#55329=CARTESIAN_POINT('Ctrl Pts',(66.2024832934866,-23.1474017566484,12.));
#55330=CARTESIAN_POINT('Ctrl Pts',(66.2222592165473,-23.1487761349328,0.));
#55331=CARTESIAN_POINT('Ctrl Pts',(66.2222592165473,-23.1487761349328,12.));
#55332=CARTESIAN_POINT('Ctrl Pts',(66.2420899237317,-23.1501329914488,0.));
#55333=CARTESIAN_POINT('Ctrl Pts',(66.2420899237317,-23.1501329914488,12.));
#55334=CARTESIAN_POINT('Ctrl Pts',(66.2619751878741,-23.1514722022483,0.));
#55335=CARTESIAN_POINT('Ctrl Pts',(66.2619751878741,-23.1514722022483,12.));
#55336=CARTESIAN_POINT('Ctrl Pts',(66.2819148131071,-23.1527936592625,0.));
#55337=CARTESIAN_POINT('Ctrl Pts',(66.2819148131071,-23.1527936592625,12.));
#55338=CARTESIAN_POINT('Ctrl Pts',(66.301908627539,-23.154097266617,0.));
#55339=CARTESIAN_POINT('Ctrl Pts',(66.301908627539,-23.154097266617,12.));
#55340=CARTESIAN_POINT('Ctrl Pts',(66.3219564725161,-23.1553829352531,0.));
#55341=CARTESIAN_POINT('Ctrl Pts',(66.3219564725161,-23.1553829352531,12.));
#55342=CARTESIAN_POINT('Ctrl Pts',(66.3420581937159,-23.1566505784626,0.));
#55343=CARTESIAN_POINT('Ctrl Pts',(66.3420581937159,-23.1566505784626,12.));
#55344=CARTESIAN_POINT('Ctrl Pts',(66.3622136300691,-23.1579001063438,0.));
#55345=CARTESIAN_POINT('Ctrl Pts',(66.3622136300691,-23.1579001063438,12.));
#55346=CARTESIAN_POINT('Ctrl Pts',(66.382422608185,-23.1591314230101,0.));
#55347=CARTESIAN_POINT('Ctrl Pts',(66.382422608185,-23.1591314230101,12.));
#55348=CARTESIAN_POINT('Ctrl Pts',(66.402684948127,-23.1603444294754,0.));
#55349=CARTESIAN_POINT('Ctrl Pts',(66.402684948127,-23.1603444294754,12.));
#55350=CARTESIAN_POINT('Ctrl Pts',(66.4230004670288,-23.1615390254636,0.));
#55351=CARTESIAN_POINT('Ctrl Pts',(66.4230004670288,-23.1615390254636,12.));
#55352=CARTESIAN_POINT('Ctrl Pts',(66.4433689832454,-23.1627151114875,0.));
#55353=CARTESIAN_POINT('Ctrl Pts',(66.4433689832454,-23.1627151114875,12.));
#55354=CARTESIAN_POINT('Ctrl Pts',(66.4637903210682,-23.163872591218,0.));
#55355=CARTESIAN_POINT('Ctrl Pts',(66.4637903210682,-23.163872591218,12.));
#55356=CARTESIAN_POINT('Ctrl Pts',(66.4842643105263,-23.1650113713792,0.));
#55357=CARTESIAN_POINT('Ctrl Pts',(66.4842643105263,-23.1650113713792,12.));
#55358=CARTESIAN_POINT('Ctrl Pts',(66.5047907851318,-23.1661313606123,0.));
#55359=CARTESIAN_POINT('Ctrl Pts',(66.5047907851318,-23.1661313606123,12.));
#55360=CARTESIAN_POINT('Ctrl Pts',(66.5253695803208,-23.1672324686928,0.));
#55361=CARTESIAN_POINT('Ctrl Pts',(66.5253695803208,-23.1672324686928,12.));
#55362=CARTESIAN_POINT('Ctrl Pts',(66.5460005315406,-23.1683146055736,0.));
#55363=CARTESIAN_POINT('Ctrl Pts',(66.5460005315406,-23.1683146055736,12.));
#55364=CARTESIAN_POINT('Ctrl Pts',(66.5666834726494,-23.169377680588,0.));
#55365=CARTESIAN_POINT('Ctrl Pts',(66.5666834726494,-23.169377680588,12.));
#55366=CARTESIAN_POINT('Ctrl Pts',(66.5874182367596,-23.1704216028626,0.));
#55367=CARTESIAN_POINT('Ctrl Pts',(66.5874182367596,-23.1704216028626,12.));
#55368=CARTESIAN_POINT('Ctrl Pts',(66.6082046569657,-23.1714462816794,0.));
#55369=CARTESIAN_POINT('Ctrl Pts',(66.6082046569657,-23.1714462816794,12.));
#55370=CARTESIAN_POINT('Ctrl Pts',(66.6290425670538,-23.1724516268299,0.));
#55371=CARTESIAN_POINT('Ctrl Pts',(66.6290425670538,-23.1724516268299,12.));
#55372=CARTESIAN_POINT('Ctrl Pts',(66.6499318023445,-23.1734375490421,0.));
#55373=CARTESIAN_POINT('Ctrl Pts',(66.6499318023445,-23.1734375490421,12.));
#55374=CARTESIAN_POINT('Ctrl Pts',(66.6708722000046,-23.174403960137,0.));
#55375=CARTESIAN_POINT('Ctrl Pts',(66.6708722000046,-23.174403960137,12.));
#55376=CARTESIAN_POINT('Ctrl Pts',(66.691863598595,-23.1753507727932,0.));
#55377=CARTESIAN_POINT('Ctrl Pts',(66.691863598595,-23.1753507727932,12.));
#55378=CARTESIAN_POINT('Ctrl Pts',(66.712905837789,-23.1762779004043,0.));
#55379=CARTESIAN_POINT('Ctrl Pts',(66.712905837789,-23.1762779004043,12.));
#55380=CARTESIAN_POINT('Ctrl Pts',(66.7339987580441,-23.1771852569137,0.));
#55381=CARTESIAN_POINT('Ctrl Pts',(66.7339987580441,-23.1771852569137,12.));
#55382=CARTESIAN_POINT('Ctrl Pts',(66.7551422002229,-23.1780727566309,0.));
#55383=CARTESIAN_POINT('Ctrl Pts',(66.7551422002229,-23.1780727566309,12.));
#55384=CARTESIAN_POINT('Ctrl Pts',(66.7763360056146,-23.1789403142376,0.));
#55385=CARTESIAN_POINT('Ctrl Pts',(66.7763360056146,-23.1789403142376,12.));
#55386=CARTESIAN_POINT('Ctrl Pts',(66.7975800161014,-23.1797878448645,0.));
#55387=CARTESIAN_POINT('Ctrl Pts',(66.7975800161014,-23.1797878448645,12.));
#55388=CARTESIAN_POINT('Ctrl Pts',(66.8188740742727,-23.1806152641475,0.));
#55389=CARTESIAN_POINT('Ctrl Pts',(66.8188740742727,-23.1806152641475,12.));
#55390=CARTESIAN_POINT('Ctrl Pts',(66.8402180235549,-23.1814224882948,0.));
#55391=CARTESIAN_POINT('Ctrl Pts',(66.8402180235549,-23.1814224882948,12.));
#55392=CARTESIAN_POINT('Ctrl Pts',(66.8616117083304,-23.1822094341508,0.));
#55393=CARTESIAN_POINT('Ctrl Pts',(66.8616117083304,-23.1822094341508,12.));
#55394=CARTESIAN_POINT('Ctrl Pts',(66.8830549738768,-23.1829760191583,0.));
#55395=CARTESIAN_POINT('Ctrl Pts',(66.8830549738768,-23.1829760191583,12.));
#55396=CARTESIAN_POINT('Ctrl Pts',(66.904547666305,-23.1837221613231,0.));
#55397=CARTESIAN_POINT('Ctrl Pts',(66.904547666305,-23.1837221613231,12.));
#55398=CARTESIAN_POINT('Ctrl Pts',(66.9260896324955,-23.1844477791816,0.));
#55399=CARTESIAN_POINT('Ctrl Pts',(66.9260896324955,-23.1844477791816,12.));
#55400=CARTESIAN_POINT('Ctrl Pts',(66.9476807200225,-23.1851527917666,0.));
#55401=CARTESIAN_POINT('Ctrl Pts',(66.9476807200225,-23.1851527917666,12.));
#55402=CARTESIAN_POINT('Ctrl Pts',(66.9693207771058,-23.1858371185852,0.));
#55403=CARTESIAN_POINT('Ctrl Pts',(66.9693207771058,-23.1858371185852,12.));
#55404=CARTESIAN_POINT('Ctrl Pts',(66.9910096526483,-23.1865006796291,0.));
#55405=CARTESIAN_POINT('Ctrl Pts',(66.9910096526483,-23.1865006796291,12.));
#55406=CARTESIAN_POINT('Ctrl Pts',(67.0127471962507,-23.1871433953796,0.));
#55407=CARTESIAN_POINT('Ctrl Pts',(67.0127471962507,-23.1871433953796,12.));
#55408=CARTESIAN_POINT('Ctrl Pts',(67.0345332582297,-23.1877651868155,0.));
#55409=CARTESIAN_POINT('Ctrl Pts',(67.0345332582297,-23.1877651868155,12.));
#55410=CARTESIAN_POINT('Ctrl Pts',(67.0563676896312,-23.1883659754268,0.));
#55411=CARTESIAN_POINT('Ctrl Pts',(67.0563676896312,-23.1883659754268,12.));
#55412=CARTESIAN_POINT('Ctrl Pts',(67.0782503422293,-23.1889456832116,0.));
#55413=CARTESIAN_POINT('Ctrl Pts',(67.0782503422293,-23.1889456832116,12.));
#55414=CARTESIAN_POINT('Ctrl Pts',(67.1001810685137,-23.1895042326626,0.));
#55415=CARTESIAN_POINT('Ctrl Pts',(67.1001810685137,-23.1895042326626,12.));
#55416=CARTESIAN_POINT('Ctrl Pts',(67.122159721674,-23.1900415467575,0.));
#55417=CARTESIAN_POINT('Ctrl Pts',(67.122159721674,-23.1900415467575,12.));
#55418=CARTESIAN_POINT('Ctrl Pts',(67.1441861555819,-23.1905575489506,0.));
#55419=CARTESIAN_POINT('Ctrl Pts',(67.1441861555819,-23.1905575489506,12.));
#55420=CARTESIAN_POINT('Ctrl Pts',(67.1662602247641,-23.1910521631658,0.));
#55421=CARTESIAN_POINT('Ctrl Pts',(67.1662602247641,-23.1910521631658,12.));
#55422=CARTESIAN_POINT('Ctrl Pts',(67.1883817844039,-23.1915253137924,0.));
#55423=CARTESIAN_POINT('Ctrl Pts',(67.1883817844039,-23.1915253137924,12.));
#55424=CARTESIAN_POINT('Ctrl Pts',(67.2105506903448,-23.1919769256804,0.));
#55425=CARTESIAN_POINT('Ctrl Pts',(67.2105506903448,-23.1919769256804,12.));
#55426=CARTESIAN_POINT('Ctrl Pts',(67.232766799088,-23.1924069241386,0.));
#55427=CARTESIAN_POINT('Ctrl Pts',(67.232766799088,-23.1924069241386,12.));
#55428=CARTESIAN_POINT('Ctrl Pts',(67.2550299677888,-23.1928152349344,0.));
#55429=CARTESIAN_POINT('Ctrl Pts',(67.2550299677888,-23.1928152349344,12.));
#55430=CARTESIAN_POINT('Ctrl Pts',(67.2773400542477,-23.1932017842954,0.));
#55431=CARTESIAN_POINT('Ctrl Pts',(67.2773400542477,-23.1932017842954,12.));
#55432=CARTESIAN_POINT('Ctrl Pts',(67.2996969169099,-23.193566498902,0.));
#55433=CARTESIAN_POINT('Ctrl Pts',(67.2996969169099,-23.193566498902,12.));
#55434=CARTESIAN_POINT('Ctrl Pts',(67.3221004148604,-23.1939093058802,0.));
#55435=CARTESIAN_POINT('Ctrl Pts',(67.3221004148604,-23.1939093058802,12.));
#55436=CARTESIAN_POINT('Ctrl Pts',(67.3445504078178,-23.1942301327979,0.));
#55437=CARTESIAN_POINT('Ctrl Pts',(67.3445504078178,-23.1942301327979,12.));
#55438=CARTESIAN_POINT('Ctrl Pts',(67.3670467561205,-23.1945289076608,0.));
#55439=CARTESIAN_POINT('Ctrl Pts',(67.3670467561205,-23.1945289076608,12.));
#55440=CARTESIAN_POINT('Ctrl Pts',(67.3895893207168,-23.1948055589123,0.));
#55441=CARTESIAN_POINT('Ctrl Pts',(67.3895893207168,-23.1948055589123,12.));
#55442=CARTESIAN_POINT('Ctrl Pts',(67.4121779631666,-23.195060015426,0.));
#55443=CARTESIAN_POINT('Ctrl Pts',(67.4121779631666,-23.195060015426,12.));
#55444=CARTESIAN_POINT('Ctrl Pts',(67.4348125456389,-23.1952922065009,0.));
#55445=CARTESIAN_POINT('Ctrl Pts',(67.4348125456389,-23.1952922065009,12.));
#55446=CARTESIAN_POINT('Ctrl Pts',(67.4574929309078,-23.1955020618591,0.));
#55447=CARTESIAN_POINT('Ctrl Pts',(67.4574929309078,-23.1955020618591,12.));
#55448=CARTESIAN_POINT('Ctrl Pts',(67.4802189823423,-23.1956895116446,0.));
#55449=CARTESIAN_POINT('Ctrl Pts',(67.4802189823423,-23.1956895116446,12.));
#55450=CARTESIAN_POINT('Ctrl Pts',(67.5029905638973,-23.1958544864225,0.));
#55451=CARTESIAN_POINT('Ctrl Pts',(67.5029905638973,-23.1958544864225,12.));
#55452=CARTESIAN_POINT('Ctrl Pts',(67.525807540117,-23.195996917171,0.));
#55453=CARTESIAN_POINT('Ctrl Pts',(67.525807540117,-23.195996917171,12.));
#55454=CARTESIAN_POINT('Ctrl Pts',(67.5486697761301,-23.1961167352777,0.));
#55455=CARTESIAN_POINT('Ctrl Pts',(67.5486697761301,-23.1961167352777,12.));
#55456=CARTESIAN_POINT('Ctrl Pts',(67.5715771376454,-23.1962138725358,0.));
#55457=CARTESIAN_POINT('Ctrl Pts',(67.5715771376454,-23.1962138725358,12.));
#55458=CARTESIAN_POINT('Ctrl Pts',(67.5945294909398,-23.1962882611444,0.));
#55459=CARTESIAN_POINT('Ctrl Pts',(67.5945294909398,-23.1962882611444,12.));
#55460=CARTESIAN_POINT('Ctrl Pts',(67.6175267028516,-23.1963398337056,0.));
#55461=CARTESIAN_POINT('Ctrl Pts',(67.6175267028516,-23.1963398337056,12.));
#55462=CARTESIAN_POINT('Ctrl Pts',(67.6405686407828,-23.1963685232176,0.));
#55463=CARTESIAN_POINT('Ctrl Pts',(67.6405686407828,-23.1963685232176,12.));
#55464=CARTESIAN_POINT('Ctrl Pts',(67.6636551726948,-23.196374263071,0.));
#55465=CARTESIAN_POINT('Ctrl Pts',(67.6636551726948,-23.196374263071,12.));
#55466=CARTESIAN_POINT('Ctrl Pts',(67.6867861671044,-23.1963569870457,0.));
#55467=CARTESIAN_POINT('Ctrl Pts',(67.6867861671044,-23.1963569870457,12.));
#55468=CARTESIAN_POINT('Ctrl Pts',(67.7099614930711,-23.1963166293116,0.));
#55469=CARTESIAN_POINT('Ctrl Pts',(67.7099614930711,-23.1963166293116,12.));
#55470=CARTESIAN_POINT('Ctrl Pts',(67.7331810201931,-23.1962531244261,0.));
#55471=CARTESIAN_POINT('Ctrl Pts',(67.7331810201931,-23.1962531244261,12.));
#55472=CARTESIAN_POINT('Ctrl Pts',(67.7564446186115,-23.1961664073274,0.));
#55473=CARTESIAN_POINT('Ctrl Pts',(67.7564446186115,-23.1961664073274,12.));
#55474=CARTESIAN_POINT('Ctrl Pts',(67.7797521590056,-23.1960564133308,0.));
#55475=CARTESIAN_POINT('Ctrl Pts',(67.7797521590056,-23.1960564133308,12.));
#55476=CARTESIAN_POINT('Ctrl Pts',(67.8031035125873,-23.1959230781265,0.));
#55477=CARTESIAN_POINT('Ctrl Pts',(67.8031035125873,-23.1959230781265,12.));
#55478=CARTESIAN_POINT('Ctrl Pts',(67.8264985510884,-23.1957663377798,0.));
#55479=CARTESIAN_POINT('Ctrl Pts',(67.8264985510884,-23.1957663377798,12.));
#55480=CARTESIAN_POINT('Ctrl Pts',(67.8499371467578,-23.1955861287276,0.));
#55481=CARTESIAN_POINT('Ctrl Pts',(67.8499371467578,-23.1955861287276,12.));
#55482=CARTESIAN_POINT('Ctrl Pts',(67.8734191723639,-23.1953823877727,0.));
#55483=CARTESIAN_POINT('Ctrl Pts',(67.8734191723639,-23.1953823877727,12.));
#55484=CARTESIAN_POINT('Ctrl Pts',(67.8969445011907,-23.19515505208,0.));
#55485=CARTESIAN_POINT('Ctrl Pts',(67.8969445011907,-23.19515505208,12.));
#55486=CARTESIAN_POINT('Ctrl Pts',(67.9205130070337,-23.1949040591748,0.));
#55487=CARTESIAN_POINT('Ctrl Pts',(67.9205130070337,-23.1949040591748,12.));
#55488=CARTESIAN_POINT('Ctrl Pts',(67.944124564187,-23.1946293469437,0.));
#55489=CARTESIAN_POINT('Ctrl Pts',(67.944124564187,-23.1946293469437,12.));
#55490=CARTESIAN_POINT('Ctrl Pts',(67.9677790474414,-23.1943308536307,0.));
#55491=CARTESIAN_POINT('Ctrl Pts',(67.9677790474414,-23.1943308536307,12.));
#55492=CARTESIAN_POINT('Ctrl Pts',(67.9914763320878,-23.194008517832,0.));
#55493=CARTESIAN_POINT('Ctrl Pts',(67.9914763320878,-23.194008517832,12.));
#55494=CARTESIAN_POINT('Ctrl Pts',(68.0152162939123,-23.193662278492,0.));
#55495=CARTESIAN_POINT('Ctrl Pts',(68.0152162939123,-23.193662278492,12.));
#55496=CARTESIAN_POINT('Ctrl Pts',(68.0389988091926,-23.1932920749021,0.));
#55497=CARTESIAN_POINT('Ctrl Pts',(68.0389988091926,-23.1932920749021,12.));
#55498=CARTESIAN_POINT('Ctrl Pts',(68.0628237546852,-23.1928978467018,0.));
#55499=CARTESIAN_POINT('Ctrl Pts',(68.0628237546852,-23.1928978467018,12.));
#55500=CARTESIAN_POINT('Ctrl Pts',(68.086691007624,-23.1924795338746,0.));
#55501=CARTESIAN_POINT('Ctrl Pts',(68.086691007624,-23.1924795338746,12.));
#55502=CARTESIAN_POINT('Ctrl Pts',(68.1106004457223,-23.1920370767424,0.));
#55503=CARTESIAN_POINT('Ctrl Pts',(68.1106004457223,-23.1920370767424,12.));
#55504=CARTESIAN_POINT('Ctrl Pts',(68.1345519471695,-23.1915704159624,0.));
#55505=CARTESIAN_POINT('Ctrl Pts',(68.1345519471695,-23.1915704159624,12.));
#55506=CARTESIAN_POINT('Ctrl Pts',(68.1585453906259,-23.1910794925252,0.));
#55507=CARTESIAN_POINT('Ctrl Pts',(68.1585453906259,-23.1910794925252,12.));
#55508=CARTESIAN_POINT('Ctrl Pts',(68.182580655213,-23.1905642477572,0.));
#55509=CARTESIAN_POINT('Ctrl Pts',(68.182580655213,-23.1905642477572,12.));
#55510=CARTESIAN_POINT('Ctrl Pts',(68.2066576205113,-23.1900246233165,0.));
#55511=CARTESIAN_POINT('Ctrl Pts',(68.2066576205113,-23.1900246233165,12.));
#55512=CARTESIAN_POINT('Ctrl Pts',(68.2307761665629,-23.189460561187,0.));
#55513=CARTESIAN_POINT('Ctrl Pts',(68.2307761665629,-23.189460561187,12.));
#55514=CARTESIAN_POINT('Ctrl Pts',(68.2549361738679,-23.1888720036757,0.));
#55515=CARTESIAN_POINT('Ctrl Pts',(68.2549361738679,-23.1888720036757,12.));
#55516=CARTESIAN_POINT('Ctrl Pts',(68.2791375233798,-23.1882588934108,0.));
#55517=CARTESIAN_POINT('Ctrl Pts',(68.2791375233798,-23.1882588934108,12.));
#55518=CARTESIAN_POINT('Ctrl Pts',(68.3033800964946,-23.1876211733439,0.));
#55519=CARTESIAN_POINT('Ctrl Pts',(68.3033800964946,-23.1876211733439,12.));
#55520=CARTESIAN_POINT('Ctrl Pts',(68.3276637750494,-23.1869587867464,0.));
#55521=CARTESIAN_POINT('Ctrl Pts',(68.3276637750494,-23.1869587867464,12.));
#55522=CARTESIAN_POINT('Ctrl Pts',(68.3519884413253,-23.1862716772034,0.));
#55523=CARTESIAN_POINT('Ctrl Pts',(68.3519884413253,-23.1862716772034,12.));
#55524=CARTESIAN_POINT('Ctrl Pts',(68.3763539780442,-23.1855597886117,0.));
#55525=CARTESIAN_POINT('Ctrl Pts',(68.3763539780442,-23.1855597886117,12.));
#55526=CARTESIAN_POINT('Ctrl Pts',(68.4007602683649,-23.1848230651776,0.));
#55527=CARTESIAN_POINT('Ctrl Pts',(68.4007602683649,-23.1848230651776,12.));
#55528=CARTESIAN_POINT('Ctrl Pts',(68.4252071958725,-23.1840614514191,0.));
#55529=CARTESIAN_POINT('Ctrl Pts',(68.4252071958725,-23.1840614514191,12.));
#55530=CARTESIAN_POINT('Ctrl Pts',(68.4496946445756,-23.1832748921629,0.));
#55531=CARTESIAN_POINT('Ctrl Pts',(68.4496946445756,-23.1832748921629,12.));
#55532=CARTESIAN_POINT('Ctrl Pts',(68.4742224989099,-23.1824633325385,0.));
#55533=CARTESIAN_POINT('Ctrl Pts',(68.4742224989099,-23.1824633325385,12.));
#55534=CARTESIAN_POINT('Ctrl Pts',(68.4987906437357,-23.1816267179752,0.));
#55535=CARTESIAN_POINT('Ctrl Pts',(68.4987906437357,-23.1816267179752,12.));
#55536=CARTESIAN_POINT('Ctrl Pts',(68.5233989643343,-23.1807649942011,0.));
#55537=CARTESIAN_POINT('Ctrl Pts',(68.5233989643343,-23.1807649942011,12.));
#55538=CARTESIAN_POINT('Ctrl Pts',(68.548047346398,-23.1798781072449,0.));
#55539=CARTESIAN_POINT('Ctrl Pts',(68.548047346398,-23.1798781072449,12.));
#55540=CARTESIAN_POINT('Ctrl Pts',(68.572735676027,-23.178966003434,0.));
#55541=CARTESIAN_POINT('Ctrl Pts',(68.572735676027,-23.178966003434,12.));
#55542=CARTESIAN_POINT('Ctrl Pts',(68.5974638397322,-23.1780286293873,0.));
#55543=CARTESIAN_POINT('Ctrl Pts',(68.5974638397322,-23.1780286293873,12.));
#55544=CARTESIAN_POINT('Ctrl Pts',(68.6222317244336,-23.1770659320137,0.));
#55545=CARTESIAN_POINT('Ctrl Pts',(68.6222317244336,-23.1770659320137,12.));
#55546=CARTESIAN_POINT('Ctrl Pts',(68.6470392174567,-23.1760778585094,0.));
#55547=CARTESIAN_POINT('Ctrl Pts',(68.6470392174567,-23.1760778585094,12.));
#55548=CARTESIAN_POINT('Ctrl Pts',(68.6718862065227,-23.1750643563606,0.));
#55549=CARTESIAN_POINT('Ctrl Pts',(68.6718862065227,-23.1750643563606,12.));
#55550=CARTESIAN_POINT('Ctrl Pts',(68.6967725797457,-23.1740253733423,0.));
#55551=CARTESIAN_POINT('Ctrl Pts',(68.6967725797457,-23.1740253733423,12.));
#55552=CARTESIAN_POINT('Ctrl Pts',(68.7216982256357,-23.1729608575116,0.));
#55553=CARTESIAN_POINT('Ctrl Pts',(68.7216982256357,-23.1729608575116,12.));
#55554=CARTESIAN_POINT('Ctrl Pts',(68.7466630330968,-23.1718707572047,0.));
#55555=CARTESIAN_POINT('Ctrl Pts',(68.7466630330968,-23.1718707572047,12.));
#55556=CARTESIAN_POINT('Ctrl Pts',(68.7716668914246,-23.1707550210359,0.));
#55557=CARTESIAN_POINT('Ctrl Pts',(68.7716668914246,-23.1707550210359,12.));
#55558=CARTESIAN_POINT('Ctrl Pts',(68.7967096902981,-23.1696135978993,0.));
#55559=CARTESIAN_POINT('Ctrl Pts',(68.7967096902981,-23.1696135978993,12.));
#55560=CARTESIAN_POINT('Ctrl Pts',(68.8217913197735,-23.1684464369681,0.));
#55561=CARTESIAN_POINT('Ctrl Pts',(68.8217913197735,-23.1684464369681,12.));
#55562=CARTESIAN_POINT('Ctrl Pts',(68.8469116702885,-23.1672534876885,0.));
#55563=CARTESIAN_POINT('Ctrl Pts',(68.8469116702885,-23.1672534876885,12.));
#55564=CARTESIAN_POINT('Ctrl Pts',(68.8720706326605,-23.1660346997763,0.));
#55565=CARTESIAN_POINT('Ctrl Pts',(68.8720706326605,-23.1660346997763,12.));
#55566=CARTESIAN_POINT('Ctrl Pts',(68.8972680980844,-23.1647900232152,0.));
#55567=CARTESIAN_POINT('Ctrl Pts',(68.8972680980844,-23.1647900232152,12.));
#55568=CARTESIAN_POINT('Ctrl Pts',(68.9225039581249,-23.1635194082582,0.));
#55569=CARTESIAN_POINT('Ctrl Pts',(68.9225039581249,-23.1635194082582,12.));
#55570=CARTESIAN_POINT('Ctrl Pts',(68.9477781047103,-23.1622228054291,0.));
#55571=CARTESIAN_POINT('Ctrl Pts',(68.9477781047103,-23.1622228054291,12.));
#55572=CARTESIAN_POINT('Ctrl Pts',(68.9730904301362,-23.1609001655154,0.));
#55573=CARTESIAN_POINT('Ctrl Pts',(68.9730904301362,-23.1609001655154,12.));
#55574=CARTESIAN_POINT('Ctrl Pts',(68.9984408270652,-23.1595514395655,0.));
#55575=CARTESIAN_POINT('Ctrl Pts',(68.9984408270652,-23.1595514395655,12.));
#55576=CARTESIAN_POINT('Ctrl Pts',(69.0238291885245,-23.1581765788869,0.));
#55577=CARTESIAN_POINT('Ctrl Pts',(69.0238291885245,-23.1581765788869,12.));
#55578=CARTESIAN_POINT('Ctrl Pts',(69.0492554078999,-23.1567755350472,0.));
#55579=CARTESIAN_POINT('Ctrl Pts',(69.0492554078999,-23.1567755350472,12.));
#55580=CARTESIAN_POINT('Ctrl Pts',(69.0747193789291,-23.1553482598768,0.));
#55581=CARTESIAN_POINT('Ctrl Pts',(69.0747193789291,-23.1553482598768,12.));
#55582=CARTESIAN_POINT('Ctrl Pts',(69.1002209957036,-23.153894705462,0.));
#55583=CARTESIAN_POINT('Ctrl Pts',(69.1002209957036,-23.153894705462,12.));
#55584=CARTESIAN_POINT('Ctrl Pts',(69.1257601526692,-23.1524148241413,0.));
#55585=CARTESIAN_POINT('Ctrl Pts',(69.1257601526692,-23.1524148241413,12.));
#55586=CARTESIAN_POINT('Ctrl Pts',(69.1513367446231,-23.1509085685033,0.));
#55587=CARTESIAN_POINT('Ctrl Pts',(69.1513367446231,-23.1509085685033,12.));
#55588=CARTESIAN_POINT('Ctrl Pts',(69.176950666708,-23.1493758913857,0.));
#55589=CARTESIAN_POINT('Ctrl Pts',(69.176950666708,-23.1493758913857,12.));
#55590=CARTESIAN_POINT('Ctrl Pts',(69.2026018144023,-23.1478167458788,0.));
#55591=CARTESIAN_POINT('Ctrl Pts',(69.2026018144023,-23.1478167458788,12.));
#55592=CARTESIAN_POINT('Ctrl Pts',(69.2282900835234,-23.1462310853205,0.));
#55593=CARTESIAN_POINT('Ctrl Pts',(69.2282900835234,-23.1462310853205,12.));
#55594=CARTESIAN_POINT('Ctrl Pts',(69.2540153702311,-23.1446188632931,0.));
#55595=CARTESIAN_POINT('Ctrl Pts',(69.2540153702311,-23.1446188632931,12.));
#55596=CARTESIAN_POINT('Ctrl Pts',(69.2797775710275,-23.1429800336221,0.));
#55597=CARTESIAN_POINT('Ctrl Pts',(69.2797775710275,-23.1429800336221,12.));
#55598=CARTESIAN_POINT('Ctrl Pts',(69.3055765827544,-23.1413145503763,0.));
#55599=CARTESIAN_POINT('Ctrl Pts',(69.3055765827544,-23.1413145503763,12.));
#55600=CARTESIAN_POINT('Ctrl Pts',(69.3314123025863,-23.1396223678725,0.));
#55601=CARTESIAN_POINT('Ctrl Pts',(69.3314123025863,-23.1396223678725,12.));
#55602=CARTESIAN_POINT('Ctrl Pts',(69.3572846280289,-23.1379034406718,0.));
#55603=CARTESIAN_POINT('Ctrl Pts',(69.3572846280289,-23.1379034406718,12.));
#55604=CARTESIAN_POINT('Ctrl Pts',(69.3831934569176,-23.1361577235708,0.));
#55605=CARTESIAN_POINT('Ctrl Pts',(69.3831934569176,-23.1361577235708,12.));
#55606=CARTESIAN_POINT('Ctrl Pts',(69.4091386874129,-23.1343851715989,0.));
#55607=CARTESIAN_POINT('Ctrl Pts',(69.4091386874129,-23.1343851715989,12.));
#55608=CARTESIAN_POINT('Ctrl Pts',(69.4351202179948,-23.1325857400145,0.));
#55609=CARTESIAN_POINT('Ctrl Pts',(69.4351202179948,-23.1325857400145,12.));
#55610=CARTESIAN_POINT('Ctrl Pts',(69.4611379474491,-23.1307593843063,0.));
#55611=CARTESIAN_POINT('Ctrl Pts',(69.4611379474491,-23.1307593843063,12.));
#55612=CARTESIAN_POINT('Ctrl Pts',(69.4871917748665,-23.1289060601927,0.));
#55613=CARTESIAN_POINT('Ctrl Pts',(69.4871917748665,-23.1289060601927,12.));
#55614=CARTESIAN_POINT('Ctrl Pts',(69.5132815996548,-23.1270257236207,0.));
#55615=CARTESIAN_POINT('Ctrl Pts',(69.5132815996548,-23.1270257236207,12.));
#55616=CARTESIAN_POINT('Ctrl Pts',(69.5394073215467,-23.1251183307678,0.));
#55617=CARTESIAN_POINT('Ctrl Pts',(69.5394073215467,-23.1251183307678,12.));
#55618=CARTESIAN_POINT('Ctrl Pts',(69.565568840605,-23.1231838380452,0.));
#55619=CARTESIAN_POINT('Ctrl Pts',(69.565568840605,-23.1231838380452,12.));
#55620=CARTESIAN_POINT('Ctrl Pts',(69.5917660572255,-23.1212222021049,0.));
#55621=CARTESIAN_POINT('Ctrl Pts',(69.5917660572255,-23.1212222021049,12.));
#55622=CARTESIAN_POINT('Ctrl Pts',(69.617998872135,-23.1192333798438,0.));
#55623=CARTESIAN_POINT('Ctrl Pts',(69.617998872135,-23.1192333798438,12.));
#55624=CARTESIAN_POINT('Ctrl Pts',(69.6442671863751,-23.1172173283856,0.));
#55625=CARTESIAN_POINT('Ctrl Pts',(69.6442671863751,-23.1172173283856,12.));
#55626=CARTESIAN_POINT('Ctrl Pts',(69.6705709012842,-23.1151740050679,0.));
#55627=CARTESIAN_POINT('Ctrl Pts',(69.6705709012842,-23.1151740050679,12.));
#55628=CARTESIAN_POINT('Ctrl Pts',(69.6969099184766,-23.1131033674301,0.));
#55629=CARTESIAN_POINT('Ctrl Pts',(69.6969099184766,-23.1131033674301,12.));
#55630=CARTESIAN_POINT('Ctrl Pts',(69.7232841398207,-23.111005373205,0.));
#55631=CARTESIAN_POINT('Ctrl Pts',(69.7232841398207,-23.111005373205,12.));
#55632=CARTESIAN_POINT('Ctrl Pts',(69.7496934674083,-23.1088799803094,0.));
#55633=CARTESIAN_POINT('Ctrl Pts',(69.7496934674083,-23.1088799803094,12.));
#55634=CARTESIAN_POINT('Ctrl Pts',(69.7761378035978,-23.1067271468615,0.));
#55635=CARTESIAN_POINT('Ctrl Pts',(69.7761378035978,-23.1067271468615,12.));
#55636=CARTESIAN_POINT('Ctrl Pts',(69.8026170510582,-23.1045468311994,0.));
#55637=CARTESIAN_POINT('Ctrl Pts',(69.8026170510582,-23.1045468311994,12.));
#55638=CARTESIAN_POINT('Ctrl Pts',(69.8291311128121,-23.1023389919052,0.));
#55639=CARTESIAN_POINT('Ctrl Pts',(69.8291311128121,-23.1023389919052,12.));
#55640=CARTESIAN_POINT('Ctrl Pts',(69.8556798922687,-23.100103587824,0.));
#55641=CARTESIAN_POINT('Ctrl Pts',(69.8556798922687,-23.100103587824,12.));
#55642=CARTESIAN_POINT('Ctrl Pts',(69.8822632932759,-23.0978405781018,0.));
#55643=CARTESIAN_POINT('Ctrl Pts',(69.8822632932759,-23.0978405781018,12.));
#55644=CARTESIAN_POINT('Ctrl Pts',(69.9088812200703,-23.0955499221556,0.));
#55645=CARTESIAN_POINT('Ctrl Pts',(69.9088812200703,-23.0955499221556,12.));
#55646=CARTESIAN_POINT('Ctrl Pts',(69.9355335771722,-23.0932315796066,0.));
#55647=CARTESIAN_POINT('Ctrl Pts',(69.9355335771722,-23.0932315796066,12.));
#55648=CARTESIAN_POINT('Ctrl Pts',(69.9622202692871,-23.0908855102251,0.));
#55649=CARTESIAN_POINT('Ctrl Pts',(69.9622202692871,-23.0908855102251,12.));
#55650=CARTESIAN_POINT('Ctrl Pts',(69.9889412012143,-23.0885116738799,0.));
#55651=CARTESIAN_POINT('Ctrl Pts',(69.9889412012143,-23.0885116738799,12.));
#55652=CARTESIAN_POINT('Ctrl Pts',(70.0156962777173,-23.0861100304731,0.));
#55653=CARTESIAN_POINT('Ctrl Pts',(70.0156962777173,-23.0861100304731,12.));
#55654=CARTESIAN_POINT('Ctrl Pts',(70.0424854035125,-23.0836805399378,0.));
#55655=CARTESIAN_POINT('Ctrl Pts',(70.0424854035125,-23.0836805399378,12.));
#55656=CARTESIAN_POINT('Ctrl Pts',(70.0693084835387,-23.081223162377,0.));
#55657=CARTESIAN_POINT('Ctrl Pts',(70.0693084835387,-23.081223162377,12.));
#55658=CARTESIAN_POINT('Ctrl Pts',(70.096165423165,-23.0787378581778,0.));
#55659=CARTESIAN_POINT('Ctrl Pts',(70.096165423165,-23.0787378581778,12.));
#55660=CARTESIAN_POINT('Ctrl Pts',(70.1230561284222,-23.076224588139,0.));
#55661=CARTESIAN_POINT('Ctrl Pts',(70.1230561284222,-23.076224588139,12.));
#55662=CARTESIAN_POINT('Ctrl Pts',(70.1499805062159,-23.0736833135934,0.));
#55663=CARTESIAN_POINT('Ctrl Pts',(70.1499805062159,-23.0736833135934,12.));
#55664=CARTESIAN_POINT('Ctrl Pts',(70.176938464556,-23.0711139965432,0.));
#55665=CARTESIAN_POINT('Ctrl Pts',(70.176938464556,-23.0711139965432,12.));
#55666=CARTESIAN_POINT('Ctrl Pts',(70.2039299120456,-23.0685165993682,0.));
#55667=CARTESIAN_POINT('Ctrl Pts',(70.2039299120456,-23.0685165993682,12.));
#55668=CARTESIAN_POINT('Ctrl Pts',(70.2309547573788,-23.0658910845425,0.));
#55669=CARTESIAN_POINT('Ctrl Pts',(70.2309547573788,-23.0658910845425,12.));
#55670=CARTESIAN_POINT('Ctrl Pts',(70.2580129087877,-23.0632374143276,0.));
#55671=CARTESIAN_POINT('Ctrl Pts',(70.2580129087877,-23.0632374143276,12.));
#55672=CARTESIAN_POINT('Ctrl Pts',(70.2851042736081,-23.0605555505326,0.));
#55673=CARTESIAN_POINT('Ctrl Pts',(70.2851042736081,-23.0605555505326,12.));
#55674=CARTESIAN_POINT('Ctrl Pts',(70.3122287575374,-23.0578454541116,0.));
#55675=CARTESIAN_POINT('Ctrl Pts',(70.3122287575374,-23.0578454541116,12.));
#55676=CARTESIAN_POINT('Ctrl Pts',(70.3393862652353,-23.0551070854942,0.));
#55677=CARTESIAN_POINT('Ctrl Pts',(70.3393862652353,-23.0551070854942,12.));
#55678=CARTESIAN_POINT('Ctrl Pts',(70.3665767016596,-23.0523404053188,0.));
#55679=CARTESIAN_POINT('Ctrl Pts',(70.3665767016596,-23.0523404053188,12.));
#55680=CARTESIAN_POINT('Ctrl Pts',(70.39379997323,-23.0495453750773,0.));
#55681=CARTESIAN_POINT('Ctrl Pts',(70.39379997323,-23.0495453750773,12.));
#55682=CARTESIAN_POINT('Ctrl Pts',(70.421055988934,-23.0467219577289,0.));
#55683=CARTESIAN_POINT('Ctrl Pts',(70.421055988934,-23.0467219577289,12.));
#55684=CARTESIAN_POINT('Ctrl Pts',(70.4483446617552,-23.0438701184996,0.));
#55685=CARTESIAN_POINT('Ctrl Pts',(70.4483446617552,-23.0438701184996,12.));
#55686=CARTESIAN_POINT('Ctrl Pts',(70.4756659090104,-23.0409898250727,0.));
#55687=CARTESIAN_POINT('Ctrl Pts',(70.4756659090104,-23.0409898250727,12.));
#55688=CARTESIAN_POINT('Ctrl Pts',(70.5030196491883,-23.0380810458237,0.));
#55689=CARTESIAN_POINT('Ctrl Pts',(70.5030196491883,-23.0380810458237,12.));
#55690=CARTESIAN_POINT('Ctrl Pts',(70.5304057994537,-23.035143748431,0.));
#55691=CARTESIAN_POINT('Ctrl Pts',(70.5304057994537,-23.035143748431,12.));
#55692=CARTESIAN_POINT('Ctrl Pts',(70.5578242727606,-23.0321778982705,0.));
#55693=CARTESIAN_POINT('Ctrl Pts',(70.5578242727606,-23.0321778982705,12.));
#55694=CARTESIAN_POINT('Ctrl Pts',(70.5852749754167,-23.0291834570688,0.));
#55695=CARTESIAN_POINT('Ctrl Pts',(70.5852749754167,-23.0291834570688,12.));
#55696=CARTESIAN_POINT('Ctrl Pts',(70.6127578036869,-23.0261603810187,0.));
#55697=CARTESIAN_POINT('Ctrl Pts',(70.6127578036869,-23.0261603810187,12.));
#55698=CARTESIAN_POINT('Ctrl Pts',(70.6402726486718,-23.0231086235263,0.));
#55699=CARTESIAN_POINT('Ctrl Pts',(70.6402726486718,-23.0231086235263,12.));
#55700=CARTESIAN_POINT('Ctrl Pts',(70.6678194023388,-23.0200281385906,0.));
#55701=CARTESIAN_POINT('Ctrl Pts',(70.6678194023388,-23.0200281385906,12.));
#55702=CARTESIAN_POINT('Ctrl Pts',(70.6953979633561,-23.0169188841084,0.));
#55703=CARTESIAN_POINT('Ctrl Pts',(70.6953979633561,-23.0169188841084,12.));
#55704=CARTESIAN_POINT('Ctrl Pts',(70.7230082425324,-23.0137808248899,0.));
#55705=CARTESIAN_POINT('Ctrl Pts',(70.7230082425324,-23.0137808248899,12.));
#55706=CARTESIAN_POINT('Ctrl Pts',(70.7506501695822,-23.0106139365941,0.));
#55707=CARTESIAN_POINT('Ctrl Pts',(70.7506501695822,-23.0106139365941,12.));
#55708=CARTESIAN_POINT('Ctrl Pts',(70.7783236950588,-23.0074182063611,0.));
#55709=CARTESIAN_POINT('Ctrl Pts',(70.7783236950588,-23.0074182063611,12.));
#55710=CARTESIAN_POINT('Ctrl Pts',(70.806028785987,-23.004193629142,0.));
#55711=CARTESIAN_POINT('Ctrl Pts',(70.806028785987,-23.004193629142,12.));
#55712=CARTESIAN_POINT('Ctrl Pts',(70.8282180956627,-23.0015908899222,0.));
#55713=CARTESIAN_POINT('Ctrl Pts',(70.8282180956627,-23.0015908899222,12.));
#55714=CARTESIAN_POINT('Ctrl Pts',(70.8448742696328,-22.9996258555187,0.));
#55715=CARTESIAN_POINT('Ctrl Pts',(70.8448742696328,-22.9996258555187,12.));
#55716=CARTESIAN_POINT('Ctrl Pts',(70.8559846927868,-22.9983100639354,0.));
#55717=CARTESIAN_POINT('Ctrl Pts',(70.8559846927868,-22.9983100639354,12.));
#55718=CARTESIAN_POINT('Ctrl Pts',(70.8615414811571,-22.9976507259817,0.));
#55719=CARTESIAN_POINT('Ctrl Pts',(70.8615414811571,-22.9976507259817,12.));
#55720=CARTESIAN_POINT('',(66.0656156664138,-23.1372951448024,0.));
#55721=CARTESIAN_POINT('Ctrl Pts',(66.0656156664138,-23.1372951448024,0.));
#55722=CARTESIAN_POINT('Ctrl Pts',(66.0694876382126,-23.1375957166104,0.));
#55723=CARTESIAN_POINT('Ctrl Pts',(66.0772371487248,-23.13819515974,0.));
#55724=CARTESIAN_POINT('Ctrl Pts',(66.088878115242,-23.1390892229779,0.));
#55725=CARTESIAN_POINT('Ctrl Pts',(66.1044328067355,-23.1402711039425,0.));
#55726=CARTESIAN_POINT('Ctrl Pts',(66.1239318368548,-23.1417314398398,0.));
#55727=CARTESIAN_POINT('Ctrl Pts',(66.1434865015027,-23.1431747350098,0.));
#55728=CARTESIAN_POINT('Ctrl Pts',(66.1630967296747,-23.1446009424903,0.));
#55729=CARTESIAN_POINT('Ctrl Pts',(66.1827623902899,-23.1460099850763,0.));
#55730=CARTESIAN_POINT('Ctrl Pts',(66.2024832934866,-23.1474017566484,0.));
#55731=CARTESIAN_POINT('Ctrl Pts',(66.2222592165473,-23.1487761349328,0.));
#55732=CARTESIAN_POINT('Ctrl Pts',(66.2420899237317,-23.1501329914488,0.));
#55733=CARTESIAN_POINT('Ctrl Pts',(66.2619751878741,-23.1514722022483,0.));
#55734=CARTESIAN_POINT('Ctrl Pts',(66.2819148131071,-23.1527936592625,0.));
#55735=CARTESIAN_POINT('Ctrl Pts',(66.301908627539,-23.154097266617,0.));
#55736=CARTESIAN_POINT('Ctrl Pts',(66.3219564725161,-23.1553829352531,0.));
#55737=CARTESIAN_POINT('Ctrl Pts',(66.3420581937159,-23.1566505784626,0.));
#55738=CARTESIAN_POINT('Ctrl Pts',(66.3622136300691,-23.1579001063438,0.));
#55739=CARTESIAN_POINT('Ctrl Pts',(66.382422608185,-23.1591314230101,0.));
#55740=CARTESIAN_POINT('Ctrl Pts',(66.402684948127,-23.1603444294754,0.));
#55741=CARTESIAN_POINT('Ctrl Pts',(66.4230004670288,-23.1615390254636,0.));
#55742=CARTESIAN_POINT('Ctrl Pts',(66.4433689832454,-23.1627151114875,0.));
#55743=CARTESIAN_POINT('Ctrl Pts',(66.4637903210682,-23.163872591218,0.));
#55744=CARTESIAN_POINT('Ctrl Pts',(66.4842643105263,-23.1650113713792,0.));
#55745=CARTESIAN_POINT('Ctrl Pts',(66.5047907851318,-23.1661313606123,0.));
#55746=CARTESIAN_POINT('Ctrl Pts',(66.5253695803208,-23.1672324686928,0.));
#55747=CARTESIAN_POINT('Ctrl Pts',(66.5460005315406,-23.1683146055736,0.));
#55748=CARTESIAN_POINT('Ctrl Pts',(66.5666834726494,-23.169377680588,0.));
#55749=CARTESIAN_POINT('Ctrl Pts',(66.5874182367596,-23.1704216028626,0.));
#55750=CARTESIAN_POINT('Ctrl Pts',(66.6082046569657,-23.1714462816794,0.));
#55751=CARTESIAN_POINT('Ctrl Pts',(66.6290425670538,-23.1724516268299,0.));
#55752=CARTESIAN_POINT('Ctrl Pts',(66.6499318023445,-23.1734375490421,0.));
#55753=CARTESIAN_POINT('Ctrl Pts',(66.6708722000046,-23.174403960137,0.));
#55754=CARTESIAN_POINT('Ctrl Pts',(66.691863598595,-23.1753507727932,0.));
#55755=CARTESIAN_POINT('Ctrl Pts',(66.712905837789,-23.1762779004043,0.));
#55756=CARTESIAN_POINT('Ctrl Pts',(66.7339987580441,-23.1771852569137,0.));
#55757=CARTESIAN_POINT('Ctrl Pts',(66.7551422002229,-23.1780727566309,0.));
#55758=CARTESIAN_POINT('Ctrl Pts',(66.7763360056146,-23.1789403142376,0.));
#55759=CARTESIAN_POINT('Ctrl Pts',(66.7975800161014,-23.1797878448645,0.));
#55760=CARTESIAN_POINT('Ctrl Pts',(66.8188740742727,-23.1806152641475,0.));
#55761=CARTESIAN_POINT('Ctrl Pts',(66.8402180235549,-23.1814224882948,0.));
#55762=CARTESIAN_POINT('Ctrl Pts',(66.8616117083304,-23.1822094341508,0.));
#55763=CARTESIAN_POINT('Ctrl Pts',(66.8830549738768,-23.1829760191583,0.));
#55764=CARTESIAN_POINT('Ctrl Pts',(66.904547666305,-23.1837221613231,0.));
#55765=CARTESIAN_POINT('Ctrl Pts',(66.9260896324955,-23.1844477791816,0.));
#55766=CARTESIAN_POINT('Ctrl Pts',(66.9476807200225,-23.1851527917666,0.));
#55767=CARTESIAN_POINT('Ctrl Pts',(66.9693207771058,-23.1858371185852,0.));
#55768=CARTESIAN_POINT('Ctrl Pts',(66.9910096526483,-23.1865006796291,0.));
#55769=CARTESIAN_POINT('Ctrl Pts',(67.0127471962507,-23.1871433953796,0.));
#55770=CARTESIAN_POINT('Ctrl Pts',(67.0345332582297,-23.1877651868155,0.));
#55771=CARTESIAN_POINT('Ctrl Pts',(67.0563676896312,-23.1883659754268,0.));
#55772=CARTESIAN_POINT('Ctrl Pts',(67.0782503422293,-23.1889456832116,0.));
#55773=CARTESIAN_POINT('Ctrl Pts',(67.1001810685137,-23.1895042326626,0.));
#55774=CARTESIAN_POINT('Ctrl Pts',(67.122159721674,-23.1900415467575,0.));
#55775=CARTESIAN_POINT('Ctrl Pts',(67.1441861555819,-23.1905575489506,0.));
#55776=CARTESIAN_POINT('Ctrl Pts',(67.1662602247641,-23.1910521631658,0.));
#55777=CARTESIAN_POINT('Ctrl Pts',(67.1883817844039,-23.1915253137924,0.));
#55778=CARTESIAN_POINT('Ctrl Pts',(67.2105506903448,-23.1919769256804,0.));
#55779=CARTESIAN_POINT('Ctrl Pts',(67.232766799088,-23.1924069241386,0.));
#55780=CARTESIAN_POINT('Ctrl Pts',(67.2550299677888,-23.1928152349344,0.));
#55781=CARTESIAN_POINT('Ctrl Pts',(67.2773400542477,-23.1932017842954,0.));
#55782=CARTESIAN_POINT('Ctrl Pts',(67.2996969169099,-23.193566498902,0.));
#55783=CARTESIAN_POINT('Ctrl Pts',(67.3221004148604,-23.1939093058802,0.));
#55784=CARTESIAN_POINT('Ctrl Pts',(67.3445504078178,-23.1942301327979,0.));
#55785=CARTESIAN_POINT('Ctrl Pts',(67.3670467561205,-23.1945289076608,0.));
#55786=CARTESIAN_POINT('Ctrl Pts',(67.3895893207168,-23.1948055589123,0.));
#55787=CARTESIAN_POINT('Ctrl Pts',(67.4121779631666,-23.195060015426,0.));
#55788=CARTESIAN_POINT('Ctrl Pts',(67.4348125456389,-23.1952922065009,0.));
#55789=CARTESIAN_POINT('Ctrl Pts',(67.4574929309078,-23.1955020618591,0.));
#55790=CARTESIAN_POINT('Ctrl Pts',(67.4802189823423,-23.1956895116446,0.));
#55791=CARTESIAN_POINT('Ctrl Pts',(67.5029905638973,-23.1958544864225,0.));
#55792=CARTESIAN_POINT('Ctrl Pts',(67.525807540117,-23.195996917171,0.));
#55793=CARTESIAN_POINT('Ctrl Pts',(67.5486697761301,-23.1961167352777,0.));
#55794=CARTESIAN_POINT('Ctrl Pts',(67.5715771376454,-23.1962138725358,0.));
#55795=CARTESIAN_POINT('Ctrl Pts',(67.5945294909398,-23.1962882611444,0.));
#55796=CARTESIAN_POINT('Ctrl Pts',(67.6175267028516,-23.1963398337056,0.));
#55797=CARTESIAN_POINT('Ctrl Pts',(67.6405686407828,-23.1963685232176,0.));
#55798=CARTESIAN_POINT('Ctrl Pts',(67.6636551726948,-23.196374263071,0.));
#55799=CARTESIAN_POINT('Ctrl Pts',(67.6867861671044,-23.1963569870457,0.));
#55800=CARTESIAN_POINT('Ctrl Pts',(67.7099614930711,-23.1963166293116,0.));
#55801=CARTESIAN_POINT('Ctrl Pts',(67.7331810201931,-23.1962531244261,0.));
#55802=CARTESIAN_POINT('Ctrl Pts',(67.7564446186115,-23.1961664073274,0.));
#55803=CARTESIAN_POINT('Ctrl Pts',(67.7797521590056,-23.1960564133308,0.));
#55804=CARTESIAN_POINT('Ctrl Pts',(67.8031035125873,-23.1959230781265,0.));
#55805=CARTESIAN_POINT('Ctrl Pts',(67.8264985510884,-23.1957663377798,0.));
#55806=CARTESIAN_POINT('Ctrl Pts',(67.8499371467578,-23.1955861287276,0.));
#55807=CARTESIAN_POINT('Ctrl Pts',(67.8734191723639,-23.1953823877727,0.));
#55808=CARTESIAN_POINT('Ctrl Pts',(67.8969445011907,-23.19515505208,0.));
#55809=CARTESIAN_POINT('Ctrl Pts',(67.9205130070337,-23.1949040591748,0.));
#55810=CARTESIAN_POINT('Ctrl Pts',(67.944124564187,-23.1946293469437,0.));
#55811=CARTESIAN_POINT('Ctrl Pts',(67.9677790474414,-23.1943308536307,0.));
#55812=CARTESIAN_POINT('Ctrl Pts',(67.9914763320878,-23.194008517832,0.));
#55813=CARTESIAN_POINT('Ctrl Pts',(68.0152162939123,-23.193662278492,0.));
#55814=CARTESIAN_POINT('Ctrl Pts',(68.0389988091926,-23.1932920749021,0.));
#55815=CARTESIAN_POINT('Ctrl Pts',(68.0628237546852,-23.1928978467018,0.));
#55816=CARTESIAN_POINT('Ctrl Pts',(68.086691007624,-23.1924795338746,0.));
#55817=CARTESIAN_POINT('Ctrl Pts',(68.1106004457223,-23.1920370767424,0.));
#55818=CARTESIAN_POINT('Ctrl Pts',(68.1345519471695,-23.1915704159624,0.));
#55819=CARTESIAN_POINT('Ctrl Pts',(68.1585453906259,-23.1910794925252,0.));
#55820=CARTESIAN_POINT('Ctrl Pts',(68.182580655213,-23.1905642477572,0.));
#55821=CARTESIAN_POINT('Ctrl Pts',(68.2066576205113,-23.1900246233165,0.));
#55822=CARTESIAN_POINT('Ctrl Pts',(68.2307761665629,-23.189460561187,0.));
#55823=CARTESIAN_POINT('Ctrl Pts',(68.2549361738679,-23.1888720036757,0.));
#55824=CARTESIAN_POINT('Ctrl Pts',(68.2791375233798,-23.1882588934108,0.));
#55825=CARTESIAN_POINT('Ctrl Pts',(68.3033800964946,-23.1876211733439,0.));
#55826=CARTESIAN_POINT('Ctrl Pts',(68.3276637750494,-23.1869587867464,0.));
#55827=CARTESIAN_POINT('Ctrl Pts',(68.3519884413253,-23.1862716772034,0.));
#55828=CARTESIAN_POINT('Ctrl Pts',(68.3763539780442,-23.1855597886117,0.));
#55829=CARTESIAN_POINT('Ctrl Pts',(68.4007602683649,-23.1848230651776,0.));
#55830=CARTESIAN_POINT('Ctrl Pts',(68.4252071958725,-23.1840614514191,0.));
#55831=CARTESIAN_POINT('Ctrl Pts',(68.4496946445756,-23.1832748921629,0.));
#55832=CARTESIAN_POINT('Ctrl Pts',(68.4742224989099,-23.1824633325385,0.));
#55833=CARTESIAN_POINT('Ctrl Pts',(68.4987906437357,-23.1816267179752,0.));
#55834=CARTESIAN_POINT('Ctrl Pts',(68.5233989643343,-23.1807649942011,0.));
#55835=CARTESIAN_POINT('Ctrl Pts',(68.548047346398,-23.1798781072449,0.));
#55836=CARTESIAN_POINT('Ctrl Pts',(68.572735676027,-23.178966003434,0.));
#55837=CARTESIAN_POINT('Ctrl Pts',(68.5974638397322,-23.1780286293873,0.));
#55838=CARTESIAN_POINT('Ctrl Pts',(68.6222317244336,-23.1770659320137,0.));
#55839=CARTESIAN_POINT('Ctrl Pts',(68.6470392174567,-23.1760778585094,0.));
#55840=CARTESIAN_POINT('Ctrl Pts',(68.6718862065227,-23.1750643563606,0.));
#55841=CARTESIAN_POINT('Ctrl Pts',(68.6967725797457,-23.1740253733423,0.));
#55842=CARTESIAN_POINT('Ctrl Pts',(68.7216982256357,-23.1729608575116,0.));
#55843=CARTESIAN_POINT('Ctrl Pts',(68.7466630330968,-23.1718707572047,0.));
#55844=CARTESIAN_POINT('Ctrl Pts',(68.7716668914246,-23.1707550210359,0.));
#55845=CARTESIAN_POINT('Ctrl Pts',(68.7967096902981,-23.1696135978993,0.));
#55846=CARTESIAN_POINT('Ctrl Pts',(68.8217913197735,-23.1684464369681,0.));
#55847=CARTESIAN_POINT('Ctrl Pts',(68.8469116702885,-23.1672534876885,0.));
#55848=CARTESIAN_POINT('Ctrl Pts',(68.8720706326605,-23.1660346997763,0.));
#55849=CARTESIAN_POINT('Ctrl Pts',(68.8972680980844,-23.1647900232152,0.));
#55850=CARTESIAN_POINT('Ctrl Pts',(68.9225039581249,-23.1635194082582,0.));
#55851=CARTESIAN_POINT('Ctrl Pts',(68.9477781047103,-23.1622228054291,0.));
#55852=CARTESIAN_POINT('Ctrl Pts',(68.9730904301362,-23.1609001655154,0.));
#55853=CARTESIAN_POINT('Ctrl Pts',(68.9984408270652,-23.1595514395655,0.));
#55854=CARTESIAN_POINT('Ctrl Pts',(69.0238291885245,-23.1581765788869,0.));
#55855=CARTESIAN_POINT('Ctrl Pts',(69.0492554078999,-23.1567755350472,0.));
#55856=CARTESIAN_POINT('Ctrl Pts',(69.0747193789291,-23.1553482598768,0.));
#55857=CARTESIAN_POINT('Ctrl Pts',(69.1002209957036,-23.153894705462,0.));
#55858=CARTESIAN_POINT('Ctrl Pts',(69.1257601526692,-23.1524148241413,0.));
#55859=CARTESIAN_POINT('Ctrl Pts',(69.1513367446231,-23.1509085685033,0.));
#55860=CARTESIAN_POINT('Ctrl Pts',(69.176950666708,-23.1493758913857,0.));
#55861=CARTESIAN_POINT('Ctrl Pts',(69.2026018144023,-23.1478167458788,0.));
#55862=CARTESIAN_POINT('Ctrl Pts',(69.2282900835234,-23.1462310853205,0.));
#55863=CARTESIAN_POINT('Ctrl Pts',(69.2540153702311,-23.1446188632931,0.));
#55864=CARTESIAN_POINT('Ctrl Pts',(69.2797775710275,-23.1429800336221,0.));
#55865=CARTESIAN_POINT('Ctrl Pts',(69.3055765827544,-23.1413145503763,0.));
#55866=CARTESIAN_POINT('Ctrl Pts',(69.3314123025863,-23.1396223678725,0.));
#55867=CARTESIAN_POINT('Ctrl Pts',(69.3572846280289,-23.1379034406718,0.));
#55868=CARTESIAN_POINT('Ctrl Pts',(69.3831934569176,-23.1361577235708,0.));
#55869=CARTESIAN_POINT('Ctrl Pts',(69.4091386874129,-23.1343851715989,0.));
#55870=CARTESIAN_POINT('Ctrl Pts',(69.4351202179948,-23.1325857400145,0.));
#55871=CARTESIAN_POINT('Ctrl Pts',(69.4611379474491,-23.1307593843063,0.));
#55872=CARTESIAN_POINT('Ctrl Pts',(69.4871917748665,-23.1289060601927,0.));
#55873=CARTESIAN_POINT('Ctrl Pts',(69.5132815996548,-23.1270257236207,0.));
#55874=CARTESIAN_POINT('Ctrl Pts',(69.5394073215467,-23.1251183307678,0.));
#55875=CARTESIAN_POINT('Ctrl Pts',(69.565568840605,-23.1231838380452,0.));
#55876=CARTESIAN_POINT('Ctrl Pts',(69.5917660572255,-23.1212222021049,0.));
#55877=CARTESIAN_POINT('Ctrl Pts',(69.617998872135,-23.1192333798438,0.));
#55878=CARTESIAN_POINT('Ctrl Pts',(69.6442671863751,-23.1172173283856,0.));
#55879=CARTESIAN_POINT('Ctrl Pts',(69.6705709012842,-23.1151740050679,0.));
#55880=CARTESIAN_POINT('Ctrl Pts',(69.6969099184766,-23.1131033674301,0.));
#55881=CARTESIAN_POINT('Ctrl Pts',(69.7232841398207,-23.111005373205,0.));
#55882=CARTESIAN_POINT('Ctrl Pts',(69.7496934674083,-23.1088799803094,0.));
#55883=CARTESIAN_POINT('Ctrl Pts',(69.7761378035978,-23.1067271468615,0.));
#55884=CARTESIAN_POINT('Ctrl Pts',(69.8026170510582,-23.1045468311994,0.));
#55885=CARTESIAN_POINT('Ctrl Pts',(69.8291311128121,-23.1023389919052,0.));
#55886=CARTESIAN_POINT('Ctrl Pts',(69.8556798922687,-23.100103587824,0.));
#55887=CARTESIAN_POINT('Ctrl Pts',(69.8822632932759,-23.0978405781018,0.));
#55888=CARTESIAN_POINT('Ctrl Pts',(69.9088812200703,-23.0955499221556,0.));
#55889=CARTESIAN_POINT('Ctrl Pts',(69.9355335771722,-23.0932315796066,0.));
#55890=CARTESIAN_POINT('Ctrl Pts',(69.9622202692871,-23.0908855102251,0.));
#55891=CARTESIAN_POINT('Ctrl Pts',(69.9889412012143,-23.0885116738799,0.));
#55892=CARTESIAN_POINT('Ctrl Pts',(70.0156962777173,-23.0861100304731,0.));
#55893=CARTESIAN_POINT('Ctrl Pts',(70.0424854035125,-23.0836805399378,0.));
#55894=CARTESIAN_POINT('Ctrl Pts',(70.0693084835387,-23.081223162377,0.));
#55895=CARTESIAN_POINT('Ctrl Pts',(70.096165423165,-23.0787378581778,0.));
#55896=CARTESIAN_POINT('Ctrl Pts',(70.1230561284222,-23.076224588139,0.));
#55897=CARTESIAN_POINT('Ctrl Pts',(70.1499805062159,-23.0736833135934,0.));
#55898=CARTESIAN_POINT('Ctrl Pts',(70.176938464556,-23.0711139965432,0.));
#55899=CARTESIAN_POINT('Ctrl Pts',(70.2039299120456,-23.0685165993682,0.));
#55900=CARTESIAN_POINT('Ctrl Pts',(70.2309547573788,-23.0658910845425,0.));
#55901=CARTESIAN_POINT('Ctrl Pts',(70.2580129087877,-23.0632374143276,0.));
#55902=CARTESIAN_POINT('Ctrl Pts',(70.2851042736081,-23.0605555505326,0.));
#55903=CARTESIAN_POINT('Ctrl Pts',(70.3122287575374,-23.0578454541116,0.));
#55904=CARTESIAN_POINT('Ctrl Pts',(70.3393862652353,-23.0551070854942,0.));
#55905=CARTESIAN_POINT('Ctrl Pts',(70.3665767016596,-23.0523404053188,0.));
#55906=CARTESIAN_POINT('Ctrl Pts',(70.39379997323,-23.0495453750773,0.));
#55907=CARTESIAN_POINT('Ctrl Pts',(70.421055988934,-23.0467219577289,0.));
#55908=CARTESIAN_POINT('Ctrl Pts',(70.4483446617552,-23.0438701184996,0.));
#55909=CARTESIAN_POINT('Ctrl Pts',(70.4756659090104,-23.0409898250727,0.));
#55910=CARTESIAN_POINT('Ctrl Pts',(70.4991133648756,-23.0384964376011,0.));
#55911=CARTESIAN_POINT('Ctrl Pts',(70.5171075702495,-23.0365694096159,0.));
#55912=CARTESIAN_POINT('Ctrl Pts',(70.5296341535253,-23.0352213647764,0.));
#55913=CARTESIAN_POINT('Ctrl Pts',(70.53668363813,-23.034460662331,0.));
#55914=CARTESIAN_POINT('Ctrl Pts',(70.5382514078489,-23.0342913834093,0.));
#55915=CARTESIAN_POINT('',(66.0656156664138,-23.1372951448024,12.));
#55916=CARTESIAN_POINT('',(66.0656156664138,-23.1372951448024,0.));
#55917=CARTESIAN_POINT('Ctrl Pts',(70.5382514078489,-23.0342913834094,12.));
#55918=CARTESIAN_POINT('Ctrl Pts',(70.53668363813,-23.034460662331,12.));
#55919=CARTESIAN_POINT('Ctrl Pts',(70.5296341535253,-23.0352213647764,12.));
#55920=CARTESIAN_POINT('Ctrl Pts',(70.5171075702495,-23.0365694096159,12.));
#55921=CARTESIAN_POINT('Ctrl Pts',(70.4991133648756,-23.0384964376011,12.));
#55922=CARTESIAN_POINT('Ctrl Pts',(70.4756659090104,-23.0409898250727,12.));
#55923=CARTESIAN_POINT('Ctrl Pts',(70.4483446617552,-23.0438701184996,12.));
#55924=CARTESIAN_POINT('Ctrl Pts',(70.421055988934,-23.0467219577289,12.));
#55925=CARTESIAN_POINT('Ctrl Pts',(70.39379997323,-23.0495453750773,12.));
#55926=CARTESIAN_POINT('Ctrl Pts',(70.3665767016596,-23.0523404053188,12.));
#55927=CARTESIAN_POINT('Ctrl Pts',(70.3393862652353,-23.0551070854942,12.));
#55928=CARTESIAN_POINT('Ctrl Pts',(70.3122287575374,-23.0578454541116,12.));
#55929=CARTESIAN_POINT('Ctrl Pts',(70.2851042736081,-23.0605555505326,12.));
#55930=CARTESIAN_POINT('Ctrl Pts',(70.2580129087877,-23.0632374143276,12.));
#55931=CARTESIAN_POINT('Ctrl Pts',(70.2309547573788,-23.0658910845425,12.));
#55932=CARTESIAN_POINT('Ctrl Pts',(70.2039299120456,-23.0685165993682,12.));
#55933=CARTESIAN_POINT('Ctrl Pts',(70.176938464556,-23.0711139965432,12.));
#55934=CARTESIAN_POINT('Ctrl Pts',(70.1499805062159,-23.0736833135934,12.));
#55935=CARTESIAN_POINT('Ctrl Pts',(70.1230561284222,-23.076224588139,12.));
#55936=CARTESIAN_POINT('Ctrl Pts',(70.096165423165,-23.0787378581778,12.));
#55937=CARTESIAN_POINT('Ctrl Pts',(70.0693084835387,-23.081223162377,12.));
#55938=CARTESIAN_POINT('Ctrl Pts',(70.0424854035125,-23.0836805399378,12.));
#55939=CARTESIAN_POINT('Ctrl Pts',(70.0156962777173,-23.0861100304731,12.));
#55940=CARTESIAN_POINT('Ctrl Pts',(69.9889412012143,-23.0885116738799,12.));
#55941=CARTESIAN_POINT('Ctrl Pts',(69.9622202692871,-23.0908855102251,12.));
#55942=CARTESIAN_POINT('Ctrl Pts',(69.9355335771722,-23.0932315796066,12.));
#55943=CARTESIAN_POINT('Ctrl Pts',(69.9088812200703,-23.0955499221556,12.));
#55944=CARTESIAN_POINT('Ctrl Pts',(69.8822632932759,-23.0978405781018,12.));
#55945=CARTESIAN_POINT('Ctrl Pts',(69.8556798922687,-23.100103587824,12.));
#55946=CARTESIAN_POINT('Ctrl Pts',(69.8291311128121,-23.1023389919052,12.));
#55947=CARTESIAN_POINT('Ctrl Pts',(69.8026170510582,-23.1045468311994,12.));
#55948=CARTESIAN_POINT('Ctrl Pts',(69.7761378035978,-23.1067271468615,12.));
#55949=CARTESIAN_POINT('Ctrl Pts',(69.7496934674083,-23.1088799803094,12.));
#55950=CARTESIAN_POINT('Ctrl Pts',(69.7232841398207,-23.111005373205,12.));
#55951=CARTESIAN_POINT('Ctrl Pts',(69.6969099184766,-23.1131033674301,12.));
#55952=CARTESIAN_POINT('Ctrl Pts',(69.6705709012842,-23.1151740050679,12.));
#55953=CARTESIAN_POINT('Ctrl Pts',(69.6442671863751,-23.1172173283856,12.));
#55954=CARTESIAN_POINT('Ctrl Pts',(69.617998872135,-23.1192333798438,12.));
#55955=CARTESIAN_POINT('Ctrl Pts',(69.5917660572255,-23.1212222021049,12.));
#55956=CARTESIAN_POINT('Ctrl Pts',(69.565568840605,-23.1231838380452,12.));
#55957=CARTESIAN_POINT('Ctrl Pts',(69.5394073215467,-23.1251183307678,12.));
#55958=CARTESIAN_POINT('Ctrl Pts',(69.5132815996548,-23.1270257236207,12.));
#55959=CARTESIAN_POINT('Ctrl Pts',(69.4871917748665,-23.1289060601927,12.));
#55960=CARTESIAN_POINT('Ctrl Pts',(69.4611379474491,-23.1307593843063,12.));
#55961=CARTESIAN_POINT('Ctrl Pts',(69.4351202179948,-23.1325857400145,12.));
#55962=CARTESIAN_POINT('Ctrl Pts',(69.4091386874129,-23.1343851715989,12.));
#55963=CARTESIAN_POINT('Ctrl Pts',(69.3831934569176,-23.1361577235708,12.));
#55964=CARTESIAN_POINT('Ctrl Pts',(69.3572846280289,-23.1379034406718,12.));
#55965=CARTESIAN_POINT('Ctrl Pts',(69.3314123025863,-23.1396223678725,12.));
#55966=CARTESIAN_POINT('Ctrl Pts',(69.3055765827544,-23.1413145503763,12.));
#55967=CARTESIAN_POINT('Ctrl Pts',(69.2797775710275,-23.1429800336221,12.));
#55968=CARTESIAN_POINT('Ctrl Pts',(69.2540153702311,-23.1446188632931,12.));
#55969=CARTESIAN_POINT('Ctrl Pts',(69.2282900835234,-23.1462310853205,12.));
#55970=CARTESIAN_POINT('Ctrl Pts',(69.2026018144023,-23.1478167458788,12.));
#55971=CARTESIAN_POINT('Ctrl Pts',(69.176950666708,-23.1493758913857,12.));
#55972=CARTESIAN_POINT('Ctrl Pts',(69.1513367446231,-23.1509085685033,12.));
#55973=CARTESIAN_POINT('Ctrl Pts',(69.1257601526692,-23.1524148241413,12.));
#55974=CARTESIAN_POINT('Ctrl Pts',(69.1002209957036,-23.153894705462,12.));
#55975=CARTESIAN_POINT('Ctrl Pts',(69.0747193789291,-23.1553482598768,12.));
#55976=CARTESIAN_POINT('Ctrl Pts',(69.0492554078999,-23.1567755350472,12.));
#55977=CARTESIAN_POINT('Ctrl Pts',(69.0238291885245,-23.1581765788869,12.));
#55978=CARTESIAN_POINT('Ctrl Pts',(68.9984408270652,-23.1595514395655,12.));
#55979=CARTESIAN_POINT('Ctrl Pts',(68.9730904301362,-23.1609001655154,12.));
#55980=CARTESIAN_POINT('Ctrl Pts',(68.9477781047103,-23.1622228054291,12.));
#55981=CARTESIAN_POINT('Ctrl Pts',(68.9225039581249,-23.1635194082582,12.));
#55982=CARTESIAN_POINT('Ctrl Pts',(68.8972680980844,-23.1647900232152,12.));
#55983=CARTESIAN_POINT('Ctrl Pts',(68.8720706326605,-23.1660346997763,12.));
#55984=CARTESIAN_POINT('Ctrl Pts',(68.8469116702885,-23.1672534876885,12.));
#55985=CARTESIAN_POINT('Ctrl Pts',(68.8217913197735,-23.1684464369681,12.));
#55986=CARTESIAN_POINT('Ctrl Pts',(68.7967096902981,-23.1696135978993,12.));
#55987=CARTESIAN_POINT('Ctrl Pts',(68.7716668914246,-23.1707550210359,12.));
#55988=CARTESIAN_POINT('Ctrl Pts',(68.7466630330968,-23.1718707572047,12.));
#55989=CARTESIAN_POINT('Ctrl Pts',(68.7216982256357,-23.1729608575116,12.));
#55990=CARTESIAN_POINT('Ctrl Pts',(68.6967725797457,-23.1740253733423,12.));
#55991=CARTESIAN_POINT('Ctrl Pts',(68.6718862065227,-23.1750643563606,12.));
#55992=CARTESIAN_POINT('Ctrl Pts',(68.6470392174567,-23.1760778585094,12.));
#55993=CARTESIAN_POINT('Ctrl Pts',(68.6222317244336,-23.1770659320137,12.));
#55994=CARTESIAN_POINT('Ctrl Pts',(68.5974638397322,-23.1780286293873,12.));
#55995=CARTESIAN_POINT('Ctrl Pts',(68.572735676027,-23.178966003434,12.));
#55996=CARTESIAN_POINT('Ctrl Pts',(68.548047346398,-23.1798781072449,12.));
#55997=CARTESIAN_POINT('Ctrl Pts',(68.5233989643343,-23.1807649942011,12.));
#55998=CARTESIAN_POINT('Ctrl Pts',(68.4987906437357,-23.1816267179752,12.));
#55999=CARTESIAN_POINT('Ctrl Pts',(68.4742224989099,-23.1824633325385,12.));
#56000=CARTESIAN_POINT('Ctrl Pts',(68.4496946445756,-23.1832748921629,12.));
#56001=CARTESIAN_POINT('Ctrl Pts',(68.4252071958725,-23.1840614514191,12.));
#56002=CARTESIAN_POINT('Ctrl Pts',(68.4007602683649,-23.1848230651776,12.));
#56003=CARTESIAN_POINT('Ctrl Pts',(68.3763539780442,-23.1855597886117,12.));
#56004=CARTESIAN_POINT('Ctrl Pts',(68.3519884413253,-23.1862716772034,12.));
#56005=CARTESIAN_POINT('Ctrl Pts',(68.3276637750494,-23.1869587867464,12.));
#56006=CARTESIAN_POINT('Ctrl Pts',(68.3033800964946,-23.1876211733439,12.));
#56007=CARTESIAN_POINT('Ctrl Pts',(68.2791375233798,-23.1882588934108,12.));
#56008=CARTESIAN_POINT('Ctrl Pts',(68.2549361738679,-23.1888720036757,12.));
#56009=CARTESIAN_POINT('Ctrl Pts',(68.2307761665629,-23.189460561187,12.));
#56010=CARTESIAN_POINT('Ctrl Pts',(68.2066576205113,-23.1900246233165,12.));
#56011=CARTESIAN_POINT('Ctrl Pts',(68.182580655213,-23.1905642477572,12.));
#56012=CARTESIAN_POINT('Ctrl Pts',(68.1585453906259,-23.1910794925252,12.));
#56013=CARTESIAN_POINT('Ctrl Pts',(68.1345519471695,-23.1915704159624,12.));
#56014=CARTESIAN_POINT('Ctrl Pts',(68.1106004457223,-23.1920370767424,12.));
#56015=CARTESIAN_POINT('Ctrl Pts',(68.086691007624,-23.1924795338746,12.));
#56016=CARTESIAN_POINT('Ctrl Pts',(68.0628237546852,-23.1928978467018,12.));
#56017=CARTESIAN_POINT('Ctrl Pts',(68.0389988091926,-23.1932920749021,12.));
#56018=CARTESIAN_POINT('Ctrl Pts',(68.0152162939123,-23.193662278492,12.));
#56019=CARTESIAN_POINT('Ctrl Pts',(67.9914763320878,-23.194008517832,12.));
#56020=CARTESIAN_POINT('Ctrl Pts',(67.9677790474414,-23.1943308536307,12.));
#56021=CARTESIAN_POINT('Ctrl Pts',(67.944124564187,-23.1946293469437,12.));
#56022=CARTESIAN_POINT('Ctrl Pts',(67.9205130070337,-23.1949040591748,12.));
#56023=CARTESIAN_POINT('Ctrl Pts',(67.8969445011907,-23.19515505208,12.));
#56024=CARTESIAN_POINT('Ctrl Pts',(67.8734191723639,-23.1953823877727,12.));
#56025=CARTESIAN_POINT('Ctrl Pts',(67.8499371467578,-23.1955861287276,12.));
#56026=CARTESIAN_POINT('Ctrl Pts',(67.8264985510884,-23.1957663377798,12.));
#56027=CARTESIAN_POINT('Ctrl Pts',(67.8031035125873,-23.1959230781265,12.));
#56028=CARTESIAN_POINT('Ctrl Pts',(67.7797521590056,-23.1960564133308,12.));
#56029=CARTESIAN_POINT('Ctrl Pts',(67.7564446186115,-23.1961664073274,12.));
#56030=CARTESIAN_POINT('Ctrl Pts',(67.7331810201931,-23.1962531244261,12.));
#56031=CARTESIAN_POINT('Ctrl Pts',(67.7099614930711,-23.1963166293116,12.));
#56032=CARTESIAN_POINT('Ctrl Pts',(67.6867861671044,-23.1963569870457,12.));
#56033=CARTESIAN_POINT('Ctrl Pts',(67.6636551726948,-23.196374263071,12.));
#56034=CARTESIAN_POINT('Ctrl Pts',(67.6405686407828,-23.1963685232176,12.));
#56035=CARTESIAN_POINT('Ctrl Pts',(67.6175267028516,-23.1963398337056,12.));
#56036=CARTESIAN_POINT('Ctrl Pts',(67.5945294909398,-23.1962882611444,12.));
#56037=CARTESIAN_POINT('Ctrl Pts',(67.5715771376454,-23.1962138725358,12.));
#56038=CARTESIAN_POINT('Ctrl Pts',(67.5486697761301,-23.1961167352777,12.));
#56039=CARTESIAN_POINT('Ctrl Pts',(67.525807540117,-23.195996917171,12.));
#56040=CARTESIAN_POINT('Ctrl Pts',(67.5029905638973,-23.1958544864225,12.));
#56041=CARTESIAN_POINT('Ctrl Pts',(67.4802189823423,-23.1956895116446,12.));
#56042=CARTESIAN_POINT('Ctrl Pts',(67.4574929309078,-23.1955020618591,12.));
#56043=CARTESIAN_POINT('Ctrl Pts',(67.4348125456389,-23.1952922065009,12.));
#56044=CARTESIAN_POINT('Ctrl Pts',(67.4121779631666,-23.195060015426,12.));
#56045=CARTESIAN_POINT('Ctrl Pts',(67.3895893207168,-23.1948055589123,12.));
#56046=CARTESIAN_POINT('Ctrl Pts',(67.3670467561205,-23.1945289076608,12.));
#56047=CARTESIAN_POINT('Ctrl Pts',(67.3445504078178,-23.1942301327979,12.));
#56048=CARTESIAN_POINT('Ctrl Pts',(67.3221004148604,-23.1939093058802,12.));
#56049=CARTESIAN_POINT('Ctrl Pts',(67.2996969169099,-23.193566498902,12.));
#56050=CARTESIAN_POINT('Ctrl Pts',(67.2773400542477,-23.1932017842954,12.));
#56051=CARTESIAN_POINT('Ctrl Pts',(67.2550299677888,-23.1928152349344,12.));
#56052=CARTESIAN_POINT('Ctrl Pts',(67.232766799088,-23.1924069241386,12.));
#56053=CARTESIAN_POINT('Ctrl Pts',(67.2105506903448,-23.1919769256804,12.));
#56054=CARTESIAN_POINT('Ctrl Pts',(67.1883817844039,-23.1915253137924,12.));
#56055=CARTESIAN_POINT('Ctrl Pts',(67.1662602247641,-23.1910521631658,12.));
#56056=CARTESIAN_POINT('Ctrl Pts',(67.1441861555819,-23.1905575489506,12.));
#56057=CARTESIAN_POINT('Ctrl Pts',(67.122159721674,-23.1900415467575,12.));
#56058=CARTESIAN_POINT('Ctrl Pts',(67.1001810685137,-23.1895042326626,12.));
#56059=CARTESIAN_POINT('Ctrl Pts',(67.0782503422293,-23.1889456832116,12.));
#56060=CARTESIAN_POINT('Ctrl Pts',(67.0563676896312,-23.1883659754268,12.));
#56061=CARTESIAN_POINT('Ctrl Pts',(67.0345332582297,-23.1877651868155,12.));
#56062=CARTESIAN_POINT('Ctrl Pts',(67.0127471962507,-23.1871433953796,12.));
#56063=CARTESIAN_POINT('Ctrl Pts',(66.9910096526483,-23.1865006796291,12.));
#56064=CARTESIAN_POINT('Ctrl Pts',(66.9693207771058,-23.1858371185852,12.));
#56065=CARTESIAN_POINT('Ctrl Pts',(66.9476807200225,-23.1851527917666,12.));
#56066=CARTESIAN_POINT('Ctrl Pts',(66.9260896324955,-23.1844477791816,12.));
#56067=CARTESIAN_POINT('Ctrl Pts',(66.904547666305,-23.1837221613231,12.));
#56068=CARTESIAN_POINT('Ctrl Pts',(66.8830549738768,-23.1829760191583,12.));
#56069=CARTESIAN_POINT('Ctrl Pts',(66.8616117083304,-23.1822094341508,12.));
#56070=CARTESIAN_POINT('Ctrl Pts',(66.8402180235549,-23.1814224882948,12.));
#56071=CARTESIAN_POINT('Ctrl Pts',(66.8188740742727,-23.1806152641475,12.));
#56072=CARTESIAN_POINT('Ctrl Pts',(66.7975800161014,-23.1797878448645,12.));
#56073=CARTESIAN_POINT('Ctrl Pts',(66.7763360056146,-23.1789403142376,12.));
#56074=CARTESIAN_POINT('Ctrl Pts',(66.7551422002229,-23.1780727566309,12.));
#56075=CARTESIAN_POINT('Ctrl Pts',(66.7339987580441,-23.1771852569137,12.));
#56076=CARTESIAN_POINT('Ctrl Pts',(66.712905837789,-23.1762779004043,12.));
#56077=CARTESIAN_POINT('Ctrl Pts',(66.691863598595,-23.1753507727932,12.));
#56078=CARTESIAN_POINT('Ctrl Pts',(66.6708722000046,-23.174403960137,12.));
#56079=CARTESIAN_POINT('Ctrl Pts',(66.6499318023445,-23.1734375490421,12.));
#56080=CARTESIAN_POINT('Ctrl Pts',(66.6290425670538,-23.1724516268299,12.));
#56081=CARTESIAN_POINT('Ctrl Pts',(66.6082046569657,-23.1714462816794,12.));
#56082=CARTESIAN_POINT('Ctrl Pts',(66.5874182367596,-23.1704216028626,12.));
#56083=CARTESIAN_POINT('Ctrl Pts',(66.5666834726494,-23.169377680588,12.));
#56084=CARTESIAN_POINT('Ctrl Pts',(66.5460005315406,-23.1683146055736,12.));
#56085=CARTESIAN_POINT('Ctrl Pts',(66.5253695803208,-23.1672324686928,12.));
#56086=CARTESIAN_POINT('Ctrl Pts',(66.5047907851318,-23.1661313606123,12.));
#56087=CARTESIAN_POINT('Ctrl Pts',(66.4842643105263,-23.1650113713792,12.));
#56088=CARTESIAN_POINT('Ctrl Pts',(66.4637903210682,-23.163872591218,12.));
#56089=CARTESIAN_POINT('Ctrl Pts',(66.4433689832454,-23.1627151114875,12.));
#56090=CARTESIAN_POINT('Ctrl Pts',(66.4230004670288,-23.1615390254636,12.));
#56091=CARTESIAN_POINT('Ctrl Pts',(66.402684948127,-23.1603444294754,12.));
#56092=CARTESIAN_POINT('Ctrl Pts',(66.382422608185,-23.1591314230101,12.));
#56093=CARTESIAN_POINT('Ctrl Pts',(66.3622136300691,-23.1579001063438,12.));
#56094=CARTESIAN_POINT('Ctrl Pts',(66.3420581937159,-23.1566505784626,12.));
#56095=CARTESIAN_POINT('Ctrl Pts',(66.3219564725161,-23.1553829352531,12.));
#56096=CARTESIAN_POINT('Ctrl Pts',(66.301908627539,-23.154097266617,12.));
#56097=CARTESIAN_POINT('Ctrl Pts',(66.2819148131071,-23.1527936592625,12.));
#56098=CARTESIAN_POINT('Ctrl Pts',(66.2619751878741,-23.1514722022483,12.));
#56099=CARTESIAN_POINT('Ctrl Pts',(66.2420899237317,-23.1501329914488,12.));
#56100=CARTESIAN_POINT('Ctrl Pts',(66.2222592165473,-23.1487761349328,12.));
#56101=CARTESIAN_POINT('Ctrl Pts',(66.2024832934866,-23.1474017566484,12.));
#56102=CARTESIAN_POINT('Ctrl Pts',(66.1827623902899,-23.1460099850763,12.));
#56103=CARTESIAN_POINT('Ctrl Pts',(66.1630967296747,-23.1446009424903,12.));
#56104=CARTESIAN_POINT('Ctrl Pts',(66.1434865015027,-23.1431747350098,12.));
#56105=CARTESIAN_POINT('Ctrl Pts',(66.1239318368548,-23.1417314398398,12.));
#56106=CARTESIAN_POINT('Ctrl Pts',(66.1044328067355,-23.1402711039425,12.));
#56107=CARTESIAN_POINT('Ctrl Pts',(66.088878115242,-23.1390892229779,12.));
#56108=CARTESIAN_POINT('Ctrl Pts',(66.0772371487248,-23.13819515974,12.));
#56109=CARTESIAN_POINT('Ctrl Pts',(66.0694876382126,-23.1375957166104,12.));
#56110=CARTESIAN_POINT('Ctrl Pts',(66.0656156664138,-23.1372951448024,12.));
#56111=CARTESIAN_POINT('Ctrl Pts',(70.9934796069117,-21.5904919935063,-5.55111512312578E-16));
#56112=CARTESIAN_POINT('Ctrl Pts',(70.9934796069117,-21.5904919935063,4.));
#56113=CARTESIAN_POINT('Ctrl Pts',(70.9934796069117,-21.5904919935063,8.));
#56114=CARTESIAN_POINT('Ctrl Pts',(70.9934796069117,-21.5904919935063,12.));
#56115=CARTESIAN_POINT('Ctrl Pts',(71.0762040404458,-21.6628164325802,-5.55111512312578E-16));
#56116=CARTESIAN_POINT('Ctrl Pts',(71.0762040404458,-21.6628164325802,4.));
#56117=CARTESIAN_POINT('Ctrl Pts',(71.0762040404458,-21.6628164325802,8.00000000000001));
#56118=CARTESIAN_POINT('Ctrl Pts',(71.0762040404458,-21.6628164325802,12.));
#56119=CARTESIAN_POINT('Ctrl Pts',(71.1771795679081,-21.8385342042357,-5.55111512312578E-16));
#56120=CARTESIAN_POINT('Ctrl Pts',(71.1771795679081,-21.8385342042357,4.));
#56121=CARTESIAN_POINT('Ctrl Pts',(71.1771795679082,-21.8385342042357,7.99999999999999));
#56122=CARTESIAN_POINT('Ctrl Pts',(71.1771795679082,-21.8385342042357,12.));
#56123=CARTESIAN_POINT('Ctrl Pts',(71.1663065220506,-22.0366423876808,-5.55111512312578E-16));
#56124=CARTESIAN_POINT('Ctrl Pts',(71.1663065220506,-22.0366423876808,4.));
#56125=CARTESIAN_POINT('Ctrl Pts',(71.1663065220506,-22.0366423876808,8.00000000000001));
#56126=CARTESIAN_POINT('Ctrl Pts',(71.1663065220506,-22.0366423876808,12.));
#56127=CARTESIAN_POINT('Ctrl Pts',(71.1418425484891,-22.1153394458689,-5.55111512312578E-16));
#56128=CARTESIAN_POINT('Ctrl Pts',(71.1418425484891,-22.1153394458689,4.));
#56129=CARTESIAN_POINT('Ctrl Pts',(71.1418425484892,-22.1153394458689,8.));
#56130=CARTESIAN_POINT('Ctrl Pts',(71.1418425484892,-22.1153394458689,12.));
#56131=CARTESIAN_POINT('',(70.9934796069117,-21.5904919935063,2.77555756156289E-16));
#56132=CARTESIAN_POINT('',(71.141842548489,-22.1153394458688,0.));
#56133=CARTESIAN_POINT('Ctrl Pts',(70.9934796069117,-21.5904919935063,-1.38777878078145E-16));
#56134=CARTESIAN_POINT('Ctrl Pts',(71.0762040404458,-21.6628164325802,-1.38777878078145E-16));
#56135=CARTESIAN_POINT('Ctrl Pts',(71.1339043418528,-21.7632265878119,-1.38777878078144E-16));
#56136=CARTESIAN_POINT('Ctrl Pts',(71.1550826601351,-21.8709478979137,-1.38777878078145E-16));
#56137=CARTESIAN_POINT('Ctrl Pts',(71.1709663988467,-21.95173888049,-1.38777878078145E-16));
#56138=CARTESIAN_POINT('Ctrl Pts',(71.1663065220506,-22.0366423876808,-1.38777878078145E-16));
#56139=CARTESIAN_POINT('Ctrl Pts',(71.1418425484891,-22.1153394458689,-1.38777878078145E-16));
#56140=CARTESIAN_POINT('',(71.141842548489,-22.1153394458688,12.));
#56141=CARTESIAN_POINT('Ctrl Pts',(71.1418425484891,-22.1153394458689,-5.55111512312578E-16));
#56142=CARTESIAN_POINT('Ctrl Pts',(71.1418425484891,-22.1153394458689,4.));
#56143=CARTESIAN_POINT('Ctrl Pts',(71.1418425484892,-22.1153394458689,8.));
#56144=CARTESIAN_POINT('Ctrl Pts',(71.1418425484892,-22.1153394458689,12.));
#56145=CARTESIAN_POINT('',(70.9934796069117,-21.5904919935063,12.));
#56146=CARTESIAN_POINT('Ctrl Pts',(71.1418425484892,-22.1153394458689,12.));
#56147=CARTESIAN_POINT('Ctrl Pts',(71.1663065220506,-22.0366423876808,12.));
#56148=CARTESIAN_POINT('Ctrl Pts',(71.1709663988467,-21.9517388804901,12.));
#56149=CARTESIAN_POINT('Ctrl Pts',(71.1550826601351,-21.8709478979137,12.));
#56150=CARTESIAN_POINT('Ctrl Pts',(71.1339043418529,-21.7632265878119,12.));
#56151=CARTESIAN_POINT('Ctrl Pts',(71.0762040404458,-21.6628164325802,12.));
#56152=CARTESIAN_POINT('Ctrl Pts',(70.9934796069117,-21.5904919935063,12.));
#56153=CARTESIAN_POINT('Ctrl Pts',(70.9934796069117,-21.5904919935063,12.));
#56154=CARTESIAN_POINT('Ctrl Pts',(70.9934796069117,-21.5904919935063,8.));
#56155=CARTESIAN_POINT('Ctrl Pts',(70.9934796069117,-21.5904919935063,4.));
#56156=CARTESIAN_POINT('Ctrl Pts',(70.9934796069117,-21.5904919935063,-5.55111512312578E-16));
#56157=CARTESIAN_POINT('Origin',(3.57524700084383E-10,-1.12623029467293E-10,
0.));
#56158=CARTESIAN_POINT('Origin',(3.57524700084383E-10,-1.12623029467293E-10,
12.));
#56159=CARTESIAN_POINT('Origin',(3.57524700084383E-10,-1.12623029467293E-10,
0.));
#56160=CARTESIAN_POINT('Ctrl Pts',(68.7132793373328,-28.7877620302391,0.));
#56161=CARTESIAN_POINT('Ctrl Pts',(68.7132793373328,-28.7877620302391,4.));
#56162=CARTESIAN_POINT('Ctrl Pts',(68.7132793373328,-28.7877620302391,8.));
#56163=CARTESIAN_POINT('Ctrl Pts',(68.7132793373328,-28.7877620302391,12.));
#56164=CARTESIAN_POINT('Ctrl Pts',(68.6708193334379,-28.8891094745186,0.));
#56165=CARTESIAN_POINT('Ctrl Pts',(68.6708193334379,-28.8891094745186,4.));
#56166=CARTESIAN_POINT('Ctrl Pts',(68.6708193334379,-28.8891094745186,8.));
#56167=CARTESIAN_POINT('Ctrl Pts',(68.6708193334379,-28.8891094745186,12.));
#56168=CARTESIAN_POINT('Ctrl Pts',(68.5360395709811,-29.0404604348957,0.));
#56169=CARTESIAN_POINT('Ctrl Pts',(68.5360395709811,-29.0404604348957,4.));
#56170=CARTESIAN_POINT('Ctrl Pts',(68.5360395709811,-29.0404604348957,7.99999999999999));
#56171=CARTESIAN_POINT('Ctrl Pts',(68.5360395709811,-29.0404604348957,12.));
#56172=CARTESIAN_POINT('Ctrl Pts',(68.3446561754307,-29.0927805237118,0.));
#56173=CARTESIAN_POINT('Ctrl Pts',(68.3446561754307,-29.0927805237118,4.));
#56174=CARTESIAN_POINT('Ctrl Pts',(68.3446561754307,-29.0927805237118,8.00000000000001));
#56175=CARTESIAN_POINT('Ctrl Pts',(68.3446561754307,-29.0927805237118,12.));
#56176=CARTESIAN_POINT('Ctrl Pts',(68.2622612909744,-29.0944526440248,0.));
#56177=CARTESIAN_POINT('Ctrl Pts',(68.2622612909744,-29.0944526440248,4.));
#56178=CARTESIAN_POINT('Ctrl Pts',(68.2622612909744,-29.0944526440248,8.));
#56179=CARTESIAN_POINT('Ctrl Pts',(68.2622612909744,-29.0944526440248,12.));
#56180=CARTESIAN_POINT('',(68.7132793373328,-28.7877620302391,0.));
#56181=CARTESIAN_POINT('',(68.2622612909744,-29.0944526440249,0.));
#56182=CARTESIAN_POINT('Ctrl Pts',(68.7132793373328,-28.7877620302391,0.));
#56183=CARTESIAN_POINT('Ctrl Pts',(68.6708193334379,-28.8891094745186,0.));
#56184=CARTESIAN_POINT('Ctrl Pts',(68.5938023263198,-28.9755957375912,0.));
#56185=CARTESIAN_POINT('Ctrl Pts',(68.4983025002323,-29.0297453895419,0.));
#56186=CARTESIAN_POINT('Ctrl Pts',(68.4266776306666,-29.0703576285049,0.));
#56187=CARTESIAN_POINT('Ctrl Pts',(68.3446561754307,-29.0927805237118,0.));
#56188=CARTESIAN_POINT('Ctrl Pts',(68.2622612909744,-29.0944526440248,0.));
#56189=CARTESIAN_POINT('',(68.2622612909744,-29.0944526440249,12.));
#56190=CARTESIAN_POINT('Ctrl Pts',(68.2622612909744,-29.0944526440248,0.));
#56191=CARTESIAN_POINT('Ctrl Pts',(68.2622612909744,-29.0944526440248,4.));
#56192=CARTESIAN_POINT('Ctrl Pts',(68.2622612909744,-29.0944526440248,8.));
#56193=CARTESIAN_POINT('Ctrl Pts',(68.2622612909744,-29.0944526440248,12.));
#56194=CARTESIAN_POINT('',(68.7132793373328,-28.7877620302391,12.));
#56195=CARTESIAN_POINT('Ctrl Pts',(68.2622612909744,-29.0944526440248,12.));
#56196=CARTESIAN_POINT('Ctrl Pts',(68.3446561754307,-29.0927805237118,12.));
#56197=CARTESIAN_POINT('Ctrl Pts',(68.4266776306666,-29.0703576285049,12.));
#56198=CARTESIAN_POINT('Ctrl Pts',(68.4983025002323,-29.0297453895419,12.));
#56199=CARTESIAN_POINT('Ctrl Pts',(68.5938023263198,-28.9755957375912,12.));
#56200=CARTESIAN_POINT('Ctrl Pts',(68.6708193334379,-28.8891094745186,12.));
#56201=CARTESIAN_POINT('Ctrl Pts',(68.7132793373328,-28.7877620302391,12.));
#56202=CARTESIAN_POINT('Ctrl Pts',(68.7132793373328,-28.7877620302391,12.));
#56203=CARTESIAN_POINT('Ctrl Pts',(68.7132793373328,-28.7877620302391,8.));
#56204=CARTESIAN_POINT('Ctrl Pts',(68.7132793373328,-28.7877620302391,4.));
#56205=CARTESIAN_POINT('Ctrl Pts',(68.7132793373328,-28.7877620302391,0.));
#56206=CARTESIAN_POINT('Ctrl Pts',(63.7976679095314,-28.8072485549237,0.));
#56207=CARTESIAN_POINT('Ctrl Pts',(63.7976679095314,-28.8072485549237,12.));
#56208=CARTESIAN_POINT('Ctrl Pts',(63.8014989507494,-28.8078854475432,0.));
#56209=CARTESIAN_POINT('Ctrl Pts',(63.8014989507494,-28.8078854475432,12.));
#56210=CARTESIAN_POINT('Ctrl Pts',(63.8091667271231,-28.8091580239553,0.));
#56211=CARTESIAN_POINT('Ctrl Pts',(63.8091667271231,-28.8091580239553,12.));
#56212=CARTESIAN_POINT('Ctrl Pts',(63.8206854735027,-28.8110632620958,0.));
#56213=CARTESIAN_POINT('Ctrl Pts',(63.8206854735027,-28.8110632620958,12.));
#56214=CARTESIAN_POINT('Ctrl Pts',(63.8360779669856,-28.8135963263369,0.));
#56215=CARTESIAN_POINT('Ctrl Pts',(63.8360779669856,-28.8135963263369,12.));
#56216=CARTESIAN_POINT('Ctrl Pts',(63.8553755207486,-28.8167505576681,0.));
#56217=CARTESIAN_POINT('Ctrl Pts',(63.8553755207486,-28.8167505576681,12.));
#56218=CARTESIAN_POINT('Ctrl Pts',(63.8747299825313,-28.8198926619858,0.));
#56219=CARTESIAN_POINT('Ctrl Pts',(63.8747299825313,-28.8198926619858,12.));
#56220=CARTESIAN_POINT('Ctrl Pts',(63.8941412856923,-28.823022586318,0.));
#56221=CARTESIAN_POINT('Ctrl Pts',(63.8941412856923,-28.823022586318,12.));
#56222=CARTESIAN_POINT('Ctrl Pts',(63.9136093063786,-28.8261402423291,0.));
#56223=CARTESIAN_POINT('Ctrl Pts',(63.9136093063786,-28.8261402423291,12.));
#56224=CARTESIAN_POINT('Ctrl Pts',(63.9331338646996,-28.829245507756,0.));
#56225=CARTESIAN_POINT('Ctrl Pts',(63.9331338646996,-28.829245507756,12.));
#56226=CARTESIAN_POINT('Ctrl Pts',(63.9527147494423,-28.8323382413789,0.));
#56227=CARTESIAN_POINT('Ctrl Pts',(63.9527147494423,-28.8323382413789,12.));
#56228=CARTESIAN_POINT('Ctrl Pts',(63.9723517369614,-28.8354182946601,0.));
#56229=CARTESIAN_POINT('Ctrl Pts',(63.9723517369614,-28.8354182946601,12.));
#56230=CARTESIAN_POINT('Ctrl Pts',(63.9920446117582,-28.8384855243243,0.));
#56231=CARTESIAN_POINT('Ctrl Pts',(63.9920446117582,-28.8384855243243,12.));
#56232=CARTESIAN_POINT('Ctrl Pts',(64.0117931881298,-28.8415398056428,0.));
#56233=CARTESIAN_POINT('Ctrl Pts',(64.0117931881298,-28.8415398056428,12.));
#56234=CARTESIAN_POINT('Ctrl Pts',(64.0315973031942,-28.844581028125,0.));
#56235=CARTESIAN_POINT('Ctrl Pts',(64.0315973031942,-28.844581028125,12.));
#56236=CARTESIAN_POINT('Ctrl Pts',(64.0514568066637,-28.8476090892232,0.));
#56237=CARTESIAN_POINT('Ctrl Pts',(64.0514568066637,-28.8476090892232,12.));
#56238=CARTESIAN_POINT('Ctrl Pts',(64.0713715523599,-28.8506238891093,0.));
#56239=CARTESIAN_POINT('Ctrl Pts',(64.0713715523599,-28.8506238891093,12.));
#56240=CARTESIAN_POINT('Ctrl Pts',(64.0913413876622,-28.8536253241854,0.));
#56241=CARTESIAN_POINT('Ctrl Pts',(64.0913413876622,-28.8536253241854,12.));
#56242=CARTESIAN_POINT('Ctrl Pts',(64.1113661481965,-28.8566132838179,0.));
#56243=CARTESIAN_POINT('Ctrl Pts',(64.1113661481965,-28.8566132838179,12.));
#56244=CARTESIAN_POINT('Ctrl Pts',(64.1314456633381,-28.8595876537148,0.));
#56245=CARTESIAN_POINT('Ctrl Pts',(64.1314456633381,-28.8595876537148,12.));
#56246=CARTESIAN_POINT('Ctrl Pts',(64.1515797596564,-28.8625483180438,0.));
#56247=CARTESIAN_POINT('Ctrl Pts',(64.1515797596564,-28.8625483180438,12.));
#56248=CARTESIAN_POINT('Ctrl Pts',(64.1717682648685,-28.8654951618649,0.));
#56249=CARTESIAN_POINT('Ctrl Pts',(64.1717682648685,-28.8654951618649,12.));
#56250=CARTESIAN_POINT('Ctrl Pts',(64.1920110123299,-28.8684280739014,0.));
#56251=CARTESIAN_POINT('Ctrl Pts',(64.1920110123299,-28.8684280739014,12.));
#56252=CARTESIAN_POINT('Ctrl Pts',(64.2123078408461,-28.8713469464185,0.));
#56253=CARTESIAN_POINT('Ctrl Pts',(64.2123078408461,-28.8713469464185,12.));
#56254=CARTESIAN_POINT('Ctrl Pts',(64.2326585925252,-28.8742516738947,0.));
#56255=CARTESIAN_POINT('Ctrl Pts',(64.2326585925252,-28.8742516738947,12.));
#56256=CARTESIAN_POINT('Ctrl Pts',(64.2530631112929,-28.877142152106,0.));
#56257=CARTESIAN_POINT('Ctrl Pts',(64.2530631112929,-28.877142152106,12.));
#56258=CARTESIAN_POINT('Ctrl Pts',(64.273521241071,-28.8800182770065,0.));
#56259=CARTESIAN_POINT('Ctrl Pts',(64.273521241071,-28.8800182770065,12.));
#56260=CARTESIAN_POINT('Ctrl Pts',(64.2940328242521,-28.882879943794,0.));
#56261=CARTESIAN_POINT('Ctrl Pts',(64.2940328242521,-28.882879943794,12.));
#56262=CARTESIAN_POINT('Ctrl Pts',(64.3145977025037,-28.8857270473959,0.));
#56263=CARTESIAN_POINT('Ctrl Pts',(64.3145977025037,-28.8857270473959,12.));
#56264=CARTESIAN_POINT('Ctrl Pts',(64.3352157174619,-28.8885594828926,0.));
#56265=CARTESIAN_POINT('Ctrl Pts',(64.3352157174619,-28.8885594828926,12.));
#56266=CARTESIAN_POINT('Ctrl Pts',(64.3558867114076,-28.8913771459323,0.));
#56267=CARTESIAN_POINT('Ctrl Pts',(64.3558867114076,-28.8913771459323,12.));
#56268=CARTESIAN_POINT('Ctrl Pts',(64.3766105280688,-28.89417993323,0.));
#56269=CARTESIAN_POINT('Ctrl Pts',(64.3766105280688,-28.89417993323,12.));
#56270=CARTESIAN_POINT('Ctrl Pts',(64.3973870129169,-28.8969677427504,0.));
#56271=CARTESIAN_POINT('Ctrl Pts',(64.3973870129169,-28.8969677427504,12.));
#56272=CARTESIAN_POINT('Ctrl Pts',(64.4182160127379,-28.899740473434,0.));
#56273=CARTESIAN_POINT('Ctrl Pts',(64.4182160127379,-28.899740473434,12.));
#56274=CARTESIAN_POINT('Ctrl Pts',(64.4390973753634,-28.9024980250307,0.));
#56275=CARTESIAN_POINT('Ctrl Pts',(64.4390973753634,-28.9024980250307,12.));
#56276=CARTESIAN_POINT('Ctrl Pts',(64.4600309493583,-28.9052402979062,0.));
#56277=CARTESIAN_POINT('Ctrl Pts',(64.4600309493583,-28.9052402979062,12.));
#56278=CARTESIAN_POINT('Ctrl Pts',(64.4810165836592,-28.9079671928264,0.));
#56279=CARTESIAN_POINT('Ctrl Pts',(64.4810165836592,-28.9079671928264,12.));
#56280=CARTESIAN_POINT('Ctrl Pts',(64.5020541275951,-28.910678610965,0.));
#56281=CARTESIAN_POINT('Ctrl Pts',(64.5020541275951,-28.910678610965,12.));
#56282=CARTESIAN_POINT('Ctrl Pts',(64.523143431047,-28.9133744539949,0.));
#56283=CARTESIAN_POINT('Ctrl Pts',(64.523143431047,-28.9133744539949,12.));
#56284=CARTESIAN_POINT('Ctrl Pts',(64.5442843445559,-28.9160546241538,0.));
#56285=CARTESIAN_POINT('Ctrl Pts',(64.5442843445559,-28.9160546241538,12.));
#56286=CARTESIAN_POINT('Ctrl Pts',(64.5654767194471,-28.9187190243224,0.));
#56287=CARTESIAN_POINT('Ctrl Pts',(64.5654767194471,-28.9187190243224,12.));
#56288=CARTESIAN_POINT('Ctrl Pts',(64.5867204079426,-28.9213675580985,0.));
#56289=CARTESIAN_POINT('Ctrl Pts',(64.5867204079426,-28.9213675580985,12.));
#56290=CARTESIAN_POINT('Ctrl Pts',(64.6080152631039,-28.9240001297542,0.));
#56291=CARTESIAN_POINT('Ctrl Pts',(64.6080152631039,-28.9240001297542,12.));
#56292=CARTESIAN_POINT('Ctrl Pts',(64.629361138774,-28.9266166441951,0.));
#56293=CARTESIAN_POINT('Ctrl Pts',(64.629361138774,-28.9266166441951,12.));
#56294=CARTESIAN_POINT('Ctrl Pts',(64.6507578895161,-28.9292170069222,0.));
#56295=CARTESIAN_POINT('Ctrl Pts',(64.6507578895161,-28.9292170069222,12.));
#56296=CARTESIAN_POINT('Ctrl Pts',(64.672205370541,-28.9318011239915,0.));
#56297=CARTESIAN_POINT('Ctrl Pts',(64.672205370541,-28.9318011239915,12.));
#56298=CARTESIAN_POINT('Ctrl Pts',(64.6937034376617,-28.9343689019882,0.));
#56299=CARTESIAN_POINT('Ctrl Pts',(64.6937034376617,-28.9343689019882,12.));
#56300=CARTESIAN_POINT('Ctrl Pts',(64.715251947329,-28.9369202480393,0.));
#56301=CARTESIAN_POINT('Ctrl Pts',(64.715251947329,-28.9369202480393,12.));
#56302=CARTESIAN_POINT('Ctrl Pts',(64.7368507566467,-28.9394550698204,0.));
#56303=CARTESIAN_POINT('Ctrl Pts',(64.7368507566467,-28.9394550698204,12.));
#56304=CARTESIAN_POINT('Ctrl Pts',(64.758499723388,-28.9419732755656,0.));
#56305=CARTESIAN_POINT('Ctrl Pts',(64.758499723388,-28.9419732755656,12.));
#56306=CARTESIAN_POINT('Ctrl Pts',(64.7801987060084,-28.944474774081,0.));
#56307=CARTESIAN_POINT('Ctrl Pts',(64.7801987060084,-28.944474774081,12.));
#56308=CARTESIAN_POINT('Ctrl Pts',(64.8019475636442,-28.9469594747432,0.));
#56309=CARTESIAN_POINT('Ctrl Pts',(64.8019475636442,-28.9469594747432,12.));
#56310=CARTESIAN_POINT('Ctrl Pts',(64.8237461561018,-28.9494272874832,0.));
#56311=CARTESIAN_POINT('Ctrl Pts',(64.8237461561018,-28.9494272874832,12.));
#56312=CARTESIAN_POINT('Ctrl Pts',(64.8455943438423,-28.9518781227765,0.));
#56313=CARTESIAN_POINT('Ctrl Pts',(64.8455943438423,-28.9518781227765,12.));
#56314=CARTESIAN_POINT('Ctrl Pts',(64.8674919879648,-28.9543118916328,0.));
#56315=CARTESIAN_POINT('Ctrl Pts',(64.8674919879648,-28.9543118916328,12.));
#56316=CARTESIAN_POINT('Ctrl Pts',(64.8894389501801,-28.9567285055867,0.));
#56317=CARTESIAN_POINT('Ctrl Pts',(64.8894389501801,-28.9567285055867,12.));
#56318=CARTESIAN_POINT('Ctrl Pts',(64.9114350928125,-28.9591278766934,0.));
#56319=CARTESIAN_POINT('Ctrl Pts',(64.9114350928125,-28.9591278766934,12.));
#56320=CARTESIAN_POINT('Ctrl Pts',(64.9334802788038,-28.961509917525,0.));
#56321=CARTESIAN_POINT('Ctrl Pts',(64.9334802788038,-28.961509917525,12.));
#56322=CARTESIAN_POINT('Ctrl Pts',(64.9555743717109,-28.9638745411677,0.));
#56323=CARTESIAN_POINT('Ctrl Pts',(64.9555743717109,-28.9638745411677,12.));
#56324=CARTESIAN_POINT('Ctrl Pts',(64.9777172357027,-28.9662216612217,0.));
#56325=CARTESIAN_POINT('Ctrl Pts',(64.9777172357027,-28.9662216612217,12.));
#56326=CARTESIAN_POINT('Ctrl Pts',(64.9999087355504,-28.9685511918019,0.));
#56327=CARTESIAN_POINT('Ctrl Pts',(64.9999087355504,-28.9685511918019,12.));
#56328=CARTESIAN_POINT('Ctrl Pts',(65.022148736628,-28.97086304753,0.));
#56329=CARTESIAN_POINT('Ctrl Pts',(65.022148736628,-28.97086304753,12.));
#56330=CARTESIAN_POINT('Ctrl Pts',(65.0444371049082,-28.9731571435283,0.));
#56331=CARTESIAN_POINT('Ctrl Pts',(65.0444371049082,-28.9731571435283,12.));
#56332=CARTESIAN_POINT('Ctrl Pts',(65.0667737069563,-28.9754333954135,0.));
#56333=CARTESIAN_POINT('Ctrl Pts',(65.0667737069563,-28.9754333954135,12.));
#56334=CARTESIAN_POINT('Ctrl Pts',(65.0891584099168,-28.9776917192933,0.));
#56335=CARTESIAN_POINT('Ctrl Pts',(65.0891584099168,-28.9776917192933,12.));
#56336=CARTESIAN_POINT('Ctrl Pts',(65.1115910815037,-28.9799320317641,0.));
#56337=CARTESIAN_POINT('Ctrl Pts',(65.1115910815037,-28.9799320317641,12.));
#56338=CARTESIAN_POINT('Ctrl Pts',(65.1340715900028,-28.9821542499043,0.));
#56339=CARTESIAN_POINT('Ctrl Pts',(65.1340715900028,-28.9821542499043,12.));
#56340=CARTESIAN_POINT('Ctrl Pts',(65.1565998042697,-28.9843582912693,0.));
#56341=CARTESIAN_POINT('Ctrl Pts',(65.1565998042697,-28.9843582912693,12.));
#56342=CARTESIAN_POINT('Ctrl Pts',(65.1791755937256,-28.9865440738884,0.));
#56343=CARTESIAN_POINT('Ctrl Pts',(65.1791755937256,-28.9865440738884,12.));
#56344=CARTESIAN_POINT('Ctrl Pts',(65.2017988283479,-28.9887115162634,0.));
#56345=CARTESIAN_POINT('Ctrl Pts',(65.2017988283479,-28.9887115162634,12.));
#56346=CARTESIAN_POINT('Ctrl Pts',(65.2244693786609,-28.9908605373663,0.));
#56347=CARTESIAN_POINT('Ctrl Pts',(65.2244693786609,-28.9908605373663,12.));
#56348=CARTESIAN_POINT('Ctrl Pts',(65.2471871157397,-28.9929910566325,0.));
#56349=CARTESIAN_POINT('Ctrl Pts',(65.2471871157397,-28.9929910566325,12.));
#56350=CARTESIAN_POINT('Ctrl Pts',(65.2699519112064,-28.9951029939557,0.));
#56351=CARTESIAN_POINT('Ctrl Pts',(65.2699519112064,-28.9951029939557,12.));
#56352=CARTESIAN_POINT('Ctrl Pts',(65.2927636372253,-28.9971962696845,0.));
#56353=CARTESIAN_POINT('Ctrl Pts',(65.2927636372253,-28.9971962696845,12.));
#56354=CARTESIAN_POINT('Ctrl Pts',(65.3156221664916,-28.9992708046212,0.));
#56355=CARTESIAN_POINT('Ctrl Pts',(65.3156221664916,-28.9992708046212,12.));
#56356=CARTESIAN_POINT('Ctrl Pts',(65.3385273722241,-29.0013265200185,0.));
#56357=CARTESIAN_POINT('Ctrl Pts',(65.3385273722241,-29.0013265200185,12.));
#56358=CARTESIAN_POINT('Ctrl Pts',(65.3614791281692,-29.003363337573,0.));
#56359=CARTESIAN_POINT('Ctrl Pts',(65.3614791281692,-29.003363337573,12.));
#56360=CARTESIAN_POINT('Ctrl Pts',(65.3844773085961,-29.0053811794207,0.));
#56361=CARTESIAN_POINT('Ctrl Pts',(65.3844773085961,-29.0053811794207,12.));
#56362=CARTESIAN_POINT('Ctrl Pts',(65.4075217882934,-29.0073799681342,0.));
#56363=CARTESIAN_POINT('Ctrl Pts',(65.4075217882934,-29.0073799681342,12.));
#56364=CARTESIAN_POINT('Ctrl Pts',(65.4306124425562,-29.0093596267216,0.));
#56365=CARTESIAN_POINT('Ctrl Pts',(65.4306124425562,-29.0093596267216,12.));
#56366=CARTESIAN_POINT('Ctrl Pts',(65.4537491471828,-29.0113200786239,0.));
#56367=CARTESIAN_POINT('Ctrl Pts',(65.4537491471828,-29.0113200786239,12.));
#56368=CARTESIAN_POINT('Ctrl Pts',(65.4769317784789,-29.013261247709,0.));
#56369=CARTESIAN_POINT('Ctrl Pts',(65.4769317784789,-29.013261247709,12.));
#56370=CARTESIAN_POINT('Ctrl Pts',(65.5001602132535,-29.0151830582675,0.));
#56371=CARTESIAN_POINT('Ctrl Pts',(65.5001602132535,-29.0151830582675,12.));
#56372=CARTESIAN_POINT('Ctrl Pts',(65.5234343288136,-29.0170854350095,0.));
#56373=CARTESIAN_POINT('Ctrl Pts',(65.5234343288136,-29.0170854350095,12.));
#56374=CARTESIAN_POINT('Ctrl Pts',(65.5467540029514,-29.0189683030642,0.));
#56375=CARTESIAN_POINT('Ctrl Pts',(65.5467540029514,-29.0189683030642,12.));
#56376=CARTESIAN_POINT('Ctrl Pts',(65.5701191139418,-29.0208315879764,0.));
#56377=CARTESIAN_POINT('Ctrl Pts',(65.5701191139418,-29.0208315879764,12.));
#56378=CARTESIAN_POINT('Ctrl Pts',(65.5935295405453,-29.0226752157003,0.));
#56379=CARTESIAN_POINT('Ctrl Pts',(65.5935295405453,-29.0226752157003,12.));
#56380=CARTESIAN_POINT('Ctrl Pts',(65.6169851620046,-29.0244991125959,0.));
#56381=CARTESIAN_POINT('Ctrl Pts',(65.6169851620046,-29.0244991125959,12.));
#56382=CARTESIAN_POINT('Ctrl Pts',(65.6404858580403,-29.0263032054267,0.));
#56383=CARTESIAN_POINT('Ctrl Pts',(65.6404858580403,-29.0263032054267,12.));
#56384=CARTESIAN_POINT('Ctrl Pts',(65.6640315088388,-29.0280874213596,0.));
#56385=CARTESIAN_POINT('Ctrl Pts',(65.6640315088388,-29.0280874213596,12.));
#56386=CARTESIAN_POINT('Ctrl Pts',(65.6876219950493,-29.0298516879612,0.));
#56387=CARTESIAN_POINT('Ctrl Pts',(65.6876219950493,-29.0298516879612,12.));
#56388=CARTESIAN_POINT('Ctrl Pts',(65.7112571977891,-29.0315959331919,0.));
#56389=CARTESIAN_POINT('Ctrl Pts',(65.7112571977891,-29.0315959331919,12.));
#56390=CARTESIAN_POINT('Ctrl Pts',(65.7349369986384,-29.0333200854028,0.));
#56391=CARTESIAN_POINT('Ctrl Pts',(65.7349369986384,-29.0333200854028,12.));
#56392=CARTESIAN_POINT('Ctrl Pts',(65.7586612796368,-29.035024073333,0.));
#56393=CARTESIAN_POINT('Ctrl Pts',(65.7586612796368,-29.035024073333,12.));
#56394=CARTESIAN_POINT('Ctrl Pts',(65.7824299232705,-29.0367078261103,0.));
#56395=CARTESIAN_POINT('Ctrl Pts',(65.7824299232705,-29.0367078261103,12.));
#56396=CARTESIAN_POINT('Ctrl Pts',(65.8062428124713,-29.0383712732469,0.));
#56397=CARTESIAN_POINT('Ctrl Pts',(65.8062428124713,-29.0383712732469,12.));
#56398=CARTESIAN_POINT('Ctrl Pts',(65.8300998306191,-29.0400143446338,0.));
#56399=CARTESIAN_POINT('Ctrl Pts',(65.8300998306191,-29.0400143446338,12.));
#56400=CARTESIAN_POINT('Ctrl Pts',(65.854000861539,-29.0416369705376,0.));
#56401=CARTESIAN_POINT('Ctrl Pts',(65.854000861539,-29.0416369705376,12.));
#56402=CARTESIAN_POINT('Ctrl Pts',(65.8779457894961,-29.0432390815978,0.));
#56403=CARTESIAN_POINT('Ctrl Pts',(65.8779457894961,-29.0432390815978,12.));
#56404=CARTESIAN_POINT('Ctrl Pts',(65.9019344991854,-29.0448206088289,0.));
#56405=CARTESIAN_POINT('Ctrl Pts',(65.9019344991854,-29.0448206088289,12.));
#56406=CARTESIAN_POINT('Ctrl Pts',(65.9259668757306,-29.0463814836158,0.));
#56407=CARTESIAN_POINT('Ctrl Pts',(65.9259668757306,-29.0463814836158,12.));
#56408=CARTESIAN_POINT('Ctrl Pts',(65.9500428046868,-29.0479216377081,0.));
#56409=CARTESIAN_POINT('Ctrl Pts',(65.9500428046868,-29.0479216377081,12.));
#56410=CARTESIAN_POINT('Ctrl Pts',(65.9741621720369,-29.0494410032173,0.));
#56411=CARTESIAN_POINT('Ctrl Pts',(65.9741621720369,-29.0494410032173,12.));
#56412=CARTESIAN_POINT('Ctrl Pts',(65.9983248641879,-29.0509395126143,0.));
#56413=CARTESIAN_POINT('Ctrl Pts',(65.9983248641879,-29.0509395126143,12.));
#56414=CARTESIAN_POINT('Ctrl Pts',(66.0225307679591,-29.0524170987307,0.));
#56415=CARTESIAN_POINT('Ctrl Pts',(66.0225307679591,-29.0524170987307,12.));
#56416=CARTESIAN_POINT('Ctrl Pts',(66.0467797705815,-29.0538736947552,0.));
#56417=CARTESIAN_POINT('Ctrl Pts',(66.0467797705815,-29.0538736947552,12.));
#56418=CARTESIAN_POINT('Ctrl Pts',(66.0710717597009,-29.0553092342279,0.));
#56419=CARTESIAN_POINT('Ctrl Pts',(66.0710717597009,-29.0553092342279,12.));
#56420=CARTESIAN_POINT('Ctrl Pts',(66.0954066233754,-29.0567236510374,0.));
#56421=CARTESIAN_POINT('Ctrl Pts',(66.0954066233754,-29.0567236510374,12.));
#56422=CARTESIAN_POINT('Ctrl Pts',(66.1197842500711,-29.058116879419,0.));
#56423=CARTESIAN_POINT('Ctrl Pts',(66.1197842500711,-29.058116879419,12.));
#56424=CARTESIAN_POINT('Ctrl Pts',(66.1442045286516,-29.0594888539556,0.));
#56425=CARTESIAN_POINT('Ctrl Pts',(66.1442045286516,-29.0594888539556,12.));
#56426=CARTESIAN_POINT('Ctrl Pts',(66.1686673483755,-29.0608395095746,0.));
#56427=CARTESIAN_POINT('Ctrl Pts',(66.1686673483755,-29.0608395095746,12.));
#56428=CARTESIAN_POINT('Ctrl Pts',(66.1931725989008,-29.062168781542,0.));
#56429=CARTESIAN_POINT('Ctrl Pts',(66.1931725989008,-29.062168781542,12.));
#56430=CARTESIAN_POINT('Ctrl Pts',(66.2177201702819,-29.0634766054599,0.));
#56431=CARTESIAN_POINT('Ctrl Pts',(66.2177201702819,-29.0634766054599,12.));
#56432=CARTESIAN_POINT('Ctrl Pts',(66.2423099529668,-29.0647629172645,0.));
#56433=CARTESIAN_POINT('Ctrl Pts',(66.2423099529668,-29.0647629172645,12.));
#56434=CARTESIAN_POINT('Ctrl Pts',(66.2669418377865,-29.0660276532272,0.));
#56435=CARTESIAN_POINT('Ctrl Pts',(66.2669418377865,-29.0660276532272,12.));
#56436=CARTESIAN_POINT('Ctrl Pts',(66.2916157159527,-29.0672707499527,0.));
#56437=CARTESIAN_POINT('Ctrl Pts',(66.2916157159527,-29.0672707499527,12.));
#56438=CARTESIAN_POINT('Ctrl Pts',(66.3163314790607,-29.0684921443718,0.));
#56439=CARTESIAN_POINT('Ctrl Pts',(66.3163314790607,-29.0684921443718,12.));
#56440=CARTESIAN_POINT('Ctrl Pts',(66.3410890190879,-29.0696917737398,0.));
#56441=CARTESIAN_POINT('Ctrl Pts',(66.3410890190879,-29.0696917737398,12.));
#56442=CARTESIAN_POINT('Ctrl Pts',(66.3658882283906,-29.0708695756336,0.));
#56443=CARTESIAN_POINT('Ctrl Pts',(66.3658882283906,-29.0708695756336,12.));
#56444=CARTESIAN_POINT('Ctrl Pts',(66.3907289996942,-29.0720254879535,0.));
#56445=CARTESIAN_POINT('Ctrl Pts',(66.3907289996942,-29.0720254879535,12.));
#56446=CARTESIAN_POINT('Ctrl Pts',(66.4156112260904,-29.0731594489219,0.));
#56447=CARTESIAN_POINT('Ctrl Pts',(66.4156112260904,-29.0731594489219,12.));
#56448=CARTESIAN_POINT('Ctrl Pts',(66.4405348010404,-29.0742713970763,0.));
#56449=CARTESIAN_POINT('Ctrl Pts',(66.4405348010404,-29.0742713970763,12.));
#56450=CARTESIAN_POINT('Ctrl Pts',(66.4654996183739,-29.075361271267,0.));
#56451=CARTESIAN_POINT('Ctrl Pts',(66.4654996183739,-29.075361271267,12.));
#56452=CARTESIAN_POINT('Ctrl Pts',(66.4905055722864,-29.0764290106553,0.));
#56453=CARTESIAN_POINT('Ctrl Pts',(66.4905055722864,-29.0764290106553,12.));
#56454=CARTESIAN_POINT('Ctrl Pts',(66.5155525573308,-29.0774745547146,0.));
#56455=CARTESIAN_POINT('Ctrl Pts',(66.5155525573308,-29.0774745547146,12.));
#56456=CARTESIAN_POINT('Ctrl Pts',(66.5406404684116,-29.0784978432294,0.));
#56457=CARTESIAN_POINT('Ctrl Pts',(66.5406404684116,-29.0784978432294,12.));
#56458=CARTESIAN_POINT('Ctrl Pts',(66.5657692007894,-29.0794988162892,0.));
#56459=CARTESIAN_POINT('Ctrl Pts',(66.5657692007894,-29.0794988162892,12.));
#56460=CARTESIAN_POINT('Ctrl Pts',(66.5909386500796,-29.0804774142852,0.));
#56461=CARTESIAN_POINT('Ctrl Pts',(66.5909386500796,-29.0804774142852,12.));
#56462=CARTESIAN_POINT('Ctrl Pts',(66.6161487122504,-29.0814335779086,0.));
#56463=CARTESIAN_POINT('Ctrl Pts',(66.6161487122504,-29.0814335779086,12.));
#56464=CARTESIAN_POINT('Ctrl Pts',(66.6413992836148,-29.0823672481508,0.));
#56465=CARTESIAN_POINT('Ctrl Pts',(66.6413992836148,-29.0823672481508,12.));
#56466=CARTESIAN_POINT('Ctrl Pts',(66.6666902608246,-29.0832783663049,0.));
#56467=CARTESIAN_POINT('Ctrl Pts',(66.6666902608246,-29.0832783663049,12.));
#56468=CARTESIAN_POINT('Ctrl Pts',(66.6920215408744,-29.0841668739585,0.));
#56469=CARTESIAN_POINT('Ctrl Pts',(66.6920215408744,-29.0841668739585,12.));
#56470=CARTESIAN_POINT('Ctrl Pts',(66.7173930211015,-29.0850327129914,0.));
#56471=CARTESIAN_POINT('Ctrl Pts',(66.7173930211015,-29.0850327129914,12.));
#56472=CARTESIAN_POINT('Ctrl Pts',(66.742804599184,-29.0858758255729,0.));
#56473=CARTESIAN_POINT('Ctrl Pts',(66.742804599184,-29.0858758255729,12.));
#56474=CARTESIAN_POINT('Ctrl Pts',(66.7682561731348,-29.086696154163,0.));
#56475=CARTESIAN_POINT('Ctrl Pts',(66.7682561731348,-29.086696154163,12.));
#56476=CARTESIAN_POINT('Ctrl Pts',(66.7937476412941,-29.0874936415138,0.));
#56477=CARTESIAN_POINT('Ctrl Pts',(66.7937476412941,-29.0874936415138,12.));
#56478=CARTESIAN_POINT('Ctrl Pts',(66.8192789023323,-29.0882682306636,0.));
#56479=CARTESIAN_POINT('Ctrl Pts',(66.8192789023323,-29.0882682306636,12.));
#56480=CARTESIAN_POINT('Ctrl Pts',(66.8448498552508,-29.0890198649327,0.));
#56481=CARTESIAN_POINT('Ctrl Pts',(66.8448498552508,-29.0890198649327,12.));
#56482=CARTESIAN_POINT('Ctrl Pts',(66.8704603993794,-29.0897484879208,0.));
#56483=CARTESIAN_POINT('Ctrl Pts',(66.8704603993794,-29.0897484879208,12.));
#56484=CARTESIAN_POINT('Ctrl Pts',(66.8961104343703,-29.0904540435064,0.));
#56485=CARTESIAN_POINT('Ctrl Pts',(66.8961104343703,-29.0904540435064,12.));
#56486=CARTESIAN_POINT('Ctrl Pts',(66.9217998601881,-29.0911364758484,0.));
#56487=CARTESIAN_POINT('Ctrl Pts',(66.9217998601881,-29.0911364758484,12.));
#56488=CARTESIAN_POINT('Ctrl Pts',(66.9475285771133,-29.0917957293825,0.));
#56489=CARTESIAN_POINT('Ctrl Pts',(66.9475285771133,-29.0917957293825,12.));
#56490=CARTESIAN_POINT('Ctrl Pts',(66.9732964857467,-29.092431748817,0.));
#56491=CARTESIAN_POINT('Ctrl Pts',(66.9732964857467,-29.092431748817,12.));
#56492=CARTESIAN_POINT('Ctrl Pts',(66.9991034870084,-29.0930444791329,0.));
#56493=CARTESIAN_POINT('Ctrl Pts',(66.9991034870084,-29.0930444791329,12.));
#56494=CARTESIAN_POINT('Ctrl Pts',(67.0249494821361,-29.0936338655828,0.));
#56495=CARTESIAN_POINT('Ctrl Pts',(67.0249494821361,-29.0936338655828,12.));
#56496=CARTESIAN_POINT('Ctrl Pts',(67.0508343726771,-29.0941998536958,0.));
#56497=CARTESIAN_POINT('Ctrl Pts',(67.0508343726771,-29.0941998536958,12.));
#56498=CARTESIAN_POINT('Ctrl Pts',(67.0767580604872,-29.0947423892725,0.));
#56499=CARTESIAN_POINT('Ctrl Pts',(67.0767580604872,-29.0947423892725,12.));
#56500=CARTESIAN_POINT('Ctrl Pts',(67.1027204477304,-29.0952614183778,0.));
#56501=CARTESIAN_POINT('Ctrl Pts',(67.1027204477304,-29.0952614183778,12.));
#56502=CARTESIAN_POINT('Ctrl Pts',(67.1287214368743,-29.0957568873358,0.));
#56503=CARTESIAN_POINT('Ctrl Pts',(67.1287214368743,-29.0957568873358,12.));
#56504=CARTESIAN_POINT('Ctrl Pts',(67.1547609306845,-29.0962287427275,0.));
#56505=CARTESIAN_POINT('Ctrl Pts',(67.1547609306845,-29.0962287427275,12.));
#56506=CARTESIAN_POINT('Ctrl Pts',(67.1808388322116,-29.0966769313893,0.));
#56507=CARTESIAN_POINT('Ctrl Pts',(67.1808388322116,-29.0966769313893,12.));
#56508=CARTESIAN_POINT('Ctrl Pts',(67.2069550447895,-29.0971014004135,0.));
#56509=CARTESIAN_POINT('Ctrl Pts',(67.2069550447895,-29.0971014004135,12.));
#56510=CARTESIAN_POINT('Ctrl Pts',(67.2331094720482,-29.0975020971474,0.));
#56511=CARTESIAN_POINT('Ctrl Pts',(67.2331094720482,-29.0975020971474,12.));
#56512=CARTESIAN_POINT('Ctrl Pts',(67.2593020179216,-29.0978789691965,0.));
#56513=CARTESIAN_POINT('Ctrl Pts',(67.2593020179216,-29.0978789691965,12.));
#56514=CARTESIAN_POINT('Ctrl Pts',(67.2855325866516,-29.0982319644277,0.));
#56515=CARTESIAN_POINT('Ctrl Pts',(67.2855325866516,-29.0982319644277,12.));
#56516=CARTESIAN_POINT('Ctrl Pts',(67.311801082791,-29.0985610309768,0.));
#56517=CARTESIAN_POINT('Ctrl Pts',(67.311801082791,-29.0985610309768,12.));
#56518=CARTESIAN_POINT('Ctrl Pts',(67.3381074112013,-29.0988661172526,0.));
#56519=CARTESIAN_POINT('Ctrl Pts',(67.3381074112013,-29.0988661172526,12.));
#56520=CARTESIAN_POINT('Ctrl Pts',(67.3644514770373,-29.0991471719172,0.));
#56521=CARTESIAN_POINT('Ctrl Pts',(67.3644514770373,-29.0991471719172,12.));
#56522=CARTESIAN_POINT('Ctrl Pts',(67.3908331857313,-29.0994041438715,0.));
#56523=CARTESIAN_POINT('Ctrl Pts',(67.3908331857313,-29.0994041438715,12.));
#56524=CARTESIAN_POINT('Ctrl Pts',(67.4172524429726,-29.0996369822418,0.));
#56525=CARTESIAN_POINT('Ctrl Pts',(67.4172524429726,-29.0996369822418,12.));
#56526=CARTESIAN_POINT('Ctrl Pts',(67.4437091546869,-29.0998456363687,0.));
#56527=CARTESIAN_POINT('Ctrl Pts',(67.4437091546869,-29.0998456363687,12.));
#56528=CARTESIAN_POINT('Ctrl Pts',(67.4702032270062,-29.1000300557961,0.));
#56529=CARTESIAN_POINT('Ctrl Pts',(67.4702032270062,-29.1000300557961,12.));
#56530=CARTESIAN_POINT('Ctrl Pts',(67.496734566311,-29.1001901902915,0.));
#56531=CARTESIAN_POINT('Ctrl Pts',(67.496734566311,-29.1001901902915,12.));
#56532=CARTESIAN_POINT('Ctrl Pts',(67.5233030792714,-29.1003259898686,0.));
#56533=CARTESIAN_POINT('Ctrl Pts',(67.5233030792714,-29.1003259898686,12.));
#56534=CARTESIAN_POINT('Ctrl Pts',(67.5499086728891,-29.1004374048149,0.));
#56535=CARTESIAN_POINT('Ctrl Pts',(67.5499086728891,-29.1004374048149,12.));
#56536=CARTESIAN_POINT('Ctrl Pts',(67.5765512545276,-29.1005243857137,0.));
#56537=CARTESIAN_POINT('Ctrl Pts',(67.5765512545276,-29.1005243857137,12.));
#56538=CARTESIAN_POINT('Ctrl Pts',(67.6032307319614,-29.1005868834863,0.));
#56539=CARTESIAN_POINT('Ctrl Pts',(67.6032307319614,-29.1005868834863,12.));
#56540=CARTESIAN_POINT('Ctrl Pts',(67.6299470133286,-29.1006248493577,0.));
#56541=CARTESIAN_POINT('Ctrl Pts',(67.6299470133286,-29.1006248493577,12.));
#56542=CARTESIAN_POINT('Ctrl Pts',(67.6567000070319,-29.1006382347812,0.));
#56543=CARTESIAN_POINT('Ctrl Pts',(67.6567000070319,-29.1006382347812,12.));
#56544=CARTESIAN_POINT('Ctrl Pts',(67.6834896216458,-29.1006269913747,0.));
#56545=CARTESIAN_POINT('Ctrl Pts',(67.6834896216458,-29.1006269913747,12.));
#56546=CARTESIAN_POINT('Ctrl Pts',(67.7103157658296,-29.1005910708625,0.));
#56547=CARTESIAN_POINT('Ctrl Pts',(67.7103157658296,-29.1005910708625,12.));
#56548=CARTESIAN_POINT('Ctrl Pts',(67.7371783482039,-29.1005304249989,0.));
#56549=CARTESIAN_POINT('Ctrl Pts',(67.7371783482039,-29.1005304249989,12.));
#56550=CARTESIAN_POINT('Ctrl Pts',(67.7640772773397,-29.1004450055647,0.));
#56551=CARTESIAN_POINT('Ctrl Pts',(67.7640772773397,-29.1004450055647,12.));
#56552=CARTESIAN_POINT('Ctrl Pts',(67.7910124620148,-29.10033476453,0.));
#56553=CARTESIAN_POINT('Ctrl Pts',(67.7910124620148,-29.10033476453,12.));
#56554=CARTESIAN_POINT('Ctrl Pts',(67.817983811411,-29.1001996541847,0.));
#56555=CARTESIAN_POINT('Ctrl Pts',(67.817983811411,-29.1001996541847,12.));
#56556=CARTESIAN_POINT('Ctrl Pts',(67.844991235333,-29.1000396272868,0.));
#56557=CARTESIAN_POINT('Ctrl Pts',(67.844991235333,-29.1000396272868,12.));
#56558=CARTESIAN_POINT('Ctrl Pts',(67.8720346444111,-29.0998546372027,0.));
#56559=CARTESIAN_POINT('Ctrl Pts',(67.8720346444111,-29.0998546372027,12.));
#56560=CARTESIAN_POINT('Ctrl Pts',(67.8991139503168,-29.0996446380617,0.));
#56561=CARTESIAN_POINT('Ctrl Pts',(67.8991139503168,-29.0996446380617,12.));
#56562=CARTESIAN_POINT('Ctrl Pts',(67.9262290652797,-29.0994095844208,0.));
#56563=CARTESIAN_POINT('Ctrl Pts',(67.9262290652797,-29.0994095844208,12.));
#56564=CARTESIAN_POINT('Ctrl Pts',(67.9533799016122,-29.0991494309395,0.));
#56565=CARTESIAN_POINT('Ctrl Pts',(67.9533799016122,-29.0991494309395,12.));
#56566=CARTESIAN_POINT('Ctrl Pts',(67.9805663711845,-29.0988641320243,0.));
#56567=CARTESIAN_POINT('Ctrl Pts',(67.9805663711845,-29.0988641320243,12.));
#56568=CARTESIAN_POINT('Ctrl Pts',(68.0077883850136,-29.0985536415537,0.));
#56569=CARTESIAN_POINT('Ctrl Pts',(68.0077883850136,-29.0985536415537,12.));
#56570=CARTESIAN_POINT('Ctrl Pts',(68.0350458525589,-29.0982179124113,0.));
#56571=CARTESIAN_POINT('Ctrl Pts',(68.0350458525589,-29.0982179124113,12.));
#56572=CARTESIAN_POINT('Ctrl Pts',(68.0623386822917,-29.0978568968678,0.));
#56573=CARTESIAN_POINT('Ctrl Pts',(68.0623386822917,-29.0978568968678,12.));
#56574=CARTESIAN_POINT('Ctrl Pts',(68.089666782962,-29.0974705474279,0.));
#56575=CARTESIAN_POINT('Ctrl Pts',(68.089666782962,-29.0974705474279,12.));
#56576=CARTESIAN_POINT('Ctrl Pts',(68.1170300647019,-29.0970588175741,0.));
#56577=CARTESIAN_POINT('Ctrl Pts',(68.1170300647019,-29.0970588175741,12.));
#56578=CARTESIAN_POINT('Ctrl Pts',(68.1444284400734,-29.0966216624741,0.));
#56579=CARTESIAN_POINT('Ctrl Pts',(68.1444284400734,-29.0966216624741,12.));
#56580=CARTESIAN_POINT('Ctrl Pts',(68.1718618254221,-29.0961590399024,0.));
#56581=CARTESIAN_POINT('Ctrl Pts',(68.1718618254221,-29.0961590399024,12.));
#56582=CARTESIAN_POINT('Ctrl Pts',(68.1993301411959,-29.0956709104588,0.));
#56583=CARTESIAN_POINT('Ctrl Pts',(68.1993301411959,-29.0956709104588,12.));
#56584=CARTESIAN_POINT('Ctrl Pts',(68.22683330895,-29.0951572355353,0.));
#56585=CARTESIAN_POINT('Ctrl Pts',(68.22683330895,-29.0951572355353,12.));
#56586=CARTESIAN_POINT('Ctrl Pts',(68.2543712489815,-29.0946179757133,0.));
#56587=CARTESIAN_POINT('Ctrl Pts',(68.2543712489815,-29.0946179757133,12.));
#56588=CARTESIAN_POINT('Ctrl Pts',(68.2819438775932,-29.0940530889142,0.));
#56589=CARTESIAN_POINT('Ctrl Pts',(68.2819438775932,-29.0940530889142,12.));
#56590=CARTESIAN_POINT('Ctrl Pts',(68.3095511047852,-29.0934625288442,0.));
#56591=CARTESIAN_POINT('Ctrl Pts',(68.3095511047852,-29.0934625288442,12.));
#56592=CARTESIAN_POINT('Ctrl Pts',(68.3371928310351,-29.0928462428219,0.));
#56593=CARTESIAN_POINT('Ctrl Pts',(68.3371928310351,-29.0928462428219,12.));
#56594=CARTESIAN_POINT('Ctrl Pts',(68.3648689519188,-29.0922041749393,0.));
#56595=CARTESIAN_POINT('Ctrl Pts',(68.3648689519188,-29.0922041749393,12.));
#56596=CARTESIAN_POINT('Ctrl Pts',(68.3925793638241,-29.091536269955,0.));
#56597=CARTESIAN_POINT('Ctrl Pts',(68.3925793638241,-29.091536269955,12.));
#56598=CARTESIAN_POINT('Ctrl Pts',(68.4203239694742,-29.0908424770941,0.));
#56599=CARTESIAN_POINT('Ctrl Pts',(68.4203239694742,-29.0908424770941,12.));
#56600=CARTESIAN_POINT('Ctrl Pts',(68.4481026830845,-29.0901227535274,0.));
#56601=CARTESIAN_POINT('Ctrl Pts',(68.4481026830845,-29.0901227535274,12.));
#56602=CARTESIAN_POINT('Ctrl Pts',(68.4759154367582,-29.0893770688808,0.));
#56603=CARTESIAN_POINT('Ctrl Pts',(68.4759154367582,-29.0893770688808,12.));
#56604=CARTESIAN_POINT('Ctrl Pts',(68.5037621823575,-29.0886054060334,0.));
#56605=CARTESIAN_POINT('Ctrl Pts',(68.5037621823575,-29.0886054060334,12.));
#56606=CARTESIAN_POINT('Ctrl Pts',(68.5316428874729,-29.0878077570819,0.));
#56607=CARTESIAN_POINT('Ctrl Pts',(68.5316428874729,-29.0878077570819,12.));
#56608=CARTESIAN_POINT('Ctrl Pts',(68.5539746037961,-29.0871488478365,0.));
#56609=CARTESIAN_POINT('Ctrl Pts',(68.5539746037961,-29.0871488478365,12.));
#56610=CARTESIAN_POINT('Ctrl Pts',(68.5707386600286,-29.0866429721959,0.));
#56611=CARTESIAN_POINT('Ctrl Pts',(68.5707386600286,-29.0866429721959,12.));
#56612=CARTESIAN_POINT('Ctrl Pts',(68.5819214834609,-29.086300524779,0.));
#56613=CARTESIAN_POINT('Ctrl Pts',(68.5819214834609,-29.086300524779,12.));
#56614=CARTESIAN_POINT('Ctrl Pts',(68.5875145916629,-29.086128001823,0.));
#56615=CARTESIAN_POINT('Ctrl Pts',(68.5875145916629,-29.086128001823,12.));
#56616=CARTESIAN_POINT('',(63.7976679095314,-28.8072485549237,0.));
#56617=CARTESIAN_POINT('Ctrl Pts',(63.7976679095314,-28.8072485549237,0.));
#56618=CARTESIAN_POINT('Ctrl Pts',(63.8014989507494,-28.8078854475432,0.));
#56619=CARTESIAN_POINT('Ctrl Pts',(63.8091667271231,-28.8091580239553,0.));
#56620=CARTESIAN_POINT('Ctrl Pts',(63.8206854735027,-28.8110632620958,0.));
#56621=CARTESIAN_POINT('Ctrl Pts',(63.8360779669856,-28.8135963263369,0.));
#56622=CARTESIAN_POINT('Ctrl Pts',(63.8553755207486,-28.8167505576681,0.));
#56623=CARTESIAN_POINT('Ctrl Pts',(63.8747299825313,-28.8198926619858,0.));
#56624=CARTESIAN_POINT('Ctrl Pts',(63.8941412856923,-28.823022586318,0.));
#56625=CARTESIAN_POINT('Ctrl Pts',(63.9136093063786,-28.8261402423291,0.));
#56626=CARTESIAN_POINT('Ctrl Pts',(63.9331338646996,-28.829245507756,0.));
#56627=CARTESIAN_POINT('Ctrl Pts',(63.9527147494423,-28.8323382413789,0.));
#56628=CARTESIAN_POINT('Ctrl Pts',(63.9723517369614,-28.8354182946601,0.));
#56629=CARTESIAN_POINT('Ctrl Pts',(63.9920446117582,-28.8384855243243,0.));
#56630=CARTESIAN_POINT('Ctrl Pts',(64.0117931881298,-28.8415398056428,0.));
#56631=CARTESIAN_POINT('Ctrl Pts',(64.0315973031942,-28.844581028125,0.));
#56632=CARTESIAN_POINT('Ctrl Pts',(64.0514568066637,-28.8476090892232,0.));
#56633=CARTESIAN_POINT('Ctrl Pts',(64.0713715523599,-28.8506238891093,0.));
#56634=CARTESIAN_POINT('Ctrl Pts',(64.0913413876622,-28.8536253241854,0.));
#56635=CARTESIAN_POINT('Ctrl Pts',(64.1113661481965,-28.8566132838179,0.));
#56636=CARTESIAN_POINT('Ctrl Pts',(64.1314456633381,-28.8595876537148,0.));
#56637=CARTESIAN_POINT('Ctrl Pts',(64.1515797596564,-28.8625483180438,0.));
#56638=CARTESIAN_POINT('Ctrl Pts',(64.1717682648685,-28.8654951618649,0.));
#56639=CARTESIAN_POINT('Ctrl Pts',(64.1920110123299,-28.8684280739014,0.));
#56640=CARTESIAN_POINT('Ctrl Pts',(64.2123078408461,-28.8713469464185,0.));
#56641=CARTESIAN_POINT('Ctrl Pts',(64.2326585925252,-28.8742516738947,0.));
#56642=CARTESIAN_POINT('Ctrl Pts',(64.2530631112929,-28.877142152106,0.));
#56643=CARTESIAN_POINT('Ctrl Pts',(64.273521241071,-28.8800182770065,0.));
#56644=CARTESIAN_POINT('Ctrl Pts',(64.2940328242521,-28.882879943794,0.));
#56645=CARTESIAN_POINT('Ctrl Pts',(64.3145977025037,-28.8857270473959,0.));
#56646=CARTESIAN_POINT('Ctrl Pts',(64.3352157174619,-28.8885594828926,0.));
#56647=CARTESIAN_POINT('Ctrl Pts',(64.3558867114076,-28.8913771459323,0.));
#56648=CARTESIAN_POINT('Ctrl Pts',(64.3766105280688,-28.89417993323,0.));
#56649=CARTESIAN_POINT('Ctrl Pts',(64.3973870129169,-28.8969677427504,0.));
#56650=CARTESIAN_POINT('Ctrl Pts',(64.4182160127379,-28.899740473434,0.));
#56651=CARTESIAN_POINT('Ctrl Pts',(64.4390973753634,-28.9024980250307,0.));
#56652=CARTESIAN_POINT('Ctrl Pts',(64.4600309493583,-28.9052402979062,0.));
#56653=CARTESIAN_POINT('Ctrl Pts',(64.4810165836592,-28.9079671928264,0.));
#56654=CARTESIAN_POINT('Ctrl Pts',(64.5020541275951,-28.910678610965,0.));
#56655=CARTESIAN_POINT('Ctrl Pts',(64.523143431047,-28.9133744539949,0.));
#56656=CARTESIAN_POINT('Ctrl Pts',(64.5442843445559,-28.9160546241538,0.));
#56657=CARTESIAN_POINT('Ctrl Pts',(64.5654767194471,-28.9187190243224,0.));
#56658=CARTESIAN_POINT('Ctrl Pts',(64.5867204079426,-28.9213675580985,0.));
#56659=CARTESIAN_POINT('Ctrl Pts',(64.6080152631039,-28.9240001297542,0.));
#56660=CARTESIAN_POINT('Ctrl Pts',(64.629361138774,-28.9266166441951,0.));
#56661=CARTESIAN_POINT('Ctrl Pts',(64.6507578895161,-28.9292170069222,0.));
#56662=CARTESIAN_POINT('Ctrl Pts',(64.672205370541,-28.9318011239915,0.));
#56663=CARTESIAN_POINT('Ctrl Pts',(64.6937034376617,-28.9343689019882,0.));
#56664=CARTESIAN_POINT('Ctrl Pts',(64.715251947329,-28.9369202480393,0.));
#56665=CARTESIAN_POINT('Ctrl Pts',(64.7368507566467,-28.9394550698204,0.));
#56666=CARTESIAN_POINT('Ctrl Pts',(64.758499723388,-28.9419732755656,0.));
#56667=CARTESIAN_POINT('Ctrl Pts',(64.7801987060084,-28.944474774081,0.));
#56668=CARTESIAN_POINT('Ctrl Pts',(64.8019475636442,-28.9469594747432,0.));
#56669=CARTESIAN_POINT('Ctrl Pts',(64.8237461561018,-28.9494272874832,0.));
#56670=CARTESIAN_POINT('Ctrl Pts',(64.8455943438423,-28.9518781227765,0.));
#56671=CARTESIAN_POINT('Ctrl Pts',(64.8674919879648,-28.9543118916328,0.));
#56672=CARTESIAN_POINT('Ctrl Pts',(64.8894389501801,-28.9567285055867,0.));
#56673=CARTESIAN_POINT('Ctrl Pts',(64.9114350928125,-28.9591278766934,0.));
#56674=CARTESIAN_POINT('Ctrl Pts',(64.9334802788038,-28.961509917525,0.));
#56675=CARTESIAN_POINT('Ctrl Pts',(64.9555743717109,-28.9638745411677,0.));
#56676=CARTESIAN_POINT('Ctrl Pts',(64.9777172357027,-28.9662216612217,0.));
#56677=CARTESIAN_POINT('Ctrl Pts',(64.9999087355504,-28.9685511918019,0.));
#56678=CARTESIAN_POINT('Ctrl Pts',(65.022148736628,-28.97086304753,0.));
#56679=CARTESIAN_POINT('Ctrl Pts',(65.0444371049082,-28.9731571435283,0.));
#56680=CARTESIAN_POINT('Ctrl Pts',(65.0667737069563,-28.9754333954135,0.));
#56681=CARTESIAN_POINT('Ctrl Pts',(65.0891584099168,-28.9776917192933,0.));
#56682=CARTESIAN_POINT('Ctrl Pts',(65.1115910815037,-28.9799320317641,0.));
#56683=CARTESIAN_POINT('Ctrl Pts',(65.1340715900028,-28.9821542499043,0.));
#56684=CARTESIAN_POINT('Ctrl Pts',(65.1565998042697,-28.9843582912693,0.));
#56685=CARTESIAN_POINT('Ctrl Pts',(65.1791755937256,-28.9865440738884,0.));
#56686=CARTESIAN_POINT('Ctrl Pts',(65.2017988283479,-28.9887115162634,0.));
#56687=CARTESIAN_POINT('Ctrl Pts',(65.2244693786609,-28.9908605373663,0.));
#56688=CARTESIAN_POINT('Ctrl Pts',(65.2471871157397,-28.9929910566325,0.));
#56689=CARTESIAN_POINT('Ctrl Pts',(65.2699519112064,-28.9951029939557,0.));
#56690=CARTESIAN_POINT('Ctrl Pts',(65.2927636372253,-28.9971962696845,0.));
#56691=CARTESIAN_POINT('Ctrl Pts',(65.3156221664916,-28.9992708046212,0.));
#56692=CARTESIAN_POINT('Ctrl Pts',(65.3385273722241,-29.0013265200185,0.));
#56693=CARTESIAN_POINT('Ctrl Pts',(65.3614791281692,-29.003363337573,0.));
#56694=CARTESIAN_POINT('Ctrl Pts',(65.3844773085961,-29.0053811794207,0.));
#56695=CARTESIAN_POINT('Ctrl Pts',(65.4075217882934,-29.0073799681342,0.));
#56696=CARTESIAN_POINT('Ctrl Pts',(65.4306124425562,-29.0093596267216,0.));
#56697=CARTESIAN_POINT('Ctrl Pts',(65.4537491471828,-29.0113200786239,0.));
#56698=CARTESIAN_POINT('Ctrl Pts',(65.4769317784789,-29.013261247709,0.));
#56699=CARTESIAN_POINT('Ctrl Pts',(65.5001602132535,-29.0151830582675,0.));
#56700=CARTESIAN_POINT('Ctrl Pts',(65.5234343288136,-29.0170854350095,0.));
#56701=CARTESIAN_POINT('Ctrl Pts',(65.5467540029514,-29.0189683030642,0.));
#56702=CARTESIAN_POINT('Ctrl Pts',(65.5701191139418,-29.0208315879764,0.));
#56703=CARTESIAN_POINT('Ctrl Pts',(65.5935295405453,-29.0226752157003,0.));
#56704=CARTESIAN_POINT('Ctrl Pts',(65.6169851620046,-29.0244991125959,0.));
#56705=CARTESIAN_POINT('Ctrl Pts',(65.6404858580403,-29.0263032054267,0.));
#56706=CARTESIAN_POINT('Ctrl Pts',(65.6640315088388,-29.0280874213596,0.));
#56707=CARTESIAN_POINT('Ctrl Pts',(65.6876219950493,-29.0298516879612,0.));
#56708=CARTESIAN_POINT('Ctrl Pts',(65.7112571977891,-29.0315959331919,0.));
#56709=CARTESIAN_POINT('Ctrl Pts',(65.7349369986384,-29.0333200854028,0.));
#56710=CARTESIAN_POINT('Ctrl Pts',(65.7586612796368,-29.035024073333,0.));
#56711=CARTESIAN_POINT('Ctrl Pts',(65.7824299232705,-29.0367078261103,0.));
#56712=CARTESIAN_POINT('Ctrl Pts',(65.8062428124713,-29.0383712732469,0.));
#56713=CARTESIAN_POINT('Ctrl Pts',(65.8300998306191,-29.0400143446338,0.));
#56714=CARTESIAN_POINT('Ctrl Pts',(65.854000861539,-29.0416369705376,0.));
#56715=CARTESIAN_POINT('Ctrl Pts',(65.8779457894961,-29.0432390815978,0.));
#56716=CARTESIAN_POINT('Ctrl Pts',(65.9019344991854,-29.0448206088289,0.));
#56717=CARTESIAN_POINT('Ctrl Pts',(65.9259668757306,-29.0463814836158,0.));
#56718=CARTESIAN_POINT('Ctrl Pts',(65.9500428046868,-29.0479216377081,0.));
#56719=CARTESIAN_POINT('Ctrl Pts',(65.9741621720369,-29.0494410032173,0.));
#56720=CARTESIAN_POINT('Ctrl Pts',(65.9983248641879,-29.0509395126143,0.));
#56721=CARTESIAN_POINT('Ctrl Pts',(66.0225307679591,-29.0524170987307,0.));
#56722=CARTESIAN_POINT('Ctrl Pts',(66.0467797705815,-29.0538736947552,0.));
#56723=CARTESIAN_POINT('Ctrl Pts',(66.0710717597009,-29.0553092342279,0.));
#56724=CARTESIAN_POINT('Ctrl Pts',(66.0954066233754,-29.0567236510374,0.));
#56725=CARTESIAN_POINT('Ctrl Pts',(66.1197842500711,-29.058116879419,0.));
#56726=CARTESIAN_POINT('Ctrl Pts',(66.1442045286516,-29.0594888539556,0.));
#56727=CARTESIAN_POINT('Ctrl Pts',(66.1686673483755,-29.0608395095746,0.));
#56728=CARTESIAN_POINT('Ctrl Pts',(66.1931725989008,-29.062168781542,0.));
#56729=CARTESIAN_POINT('Ctrl Pts',(66.2177201702819,-29.0634766054599,0.));
#56730=CARTESIAN_POINT('Ctrl Pts',(66.2423099529668,-29.0647629172645,0.));
#56731=CARTESIAN_POINT('Ctrl Pts',(66.2669418377865,-29.0660276532272,0.));
#56732=CARTESIAN_POINT('Ctrl Pts',(66.2916157159527,-29.0672707499527,0.));
#56733=CARTESIAN_POINT('Ctrl Pts',(66.3163314790607,-29.0684921443718,0.));
#56734=CARTESIAN_POINT('Ctrl Pts',(66.3410890190879,-29.0696917737398,0.));
#56735=CARTESIAN_POINT('Ctrl Pts',(66.3658882283906,-29.0708695756336,0.));
#56736=CARTESIAN_POINT('Ctrl Pts',(66.3907289996942,-29.0720254879535,0.));
#56737=CARTESIAN_POINT('Ctrl Pts',(66.4156112260904,-29.0731594489219,0.));
#56738=CARTESIAN_POINT('Ctrl Pts',(66.4405348010404,-29.0742713970763,0.));
#56739=CARTESIAN_POINT('Ctrl Pts',(66.4654996183739,-29.075361271267,0.));
#56740=CARTESIAN_POINT('Ctrl Pts',(66.4905055722864,-29.0764290106553,0.));
#56741=CARTESIAN_POINT('Ctrl Pts',(66.5155525573308,-29.0774745547146,0.));
#56742=CARTESIAN_POINT('Ctrl Pts',(66.5406404684116,-29.0784978432294,0.));
#56743=CARTESIAN_POINT('Ctrl Pts',(66.5657692007894,-29.0794988162892,0.));
#56744=CARTESIAN_POINT('Ctrl Pts',(66.5909386500796,-29.0804774142852,0.));
#56745=CARTESIAN_POINT('Ctrl Pts',(66.6161487122504,-29.0814335779086,0.));
#56746=CARTESIAN_POINT('Ctrl Pts',(66.6413992836148,-29.0823672481508,0.));
#56747=CARTESIAN_POINT('Ctrl Pts',(66.6666902608246,-29.0832783663049,0.));
#56748=CARTESIAN_POINT('Ctrl Pts',(66.6920215408744,-29.0841668739585,0.));
#56749=CARTESIAN_POINT('Ctrl Pts',(66.7173930211015,-29.0850327129914,0.));
#56750=CARTESIAN_POINT('Ctrl Pts',(66.742804599184,-29.0858758255729,0.));
#56751=CARTESIAN_POINT('Ctrl Pts',(66.7682561731348,-29.086696154163,0.));
#56752=CARTESIAN_POINT('Ctrl Pts',(66.7937476412941,-29.0874936415138,0.));
#56753=CARTESIAN_POINT('Ctrl Pts',(66.8192789023323,-29.0882682306636,0.));
#56754=CARTESIAN_POINT('Ctrl Pts',(66.8448498552508,-29.0890198649327,0.));
#56755=CARTESIAN_POINT('Ctrl Pts',(66.8704603993794,-29.0897484879208,0.));
#56756=CARTESIAN_POINT('Ctrl Pts',(66.8961104343703,-29.0904540435064,0.));
#56757=CARTESIAN_POINT('Ctrl Pts',(66.9217998601881,-29.0911364758484,0.));
#56758=CARTESIAN_POINT('Ctrl Pts',(66.9475285771133,-29.0917957293825,0.));
#56759=CARTESIAN_POINT('Ctrl Pts',(66.9732964857467,-29.092431748817,0.));
#56760=CARTESIAN_POINT('Ctrl Pts',(66.9991034870084,-29.0930444791329,0.));
#56761=CARTESIAN_POINT('Ctrl Pts',(67.0249494821361,-29.0936338655828,0.));
#56762=CARTESIAN_POINT('Ctrl Pts',(67.0508343726771,-29.0941998536958,0.));
#56763=CARTESIAN_POINT('Ctrl Pts',(67.0767580604872,-29.0947423892725,0.));
#56764=CARTESIAN_POINT('Ctrl Pts',(67.1027204477304,-29.0952614183778,0.));
#56765=CARTESIAN_POINT('Ctrl Pts',(67.1287214368743,-29.0957568873358,0.));
#56766=CARTESIAN_POINT('Ctrl Pts',(67.1547609306845,-29.0962287427275,0.));
#56767=CARTESIAN_POINT('Ctrl Pts',(67.1808388322116,-29.0966769313893,0.));
#56768=CARTESIAN_POINT('Ctrl Pts',(67.2069550447895,-29.0971014004135,0.));
#56769=CARTESIAN_POINT('Ctrl Pts',(67.2331094720482,-29.0975020971474,0.));
#56770=CARTESIAN_POINT('Ctrl Pts',(67.2593020179216,-29.0978789691965,0.));
#56771=CARTESIAN_POINT('Ctrl Pts',(67.2855325866516,-29.0982319644277,0.));
#56772=CARTESIAN_POINT('Ctrl Pts',(67.311801082791,-29.0985610309768,0.));
#56773=CARTESIAN_POINT('Ctrl Pts',(67.3381074112013,-29.0988661172526,0.));
#56774=CARTESIAN_POINT('Ctrl Pts',(67.3644514770373,-29.0991471719172,0.));
#56775=CARTESIAN_POINT('Ctrl Pts',(67.3908331857313,-29.0994041438715,0.));
#56776=CARTESIAN_POINT('Ctrl Pts',(67.4172524429726,-29.0996369822418,0.));
#56777=CARTESIAN_POINT('Ctrl Pts',(67.4437091546869,-29.0998456363687,0.));
#56778=CARTESIAN_POINT('Ctrl Pts',(67.4702032270062,-29.1000300557961,0.));
#56779=CARTESIAN_POINT('Ctrl Pts',(67.496734566311,-29.1001901902915,0.));
#56780=CARTESIAN_POINT('Ctrl Pts',(67.5233030792714,-29.1003259898686,0.));
#56781=CARTESIAN_POINT('Ctrl Pts',(67.5499086728891,-29.1004374048149,0.));
#56782=CARTESIAN_POINT('Ctrl Pts',(67.5765512545276,-29.1005243857137,0.));
#56783=CARTESIAN_POINT('Ctrl Pts',(67.6032307319614,-29.1005868834863,0.));
#56784=CARTESIAN_POINT('Ctrl Pts',(67.6299470133286,-29.1006248493577,0.));
#56785=CARTESIAN_POINT('Ctrl Pts',(67.6567000070319,-29.1006382347812,0.));
#56786=CARTESIAN_POINT('Ctrl Pts',(67.6834896216458,-29.1006269913747,0.));
#56787=CARTESIAN_POINT('Ctrl Pts',(67.7103157658296,-29.1005910708625,0.));
#56788=CARTESIAN_POINT('Ctrl Pts',(67.7371783482039,-29.1005304249989,0.));
#56789=CARTESIAN_POINT('Ctrl Pts',(67.7640772773397,-29.1004450055647,0.));
#56790=CARTESIAN_POINT('Ctrl Pts',(67.7910124620148,-29.10033476453,0.));
#56791=CARTESIAN_POINT('Ctrl Pts',(67.817983811411,-29.1001996541847,0.));
#56792=CARTESIAN_POINT('Ctrl Pts',(67.844991235333,-29.1000396272868,0.));
#56793=CARTESIAN_POINT('Ctrl Pts',(67.8720346444111,-29.0998546372027,0.));
#56794=CARTESIAN_POINT('Ctrl Pts',(67.8991139503168,-29.0996446380617,0.));
#56795=CARTESIAN_POINT('Ctrl Pts',(67.9262290652797,-29.0994095844208,0.));
#56796=CARTESIAN_POINT('Ctrl Pts',(67.9533799016122,-29.0991494309395,0.));
#56797=CARTESIAN_POINT('Ctrl Pts',(67.9805663711845,-29.0988641320243,0.));
#56798=CARTESIAN_POINT('Ctrl Pts',(68.0077883850136,-29.0985536415537,0.));
#56799=CARTESIAN_POINT('Ctrl Pts',(68.0350458525589,-29.0982179124113,0.));
#56800=CARTESIAN_POINT('Ctrl Pts',(68.0623386822917,-29.0978568968678,0.));
#56801=CARTESIAN_POINT('Ctrl Pts',(68.089666782962,-29.0974705474279,0.));
#56802=CARTESIAN_POINT('Ctrl Pts',(68.1170300647019,-29.0970588175741,0.));
#56803=CARTESIAN_POINT('Ctrl Pts',(68.1444284400734,-29.0966216624741,0.));
#56804=CARTESIAN_POINT('Ctrl Pts',(68.1718618254221,-29.0961590399024,0.));
#56805=CARTESIAN_POINT('Ctrl Pts',(68.1993301411959,-29.0956709104588,0.));
#56806=CARTESIAN_POINT('Ctrl Pts',(68.2229056854495,-29.0952305915108,0.));
#56807=CARTESIAN_POINT('Ctrl Pts',(68.2409993689947,-29.0948791947834,0.));
#56808=CARTESIAN_POINT('Ctrl Pts',(68.2535957746883,-29.0946280433311,0.));
#56809=CARTESIAN_POINT('Ctrl Pts',(68.2606847334624,-29.0944846386549,0.));
#56810=CARTESIAN_POINT('Ctrl Pts',(68.2622612909744,-29.0944526440249,0.));
#56811=CARTESIAN_POINT('',(63.7976679095314,-28.8072485549237,12.));
#56812=CARTESIAN_POINT('',(63.7976679095314,-28.8072485549237,0.));
#56813=CARTESIAN_POINT('Ctrl Pts',(68.2622612909744,-29.0944526440249,12.));
#56814=CARTESIAN_POINT('Ctrl Pts',(68.2606847334624,-29.0944846386549,12.));
#56815=CARTESIAN_POINT('Ctrl Pts',(68.2535957746883,-29.0946280433311,12.));
#56816=CARTESIAN_POINT('Ctrl Pts',(68.2409993689947,-29.0948791947834,12.));
#56817=CARTESIAN_POINT('Ctrl Pts',(68.2229056854495,-29.0952305915108,12.));
#56818=CARTESIAN_POINT('Ctrl Pts',(68.1993301411959,-29.0956709104588,12.));
#56819=CARTESIAN_POINT('Ctrl Pts',(68.1718618254221,-29.0961590399024,12.));
#56820=CARTESIAN_POINT('Ctrl Pts',(68.1444284400734,-29.0966216624741,12.));
#56821=CARTESIAN_POINT('Ctrl Pts',(68.1170300647019,-29.0970588175741,12.));
#56822=CARTESIAN_POINT('Ctrl Pts',(68.089666782962,-29.0974705474279,12.));
#56823=CARTESIAN_POINT('Ctrl Pts',(68.0623386822917,-29.0978568968678,12.));
#56824=CARTESIAN_POINT('Ctrl Pts',(68.0350458525589,-29.0982179124113,12.));
#56825=CARTESIAN_POINT('Ctrl Pts',(68.0077883850136,-29.0985536415537,12.));
#56826=CARTESIAN_POINT('Ctrl Pts',(67.9805663711845,-29.0988641320243,12.));
#56827=CARTESIAN_POINT('Ctrl Pts',(67.9533799016122,-29.0991494309395,12.));
#56828=CARTESIAN_POINT('Ctrl Pts',(67.9262290652797,-29.0994095844208,12.));
#56829=CARTESIAN_POINT('Ctrl Pts',(67.8991139503168,-29.0996446380617,12.));
#56830=CARTESIAN_POINT('Ctrl Pts',(67.8720346444111,-29.0998546372027,12.));
#56831=CARTESIAN_POINT('Ctrl Pts',(67.844991235333,-29.1000396272868,12.));
#56832=CARTESIAN_POINT('Ctrl Pts',(67.817983811411,-29.1001996541847,12.));
#56833=CARTESIAN_POINT('Ctrl Pts',(67.7910124620148,-29.10033476453,12.));
#56834=CARTESIAN_POINT('Ctrl Pts',(67.7640772773397,-29.1004450055647,12.));
#56835=CARTESIAN_POINT('Ctrl Pts',(67.7371783482039,-29.1005304249989,12.));
#56836=CARTESIAN_POINT('Ctrl Pts',(67.7103157658296,-29.1005910708625,12.));
#56837=CARTESIAN_POINT('Ctrl Pts',(67.6834896216458,-29.1006269913747,12.));
#56838=CARTESIAN_POINT('Ctrl Pts',(67.6567000070319,-29.1006382347812,12.));
#56839=CARTESIAN_POINT('Ctrl Pts',(67.6299470133286,-29.1006248493577,12.));
#56840=CARTESIAN_POINT('Ctrl Pts',(67.6032307319614,-29.1005868834863,12.));
#56841=CARTESIAN_POINT('Ctrl Pts',(67.5765512545276,-29.1005243857137,12.));
#56842=CARTESIAN_POINT('Ctrl Pts',(67.5499086728891,-29.1004374048149,12.));
#56843=CARTESIAN_POINT('Ctrl Pts',(67.5233030792714,-29.1003259898686,12.));
#56844=CARTESIAN_POINT('Ctrl Pts',(67.496734566311,-29.1001901902915,12.));
#56845=CARTESIAN_POINT('Ctrl Pts',(67.4702032270062,-29.1000300557961,12.));
#56846=CARTESIAN_POINT('Ctrl Pts',(67.4437091546869,-29.0998456363687,12.));
#56847=CARTESIAN_POINT('Ctrl Pts',(67.4172524429726,-29.0996369822418,12.));
#56848=CARTESIAN_POINT('Ctrl Pts',(67.3908331857313,-29.0994041438715,12.));
#56849=CARTESIAN_POINT('Ctrl Pts',(67.3644514770373,-29.0991471719172,12.));
#56850=CARTESIAN_POINT('Ctrl Pts',(67.3381074112013,-29.0988661172526,12.));
#56851=CARTESIAN_POINT('Ctrl Pts',(67.311801082791,-29.0985610309768,12.));
#56852=CARTESIAN_POINT('Ctrl Pts',(67.2855325866516,-29.0982319644277,12.));
#56853=CARTESIAN_POINT('Ctrl Pts',(67.2593020179216,-29.0978789691965,12.));
#56854=CARTESIAN_POINT('Ctrl Pts',(67.2331094720482,-29.0975020971474,12.));
#56855=CARTESIAN_POINT('Ctrl Pts',(67.2069550447895,-29.0971014004135,12.));
#56856=CARTESIAN_POINT('Ctrl Pts',(67.1808388322116,-29.0966769313893,12.));
#56857=CARTESIAN_POINT('Ctrl Pts',(67.1547609306845,-29.0962287427275,12.));
#56858=CARTESIAN_POINT('Ctrl Pts',(67.1287214368743,-29.0957568873358,12.));
#56859=CARTESIAN_POINT('Ctrl Pts',(67.1027204477304,-29.0952614183778,12.));
#56860=CARTESIAN_POINT('Ctrl Pts',(67.0767580604872,-29.0947423892725,12.));
#56861=CARTESIAN_POINT('Ctrl Pts',(67.0508343726771,-29.0941998536958,12.));
#56862=CARTESIAN_POINT('Ctrl Pts',(67.0249494821361,-29.0936338655828,12.));
#56863=CARTESIAN_POINT('Ctrl Pts',(66.9991034870084,-29.0930444791329,12.));
#56864=CARTESIAN_POINT('Ctrl Pts',(66.9732964857467,-29.092431748817,12.));
#56865=CARTESIAN_POINT('Ctrl Pts',(66.9475285771133,-29.0917957293825,12.));
#56866=CARTESIAN_POINT('Ctrl Pts',(66.9217998601881,-29.0911364758484,12.));
#56867=CARTESIAN_POINT('Ctrl Pts',(66.8961104343703,-29.0904540435064,12.));
#56868=CARTESIAN_POINT('Ctrl Pts',(66.8704603993794,-29.0897484879208,12.));
#56869=CARTESIAN_POINT('Ctrl Pts',(66.8448498552508,-29.0890198649327,12.));
#56870=CARTESIAN_POINT('Ctrl Pts',(66.8192789023323,-29.0882682306636,12.));
#56871=CARTESIAN_POINT('Ctrl Pts',(66.7937476412941,-29.0874936415138,12.));
#56872=CARTESIAN_POINT('Ctrl Pts',(66.7682561731348,-29.086696154163,12.));
#56873=CARTESIAN_POINT('Ctrl Pts',(66.742804599184,-29.0858758255729,12.));
#56874=CARTESIAN_POINT('Ctrl Pts',(66.7173930211015,-29.0850327129914,12.));
#56875=CARTESIAN_POINT('Ctrl Pts',(66.6920215408744,-29.0841668739585,12.));
#56876=CARTESIAN_POINT('Ctrl Pts',(66.6666902608246,-29.0832783663049,12.));
#56877=CARTESIAN_POINT('Ctrl Pts',(66.6413992836148,-29.0823672481508,12.));
#56878=CARTESIAN_POINT('Ctrl Pts',(66.6161487122504,-29.0814335779086,12.));
#56879=CARTESIAN_POINT('Ctrl Pts',(66.5909386500796,-29.0804774142852,12.));
#56880=CARTESIAN_POINT('Ctrl Pts',(66.5657692007894,-29.0794988162892,12.));
#56881=CARTESIAN_POINT('Ctrl Pts',(66.5406404684116,-29.0784978432294,12.));
#56882=CARTESIAN_POINT('Ctrl Pts',(66.5155525573308,-29.0774745547146,12.));
#56883=CARTESIAN_POINT('Ctrl Pts',(66.4905055722864,-29.0764290106553,12.));
#56884=CARTESIAN_POINT('Ctrl Pts',(66.4654996183739,-29.075361271267,12.));
#56885=CARTESIAN_POINT('Ctrl Pts',(66.4405348010404,-29.0742713970763,12.));
#56886=CARTESIAN_POINT('Ctrl Pts',(66.4156112260904,-29.0731594489219,12.));
#56887=CARTESIAN_POINT('Ctrl Pts',(66.3907289996942,-29.0720254879535,12.));
#56888=CARTESIAN_POINT('Ctrl Pts',(66.3658882283906,-29.0708695756336,12.));
#56889=CARTESIAN_POINT('Ctrl Pts',(66.3410890190879,-29.0696917737398,12.));
#56890=CARTESIAN_POINT('Ctrl Pts',(66.3163314790607,-29.0684921443718,12.));
#56891=CARTESIAN_POINT('Ctrl Pts',(66.2916157159527,-29.0672707499527,12.));
#56892=CARTESIAN_POINT('Ctrl Pts',(66.2669418377865,-29.0660276532272,12.));
#56893=CARTESIAN_POINT('Ctrl Pts',(66.2423099529668,-29.0647629172645,12.));
#56894=CARTESIAN_POINT('Ctrl Pts',(66.2177201702819,-29.0634766054599,12.));
#56895=CARTESIAN_POINT('Ctrl Pts',(66.1931725989008,-29.062168781542,12.));
#56896=CARTESIAN_POINT('Ctrl Pts',(66.1686673483755,-29.0608395095746,12.));
#56897=CARTESIAN_POINT('Ctrl Pts',(66.1442045286516,-29.0594888539556,12.));
#56898=CARTESIAN_POINT('Ctrl Pts',(66.1197842500711,-29.058116879419,12.));
#56899=CARTESIAN_POINT('Ctrl Pts',(66.0954066233754,-29.0567236510374,12.));
#56900=CARTESIAN_POINT('Ctrl Pts',(66.0710717597009,-29.0553092342279,12.));
#56901=CARTESIAN_POINT('Ctrl Pts',(66.0467797705815,-29.0538736947552,12.));
#56902=CARTESIAN_POINT('Ctrl Pts',(66.0225307679591,-29.0524170987307,12.));
#56903=CARTESIAN_POINT('Ctrl Pts',(65.9983248641879,-29.0509395126143,12.));
#56904=CARTESIAN_POINT('Ctrl Pts',(65.9741621720369,-29.0494410032173,12.));
#56905=CARTESIAN_POINT('Ctrl Pts',(65.9500428046868,-29.0479216377081,12.));
#56906=CARTESIAN_POINT('Ctrl Pts',(65.9259668757306,-29.0463814836158,12.));
#56907=CARTESIAN_POINT('Ctrl Pts',(65.9019344991854,-29.0448206088289,12.));
#56908=CARTESIAN_POINT('Ctrl Pts',(65.8779457894961,-29.0432390815978,12.));
#56909=CARTESIAN_POINT('Ctrl Pts',(65.854000861539,-29.0416369705376,12.));
#56910=CARTESIAN_POINT('Ctrl Pts',(65.8300998306191,-29.0400143446338,12.));
#56911=CARTESIAN_POINT('Ctrl Pts',(65.8062428124713,-29.0383712732469,12.));
#56912=CARTESIAN_POINT('Ctrl Pts',(65.7824299232705,-29.0367078261103,12.));
#56913=CARTESIAN_POINT('Ctrl Pts',(65.7586612796368,-29.035024073333,12.));
#56914=CARTESIAN_POINT('Ctrl Pts',(65.7349369986384,-29.0333200854028,12.));
#56915=CARTESIAN_POINT('Ctrl Pts',(65.7112571977891,-29.0315959331919,12.));
#56916=CARTESIAN_POINT('Ctrl Pts',(65.6876219950493,-29.0298516879612,12.));
#56917=CARTESIAN_POINT('Ctrl Pts',(65.6640315088388,-29.0280874213596,12.));
#56918=CARTESIAN_POINT('Ctrl Pts',(65.6404858580403,-29.0263032054267,12.));
#56919=CARTESIAN_POINT('Ctrl Pts',(65.6169851620046,-29.0244991125959,12.));
#56920=CARTESIAN_POINT('Ctrl Pts',(65.5935295405453,-29.0226752157003,12.));
#56921=CARTESIAN_POINT('Ctrl Pts',(65.5701191139418,-29.0208315879764,12.));
#56922=CARTESIAN_POINT('Ctrl Pts',(65.5467540029514,-29.0189683030642,12.));
#56923=CARTESIAN_POINT('Ctrl Pts',(65.5234343288136,-29.0170854350095,12.));
#56924=CARTESIAN_POINT('Ctrl Pts',(65.5001602132535,-29.0151830582675,12.));
#56925=CARTESIAN_POINT('Ctrl Pts',(65.4769317784789,-29.013261247709,12.));
#56926=CARTESIAN_POINT('Ctrl Pts',(65.4537491471828,-29.0113200786239,12.));
#56927=CARTESIAN_POINT('Ctrl Pts',(65.4306124425562,-29.0093596267216,12.));
#56928=CARTESIAN_POINT('Ctrl Pts',(65.4075217882934,-29.0073799681342,12.));
#56929=CARTESIAN_POINT('Ctrl Pts',(65.3844773085961,-29.0053811794207,12.));
#56930=CARTESIAN_POINT('Ctrl Pts',(65.3614791281692,-29.003363337573,12.));
#56931=CARTESIAN_POINT('Ctrl Pts',(65.3385273722241,-29.0013265200185,12.));
#56932=CARTESIAN_POINT('Ctrl Pts',(65.3156221664916,-28.9992708046212,12.));
#56933=CARTESIAN_POINT('Ctrl Pts',(65.2927636372253,-28.9971962696845,12.));
#56934=CARTESIAN_POINT('Ctrl Pts',(65.2699519112064,-28.9951029939557,12.));
#56935=CARTESIAN_POINT('Ctrl Pts',(65.2471871157397,-28.9929910566325,12.));
#56936=CARTESIAN_POINT('Ctrl Pts',(65.2244693786609,-28.9908605373663,12.));
#56937=CARTESIAN_POINT('Ctrl Pts',(65.2017988283479,-28.9887115162634,12.));
#56938=CARTESIAN_POINT('Ctrl Pts',(65.1791755937256,-28.9865440738884,12.));
#56939=CARTESIAN_POINT('Ctrl Pts',(65.1565998042697,-28.9843582912693,12.));
#56940=CARTESIAN_POINT('Ctrl Pts',(65.1340715900028,-28.9821542499043,12.));
#56941=CARTESIAN_POINT('Ctrl Pts',(65.1115910815037,-28.9799320317641,12.));
#56942=CARTESIAN_POINT('Ctrl Pts',(65.0891584099168,-28.9776917192933,12.));
#56943=CARTESIAN_POINT('Ctrl Pts',(65.0667737069563,-28.9754333954135,12.));
#56944=CARTESIAN_POINT('Ctrl Pts',(65.0444371049082,-28.9731571435283,12.));
#56945=CARTESIAN_POINT('Ctrl Pts',(65.022148736628,-28.97086304753,12.));
#56946=CARTESIAN_POINT('Ctrl Pts',(64.9999087355504,-28.9685511918019,12.));
#56947=CARTESIAN_POINT('Ctrl Pts',(64.9777172357027,-28.9662216612217,12.));
#56948=CARTESIAN_POINT('Ctrl Pts',(64.9555743717109,-28.9638745411677,12.));
#56949=CARTESIAN_POINT('Ctrl Pts',(64.9334802788038,-28.961509917525,12.));
#56950=CARTESIAN_POINT('Ctrl Pts',(64.9114350928125,-28.9591278766934,12.));
#56951=CARTESIAN_POINT('Ctrl Pts',(64.8894389501801,-28.9567285055867,12.));
#56952=CARTESIAN_POINT('Ctrl Pts',(64.8674919879648,-28.9543118916328,12.));
#56953=CARTESIAN_POINT('Ctrl Pts',(64.8455943438423,-28.9518781227765,12.));
#56954=CARTESIAN_POINT('Ctrl Pts',(64.8237461561018,-28.9494272874832,12.));
#56955=CARTESIAN_POINT('Ctrl Pts',(64.8019475636442,-28.9469594747432,12.));
#56956=CARTESIAN_POINT('Ctrl Pts',(64.7801987060084,-28.944474774081,12.));
#56957=CARTESIAN_POINT('Ctrl Pts',(64.758499723388,-28.9419732755656,12.));
#56958=CARTESIAN_POINT('Ctrl Pts',(64.7368507566467,-28.9394550698204,12.));
#56959=CARTESIAN_POINT('Ctrl Pts',(64.715251947329,-28.9369202480393,12.));
#56960=CARTESIAN_POINT('Ctrl Pts',(64.6937034376617,-28.9343689019882,12.));
#56961=CARTESIAN_POINT('Ctrl Pts',(64.672205370541,-28.9318011239915,12.));
#56962=CARTESIAN_POINT('Ctrl Pts',(64.6507578895161,-28.9292170069222,12.));
#56963=CARTESIAN_POINT('Ctrl Pts',(64.629361138774,-28.9266166441951,12.));
#56964=CARTESIAN_POINT('Ctrl Pts',(64.6080152631039,-28.9240001297542,12.));
#56965=CARTESIAN_POINT('Ctrl Pts',(64.5867204079426,-28.9213675580985,12.));
#56966=CARTESIAN_POINT('Ctrl Pts',(64.5654767194471,-28.9187190243224,12.));
#56967=CARTESIAN_POINT('Ctrl Pts',(64.5442843445559,-28.9160546241538,12.));
#56968=CARTESIAN_POINT('Ctrl Pts',(64.523143431047,-28.9133744539949,12.));
#56969=CARTESIAN_POINT('Ctrl Pts',(64.5020541275951,-28.910678610965,12.));
#56970=CARTESIAN_POINT('Ctrl Pts',(64.4810165836592,-28.9079671928264,12.));
#56971=CARTESIAN_POINT('Ctrl Pts',(64.4600309493583,-28.9052402979062,12.));
#56972=CARTESIAN_POINT('Ctrl Pts',(64.4390973753634,-28.9024980250307,12.));
#56973=CARTESIAN_POINT('Ctrl Pts',(64.4182160127379,-28.899740473434,12.));
#56974=CARTESIAN_POINT('Ctrl Pts',(64.3973870129169,-28.8969677427504,12.));
#56975=CARTESIAN_POINT('Ctrl Pts',(64.3766105280688,-28.89417993323,12.));
#56976=CARTESIAN_POINT('Ctrl Pts',(64.3558867114076,-28.8913771459323,12.));
#56977=CARTESIAN_POINT('Ctrl Pts',(64.3352157174619,-28.8885594828926,12.));
#56978=CARTESIAN_POINT('Ctrl Pts',(64.3145977025037,-28.8857270473959,12.));
#56979=CARTESIAN_POINT('Ctrl Pts',(64.2940328242521,-28.882879943794,12.));
#56980=CARTESIAN_POINT('Ctrl Pts',(64.273521241071,-28.8800182770065,12.));
#56981=CARTESIAN_POINT('Ctrl Pts',(64.2530631112929,-28.877142152106,12.));
#56982=CARTESIAN_POINT('Ctrl Pts',(64.2326585925252,-28.8742516738947,12.));
#56983=CARTESIAN_POINT('Ctrl Pts',(64.2123078408461,-28.8713469464185,12.));
#56984=CARTESIAN_POINT('Ctrl Pts',(64.1920110123299,-28.8684280739014,12.));
#56985=CARTESIAN_POINT('Ctrl Pts',(64.1717682648685,-28.8654951618649,12.));
#56986=CARTESIAN_POINT('Ctrl Pts',(64.1515797596564,-28.8625483180438,12.));
#56987=CARTESIAN_POINT('Ctrl Pts',(64.1314456633381,-28.8595876537148,12.));
#56988=CARTESIAN_POINT('Ctrl Pts',(64.1113661481965,-28.8566132838179,12.));
#56989=CARTESIAN_POINT('Ctrl Pts',(64.0913413876622,-28.8536253241854,12.));
#56990=CARTESIAN_POINT('Ctrl Pts',(64.0713715523599,-28.8506238891093,12.));
#56991=CARTESIAN_POINT('Ctrl Pts',(64.0514568066637,-28.8476090892232,12.));
#56992=CARTESIAN_POINT('Ctrl Pts',(64.0315973031942,-28.844581028125,12.));
#56993=CARTESIAN_POINT('Ctrl Pts',(64.0117931881298,-28.8415398056428,12.));
#56994=CARTESIAN_POINT('Ctrl Pts',(63.9920446117582,-28.8384855243243,12.));
#56995=CARTESIAN_POINT('Ctrl Pts',(63.9723517369614,-28.8354182946601,12.));
#56996=CARTESIAN_POINT('Ctrl Pts',(63.9527147494423,-28.8323382413789,12.));
#56997=CARTESIAN_POINT('Ctrl Pts',(63.9331338646996,-28.829245507756,12.));
#56998=CARTESIAN_POINT('Ctrl Pts',(63.9136093063786,-28.8261402423291,12.));
#56999=CARTESIAN_POINT('Ctrl Pts',(63.8941412856923,-28.823022586318,12.));
#57000=CARTESIAN_POINT('Ctrl Pts',(63.8747299825313,-28.8198926619858,12.));
#57001=CARTESIAN_POINT('Ctrl Pts',(63.8553755207486,-28.8167505576681,12.));
#57002=CARTESIAN_POINT('Ctrl Pts',(63.8360779669856,-28.8135963263369,12.));
#57003=CARTESIAN_POINT('Ctrl Pts',(63.8206854735027,-28.8110632620958,12.));
#57004=CARTESIAN_POINT('Ctrl Pts',(63.8091667271231,-28.8091580239553,12.));
#57005=CARTESIAN_POINT('Ctrl Pts',(63.8014989507494,-28.8078854475432,12.));
#57006=CARTESIAN_POINT('Ctrl Pts',(63.7976679095314,-28.8072485549237,12.));
#57007=CARTESIAN_POINT('Ctrl Pts',(68.8415926175082,-27.6958230985041,-5.55111512312578E-16));
#57008=CARTESIAN_POINT('Ctrl Pts',(68.8415926175082,-27.6958230985041,4.));
#57009=CARTESIAN_POINT('Ctrl Pts',(68.8415926175082,-27.6958230985041,8.));
#57010=CARTESIAN_POINT('Ctrl Pts',(68.8415926175082,-27.6958230985041,12.));
#57011=CARTESIAN_POINT('Ctrl Pts',(68.9176987693914,-27.7750822307,-5.55111512312578E-16));
#57012=CARTESIAN_POINT('Ctrl Pts',(68.9176987693914,-27.7750822307,4.));
#57013=CARTESIAN_POINT('Ctrl Pts',(68.9176987693914,-27.7750822307,8.));
#57014=CARTESIAN_POINT('Ctrl Pts',(68.9176987693914,-27.7750822307,12.));
#57015=CARTESIAN_POINT('Ctrl Pts',(69.0029745467582,-27.9589320265197,-5.55111512312578E-16));
#57016=CARTESIAN_POINT('Ctrl Pts',(69.0029745467582,-27.9589320265197,4.00000000000001));
#57017=CARTESIAN_POINT('Ctrl Pts',(69.0029745467582,-27.9589320265197,7.99999999999999));
#57018=CARTESIAN_POINT('Ctrl Pts',(69.0029745467582,-27.9589320265197,12.));
#57019=CARTESIAN_POINT('Ctrl Pts',(68.9748773050761,-28.1553386138883,-5.55111512312578E-16));
#57020=CARTESIAN_POINT('Ctrl Pts',(68.9748773050761,-28.1553386138883,4.));
#57021=CARTESIAN_POINT('Ctrl Pts',(68.9748773050761,-28.1553386138883,8.00000000000001));
#57022=CARTESIAN_POINT('Ctrl Pts',(68.9748773050761,-28.1553386138883,12.));
#57023=CARTESIAN_POINT('Ctrl Pts',(68.9436475237615,-28.2316040302245,-5.55111512312578E-16));
#57024=CARTESIAN_POINT('Ctrl Pts',(68.9436475237615,-28.2316040302245,4.));
#57025=CARTESIAN_POINT('Ctrl Pts',(68.9436475237615,-28.2316040302245,8.));
#57026=CARTESIAN_POINT('Ctrl Pts',(68.9436475237615,-28.2316040302245,12.));
#57027=CARTESIAN_POINT('',(68.8415926175082,-27.6958230985041,0.));
#57028=CARTESIAN_POINT('',(68.9436475237612,-28.2316040302243,0.));
#57029=CARTESIAN_POINT('Ctrl Pts',(68.8415926175082,-27.6958230985041,-5.55111512312578E-16));
#57030=CARTESIAN_POINT('Ctrl Pts',(68.9176987693914,-27.7750822307,-5.55111512312578E-16));
#57031=CARTESIAN_POINT('Ctrl Pts',(68.9664277850296,-27.8801392568827,-5.55111512312578E-16));
#57032=CARTESIAN_POINT('Ctrl Pts',(68.9781370393457,-27.9892964598977,-5.55111512312578E-16));
#57033=CARTESIAN_POINT('Ctrl Pts',(68.9869189800827,-28.0711643621589,-5.55111512312578E-16));
#57034=CARTESIAN_POINT('Ctrl Pts',(68.9748773050761,-28.1553386138883,-5.55111512312578E-16));
#57035=CARTESIAN_POINT('Ctrl Pts',(68.9436475237615,-28.2316040302245,-5.55111512312578E-16));
#57036=CARTESIAN_POINT('',(68.9436475237612,-28.2316040302243,12.));
#57037=CARTESIAN_POINT('Ctrl Pts',(68.9436475237615,-28.2316040302245,-5.55111512312578E-16));
#57038=CARTESIAN_POINT('Ctrl Pts',(68.9436475237615,-28.2316040302245,4.));
#57039=CARTESIAN_POINT('Ctrl Pts',(68.9436475237615,-28.2316040302245,8.));
#57040=CARTESIAN_POINT('Ctrl Pts',(68.9436475237615,-28.2316040302245,12.));
#57041=CARTESIAN_POINT('',(68.8415926175082,-27.6958230985041,12.));
#57042=CARTESIAN_POINT('Ctrl Pts',(68.9436475237615,-28.2316040302245,12.));
#57043=CARTESIAN_POINT('Ctrl Pts',(68.9748773050761,-28.1553386138883,12.));
#57044=CARTESIAN_POINT('Ctrl Pts',(68.9869189800827,-28.0711643621589,12.));
#57045=CARTESIAN_POINT('Ctrl Pts',(68.9781370393457,-27.9892964598977,12.));
#57046=CARTESIAN_POINT('Ctrl Pts',(68.9664277850296,-27.8801392568827,12.));
#57047=CARTESIAN_POINT('Ctrl Pts',(68.9176987693914,-27.7750822307,12.));
#57048=CARTESIAN_POINT('Ctrl Pts',(68.8415926175082,-27.6958230985041,12.));
#57049=CARTESIAN_POINT('Ctrl Pts',(68.8415926175082,-27.6958230985041,12.));
#57050=CARTESIAN_POINT('Ctrl Pts',(68.8415926175082,-27.6958230985041,8.));
#57051=CARTESIAN_POINT('Ctrl Pts',(68.8415926175082,-27.6958230985041,4.));
#57052=CARTESIAN_POINT('Ctrl Pts',(68.8415926175082,-27.6958230985041,-5.55111512312578E-16));
#57053=CARTESIAN_POINT('Origin',(3.4634846687719E-10,-1.43354795624835E-10,
0.));
#57054=CARTESIAN_POINT('Origin',(3.4634846687719E-10,-1.43354795624835E-10,
12.));
#57055=CARTESIAN_POINT('Origin',(3.4634846687719E-10,-1.43354795624835E-10,
0.));
#57056=CARTESIAN_POINT('Ctrl Pts',(65.9427857825597,-34.6669728017237,-5.55111512312578E-16));
#57057=CARTESIAN_POINT('Ctrl Pts',(65.9427857825597,-34.6669728017237,4.));
#57058=CARTESIAN_POINT('Ctrl Pts',(65.9427857825597,-34.6669728017237,8.));
#57059=CARTESIAN_POINT('Ctrl Pts',(65.9427857825597,-34.6669728017237,12.));
#57060=CARTESIAN_POINT('Ctrl Pts',(65.8916543400169,-34.7642339552035,-5.55111512312578E-16));
#57061=CARTESIAN_POINT('Ctrl Pts',(65.8916543400169,-34.7642339552035,4.));
#57062=CARTESIAN_POINT('Ctrl Pts',(65.8916543400169,-34.7642339552036,8.));
#57063=CARTESIAN_POINT('Ctrl Pts',(65.8916543400169,-34.7642339552036,12.));
#57064=CARTESIAN_POINT('Ctrl Pts',(65.7441961270804,-34.9032616822024,-5.55111512312578E-16));
#57065=CARTESIAN_POINT('Ctrl Pts',(65.7441961270804,-34.9032616822024,4.));
#57066=CARTESIAN_POINT('Ctrl Pts',(65.7441961270804,-34.9032616822024,8.));
#57067=CARTESIAN_POINT('Ctrl Pts',(65.7441961270804,-34.9032616822024,12.));
#57068=CARTESIAN_POINT('Ctrl Pts',(65.5489812297286,-34.9387029822717,-5.55111512312578E-16));
#57069=CARTESIAN_POINT('Ctrl Pts',(65.5489812297286,-34.9387029822717,4.));
#57070=CARTESIAN_POINT('Ctrl Pts',(65.5489812297286,-34.9387029822717,8.));
#57071=CARTESIAN_POINT('Ctrl Pts',(65.5489812297286,-34.9387029822717,12.));
#57072=CARTESIAN_POINT('Ctrl Pts',(65.4667541477954,-34.9331875523087,-5.55111512312578E-16));
#57073=CARTESIAN_POINT('Ctrl Pts',(65.4667541477954,-34.9331875523087,4.));
#57074=CARTESIAN_POINT('Ctrl Pts',(65.4667541477954,-34.9331875523087,8.));
#57075=CARTESIAN_POINT('Ctrl Pts',(65.4667541477954,-34.9331875523087,12.));
#57076=CARTESIAN_POINT('',(65.9427857825597,-34.6669728017237,0.));
#57077=CARTESIAN_POINT('',(65.4667541477955,-34.9331875523085,2.77555756156289E-16));
#57078=CARTESIAN_POINT('Ctrl Pts',(65.9427857825597,-34.6669728017237,-1.38777878078145E-16));
#57079=CARTESIAN_POINT('Ctrl Pts',(65.8916543400169,-34.7642339552035,-1.38777878078145E-16));
#57080=CARTESIAN_POINT('Ctrl Pts',(65.8073925040532,-34.8436783706315,-1.38777878078144E-16));
#57081=CARTESIAN_POINT('Ctrl Pts',(65.7075366486885,-34.8892986466538,-1.38777878078145E-16));
#57082=CARTESIAN_POINT('Ctrl Pts',(65.6326447571651,-34.9235138536706,-1.38777878078145E-16));
#57083=CARTESIAN_POINT('Ctrl Pts',(65.5489812297286,-34.9387029822717,-1.38777878078145E-16));
#57084=CARTESIAN_POINT('Ctrl Pts',(65.4667541477954,-34.9331875523087,-1.38777878078145E-16));
#57085=CARTESIAN_POINT('',(65.4667541477955,-34.9331875523085,12.));
#57086=CARTESIAN_POINT('Ctrl Pts',(65.4667541477954,-34.9331875523087,-5.55111512312578E-16));
#57087=CARTESIAN_POINT('Ctrl Pts',(65.4667541477954,-34.9331875523087,4.));
#57088=CARTESIAN_POINT('Ctrl Pts',(65.4667541477954,-34.9331875523087,8.));
#57089=CARTESIAN_POINT('Ctrl Pts',(65.4667541477954,-34.9331875523087,12.));
#57090=CARTESIAN_POINT('',(65.9427857825597,-34.6669728017237,12.));
#57091=CARTESIAN_POINT('Ctrl Pts',(65.4667541477954,-34.9331875523087,12.));
#57092=CARTESIAN_POINT('Ctrl Pts',(65.5489812297286,-34.9387029822717,12.));
#57093=CARTESIAN_POINT('Ctrl Pts',(65.6326447571651,-34.9235138536706,12.));
#57094=CARTESIAN_POINT('Ctrl Pts',(65.7075366486885,-34.8892986466538,12.));
#57095=CARTESIAN_POINT('Ctrl Pts',(65.8073925040532,-34.8436783706315,12.));
#57096=CARTESIAN_POINT('Ctrl Pts',(65.8916543400169,-34.7642339552036,12.));
#57097=CARTESIAN_POINT('Ctrl Pts',(65.9427857825597,-34.6669728017237,12.));
#57098=CARTESIAN_POINT('Ctrl Pts',(65.9427857825597,-34.6669728017237,12.));
#57099=CARTESIAN_POINT('Ctrl Pts',(65.9427857825597,-34.6669728017237,8.));
#57100=CARTESIAN_POINT('Ctrl Pts',(65.9427857825597,-34.6669728017237,4.));
#57101=CARTESIAN_POINT('Ctrl Pts',(65.9427857825597,-34.6669728017237,-5.55111512312578E-16));
#57102=CARTESIAN_POINT('Ctrl Pts',(61.0441813777723,-34.2579614092497,0.));
#57103=CARTESIAN_POINT('Ctrl Pts',(61.0441813777723,-34.2579614092497,12.));
#57104=CARTESIAN_POINT('Ctrl Pts',(61.0479423318725,-34.2589297755434,0.));
#57105=CARTESIAN_POINT('Ctrl Pts',(61.0479423318725,-34.2589297755434,12.));
#57106=CARTESIAN_POINT('Ctrl Pts',(61.0554700176998,-34.2608658001631,0.));
#57107=CARTESIAN_POINT('Ctrl Pts',(61.0554700176998,-34.2608658001631,12.));
#57108=CARTESIAN_POINT('Ctrl Pts',(61.0667788793266,-34.2637677131935,0.));
#57109=CARTESIAN_POINT('Ctrl Pts',(61.0667788793266,-34.2637677131935,12.));
#57110=CARTESIAN_POINT('Ctrl Pts',(61.0818920286293,-34.2676326825626,0.));
#57111=CARTESIAN_POINT('Ctrl Pts',(61.0818920286293,-34.2676326825626,12.));
#57112=CARTESIAN_POINT('Ctrl Pts',(61.1008412399997,-34.2724568037228,0.));
#57113=CARTESIAN_POINT('Ctrl Pts',(61.1008412399997,-34.2724568037228,12.));
#57114=CARTESIAN_POINT('Ctrl Pts',(61.1198481997764,-34.2772738038771,0.));
#57115=CARTESIAN_POINT('Ctrl Pts',(61.1198481997764,-34.2772738038771,12.));
#57116=CARTESIAN_POINT('Ctrl Pts',(61.1389128461885,-34.282083624447,0.));
#57117=CARTESIAN_POINT('Ctrl Pts',(61.1389128461885,-34.282083624447,12.));
#57118=CARTESIAN_POINT('Ctrl Pts',(61.1580350635532,-34.2868861666384,0.));
#57119=CARTESIAN_POINT('Ctrl Pts',(61.1580350635532,-34.2868861666384,12.));
#57120=CARTESIAN_POINT('Ctrl Pts',(61.1772146833205,-34.2916812929751,0.));
#57121=CARTESIAN_POINT('Ctrl Pts',(61.1772146833205,-34.2916812929751,12.));
#57122=CARTESIAN_POINT('Ctrl Pts',(61.1964515073891,-34.2964688443663,0.));
#57123=CARTESIAN_POINT('Ctrl Pts',(61.1964515073891,-34.2964688443663,12.));
#57124=CARTESIAN_POINT('Ctrl Pts',(61.2157453259107,-34.3012486533474,0.));
#57125=CARTESIAN_POINT('Ctrl Pts',(61.2157453259107,-34.3012486533474,12.));
#57126=CARTESIAN_POINT('Ctrl Pts',(61.2350959366939,-34.3060205584065,0.));
#57127=CARTESIAN_POINT('Ctrl Pts',(61.2350959366939,-34.3060205584065,12.));
#57128=CARTESIAN_POINT('Ctrl Pts',(61.2545031656133,-34.3107844191044,0.));
#57129=CARTESIAN_POINT('Ctrl Pts',(61.2545031656133,-34.3107844191044,12.));
#57130=CARTESIAN_POINT('Ctrl Pts',(61.2739668600365,-34.3155401111747,0.));
#57131=CARTESIAN_POINT('Ctrl Pts',(61.2739668600365,-34.3155401111747,12.));
#57132=CARTESIAN_POINT('Ctrl Pts',(61.2934868791854,-34.3202875193618,0.));
#57133=CARTESIAN_POINT('Ctrl Pts',(61.2934868791854,-34.3202875193618,12.));
#57134=CARTESIAN_POINT('Ctrl Pts',(61.3130630861386,-34.3250265314768,0.));
#57135=CARTESIAN_POINT('Ctrl Pts',(61.3130630861386,-34.3250265314768,12.));
#57136=CARTESIAN_POINT('Ctrl Pts',(61.3326953378851,-34.3297570310146,0.));
#57137=CARTESIAN_POINT('Ctrl Pts',(61.3326953378851,-34.3297570310146,12.));
#57138=CARTESIAN_POINT('Ctrl Pts',(61.3523834803188,-34.3344788934363,0.));
#57139=CARTESIAN_POINT('Ctrl Pts',(61.3523834803188,-34.3344788934363,12.));
#57140=CARTESIAN_POINT('Ctrl Pts',(61.3721273534256,-34.339191990014,0.));
#57141=CARTESIAN_POINT('Ctrl Pts',(61.3721273534256,-34.339191990014,12.));
#57142=CARTESIAN_POINT('Ctrl Pts',(61.3919267945302,-34.3438961902405,0.));
#57143=CARTESIAN_POINT('Ctrl Pts',(61.3919267945302,-34.3438961902405,12.));
#57144=CARTESIAN_POINT('Ctrl Pts',(61.4117816420228,-34.3485913645979,0.));
#57145=CARTESIAN_POINT('Ctrl Pts',(61.4117816420228,-34.3485913645979,12.));
#57146=CARTESIAN_POINT('Ctrl Pts',(61.4316917395918,-34.3532773877089,0.));
#57147=CARTESIAN_POINT('Ctrl Pts',(61.4316917395918,-34.3532773877089,12.));
#57148=CARTESIAN_POINT('Ctrl Pts',(61.4516569360454,-34.3579541381996,0.));
#57149=CARTESIAN_POINT('Ctrl Pts',(61.4516569360454,-34.3579541381996,12.));
#57150=CARTESIAN_POINT('Ctrl Pts',(61.4716770832896,-34.3626214971889,0.));
#57151=CARTESIAN_POINT('Ctrl Pts',(61.4716770832896,-34.3626214971889,12.));
#57152=CARTESIAN_POINT('Ctrl Pts',(61.4917520349278,-34.3672793472466,0.));
#57153=CARTESIAN_POINT('Ctrl Pts',(61.4917520349278,-34.3672793472466,12.));
#57154=CARTESIAN_POINT('Ctrl Pts',(61.5118816445437,-34.3719275711195,0.));
#57155=CARTESIAN_POINT('Ctrl Pts',(61.5118816445437,-34.3719275711195,12.));
#57156=CARTESIAN_POINT('Ctrl Pts',(61.5320657642638,-34.376566050668,0.));
#57157=CARTESIAN_POINT('Ctrl Pts',(61.5320657642638,-34.376566050668,12.));
#57158=CARTESIAN_POINT('Ctrl Pts',(61.5523042455158,-34.3811946674197,0.));
#57159=CARTESIAN_POINT('Ctrl Pts',(61.5523042455158,-34.3811946674197,12.));
#57160=CARTESIAN_POINT('Ctrl Pts',(61.5725969396829,-34.3858133030518,0.));
#57161=CARTESIAN_POINT('Ctrl Pts',(61.5725969396829,-34.3858133030518,12.));
#57162=CARTESIAN_POINT('Ctrl Pts',(61.5929436987409,-34.3904218398637,0.));
#57163=CARTESIAN_POINT('Ctrl Pts',(61.5929436987409,-34.3904218398637,12.));
#57164=CARTESIAN_POINT('Ctrl Pts',(61.6133443760142,-34.3950201613432,0.));
#57165=CARTESIAN_POINT('Ctrl Pts',(61.6133443760142,-34.3950201613432,12.));
#57166=CARTESIAN_POINT('Ctrl Pts',(61.6337988264556,-34.3996081523753,0.));
#57167=CARTESIAN_POINT('Ctrl Pts',(61.6337988264556,-34.3996081523753,12.));
#57168=CARTESIAN_POINT('Ctrl Pts',(61.6543069062416,-34.4041856989317,0.));
#57169=CARTESIAN_POINT('Ctrl Pts',(61.6543069062416,-34.4041856989317,12.));
#57170=CARTESIAN_POINT('Ctrl Pts',(61.6748684725205,-34.4087526878812,0.));
#57171=CARTESIAN_POINT('Ctrl Pts',(61.6748684725205,-34.4087526878812,12.));
#57172=CARTESIAN_POINT('Ctrl Pts',(61.695483383117,-34.4133090067704,0.));
#57173=CARTESIAN_POINT('Ctrl Pts',(61.695483383117,-34.4133090067704,12.));
#57174=CARTESIAN_POINT('Ctrl Pts',(61.7161514961914,-34.4178545435767,0.));
#57175=CARTESIAN_POINT('Ctrl Pts',(61.7161514961914,-34.4178545435767,12.));
#57176=CARTESIAN_POINT('Ctrl Pts',(61.7368726702596,-34.422389186718,0.));
#57177=CARTESIAN_POINT('Ctrl Pts',(61.7368726702596,-34.422389186718,12.));
#57178=CARTESIAN_POINT('Ctrl Pts',(61.7576467643432,-34.4269128251577,0.));
#57179=CARTESIAN_POINT('Ctrl Pts',(61.7576467643432,-34.4269128251577,12.));
#57180=CARTESIAN_POINT('Ctrl Pts',(61.7784736380727,-34.4314253484792,0.));
#57181=CARTESIAN_POINT('Ctrl Pts',(61.7784736380727,-34.4314253484792,12.));
#57182=CARTESIAN_POINT('Ctrl Pts',(61.7993531518036,-34.4359266469749,0.));
#57183=CARTESIAN_POINT('Ctrl Pts',(61.7993531518036,-34.4359266469749,12.));
#57184=CARTESIAN_POINT('Ctrl Pts',(61.8202851667222,-34.4404166117299,0.));
#57185=CARTESIAN_POINT('Ctrl Pts',(61.8202851667222,-34.4404166117299,12.));
#57186=CARTESIAN_POINT('Ctrl Pts',(61.8412695447926,-34.444895134574,0.));
#57187=CARTESIAN_POINT('Ctrl Pts',(61.8412695447926,-34.444895134574,12.));
#57188=CARTESIAN_POINT('Ctrl Pts',(61.8623061487018,-34.4493621080361,0.));
#57189=CARTESIAN_POINT('Ctrl Pts',(61.8623061487018,-34.4493621080361,12.));
#57190=CARTESIAN_POINT('Ctrl Pts',(61.8833948418025,-34.4538174253012,0.));
#57191=CARTESIAN_POINT('Ctrl Pts',(61.8833948418025,-34.4538174253012,12.));
#57192=CARTESIAN_POINT('Ctrl Pts',(61.9045354880444,-34.4582609801637,0.));
#57193=CARTESIAN_POINT('Ctrl Pts',(61.9045354880444,-34.4582609801637,12.));
#57194=CARTESIAN_POINT('Ctrl Pts',(61.9257279519308,-34.4626926669975,0.));
#57195=CARTESIAN_POINT('Ctrl Pts',(61.9257279519308,-34.4626926669975,12.));
#57196=CARTESIAN_POINT('Ctrl Pts',(61.9469720985531,-34.4671123807717,0.));
#57197=CARTESIAN_POINT('Ctrl Pts',(61.9469720985531,-34.4671123807717,12.));
#57198=CARTESIAN_POINT('Ctrl Pts',(61.9682677936053,-34.4715200170592,0.));
#57199=CARTESIAN_POINT('Ctrl Pts',(61.9682677936053,-34.4715200170592,12.));
#57200=CARTESIAN_POINT('Ctrl Pts',(61.9896149034001,-34.4759154720473,0.));
#57201=CARTESIAN_POINT('Ctrl Pts',(61.9896149034001,-34.4759154720473,12.));
#57202=CARTESIAN_POINT('Ctrl Pts',(62.0110132948794,-34.4802986425528,0.));
#57203=CARTESIAN_POINT('Ctrl Pts',(62.0110132948794,-34.4802986425528,12.));
#57204=CARTESIAN_POINT('Ctrl Pts',(62.0324628356141,-34.48466942602,0.));
#57205=CARTESIAN_POINT('Ctrl Pts',(62.0324628356141,-34.48466942602,12.));
#57206=CARTESIAN_POINT('Ctrl Pts',(62.0539633937939,-34.489027720504,0.));
#57207=CARTESIAN_POINT('Ctrl Pts',(62.0539633937939,-34.489027720504,12.));
#57208=CARTESIAN_POINT('Ctrl Pts',(62.0755148382135,-34.4933734246593,0.));
#57209=CARTESIAN_POINT('Ctrl Pts',(62.0755148382135,-34.4933734246593,12.));
#57210=CARTESIAN_POINT('Ctrl Pts',(62.0971170382567,-34.4977064377282,0.));
#57211=CARTESIAN_POINT('Ctrl Pts',(62.0971170382567,-34.4977064377282,12.));
#57212=CARTESIAN_POINT('Ctrl Pts',(62.1187698638707,-34.5020266595293,0.));
#57213=CARTESIAN_POINT('Ctrl Pts',(62.1187698638707,-34.5020266595293,12.));
#57214=CARTESIAN_POINT('Ctrl Pts',(62.1404731855687,-34.5063339904533,0.));
#57215=CARTESIAN_POINT('Ctrl Pts',(62.1404731855687,-34.5063339904533,12.));
#57216=CARTESIAN_POINT('Ctrl Pts',(62.1622268744337,-34.5106283314594,0.));
#57217=CARTESIAN_POINT('Ctrl Pts',(62.1622268744337,-34.5106283314594,12.));
#57218=CARTESIAN_POINT('Ctrl Pts',(62.184030802117,-34.514909584073,0.));
#57219=CARTESIAN_POINT('Ctrl Pts',(62.184030802117,-34.514909584073,12.));
#57220=CARTESIAN_POINT('Ctrl Pts',(62.2058848408346,-34.5191776503843,0.));
#57221=CARTESIAN_POINT('Ctrl Pts',(62.2058848408346,-34.5191776503843,12.));
#57222=CARTESIAN_POINT('Ctrl Pts',(62.2277888633576,-34.5234324330492,0.));
#57223=CARTESIAN_POINT('Ctrl Pts',(62.2277888633576,-34.5234324330492,12.));
#57224=CARTESIAN_POINT('Ctrl Pts',(62.2497427430136,-34.527673835281,0.));
#57225=CARTESIAN_POINT('Ctrl Pts',(62.2497427430136,-34.527673835281,12.));
#57226=CARTESIAN_POINT('Ctrl Pts',(62.2717463536828,-34.5319017608435,0.));
#57227=CARTESIAN_POINT('Ctrl Pts',(62.2717463536828,-34.5319017608435,12.));
#57228=CARTESIAN_POINT('Ctrl Pts',(62.2937995697927,-34.536116114045,0.));
#57229=CARTESIAN_POINT('Ctrl Pts',(62.2937995697927,-34.536116114045,12.));
#57230=CARTESIAN_POINT('Ctrl Pts',(62.3159022663052,-34.5403167997333,0.));
#57231=CARTESIAN_POINT('Ctrl Pts',(62.3159022663052,-34.5403167997333,12.));
#57232=CARTESIAN_POINT('Ctrl Pts',(62.3380543187067,-34.5445037232928,0.));
#57233=CARTESIAN_POINT('Ctrl Pts',(62.3380543187067,-34.5445037232928,12.));
#57234=CARTESIAN_POINT('Ctrl Pts',(62.3602556030114,-34.5486767906376,0.));
#57235=CARTESIAN_POINT('Ctrl Pts',(62.3602556030114,-34.5486767906376,12.));
#57236=CARTESIAN_POINT('Ctrl Pts',(62.3825059957593,-34.552835908207,0.));
#57237=CARTESIAN_POINT('Ctrl Pts',(62.3825059957593,-34.552835908207,12.));
#57238=CARTESIAN_POINT('Ctrl Pts',(62.4048053740129,-34.5569809829615,0.));
#57239=CARTESIAN_POINT('Ctrl Pts',(62.4048053740129,-34.5569809829615,12.));
#57240=CARTESIAN_POINT('Ctrl Pts',(62.4271536153473,-34.5611119223807,0.));
#57241=CARTESIAN_POINT('Ctrl Pts',(62.4271536153473,-34.5611119223807,12.));
#57242=CARTESIAN_POINT('Ctrl Pts',(62.4495505978415,-34.5652286344606,0.));
#57243=CARTESIAN_POINT('Ctrl Pts',(62.4495505978415,-34.5652286344606,12.));
#57244=CARTESIAN_POINT('Ctrl Pts',(62.4719962000829,-34.5693310277064,0.));
#57245=CARTESIAN_POINT('Ctrl Pts',(62.4719962000829,-34.5693310277064,12.));
#57246=CARTESIAN_POINT('Ctrl Pts',(62.494490301164,-34.5734190111279,0.));
#57247=CARTESIAN_POINT('Ctrl Pts',(62.494490301164,-34.5734190111279,12.));
#57248=CARTESIAN_POINT('Ctrl Pts',(62.5170327806774,-34.5774924942351,0.));
#57249=CARTESIAN_POINT('Ctrl Pts',(62.5170327806774,-34.5774924942351,12.));
#57250=CARTESIAN_POINT('Ctrl Pts',(62.5396235187053,-34.5815513870363,0.));
#57251=CARTESIAN_POINT('Ctrl Pts',(62.5396235187053,-34.5815513870363,12.));
#57252=CARTESIAN_POINT('Ctrl Pts',(62.5622623958125,-34.5855956000344,0.));
#57253=CARTESIAN_POINT('Ctrl Pts',(62.5622623958125,-34.5855956000344,12.));
#57254=CARTESIAN_POINT('Ctrl Pts',(62.5849492930501,-34.5896250442199,0.));
#57255=CARTESIAN_POINT('Ctrl Pts',(62.5849492930501,-34.5896250442199,12.));
#57256=CARTESIAN_POINT('Ctrl Pts',(62.6076840919521,-34.5936396310671,0.));
#57257=CARTESIAN_POINT('Ctrl Pts',(62.6076840919521,-34.5936396310671,12.));
#57258=CARTESIAN_POINT('Ctrl Pts',(62.6304666745319,-34.5976392725303,0.));
#57259=CARTESIAN_POINT('Ctrl Pts',(62.6304666745319,-34.5976392725303,12.));
#57260=CARTESIAN_POINT('Ctrl Pts',(62.6532969232695,-34.6016238810419,0.));
#57261=CARTESIAN_POINT('Ctrl Pts',(62.6532969232695,-34.6016238810419,12.));
#57262=CARTESIAN_POINT('Ctrl Pts',(62.6761747211081,-34.6055933695093,0.));
#57263=CARTESIAN_POINT('Ctrl Pts',(62.6761747211081,-34.6055933695093,12.));
#57264=CARTESIAN_POINT('Ctrl Pts',(62.6990999514597,-34.6095476513095,0.));
#57265=CARTESIAN_POINT('Ctrl Pts',(62.6990999514597,-34.6095476513095,12.));
#57266=CARTESIAN_POINT('Ctrl Pts',(62.7220724982005,-34.6134866402842,0.));
#57267=CARTESIAN_POINT('Ctrl Pts',(62.7220724982005,-34.6134866402842,12.));
#57268=CARTESIAN_POINT('Ctrl Pts',(62.7450922456662,-34.6174102507368,0.));
#57269=CARTESIAN_POINT('Ctrl Pts',(62.7450922456662,-34.6174102507368,12.));
#57270=CARTESIAN_POINT('Ctrl Pts',(62.7681590786398,-34.6213183974303,0.));
#57271=CARTESIAN_POINT('Ctrl Pts',(62.7681590786398,-34.6213183974303,12.));
#57272=CARTESIAN_POINT('Ctrl Pts',(62.7912728823482,-34.6252109955836,0.));
#57273=CARTESIAN_POINT('Ctrl Pts',(62.7912728823482,-34.6252109955836,12.));
#57274=CARTESIAN_POINT('Ctrl Pts',(62.8144335424671,-34.629087960866,0.));
#57275=CARTESIAN_POINT('Ctrl Pts',(62.8144335424671,-34.629087960866,12.));
#57276=CARTESIAN_POINT('Ctrl Pts',(62.8376409451167,-34.6329492093932,0.));
#57277=CARTESIAN_POINT('Ctrl Pts',(62.8376409451167,-34.6329492093932,12.));
#57278=CARTESIAN_POINT('Ctrl Pts',(62.8608949768583,-34.6367946577241,0.));
#57279=CARTESIAN_POINT('Ctrl Pts',(62.8608949768583,-34.6367946577241,12.));
#57280=CARTESIAN_POINT('Ctrl Pts',(62.8841955246819,-34.6406242228606,0.));
#57281=CARTESIAN_POINT('Ctrl Pts',(62.8841955246819,-34.6406242228606,12.));
#57282=CARTESIAN_POINT('Ctrl Pts',(62.9075424760042,-34.6444378222425,0.));
#57283=CARTESIAN_POINT('Ctrl Pts',(62.9075424760042,-34.6444378222425,12.));
#57284=CARTESIAN_POINT('Ctrl Pts',(62.9309357186733,-34.6482353737434,0.));
#57285=CARTESIAN_POINT('Ctrl Pts',(62.9309357186733,-34.6482353737434,12.));
#57286=CARTESIAN_POINT('Ctrl Pts',(62.9543751409647,-34.6520167956657,0.));
#57287=CARTESIAN_POINT('Ctrl Pts',(62.9543751409647,-34.6520167956657,12.));
#57288=CARTESIAN_POINT('Ctrl Pts',(62.9778606315777,-34.655782006739,0.));
#57289=CARTESIAN_POINT('Ctrl Pts',(62.9778606315777,-34.655782006739,12.));
#57290=CARTESIAN_POINT('Ctrl Pts',(63.0013920796225,-34.6595309261186,0.));
#57291=CARTESIAN_POINT('Ctrl Pts',(63.0013920796225,-34.6595309261186,12.));
#57292=CARTESIAN_POINT('Ctrl Pts',(63.0249693746198,-34.6632634733819,0.));
#57293=CARTESIAN_POINT('Ctrl Pts',(63.0249693746198,-34.6632634733819,12.));
#57294=CARTESIAN_POINT('Ctrl Pts',(63.0485924065039,-34.6669795685225,0.));
#57295=CARTESIAN_POINT('Ctrl Pts',(63.0485924065039,-34.6669795685225,12.));
#57296=CARTESIAN_POINT('Ctrl Pts',(63.0722610656194,-34.6706791319471,0.));
#57297=CARTESIAN_POINT('Ctrl Pts',(63.0722610656194,-34.6706791319471,12.));
#57298=CARTESIAN_POINT('Ctrl Pts',(63.0959752427169,-34.6743620844722,0.));
#57299=CARTESIAN_POINT('Ctrl Pts',(63.0959752427169,-34.6743620844722,12.));
#57300=CARTESIAN_POINT('Ctrl Pts',(63.119734828943,-34.6780283473252,0.));
#57301=CARTESIAN_POINT('Ctrl Pts',(63.119734828943,-34.6780283473252,12.));
#57302=CARTESIAN_POINT('Ctrl Pts',(63.1435397158385,-34.6816778421401,0.));
#57303=CARTESIAN_POINT('Ctrl Pts',(63.1435397158385,-34.6816778421401,12.));
#57304=CARTESIAN_POINT('Ctrl Pts',(63.1673897953425,-34.6853104909516,0.));
#57305=CARTESIAN_POINT('Ctrl Pts',(63.1673897953425,-34.6853104909516,12.));
#57306=CARTESIAN_POINT('Ctrl Pts',(63.1912849597885,-34.6889262161923,0.));
#57307=CARTESIAN_POINT('Ctrl Pts',(63.1912849597885,-34.6889262161923,12.));
#57308=CARTESIAN_POINT('Ctrl Pts',(63.2152251019014,-34.6925249406899,0.));
#57309=CARTESIAN_POINT('Ctrl Pts',(63.2152251019014,-34.6925249406899,12.));
#57310=CARTESIAN_POINT('Ctrl Pts',(63.2392101147853,-34.6961065876671,0.));
#57311=CARTESIAN_POINT('Ctrl Pts',(63.2392101147853,-34.6961065876671,12.));
#57312=CARTESIAN_POINT('Ctrl Pts',(63.2632398919234,-34.6996710807384,0.));
#57313=CARTESIAN_POINT('Ctrl Pts',(63.2632398919234,-34.6996710807384,12.));
#57314=CARTESIAN_POINT('Ctrl Pts',(63.2873143271812,-34.7032183439045,0.));
#57315=CARTESIAN_POINT('Ctrl Pts',(63.2873143271812,-34.7032183439045,12.));
#57316=CARTESIAN_POINT('Ctrl Pts',(63.311433314805,-34.7067483015492,0.));
#57317=CARTESIAN_POINT('Ctrl Pts',(63.311433314805,-34.7067483015492,12.));
#57318=CARTESIAN_POINT('Ctrl Pts',(63.3355967494169,-34.7102608784373,0.));
#57319=CARTESIAN_POINT('Ctrl Pts',(63.3355967494169,-34.7102608784373,12.));
#57320=CARTESIAN_POINT('Ctrl Pts',(63.3598045260049,-34.7137559997143,0.));
#57321=CARTESIAN_POINT('Ctrl Pts',(63.3598045260049,-34.7137559997143,12.));
#57322=CARTESIAN_POINT('Ctrl Pts',(63.3840565399206,-34.7172335909037,0.));
#57323=CARTESIAN_POINT('Ctrl Pts',(63.3840565399206,-34.7172335909037,12.));
#57324=CARTESIAN_POINT('Ctrl Pts',(63.4083526868837,-34.7206935779007,0.));
#57325=CARTESIAN_POINT('Ctrl Pts',(63.4083526868837,-34.7206935779007,12.));
#57326=CARTESIAN_POINT('Ctrl Pts',(63.4326928629796,-34.7241358869702,0.));
#57327=CARTESIAN_POINT('Ctrl Pts',(63.4326928629796,-34.7241358869702,12.));
#57328=CARTESIAN_POINT('Ctrl Pts',(63.4570769646568,-34.7275604447439,0.));
#57329=CARTESIAN_POINT('Ctrl Pts',(63.4570769646568,-34.7275604447439,12.));
#57330=CARTESIAN_POINT('Ctrl Pts',(63.481504888716,-34.7309671782212,0.));
#57331=CARTESIAN_POINT('Ctrl Pts',(63.481504888716,-34.7309671782212,12.));
#57332=CARTESIAN_POINT('Ctrl Pts',(63.5059765323082,-34.7343560147663,0.));
#57333=CARTESIAN_POINT('Ctrl Pts',(63.5059765323082,-34.7343560147663,12.));
#57334=CARTESIAN_POINT('Ctrl Pts',(63.5304917929378,-34.7377268821022,0.));
#57335=CARTESIAN_POINT('Ctrl Pts',(63.5304917929378,-34.7377268821022,12.));
#57336=CARTESIAN_POINT('Ctrl Pts',(63.5550505684621,-34.7410797083079,0.));
#57337=CARTESIAN_POINT('Ctrl Pts',(63.5550505684621,-34.7410797083079,12.));
#57338=CARTESIAN_POINT('Ctrl Pts',(63.5796527570874,-34.7444144218162,0.));
#57339=CARTESIAN_POINT('Ctrl Pts',(63.5796527570874,-34.7444144218162,12.));
#57340=CARTESIAN_POINT('Ctrl Pts',(63.6042982573598,-34.7477309514142,0.));
#57341=CARTESIAN_POINT('Ctrl Pts',(63.6042982573598,-34.7477309514142,12.));
#57342=CARTESIAN_POINT('Ctrl Pts',(63.628986968162,-34.7510292262415,0.));
#57343=CARTESIAN_POINT('Ctrl Pts',(63.628986968162,-34.7510292262415,12.));
#57344=CARTESIAN_POINT('Ctrl Pts',(63.6537187887174,-34.7543091757842,0.));
#57345=CARTESIAN_POINT('Ctrl Pts',(63.6537187887174,-34.7543091757842,12.));
#57346=CARTESIAN_POINT('Ctrl Pts',(63.6784936185893,-34.7575707298718,0.));
#57347=CARTESIAN_POINT('Ctrl Pts',(63.6784936185893,-34.7575707298718,12.));
#57348=CARTESIAN_POINT('Ctrl Pts',(63.7033113576782,-34.7608138186758,0.));
#57349=CARTESIAN_POINT('Ctrl Pts',(63.7033113576782,-34.7608138186758,12.));
#57350=CARTESIAN_POINT('Ctrl Pts',(63.7281719062135,-34.7640383727094,0.));
#57351=CARTESIAN_POINT('Ctrl Pts',(63.7281719062135,-34.7640383727094,12.));
#57352=CARTESIAN_POINT('Ctrl Pts',(63.7530751647478,-34.7672443228267,0.));
#57353=CARTESIAN_POINT('Ctrl Pts',(63.7530751647478,-34.7672443228267,12.));
#57354=CARTESIAN_POINT('Ctrl Pts',(63.7780210341618,-34.7704316002165,0.));
#57355=CARTESIAN_POINT('Ctrl Pts',(63.7780210341618,-34.7704316002165,12.));
#57356=CARTESIAN_POINT('Ctrl Pts',(63.8030094156635,-34.7736001363991,0.));
#57357=CARTESIAN_POINT('Ctrl Pts',(63.8030094156635,-34.7736001363991,12.));
#57358=CARTESIAN_POINT('Ctrl Pts',(63.8280402107858,-34.7767498632244,0.));
#57359=CARTESIAN_POINT('Ctrl Pts',(63.8280402107858,-34.7767498632244,12.));
#57360=CARTESIAN_POINT('Ctrl Pts',(63.8531133213794,-34.7798807128716,0.));
#57361=CARTESIAN_POINT('Ctrl Pts',(63.8531133213794,-34.7798807128716,12.));
#57362=CARTESIAN_POINT('Ctrl Pts',(63.8782286496059,-34.7829926178495,0.));
#57363=CARTESIAN_POINT('Ctrl Pts',(63.8782286496059,-34.7829926178495,12.));
#57364=CARTESIAN_POINT('Ctrl Pts',(63.9033860979428,-34.7860855109908,0.));
#57365=CARTESIAN_POINT('Ctrl Pts',(63.9033860979428,-34.7860855109908,12.));
#57366=CARTESIAN_POINT('Ctrl Pts',(63.9285855691838,-34.7891593254485,0.));
#57367=CARTESIAN_POINT('Ctrl Pts',(63.9285855691838,-34.7891593254485,12.));
#57368=CARTESIAN_POINT('Ctrl Pts',(63.9538269664365,-34.7922139946943,0.));
#57369=CARTESIAN_POINT('Ctrl Pts',(63.9538269664365,-34.7922139946943,12.));
#57370=CARTESIAN_POINT('Ctrl Pts',(63.9791101931169,-34.7952494525182,0.));
#57371=CARTESIAN_POINT('Ctrl Pts',(63.9791101931169,-34.7952494525182,12.));
#57372=CARTESIAN_POINT('Ctrl Pts',(64.0044351529413,-34.79826563303,0.));
#57373=CARTESIAN_POINT('Ctrl Pts',(64.0044351529413,-34.79826563303,12.));
#57374=CARTESIAN_POINT('Ctrl Pts',(64.0298017499304,-34.8012624706534,0.));
#57375=CARTESIAN_POINT('Ctrl Pts',(64.0298017499304,-34.8012624706534,12.));
#57376=CARTESIAN_POINT('Ctrl Pts',(64.05520988841,-34.8042399001215,0.));
#57377=CARTESIAN_POINT('Ctrl Pts',(64.05520988841,-34.8042399001215,12.));
#57378=CARTESIAN_POINT('Ctrl Pts',(64.0806594730084,-34.8071978564748,0.));
#57379=CARTESIAN_POINT('Ctrl Pts',(64.0806594730084,-34.8071978564748,12.));
#57380=CARTESIAN_POINT('Ctrl Pts',(64.1061504086512,-34.8101362750595,0.));
#57381=CARTESIAN_POINT('Ctrl Pts',(64.1061504086512,-34.8101362750595,12.));
#57382=CARTESIAN_POINT('Ctrl Pts',(64.1316826005502,-34.8130550915284,0.));
#57383=CARTESIAN_POINT('Ctrl Pts',(64.1316826005502,-34.8130550915284,12.));
#57384=CARTESIAN_POINT('Ctrl Pts',(64.1572559542084,-34.8159542418372,0.));
#57385=CARTESIAN_POINT('Ctrl Pts',(64.1572559542084,-34.8159542418372,12.));
#57386=CARTESIAN_POINT('Ctrl Pts',(64.1828703754237,-34.8188336622419,0.));
#57387=CARTESIAN_POINT('Ctrl Pts',(64.1828703754237,-34.8188336622419,12.));
#57388=CARTESIAN_POINT('Ctrl Pts',(64.2085257702885,-34.8216932892969,0.));
#57389=CARTESIAN_POINT('Ctrl Pts',(64.2085257702885,-34.8216932892969,12.));
#57390=CARTESIAN_POINT('Ctrl Pts',(64.2342220451878,-34.8245330598559,0.));
#57391=CARTESIAN_POINT('Ctrl Pts',(64.2342220451878,-34.8245330598559,12.));
#57392=CARTESIAN_POINT('Ctrl Pts',(64.259959106791,-34.8273529110742,0.));
#57393=CARTESIAN_POINT('Ctrl Pts',(64.259959106791,-34.8273529110742,12.));
#57394=CARTESIAN_POINT('Ctrl Pts',(64.2857368620513,-34.8301527804052,0.));
#57395=CARTESIAN_POINT('Ctrl Pts',(64.2857368620513,-34.8301527804052,12.));
#57396=CARTESIAN_POINT('Ctrl Pts',(64.3115552182056,-34.8329326055916,0.));
#57397=CARTESIAN_POINT('Ctrl Pts',(64.3115552182056,-34.8329326055916,12.));
#57398=CARTESIAN_POINT('Ctrl Pts',(64.3374140827708,-34.8356923246617,0.));
#57399=CARTESIAN_POINT('Ctrl Pts',(64.3374140827708,-34.8356923246617,12.));
#57400=CARTESIAN_POINT('Ctrl Pts',(64.3633133635384,-34.838431875925,0.));
#57401=CARTESIAN_POINT('Ctrl Pts',(64.3633133635384,-34.838431875925,12.));
#57402=CARTESIAN_POINT('Ctrl Pts',(64.3892529685614,-34.8411511979705,0.));
#57403=CARTESIAN_POINT('Ctrl Pts',(64.3892529685614,-34.8411511979705,12.));
#57404=CARTESIAN_POINT('Ctrl Pts',(64.4152328061526,-34.8438502296669,0.));
#57405=CARTESIAN_POINT('Ctrl Pts',(64.4152328061526,-34.8438502296669,12.));
#57406=CARTESIAN_POINT('Ctrl Pts',(64.4412527848979,-34.8465289101626,0.));
#57407=CARTESIAN_POINT('Ctrl Pts',(64.4412527848979,-34.8465289101626,12.));
#57408=CARTESIAN_POINT('Ctrl Pts',(64.4673128136631,-34.8491871788899,0.));
#57409=CARTESIAN_POINT('Ctrl Pts',(64.4673128136631,-34.8491871788899,12.));
#57410=CARTESIAN_POINT('Ctrl Pts',(64.4934128015983,-34.851824975568,0.));
#57411=CARTESIAN_POINT('Ctrl Pts',(64.4934128015983,-34.851824975568,12.));
#57412=CARTESIAN_POINT('Ctrl Pts',(64.5195526581398,-34.8544422402114,0.));
#57413=CARTESIAN_POINT('Ctrl Pts',(64.5195526581398,-34.8544422402114,12.));
#57414=CARTESIAN_POINT('Ctrl Pts',(64.5457322930074,-34.8570389131334,0.));
#57415=CARTESIAN_POINT('Ctrl Pts',(64.5457322930074,-34.8570389131334,12.));
#57416=CARTESIAN_POINT('Ctrl Pts',(64.5719516161913,-34.8596149349251,0.));
#57417=CARTESIAN_POINT('Ctrl Pts',(64.5719516161913,-34.8596149349251,12.));
#57418=CARTESIAN_POINT('Ctrl Pts',(64.5982105379374,-34.8621702464397,0.));
#57419=CARTESIAN_POINT('Ctrl Pts',(64.5982105379374,-34.8621702464397,12.));
#57420=CARTESIAN_POINT('Ctrl Pts',(64.6245089687276,-34.8647047887774,0.));
#57421=CARTESIAN_POINT('Ctrl Pts',(64.6245089687276,-34.8647047887774,12.));
#57422=CARTESIAN_POINT('Ctrl Pts',(64.6508468192609,-34.8672185032725,0.));
#57423=CARTESIAN_POINT('Ctrl Pts',(64.6508468192609,-34.8672185032725,12.));
#57424=CARTESIAN_POINT('Ctrl Pts',(64.6772240004241,-34.8697113314797,0.));
#57425=CARTESIAN_POINT('Ctrl Pts',(64.6772240004241,-34.8697113314797,12.));
#57426=CARTESIAN_POINT('Ctrl Pts',(64.7036404233319,-34.8721832151982,0.));
#57427=CARTESIAN_POINT('Ctrl Pts',(64.7036404233319,-34.8721832151982,12.));
#57428=CARTESIAN_POINT('Ctrl Pts',(64.7300959993662,-34.8746340964977,0.));
#57429=CARTESIAN_POINT('Ctrl Pts',(64.7300959993662,-34.8746340964977,12.));
#57430=CARTESIAN_POINT('Ctrl Pts',(64.7565906402153,-34.8770639177494,0.));
#57431=CARTESIAN_POINT('Ctrl Pts',(64.7565906402153,-34.8770639177494,12.));
#57432=CARTESIAN_POINT('Ctrl Pts',(64.7831242579023,-34.8794726216511,0.));
#57433=CARTESIAN_POINT('Ctrl Pts',(64.7831242579023,-34.8794726216511,12.));
#57434=CARTESIAN_POINT('Ctrl Pts',(64.8096967648299,-34.8818601512726,0.));
#57435=CARTESIAN_POINT('Ctrl Pts',(64.8096967648299,-34.8818601512726,12.));
#57436=CARTESIAN_POINT('Ctrl Pts',(64.8363080737369,-34.8842264500184,0.));
#57437=CARTESIAN_POINT('Ctrl Pts',(64.8363080737369,-34.8842264500184,12.));
#57438=CARTESIAN_POINT('Ctrl Pts',(64.8629580976057,-34.8865714615433,0.));
#57439=CARTESIAN_POINT('Ctrl Pts',(64.8629580976057,-34.8865714615433,12.));
#57440=CARTESIAN_POINT('Ctrl Pts',(64.8896467495754,-34.888895129681,0.));
#57441=CARTESIAN_POINT('Ctrl Pts',(64.8896467495754,-34.888895129681,12.));
#57442=CARTESIAN_POINT('Ctrl Pts',(64.9163739428606,-34.8911973983785,0.));
#57443=CARTESIAN_POINT('Ctrl Pts',(64.9163739428606,-34.8911973983785,12.));
#57444=CARTESIAN_POINT('Ctrl Pts',(64.943139590634,-34.8934782116097,0.));
#57445=CARTESIAN_POINT('Ctrl Pts',(64.943139590634,-34.8934782116097,12.));
#57446=CARTESIAN_POINT('Ctrl Pts',(64.9699436060178,-34.8957375133702,0.));
#57447=CARTESIAN_POINT('Ctrl Pts',(64.9699436060178,-34.8957375133702,12.));
#57448=CARTESIAN_POINT('Ctrl Pts',(64.9967859023225,-34.8979752478623,0.));
#57449=CARTESIAN_POINT('Ctrl Pts',(64.9967859023225,-34.8979752478623,12.));
#57450=CARTESIAN_POINT('Ctrl Pts',(65.0236663932338,-34.9001913596422,0.));
#57451=CARTESIAN_POINT('Ctrl Pts',(65.0236663932338,-34.9001913596422,12.));
#57452=CARTESIAN_POINT('Ctrl Pts',(65.0505849930172,-34.9023857937866,0.));
#57453=CARTESIAN_POINT('Ctrl Pts',(65.0505849930172,-34.9023857937866,12.));
#57454=CARTESIAN_POINT('Ctrl Pts',(65.0775416167073,-34.9045584960503,0.));
#57455=CARTESIAN_POINT('Ctrl Pts',(65.0775416167073,-34.9045584960503,12.));
#57456=CARTESIAN_POINT('Ctrl Pts',(65.1045361803097,-34.9067094130387,0.));
#57457=CARTESIAN_POINT('Ctrl Pts',(65.1045361803097,-34.9067094130387,12.));
#57458=CARTESIAN_POINT('Ctrl Pts',(65.1315686003485,-34.9088384918322,0.));
#57459=CARTESIAN_POINT('Ctrl Pts',(65.1315686003485,-34.9088384918322,12.));
#57460=CARTESIAN_POINT('Ctrl Pts',(65.1586387934216,-34.9109456796201,0.));
#57461=CARTESIAN_POINT('Ctrl Pts',(65.1586387934216,-34.9109456796201,12.));
#57462=CARTESIAN_POINT('Ctrl Pts',(65.1857466757082,-34.9130309233017,0.));
#57463=CARTESIAN_POINT('Ctrl Pts',(65.1857466757082,-34.9130309233017,12.));
#57464=CARTESIAN_POINT('Ctrl Pts',(65.2128921625837,-34.9150941691754,0.));
#57465=CARTESIAN_POINT('Ctrl Pts',(65.2128921625837,-34.9150941691754,12.));
#57466=CARTESIAN_POINT('Ctrl Pts',(65.2400751679586,-34.9171353624131,0.));
#57467=CARTESIAN_POINT('Ctrl Pts',(65.2400751679586,-34.9171353624131,12.));
#57468=CARTESIAN_POINT('Ctrl Pts',(65.2672956048121,-34.9191544474898,0.));
#57469=CARTESIAN_POINT('Ctrl Pts',(65.2672956048121,-34.9191544474898,12.));
#57470=CARTESIAN_POINT('Ctrl Pts',(65.2945533863812,-34.921151369138,0.));
#57471=CARTESIAN_POINT('Ctrl Pts',(65.2945533863812,-34.921151369138,12.));
#57472=CARTESIAN_POINT('Ctrl Pts',(65.3218484271941,-34.9231260731846,0.));
#57473=CARTESIAN_POINT('Ctrl Pts',(65.3218484271941,-34.9231260731846,12.));
#57474=CARTESIAN_POINT('Ctrl Pts',(65.3491806440529,-34.9250785073473,0.));
#57475=CARTESIAN_POINT('Ctrl Pts',(65.3491806440529,-34.9250785073473,12.));
#57476=CARTESIAN_POINT('Ctrl Pts',(65.3765499573019,-34.9270086222703,0.));
#57477=CARTESIAN_POINT('Ctrl Pts',(65.3765499573019,-34.9270086222703,12.));
#57478=CARTESIAN_POINT('Ctrl Pts',(65.4039562911254,-34.92891637177,0.));
#57479=CARTESIAN_POINT('Ctrl Pts',(65.4039562911254,-34.92891637177,12.));
#57480=CARTESIAN_POINT('Ctrl Pts',(65.4313995707423,-34.9308017105481,0.));
#57481=CARTESIAN_POINT('Ctrl Pts',(65.4313995707423,-34.9308017105481,12.));
#57482=CARTESIAN_POINT('Ctrl Pts',(65.4588797201884,-34.9326645923897,0.));
#57483=CARTESIAN_POINT('Ctrl Pts',(65.4588797201884,-34.9326645923897,12.));
#57484=CARTESIAN_POINT('Ctrl Pts',(65.4863966597523,-34.9345049680816,0.));
#57485=CARTESIAN_POINT('Ctrl Pts',(65.4863966597523,-34.9345049680816,12.));
#57486=CARTESIAN_POINT('Ctrl Pts',(65.5139503038116,-34.9363227836621,0.));
#57487=CARTESIAN_POINT('Ctrl Pts',(65.5139503038116,-34.9363227836621,12.));
#57488=CARTESIAN_POINT('Ctrl Pts',(65.5415405578138,-34.9381179779763,0.));
#57489=CARTESIAN_POINT('Ctrl Pts',(65.5415405578138,-34.9381179779763,12.));
#57490=CARTESIAN_POINT('Ctrl Pts',(65.5691673226051,-34.9398904862279,0.));
#57491=CARTESIAN_POINT('Ctrl Pts',(65.5691673226051,-34.9398904862279,12.));
#57492=CARTESIAN_POINT('Ctrl Pts',(65.5968304997821,-34.9416402443551,0.));
#57493=CARTESIAN_POINT('Ctrl Pts',(65.5968304997821,-34.9416402443551,12.));
#57494=CARTESIAN_POINT('Ctrl Pts',(65.6245299968635,-34.9433671932982,0.));
#57495=CARTESIAN_POINT('Ctrl Pts',(65.6245299968635,-34.9433671932982,12.));
#57496=CARTESIAN_POINT('Ctrl Pts',(65.6522657321239,-34.9450712829143,0.));
#57497=CARTESIAN_POINT('Ctrl Pts',(65.6522657321239,-34.9450712829143,12.));
#57498=CARTESIAN_POINT('Ctrl Pts',(65.6800376405722,-34.9467524770271,0.));
#57499=CARTESIAN_POINT('Ctrl Pts',(65.6800376405722,-34.9467524770271,12.));
#57500=CARTESIAN_POINT('Ctrl Pts',(65.707845675746,-34.9484107543857,0.));
#57501=CARTESIAN_POINT('Ctrl Pts',(65.707845675746,-34.9484107543857,12.));
#57502=CARTESIAN_POINT('Ctrl Pts',(65.7356898060478,-34.9500461042919,0.));
#57503=CARTESIAN_POINT('Ctrl Pts',(65.7356898060478,-34.9500461042919,12.));
#57504=CARTESIAN_POINT('Ctrl Pts',(65.757993971173,-34.9513360397181,0.));
#57505=CARTESIAN_POINT('Ctrl Pts',(65.757993971173,-34.9513360397181,12.));
#57506=CARTESIAN_POINT('Ctrl Pts',(65.7747383250775,-34.9522931728594,0.));
#57507=CARTESIAN_POINT('Ctrl Pts',(65.7747383250775,-34.9522931728594,12.));
#57508=CARTESIAN_POINT('Ctrl Pts',(65.7859084407494,-34.9529266758406,0.));
#57509=CARTESIAN_POINT('Ctrl Pts',(65.7859084407494,-34.9529266758406,12.));
#57510=CARTESIAN_POINT('Ctrl Pts',(65.7914953018524,-34.9532422808861,0.));
#57511=CARTESIAN_POINT('Ctrl Pts',(65.7914953018524,-34.9532422808861,12.));
#57512=CARTESIAN_POINT('',(61.0441813777723,-34.2579614092497,0.));
#57513=CARTESIAN_POINT('Ctrl Pts',(61.0441813777723,-34.2579614092497,0.));
#57514=CARTESIAN_POINT('Ctrl Pts',(61.0479423318725,-34.2589297755434,0.));
#57515=CARTESIAN_POINT('Ctrl Pts',(61.0554700176998,-34.2608658001631,0.));
#57516=CARTESIAN_POINT('Ctrl Pts',(61.0667788793266,-34.2637677131935,0.));
#57517=CARTESIAN_POINT('Ctrl Pts',(61.0818920286293,-34.2676326825626,0.));
#57518=CARTESIAN_POINT('Ctrl Pts',(61.1008412399997,-34.2724568037228,0.));
#57519=CARTESIAN_POINT('Ctrl Pts',(61.1198481997764,-34.2772738038771,0.));
#57520=CARTESIAN_POINT('Ctrl Pts',(61.1389128461885,-34.282083624447,0.));
#57521=CARTESIAN_POINT('Ctrl Pts',(61.1580350635532,-34.2868861666384,0.));
#57522=CARTESIAN_POINT('Ctrl Pts',(61.1772146833205,-34.2916812929751,0.));
#57523=CARTESIAN_POINT('Ctrl Pts',(61.1964515073891,-34.2964688443663,0.));
#57524=CARTESIAN_POINT('Ctrl Pts',(61.2157453259107,-34.3012486533474,0.));
#57525=CARTESIAN_POINT('Ctrl Pts',(61.2350959366939,-34.3060205584065,0.));
#57526=CARTESIAN_POINT('Ctrl Pts',(61.2545031656133,-34.3107844191044,0.));
#57527=CARTESIAN_POINT('Ctrl Pts',(61.2739668600365,-34.3155401111747,0.));
#57528=CARTESIAN_POINT('Ctrl Pts',(61.2934868791854,-34.3202875193618,0.));
#57529=CARTESIAN_POINT('Ctrl Pts',(61.3130630861386,-34.3250265314768,0.));
#57530=CARTESIAN_POINT('Ctrl Pts',(61.3326953378851,-34.3297570310146,0.));
#57531=CARTESIAN_POINT('Ctrl Pts',(61.3523834803188,-34.3344788934363,0.));
#57532=CARTESIAN_POINT('Ctrl Pts',(61.3721273534256,-34.339191990014,0.));
#57533=CARTESIAN_POINT('Ctrl Pts',(61.3919267945302,-34.3438961902405,0.));
#57534=CARTESIAN_POINT('Ctrl Pts',(61.4117816420228,-34.3485913645979,0.));
#57535=CARTESIAN_POINT('Ctrl Pts',(61.4316917395918,-34.3532773877089,0.));
#57536=CARTESIAN_POINT('Ctrl Pts',(61.4516569360454,-34.3579541381996,0.));
#57537=CARTESIAN_POINT('Ctrl Pts',(61.4716770832896,-34.3626214971889,0.));
#57538=CARTESIAN_POINT('Ctrl Pts',(61.4917520349278,-34.3672793472466,0.));
#57539=CARTESIAN_POINT('Ctrl Pts',(61.5118816445437,-34.3719275711195,0.));
#57540=CARTESIAN_POINT('Ctrl Pts',(61.5320657642638,-34.376566050668,0.));
#57541=CARTESIAN_POINT('Ctrl Pts',(61.5523042455158,-34.3811946674197,0.));
#57542=CARTESIAN_POINT('Ctrl Pts',(61.5725969396829,-34.3858133030518,0.));
#57543=CARTESIAN_POINT('Ctrl Pts',(61.5929436987409,-34.3904218398637,0.));
#57544=CARTESIAN_POINT('Ctrl Pts',(61.6133443760142,-34.3950201613432,0.));
#57545=CARTESIAN_POINT('Ctrl Pts',(61.6337988264556,-34.3996081523753,0.));
#57546=CARTESIAN_POINT('Ctrl Pts',(61.6543069062416,-34.4041856989317,0.));
#57547=CARTESIAN_POINT('Ctrl Pts',(61.6748684725205,-34.4087526878812,0.));
#57548=CARTESIAN_POINT('Ctrl Pts',(61.695483383117,-34.4133090067704,0.));
#57549=CARTESIAN_POINT('Ctrl Pts',(61.7161514961914,-34.4178545435767,0.));
#57550=CARTESIAN_POINT('Ctrl Pts',(61.7368726702596,-34.422389186718,0.));
#57551=CARTESIAN_POINT('Ctrl Pts',(61.7576467643432,-34.4269128251577,0.));
#57552=CARTESIAN_POINT('Ctrl Pts',(61.7784736380727,-34.4314253484792,0.));
#57553=CARTESIAN_POINT('Ctrl Pts',(61.7993531518036,-34.4359266469749,0.));
#57554=CARTESIAN_POINT('Ctrl Pts',(61.8202851667222,-34.4404166117299,0.));
#57555=CARTESIAN_POINT('Ctrl Pts',(61.8412695447926,-34.444895134574,0.));
#57556=CARTESIAN_POINT('Ctrl Pts',(61.8623061487018,-34.4493621080361,0.));
#57557=CARTESIAN_POINT('Ctrl Pts',(61.8833948418025,-34.4538174253012,0.));
#57558=CARTESIAN_POINT('Ctrl Pts',(61.9045354880444,-34.4582609801637,0.));
#57559=CARTESIAN_POINT('Ctrl Pts',(61.9257279519308,-34.4626926669975,0.));
#57560=CARTESIAN_POINT('Ctrl Pts',(61.9469720985531,-34.4671123807717,0.));
#57561=CARTESIAN_POINT('Ctrl Pts',(61.9682677936053,-34.4715200170592,0.));
#57562=CARTESIAN_POINT('Ctrl Pts',(61.9896149034001,-34.4759154720473,0.));
#57563=CARTESIAN_POINT('Ctrl Pts',(62.0110132948794,-34.4802986425528,0.));
#57564=CARTESIAN_POINT('Ctrl Pts',(62.0324628356141,-34.48466942602,0.));
#57565=CARTESIAN_POINT('Ctrl Pts',(62.0539633937939,-34.489027720504,0.));
#57566=CARTESIAN_POINT('Ctrl Pts',(62.0755148382135,-34.4933734246593,0.));
#57567=CARTESIAN_POINT('Ctrl Pts',(62.0971170382567,-34.4977064377282,0.));
#57568=CARTESIAN_POINT('Ctrl Pts',(62.1187698638707,-34.5020266595293,0.));
#57569=CARTESIAN_POINT('Ctrl Pts',(62.1404731855687,-34.5063339904533,0.));
#57570=CARTESIAN_POINT('Ctrl Pts',(62.1622268744337,-34.5106283314594,0.));
#57571=CARTESIAN_POINT('Ctrl Pts',(62.184030802117,-34.514909584073,0.));
#57572=CARTESIAN_POINT('Ctrl Pts',(62.2058848408346,-34.5191776503843,0.));
#57573=CARTESIAN_POINT('Ctrl Pts',(62.2277888633576,-34.5234324330492,0.));
#57574=CARTESIAN_POINT('Ctrl Pts',(62.2497427430136,-34.527673835281,0.));
#57575=CARTESIAN_POINT('Ctrl Pts',(62.2717463536828,-34.5319017608435,0.));
#57576=CARTESIAN_POINT('Ctrl Pts',(62.2937995697927,-34.536116114045,0.));
#57577=CARTESIAN_POINT('Ctrl Pts',(62.3159022663052,-34.5403167997333,0.));
#57578=CARTESIAN_POINT('Ctrl Pts',(62.3380543187067,-34.5445037232928,0.));
#57579=CARTESIAN_POINT('Ctrl Pts',(62.3602556030114,-34.5486767906376,0.));
#57580=CARTESIAN_POINT('Ctrl Pts',(62.3825059957593,-34.552835908207,0.));
#57581=CARTESIAN_POINT('Ctrl Pts',(62.4048053740129,-34.5569809829615,0.));
#57582=CARTESIAN_POINT('Ctrl Pts',(62.4271536153473,-34.5611119223807,0.));
#57583=CARTESIAN_POINT('Ctrl Pts',(62.4495505978415,-34.5652286344606,0.));
#57584=CARTESIAN_POINT('Ctrl Pts',(62.4719962000829,-34.5693310277064,0.));
#57585=CARTESIAN_POINT('Ctrl Pts',(62.494490301164,-34.5734190111279,0.));
#57586=CARTESIAN_POINT('Ctrl Pts',(62.5170327806774,-34.5774924942351,0.));
#57587=CARTESIAN_POINT('Ctrl Pts',(62.5396235187053,-34.5815513870363,0.));
#57588=CARTESIAN_POINT('Ctrl Pts',(62.5622623958125,-34.5855956000344,0.));
#57589=CARTESIAN_POINT('Ctrl Pts',(62.5849492930501,-34.5896250442199,0.));
#57590=CARTESIAN_POINT('Ctrl Pts',(62.6076840919521,-34.5936396310671,0.));
#57591=CARTESIAN_POINT('Ctrl Pts',(62.6304666745319,-34.5976392725303,0.));
#57592=CARTESIAN_POINT('Ctrl Pts',(62.6532969232695,-34.6016238810419,0.));
#57593=CARTESIAN_POINT('Ctrl Pts',(62.6761747211081,-34.6055933695093,0.));
#57594=CARTESIAN_POINT('Ctrl Pts',(62.6990999514597,-34.6095476513095,0.));
#57595=CARTESIAN_POINT('Ctrl Pts',(62.7220724982005,-34.6134866402842,0.));
#57596=CARTESIAN_POINT('Ctrl Pts',(62.7450922456662,-34.6174102507368,0.));
#57597=CARTESIAN_POINT('Ctrl Pts',(62.7681590786398,-34.6213183974303,0.));
#57598=CARTESIAN_POINT('Ctrl Pts',(62.7912728823482,-34.6252109955836,0.));
#57599=CARTESIAN_POINT('Ctrl Pts',(62.8144335424671,-34.629087960866,0.));
#57600=CARTESIAN_POINT('Ctrl Pts',(62.8376409451167,-34.6329492093932,0.));
#57601=CARTESIAN_POINT('Ctrl Pts',(62.8608949768583,-34.6367946577241,0.));
#57602=CARTESIAN_POINT('Ctrl Pts',(62.8841955246819,-34.6406242228606,0.));
#57603=CARTESIAN_POINT('Ctrl Pts',(62.9075424760042,-34.6444378222425,0.));
#57604=CARTESIAN_POINT('Ctrl Pts',(62.9309357186733,-34.6482353737434,0.));
#57605=CARTESIAN_POINT('Ctrl Pts',(62.9543751409647,-34.6520167956657,0.));
#57606=CARTESIAN_POINT('Ctrl Pts',(62.9778606315777,-34.655782006739,0.));
#57607=CARTESIAN_POINT('Ctrl Pts',(63.0013920796225,-34.6595309261186,0.));
#57608=CARTESIAN_POINT('Ctrl Pts',(63.0249693746198,-34.6632634733819,0.));
#57609=CARTESIAN_POINT('Ctrl Pts',(63.0485924065039,-34.6669795685225,0.));
#57610=CARTESIAN_POINT('Ctrl Pts',(63.0722610656194,-34.6706791319471,0.));
#57611=CARTESIAN_POINT('Ctrl Pts',(63.0959752427169,-34.6743620844722,0.));
#57612=CARTESIAN_POINT('Ctrl Pts',(63.119734828943,-34.6780283473252,0.));
#57613=CARTESIAN_POINT('Ctrl Pts',(63.1435397158385,-34.6816778421401,0.));
#57614=CARTESIAN_POINT('Ctrl Pts',(63.1673897953425,-34.6853104909516,0.));
#57615=CARTESIAN_POINT('Ctrl Pts',(63.1912849597885,-34.6889262161923,0.));
#57616=CARTESIAN_POINT('Ctrl Pts',(63.2152251019014,-34.6925249406899,0.));
#57617=CARTESIAN_POINT('Ctrl Pts',(63.2392101147853,-34.6961065876671,0.));
#57618=CARTESIAN_POINT('Ctrl Pts',(63.2632398919234,-34.6996710807384,0.));
#57619=CARTESIAN_POINT('Ctrl Pts',(63.2873143271812,-34.7032183439045,0.));
#57620=CARTESIAN_POINT('Ctrl Pts',(63.311433314805,-34.7067483015492,0.));
#57621=CARTESIAN_POINT('Ctrl Pts',(63.3355967494169,-34.7102608784373,0.));
#57622=CARTESIAN_POINT('Ctrl Pts',(63.3598045260049,-34.7137559997143,0.));
#57623=CARTESIAN_POINT('Ctrl Pts',(63.3840565399206,-34.7172335909037,0.));
#57624=CARTESIAN_POINT('Ctrl Pts',(63.4083526868837,-34.7206935779007,0.));
#57625=CARTESIAN_POINT('Ctrl Pts',(63.4326928629796,-34.7241358869702,0.));
#57626=CARTESIAN_POINT('Ctrl Pts',(63.4570769646568,-34.7275604447439,0.));
#57627=CARTESIAN_POINT('Ctrl Pts',(63.481504888716,-34.7309671782212,0.));
#57628=CARTESIAN_POINT('Ctrl Pts',(63.5059765323082,-34.7343560147663,0.));
#57629=CARTESIAN_POINT('Ctrl Pts',(63.5304917929378,-34.7377268821022,0.));
#57630=CARTESIAN_POINT('Ctrl Pts',(63.5550505684621,-34.7410797083079,0.));
#57631=CARTESIAN_POINT('Ctrl Pts',(63.5796527570874,-34.7444144218162,0.));
#57632=CARTESIAN_POINT('Ctrl Pts',(63.6042982573598,-34.7477309514142,0.));
#57633=CARTESIAN_POINT('Ctrl Pts',(63.628986968162,-34.7510292262415,0.));
#57634=CARTESIAN_POINT('Ctrl Pts',(63.6537187887174,-34.7543091757842,0.));
#57635=CARTESIAN_POINT('Ctrl Pts',(63.6784936185893,-34.7575707298718,0.));
#57636=CARTESIAN_POINT('Ctrl Pts',(63.7033113576782,-34.7608138186758,0.));
#57637=CARTESIAN_POINT('Ctrl Pts',(63.7281719062135,-34.7640383727094,0.));
#57638=CARTESIAN_POINT('Ctrl Pts',(63.7530751647478,-34.7672443228267,0.));
#57639=CARTESIAN_POINT('Ctrl Pts',(63.7780210341618,-34.7704316002165,0.));
#57640=CARTESIAN_POINT('Ctrl Pts',(63.8030094156635,-34.7736001363991,0.));
#57641=CARTESIAN_POINT('Ctrl Pts',(63.8280402107858,-34.7767498632244,0.));
#57642=CARTESIAN_POINT('Ctrl Pts',(63.8531133213794,-34.7798807128716,0.));
#57643=CARTESIAN_POINT('Ctrl Pts',(63.8782286496059,-34.7829926178495,0.));
#57644=CARTESIAN_POINT('Ctrl Pts',(63.9033860979428,-34.7860855109908,0.));
#57645=CARTESIAN_POINT('Ctrl Pts',(63.9285855691838,-34.7891593254485,0.));
#57646=CARTESIAN_POINT('Ctrl Pts',(63.9538269664365,-34.7922139946943,0.));
#57647=CARTESIAN_POINT('Ctrl Pts',(63.9791101931169,-34.7952494525182,0.));
#57648=CARTESIAN_POINT('Ctrl Pts',(64.0044351529413,-34.79826563303,0.));
#57649=CARTESIAN_POINT('Ctrl Pts',(64.0298017499304,-34.8012624706534,0.));
#57650=CARTESIAN_POINT('Ctrl Pts',(64.05520988841,-34.8042399001215,0.));
#57651=CARTESIAN_POINT('Ctrl Pts',(64.0806594730084,-34.8071978564748,0.));
#57652=CARTESIAN_POINT('Ctrl Pts',(64.1061504086512,-34.8101362750595,0.));
#57653=CARTESIAN_POINT('Ctrl Pts',(64.1316826005502,-34.8130550915284,0.));
#57654=CARTESIAN_POINT('Ctrl Pts',(64.1572559542084,-34.8159542418372,0.));
#57655=CARTESIAN_POINT('Ctrl Pts',(64.1828703754237,-34.8188336622419,0.));
#57656=CARTESIAN_POINT('Ctrl Pts',(64.2085257702885,-34.8216932892969,0.));
#57657=CARTESIAN_POINT('Ctrl Pts',(64.2342220451878,-34.8245330598559,0.));
#57658=CARTESIAN_POINT('Ctrl Pts',(64.259959106791,-34.8273529110742,0.));
#57659=CARTESIAN_POINT('Ctrl Pts',(64.2857368620513,-34.8301527804052,0.));
#57660=CARTESIAN_POINT('Ctrl Pts',(64.3115552182056,-34.8329326055916,0.));
#57661=CARTESIAN_POINT('Ctrl Pts',(64.3374140827708,-34.8356923246617,0.));
#57662=CARTESIAN_POINT('Ctrl Pts',(64.3633133635384,-34.838431875925,0.));
#57663=CARTESIAN_POINT('Ctrl Pts',(64.3892529685614,-34.8411511979705,0.));
#57664=CARTESIAN_POINT('Ctrl Pts',(64.4152328061526,-34.8438502296669,0.));
#57665=CARTESIAN_POINT('Ctrl Pts',(64.4412527848979,-34.8465289101626,0.));
#57666=CARTESIAN_POINT('Ctrl Pts',(64.4673128136631,-34.8491871788899,0.));
#57667=CARTESIAN_POINT('Ctrl Pts',(64.4934128015983,-34.851824975568,0.));
#57668=CARTESIAN_POINT('Ctrl Pts',(64.5195526581398,-34.8544422402114,0.));
#57669=CARTESIAN_POINT('Ctrl Pts',(64.5457322930074,-34.8570389131334,0.));
#57670=CARTESIAN_POINT('Ctrl Pts',(64.5719516161913,-34.8596149349251,0.));
#57671=CARTESIAN_POINT('Ctrl Pts',(64.5982105379374,-34.8621702464397,0.));
#57672=CARTESIAN_POINT('Ctrl Pts',(64.6245089687276,-34.8647047887774,0.));
#57673=CARTESIAN_POINT('Ctrl Pts',(64.6508468192609,-34.8672185032725,0.));
#57674=CARTESIAN_POINT('Ctrl Pts',(64.6772240004241,-34.8697113314797,0.));
#57675=CARTESIAN_POINT('Ctrl Pts',(64.7036404233319,-34.8721832151982,0.));
#57676=CARTESIAN_POINT('Ctrl Pts',(64.7300959993662,-34.8746340964977,0.));
#57677=CARTESIAN_POINT('Ctrl Pts',(64.7565906402153,-34.8770639177494,0.));
#57678=CARTESIAN_POINT('Ctrl Pts',(64.7831242579023,-34.8794726216511,0.));
#57679=CARTESIAN_POINT('Ctrl Pts',(64.8096967648299,-34.8818601512726,0.));
#57680=CARTESIAN_POINT('Ctrl Pts',(64.8363080737369,-34.8842264500184,0.));
#57681=CARTESIAN_POINT('Ctrl Pts',(64.8629580976057,-34.8865714615433,0.));
#57682=CARTESIAN_POINT('Ctrl Pts',(64.8896467495754,-34.888895129681,0.));
#57683=CARTESIAN_POINT('Ctrl Pts',(64.9163739428606,-34.8911973983785,0.));
#57684=CARTESIAN_POINT('Ctrl Pts',(64.943139590634,-34.8934782116097,0.));
#57685=CARTESIAN_POINT('Ctrl Pts',(64.9699436060178,-34.8957375133702,0.));
#57686=CARTESIAN_POINT('Ctrl Pts',(64.9967859023225,-34.8979752478623,0.));
#57687=CARTESIAN_POINT('Ctrl Pts',(65.0236663932338,-34.9001913596422,0.));
#57688=CARTESIAN_POINT('Ctrl Pts',(65.0505849930172,-34.9023857937866,0.));
#57689=CARTESIAN_POINT('Ctrl Pts',(65.0775416167073,-34.9045584960503,0.));
#57690=CARTESIAN_POINT('Ctrl Pts',(65.1045361803097,-34.9067094130387,0.));
#57691=CARTESIAN_POINT('Ctrl Pts',(65.1315686003485,-34.9088384918322,0.));
#57692=CARTESIAN_POINT('Ctrl Pts',(65.1586387934216,-34.9109456796201,0.));
#57693=CARTESIAN_POINT('Ctrl Pts',(65.1857466757082,-34.9130309233017,0.));
#57694=CARTESIAN_POINT('Ctrl Pts',(65.2128921625837,-34.9150941691754,0.));
#57695=CARTESIAN_POINT('Ctrl Pts',(65.2400751679586,-34.9171353624131,0.));
#57696=CARTESIAN_POINT('Ctrl Pts',(65.2672956048121,-34.9191544474898,0.));
#57697=CARTESIAN_POINT('Ctrl Pts',(65.2945533863812,-34.921151369138,0.));
#57698=CARTESIAN_POINT('Ctrl Pts',(65.3218484271941,-34.9231260731846,0.));
#57699=CARTESIAN_POINT('Ctrl Pts',(65.3491806440529,-34.9250785073473,0.));
#57700=CARTESIAN_POINT('Ctrl Pts',(65.3765499573019,-34.9270086222703,0.));
#57701=CARTESIAN_POINT('Ctrl Pts',(65.4039562911254,-34.92891637177,0.));
#57702=CARTESIAN_POINT('Ctrl Pts',(65.4274804996405,-34.9305324724386,0.));
#57703=CARTESIAN_POINT('Ctrl Pts',(65.4455359574999,-34.9317593813103,0.));
#57704=CARTESIAN_POINT('Ctrl Pts',(65.4581063193583,-34.9326070346592,0.));
#57705=CARTESIAN_POINT('Ctrl Pts',(65.4651808010451,-34.9330820191484,0.));
#57706=CARTESIAN_POINT('Ctrl Pts',(65.4667541477954,-34.9331875523085,0.));
#57707=CARTESIAN_POINT('',(61.0441813777723,-34.2579614092497,12.));
#57708=CARTESIAN_POINT('',(61.0441813777723,-34.2579614092497,0.));
#57709=CARTESIAN_POINT('Ctrl Pts',(65.4667541477954,-34.9331875523085,12.));
#57710=CARTESIAN_POINT('Ctrl Pts',(65.4651808010451,-34.9330820191484,12.));
#57711=CARTESIAN_POINT('Ctrl Pts',(65.4581063193583,-34.9326070346592,12.));
#57712=CARTESIAN_POINT('Ctrl Pts',(65.4455359574999,-34.9317593813103,12.));
#57713=CARTESIAN_POINT('Ctrl Pts',(65.4274804996405,-34.9305324724386,12.));
#57714=CARTESIAN_POINT('Ctrl Pts',(65.4039562911254,-34.92891637177,12.));
#57715=CARTESIAN_POINT('Ctrl Pts',(65.3765499573019,-34.9270086222703,12.));
#57716=CARTESIAN_POINT('Ctrl Pts',(65.3491806440529,-34.9250785073473,12.));
#57717=CARTESIAN_POINT('Ctrl Pts',(65.3218484271941,-34.9231260731846,12.));
#57718=CARTESIAN_POINT('Ctrl Pts',(65.2945533863812,-34.921151369138,12.));
#57719=CARTESIAN_POINT('Ctrl Pts',(65.2672956048121,-34.9191544474898,12.));
#57720=CARTESIAN_POINT('Ctrl Pts',(65.2400751679586,-34.9171353624131,12.));
#57721=CARTESIAN_POINT('Ctrl Pts',(65.2128921625837,-34.9150941691754,12.));
#57722=CARTESIAN_POINT('Ctrl Pts',(65.1857466757082,-34.9130309233017,12.));
#57723=CARTESIAN_POINT('Ctrl Pts',(65.1586387934216,-34.9109456796201,12.));
#57724=CARTESIAN_POINT('Ctrl Pts',(65.1315686003485,-34.9088384918322,12.));
#57725=CARTESIAN_POINT('Ctrl Pts',(65.1045361803097,-34.9067094130387,12.));
#57726=CARTESIAN_POINT('Ctrl Pts',(65.0775416167073,-34.9045584960503,12.));
#57727=CARTESIAN_POINT('Ctrl Pts',(65.0505849930172,-34.9023857937866,12.));
#57728=CARTESIAN_POINT('Ctrl Pts',(65.0236663932338,-34.9001913596422,12.));
#57729=CARTESIAN_POINT('Ctrl Pts',(64.9967859023225,-34.8979752478623,12.));
#57730=CARTESIAN_POINT('Ctrl Pts',(64.9699436060178,-34.8957375133702,12.));
#57731=CARTESIAN_POINT('Ctrl Pts',(64.943139590634,-34.8934782116097,12.));
#57732=CARTESIAN_POINT('Ctrl Pts',(64.9163739428606,-34.8911973983785,12.));
#57733=CARTESIAN_POINT('Ctrl Pts',(64.8896467495754,-34.888895129681,12.));
#57734=CARTESIAN_POINT('Ctrl Pts',(64.8629580976057,-34.8865714615433,12.));
#57735=CARTESIAN_POINT('Ctrl Pts',(64.8363080737369,-34.8842264500184,12.));
#57736=CARTESIAN_POINT('Ctrl Pts',(64.8096967648299,-34.8818601512726,12.));
#57737=CARTESIAN_POINT('Ctrl Pts',(64.7831242579023,-34.8794726216511,12.));
#57738=CARTESIAN_POINT('Ctrl Pts',(64.7565906402153,-34.8770639177494,12.));
#57739=CARTESIAN_POINT('Ctrl Pts',(64.7300959993662,-34.8746340964977,12.));
#57740=CARTESIAN_POINT('Ctrl Pts',(64.7036404233319,-34.8721832151982,12.));
#57741=CARTESIAN_POINT('Ctrl Pts',(64.6772240004241,-34.8697113314797,12.));
#57742=CARTESIAN_POINT('Ctrl Pts',(64.6508468192609,-34.8672185032725,12.));
#57743=CARTESIAN_POINT('Ctrl Pts',(64.6245089687276,-34.8647047887774,12.));
#57744=CARTESIAN_POINT('Ctrl Pts',(64.5982105379374,-34.8621702464397,12.));
#57745=CARTESIAN_POINT('Ctrl Pts',(64.5719516161913,-34.8596149349251,12.));
#57746=CARTESIAN_POINT('Ctrl Pts',(64.5457322930074,-34.8570389131334,12.));
#57747=CARTESIAN_POINT('Ctrl Pts',(64.5195526581398,-34.8544422402114,12.));
#57748=CARTESIAN_POINT('Ctrl Pts',(64.4934128015983,-34.851824975568,12.));
#57749=CARTESIAN_POINT('Ctrl Pts',(64.4673128136631,-34.8491871788899,12.));
#57750=CARTESIAN_POINT('Ctrl Pts',(64.4412527848979,-34.8465289101626,12.));
#57751=CARTESIAN_POINT('Ctrl Pts',(64.4152328061526,-34.8438502296669,12.));
#57752=CARTESIAN_POINT('Ctrl Pts',(64.3892529685614,-34.8411511979705,12.));
#57753=CARTESIAN_POINT('Ctrl Pts',(64.3633133635384,-34.838431875925,12.));
#57754=CARTESIAN_POINT('Ctrl Pts',(64.3374140827708,-34.8356923246617,12.));
#57755=CARTESIAN_POINT('Ctrl Pts',(64.3115552182056,-34.8329326055916,12.));
#57756=CARTESIAN_POINT('Ctrl Pts',(64.2857368620513,-34.8301527804052,12.));
#57757=CARTESIAN_POINT('Ctrl Pts',(64.259959106791,-34.8273529110742,12.));
#57758=CARTESIAN_POINT('Ctrl Pts',(64.2342220451878,-34.8245330598559,12.));
#57759=CARTESIAN_POINT('Ctrl Pts',(64.2085257702885,-34.8216932892969,12.));
#57760=CARTESIAN_POINT('Ctrl Pts',(64.1828703754237,-34.8188336622419,12.));
#57761=CARTESIAN_POINT('Ctrl Pts',(64.1572559542084,-34.8159542418372,12.));
#57762=CARTESIAN_POINT('Ctrl Pts',(64.1316826005502,-34.8130550915284,12.));
#57763=CARTESIAN_POINT('Ctrl Pts',(64.1061504086512,-34.8101362750595,12.));
#57764=CARTESIAN_POINT('Ctrl Pts',(64.0806594730084,-34.8071978564748,12.));
#57765=CARTESIAN_POINT('Ctrl Pts',(64.05520988841,-34.8042399001215,12.));
#57766=CARTESIAN_POINT('Ctrl Pts',(64.0298017499304,-34.8012624706534,12.));
#57767=CARTESIAN_POINT('Ctrl Pts',(64.0044351529413,-34.79826563303,12.));
#57768=CARTESIAN_POINT('Ctrl Pts',(63.9791101931169,-34.7952494525182,12.));
#57769=CARTESIAN_POINT('Ctrl Pts',(63.9538269664365,-34.7922139946943,12.));
#57770=CARTESIAN_POINT('Ctrl Pts',(63.9285855691838,-34.7891593254485,12.));
#57771=CARTESIAN_POINT('Ctrl Pts',(63.9033860979428,-34.7860855109908,12.));
#57772=CARTESIAN_POINT('Ctrl Pts',(63.8782286496059,-34.7829926178495,12.));
#57773=CARTESIAN_POINT('Ctrl Pts',(63.8531133213794,-34.7798807128716,12.));
#57774=CARTESIAN_POINT('Ctrl Pts',(63.8280402107858,-34.7767498632244,12.));
#57775=CARTESIAN_POINT('Ctrl Pts',(63.8030094156635,-34.7736001363991,12.));
#57776=CARTESIAN_POINT('Ctrl Pts',(63.7780210341618,-34.7704316002165,12.));
#57777=CARTESIAN_POINT('Ctrl Pts',(63.7530751647478,-34.7672443228267,12.));
#57778=CARTESIAN_POINT('Ctrl Pts',(63.7281719062135,-34.7640383727094,12.));
#57779=CARTESIAN_POINT('Ctrl Pts',(63.7033113576782,-34.7608138186758,12.));
#57780=CARTESIAN_POINT('Ctrl Pts',(63.6784936185893,-34.7575707298718,12.));
#57781=CARTESIAN_POINT('Ctrl Pts',(63.6537187887174,-34.7543091757842,12.));
#57782=CARTESIAN_POINT('Ctrl Pts',(63.628986968162,-34.7510292262415,12.));
#57783=CARTESIAN_POINT('Ctrl Pts',(63.6042982573598,-34.7477309514142,12.));
#57784=CARTESIAN_POINT('Ctrl Pts',(63.5796527570874,-34.7444144218162,12.));
#57785=CARTESIAN_POINT('Ctrl Pts',(63.5550505684621,-34.7410797083079,12.));
#57786=CARTESIAN_POINT('Ctrl Pts',(63.5304917929378,-34.7377268821022,12.));
#57787=CARTESIAN_POINT('Ctrl Pts',(63.5059765323082,-34.7343560147663,12.));
#57788=CARTESIAN_POINT('Ctrl Pts',(63.481504888716,-34.7309671782212,12.));
#57789=CARTESIAN_POINT('Ctrl Pts',(63.4570769646568,-34.7275604447439,12.));
#57790=CARTESIAN_POINT('Ctrl Pts',(63.4326928629796,-34.7241358869702,12.));
#57791=CARTESIAN_POINT('Ctrl Pts',(63.4083526868837,-34.7206935779007,12.));
#57792=CARTESIAN_POINT('Ctrl Pts',(63.3840565399206,-34.7172335909037,12.));
#57793=CARTESIAN_POINT('Ctrl Pts',(63.3598045260049,-34.7137559997143,12.));
#57794=CARTESIAN_POINT('Ctrl Pts',(63.3355967494169,-34.7102608784373,12.));
#57795=CARTESIAN_POINT('Ctrl Pts',(63.311433314805,-34.7067483015492,12.));
#57796=CARTESIAN_POINT('Ctrl Pts',(63.2873143271812,-34.7032183439045,12.));
#57797=CARTESIAN_POINT('Ctrl Pts',(63.2632398919234,-34.6996710807384,12.));
#57798=CARTESIAN_POINT('Ctrl Pts',(63.2392101147853,-34.6961065876671,12.));
#57799=CARTESIAN_POINT('Ctrl Pts',(63.2152251019014,-34.6925249406899,12.));
#57800=CARTESIAN_POINT('Ctrl Pts',(63.1912849597885,-34.6889262161923,12.));
#57801=CARTESIAN_POINT('Ctrl Pts',(63.1673897953425,-34.6853104909516,12.));
#57802=CARTESIAN_POINT('Ctrl Pts',(63.1435397158385,-34.6816778421401,12.));
#57803=CARTESIAN_POINT('Ctrl Pts',(63.119734828943,-34.6780283473252,12.));
#57804=CARTESIAN_POINT('Ctrl Pts',(63.0959752427169,-34.6743620844722,12.));
#57805=CARTESIAN_POINT('Ctrl Pts',(63.0722610656194,-34.6706791319471,12.));
#57806=CARTESIAN_POINT('Ctrl Pts',(63.0485924065039,-34.6669795685225,12.));
#57807=CARTESIAN_POINT('Ctrl Pts',(63.0249693746198,-34.6632634733819,12.));
#57808=CARTESIAN_POINT('Ctrl Pts',(63.0013920796225,-34.6595309261186,12.));
#57809=CARTESIAN_POINT('Ctrl Pts',(62.9778606315777,-34.655782006739,12.));
#57810=CARTESIAN_POINT('Ctrl Pts',(62.9543751409647,-34.6520167956657,12.));
#57811=CARTESIAN_POINT('Ctrl Pts',(62.9309357186733,-34.6482353737434,12.));
#57812=CARTESIAN_POINT('Ctrl Pts',(62.9075424760042,-34.6444378222425,12.));
#57813=CARTESIAN_POINT('Ctrl Pts',(62.8841955246819,-34.6406242228606,12.));
#57814=CARTESIAN_POINT('Ctrl Pts',(62.8608949768583,-34.6367946577241,12.));
#57815=CARTESIAN_POINT('Ctrl Pts',(62.8376409451167,-34.6329492093932,12.));
#57816=CARTESIAN_POINT('Ctrl Pts',(62.8144335424671,-34.629087960866,12.));
#57817=CARTESIAN_POINT('Ctrl Pts',(62.7912728823482,-34.6252109955836,12.));
#57818=CARTESIAN_POINT('Ctrl Pts',(62.7681590786398,-34.6213183974303,12.));
#57819=CARTESIAN_POINT('Ctrl Pts',(62.7450922456662,-34.6174102507368,12.));
#57820=CARTESIAN_POINT('Ctrl Pts',(62.7220724982005,-34.6134866402842,12.));
#57821=CARTESIAN_POINT('Ctrl Pts',(62.6990999514597,-34.6095476513095,12.));
#57822=CARTESIAN_POINT('Ctrl Pts',(62.6761747211081,-34.6055933695093,12.));
#57823=CARTESIAN_POINT('Ctrl Pts',(62.6532969232695,-34.6016238810419,12.));
#57824=CARTESIAN_POINT('Ctrl Pts',(62.6304666745319,-34.5976392725303,12.));
#57825=CARTESIAN_POINT('Ctrl Pts',(62.6076840919521,-34.5936396310671,12.));
#57826=CARTESIAN_POINT('Ctrl Pts',(62.5849492930501,-34.5896250442199,12.));
#57827=CARTESIAN_POINT('Ctrl Pts',(62.5622623958125,-34.5855956000344,12.));
#57828=CARTESIAN_POINT('Ctrl Pts',(62.5396235187053,-34.5815513870363,12.));
#57829=CARTESIAN_POINT('Ctrl Pts',(62.5170327806774,-34.5774924942351,12.));
#57830=CARTESIAN_POINT('Ctrl Pts',(62.494490301164,-34.5734190111279,12.));
#57831=CARTESIAN_POINT('Ctrl Pts',(62.4719962000829,-34.5693310277064,12.));
#57832=CARTESIAN_POINT('Ctrl Pts',(62.4495505978415,-34.5652286344606,12.));
#57833=CARTESIAN_POINT('Ctrl Pts',(62.4271536153473,-34.5611119223807,12.));
#57834=CARTESIAN_POINT('Ctrl Pts',(62.4048053740129,-34.5569809829615,12.));
#57835=CARTESIAN_POINT('Ctrl Pts',(62.3825059957593,-34.552835908207,12.));
#57836=CARTESIAN_POINT('Ctrl Pts',(62.3602556030114,-34.5486767906376,12.));
#57837=CARTESIAN_POINT('Ctrl Pts',(62.3380543187067,-34.5445037232928,12.));
#57838=CARTESIAN_POINT('Ctrl Pts',(62.3159022663052,-34.5403167997333,12.));
#57839=CARTESIAN_POINT('Ctrl Pts',(62.2937995697927,-34.536116114045,12.));
#57840=CARTESIAN_POINT('Ctrl Pts',(62.2717463536828,-34.5319017608435,12.));
#57841=CARTESIAN_POINT('Ctrl Pts',(62.2497427430136,-34.527673835281,12.));
#57842=CARTESIAN_POINT('Ctrl Pts',(62.2277888633576,-34.5234324330492,12.));
#57843=CARTESIAN_POINT('Ctrl Pts',(62.2058848408346,-34.5191776503843,12.));
#57844=CARTESIAN_POINT('Ctrl Pts',(62.184030802117,-34.514909584073,12.));
#57845=CARTESIAN_POINT('Ctrl Pts',(62.1622268744337,-34.5106283314594,12.));
#57846=CARTESIAN_POINT('Ctrl Pts',(62.1404731855687,-34.5063339904533,12.));
#57847=CARTESIAN_POINT('Ctrl Pts',(62.1187698638707,-34.5020266595293,12.));
#57848=CARTESIAN_POINT('Ctrl Pts',(62.0971170382567,-34.4977064377282,12.));
#57849=CARTESIAN_POINT('Ctrl Pts',(62.0755148382135,-34.4933734246593,12.));
#57850=CARTESIAN_POINT('Ctrl Pts',(62.0539633937939,-34.489027720504,12.));
#57851=CARTESIAN_POINT('Ctrl Pts',(62.0324628356141,-34.48466942602,12.));
#57852=CARTESIAN_POINT('Ctrl Pts',(62.0110132948794,-34.4802986425528,12.));
#57853=CARTESIAN_POINT('Ctrl Pts',(61.9896149034001,-34.4759154720473,12.));
#57854=CARTESIAN_POINT('Ctrl Pts',(61.9682677936053,-34.4715200170592,12.));
#57855=CARTESIAN_POINT('Ctrl Pts',(61.9469720985531,-34.4671123807717,12.));
#57856=CARTESIAN_POINT('Ctrl Pts',(61.9257279519308,-34.4626926669975,12.));
#57857=CARTESIAN_POINT('Ctrl Pts',(61.9045354880444,-34.4582609801637,12.));
#57858=CARTESIAN_POINT('Ctrl Pts',(61.8833948418025,-34.4538174253012,12.));
#57859=CARTESIAN_POINT('Ctrl Pts',(61.8623061487018,-34.4493621080361,12.));
#57860=CARTESIAN_POINT('Ctrl Pts',(61.8412695447926,-34.444895134574,12.));
#57861=CARTESIAN_POINT('Ctrl Pts',(61.8202851667222,-34.4404166117299,12.));
#57862=CARTESIAN_POINT('Ctrl Pts',(61.7993531518036,-34.4359266469749,12.));
#57863=CARTESIAN_POINT('Ctrl Pts',(61.7784736380727,-34.4314253484792,12.));
#57864=CARTESIAN_POINT('Ctrl Pts',(61.7576467643432,-34.4269128251577,12.));
#57865=CARTESIAN_POINT('Ctrl Pts',(61.7368726702596,-34.422389186718,12.));
#57866=CARTESIAN_POINT('Ctrl Pts',(61.7161514961914,-34.4178545435767,12.));
#57867=CARTESIAN_POINT('Ctrl Pts',(61.695483383117,-34.4133090067704,12.));
#57868=CARTESIAN_POINT('Ctrl Pts',(61.6748684725205,-34.4087526878812,12.));
#57869=CARTESIAN_POINT('Ctrl Pts',(61.6543069062416,-34.4041856989317,12.));
#57870=CARTESIAN_POINT('Ctrl Pts',(61.6337988264556,-34.3996081523753,12.));
#57871=CARTESIAN_POINT('Ctrl Pts',(61.6133443760142,-34.3950201613432,12.));
#57872=CARTESIAN_POINT('Ctrl Pts',(61.5929436987409,-34.3904218398637,12.));
#57873=CARTESIAN_POINT('Ctrl Pts',(61.5725969396829,-34.3858133030518,12.));
#57874=CARTESIAN_POINT('Ctrl Pts',(61.5523042455158,-34.3811946674197,12.));
#57875=CARTESIAN_POINT('Ctrl Pts',(61.5320657642638,-34.376566050668,12.));
#57876=CARTESIAN_POINT('Ctrl Pts',(61.5118816445437,-34.3719275711195,12.));
#57877=CARTESIAN_POINT('Ctrl Pts',(61.4917520349278,-34.3672793472466,12.));
#57878=CARTESIAN_POINT('Ctrl Pts',(61.4716770832896,-34.3626214971889,12.));
#57879=CARTESIAN_POINT('Ctrl Pts',(61.4516569360454,-34.3579541381996,12.));
#57880=CARTESIAN_POINT('Ctrl Pts',(61.4316917395918,-34.3532773877089,12.));
#57881=CARTESIAN_POINT('Ctrl Pts',(61.4117816420228,-34.3485913645979,12.));
#57882=CARTESIAN_POINT('Ctrl Pts',(61.3919267945302,-34.3438961902405,12.));
#57883=CARTESIAN_POINT('Ctrl Pts',(61.3721273534256,-34.339191990014,12.));
#57884=CARTESIAN_POINT('Ctrl Pts',(61.3523834803188,-34.3344788934363,12.));
#57885=CARTESIAN_POINT('Ctrl Pts',(61.3326953378851,-34.3297570310146,12.));
#57886=CARTESIAN_POINT('Ctrl Pts',(61.3130630861386,-34.3250265314768,12.));
#57887=CARTESIAN_POINT('Ctrl Pts',(61.2934868791854,-34.3202875193618,12.));
#57888=CARTESIAN_POINT('Ctrl Pts',(61.2739668600365,-34.3155401111747,12.));
#57889=CARTESIAN_POINT('Ctrl Pts',(61.2545031656133,-34.3107844191044,12.));
#57890=CARTESIAN_POINT('Ctrl Pts',(61.2350959366939,-34.3060205584065,12.));
#57891=CARTESIAN_POINT('Ctrl Pts',(61.2157453259107,-34.3012486533474,12.));
#57892=CARTESIAN_POINT('Ctrl Pts',(61.1964515073891,-34.2964688443663,12.));
#57893=CARTESIAN_POINT('Ctrl Pts',(61.1772146833205,-34.2916812929751,12.));
#57894=CARTESIAN_POINT('Ctrl Pts',(61.1580350635532,-34.2868861666384,12.));
#57895=CARTESIAN_POINT('Ctrl Pts',(61.1389128461885,-34.282083624447,12.));
#57896=CARTESIAN_POINT('Ctrl Pts',(61.1198481997764,-34.2772738038771,12.));
#57897=CARTESIAN_POINT('Ctrl Pts',(61.1008412399997,-34.2724568037228,12.));
#57898=CARTESIAN_POINT('Ctrl Pts',(61.0818920286293,-34.2676326825626,12.));
#57899=CARTESIAN_POINT('Ctrl Pts',(61.0667788793266,-34.2637677131935,12.));
#57900=CARTESIAN_POINT('Ctrl Pts',(61.0554700176998,-34.2608658001631,12.));
#57901=CARTESIAN_POINT('Ctrl Pts',(61.0479423318725,-34.2589297755434,12.));
#57902=CARTESIAN_POINT('Ctrl Pts',(61.0441813777723,-34.2579614092497,12.));
#57903=CARTESIAN_POINT('Ctrl Pts',(66.1657795405962,-33.590372266528,-5.55111512312578E-16));
#57904=CARTESIAN_POINT('Ctrl Pts',(66.1657795405962,-33.590372266528,4.));
#57905=CARTESIAN_POINT('Ctrl Pts',(66.1657795405962,-33.590372266528,8.));
#57906=CARTESIAN_POINT('Ctrl Pts',(66.1657795405962,-33.590372266528,12.));
#57907=CARTESIAN_POINT('Ctrl Pts',(66.2346881970582,-33.6759628819919,-5.55111512312578E-16));
#57908=CARTESIAN_POINT('Ctrl Pts',(66.2346881970582,-33.6759628819919,4.));
#57909=CARTESIAN_POINT('Ctrl Pts',(66.2346881970582,-33.675962881992,8.));
#57910=CARTESIAN_POINT('Ctrl Pts',(66.2346881970582,-33.675962881992,12.));
#57911=CARTESIAN_POINT('Ctrl Pts',(66.3036153738448,-33.8665453669335,-5.55111512312578E-16));
#57912=CARTESIAN_POINT('Ctrl Pts',(66.3036153738448,-33.8665453669335,4.));
#57913=CARTESIAN_POINT('Ctrl Pts',(66.3036153738447,-33.8665453669334,8.));
#57914=CARTESIAN_POINT('Ctrl Pts',(66.3036153738447,-33.8665453669334,12.));
#57915=CARTESIAN_POINT('Ctrl Pts',(66.2585076236406,-34.0597557125863,-5.55111512312578E-16));
#57916=CARTESIAN_POINT('Ctrl Pts',(66.2585076236406,-34.0597557125863,4.));
#57917=CARTESIAN_POINT('Ctrl Pts',(66.2585076236405,-34.0597557125862,8.));
#57918=CARTESIAN_POINT('Ctrl Pts',(66.2585076236405,-34.0597557125862,12.));
#57919=CARTESIAN_POINT('Ctrl Pts',(66.2207497120656,-34.1330090612018,-5.55111512312578E-16));
#57920=CARTESIAN_POINT('Ctrl Pts',(66.2207497120656,-34.1330090612018,4.));
#57921=CARTESIAN_POINT('Ctrl Pts',(66.2207497120656,-34.1330090612017,8.));
#57922=CARTESIAN_POINT('Ctrl Pts',(66.2207497120656,-34.1330090612017,12.));
#57923=CARTESIAN_POINT('',(66.1657795405962,-33.590372266528,-2.77555756156289E-16));
#57924=CARTESIAN_POINT('',(66.2207497120649,-34.1330090612014,2.77555756156289E-16));
#57925=CARTESIAN_POINT('Ctrl Pts',(66.1657795405962,-33.590372266528,-5.44214888274584E-16));
#57926=CARTESIAN_POINT('Ctrl Pts',(66.2346881970582,-33.6759628819919,-5.44214888274584E-16));
#57927=CARTESIAN_POINT('Ctrl Pts',(66.274075155222,-33.7848671591014,-5.44214888274584E-16));
#57928=CARTESIAN_POINT('Ctrl Pts',(66.2762262188581,-33.8946295131778,-5.44214888274584E-16));
#57929=CARTESIAN_POINT('Ctrl Pts',(66.2778395165852,-33.9769512787351,-5.44214888274584E-16));
#57930=CARTESIAN_POINT('Ctrl Pts',(66.2585076236406,-34.0597557125863,-5.44214888274584E-16));
#57931=CARTESIAN_POINT('Ctrl Pts',(66.2207497120656,-34.1330090612018,-5.44214888274584E-16));
#57932=CARTESIAN_POINT('',(66.2207497120649,-34.1330090612013,12.));
#57933=CARTESIAN_POINT('Ctrl Pts',(66.2207497120656,-34.1330090612018,-5.55111512312578E-16));
#57934=CARTESIAN_POINT('Ctrl Pts',(66.2207497120656,-34.1330090612018,4.));
#57935=CARTESIAN_POINT('Ctrl Pts',(66.2207497120656,-34.1330090612017,8.));
#57936=CARTESIAN_POINT('Ctrl Pts',(66.2207497120656,-34.1330090612017,12.));
#57937=CARTESIAN_POINT('',(66.1657795405962,-33.590372266528,12.));
#57938=CARTESIAN_POINT('Ctrl Pts',(66.2207497120656,-34.1330090612017,12.));
#57939=CARTESIAN_POINT('Ctrl Pts',(66.2585076236405,-34.0597557125862,12.));
#57940=CARTESIAN_POINT('Ctrl Pts',(66.2778395165851,-33.976951278735,12.));
#57941=CARTESIAN_POINT('Ctrl Pts',(66.2762262188581,-33.8946295131777,12.));
#57942=CARTESIAN_POINT('Ctrl Pts',(66.2740751552219,-33.7848671591014,12.));
#57943=CARTESIAN_POINT('Ctrl Pts',(66.2346881970582,-33.675962881992,12.));
#57944=CARTESIAN_POINT('Ctrl Pts',(66.1657795405962,-33.590372266528,12.));
#57945=CARTESIAN_POINT('Ctrl Pts',(66.1657795405962,-33.590372266528,12.));
#57946=CARTESIAN_POINT('Ctrl Pts',(66.1657795405962,-33.590372266528,8.));
#57947=CARTESIAN_POINT('Ctrl Pts',(66.1657795405962,-33.590372266528,4.));
#57948=CARTESIAN_POINT('Ctrl Pts',(66.1657795405962,-33.590372266528,-5.55111512312578E-16));
#57949=CARTESIAN_POINT('Origin',(3.3253631270614E-10,-1.72995545227681E-10,
0.));
#57950=CARTESIAN_POINT('Origin',(3.3253631270614E-10,-1.72995545227681E-10,
12.));
#57951=CARTESIAN_POINT('Origin',(3.3253631270614E-10,-1.72995545227681E-10,
0.));
#57952=CARTESIAN_POINT('Ctrl Pts',(62.6704278106385,-40.2823469776966,0.));
#57953=CARTESIAN_POINT('Ctrl Pts',(62.6704278106385,-40.2823469776966,4.));
#57954=CARTESIAN_POINT('Ctrl Pts',(62.6704278106385,-40.2823469776966,8.));
#57955=CARTESIAN_POINT('Ctrl Pts',(62.6704278106385,-40.2823469776966,12.));
#57956=CARTESIAN_POINT('Ctrl Pts',(62.6110140705996,-40.374781624271,0.));
#57957=CARTESIAN_POINT('Ctrl Pts',(62.6110140705996,-40.374781624271,4.));
#57958=CARTESIAN_POINT('Ctrl Pts',(62.6110140705996,-40.374781624271,8.));
#57959=CARTESIAN_POINT('Ctrl Pts',(62.6110140705996,-40.374781624271,12.));
#57960=CARTESIAN_POINT('Ctrl Pts',(62.451999785206,-40.5004281293559,0.));
#57961=CARTESIAN_POINT('Ctrl Pts',(62.451999785206,-40.5004281293559,4.));
#57962=CARTESIAN_POINT('Ctrl Pts',(62.451999785206,-40.5004281293559,7.99999999999999));
#57963=CARTESIAN_POINT('Ctrl Pts',(62.451999785206,-40.5004281293559,12.));
#57964=CARTESIAN_POINT('Ctrl Pts',(62.2544389573111,-40.5187208145707,0.));
#57965=CARTESIAN_POINT('Ctrl Pts',(62.2544389573111,-40.5187208145707,4.));
#57966=CARTESIAN_POINT('Ctrl Pts',(62.2544389573111,-40.5187208145707,8.00000000000001));
#57967=CARTESIAN_POINT('Ctrl Pts',(62.2544389573111,-40.5187208145707,12.));
#57968=CARTESIAN_POINT('Ctrl Pts',(62.1730054756448,-40.506059810084,0.));
#57969=CARTESIAN_POINT('Ctrl Pts',(62.1730054756448,-40.506059810084,4.));
#57970=CARTESIAN_POINT('Ctrl Pts',(62.1730054756447,-40.506059810084,8.));
#57971=CARTESIAN_POINT('Ctrl Pts',(62.1730054756447,-40.506059810084,12.));
#57972=CARTESIAN_POINT('',(62.6704278106385,-40.2823469776966,0.));
#57973=CARTESIAN_POINT('',(62.1730054756448,-40.5060598100837,0.));
#57974=CARTESIAN_POINT('Ctrl Pts',(62.6704278106385,-40.2823469776966,0.));
#57975=CARTESIAN_POINT('Ctrl Pts',(62.6110140705996,-40.374781624271,0.));
#57976=CARTESIAN_POINT('Ctrl Pts',(62.5201487646604,-40.4465796271766,0.));
#57977=CARTESIAN_POINT('Ctrl Pts',(62.4166968325983,-40.4833233215533,0.));
#57978=CARTESIAN_POINT('Ctrl Pts',(62.3391078835518,-40.5108810923358,0.));
#57979=CARTESIAN_POINT('Ctrl Pts',(62.2544389573111,-40.5187208145707,0.));
#57980=CARTESIAN_POINT('Ctrl Pts',(62.1730054756448,-40.506059810084,0.));
#57981=CARTESIAN_POINT('',(62.1730054756448,-40.5060598100837,12.));
#57982=CARTESIAN_POINT('Ctrl Pts',(62.1730054756448,-40.506059810084,0.));
#57983=CARTESIAN_POINT('Ctrl Pts',(62.1730054756448,-40.506059810084,4.));
#57984=CARTESIAN_POINT('Ctrl Pts',(62.1730054756447,-40.506059810084,8.));
#57985=CARTESIAN_POINT('Ctrl Pts',(62.1730054756447,-40.506059810084,12.));
#57986=CARTESIAN_POINT('',(62.6704278106385,-40.2823469776966,12.));
#57987=CARTESIAN_POINT('Ctrl Pts',(62.1730054756447,-40.506059810084,12.));
#57988=CARTESIAN_POINT('Ctrl Pts',(62.2544389573111,-40.5187208145707,12.));
#57989=CARTESIAN_POINT('Ctrl Pts',(62.3391078835518,-40.5108810923358,12.));
#57990=CARTESIAN_POINT('Ctrl Pts',(62.4166968325983,-40.4833233215533,12.));
#57991=CARTESIAN_POINT('Ctrl Pts',(62.5201487646604,-40.4465796271767,12.));
#57992=CARTESIAN_POINT('Ctrl Pts',(62.6110140705996,-40.374781624271,12.));
#57993=CARTESIAN_POINT('Ctrl Pts',(62.6704278106385,-40.2823469776966,12.));
#57994=CARTESIAN_POINT('Ctrl Pts',(62.6704278106385,-40.2823469776966,12.));
#57995=CARTESIAN_POINT('Ctrl Pts',(62.6704278106385,-40.2823469776966,8.));
#57996=CARTESIAN_POINT('Ctrl Pts',(62.6704278106385,-40.2823469776966,4.));
#57997=CARTESIAN_POINT('Ctrl Pts',(62.6704278106385,-40.2823469776966,0.));
#57998=CARTESIAN_POINT('Ctrl Pts',(57.8261117662438,-39.4479504917287,0.));
#57999=CARTESIAN_POINT('Ctrl Pts',(57.8261117662438,-39.4479504917287,12.));
#58000=CARTESIAN_POINT('Ctrl Pts',(57.8297740100947,-39.4492429618443,0.));
#58001=CARTESIAN_POINT('Ctrl Pts',(57.8297740100947,-39.4492429618443,12.));
#58002=CARTESIAN_POINT('Ctrl Pts',(57.837104315141,-39.4518277003553,0.));
#58003=CARTESIAN_POINT('Ctrl Pts',(57.837104315141,-39.4518277003553,12.));
#58004=CARTESIAN_POINT('Ctrl Pts',(57.8481172247495,-39.4557042029652,0.));
#58005=CARTESIAN_POINT('Ctrl Pts',(57.8481172247495,-39.4557042029652,12.));
#58006=CARTESIAN_POINT('Ctrl Pts',(57.8628360096803,-39.4608716627118,0.));
#58007=CARTESIAN_POINT('Ctrl Pts',(57.8628360096803,-39.4608716627118,12.));
#58008=CARTESIAN_POINT('Ctrl Pts',(57.8812926637177,-39.4673289592259,0.));
#58009=CARTESIAN_POINT('Ctrl Pts',(57.8812926637177,-39.4673289592259,12.));
#58010=CARTESIAN_POINT('Ctrl Pts',(57.8998074670478,-39.473784194937,0.));
#58011=CARTESIAN_POINT('Ctrl Pts',(57.8998074670478,-39.473784194937,12.));
#58012=CARTESIAN_POINT('Ctrl Pts',(57.9183803632403,-39.4802373061058,0.));
#58013=CARTESIAN_POINT('Ctrl Pts',(57.9183803632403,-39.4802373061058,12.));
#58014=CARTESIAN_POINT('Ctrl Pts',(57.937011245663,-39.4866881842317,0.));
#58015=CARTESIAN_POINT('Ctrl Pts',(57.937011245663,-39.4866881842317,12.));
#58016=CARTESIAN_POINT('Ctrl Pts',(57.9556999583892,-39.4931366776714,0.));
#58017=CARTESIAN_POINT('Ctrl Pts',(57.9556999583892,-39.4931366776714,12.));
#58018=CARTESIAN_POINT('Ctrl Pts',(57.974446317937,-39.499582610674,0.));
#58019=CARTESIAN_POINT('Ctrl Pts',(57.974446317937,-39.499582610674,12.));
#58020=CARTESIAN_POINT('Ctrl Pts',(57.9932501298522,-39.5060257981225,0.));
#58021=CARTESIAN_POINT('Ctrl Pts',(57.9932501298522,-39.5060257981225,12.));
#58022=CARTESIAN_POINT('Ctrl Pts',(58.0121112067895,-39.5124660614976,0.));
#58023=CARTESIAN_POINT('Ctrl Pts',(58.0121112067895,-39.5124660614976,12.));
#58024=CARTESIAN_POINT('Ctrl Pts',(58.0310293875262,-39.5189032457184,0.));
#58025=CARTESIAN_POINT('Ctrl Pts',(58.0310293875262,-39.5189032457184,12.));
#58026=CARTESIAN_POINT('Ctrl Pts',(58.0500045308412,-39.5253372136887,0.));
#58027=CARTESIAN_POINT('Ctrl Pts',(58.0500045308412,-39.5253372136887,12.));
#58028=CARTESIAN_POINT('Ctrl Pts',(58.0690365065374,-39.5317678383217,0.));
#58029=CARTESIAN_POINT('Ctrl Pts',(58.0690365065374,-39.5317678383217,12.));
#58030=CARTESIAN_POINT('Ctrl Pts',(58.088125187992,-39.5381949959221,0.));
#58031=CARTESIAN_POINT('Ctrl Pts',(58.088125187992,-39.5381949959221,12.));
#58032=CARTESIAN_POINT('Ctrl Pts',(58.1072704428928,-39.5446185579638,0.));
#58033=CARTESIAN_POINT('Ctrl Pts',(58.1072704428928,-39.5446185579638,12.));
#58034=CARTESIAN_POINT('Ctrl Pts',(58.126472128574,-39.5510383869505,0.));
#58035=CARTESIAN_POINT('Ctrl Pts',(58.126472128574,-39.5510383869505,12.));
#58036=CARTESIAN_POINT('Ctrl Pts',(58.1457300968499,-39.5574543406982,0.));
#58037=CARTESIAN_POINT('Ctrl Pts',(58.1457300968499,-39.5574543406982,12.));
#58038=CARTESIAN_POINT('Ctrl Pts',(58.1650441970387,-39.563866275018,0.));
#58039=CARTESIAN_POINT('Ctrl Pts',(58.1650441970387,-39.563866275018,12.));
#58040=CARTESIAN_POINT('Ctrl Pts',(58.1844142794338,-39.5702740467999,0.));
#58041=CARTESIAN_POINT('Ctrl Pts',(58.1844142794338,-39.5702740467999,12.));
#58042=CARTESIAN_POINT('Ctrl Pts',(58.2038401992457,-39.57667751752,0.));
#58043=CARTESIAN_POINT('Ctrl Pts',(58.2038401992457,-39.57667751752,12.));
#58044=CARTESIAN_POINT('Ctrl Pts',(58.2233218164365,-39.5830765530891,0.));
#58045=CARTESIAN_POINT('Ctrl Pts',(58.2233218164365,-39.5830765530891,12.));
#58046=CARTESIAN_POINT('Ctrl Pts',(58.2428589938369,-39.5894710221713,0.));
#58047=CARTESIAN_POINT('Ctrl Pts',(58.2428589938369,-39.5894710221713,12.));
#58048=CARTESIAN_POINT('Ctrl Pts',(58.2624515958419,-39.5958607950239,0.));
#58049=CARTESIAN_POINT('Ctrl Pts',(58.2624515958419,-39.5958607950239,12.));
#58050=CARTESIAN_POINT('Ctrl Pts',(58.2820994868118,-39.602245742079,0.));
#58051=CARTESIAN_POINT('Ctrl Pts',(58.2820994868118,-39.602245742079,12.));
#58052=CARTESIAN_POINT('Ctrl Pts',(58.3018025297323,-39.6086257327583,0.));
#58053=CARTESIAN_POINT('Ctrl Pts',(58.3018025297323,-39.6086257327583,12.));
#58054=CARTESIAN_POINT('Ctrl Pts',(58.3215605869221,-39.6150006360915,0.));
#58055=CARTESIAN_POINT('Ctrl Pts',(58.3215605869221,-39.6150006360915,12.));
#58056=CARTESIAN_POINT('Ctrl Pts',(58.3413735206423,-39.6213703212531,0.));
#58057=CARTESIAN_POINT('Ctrl Pts',(58.3413735206423,-39.6213703212531,12.));
#58058=CARTESIAN_POINT('Ctrl Pts',(58.3612411936904,-39.6277346580892,0.));
#58059=CARTESIAN_POINT('Ctrl Pts',(58.3612411936904,-39.6277346580892,12.));
#58060=CARTESIAN_POINT('Ctrl Pts',(58.3811634701037,-39.6340935177476,0.));
#58061=CARTESIAN_POINT('Ctrl Pts',(58.3811634701037,-39.6340935177476,12.));
#58062=CARTESIAN_POINT('Ctrl Pts',(58.4011402154196,-39.6404467729094,0.));
#58063=CARTESIAN_POINT('Ctrl Pts',(58.4011402154196,-39.6404467729094,12.));
#58064=CARTESIAN_POINT('Ctrl Pts',(58.4211712963004,-39.6467942974451,0.));
#58065=CARTESIAN_POINT('Ctrl Pts',(58.4211712963004,-39.6467942974451,12.));
#58066=CARTESIAN_POINT('Ctrl Pts',(58.4412565802979,-39.653135966204,0.));
#58067=CARTESIAN_POINT('Ctrl Pts',(58.4412565802979,-39.653135966204,12.));
#58068=CARTESIAN_POINT('Ctrl Pts',(58.4613959355788,-39.6594716547689,0.));
#58069=CARTESIAN_POINT('Ctrl Pts',(58.4613959355788,-39.6594716547689,12.));
#58070=CARTESIAN_POINT('Ctrl Pts',(58.4815892306066,-39.6658012391815,0.));
#58071=CARTESIAN_POINT('Ctrl Pts',(58.4815892306066,-39.6658012391815,12.));
#58072=CARTESIAN_POINT('Ctrl Pts',(58.5018363341604,-39.6721245959531,0.));
#58073=CARTESIAN_POINT('Ctrl Pts',(58.5018363341604,-39.6721245959531,12.));
#58074=CARTESIAN_POINT('Ctrl Pts',(58.5221371154761,-39.6784416021826,0.));
#58075=CARTESIAN_POINT('Ctrl Pts',(58.5221371154761,-39.6784416021826,12.));
#58076=CARTESIAN_POINT('Ctrl Pts',(58.5424914443415,-39.6847521356395,0.));
#58077=CARTESIAN_POINT('Ctrl Pts',(58.5424914443415,-39.6847521356395,12.));
#58078=CARTESIAN_POINT('Ctrl Pts',(58.5628991912052,-39.6910560748629,0.));
#58079=CARTESIAN_POINT('Ctrl Pts',(58.5628991912052,-39.6910560748629,12.));
#58080=CARTESIAN_POINT('Ctrl Pts',(58.5833602272743,-39.697353299254,0.));
#58081=CARTESIAN_POINT('Ctrl Pts',(58.5833602272743,-39.697353299254,12.));
#58082=CARTESIAN_POINT('Ctrl Pts',(58.6038744244659,-39.7036436890233,0.));
#58083=CARTESIAN_POINT('Ctrl Pts',(58.6038744244659,-39.7036436890233,12.));
#58084=CARTESIAN_POINT('Ctrl Pts',(58.6244416553562,-39.7099271251413,0.));
#58085=CARTESIAN_POINT('Ctrl Pts',(58.6244416553562,-39.7099271251413,12.));
#58086=CARTESIAN_POINT('Ctrl Pts',(58.6450617931274,-39.71620348929,0.));
#58087=CARTESIAN_POINT('Ctrl Pts',(58.6450617931274,-39.71620348929,12.));
#58088=CARTESIAN_POINT('Ctrl Pts',(58.6657347115034,-39.7224726638101,0.));
#58089=CARTESIAN_POINT('Ctrl Pts',(58.6657347115034,-39.7224726638101,12.));
#58090=CARTESIAN_POINT('Ctrl Pts',(58.6864602847088,-39.7287345316681,0.));
#58091=CARTESIAN_POINT('Ctrl Pts',(58.6864602847088,-39.7287345316681,12.));
#58092=CARTESIAN_POINT('Ctrl Pts',(58.7072383875027,-39.734988976475,0.));
#58093=CARTESIAN_POINT('Ctrl Pts',(58.7072383875027,-39.734988976475,12.));
#58094=CARTESIAN_POINT('Ctrl Pts',(58.7280688951916,-39.7412358824953,0.));
#58095=CARTESIAN_POINT('Ctrl Pts',(58.7280688951916,-39.7412358824953,12.));
#58096=CARTESIAN_POINT('Ctrl Pts',(58.7489516836445,-39.7474751346599,0.));
#58097=CARTESIAN_POINT('Ctrl Pts',(58.7489516836445,-39.7474751346599,12.));
#58098=CARTESIAN_POINT('Ctrl Pts',(58.7698866293029,-39.7537066185813,0.));
#58099=CARTESIAN_POINT('Ctrl Pts',(58.7698866293029,-39.7537066185813,12.));
#58100=CARTESIAN_POINT('Ctrl Pts',(58.7908736091798,-39.7599302205521,0.));
#58101=CARTESIAN_POINT('Ctrl Pts',(58.7908736091798,-39.7599302205521,12.));
#58102=CARTESIAN_POINT('Ctrl Pts',(58.8119125008517,-39.7661458275274,0.));
#58103=CARTESIAN_POINT('Ctrl Pts',(58.8119125008517,-39.7661458275274,12.));
#58104=CARTESIAN_POINT('Ctrl Pts',(58.8330031824453,-39.772353327112,0.));
#58105=CARTESIAN_POINT('Ctrl Pts',(58.8330031824453,-39.772353327112,12.));
#58106=CARTESIAN_POINT('Ctrl Pts',(58.8541455326231,-39.7785526075479,0.));
#58107=CARTESIAN_POINT('Ctrl Pts',(58.8541455326231,-39.7785526075479,12.));
#58108=CARTESIAN_POINT('Ctrl Pts',(58.8753394305585,-39.7847435576997,0.));
#58109=CARTESIAN_POINT('Ctrl Pts',(58.8753394305585,-39.7847435576997,12.));
#58110=CARTESIAN_POINT('Ctrl Pts',(58.8965847559391,-39.7909260670517,0.));
#58111=CARTESIAN_POINT('Ctrl Pts',(58.8965847559391,-39.7909260670517,12.));
#58112=CARTESIAN_POINT('Ctrl Pts',(58.9178813889703,-39.7971000257044,0.));
#58113=CARTESIAN_POINT('Ctrl Pts',(58.9178813889703,-39.7971000257044,12.));
#58114=CARTESIAN_POINT('Ctrl Pts',(58.9392292103747,-39.8032653243712,0.));
#58115=CARTESIAN_POINT('Ctrl Pts',(58.9392292103747,-39.8032653243712,12.));
#58116=CARTESIAN_POINT('Ctrl Pts',(58.9606281013875,-39.8094218543782,0.));
#58117=CARTESIAN_POINT('Ctrl Pts',(58.9606281013875,-39.8094218543782,12.));
#58118=CARTESIAN_POINT('Ctrl Pts',(58.9820779437484,-39.8155695076626,0.));
#58119=CARTESIAN_POINT('Ctrl Pts',(58.9820779437484,-39.8155695076626,12.));
#58120=CARTESIAN_POINT('Ctrl Pts',(59.0035786197024,-39.821708176766,0.));
#58121=CARTESIAN_POINT('Ctrl Pts',(59.0035786197024,-39.821708176766,12.));
#58122=CARTESIAN_POINT('Ctrl Pts',(59.0251300119973,-39.8278377548262,0.));
#58123=CARTESIAN_POINT('Ctrl Pts',(59.0251300119973,-39.8278377548262,12.));
#58124=CARTESIAN_POINT('Ctrl Pts',(59.0467320038784,-39.8339581355716,0.));
#58125=CARTESIAN_POINT('Ctrl Pts',(59.0467320038784,-39.8339581355716,12.));
#58126=CARTESIAN_POINT('Ctrl Pts',(59.0683844790764,-39.8400692133139,0.));
#58127=CARTESIAN_POINT('Ctrl Pts',(59.0683844790764,-39.8400692133139,12.));
#58128=CARTESIAN_POINT('Ctrl Pts',(59.090087321798,-39.8461708829456,0.));
#58129=CARTESIAN_POINT('Ctrl Pts',(59.090087321798,-39.8461708829456,12.));
#58130=CARTESIAN_POINT('Ctrl Pts',(59.1118404167292,-39.8522630399328,0.));
#58131=CARTESIAN_POINT('Ctrl Pts',(59.1118404167292,-39.8522630399328,12.));
#58132=CARTESIAN_POINT('Ctrl Pts',(59.1336436490342,-39.8583455803105,0.));
#58133=CARTESIAN_POINT('Ctrl Pts',(59.1336436490342,-39.8583455803105,12.));
#58134=CARTESIAN_POINT('Ctrl Pts',(59.1554969043522,-39.8644184006787,0.));
#58135=CARTESIAN_POINT('Ctrl Pts',(59.1554969043522,-39.8644184006787,12.));
#58136=CARTESIAN_POINT('Ctrl Pts',(59.1774000687879,-39.8704813981989,0.));
#58137=CARTESIAN_POINT('Ctrl Pts',(59.1774000687879,-39.8704813981989,12.));
#58138=CARTESIAN_POINT('Ctrl Pts',(59.1993530289028,-39.876534470591,0.));
#58139=CARTESIAN_POINT('Ctrl Pts',(59.1993530289028,-39.876534470591,12.));
#58140=CARTESIAN_POINT('Ctrl Pts',(59.2213556717209,-39.8825775161267,0.));
#58141=CARTESIAN_POINT('Ctrl Pts',(59.2213556717209,-39.8825775161267,12.));
#58142=CARTESIAN_POINT('Ctrl Pts',(59.2434078847247,-39.8886104336242,0.));
#58143=CARTESIAN_POINT('Ctrl Pts',(59.2434078847247,-39.8886104336242,12.));
#58144=CARTESIAN_POINT('Ctrl Pts',(59.2655095558521,-39.8946331224438,0.));
#58145=CARTESIAN_POINT('Ctrl Pts',(59.2655095558521,-39.8946331224438,12.));
#58146=CARTESIAN_POINT('Ctrl Pts',(59.2876605734846,-39.9006454824845,0.));
#58147=CARTESIAN_POINT('Ctrl Pts',(59.2876605734846,-39.9006454824845,12.));
#58148=CARTESIAN_POINT('Ctrl Pts',(59.3098608264419,-39.9066474141803,0.));
#58149=CARTESIAN_POINT('Ctrl Pts',(59.3098608264419,-39.9066474141803,12.));
#58150=CARTESIAN_POINT('Ctrl Pts',(59.3321102039852,-39.9126388184936,0.));
#58151=CARTESIAN_POINT('Ctrl Pts',(59.3321102039852,-39.9126388184936,12.));
#58152=CARTESIAN_POINT('Ctrl Pts',(59.3544085958151,-39.9186195969104,0.));
#58153=CARTESIAN_POINT('Ctrl Pts',(59.3544085958151,-39.9186195969104,12.));
#58154=CARTESIAN_POINT('Ctrl Pts',(59.3767558920675,-39.9245896514367,0.));
#58155=CARTESIAN_POINT('Ctrl Pts',(59.3767558920675,-39.9245896514367,12.));
#58156=CARTESIAN_POINT('Ctrl Pts',(59.3991519833016,-39.9305488845958,0.));
#58157=CARTESIAN_POINT('Ctrl Pts',(59.3991519833016,-39.9305488845958,12.));
#58158=CARTESIAN_POINT('Ctrl Pts',(59.4215967604967,-39.9364971994242,0.));
#58159=CARTESIAN_POINT('Ctrl Pts',(59.4215967604967,-39.9364971994242,12.));
#58160=CARTESIAN_POINT('Ctrl Pts',(59.4440901150582,-39.9424344994673,0.));
#58161=CARTESIAN_POINT('Ctrl Pts',(59.4440901150582,-39.9424344994673,12.));
#58162=CARTESIAN_POINT('Ctrl Pts',(59.4666319388133,-39.9483606887738,0.));
#58163=CARTESIAN_POINT('Ctrl Pts',(59.4666319388133,-39.9483606887738,12.));
#58164=CARTESIAN_POINT('Ctrl Pts',(59.4892221240068,-39.9542756718922,0.));
#58165=CARTESIAN_POINT('Ctrl Pts',(59.4892221240068,-39.9542756718922,12.));
#58166=CARTESIAN_POINT('Ctrl Pts',(59.511860563289,-39.9601793538683,0.));
#58167=CARTESIAN_POINT('Ctrl Pts',(59.511860563289,-39.9601793538683,12.));
#58168=CARTESIAN_POINT('Ctrl Pts',(59.5345471497128,-39.9660716402403,0.));
#58169=CARTESIAN_POINT('Ctrl Pts',(59.5345471497128,-39.9660716402403,12.));
#58170=CARTESIAN_POINT('Ctrl Pts',(59.5572817767388,-39.9719524370346,0.));
#58171=CARTESIAN_POINT('Ctrl Pts',(59.5572817767388,-39.9719524370346,12.));
#58172=CARTESIAN_POINT('Ctrl Pts',(59.5800643382314,-39.9778216507605,0.));
#58173=CARTESIAN_POINT('Ctrl Pts',(59.5800643382314,-39.9778216507605,12.));
#58174=CARTESIAN_POINT('Ctrl Pts',(59.6028947284562,-39.9836791884079,0.));
#58175=CARTESIAN_POINT('Ctrl Pts',(59.6028947284562,-39.9836791884079,12.));
#58176=CARTESIAN_POINT('Ctrl Pts',(59.6257728420669,-39.9895249574448,0.));
#58177=CARTESIAN_POINT('Ctrl Pts',(59.6257728420669,-39.9895249574448,12.));
#58178=CARTESIAN_POINT('Ctrl Pts',(59.6486985741041,-39.9953588658132,0.));
#58179=CARTESIAN_POINT('Ctrl Pts',(59.6486985741041,-39.9953588658132,12.));
#58180=CARTESIAN_POINT('Ctrl Pts',(59.6716718200005,-40.0011808219241,0.));
#58181=CARTESIAN_POINT('Ctrl Pts',(59.6716718200005,-40.0011808219241,12.));
#58182=CARTESIAN_POINT('Ctrl Pts',(59.6946924755773,-40.0069907346538,0.));
#58183=CARTESIAN_POINT('Ctrl Pts',(59.6946924755773,-40.0069907346538,12.));
#58184=CARTESIAN_POINT('Ctrl Pts',(59.7177604370403,-40.0127885133403,0.));
#58185=CARTESIAN_POINT('Ctrl Pts',(59.7177604370403,-40.0127885133403,12.));
#58186=CARTESIAN_POINT('Ctrl Pts',(59.7408756009679,-40.0185740677821,0.));
#58187=CARTESIAN_POINT('Ctrl Pts',(59.7408756009679,-40.0185740677821,12.));
#58188=CARTESIAN_POINT('Ctrl Pts',(59.7640378643106,-40.0243473082337,0.));
#58189=CARTESIAN_POINT('Ctrl Pts',(59.7640378643106,-40.0243473082337,12.));
#58190=CARTESIAN_POINT('Ctrl Pts',(59.7872471243942,-40.0301081454002,0.));
#58191=CARTESIAN_POINT('Ctrl Pts',(59.7872471243942,-40.0301081454002,12.));
#58192=CARTESIAN_POINT('Ctrl Pts',(59.8105032789179,-40.0358564904341,0.));
#58193=CARTESIAN_POINT('Ctrl Pts',(59.8105032789179,-40.0358564904341,12.));
#58194=CARTESIAN_POINT('Ctrl Pts',(59.8338062259492,-40.0415922549315,0.));
#58195=CARTESIAN_POINT('Ctrl Pts',(59.8338062259492,-40.0415922549315,12.));
#58196=CARTESIAN_POINT('Ctrl Pts',(59.8571558639145,-40.0473153509324,0.));
#58197=CARTESIAN_POINT('Ctrl Pts',(59.8571558639145,-40.0473153509324,12.));
#58198=CARTESIAN_POINT('Ctrl Pts',(59.8805520915972,-40.0530256909161,0.));
#58199=CARTESIAN_POINT('Ctrl Pts',(59.8805520915972,-40.0530256909161,12.));
#58200=CARTESIAN_POINT('Ctrl Pts',(59.9039948081428,-40.0587231877959,0.));
#58201=CARTESIAN_POINT('Ctrl Pts',(59.9039948081428,-40.0587231877959,12.));
#58202=CARTESIAN_POINT('Ctrl Pts',(59.927483913055,-40.0644077549158,0.));
#58203=CARTESIAN_POINT('Ctrl Pts',(59.927483913055,-40.0644077549158,12.));
#58204=CARTESIAN_POINT('Ctrl Pts',(59.9510193061929,-40.0700793060475,0.));
#58205=CARTESIAN_POINT('Ctrl Pts',(59.9510193061929,-40.0700793060475,12.));
#58206=CARTESIAN_POINT('Ctrl Pts',(59.974600887759,-40.0757377553894,0.));
#58207=CARTESIAN_POINT('Ctrl Pts',(59.974600887759,-40.0757377553894,12.));
#58208=CARTESIAN_POINT('Ctrl Pts',(59.9982285582991,-40.0813830175629,0.));
#58209=CARTESIAN_POINT('Ctrl Pts',(59.9982285582991,-40.0813830175629,12.));
#58210=CARTESIAN_POINT('Ctrl Pts',(60.0219022187066,-40.0870150076078,0.));
#58211=CARTESIAN_POINT('Ctrl Pts',(60.0219022187066,-40.0870150076078,12.));
#58212=CARTESIAN_POINT('Ctrl Pts',(60.0456217702203,-40.0926336409787,0.));
#58213=CARTESIAN_POINT('Ctrl Pts',(60.0456217702203,-40.0926336409787,12.));
#58214=CARTESIAN_POINT('Ctrl Pts',(60.0693871144207,-40.0982388335421,0.));
#58215=CARTESIAN_POINT('Ctrl Pts',(60.0693871144207,-40.0982388335421,12.));
#58216=CARTESIAN_POINT('Ctrl Pts',(60.0931981532194,-40.1038305015764,0.));
#58217=CARTESIAN_POINT('Ctrl Pts',(60.0931981532194,-40.1038305015764,12.));
#58218=CARTESIAN_POINT('Ctrl Pts',(60.1170547888572,-40.1094085617672,0.));
#58219=CARTESIAN_POINT('Ctrl Pts',(60.1170547888572,-40.1094085617672,12.));
#58220=CARTESIAN_POINT('Ctrl Pts',(60.1409569239092,-40.1149729312036,0.));
#58221=CARTESIAN_POINT('Ctrl Pts',(60.1409569239092,-40.1149729312036,12.));
#58222=CARTESIAN_POINT('Ctrl Pts',(60.1649044612829,-40.120523527374,0.));
#58223=CARTESIAN_POINT('Ctrl Pts',(60.1649044612829,-40.120523527374,12.));
#58224=CARTESIAN_POINT('Ctrl Pts',(60.1888973042151,-40.1260602681644,0.));
#58225=CARTESIAN_POINT('Ctrl Pts',(60.1888973042151,-40.1260602681644,12.));
#58226=CARTESIAN_POINT('Ctrl Pts',(60.2129353562617,-40.1315830718575,0.));
#58227=CARTESIAN_POINT('Ctrl Pts',(60.2129353562617,-40.1315830718575,12.));
#58228=CARTESIAN_POINT('Ctrl Pts',(60.2370185212957,-40.13709185713,0.));
#58229=CARTESIAN_POINT('Ctrl Pts',(60.2370185212957,-40.13709185713,12.));
#58230=CARTESIAN_POINT('Ctrl Pts',(60.2611467035109,-40.1425865430468,0.));
#58231=CARTESIAN_POINT('Ctrl Pts',(60.2611467035109,-40.1425865430468,12.));
#58232=CARTESIAN_POINT('Ctrl Pts',(60.2853198074215,-40.1480670490583,0.));
#58233=CARTESIAN_POINT('Ctrl Pts',(60.2853198074215,-40.1480670490583,12.));
#58234=CARTESIAN_POINT('Ctrl Pts',(60.3095377378589,-40.1535332949978,0.));
#58235=CARTESIAN_POINT('Ctrl Pts',(60.3095377378589,-40.1535332949978,12.));
#58236=CARTESIAN_POINT('Ctrl Pts',(60.3338003999616,-40.1589852010811,0.));
#58237=CARTESIAN_POINT('Ctrl Pts',(60.3338003999616,-40.1589852010811,12.));
#58238=CARTESIAN_POINT('Ctrl Pts',(60.3581076991731,-40.1644226879043,0.));
#58239=CARTESIAN_POINT('Ctrl Pts',(60.3581076991731,-40.1644226879043,12.));
#58240=CARTESIAN_POINT('Ctrl Pts',(60.382459541246,-40.1698456764387,0.));
#58241=CARTESIAN_POINT('Ctrl Pts',(60.382459541246,-40.1698456764387,12.));
#58242=CARTESIAN_POINT('Ctrl Pts',(60.4068558322414,-40.1752540880273,0.));
#58243=CARTESIAN_POINT('Ctrl Pts',(60.4068558322414,-40.1752540880273,12.));
#58244=CARTESIAN_POINT('Ctrl Pts',(60.4312964785269,-40.1806478443829,0.));
#58245=CARTESIAN_POINT('Ctrl Pts',(60.4312964785269,-40.1806478443829,12.));
#58246=CARTESIAN_POINT('Ctrl Pts',(60.4557813867677,-40.1860268675876,0.));
#58247=CARTESIAN_POINT('Ctrl Pts',(60.4557813867677,-40.1860268675876,12.));
#58248=CARTESIAN_POINT('Ctrl Pts',(60.4803104639211,-40.1913910800912,0.));
#58249=CARTESIAN_POINT('Ctrl Pts',(60.4803104639211,-40.1913910800912,12.));
#58250=CARTESIAN_POINT('Ctrl Pts',(60.5048836172423,-40.1967404047055,0.));
#58251=CARTESIAN_POINT('Ctrl Pts',(60.5048836172423,-40.1967404047055,12.));
#58252=CARTESIAN_POINT('Ctrl Pts',(60.5295007542838,-40.2020747646012,0.));
#58253=CARTESIAN_POINT('Ctrl Pts',(60.5295007542838,-40.2020747646012,12.));
#58254=CARTESIAN_POINT('Ctrl Pts',(60.5541617828927,-40.2073940833054,0.));
#58255=CARTESIAN_POINT('Ctrl Pts',(60.5541617828927,-40.2073940833054,12.));
#58256=CARTESIAN_POINT('Ctrl Pts',(60.5788666112043,-40.2126982847012,0.));
#58257=CARTESIAN_POINT('Ctrl Pts',(60.5788666112043,-40.2126982847012,12.));
#58258=CARTESIAN_POINT('Ctrl Pts',(60.6036151476347,-40.2179872930272,0.));
#58259=CARTESIAN_POINT('Ctrl Pts',(60.6036151476347,-40.2179872930272,12.));
#58260=CARTESIAN_POINT('Ctrl Pts',(60.6284073008865,-40.2232610328717,0.));
#58261=CARTESIAN_POINT('Ctrl Pts',(60.6284073008865,-40.2232610328717,12.));
#58262=CARTESIAN_POINT('Ctrl Pts',(60.6532429799493,-40.2285194291702,0.));
#58263=CARTESIAN_POINT('Ctrl Pts',(60.6532429799493,-40.2285194291702,12.));
#58264=CARTESIAN_POINT('Ctrl Pts',(60.6781220940979,-40.2337624072029,0.));
#58265=CARTESIAN_POINT('Ctrl Pts',(60.6781220940979,-40.2337624072029,12.));
#58266=CARTESIAN_POINT('Ctrl Pts',(60.7030445528863,-40.2389898925937,0.));
#58267=CARTESIAN_POINT('Ctrl Pts',(60.7030445528863,-40.2389898925937,12.));
#58268=CARTESIAN_POINT('Ctrl Pts',(60.72801026614,-40.2442018113116,0.));
#58269=CARTESIAN_POINT('Ctrl Pts',(60.72801026614,-40.2442018113116,12.));
#58270=CARTESIAN_POINT('Ctrl Pts',(60.7530191439603,-40.2493980896646,0.));
#58271=CARTESIAN_POINT('Ctrl Pts',(60.7530191439603,-40.2493980896646,12.));
#58272=CARTESIAN_POINT('Ctrl Pts',(60.7780710967253,-40.2545786542957,0.));
#58273=CARTESIAN_POINT('Ctrl Pts',(60.7780710967253,-40.2545786542957,12.));
#58274=CARTESIAN_POINT('Ctrl Pts',(60.8031660350878,-40.2597434321804,0.));
#58275=CARTESIAN_POINT('Ctrl Pts',(60.8031660350878,-40.2597434321804,12.));
#58276=CARTESIAN_POINT('Ctrl Pts',(60.8283038699703,-40.2648923506245,0.));
#58277=CARTESIAN_POINT('Ctrl Pts',(60.8283038699703,-40.2648923506245,12.));
#58278=CARTESIAN_POINT('Ctrl Pts',(60.8534845125535,-40.2700253372644,0.));
#58279=CARTESIAN_POINT('Ctrl Pts',(60.8534845125535,-40.2700253372644,12.));
#58280=CARTESIAN_POINT('Ctrl Pts',(60.8787078742817,-40.2751423200637,0.));
#58281=CARTESIAN_POINT('Ctrl Pts',(60.8787078742817,-40.2751423200637,12.));
#58282=CARTESIAN_POINT('Ctrl Pts',(60.903973866867,-40.2802432273105,0.));
#58283=CARTESIAN_POINT('Ctrl Pts',(60.903973866867,-40.2802432273105,12.));
#58284=CARTESIAN_POINT('Ctrl Pts',(60.9292824022888,-40.2853279876162,0.));
#58285=CARTESIAN_POINT('Ctrl Pts',(60.9292824022888,-40.2853279876162,12.));
#58286=CARTESIAN_POINT('Ctrl Pts',(60.9546333927919,-40.2903965299155,0.));
#58287=CARTESIAN_POINT('Ctrl Pts',(60.9546333927919,-40.2903965299155,12.));
#58288=CARTESIAN_POINT('Ctrl Pts',(60.9800267508781,-40.2954487834688,0.));
#58289=CARTESIAN_POINT('Ctrl Pts',(60.9800267508781,-40.2954487834688,12.));
#58290=CARTESIAN_POINT('Ctrl Pts',(61.0054623893059,-40.3004846778577,0.));
#58291=CARTESIAN_POINT('Ctrl Pts',(61.0054623893059,-40.3004846778577,12.));
#58292=CARTESIAN_POINT('Ctrl Pts',(61.0309402210915,-40.3055041429772,0.));
#58293=CARTESIAN_POINT('Ctrl Pts',(61.0309402210915,-40.3055041429772,12.));
#58294=CARTESIAN_POINT('Ctrl Pts',(61.0564601595047,-40.3105071090308,0.));
#58295=CARTESIAN_POINT('Ctrl Pts',(61.0564601595047,-40.3105071090308,12.));
#58296=CARTESIAN_POINT('Ctrl Pts',(61.0820221180646,-40.3154935065264,0.));
#58297=CARTESIAN_POINT('Ctrl Pts',(61.0820221180646,-40.3154935065264,12.));
#58298=CARTESIAN_POINT('Ctrl Pts',(61.1076260105265,-40.3204632662729,0.));
#58299=CARTESIAN_POINT('Ctrl Pts',(61.1076260105265,-40.3204632662729,12.));
#58300=CARTESIAN_POINT('Ctrl Pts',(61.1332717508799,-40.3254163193806,0.));
#58301=CARTESIAN_POINT('Ctrl Pts',(61.1332717508799,-40.3254163193806,12.));
#58302=CARTESIAN_POINT('Ctrl Pts',(61.1589592533623,-40.3303525972621,0.));
#58303=CARTESIAN_POINT('Ctrl Pts',(61.1589592533623,-40.3303525972621,12.));
#58304=CARTESIAN_POINT('Ctrl Pts',(61.184688432465,-40.3352720316373,0.));
#58305=CARTESIAN_POINT('Ctrl Pts',(61.184688432465,-40.3352720316373,12.));
#58306=CARTESIAN_POINT('Ctrl Pts',(61.2104592029375,-40.3401745545369,0.));
#58307=CARTESIAN_POINT('Ctrl Pts',(61.2104592029375,-40.3401745545369,12.));
#58308=CARTESIAN_POINT('Ctrl Pts',(61.236271479789,-40.3450600983104,0.));
#58309=CARTESIAN_POINT('Ctrl Pts',(61.236271479789,-40.3450600983104,12.));
#58310=CARTESIAN_POINT('Ctrl Pts',(61.2621251782849,-40.3499285956297,0.));
#58311=CARTESIAN_POINT('Ctrl Pts',(61.2621251782849,-40.3499285956297,12.));
#58312=CARTESIAN_POINT('Ctrl Pts',(61.2880202139358,-40.3547799794672,0.));
#58313=CARTESIAN_POINT('Ctrl Pts',(61.2880202139358,-40.3547799794672,12.));
#58314=CARTESIAN_POINT('Ctrl Pts',(61.3139565024838,-40.3596141830786,0.));
#58315=CARTESIAN_POINT('Ctrl Pts',(61.3139565024838,-40.3596141830786,12.));
#58316=CARTESIAN_POINT('Ctrl Pts',(61.3399339598851,-40.3644311399861,0.));
#58317=CARTESIAN_POINT('Ctrl Pts',(61.3399339598851,-40.3644311399861,12.));
#58318=CARTESIAN_POINT('Ctrl Pts',(61.3659525022917,-40.3692307839642,0.));
#58319=CARTESIAN_POINT('Ctrl Pts',(61.3659525022917,-40.3692307839642,12.));
#58320=CARTESIAN_POINT('Ctrl Pts',(61.3920120460232,-40.3740130490233,0.));
#58321=CARTESIAN_POINT('Ctrl Pts',(61.3920120460232,-40.3740130490233,12.));
#58322=CARTESIAN_POINT('Ctrl Pts',(61.418112507605,-40.3787778694373,0.));
#58323=CARTESIAN_POINT('Ctrl Pts',(61.418112507605,-40.3787778694373,12.));
#58324=CARTESIAN_POINT('Ctrl Pts',(61.4442538038053,-40.3835251797726,0.));
#58325=CARTESIAN_POINT('Ctrl Pts',(61.4442538038053,-40.3835251797726,12.));
#58326=CARTESIAN_POINT('Ctrl Pts',(61.4704358516711,-40.3882549149229,0.));
#58327=CARTESIAN_POINT('Ctrl Pts',(61.4704358516711,-40.3882549149229,12.));
#58328=CARTESIAN_POINT('Ctrl Pts',(61.4966585685544,-40.3929670101363,0.));
#58329=CARTESIAN_POINT('Ctrl Pts',(61.4966585685544,-40.3929670101363,12.));
#58330=CARTESIAN_POINT('Ctrl Pts',(61.5229218721532,-40.3976614010648,0.));
#58331=CARTESIAN_POINT('Ctrl Pts',(61.5229218721532,-40.3976614010648,12.));
#58332=CARTESIAN_POINT('Ctrl Pts',(61.5492256804709,-40.4023380237227,0.));
#58333=CARTESIAN_POINT('Ctrl Pts',(61.5492256804709,-40.4023380237227,12.));
#58334=CARTESIAN_POINT('Ctrl Pts',(61.5755699117318,-40.4069968143953,0.));
#58335=CARTESIAN_POINT('Ctrl Pts',(61.5755699117318,-40.4069968143953,12.));
#58336=CARTESIAN_POINT('Ctrl Pts',(61.6019544843008,-40.4116377095595,0.));
#58337=CARTESIAN_POINT('Ctrl Pts',(61.6019544843008,-40.4116377095595,12.));
#58338=CARTESIAN_POINT('Ctrl Pts',(61.628379316608,-40.4162606458119,0.));
#58339=CARTESIAN_POINT('Ctrl Pts',(61.628379316608,-40.4162606458119,12.));
#58340=CARTESIAN_POINT('Ctrl Pts',(61.6548443270397,-40.420865559772,0.));
#58341=CARTESIAN_POINT('Ctrl Pts',(61.6548443270397,-40.420865559772,12.));
#58342=CARTESIAN_POINT('Ctrl Pts',(61.6813494339295,-40.4254523880766,0.));
#58343=CARTESIAN_POINT('Ctrl Pts',(61.6813494339295,-40.4254523880766,12.));
#58344=CARTESIAN_POINT('Ctrl Pts',(61.7078945557812,-40.4300210675848,0.));
#58345=CARTESIAN_POINT('Ctrl Pts',(61.7078945557812,-40.4300210675848,12.));
#58346=CARTESIAN_POINT('Ctrl Pts',(61.7344796114409,-40.4345715355411,0.));
#58347=CARTESIAN_POINT('Ctrl Pts',(61.7344796114409,-40.4345715355411,12.));
#58348=CARTESIAN_POINT('Ctrl Pts',(61.7611045202875,-40.439103729759,0.));
#58349=CARTESIAN_POINT('Ctrl Pts',(61.7611045202875,-40.439103729759,12.));
#58350=CARTESIAN_POINT('Ctrl Pts',(61.7877692024064,-40.4436175887943,0.));
#58351=CARTESIAN_POINT('Ctrl Pts',(61.7877692024064,-40.4436175887943,12.));
#58352=CARTESIAN_POINT('Ctrl Pts',(61.8144735787767,-40.448113052135,0.));
#58353=CARTESIAN_POINT('Ctrl Pts',(61.8144735787767,-40.448113052135,12.));
#58354=CARTESIAN_POINT('Ctrl Pts',(61.8412175708523,-40.4525900597877,0.));
#58355=CARTESIAN_POINT('Ctrl Pts',(61.8412175708523,-40.4525900597877,12.));
#58356=CARTESIAN_POINT('Ctrl Pts',(61.8680011001513,-40.4570485518735,0.));
#58357=CARTESIAN_POINT('Ctrl Pts',(61.8680011001513,-40.4570485518735,12.));
#58358=CARTESIAN_POINT('Ctrl Pts',(61.8948240877998,-40.4614884681884,0.));
#58359=CARTESIAN_POINT('Ctrl Pts',(61.8948240877998,-40.4614884681884,12.));
#58360=CARTESIAN_POINT('Ctrl Pts',(61.9216864541758,-40.4659097478595,0.));
#58361=CARTESIAN_POINT('Ctrl Pts',(61.9216864541758,-40.4659097478595,12.));
#58362=CARTESIAN_POINT('Ctrl Pts',(61.9485881182957,-40.4703123287642,0.));
#58363=CARTESIAN_POINT('Ctrl Pts',(61.9485881182957,-40.4703123287642,12.));
#58364=CARTESIAN_POINT('Ctrl Pts',(61.9755289983093,-40.4746961480045,0.));
#58365=CARTESIAN_POINT('Ctrl Pts',(61.9755289983093,-40.4746961480045,12.));
#58366=CARTESIAN_POINT('Ctrl Pts',(62.0025090126008,-40.4790611429613,0.));
#58367=CARTESIAN_POINT('Ctrl Pts',(62.0025090126008,-40.4790611429613,12.));
#58368=CARTESIAN_POINT('Ctrl Pts',(62.0295280807449,-40.4834072522182,0.));
#58369=CARTESIAN_POINT('Ctrl Pts',(62.0295280807449,-40.4834072522182,12.));
#58370=CARTESIAN_POINT('Ctrl Pts',(62.0565861244171,-40.4877344164407,0.));
#58371=CARTESIAN_POINT('Ctrl Pts',(62.0565861244171,-40.4877344164407,12.));
#58372=CARTESIAN_POINT('Ctrl Pts',(62.0836830685665,-40.4920425795184,0.));
#58373=CARTESIAN_POINT('Ctrl Pts',(62.0836830685665,-40.4920425795184,12.));
#58374=CARTESIAN_POINT('Ctrl Pts',(62.110818841691,-40.4963316888357,0.));
#58375=CARTESIAN_POINT('Ctrl Pts',(62.110818841691,-40.4963316888357,12.));
#58376=CARTESIAN_POINT('Ctrl Pts',(62.137993373242,-40.500601692749,0.));
#58377=CARTESIAN_POINT('Ctrl Pts',(62.137993373242,-40.500601692749,12.));
#58378=CARTESIAN_POINT('Ctrl Pts',(62.1652065915724,-40.5048525385985,0.));
#58379=CARTESIAN_POINT('Ctrl Pts',(62.1652065915724,-40.5048525385985,12.));
#58380=CARTESIAN_POINT('Ctrl Pts',(62.1924584215634,-40.5090841704111,0.));
#58381=CARTESIAN_POINT('Ctrl Pts',(62.1924584215634,-40.5090841704111,12.));
#58382=CARTESIAN_POINT('Ctrl Pts',(62.2197487826212,-40.5132965269679,0.));
#58383=CARTESIAN_POINT('Ctrl Pts',(62.2197487826212,-40.5132965269679,12.));
#58384=CARTESIAN_POINT('Ctrl Pts',(62.2470775858834,-40.5174895391059,0.));
#58385=CARTESIAN_POINT('Ctrl Pts',(62.2470775858834,-40.5174895391059,12.));
#58386=CARTESIAN_POINT('Ctrl Pts',(62.2744447382207,-40.5216631336335,0.));
#58387=CARTESIAN_POINT('Ctrl Pts',(62.2744447382207,-40.5216631336335,12.));
#58388=CARTESIAN_POINT('Ctrl Pts',(62.3018501471876,-40.5258172381565,0.));
#58389=CARTESIAN_POINT('Ctrl Pts',(62.3018501471876,-40.5258172381565,12.));
#58390=CARTESIAN_POINT('Ctrl Pts',(62.3292937258021,-40.5299517857793,0.));
#58391=CARTESIAN_POINT('Ctrl Pts',(62.3292937258021,-40.5299517857793,12.));
#58392=CARTESIAN_POINT('Ctrl Pts',(62.35677539702,-40.5340667194272,0.));
#58393=CARTESIAN_POINT('Ctrl Pts',(62.35677539702,-40.5340667194272,12.));
#58394=CARTESIAN_POINT('Ctrl Pts',(62.3842950992504,-40.5381619973972,0.));
#58395=CARTESIAN_POINT('Ctrl Pts',(62.3842950992504,-40.5381619973972,12.));
#58396=CARTESIAN_POINT('Ctrl Pts',(62.4118527880601,-40.5422375944697,0.));
#58397=CARTESIAN_POINT('Ctrl Pts',(62.4118527880601,-40.5422375944697,12.));
#58398=CARTESIAN_POINT('Ctrl Pts',(62.439448432904,-40.5462934972335,0.));
#58399=CARTESIAN_POINT('Ctrl Pts',(62.439448432904,-40.5462934972335,12.));
#58400=CARTESIAN_POINT('Ctrl Pts',(62.4615552986669,-40.5495224601437,0.));
#58401=CARTESIAN_POINT('Ctrl Pts',(62.4615552986669,-40.5495224601437,12.));
#58402=CARTESIAN_POINT('Ctrl Pts',(62.4781525155997,-40.5519353177058,0.));
#58403=CARTESIAN_POINT('Ctrl Pts',(62.4781525155997,-40.5519353177058,12.));
#58404=CARTESIAN_POINT('Ctrl Pts',(62.4892249121863,-40.5535399497449,0.));
#58405=CARTESIAN_POINT('Ctrl Pts',(62.4892249121863,-40.5535399497449,12.));
#58406=CARTESIAN_POINT('Ctrl Pts',(62.4947630068039,-40.554341280847,0.));
#58407=CARTESIAN_POINT('Ctrl Pts',(62.4947630068039,-40.554341280847,12.));
#58408=CARTESIAN_POINT('',(57.8261117662438,-39.4479504917287,0.));
#58409=CARTESIAN_POINT('Ctrl Pts',(57.8261117662438,-39.4479504917287,0.));
#58410=CARTESIAN_POINT('Ctrl Pts',(57.8297740100947,-39.4492429618443,0.));
#58411=CARTESIAN_POINT('Ctrl Pts',(57.837104315141,-39.4518277003553,0.));
#58412=CARTESIAN_POINT('Ctrl Pts',(57.8481172247495,-39.4557042029652,0.));
#58413=CARTESIAN_POINT('Ctrl Pts',(57.8628360096803,-39.4608716627118,0.));
#58414=CARTESIAN_POINT('Ctrl Pts',(57.8812926637177,-39.4673289592259,0.));
#58415=CARTESIAN_POINT('Ctrl Pts',(57.8998074670478,-39.473784194937,0.));
#58416=CARTESIAN_POINT('Ctrl Pts',(57.9183803632403,-39.4802373061058,0.));
#58417=CARTESIAN_POINT('Ctrl Pts',(57.937011245663,-39.4866881842317,0.));
#58418=CARTESIAN_POINT('Ctrl Pts',(57.9556999583892,-39.4931366776714,0.));
#58419=CARTESIAN_POINT('Ctrl Pts',(57.974446317937,-39.499582610674,0.));
#58420=CARTESIAN_POINT('Ctrl Pts',(57.9932501298522,-39.5060257981225,0.));
#58421=CARTESIAN_POINT('Ctrl Pts',(58.0121112067895,-39.5124660614976,0.));
#58422=CARTESIAN_POINT('Ctrl Pts',(58.0310293875262,-39.5189032457184,0.));
#58423=CARTESIAN_POINT('Ctrl Pts',(58.0500045308412,-39.5253372136887,0.));
#58424=CARTESIAN_POINT('Ctrl Pts',(58.0690365065374,-39.5317678383217,0.));
#58425=CARTESIAN_POINT('Ctrl Pts',(58.088125187992,-39.5381949959221,0.));
#58426=CARTESIAN_POINT('Ctrl Pts',(58.1072704428928,-39.5446185579638,0.));
#58427=CARTESIAN_POINT('Ctrl Pts',(58.126472128574,-39.5510383869505,0.));
#58428=CARTESIAN_POINT('Ctrl Pts',(58.1457300968499,-39.5574543406982,0.));
#58429=CARTESIAN_POINT('Ctrl Pts',(58.1650441970387,-39.563866275018,0.));
#58430=CARTESIAN_POINT('Ctrl Pts',(58.1844142794338,-39.5702740467999,0.));
#58431=CARTESIAN_POINT('Ctrl Pts',(58.2038401992457,-39.57667751752,0.));
#58432=CARTESIAN_POINT('Ctrl Pts',(58.2233218164365,-39.5830765530891,0.));
#58433=CARTESIAN_POINT('Ctrl Pts',(58.2428589938369,-39.5894710221713,0.));
#58434=CARTESIAN_POINT('Ctrl Pts',(58.2624515958419,-39.5958607950239,0.));
#58435=CARTESIAN_POINT('Ctrl Pts',(58.2820994868118,-39.602245742079,0.));
#58436=CARTESIAN_POINT('Ctrl Pts',(58.3018025297323,-39.6086257327583,0.));
#58437=CARTESIAN_POINT('Ctrl Pts',(58.3215605869221,-39.6150006360915,0.));
#58438=CARTESIAN_POINT('Ctrl Pts',(58.3413735206423,-39.6213703212531,0.));
#58439=CARTESIAN_POINT('Ctrl Pts',(58.3612411936904,-39.6277346580892,0.));
#58440=CARTESIAN_POINT('Ctrl Pts',(58.3811634701037,-39.6340935177476,0.));
#58441=CARTESIAN_POINT('Ctrl Pts',(58.4011402154196,-39.6404467729094,0.));
#58442=CARTESIAN_POINT('Ctrl Pts',(58.4211712963004,-39.6467942974451,0.));
#58443=CARTESIAN_POINT('Ctrl Pts',(58.4412565802979,-39.653135966204,0.));
#58444=CARTESIAN_POINT('Ctrl Pts',(58.4613959355788,-39.6594716547689,0.));
#58445=CARTESIAN_POINT('Ctrl Pts',(58.4815892306066,-39.6658012391815,0.));
#58446=CARTESIAN_POINT('Ctrl Pts',(58.5018363341604,-39.6721245959531,0.));
#58447=CARTESIAN_POINT('Ctrl Pts',(58.5221371154761,-39.6784416021826,0.));
#58448=CARTESIAN_POINT('Ctrl Pts',(58.5424914443415,-39.6847521356395,0.));
#58449=CARTESIAN_POINT('Ctrl Pts',(58.5628991912052,-39.6910560748629,0.));
#58450=CARTESIAN_POINT('Ctrl Pts',(58.5833602272743,-39.697353299254,0.));
#58451=CARTESIAN_POINT('Ctrl Pts',(58.6038744244659,-39.7036436890233,0.));
#58452=CARTESIAN_POINT('Ctrl Pts',(58.6244416553562,-39.7099271251413,0.));
#58453=CARTESIAN_POINT('Ctrl Pts',(58.6450617931274,-39.71620348929,0.));
#58454=CARTESIAN_POINT('Ctrl Pts',(58.6657347115034,-39.7224726638101,0.));
#58455=CARTESIAN_POINT('Ctrl Pts',(58.6864602847088,-39.7287345316681,0.));
#58456=CARTESIAN_POINT('Ctrl Pts',(58.7072383875027,-39.734988976475,0.));
#58457=CARTESIAN_POINT('Ctrl Pts',(58.7280688951916,-39.7412358824953,0.));
#58458=CARTESIAN_POINT('Ctrl Pts',(58.7489516836445,-39.7474751346599,0.));
#58459=CARTESIAN_POINT('Ctrl Pts',(58.7698866293029,-39.7537066185813,0.));
#58460=CARTESIAN_POINT('Ctrl Pts',(58.7908736091798,-39.7599302205521,0.));
#58461=CARTESIAN_POINT('Ctrl Pts',(58.8119125008517,-39.7661458275274,0.));
#58462=CARTESIAN_POINT('Ctrl Pts',(58.8330031824453,-39.772353327112,0.));
#58463=CARTESIAN_POINT('Ctrl Pts',(58.8541455326231,-39.7785526075479,0.));
#58464=CARTESIAN_POINT('Ctrl Pts',(58.8753394305585,-39.7847435576997,0.));
#58465=CARTESIAN_POINT('Ctrl Pts',(58.8965847559391,-39.7909260670517,0.));
#58466=CARTESIAN_POINT('Ctrl Pts',(58.9178813889703,-39.7971000257044,0.));
#58467=CARTESIAN_POINT('Ctrl Pts',(58.9392292103747,-39.8032653243712,0.));
#58468=CARTESIAN_POINT('Ctrl Pts',(58.9606281013875,-39.8094218543782,0.));
#58469=CARTESIAN_POINT('Ctrl Pts',(58.9820779437484,-39.8155695076626,0.));
#58470=CARTESIAN_POINT('Ctrl Pts',(59.0035786197024,-39.821708176766,0.));
#58471=CARTESIAN_POINT('Ctrl Pts',(59.0251300119973,-39.8278377548262,0.));
#58472=CARTESIAN_POINT('Ctrl Pts',(59.0467320038784,-39.8339581355716,0.));
#58473=CARTESIAN_POINT('Ctrl Pts',(59.0683844790764,-39.8400692133139,0.));
#58474=CARTESIAN_POINT('Ctrl Pts',(59.090087321798,-39.8461708829456,0.));
#58475=CARTESIAN_POINT('Ctrl Pts',(59.1118404167292,-39.8522630399328,0.));
#58476=CARTESIAN_POINT('Ctrl Pts',(59.1336436490342,-39.8583455803105,0.));
#58477=CARTESIAN_POINT('Ctrl Pts',(59.1554969043522,-39.8644184006787,0.));
#58478=CARTESIAN_POINT('Ctrl Pts',(59.1774000687879,-39.8704813981989,0.));
#58479=CARTESIAN_POINT('Ctrl Pts',(59.1993530289028,-39.876534470591,0.));
#58480=CARTESIAN_POINT('Ctrl Pts',(59.2213556717209,-39.8825775161267,0.));
#58481=CARTESIAN_POINT('Ctrl Pts',(59.2434078847247,-39.8886104336242,0.));
#58482=CARTESIAN_POINT('Ctrl Pts',(59.2655095558521,-39.8946331224438,0.));
#58483=CARTESIAN_POINT('Ctrl Pts',(59.2876605734846,-39.9006454824845,0.));
#58484=CARTESIAN_POINT('Ctrl Pts',(59.3098608264419,-39.9066474141803,0.));
#58485=CARTESIAN_POINT('Ctrl Pts',(59.3321102039852,-39.9126388184936,0.));
#58486=CARTESIAN_POINT('Ctrl Pts',(59.3544085958151,-39.9186195969104,0.));
#58487=CARTESIAN_POINT('Ctrl Pts',(59.3767558920675,-39.9245896514367,0.));
#58488=CARTESIAN_POINT('Ctrl Pts',(59.3991519833016,-39.9305488845958,0.));
#58489=CARTESIAN_POINT('Ctrl Pts',(59.4215967604967,-39.9364971994242,0.));
#58490=CARTESIAN_POINT('Ctrl Pts',(59.4440901150582,-39.9424344994673,0.));
#58491=CARTESIAN_POINT('Ctrl Pts',(59.4666319388133,-39.9483606887738,0.));
#58492=CARTESIAN_POINT('Ctrl Pts',(59.4892221240068,-39.9542756718922,0.));
#58493=CARTESIAN_POINT('Ctrl Pts',(59.511860563289,-39.9601793538683,0.));
#58494=CARTESIAN_POINT('Ctrl Pts',(59.5345471497128,-39.9660716402403,0.));
#58495=CARTESIAN_POINT('Ctrl Pts',(59.5572817767388,-39.9719524370346,0.));
#58496=CARTESIAN_POINT('Ctrl Pts',(59.5800643382314,-39.9778216507605,0.));
#58497=CARTESIAN_POINT('Ctrl Pts',(59.6028947284562,-39.9836791884079,0.));
#58498=CARTESIAN_POINT('Ctrl Pts',(59.6257728420669,-39.9895249574448,0.));
#58499=CARTESIAN_POINT('Ctrl Pts',(59.6486985741041,-39.9953588658132,0.));
#58500=CARTESIAN_POINT('Ctrl Pts',(59.6716718200005,-40.0011808219241,0.));
#58501=CARTESIAN_POINT('Ctrl Pts',(59.6946924755773,-40.0069907346538,0.));
#58502=CARTESIAN_POINT('Ctrl Pts',(59.7177604370403,-40.0127885133403,0.));
#58503=CARTESIAN_POINT('Ctrl Pts',(59.7408756009679,-40.0185740677821,0.));
#58504=CARTESIAN_POINT('Ctrl Pts',(59.7640378643106,-40.0243473082337,0.));
#58505=CARTESIAN_POINT('Ctrl Pts',(59.7872471243942,-40.0301081454002,0.));
#58506=CARTESIAN_POINT('Ctrl Pts',(59.8105032789179,-40.0358564904341,0.));
#58507=CARTESIAN_POINT('Ctrl Pts',(59.8338062259492,-40.0415922549315,0.));
#58508=CARTESIAN_POINT('Ctrl Pts',(59.8571558639145,-40.0473153509324,0.));
#58509=CARTESIAN_POINT('Ctrl Pts',(59.8805520915972,-40.0530256909161,0.));
#58510=CARTESIAN_POINT('Ctrl Pts',(59.9039948081428,-40.0587231877959,0.));
#58511=CARTESIAN_POINT('Ctrl Pts',(59.927483913055,-40.0644077549158,0.));
#58512=CARTESIAN_POINT('Ctrl Pts',(59.9510193061929,-40.0700793060475,0.));
#58513=CARTESIAN_POINT('Ctrl Pts',(59.974600887759,-40.0757377553894,0.));
#58514=CARTESIAN_POINT('Ctrl Pts',(59.9982285582991,-40.0813830175629,0.));
#58515=CARTESIAN_POINT('Ctrl Pts',(60.0219022187066,-40.0870150076078,0.));
#58516=CARTESIAN_POINT('Ctrl Pts',(60.0456217702203,-40.0926336409787,0.));
#58517=CARTESIAN_POINT('Ctrl Pts',(60.0693871144207,-40.0982388335421,0.));
#58518=CARTESIAN_POINT('Ctrl Pts',(60.0931981532194,-40.1038305015764,0.));
#58519=CARTESIAN_POINT('Ctrl Pts',(60.1170547888572,-40.1094085617672,0.));
#58520=CARTESIAN_POINT('Ctrl Pts',(60.1409569239092,-40.1149729312036,0.));
#58521=CARTESIAN_POINT('Ctrl Pts',(60.1649044612829,-40.120523527374,0.));
#58522=CARTESIAN_POINT('Ctrl Pts',(60.1888973042151,-40.1260602681644,0.));
#58523=CARTESIAN_POINT('Ctrl Pts',(60.2129353562617,-40.1315830718575,0.));
#58524=CARTESIAN_POINT('Ctrl Pts',(60.2370185212957,-40.13709185713,0.));
#58525=CARTESIAN_POINT('Ctrl Pts',(60.2611467035109,-40.1425865430468,0.));
#58526=CARTESIAN_POINT('Ctrl Pts',(60.2853198074215,-40.1480670490583,0.));
#58527=CARTESIAN_POINT('Ctrl Pts',(60.3095377378589,-40.1535332949978,0.));
#58528=CARTESIAN_POINT('Ctrl Pts',(60.3338003999616,-40.1589852010811,0.));
#58529=CARTESIAN_POINT('Ctrl Pts',(60.3581076991731,-40.1644226879043,0.));
#58530=CARTESIAN_POINT('Ctrl Pts',(60.382459541246,-40.1698456764387,0.));
#58531=CARTESIAN_POINT('Ctrl Pts',(60.4068558322414,-40.1752540880273,0.));
#58532=CARTESIAN_POINT('Ctrl Pts',(60.4312964785269,-40.1806478443829,0.));
#58533=CARTESIAN_POINT('Ctrl Pts',(60.4557813867677,-40.1860268675876,0.));
#58534=CARTESIAN_POINT('Ctrl Pts',(60.4803104639211,-40.1913910800912,0.));
#58535=CARTESIAN_POINT('Ctrl Pts',(60.5048836172423,-40.1967404047055,0.));
#58536=CARTESIAN_POINT('Ctrl Pts',(60.5295007542838,-40.2020747646012,0.));
#58537=CARTESIAN_POINT('Ctrl Pts',(60.5541617828927,-40.2073940833054,0.));
#58538=CARTESIAN_POINT('Ctrl Pts',(60.5788666112043,-40.2126982847012,0.));
#58539=CARTESIAN_POINT('Ctrl Pts',(60.6036151476347,-40.2179872930272,0.));
#58540=CARTESIAN_POINT('Ctrl Pts',(60.6284073008865,-40.2232610328717,0.));
#58541=CARTESIAN_POINT('Ctrl Pts',(60.6532429799493,-40.2285194291702,0.));
#58542=CARTESIAN_POINT('Ctrl Pts',(60.6781220940979,-40.2337624072029,0.));
#58543=CARTESIAN_POINT('Ctrl Pts',(60.7030445528863,-40.2389898925937,0.));
#58544=CARTESIAN_POINT('Ctrl Pts',(60.72801026614,-40.2442018113116,0.));
#58545=CARTESIAN_POINT('Ctrl Pts',(60.7530191439603,-40.2493980896646,0.));
#58546=CARTESIAN_POINT('Ctrl Pts',(60.7780710967253,-40.2545786542957,0.));
#58547=CARTESIAN_POINT('Ctrl Pts',(60.8031660350878,-40.2597434321804,0.));
#58548=CARTESIAN_POINT('Ctrl Pts',(60.8283038699703,-40.2648923506245,0.));
#58549=CARTESIAN_POINT('Ctrl Pts',(60.8534845125535,-40.2700253372644,0.));
#58550=CARTESIAN_POINT('Ctrl Pts',(60.8787078742817,-40.2751423200637,0.));
#58551=CARTESIAN_POINT('Ctrl Pts',(60.903973866867,-40.2802432273105,0.));
#58552=CARTESIAN_POINT('Ctrl Pts',(60.9292824022888,-40.2853279876162,0.));
#58553=CARTESIAN_POINT('Ctrl Pts',(60.9546333927919,-40.2903965299155,0.));
#58554=CARTESIAN_POINT('Ctrl Pts',(60.9800267508781,-40.2954487834688,0.));
#58555=CARTESIAN_POINT('Ctrl Pts',(61.0054623893059,-40.3004846778577,0.));
#58556=CARTESIAN_POINT('Ctrl Pts',(61.0309402210915,-40.3055041429772,0.));
#58557=CARTESIAN_POINT('Ctrl Pts',(61.0564601595047,-40.3105071090308,0.));
#58558=CARTESIAN_POINT('Ctrl Pts',(61.0820221180646,-40.3154935065264,0.));
#58559=CARTESIAN_POINT('Ctrl Pts',(61.1076260105265,-40.3204632662729,0.));
#58560=CARTESIAN_POINT('Ctrl Pts',(61.1332717508799,-40.3254163193806,0.));
#58561=CARTESIAN_POINT('Ctrl Pts',(61.1589592533623,-40.3303525972621,0.));
#58562=CARTESIAN_POINT('Ctrl Pts',(61.184688432465,-40.3352720316373,0.));
#58563=CARTESIAN_POINT('Ctrl Pts',(61.2104592029375,-40.3401745545369,0.));
#58564=CARTESIAN_POINT('Ctrl Pts',(61.236271479789,-40.3450600983104,0.));
#58565=CARTESIAN_POINT('Ctrl Pts',(61.2621251782849,-40.3499285956297,0.));
#58566=CARTESIAN_POINT('Ctrl Pts',(61.2880202139358,-40.3547799794672,0.));
#58567=CARTESIAN_POINT('Ctrl Pts',(61.3139565024838,-40.3596141830786,0.));
#58568=CARTESIAN_POINT('Ctrl Pts',(61.3399339598851,-40.3644311399861,0.));
#58569=CARTESIAN_POINT('Ctrl Pts',(61.3659525022917,-40.3692307839642,0.));
#58570=CARTESIAN_POINT('Ctrl Pts',(61.3920120460232,-40.3740130490233,0.));
#58571=CARTESIAN_POINT('Ctrl Pts',(61.418112507605,-40.3787778694373,0.));
#58572=CARTESIAN_POINT('Ctrl Pts',(61.4442538038053,-40.3835251797726,0.));
#58573=CARTESIAN_POINT('Ctrl Pts',(61.4704358516711,-40.3882549149229,0.));
#58574=CARTESIAN_POINT('Ctrl Pts',(61.4966585685544,-40.3929670101363,0.));
#58575=CARTESIAN_POINT('Ctrl Pts',(61.5229218721532,-40.3976614010648,0.));
#58576=CARTESIAN_POINT('Ctrl Pts',(61.5492256804709,-40.4023380237227,0.));
#58577=CARTESIAN_POINT('Ctrl Pts',(61.5755699117318,-40.4069968143953,0.));
#58578=CARTESIAN_POINT('Ctrl Pts',(61.6019544843008,-40.4116377095595,0.));
#58579=CARTESIAN_POINT('Ctrl Pts',(61.628379316608,-40.4162606458119,0.));
#58580=CARTESIAN_POINT('Ctrl Pts',(61.6548443270397,-40.420865559772,0.));
#58581=CARTESIAN_POINT('Ctrl Pts',(61.6813494339295,-40.4254523880766,0.));
#58582=CARTESIAN_POINT('Ctrl Pts',(61.7078945557812,-40.4300210675848,0.));
#58583=CARTESIAN_POINT('Ctrl Pts',(61.7344796114409,-40.4345715355411,0.));
#58584=CARTESIAN_POINT('Ctrl Pts',(61.7611045202875,-40.439103729759,0.));
#58585=CARTESIAN_POINT('Ctrl Pts',(61.7877692024064,-40.4436175887943,0.));
#58586=CARTESIAN_POINT('Ctrl Pts',(61.8144735787767,-40.448113052135,0.));
#58587=CARTESIAN_POINT('Ctrl Pts',(61.8412175708523,-40.4525900597877,0.));
#58588=CARTESIAN_POINT('Ctrl Pts',(61.8680011001513,-40.4570485518735,0.));
#58589=CARTESIAN_POINT('Ctrl Pts',(61.8948240877998,-40.4614884681884,0.));
#58590=CARTESIAN_POINT('Ctrl Pts',(61.9216864541758,-40.4659097478595,0.));
#58591=CARTESIAN_POINT('Ctrl Pts',(61.9485881182957,-40.4703123287642,0.));
#58592=CARTESIAN_POINT('Ctrl Pts',(61.9755289983093,-40.4746961480045,0.));
#58593=CARTESIAN_POINT('Ctrl Pts',(62.0025090126008,-40.4790611429613,0.));
#58594=CARTESIAN_POINT('Ctrl Pts',(62.0295280807449,-40.4834072522182,0.));
#58595=CARTESIAN_POINT('Ctrl Pts',(62.0565861244171,-40.4877344164407,0.));
#58596=CARTESIAN_POINT('Ctrl Pts',(62.0836830685665,-40.4920425795184,0.));
#58597=CARTESIAN_POINT('Ctrl Pts',(62.110818841691,-40.4963316888357,0.));
#58598=CARTESIAN_POINT('Ctrl Pts',(62.1341126810363,-40.499991909619,0.));
#58599=CARTESIAN_POINT('Ctrl Pts',(62.1519925002735,-40.5027877865723,0.));
#58600=CARTESIAN_POINT('Ctrl Pts',(62.1644411502527,-40.5047277935687,0.));
#58601=CARTESIAN_POINT('Ctrl Pts',(62.1714473137748,-40.5058175523045,0.));
#58602=CARTESIAN_POINT('Ctrl Pts',(62.1730054756448,-40.5060598100837,0.));
#58603=CARTESIAN_POINT('',(57.8261117662438,-39.4479504917287,12.));
#58604=CARTESIAN_POINT('',(57.8261117662438,-39.4479504917287,0.));
#58605=CARTESIAN_POINT('Ctrl Pts',(62.1730054756448,-40.5060598100837,12.));
#58606=CARTESIAN_POINT('Ctrl Pts',(62.1714473137748,-40.5058175523045,12.));
#58607=CARTESIAN_POINT('Ctrl Pts',(62.1644411502527,-40.5047277935687,12.));
#58608=CARTESIAN_POINT('Ctrl Pts',(62.1519925002735,-40.5027877865723,12.));
#58609=CARTESIAN_POINT('Ctrl Pts',(62.1341126810363,-40.499991909619,12.));
#58610=CARTESIAN_POINT('Ctrl Pts',(62.110818841691,-40.4963316888357,12.));
#58611=CARTESIAN_POINT('Ctrl Pts',(62.0836830685665,-40.4920425795184,12.));
#58612=CARTESIAN_POINT('Ctrl Pts',(62.0565861244171,-40.4877344164407,12.));
#58613=CARTESIAN_POINT('Ctrl Pts',(62.0295280807449,-40.4834072522182,12.));
#58614=CARTESIAN_POINT('Ctrl Pts',(62.0025090126008,-40.4790611429613,12.));
#58615=CARTESIAN_POINT('Ctrl Pts',(61.9755289983093,-40.4746961480045,12.));
#58616=CARTESIAN_POINT('Ctrl Pts',(61.9485881182957,-40.4703123287642,12.));
#58617=CARTESIAN_POINT('Ctrl Pts',(61.9216864541758,-40.4659097478595,12.));
#58618=CARTESIAN_POINT('Ctrl Pts',(61.8948240877998,-40.4614884681884,12.));
#58619=CARTESIAN_POINT('Ctrl Pts',(61.8680011001513,-40.4570485518735,12.));
#58620=CARTESIAN_POINT('Ctrl Pts',(61.8412175708523,-40.4525900597877,12.));
#58621=CARTESIAN_POINT('Ctrl Pts',(61.8144735787767,-40.448113052135,12.));
#58622=CARTESIAN_POINT('Ctrl Pts',(61.7877692024064,-40.4436175887943,12.));
#58623=CARTESIAN_POINT('Ctrl Pts',(61.7611045202875,-40.439103729759,12.));
#58624=CARTESIAN_POINT('Ctrl Pts',(61.7344796114409,-40.4345715355411,12.));
#58625=CARTESIAN_POINT('Ctrl Pts',(61.7078945557812,-40.4300210675848,12.));
#58626=CARTESIAN_POINT('Ctrl Pts',(61.6813494339295,-40.4254523880766,12.));
#58627=CARTESIAN_POINT('Ctrl Pts',(61.6548443270397,-40.420865559772,12.));
#58628=CARTESIAN_POINT('Ctrl Pts',(61.628379316608,-40.4162606458119,12.));
#58629=CARTESIAN_POINT('Ctrl Pts',(61.6019544843008,-40.4116377095595,12.));
#58630=CARTESIAN_POINT('Ctrl Pts',(61.5755699117318,-40.4069968143953,12.));
#58631=CARTESIAN_POINT('Ctrl Pts',(61.5492256804709,-40.4023380237227,12.));
#58632=CARTESIAN_POINT('Ctrl Pts',(61.5229218721532,-40.3976614010648,12.));
#58633=CARTESIAN_POINT('Ctrl Pts',(61.4966585685544,-40.3929670101363,12.));
#58634=CARTESIAN_POINT('Ctrl Pts',(61.4704358516711,-40.3882549149229,12.));
#58635=CARTESIAN_POINT('Ctrl Pts',(61.4442538038053,-40.3835251797726,12.));
#58636=CARTESIAN_POINT('Ctrl Pts',(61.418112507605,-40.3787778694373,12.));
#58637=CARTESIAN_POINT('Ctrl Pts',(61.3920120460232,-40.3740130490233,12.));
#58638=CARTESIAN_POINT('Ctrl Pts',(61.3659525022917,-40.3692307839642,12.));
#58639=CARTESIAN_POINT('Ctrl Pts',(61.3399339598851,-40.3644311399861,12.));
#58640=CARTESIAN_POINT('Ctrl Pts',(61.3139565024838,-40.3596141830786,12.));
#58641=CARTESIAN_POINT('Ctrl Pts',(61.2880202139358,-40.3547799794672,12.));
#58642=CARTESIAN_POINT('Ctrl Pts',(61.2621251782849,-40.3499285956297,12.));
#58643=CARTESIAN_POINT('Ctrl Pts',(61.236271479789,-40.3450600983104,12.));
#58644=CARTESIAN_POINT('Ctrl Pts',(61.2104592029375,-40.3401745545369,12.));
#58645=CARTESIAN_POINT('Ctrl Pts',(61.184688432465,-40.3352720316373,12.));
#58646=CARTESIAN_POINT('Ctrl Pts',(61.1589592533623,-40.3303525972621,12.));
#58647=CARTESIAN_POINT('Ctrl Pts',(61.1332717508799,-40.3254163193806,12.));
#58648=CARTESIAN_POINT('Ctrl Pts',(61.1076260105265,-40.3204632662729,12.));
#58649=CARTESIAN_POINT('Ctrl Pts',(61.0820221180646,-40.3154935065264,12.));
#58650=CARTESIAN_POINT('Ctrl Pts',(61.0564601595047,-40.3105071090308,12.));
#58651=CARTESIAN_POINT('Ctrl Pts',(61.0309402210915,-40.3055041429772,12.));
#58652=CARTESIAN_POINT('Ctrl Pts',(61.0054623893059,-40.3004846778577,12.));
#58653=CARTESIAN_POINT('Ctrl Pts',(60.9800267508781,-40.2954487834688,12.));
#58654=CARTESIAN_POINT('Ctrl Pts',(60.9546333927919,-40.2903965299155,12.));
#58655=CARTESIAN_POINT('Ctrl Pts',(60.9292824022888,-40.2853279876162,12.));
#58656=CARTESIAN_POINT('Ctrl Pts',(60.903973866867,-40.2802432273105,12.));
#58657=CARTESIAN_POINT('Ctrl Pts',(60.8787078742817,-40.2751423200637,12.));
#58658=CARTESIAN_POINT('Ctrl Pts',(60.8534845125535,-40.2700253372644,12.));
#58659=CARTESIAN_POINT('Ctrl Pts',(60.8283038699703,-40.2648923506245,12.));
#58660=CARTESIAN_POINT('Ctrl Pts',(60.8031660350878,-40.2597434321804,12.));
#58661=CARTESIAN_POINT('Ctrl Pts',(60.7780710967253,-40.2545786542957,12.));
#58662=CARTESIAN_POINT('Ctrl Pts',(60.7530191439603,-40.2493980896646,12.));
#58663=CARTESIAN_POINT('Ctrl Pts',(60.72801026614,-40.2442018113116,12.));
#58664=CARTESIAN_POINT('Ctrl Pts',(60.7030445528863,-40.2389898925937,12.));
#58665=CARTESIAN_POINT('Ctrl Pts',(60.6781220940979,-40.2337624072029,12.));
#58666=CARTESIAN_POINT('Ctrl Pts',(60.6532429799493,-40.2285194291702,12.));
#58667=CARTESIAN_POINT('Ctrl Pts',(60.6284073008865,-40.2232610328717,12.));
#58668=CARTESIAN_POINT('Ctrl Pts',(60.6036151476347,-40.2179872930272,12.));
#58669=CARTESIAN_POINT('Ctrl Pts',(60.5788666112043,-40.2126982847012,12.));
#58670=CARTESIAN_POINT('Ctrl Pts',(60.5541617828927,-40.2073940833054,12.));
#58671=CARTESIAN_POINT('Ctrl Pts',(60.5295007542838,-40.2020747646012,12.));
#58672=CARTESIAN_POINT('Ctrl Pts',(60.5048836172423,-40.1967404047055,12.));
#58673=CARTESIAN_POINT('Ctrl Pts',(60.4803104639211,-40.1913910800912,12.));
#58674=CARTESIAN_POINT('Ctrl Pts',(60.4557813867677,-40.1860268675876,12.));
#58675=CARTESIAN_POINT('Ctrl Pts',(60.4312964785269,-40.1806478443829,12.));
#58676=CARTESIAN_POINT('Ctrl Pts',(60.4068558322414,-40.1752540880273,12.));
#58677=CARTESIAN_POINT('Ctrl Pts',(60.382459541246,-40.1698456764387,12.));
#58678=CARTESIAN_POINT('Ctrl Pts',(60.3581076991731,-40.1644226879043,12.));
#58679=CARTESIAN_POINT('Ctrl Pts',(60.3338003999616,-40.1589852010811,12.));
#58680=CARTESIAN_POINT('Ctrl Pts',(60.3095377378589,-40.1535332949978,12.));
#58681=CARTESIAN_POINT('Ctrl Pts',(60.2853198074215,-40.1480670490583,12.));
#58682=CARTESIAN_POINT('Ctrl Pts',(60.2611467035109,-40.1425865430468,12.));
#58683=CARTESIAN_POINT('Ctrl Pts',(60.2370185212957,-40.13709185713,12.));
#58684=CARTESIAN_POINT('Ctrl Pts',(60.2129353562617,-40.1315830718575,12.));
#58685=CARTESIAN_POINT('Ctrl Pts',(60.1888973042151,-40.1260602681644,12.));
#58686=CARTESIAN_POINT('Ctrl Pts',(60.1649044612829,-40.120523527374,12.));
#58687=CARTESIAN_POINT('Ctrl Pts',(60.1409569239092,-40.1149729312036,12.));
#58688=CARTESIAN_POINT('Ctrl Pts',(60.1170547888572,-40.1094085617672,12.));
#58689=CARTESIAN_POINT('Ctrl Pts',(60.0931981532194,-40.1038305015764,12.));
#58690=CARTESIAN_POINT('Ctrl Pts',(60.0693871144207,-40.0982388335421,12.));
#58691=CARTESIAN_POINT('Ctrl Pts',(60.0456217702203,-40.0926336409787,12.));
#58692=CARTESIAN_POINT('Ctrl Pts',(60.0219022187066,-40.0870150076078,12.));
#58693=CARTESIAN_POINT('Ctrl Pts',(59.9982285582991,-40.0813830175629,12.));
#58694=CARTESIAN_POINT('Ctrl Pts',(59.974600887759,-40.0757377553894,12.));
#58695=CARTESIAN_POINT('Ctrl Pts',(59.9510193061929,-40.0700793060475,12.));
#58696=CARTESIAN_POINT('Ctrl Pts',(59.927483913055,-40.0644077549158,12.));
#58697=CARTESIAN_POINT('Ctrl Pts',(59.9039948081428,-40.0587231877959,12.));
#58698=CARTESIAN_POINT('Ctrl Pts',(59.8805520915972,-40.0530256909161,12.));
#58699=CARTESIAN_POINT('Ctrl Pts',(59.8571558639145,-40.0473153509324,12.));
#58700=CARTESIAN_POINT('Ctrl Pts',(59.8338062259492,-40.0415922549315,12.));
#58701=CARTESIAN_POINT('Ctrl Pts',(59.8105032789179,-40.0358564904341,12.));
#58702=CARTESIAN_POINT('Ctrl Pts',(59.7872471243942,-40.0301081454002,12.));
#58703=CARTESIAN_POINT('Ctrl Pts',(59.7640378643106,-40.0243473082337,12.));
#58704=CARTESIAN_POINT('Ctrl Pts',(59.7408756009679,-40.0185740677821,12.));
#58705=CARTESIAN_POINT('Ctrl Pts',(59.7177604370403,-40.0127885133403,12.));
#58706=CARTESIAN_POINT('Ctrl Pts',(59.6946924755773,-40.0069907346538,12.));
#58707=CARTESIAN_POINT('Ctrl Pts',(59.6716718200005,-40.0011808219241,12.));
#58708=CARTESIAN_POINT('Ctrl Pts',(59.6486985741041,-39.9953588658132,12.));
#58709=CARTESIAN_POINT('Ctrl Pts',(59.6257728420669,-39.9895249574448,12.));
#58710=CARTESIAN_POINT('Ctrl Pts',(59.6028947284562,-39.9836791884079,12.));
#58711=CARTESIAN_POINT('Ctrl Pts',(59.5800643382314,-39.9778216507605,12.));
#58712=CARTESIAN_POINT('Ctrl Pts',(59.5572817767388,-39.9719524370346,12.));
#58713=CARTESIAN_POINT('Ctrl Pts',(59.5345471497128,-39.9660716402403,12.));
#58714=CARTESIAN_POINT('Ctrl Pts',(59.511860563289,-39.9601793538683,12.));
#58715=CARTESIAN_POINT('Ctrl Pts',(59.4892221240068,-39.9542756718922,12.));
#58716=CARTESIAN_POINT('Ctrl Pts',(59.4666319388133,-39.9483606887738,12.));
#58717=CARTESIAN_POINT('Ctrl Pts',(59.4440901150582,-39.9424344994673,12.));
#58718=CARTESIAN_POINT('Ctrl Pts',(59.4215967604967,-39.9364971994242,12.));
#58719=CARTESIAN_POINT('Ctrl Pts',(59.3991519833016,-39.9305488845958,12.));
#58720=CARTESIAN_POINT('Ctrl Pts',(59.3767558920675,-39.9245896514367,12.));
#58721=CARTESIAN_POINT('Ctrl Pts',(59.3544085958151,-39.9186195969104,12.));
#58722=CARTESIAN_POINT('Ctrl Pts',(59.3321102039852,-39.9126388184936,12.));
#58723=CARTESIAN_POINT('Ctrl Pts',(59.3098608264419,-39.9066474141803,12.));
#58724=CARTESIAN_POINT('Ctrl Pts',(59.2876605734846,-39.9006454824845,12.));
#58725=CARTESIAN_POINT('Ctrl Pts',(59.2655095558521,-39.8946331224438,12.));
#58726=CARTESIAN_POINT('Ctrl Pts',(59.2434078847247,-39.8886104336242,12.));
#58727=CARTESIAN_POINT('Ctrl Pts',(59.2213556717209,-39.8825775161267,12.));
#58728=CARTESIAN_POINT('Ctrl Pts',(59.1993530289028,-39.876534470591,12.));
#58729=CARTESIAN_POINT('Ctrl Pts',(59.1774000687879,-39.8704813981989,12.));
#58730=CARTESIAN_POINT('Ctrl Pts',(59.1554969043522,-39.8644184006787,12.));
#58731=CARTESIAN_POINT('Ctrl Pts',(59.1336436490342,-39.8583455803105,12.));
#58732=CARTESIAN_POINT('Ctrl Pts',(59.1118404167292,-39.8522630399328,12.));
#58733=CARTESIAN_POINT('Ctrl Pts',(59.090087321798,-39.8461708829456,12.));
#58734=CARTESIAN_POINT('Ctrl Pts',(59.0683844790764,-39.8400692133139,12.));
#58735=CARTESIAN_POINT('Ctrl Pts',(59.0467320038784,-39.8339581355716,12.));
#58736=CARTESIAN_POINT('Ctrl Pts',(59.0251300119973,-39.8278377548262,12.));
#58737=CARTESIAN_POINT('Ctrl Pts',(59.0035786197024,-39.821708176766,12.));
#58738=CARTESIAN_POINT('Ctrl Pts',(58.9820779437484,-39.8155695076626,12.));
#58739=CARTESIAN_POINT('Ctrl Pts',(58.9606281013875,-39.8094218543782,12.));
#58740=CARTESIAN_POINT('Ctrl Pts',(58.9392292103747,-39.8032653243712,12.));
#58741=CARTESIAN_POINT('Ctrl Pts',(58.9178813889703,-39.7971000257044,12.));
#58742=CARTESIAN_POINT('Ctrl Pts',(58.8965847559391,-39.7909260670517,12.));
#58743=CARTESIAN_POINT('Ctrl Pts',(58.8753394305585,-39.7847435576997,12.));
#58744=CARTESIAN_POINT('Ctrl Pts',(58.8541455326231,-39.7785526075479,12.));
#58745=CARTESIAN_POINT('Ctrl Pts',(58.8330031824453,-39.772353327112,12.));
#58746=CARTESIAN_POINT('Ctrl Pts',(58.8119125008517,-39.7661458275274,12.));
#58747=CARTESIAN_POINT('Ctrl Pts',(58.7908736091798,-39.7599302205521,12.));
#58748=CARTESIAN_POINT('Ctrl Pts',(58.7698866293029,-39.7537066185813,12.));
#58749=CARTESIAN_POINT('Ctrl Pts',(58.7489516836445,-39.7474751346599,12.));
#58750=CARTESIAN_POINT('Ctrl Pts',(58.7280688951916,-39.7412358824953,12.));
#58751=CARTESIAN_POINT('Ctrl Pts',(58.7072383875027,-39.734988976475,12.));
#58752=CARTESIAN_POINT('Ctrl Pts',(58.6864602847088,-39.7287345316681,12.));
#58753=CARTESIAN_POINT('Ctrl Pts',(58.6657347115034,-39.7224726638101,12.));
#58754=CARTESIAN_POINT('Ctrl Pts',(58.6450617931274,-39.71620348929,12.));
#58755=CARTESIAN_POINT('Ctrl Pts',(58.6244416553562,-39.7099271251413,12.));
#58756=CARTESIAN_POINT('Ctrl Pts',(58.6038744244659,-39.7036436890233,12.));
#58757=CARTESIAN_POINT('Ctrl Pts',(58.5833602272743,-39.697353299254,12.));
#58758=CARTESIAN_POINT('Ctrl Pts',(58.5628991912052,-39.6910560748629,12.));
#58759=CARTESIAN_POINT('Ctrl Pts',(58.5424914443415,-39.6847521356395,12.));
#58760=CARTESIAN_POINT('Ctrl Pts',(58.5221371154761,-39.6784416021826,12.));
#58761=CARTESIAN_POINT('Ctrl Pts',(58.5018363341604,-39.6721245959531,12.));
#58762=CARTESIAN_POINT('Ctrl Pts',(58.4815892306066,-39.6658012391815,12.));
#58763=CARTESIAN_POINT('Ctrl Pts',(58.4613959355788,-39.6594716547689,12.));
#58764=CARTESIAN_POINT('Ctrl Pts',(58.4412565802979,-39.653135966204,12.));
#58765=CARTESIAN_POINT('Ctrl Pts',(58.4211712963004,-39.6467942974451,12.));
#58766=CARTESIAN_POINT('Ctrl Pts',(58.4011402154196,-39.6404467729094,12.));
#58767=CARTESIAN_POINT('Ctrl Pts',(58.3811634701037,-39.6340935177476,12.));
#58768=CARTESIAN_POINT('Ctrl Pts',(58.3612411936904,-39.6277346580892,12.));
#58769=CARTESIAN_POINT('Ctrl Pts',(58.3413735206423,-39.6213703212531,12.));
#58770=CARTESIAN_POINT('Ctrl Pts',(58.3215605869221,-39.6150006360915,12.));
#58771=CARTESIAN_POINT('Ctrl Pts',(58.3018025297323,-39.6086257327583,12.));
#58772=CARTESIAN_POINT('Ctrl Pts',(58.2820994868118,-39.602245742079,12.));
#58773=CARTESIAN_POINT('Ctrl Pts',(58.2624515958419,-39.5958607950239,12.));
#58774=CARTESIAN_POINT('Ctrl Pts',(58.2428589938369,-39.5894710221713,12.));
#58775=CARTESIAN_POINT('Ctrl Pts',(58.2233218164365,-39.5830765530891,12.));
#58776=CARTESIAN_POINT('Ctrl Pts',(58.2038401992457,-39.57667751752,12.));
#58777=CARTESIAN_POINT('Ctrl Pts',(58.1844142794338,-39.5702740467999,12.));
#58778=CARTESIAN_POINT('Ctrl Pts',(58.1650441970387,-39.563866275018,12.));
#58779=CARTESIAN_POINT('Ctrl Pts',(58.1457300968499,-39.5574543406982,12.));
#58780=CARTESIAN_POINT('Ctrl Pts',(58.126472128574,-39.5510383869505,12.));
#58781=CARTESIAN_POINT('Ctrl Pts',(58.1072704428928,-39.5446185579638,12.));
#58782=CARTESIAN_POINT('Ctrl Pts',(58.088125187992,-39.5381949959221,12.));
#58783=CARTESIAN_POINT('Ctrl Pts',(58.0690365065374,-39.5317678383217,12.));
#58784=CARTESIAN_POINT('Ctrl Pts',(58.0500045308412,-39.5253372136887,12.));
#58785=CARTESIAN_POINT('Ctrl Pts',(58.0310293875262,-39.5189032457184,12.));
#58786=CARTESIAN_POINT('Ctrl Pts',(58.0121112067895,-39.5124660614976,12.));
#58787=CARTESIAN_POINT('Ctrl Pts',(57.9932501298522,-39.5060257981225,12.));
#58788=CARTESIAN_POINT('Ctrl Pts',(57.974446317937,-39.499582610674,12.));
#58789=CARTESIAN_POINT('Ctrl Pts',(57.9556999583892,-39.4931366776714,12.));
#58790=CARTESIAN_POINT('Ctrl Pts',(57.937011245663,-39.4866881842317,12.));
#58791=CARTESIAN_POINT('Ctrl Pts',(57.9183803632403,-39.4802373061058,12.));
#58792=CARTESIAN_POINT('Ctrl Pts',(57.8998074670478,-39.473784194937,12.));
#58793=CARTESIAN_POINT('Ctrl Pts',(57.8812926637177,-39.4673289592259,12.));
#58794=CARTESIAN_POINT('Ctrl Pts',(57.8628360096803,-39.4608716627118,12.));
#58795=CARTESIAN_POINT('Ctrl Pts',(57.8481172247495,-39.4557042029652,12.));
#58796=CARTESIAN_POINT('Ctrl Pts',(57.837104315141,-39.4518277003553,12.));
#58797=CARTESIAN_POINT('Ctrl Pts',(57.8297740100947,-39.4492429618443,12.));
#58798=CARTESIAN_POINT('Ctrl Pts',(57.8261117662438,-39.4479504917287,12.));
#58799=CARTESIAN_POINT('Ctrl Pts',(62.9864049293894,-39.2292784191813,-5.55111512312578E-16));
#58800=CARTESIAN_POINT('Ctrl Pts',(62.9864049293894,-39.2292784191813,4.));
#58801=CARTESIAN_POINT('Ctrl Pts',(62.9864049293894,-39.2292784191812,8.));
#58802=CARTESIAN_POINT('Ctrl Pts',(62.9864049293894,-39.2292784191812,12.));
#58803=CARTESIAN_POINT('Ctrl Pts',(63.0475916539463,-39.3205491216485,-5.55111512312578E-16));
#58804=CARTESIAN_POINT('Ctrl Pts',(63.0475916539463,-39.3205491216485,4.));
#58805=CARTESIAN_POINT('Ctrl Pts',(63.0475916539463,-39.3205491216485,8.));
#58806=CARTESIAN_POINT('Ctrl Pts',(63.0475916539463,-39.3205491216485,12.));
#58807=CARTESIAN_POINT('Ctrl Pts',(63.0996457958581,-39.5164137621548,-5.55111512312578E-16));
#58808=CARTESIAN_POINT('Ctrl Pts',(63.0996457958581,-39.5164137621548,4.));
#58809=CARTESIAN_POINT('Ctrl Pts',(63.0996457958582,-39.5164137621548,7.99999999999999));
#58810=CARTESIAN_POINT('Ctrl Pts',(63.0996457958582,-39.5164137621548,12.));
#58811=CARTESIAN_POINT('Ctrl Pts',(63.0378706912073,-39.7049575044674,-5.55111512312578E-16));
#58812=CARTESIAN_POINT('Ctrl Pts',(63.0378706912073,-39.7049575044674,4.));
#58813=CARTESIAN_POINT('Ctrl Pts',(63.0378706912074,-39.7049575044674,8.00000000000001));
#58814=CARTESIAN_POINT('Ctrl Pts',(63.0378706912074,-39.7049575044674,12.));
#58815=CARTESIAN_POINT('Ctrl Pts',(62.9938720098781,-39.7746412831476,-5.55111512312578E-16));
#58816=CARTESIAN_POINT('Ctrl Pts',(62.9938720098781,-39.7746412831476,4.));
#58817=CARTESIAN_POINT('Ctrl Pts',(62.9938720098781,-39.7746412831477,8.));
#58818=CARTESIAN_POINT('Ctrl Pts',(62.9938720098781,-39.7746412831477,12.));
#58819=CARTESIAN_POINT('',(62.9864049293894,-39.2292784191813,2.77555756156289E-16));
#58820=CARTESIAN_POINT('',(62.9938720098782,-39.7746412831477,0.));
#58821=CARTESIAN_POINT('Ctrl Pts',(62.9864049293894,-39.2292784191813,-1.38777878078145E-16));
#58822=CARTESIAN_POINT('Ctrl Pts',(63.0475916539463,-39.3205491216485,-1.38777878078145E-16));
#58823=CARTESIAN_POINT('Ctrl Pts',(63.0773368778959,-39.4324717733664,-1.38777878078144E-16));
#58824=CARTESIAN_POINT('Ctrl Pts',(63.0699133682741,-39.5420039277149,-1.38777878078145E-16));
#58825=CARTESIAN_POINT('Ctrl Pts',(63.0643457360577,-39.6241530434763,-1.38777878078145E-16));
#58826=CARTESIAN_POINT('Ctrl Pts',(63.0378706912073,-39.7049575044674,-1.38777878078145E-16));
#58827=CARTESIAN_POINT('Ctrl Pts',(62.9938720098781,-39.7746412831476,-1.38777878078145E-16));
#58828=CARTESIAN_POINT('',(62.9938720098782,-39.7746412831478,12.));
#58829=CARTESIAN_POINT('Ctrl Pts',(62.9938720098781,-39.7746412831476,-5.55111512312578E-16));
#58830=CARTESIAN_POINT('Ctrl Pts',(62.9938720098781,-39.7746412831476,4.));
#58831=CARTESIAN_POINT('Ctrl Pts',(62.9938720098781,-39.7746412831477,8.));
#58832=CARTESIAN_POINT('Ctrl Pts',(62.9938720098781,-39.7746412831477,12.));
#58833=CARTESIAN_POINT('',(62.9864049293894,-39.2292784191812,12.));
#58834=CARTESIAN_POINT('Ctrl Pts',(62.9938720098781,-39.7746412831477,12.));
#58835=CARTESIAN_POINT('Ctrl Pts',(63.0378706912074,-39.7049575044674,12.));
#58836=CARTESIAN_POINT('Ctrl Pts',(63.0643457360577,-39.6241530434763,12.));
#58837=CARTESIAN_POINT('Ctrl Pts',(63.0699133682741,-39.5420039277149,12.));
#58838=CARTESIAN_POINT('Ctrl Pts',(63.077336877896,-39.4324717733664,12.));
#58839=CARTESIAN_POINT('Ctrl Pts',(63.0475916539463,-39.3205491216485,12.));
#58840=CARTESIAN_POINT('Ctrl Pts',(62.9864049293894,-39.2292784191812,12.));
#58841=CARTESIAN_POINT('Ctrl Pts',(62.9864049293894,-39.2292784191812,12.));
#58842=CARTESIAN_POINT('Ctrl Pts',(62.9864049293894,-39.2292784191812,8.));
#58843=CARTESIAN_POINT('Ctrl Pts',(62.9864049293894,-39.2292784191813,4.));
#58844=CARTESIAN_POINT('Ctrl Pts',(62.9864049293894,-39.2292784191813,-5.55111512312578E-16));
#58845=CARTESIAN_POINT('Origin',(3.16193356404481E-10,-2.01319694273778E-10,
0.));
#58846=CARTESIAN_POINT('Origin',(3.16193356404481E-10,-2.01319694273778E-10,
12.));
#58847=CARTESIAN_POINT('Origin',(3.16193356404481E-10,-2.01319694273778E-10,
0.));
#58848=CARTESIAN_POINT('Ctrl Pts',(58.9211100416397,-45.591148170023,-2.77555756156289E-15));
#58849=CARTESIAN_POINT('Ctrl Pts',(58.9211100416397,-45.591148170023,4.));
#58850=CARTESIAN_POINT('Ctrl Pts',(58.9211100416396,-45.591148170023,8.));
#58851=CARTESIAN_POINT('Ctrl Pts',(58.9211100416396,-45.591148170023,12.));
#58852=CARTESIAN_POINT('Ctrl Pts',(58.8538661785413,-45.6780528262178,-2.77555756156289E-15));
#58853=CARTESIAN_POINT('Ctrl Pts',(58.8538661785413,-45.6780528262178,4.));
#58854=CARTESIAN_POINT('Ctrl Pts',(58.8538661785413,-45.6780528262179,8.));
#58855=CARTESIAN_POINT('Ctrl Pts',(58.8538661785413,-45.6780528262179,12.));
#58856=CARTESIAN_POINT('Ctrl Pts',(58.6845061116498,-45.7893619681936,-2.55630692362817E-15));
#58857=CARTESIAN_POINT('Ctrl Pts',(58.6845061116498,-45.7893619681936,4.));
#58858=CARTESIAN_POINT('Ctrl Pts',(58.6845061116497,-45.7893619681937,7.99999999999999));
#58859=CARTESIAN_POINT('Ctrl Pts',(58.6845061116497,-45.7893619681937,12.));
#58860=CARTESIAN_POINT('Ctrl Pts',(58.4861028141709,-45.7903667155979,-2.0357240208649E-15));
#58861=CARTESIAN_POINT('Ctrl Pts',(58.4861028141709,-45.7903667155979,4.));
#58862=CARTESIAN_POINT('Ctrl Pts',(58.4861028141708,-45.790366715598,8.00000000000001));
#58863=CARTESIAN_POINT('Ctrl Pts',(58.4861028141708,-45.790366715598,12.));
#58864=CARTESIAN_POINT('Ctrl Pts',(58.4060826907377,-45.7706564944765,-1.78476208015248E-15));
#58865=CARTESIAN_POINT('Ctrl Pts',(58.4060826907377,-45.7706564944765,4.));
#58866=CARTESIAN_POINT('Ctrl Pts',(58.4060826907376,-45.7706564944766,8.));
#58867=CARTESIAN_POINT('Ctrl Pts',(58.4060826907376,-45.7706564944766,12.));
#58868=CARTESIAN_POINT('',(58.9211100416397,-45.591148170023,2.77555756156289E-16));
#58869=CARTESIAN_POINT('',(58.4060826907377,-45.7706564944766,0.));
#58870=CARTESIAN_POINT('Ctrl Pts',(58.9211100416397,-45.591148170023,-9.71445146547012E-16));
#58871=CARTESIAN_POINT('Ctrl Pts',(58.8538661785413,-45.6780528262178,-9.71445146547012E-16));
#58872=CARTESIAN_POINT('Ctrl Pts',(58.7570889974605,-45.741658050204,-8.46159067727172E-16));
#58873=CARTESIAN_POINT('Ctrl Pts',(58.6508283125143,-45.7692455126974,-6.22478779983725E-16));
#58874=CARTESIAN_POINT('Ctrl Pts',(58.5711327988047,-45.7899361095675,-4.5471856417614E-16));
#58875=CARTESIAN_POINT('Ctrl Pts',(58.4861028141709,-45.7903667155979,-2.31611605849026E-16));
#58876=CARTESIAN_POINT('Ctrl Pts',(58.4060826907377,-45.7706564944765,1.93503348634022E-17));
#58877=CARTESIAN_POINT('',(58.4060826907376,-45.7706564944766,12.));
#58878=CARTESIAN_POINT('Ctrl Pts',(58.4060826907377,-45.7706564944765,-1.78476208015248E-15));
#58879=CARTESIAN_POINT('Ctrl Pts',(58.4060826907377,-45.7706564944765,4.));
#58880=CARTESIAN_POINT('Ctrl Pts',(58.4060826907376,-45.7706564944766,8.));
#58881=CARTESIAN_POINT('Ctrl Pts',(58.4060826907376,-45.7706564944766,12.));
#58882=CARTESIAN_POINT('',(58.9211100416396,-45.591148170023,12.));
#58883=CARTESIAN_POINT('Ctrl Pts',(58.4060826907376,-45.7706564944766,12.));
#58884=CARTESIAN_POINT('Ctrl Pts',(58.4861028141708,-45.790366715598,12.));
#58885=CARTESIAN_POINT('Ctrl Pts',(58.5711327988046,-45.7899361095676,12.));
#58886=CARTESIAN_POINT('Ctrl Pts',(58.6508283125142,-45.7692455126975,12.));
#58887=CARTESIAN_POINT('Ctrl Pts',(58.7570889974604,-45.7416580502041,12.));
#58888=CARTESIAN_POINT('Ctrl Pts',(58.8538661785413,-45.6780528262179,12.));
#58889=CARTESIAN_POINT('Ctrl Pts',(58.9211100416396,-45.591148170023,12.));
#58890=CARTESIAN_POINT('Ctrl Pts',(58.9211100416396,-45.591148170023,12.));
#58891=CARTESIAN_POINT('Ctrl Pts',(58.9211100416396,-45.591148170023,8.));
#58892=CARTESIAN_POINT('Ctrl Pts',(58.9211100416397,-45.591148170023,4.));
#58893=CARTESIAN_POINT('Ctrl Pts',(58.9211100416397,-45.591148170023,-2.77555756156289E-15));
#58894=CARTESIAN_POINT('Ctrl Pts',(54.1679505278134,-44.3377168516418,0.));
#58895=CARTESIAN_POINT('Ctrl Pts',(54.1679505278134,-44.3377168516418,12.));
#58896=CARTESIAN_POINT('Ctrl Pts',(54.1714861895278,-44.3393235891014,0.));
#58897=CARTESIAN_POINT('Ctrl Pts',(54.1714861895278,-44.3393235891014,12.));
#58898=CARTESIAN_POINT('Ctrl Pts',(54.1785633257456,-44.3425373700829,0.));
#58899=CARTESIAN_POINT('Ctrl Pts',(54.1785633257456,-44.3425373700829,12.));
#58900=CARTESIAN_POINT('Ctrl Pts',(54.1891964684439,-44.3473589597468,0.));
#58901=CARTESIAN_POINT('Ctrl Pts',(54.1891964684439,-44.3473589597468,12.));
#58902=CARTESIAN_POINT('Ctrl Pts',(54.203408870162,-44.3537895823819,0.));
#58903=CARTESIAN_POINT('Ctrl Pts',(54.203408870162,-44.3537895823819,12.));
#58904=CARTESIAN_POINT('Ctrl Pts',(54.2212325005847,-44.3618309103245,0.));
#58905=CARTESIAN_POINT('Ctrl Pts',(54.2212325005847,-44.3618309103245,12.));
#58906=CARTESIAN_POINT('Ctrl Pts',(54.2391142386354,-44.369875253351,0.));
#58907=CARTESIAN_POINT('Ctrl Pts',(54.2391142386354,-44.369875253351,12.));
#58908=CARTESIAN_POINT('Ctrl Pts',(54.2570540336536,-44.3779225430461,0.));
#58909=CARTESIAN_POINT('Ctrl Pts',(54.2570540336536,-44.3779225430461,12.));
#58910=CARTESIAN_POINT('Ctrl Pts',(54.2750517888695,-44.3859726620288,0.));
#58911=CARTESIAN_POINT('Ctrl Pts',(54.2750517888695,-44.3859726620288,12.));
#58912=CARTESIAN_POINT('Ctrl Pts',(54.2931073621661,-44.3940254456427,0.));
#58913=CARTESIAN_POINT('Ctrl Pts',(54.2931073621661,-44.3940254456427,12.));
#58914=CARTESIAN_POINT('Ctrl Pts',(54.3112205860776,-44.4020807028144,0.));
#58915=CARTESIAN_POINT('Ctrl Pts',(54.3112205860776,-44.4020807028144,12.));
#58916=CARTESIAN_POINT('Ctrl Pts',(54.3293912830237,-44.4101382321834,0.));
#58917=CARTESIAN_POINT('Ctrl Pts',(54.3293912830237,-44.4101382321834,12.));
#58918=CARTESIAN_POINT('Ctrl Pts',(54.347619281931,-44.4181978395814,0.));
#58919=CARTESIAN_POINT('Ctrl Pts',(54.347619281931,-44.4181978395814,12.));
#58920=CARTESIAN_POINT('Ctrl Pts',(54.3659044357064,-44.4262593564664,0.));
#58921=CARTESIAN_POINT('Ctrl Pts',(54.3659044357064,-44.4262593564664,12.));
#58922=CARTESIAN_POINT('Ctrl Pts',(54.3842466156151,-44.4343226339555,0.));
#58923=CARTESIAN_POINT('Ctrl Pts',(54.3842466156151,-44.4343226339555,12.));
#58924=CARTESIAN_POINT('Ctrl Pts',(54.4026457030316,-44.442387534098,0.));
#58925=CARTESIAN_POINT('Ctrl Pts',(54.4026457030316,-44.442387534098,12.));
#58926=CARTESIAN_POINT('Ctrl Pts',(54.4211015825959,-44.4504539226336,0.));
#58927=CARTESIAN_POINT('Ctrl Pts',(54.4211015825959,-44.4504539226336,12.));
#58928=CARTESIAN_POINT('Ctrl Pts',(54.4396141337008,-44.4585216599933,0.));
#58929=CARTESIAN_POINT('Ctrl Pts',(54.4396141337008,-44.4585216599933,12.));
#58930=CARTESIAN_POINT('Ctrl Pts',(54.4581832262072,-44.4665905967701,0.));
#58931=CARTESIAN_POINT('Ctrl Pts',(54.4581832262072,-44.4665905967701,12.));
#58932=CARTESIAN_POINT('Ctrl Pts',(54.4768087248854,-44.4746605784056,0.));
#58933=CARTESIAN_POINT('Ctrl Pts',(54.4768087248854,-44.4746605784056,12.));
#58934=CARTESIAN_POINT('Ctrl Pts',(54.4954904921938,-44.4827314481271,0.));
#58935=CARTESIAN_POINT('Ctrl Pts',(54.4954904921938,-44.4827314481271,12.));
#58936=CARTESIAN_POINT('Ctrl Pts',(54.5142283914684,-44.4908030503209,0.));
#58937=CARTESIAN_POINT('Ctrl Pts',(54.5142283914684,-44.4908030503209,12.));
#58938=CARTESIAN_POINT('Ctrl Pts',(54.5330222905438,-44.4988752343715,0.));
#58939=CARTESIAN_POINT('Ctrl Pts',(54.5330222905438,-44.4988752343715,12.));
#58940=CARTESIAN_POINT('Ctrl Pts',(54.5518720616016,-44.5069478544945,0.));
#58941=CARTESIAN_POINT('Ctrl Pts',(54.5518720616016,-44.5069478544945,12.));
#58942=CARTESIAN_POINT('Ctrl Pts',(54.5707775794412,-44.5150207678988,0.));
#58943=CARTESIAN_POINT('Ctrl Pts',(54.5707775794412,-44.5150207678988,12.));
#58944=CARTESIAN_POINT('Ctrl Pts',(54.5897387202815,-44.5230938335167,0.));
#58945=CARTESIAN_POINT('Ctrl Pts',(54.5897387202815,-44.5230938335167,12.));
#58946=CARTESIAN_POINT('Ctrl Pts',(54.6087553602914,-44.5311669104515,0.));
#58947=CARTESIAN_POINT('Ctrl Pts',(54.6087553602914,-44.5311669104515,12.));
#58948=CARTESIAN_POINT('Ctrl Pts',(54.6278273743587,-44.5392398566802,0.));
#58949=CARTESIAN_POINT('Ctrl Pts',(54.6278273743587,-44.5392398566802,12.));
#58950=CARTESIAN_POINT('Ctrl Pts',(54.6469546367408,-44.5473125297312,0.));
#58951=CARTESIAN_POINT('Ctrl Pts',(54.6469546367408,-44.5473125297312,12.));
#58952=CARTESIAN_POINT('Ctrl Pts',(54.6661370216252,-44.5553847872721,0.));
#58953=CARTESIAN_POINT('Ctrl Pts',(54.6661370216252,-44.5553847872721,12.));
#58954=CARTESIAN_POINT('Ctrl Pts',(54.6853744036751,-44.5634564876863,0.));
#58955=CARTESIAN_POINT('Ctrl Pts',(54.6853744036751,-44.5634564876863,12.));
#58956=CARTESIAN_POINT('Ctrl Pts',(54.7046666586754,-44.5715274907619,0.));
#58957=CARTESIAN_POINT('Ctrl Pts',(54.7046666586754,-44.5715274907619,12.));
#58958=CARTESIAN_POINT('Ctrl Pts',(54.7240136637717,-44.5795976579454,0.));
#58959=CARTESIAN_POINT('Ctrl Pts',(54.7240136637717,-44.5795976579454,12.));
#58960=CARTESIAN_POINT('Ctrl Pts',(54.7434152971267,-44.5876668519661,0.));
#58961=CARTESIAN_POINT('Ctrl Pts',(54.7434152971267,-44.5876668519661,12.));
#58962=CARTESIAN_POINT('Ctrl Pts',(54.7628714377037,-44.5957349366059,0.));
#58963=CARTESIAN_POINT('Ctrl Pts',(54.7628714377037,-44.5957349366059,12.));
#58964=CARTESIAN_POINT('Ctrl Pts',(54.7823819650148,-44.603801776431,0.));
#58965=CARTESIAN_POINT('Ctrl Pts',(54.7823819650148,-44.603801776431,12.));
#58966=CARTESIAN_POINT('Ctrl Pts',(54.8019467588278,-44.6118672364906,0.));
#58967=CARTESIAN_POINT('Ctrl Pts',(54.8019467588278,-44.6118672364906,12.));
#58968=CARTESIAN_POINT('Ctrl Pts',(54.8215656991837,-44.6199311823293,0.));
#58969=CARTESIAN_POINT('Ctrl Pts',(54.8215656991837,-44.6199311823293,12.));
#58970=CARTESIAN_POINT('Ctrl Pts',(54.8412386665276,-44.6279934801169,0.));
#58971=CARTESIAN_POINT('Ctrl Pts',(54.8412386665276,-44.6279934801169,12.));
#58972=CARTESIAN_POINT('Ctrl Pts',(54.860965541796,-44.6360539967392,0.));
#58973=CARTESIAN_POINT('Ctrl Pts',(54.860965541796,-44.6360539967392,12.));
#58974=CARTESIAN_POINT('Ctrl Pts',(54.8807462065164,-44.6441125999063,0.));
#58975=CARTESIAN_POINT('Ctrl Pts',(54.8807462065164,-44.6441125999063,12.));
#58976=CARTESIAN_POINT('Ctrl Pts',(54.9005805428969,-44.6521691582534,0.));
#58977=CARTESIAN_POINT('Ctrl Pts',(54.9005805428969,-44.6521691582534,12.));
#58978=CARTESIAN_POINT('Ctrl Pts',(54.9204684337822,-44.6602235412836,0.));
#58979=CARTESIAN_POINT('Ctrl Pts',(54.9204684337822,-44.6602235412836,12.));
#58980=CARTESIAN_POINT('Ctrl Pts',(54.9404097626077,-44.6682756193147,0.));
#58981=CARTESIAN_POINT('Ctrl Pts',(54.9404097626077,-44.6682756193147,12.));
#58982=CARTESIAN_POINT('Ctrl Pts',(54.9604044133501,-44.6763252634259,0.));
#58983=CARTESIAN_POINT('Ctrl Pts',(54.9604044133501,-44.6763252634259,12.));
#58984=CARTESIAN_POINT('Ctrl Pts',(54.9804522704686,-44.6843723454,0.));
#58985=CARTESIAN_POINT('Ctrl Pts',(54.9804522704686,-44.6843723454,12.));
#58986=CARTESIAN_POINT('Ctrl Pts',(55.0005532188667,-44.6924167376869,0.));
#58987=CARTESIAN_POINT('Ctrl Pts',(55.0005532188667,-44.6924167376869,12.));
#58988=CARTESIAN_POINT('Ctrl Pts',(55.0207071439237,-44.7004583134249,0.));
#58989=CARTESIAN_POINT('Ctrl Pts',(55.0207071439237,-44.7004583134249,12.));
#58990=CARTESIAN_POINT('Ctrl Pts',(55.0409139315078,-44.7084969464513,0.));
#58991=CARTESIAN_POINT('Ctrl Pts',(55.0409139315078,-44.7084969464513,12.));
#58992=CARTESIAN_POINT('Ctrl Pts',(55.0611734679894,-44.716532511316,0.));
#58993=CARTESIAN_POINT('Ctrl Pts',(55.0611734679894,-44.716532511316,12.));
#58994=CARTESIAN_POINT('Ctrl Pts',(55.0814856402495,-44.7245648832979,0.));
#58995=CARTESIAN_POINT('Ctrl Pts',(55.0814856402495,-44.7245648832979,12.));
#58996=CARTESIAN_POINT('Ctrl Pts',(55.1018503356795,-44.7325939384035,0.));
#58997=CARTESIAN_POINT('Ctrl Pts',(55.1018503356795,-44.7325939384035,12.));
#58998=CARTESIAN_POINT('Ctrl Pts',(55.1222674421743,-44.740619553348,0.));
#58999=CARTESIAN_POINT('Ctrl Pts',(55.1222674421743,-44.740619553348,12.));
#59000=CARTESIAN_POINT('Ctrl Pts',(55.14273684812,-44.748641605542,0.));
#59001=CARTESIAN_POINT('Ctrl Pts',(55.14273684812,-44.748641605542,12.));
#59002=CARTESIAN_POINT('Ctrl Pts',(55.1632584423815,-44.7566599730773,0.));
#59003=CARTESIAN_POINT('Ctrl Pts',(55.1632584423815,-44.7566599730773,12.));
#59004=CARTESIAN_POINT('Ctrl Pts',(55.1838321142779,-44.7646745347109,0.));
#59005=CARTESIAN_POINT('Ctrl Pts',(55.1838321142779,-44.7646745347109,12.));
#59006=CARTESIAN_POINT('Ctrl Pts',(55.2044577535866,-44.7726851698619,0.));
#59007=CARTESIAN_POINT('Ctrl Pts',(55.2044577535866,-44.7726851698619,12.));
#59008=CARTESIAN_POINT('Ctrl Pts',(55.2251352505475,-44.7806917586077,0.));
#59009=CARTESIAN_POINT('Ctrl Pts',(55.2251352505475,-44.7806917586077,12.));
#59010=CARTESIAN_POINT('Ctrl Pts',(55.2458644958617,-44.7886941816823,0.));
#59011=CARTESIAN_POINT('Ctrl Pts',(55.2458644958617,-44.7886941816823,12.));
#59012=CARTESIAN_POINT('Ctrl Pts',(55.2666453806882,-44.7966923204741,0.));
#59013=CARTESIAN_POINT('Ctrl Pts',(55.2666453806882,-44.7966923204741,12.));
#59014=CARTESIAN_POINT('Ctrl Pts',(55.2874777966349,-44.8046860570245,0.));
#59015=CARTESIAN_POINT('Ctrl Pts',(55.2874777966349,-44.8046860570245,12.));
#59016=CARTESIAN_POINT('Ctrl Pts',(55.3083616357605,-44.812675274021,0.));
#59017=CARTESIAN_POINT('Ctrl Pts',(55.3083616357605,-44.812675274021,12.));
#59018=CARTESIAN_POINT('Ctrl Pts',(55.3292967905725,-44.8206598547889,0.));
#59019=CARTESIAN_POINT('Ctrl Pts',(55.3292967905725,-44.8206598547889,12.));
#59020=CARTESIAN_POINT('Ctrl Pts',(55.3502831540229,-44.8286396832849,0.));
#59021=CARTESIAN_POINT('Ctrl Pts',(55.3502831540229,-44.8286396832849,12.));
#59022=CARTESIAN_POINT('Ctrl Pts',(55.3713206194962,-44.8366146440896,0.));
#59023=CARTESIAN_POINT('Ctrl Pts',(55.3713206194962,-44.8366146440896,12.));
#59024=CARTESIAN_POINT('Ctrl Pts',(55.3924090808002,-44.8445846224034,0.));
#59025=CARTESIAN_POINT('Ctrl Pts',(55.3924090808002,-44.8445846224034,12.));
#59026=CARTESIAN_POINT('Ctrl Pts',(55.4135484321706,-44.8525495040398,0.));
#59027=CARTESIAN_POINT('Ctrl Pts',(55.4135484321706,-44.8525495040398,12.));
#59028=CARTESIAN_POINT('Ctrl Pts',(55.4347385682697,-44.8605091754208,0.));
#59029=CARTESIAN_POINT('Ctrl Pts',(55.4347385682697,-44.8605091754208,12.));
#59030=CARTESIAN_POINT('Ctrl Pts',(55.4559793841838,-44.8684635235727,0.));
#59031=CARTESIAN_POINT('Ctrl Pts',(55.4559793841838,-44.8684635235727,12.));
#59032=CARTESIAN_POINT('Ctrl Pts',(55.4772707754139,-44.8764124361218,0.));
#59033=CARTESIAN_POINT('Ctrl Pts',(55.4772707754139,-44.8764124361218,12.));
#59034=CARTESIAN_POINT('Ctrl Pts',(55.4986126378676,-44.8843558012903,0.));
#59035=CARTESIAN_POINT('Ctrl Pts',(55.4986126378676,-44.8843558012903,12.));
#59036=CARTESIAN_POINT('Ctrl Pts',(55.5200048678648,-44.8922935078905,0.));
#59037=CARTESIAN_POINT('Ctrl Pts',(55.5200048678648,-44.8922935078905,12.));
#59038=CARTESIAN_POINT('Ctrl Pts',(55.541447362135,-44.9002254453192,0.));
#59039=CARTESIAN_POINT('Ctrl Pts',(55.541447362135,-44.9002254453192,12.));
#59040=CARTESIAN_POINT('Ctrl Pts',(55.5629400178136,-44.9081515035526,0.));
#59041=CARTESIAN_POINT('Ctrl Pts',(55.5629400178136,-44.9081515035526,12.));
#59042=CARTESIAN_POINT('Ctrl Pts',(55.5844827324315,-44.9160715731425,0.));
#59043=CARTESIAN_POINT('Ctrl Pts',(55.5844827324315,-44.9160715731425,12.));
#59044=CARTESIAN_POINT('Ctrl Pts',(55.6060754039089,-44.9239855452119,0.));
#59045=CARTESIAN_POINT('Ctrl Pts',(55.6060754039089,-44.9239855452119,12.));
#59046=CARTESIAN_POINT('Ctrl Pts',(55.6277179305604,-44.9318933114483,0.));
#59047=CARTESIAN_POINT('Ctrl Pts',(55.6277179305604,-44.9318933114483,12.));
#59048=CARTESIAN_POINT('Ctrl Pts',(55.6494102110922,-44.9397947640996,0.));
#59049=CARTESIAN_POINT('Ctrl Pts',(55.6494102110922,-44.9397947640996,12.));
#59050=CARTESIAN_POINT('Ctrl Pts',(55.671152144599,-44.9476897959694,0.));
#59051=CARTESIAN_POINT('Ctrl Pts',(55.671152144599,-44.9476897959694,12.));
#59052=CARTESIAN_POINT('Ctrl Pts',(55.6929436305522,-44.9555783004133,0.));
#59053=CARTESIAN_POINT('Ctrl Pts',(55.6929436305522,-44.9555783004133,12.));
#59054=CARTESIAN_POINT('Ctrl Pts',(55.7147845687969,-44.9634601713352,0.));
#59055=CARTESIAN_POINT('Ctrl Pts',(55.7147845687969,-44.9634601713352,12.));
#59056=CARTESIAN_POINT('Ctrl Pts',(55.7366748595582,-44.9713353031827,0.));
#59057=CARTESIAN_POINT('Ctrl Pts',(55.7366748595582,-44.9713353031827,12.));
#59058=CARTESIAN_POINT('Ctrl Pts',(55.7586144034376,-44.979203590942,0.));
#59059=CARTESIAN_POINT('Ctrl Pts',(55.7586144034376,-44.979203590942,12.));
#59060=CARTESIAN_POINT('Ctrl Pts',(55.7806031014093,-44.9870649301333,0.));
#59061=CARTESIAN_POINT('Ctrl Pts',(55.7806031014093,-44.9870649301333,12.));
#59062=CARTESIAN_POINT('Ctrl Pts',(55.8026408548078,-44.9949192168073,0.));
#59063=CARTESIAN_POINT('Ctrl Pts',(55.8026408548078,-44.9949192168073,12.));
#59064=CARTESIAN_POINT('Ctrl Pts',(55.8247275653257,-45.002766347541,0.));
#59065=CARTESIAN_POINT('Ctrl Pts',(55.8247275653257,-45.002766347541,12.));
#59066=CARTESIAN_POINT('Ctrl Pts',(55.8468631350195,-45.0106062194325,0.));
#59067=CARTESIAN_POINT('Ctrl Pts',(55.8468631350195,-45.0106062194325,12.));
#59068=CARTESIAN_POINT('Ctrl Pts',(55.8690474663058,-45.0184387300968,0.));
#59069=CARTESIAN_POINT('Ctrl Pts',(55.8690474663058,-45.0184387300968,12.));
#59070=CARTESIAN_POINT('Ctrl Pts',(55.8912804619588,-45.0262637776623,0.));
#59071=CARTESIAN_POINT('Ctrl Pts',(55.8912804619588,-45.0262637776623,12.));
#59072=CARTESIAN_POINT('Ctrl Pts',(55.9135620250977,-45.0340812607676,0.));
#59073=CARTESIAN_POINT('Ctrl Pts',(55.9135620250977,-45.0340812607676,12.));
#59074=CARTESIAN_POINT('Ctrl Pts',(55.9358920591861,-45.041891078557,0.));
#59075=CARTESIAN_POINT('Ctrl Pts',(55.9358920591861,-45.041891078557,12.));
#59076=CARTESIAN_POINT('Ctrl Pts',(55.958270468037,-45.0496931306767,0.));
#59077=CARTESIAN_POINT('Ctrl Pts',(55.958270468037,-45.0496931306767,12.));
#59078=CARTESIAN_POINT('Ctrl Pts',(55.9806971558099,-45.0574873172696,0.));
#59079=CARTESIAN_POINT('Ctrl Pts',(55.9806971558099,-45.0574873172696,12.));
#59080=CARTESIAN_POINT('Ctrl Pts',(56.0031720270074,-45.0652735389729,0.));
#59081=CARTESIAN_POINT('Ctrl Pts',(56.0031720270074,-45.0652735389729,12.));
#59082=CARTESIAN_POINT('Ctrl Pts',(56.025694986463,-45.0730516969142,0.));
#59083=CARTESIAN_POINT('Ctrl Pts',(56.025694986463,-45.0730516969142,12.));
#59084=CARTESIAN_POINT('Ctrl Pts',(56.0482659393412,-45.0808216927082,0.));
#59085=CARTESIAN_POINT('Ctrl Pts',(56.0482659393412,-45.0808216927082,12.));
#59086=CARTESIAN_POINT('Ctrl Pts',(56.070884791141,-45.0885834284513,0.));
#59087=CARTESIAN_POINT('Ctrl Pts',(56.070884791141,-45.0885834284513,12.));
#59088=CARTESIAN_POINT('Ctrl Pts',(56.0935514476945,-45.0963368067177,0.));
#59089=CARTESIAN_POINT('Ctrl Pts',(56.0935514476945,-45.0963368067177,12.));
#59090=CARTESIAN_POINT('Ctrl Pts',(56.1162658151621,-45.1040817305563,0.));
#59091=CARTESIAN_POINT('Ctrl Pts',(56.1162658151621,-45.1040817305563,12.));
#59092=CARTESIAN_POINT('Ctrl Pts',(56.1390278000226,-45.1118181034888,0.));
#59093=CARTESIAN_POINT('Ctrl Pts',(56.1390278000226,-45.1118181034888,12.));
#59094=CARTESIAN_POINT('Ctrl Pts',(56.1618373090729,-45.119545829506,0.));
#59095=CARTESIAN_POINT('Ctrl Pts',(56.1618373090729,-45.119545829506,12.));
#59096=CARTESIAN_POINT('Ctrl Pts',(56.1846942494321,-45.1272648130627,0.));
#59097=CARTESIAN_POINT('Ctrl Pts',(56.1846942494321,-45.1272648130627,12.));
#59098=CARTESIAN_POINT('Ctrl Pts',(56.2075985285391,-45.1349749590736,0.));
#59099=CARTESIAN_POINT('Ctrl Pts',(56.2075985285391,-45.1349749590736,12.));
#59100=CARTESIAN_POINT('Ctrl Pts',(56.2305500541491,-45.1426761729107,0.));
#59101=CARTESIAN_POINT('Ctrl Pts',(56.2305500541491,-45.1426761729107,12.));
#59102=CARTESIAN_POINT('Ctrl Pts',(56.2535487343227,-45.150368360401,0.));
#59103=CARTESIAN_POINT('Ctrl Pts',(56.2535487343227,-45.150368360401,12.));
#59104=CARTESIAN_POINT('Ctrl Pts',(56.2765944774252,-45.158051427823,0.));
#59105=CARTESIAN_POINT('Ctrl Pts',(56.2765944774252,-45.158051427823,12.));
#59106=CARTESIAN_POINT('Ctrl Pts',(56.2996871921321,-45.1657252819018,0.));
#59107=CARTESIAN_POINT('Ctrl Pts',(56.2996871921321,-45.1657252819018,12.));
#59108=CARTESIAN_POINT('Ctrl Pts',(56.3228267874265,-45.1733898298062,0.));
#59109=CARTESIAN_POINT('Ctrl Pts',(56.3228267874265,-45.1733898298062,12.));
#59110=CARTESIAN_POINT('Ctrl Pts',(56.3460131725962,-45.1810449791451,0.));
#59111=CARTESIAN_POINT('Ctrl Pts',(56.3460131725962,-45.1810449791451,12.));
#59112=CARTESIAN_POINT('Ctrl Pts',(56.3692462572228,-45.1886906379664,0.));
#59113=CARTESIAN_POINT('Ctrl Pts',(56.3692462572228,-45.1886906379664,12.));
#59114=CARTESIAN_POINT('Ctrl Pts',(56.3925259511804,-45.1963267147527,0.));
#59115=CARTESIAN_POINT('Ctrl Pts',(56.3925259511804,-45.1963267147527,12.));
#59116=CARTESIAN_POINT('Ctrl Pts',(56.4158521646412,-45.2039531184172,0.));
#59117=CARTESIAN_POINT('Ctrl Pts',(56.4158521646412,-45.2039531184172,12.));
#59118=CARTESIAN_POINT('Ctrl Pts',(56.4392248080733,-45.2115697583002,0.));
#59119=CARTESIAN_POINT('Ctrl Pts',(56.4392248080733,-45.2115697583002,12.));
#59120=CARTESIAN_POINT('Ctrl Pts',(56.4626437922385,-45.2191765441666,0.));
#59121=CARTESIAN_POINT('Ctrl Pts',(56.4626437922385,-45.2191765441666,12.));
#59122=CARTESIAN_POINT('Ctrl Pts',(56.4861090281819,-45.2267733862046,0.));
#59123=CARTESIAN_POINT('Ctrl Pts',(56.4861090281819,-45.2267733862046,12.));
#59124=CARTESIAN_POINT('Ctrl Pts',(56.5096204272299,-45.2343601950222,0.));
#59125=CARTESIAN_POINT('Ctrl Pts',(56.5096204272299,-45.2343601950222,12.));
#59126=CARTESIAN_POINT('Ctrl Pts',(56.533177900995,-45.2419368816424,0.));
#59127=CARTESIAN_POINT('Ctrl Pts',(56.533177900995,-45.2419368816424,12.));
#59128=CARTESIAN_POINT('Ctrl Pts',(56.5567813613752,-45.2495033574997,0.));
#59129=CARTESIAN_POINT('Ctrl Pts',(56.5567813613752,-45.2495033574997,12.));
#59130=CARTESIAN_POINT('Ctrl Pts',(56.5804307205507,-45.2570595344382,0.));
#59131=CARTESIAN_POINT('Ctrl Pts',(56.5804307205507,-45.2570595344382,12.));
#59132=CARTESIAN_POINT('Ctrl Pts',(56.604125890975,-45.2646053247094,0.));
#59133=CARTESIAN_POINT('Ctrl Pts',(56.604125890975,-45.2646053247094,12.));
#59134=CARTESIAN_POINT('Ctrl Pts',(56.6278667853716,-45.2721406409707,0.));
#59135=CARTESIAN_POINT('Ctrl Pts',(56.6278667853716,-45.2721406409707,12.));
#59136=CARTESIAN_POINT('Ctrl Pts',(56.6516533167398,-45.2796653962796,0.));
#59137=CARTESIAN_POINT('Ctrl Pts',(56.6516533167398,-45.2796653962796,12.));
#59138=CARTESIAN_POINT('Ctrl Pts',(56.6754853983535,-45.2871795040912,0.));
#59139=CARTESIAN_POINT('Ctrl Pts',(56.6754853983535,-45.2871795040912,12.));
#59140=CARTESIAN_POINT('Ctrl Pts',(56.6993629437596,-45.2946828782557,0.));
#59141=CARTESIAN_POINT('Ctrl Pts',(56.6993629437596,-45.2946828782557,12.));
#59142=CARTESIAN_POINT('Ctrl Pts',(56.7232858667697,-45.3021754330169,0.));
#59143=CARTESIAN_POINT('Ctrl Pts',(56.7232858667697,-45.3021754330169,12.));
#59144=CARTESIAN_POINT('Ctrl Pts',(56.747254081454,-45.3096570830107,0.));
#59145=CARTESIAN_POINT('Ctrl Pts',(56.747254081454,-45.3096570830107,12.));
#59146=CARTESIAN_POINT('Ctrl Pts',(56.771267502148,-45.3171277432592,0.));
#59147=CARTESIAN_POINT('Ctrl Pts',(56.771267502148,-45.3171277432592,12.));
#59148=CARTESIAN_POINT('Ctrl Pts',(56.7953260434521,-45.3245873291682,0.));
#59149=CARTESIAN_POINT('Ctrl Pts',(56.7953260434521,-45.3245873291682,12.));
#59150=CARTESIAN_POINT('Ctrl Pts',(56.8194296202292,-45.3320357565241,0.));
#59151=CARTESIAN_POINT('Ctrl Pts',(56.8194296202292,-45.3320357565241,12.));
#59152=CARTESIAN_POINT('Ctrl Pts',(56.8435781475982,-45.3394729414932,0.));
#59153=CARTESIAN_POINT('Ctrl Pts',(56.8435781475982,-45.3394729414932,12.));
#59154=CARTESIAN_POINT('Ctrl Pts',(56.8677715409266,-45.3468988006202,0.));
#59155=CARTESIAN_POINT('Ctrl Pts',(56.8677715409266,-45.3468988006202,12.));
#59156=CARTESIAN_POINT('Ctrl Pts',(56.8920097158371,-45.3543132508234,0.));
#59157=CARTESIAN_POINT('Ctrl Pts',(56.8920097158371,-45.3543132508234,12.));
#59158=CARTESIAN_POINT('Ctrl Pts',(56.916292588208,-45.3617162093918,0.));
#59159=CARTESIAN_POINT('Ctrl Pts',(56.916292588208,-45.3617162093918,12.));
#59160=CARTESIAN_POINT('Ctrl Pts',(56.9406200741714,-45.3691075939827,0.));
#59161=CARTESIAN_POINT('Ctrl Pts',(56.9406200741714,-45.3691075939827,12.));
#59162=CARTESIAN_POINT('Ctrl Pts',(56.9649920901079,-45.3764873226202,0.));
#59163=CARTESIAN_POINT('Ctrl Pts',(56.9649920901079,-45.3764873226202,12.));
#59164=CARTESIAN_POINT('Ctrl Pts',(56.9894085526383,-45.3838553136957,0.));
#59165=CARTESIAN_POINT('Ctrl Pts',(56.9894085526383,-45.3838553136957,12.));
#59166=CARTESIAN_POINT('Ctrl Pts',(57.0138693786287,-45.3912114859625,0.));
#59167=CARTESIAN_POINT('Ctrl Pts',(57.0138693786287,-45.3912114859625,12.));
#59168=CARTESIAN_POINT('Ctrl Pts',(57.0383744851917,-45.3985557585316,0.));
#59169=CARTESIAN_POINT('Ctrl Pts',(57.0383744851917,-45.3985557585316,12.));
#59170=CARTESIAN_POINT('Ctrl Pts',(57.0629237896848,-45.4058880508693,0.));
#59171=CARTESIAN_POINT('Ctrl Pts',(57.0629237896848,-45.4058880508693,12.));
#59172=CARTESIAN_POINT('Ctrl Pts',(57.0875172097048,-45.4132082827945,0.));
#59173=CARTESIAN_POINT('Ctrl Pts',(57.0875172097048,-45.4132082827945,12.));
#59174=CARTESIAN_POINT('Ctrl Pts',(57.1121546630776,-45.4205163744778,0.));
#59175=CARTESIAN_POINT('Ctrl Pts',(57.1121546630776,-45.4205163744778,12.));
#59176=CARTESIAN_POINT('Ctrl Pts',(57.1368360678629,-45.4278122464387,0.));
#59177=CARTESIAN_POINT('Ctrl Pts',(57.1368360678629,-45.4278122464387,12.));
#59178=CARTESIAN_POINT('Ctrl Pts',(57.1615613423586,-45.4350958195434,0.));
#59179=CARTESIAN_POINT('Ctrl Pts',(57.1615613423586,-45.4350958195434,12.));
#59180=CARTESIAN_POINT('Ctrl Pts',(57.1863304051011,-45.4423670150035,0.));
#59181=CARTESIAN_POINT('Ctrl Pts',(57.1863304051011,-45.4423670150035,12.));
#59182=CARTESIAN_POINT('Ctrl Pts',(57.2111431748629,-45.4496257543759,0.));
#59183=CARTESIAN_POINT('Ctrl Pts',(57.2111431748629,-45.4496257543759,12.));
#59184=CARTESIAN_POINT('Ctrl Pts',(57.2359995706441,-45.4568719595639,0.));
#59185=CARTESIAN_POINT('Ctrl Pts',(57.2359995706441,-45.4568719595639,12.));
#59186=CARTESIAN_POINT('Ctrl Pts',(57.2608995116727,-45.4641055528138,0.));
#59187=CARTESIAN_POINT('Ctrl Pts',(57.2608995116727,-45.4641055528138,12.));
#59188=CARTESIAN_POINT('Ctrl Pts',(57.2858429174056,-45.4713264567059,0.));
#59189=CARTESIAN_POINT('Ctrl Pts',(57.2858429174056,-45.4713264567059,12.));
#59190=CARTESIAN_POINT('Ctrl Pts',(57.3108297075262,-45.4785345941506,0.));
#59191=CARTESIAN_POINT('Ctrl Pts',(57.3108297075262,-45.4785345941506,12.));
#59192=CARTESIAN_POINT('Ctrl Pts',(57.335859801939,-45.4857298883826,0.));
#59193=CARTESIAN_POINT('Ctrl Pts',(57.335859801939,-45.4857298883826,12.));
#59194=CARTESIAN_POINT('Ctrl Pts',(57.360933120758,-45.4929122629576,0.));
#59195=CARTESIAN_POINT('Ctrl Pts',(57.360933120758,-45.4929122629576,12.));
#59196=CARTESIAN_POINT('Ctrl Pts',(57.3860495843043,-45.5000816417516,0.));
#59197=CARTESIAN_POINT('Ctrl Pts',(57.3860495843043,-45.5000816417516,12.));
#59198=CARTESIAN_POINT('Ctrl Pts',(57.4112091131193,-45.5072379489637,0.));
#59199=CARTESIAN_POINT('Ctrl Pts',(57.4112091131193,-45.5072379489637,12.));
#59200=CARTESIAN_POINT('Ctrl Pts',(57.4364116279708,-45.5143811091209,0.));
#59201=CARTESIAN_POINT('Ctrl Pts',(57.4364116279708,-45.5143811091209,12.));
#59202=CARTESIAN_POINT('Ctrl Pts',(57.4616570498566,-45.5215110470825,0.));
#59203=CARTESIAN_POINT('Ctrl Pts',(57.4616570498566,-45.5215110470825,12.));
#59204=CARTESIAN_POINT('Ctrl Pts',(57.4869453000055,-45.5286276880479,0.));
#59205=CARTESIAN_POINT('Ctrl Pts',(57.4869453000055,-45.5286276880479,12.));
#59206=CARTESIAN_POINT('Ctrl Pts',(57.5122762998732,-45.5357309575603,0.));
#59207=CARTESIAN_POINT('Ctrl Pts',(57.5122762998732,-45.5357309575603,12.));
#59208=CARTESIAN_POINT('Ctrl Pts',(57.5376499711338,-45.5428207814832,0.));
#59209=CARTESIAN_POINT('Ctrl Pts',(57.5376499711338,-45.5428207814832,12.));
#59210=CARTESIAN_POINT('Ctrl Pts',(57.5630662356671,-45.5498970859829,0.));
#59211=CARTESIAN_POINT('Ctrl Pts',(57.5630662356671,-45.5498970859829,12.));
#59212=CARTESIAN_POINT('Ctrl Pts',(57.5885250155432,-45.5569597975096,0.));
#59213=CARTESIAN_POINT('Ctrl Pts',(57.5885250155432,-45.5569597975096,12.));
#59214=CARTESIAN_POINT('Ctrl Pts',(57.6140262330048,-45.5640088427819,0.));
#59215=CARTESIAN_POINT('Ctrl Pts',(57.6140262330048,-45.5640088427819,12.));
#59216=CARTESIAN_POINT('Ctrl Pts',(57.6395698104416,-45.5710441487683,0.));
#59217=CARTESIAN_POINT('Ctrl Pts',(57.6395698104416,-45.5710441487683,12.));
#59218=CARTESIAN_POINT('Ctrl Pts',(57.6651556704249,-45.5780656427173,0.));
#59219=CARTESIAN_POINT('Ctrl Pts',(57.6651556704249,-45.5780656427173,12.));
#59220=CARTESIAN_POINT('Ctrl Pts',(57.6907837357425,-45.5850732521902,0.));
#59221=CARTESIAN_POINT('Ctrl Pts',(57.6907837357425,-45.5850732521902,12.));
#59222=CARTESIAN_POINT('Ctrl Pts',(57.7164539294316,-45.5920669050988,0.));
#59223=CARTESIAN_POINT('Ctrl Pts',(57.7164539294316,-45.5920669050988,12.));
#59224=CARTESIAN_POINT('Ctrl Pts',(57.7421661748021,-45.5990465297341,0.));
#59225=CARTESIAN_POINT('Ctrl Pts',(57.7421661748021,-45.5990465297341,12.));
#59226=CARTESIAN_POINT('Ctrl Pts',(57.7679203954735,-45.6060120548199,0.));
#59227=CARTESIAN_POINT('Ctrl Pts',(57.7679203954735,-45.6060120548199,12.));
#59228=CARTESIAN_POINT('Ctrl Pts',(57.7937165153379,-45.6129634094678,0.));
#59229=CARTESIAN_POINT('Ctrl Pts',(57.7937165153379,-45.6129634094678,12.));
#59230=CARTESIAN_POINT('Ctrl Pts',(57.819554458484,-45.619900523078,0.));
#59231=CARTESIAN_POINT('Ctrl Pts',(57.819554458484,-45.619900523078,12.));
#59232=CARTESIAN_POINT('Ctrl Pts',(57.8454341491236,-45.6268233252543,0.));
#59233=CARTESIAN_POINT('Ctrl Pts',(57.8454341491236,-45.6268233252543,12.));
#59234=CARTESIAN_POINT('Ctrl Pts',(57.8713555115232,-45.6337317457253,0.));
#59235=CARTESIAN_POINT('Ctrl Pts',(57.8713555115232,-45.6337317457253,12.));
#59236=CARTESIAN_POINT('Ctrl Pts',(57.8973184699037,-45.6406257142385,0.));
#59237=CARTESIAN_POINT('Ctrl Pts',(57.8973184699037,-45.6406257142385,12.));
#59238=CARTESIAN_POINT('Ctrl Pts',(57.923322948432,-45.6475051605542,0.));
#59239=CARTESIAN_POINT('Ctrl Pts',(57.923322948432,-45.6475051605542,12.));
#59240=CARTESIAN_POINT('Ctrl Pts',(57.9493688714249,-45.6543700146689,0.));
#59241=CARTESIAN_POINT('Ctrl Pts',(57.9493688714249,-45.6543700146689,12.));
#59242=CARTESIAN_POINT('Ctrl Pts',(57.975456163507,-45.6612202069928,0.));
#59243=CARTESIAN_POINT('Ctrl Pts',(57.975456163507,-45.6612202069928,12.));
#59244=CARTESIAN_POINT('Ctrl Pts',(58.0015847497838,-45.6680556685494,0.));
#59245=CARTESIAN_POINT('Ctrl Pts',(58.0015847497838,-45.6680556685494,12.));
#59246=CARTESIAN_POINT('Ctrl Pts',(58.0277545560001,-45.6748763311635,0.));
#59247=CARTESIAN_POINT('Ctrl Pts',(58.0277545560001,-45.6748763311635,12.));
#59248=CARTESIAN_POINT('Ctrl Pts',(58.0539655087095,-45.6816821276662,0.));
#59249=CARTESIAN_POINT('Ctrl Pts',(58.0539655087095,-45.6816821276662,12.));
#59250=CARTESIAN_POINT('Ctrl Pts',(58.0802175348939,-45.6884729914465,0.));
#59251=CARTESIAN_POINT('Ctrl Pts',(58.0802175348939,-45.6884729914465,12.));
#59252=CARTESIAN_POINT('Ctrl Pts',(58.1065105615884,-45.6952488560134,0.));
#59253=CARTESIAN_POINT('Ctrl Pts',(58.1065105615884,-45.6952488560134,12.));
#59254=CARTESIAN_POINT('Ctrl Pts',(58.1328445154667,-45.7020096545174,0.));
#59255=CARTESIAN_POINT('Ctrl Pts',(58.1328445154667,-45.7020096545174,12.));
#59256=CARTESIAN_POINT('Ctrl Pts',(58.159219322515,-45.708755319378,0.));
#59257=CARTESIAN_POINT('Ctrl Pts',(58.159219322515,-45.708755319378,12.));
#59258=CARTESIAN_POINT('Ctrl Pts',(58.1856349074723,-45.7154857816507,0.));
#59259=CARTESIAN_POINT('Ctrl Pts',(58.1856349074723,-45.7154857816507,12.));
#59260=CARTESIAN_POINT('Ctrl Pts',(58.2120911942819,-45.7222009715431,0.));
#59261=CARTESIAN_POINT('Ctrl Pts',(58.2120911942819,-45.7222009715431,12.));
#59262=CARTESIAN_POINT('Ctrl Pts',(58.2385881070959,-45.7289008195612,0.));
#59263=CARTESIAN_POINT('Ctrl Pts',(58.2385881070959,-45.7289008195612,12.));
#59264=CARTESIAN_POINT('Ctrl Pts',(58.2651255711481,-45.7355852575127,0.));
#59265=CARTESIAN_POINT('Ctrl Pts',(58.2651255711481,-45.7355852575127,12.));
#59266=CARTESIAN_POINT('Ctrl Pts',(58.2917035135833,-45.7422542194625,0.));
#59267=CARTESIAN_POINT('Ctrl Pts',(58.2917035135833,-45.7422542194625,12.));
#59268=CARTESIAN_POINT('Ctrl Pts',(58.3183218645265,-45.7489076429725,0.));
#59269=CARTESIAN_POINT('Ctrl Pts',(58.3183218645265,-45.7489076429725,12.));
#59270=CARTESIAN_POINT('Ctrl Pts',(58.3449805573335,-45.7555454693956,0.));
#59271=CARTESIAN_POINT('Ctrl Pts',(58.3449805573335,-45.7555454693956,12.));
#59272=CARTESIAN_POINT('Ctrl Pts',(58.3716795262251,-45.7621676411361,0.));
#59273=CARTESIAN_POINT('Ctrl Pts',(58.3716795262251,-45.7621676411361,12.));
#59274=CARTESIAN_POINT('Ctrl Pts',(58.3984187044166,-45.76877409949,0.));
#59275=CARTESIAN_POINT('Ctrl Pts',(58.3984187044166,-45.76877409949,12.));
#59276=CARTESIAN_POINT('Ctrl Pts',(58.4251980219532,-45.77536478215,0.));
#59277=CARTESIAN_POINT('Ctrl Pts',(58.4251980219532,-45.77536478215,12.));
#59278=CARTESIAN_POINT('Ctrl Pts',(58.4520174038836,-45.7819396211062,0.));
#59279=CARTESIAN_POINT('Ctrl Pts',(58.4520174038836,-45.7819396211062,12.));
#59280=CARTESIAN_POINT('Ctrl Pts',(58.4788767677114,-45.7884985397138,0.));
#59281=CARTESIAN_POINT('Ctrl Pts',(58.4788767677114,-45.7884985397138,12.));
#59282=CARTESIAN_POINT('Ctrl Pts',(58.5057760270406,-45.7950414569431,0.));
#59283=CARTESIAN_POINT('Ctrl Pts',(58.5057760270406,-45.7950414569431,12.));
#59284=CARTESIAN_POINT('Ctrl Pts',(58.5327150960874,-45.801568292618,0.));
#59285=CARTESIAN_POINT('Ctrl Pts',(58.5327150960874,-45.801568292618,12.));
#59286=CARTESIAN_POINT('Ctrl Pts',(58.5596938940308,-45.8080789725167,0.));
#59287=CARTESIAN_POINT('Ctrl Pts',(58.5596938940308,-45.8080789725167,12.));
#59288=CARTESIAN_POINT('Ctrl Pts',(58.5867123490943,-45.8145734330666,0.));
#59289=CARTESIAN_POINT('Ctrl Pts',(58.5867123490943,-45.8145734330666,12.));
#59290=CARTESIAN_POINT('Ctrl Pts',(58.6137704035561,-45.8210516273556,0.));
#59291=CARTESIAN_POINT('Ctrl Pts',(58.6137704035561,-45.8210516273556,12.));
#59292=CARTESIAN_POINT('Ctrl Pts',(58.64086801535,-45.8275135263874,0.));
#59293=CARTESIAN_POINT('Ctrl Pts',(58.64086801535,-45.8275135263874,12.));
#59294=CARTESIAN_POINT('Ctrl Pts',(58.668005155216,-45.8339591141396,0.));
#59295=CARTESIAN_POINT('Ctrl Pts',(58.668005155216,-45.8339591141396,12.));
#59296=CARTESIAN_POINT('Ctrl Pts',(58.6897464750196,-45.8391025301766,0.));
#59297=CARTESIAN_POINT('Ctrl Pts',(58.6897464750196,-45.8391025301766,12.));
#59298=CARTESIAN_POINT('Ctrl Pts',(58.7060702401382,-45.8429527488565,0.));
#59299=CARTESIAN_POINT('Ctrl Pts',(58.7060702401382,-45.8429527488565,12.));
#59300=CARTESIAN_POINT('Ctrl Pts',(58.7169606500157,-45.8455162977347,0.));
#59301=CARTESIAN_POINT('Ctrl Pts',(58.7169606500157,-45.8455162977347,12.));
#59302=CARTESIAN_POINT('Ctrl Pts',(58.722407829904,-45.8467972562798,0.));
#59303=CARTESIAN_POINT('Ctrl Pts',(58.722407829904,-45.8467972562798,12.));
#59304=CARTESIAN_POINT('',(54.1679505278134,-44.3377168516418,0.));
#59305=CARTESIAN_POINT('Ctrl Pts',(54.1679505278134,-44.3377168516418,0.));
#59306=CARTESIAN_POINT('Ctrl Pts',(54.1714861895278,-44.3393235891014,0.));
#59307=CARTESIAN_POINT('Ctrl Pts',(54.1785633257456,-44.3425373700829,0.));
#59308=CARTESIAN_POINT('Ctrl Pts',(54.1891964684439,-44.3473589597468,0.));
#59309=CARTESIAN_POINT('Ctrl Pts',(54.203408870162,-44.3537895823819,0.));
#59310=CARTESIAN_POINT('Ctrl Pts',(54.2212325005847,-44.3618309103245,0.));
#59311=CARTESIAN_POINT('Ctrl Pts',(54.2391142386354,-44.369875253351,0.));
#59312=CARTESIAN_POINT('Ctrl Pts',(54.2570540336536,-44.3779225430461,0.));
#59313=CARTESIAN_POINT('Ctrl Pts',(54.2750517888695,-44.3859726620288,0.));
#59314=CARTESIAN_POINT('Ctrl Pts',(54.2931073621661,-44.3940254456427,0.));
#59315=CARTESIAN_POINT('Ctrl Pts',(54.3112205860776,-44.4020807028144,0.));
#59316=CARTESIAN_POINT('Ctrl Pts',(54.3293912830237,-44.4101382321834,0.));
#59317=CARTESIAN_POINT('Ctrl Pts',(54.347619281931,-44.4181978395814,0.));
#59318=CARTESIAN_POINT('Ctrl Pts',(54.3659044357064,-44.4262593564664,0.));
#59319=CARTESIAN_POINT('Ctrl Pts',(54.3842466156151,-44.4343226339555,0.));
#59320=CARTESIAN_POINT('Ctrl Pts',(54.4026457030316,-44.442387534098,0.));
#59321=CARTESIAN_POINT('Ctrl Pts',(54.4211015825959,-44.4504539226336,0.));
#59322=CARTESIAN_POINT('Ctrl Pts',(54.4396141337008,-44.4585216599933,0.));
#59323=CARTESIAN_POINT('Ctrl Pts',(54.4581832262072,-44.4665905967701,0.));
#59324=CARTESIAN_POINT('Ctrl Pts',(54.4768087248854,-44.4746605784056,0.));
#59325=CARTESIAN_POINT('Ctrl Pts',(54.4954904921938,-44.4827314481271,0.));
#59326=CARTESIAN_POINT('Ctrl Pts',(54.5142283914684,-44.4908030503209,0.));
#59327=CARTESIAN_POINT('Ctrl Pts',(54.5330222905438,-44.4988752343715,0.));
#59328=CARTESIAN_POINT('Ctrl Pts',(54.5518720616016,-44.5069478544945,0.));
#59329=CARTESIAN_POINT('Ctrl Pts',(54.5707775794412,-44.5150207678988,0.));
#59330=CARTESIAN_POINT('Ctrl Pts',(54.5897387202815,-44.5230938335167,0.));
#59331=CARTESIAN_POINT('Ctrl Pts',(54.6087553602914,-44.5311669104515,0.));
#59332=CARTESIAN_POINT('Ctrl Pts',(54.6278273743587,-44.5392398566802,0.));
#59333=CARTESIAN_POINT('Ctrl Pts',(54.6469546367408,-44.5473125297312,0.));
#59334=CARTESIAN_POINT('Ctrl Pts',(54.6661370216252,-44.5553847872721,0.));
#59335=CARTESIAN_POINT('Ctrl Pts',(54.6853744036751,-44.5634564876863,0.));
#59336=CARTESIAN_POINT('Ctrl Pts',(54.7046666586754,-44.5715274907619,0.));
#59337=CARTESIAN_POINT('Ctrl Pts',(54.7240136637717,-44.5795976579454,0.));
#59338=CARTESIAN_POINT('Ctrl Pts',(54.7434152971267,-44.5876668519661,0.));
#59339=CARTESIAN_POINT('Ctrl Pts',(54.7628714377037,-44.5957349366059,0.));
#59340=CARTESIAN_POINT('Ctrl Pts',(54.7823819650148,-44.603801776431,0.));
#59341=CARTESIAN_POINT('Ctrl Pts',(54.8019467588278,-44.6118672364906,0.));
#59342=CARTESIAN_POINT('Ctrl Pts',(54.8215656991837,-44.6199311823293,0.));
#59343=CARTESIAN_POINT('Ctrl Pts',(54.8412386665276,-44.6279934801169,0.));
#59344=CARTESIAN_POINT('Ctrl Pts',(54.860965541796,-44.6360539967392,0.));
#59345=CARTESIAN_POINT('Ctrl Pts',(54.8807462065164,-44.6441125999063,0.));
#59346=CARTESIAN_POINT('Ctrl Pts',(54.9005805428969,-44.6521691582534,0.));
#59347=CARTESIAN_POINT('Ctrl Pts',(54.9204684337822,-44.6602235412836,0.));
#59348=CARTESIAN_POINT('Ctrl Pts',(54.9404097626077,-44.6682756193147,0.));
#59349=CARTESIAN_POINT('Ctrl Pts',(54.9604044133501,-44.6763252634259,0.));
#59350=CARTESIAN_POINT('Ctrl Pts',(54.9804522704686,-44.6843723454,0.));
#59351=CARTESIAN_POINT('Ctrl Pts',(55.0005532188667,-44.6924167376869,0.));
#59352=CARTESIAN_POINT('Ctrl Pts',(55.0207071439237,-44.7004583134249,0.));
#59353=CARTESIAN_POINT('Ctrl Pts',(55.0409139315078,-44.7084969464513,0.));
#59354=CARTESIAN_POINT('Ctrl Pts',(55.0611734679894,-44.716532511316,0.));
#59355=CARTESIAN_POINT('Ctrl Pts',(55.0814856402495,-44.7245648832979,0.));
#59356=CARTESIAN_POINT('Ctrl Pts',(55.1018503356795,-44.7325939384035,0.));
#59357=CARTESIAN_POINT('Ctrl Pts',(55.1222674421743,-44.740619553348,0.));
#59358=CARTESIAN_POINT('Ctrl Pts',(55.14273684812,-44.748641605542,0.));
#59359=CARTESIAN_POINT('Ctrl Pts',(55.1632584423815,-44.7566599730773,0.));
#59360=CARTESIAN_POINT('Ctrl Pts',(55.1838321142779,-44.7646745347109,0.));
#59361=CARTESIAN_POINT('Ctrl Pts',(55.2044577535866,-44.7726851698619,0.));
#59362=CARTESIAN_POINT('Ctrl Pts',(55.2251352505475,-44.7806917586077,0.));
#59363=CARTESIAN_POINT('Ctrl Pts',(55.2458644958617,-44.7886941816823,0.));
#59364=CARTESIAN_POINT('Ctrl Pts',(55.2666453806882,-44.7966923204741,0.));
#59365=CARTESIAN_POINT('Ctrl Pts',(55.2874777966349,-44.8046860570245,0.));
#59366=CARTESIAN_POINT('Ctrl Pts',(55.3083616357605,-44.812675274021,0.));
#59367=CARTESIAN_POINT('Ctrl Pts',(55.3292967905725,-44.8206598547889,0.));
#59368=CARTESIAN_POINT('Ctrl Pts',(55.3502831540229,-44.8286396832849,0.));
#59369=CARTESIAN_POINT('Ctrl Pts',(55.3713206194962,-44.8366146440896,0.));
#59370=CARTESIAN_POINT('Ctrl Pts',(55.3924090808002,-44.8445846224034,0.));
#59371=CARTESIAN_POINT('Ctrl Pts',(55.4135484321706,-44.8525495040398,0.));
#59372=CARTESIAN_POINT('Ctrl Pts',(55.4347385682697,-44.8605091754208,0.));
#59373=CARTESIAN_POINT('Ctrl Pts',(55.4559793841838,-44.8684635235727,0.));
#59374=CARTESIAN_POINT('Ctrl Pts',(55.4772707754139,-44.8764124361218,0.));
#59375=CARTESIAN_POINT('Ctrl Pts',(55.4986126378676,-44.8843558012903,0.));
#59376=CARTESIAN_POINT('Ctrl Pts',(55.5200048678648,-44.8922935078905,0.));
#59377=CARTESIAN_POINT('Ctrl Pts',(55.541447362135,-44.9002254453192,0.));
#59378=CARTESIAN_POINT('Ctrl Pts',(55.5629400178136,-44.9081515035526,0.));
#59379=CARTESIAN_POINT('Ctrl Pts',(55.5844827324315,-44.9160715731425,0.));
#59380=CARTESIAN_POINT('Ctrl Pts',(55.6060754039089,-44.9239855452119,0.));
#59381=CARTESIAN_POINT('Ctrl Pts',(55.6277179305604,-44.9318933114483,0.));
#59382=CARTESIAN_POINT('Ctrl Pts',(55.6494102110922,-44.9397947640996,0.));
#59383=CARTESIAN_POINT('Ctrl Pts',(55.671152144599,-44.9476897959694,0.));
#59384=CARTESIAN_POINT('Ctrl Pts',(55.6929436305522,-44.9555783004133,0.));
#59385=CARTESIAN_POINT('Ctrl Pts',(55.7147845687969,-44.9634601713352,0.));
#59386=CARTESIAN_POINT('Ctrl Pts',(55.7366748595582,-44.9713353031827,0.));
#59387=CARTESIAN_POINT('Ctrl Pts',(55.7586144034376,-44.979203590942,0.));
#59388=CARTESIAN_POINT('Ctrl Pts',(55.7806031014093,-44.9870649301333,0.));
#59389=CARTESIAN_POINT('Ctrl Pts',(55.8026408548078,-44.9949192168073,0.));
#59390=CARTESIAN_POINT('Ctrl Pts',(55.8247275653257,-45.002766347541,0.));
#59391=CARTESIAN_POINT('Ctrl Pts',(55.8468631350195,-45.0106062194325,0.));
#59392=CARTESIAN_POINT('Ctrl Pts',(55.8690474663058,-45.0184387300968,0.));
#59393=CARTESIAN_POINT('Ctrl Pts',(55.8912804619588,-45.0262637776623,0.));
#59394=CARTESIAN_POINT('Ctrl Pts',(55.9135620250977,-45.0340812607676,0.));
#59395=CARTESIAN_POINT('Ctrl Pts',(55.9358920591861,-45.041891078557,0.));
#59396=CARTESIAN_POINT('Ctrl Pts',(55.958270468037,-45.0496931306767,0.));
#59397=CARTESIAN_POINT('Ctrl Pts',(55.9806971558099,-45.0574873172696,0.));
#59398=CARTESIAN_POINT('Ctrl Pts',(56.0031720270074,-45.0652735389729,0.));
#59399=CARTESIAN_POINT('Ctrl Pts',(56.025694986463,-45.0730516969142,0.));
#59400=CARTESIAN_POINT('Ctrl Pts',(56.0482659393412,-45.0808216927082,0.));
#59401=CARTESIAN_POINT('Ctrl Pts',(56.070884791141,-45.0885834284513,0.));
#59402=CARTESIAN_POINT('Ctrl Pts',(56.0935514476945,-45.0963368067177,0.));
#59403=CARTESIAN_POINT('Ctrl Pts',(56.1162658151621,-45.1040817305563,0.));
#59404=CARTESIAN_POINT('Ctrl Pts',(56.1390278000226,-45.1118181034888,0.));
#59405=CARTESIAN_POINT('Ctrl Pts',(56.1618373090729,-45.119545829506,0.));
#59406=CARTESIAN_POINT('Ctrl Pts',(56.1846942494321,-45.1272648130627,0.));
#59407=CARTESIAN_POINT('Ctrl Pts',(56.2075985285391,-45.1349749590736,0.));
#59408=CARTESIAN_POINT('Ctrl Pts',(56.2305500541491,-45.1426761729107,0.));
#59409=CARTESIAN_POINT('Ctrl Pts',(56.2535487343227,-45.150368360401,0.));
#59410=CARTESIAN_POINT('Ctrl Pts',(56.2765944774252,-45.158051427823,0.));
#59411=CARTESIAN_POINT('Ctrl Pts',(56.2996871921321,-45.1657252819018,0.));
#59412=CARTESIAN_POINT('Ctrl Pts',(56.3228267874265,-45.1733898298062,0.));
#59413=CARTESIAN_POINT('Ctrl Pts',(56.3460131725962,-45.1810449791451,0.));
#59414=CARTESIAN_POINT('Ctrl Pts',(56.3692462572228,-45.1886906379664,0.));
#59415=CARTESIAN_POINT('Ctrl Pts',(56.3925259511804,-45.1963267147527,0.));
#59416=CARTESIAN_POINT('Ctrl Pts',(56.4158521646412,-45.2039531184172,0.));
#59417=CARTESIAN_POINT('Ctrl Pts',(56.4392248080733,-45.2115697583002,0.));
#59418=CARTESIAN_POINT('Ctrl Pts',(56.4626437922385,-45.2191765441666,0.));
#59419=CARTESIAN_POINT('Ctrl Pts',(56.4861090281819,-45.2267733862046,0.));
#59420=CARTESIAN_POINT('Ctrl Pts',(56.5096204272299,-45.2343601950222,0.));
#59421=CARTESIAN_POINT('Ctrl Pts',(56.533177900995,-45.2419368816424,0.));
#59422=CARTESIAN_POINT('Ctrl Pts',(56.5567813613752,-45.2495033574997,0.));
#59423=CARTESIAN_POINT('Ctrl Pts',(56.5804307205507,-45.2570595344382,0.));
#59424=CARTESIAN_POINT('Ctrl Pts',(56.604125890975,-45.2646053247094,0.));
#59425=CARTESIAN_POINT('Ctrl Pts',(56.6278667853716,-45.2721406409707,0.));
#59426=CARTESIAN_POINT('Ctrl Pts',(56.6516533167398,-45.2796653962796,0.));
#59427=CARTESIAN_POINT('Ctrl Pts',(56.6754853983535,-45.2871795040912,0.));
#59428=CARTESIAN_POINT('Ctrl Pts',(56.6993629437596,-45.2946828782557,0.));
#59429=CARTESIAN_POINT('Ctrl Pts',(56.7232858667697,-45.3021754330169,0.));
#59430=CARTESIAN_POINT('Ctrl Pts',(56.747254081454,-45.3096570830107,0.));
#59431=CARTESIAN_POINT('Ctrl Pts',(56.771267502148,-45.3171277432592,0.));
#59432=CARTESIAN_POINT('Ctrl Pts',(56.7953260434521,-45.3245873291682,0.));
#59433=CARTESIAN_POINT('Ctrl Pts',(56.8194296202292,-45.3320357565241,0.));
#59434=CARTESIAN_POINT('Ctrl Pts',(56.8435781475982,-45.3394729414932,0.));
#59435=CARTESIAN_POINT('Ctrl Pts',(56.8677715409266,-45.3468988006202,0.));
#59436=CARTESIAN_POINT('Ctrl Pts',(56.8920097158371,-45.3543132508234,0.));
#59437=CARTESIAN_POINT('Ctrl Pts',(56.916292588208,-45.3617162093918,0.));
#59438=CARTESIAN_POINT('Ctrl Pts',(56.9406200741714,-45.3691075939827,0.));
#59439=CARTESIAN_POINT('Ctrl Pts',(56.9649920901079,-45.3764873226202,0.));
#59440=CARTESIAN_POINT('Ctrl Pts',(56.9894085526383,-45.3838553136957,0.));
#59441=CARTESIAN_POINT('Ctrl Pts',(57.0138693786287,-45.3912114859625,0.));
#59442=CARTESIAN_POINT('Ctrl Pts',(57.0383744851917,-45.3985557585316,0.));
#59443=CARTESIAN_POINT('Ctrl Pts',(57.0629237896848,-45.4058880508693,0.));
#59444=CARTESIAN_POINT('Ctrl Pts',(57.0875172097048,-45.4132082827945,0.));
#59445=CARTESIAN_POINT('Ctrl Pts',(57.1121546630776,-45.4205163744778,0.));
#59446=CARTESIAN_POINT('Ctrl Pts',(57.1368360678629,-45.4278122464387,0.));
#59447=CARTESIAN_POINT('Ctrl Pts',(57.1615613423586,-45.4350958195434,0.));
#59448=CARTESIAN_POINT('Ctrl Pts',(57.1863304051011,-45.4423670150035,0.));
#59449=CARTESIAN_POINT('Ctrl Pts',(57.2111431748629,-45.4496257543759,0.));
#59450=CARTESIAN_POINT('Ctrl Pts',(57.2359995706441,-45.4568719595639,0.));
#59451=CARTESIAN_POINT('Ctrl Pts',(57.2608995116727,-45.4641055528138,0.));
#59452=CARTESIAN_POINT('Ctrl Pts',(57.2858429174056,-45.4713264567059,0.));
#59453=CARTESIAN_POINT('Ctrl Pts',(57.3108297075262,-45.4785345941506,0.));
#59454=CARTESIAN_POINT('Ctrl Pts',(57.335859801939,-45.4857298883826,0.));
#59455=CARTESIAN_POINT('Ctrl Pts',(57.360933120758,-45.4929122629576,0.));
#59456=CARTESIAN_POINT('Ctrl Pts',(57.3860495843043,-45.5000816417516,0.));
#59457=CARTESIAN_POINT('Ctrl Pts',(57.4112091131193,-45.5072379489637,0.));
#59458=CARTESIAN_POINT('Ctrl Pts',(57.4364116279708,-45.5143811091209,0.));
#59459=CARTESIAN_POINT('Ctrl Pts',(57.4616570498566,-45.5215110470825,0.));
#59460=CARTESIAN_POINT('Ctrl Pts',(57.4869453000055,-45.5286276880479,0.));
#59461=CARTESIAN_POINT('Ctrl Pts',(57.5122762998732,-45.5357309575603,0.));
#59462=CARTESIAN_POINT('Ctrl Pts',(57.5376499711338,-45.5428207814832,0.));
#59463=CARTESIAN_POINT('Ctrl Pts',(57.5630662356671,-45.5498970859829,0.));
#59464=CARTESIAN_POINT('Ctrl Pts',(57.5885250155432,-45.5569597975096,0.));
#59465=CARTESIAN_POINT('Ctrl Pts',(57.6140262330048,-45.5640088427819,0.));
#59466=CARTESIAN_POINT('Ctrl Pts',(57.6395698104416,-45.5710441487683,0.));
#59467=CARTESIAN_POINT('Ctrl Pts',(57.6651556704249,-45.5780656427173,0.));
#59468=CARTESIAN_POINT('Ctrl Pts',(57.6907837357425,-45.5850732521902,0.));
#59469=CARTESIAN_POINT('Ctrl Pts',(57.7164539294316,-45.5920669050988,0.));
#59470=CARTESIAN_POINT('Ctrl Pts',(57.7421661748021,-45.5990465297341,0.));
#59471=CARTESIAN_POINT('Ctrl Pts',(57.7679203954735,-45.6060120548199,0.));
#59472=CARTESIAN_POINT('Ctrl Pts',(57.7937165153379,-45.6129634094678,0.));
#59473=CARTESIAN_POINT('Ctrl Pts',(57.819554458484,-45.619900523078,0.));
#59474=CARTESIAN_POINT('Ctrl Pts',(57.8454341491236,-45.6268233252543,0.));
#59475=CARTESIAN_POINT('Ctrl Pts',(57.8713555115232,-45.6337317457253,0.));
#59476=CARTESIAN_POINT('Ctrl Pts',(57.8973184699037,-45.6406257142385,0.));
#59477=CARTESIAN_POINT('Ctrl Pts',(57.923322948432,-45.6475051605542,0.));
#59478=CARTESIAN_POINT('Ctrl Pts',(57.9493688714249,-45.6543700146689,0.));
#59479=CARTESIAN_POINT('Ctrl Pts',(57.975456163507,-45.6612202069928,0.));
#59480=CARTESIAN_POINT('Ctrl Pts',(58.0015847497838,-45.6680556685494,0.));
#59481=CARTESIAN_POINT('Ctrl Pts',(58.0277545560001,-45.6748763311635,0.));
#59482=CARTESIAN_POINT('Ctrl Pts',(58.0539655087095,-45.6816821276662,0.));
#59483=CARTESIAN_POINT('Ctrl Pts',(58.0802175348939,-45.6884729914465,0.));
#59484=CARTESIAN_POINT('Ctrl Pts',(58.1065105615884,-45.6952488560134,0.));
#59485=CARTESIAN_POINT('Ctrl Pts',(58.1328445154667,-45.7020096545174,0.));
#59486=CARTESIAN_POINT('Ctrl Pts',(58.159219322515,-45.708755319378,0.));
#59487=CARTESIAN_POINT('Ctrl Pts',(58.1856349074723,-45.7154857816507,0.));
#59488=CARTESIAN_POINT('Ctrl Pts',(58.2120911942819,-45.7222009715431,0.));
#59489=CARTESIAN_POINT('Ctrl Pts',(58.2385881070959,-45.7289008195612,0.));
#59490=CARTESIAN_POINT('Ctrl Pts',(58.2651255711481,-45.7355852575127,0.));
#59491=CARTESIAN_POINT('Ctrl Pts',(58.2917035135833,-45.7422542194625,0.));
#59492=CARTESIAN_POINT('Ctrl Pts',(58.3183218645265,-45.7489076429725,0.));
#59493=CARTESIAN_POINT('Ctrl Pts',(58.3449805573335,-45.7555454693956,0.));
#59494=CARTESIAN_POINT('Ctrl Pts',(58.3678667473265,-45.7612219538034,0.));
#59495=CARTESIAN_POINT('Ctrl Pts',(58.3854348517209,-45.7655655205267,0.));
#59496=CARTESIAN_POINT('Ctrl Pts',(58.397667048078,-45.7685831165459,0.));
#59497=CARTESIAN_POINT('Ctrl Pts',(58.4045515723007,-45.7702793558063,0.));
#59498=CARTESIAN_POINT('Ctrl Pts',(58.4060826907377,-45.7706564944766,0.));
#59499=CARTESIAN_POINT('',(54.1679505278134,-44.3377168516418,12.));
#59500=CARTESIAN_POINT('',(54.1679505278134,-44.3377168516418,0.));
#59501=CARTESIAN_POINT('Ctrl Pts',(58.4060826907375,-45.7706564944766,12.));
#59502=CARTESIAN_POINT('Ctrl Pts',(58.4045515723006,-45.7702793558062,12.));
#59503=CARTESIAN_POINT('Ctrl Pts',(58.3976670480779,-45.7685831165459,12.));
#59504=CARTESIAN_POINT('Ctrl Pts',(58.3854348517209,-45.7655655205267,12.));
#59505=CARTESIAN_POINT('Ctrl Pts',(58.3678667473265,-45.7612219538034,12.));
#59506=CARTESIAN_POINT('Ctrl Pts',(58.3449805573335,-45.7555454693956,12.));
#59507=CARTESIAN_POINT('Ctrl Pts',(58.3183218645265,-45.7489076429725,12.));
#59508=CARTESIAN_POINT('Ctrl Pts',(58.2917035135833,-45.7422542194625,12.));
#59509=CARTESIAN_POINT('Ctrl Pts',(58.2651255711481,-45.7355852575127,12.));
#59510=CARTESIAN_POINT('Ctrl Pts',(58.2385881070959,-45.7289008195612,12.));
#59511=CARTESIAN_POINT('Ctrl Pts',(58.2120911942819,-45.7222009715431,12.));
#59512=CARTESIAN_POINT('Ctrl Pts',(58.1856349074723,-45.7154857816507,12.));
#59513=CARTESIAN_POINT('Ctrl Pts',(58.159219322515,-45.708755319378,12.));
#59514=CARTESIAN_POINT('Ctrl Pts',(58.1328445154667,-45.7020096545174,12.));
#59515=CARTESIAN_POINT('Ctrl Pts',(58.1065105615884,-45.6952488560134,12.));
#59516=CARTESIAN_POINT('Ctrl Pts',(58.0802175348939,-45.6884729914465,12.));
#59517=CARTESIAN_POINT('Ctrl Pts',(58.0539655087095,-45.6816821276662,12.));
#59518=CARTESIAN_POINT('Ctrl Pts',(58.0277545560001,-45.6748763311635,12.));
#59519=CARTESIAN_POINT('Ctrl Pts',(58.0015847497838,-45.6680556685494,12.));
#59520=CARTESIAN_POINT('Ctrl Pts',(57.975456163507,-45.6612202069928,12.));
#59521=CARTESIAN_POINT('Ctrl Pts',(57.9493688714249,-45.6543700146689,12.));
#59522=CARTESIAN_POINT('Ctrl Pts',(57.923322948432,-45.6475051605542,12.));
#59523=CARTESIAN_POINT('Ctrl Pts',(57.8973184699037,-45.6406257142385,12.));
#59524=CARTESIAN_POINT('Ctrl Pts',(57.8713555115232,-45.6337317457253,12.));
#59525=CARTESIAN_POINT('Ctrl Pts',(57.8454341491236,-45.6268233252543,12.));
#59526=CARTESIAN_POINT('Ctrl Pts',(57.819554458484,-45.619900523078,12.));
#59527=CARTESIAN_POINT('Ctrl Pts',(57.7937165153379,-45.6129634094678,12.));
#59528=CARTESIAN_POINT('Ctrl Pts',(57.7679203954735,-45.6060120548199,12.));
#59529=CARTESIAN_POINT('Ctrl Pts',(57.7421661748021,-45.5990465297341,12.));
#59530=CARTESIAN_POINT('Ctrl Pts',(57.7164539294316,-45.5920669050988,12.));
#59531=CARTESIAN_POINT('Ctrl Pts',(57.6907837357425,-45.5850732521902,12.));
#59532=CARTESIAN_POINT('Ctrl Pts',(57.6651556704249,-45.5780656427173,12.));
#59533=CARTESIAN_POINT('Ctrl Pts',(57.6395698104416,-45.5710441487683,12.));
#59534=CARTESIAN_POINT('Ctrl Pts',(57.6140262330048,-45.5640088427819,12.));
#59535=CARTESIAN_POINT('Ctrl Pts',(57.5885250155432,-45.5569597975096,12.));
#59536=CARTESIAN_POINT('Ctrl Pts',(57.5630662356671,-45.5498970859829,12.));
#59537=CARTESIAN_POINT('Ctrl Pts',(57.5376499711338,-45.5428207814832,12.));
#59538=CARTESIAN_POINT('Ctrl Pts',(57.5122762998732,-45.5357309575603,12.));
#59539=CARTESIAN_POINT('Ctrl Pts',(57.4869453000055,-45.5286276880479,12.));
#59540=CARTESIAN_POINT('Ctrl Pts',(57.4616570498566,-45.5215110470825,12.));
#59541=CARTESIAN_POINT('Ctrl Pts',(57.4364116279708,-45.5143811091209,12.));
#59542=CARTESIAN_POINT('Ctrl Pts',(57.4112091131193,-45.5072379489637,12.));
#59543=CARTESIAN_POINT('Ctrl Pts',(57.3860495843043,-45.5000816417516,12.));
#59544=CARTESIAN_POINT('Ctrl Pts',(57.360933120758,-45.4929122629576,12.));
#59545=CARTESIAN_POINT('Ctrl Pts',(57.335859801939,-45.4857298883826,12.));
#59546=CARTESIAN_POINT('Ctrl Pts',(57.3108297075262,-45.4785345941506,12.));
#59547=CARTESIAN_POINT('Ctrl Pts',(57.2858429174056,-45.4713264567059,12.));
#59548=CARTESIAN_POINT('Ctrl Pts',(57.2608995116727,-45.4641055528138,12.));
#59549=CARTESIAN_POINT('Ctrl Pts',(57.2359995706441,-45.4568719595639,12.));
#59550=CARTESIAN_POINT('Ctrl Pts',(57.2111431748629,-45.4496257543759,12.));
#59551=CARTESIAN_POINT('Ctrl Pts',(57.1863304051011,-45.4423670150035,12.));
#59552=CARTESIAN_POINT('Ctrl Pts',(57.1615613423586,-45.4350958195434,12.));
#59553=CARTESIAN_POINT('Ctrl Pts',(57.1368360678629,-45.4278122464387,12.));
#59554=CARTESIAN_POINT('Ctrl Pts',(57.1121546630776,-45.4205163744778,12.));
#59555=CARTESIAN_POINT('Ctrl Pts',(57.0875172097048,-45.4132082827945,12.));
#59556=CARTESIAN_POINT('Ctrl Pts',(57.0629237896848,-45.4058880508693,12.));
#59557=CARTESIAN_POINT('Ctrl Pts',(57.0383744851917,-45.3985557585316,12.));
#59558=CARTESIAN_POINT('Ctrl Pts',(57.0138693786287,-45.3912114859625,12.));
#59559=CARTESIAN_POINT('Ctrl Pts',(56.9894085526383,-45.3838553136957,12.));
#59560=CARTESIAN_POINT('Ctrl Pts',(56.9649920901079,-45.3764873226202,12.));
#59561=CARTESIAN_POINT('Ctrl Pts',(56.9406200741714,-45.3691075939827,12.));
#59562=CARTESIAN_POINT('Ctrl Pts',(56.916292588208,-45.3617162093918,12.));
#59563=CARTESIAN_POINT('Ctrl Pts',(56.8920097158371,-45.3543132508234,12.));
#59564=CARTESIAN_POINT('Ctrl Pts',(56.8677715409266,-45.3468988006202,12.));
#59565=CARTESIAN_POINT('Ctrl Pts',(56.8435781475982,-45.3394729414932,12.));
#59566=CARTESIAN_POINT('Ctrl Pts',(56.8194296202292,-45.3320357565241,12.));
#59567=CARTESIAN_POINT('Ctrl Pts',(56.7953260434521,-45.3245873291682,12.));
#59568=CARTESIAN_POINT('Ctrl Pts',(56.771267502148,-45.3171277432592,12.));
#59569=CARTESIAN_POINT('Ctrl Pts',(56.747254081454,-45.3096570830107,12.));
#59570=CARTESIAN_POINT('Ctrl Pts',(56.7232858667697,-45.3021754330169,12.));
#59571=CARTESIAN_POINT('Ctrl Pts',(56.6993629437596,-45.2946828782557,12.));
#59572=CARTESIAN_POINT('Ctrl Pts',(56.6754853983535,-45.2871795040912,12.));
#59573=CARTESIAN_POINT('Ctrl Pts',(56.6516533167398,-45.2796653962796,12.));
#59574=CARTESIAN_POINT('Ctrl Pts',(56.6278667853716,-45.2721406409707,12.));
#59575=CARTESIAN_POINT('Ctrl Pts',(56.604125890975,-45.2646053247094,12.));
#59576=CARTESIAN_POINT('Ctrl Pts',(56.5804307205507,-45.2570595344382,12.));
#59577=CARTESIAN_POINT('Ctrl Pts',(56.5567813613752,-45.2495033574997,12.));
#59578=CARTESIAN_POINT('Ctrl Pts',(56.533177900995,-45.2419368816424,12.));
#59579=CARTESIAN_POINT('Ctrl Pts',(56.5096204272299,-45.2343601950222,12.));
#59580=CARTESIAN_POINT('Ctrl Pts',(56.4861090281819,-45.2267733862046,12.));
#59581=CARTESIAN_POINT('Ctrl Pts',(56.4626437922385,-45.2191765441666,12.));
#59582=CARTESIAN_POINT('Ctrl Pts',(56.4392248080733,-45.2115697583002,12.));
#59583=CARTESIAN_POINT('Ctrl Pts',(56.4158521646412,-45.2039531184172,12.));
#59584=CARTESIAN_POINT('Ctrl Pts',(56.3925259511804,-45.1963267147527,12.));
#59585=CARTESIAN_POINT('Ctrl Pts',(56.3692462572228,-45.1886906379664,12.));
#59586=CARTESIAN_POINT('Ctrl Pts',(56.3460131725962,-45.1810449791451,12.));
#59587=CARTESIAN_POINT('Ctrl Pts',(56.3228267874265,-45.1733898298062,12.));
#59588=CARTESIAN_POINT('Ctrl Pts',(56.2996871921321,-45.1657252819018,12.));
#59589=CARTESIAN_POINT('Ctrl Pts',(56.2765944774252,-45.158051427823,12.));
#59590=CARTESIAN_POINT('Ctrl Pts',(56.2535487343227,-45.150368360401,12.));
#59591=CARTESIAN_POINT('Ctrl Pts',(56.2305500541491,-45.1426761729107,12.));
#59592=CARTESIAN_POINT('Ctrl Pts',(56.2075985285391,-45.1349749590736,12.));
#59593=CARTESIAN_POINT('Ctrl Pts',(56.1846942494321,-45.1272648130627,12.));
#59594=CARTESIAN_POINT('Ctrl Pts',(56.1618373090729,-45.119545829506,12.));
#59595=CARTESIAN_POINT('Ctrl Pts',(56.1390278000226,-45.1118181034888,12.));
#59596=CARTESIAN_POINT('Ctrl Pts',(56.1162658151621,-45.1040817305563,12.));
#59597=CARTESIAN_POINT('Ctrl Pts',(56.0935514476945,-45.0963368067177,12.));
#59598=CARTESIAN_POINT('Ctrl Pts',(56.070884791141,-45.0885834284513,12.));
#59599=CARTESIAN_POINT('Ctrl Pts',(56.0482659393412,-45.0808216927082,12.));
#59600=CARTESIAN_POINT('Ctrl Pts',(56.025694986463,-45.0730516969142,12.));
#59601=CARTESIAN_POINT('Ctrl Pts',(56.0031720270074,-45.0652735389729,12.));
#59602=CARTESIAN_POINT('Ctrl Pts',(55.9806971558099,-45.0574873172696,12.));
#59603=CARTESIAN_POINT('Ctrl Pts',(55.958270468037,-45.0496931306767,12.));
#59604=CARTESIAN_POINT('Ctrl Pts',(55.9358920591861,-45.041891078557,12.));
#59605=CARTESIAN_POINT('Ctrl Pts',(55.9135620250977,-45.0340812607676,12.));
#59606=CARTESIAN_POINT('Ctrl Pts',(55.8912804619588,-45.0262637776623,12.));
#59607=CARTESIAN_POINT('Ctrl Pts',(55.8690474663058,-45.0184387300968,12.));
#59608=CARTESIAN_POINT('Ctrl Pts',(55.8468631350195,-45.0106062194325,12.));
#59609=CARTESIAN_POINT('Ctrl Pts',(55.8247275653257,-45.002766347541,12.));
#59610=CARTESIAN_POINT('Ctrl Pts',(55.8026408548078,-44.9949192168073,12.));
#59611=CARTESIAN_POINT('Ctrl Pts',(55.7806031014093,-44.9870649301333,12.));
#59612=CARTESIAN_POINT('Ctrl Pts',(55.7586144034376,-44.979203590942,12.));
#59613=CARTESIAN_POINT('Ctrl Pts',(55.7366748595582,-44.9713353031827,12.));
#59614=CARTESIAN_POINT('Ctrl Pts',(55.7147845687969,-44.9634601713352,12.));
#59615=CARTESIAN_POINT('Ctrl Pts',(55.6929436305522,-44.9555783004133,12.));
#59616=CARTESIAN_POINT('Ctrl Pts',(55.671152144599,-44.9476897959694,12.));
#59617=CARTESIAN_POINT('Ctrl Pts',(55.6494102110922,-44.9397947640996,12.));
#59618=CARTESIAN_POINT('Ctrl Pts',(55.6277179305604,-44.9318933114483,12.));
#59619=CARTESIAN_POINT('Ctrl Pts',(55.6060754039089,-44.9239855452119,12.));
#59620=CARTESIAN_POINT('Ctrl Pts',(55.5844827324315,-44.9160715731425,12.));
#59621=CARTESIAN_POINT('Ctrl Pts',(55.5629400178136,-44.9081515035526,12.));
#59622=CARTESIAN_POINT('Ctrl Pts',(55.541447362135,-44.9002254453192,12.));
#59623=CARTESIAN_POINT('Ctrl Pts',(55.5200048678648,-44.8922935078905,12.));
#59624=CARTESIAN_POINT('Ctrl Pts',(55.4986126378676,-44.8843558012903,12.));
#59625=CARTESIAN_POINT('Ctrl Pts',(55.4772707754139,-44.8764124361218,12.));
#59626=CARTESIAN_POINT('Ctrl Pts',(55.4559793841838,-44.8684635235727,12.));
#59627=CARTESIAN_POINT('Ctrl Pts',(55.4347385682697,-44.8605091754208,12.));
#59628=CARTESIAN_POINT('Ctrl Pts',(55.4135484321706,-44.8525495040398,12.));
#59629=CARTESIAN_POINT('Ctrl Pts',(55.3924090808002,-44.8445846224034,12.));
#59630=CARTESIAN_POINT('Ctrl Pts',(55.3713206194962,-44.8366146440896,12.));
#59631=CARTESIAN_POINT('Ctrl Pts',(55.3502831540229,-44.8286396832849,12.));
#59632=CARTESIAN_POINT('Ctrl Pts',(55.3292967905725,-44.8206598547889,12.));
#59633=CARTESIAN_POINT('Ctrl Pts',(55.3083616357605,-44.812675274021,12.));
#59634=CARTESIAN_POINT('Ctrl Pts',(55.2874777966349,-44.8046860570245,12.));
#59635=CARTESIAN_POINT('Ctrl Pts',(55.2666453806882,-44.7966923204741,12.));
#59636=CARTESIAN_POINT('Ctrl Pts',(55.2458644958617,-44.7886941816823,12.));
#59637=CARTESIAN_POINT('Ctrl Pts',(55.2251352505475,-44.7806917586077,12.));
#59638=CARTESIAN_POINT('Ctrl Pts',(55.2044577535866,-44.7726851698619,12.));
#59639=CARTESIAN_POINT('Ctrl Pts',(55.1838321142779,-44.7646745347109,12.));
#59640=CARTESIAN_POINT('Ctrl Pts',(55.1632584423815,-44.7566599730773,12.));
#59641=CARTESIAN_POINT('Ctrl Pts',(55.14273684812,-44.748641605542,12.));
#59642=CARTESIAN_POINT('Ctrl Pts',(55.1222674421743,-44.740619553348,12.));
#59643=CARTESIAN_POINT('Ctrl Pts',(55.1018503356795,-44.7325939384035,12.));
#59644=CARTESIAN_POINT('Ctrl Pts',(55.0814856402495,-44.7245648832979,12.));
#59645=CARTESIAN_POINT('Ctrl Pts',(55.0611734679894,-44.716532511316,12.));
#59646=CARTESIAN_POINT('Ctrl Pts',(55.0409139315078,-44.7084969464513,12.));
#59647=CARTESIAN_POINT('Ctrl Pts',(55.0207071439237,-44.7004583134249,12.));
#59648=CARTESIAN_POINT('Ctrl Pts',(55.0005532188667,-44.6924167376869,12.));
#59649=CARTESIAN_POINT('Ctrl Pts',(54.9804522704686,-44.6843723454,12.));
#59650=CARTESIAN_POINT('Ctrl Pts',(54.9604044133501,-44.6763252634259,12.));
#59651=CARTESIAN_POINT('Ctrl Pts',(54.9404097626077,-44.6682756193147,12.));
#59652=CARTESIAN_POINT('Ctrl Pts',(54.9204684337822,-44.6602235412836,12.));
#59653=CARTESIAN_POINT('Ctrl Pts',(54.9005805428969,-44.6521691582534,12.));
#59654=CARTESIAN_POINT('Ctrl Pts',(54.8807462065164,-44.6441125999063,12.));
#59655=CARTESIAN_POINT('Ctrl Pts',(54.860965541796,-44.6360539967392,12.));
#59656=CARTESIAN_POINT('Ctrl Pts',(54.8412386665276,-44.6279934801169,12.));
#59657=CARTESIAN_POINT('Ctrl Pts',(54.8215656991837,-44.6199311823293,12.));
#59658=CARTESIAN_POINT('Ctrl Pts',(54.8019467588278,-44.6118672364906,12.));
#59659=CARTESIAN_POINT('Ctrl Pts',(54.7823819650148,-44.603801776431,12.));
#59660=CARTESIAN_POINT('Ctrl Pts',(54.7628714377037,-44.5957349366059,12.));
#59661=CARTESIAN_POINT('Ctrl Pts',(54.7434152971267,-44.5876668519661,12.));
#59662=CARTESIAN_POINT('Ctrl Pts',(54.7240136637717,-44.5795976579454,12.));
#59663=CARTESIAN_POINT('Ctrl Pts',(54.7046666586754,-44.5715274907619,12.));
#59664=CARTESIAN_POINT('Ctrl Pts',(54.6853744036751,-44.5634564876863,12.));
#59665=CARTESIAN_POINT('Ctrl Pts',(54.6661370216252,-44.5553847872721,12.));
#59666=CARTESIAN_POINT('Ctrl Pts',(54.6469546367408,-44.5473125297312,12.));
#59667=CARTESIAN_POINT('Ctrl Pts',(54.6278273743587,-44.5392398566802,12.));
#59668=CARTESIAN_POINT('Ctrl Pts',(54.6087553602914,-44.5311669104515,12.));
#59669=CARTESIAN_POINT('Ctrl Pts',(54.5897387202815,-44.5230938335167,12.));
#59670=CARTESIAN_POINT('Ctrl Pts',(54.5707775794412,-44.5150207678988,12.));
#59671=CARTESIAN_POINT('Ctrl Pts',(54.5518720616016,-44.5069478544945,12.));
#59672=CARTESIAN_POINT('Ctrl Pts',(54.5330222905438,-44.4988752343715,12.));
#59673=CARTESIAN_POINT('Ctrl Pts',(54.5142283914684,-44.4908030503209,12.));
#59674=CARTESIAN_POINT('Ctrl Pts',(54.4954904921938,-44.4827314481271,12.));
#59675=CARTESIAN_POINT('Ctrl Pts',(54.4768087248854,-44.4746605784056,12.));
#59676=CARTESIAN_POINT('Ctrl Pts',(54.4581832262072,-44.4665905967701,12.));
#59677=CARTESIAN_POINT('Ctrl Pts',(54.4396141337008,-44.4585216599933,12.));
#59678=CARTESIAN_POINT('Ctrl Pts',(54.4211015825959,-44.4504539226336,12.));
#59679=CARTESIAN_POINT('Ctrl Pts',(54.4026457030316,-44.442387534098,12.));
#59680=CARTESIAN_POINT('Ctrl Pts',(54.3842466156151,-44.4343226339555,12.));
#59681=CARTESIAN_POINT('Ctrl Pts',(54.3659044357064,-44.4262593564664,12.));
#59682=CARTESIAN_POINT('Ctrl Pts',(54.347619281931,-44.4181978395814,12.));
#59683=CARTESIAN_POINT('Ctrl Pts',(54.3293912830237,-44.4101382321834,12.));
#59684=CARTESIAN_POINT('Ctrl Pts',(54.3112205860776,-44.4020807028144,12.));
#59685=CARTESIAN_POINT('Ctrl Pts',(54.2931073621661,-44.3940254456427,12.));
#59686=CARTESIAN_POINT('Ctrl Pts',(54.2750517888695,-44.3859726620288,12.));
#59687=CARTESIAN_POINT('Ctrl Pts',(54.2570540336536,-44.3779225430461,12.));
#59688=CARTESIAN_POINT('Ctrl Pts',(54.2391142386354,-44.369875253351,12.));
#59689=CARTESIAN_POINT('Ctrl Pts',(54.2212325005847,-44.3618309103245,12.));
#59690=CARTESIAN_POINT('Ctrl Pts',(54.203408870162,-44.3537895823819,12.));
#59691=CARTESIAN_POINT('Ctrl Pts',(54.1891964684439,-44.3473589597468,12.));
#59692=CARTESIAN_POINT('Ctrl Pts',(54.1785633257456,-44.3425373700829,12.));
#59693=CARTESIAN_POINT('Ctrl Pts',(54.1714861895278,-44.3393235891014,12.));
#59694=CARTESIAN_POINT('Ctrl Pts',(54.1679505278134,-44.3377168516418,12.));
#59695=CARTESIAN_POINT('Ctrl Pts',(59.3276657444391,-44.569626075779,0.));
#59696=CARTESIAN_POINT('Ctrl Pts',(59.3276657444391,-44.569626075779,4.));
#59697=CARTESIAN_POINT('Ctrl Pts',(59.3276657444392,-44.5696260757792,8.));
#59698=CARTESIAN_POINT('Ctrl Pts',(59.3276657444392,-44.5696260757792,12.));
#59699=CARTESIAN_POINT('Ctrl Pts',(59.3806648691717,-44.6658822400931,0.));
#59700=CARTESIAN_POINT('Ctrl Pts',(59.3806648691717,-44.6658822400931,4.));
#59701=CARTESIAN_POINT('Ctrl Pts',(59.3806648691718,-44.6658822400932,8.00000000000001));
#59702=CARTESIAN_POINT('Ctrl Pts',(59.3806648691718,-44.6658822400932,12.));
#59703=CARTESIAN_POINT('Ctrl Pts',(59.4154499491515,-44.8655383388338,0.));
#59704=CARTESIAN_POINT('Ctrl Pts',(59.4154499491515,-44.8655383388338,4.));
#59705=CARTESIAN_POINT('Ctrl Pts',(59.4154499491515,-44.8655383388339,7.99999999999999));
#59706=CARTESIAN_POINT('Ctrl Pts',(59.4154499491515,-44.8655383388339,12.));
#59707=CARTESIAN_POINT('Ctrl Pts',(59.3374774995078,-45.0479805952316,0.));
#59708=CARTESIAN_POINT('Ctrl Pts',(59.3374774995078,-45.0479805952316,4.));
#59709=CARTESIAN_POINT('Ctrl Pts',(59.3374774995078,-45.0479805952316,8.00000000000001));
#59710=CARTESIAN_POINT('Ctrl Pts',(59.3374774995078,-45.0479805952316,12.));
#59711=CARTESIAN_POINT('Ctrl Pts',(59.2875729049562,-45.1135644683446,0.));
#59712=CARTESIAN_POINT('Ctrl Pts',(59.2875729049562,-45.1135644683446,4.));
#59713=CARTESIAN_POINT('Ctrl Pts',(59.2875729049562,-45.1135644683447,8.));
#59714=CARTESIAN_POINT('Ctrl Pts',(59.2875729049562,-45.1135644683447,12.));
#59715=CARTESIAN_POINT('',(59.3276657444391,-44.569626075779,0.));
#59716=CARTESIAN_POINT('',(59.2875729049563,-45.1135644683447,0.));
#59717=CARTESIAN_POINT('Ctrl Pts',(59.3276657444391,-44.569626075779,1.38777878078145E-16));
#59718=CARTESIAN_POINT('Ctrl Pts',(59.3806648691717,-44.6658822400931,1.38777878078145E-16));
#59719=CARTESIAN_POINT('Ctrl Pts',(59.4005420577316,-44.7799714393735,1.38777878078145E-16));
#59720=CARTESIAN_POINT('Ctrl Pts',(59.3836004611083,-44.8884397921746,1.38777878078145E-16));
#59721=CARTESIAN_POINT('Ctrl Pts',(59.3708942636408,-44.9697910567754,1.38777878078145E-16));
#59722=CARTESIAN_POINT('Ctrl Pts',(59.3374774995078,-45.0479805952316,1.38777878078144E-16));
#59723=CARTESIAN_POINT('Ctrl Pts',(59.2875729049562,-45.1135644683446,1.38777878078145E-16));
#59724=CARTESIAN_POINT('',(59.2875729049563,-45.1135644683447,12.));
#59725=CARTESIAN_POINT('Ctrl Pts',(59.2875729049562,-45.1135644683446,0.));
#59726=CARTESIAN_POINT('Ctrl Pts',(59.2875729049562,-45.1135644683446,4.));
#59727=CARTESIAN_POINT('Ctrl Pts',(59.2875729049562,-45.1135644683447,8.));
#59728=CARTESIAN_POINT('Ctrl Pts',(59.2875729049562,-45.1135644683447,12.));
#59729=CARTESIAN_POINT('',(59.3276657444392,-44.5696260757792,12.));
#59730=CARTESIAN_POINT('Ctrl Pts',(59.2875729049562,-45.1135644683447,12.));
#59731=CARTESIAN_POINT('Ctrl Pts',(59.3374774995078,-45.0479805952316,12.));
#59732=CARTESIAN_POINT('Ctrl Pts',(59.3708942636408,-44.9697910567755,12.));
#59733=CARTESIAN_POINT('Ctrl Pts',(59.3836004611083,-44.8884397921747,12.));
#59734=CARTESIAN_POINT('Ctrl Pts',(59.4005420577316,-44.7799714393736,12.));
#59735=CARTESIAN_POINT('Ctrl Pts',(59.3806648691718,-44.6658822400932,12.));
#59736=CARTESIAN_POINT('Ctrl Pts',(59.3276657444392,-44.5696260757792,12.));
#59737=CARTESIAN_POINT('Ctrl Pts',(59.3276657444392,-44.5696260757792,12.));
#59738=CARTESIAN_POINT('Ctrl Pts',(59.3276657444392,-44.5696260757792,8.));
#59739=CARTESIAN_POINT('Ctrl Pts',(59.3276657444391,-44.569626075779,4.));
#59740=CARTESIAN_POINT('Ctrl Pts',(59.3276657444391,-44.569626075779,0.));
#59741=CARTESIAN_POINT('Origin',(2.97443977737815E-10,-2.28111678886296E-10,
0.));
#59742=CARTESIAN_POINT('Origin',(2.97443977737815E-10,-2.28111678886296E-10,
12.));
#59743=CARTESIAN_POINT('Origin',(2.97443977737815E-10,-2.28111678886296E-10,
0.));
#59744=CARTESIAN_POINT('Ctrl Pts',(54.7233670476848,-50.5529731960877,0.));
#59745=CARTESIAN_POINT('Ctrl Pts',(54.7233670476848,-50.5529731960877,4.));
#59746=CARTESIAN_POINT('Ctrl Pts',(54.7233670476849,-50.5529731960877,8.));
#59747=CARTESIAN_POINT('Ctrl Pts',(54.7233670476849,-50.5529731960877,12.));
#59748=CARTESIAN_POINT('Ctrl Pts',(54.6488048279281,-50.6336864649949,0.));
#59749=CARTESIAN_POINT('Ctrl Pts',(54.6488048279281,-50.6336864649949,4.));
#59750=CARTESIAN_POINT('Ctrl Pts',(54.6488048279282,-50.6336864649949,8.));
#59751=CARTESIAN_POINT('Ctrl Pts',(54.6488048279282,-50.6336864649949,12.));
#59752=CARTESIAN_POINT('Ctrl Pts',(54.4703879751549,-50.7298112257547,0.));
#59753=CARTESIAN_POINT('Ctrl Pts',(54.4703879751549,-50.7298112257547,4.));
#59754=CARTESIAN_POINT('Ctrl Pts',(54.470387975155,-50.7298112257547,8.));
#59755=CARTESIAN_POINT('Ctrl Pts',(54.470387975155,-50.7298112257547,12.));
#59756=CARTESIAN_POINT('Ctrl Pts',(54.2726521137402,-50.7135202769403,0.));
#59757=CARTESIAN_POINT('Ctrl Pts',(54.2726521137402,-50.7135202769403,4.));
#59758=CARTESIAN_POINT('Ctrl Pts',(54.2726521137402,-50.7135202769403,8.00000000000001));
#59759=CARTESIAN_POINT('Ctrl Pts',(54.2726521137402,-50.7135202769403,12.));
#59760=CARTESIAN_POINT('Ctrl Pts',(54.194654349997,-50.6869108458685,0.));
#59761=CARTESIAN_POINT('Ctrl Pts',(54.194654349997,-50.6869108458685,4.));
#59762=CARTESIAN_POINT('Ctrl Pts',(54.194654349997,-50.6869108458684,8.));
#59763=CARTESIAN_POINT('Ctrl Pts',(54.194654349997,-50.6869108458684,12.));
#59764=CARTESIAN_POINT('',(54.7233670476848,-50.5529731960877,0.));
#59765=CARTESIAN_POINT('',(54.1946543499969,-50.6869108458685,0.));
#59766=CARTESIAN_POINT('Ctrl Pts',(54.7233670476848,-50.5529731960877,0.));
#59767=CARTESIAN_POINT('Ctrl Pts',(54.6488048279281,-50.6336864649949,0.));
#59768=CARTESIAN_POINT('Ctrl Pts',(54.5468523406292,-50.6886148997148,0.));
#59769=CARTESIAN_POINT('Ctrl Pts',(54.4385916056105,-50.7068361639615,0.));
#59770=CARTESIAN_POINT('Ctrl Pts',(54.3573960543465,-50.7205021121465,0.));
#59771=CARTESIAN_POINT('Ctrl Pts',(54.2726521137402,-50.7135202769403,0.));
#59772=CARTESIAN_POINT('Ctrl Pts',(54.194654349997,-50.6869108458685,0.));
#59773=CARTESIAN_POINT('',(54.1946543499969,-50.6869108458685,12.));
#59774=CARTESIAN_POINT('Ctrl Pts',(54.194654349997,-50.6869108458685,0.));
#59775=CARTESIAN_POINT('Ctrl Pts',(54.194654349997,-50.6869108458685,4.));
#59776=CARTESIAN_POINT('Ctrl Pts',(54.194654349997,-50.6869108458684,8.));
#59777=CARTESIAN_POINT('Ctrl Pts',(54.194654349997,-50.6869108458684,12.));
#59778=CARTESIAN_POINT('',(54.7233670476849,-50.5529731960877,12.));
#59779=CARTESIAN_POINT('Ctrl Pts',(54.194654349997,-50.6869108458684,12.));
#59780=CARTESIAN_POINT('Ctrl Pts',(54.2726521137402,-50.7135202769403,12.));
#59781=CARTESIAN_POINT('Ctrl Pts',(54.3573960543465,-50.7205021121465,12.));
#59782=CARTESIAN_POINT('Ctrl Pts',(54.4385916056105,-50.7068361639615,12.));
#59783=CARTESIAN_POINT('Ctrl Pts',(54.5468523406292,-50.6886148997148,12.));
#59784=CARTESIAN_POINT('Ctrl Pts',(54.6488048279282,-50.6336864649949,12.));
#59785=CARTESIAN_POINT('Ctrl Pts',(54.7233670476849,-50.5529731960877,12.));
#59786=CARTESIAN_POINT('Ctrl Pts',(54.7233670476849,-50.5529731960877,12.));
#59787=CARTESIAN_POINT('Ctrl Pts',(54.7233670476849,-50.5529731960877,8.));
#59788=CARTESIAN_POINT('Ctrl Pts',(54.7233670476848,-50.5529731960877,4.));
#59789=CARTESIAN_POINT('Ctrl Pts',(54.7233670476848,-50.5529731960877,0.));
#59790=CARTESIAN_POINT('Ctrl Pts',(50.0975384783634,-48.8900464144686,0.));
#59791=CARTESIAN_POINT('Ctrl Pts',(50.0975384783634,-48.8900464144686,12.));
#59792=CARTESIAN_POINT('Ctrl Pts',(50.1009206494209,-48.8919551910299,0.));
#59793=CARTESIAN_POINT('Ctrl Pts',(50.1009206494209,-48.8919551910299,12.));
#59794=CARTESIAN_POINT('Ctrl Pts',(50.1076907555303,-48.8957735556681,0.));
#59795=CARTESIAN_POINT('Ctrl Pts',(50.1076907555303,-48.8957735556681,12.));
#59796=CARTESIAN_POINT('Ctrl Pts',(50.1178632066821,-48.9015035371772,0.));
#59797=CARTESIAN_POINT('Ctrl Pts',(50.1178632066821,-48.9015035371772,12.));
#59798=CARTESIAN_POINT('Ctrl Pts',(50.1314610602286,-48.9091483817797,0.));
#59799=CARTESIAN_POINT('Ctrl Pts',(50.1314610602286,-48.9091483817797,12.));
#59800=CARTESIAN_POINT('Ctrl Pts',(50.148516018447,-48.9187125417897,0.));
#59801=CARTESIAN_POINT('Ctrl Pts',(50.148516018447,-48.9187125417897,12.));
#59802=CARTESIAN_POINT('Ctrl Pts',(50.1656286003943,-48.9282847698237,0.));
#59803=CARTESIAN_POINT('Ctrl Pts',(50.1656286003943,-48.9282847698237,12.));
#59804=CARTESIAN_POINT('Ctrl Pts',(50.1827987615659,-48.9378649933116,0.));
#59805=CARTESIAN_POINT('Ctrl Pts',(50.1827987615659,-48.9378649933116,12.));
#59806=CARTESIAN_POINT('Ctrl Pts',(50.2000264157903,-48.9474530868847,0.));
#59807=CARTESIAN_POINT('Ctrl Pts',(50.2000264157903,-48.9474530868847,12.));
#59808=CARTESIAN_POINT('Ctrl Pts',(50.2173114358423,-48.9570488741273,0.));
#59809=CARTESIAN_POINT('Ctrl Pts',(50.2173114358423,-48.9570488741273,12.));
#59810=CARTESIAN_POINT('Ctrl Pts',(50.2346536715465,-48.9666521500969,0.));
#59811=CARTESIAN_POINT('Ctrl Pts',(50.2346536715465,-48.9666521500969,12.));
#59812=CARTESIAN_POINT('Ctrl Pts',(50.252052963548,-48.9762626987227,0.));
#59813=CARTESIAN_POINT('Ctrl Pts',(50.252052963548,-48.9762626987227,12.));
#59814=CARTESIAN_POINT('Ctrl Pts',(50.2695091583472,-48.9858803116649,0.));
#59815=CARTESIAN_POINT('Ctrl Pts',(50.2695091583472,-48.9858803116649,12.));
#59816=CARTESIAN_POINT('Ctrl Pts',(50.2870221241003,-48.9955048082028,0.));
#59817=CARTESIAN_POINT('Ctrl Pts',(50.2870221241003,-48.9955048082028,12.));
#59818=CARTESIAN_POINT('Ctrl Pts',(50.3045917455383,-49.0051360288002,0.));
#59819=CARTESIAN_POINT('Ctrl Pts',(50.3045917455383,-49.0051360288002,12.));
#59820=CARTESIAN_POINT('Ctrl Pts',(50.3222179165102,-49.0147738256925,0.));
#59821=CARTESIAN_POINT('Ctrl Pts',(50.3222179165102,-49.0147738256925,12.));
#59822=CARTESIAN_POINT('Ctrl Pts',(50.3399005337967,-49.0244180550759,0.));
#59823=CARTESIAN_POINT('Ctrl Pts',(50.3399005337967,-49.0244180550759,12.));
#59824=CARTESIAN_POINT('Ctrl Pts',(50.3576394894136,-49.034068567401,0.));
#59825=CARTESIAN_POINT('Ctrl Pts',(50.3576394894136,-49.034068567401,12.));
#59826=CARTESIAN_POINT('Ctrl Pts',(50.3754346667389,-49.0437252024868,0.));
#59827=CARTESIAN_POINT('Ctrl Pts',(50.3754346667389,-49.0437252024868,12.));
#59828=CARTESIAN_POINT('Ctrl Pts',(50.393285944528,-49.0533877945771,0.));
#59829=CARTESIAN_POINT('Ctrl Pts',(50.393285944528,-49.0533877945771,12.));
#59830=CARTESIAN_POINT('Ctrl Pts',(50.4111931994264,-49.0630561755082,0.));
#59831=CARTESIAN_POINT('Ctrl Pts',(50.4111931994264,-49.0630561755082,12.));
#59832=CARTESIAN_POINT('Ctrl Pts',(50.4291563088528,-49.0727301783477,0.));
#59833=CARTESIAN_POINT('Ctrl Pts',(50.4291563088528,-49.0727301783477,12.));
#59834=CARTESIAN_POINT('Ctrl Pts',(50.4471751542717,-49.0824096415339,0.));
#59835=CARTESIAN_POINT('Ctrl Pts',(50.4471751542717,-49.0824096415339,12.));
#59836=CARTESIAN_POINT('Ctrl Pts',(50.465249621057,-49.0920944086973,0.));
#59837=CARTESIAN_POINT('Ctrl Pts',(50.465249621057,-49.0920944086973,12.));
#59838=CARTESIAN_POINT('Ctrl Pts',(50.4833795969296,-49.1017843266782,0.));
#59839=CARTESIAN_POINT('Ctrl Pts',(50.4833795969296,-49.1017843266782,12.));
#59840=CARTESIAN_POINT('Ctrl Pts',(50.5015649708742,-49.1114792441573,0.));
#59841=CARTESIAN_POINT('Ctrl Pts',(50.5015649708742,-49.1114792441573,12.));
#59842=CARTESIAN_POINT('Ctrl Pts',(50.5198056318111,-49.1211790099817,0.));
#59843=CARTESIAN_POINT('Ctrl Pts',(50.5198056318111,-49.1211790099817,12.));
#59844=CARTESIAN_POINT('Ctrl Pts',(50.5381014674822,-49.1308834717645,0.));
#59845=CARTESIAN_POINT('Ctrl Pts',(50.5381014674822,-49.1308834717645,12.));
#59846=CARTESIAN_POINT('Ctrl Pts',(50.5564523650406,-49.1405924766169,0.));
#59847=CARTESIAN_POINT('Ctrl Pts',(50.5564523650406,-49.1405924766169,12.));
#59848=CARTESIAN_POINT('Ctrl Pts',(50.5748582115575,-49.1503058717831,0.));
#59849=CARTESIAN_POINT('Ctrl Pts',(50.5748582115575,-49.1503058717831,12.));
#59850=CARTESIAN_POINT('Ctrl Pts',(50.593318894516,-49.1600235052613,0.));
#59851=CARTESIAN_POINT('Ctrl Pts',(50.593318894516,-49.1600235052613,12.));
#59852=CARTESIAN_POINT('Ctrl Pts',(50.6118343023937,-49.1697452265473,0.));
#59853=CARTESIAN_POINT('Ctrl Pts',(50.6118343023937,-49.1697452265473,12.));
#59854=CARTESIAN_POINT('Ctrl Pts',(50.6304043248796,-49.1794708869074,0.));
#59855=CARTESIAN_POINT('Ctrl Pts',(50.6304043248796,-49.1794708869074,12.));
#59856=CARTESIAN_POINT('Ctrl Pts',(50.6490288525639,-49.1892003389743,0.));
#59857=CARTESIAN_POINT('Ctrl Pts',(50.6490288525639,-49.1892003389743,12.));
#59858=CARTESIAN_POINT('Ctrl Pts',(50.6677077767427,-49.1989334364992,0.));
#59859=CARTESIAN_POINT('Ctrl Pts',(50.6677077767427,-49.1989334364992,12.));
#59860=CARTESIAN_POINT('Ctrl Pts',(50.6864409891905,-49.2086700340625,0.));
#59861=CARTESIAN_POINT('Ctrl Pts',(50.6864409891905,-49.2086700340625,12.));
#59862=CARTESIAN_POINT('Ctrl Pts',(50.7052283818941,-49.218409986748,0.));
#59863=CARTESIAN_POINT('Ctrl Pts',(50.7052283818941,-49.218409986748,12.));
#59864=CARTESIAN_POINT('Ctrl Pts',(50.7240698470698,-49.2281531501569,0.));
#59865=CARTESIAN_POINT('Ctrl Pts',(50.7240698470698,-49.2281531501569,12.));
#59866=CARTESIAN_POINT('Ctrl Pts',(50.7429652772816,-49.2378993805482,0.));
#59867=CARTESIAN_POINT('Ctrl Pts',(50.7429652772816,-49.2378993805482,12.));
#59868=CARTESIAN_POINT('Ctrl Pts',(50.7619145655207,-49.2476485349373,0.));
#59869=CARTESIAN_POINT('Ctrl Pts',(50.7619145655207,-49.2476485349373,12.));
#59870=CARTESIAN_POINT('Ctrl Pts',(50.7809176052954,-49.2574004712122,0.));
#59871=CARTESIAN_POINT('Ctrl Pts',(50.7809176052954,-49.2574004712122,12.));
#59872=CARTESIAN_POINT('Ctrl Pts',(50.799974290711,-49.2671550482415,0.));
#59873=CARTESIAN_POINT('Ctrl Pts',(50.799974290711,-49.2671550482415,12.));
#59874=CARTESIAN_POINT('Ctrl Pts',(50.8190845164319,-49.2769121258144,0.));
#59875=CARTESIAN_POINT('Ctrl Pts',(50.8190845164319,-49.2769121258144,12.));
#59876=CARTESIAN_POINT('Ctrl Pts',(50.8382481776392,-49.2866715645828,0.));
#59877=CARTESIAN_POINT('Ctrl Pts',(50.8382481776392,-49.2866715645828,12.));
#59878=CARTESIAN_POINT('Ctrl Pts',(50.8574651699877,-49.2964332260043,0.));
#59879=CARTESIAN_POINT('Ctrl Pts',(50.8574651699877,-49.2964332260043,12.));
#59880=CARTESIAN_POINT('Ctrl Pts',(50.8767353895509,-49.3061969722798,0.));
#59881=CARTESIAN_POINT('Ctrl Pts',(50.8767353895509,-49.3061969722798,12.));
#59882=CARTESIAN_POINT('Ctrl Pts',(50.8960587327869,-49.3159626663129,0.));
#59883=CARTESIAN_POINT('Ctrl Pts',(50.8960587327869,-49.3159626663129,12.));
#59884=CARTESIAN_POINT('Ctrl Pts',(50.9154350965681,-49.325730171735,0.));
#59885=CARTESIAN_POINT('Ctrl Pts',(50.9154350965681,-49.325730171735,12.));
#59886=CARTESIAN_POINT('Ctrl Pts',(50.9348643781928,-49.3354993529163,0.));
#59887=CARTESIAN_POINT('Ctrl Pts',(50.9348643781928,-49.3354993529163,12.));
#59888=CARTESIAN_POINT('Ctrl Pts',(50.9543464753974,-49.3452700749804,0.));
#59889=CARTESIAN_POINT('Ctrl Pts',(50.9543464753974,-49.3452700749804,12.));
#59890=CARTESIAN_POINT('Ctrl Pts',(50.9738812863635,-49.3550422038221,0.));
#59891=CARTESIAN_POINT('Ctrl Pts',(50.9738812863635,-49.3550422038221,12.));
#59892=CARTESIAN_POINT('Ctrl Pts',(50.9934687097179,-49.3648156061049,0.));
#59893=CARTESIAN_POINT('Ctrl Pts',(50.9934687097179,-49.3648156061049,12.));
#59894=CARTESIAN_POINT('Ctrl Pts',(51.0131086445268,-49.3745901492429,0.));
#59895=CARTESIAN_POINT('Ctrl Pts',(51.0131086445268,-49.3745901492429,12.));
#59896=CARTESIAN_POINT('Ctrl Pts',(51.0328009902857,-49.3843657013851,0.));
#59897=CARTESIAN_POINT('Ctrl Pts',(51.0328009902857,-49.3843657013851,12.));
#59898=CARTESIAN_POINT('Ctrl Pts',(51.0525456469072,-49.3941421314014,0.));
#59899=CARTESIAN_POINT('Ctrl Pts',(51.0525456469072,-49.3941421314014,12.));
#59900=CARTESIAN_POINT('Ctrl Pts',(51.0723425146987,-49.4039193088636,0.));
#59901=CARTESIAN_POINT('Ctrl Pts',(51.0723425146987,-49.4039193088636,12.));
#59902=CARTESIAN_POINT('Ctrl Pts',(51.0921914943663,-49.4136971040428,0.));
#59903=CARTESIAN_POINT('Ctrl Pts',(51.0921914943663,-49.4136971040428,12.));
#59904=CARTESIAN_POINT('Ctrl Pts',(51.1120924870196,-49.4234753879071,0.));
#59905=CARTESIAN_POINT('Ctrl Pts',(51.1120924870196,-49.4234753879071,12.));
#59906=CARTESIAN_POINT('Ctrl Pts',(51.1320453941702,-49.4332540321178,0.));
#59907=CARTESIAN_POINT('Ctrl Pts',(51.1320453941702,-49.4332540321178,12.));
#59908=CARTESIAN_POINT('Ctrl Pts',(51.1520501177291,-49.4430329090288,0.));
#59909=CARTESIAN_POINT('Ctrl Pts',(51.1520501177291,-49.4430329090288,12.));
#59910=CARTESIAN_POINT('Ctrl Pts',(51.1721065599972,-49.4528118916833,0.));
#59911=CARTESIAN_POINT('Ctrl Pts',(51.1721065599972,-49.4528118916833,12.));
#59912=CARTESIAN_POINT('Ctrl Pts',(51.1922146236686,-49.4625908538076,0.));
#59913=CARTESIAN_POINT('Ctrl Pts',(51.1922146236686,-49.4625908538076,12.));
#59914=CARTESIAN_POINT('Ctrl Pts',(51.2123742118288,-49.4723696698022,0.));
#59915=CARTESIAN_POINT('Ctrl Pts',(51.2123742118288,-49.4723696698022,12.));
#59916=CARTESIAN_POINT('Ctrl Pts',(51.2325852279507,-49.4821482147357,0.));
#59917=CARTESIAN_POINT('Ctrl Pts',(51.2325852279507,-49.4821482147357,12.));
#59918=CARTESIAN_POINT('Ctrl Pts',(51.2528475758841,-49.4919263643357,0.));
#59919=CARTESIAN_POINT('Ctrl Pts',(51.2528475758841,-49.4919263643357,12.));
#59920=CARTESIAN_POINT('Ctrl Pts',(51.2731611598465,-49.5017039949841,0.));
#59921=CARTESIAN_POINT('Ctrl Pts',(51.2731611598465,-49.5017039949841,12.));
#59922=CARTESIAN_POINT('Ctrl Pts',(51.2935258844278,-49.5114809837111,0.));
#59923=CARTESIAN_POINT('Ctrl Pts',(51.2935258844278,-49.5114809837111,12.));
#59924=CARTESIAN_POINT('Ctrl Pts',(51.3139416545903,-49.5212572081901,0.));
#59925=CARTESIAN_POINT('Ctrl Pts',(51.3139416545903,-49.5212572081901,12.));
#59926=CARTESIAN_POINT('Ctrl Pts',(51.3344083756659,-49.5310325467334,0.));
#59927=CARTESIAN_POINT('Ctrl Pts',(51.3344083756659,-49.5310325467334,12.));
#59928=CARTESIAN_POINT('Ctrl Pts',(51.354925953347,-49.5408068782871,0.));
#59929=CARTESIAN_POINT('Ctrl Pts',(51.354925953347,-49.5408068782871,12.));
#59930=CARTESIAN_POINT('Ctrl Pts',(51.3754942936796,-49.5505800824268,0.));
#59931=CARTESIAN_POINT('Ctrl Pts',(51.3754942936796,-49.5505800824268,12.));
#59932=CARTESIAN_POINT('Ctrl Pts',(51.3961133030688,-49.5603520393514,0.));
#59933=CARTESIAN_POINT('Ctrl Pts',(51.3961133030688,-49.5603520393514,12.));
#59934=CARTESIAN_POINT('Ctrl Pts',(51.4167828882765,-49.5701226298779,0.));
#59935=CARTESIAN_POINT('Ctrl Pts',(51.4167828882765,-49.5701226298779,12.));
#59936=CARTESIAN_POINT('Ctrl Pts',(51.4375029564191,-49.579891735436,0.));
#59937=CARTESIAN_POINT('Ctrl Pts',(51.4375029564191,-49.579891735436,12.));
#59938=CARTESIAN_POINT('Ctrl Pts',(51.4582734149562,-49.5896592380634,0.));
#59939=CARTESIAN_POINT('Ctrl Pts',(51.4582734149562,-49.5896592380634,12.));
#59940=CARTESIAN_POINT('Ctrl Pts',(51.4790941716859,-49.5994250204003,0.));
#59941=CARTESIAN_POINT('Ctrl Pts',(51.4790941716859,-49.5994250204003,12.));
#59942=CARTESIAN_POINT('Ctrl Pts',(51.4999651347496,-49.609188965684,0.));
#59943=CARTESIAN_POINT('Ctrl Pts',(51.4999651347496,-49.609188965684,12.));
#59944=CARTESIAN_POINT('Ctrl Pts',(51.5208862126303,-49.6189509577441,0.));
#59945=CARTESIAN_POINT('Ctrl Pts',(51.5208862126303,-49.6189509577441,12.));
#59946=CARTESIAN_POINT('Ctrl Pts',(51.5418573141494,-49.6287108809975,0.));
#59947=CARTESIAN_POINT('Ctrl Pts',(51.5418573141494,-49.6287108809975,12.));
#59948=CARTESIAN_POINT('Ctrl Pts',(51.5628783484556,-49.6384686204443,0.));
#59949=CARTESIAN_POINT('Ctrl Pts',(51.5628783484556,-49.6384686204443,12.));
#59950=CARTESIAN_POINT('Ctrl Pts',(51.5839492250218,-49.6482240616627,0.));
#59951=CARTESIAN_POINT('Ctrl Pts',(51.5839492250218,-49.6482240616627,12.));
#59952=CARTESIAN_POINT('Ctrl Pts',(51.6050698536525,-49.6579770908063,0.));
#59953=CARTESIAN_POINT('Ctrl Pts',(51.6050698536525,-49.6579770908063,12.));
#59954=CARTESIAN_POINT('Ctrl Pts',(51.6262401444799,-49.6677275945975,0.));
#59955=CARTESIAN_POINT('Ctrl Pts',(51.6262401444799,-49.6677275945975,12.));
#59956=CARTESIAN_POINT('Ctrl Pts',(51.6474600079611,-49.6774754603235,0.));
#59957=CARTESIAN_POINT('Ctrl Pts',(51.6474600079611,-49.6774754603235,12.));
#59958=CARTESIAN_POINT('Ctrl Pts',(51.6687293548656,-49.6872205758314,0.));
#59959=CARTESIAN_POINT('Ctrl Pts',(51.6687293548656,-49.6872205758314,12.));
#59960=CARTESIAN_POINT('Ctrl Pts',(51.6900480962743,-49.6969628295236,0.));
#59961=CARTESIAN_POINT('Ctrl Pts',(51.6900480962743,-49.6969628295236,12.));
#59962=CARTESIAN_POINT('Ctrl Pts',(51.7114161435847,-49.7067021103534,0.));
#59963=CARTESIAN_POINT('Ctrl Pts',(51.7114161435847,-49.7067021103534,12.));
#59964=CARTESIAN_POINT('Ctrl Pts',(51.7328334085084,-49.7164383078206,0.));
#59965=CARTESIAN_POINT('Ctrl Pts',(51.7328334085084,-49.7164383078206,12.));
#59966=CARTESIAN_POINT('Ctrl Pts',(51.7542998030679,-49.7261713119672,0.));
#59967=CARTESIAN_POINT('Ctrl Pts',(51.7542998030679,-49.7261713119672,12.));
#59968=CARTESIAN_POINT('Ctrl Pts',(51.7758152395857,-49.7359010133741,0.));
#59969=CARTESIAN_POINT('Ctrl Pts',(51.7758152395857,-49.7359010133741,12.));
#59970=CARTESIAN_POINT('Ctrl Pts',(51.7973796306826,-49.7456273031555,0.));
#59971=CARTESIAN_POINT('Ctrl Pts',(51.7973796306826,-49.7456273031555,12.));
#59972=CARTESIAN_POINT('Ctrl Pts',(51.8189928892841,-49.7553500729563,0.));
#59973=CARTESIAN_POINT('Ctrl Pts',(51.8189928892841,-49.7553500729563,12.));
#59974=CARTESIAN_POINT('Ctrl Pts',(51.8406549286176,-49.7650692149464,0.));
#59975=CARTESIAN_POINT('Ctrl Pts',(51.8406549286176,-49.7650692149464,12.));
#59976=CARTESIAN_POINT('Ctrl Pts',(51.8623656622092,-49.7747846218177,0.));
#59977=CARTESIAN_POINT('Ctrl Pts',(51.8623656622092,-49.7747846218177,12.));
#59978=CARTESIAN_POINT('Ctrl Pts',(51.8841250038716,-49.78449618678,0.));
#59979=CARTESIAN_POINT('Ctrl Pts',(51.8841250038716,-49.78449618678,12.));
#59980=CARTESIAN_POINT('Ctrl Pts',(51.9059328677051,-49.7942038035568,0.));
#59981=CARTESIAN_POINT('Ctrl Pts',(51.9059328677051,-49.7942038035568,12.));
#59982=CARTESIAN_POINT('Ctrl Pts',(51.9277891681013,-49.8039073663808,0.));
#59983=CARTESIAN_POINT('Ctrl Pts',(51.9277891681013,-49.8039073663808,12.));
#59984=CARTESIAN_POINT('Ctrl Pts',(51.9496938197418,-49.8136067699896,0.));
#59985=CARTESIAN_POINT('Ctrl Pts',(51.9496938197418,-49.8136067699896,12.));
#59986=CARTESIAN_POINT('Ctrl Pts',(51.9716467375938,-49.8233019096224,0.));
#59987=CARTESIAN_POINT('Ctrl Pts',(51.9716467375938,-49.8233019096224,12.));
#59988=CARTESIAN_POINT('Ctrl Pts',(51.9936478369008,-49.8329926810172,0.));
#59989=CARTESIAN_POINT('Ctrl Pts',(51.9936478369008,-49.8329926810172,12.));
#59990=CARTESIAN_POINT('Ctrl Pts',(52.015697033182,-49.8426789804068,0.));
#59991=CARTESIAN_POINT('Ctrl Pts',(52.015697033182,-49.8426789804068,12.));
#59992=CARTESIAN_POINT('Ctrl Pts',(52.0377942422373,-49.8523607045146,0.));
#59993=CARTESIAN_POINT('Ctrl Pts',(52.0377942422373,-49.8523607045146,12.));
#59994=CARTESIAN_POINT('Ctrl Pts',(52.059939380145,-49.8620377505498,0.));
#59995=CARTESIAN_POINT('Ctrl Pts',(52.059939380145,-49.8620377505498,12.));
#59996=CARTESIAN_POINT('Ctrl Pts',(52.0821323632588,-49.871710016205,0.));
#59997=CARTESIAN_POINT('Ctrl Pts',(52.0821323632588,-49.871710016205,12.));
#59998=CARTESIAN_POINT('Ctrl Pts',(52.1043731081968,-49.8813773996523,0.));
#59999=CARTESIAN_POINT('Ctrl Pts',(52.1043731081968,-49.8813773996523,12.));
#60000=CARTESIAN_POINT('Ctrl Pts',(52.1266615318414,-49.8910397995404,0.));
#60001=CARTESIAN_POINT('Ctrl Pts',(52.1266615318414,-49.8910397995404,12.));
#60002=CARTESIAN_POINT('Ctrl Pts',(52.1489975513449,-49.90069711499,0.));
#60003=CARTESIAN_POINT('Ctrl Pts',(52.1489975513449,-49.90069711499,12.));
#60004=CARTESIAN_POINT('Ctrl Pts',(52.1713810841277,-49.9103492455904,0.));
#60005=CARTESIAN_POINT('Ctrl Pts',(52.1713810841277,-49.9103492455904,12.));
#60006=CARTESIAN_POINT('Ctrl Pts',(52.1938120478752,-49.919996091396,0.));
#60007=CARTESIAN_POINT('Ctrl Pts',(52.1938120478752,-49.919996091396,12.));
#60008=CARTESIAN_POINT('Ctrl Pts',(52.2162903605272,-49.9296375529241,0.));
#60009=CARTESIAN_POINT('Ctrl Pts',(52.2162903605272,-49.9296375529241,12.));
#60010=CARTESIAN_POINT('Ctrl Pts',(52.238815940277,-49.9392735311507,0.));
#60011=CARTESIAN_POINT('Ctrl Pts',(52.238815940277,-49.9392735311507,12.));
#60012=CARTESIAN_POINT('Ctrl Pts',(52.2613887055773,-49.9489039275064,0.));
#60013=CARTESIAN_POINT('Ctrl Pts',(52.2613887055773,-49.9489039275064,12.));
#60014=CARTESIAN_POINT('Ctrl Pts',(52.2840085751385,-49.9585286438734,0.));
#60015=CARTESIAN_POINT('Ctrl Pts',(52.2840085751385,-49.9585286438734,12.));
#60016=CARTESIAN_POINT('Ctrl Pts',(52.3066754679264,-49.9681475825824,0.));
#60017=CARTESIAN_POINT('Ctrl Pts',(52.3066754679264,-49.9681475825824,12.));
#60018=CARTESIAN_POINT('Ctrl Pts',(52.3293893031524,-49.9777606464103,0.));
#60019=CARTESIAN_POINT('Ctrl Pts',(52.3293893031524,-49.9777606464103,12.));
#60020=CARTESIAN_POINT('Ctrl Pts',(52.3521500002711,-49.9873677385769,0.));
#60021=CARTESIAN_POINT('Ctrl Pts',(52.3521500002711,-49.9873677385769,12.));
#60022=CARTESIAN_POINT('Ctrl Pts',(52.3749574789865,-49.9969687627402,0.));
#60023=CARTESIAN_POINT('Ctrl Pts',(52.3749574789865,-49.9969687627402,12.));
#60024=CARTESIAN_POINT('Ctrl Pts',(52.3978116592505,-50.0065636229934,0.));
#60025=CARTESIAN_POINT('Ctrl Pts',(52.3978116592505,-50.0065636229934,12.));
#60026=CARTESIAN_POINT('Ctrl Pts',(52.420712461261,-50.0161522238619,0.));
#60027=CARTESIAN_POINT('Ctrl Pts',(52.420712461261,-50.0161522238619,12.));
#60028=CARTESIAN_POINT('Ctrl Pts',(52.4436598054523,-50.0257344703008,0.));
#60029=CARTESIAN_POINT('Ctrl Pts',(52.4436598054523,-50.0257344703008,12.));
#60030=CARTESIAN_POINT('Ctrl Pts',(52.4666536124926,-50.0353102676933,0.));
#60031=CARTESIAN_POINT('Ctrl Pts',(52.4666536124926,-50.0353102676933,12.));
#60032=CARTESIAN_POINT('Ctrl Pts',(52.4896938032896,-50.0448795218453,0.));
#60033=CARTESIAN_POINT('Ctrl Pts',(52.4896938032896,-50.0448795218453,12.));
#60034=CARTESIAN_POINT('Ctrl Pts',(52.5127802989903,-50.0544421389824,0.));
#60035=CARTESIAN_POINT('Ctrl Pts',(52.5127802989903,-50.0544421389824,12.));
#60036=CARTESIAN_POINT('Ctrl Pts',(52.5359130209789,-50.0639980257477,0.));
#60037=CARTESIAN_POINT('Ctrl Pts',(52.5359130209789,-50.0639980257477,12.));
#60038=CARTESIAN_POINT('Ctrl Pts',(52.5590918908691,-50.0735470891996,0.));
#60039=CARTESIAN_POINT('Ctrl Pts',(52.5590918908691,-50.0735470891996,12.));
#60040=CARTESIAN_POINT('Ctrl Pts',(52.5823168304981,-50.0830892368095,0.));
#60041=CARTESIAN_POINT('Ctrl Pts',(52.5823168304981,-50.0830892368095,12.));
#60042=CARTESIAN_POINT('Ctrl Pts',(52.6055877619338,-50.0926243764569,0.));
#60043=CARTESIAN_POINT('Ctrl Pts',(52.6055877619338,-50.0926243764569,12.));
#60044=CARTESIAN_POINT('Ctrl Pts',(52.6289046074743,-50.1021524164261,0.));
#60045=CARTESIAN_POINT('Ctrl Pts',(52.6289046074743,-50.1021524164261,12.));
#60046=CARTESIAN_POINT('Ctrl Pts',(52.6522672896462,-50.1116732654041,0.));
#60047=CARTESIAN_POINT('Ctrl Pts',(52.6522672896462,-50.1116732654041,12.));
#60048=CARTESIAN_POINT('Ctrl Pts',(52.6756757311979,-50.1211868324781,0.));
#60049=CARTESIAN_POINT('Ctrl Pts',(52.6756757311979,-50.1211868324781,12.));
#60050=CARTESIAN_POINT('Ctrl Pts',(52.6991298550928,-50.1306930271343,0.));
#60051=CARTESIAN_POINT('Ctrl Pts',(52.6991298550928,-50.1306930271343,12.));
#60052=CARTESIAN_POINT('Ctrl Pts',(52.7226295845155,-50.1401917592532,0.));
#60053=CARTESIAN_POINT('Ctrl Pts',(52.7226295845155,-50.1401917592532,12.));
#60054=CARTESIAN_POINT('Ctrl Pts',(52.7461748428733,-50.1496829391068,0.));
#60055=CARTESIAN_POINT('Ctrl Pts',(52.7461748428733,-50.1496829391068,12.));
#60056=CARTESIAN_POINT('Ctrl Pts',(52.769765553794,-50.1591664773561,0.));
#60057=CARTESIAN_POINT('Ctrl Pts',(52.769765553794,-50.1591664773561,12.));
#60058=CARTESIAN_POINT('Ctrl Pts',(52.793401641121,-50.1686422850493,0.));
#60059=CARTESIAN_POINT('Ctrl Pts',(52.793401641121,-50.1686422850493,12.));
#60060=CARTESIAN_POINT('Ctrl Pts',(52.8170830289052,-50.1781102736215,0.));
#60061=CARTESIAN_POINT('Ctrl Pts',(52.8170830289052,-50.1781102736215,12.));
#60062=CARTESIAN_POINT('Ctrl Pts',(52.8408096414101,-50.1875703548893,0.));
#60063=CARTESIAN_POINT('Ctrl Pts',(52.8408096414101,-50.1875703548893,12.));
#60064=CARTESIAN_POINT('Ctrl Pts',(52.8645814031137,-50.1970224410476,0.));
#60065=CARTESIAN_POINT('Ctrl Pts',(52.8645814031137,-50.1970224410476,12.));
#60066=CARTESIAN_POINT('Ctrl Pts',(52.8883982387068,-50.2064664446663,0.));
#60067=CARTESIAN_POINT('Ctrl Pts',(52.8883982387068,-50.2064664446663,12.));
#60068=CARTESIAN_POINT('Ctrl Pts',(52.9122600730882,-50.2159022786876,0.));
#60069=CARTESIAN_POINT('Ctrl Pts',(52.9122600730882,-50.2159022786876,12.));
#60070=CARTESIAN_POINT('Ctrl Pts',(52.9361668313539,-50.2253298564237,0.));
#60071=CARTESIAN_POINT('Ctrl Pts',(52.9361668313539,-50.2253298564237,12.));
#60072=CARTESIAN_POINT('Ctrl Pts',(52.9601184388027,-50.2347490915553,0.));
#60073=CARTESIAN_POINT('Ctrl Pts',(52.9601184388027,-50.2347490915553,12.));
#60074=CARTESIAN_POINT('Ctrl Pts',(52.9841148209404,-50.2441598981286,0.));
#60075=CARTESIAN_POINT('Ctrl Pts',(52.9841148209404,-50.2441598981286,12.));
#60076=CARTESIAN_POINT('Ctrl Pts',(53.0081559034802,-50.2535621905553,0.));
#60077=CARTESIAN_POINT('Ctrl Pts',(53.0081559034802,-50.2535621905553,12.));
#60078=CARTESIAN_POINT('Ctrl Pts',(53.0322416123404,-50.2629558836111,0.));
#60079=CARTESIAN_POINT('Ctrl Pts',(53.0322416123404,-50.2629558836111,12.));
#60080=CARTESIAN_POINT('Ctrl Pts',(53.0563718736361,-50.272340892437,0.));
#60081=CARTESIAN_POINT('Ctrl Pts',(53.0563718736361,-50.272340892437,12.));
#60082=CARTESIAN_POINT('Ctrl Pts',(53.0805466136791,-50.2817171325354,0.));
#60083=CARTESIAN_POINT('Ctrl Pts',(53.0805466136791,-50.2817171325354,12.));
#60084=CARTESIAN_POINT('Ctrl Pts',(53.1047657589806,-50.2910845197615,0.));
#60085=CARTESIAN_POINT('Ctrl Pts',(53.1047657589806,-50.2910845197615,12.));
#60086=CARTESIAN_POINT('Ctrl Pts',(53.1290292362482,-50.3004429703188,0.));
#60087=CARTESIAN_POINT('Ctrl Pts',(53.1290292362482,-50.3004429703188,12.));
#60088=CARTESIAN_POINT('Ctrl Pts',(53.153336972382,-50.3097924007536,0.));
#60089=CARTESIAN_POINT('Ctrl Pts',(53.153336972382,-50.3097924007536,12.));
#60090=CARTESIAN_POINT('Ctrl Pts',(53.1776888944622,-50.3191327279497,0.));
#60091=CARTESIAN_POINT('Ctrl Pts',(53.1776888944622,-50.3191327279497,12.));
#60092=CARTESIAN_POINT('Ctrl Pts',(53.202084929748,-50.3284638691285,0.));
#60093=CARTESIAN_POINT('Ctrl Pts',(53.202084929748,-50.3284638691285,12.));
#60094=CARTESIAN_POINT('Ctrl Pts',(53.2265250056896,-50.3377857418522,0.));
#60095=CARTESIAN_POINT('Ctrl Pts',(53.2265250056896,-50.3377857418522,12.));
#60096=CARTESIAN_POINT('Ctrl Pts',(53.2510090499341,-50.3470982640294,0.));
#60097=CARTESIAN_POINT('Ctrl Pts',(53.2510090499341,-50.3470982640294,12.));
#60098=CARTESIAN_POINT('Ctrl Pts',(53.2755369903291,-50.3564013539198,0.));
#60099=CARTESIAN_POINT('Ctrl Pts',(53.2755369903291,-50.3564013539198,12.));
#60100=CARTESIAN_POINT('Ctrl Pts',(53.3001087549222,-50.3656949301424,0.));
#60101=CARTESIAN_POINT('Ctrl Pts',(53.3001087549222,-50.3656949301424,12.));
#60102=CARTESIAN_POINT('Ctrl Pts',(53.3247242719575,-50.3749789116777,0.));
#60103=CARTESIAN_POINT('Ctrl Pts',(53.3247242719575,-50.3749789116777,12.));
#60104=CARTESIAN_POINT('Ctrl Pts',(53.3493834698685,-50.3842532178451,0.));
#60105=CARTESIAN_POINT('Ctrl Pts',(53.3493834698685,-50.3842532178451,12.));
#60106=CARTESIAN_POINT('Ctrl Pts',(53.3740862772673,-50.393517768283,0.));
#60107=CARTESIAN_POINT('Ctrl Pts',(53.3740862772673,-50.393517768283,12.));
#60108=CARTESIAN_POINT('Ctrl Pts',(53.3988326229308,-50.4027724829296,0.));
#60109=CARTESIAN_POINT('Ctrl Pts',(53.3988326229308,-50.4027724829296,12.));
#60110=CARTESIAN_POINT('Ctrl Pts',(53.4236224357846,-50.4120172820054,0.));
#60111=CARTESIAN_POINT('Ctrl Pts',(53.4236224357846,-50.4120172820054,12.));
#60112=CARTESIAN_POINT('Ctrl Pts',(53.4484556448787,-50.4212520859924,0.));
#60113=CARTESIAN_POINT('Ctrl Pts',(53.4484556448787,-50.4212520859924,12.));
#60114=CARTESIAN_POINT('Ctrl Pts',(53.4733321794199,-50.4304768156677,0.));
#60115=CARTESIAN_POINT('Ctrl Pts',(53.4733321794199,-50.4304768156677,12.));
#60116=CARTESIAN_POINT('Ctrl Pts',(53.4982519688032,-50.4396913921389,0.));
#60117=CARTESIAN_POINT('Ctrl Pts',(53.4982519688032,-50.4396913921389,12.));
#60118=CARTESIAN_POINT('Ctrl Pts',(53.5232149426415,-50.4488957368841,0.));
#60119=CARTESIAN_POINT('Ctrl Pts',(53.5232149426415,-50.4488957368841,12.));
#60120=CARTESIAN_POINT('Ctrl Pts',(53.5482210307864,-50.4580897717835,0.));
#60121=CARTESIAN_POINT('Ctrl Pts',(53.5482210307864,-50.4580897717835,12.));
#60122=CARTESIAN_POINT('Ctrl Pts',(53.5732701633602,-50.467273419175,0.));
#60123=CARTESIAN_POINT('Ctrl Pts',(53.5732701633602,-50.467273419175,12.));
#60124=CARTESIAN_POINT('Ctrl Pts',(53.5983622707231,-50.4764466018064,0.));
#60125=CARTESIAN_POINT('Ctrl Pts',(53.5983622707231,-50.4764466018064,12.));
#60126=CARTESIAN_POINT('Ctrl Pts',(53.6234972834055,-50.485609242731,0.));
#60127=CARTESIAN_POINT('Ctrl Pts',(53.6234972834055,-50.485609242731,12.));
#60128=CARTESIAN_POINT('Ctrl Pts',(53.6486751320434,-50.4947612652147,0.));
#60129=CARTESIAN_POINT('Ctrl Pts',(53.6486751320434,-50.4947612652147,12.));
#60130=CARTESIAN_POINT('Ctrl Pts',(53.6738957473158,-50.5039025926531,0.));
#60131=CARTESIAN_POINT('Ctrl Pts',(53.6738957473158,-50.5039025926531,12.));
#60132=CARTESIAN_POINT('Ctrl Pts',(53.6991590598551,-50.5130331484563,0.));
#60133=CARTESIAN_POINT('Ctrl Pts',(53.6991590598551,-50.5130331484563,12.));
#60134=CARTESIAN_POINT('Ctrl Pts',(53.7244650002382,-50.5221528560427,0.));
#60135=CARTESIAN_POINT('Ctrl Pts',(53.7244650002382,-50.5221528560427,12.));
#60136=CARTESIAN_POINT('Ctrl Pts',(53.7498134991714,-50.5312616390789,0.));
#60137=CARTESIAN_POINT('Ctrl Pts',(53.7498134991714,-50.5312616390789,12.));
#60138=CARTESIAN_POINT('Ctrl Pts',(53.7752044876312,-50.5403594216706,0.));
#60139=CARTESIAN_POINT('Ctrl Pts',(53.7752044876312,-50.5403594216706,12.));
#60140=CARTESIAN_POINT('Ctrl Pts',(53.8006378970198,-50.5494461285762,0.));
#60141=CARTESIAN_POINT('Ctrl Pts',(53.8006378970198,-50.5494461285762,12.));
#60142=CARTESIAN_POINT('Ctrl Pts',(53.8261136593064,-50.5585216854082,0.));
#60143=CARTESIAN_POINT('Ctrl Pts',(53.8261136593064,-50.5585216854082,12.));
#60144=CARTESIAN_POINT('Ctrl Pts',(53.8516317071783,-50.567586018852,0.));
#60145=CARTESIAN_POINT('Ctrl Pts',(53.8516317071783,-50.567586018852,12.));
#60146=CARTESIAN_POINT('Ctrl Pts',(53.8771919737007,-50.5766390561861,0.));
#60147=CARTESIAN_POINT('Ctrl Pts',(53.8771919737007,-50.5766390561861,12.));
#60148=CARTESIAN_POINT('Ctrl Pts',(53.9027943919814,-50.5856807248133,0.));
#60149=CARTESIAN_POINT('Ctrl Pts',(53.9027943919814,-50.5856807248133,12.));
#60150=CARTESIAN_POINT('Ctrl Pts',(53.9284388947996,-50.5947109517476,0.));
#60151=CARTESIAN_POINT('Ctrl Pts',(53.9284388947996,-50.5947109517476,12.));
#60152=CARTESIAN_POINT('Ctrl Pts',(53.954125414313,-50.603729663215,0.));
#60153=CARTESIAN_POINT('Ctrl Pts',(53.954125414313,-50.603729663215,12.));
#60154=CARTESIAN_POINT('Ctrl Pts',(53.9798538815561,-50.6127367839738,0.));
#60155=CARTESIAN_POINT('Ctrl Pts',(53.9798538815561,-50.6127367839738,12.));
#60156=CARTESIAN_POINT('Ctrl Pts',(54.0056242268443,-50.6217322378686,0.));
#60157=CARTESIAN_POINT('Ctrl Pts',(54.0056242268443,-50.6217322378686,12.));
#60158=CARTESIAN_POINT('Ctrl Pts',(54.0314363806751,-50.630715949059,0.));
#60159=CARTESIAN_POINT('Ctrl Pts',(54.0314363806751,-50.630715949059,12.));
#60160=CARTESIAN_POINT('Ctrl Pts',(54.0572902745101,-50.6396878430961,0.));
#60161=CARTESIAN_POINT('Ctrl Pts',(54.0572902745101,-50.6396878430961,12.));
#60162=CARTESIAN_POINT('Ctrl Pts',(54.0831858415182,-50.648647847946,0.));
#60163=CARTESIAN_POINT('Ctrl Pts',(54.0831858415182,-50.648647847946,12.));
#60164=CARTESIAN_POINT('Ctrl Pts',(54.1091230175319,-50.657595895318,0.));
#60165=CARTESIAN_POINT('Ctrl Pts',(54.1091230175319,-50.657595895318,12.));
#60166=CARTESIAN_POINT('Ctrl Pts',(54.1351017412721,-50.6665319209798,0.));
#60167=CARTESIAN_POINT('Ctrl Pts',(54.1351017412721,-50.6665319209798,12.));
#60168=CARTESIAN_POINT('Ctrl Pts',(54.1611219522299,-50.6754558618218,0.));
#60169=CARTESIAN_POINT('Ctrl Pts',(54.1611219522299,-50.6754558618218,12.));
#60170=CARTESIAN_POINT('Ctrl Pts',(54.1871835889908,-50.6843676535428,0.));
#60171=CARTESIAN_POINT('Ctrl Pts',(54.1871835889908,-50.6843676535428,12.));
#60172=CARTESIAN_POINT('Ctrl Pts',(54.2132865872968,-50.6932672279758,0.));
#60173=CARTESIAN_POINT('Ctrl Pts',(54.2132865872968,-50.6932672279758,12.));
#60174=CARTESIAN_POINT('Ctrl Pts',(54.2394308784093,-50.7021545108369,0.));
#60175=CARTESIAN_POINT('Ctrl Pts',(54.2394308784093,-50.7021545108369,12.));
#60176=CARTESIAN_POINT('Ctrl Pts',(54.2656163868258,-50.7110294185832,0.));
#60177=CARTESIAN_POINT('Ctrl Pts',(54.2656163868258,-50.7110294185832,12.));
#60178=CARTESIAN_POINT('Ctrl Pts',(54.2918430335414,-50.7198918629632,0.));
#60179=CARTESIAN_POINT('Ctrl Pts',(54.2918430335414,-50.7198918629632,12.));
#60180=CARTESIAN_POINT('Ctrl Pts',(54.3181107400862,-50.7287417566296,0.));
#60181=CARTESIAN_POINT('Ctrl Pts',(54.3181107400862,-50.7287417566296,12.));
#60182=CARTESIAN_POINT('Ctrl Pts',(54.344419432416,-50.7375790185988,0.));
#60183=CARTESIAN_POINT('Ctrl Pts',(54.344419432416,-50.7375790185988,12.));
#60184=CARTESIAN_POINT('Ctrl Pts',(54.3707690445679,-50.7464035792846,0.));
#60185=CARTESIAN_POINT('Ctrl Pts',(54.3707690445679,-50.7464035792846,12.));
#60186=CARTESIAN_POINT('Ctrl Pts',(54.3971595231285,-50.7552153869224,0.));
#60187=CARTESIAN_POINT('Ctrl Pts',(54.3971595231285,-50.7552153869224,12.));
#60188=CARTESIAN_POINT('Ctrl Pts',(54.4235908287188,-50.7640144089601,0.));
#60189=CARTESIAN_POINT('Ctrl Pts',(54.4235908287188,-50.7640144089601,12.));
#60190=CARTESIAN_POINT('Ctrl Pts',(54.4500629335867,-50.772800626886,0.));
#60191=CARTESIAN_POINT('Ctrl Pts',(54.4500629335867,-50.772800626886,12.));
#60192=CARTESIAN_POINT('Ctrl Pts',(54.4712732428597,-50.7798193515479,0.));
#60193=CARTESIAN_POINT('Ctrl Pts',(54.4712732428597,-50.7798193515479,12.));
#60194=CARTESIAN_POINT('Ctrl Pts',(54.4871993224549,-50.7850776288567,0.));
#60195=CARTESIAN_POINT('Ctrl Pts',(54.4871993224549,-50.7850776288567,12.));
#60196=CARTESIAN_POINT('Ctrl Pts',(54.4978248630284,-50.7885805844191,0.));
#60197=CARTESIAN_POINT('Ctrl Pts',(54.4978248630284,-50.7885805844191,12.));
#60198=CARTESIAN_POINT('Ctrl Pts',(54.5031396718592,-50.7903314215393,0.));
#60199=CARTESIAN_POINT('Ctrl Pts',(54.5031396718592,-50.7903314215393,12.));
#60200=CARTESIAN_POINT('',(50.0975384783634,-48.8900464144686,0.));
#60201=CARTESIAN_POINT('Ctrl Pts',(50.0975384783634,-48.8900464144686,0.));
#60202=CARTESIAN_POINT('Ctrl Pts',(50.1009206494209,-48.8919551910299,0.));
#60203=CARTESIAN_POINT('Ctrl Pts',(50.1076907555303,-48.8957735556681,0.));
#60204=CARTESIAN_POINT('Ctrl Pts',(50.1178632066821,-48.9015035371772,0.));
#60205=CARTESIAN_POINT('Ctrl Pts',(50.1314610602286,-48.9091483817797,0.));
#60206=CARTESIAN_POINT('Ctrl Pts',(50.148516018447,-48.9187125417897,0.));
#60207=CARTESIAN_POINT('Ctrl Pts',(50.1656286003943,-48.9282847698237,0.));
#60208=CARTESIAN_POINT('Ctrl Pts',(50.1827987615659,-48.9378649933116,0.));
#60209=CARTESIAN_POINT('Ctrl Pts',(50.2000264157903,-48.9474530868847,0.));
#60210=CARTESIAN_POINT('Ctrl Pts',(50.2173114358423,-48.9570488741273,0.));
#60211=CARTESIAN_POINT('Ctrl Pts',(50.2346536715465,-48.9666521500969,0.));
#60212=CARTESIAN_POINT('Ctrl Pts',(50.252052963548,-48.9762626987227,0.));
#60213=CARTESIAN_POINT('Ctrl Pts',(50.2695091583472,-48.9858803116649,0.));
#60214=CARTESIAN_POINT('Ctrl Pts',(50.2870221241003,-48.9955048082028,0.));
#60215=CARTESIAN_POINT('Ctrl Pts',(50.3045917455383,-49.0051360288002,0.));
#60216=CARTESIAN_POINT('Ctrl Pts',(50.3222179165102,-49.0147738256925,0.));
#60217=CARTESIAN_POINT('Ctrl Pts',(50.3399005337967,-49.0244180550759,0.));
#60218=CARTESIAN_POINT('Ctrl Pts',(50.3576394894136,-49.034068567401,0.));
#60219=CARTESIAN_POINT('Ctrl Pts',(50.3754346667389,-49.0437252024868,0.));
#60220=CARTESIAN_POINT('Ctrl Pts',(50.393285944528,-49.0533877945771,0.));
#60221=CARTESIAN_POINT('Ctrl Pts',(50.4111931994264,-49.0630561755082,0.));
#60222=CARTESIAN_POINT('Ctrl Pts',(50.4291563088528,-49.0727301783477,0.));
#60223=CARTESIAN_POINT('Ctrl Pts',(50.4471751542717,-49.0824096415339,0.));
#60224=CARTESIAN_POINT('Ctrl Pts',(50.465249621057,-49.0920944086973,0.));
#60225=CARTESIAN_POINT('Ctrl Pts',(50.4833795969296,-49.1017843266782,0.));
#60226=CARTESIAN_POINT('Ctrl Pts',(50.5015649708742,-49.1114792441573,0.));
#60227=CARTESIAN_POINT('Ctrl Pts',(50.5198056318111,-49.1211790099817,0.));
#60228=CARTESIAN_POINT('Ctrl Pts',(50.5381014674822,-49.1308834717645,0.));
#60229=CARTESIAN_POINT('Ctrl Pts',(50.5564523650406,-49.1405924766169,0.));
#60230=CARTESIAN_POINT('Ctrl Pts',(50.5748582115575,-49.1503058717831,0.));
#60231=CARTESIAN_POINT('Ctrl Pts',(50.593318894516,-49.1600235052613,0.));
#60232=CARTESIAN_POINT('Ctrl Pts',(50.6118343023937,-49.1697452265473,0.));
#60233=CARTESIAN_POINT('Ctrl Pts',(50.6304043248796,-49.1794708869074,0.));
#60234=CARTESIAN_POINT('Ctrl Pts',(50.6490288525639,-49.1892003389743,0.));
#60235=CARTESIAN_POINT('Ctrl Pts',(50.6677077767427,-49.1989334364992,0.));
#60236=CARTESIAN_POINT('Ctrl Pts',(50.6864409891905,-49.2086700340625,0.));
#60237=CARTESIAN_POINT('Ctrl Pts',(50.7052283818941,-49.218409986748,0.));
#60238=CARTESIAN_POINT('Ctrl Pts',(50.7240698470698,-49.2281531501569,0.));
#60239=CARTESIAN_POINT('Ctrl Pts',(50.7429652772816,-49.2378993805482,0.));
#60240=CARTESIAN_POINT('Ctrl Pts',(50.7619145655207,-49.2476485349373,0.));
#60241=CARTESIAN_POINT('Ctrl Pts',(50.7809176052954,-49.2574004712122,0.));
#60242=CARTESIAN_POINT('Ctrl Pts',(50.799974290711,-49.2671550482415,0.));
#60243=CARTESIAN_POINT('Ctrl Pts',(50.8190845164319,-49.2769121258144,0.));
#60244=CARTESIAN_POINT('Ctrl Pts',(50.8382481776392,-49.2866715645828,0.));
#60245=CARTESIAN_POINT('Ctrl Pts',(50.8574651699877,-49.2964332260043,0.));
#60246=CARTESIAN_POINT('Ctrl Pts',(50.8767353895509,-49.3061969722798,0.));
#60247=CARTESIAN_POINT('Ctrl Pts',(50.8960587327869,-49.3159626663129,0.));
#60248=CARTESIAN_POINT('Ctrl Pts',(50.9154350965681,-49.325730171735,0.));
#60249=CARTESIAN_POINT('Ctrl Pts',(50.9348643781928,-49.3354993529163,0.));
#60250=CARTESIAN_POINT('Ctrl Pts',(50.9543464753974,-49.3452700749804,0.));
#60251=CARTESIAN_POINT('Ctrl Pts',(50.9738812863635,-49.3550422038221,0.));
#60252=CARTESIAN_POINT('Ctrl Pts',(50.9934687097179,-49.3648156061049,0.));
#60253=CARTESIAN_POINT('Ctrl Pts',(51.0131086445268,-49.3745901492429,0.));
#60254=CARTESIAN_POINT('Ctrl Pts',(51.0328009902857,-49.3843657013851,0.));
#60255=CARTESIAN_POINT('Ctrl Pts',(51.0525456469072,-49.3941421314014,0.));
#60256=CARTESIAN_POINT('Ctrl Pts',(51.0723425146987,-49.4039193088636,0.));
#60257=CARTESIAN_POINT('Ctrl Pts',(51.0921914943663,-49.4136971040428,0.));
#60258=CARTESIAN_POINT('Ctrl Pts',(51.1120924870196,-49.4234753879071,0.));
#60259=CARTESIAN_POINT('Ctrl Pts',(51.1320453941702,-49.4332540321178,0.));
#60260=CARTESIAN_POINT('Ctrl Pts',(51.1520501177291,-49.4430329090288,0.));
#60261=CARTESIAN_POINT('Ctrl Pts',(51.1721065599972,-49.4528118916833,0.));
#60262=CARTESIAN_POINT('Ctrl Pts',(51.1922146236686,-49.4625908538076,0.));
#60263=CARTESIAN_POINT('Ctrl Pts',(51.2123742118288,-49.4723696698022,0.));
#60264=CARTESIAN_POINT('Ctrl Pts',(51.2325852279507,-49.4821482147357,0.));
#60265=CARTESIAN_POINT('Ctrl Pts',(51.2528475758841,-49.4919263643357,0.));
#60266=CARTESIAN_POINT('Ctrl Pts',(51.2731611598465,-49.5017039949841,0.));
#60267=CARTESIAN_POINT('Ctrl Pts',(51.2935258844278,-49.5114809837111,0.));
#60268=CARTESIAN_POINT('Ctrl Pts',(51.3139416545903,-49.5212572081901,0.));
#60269=CARTESIAN_POINT('Ctrl Pts',(51.3344083756659,-49.5310325467334,0.));
#60270=CARTESIAN_POINT('Ctrl Pts',(51.354925953347,-49.5408068782871,0.));
#60271=CARTESIAN_POINT('Ctrl Pts',(51.3754942936796,-49.5505800824268,0.));
#60272=CARTESIAN_POINT('Ctrl Pts',(51.3961133030688,-49.5603520393514,0.));
#60273=CARTESIAN_POINT('Ctrl Pts',(51.4167828882765,-49.5701226298779,0.));
#60274=CARTESIAN_POINT('Ctrl Pts',(51.4375029564191,-49.579891735436,0.));
#60275=CARTESIAN_POINT('Ctrl Pts',(51.4582734149562,-49.5896592380634,0.));
#60276=CARTESIAN_POINT('Ctrl Pts',(51.4790941716859,-49.5994250204003,0.));
#60277=CARTESIAN_POINT('Ctrl Pts',(51.4999651347496,-49.609188965684,0.));
#60278=CARTESIAN_POINT('Ctrl Pts',(51.5208862126303,-49.6189509577441,0.));
#60279=CARTESIAN_POINT('Ctrl Pts',(51.5418573141494,-49.6287108809975,0.));
#60280=CARTESIAN_POINT('Ctrl Pts',(51.5628783484556,-49.6384686204443,0.));
#60281=CARTESIAN_POINT('Ctrl Pts',(51.5839492250218,-49.6482240616627,0.));
#60282=CARTESIAN_POINT('Ctrl Pts',(51.6050698536525,-49.6579770908063,0.));
#60283=CARTESIAN_POINT('Ctrl Pts',(51.6262401444799,-49.6677275945975,0.));
#60284=CARTESIAN_POINT('Ctrl Pts',(51.6474600079611,-49.6774754603235,0.));
#60285=CARTESIAN_POINT('Ctrl Pts',(51.6687293548656,-49.6872205758314,0.));
#60286=CARTESIAN_POINT('Ctrl Pts',(51.6900480962743,-49.6969628295236,0.));
#60287=CARTESIAN_POINT('Ctrl Pts',(51.7114161435847,-49.7067021103534,0.));
#60288=CARTESIAN_POINT('Ctrl Pts',(51.7328334085084,-49.7164383078206,0.));
#60289=CARTESIAN_POINT('Ctrl Pts',(51.7542998030679,-49.7261713119672,0.));
#60290=CARTESIAN_POINT('Ctrl Pts',(51.7758152395857,-49.7359010133741,0.));
#60291=CARTESIAN_POINT('Ctrl Pts',(51.7973796306826,-49.7456273031555,0.));
#60292=CARTESIAN_POINT('Ctrl Pts',(51.8189928892841,-49.7553500729563,0.));
#60293=CARTESIAN_POINT('Ctrl Pts',(51.8406549286176,-49.7650692149464,0.));
#60294=CARTESIAN_POINT('Ctrl Pts',(51.8623656622092,-49.7747846218177,0.));
#60295=CARTESIAN_POINT('Ctrl Pts',(51.8841250038716,-49.78449618678,0.));
#60296=CARTESIAN_POINT('Ctrl Pts',(51.9059328677051,-49.7942038035568,0.));
#60297=CARTESIAN_POINT('Ctrl Pts',(51.9277891681013,-49.8039073663808,0.));
#60298=CARTESIAN_POINT('Ctrl Pts',(51.9496938197418,-49.8136067699896,0.));
#60299=CARTESIAN_POINT('Ctrl Pts',(51.9716467375938,-49.8233019096224,0.));
#60300=CARTESIAN_POINT('Ctrl Pts',(51.9936478369008,-49.8329926810172,0.));
#60301=CARTESIAN_POINT('Ctrl Pts',(52.015697033182,-49.8426789804068,0.));
#60302=CARTESIAN_POINT('Ctrl Pts',(52.0377942422373,-49.8523607045146,0.));
#60303=CARTESIAN_POINT('Ctrl Pts',(52.059939380145,-49.8620377505498,0.));
#60304=CARTESIAN_POINT('Ctrl Pts',(52.0821323632588,-49.871710016205,0.));
#60305=CARTESIAN_POINT('Ctrl Pts',(52.1043731081968,-49.8813773996523,0.));
#60306=CARTESIAN_POINT('Ctrl Pts',(52.1266615318414,-49.8910397995404,0.));
#60307=CARTESIAN_POINT('Ctrl Pts',(52.1489975513449,-49.90069711499,0.));
#60308=CARTESIAN_POINT('Ctrl Pts',(52.1713810841277,-49.9103492455904,0.));
#60309=CARTESIAN_POINT('Ctrl Pts',(52.1938120478752,-49.919996091396,0.));
#60310=CARTESIAN_POINT('Ctrl Pts',(52.2162903605272,-49.9296375529241,0.));
#60311=CARTESIAN_POINT('Ctrl Pts',(52.238815940277,-49.9392735311507,0.));
#60312=CARTESIAN_POINT('Ctrl Pts',(52.2613887055773,-49.9489039275064,0.));
#60313=CARTESIAN_POINT('Ctrl Pts',(52.2840085751385,-49.9585286438734,0.));
#60314=CARTESIAN_POINT('Ctrl Pts',(52.3066754679264,-49.9681475825824,0.));
#60315=CARTESIAN_POINT('Ctrl Pts',(52.3293893031524,-49.9777606464103,0.));
#60316=CARTESIAN_POINT('Ctrl Pts',(52.3521500002711,-49.9873677385769,0.));
#60317=CARTESIAN_POINT('Ctrl Pts',(52.3749574789865,-49.9969687627402,0.));
#60318=CARTESIAN_POINT('Ctrl Pts',(52.3978116592505,-50.0065636229934,0.));
#60319=CARTESIAN_POINT('Ctrl Pts',(52.420712461261,-50.0161522238619,0.));
#60320=CARTESIAN_POINT('Ctrl Pts',(52.4436598054523,-50.0257344703008,0.));
#60321=CARTESIAN_POINT('Ctrl Pts',(52.4666536124926,-50.0353102676933,0.));
#60322=CARTESIAN_POINT('Ctrl Pts',(52.4896938032896,-50.0448795218453,0.));
#60323=CARTESIAN_POINT('Ctrl Pts',(52.5127802989903,-50.0544421389824,0.));
#60324=CARTESIAN_POINT('Ctrl Pts',(52.5359130209789,-50.0639980257477,0.));
#60325=CARTESIAN_POINT('Ctrl Pts',(52.5590918908691,-50.0735470891996,0.));
#60326=CARTESIAN_POINT('Ctrl Pts',(52.5823168304981,-50.0830892368095,0.));
#60327=CARTESIAN_POINT('Ctrl Pts',(52.6055877619338,-50.0926243764569,0.));
#60328=CARTESIAN_POINT('Ctrl Pts',(52.6289046074743,-50.1021524164261,0.));
#60329=CARTESIAN_POINT('Ctrl Pts',(52.6522672896462,-50.1116732654041,0.));
#60330=CARTESIAN_POINT('Ctrl Pts',(52.6756757311979,-50.1211868324781,0.));
#60331=CARTESIAN_POINT('Ctrl Pts',(52.6991298550928,-50.1306930271343,0.));
#60332=CARTESIAN_POINT('Ctrl Pts',(52.7226295845155,-50.1401917592532,0.));
#60333=CARTESIAN_POINT('Ctrl Pts',(52.7461748428733,-50.1496829391068,0.));
#60334=CARTESIAN_POINT('Ctrl Pts',(52.769765553794,-50.1591664773561,0.));
#60335=CARTESIAN_POINT('Ctrl Pts',(52.793401641121,-50.1686422850493,0.));
#60336=CARTESIAN_POINT('Ctrl Pts',(52.8170830289052,-50.1781102736215,0.));
#60337=CARTESIAN_POINT('Ctrl Pts',(52.8408096414101,-50.1875703548893,0.));
#60338=CARTESIAN_POINT('Ctrl Pts',(52.8645814031137,-50.1970224410476,0.));
#60339=CARTESIAN_POINT('Ctrl Pts',(52.8883982387068,-50.2064664446663,0.));
#60340=CARTESIAN_POINT('Ctrl Pts',(52.9122600730882,-50.2159022786876,0.));
#60341=CARTESIAN_POINT('Ctrl Pts',(52.9361668313539,-50.2253298564237,0.));
#60342=CARTESIAN_POINT('Ctrl Pts',(52.9601184388027,-50.2347490915553,0.));
#60343=CARTESIAN_POINT('Ctrl Pts',(52.9841148209404,-50.2441598981286,0.));
#60344=CARTESIAN_POINT('Ctrl Pts',(53.0081559034802,-50.2535621905553,0.));
#60345=CARTESIAN_POINT('Ctrl Pts',(53.0322416123404,-50.2629558836111,0.));
#60346=CARTESIAN_POINT('Ctrl Pts',(53.0563718736361,-50.272340892437,0.));
#60347=CARTESIAN_POINT('Ctrl Pts',(53.0805466136791,-50.2817171325354,0.));
#60348=CARTESIAN_POINT('Ctrl Pts',(53.1047657589806,-50.2910845197615,0.));
#60349=CARTESIAN_POINT('Ctrl Pts',(53.1290292362482,-50.3004429703188,0.));
#60350=CARTESIAN_POINT('Ctrl Pts',(53.153336972382,-50.3097924007536,0.));
#60351=CARTESIAN_POINT('Ctrl Pts',(53.1776888944622,-50.3191327279497,0.));
#60352=CARTESIAN_POINT('Ctrl Pts',(53.202084929748,-50.3284638691285,0.));
#60353=CARTESIAN_POINT('Ctrl Pts',(53.2265250056896,-50.3377857418522,0.));
#60354=CARTESIAN_POINT('Ctrl Pts',(53.2510090499341,-50.3470982640294,0.));
#60355=CARTESIAN_POINT('Ctrl Pts',(53.2755369903291,-50.3564013539198,0.));
#60356=CARTESIAN_POINT('Ctrl Pts',(53.3001087549222,-50.3656949301424,0.));
#60357=CARTESIAN_POINT('Ctrl Pts',(53.3247242719575,-50.3749789116777,0.));
#60358=CARTESIAN_POINT('Ctrl Pts',(53.3493834698685,-50.3842532178451,0.));
#60359=CARTESIAN_POINT('Ctrl Pts',(53.3740862772673,-50.393517768283,0.));
#60360=CARTESIAN_POINT('Ctrl Pts',(53.3988326229308,-50.4027724829296,0.));
#60361=CARTESIAN_POINT('Ctrl Pts',(53.4236224357846,-50.4120172820054,0.));
#60362=CARTESIAN_POINT('Ctrl Pts',(53.4484556448787,-50.4212520859924,0.));
#60363=CARTESIAN_POINT('Ctrl Pts',(53.4733321794199,-50.4304768156677,0.));
#60364=CARTESIAN_POINT('Ctrl Pts',(53.4982519688032,-50.4396913921389,0.));
#60365=CARTESIAN_POINT('Ctrl Pts',(53.5232149426415,-50.4488957368841,0.));
#60366=CARTESIAN_POINT('Ctrl Pts',(53.5482210307864,-50.4580897717835,0.));
#60367=CARTESIAN_POINT('Ctrl Pts',(53.5732701633602,-50.467273419175,0.));
#60368=CARTESIAN_POINT('Ctrl Pts',(53.5983622707231,-50.4764466018064,0.));
#60369=CARTESIAN_POINT('Ctrl Pts',(53.6234972834055,-50.485609242731,0.));
#60370=CARTESIAN_POINT('Ctrl Pts',(53.6486751320434,-50.4947612652147,0.));
#60371=CARTESIAN_POINT('Ctrl Pts',(53.6738957473158,-50.5039025926531,0.));
#60372=CARTESIAN_POINT('Ctrl Pts',(53.6991590598551,-50.5130331484563,0.));
#60373=CARTESIAN_POINT('Ctrl Pts',(53.7244650002382,-50.5221528560427,0.));
#60374=CARTESIAN_POINT('Ctrl Pts',(53.7498134991714,-50.5312616390789,0.));
#60375=CARTESIAN_POINT('Ctrl Pts',(53.7752044876312,-50.5403594216706,0.));
#60376=CARTESIAN_POINT('Ctrl Pts',(53.8006378970198,-50.5494461285762,0.));
#60377=CARTESIAN_POINT('Ctrl Pts',(53.8261136593064,-50.5585216854082,0.));
#60378=CARTESIAN_POINT('Ctrl Pts',(53.8516317071783,-50.567586018852,0.));
#60379=CARTESIAN_POINT('Ctrl Pts',(53.8771919737007,-50.5766390561861,0.));
#60380=CARTESIAN_POINT('Ctrl Pts',(53.9027943919814,-50.5856807248133,0.));
#60381=CARTESIAN_POINT('Ctrl Pts',(53.9284388947996,-50.5947109517476,0.));
#60382=CARTESIAN_POINT('Ctrl Pts',(53.954125414313,-50.603729663215,0.));
#60383=CARTESIAN_POINT('Ctrl Pts',(53.9798538815561,-50.6127367839738,0.));
#60384=CARTESIAN_POINT('Ctrl Pts',(54.0056242268443,-50.6217322378686,0.));
#60385=CARTESIAN_POINT('Ctrl Pts',(54.0314363806751,-50.630715949059,0.));
#60386=CARTESIAN_POINT('Ctrl Pts',(54.0572902745101,-50.6396878430961,0.));
#60387=CARTESIAN_POINT('Ctrl Pts',(54.0831858415182,-50.648647847946,0.));
#60388=CARTESIAN_POINT('Ctrl Pts',(54.1091230175319,-50.657595895318,0.));
#60389=CARTESIAN_POINT('Ctrl Pts',(54.1351017412721,-50.6665319209798,0.));
#60390=CARTESIAN_POINT('Ctrl Pts',(54.157406104188,-50.6741814675381,0.));
#60391=CARTESIAN_POINT('Ctrl Pts',(54.1745287898573,-50.6800396668658,0.));
#60392=CARTESIAN_POINT('Ctrl Pts',(54.1864514381918,-50.6841118861801,0.));
#60393=CARTESIAN_POINT('Ctrl Pts',(54.1931619277288,-50.68640169656,0.));
#60394=CARTESIAN_POINT('Ctrl Pts',(54.1946543499969,-50.6869108458685,0.));
#60395=CARTESIAN_POINT('',(50.0975384783634,-48.8900464144686,12.));
#60396=CARTESIAN_POINT('',(50.0975384783634,-48.8900464144686,0.));
#60397=CARTESIAN_POINT('Ctrl Pts',(54.1946543499969,-50.6869108458685,12.));
#60398=CARTESIAN_POINT('Ctrl Pts',(54.1931619277288,-50.68640169656,12.));
#60399=CARTESIAN_POINT('Ctrl Pts',(54.1864514381918,-50.6841118861801,12.));
#60400=CARTESIAN_POINT('Ctrl Pts',(54.1745287898573,-50.6800396668658,12.));
#60401=CARTESIAN_POINT('Ctrl Pts',(54.157406104188,-50.6741814675381,12.));
#60402=CARTESIAN_POINT('Ctrl Pts',(54.1351017412721,-50.6665319209798,12.));
#60403=CARTESIAN_POINT('Ctrl Pts',(54.1091230175319,-50.657595895318,12.));
#60404=CARTESIAN_POINT('Ctrl Pts',(54.0831858415182,-50.648647847946,12.));
#60405=CARTESIAN_POINT('Ctrl Pts',(54.0572902745101,-50.6396878430961,12.));
#60406=CARTESIAN_POINT('Ctrl Pts',(54.0314363806751,-50.630715949059,12.));
#60407=CARTESIAN_POINT('Ctrl Pts',(54.0056242268443,-50.6217322378686,12.));
#60408=CARTESIAN_POINT('Ctrl Pts',(53.9798538815561,-50.6127367839738,12.));
#60409=CARTESIAN_POINT('Ctrl Pts',(53.954125414313,-50.603729663215,12.));
#60410=CARTESIAN_POINT('Ctrl Pts',(53.9284388947996,-50.5947109517476,12.));
#60411=CARTESIAN_POINT('Ctrl Pts',(53.9027943919814,-50.5856807248133,12.));
#60412=CARTESIAN_POINT('Ctrl Pts',(53.8771919737007,-50.5766390561861,12.));
#60413=CARTESIAN_POINT('Ctrl Pts',(53.8516317071783,-50.567586018852,12.));
#60414=CARTESIAN_POINT('Ctrl Pts',(53.8261136593064,-50.5585216854082,12.));
#60415=CARTESIAN_POINT('Ctrl Pts',(53.8006378970198,-50.5494461285762,12.));
#60416=CARTESIAN_POINT('Ctrl Pts',(53.7752044876312,-50.5403594216706,12.));
#60417=CARTESIAN_POINT('Ctrl Pts',(53.7498134991714,-50.5312616390789,12.));
#60418=CARTESIAN_POINT('Ctrl Pts',(53.7244650002382,-50.5221528560427,12.));
#60419=CARTESIAN_POINT('Ctrl Pts',(53.6991590598551,-50.5130331484563,12.));
#60420=CARTESIAN_POINT('Ctrl Pts',(53.6738957473158,-50.5039025926531,12.));
#60421=CARTESIAN_POINT('Ctrl Pts',(53.6486751320434,-50.4947612652147,12.));
#60422=CARTESIAN_POINT('Ctrl Pts',(53.6234972834055,-50.485609242731,12.));
#60423=CARTESIAN_POINT('Ctrl Pts',(53.5983622707231,-50.4764466018064,12.));
#60424=CARTESIAN_POINT('Ctrl Pts',(53.5732701633602,-50.467273419175,12.));
#60425=CARTESIAN_POINT('Ctrl Pts',(53.5482210307864,-50.4580897717835,12.));
#60426=CARTESIAN_POINT('Ctrl Pts',(53.5232149426415,-50.4488957368841,12.));
#60427=CARTESIAN_POINT('Ctrl Pts',(53.4982519688032,-50.4396913921389,12.));
#60428=CARTESIAN_POINT('Ctrl Pts',(53.4733321794199,-50.4304768156677,12.));
#60429=CARTESIAN_POINT('Ctrl Pts',(53.4484556448787,-50.4212520859924,12.));
#60430=CARTESIAN_POINT('Ctrl Pts',(53.4236224357846,-50.4120172820054,12.));
#60431=CARTESIAN_POINT('Ctrl Pts',(53.3988326229308,-50.4027724829296,12.));
#60432=CARTESIAN_POINT('Ctrl Pts',(53.3740862772673,-50.393517768283,12.));
#60433=CARTESIAN_POINT('Ctrl Pts',(53.3493834698685,-50.3842532178451,12.));
#60434=CARTESIAN_POINT('Ctrl Pts',(53.3247242719575,-50.3749789116777,12.));
#60435=CARTESIAN_POINT('Ctrl Pts',(53.3001087549222,-50.3656949301424,12.));
#60436=CARTESIAN_POINT('Ctrl Pts',(53.2755369903291,-50.3564013539198,12.));
#60437=CARTESIAN_POINT('Ctrl Pts',(53.2510090499341,-50.3470982640294,12.));
#60438=CARTESIAN_POINT('Ctrl Pts',(53.2265250056896,-50.3377857418522,12.));
#60439=CARTESIAN_POINT('Ctrl Pts',(53.202084929748,-50.3284638691285,12.));
#60440=CARTESIAN_POINT('Ctrl Pts',(53.1776888944622,-50.3191327279497,12.));
#60441=CARTESIAN_POINT('Ctrl Pts',(53.153336972382,-50.3097924007536,12.));
#60442=CARTESIAN_POINT('Ctrl Pts',(53.1290292362482,-50.3004429703188,12.));
#60443=CARTESIAN_POINT('Ctrl Pts',(53.1047657589806,-50.2910845197615,12.));
#60444=CARTESIAN_POINT('Ctrl Pts',(53.0805466136791,-50.2817171325354,12.));
#60445=CARTESIAN_POINT('Ctrl Pts',(53.0563718736361,-50.272340892437,12.));
#60446=CARTESIAN_POINT('Ctrl Pts',(53.0322416123404,-50.2629558836111,12.));
#60447=CARTESIAN_POINT('Ctrl Pts',(53.0081559034802,-50.2535621905553,12.));
#60448=CARTESIAN_POINT('Ctrl Pts',(52.9841148209404,-50.2441598981286,12.));
#60449=CARTESIAN_POINT('Ctrl Pts',(52.9601184388027,-50.2347490915553,12.));
#60450=CARTESIAN_POINT('Ctrl Pts',(52.9361668313539,-50.2253298564237,12.));
#60451=CARTESIAN_POINT('Ctrl Pts',(52.9122600730882,-50.2159022786876,12.));
#60452=CARTESIAN_POINT('Ctrl Pts',(52.8883982387068,-50.2064664446663,12.));
#60453=CARTESIAN_POINT('Ctrl Pts',(52.8645814031137,-50.1970224410476,12.));
#60454=CARTESIAN_POINT('Ctrl Pts',(52.8408096414101,-50.1875703548893,12.));
#60455=CARTESIAN_POINT('Ctrl Pts',(52.8170830289052,-50.1781102736215,12.));
#60456=CARTESIAN_POINT('Ctrl Pts',(52.793401641121,-50.1686422850493,12.));
#60457=CARTESIAN_POINT('Ctrl Pts',(52.769765553794,-50.1591664773561,12.));
#60458=CARTESIAN_POINT('Ctrl Pts',(52.7461748428733,-50.1496829391068,12.));
#60459=CARTESIAN_POINT('Ctrl Pts',(52.7226295845155,-50.1401917592532,12.));
#60460=CARTESIAN_POINT('Ctrl Pts',(52.6991298550928,-50.1306930271343,12.));
#60461=CARTESIAN_POINT('Ctrl Pts',(52.6756757311979,-50.1211868324781,12.));
#60462=CARTESIAN_POINT('Ctrl Pts',(52.6522672896462,-50.1116732654041,12.));
#60463=CARTESIAN_POINT('Ctrl Pts',(52.6289046074743,-50.1021524164261,12.));
#60464=CARTESIAN_POINT('Ctrl Pts',(52.6055877619338,-50.0926243764569,12.));
#60465=CARTESIAN_POINT('Ctrl Pts',(52.5823168304981,-50.0830892368095,12.));
#60466=CARTESIAN_POINT('Ctrl Pts',(52.5590918908691,-50.0735470891996,12.));
#60467=CARTESIAN_POINT('Ctrl Pts',(52.5359130209789,-50.0639980257477,12.));
#60468=CARTESIAN_POINT('Ctrl Pts',(52.5127802989903,-50.0544421389824,12.));
#60469=CARTESIAN_POINT('Ctrl Pts',(52.4896938032896,-50.0448795218453,12.));
#60470=CARTESIAN_POINT('Ctrl Pts',(52.4666536124926,-50.0353102676933,12.));
#60471=CARTESIAN_POINT('Ctrl Pts',(52.4436598054523,-50.0257344703008,12.));
#60472=CARTESIAN_POINT('Ctrl Pts',(52.420712461261,-50.0161522238619,12.));
#60473=CARTESIAN_POINT('Ctrl Pts',(52.3978116592505,-50.0065636229934,12.));
#60474=CARTESIAN_POINT('Ctrl Pts',(52.3749574789865,-49.9969687627402,12.));
#60475=CARTESIAN_POINT('Ctrl Pts',(52.3521500002711,-49.9873677385769,12.));
#60476=CARTESIAN_POINT('Ctrl Pts',(52.3293893031524,-49.9777606464103,12.));
#60477=CARTESIAN_POINT('Ctrl Pts',(52.3066754679264,-49.9681475825824,12.));
#60478=CARTESIAN_POINT('Ctrl Pts',(52.2840085751385,-49.9585286438734,12.));
#60479=CARTESIAN_POINT('Ctrl Pts',(52.2613887055773,-49.9489039275064,12.));
#60480=CARTESIAN_POINT('Ctrl Pts',(52.238815940277,-49.9392735311507,12.));
#60481=CARTESIAN_POINT('Ctrl Pts',(52.2162903605272,-49.9296375529241,12.));
#60482=CARTESIAN_POINT('Ctrl Pts',(52.1938120478752,-49.919996091396,12.));
#60483=CARTESIAN_POINT('Ctrl Pts',(52.1713810841277,-49.9103492455904,12.));
#60484=CARTESIAN_POINT('Ctrl Pts',(52.1489975513449,-49.90069711499,12.));
#60485=CARTESIAN_POINT('Ctrl Pts',(52.1266615318414,-49.8910397995404,12.));
#60486=CARTESIAN_POINT('Ctrl Pts',(52.1043731081968,-49.8813773996523,12.));
#60487=CARTESIAN_POINT('Ctrl Pts',(52.0821323632588,-49.871710016205,12.));
#60488=CARTESIAN_POINT('Ctrl Pts',(52.059939380145,-49.8620377505498,12.));
#60489=CARTESIAN_POINT('Ctrl Pts',(52.0377942422373,-49.8523607045146,12.));
#60490=CARTESIAN_POINT('Ctrl Pts',(52.015697033182,-49.8426789804068,12.));
#60491=CARTESIAN_POINT('Ctrl Pts',(51.9936478369008,-49.8329926810172,12.));
#60492=CARTESIAN_POINT('Ctrl Pts',(51.9716467375938,-49.8233019096224,12.));
#60493=CARTESIAN_POINT('Ctrl Pts',(51.9496938197418,-49.8136067699896,12.));
#60494=CARTESIAN_POINT('Ctrl Pts',(51.9277891681013,-49.8039073663808,12.));
#60495=CARTESIAN_POINT('Ctrl Pts',(51.9059328677051,-49.7942038035568,12.));
#60496=CARTESIAN_POINT('Ctrl Pts',(51.8841250038716,-49.78449618678,12.));
#60497=CARTESIAN_POINT('Ctrl Pts',(51.8623656622092,-49.7747846218177,12.));
#60498=CARTESIAN_POINT('Ctrl Pts',(51.8406549286176,-49.7650692149464,12.));
#60499=CARTESIAN_POINT('Ctrl Pts',(51.8189928892841,-49.7553500729563,12.));
#60500=CARTESIAN_POINT('Ctrl Pts',(51.7973796306826,-49.7456273031555,12.));
#60501=CARTESIAN_POINT('Ctrl Pts',(51.7758152395857,-49.7359010133741,12.));
#60502=CARTESIAN_POINT('Ctrl Pts',(51.7542998030679,-49.7261713119672,12.));
#60503=CARTESIAN_POINT('Ctrl Pts',(51.7328334085084,-49.7164383078206,12.));
#60504=CARTESIAN_POINT('Ctrl Pts',(51.7114161435847,-49.7067021103534,12.));
#60505=CARTESIAN_POINT('Ctrl Pts',(51.6900480962743,-49.6969628295236,12.));
#60506=CARTESIAN_POINT('Ctrl Pts',(51.6687293548656,-49.6872205758314,12.));
#60507=CARTESIAN_POINT('Ctrl Pts',(51.6474600079611,-49.6774754603235,12.));
#60508=CARTESIAN_POINT('Ctrl Pts',(51.6262401444799,-49.6677275945975,12.));
#60509=CARTESIAN_POINT('Ctrl Pts',(51.6050698536525,-49.6579770908063,12.));
#60510=CARTESIAN_POINT('Ctrl Pts',(51.5839492250218,-49.6482240616627,12.));
#60511=CARTESIAN_POINT('Ctrl Pts',(51.5628783484556,-49.6384686204443,12.));
#60512=CARTESIAN_POINT('Ctrl Pts',(51.5418573141494,-49.6287108809975,12.));
#60513=CARTESIAN_POINT('Ctrl Pts',(51.5208862126303,-49.6189509577441,12.));
#60514=CARTESIAN_POINT('Ctrl Pts',(51.4999651347496,-49.609188965684,12.));
#60515=CARTESIAN_POINT('Ctrl Pts',(51.4790941716859,-49.5994250204003,12.));
#60516=CARTESIAN_POINT('Ctrl Pts',(51.4582734149562,-49.5896592380634,12.));
#60517=CARTESIAN_POINT('Ctrl Pts',(51.4375029564191,-49.579891735436,12.));
#60518=CARTESIAN_POINT('Ctrl Pts',(51.4167828882765,-49.5701226298779,12.));
#60519=CARTESIAN_POINT('Ctrl Pts',(51.3961133030688,-49.5603520393514,12.));
#60520=CARTESIAN_POINT('Ctrl Pts',(51.3754942936796,-49.5505800824268,12.));
#60521=CARTESIAN_POINT('Ctrl Pts',(51.354925953347,-49.5408068782871,12.));
#60522=CARTESIAN_POINT('Ctrl Pts',(51.3344083756659,-49.5310325467334,12.));
#60523=CARTESIAN_POINT('Ctrl Pts',(51.3139416545903,-49.5212572081901,12.));
#60524=CARTESIAN_POINT('Ctrl Pts',(51.2935258844278,-49.5114809837111,12.));
#60525=CARTESIAN_POINT('Ctrl Pts',(51.2731611598465,-49.5017039949841,12.));
#60526=CARTESIAN_POINT('Ctrl Pts',(51.2528475758841,-49.4919263643357,12.));
#60527=CARTESIAN_POINT('Ctrl Pts',(51.2325852279507,-49.4821482147357,12.));
#60528=CARTESIAN_POINT('Ctrl Pts',(51.2123742118288,-49.4723696698022,12.));
#60529=CARTESIAN_POINT('Ctrl Pts',(51.1922146236686,-49.4625908538076,12.));
#60530=CARTESIAN_POINT('Ctrl Pts',(51.1721065599972,-49.4528118916833,12.));
#60531=CARTESIAN_POINT('Ctrl Pts',(51.1520501177291,-49.4430329090288,12.));
#60532=CARTESIAN_POINT('Ctrl Pts',(51.1320453941702,-49.4332540321178,12.));
#60533=CARTESIAN_POINT('Ctrl Pts',(51.1120924870196,-49.4234753879071,12.));
#60534=CARTESIAN_POINT('Ctrl Pts',(51.0921914943663,-49.4136971040428,12.));
#60535=CARTESIAN_POINT('Ctrl Pts',(51.0723425146987,-49.4039193088636,12.));
#60536=CARTESIAN_POINT('Ctrl Pts',(51.0525456469072,-49.3941421314014,12.));
#60537=CARTESIAN_POINT('Ctrl Pts',(51.0328009902857,-49.3843657013851,12.));
#60538=CARTESIAN_POINT('Ctrl Pts',(51.0131086445268,-49.3745901492429,12.));
#60539=CARTESIAN_POINT('Ctrl Pts',(50.9934687097179,-49.3648156061049,12.));
#60540=CARTESIAN_POINT('Ctrl Pts',(50.9738812863635,-49.3550422038221,12.));
#60541=CARTESIAN_POINT('Ctrl Pts',(50.9543464753974,-49.3452700749804,12.));
#60542=CARTESIAN_POINT('Ctrl Pts',(50.9348643781928,-49.3354993529163,12.));
#60543=CARTESIAN_POINT('Ctrl Pts',(50.9154350965681,-49.325730171735,12.));
#60544=CARTESIAN_POINT('Ctrl Pts',(50.8960587327869,-49.3159626663129,12.));
#60545=CARTESIAN_POINT('Ctrl Pts',(50.8767353895509,-49.3061969722798,12.));
#60546=CARTESIAN_POINT('Ctrl Pts',(50.8574651699877,-49.2964332260043,12.));
#60547=CARTESIAN_POINT('Ctrl Pts',(50.8382481776392,-49.2866715645828,12.));
#60548=CARTESIAN_POINT('Ctrl Pts',(50.8190845164319,-49.2769121258144,12.));
#60549=CARTESIAN_POINT('Ctrl Pts',(50.799974290711,-49.2671550482415,12.));
#60550=CARTESIAN_POINT('Ctrl Pts',(50.7809176052954,-49.2574004712122,12.));
#60551=CARTESIAN_POINT('Ctrl Pts',(50.7619145655207,-49.2476485349373,12.));
#60552=CARTESIAN_POINT('Ctrl Pts',(50.7429652772816,-49.2378993805482,12.));
#60553=CARTESIAN_POINT('Ctrl Pts',(50.7240698470698,-49.2281531501569,12.));
#60554=CARTESIAN_POINT('Ctrl Pts',(50.7052283818941,-49.218409986748,12.));
#60555=CARTESIAN_POINT('Ctrl Pts',(50.6864409891905,-49.2086700340625,12.));
#60556=CARTESIAN_POINT('Ctrl Pts',(50.6677077767427,-49.1989334364992,12.));
#60557=CARTESIAN_POINT('Ctrl Pts',(50.6490288525639,-49.1892003389743,12.));
#60558=CARTESIAN_POINT('Ctrl Pts',(50.6304043248796,-49.1794708869074,12.));
#60559=CARTESIAN_POINT('Ctrl Pts',(50.6118343023937,-49.1697452265473,12.));
#60560=CARTESIAN_POINT('Ctrl Pts',(50.593318894516,-49.1600235052613,12.));
#60561=CARTESIAN_POINT('Ctrl Pts',(50.5748582115575,-49.1503058717831,12.));
#60562=CARTESIAN_POINT('Ctrl Pts',(50.5564523650406,-49.1405924766169,12.));
#60563=CARTESIAN_POINT('Ctrl Pts',(50.5381014674822,-49.1308834717645,12.));
#60564=CARTESIAN_POINT('Ctrl Pts',(50.5198056318111,-49.1211790099817,12.));
#60565=CARTESIAN_POINT('Ctrl Pts',(50.5015649708742,-49.1114792441573,12.));
#60566=CARTESIAN_POINT('Ctrl Pts',(50.4833795969296,-49.1017843266782,12.));
#60567=CARTESIAN_POINT('Ctrl Pts',(50.465249621057,-49.0920944086973,12.));
#60568=CARTESIAN_POINT('Ctrl Pts',(50.4471751542717,-49.0824096415339,12.));
#60569=CARTESIAN_POINT('Ctrl Pts',(50.4291563088528,-49.0727301783477,12.));
#60570=CARTESIAN_POINT('Ctrl Pts',(50.4111931994264,-49.0630561755082,12.));
#60571=CARTESIAN_POINT('Ctrl Pts',(50.393285944528,-49.0533877945771,12.));
#60572=CARTESIAN_POINT('Ctrl Pts',(50.3754346667389,-49.0437252024868,12.));
#60573=CARTESIAN_POINT('Ctrl Pts',(50.3576394894136,-49.034068567401,12.));
#60574=CARTESIAN_POINT('Ctrl Pts',(50.3399005337967,-49.0244180550759,12.));
#60575=CARTESIAN_POINT('Ctrl Pts',(50.3222179165102,-49.0147738256925,12.));
#60576=CARTESIAN_POINT('Ctrl Pts',(50.3045917455383,-49.0051360288002,12.));
#60577=CARTESIAN_POINT('Ctrl Pts',(50.2870221241003,-48.9955048082028,12.));
#60578=CARTESIAN_POINT('Ctrl Pts',(50.2695091583472,-48.9858803116649,12.));
#60579=CARTESIAN_POINT('Ctrl Pts',(50.252052963548,-48.9762626987227,12.));
#60580=CARTESIAN_POINT('Ctrl Pts',(50.2346536715465,-48.9666521500969,12.));
#60581=CARTESIAN_POINT('Ctrl Pts',(50.2173114358423,-48.9570488741273,12.));
#60582=CARTESIAN_POINT('Ctrl Pts',(50.2000264157903,-48.9474530868847,12.));
#60583=CARTESIAN_POINT('Ctrl Pts',(50.1827987615659,-48.9378649933116,12.));
#60584=CARTESIAN_POINT('Ctrl Pts',(50.1656286003943,-48.9282847698237,12.));
#60585=CARTESIAN_POINT('Ctrl Pts',(50.148516018447,-48.9187125417897,12.));
#60586=CARTESIAN_POINT('Ctrl Pts',(50.1314610602286,-48.9091483817797,12.));
#60587=CARTESIAN_POINT('Ctrl Pts',(50.1178632066821,-48.9015035371772,12.));
#60588=CARTESIAN_POINT('Ctrl Pts',(50.1076907555303,-48.8957735556681,12.));
#60589=CARTESIAN_POINT('Ctrl Pts',(50.1009206494209,-48.8919551910299,12.));
#60590=CARTESIAN_POINT('Ctrl Pts',(50.0975384783634,-48.8900464144686,12.));
#60591=CARTESIAN_POINT('Ctrl Pts',(55.2174072001497,-49.5707719660643,-5.55111512312578E-16));
#60592=CARTESIAN_POINT('Ctrl Pts',(55.2174072001497,-49.5707719660643,4.));
#60593=CARTESIAN_POINT('Ctrl Pts',(55.2174072001497,-49.5707719660643,8.));
#60594=CARTESIAN_POINT('Ctrl Pts',(55.2174072001497,-49.5707719660643,12.));
#60595=CARTESIAN_POINT('Ctrl Pts',(55.2618153697169,-49.6712810246937,-5.55111512312578E-16));
#60596=CARTESIAN_POINT('Ctrl Pts',(55.2618153697169,-49.6712810246937,4.));
#60597=CARTESIAN_POINT('Ctrl Pts',(55.2618153697169,-49.6712810246937,8.));
#60598=CARTESIAN_POINT('Ctrl Pts',(55.2618153697169,-49.6712810246937,12.));
#60599=CARTESIAN_POINT('Ctrl Pts',(55.2790667815471,-49.8732090625343,-6.28195156302604E-16));
#60600=CARTESIAN_POINT('Ctrl Pts',(55.2790667815471,-49.8732090625343,4.));
#60601=CARTESIAN_POINT('Ctrl Pts',(55.2790667815471,-49.8732090625343,7.99999999999999));
#60602=CARTESIAN_POINT('Ctrl Pts',(55.2790667815471,-49.8732090625343,12.));
#60603=CARTESIAN_POINT('Ctrl Pts',(55.1854902750883,-50.0481613529515,-8.01722692509434E-16));
#60604=CARTESIAN_POINT('Ctrl Pts',(55.1854902750883,-50.0481613529515,4.));
#60605=CARTESIAN_POINT('Ctrl Pts',(55.1854902750883,-50.0481613529515,8.00000000000001));
#60606=CARTESIAN_POINT('Ctrl Pts',(55.1854902750883,-50.0481613529515,12.));
#60607=CARTESIAN_POINT('Ctrl Pts',(55.1300595714122,-50.1091461876223,-8.85376672737052E-16));
#60608=CARTESIAN_POINT('Ctrl Pts',(55.1300595714122,-50.1091461876223,4.));
#60609=CARTESIAN_POINT('Ctrl Pts',(55.1300595714122,-50.1091461876224,8.));
#60610=CARTESIAN_POINT('Ctrl Pts',(55.1300595714122,-50.1091461876224,12.));
#60611=CARTESIAN_POINT('',(55.2174072001497,-49.5707719660643,0.));
#60612=CARTESIAN_POINT('',(55.1300595714124,-50.1091461876225,0.));
#60613=CARTESIAN_POINT('Ctrl Pts',(55.2174072001497,-49.5707719660643,-4.91496295208056E-16));
#60614=CARTESIAN_POINT('Ctrl Pts',(55.2618153697169,-49.6712810246937,-4.91496295208056E-16));
#60615=CARTESIAN_POINT('Ctrl Pts',(55.2716733193341,-49.7866684748883,-5.3325837748807E-16));
#60616=CARTESIAN_POINT('Ctrl Pts',(55.2453425609387,-49.893247517761,-6.07818465389898E-16));
#60617=CARTESIAN_POINT('Ctrl Pts',(55.2255944921421,-49.9731817999155,-6.6373853131627E-16));
#60618=CARTESIAN_POINT('Ctrl Pts',(55.1854902750883,-50.0481613529515,-7.38107475404911E-16));
#60619=CARTESIAN_POINT('Ctrl Pts',(55.1300595714122,-50.1091461876223,-8.21761455632529E-16));
#60620=CARTESIAN_POINT('',(55.1300595714124,-50.1091461876225,12.));
#60621=CARTESIAN_POINT('Ctrl Pts',(55.1300595714122,-50.1091461876223,-8.85376672737052E-16));
#60622=CARTESIAN_POINT('Ctrl Pts',(55.1300595714122,-50.1091461876223,4.));
#60623=CARTESIAN_POINT('Ctrl Pts',(55.1300595714122,-50.1091461876224,8.));
#60624=CARTESIAN_POINT('Ctrl Pts',(55.1300595714122,-50.1091461876224,12.));
#60625=CARTESIAN_POINT('',(55.2174072001497,-49.5707719660643,12.));
#60626=CARTESIAN_POINT('Ctrl Pts',(55.1300595714122,-50.1091461876224,12.));
#60627=CARTESIAN_POINT('Ctrl Pts',(55.1854902750883,-50.0481613529515,12.));
#60628=CARTESIAN_POINT('Ctrl Pts',(55.2255944921421,-49.9731817999156,12.));
#60629=CARTESIAN_POINT('Ctrl Pts',(55.2453425609387,-49.893247517761,12.));
#60630=CARTESIAN_POINT('Ctrl Pts',(55.2716733193342,-49.7866684748883,12.));
#60631=CARTESIAN_POINT('Ctrl Pts',(55.2618153697169,-49.6712810246937,12.));
#60632=CARTESIAN_POINT('Ctrl Pts',(55.2174072001497,-49.5707719660643,12.));
#60633=CARTESIAN_POINT('Ctrl Pts',(55.2174072001497,-49.5707719660643,12.));
#60634=CARTESIAN_POINT('Ctrl Pts',(55.2174072001497,-49.5707719660643,8.));
#60635=CARTESIAN_POINT('Ctrl Pts',(55.2174072001497,-49.5707719660643,4.));
#60636=CARTESIAN_POINT('Ctrl Pts',(55.2174072001497,-49.5707719660643,-5.55111512312578E-16));
#60637=CARTESIAN_POINT('Origin',(2.7643087079898E-10,-2.53167595884892E-10,
0.));
#60638=CARTESIAN_POINT('Origin',(2.7643087079898E-10,-2.53167595884892E-10,
12.));
#60639=CARTESIAN_POINT('Origin',(2.7643087079898E-10,-2.53167595884892E-10,
0.));
#60640=CARTESIAN_POINT('Ctrl Pts',(50.1091461876248,-55.1300595714103,-5.55111512312578E-16));
#60641=CARTESIAN_POINT('Ctrl Pts',(50.1091461876248,-55.1300595714103,4.));
#60642=CARTESIAN_POINT('Ctrl Pts',(50.1091461876248,-55.1300595714103,8.));
#60643=CARTESIAN_POINT('Ctrl Pts',(50.1091461876248,-55.1300595714103,12.));
#60644=CARTESIAN_POINT('Ctrl Pts',(50.0278330747241,-55.2039671763175,-5.55111512312578E-16));
#60645=CARTESIAN_POINT('Ctrl Pts',(50.0278330747241,-55.2039671763175,4.));
#60646=CARTESIAN_POINT('Ctrl Pts',(50.0278330747241,-55.2039671763174,8.00000000000001));
#60647=CARTESIAN_POINT('Ctrl Pts',(50.0278330747241,-55.2039671763174,12.));
#60648=CARTESIAN_POINT('Ctrl Pts',(49.8417173275618,-55.2841761056302,-6.28195156314307E-16));
#60649=CARTESIAN_POINT('Ctrl Pts',(49.8417173275618,-55.2841761056302,4.00000000000001));
#60650=CARTESIAN_POINT('Ctrl Pts',(49.8417173275618,-55.2841761056302,7.99999999999999));
#60651=CARTESIAN_POINT('Ctrl Pts',(49.8417173275618,-55.2841761056302,12.));
#60652=CARTESIAN_POINT('Ctrl Pts',(49.6461537600011,-55.2507133273144,-8.01722692544929E-16));
#60653=CARTESIAN_POINT('Ctrl Pts',(49.6461537600011,-55.2507133273144,4.));
#60654=CARTESIAN_POINT('Ctrl Pts',(49.6461537600011,-55.2507133273144,8.00000000000001));
#60655=CARTESIAN_POINT('Ctrl Pts',(49.6461537600011,-55.2507133273144,12.));
#60656=CARTESIAN_POINT('Ctrl Pts',(49.5707719660263,-55.2174072001298,-8.85376672782319E-16));
#60657=CARTESIAN_POINT('Ctrl Pts',(49.5707719660263,-55.2174072001298,4.));
#60658=CARTESIAN_POINT('Ctrl Pts',(49.5707719660263,-55.2174072001297,8.));
#60659=CARTESIAN_POINT('Ctrl Pts',(49.5707719660263,-55.2174072001297,12.));
#60660=CARTESIAN_POINT('',(50.1091461876248,-55.1300595714103,0.));
#60661=CARTESIAN_POINT('',(49.5707719660262,-55.21740720013,0.));
#60662=CARTESIAN_POINT('Ctrl Pts',(50.1091461876248,-55.1300595714103,-5.27668960562141E-16));
#60663=CARTESIAN_POINT('Ctrl Pts',(50.0278330747241,-55.2039671763175,-5.27668960562141E-16));
#60664=CARTESIAN_POINT('Ctrl Pts',(49.9214812192028,-55.2498008502104,-5.69431042848843E-16));
#60665=CARTESIAN_POINT('Ctrl Pts',(49.8120443611024,-55.2585172318166,-6.43991130761306E-16));
#60666=CARTESIAN_POINT('Ctrl Pts',(49.7299667175271,-55.2650545180212,-6.99911196695654E-16));
#60667=CARTESIAN_POINT('Ctrl Pts',(49.6461537600011,-55.2507133273144,-7.74280140794491E-16));
#60668=CARTESIAN_POINT('Ctrl Pts',(49.5707719660263,-55.2174072001298,-8.57934121031881E-16));
#60669=CARTESIAN_POINT('',(49.5707719660262,-55.21740720013,12.));
#60670=CARTESIAN_POINT('Ctrl Pts',(49.5707719660263,-55.2174072001298,-8.85376672782319E-16));
#60671=CARTESIAN_POINT('Ctrl Pts',(49.5707719660263,-55.2174072001298,4.));
#60672=CARTESIAN_POINT('Ctrl Pts',(49.5707719660263,-55.2174072001297,8.));
#60673=CARTESIAN_POINT('Ctrl Pts',(49.5707719660263,-55.2174072001297,12.));
#60674=CARTESIAN_POINT('',(50.1091461876248,-55.1300595714103,12.));
#60675=CARTESIAN_POINT('Ctrl Pts',(49.5707719660263,-55.2174072001297,12.));
#60676=CARTESIAN_POINT('Ctrl Pts',(49.6461537600011,-55.2507133273144,12.));
#60677=CARTESIAN_POINT('Ctrl Pts',(49.7299667175271,-55.2650545180211,12.));
#60678=CARTESIAN_POINT('Ctrl Pts',(49.8120443611024,-55.2585172318165,12.));
#60679=CARTESIAN_POINT('Ctrl Pts',(49.9214812192028,-55.2498008502104,12.));
#60680=CARTESIAN_POINT('Ctrl Pts',(50.0278330747241,-55.2039671763174,12.));
#60681=CARTESIAN_POINT('Ctrl Pts',(50.1091461876248,-55.1300595714103,12.));
#60682=CARTESIAN_POINT('Ctrl Pts',(50.1091461876248,-55.1300595714103,12.));
#60683=CARTESIAN_POINT('Ctrl Pts',(50.1091461876248,-55.1300595714103,8.));
#60684=CARTESIAN_POINT('Ctrl Pts',(50.1091461876248,-55.1300595714103,4.));
#60685=CARTESIAN_POINT('Ctrl Pts',(50.1091461876248,-55.1300595714103,-5.55111512312578E-16));
#60686=CARTESIAN_POINT('Ctrl Pts',(45.6458539113724,-53.0702932034641,0.));
#60687=CARTESIAN_POINT('Ctrl Pts',(45.6458539113724,-53.0702932034641,12.));
#60688=CARTESIAN_POINT('Ctrl Pts',(45.6490568514089,-53.0724894921849,0.));
#60689=CARTESIAN_POINT('Ctrl Pts',(45.6490568514089,-53.0724894921849,12.));
#60690=CARTESIAN_POINT('Ctrl Pts',(45.6554684028145,-53.0768833804193,0.));
#60691=CARTESIAN_POINT('Ctrl Pts',(45.6554684028145,-53.0768833804193,12.));
#60692=CARTESIAN_POINT('Ctrl Pts',(45.6651027439241,-53.0834781451546,0.));
#60693=CARTESIAN_POINT('Ctrl Pts',(45.6651027439241,-53.0834781451546,12.));
#60694=CARTESIAN_POINT('Ctrl Pts',(45.6779825614231,-53.0922790298409,0.));
#60695=CARTESIAN_POINT('Ctrl Pts',(45.6779825614231,-53.0922790298409,12.));
#60696=CARTESIAN_POINT('Ctrl Pts',(45.694139048907,-53.1032932328857,0.));
#60697=CARTESIAN_POINT('Ctrl Pts',(45.694139048907,-53.1032932328857,12.));
#60698=CARTESIAN_POINT('Ctrl Pts',(45.7103522376696,-53.114320495492,0.));
#60699=CARTESIAN_POINT('Ctrl Pts',(45.7103522376696,-53.114320495492,12.));
#60700=CARTESIAN_POINT('Ctrl Pts',(45.7266220897003,-53.1253607414872,0.));
#60701=CARTESIAN_POINT('Ctrl Pts',(45.7266220897003,-53.1253607414872,12.));
#60702=CARTESIAN_POINT('Ctrl Pts',(45.7429485300823,-53.1364138384693,0.));
#60703=CARTESIAN_POINT('Ctrl Pts',(45.7429485300823,-53.1364138384693,12.));
#60704=CARTESIAN_POINT('Ctrl Pts',(45.7593314474501,-53.1474795996053,0.));
#60705=CARTESIAN_POINT('Ctrl Pts',(45.7593314474501,-53.1474795996053,12.));
#60706=CARTESIAN_POINT('Ctrl Pts',(45.7757707100618,-53.1585578076444,0.));
#60707=CARTESIAN_POINT('Ctrl Pts',(45.7757707100618,-53.1585578076444,12.));
#60708=CARTESIAN_POINT('Ctrl Pts',(45.7922661780005,-53.1696482334487,0.));
#60709=CARTESIAN_POINT('Ctrl Pts',(45.7922661780005,-53.1696482334487,12.));
#60710=CARTESIAN_POINT('Ctrl Pts',(45.8088177165089,-53.1807506560933,0.));
#60711=CARTESIAN_POINT('Ctrl Pts',(45.8088177165089,-53.1807506560933,12.));
#60712=CARTESIAN_POINT('Ctrl Pts',(45.8254252099957,-53.1918648840541,0.));
#60713=CARTESIAN_POINT('Ctrl Pts',(45.8254252099957,-53.1918648840541,12.));
#60714=CARTESIAN_POINT('Ctrl Pts',(45.8420885575349,-53.2029907483557,0.));
#60715=CARTESIAN_POINT('Ctrl Pts',(45.8420885575349,-53.2029907483557,12.));
#60716=CARTESIAN_POINT('Ctrl Pts',(45.8588076662582,-53.2141280925439,0.));
#60717=CARTESIAN_POINT('Ctrl Pts',(45.8588076662582,-53.2141280925439,12.));
#60718=CARTESIAN_POINT('Ctrl Pts',(45.8755824458722,-53.2252767643662,0.));
#60719=CARTESIAN_POINT('Ctrl Pts',(45.8755824458722,-53.2252767643662,12.));
#60720=CARTESIAN_POINT('Ctrl Pts',(45.8924128018379,-53.2364366054306,0.));
#60721=CARTESIAN_POINT('Ctrl Pts',(45.8924128018379,-53.2364366054306,12.));
#60722=CARTESIAN_POINT('Ctrl Pts',(45.9092986319377,-53.2476074460017,0.));
#60723=CARTESIAN_POINT('Ctrl Pts',(45.9092986319377,-53.2476074460017,12.));
#60724=CARTESIAN_POINT('Ctrl Pts',(45.9262398298349,-53.2587891103866,0.));
#60725=CARTESIAN_POINT('Ctrl Pts',(45.9262398298349,-53.2587891103866,12.));
#60726=CARTESIAN_POINT('Ctrl Pts',(45.9432362873008,-53.2699814203105,0.));
#60727=CARTESIAN_POINT('Ctrl Pts',(45.9432362873008,-53.2699814203105,12.));
#60728=CARTESIAN_POINT('Ctrl Pts',(45.9602878967698,-53.2811841987926,0.));
#60729=CARTESIAN_POINT('Ctrl Pts',(45.9602878967698,-53.2811841987926,12.));
#60730=CARTESIAN_POINT('Ctrl Pts',(45.9773945542384,-53.292397274555,0.));
#60731=CARTESIAN_POINT('Ctrl Pts',(45.9773945542384,-53.292397274555,12.));
#60732=CARTESIAN_POINT('Ctrl Pts',(45.9945561591453,-53.3036204818329,0.));
#60733=CARTESIAN_POINT('Ctrl Pts',(45.9945561591453,-53.3036204818329,12.));
#60734=CARTESIAN_POINT('Ctrl Pts',(46.0117726129873,-53.3148536582635,0.));
#60735=CARTESIAN_POINT('Ctrl Pts',(46.0117726129873,-53.3148536582635,12.));
#60736=CARTESIAN_POINT('Ctrl Pts',(46.02904381836,-53.326096643428,0.));
#60737=CARTESIAN_POINT('Ctrl Pts',(46.02904381836,-53.326096643428,12.));
#60738=CARTESIAN_POINT('Ctrl Pts',(46.0463696777801,-53.3373492770671,0.));
#60739=CARTESIAN_POINT('Ctrl Pts',(46.0463696777801,-53.3373492770671,12.));
#60740=CARTESIAN_POINT('Ctrl Pts',(46.0637500926982,-53.3486113975901,0.));
#60741=CARTESIAN_POINT('Ctrl Pts',(46.0637500926982,-53.3486113975901,12.));
#60742=CARTESIAN_POINT('Ctrl Pts',(46.0811849640218,-53.3598828428546,0.));
#60743=CARTESIAN_POINT('Ctrl Pts',(46.0811849640218,-53.3598828428546,12.));
#60744=CARTESIAN_POINT('Ctrl Pts',(46.0986741925656,-53.3711634508437,0.));
#60745=CARTESIAN_POINT('Ctrl Pts',(46.0986741925656,-53.3711634508437,12.));
#60746=CARTESIAN_POINT('Ctrl Pts',(46.1162176794884,-53.3824530603276,0.));
#60747=CARTESIAN_POINT('Ctrl Pts',(46.1162176794884,-53.3824530603276,12.));
#60748=CARTESIAN_POINT('Ctrl Pts',(46.1338153268097,-53.3937515116549,0.));
#60749=CARTESIAN_POINT('Ctrl Pts',(46.1338153268097,-53.3937515116549,12.));
#60750=CARTESIAN_POINT('Ctrl Pts',(46.1514670376012,-53.4050586470436,0.));
#60751=CARTESIAN_POINT('Ctrl Pts',(46.1514670376012,-53.4050586470436,12.));
#60752=CARTESIAN_POINT('Ctrl Pts',(46.1691727157134,-53.4163743101517,0.));
#60753=CARTESIAN_POINT('Ctrl Pts',(46.1691727157134,-53.4163743101517,12.));
#60754=CARTESIAN_POINT('Ctrl Pts',(46.1869322656023,-53.4276983458125,0.));
#60755=CARTESIAN_POINT('Ctrl Pts',(46.1869322656023,-53.4276983458125,12.));
#60756=CARTESIAN_POINT('Ctrl Pts',(46.2047455921286,-53.4390305997274,0.));
#60757=CARTESIAN_POINT('Ctrl Pts',(46.2047455921286,-53.4390305997274,12.));
#60758=CARTESIAN_POINT('Ctrl Pts',(46.2226126003202,-53.4503709181178,0.));
#60759=CARTESIAN_POINT('Ctrl Pts',(46.2226126003202,-53.4503709181178,12.));
#60760=CARTESIAN_POINT('Ctrl Pts',(46.2405331953889,-53.4617191477402,0.));
#60761=CARTESIAN_POINT('Ctrl Pts',(46.2405331953889,-53.4617191477402,12.));
#60762=CARTESIAN_POINT('Ctrl Pts',(46.2585072828353,-53.4730751360371,0.));
#60763=CARTESIAN_POINT('Ctrl Pts',(46.2585072828353,-53.4730751360371,12.));
#60764=CARTESIAN_POINT('Ctrl Pts',(46.2765347685198,-53.4844387312414,0.));
#60765=CARTESIAN_POINT('Ctrl Pts',(46.2765347685198,-53.4844387312414,12.));
#60766=CARTESIAN_POINT('Ctrl Pts',(46.2946155587417,-53.4958097825006,0.));
#60767=CARTESIAN_POINT('Ctrl Pts',(46.2946155587417,-53.4958097825006,12.));
#60768=CARTESIAN_POINT('Ctrl Pts',(46.3127495603098,-53.5071881399911,0.));
#60769=CARTESIAN_POINT('Ctrl Pts',(46.3127495603098,-53.5071881399911,12.));
#60770=CARTESIAN_POINT('Ctrl Pts',(46.3309366805093,-53.5185736548548,0.));
#60771=CARTESIAN_POINT('Ctrl Pts',(46.3309366805093,-53.5185736548548,12.));
#60772=CARTESIAN_POINT('Ctrl Pts',(46.3491768270655,-53.5299661791385,0.));
#60773=CARTESIAN_POINT('Ctrl Pts',(46.3491768270655,-53.5299661791385,12.));
#60774=CARTESIAN_POINT('Ctrl Pts',(46.3674699081046,-53.5413655657327,0.));
#60775=CARTESIAN_POINT('Ctrl Pts',(46.3674699081046,-53.5413655657327,12.));
#60776=CARTESIAN_POINT('Ctrl Pts',(46.3858158321059,-53.5527716683048,0.));
#60777=CARTESIAN_POINT('Ctrl Pts',(46.3858158321059,-53.5527716683048,12.));
#60778=CARTESIAN_POINT('Ctrl Pts',(46.4042145078701,-53.5641843412559,0.));
#60779=CARTESIAN_POINT('Ctrl Pts',(46.4042145078701,-53.5641843412559,12.));
#60780=CARTESIAN_POINT('Ctrl Pts',(46.4226658445474,-53.5756034397481,0.));
#60781=CARTESIAN_POINT('Ctrl Pts',(46.4226658445474,-53.5756034397481,12.));
#60782=CARTESIAN_POINT('Ctrl Pts',(46.4411697516478,-53.5870288197166,0.));
#60783=CARTESIAN_POINT('Ctrl Pts',(46.4411697516478,-53.5870288197166,12.));
#60784=CARTESIAN_POINT('Ctrl Pts',(46.459726139052,-53.5984603378855,0.));
#60785=CARTESIAN_POINT('Ctrl Pts',(46.459726139052,-53.5984603378855,12.));
#60786=CARTESIAN_POINT('Ctrl Pts',(46.4783349170173,-53.6098978517859,0.));
#60787=CARTESIAN_POINT('Ctrl Pts',(46.4783349170173,-53.6098978517859,12.));
#60788=CARTESIAN_POINT('Ctrl Pts',(46.496995996177,-53.6213412197533,0.));
#60789=CARTESIAN_POINT('Ctrl Pts',(46.496995996177,-53.6213412197533,12.));
#60790=CARTESIAN_POINT('Ctrl Pts',(46.5157092875373,-53.6327903009094,0.));
#60791=CARTESIAN_POINT('Ctrl Pts',(46.5157092875373,-53.6327903009094,12.));
#60792=CARTESIAN_POINT('Ctrl Pts',(46.5344747024676,-53.6442449551455,0.));
#60793=CARTESIAN_POINT('Ctrl Pts',(46.5344747024676,-53.6442449551455,12.));
#60794=CARTESIAN_POINT('Ctrl Pts',(46.5532921526901,-53.6557050431071,0.));
#60795=CARTESIAN_POINT('Ctrl Pts',(46.5532921526901,-53.6557050431071,12.));
#60796=CARTESIAN_POINT('Ctrl Pts',(46.5721615502591,-53.6671704261737,0.));
#60797=CARTESIAN_POINT('Ctrl Pts',(46.5721615502591,-53.6671704261737,12.));
#60798=CARTESIAN_POINT('Ctrl Pts',(46.5910828075653,-53.678640966456,0.));
#60799=CARTESIAN_POINT('Ctrl Pts',(46.5910828075653,-53.678640966456,12.));
#60800=CARTESIAN_POINT('Ctrl Pts',(46.6100558373402,-53.6901165267941,0.));
#60801=CARTESIAN_POINT('Ctrl Pts',(46.6100558373402,-53.6901165267941,12.));
#60802=CARTESIAN_POINT('Ctrl Pts',(46.6290805526559,-53.701596970754,0.));
#60803=CARTESIAN_POINT('Ctrl Pts',(46.6290805526559,-53.701596970754,12.));
#60804=CARTESIAN_POINT('Ctrl Pts',(46.6481568669216,-53.7130821626263,0.));
#60805=CARTESIAN_POINT('Ctrl Pts',(46.6481568669216,-53.7130821626263,12.));
#60806=CARTESIAN_POINT('Ctrl Pts',(46.6672846938752,-53.7245719674222,0.));
#60807=CARTESIAN_POINT('Ctrl Pts',(46.6672846938752,-53.7245719674222,12.));
#60808=CARTESIAN_POINT('Ctrl Pts',(46.6864639475863,-53.7360662508677,0.));
#60809=CARTESIAN_POINT('Ctrl Pts',(46.6864639475863,-53.7360662508677,12.));
#60810=CARTESIAN_POINT('Ctrl Pts',(46.7056945424559,-53.7475648793948,0.));
#60811=CARTESIAN_POINT('Ctrl Pts',(46.7056945424559,-53.7475648793948,12.));
#60812=CARTESIAN_POINT('Ctrl Pts',(46.724976393213,-53.7590677201344,0.));
#60813=CARTESIAN_POINT('Ctrl Pts',(46.724976393213,-53.7590677201344,12.));
#60814=CARTESIAN_POINT('Ctrl Pts',(46.7443094149041,-53.770574640907,0.));
#60815=CARTESIAN_POINT('Ctrl Pts',(46.7443094149041,-53.770574640907,12.));
#60816=CARTESIAN_POINT('Ctrl Pts',(46.7636935228851,-53.782085510217,0.));
#60817=CARTESIAN_POINT('Ctrl Pts',(46.7636935228851,-53.782085510217,12.));
#60818=CARTESIAN_POINT('Ctrl Pts',(46.7831286328268,-53.7936001972468,0.));
#60819=CARTESIAN_POINT('Ctrl Pts',(46.7831286328268,-53.7936001972468,12.));
#60820=CARTESIAN_POINT('Ctrl Pts',(46.8026146607144,-53.8051185718525,0.));
#60821=CARTESIAN_POINT('Ctrl Pts',(46.8026146607144,-53.8051185718525,12.));
#60822=CARTESIAN_POINT('Ctrl Pts',(46.8221515228459,-53.8166405045582,0.));
#60823=CARTESIAN_POINT('Ctrl Pts',(46.8221515228459,-53.8166405045582,12.));
#60824=CARTESIAN_POINT('Ctrl Pts',(46.8417391358231,-53.8281658665517,0.));
#60825=CARTESIAN_POINT('Ctrl Pts',(46.8417391358231,-53.8281658665517,12.));
#60826=CARTESIAN_POINT('Ctrl Pts',(46.8613774165452,-53.8396945296777,0.));
#60827=CARTESIAN_POINT('Ctrl Pts',(46.8613774165452,-53.8396945296777,12.));
#60828=CARTESIAN_POINT('Ctrl Pts',(46.8810662822146,-53.851226366434,0.));
#60829=CARTESIAN_POINT('Ctrl Pts',(46.8810662822146,-53.851226366434,12.));
#60830=CARTESIAN_POINT('Ctrl Pts',(46.900805650336,-53.8627612499648,0.));
#60831=CARTESIAN_POINT('Ctrl Pts',(46.900805650336,-53.8627612499648,12.));
#60832=CARTESIAN_POINT('Ctrl Pts',(46.9205954387128,-53.8742990540557,0.));
#60833=CARTESIAN_POINT('Ctrl Pts',(46.9205954387128,-53.8742990540557,12.));
#60834=CARTESIAN_POINT('Ctrl Pts',(46.9404355654381,-53.8858396531277,0.));
#60835=CARTESIAN_POINT('Ctrl Pts',(46.9404355654381,-53.8858396531277,12.));
#60836=CARTESIAN_POINT('Ctrl Pts',(46.9603259488894,-53.8973829222317,0.));
#60837=CARTESIAN_POINT('Ctrl Pts',(46.9603259488894,-53.8973829222317,12.));
#60838=CARTESIAN_POINT('Ctrl Pts',(46.9802665077342,-53.9089287370436,0.));
#60839=CARTESIAN_POINT('Ctrl Pts',(46.9802665077342,-53.9089287370436,12.));
#60840=CARTESIAN_POINT('Ctrl Pts',(47.0002571609286,-53.9204769738584,0.));
#60841=CARTESIAN_POINT('Ctrl Pts',(47.0002571609286,-53.9204769738584,12.));
#60842=CARTESIAN_POINT('Ctrl Pts',(47.0202978277148,-53.9320275095864,0.));
#60843=CARTESIAN_POINT('Ctrl Pts',(47.0202978277148,-53.9320275095864,12.));
#60844=CARTESIAN_POINT('Ctrl Pts',(47.04038842761,-53.9435802217468,0.));
#60845=CARTESIAN_POINT('Ctrl Pts',(47.04038842761,-53.9435802217468,12.));
#60846=CARTESIAN_POINT('Ctrl Pts',(47.0605288804042,-53.9551349884637,0.));
#60847=CARTESIAN_POINT('Ctrl Pts',(47.0605288804042,-53.9551349884637,12.));
#60848=CARTESIAN_POINT('Ctrl Pts',(47.0807191061673,-53.9666916884624,0.));
#60849=CARTESIAN_POINT('Ctrl Pts',(47.0807191061673,-53.9666916884624,12.));
#60850=CARTESIAN_POINT('Ctrl Pts',(47.1009590252466,-53.9782502010642,0.));
#60851=CARTESIAN_POINT('Ctrl Pts',(47.1009590252466,-53.9782502010642,12.));
#60852=CARTESIAN_POINT('Ctrl Pts',(47.1212485582632,-53.9898104061809,0.));
#60853=CARTESIAN_POINT('Ctrl Pts',(47.1212485582632,-53.9898104061809,12.));
#60854=CARTESIAN_POINT('Ctrl Pts',(47.1415876261012,-54.0013721843094,0.));
#60855=CARTESIAN_POINT('Ctrl Pts',(47.1415876261012,-54.0013721843094,12.));
#60856=CARTESIAN_POINT('Ctrl Pts',(47.161976149906,-54.0129354165269,0.));
#60857=CARTESIAN_POINT('Ctrl Pts',(47.161976149906,-54.0129354165269,12.));
#60858=CARTESIAN_POINT('Ctrl Pts',(47.1824140510906,-54.0244999844872,0.));
#60859=CARTESIAN_POINT('Ctrl Pts',(47.1824140510906,-54.0244999844872,12.));
#60860=CARTESIAN_POINT('Ctrl Pts',(47.2029012513334,-54.0360657704156,0.));
#60861=CARTESIAN_POINT('Ctrl Pts',(47.2029012513334,-54.0360657704156,12.));
#60862=CARTESIAN_POINT('Ctrl Pts',(47.2234376725752,-54.047632657105,0.));
#60863=CARTESIAN_POINT('Ctrl Pts',(47.2234376725752,-54.047632657105,12.));
#60864=CARTESIAN_POINT('Ctrl Pts',(47.2440232370085,-54.0592005279108,0.));
#60865=CARTESIAN_POINT('Ctrl Pts',(47.2440232370085,-54.0592005279108,12.));
#60866=CARTESIAN_POINT('Ctrl Pts',(47.2646578670767,-54.0707692667461,0.));
#60867=CARTESIAN_POINT('Ctrl Pts',(47.2646578670767,-54.0707692667461,12.));
#60868=CARTESIAN_POINT('Ctrl Pts',(47.2853414854805,-54.082338758079,0.));
#60869=CARTESIAN_POINT('Ctrl Pts',(47.2853414854805,-54.082338758079,12.));
#60870=CARTESIAN_POINT('Ctrl Pts',(47.3060740151754,-54.0939088869271,0.));
#60871=CARTESIAN_POINT('Ctrl Pts',(47.3060740151754,-54.0939088869271,12.));
#60872=CARTESIAN_POINT('Ctrl Pts',(47.326855379369,-54.1054795388538,0.));
#60873=CARTESIAN_POINT('Ctrl Pts',(47.326855379369,-54.1054795388538,12.));
#60874=CARTESIAN_POINT('Ctrl Pts',(47.3476855015095,-54.1170505999637,0.));
#60875=CARTESIAN_POINT('Ctrl Pts',(47.3476855015095,-54.1170505999637,12.));
#60876=CARTESIAN_POINT('Ctrl Pts',(47.3685643052867,-54.1286219568981,0.));
#60877=CARTESIAN_POINT('Ctrl Pts',(47.3685643052867,-54.1286219568981,12.));
#60878=CARTESIAN_POINT('Ctrl Pts',(47.3894917146361,-54.1401934968306,0.));
#60879=CARTESIAN_POINT('Ctrl Pts',(47.3894917146361,-54.1401934968306,12.));
#60880=CARTESIAN_POINT('Ctrl Pts',(47.4104676537381,-54.1517651074638,0.));
#60881=CARTESIAN_POINT('Ctrl Pts',(47.4104676537381,-54.1517651074638,12.));
#60882=CARTESIAN_POINT('Ctrl Pts',(47.4314920470142,-54.163336677024,0.));
#60883=CARTESIAN_POINT('Ctrl Pts',(47.4314920470142,-54.163336677024,12.));
#60884=CARTESIAN_POINT('Ctrl Pts',(47.4525648191173,-54.1749080942593,0.));
#60885=CARTESIAN_POINT('Ctrl Pts',(47.4525648191173,-54.1749080942593,12.));
#60886=CARTESIAN_POINT('Ctrl Pts',(47.473685894932,-54.1864792484343,0.));
#60887=CARTESIAN_POINT('Ctrl Pts',(47.473685894932,-54.1864792484343,12.));
#60888=CARTESIAN_POINT('Ctrl Pts',(47.4948551995798,-54.1980500293267,0.));
#60889=CARTESIAN_POINT('Ctrl Pts',(47.4948551995798,-54.1980500293267,12.));
#60890=CARTESIAN_POINT('Ctrl Pts',(47.5160726584172,-54.2096203272228,0.));
#60891=CARTESIAN_POINT('Ctrl Pts',(47.5160726584172,-54.2096203272228,12.));
#60892=CARTESIAN_POINT('Ctrl Pts',(47.5373381970328,-54.2211900329141,0.));
#60893=CARTESIAN_POINT('Ctrl Pts',(47.5373381970328,-54.2211900329141,12.));
#60894=CARTESIAN_POINT('Ctrl Pts',(47.5586517412368,-54.232759037693,0.));
#60895=CARTESIAN_POINT('Ctrl Pts',(47.5586517412368,-54.232759037693,12.));
#60896=CARTESIAN_POINT('Ctrl Pts',(47.5800132170614,-54.2443272333498,0.));
#60897=CARTESIAN_POINT('Ctrl Pts',(47.5800132170614,-54.2443272333498,12.));
#60898=CARTESIAN_POINT('Ctrl Pts',(47.6014225507663,-54.2558945121684,0.));
#60899=CARTESIAN_POINT('Ctrl Pts',(47.6014225507663,-54.2558945121684,12.));
#60900=CARTESIAN_POINT('Ctrl Pts',(47.6228796688376,-54.2674607669228,0.));
#60901=CARTESIAN_POINT('Ctrl Pts',(47.6228796688376,-54.2674607669228,12.));
#60902=CARTESIAN_POINT('Ctrl Pts',(47.6443844979846,-54.2790258908736,0.));
#60903=CARTESIAN_POINT('Ctrl Pts',(47.6443844979846,-54.2790258908736,12.));
#60904=CARTESIAN_POINT('Ctrl Pts',(47.6659369651299,-54.2905897777647,0.));
#60905=CARTESIAN_POINT('Ctrl Pts',(47.6659369651299,-54.2905897777647,12.));
#60906=CARTESIAN_POINT('Ctrl Pts',(47.6875369974086,-54.3021523218188,0.));
#60907=CARTESIAN_POINT('Ctrl Pts',(47.6875369974086,-54.3021523218188,12.));
#60908=CARTESIAN_POINT('Ctrl Pts',(47.7091845221747,-54.3137134177345,0.));
#60909=CARTESIAN_POINT('Ctrl Pts',(47.7091845221747,-54.3137134177345,12.));
#60910=CARTESIAN_POINT('Ctrl Pts',(47.7308794669994,-54.3252729606824,0.));
#60911=CARTESIAN_POINT('Ctrl Pts',(47.7308794669994,-54.3252729606824,12.));
#60912=CARTESIAN_POINT('Ctrl Pts',(47.7526217596694,-54.3368308463023,0.));
#60913=CARTESIAN_POINT('Ctrl Pts',(47.7526217596694,-54.3368308463023,12.));
#60914=CARTESIAN_POINT('Ctrl Pts',(47.7744113281767,-54.3483869706998,0.));
#60915=CARTESIAN_POINT('Ctrl Pts',(47.7744113281767,-54.3483869706998,12.));
#60916=CARTESIAN_POINT('Ctrl Pts',(47.7962481007179,-54.3599412304431,0.));
#60917=CARTESIAN_POINT('Ctrl Pts',(47.7962481007179,-54.3599412304431,12.));
#60918=CARTESIAN_POINT('Ctrl Pts',(47.8181320056988,-54.3714935225585,0.));
#60919=CARTESIAN_POINT('Ctrl Pts',(47.8181320056988,-54.3714935225585,12.));
#60920=CARTESIAN_POINT('Ctrl Pts',(47.8400629717352,-54.3830437445275,0.));
#60921=CARTESIAN_POINT('Ctrl Pts',(47.8400629717352,-54.3830437445275,12.));
#60922=CARTESIAN_POINT('Ctrl Pts',(47.8620409276495,-54.3945917942835,0.));
#60923=CARTESIAN_POINT('Ctrl Pts',(47.8620409276495,-54.3945917942835,12.));
#60924=CARTESIAN_POINT('Ctrl Pts',(47.8840658024626,-54.4061375702088,0.));
#60925=CARTESIAN_POINT('Ctrl Pts',(47.8840658024626,-54.4061375702088,12.));
#60926=CARTESIAN_POINT('Ctrl Pts',(47.9061375253909,-54.4176809711324,0.));
#60927=CARTESIAN_POINT('Ctrl Pts',(47.9061375253909,-54.4176809711324,12.));
#60928=CARTESIAN_POINT('Ctrl Pts',(47.9282560258528,-54.4292218963253,0.));
#60929=CARTESIAN_POINT('Ctrl Pts',(47.9282560258528,-54.4292218963253,12.));
#60930=CARTESIAN_POINT('Ctrl Pts',(47.9504212334681,-54.4407602454974,0.));
#60931=CARTESIAN_POINT('Ctrl Pts',(47.9504212334681,-54.4407602454974,12.));
#60932=CARTESIAN_POINT('Ctrl Pts',(47.972633078057,-54.4522959187952,0.));
#60933=CARTESIAN_POINT('Ctrl Pts',(47.972633078057,-54.4522959187952,12.));
#60934=CARTESIAN_POINT('Ctrl Pts',(47.9948914896316,-54.4638288167991,0.));
#60935=CARTESIAN_POINT('Ctrl Pts',(47.9948914896316,-54.4638288167991,12.));
#60936=CARTESIAN_POINT('Ctrl Pts',(48.0171963983912,-54.4753588405202,0.));
#60937=CARTESIAN_POINT('Ctrl Pts',(48.0171963983912,-54.4753588405202,12.));
#60938=CARTESIAN_POINT('Ctrl Pts',(48.039547734729,-54.4868858913961,0.));
#60939=CARTESIAN_POINT('Ctrl Pts',(48.039547734729,-54.4868858913961,12.));
#60940=CARTESIAN_POINT('Ctrl Pts',(48.0619454292321,-54.4984098712883,0.));
#60941=CARTESIAN_POINT('Ctrl Pts',(48.0619454292321,-54.4984098712883,12.));
#60942=CARTESIAN_POINT('Ctrl Pts',(48.0843894126807,-54.5099306824788,0.));
#60943=CARTESIAN_POINT('Ctrl Pts',(48.0843894126807,-54.5099306824788,12.));
#60944=CARTESIAN_POINT('Ctrl Pts',(48.1068796160406,-54.5214482276679,0.));
#60945=CARTESIAN_POINT('Ctrl Pts',(48.1068796160406,-54.5214482276679,12.));
#60946=CARTESIAN_POINT('Ctrl Pts',(48.1294159704571,-54.5329624099719,0.));
#60947=CARTESIAN_POINT('Ctrl Pts',(48.1294159704571,-54.5329624099719,12.));
#60948=CARTESIAN_POINT('Ctrl Pts',(48.1519984072617,-54.5444731329196,0.));
#60949=CARTESIAN_POINT('Ctrl Pts',(48.1519984072617,-54.5444731329196,12.));
#60950=CARTESIAN_POINT('Ctrl Pts',(48.1746268579732,-54.5559803004487,0.));
#60951=CARTESIAN_POINT('Ctrl Pts',(48.1746268579732,-54.5559803004487,12.));
#60952=CARTESIAN_POINT('Ctrl Pts',(48.1973012542966,-54.5674838169041,0.));
#60953=CARTESIAN_POINT('Ctrl Pts',(48.1973012542966,-54.5674838169041,12.));
#60954=CARTESIAN_POINT('Ctrl Pts',(48.2200215281178,-54.5789835870348,0.));
#60955=CARTESIAN_POINT('Ctrl Pts',(48.2200215281178,-54.5789835870348,12.));
#60956=CARTESIAN_POINT('Ctrl Pts',(48.2427876114955,-54.5904795159936,0.));
#60957=CARTESIAN_POINT('Ctrl Pts',(48.2427876114955,-54.5904795159936,12.));
#60958=CARTESIAN_POINT('Ctrl Pts',(48.2655994366672,-54.6019715093319,0.));
#60959=CARTESIAN_POINT('Ctrl Pts',(48.2655994366672,-54.6019715093319,12.));
#60960=CARTESIAN_POINT('Ctrl Pts',(48.288456936051,-54.6134594729964,0.));
#60961=CARTESIAN_POINT('Ctrl Pts',(48.288456936051,-54.6134594729964,12.));
#60962=CARTESIAN_POINT('Ctrl Pts',(48.3113600422443,-54.6249433133262,0.));
#60963=CARTESIAN_POINT('Ctrl Pts',(48.3113600422443,-54.6249433133262,12.));
#60964=CARTESIAN_POINT('Ctrl Pts',(48.3343086880192,-54.636422937049,0.));
#60965=CARTESIAN_POINT('Ctrl Pts',(48.3343086880192,-54.636422937049,12.));
#60966=CARTESIAN_POINT('Ctrl Pts',(48.3573028063121,-54.647898251279,0.));
#60967=CARTESIAN_POINT('Ctrl Pts',(48.3573028063121,-54.647898251279,12.));
#60968=CARTESIAN_POINT('Ctrl Pts',(48.3803423302294,-54.6593691635143,0.));
#60969=CARTESIAN_POINT('Ctrl Pts',(48.3803423302294,-54.6593691635143,12.));
#60970=CARTESIAN_POINT('Ctrl Pts',(48.4034271930516,-54.6708355816359,0.));
#60971=CARTESIAN_POINT('Ctrl Pts',(48.4034271930516,-54.6708355816359,12.));
#60972=CARTESIAN_POINT('Ctrl Pts',(48.4265573282341,-54.6822974139065,0.));
#60973=CARTESIAN_POINT('Ctrl Pts',(48.4265573282341,-54.6822974139065,12.));
#60974=CARTESIAN_POINT('Ctrl Pts',(48.4497326694051,-54.6937545689694,0.));
#60975=CARTESIAN_POINT('Ctrl Pts',(48.4497326694051,-54.6937545689694,12.));
#60976=CARTESIAN_POINT('Ctrl Pts',(48.4729531503565,-54.7052069558493,0.));
#60977=CARTESIAN_POINT('Ctrl Pts',(48.4729531503565,-54.7052069558493,12.));
#60978=CARTESIAN_POINT('Ctrl Pts',(48.4962187050451,-54.7166544839475,0.));
#60979=CARTESIAN_POINT('Ctrl Pts',(48.4962187050451,-54.7166544839475,12.));
#60980=CARTESIAN_POINT('Ctrl Pts',(48.5195292675955,-54.7280970630346,0.));
#60981=CARTESIAN_POINT('Ctrl Pts',(48.5195292675955,-54.7280970630346,12.));
#60982=CARTESIAN_POINT('Ctrl Pts',(48.5428847722974,-54.7395346032451,0.));
#60983=CARTESIAN_POINT('Ctrl Pts',(48.5428847722974,-54.7395346032451,12.));
#60984=CARTESIAN_POINT('Ctrl Pts',(48.5662851536027,-54.7509670150716,0.));
#60985=CARTESIAN_POINT('Ctrl Pts',(48.5662851536027,-54.7509670150716,12.));
#60986=CARTESIAN_POINT('Ctrl Pts',(48.5897303461131,-54.7623942093591,0.));
#60987=CARTESIAN_POINT('Ctrl Pts',(48.5897303461131,-54.7623942093591,12.));
#60988=CARTESIAN_POINT('Ctrl Pts',(48.6132202845792,-54.773816097304,0.));
#60989=CARTESIAN_POINT('Ctrl Pts',(48.6132202845792,-54.773816097304,12.));
#60990=CARTESIAN_POINT('Ctrl Pts',(48.6367549039121,-54.7852325904591,0.));
#60991=CARTESIAN_POINT('Ctrl Pts',(48.6367549039121,-54.7852325904591,12.));
#60992=CARTESIAN_POINT('Ctrl Pts',(48.6603341391891,-54.7966436007395,0.));
#60993=CARTESIAN_POINT('Ctrl Pts',(48.6603341391891,-54.7966436007395,12.));
#60994=CARTESIAN_POINT('Ctrl Pts',(48.6839579256565,-54.8080490404274,0.));
#60995=CARTESIAN_POINT('Ctrl Pts',(48.6839579256565,-54.8080490404274,12.));
#60996=CARTESIAN_POINT('Ctrl Pts',(48.7076261987284,-54.8194488221803,0.));
#60997=CARTESIAN_POINT('Ctrl Pts',(48.7076261987284,-54.8194488221803,12.));
#60998=CARTESIAN_POINT('Ctrl Pts',(48.7313388939834,-54.8308428590334,0.));
#60999=CARTESIAN_POINT('Ctrl Pts',(48.7313388939834,-54.8308428590334,12.));
#61000=CARTESIAN_POINT('Ctrl Pts',(48.755095947159,-54.8422310643752,0.));
#61001=CARTESIAN_POINT('Ctrl Pts',(48.755095947159,-54.8422310643752,12.));
#61002=CARTESIAN_POINT('Ctrl Pts',(48.7788972941431,-54.8536133519285,0.));
#61003=CARTESIAN_POINT('Ctrl Pts',(48.7788972941431,-54.8536133519285,12.));
#61004=CARTESIAN_POINT('Ctrl Pts',(48.8027428709613,-54.8649896357284,0.));
#61005=CARTESIAN_POINT('Ctrl Pts',(48.8027428709613,-54.8649896357284,12.));
#61006=CARTESIAN_POINT('Ctrl Pts',(48.8266326137629,-54.8763598301045,0.));
#61007=CARTESIAN_POINT('Ctrl Pts',(48.8266326137629,-54.8763598301045,12.));
#61008=CARTESIAN_POINT('Ctrl Pts',(48.8505664587984,-54.8877238496577,0.));
#61009=CARTESIAN_POINT('Ctrl Pts',(48.8505664587984,-54.8877238496577,12.));
#61010=CARTESIAN_POINT('Ctrl Pts',(48.8745443424488,-54.8990816092964,0.));
#61011=CARTESIAN_POINT('Ctrl Pts',(48.8745443424488,-54.8990816092964,12.));
#61012=CARTESIAN_POINT('Ctrl Pts',(48.8985662012535,-54.910433024275,0.));
#61013=CARTESIAN_POINT('Ctrl Pts',(48.8985662012535,-54.910433024275,12.));
#61014=CARTESIAN_POINT('Ctrl Pts',(48.922631971937,-54.9217780102357,0.));
#61015=CARTESIAN_POINT('Ctrl Pts',(48.922631971937,-54.9217780102357,12.));
#61016=CARTESIAN_POINT('Ctrl Pts',(48.9467415914266,-54.933116483242,0.));
#61017=CARTESIAN_POINT('Ctrl Pts',(48.9467415914266,-54.933116483242,12.));
#61018=CARTESIAN_POINT('Ctrl Pts',(48.9708949968789,-54.9444483598372,0.));
#61019=CARTESIAN_POINT('Ctrl Pts',(48.9708949968789,-54.9444483598372,12.));
#61020=CARTESIAN_POINT('Ctrl Pts',(48.995092125652,-54.9557735569936,0.));
#61021=CARTESIAN_POINT('Ctrl Pts',(48.995092125652,-54.9557735569936,12.));
#61022=CARTESIAN_POINT('Ctrl Pts',(49.0193329152475,-54.9670919920024,0.));
#61023=CARTESIAN_POINT('Ctrl Pts',(49.0193329152475,-54.9670919920024,12.));
#61024=CARTESIAN_POINT('Ctrl Pts',(49.0436173032527,-54.9784035823764,0.));
#61025=CARTESIAN_POINT('Ctrl Pts',(49.0436173032527,-54.9784035823764,12.));
#61026=CARTESIAN_POINT('Ctrl Pts',(49.0679452272871,-54.9897082457607,0.));
#61027=CARTESIAN_POINT('Ctrl Pts',(49.0679452272871,-54.9897082457607,12.));
#61028=CARTESIAN_POINT('Ctrl Pts',(49.0923166249222,-55.0010058998111,0.));
#61029=CARTESIAN_POINT('Ctrl Pts',(49.0923166249222,-55.0010058998111,12.));
#61030=CARTESIAN_POINT('Ctrl Pts',(49.1167314336737,-55.0122964621868,0.));
#61031=CARTESIAN_POINT('Ctrl Pts',(49.1167314336737,-55.0122964621868,12.));
#61032=CARTESIAN_POINT('Ctrl Pts',(49.1411895911645,-55.0235798508056,0.));
#61033=CARTESIAN_POINT('Ctrl Pts',(49.1411895911645,-55.0235798508056,12.));
#61034=CARTESIAN_POINT('Ctrl Pts',(49.1656910352484,-55.0348559840462,0.));
#61035=CARTESIAN_POINT('Ctrl Pts',(49.1656910352484,-55.0348559840462,12.));
#61036=CARTESIAN_POINT('Ctrl Pts',(49.1902357041462,-55.0461247809745,0.));
#61037=CARTESIAN_POINT('Ctrl Pts',(49.1902357041462,-55.0461247809745,12.));
#61038=CARTESIAN_POINT('Ctrl Pts',(49.2148235365694,-55.0573861615569,0.));
#61039=CARTESIAN_POINT('Ctrl Pts',(49.2148235365694,-55.0573861615569,12.));
#61040=CARTESIAN_POINT('Ctrl Pts',(49.2394544718512,-55.0686400468911,0.));
#61041=CARTESIAN_POINT('Ctrl Pts',(49.2394544718512,-55.0686400468911,12.));
#61042=CARTESIAN_POINT('Ctrl Pts',(49.2641284496496,-55.0798863586986,0.));
#61043=CARTESIAN_POINT('Ctrl Pts',(49.2641284496496,-55.0798863586986,12.));
#61044=CARTESIAN_POINT('Ctrl Pts',(49.2888454096544,-55.0911250188282,0.));
#61045=CARTESIAN_POINT('Ctrl Pts',(49.2888454096544,-55.0911250188282,12.));
#61046=CARTESIAN_POINT('Ctrl Pts',(49.3136052912614,-55.1023559487133,0.));
#61047=CARTESIAN_POINT('Ctrl Pts',(49.3136052912614,-55.1023559487133,12.));
#61048=CARTESIAN_POINT('Ctrl Pts',(49.3384080333166,-55.1135790689475,0.));
#61049=CARTESIAN_POINT('Ctrl Pts',(49.3384080333166,-55.1135790689475,12.));
#61050=CARTESIAN_POINT('Ctrl Pts',(49.3632535736744,-55.1247942985649,0.));
#61051=CARTESIAN_POINT('Ctrl Pts',(49.3632535736744,-55.1247942985649,12.));
#61052=CARTESIAN_POINT('Ctrl Pts',(49.3881418495529,-55.1360015556262,0.));
#61053=CARTESIAN_POINT('Ctrl Pts',(49.3881418495529,-55.1360015556262,12.));
#61054=CARTESIAN_POINT('Ctrl Pts',(49.413072798324,-55.1472007585224,0.));
#61055=CARTESIAN_POINT('Ctrl Pts',(49.413072798324,-55.1472007585224,12.));
#61056=CARTESIAN_POINT('Ctrl Pts',(49.4380463581989,-55.158391827114,0.));
#61057=CARTESIAN_POINT('Ctrl Pts',(49.4380463581989,-55.158391827114,12.));
#61058=CARTESIAN_POINT('Ctrl Pts',(49.4630624688787,-55.1695746838168,0.));
#61059=CARTESIAN_POINT('Ctrl Pts',(49.4630624688787,-55.1695746838168,12.));
#61060=CARTESIAN_POINT('Ctrl Pts',(49.4881210723921,-55.1807492550073,0.));
#61061=CARTESIAN_POINT('Ctrl Pts',(49.4881210723921,-55.1807492550073,12.));
#61062=CARTESIAN_POINT('Ctrl Pts',(49.5132221132916,-55.1919154713569,0.));
#61063=CARTESIAN_POINT('Ctrl Pts',(49.5132221132916,-55.1919154713569,12.));
#61064=CARTESIAN_POINT('Ctrl Pts',(49.5383655367987,-55.2030732647222,0.));
#61065=CARTESIAN_POINT('Ctrl Pts',(49.5383655367987,-55.2030732647222,12.));
#61066=CARTESIAN_POINT('Ctrl Pts',(49.5635512873368,-55.2142225656943,0.));
#61067=CARTESIAN_POINT('Ctrl Pts',(49.5635512873368,-55.2142225656943,12.));
#61068=CARTESIAN_POINT('Ctrl Pts',(49.5887793068337,-55.225363300765,0.));
#61069=CARTESIAN_POINT('Ctrl Pts',(49.5887793068337,-55.225363300765,12.));
#61070=CARTESIAN_POINT('Ctrl Pts',(49.6140495332865,-55.2364953899423,0.));
#61071=CARTESIAN_POINT('Ctrl Pts',(49.6140495332865,-55.2364953899423,12.));
#61072=CARTESIAN_POINT('Ctrl Pts',(49.6393618987614,-55.2476187434204,0.));
#61073=CARTESIAN_POINT('Ctrl Pts',(49.6393618987614,-55.2476187434204,12.));
#61074=CARTESIAN_POINT('Ctrl Pts',(49.6647163322457,-55.2587332663982,0.));
#61075=CARTESIAN_POINT('Ctrl Pts',(49.6647163322457,-55.2587332663982,12.));
#61076=CARTESIAN_POINT('Ctrl Pts',(49.690112763181,-55.2698388650215,0.));
#61077=CARTESIAN_POINT('Ctrl Pts',(49.690112763181,-55.2698388650215,12.));
#61078=CARTESIAN_POINT('Ctrl Pts',(49.7155511248629,-55.2809354521616,0.));
#61079=CARTESIAN_POINT('Ctrl Pts',(49.7155511248629,-55.2809354521616,12.));
#61080=CARTESIAN_POINT('Ctrl Pts',(49.7410313576444,-55.292022952748,0.));
#61081=CARTESIAN_POINT('Ctrl Pts',(49.7410313576444,-55.292022952748,12.));
#61082=CARTESIAN_POINT('Ctrl Pts',(49.7665534128269,-55.3031013105578,0.));
#61083=CARTESIAN_POINT('Ctrl Pts',(49.7665534128269,-55.3031013105578,12.));
#61084=CARTESIAN_POINT('Ctrl Pts',(49.7921172540185,-55.3141704897307,0.));
#61085=CARTESIAN_POINT('Ctrl Pts',(49.7921172540185,-55.3141704897307,12.));
#61086=CARTESIAN_POINT('Ctrl Pts',(49.817722855186,-55.3252304694066,0.));
#61087=CARTESIAN_POINT('Ctrl Pts',(49.817722855186,-55.3252304694066,12.));
#61088=CARTESIAN_POINT('Ctrl Pts',(49.8382407306675,-55.3340710859607,0.));
#61089=CARTESIAN_POINT('Ctrl Pts',(49.8382407306675,-55.3340710859607,12.));
#61090=CARTESIAN_POINT('Ctrl Pts',(49.8536479176573,-55.340697403233,0.));
#61091=CARTESIAN_POINT('Ctrl Pts',(49.8536479176573,-55.340697403233,12.));
#61092=CARTESIAN_POINT('Ctrl Pts',(49.8639277221471,-55.3451131058727,0.));
#61093=CARTESIAN_POINT('Ctrl Pts',(49.8639277221471,-55.3451131058727,12.));
#61094=CARTESIAN_POINT('Ctrl Pts',(49.869069711016,-55.3473204966403,0.));
#61095=CARTESIAN_POINT('Ctrl Pts',(49.869069711016,-55.3473204966403,12.));
#61096=CARTESIAN_POINT('',(45.6458539113724,-53.0702932034641,0.));
#61097=CARTESIAN_POINT('Ctrl Pts',(45.6458539113724,-53.0702932034641,0.));
#61098=CARTESIAN_POINT('Ctrl Pts',(45.6490568514089,-53.0724894921849,0.));
#61099=CARTESIAN_POINT('Ctrl Pts',(45.6554684028145,-53.0768833804193,0.));
#61100=CARTESIAN_POINT('Ctrl Pts',(45.6651027439241,-53.0834781451546,0.));
#61101=CARTESIAN_POINT('Ctrl Pts',(45.6779825614231,-53.0922790298409,0.));
#61102=CARTESIAN_POINT('Ctrl Pts',(45.694139048907,-53.1032932328857,0.));
#61103=CARTESIAN_POINT('Ctrl Pts',(45.7103522376696,-53.114320495492,0.));
#61104=CARTESIAN_POINT('Ctrl Pts',(45.7266220897003,-53.1253607414872,0.));
#61105=CARTESIAN_POINT('Ctrl Pts',(45.7429485300823,-53.1364138384693,0.));
#61106=CARTESIAN_POINT('Ctrl Pts',(45.7593314474501,-53.1474795996053,0.));
#61107=CARTESIAN_POINT('Ctrl Pts',(45.7757707100618,-53.1585578076444,0.));
#61108=CARTESIAN_POINT('Ctrl Pts',(45.7922661780005,-53.1696482334487,0.));
#61109=CARTESIAN_POINT('Ctrl Pts',(45.8088177165089,-53.1807506560933,0.));
#61110=CARTESIAN_POINT('Ctrl Pts',(45.8254252099957,-53.1918648840541,0.));
#61111=CARTESIAN_POINT('Ctrl Pts',(45.8420885575349,-53.2029907483557,0.));
#61112=CARTESIAN_POINT('Ctrl Pts',(45.8588076662582,-53.2141280925439,0.));
#61113=CARTESIAN_POINT('Ctrl Pts',(45.8755824458722,-53.2252767643662,0.));
#61114=CARTESIAN_POINT('Ctrl Pts',(45.8924128018379,-53.2364366054306,0.));
#61115=CARTESIAN_POINT('Ctrl Pts',(45.9092986319377,-53.2476074460017,0.));
#61116=CARTESIAN_POINT('Ctrl Pts',(45.9262398298349,-53.2587891103866,0.));
#61117=CARTESIAN_POINT('Ctrl Pts',(45.9432362873008,-53.2699814203105,0.));
#61118=CARTESIAN_POINT('Ctrl Pts',(45.9602878967698,-53.2811841987926,0.));
#61119=CARTESIAN_POINT('Ctrl Pts',(45.9773945542384,-53.292397274555,0.));
#61120=CARTESIAN_POINT('Ctrl Pts',(45.9945561591453,-53.3036204818329,0.));
#61121=CARTESIAN_POINT('Ctrl Pts',(46.0117726129873,-53.3148536582635,0.));
#61122=CARTESIAN_POINT('Ctrl Pts',(46.02904381836,-53.326096643428,0.));
#61123=CARTESIAN_POINT('Ctrl Pts',(46.0463696777801,-53.3373492770671,0.));
#61124=CARTESIAN_POINT('Ctrl Pts',(46.0637500926982,-53.3486113975901,0.));
#61125=CARTESIAN_POINT('Ctrl Pts',(46.0811849640218,-53.3598828428546,0.));
#61126=CARTESIAN_POINT('Ctrl Pts',(46.0986741925656,-53.3711634508437,0.));
#61127=CARTESIAN_POINT('Ctrl Pts',(46.1162176794884,-53.3824530603276,0.));
#61128=CARTESIAN_POINT('Ctrl Pts',(46.1338153268097,-53.3937515116549,0.));
#61129=CARTESIAN_POINT('Ctrl Pts',(46.1514670376012,-53.4050586470436,0.));
#61130=CARTESIAN_POINT('Ctrl Pts',(46.1691727157134,-53.4163743101517,0.));
#61131=CARTESIAN_POINT('Ctrl Pts',(46.1869322656023,-53.4276983458125,0.));
#61132=CARTESIAN_POINT('Ctrl Pts',(46.2047455921286,-53.4390305997274,0.));
#61133=CARTESIAN_POINT('Ctrl Pts',(46.2226126003202,-53.4503709181178,0.));
#61134=CARTESIAN_POINT('Ctrl Pts',(46.2405331953889,-53.4617191477402,0.));
#61135=CARTESIAN_POINT('Ctrl Pts',(46.2585072828353,-53.4730751360371,0.));
#61136=CARTESIAN_POINT('Ctrl Pts',(46.2765347685198,-53.4844387312414,0.));
#61137=CARTESIAN_POINT('Ctrl Pts',(46.2946155587417,-53.4958097825006,0.));
#61138=CARTESIAN_POINT('Ctrl Pts',(46.3127495603098,-53.5071881399911,0.));
#61139=CARTESIAN_POINT('Ctrl Pts',(46.3309366805093,-53.5185736548548,0.));
#61140=CARTESIAN_POINT('Ctrl Pts',(46.3491768270655,-53.5299661791385,0.));
#61141=CARTESIAN_POINT('Ctrl Pts',(46.3674699081046,-53.5413655657327,0.));
#61142=CARTESIAN_POINT('Ctrl Pts',(46.3858158321059,-53.5527716683048,0.));
#61143=CARTESIAN_POINT('Ctrl Pts',(46.4042145078701,-53.5641843412559,0.));
#61144=CARTESIAN_POINT('Ctrl Pts',(46.4226658445474,-53.5756034397481,0.));
#61145=CARTESIAN_POINT('Ctrl Pts',(46.4411697516478,-53.5870288197166,0.));
#61146=CARTESIAN_POINT('Ctrl Pts',(46.459726139052,-53.5984603378855,0.));
#61147=CARTESIAN_POINT('Ctrl Pts',(46.4783349170173,-53.6098978517859,0.));
#61148=CARTESIAN_POINT('Ctrl Pts',(46.496995996177,-53.6213412197533,0.));
#61149=CARTESIAN_POINT('Ctrl Pts',(46.5157092875373,-53.6327903009094,0.));
#61150=CARTESIAN_POINT('Ctrl Pts',(46.5344747024676,-53.6442449551455,0.));
#61151=CARTESIAN_POINT('Ctrl Pts',(46.5532921526901,-53.6557050431071,0.));
#61152=CARTESIAN_POINT('Ctrl Pts',(46.5721615502591,-53.6671704261737,0.));
#61153=CARTESIAN_POINT('Ctrl Pts',(46.5910828075653,-53.678640966456,0.));
#61154=CARTESIAN_POINT('Ctrl Pts',(46.6100558373402,-53.6901165267941,0.));
#61155=CARTESIAN_POINT('Ctrl Pts',(46.6290805526559,-53.701596970754,0.));
#61156=CARTESIAN_POINT('Ctrl Pts',(46.6481568669216,-53.7130821626263,0.));
#61157=CARTESIAN_POINT('Ctrl Pts',(46.6672846938752,-53.7245719674222,0.));
#61158=CARTESIAN_POINT('Ctrl Pts',(46.6864639475863,-53.7360662508677,0.));
#61159=CARTESIAN_POINT('Ctrl Pts',(46.7056945424559,-53.7475648793948,0.));
#61160=CARTESIAN_POINT('Ctrl Pts',(46.724976393213,-53.7590677201344,0.));
#61161=CARTESIAN_POINT('Ctrl Pts',(46.7443094149041,-53.770574640907,0.));
#61162=CARTESIAN_POINT('Ctrl Pts',(46.7636935228851,-53.782085510217,0.));
#61163=CARTESIAN_POINT('Ctrl Pts',(46.7831286328268,-53.7936001972468,0.));
#61164=CARTESIAN_POINT('Ctrl Pts',(46.8026146607144,-53.8051185718525,0.));
#61165=CARTESIAN_POINT('Ctrl Pts',(46.8221515228459,-53.8166405045582,0.));
#61166=CARTESIAN_POINT('Ctrl Pts',(46.8417391358231,-53.8281658665517,0.));
#61167=CARTESIAN_POINT('Ctrl Pts',(46.8613774165452,-53.8396945296777,0.));
#61168=CARTESIAN_POINT('Ctrl Pts',(46.8810662822146,-53.851226366434,0.));
#61169=CARTESIAN_POINT('Ctrl Pts',(46.900805650336,-53.8627612499648,0.));
#61170=CARTESIAN_POINT('Ctrl Pts',(46.9205954387128,-53.8742990540557,0.));
#61171=CARTESIAN_POINT('Ctrl Pts',(46.9404355654381,-53.8858396531277,0.));
#61172=CARTESIAN_POINT('Ctrl Pts',(46.9603259488894,-53.8973829222317,0.));
#61173=CARTESIAN_POINT('Ctrl Pts',(46.9802665077342,-53.9089287370436,0.));
#61174=CARTESIAN_POINT('Ctrl Pts',(47.0002571609286,-53.9204769738584,0.));
#61175=CARTESIAN_POINT('Ctrl Pts',(47.0202978277148,-53.9320275095864,0.));
#61176=CARTESIAN_POINT('Ctrl Pts',(47.04038842761,-53.9435802217468,0.));
#61177=CARTESIAN_POINT('Ctrl Pts',(47.0605288804042,-53.9551349884637,0.));
#61178=CARTESIAN_POINT('Ctrl Pts',(47.0807191061673,-53.9666916884624,0.));
#61179=CARTESIAN_POINT('Ctrl Pts',(47.1009590252466,-53.9782502010642,0.));
#61180=CARTESIAN_POINT('Ctrl Pts',(47.1212485582632,-53.9898104061809,0.));
#61181=CARTESIAN_POINT('Ctrl Pts',(47.1415876261012,-54.0013721843094,0.));
#61182=CARTESIAN_POINT('Ctrl Pts',(47.161976149906,-54.0129354165269,0.));
#61183=CARTESIAN_POINT('Ctrl Pts',(47.1824140510906,-54.0244999844872,0.));
#61184=CARTESIAN_POINT('Ctrl Pts',(47.2029012513334,-54.0360657704156,0.));
#61185=CARTESIAN_POINT('Ctrl Pts',(47.2234376725752,-54.047632657105,0.));
#61186=CARTESIAN_POINT('Ctrl Pts',(47.2440232370085,-54.0592005279108,0.));
#61187=CARTESIAN_POINT('Ctrl Pts',(47.2646578670767,-54.0707692667461,0.));
#61188=CARTESIAN_POINT('Ctrl Pts',(47.2853414854805,-54.082338758079,0.));
#61189=CARTESIAN_POINT('Ctrl Pts',(47.3060740151754,-54.0939088869271,0.));
#61190=CARTESIAN_POINT('Ctrl Pts',(47.326855379369,-54.1054795388538,0.));
#61191=CARTESIAN_POINT('Ctrl Pts',(47.3476855015095,-54.1170505999637,0.));
#61192=CARTESIAN_POINT('Ctrl Pts',(47.3685643052867,-54.1286219568981,0.));
#61193=CARTESIAN_POINT('Ctrl Pts',(47.3894917146361,-54.1401934968306,0.));
#61194=CARTESIAN_POINT('Ctrl Pts',(47.4104676537381,-54.1517651074638,0.));
#61195=CARTESIAN_POINT('Ctrl Pts',(47.4314920470142,-54.163336677024,0.));
#61196=CARTESIAN_POINT('Ctrl Pts',(47.4525648191173,-54.1749080942593,0.));
#61197=CARTESIAN_POINT('Ctrl Pts',(47.473685894932,-54.1864792484343,0.));
#61198=CARTESIAN_POINT('Ctrl Pts',(47.4948551995798,-54.1980500293267,0.));
#61199=CARTESIAN_POINT('Ctrl Pts',(47.5160726584172,-54.2096203272228,0.));
#61200=CARTESIAN_POINT('Ctrl Pts',(47.5373381970328,-54.2211900329141,0.));
#61201=CARTESIAN_POINT('Ctrl Pts',(47.5586517412368,-54.232759037693,0.));
#61202=CARTESIAN_POINT('Ctrl Pts',(47.5800132170614,-54.2443272333498,0.));
#61203=CARTESIAN_POINT('Ctrl Pts',(47.6014225507663,-54.2558945121684,0.));
#61204=CARTESIAN_POINT('Ctrl Pts',(47.6228796688376,-54.2674607669228,0.));
#61205=CARTESIAN_POINT('Ctrl Pts',(47.6443844979846,-54.2790258908736,0.));
#61206=CARTESIAN_POINT('Ctrl Pts',(47.6659369651299,-54.2905897777647,0.));
#61207=CARTESIAN_POINT('Ctrl Pts',(47.6875369974086,-54.3021523218188,0.));
#61208=CARTESIAN_POINT('Ctrl Pts',(47.7091845221747,-54.3137134177345,0.));
#61209=CARTESIAN_POINT('Ctrl Pts',(47.7308794669994,-54.3252729606824,0.));
#61210=CARTESIAN_POINT('Ctrl Pts',(47.7526217596694,-54.3368308463023,0.));
#61211=CARTESIAN_POINT('Ctrl Pts',(47.7744113281767,-54.3483869706998,0.));
#61212=CARTESIAN_POINT('Ctrl Pts',(47.7962481007179,-54.3599412304431,0.));
#61213=CARTESIAN_POINT('Ctrl Pts',(47.8181320056988,-54.3714935225585,0.));
#61214=CARTESIAN_POINT('Ctrl Pts',(47.8400629717352,-54.3830437445275,0.));
#61215=CARTESIAN_POINT('Ctrl Pts',(47.8620409276495,-54.3945917942835,0.));
#61216=CARTESIAN_POINT('Ctrl Pts',(47.8840658024626,-54.4061375702088,0.));
#61217=CARTESIAN_POINT('Ctrl Pts',(47.9061375253909,-54.4176809711324,0.));
#61218=CARTESIAN_POINT('Ctrl Pts',(47.9282560258528,-54.4292218963253,0.));
#61219=CARTESIAN_POINT('Ctrl Pts',(47.9504212334681,-54.4407602454974,0.));
#61220=CARTESIAN_POINT('Ctrl Pts',(47.972633078057,-54.4522959187952,0.));
#61221=CARTESIAN_POINT('Ctrl Pts',(47.9948914896316,-54.4638288167991,0.));
#61222=CARTESIAN_POINT('Ctrl Pts',(48.0171963983912,-54.4753588405202,0.));
#61223=CARTESIAN_POINT('Ctrl Pts',(48.039547734729,-54.4868858913961,0.));
#61224=CARTESIAN_POINT('Ctrl Pts',(48.0619454292321,-54.4984098712883,0.));
#61225=CARTESIAN_POINT('Ctrl Pts',(48.0843894126807,-54.5099306824788,0.));
#61226=CARTESIAN_POINT('Ctrl Pts',(48.1068796160406,-54.5214482276679,0.));
#61227=CARTESIAN_POINT('Ctrl Pts',(48.1294159704571,-54.5329624099719,0.));
#61228=CARTESIAN_POINT('Ctrl Pts',(48.1519984072617,-54.5444731329196,0.));
#61229=CARTESIAN_POINT('Ctrl Pts',(48.1746268579732,-54.5559803004487,0.));
#61230=CARTESIAN_POINT('Ctrl Pts',(48.1973012542966,-54.5674838169041,0.));
#61231=CARTESIAN_POINT('Ctrl Pts',(48.2200215281178,-54.5789835870348,0.));
#61232=CARTESIAN_POINT('Ctrl Pts',(48.2427876114955,-54.5904795159936,0.));
#61233=CARTESIAN_POINT('Ctrl Pts',(48.2655994366672,-54.6019715093319,0.));
#61234=CARTESIAN_POINT('Ctrl Pts',(48.288456936051,-54.6134594729964,0.));
#61235=CARTESIAN_POINT('Ctrl Pts',(48.3113600422443,-54.6249433133262,0.));
#61236=CARTESIAN_POINT('Ctrl Pts',(48.3343086880192,-54.636422937049,0.));
#61237=CARTESIAN_POINT('Ctrl Pts',(48.3573028063121,-54.647898251279,0.));
#61238=CARTESIAN_POINT('Ctrl Pts',(48.3803423302294,-54.6593691635143,0.));
#61239=CARTESIAN_POINT('Ctrl Pts',(48.4034271930516,-54.6708355816359,0.));
#61240=CARTESIAN_POINT('Ctrl Pts',(48.4265573282341,-54.6822974139065,0.));
#61241=CARTESIAN_POINT('Ctrl Pts',(48.4497326694051,-54.6937545689694,0.));
#61242=CARTESIAN_POINT('Ctrl Pts',(48.4729531503565,-54.7052069558493,0.));
#61243=CARTESIAN_POINT('Ctrl Pts',(48.4962187050451,-54.7166544839475,0.));
#61244=CARTESIAN_POINT('Ctrl Pts',(48.5195292675955,-54.7280970630346,0.));
#61245=CARTESIAN_POINT('Ctrl Pts',(48.5428847722974,-54.7395346032451,0.));
#61246=CARTESIAN_POINT('Ctrl Pts',(48.5662851536027,-54.7509670150716,0.));
#61247=CARTESIAN_POINT('Ctrl Pts',(48.5897303461131,-54.7623942093591,0.));
#61248=CARTESIAN_POINT('Ctrl Pts',(48.6132202845792,-54.773816097304,0.));
#61249=CARTESIAN_POINT('Ctrl Pts',(48.6367549039121,-54.7852325904591,0.));
#61250=CARTESIAN_POINT('Ctrl Pts',(48.6603341391891,-54.7966436007395,0.));
#61251=CARTESIAN_POINT('Ctrl Pts',(48.6839579256565,-54.8080490404274,0.));
#61252=CARTESIAN_POINT('Ctrl Pts',(48.7076261987284,-54.8194488221803,0.));
#61253=CARTESIAN_POINT('Ctrl Pts',(48.7313388939834,-54.8308428590334,0.));
#61254=CARTESIAN_POINT('Ctrl Pts',(48.755095947159,-54.8422310643752,0.));
#61255=CARTESIAN_POINT('Ctrl Pts',(48.7788972941431,-54.8536133519285,0.));
#61256=CARTESIAN_POINT('Ctrl Pts',(48.8027428709613,-54.8649896357284,0.));
#61257=CARTESIAN_POINT('Ctrl Pts',(48.8266326137629,-54.8763598301045,0.));
#61258=CARTESIAN_POINT('Ctrl Pts',(48.8505664587984,-54.8877238496577,0.));
#61259=CARTESIAN_POINT('Ctrl Pts',(48.8745443424488,-54.8990816092964,0.));
#61260=CARTESIAN_POINT('Ctrl Pts',(48.8985662012535,-54.910433024275,0.));
#61261=CARTESIAN_POINT('Ctrl Pts',(48.922631971937,-54.9217780102357,0.));
#61262=CARTESIAN_POINT('Ctrl Pts',(48.9467415914266,-54.933116483242,0.));
#61263=CARTESIAN_POINT('Ctrl Pts',(48.9708949968789,-54.9444483598372,0.));
#61264=CARTESIAN_POINT('Ctrl Pts',(48.995092125652,-54.9557735569936,0.));
#61265=CARTESIAN_POINT('Ctrl Pts',(49.0193329152475,-54.9670919920024,0.));
#61266=CARTESIAN_POINT('Ctrl Pts',(49.0436173032527,-54.9784035823764,0.));
#61267=CARTESIAN_POINT('Ctrl Pts',(49.0679452272871,-54.9897082457607,0.));
#61268=CARTESIAN_POINT('Ctrl Pts',(49.0923166249222,-55.0010058998111,0.));
#61269=CARTESIAN_POINT('Ctrl Pts',(49.1167314336737,-55.0122964621868,0.));
#61270=CARTESIAN_POINT('Ctrl Pts',(49.1411895911645,-55.0235798508056,0.));
#61271=CARTESIAN_POINT('Ctrl Pts',(49.1656910352484,-55.0348559840462,0.));
#61272=CARTESIAN_POINT('Ctrl Pts',(49.1902357041462,-55.0461247809745,0.));
#61273=CARTESIAN_POINT('Ctrl Pts',(49.2148235365694,-55.0573861615569,0.));
#61274=CARTESIAN_POINT('Ctrl Pts',(49.2394544718512,-55.0686400468911,0.));
#61275=CARTESIAN_POINT('Ctrl Pts',(49.2641284496496,-55.0798863586986,0.));
#61276=CARTESIAN_POINT('Ctrl Pts',(49.2888454096544,-55.0911250188282,0.));
#61277=CARTESIAN_POINT('Ctrl Pts',(49.3136052912614,-55.1023559487133,0.));
#61278=CARTESIAN_POINT('Ctrl Pts',(49.3384080333166,-55.1135790689475,0.));
#61279=CARTESIAN_POINT('Ctrl Pts',(49.3632535736744,-55.1247942985649,0.));
#61280=CARTESIAN_POINT('Ctrl Pts',(49.3881418495529,-55.1360015556262,0.));
#61281=CARTESIAN_POINT('Ctrl Pts',(49.413072798324,-55.1472007585224,0.));
#61282=CARTESIAN_POINT('Ctrl Pts',(49.4380463581989,-55.158391827114,0.));
#61283=CARTESIAN_POINT('Ctrl Pts',(49.4630624688787,-55.1695746838168,0.));
#61284=CARTESIAN_POINT('Ctrl Pts',(49.4881210723921,-55.1807492550073,0.));
#61285=CARTESIAN_POINT('Ctrl Pts',(49.5132221132916,-55.1919154713569,0.));
#61286=CARTESIAN_POINT('Ctrl Pts',(49.5347748994608,-55.2014798623976,0.));
#61287=CARTESIAN_POINT('Ctrl Pts',(49.5513218524282,-55.2088081098956,0.));
#61288=CARTESIAN_POINT('Ctrl Pts',(49.5628442141874,-55.2139039604571,0.));
#61289=CARTESIAN_POINT('Ctrl Pts',(49.5693295981614,-55.216769915117,0.));
#61290=CARTESIAN_POINT('Ctrl Pts',(49.5707719660262,-55.21740720013,0.));
#61291=CARTESIAN_POINT('',(45.6458539113724,-53.0702932034641,12.));
#61292=CARTESIAN_POINT('',(45.6458539113724,-53.0702932034641,0.));
#61293=CARTESIAN_POINT('Ctrl Pts',(49.5707719660262,-55.21740720013,12.));
#61294=CARTESIAN_POINT('Ctrl Pts',(49.5693295981614,-55.216769915117,12.));
#61295=CARTESIAN_POINT('Ctrl Pts',(49.5628442141874,-55.2139039604571,12.));
#61296=CARTESIAN_POINT('Ctrl Pts',(49.5513218524282,-55.2088081098956,12.));
#61297=CARTESIAN_POINT('Ctrl Pts',(49.5347748994608,-55.2014798623976,12.));
#61298=CARTESIAN_POINT('Ctrl Pts',(49.5132221132916,-55.1919154713569,12.));
#61299=CARTESIAN_POINT('Ctrl Pts',(49.4881210723921,-55.1807492550073,12.));
#61300=CARTESIAN_POINT('Ctrl Pts',(49.4630624688787,-55.1695746838168,12.));
#61301=CARTESIAN_POINT('Ctrl Pts',(49.4380463581989,-55.158391827114,12.));
#61302=CARTESIAN_POINT('Ctrl Pts',(49.413072798324,-55.1472007585224,12.));
#61303=CARTESIAN_POINT('Ctrl Pts',(49.3881418495529,-55.1360015556262,12.));
#61304=CARTESIAN_POINT('Ctrl Pts',(49.3632535736744,-55.1247942985649,12.));
#61305=CARTESIAN_POINT('Ctrl Pts',(49.3384080333166,-55.1135790689475,12.));
#61306=CARTESIAN_POINT('Ctrl Pts',(49.3136052912614,-55.1023559487133,12.));
#61307=CARTESIAN_POINT('Ctrl Pts',(49.2888454096544,-55.0911250188282,12.));
#61308=CARTESIAN_POINT('Ctrl Pts',(49.2641284496496,-55.0798863586986,12.));
#61309=CARTESIAN_POINT('Ctrl Pts',(49.2394544718512,-55.0686400468911,12.));
#61310=CARTESIAN_POINT('Ctrl Pts',(49.2148235365694,-55.0573861615569,12.));
#61311=CARTESIAN_POINT('Ctrl Pts',(49.1902357041462,-55.0461247809745,12.));
#61312=CARTESIAN_POINT('Ctrl Pts',(49.1656910352484,-55.0348559840462,12.));
#61313=CARTESIAN_POINT('Ctrl Pts',(49.1411895911645,-55.0235798508056,12.));
#61314=CARTESIAN_POINT('Ctrl Pts',(49.1167314336737,-55.0122964621868,12.));
#61315=CARTESIAN_POINT('Ctrl Pts',(49.0923166249222,-55.0010058998111,12.));
#61316=CARTESIAN_POINT('Ctrl Pts',(49.0679452272871,-54.9897082457607,12.));
#61317=CARTESIAN_POINT('Ctrl Pts',(49.0436173032527,-54.9784035823764,12.));
#61318=CARTESIAN_POINT('Ctrl Pts',(49.0193329152475,-54.9670919920024,12.));
#61319=CARTESIAN_POINT('Ctrl Pts',(48.995092125652,-54.9557735569936,12.));
#61320=CARTESIAN_POINT('Ctrl Pts',(48.9708949968789,-54.9444483598372,12.));
#61321=CARTESIAN_POINT('Ctrl Pts',(48.9467415914266,-54.933116483242,12.));
#61322=CARTESIAN_POINT('Ctrl Pts',(48.922631971937,-54.9217780102357,12.));
#61323=CARTESIAN_POINT('Ctrl Pts',(48.8985662012535,-54.910433024275,12.));
#61324=CARTESIAN_POINT('Ctrl Pts',(48.8745443424488,-54.8990816092964,12.));
#61325=CARTESIAN_POINT('Ctrl Pts',(48.8505664587984,-54.8877238496577,12.));
#61326=CARTESIAN_POINT('Ctrl Pts',(48.8266326137629,-54.8763598301045,12.));
#61327=CARTESIAN_POINT('Ctrl Pts',(48.8027428709613,-54.8649896357284,12.));
#61328=CARTESIAN_POINT('Ctrl Pts',(48.7788972941431,-54.8536133519285,12.));
#61329=CARTESIAN_POINT('Ctrl Pts',(48.755095947159,-54.8422310643752,12.));
#61330=CARTESIAN_POINT('Ctrl Pts',(48.7313388939834,-54.8308428590334,12.));
#61331=CARTESIAN_POINT('Ctrl Pts',(48.7076261987284,-54.8194488221803,12.));
#61332=CARTESIAN_POINT('Ctrl Pts',(48.6839579256565,-54.8080490404274,12.));
#61333=CARTESIAN_POINT('Ctrl Pts',(48.6603341391891,-54.7966436007395,12.));
#61334=CARTESIAN_POINT('Ctrl Pts',(48.6367549039121,-54.7852325904591,12.));
#61335=CARTESIAN_POINT('Ctrl Pts',(48.6132202845792,-54.773816097304,12.));
#61336=CARTESIAN_POINT('Ctrl Pts',(48.5897303461131,-54.7623942093591,12.));
#61337=CARTESIAN_POINT('Ctrl Pts',(48.5662851536027,-54.7509670150716,12.));
#61338=CARTESIAN_POINT('Ctrl Pts',(48.5428847722974,-54.7395346032451,12.));
#61339=CARTESIAN_POINT('Ctrl Pts',(48.5195292675955,-54.7280970630346,12.));
#61340=CARTESIAN_POINT('Ctrl Pts',(48.4962187050451,-54.7166544839475,12.));
#61341=CARTESIAN_POINT('Ctrl Pts',(48.4729531503565,-54.7052069558493,12.));
#61342=CARTESIAN_POINT('Ctrl Pts',(48.4497326694051,-54.6937545689694,12.));
#61343=CARTESIAN_POINT('Ctrl Pts',(48.4265573282341,-54.6822974139065,12.));
#61344=CARTESIAN_POINT('Ctrl Pts',(48.4034271930516,-54.6708355816359,12.));
#61345=CARTESIAN_POINT('Ctrl Pts',(48.3803423302294,-54.6593691635143,12.));
#61346=CARTESIAN_POINT('Ctrl Pts',(48.3573028063121,-54.647898251279,12.));
#61347=CARTESIAN_POINT('Ctrl Pts',(48.3343086880192,-54.636422937049,12.));
#61348=CARTESIAN_POINT('Ctrl Pts',(48.3113600422443,-54.6249433133262,12.));
#61349=CARTESIAN_POINT('Ctrl Pts',(48.288456936051,-54.6134594729964,12.));
#61350=CARTESIAN_POINT('Ctrl Pts',(48.2655994366672,-54.6019715093319,12.));
#61351=CARTESIAN_POINT('Ctrl Pts',(48.2427876114955,-54.5904795159936,12.));
#61352=CARTESIAN_POINT('Ctrl Pts',(48.2200215281178,-54.5789835870348,12.));
#61353=CARTESIAN_POINT('Ctrl Pts',(48.1973012542966,-54.5674838169041,12.));
#61354=CARTESIAN_POINT('Ctrl Pts',(48.1746268579732,-54.5559803004487,12.));
#61355=CARTESIAN_POINT('Ctrl Pts',(48.1519984072617,-54.5444731329196,12.));
#61356=CARTESIAN_POINT('Ctrl Pts',(48.1294159704571,-54.5329624099719,12.));
#61357=CARTESIAN_POINT('Ctrl Pts',(48.1068796160406,-54.5214482276679,12.));
#61358=CARTESIAN_POINT('Ctrl Pts',(48.0843894126807,-54.5099306824788,12.));
#61359=CARTESIAN_POINT('Ctrl Pts',(48.0619454292321,-54.4984098712883,12.));
#61360=CARTESIAN_POINT('Ctrl Pts',(48.039547734729,-54.4868858913961,12.));
#61361=CARTESIAN_POINT('Ctrl Pts',(48.0171963983912,-54.4753588405202,12.));
#61362=CARTESIAN_POINT('Ctrl Pts',(47.9948914896316,-54.4638288167991,12.));
#61363=CARTESIAN_POINT('Ctrl Pts',(47.972633078057,-54.4522959187952,12.));
#61364=CARTESIAN_POINT('Ctrl Pts',(47.9504212334681,-54.4407602454974,12.));
#61365=CARTESIAN_POINT('Ctrl Pts',(47.9282560258528,-54.4292218963253,12.));
#61366=CARTESIAN_POINT('Ctrl Pts',(47.9061375253909,-54.4176809711324,12.));
#61367=CARTESIAN_POINT('Ctrl Pts',(47.8840658024626,-54.4061375702088,12.));
#61368=CARTESIAN_POINT('Ctrl Pts',(47.8620409276495,-54.3945917942835,12.));
#61369=CARTESIAN_POINT('Ctrl Pts',(47.8400629717352,-54.3830437445275,12.));
#61370=CARTESIAN_POINT('Ctrl Pts',(47.8181320056988,-54.3714935225585,12.));
#61371=CARTESIAN_POINT('Ctrl Pts',(47.7962481007179,-54.3599412304431,12.));
#61372=CARTESIAN_POINT('Ctrl Pts',(47.7744113281767,-54.3483869706998,12.));
#61373=CARTESIAN_POINT('Ctrl Pts',(47.7526217596694,-54.3368308463023,12.));
#61374=CARTESIAN_POINT('Ctrl Pts',(47.7308794669994,-54.3252729606824,12.));
#61375=CARTESIAN_POINT('Ctrl Pts',(47.7091845221747,-54.3137134177345,12.));
#61376=CARTESIAN_POINT('Ctrl Pts',(47.6875369974086,-54.3021523218188,12.));
#61377=CARTESIAN_POINT('Ctrl Pts',(47.6659369651299,-54.2905897777647,12.));
#61378=CARTESIAN_POINT('Ctrl Pts',(47.6443844979846,-54.2790258908736,12.));
#61379=CARTESIAN_POINT('Ctrl Pts',(47.6228796688376,-54.2674607669228,12.));
#61380=CARTESIAN_POINT('Ctrl Pts',(47.6014225507663,-54.2558945121684,12.));
#61381=CARTESIAN_POINT('Ctrl Pts',(47.5800132170614,-54.2443272333498,12.));
#61382=CARTESIAN_POINT('Ctrl Pts',(47.5586517412368,-54.232759037693,12.));
#61383=CARTESIAN_POINT('Ctrl Pts',(47.5373381970328,-54.2211900329141,12.));
#61384=CARTESIAN_POINT('Ctrl Pts',(47.5160726584172,-54.2096203272228,12.));
#61385=CARTESIAN_POINT('Ctrl Pts',(47.4948551995798,-54.1980500293267,12.));
#61386=CARTESIAN_POINT('Ctrl Pts',(47.473685894932,-54.1864792484343,12.));
#61387=CARTESIAN_POINT('Ctrl Pts',(47.4525648191173,-54.1749080942593,12.));
#61388=CARTESIAN_POINT('Ctrl Pts',(47.4314920470142,-54.163336677024,12.));
#61389=CARTESIAN_POINT('Ctrl Pts',(47.4104676537381,-54.1517651074638,12.));
#61390=CARTESIAN_POINT('Ctrl Pts',(47.3894917146361,-54.1401934968306,12.));
#61391=CARTESIAN_POINT('Ctrl Pts',(47.3685643052867,-54.1286219568981,12.));
#61392=CARTESIAN_POINT('Ctrl Pts',(47.3476855015095,-54.1170505999637,12.));
#61393=CARTESIAN_POINT('Ctrl Pts',(47.326855379369,-54.1054795388538,12.));
#61394=CARTESIAN_POINT('Ctrl Pts',(47.3060740151754,-54.0939088869271,12.));
#61395=CARTESIAN_POINT('Ctrl Pts',(47.2853414854805,-54.082338758079,12.));
#61396=CARTESIAN_POINT('Ctrl Pts',(47.2646578670767,-54.0707692667461,12.));
#61397=CARTESIAN_POINT('Ctrl Pts',(47.2440232370085,-54.0592005279108,12.));
#61398=CARTESIAN_POINT('Ctrl Pts',(47.2234376725752,-54.047632657105,12.));
#61399=CARTESIAN_POINT('Ctrl Pts',(47.2029012513334,-54.0360657704156,12.));
#61400=CARTESIAN_POINT('Ctrl Pts',(47.1824140510906,-54.0244999844872,12.));
#61401=CARTESIAN_POINT('Ctrl Pts',(47.161976149906,-54.0129354165269,12.));
#61402=CARTESIAN_POINT('Ctrl Pts',(47.1415876261012,-54.0013721843094,12.));
#61403=CARTESIAN_POINT('Ctrl Pts',(47.1212485582632,-53.9898104061809,12.));
#61404=CARTESIAN_POINT('Ctrl Pts',(47.1009590252466,-53.9782502010642,12.));
#61405=CARTESIAN_POINT('Ctrl Pts',(47.0807191061673,-53.9666916884624,12.));
#61406=CARTESIAN_POINT('Ctrl Pts',(47.0605288804042,-53.9551349884637,12.));
#61407=CARTESIAN_POINT('Ctrl Pts',(47.04038842761,-53.9435802217468,12.));
#61408=CARTESIAN_POINT('Ctrl Pts',(47.0202978277148,-53.9320275095864,12.));
#61409=CARTESIAN_POINT('Ctrl Pts',(47.0002571609286,-53.9204769738584,12.));
#61410=CARTESIAN_POINT('Ctrl Pts',(46.9802665077342,-53.9089287370436,12.));
#61411=CARTESIAN_POINT('Ctrl Pts',(46.9603259488894,-53.8973829222317,12.));
#61412=CARTESIAN_POINT('Ctrl Pts',(46.9404355654381,-53.8858396531277,12.));
#61413=CARTESIAN_POINT('Ctrl Pts',(46.9205954387128,-53.8742990540557,12.));
#61414=CARTESIAN_POINT('Ctrl Pts',(46.900805650336,-53.8627612499648,12.));
#61415=CARTESIAN_POINT('Ctrl Pts',(46.8810662822146,-53.851226366434,12.));
#61416=CARTESIAN_POINT('Ctrl Pts',(46.8613774165452,-53.8396945296777,12.));
#61417=CARTESIAN_POINT('Ctrl Pts',(46.8417391358231,-53.8281658665517,12.));
#61418=CARTESIAN_POINT('Ctrl Pts',(46.8221515228459,-53.8166405045582,12.));
#61419=CARTESIAN_POINT('Ctrl Pts',(46.8026146607144,-53.8051185718525,12.));
#61420=CARTESIAN_POINT('Ctrl Pts',(46.7831286328268,-53.7936001972468,12.));
#61421=CARTESIAN_POINT('Ctrl Pts',(46.7636935228851,-53.782085510217,12.));
#61422=CARTESIAN_POINT('Ctrl Pts',(46.7443094149041,-53.770574640907,12.));
#61423=CARTESIAN_POINT('Ctrl Pts',(46.724976393213,-53.7590677201344,12.));
#61424=CARTESIAN_POINT('Ctrl Pts',(46.7056945424559,-53.7475648793948,12.));
#61425=CARTESIAN_POINT('Ctrl Pts',(46.6864639475863,-53.7360662508677,12.));
#61426=CARTESIAN_POINT('Ctrl Pts',(46.6672846938752,-53.7245719674222,12.));
#61427=CARTESIAN_POINT('Ctrl Pts',(46.6481568669216,-53.7130821626263,12.));
#61428=CARTESIAN_POINT('Ctrl Pts',(46.6290805526559,-53.701596970754,12.));
#61429=CARTESIAN_POINT('Ctrl Pts',(46.6100558373402,-53.6901165267941,12.));
#61430=CARTESIAN_POINT('Ctrl Pts',(46.5910828075653,-53.678640966456,12.));
#61431=CARTESIAN_POINT('Ctrl Pts',(46.5721615502591,-53.6671704261737,12.));
#61432=CARTESIAN_POINT('Ctrl Pts',(46.5532921526901,-53.6557050431071,12.));
#61433=CARTESIAN_POINT('Ctrl Pts',(46.5344747024676,-53.6442449551455,12.));
#61434=CARTESIAN_POINT('Ctrl Pts',(46.5157092875373,-53.6327903009094,12.));
#61435=CARTESIAN_POINT('Ctrl Pts',(46.496995996177,-53.6213412197533,12.));
#61436=CARTESIAN_POINT('Ctrl Pts',(46.4783349170173,-53.6098978517859,12.));
#61437=CARTESIAN_POINT('Ctrl Pts',(46.459726139052,-53.5984603378855,12.));
#61438=CARTESIAN_POINT('Ctrl Pts',(46.4411697516478,-53.5870288197166,12.));
#61439=CARTESIAN_POINT('Ctrl Pts',(46.4226658445474,-53.5756034397481,12.));
#61440=CARTESIAN_POINT('Ctrl Pts',(46.4042145078701,-53.5641843412559,12.));
#61441=CARTESIAN_POINT('Ctrl Pts',(46.3858158321059,-53.5527716683048,12.));
#61442=CARTESIAN_POINT('Ctrl Pts',(46.3674699081046,-53.5413655657327,12.));
#61443=CARTESIAN_POINT('Ctrl Pts',(46.3491768270655,-53.5299661791385,12.));
#61444=CARTESIAN_POINT('Ctrl Pts',(46.3309366805093,-53.5185736548548,12.));
#61445=CARTESIAN_POINT('Ctrl Pts',(46.3127495603098,-53.5071881399911,12.));
#61446=CARTESIAN_POINT('Ctrl Pts',(46.2946155587417,-53.4958097825006,12.));
#61447=CARTESIAN_POINT('Ctrl Pts',(46.2765347685198,-53.4844387312414,12.));
#61448=CARTESIAN_POINT('Ctrl Pts',(46.2585072828353,-53.4730751360371,12.));
#61449=CARTESIAN_POINT('Ctrl Pts',(46.2405331953889,-53.4617191477402,12.));
#61450=CARTESIAN_POINT('Ctrl Pts',(46.2226126003202,-53.4503709181178,12.));
#61451=CARTESIAN_POINT('Ctrl Pts',(46.2047455921286,-53.4390305997274,12.));
#61452=CARTESIAN_POINT('Ctrl Pts',(46.1869322656023,-53.4276983458125,12.));
#61453=CARTESIAN_POINT('Ctrl Pts',(46.1691727157134,-53.4163743101517,12.));
#61454=CARTESIAN_POINT('Ctrl Pts',(46.1514670376012,-53.4050586470436,12.));
#61455=CARTESIAN_POINT('Ctrl Pts',(46.1338153268097,-53.3937515116549,12.));
#61456=CARTESIAN_POINT('Ctrl Pts',(46.1162176794884,-53.3824530603276,12.));
#61457=CARTESIAN_POINT('Ctrl Pts',(46.0986741925656,-53.3711634508437,12.));
#61458=CARTESIAN_POINT('Ctrl Pts',(46.0811849640218,-53.3598828428546,12.));
#61459=CARTESIAN_POINT('Ctrl Pts',(46.0637500926982,-53.3486113975901,12.));
#61460=CARTESIAN_POINT('Ctrl Pts',(46.0463696777801,-53.3373492770671,12.));
#61461=CARTESIAN_POINT('Ctrl Pts',(46.02904381836,-53.326096643428,12.));
#61462=CARTESIAN_POINT('Ctrl Pts',(46.0117726129873,-53.3148536582635,12.));
#61463=CARTESIAN_POINT('Ctrl Pts',(45.9945561591453,-53.3036204818329,12.));
#61464=CARTESIAN_POINT('Ctrl Pts',(45.9773945542384,-53.292397274555,12.));
#61465=CARTESIAN_POINT('Ctrl Pts',(45.9602878967698,-53.2811841987926,12.));
#61466=CARTESIAN_POINT('Ctrl Pts',(45.9432362873008,-53.2699814203105,12.));
#61467=CARTESIAN_POINT('Ctrl Pts',(45.9262398298349,-53.2587891103866,12.));
#61468=CARTESIAN_POINT('Ctrl Pts',(45.9092986319377,-53.2476074460017,12.));
#61469=CARTESIAN_POINT('Ctrl Pts',(45.8924128018379,-53.2364366054306,12.));
#61470=CARTESIAN_POINT('Ctrl Pts',(45.8755824458722,-53.2252767643662,12.));
#61471=CARTESIAN_POINT('Ctrl Pts',(45.8588076662582,-53.2141280925439,12.));
#61472=CARTESIAN_POINT('Ctrl Pts',(45.8420885575349,-53.2029907483557,12.));
#61473=CARTESIAN_POINT('Ctrl Pts',(45.8254252099957,-53.1918648840541,12.));
#61474=CARTESIAN_POINT('Ctrl Pts',(45.8088177165089,-53.1807506560933,12.));
#61475=CARTESIAN_POINT('Ctrl Pts',(45.7922661780005,-53.1696482334487,12.));
#61476=CARTESIAN_POINT('Ctrl Pts',(45.7757707100618,-53.1585578076444,12.));
#61477=CARTESIAN_POINT('Ctrl Pts',(45.7593314474501,-53.1474795996053,12.));
#61478=CARTESIAN_POINT('Ctrl Pts',(45.7429485300823,-53.1364138384693,12.));
#61479=CARTESIAN_POINT('Ctrl Pts',(45.7266220897003,-53.1253607414872,12.));
#61480=CARTESIAN_POINT('Ctrl Pts',(45.7103522376696,-53.114320495492,12.));
#61481=CARTESIAN_POINT('Ctrl Pts',(45.694139048907,-53.1032932328857,12.));
#61482=CARTESIAN_POINT('Ctrl Pts',(45.6779825614231,-53.0922790298409,12.));
#61483=CARTESIAN_POINT('Ctrl Pts',(45.6651027439241,-53.0834781451546,12.));
#61484=CARTESIAN_POINT('Ctrl Pts',(45.6554684028145,-53.0768833804193,12.));
#61485=CARTESIAN_POINT('Ctrl Pts',(45.6490568514089,-53.0724894921849,12.));
#61486=CARTESIAN_POINT('Ctrl Pts',(45.6458539113724,-53.0702932034641,12.));
#61487=CARTESIAN_POINT('Ctrl Pts',(50.6869108458849,-54.1946543500368,0.));
#61488=CARTESIAN_POINT('Ctrl Pts',(50.6869108458849,-54.1946543500368,4.));
#61489=CARTESIAN_POINT('Ctrl Pts',(50.6869108458849,-54.1946543500368,8.));
#61490=CARTESIAN_POINT('Ctrl Pts',(50.6869108458849,-54.1946543500368,12.));
#61491=CARTESIAN_POINT('Ctrl Pts',(50.722390087302,-54.2986513683562,0.));
#61492=CARTESIAN_POINT('Ctrl Pts',(50.722390087302,-54.2986513683562,4.));
#61493=CARTESIAN_POINT('Ctrl Pts',(50.722390087302,-54.2986513683562,8.));
#61494=CARTESIAN_POINT('Ctrl Pts',(50.722390087302,-54.2986513683562,12.));
#61495=CARTESIAN_POINT('Ctrl Pts',(50.7219766588193,-54.501314566926,0.));
#61496=CARTESIAN_POINT('Ctrl Pts',(50.7219766588193,-54.501314566926,4.));
#61497=CARTESIAN_POINT('Ctrl Pts',(50.7219766588193,-54.5013145669259,7.99999999999999));
#61498=CARTESIAN_POINT('Ctrl Pts',(50.7219766588193,-54.5013145669259,12.));
#61499=CARTESIAN_POINT('Ctrl Pts',(50.6135081477654,-54.6674453828693,0.));
#61500=CARTESIAN_POINT('Ctrl Pts',(50.6135081477654,-54.6674453828693,4.));
#61501=CARTESIAN_POINT('Ctrl Pts',(50.6135081477654,-54.6674453828692,8.00000000000001));
#61502=CARTESIAN_POINT('Ctrl Pts',(50.6135081477654,-54.6674453828692,12.));
#61503=CARTESIAN_POINT('Ctrl Pts',(50.5529731960897,-54.7233670476825,0.));
#61504=CARTESIAN_POINT('Ctrl Pts',(50.5529731960897,-54.7233670476825,4.));
#61505=CARTESIAN_POINT('Ctrl Pts',(50.5529731960896,-54.7233670476824,8.));
#61506=CARTESIAN_POINT('Ctrl Pts',(50.5529731960896,-54.7233670476824,12.));
#61507=CARTESIAN_POINT('',(50.6869108458849,-54.1946543500368,0.));
#61508=CARTESIAN_POINT('',(50.5529731960899,-54.7233670476828,0.));
#61509=CARTESIAN_POINT('Ctrl Pts',(50.6869108458849,-54.1946543500368,7.52391395153922E-35));
#61510=CARTESIAN_POINT('Ctrl Pts',(50.722390087302,-54.2986513683562,7.52391395153921E-35));
#61511=CARTESIAN_POINT('Ctrl Pts',(50.7221538424548,-54.4144589103961,7.52391395153922E-35));
#61512=CARTESIAN_POINT('Ctrl Pts',(50.6866343053394,-54.5183375111702,7.52391395153922E-35));
#61513=CARTESIAN_POINT('Ctrl Pts',(50.6599946525028,-54.5962464617507,7.52391395153922E-35));
#61514=CARTESIAN_POINT('Ctrl Pts',(50.6135081477654,-54.6674453828693,7.52391395153921E-35));
#61515=CARTESIAN_POINT('Ctrl Pts',(50.5529731960897,-54.7233670476825,7.52391395153922E-35));
#61516=CARTESIAN_POINT('',(50.55297319609,-54.7233670476827,12.));
#61517=CARTESIAN_POINT('Ctrl Pts',(50.5529731960897,-54.7233670476825,0.));
#61518=CARTESIAN_POINT('Ctrl Pts',(50.5529731960897,-54.7233670476825,4.));
#61519=CARTESIAN_POINT('Ctrl Pts',(50.5529731960896,-54.7233670476824,8.));
#61520=CARTESIAN_POINT('Ctrl Pts',(50.5529731960896,-54.7233670476824,12.));
#61521=CARTESIAN_POINT('',(50.6869108458849,-54.1946543500368,12.));
#61522=CARTESIAN_POINT('Ctrl Pts',(50.5529731960896,-54.7233670476824,12.));
#61523=CARTESIAN_POINT('Ctrl Pts',(50.6135081477654,-54.6674453828692,12.));
#61524=CARTESIAN_POINT('Ctrl Pts',(50.6599946525028,-54.5962464617507,12.));
#61525=CARTESIAN_POINT('Ctrl Pts',(50.6866343053393,-54.5183375111701,12.));
#61526=CARTESIAN_POINT('Ctrl Pts',(50.7221538424547,-54.414458910396,12.));
#61527=CARTESIAN_POINT('Ctrl Pts',(50.722390087302,-54.2986513683562,12.));
#61528=CARTESIAN_POINT('Ctrl Pts',(50.6869108458849,-54.1946543500368,12.));
#61529=CARTESIAN_POINT('Ctrl Pts',(50.6869108458849,-54.1946543500368,12.));
#61530=CARTESIAN_POINT('Ctrl Pts',(50.6869108458849,-54.1946543500368,8.));
#61531=CARTESIAN_POINT('Ctrl Pts',(50.6869108458849,-54.1946543500368,4.));
#61532=CARTESIAN_POINT('Ctrl Pts',(50.6869108458849,-54.1946543500368,0.));
#61533=CARTESIAN_POINT('Origin',(2.53313958019842E-10,-2.7629675461203E-10,
0.));
#61534=CARTESIAN_POINT('Origin',(2.53313958019842E-10,-2.7629675461203E-10,
12.));
#61535=CARTESIAN_POINT('Origin',(2.53313958019842E-10,-2.7629675461203E-10,
0.));
#61536=CARTESIAN_POINT('Ctrl Pts',(45.1135644683471,-59.2875729049545,0.));
#61537=CARTESIAN_POINT('Ctrl Pts',(45.1135644683471,-59.2875729049545,4.));
#61538=CARTESIAN_POINT('Ctrl Pts',(45.1135644683471,-59.2875729049545,8.));
#61539=CARTESIAN_POINT('Ctrl Pts',(45.1135644683471,-59.2875729049545,12.));
#61540=CARTESIAN_POINT('Ctrl Pts',(45.0261193041895,-59.3541123643618,0.));
#61541=CARTESIAN_POINT('Ctrl Pts',(45.0261193041895,-59.3541123643618,4.));
#61542=CARTESIAN_POINT('Ctrl Pts',(45.0261193041895,-59.3541123643618,8.));
#61543=CARTESIAN_POINT('Ctrl Pts',(45.0261193041895,-59.3541123643618,12.));
#61544=CARTESIAN_POINT('Ctrl Pts',(44.8337211159575,-59.4177951463802,0.));
#61545=CARTESIAN_POINT('Ctrl Pts',(44.8337211159575,-59.4177951463802,4.00000000000001));
#61546=CARTESIAN_POINT('Ctrl Pts',(44.8337211159575,-59.4177951463802,8.));
#61547=CARTESIAN_POINT('Ctrl Pts',(44.8337211159575,-59.4177951463802,12.));
#61548=CARTESIAN_POINT('Ctrl Pts',(44.6418181989799,-59.3674150879748,0.));
#61549=CARTESIAN_POINT('Ctrl Pts',(44.6418181989799,-59.3674150879748,4.));
#61550=CARTESIAN_POINT('Ctrl Pts',(44.6418181989798,-59.3674150879747,8.00000000000001));
#61551=CARTESIAN_POINT('Ctrl Pts',(44.6418181989798,-59.3674150879747,12.));
#61552=CARTESIAN_POINT('Ctrl Pts',(44.5696260757423,-59.3276657444157,0.));
#61553=CARTESIAN_POINT('Ctrl Pts',(44.5696260757423,-59.3276657444157,4.));
#61554=CARTESIAN_POINT('Ctrl Pts',(44.5696260757423,-59.3276657444157,8.));
#61555=CARTESIAN_POINT('Ctrl Pts',(44.5696260757423,-59.3276657444157,12.));
#61556=CARTESIAN_POINT('',(45.1135644683471,-59.2875729049545,0.));
#61557=CARTESIAN_POINT('',(44.5696260757422,-59.3276657444159,0.));
#61558=CARTESIAN_POINT('Ctrl Pts',(45.1135644683471,-59.2875729049545,0.));
#61559=CARTESIAN_POINT('Ctrl Pts',(45.0261193041895,-59.3541123643618,0.));
#61560=CARTESIAN_POINT('Ctrl Pts',(44.9161774823427,-59.3905025255151,0.));
#61561=CARTESIAN_POINT('Ctrl Pts',(44.8063973817217,-59.3896476775505,0.));
#61562=CARTESIAN_POINT('Ctrl Pts',(44.724062306256,-59.3890065415771,0.));
#61563=CARTESIAN_POINT('Ctrl Pts',(44.6418181989799,-59.3674150879748,0.));
#61564=CARTESIAN_POINT('Ctrl Pts',(44.5696260757423,-59.3276657444157,0.));
#61565=CARTESIAN_POINT('',(44.5696260757422,-59.3276657444159,12.));
#61566=CARTESIAN_POINT('Ctrl Pts',(44.5696260757423,-59.3276657444157,0.));
#61567=CARTESIAN_POINT('Ctrl Pts',(44.5696260757423,-59.3276657444157,4.));
#61568=CARTESIAN_POINT('Ctrl Pts',(44.5696260757423,-59.3276657444157,8.));
#61569=CARTESIAN_POINT('Ctrl Pts',(44.5696260757423,-59.3276657444157,12.));
#61570=CARTESIAN_POINT('',(45.1135644683471,-59.2875729049545,12.));
#61571=CARTESIAN_POINT('Ctrl Pts',(44.5696260757423,-59.3276657444157,12.));
#61572=CARTESIAN_POINT('Ctrl Pts',(44.6418181989798,-59.3674150879747,12.));
#61573=CARTESIAN_POINT('Ctrl Pts',(44.724062306256,-59.3890065415771,12.));
#61574=CARTESIAN_POINT('Ctrl Pts',(44.8063973817217,-59.3896476775505,12.));
#61575=CARTESIAN_POINT('Ctrl Pts',(44.9161774823427,-59.3905025255151,12.));
#61576=CARTESIAN_POINT('Ctrl Pts',(45.0261193041895,-59.3541123643618,12.));
#61577=CARTESIAN_POINT('Ctrl Pts',(45.1135644683471,-59.2875729049545,12.));
#61578=CARTESIAN_POINT('Ctrl Pts',(45.1135644683471,-59.2875729049545,12.));
#61579=CARTESIAN_POINT('Ctrl Pts',(45.1135644683471,-59.2875729049545,8.));
#61580=CARTESIAN_POINT('Ctrl Pts',(45.1135644683471,-59.2875729049545,4.));
#61581=CARTESIAN_POINT('Ctrl Pts',(45.1135644683471,-59.2875729049545,0.));
#61582=CARTESIAN_POINT('Ctrl Pts',(40.8467768343956,-56.8466430164621,0.));
#61583=CARTESIAN_POINT('Ctrl Pts',(40.8467768343956,-56.8466430164621,12.));
#61584=CARTESIAN_POINT('Ctrl Pts',(40.8497761671036,-56.8491101022591,0.));
#61585=CARTESIAN_POINT('Ctrl Pts',(40.8497761671036,-56.8491101022591,12.));
#61586=CARTESIAN_POINT('Ctrl Pts',(40.8557803680278,-56.8540460739472,0.));
#61587=CARTESIAN_POINT('Ctrl Pts',(40.8557803680278,-56.8540460739472,12.));
#61588=CARTESIAN_POINT('Ctrl Pts',(40.864803275942,-56.8614554317668,0.));
#61589=CARTESIAN_POINT('Ctrl Pts',(40.864803275942,-56.8614554317668,12.));
#61590=CARTESIAN_POINT('Ctrl Pts',(40.8768670342052,-56.8713453764905,0.));
#61591=CARTESIAN_POINT('Ctrl Pts',(40.8768670342052,-56.8713453764905,12.));
#61592=CARTESIAN_POINT('Ctrl Pts',(40.8920020903293,-56.8837257978343,0.));
#61593=CARTESIAN_POINT('Ctrl Pts',(40.8920020903293,-56.8837257978343,12.));
#61594=CARTESIAN_POINT('Ctrl Pts',(40.9071924937508,-56.8961241708861,0.));
#61595=CARTESIAN_POINT('Ctrl Pts',(40.9071924937508,-56.8961241708861,12.));
#61596=CARTESIAN_POINT('Ctrl Pts',(40.9224382132427,-56.9085404164502,0.));
#61597=CARTESIAN_POINT('Ctrl Pts',(40.9224382132427,-56.9085404164502,12.));
#61598=CARTESIAN_POINT('Ctrl Pts',(40.9377391857129,-56.9209743960992,0.));
#61599=CARTESIAN_POINT('Ctrl Pts',(40.9377391857129,-56.9209743960992,12.));
#61600=CARTESIAN_POINT('Ctrl Pts',(40.9530953165031,-56.9334259140049,0.));
#61601=CARTESIAN_POINT('Ctrl Pts',(40.9530953165031,-56.9334259140049,12.));
#61602=CARTESIAN_POINT('Ctrl Pts',(40.9685064933074,-56.9458947422608,0.));
#61603=CARTESIAN_POINT('Ctrl Pts',(40.9685064933074,-56.9458947422608,12.));
#61604=CARTESIAN_POINT('Ctrl Pts',(40.9839725967121,-56.9583806404069,0.));
#61605=CARTESIAN_POINT('Ctrl Pts',(40.9839725967121,-56.9583806404069,12.));
#61606=CARTESIAN_POINT('Ctrl Pts',(40.9994935117276,-56.9708833766137,0.));
#61607=CARTESIAN_POINT('Ctrl Pts',(40.9994935117276,-56.9708833766137,12.));
#61608=CARTESIAN_POINT('Ctrl Pts',(41.0150691398947,-56.9834027500117,0.));
#61609=CARTESIAN_POINT('Ctrl Pts',(41.0150691398947,-56.9834027500117,12.));
#61610=CARTESIAN_POINT('Ctrl Pts',(41.0306993953989,-56.995938583472,0.));
#61611=CARTESIAN_POINT('Ctrl Pts',(41.0306993953989,-56.995938583472,12.));
#61612=CARTESIAN_POINT('Ctrl Pts',(41.0463841993608,-57.008490713042,0.));
#61613=CARTESIAN_POINT('Ctrl Pts',(41.0463841993608,-57.008490713042,12.));
#61614=CARTESIAN_POINT('Ctrl Pts',(41.0621234751007,-57.0210589791788,0.));
#61615=CARTESIAN_POINT('Ctrl Pts',(41.0621234751007,-57.0210589791788,12.));
#61616=CARTESIAN_POINT('Ctrl Pts',(41.0779171422438,-57.0336432158536,0.));
#61617=CARTESIAN_POINT('Ctrl Pts',(41.0779171422438,-57.0336432158536,12.));
#61618=CARTESIAN_POINT('Ctrl Pts',(41.0937651137549,-57.046243245068,0.));
#61619=CARTESIAN_POINT('Ctrl Pts',(41.0937651137549,-57.046243245068,12.));
#61620=CARTESIAN_POINT('Ctrl Pts',(41.1096672990148,-57.0588588825298,0.));
#61621=CARTESIAN_POINT('Ctrl Pts',(41.1096672990148,-57.0588588825298,12.));
#61622=CARTESIAN_POINT('Ctrl Pts',(41.1256236057443,-57.0714899412099,0.));
#61623=CARTESIAN_POINT('Ctrl Pts',(41.1256236057443,-57.0714899412099,12.));
#61624=CARTESIAN_POINT('Ctrl Pts',(41.1416339422117,-57.084136235426,0.));
#61625=CARTESIAN_POINT('Ctrl Pts',(41.1416339422117,-57.084136235426,12.));
#61626=CARTESIAN_POINT('Ctrl Pts',(41.1576982197375,-57.0967975854874,0.));
#61627=CARTESIAN_POINT('Ctrl Pts',(41.1576982197375,-57.0967975854874,12.));
#61628=CARTESIAN_POINT('Ctrl Pts',(41.1738163525902,-57.1094738174957,0.));
#61629=CARTESIAN_POINT('Ctrl Pts',(41.1738163525902,-57.1094738174957,12.));
#61630=CARTESIAN_POINT('Ctrl Pts',(41.1899882567923,-57.1221647611207,0.));
#61631=CARTESIAN_POINT('Ctrl Pts',(41.1899882567923,-57.1221647611207,12.));
#61632=CARTESIAN_POINT('Ctrl Pts',(41.2062138492915,-57.1348702480647,0.));
#61633=CARTESIAN_POINT('Ctrl Pts',(41.2062138492915,-57.1348702480647,12.));
#61634=CARTESIAN_POINT('Ctrl Pts',(41.222493046943,-57.147590110182,0.));
#61635=CARTESIAN_POINT('Ctrl Pts',(41.222493046943,-57.147590110182,12.));
#61636=CARTESIAN_POINT('Ctrl Pts',(41.2388257656559,-57.1603241779077,0.));
#61637=CARTESIAN_POINT('Ctrl Pts',(41.2388257656559,-57.1603241779077,12.));
#61638=CARTESIAN_POINT('Ctrl Pts',(41.2552119208466,-57.17307228108,0.));
#61639=CARTESIAN_POINT('Ctrl Pts',(41.2552119208466,-57.17307228108,12.));
#61640=CARTESIAN_POINT('Ctrl Pts',(41.2716514278276,-57.1858342496538,0.));
#61641=CARTESIAN_POINT('Ctrl Pts',(41.2716514278276,-57.1858342496538,12.));
#61642=CARTESIAN_POINT('Ctrl Pts',(41.2881442021863,-57.1986099143983,0.));
#61643=CARTESIAN_POINT('Ctrl Pts',(41.2881442021863,-57.1986099143983,12.));
#61644=CARTESIAN_POINT('Ctrl Pts',(41.3046901602293,-57.2113991077302,0.));
#61645=CARTESIAN_POINT('Ctrl Pts',(41.3046901602293,-57.2113991077302,12.));
#61646=CARTESIAN_POINT('Ctrl Pts',(41.321289219149,-57.2242016640198,0.));
#61647=CARTESIAN_POINT('Ctrl Pts',(41.321289219149,-57.2242016640198,12.));
#61648=CARTESIAN_POINT('Ctrl Pts',(41.3379412967875,-57.2370174191401,0.));
#61649=CARTESIAN_POINT('Ctrl Pts',(41.3379412967875,-57.2370174191401,12.));
#61650=CARTESIAN_POINT('Ctrl Pts',(41.3546463114885,-57.2498462101879,0.));
#61651=CARTESIAN_POINT('Ctrl Pts',(41.3546463114885,-57.2498462101879,12.));
#61652=CARTESIAN_POINT('Ctrl Pts',(41.3714041819224,-57.2626878751596,0.));
#61653=CARTESIAN_POINT('Ctrl Pts',(41.3714041819224,-57.2626878751596,12.));
#61654=CARTESIAN_POINT('Ctrl Pts',(41.3882148268814,-57.2755422525844,0.));
#61655=CARTESIAN_POINT('Ctrl Pts',(41.3882148268814,-57.2755422525844,12.));
#61656=CARTESIAN_POINT('Ctrl Pts',(41.4050781652938,-57.2884091815406,0.));
#61657=CARTESIAN_POINT('Ctrl Pts',(41.4050781652938,-57.2884091815406,12.));
#61658=CARTESIAN_POINT('Ctrl Pts',(41.4219941163163,-57.3012885018151,0.));
#61659=CARTESIAN_POINT('Ctrl Pts',(41.4219941163163,-57.3012885018151,12.));
#61660=CARTESIAN_POINT('Ctrl Pts',(41.4389625993948,-57.3141800540137,0.));
#61661=CARTESIAN_POINT('Ctrl Pts',(41.4389625993948,-57.3141800540137,12.));
#61662=CARTESIAN_POINT('Ctrl Pts',(41.4559835343328,-57.3270836796911,0.));
#61663=CARTESIAN_POINT('Ctrl Pts',(41.4559835343328,-57.3270836796911,12.));
#61664=CARTESIAN_POINT('Ctrl Pts',(41.4730568413518,-57.3399992214717,0.));
#61665=CARTESIAN_POINT('Ctrl Pts',(41.4730568413518,-57.3399992214717,12.));
#61666=CARTESIAN_POINT('Ctrl Pts',(41.4901824410637,-57.3529265229835,0.));
#61667=CARTESIAN_POINT('Ctrl Pts',(41.4901824410637,-57.3529265229835,12.));
#61668=CARTESIAN_POINT('Ctrl Pts',(41.5073602544396,-57.3658654287937,0.));
#61669=CARTESIAN_POINT('Ctrl Pts',(41.5073602544396,-57.3658654287937,12.));
#61670=CARTESIAN_POINT('Ctrl Pts',(41.5245902027771,-57.3788157843454,0.));
#61671=CARTESIAN_POINT('Ctrl Pts',(41.5245902027771,-57.3788157843454,12.));
#61672=CARTESIAN_POINT('Ctrl Pts',(41.5418722076572,-57.3917774358863,0.));
#61673=CARTESIAN_POINT('Ctrl Pts',(41.5418722076572,-57.3917774358863,12.));
#61674=CARTESIAN_POINT('Ctrl Pts',(41.5592061909176,-57.4047502304231,0.));
#61675=CARTESIAN_POINT('Ctrl Pts',(41.5592061909176,-57.4047502304231,12.));
#61676=CARTESIAN_POINT('Ctrl Pts',(41.5765920746777,-57.4177340157508,0.));
#61677=CARTESIAN_POINT('Ctrl Pts',(41.5765920746777,-57.4177340157508,12.));
#61678=CARTESIAN_POINT('Ctrl Pts',(41.5940297813477,-57.4307286404662,0.));
#61679=CARTESIAN_POINT('Ctrl Pts',(41.5940297813477,-57.4307286404662,12.));
#61680=CARTESIAN_POINT('Ctrl Pts',(41.6115192336388,-57.4437339539841,0.));
#61681=CARTESIAN_POINT('Ctrl Pts',(41.6115192336388,-57.4437339539841,12.));
#61682=CARTESIAN_POINT('Ctrl Pts',(41.6290603545666,-57.4567498065562,0.));
#61683=CARTESIAN_POINT('Ctrl Pts',(41.6290603545666,-57.4567498065562,12.));
#61684=CARTESIAN_POINT('Ctrl Pts',(41.6466530674515,-57.4697760492683,0.));
#61685=CARTESIAN_POINT('Ctrl Pts',(41.6466530674515,-57.4697760492683,12.));
#61686=CARTESIAN_POINT('Ctrl Pts',(41.6642972959165,-57.4828125340218,0.));
#61687=CARTESIAN_POINT('Ctrl Pts',(41.6642972959165,-57.4828125340218,12.));
#61688=CARTESIAN_POINT('Ctrl Pts',(41.6819929638797,-57.4958591135165,0.));
#61689=CARTESIAN_POINT('Ctrl Pts',(41.6819929638797,-57.4958591135165,12.));
#61690=CARTESIAN_POINT('Ctrl Pts',(41.6997399955447,-57.5089156412343,0.));
#61691=CARTESIAN_POINT('Ctrl Pts',(41.6997399955447,-57.5089156412343,12.));
#61692=CARTESIAN_POINT('Ctrl Pts',(41.7175383153821,-57.5219819714171,0.));
#61693=CARTESIAN_POINT('Ctrl Pts',(41.7175383153821,-57.5219819714171,12.));
#61694=CARTESIAN_POINT('Ctrl Pts',(41.7353878481337,-57.5350579590649,0.));
#61695=CARTESIAN_POINT('Ctrl Pts',(41.7353878481337,-57.5350579590649,12.));
#61696=CARTESIAN_POINT('Ctrl Pts',(41.7532885188175,-57.5481434599335,0.));
#61697=CARTESIAN_POINT('Ctrl Pts',(41.7532885188175,-57.5481434599335,12.));
#61698=CARTESIAN_POINT('Ctrl Pts',(41.7712402527273,-57.561238330532,0.));
#61699=CARTESIAN_POINT('Ctrl Pts',(41.7712402527273,-57.561238330532,12.));
#61700=CARTESIAN_POINT('Ctrl Pts',(41.7892429754297,-57.5743424281204,0.));
#61701=CARTESIAN_POINT('Ctrl Pts',(41.7892429754297,-57.5743424281204,12.));
#61702=CARTESIAN_POINT('Ctrl Pts',(41.8072966127558,-57.5874556107056,0.));
#61703=CARTESIAN_POINT('Ctrl Pts',(41.8072966127558,-57.5874556107056,12.));
#61704=CARTESIAN_POINT('Ctrl Pts',(41.8254010908051,-57.6005777370349,0.));
#61705=CARTESIAN_POINT('Ctrl Pts',(41.8254010908051,-57.6005777370349,12.));
#61706=CARTESIAN_POINT('Ctrl Pts',(41.8435563359456,-57.6137086665882,0.));
#61707=CARTESIAN_POINT('Ctrl Pts',(41.8435563359456,-57.6137086665882,12.));
#61708=CARTESIAN_POINT('Ctrl Pts',(41.8617622748108,-57.6268482595702,0.));
#61709=CARTESIAN_POINT('Ctrl Pts',(41.8617622748108,-57.6268482595702,12.));
#61710=CARTESIAN_POINT('Ctrl Pts',(41.8800188342909,-57.6399963769003,0.));
#61711=CARTESIAN_POINT('Ctrl Pts',(41.8800188342909,-57.6399963769003,12.));
#61712=CARTESIAN_POINT('Ctrl Pts',(41.8983259415245,-57.6531528802059,0.));
#61713=CARTESIAN_POINT('Ctrl Pts',(41.8983259415245,-57.6531528802059,12.));
#61714=CARTESIAN_POINT('Ctrl Pts',(41.9166835239046,-57.6663176318176,0.));
#61715=CARTESIAN_POINT('Ctrl Pts',(41.9166835239046,-57.6663176318176,12.));
#61716=CARTESIAN_POINT('Ctrl Pts',(41.9350915090791,-57.6794904947641,0.));
#61717=CARTESIAN_POINT('Ctrl Pts',(41.9350915090791,-57.6794904947641,12.));
#61718=CARTESIAN_POINT('Ctrl Pts',(41.9535498249489,-57.6926713327674,0.));
#61719=CARTESIAN_POINT('Ctrl Pts',(41.9535498249489,-57.6926713327674,12.));
#61720=CARTESIAN_POINT('Ctrl Pts',(41.9720583996601,-57.7058600102365,0.));
#61721=CARTESIAN_POINT('Ctrl Pts',(41.9720583996601,-57.7058600102365,12.));
#61722=CARTESIAN_POINT('Ctrl Pts',(41.9906171615975,-57.7190563922614,0.));
#61723=CARTESIAN_POINT('Ctrl Pts',(41.9906171615975,-57.7190563922614,12.));
#61724=CARTESIAN_POINT('Ctrl Pts',(42.0092260393911,-57.7322603446086,0.));
#61725=CARTESIAN_POINT('Ctrl Pts',(42.0092260393911,-57.7322603446086,12.));
#61726=CARTESIAN_POINT('Ctrl Pts',(42.0278849619156,-57.7454717337151,0.));
#61727=CARTESIAN_POINT('Ctrl Pts',(42.0278849619156,-57.7454717337151,12.));
#61728=CARTESIAN_POINT('Ctrl Pts',(42.0465938582878,-57.7586904266828,0.));
#61729=CARTESIAN_POINT('Ctrl Pts',(42.0465938582878,-57.7586904266828,12.));
#61730=CARTESIAN_POINT('Ctrl Pts',(42.0653526578571,-57.7719162912721,0.));
#61731=CARTESIAN_POINT('Ctrl Pts',(42.0653526578571,-57.7719162912721,12.));
#61732=CARTESIAN_POINT('Ctrl Pts',(42.0841612902018,-57.7851491958954,0.));
#61733=CARTESIAN_POINT('Ctrl Pts',(42.0841612902018,-57.7851491958954,12.));
#61734=CARTESIAN_POINT('Ctrl Pts',(42.1030196851344,-57.798389009613,0.));
#61735=CARTESIAN_POINT('Ctrl Pts',(42.1030196851344,-57.798389009613,12.));
#61736=CARTESIAN_POINT('Ctrl Pts',(42.121927772701,-57.8116356021274,0.));
#61737=CARTESIAN_POINT('Ctrl Pts',(42.121927772701,-57.8116356021274,12.));
#61738=CARTESIAN_POINT('Ctrl Pts',(42.1408854831792,-57.8248888437787,0.));
#61739=CARTESIAN_POINT('Ctrl Pts',(42.1408854831792,-57.8248888437787,12.));
#61740=CARTESIAN_POINT('Ctrl Pts',(42.1598927470671,-57.8381486055376,0.));
#61741=CARTESIAN_POINT('Ctrl Pts',(42.1598927470671,-57.8381486055376,12.));
#61742=CARTESIAN_POINT('Ctrl Pts',(42.1789494950824,-57.8514147590012,0.));
#61743=CARTESIAN_POINT('Ctrl Pts',(42.1789494950824,-57.8514147590012,12.));
#61744=CARTESIAN_POINT('Ctrl Pts',(42.1980556581689,-57.86468717639,0.));
#61745=CARTESIAN_POINT('Ctrl Pts',(42.1980556581689,-57.86468717639,12.));
#61746=CARTESIAN_POINT('Ctrl Pts',(42.2172111674946,-57.8779657305422,0.));
#61747=CARTESIAN_POINT('Ctrl Pts',(42.2172111674946,-57.8779657305422,12.));
#61748=CARTESIAN_POINT('Ctrl Pts',(42.2364159544492,-57.8912502949084,0.));
#61749=CARTESIAN_POINT('Ctrl Pts',(42.2364159544492,-57.8912502949084,12.));
#61750=CARTESIAN_POINT('Ctrl Pts',(42.2556699506332,-57.9045407435447,0.));
#61751=CARTESIAN_POINT('Ctrl Pts',(42.2556699506332,-57.9045407435447,12.));
#61752=CARTESIAN_POINT('Ctrl Pts',(42.274973087857,-57.9178369511084,0.));
#61753=CARTESIAN_POINT('Ctrl Pts',(42.274973087857,-57.9178369511084,12.));
#61754=CARTESIAN_POINT('Ctrl Pts',(42.2943252981471,-57.9311387928541,0.));
#61755=CARTESIAN_POINT('Ctrl Pts',(42.2943252981471,-57.9311387928541,12.));
#61756=CARTESIAN_POINT('Ctrl Pts',(42.3137265137446,-57.9444461446292,0.));
#61757=CARTESIAN_POINT('Ctrl Pts',(42.3137265137446,-57.9444461446292,12.));
#61758=CARTESIAN_POINT('Ctrl Pts',(42.3331766671028,-57.9577588828693,0.));
#61759=CARTESIAN_POINT('Ctrl Pts',(42.3331766671028,-57.9577588828693,12.));
#61760=CARTESIAN_POINT('Ctrl Pts',(42.3526756908764,-57.9710768845923,0.));
#61761=CARTESIAN_POINT('Ctrl Pts',(42.3526756908764,-57.9710768845923,12.));
#61762=CARTESIAN_POINT('Ctrl Pts',(42.3722235179216,-57.9844000273936,0.));
#61763=CARTESIAN_POINT('Ctrl Pts',(42.3722235179216,-57.9844000273936,12.));
#61764=CARTESIAN_POINT('Ctrl Pts',(42.3918200813025,-57.9977281894437,0.));
#61765=CARTESIAN_POINT('Ctrl Pts',(42.3918200813025,-57.9977281894437,12.));
#61766=CARTESIAN_POINT('Ctrl Pts',(42.4114653142891,-58.011061249483,0.));
#61767=CARTESIAN_POINT('Ctrl Pts',(42.4114653142891,-58.011061249483,12.));
#61768=CARTESIAN_POINT('Ctrl Pts',(42.4311591503551,-58.0243990868175,0.));
#61769=CARTESIAN_POINT('Ctrl Pts',(42.4311591503551,-58.0243990868175,12.));
#61770=CARTESIAN_POINT('Ctrl Pts',(42.4509015231668,-58.0377415813132,0.));
#61771=CARTESIAN_POINT('Ctrl Pts',(42.4509015231668,-58.0377415813132,12.));
#61772=CARTESIAN_POINT('Ctrl Pts',(42.4706923665838,-58.0510886133917,0.));
#61773=CARTESIAN_POINT('Ctrl Pts',(42.4706923665838,-58.0510886133917,12.));
#61774=CARTESIAN_POINT('Ctrl Pts',(42.490531614665,-58.064440064027,0.));
#61775=CARTESIAN_POINT('Ctrl Pts',(42.490531614665,-58.064440064027,12.));
#61776=CARTESIAN_POINT('Ctrl Pts',(42.5104192016664,-58.0777958147404,0.));
#61777=CARTESIAN_POINT('Ctrl Pts',(42.5104192016664,-58.0777958147404,12.));
#61778=CARTESIAN_POINT('Ctrl Pts',(42.5303550620388,-58.0911557475967,0.));
#61779=CARTESIAN_POINT('Ctrl Pts',(42.5303550620388,-58.0911557475967,12.));
#61780=CARTESIAN_POINT('Ctrl Pts',(42.5503391304183,-58.1045197452003,0.));
#61781=CARTESIAN_POINT('Ctrl Pts',(42.5503391304183,-58.1045197452003,12.));
#61782=CARTESIAN_POINT('Ctrl Pts',(42.5703713416263,-58.1178876906905,0.));
#61783=CARTESIAN_POINT('Ctrl Pts',(42.5703713416263,-58.1178876906905,12.));
#61784=CARTESIAN_POINT('Ctrl Pts',(42.5904516306759,-58.1312594677383,0.));
#61785=CARTESIAN_POINT('Ctrl Pts',(42.5904516306759,-58.1312594677383,12.));
#61786=CARTESIAN_POINT('Ctrl Pts',(42.6105799327697,-58.1446349605419,0.));
#61787=CARTESIAN_POINT('Ctrl Pts',(42.6105799327697,-58.1446349605419,12.));
#61788=CARTESIAN_POINT('Ctrl Pts',(42.6307561832978,-58.158014053823,0.));
#61789=CARTESIAN_POINT('Ctrl Pts',(42.6307561832978,-58.158014053823,12.));
#61790=CARTESIAN_POINT('Ctrl Pts',(42.650980317827,-58.1713966328217,0.));
#61791=CARTESIAN_POINT('Ctrl Pts',(42.650980317827,-58.1713966328217,12.));
#61792=CARTESIAN_POINT('Ctrl Pts',(42.6712522721021,-58.1847825832932,0.));
#61793=CARTESIAN_POINT('Ctrl Pts',(42.6712522721021,-58.1847825832932,12.));
#61794=CARTESIAN_POINT('Ctrl Pts',(42.6915719820517,-58.1981717915043,0.));
#61795=CARTESIAN_POINT('Ctrl Pts',(42.6915719820517,-58.1981717915043,12.));
#61796=CARTESIAN_POINT('Ctrl Pts',(42.7119393837867,-58.2115641442302,0.));
#61797=CARTESIAN_POINT('Ctrl Pts',(42.7119393837867,-58.2115641442302,12.));
#61798=CARTESIAN_POINT('Ctrl Pts',(42.7323544135983,-58.2249595287497,0.));
#61799=CARTESIAN_POINT('Ctrl Pts',(42.7323544135983,-58.2249595287497,12.));
#61800=CARTESIAN_POINT('Ctrl Pts',(42.7528170079482,-58.238357832842,0.));
#61801=CARTESIAN_POINT('Ctrl Pts',(42.7528170079482,-58.238357832842,12.));
#61802=CARTESIAN_POINT('Ctrl Pts',(42.7733271034679,-58.2517589447818,0.));
#61803=CARTESIAN_POINT('Ctrl Pts',(42.7733271034679,-58.2517589447818,12.));
#61804=CARTESIAN_POINT('Ctrl Pts',(42.7938846369651,-58.2651627533368,0.));
#61805=CARTESIAN_POINT('Ctrl Pts',(42.7938846369651,-58.2651627533368,12.));
#61806=CARTESIAN_POINT('Ctrl Pts',(42.8144895454234,-58.278569147764,0.));
#61807=CARTESIAN_POINT('Ctrl Pts',(42.8144895454234,-58.278569147764,12.));
#61808=CARTESIAN_POINT('Ctrl Pts',(42.8351417659998,-58.2919780178063,0.));
#61809=CARTESIAN_POINT('Ctrl Pts',(42.8351417659998,-58.2919780178063,12.));
#61810=CARTESIAN_POINT('Ctrl Pts',(42.8558412360154,-58.305389253689,0.));
#61811=CARTESIAN_POINT('Ctrl Pts',(42.8558412360154,-58.305389253689,12.));
#61812=CARTESIAN_POINT('Ctrl Pts',(42.8765878929545,-58.3188027461157,0.));
#61813=CARTESIAN_POINT('Ctrl Pts',(42.8765878929545,-58.3188027461157,12.));
#61814=CARTESIAN_POINT('Ctrl Pts',(42.8973816744703,-58.3322183862647,0.));
#61815=CARTESIAN_POINT('Ctrl Pts',(42.8973816744703,-58.3322183862647,12.));
#61816=CARTESIAN_POINT('Ctrl Pts',(42.9182225183851,-58.3456360657861,0.));
#61817=CARTESIAN_POINT('Ctrl Pts',(42.9182225183851,-58.3456360657861,12.));
#61818=CARTESIAN_POINT('Ctrl Pts',(42.9391103626881,-58.3590556767981,0.));
#61819=CARTESIAN_POINT('Ctrl Pts',(42.9391103626881,-58.3590556767981,12.));
#61820=CARTESIAN_POINT('Ctrl Pts',(42.9600451455267,-58.3724771118835,0.));
#61821=CARTESIAN_POINT('Ctrl Pts',(42.9600451455267,-58.3724771118835,12.));
#61822=CARTESIAN_POINT('Ctrl Pts',(42.9810268052043,-58.3859002640871,0.));
#61823=CARTESIAN_POINT('Ctrl Pts',(42.9810268052043,-58.3859002640871,12.));
#61824=CARTESIAN_POINT('Ctrl Pts',(43.002055280187,-58.3993250269115,0.));
#61825=CARTESIAN_POINT('Ctrl Pts',(43.002055280187,-58.3993250269115,12.));
#61826=CARTESIAN_POINT('Ctrl Pts',(43.0231305091033,-58.4127512943144,0.));
#61827=CARTESIAN_POINT('Ctrl Pts',(43.0231305091033,-58.4127512943144,12.));
#61828=CARTESIAN_POINT('Ctrl Pts',(43.0442524307432,-58.4261789607055,0.));
#61829=CARTESIAN_POINT('Ctrl Pts',(43.0442524307432,-58.4261789607055,12.));
#61830=CARTESIAN_POINT('Ctrl Pts',(43.0654209840502,-58.4396079209438,0.));
#61831=CARTESIAN_POINT('Ctrl Pts',(43.0654209840502,-58.4396079209438,12.));
#61832=CARTESIAN_POINT('Ctrl Pts',(43.0866361081166,-58.4530380703335,0.));
#61833=CARTESIAN_POINT('Ctrl Pts',(43.0866361081166,-58.4530380703335,12.));
#61834=CARTESIAN_POINT('Ctrl Pts',(43.1078977421908,-58.4664693046206,0.));
#61835=CARTESIAN_POINT('Ctrl Pts',(43.1078977421908,-58.4664693046206,12.));
#61836=CARTESIAN_POINT('Ctrl Pts',(43.1292058256774,-58.4799015199904,0.));
#61837=CARTESIAN_POINT('Ctrl Pts',(43.1292058256774,-58.4799015199904,12.));
#61838=CARTESIAN_POINT('Ctrl Pts',(43.1505602981366,-58.4933346130638,0.));
#61839=CARTESIAN_POINT('Ctrl Pts',(43.1505602981366,-58.4933346130638,12.));
#61840=CARTESIAN_POINT('Ctrl Pts',(43.1719610992772,-58.5067684808946,0.));
#61841=CARTESIAN_POINT('Ctrl Pts',(43.1719610992772,-58.5067684808946,12.));
#61842=CARTESIAN_POINT('Ctrl Pts',(43.1934081689504,-58.5202030209667,0.));
#61843=CARTESIAN_POINT('Ctrl Pts',(43.1934081689504,-58.5202030209667,12.));
#61844=CARTESIAN_POINT('Ctrl Pts',(43.214901447157,-58.5336381311911,0.));
#61845=CARTESIAN_POINT('Ctrl Pts',(43.214901447157,-58.5336381311911,12.));
#61846=CARTESIAN_POINT('Ctrl Pts',(43.2364408740489,-58.5470737099027,0.));
#61847=CARTESIAN_POINT('Ctrl Pts',(43.2364408740489,-58.5470737099027,12.));
#61848=CARTESIAN_POINT('Ctrl Pts',(43.2580263899278,-58.5605096558578,0.));
#61849=CARTESIAN_POINT('Ctrl Pts',(43.2580263899278,-58.5605096558578,12.));
#61850=CARTESIAN_POINT('Ctrl Pts',(43.2796579352405,-58.5739458682317,0.));
#61851=CARTESIAN_POINT('Ctrl Pts',(43.2796579352405,-58.5739458682317,12.));
#61852=CARTESIAN_POINT('Ctrl Pts',(43.3013354505708,-58.5873822466163,0.));
#61853=CARTESIAN_POINT('Ctrl Pts',(43.3013354505708,-58.5873822466163,12.));
#61854=CARTESIAN_POINT('Ctrl Pts',(43.3230588766456,-58.6008186910166,0.));
#61855=CARTESIAN_POINT('Ctrl Pts',(43.3230588766456,-58.6008186910166,12.));
#61856=CARTESIAN_POINT('Ctrl Pts',(43.3448281543375,-58.6142551018473,0.));
#61857=CARTESIAN_POINT('Ctrl Pts',(43.3448281543375,-58.6142551018473,12.));
#61858=CARTESIAN_POINT('Ctrl Pts',(43.3666432246635,-58.627691379929,0.));
#61859=CARTESIAN_POINT('Ctrl Pts',(43.3666432246635,-58.627691379929,12.));
#61860=CARTESIAN_POINT('Ctrl Pts',(43.3885040287808,-58.6411274264854,0.));
#61861=CARTESIAN_POINT('Ctrl Pts',(43.3885040287808,-58.6411274264854,12.));
#61862=CARTESIAN_POINT('Ctrl Pts',(43.4104105079766,-58.6545631431388,0.));
#61863=CARTESIAN_POINT('Ctrl Pts',(43.4104105079766,-58.6545631431388,12.));
#61864=CARTESIAN_POINT('Ctrl Pts',(43.4323626036736,-58.6679984319095,0.));
#61865=CARTESIAN_POINT('Ctrl Pts',(43.4323626036736,-58.6679984319095,12.));
#61866=CARTESIAN_POINT('Ctrl Pts',(43.4543602574352,-58.6814331952138,0.));
#61867=CARTESIAN_POINT('Ctrl Pts',(43.4543602574352,-58.6814331952138,12.));
#61868=CARTESIAN_POINT('Ctrl Pts',(43.4764034109655,-58.6948673358639,0.));
#61869=CARTESIAN_POINT('Ctrl Pts',(43.4764034109655,-58.6948673358639,12.));
#61870=CARTESIAN_POINT('Ctrl Pts',(43.4984920061071,-58.708300757066,0.));
#61871=CARTESIAN_POINT('Ctrl Pts',(43.4984920061071,-58.708300757066,12.));
#61872=CARTESIAN_POINT('Ctrl Pts',(43.5206259848333,-58.7217333624206,0.));
#61873=CARTESIAN_POINT('Ctrl Pts',(43.5206259848333,-58.7217333624206,12.));
#61874=CARTESIAN_POINT('Ctrl Pts',(43.5428052892483,-58.7351650559176,0.));
#61875=CARTESIAN_POINT('Ctrl Pts',(43.5428052892483,-58.7351650559176,12.));
#61876=CARTESIAN_POINT('Ctrl Pts',(43.5650298615912,-58.7485957419296,0.));
#61877=CARTESIAN_POINT('Ctrl Pts',(43.5650298615912,-58.7485957419296,12.));
#61878=CARTESIAN_POINT('Ctrl Pts',(43.5872996442343,-58.7620253252059,0.));
#61879=CARTESIAN_POINT('Ctrl Pts',(43.5872996442343,-58.7620253252059,12.));
#61880=CARTESIAN_POINT('Ctrl Pts',(43.6096145796798,-58.7754537108672,0.));
#61881=CARTESIAN_POINT('Ctrl Pts',(43.6096145796798,-58.7754537108672,12.));
#61882=CARTESIAN_POINT('Ctrl Pts',(43.6319746105488,-58.7888808043976,0.));
#61883=CARTESIAN_POINT('Ctrl Pts',(43.6319746105488,-58.7888808043976,12.));
#61884=CARTESIAN_POINT('Ctrl Pts',(43.6543796795797,-58.8023065116446,0.));
#61885=CARTESIAN_POINT('Ctrl Pts',(43.6543796795797,-58.8023065116446,12.));
#61886=CARTESIAN_POINT('Ctrl Pts',(43.6768297296403,-58.8157307388247,0.));
#61887=CARTESIAN_POINT('Ctrl Pts',(43.6768297296403,-58.8157307388247,12.));
#61888=CARTESIAN_POINT('Ctrl Pts',(43.6993247037318,-58.8291533925299,0.));
#61889=CARTESIAN_POINT('Ctrl Pts',(43.6993247037318,-58.8291533925299,12.));
#61890=CARTESIAN_POINT('Ctrl Pts',(43.7218645449921,-58.8425743797325,0.));
#61891=CARTESIAN_POINT('Ctrl Pts',(43.7218645449921,-58.8425743797325,12.));
#61892=CARTESIAN_POINT('Ctrl Pts',(43.7444491966935,-58.8559936077933,0.));
#61893=CARTESIAN_POINT('Ctrl Pts',(43.7444491966935,-58.8559936077933,12.));
#61894=CARTESIAN_POINT('Ctrl Pts',(43.7670786022392,-58.8694109844636,0.));
#61895=CARTESIAN_POINT('Ctrl Pts',(43.7670786022392,-58.8694109844636,12.));
#61896=CARTESIAN_POINT('Ctrl Pts',(43.7897527051599,-58.882826417861,0.));
#61897=CARTESIAN_POINT('Ctrl Pts',(43.7897527051599,-58.882826417861,12.));
#61898=CARTESIAN_POINT('Ctrl Pts',(43.812471449107,-58.8962398164486,0.));
#61899=CARTESIAN_POINT('Ctrl Pts',(43.812471449107,-58.8962398164486,12.));
#61900=CARTESIAN_POINT('Ctrl Pts',(43.8352347778419,-58.9096510890128,0.));
#61901=CARTESIAN_POINT('Ctrl Pts',(43.8352347778419,-58.9096510890128,12.));
#61902=CARTESIAN_POINT('Ctrl Pts',(43.8580426352236,-58.9230601446445,0.));
#61903=CARTESIAN_POINT('Ctrl Pts',(43.8580426352236,-58.9230601446445,12.));
#61904=CARTESIAN_POINT('Ctrl Pts',(43.8808949651882,-58.9364668927132,0.));
#61905=CARTESIAN_POINT('Ctrl Pts',(43.8808949651882,-58.9364668927132,12.));
#61906=CARTESIAN_POINT('Ctrl Pts',(43.9037917117749,-58.9498712429066,0.));
#61907=CARTESIAN_POINT('Ctrl Pts',(43.9037917117749,-58.9498712429066,12.));
#61908=CARTESIAN_POINT('Ctrl Pts',(43.9267328191508,-58.9632731052704,0.));
#61909=CARTESIAN_POINT('Ctrl Pts',(43.9267328191508,-58.9632731052704,12.));
#61910=CARTESIAN_POINT('Ctrl Pts',(43.9497182316333,-58.9766723902531,0.));
#61911=CARTESIAN_POINT('Ctrl Pts',(43.9497182316333,-58.9766723902531,12.));
#61912=CARTESIAN_POINT('Ctrl Pts',(43.9727478937053,-58.9900690087404,0.));
#61913=CARTESIAN_POINT('Ctrl Pts',(43.9727478937053,-58.9900690087404,12.));
#61914=CARTESIAN_POINT('Ctrl Pts',(43.9958217500364,-59.0034628721161,0.));
#61915=CARTESIAN_POINT('Ctrl Pts',(43.9958217500364,-59.0034628721161,12.));
#61916=CARTESIAN_POINT('Ctrl Pts',(44.0189397454593,-59.0168538922087,0.));
#61917=CARTESIAN_POINT('Ctrl Pts',(44.0189397454593,-59.0168538922087,12.));
#61918=CARTESIAN_POINT('Ctrl Pts',(44.0421018249219,-59.0302419811772,0.));
#61919=CARTESIAN_POINT('Ctrl Pts',(44.0421018249219,-59.0302419811772,12.));
#61920=CARTESIAN_POINT('Ctrl Pts',(44.0653079334384,-59.0436270514085,0.));
#61921=CARTESIAN_POINT('Ctrl Pts',(44.0653079334384,-59.0436270514085,12.));
#61922=CARTESIAN_POINT('Ctrl Pts',(44.0885580160433,-59.0570090154243,0.));
#61923=CARTESIAN_POINT('Ctrl Pts',(44.0885580160433,-59.0570090154243,12.));
#61924=CARTESIAN_POINT('Ctrl Pts',(44.1118520177224,-59.0703877857529,0.));
#61925=CARTESIAN_POINT('Ctrl Pts',(44.1118520177224,-59.0703877857529,12.));
#61926=CARTESIAN_POINT('Ctrl Pts',(44.1351898834057,-59.0837632749209,0.));
#61927=CARTESIAN_POINT('Ctrl Pts',(44.1351898834057,-59.0837632749209,12.));
#61928=CARTESIAN_POINT('Ctrl Pts',(44.1585715581074,-59.0971353957218,0.));
#61929=CARTESIAN_POINT('Ctrl Pts',(44.1585715581074,-59.0971353957218,12.));
#61930=CARTESIAN_POINT('Ctrl Pts',(44.1819969870314,-59.1105040614285,0.));
#61931=CARTESIAN_POINT('Ctrl Pts',(44.1819969870314,-59.1105040614285,12.));
#61932=CARTESIAN_POINT('Ctrl Pts',(44.2054661156876,-59.1238691860307,0.));
#61933=CARTESIAN_POINT('Ctrl Pts',(44.2054661156876,-59.1238691860307,12.));
#61934=CARTESIAN_POINT('Ctrl Pts',(44.2289788899962,-59.1372306844575,0.));
#61935=CARTESIAN_POINT('Ctrl Pts',(44.2289788899962,-59.1372306844575,12.));
#61936=CARTESIAN_POINT('Ctrl Pts',(44.2525352563979,-59.1505884728194,0.));
#61937=CARTESIAN_POINT('Ctrl Pts',(44.2525352563979,-59.1505884728194,12.));
#61938=CARTESIAN_POINT('Ctrl Pts',(44.2761351616027,-59.1639424678766,0.));
#61939=CARTESIAN_POINT('Ctrl Pts',(44.2761351616027,-59.1639424678766,12.));
#61940=CARTESIAN_POINT('Ctrl Pts',(44.2997785523413,-59.1772925865191,0.));
#61941=CARTESIAN_POINT('Ctrl Pts',(44.2997785523413,-59.1772925865191,12.));
#61942=CARTESIAN_POINT('Ctrl Pts',(44.3234653750877,-59.1906387451971,0.));
#61943=CARTESIAN_POINT('Ctrl Pts',(44.3234653750877,-59.1906387451971,12.));
#61944=CARTESIAN_POINT('Ctrl Pts',(44.3471955758412,-59.2039808594765,0.));
#61945=CARTESIAN_POINT('Ctrl Pts',(44.3471955758412,-59.2039808594765,12.));
#61946=CARTESIAN_POINT('Ctrl Pts',(44.3709690997495,-59.217318843283,0.));
#61947=CARTESIAN_POINT('Ctrl Pts',(44.3709690997495,-59.217318843283,12.));
#61948=CARTESIAN_POINT('Ctrl Pts',(44.394785891411,-59.2306526095175,0.));
#61949=CARTESIAN_POINT('Ctrl Pts',(44.394785891411,-59.2306526095175,12.));
#61950=CARTESIAN_POINT('Ctrl Pts',(44.4186458955486,-59.2439820714231,0.));
#61951=CARTESIAN_POINT('Ctrl Pts',(44.4186458955486,-59.2439820714231,12.));
#61952=CARTESIAN_POINT('Ctrl Pts',(44.4425490575932,-59.2573071437801,0.));
#61953=CARTESIAN_POINT('Ctrl Pts',(44.4425490575932,-59.2573071437801,12.));
#61954=CARTESIAN_POINT('Ctrl Pts',(44.4664953242373,-59.2706277440438,0.));
#61955=CARTESIAN_POINT('Ctrl Pts',(44.4664953242373,-59.2706277440438,12.));
#61956=CARTESIAN_POINT('Ctrl Pts',(44.490484644147,-59.2839437938187,0.));
#61957=CARTESIAN_POINT('Ctrl Pts',(44.490484644147,-59.2839437938187,12.));
#61958=CARTESIAN_POINT('Ctrl Pts',(44.514516968128,-59.2972552192072,0.));
#61959=CARTESIAN_POINT('Ctrl Pts',(44.514516968128,-59.2972552192072,12.));
#61960=CARTESIAN_POINT('Ctrl Pts',(44.5385922475494,-59.3105619475512,0.));
#61961=CARTESIAN_POINT('Ctrl Pts',(44.5385922475494,-59.3105619475512,12.));
#61962=CARTESIAN_POINT('Ctrl Pts',(44.5627104330956,-59.3238639048618,0.));
#61963=CARTESIAN_POINT('Ctrl Pts',(44.5627104330956,-59.3238639048618,12.));
#61964=CARTESIAN_POINT('Ctrl Pts',(44.586871473322,-59.3371610128494,0.));
#61965=CARTESIAN_POINT('Ctrl Pts',(44.586871473322,-59.3371610128494,12.));
#61966=CARTESIAN_POINT('Ctrl Pts',(44.6110753134333,-59.3504531864223,0.));
#61967=CARTESIAN_POINT('Ctrl Pts',(44.6110753134333,-59.3504531864223,12.));
#61968=CARTESIAN_POINT('Ctrl Pts',(44.6353218935813,-59.3637403301959,0.));
#61969=CARTESIAN_POINT('Ctrl Pts',(44.6353218935813,-59.3637403301959,12.));
#61970=CARTESIAN_POINT('Ctrl Pts',(44.6596111512861,-59.3770223435405,0.));
#61971=CARTESIAN_POINT('Ctrl Pts',(44.6596111512861,-59.3770223435405,12.));
#61972=CARTESIAN_POINT('Ctrl Pts',(44.6839430244376,-59.3902991268094,0.));
#61973=CARTESIAN_POINT('Ctrl Pts',(44.6839430244376,-59.3902991268094,12.));
#61974=CARTESIAN_POINT('Ctrl Pts',(44.708317454179,-59.403570587392,0.));
#61975=CARTESIAN_POINT('Ctrl Pts',(44.708317454179,-59.403570587392,12.));
#61976=CARTESIAN_POINT('Ctrl Pts',(44.7327343876333,-59.4168366453047,0.));
#61977=CARTESIAN_POINT('Ctrl Pts',(44.7327343876333,-59.4168366453047,12.));
#61978=CARTESIAN_POINT('Ctrl Pts',(44.7571937811872,-59.4300972402943,0.));
#61979=CARTESIAN_POINT('Ctrl Pts',(44.7571937811872,-59.4300972402943,12.));
#61980=CARTESIAN_POINT('Ctrl Pts',(44.7816956017127,-59.4433523334651,0.));
#61981=CARTESIAN_POINT('Ctrl Pts',(44.7816956017127,-59.4433523334651,12.));
#61982=CARTESIAN_POINT('Ctrl Pts',(44.8062398250937,-59.4566019017674,0.));
#61983=CARTESIAN_POINT('Ctrl Pts',(44.8062398250937,-59.4566019017674,12.));
#61984=CARTESIAN_POINT('Ctrl Pts',(44.8259091133624,-59.4671971277837,0.));
#61985=CARTESIAN_POINT('Ctrl Pts',(44.8259091133624,-59.4671971277837,12.));
#61986=CARTESIAN_POINT('Ctrl Pts',(44.8406801497506,-59.475141054744,0.));
#61987=CARTESIAN_POINT('Ctrl Pts',(44.8406801497506,-59.475141054744,12.));
#61988=CARTESIAN_POINT('Ctrl Pts',(44.8505359826374,-59.4804358982977,0.));
#61989=CARTESIAN_POINT('Ctrl Pts',(44.8505359826374,-59.4804358982977,12.));
#61990=CARTESIAN_POINT('Ctrl Pts',(44.8554660179045,-59.483083043136,0.));
#61991=CARTESIAN_POINT('Ctrl Pts',(44.8554660179045,-59.483083043136,12.));
#61992=CARTESIAN_POINT('',(40.8467768343956,-56.8466430164621,0.));
#61993=CARTESIAN_POINT('Ctrl Pts',(40.8467768343956,-56.8466430164621,0.));
#61994=CARTESIAN_POINT('Ctrl Pts',(40.8497761671036,-56.8491101022591,0.));
#61995=CARTESIAN_POINT('Ctrl Pts',(40.8557803680278,-56.8540460739472,0.));
#61996=CARTESIAN_POINT('Ctrl Pts',(40.864803275942,-56.8614554317668,0.));
#61997=CARTESIAN_POINT('Ctrl Pts',(40.8768670342052,-56.8713453764905,0.));
#61998=CARTESIAN_POINT('Ctrl Pts',(40.8920020903293,-56.8837257978343,0.));
#61999=CARTESIAN_POINT('Ctrl Pts',(40.9071924937508,-56.8961241708861,0.));
#62000=CARTESIAN_POINT('Ctrl Pts',(40.9224382132427,-56.9085404164502,0.));
#62001=CARTESIAN_POINT('Ctrl Pts',(40.9377391857129,-56.9209743960992,0.));
#62002=CARTESIAN_POINT('Ctrl Pts',(40.9530953165031,-56.9334259140049,0.));
#62003=CARTESIAN_POINT('Ctrl Pts',(40.9685064933074,-56.9458947422608,0.));
#62004=CARTESIAN_POINT('Ctrl Pts',(40.9839725967121,-56.9583806404069,0.));
#62005=CARTESIAN_POINT('Ctrl Pts',(40.9994935117276,-56.9708833766137,0.));
#62006=CARTESIAN_POINT('Ctrl Pts',(41.0150691398947,-56.9834027500117,0.));
#62007=CARTESIAN_POINT('Ctrl Pts',(41.0306993953989,-56.995938583472,0.));
#62008=CARTESIAN_POINT('Ctrl Pts',(41.0463841993608,-57.008490713042,0.));
#62009=CARTESIAN_POINT('Ctrl Pts',(41.0621234751007,-57.0210589791788,0.));
#62010=CARTESIAN_POINT('Ctrl Pts',(41.0779171422438,-57.0336432158536,0.));
#62011=CARTESIAN_POINT('Ctrl Pts',(41.0937651137549,-57.046243245068,0.));
#62012=CARTESIAN_POINT('Ctrl Pts',(41.1096672990148,-57.0588588825298,0.));
#62013=CARTESIAN_POINT('Ctrl Pts',(41.1256236057443,-57.0714899412099,0.));
#62014=CARTESIAN_POINT('Ctrl Pts',(41.1416339422117,-57.084136235426,0.));
#62015=CARTESIAN_POINT('Ctrl Pts',(41.1576982197375,-57.0967975854874,0.));
#62016=CARTESIAN_POINT('Ctrl Pts',(41.1738163525902,-57.1094738174957,0.));
#62017=CARTESIAN_POINT('Ctrl Pts',(41.1899882567923,-57.1221647611207,0.));
#62018=CARTESIAN_POINT('Ctrl Pts',(41.2062138492915,-57.1348702480647,0.));
#62019=CARTESIAN_POINT('Ctrl Pts',(41.222493046943,-57.147590110182,0.));
#62020=CARTESIAN_POINT('Ctrl Pts',(41.2388257656559,-57.1603241779077,0.));
#62021=CARTESIAN_POINT('Ctrl Pts',(41.2552119208466,-57.17307228108,0.));
#62022=CARTESIAN_POINT('Ctrl Pts',(41.2716514278276,-57.1858342496538,0.));
#62023=CARTESIAN_POINT('Ctrl Pts',(41.2881442021863,-57.1986099143983,0.));
#62024=CARTESIAN_POINT('Ctrl Pts',(41.3046901602293,-57.2113991077302,0.));
#62025=CARTESIAN_POINT('Ctrl Pts',(41.321289219149,-57.2242016640198,0.));
#62026=CARTESIAN_POINT('Ctrl Pts',(41.3379412967875,-57.2370174191401,0.));
#62027=CARTESIAN_POINT('Ctrl Pts',(41.3546463114885,-57.2498462101879,0.));
#62028=CARTESIAN_POINT('Ctrl Pts',(41.3714041819224,-57.2626878751596,0.));
#62029=CARTESIAN_POINT('Ctrl Pts',(41.3882148268814,-57.2755422525844,0.));
#62030=CARTESIAN_POINT('Ctrl Pts',(41.4050781652938,-57.2884091815406,0.));
#62031=CARTESIAN_POINT('Ctrl Pts',(41.4219941163163,-57.3012885018151,0.));
#62032=CARTESIAN_POINT('Ctrl Pts',(41.4389625993948,-57.3141800540137,0.));
#62033=CARTESIAN_POINT('Ctrl Pts',(41.4559835343328,-57.3270836796911,0.));
#62034=CARTESIAN_POINT('Ctrl Pts',(41.4730568413518,-57.3399992214717,0.));
#62035=CARTESIAN_POINT('Ctrl Pts',(41.4901824410637,-57.3529265229835,0.));
#62036=CARTESIAN_POINT('Ctrl Pts',(41.5073602544396,-57.3658654287937,0.));
#62037=CARTESIAN_POINT('Ctrl Pts',(41.5245902027771,-57.3788157843454,0.));
#62038=CARTESIAN_POINT('Ctrl Pts',(41.5418722076572,-57.3917774358863,0.));
#62039=CARTESIAN_POINT('Ctrl Pts',(41.5592061909176,-57.4047502304231,0.));
#62040=CARTESIAN_POINT('Ctrl Pts',(41.5765920746777,-57.4177340157508,0.));
#62041=CARTESIAN_POINT('Ctrl Pts',(41.5940297813477,-57.4307286404662,0.));
#62042=CARTESIAN_POINT('Ctrl Pts',(41.6115192336388,-57.4437339539841,0.));
#62043=CARTESIAN_POINT('Ctrl Pts',(41.6290603545666,-57.4567498065562,0.));
#62044=CARTESIAN_POINT('Ctrl Pts',(41.6466530674515,-57.4697760492683,0.));
#62045=CARTESIAN_POINT('Ctrl Pts',(41.6642972959165,-57.4828125340218,0.));
#62046=CARTESIAN_POINT('Ctrl Pts',(41.6819929638797,-57.4958591135165,0.));
#62047=CARTESIAN_POINT('Ctrl Pts',(41.6997399955447,-57.5089156412343,0.));
#62048=CARTESIAN_POINT('Ctrl Pts',(41.7175383153821,-57.5219819714171,0.));
#62049=CARTESIAN_POINT('Ctrl Pts',(41.7353878481337,-57.5350579590649,0.));
#62050=CARTESIAN_POINT('Ctrl Pts',(41.7532885188175,-57.5481434599335,0.));
#62051=CARTESIAN_POINT('Ctrl Pts',(41.7712402527273,-57.561238330532,0.));
#62052=CARTESIAN_POINT('Ctrl Pts',(41.7892429754297,-57.5743424281204,0.));
#62053=CARTESIAN_POINT('Ctrl Pts',(41.8072966127558,-57.5874556107056,0.));
#62054=CARTESIAN_POINT('Ctrl Pts',(41.8254010908051,-57.6005777370349,0.));
#62055=CARTESIAN_POINT('Ctrl Pts',(41.8435563359456,-57.6137086665882,0.));
#62056=CARTESIAN_POINT('Ctrl Pts',(41.8617622748108,-57.6268482595702,0.));
#62057=CARTESIAN_POINT('Ctrl Pts',(41.8800188342909,-57.6399963769003,0.));
#62058=CARTESIAN_POINT('Ctrl Pts',(41.8983259415245,-57.6531528802059,0.));
#62059=CARTESIAN_POINT('Ctrl Pts',(41.9166835239046,-57.6663176318176,0.));
#62060=CARTESIAN_POINT('Ctrl Pts',(41.9350915090791,-57.6794904947641,0.));
#62061=CARTESIAN_POINT('Ctrl Pts',(41.9535498249489,-57.6926713327674,0.));
#62062=CARTESIAN_POINT('Ctrl Pts',(41.9720583996601,-57.7058600102365,0.));
#62063=CARTESIAN_POINT('Ctrl Pts',(41.9906171615975,-57.7190563922614,0.));
#62064=CARTESIAN_POINT('Ctrl Pts',(42.0092260393911,-57.7322603446086,0.));
#62065=CARTESIAN_POINT('Ctrl Pts',(42.0278849619156,-57.7454717337151,0.));
#62066=CARTESIAN_POINT('Ctrl Pts',(42.0465938582878,-57.7586904266828,0.));
#62067=CARTESIAN_POINT('Ctrl Pts',(42.0653526578571,-57.7719162912721,0.));
#62068=CARTESIAN_POINT('Ctrl Pts',(42.0841612902018,-57.7851491958954,0.));
#62069=CARTESIAN_POINT('Ctrl Pts',(42.1030196851344,-57.798389009613,0.));
#62070=CARTESIAN_POINT('Ctrl Pts',(42.121927772701,-57.8116356021274,0.));
#62071=CARTESIAN_POINT('Ctrl Pts',(42.1408854831792,-57.8248888437787,0.));
#62072=CARTESIAN_POINT('Ctrl Pts',(42.1598927470671,-57.8381486055376,0.));
#62073=CARTESIAN_POINT('Ctrl Pts',(42.1789494950824,-57.8514147590012,0.));
#62074=CARTESIAN_POINT('Ctrl Pts',(42.1980556581689,-57.86468717639,0.));
#62075=CARTESIAN_POINT('Ctrl Pts',(42.2172111674946,-57.8779657305422,0.));
#62076=CARTESIAN_POINT('Ctrl Pts',(42.2364159544492,-57.8912502949084,0.));
#62077=CARTESIAN_POINT('Ctrl Pts',(42.2556699506332,-57.9045407435447,0.));
#62078=CARTESIAN_POINT('Ctrl Pts',(42.274973087857,-57.9178369511084,0.));
#62079=CARTESIAN_POINT('Ctrl Pts',(42.2943252981471,-57.9311387928541,0.));
#62080=CARTESIAN_POINT('Ctrl Pts',(42.3137265137446,-57.9444461446292,0.));
#62081=CARTESIAN_POINT('Ctrl Pts',(42.3331766671028,-57.9577588828693,0.));
#62082=CARTESIAN_POINT('Ctrl Pts',(42.3526756908764,-57.9710768845923,0.));
#62083=CARTESIAN_POINT('Ctrl Pts',(42.3722235179216,-57.9844000273936,0.));
#62084=CARTESIAN_POINT('Ctrl Pts',(42.3918200813025,-57.9977281894437,0.));
#62085=CARTESIAN_POINT('Ctrl Pts',(42.4114653142891,-58.011061249483,0.));
#62086=CARTESIAN_POINT('Ctrl Pts',(42.4311591503551,-58.0243990868175,0.));
#62087=CARTESIAN_POINT('Ctrl Pts',(42.4509015231668,-58.0377415813132,0.));
#62088=CARTESIAN_POINT('Ctrl Pts',(42.4706923665838,-58.0510886133917,0.));
#62089=CARTESIAN_POINT('Ctrl Pts',(42.490531614665,-58.064440064027,0.));
#62090=CARTESIAN_POINT('Ctrl Pts',(42.5104192016664,-58.0777958147404,0.));
#62091=CARTESIAN_POINT('Ctrl Pts',(42.5303550620388,-58.0911557475967,0.));
#62092=CARTESIAN_POINT('Ctrl Pts',(42.5503391304183,-58.1045197452003,0.));
#62093=CARTESIAN_POINT('Ctrl Pts',(42.5703713416263,-58.1178876906905,0.));
#62094=CARTESIAN_POINT('Ctrl Pts',(42.5904516306759,-58.1312594677383,0.));
#62095=CARTESIAN_POINT('Ctrl Pts',(42.6105799327697,-58.1446349605419,0.));
#62096=CARTESIAN_POINT('Ctrl Pts',(42.6307561832978,-58.158014053823,0.));
#62097=CARTESIAN_POINT('Ctrl Pts',(42.650980317827,-58.1713966328217,0.));
#62098=CARTESIAN_POINT('Ctrl Pts',(42.6712522721021,-58.1847825832932,0.));
#62099=CARTESIAN_POINT('Ctrl Pts',(42.6915719820517,-58.1981717915043,0.));
#62100=CARTESIAN_POINT('Ctrl Pts',(42.7119393837867,-58.2115641442302,0.));
#62101=CARTESIAN_POINT('Ctrl Pts',(42.7323544135983,-58.2249595287497,0.));
#62102=CARTESIAN_POINT('Ctrl Pts',(42.7528170079482,-58.238357832842,0.));
#62103=CARTESIAN_POINT('Ctrl Pts',(42.7733271034679,-58.2517589447818,0.));
#62104=CARTESIAN_POINT('Ctrl Pts',(42.7938846369651,-58.2651627533368,0.));
#62105=CARTESIAN_POINT('Ctrl Pts',(42.8144895454234,-58.278569147764,0.));
#62106=CARTESIAN_POINT('Ctrl Pts',(42.8351417659998,-58.2919780178063,0.));
#62107=CARTESIAN_POINT('Ctrl Pts',(42.8558412360154,-58.305389253689,0.));
#62108=CARTESIAN_POINT('Ctrl Pts',(42.8765878929545,-58.3188027461157,0.));
#62109=CARTESIAN_POINT('Ctrl Pts',(42.8973816744703,-58.3322183862647,0.));
#62110=CARTESIAN_POINT('Ctrl Pts',(42.9182225183851,-58.3456360657861,0.));
#62111=CARTESIAN_POINT('Ctrl Pts',(42.9391103626881,-58.3590556767981,0.));
#62112=CARTESIAN_POINT('Ctrl Pts',(42.9600451455267,-58.3724771118835,0.));
#62113=CARTESIAN_POINT('Ctrl Pts',(42.9810268052043,-58.3859002640871,0.));
#62114=CARTESIAN_POINT('Ctrl Pts',(43.002055280187,-58.3993250269115,0.));
#62115=CARTESIAN_POINT('Ctrl Pts',(43.0231305091033,-58.4127512943144,0.));
#62116=CARTESIAN_POINT('Ctrl Pts',(43.0442524307432,-58.4261789607055,0.));
#62117=CARTESIAN_POINT('Ctrl Pts',(43.0654209840502,-58.4396079209438,0.));
#62118=CARTESIAN_POINT('Ctrl Pts',(43.0866361081166,-58.4530380703335,0.));
#62119=CARTESIAN_POINT('Ctrl Pts',(43.1078977421908,-58.4664693046206,0.));
#62120=CARTESIAN_POINT('Ctrl Pts',(43.1292058256774,-58.4799015199904,0.));
#62121=CARTESIAN_POINT('Ctrl Pts',(43.1505602981366,-58.4933346130638,0.));
#62122=CARTESIAN_POINT('Ctrl Pts',(43.1719610992772,-58.5067684808946,0.));
#62123=CARTESIAN_POINT('Ctrl Pts',(43.1934081689504,-58.5202030209667,0.));
#62124=CARTESIAN_POINT('Ctrl Pts',(43.214901447157,-58.5336381311911,0.));
#62125=CARTESIAN_POINT('Ctrl Pts',(43.2364408740489,-58.5470737099027,0.));
#62126=CARTESIAN_POINT('Ctrl Pts',(43.2580263899278,-58.5605096558578,0.));
#62127=CARTESIAN_POINT('Ctrl Pts',(43.2796579352405,-58.5739458682317,0.));
#62128=CARTESIAN_POINT('Ctrl Pts',(43.3013354505708,-58.5873822466163,0.));
#62129=CARTESIAN_POINT('Ctrl Pts',(43.3230588766456,-58.6008186910166,0.));
#62130=CARTESIAN_POINT('Ctrl Pts',(43.3448281543375,-58.6142551018473,0.));
#62131=CARTESIAN_POINT('Ctrl Pts',(43.3666432246635,-58.627691379929,0.));
#62132=CARTESIAN_POINT('Ctrl Pts',(43.3885040287808,-58.6411274264854,0.));
#62133=CARTESIAN_POINT('Ctrl Pts',(43.4104105079766,-58.6545631431388,0.));
#62134=CARTESIAN_POINT('Ctrl Pts',(43.4323626036736,-58.6679984319095,0.));
#62135=CARTESIAN_POINT('Ctrl Pts',(43.4543602574352,-58.6814331952138,0.));
#62136=CARTESIAN_POINT('Ctrl Pts',(43.4764034109655,-58.6948673358639,0.));
#62137=CARTESIAN_POINT('Ctrl Pts',(43.4984920061071,-58.708300757066,0.));
#62138=CARTESIAN_POINT('Ctrl Pts',(43.5206259848333,-58.7217333624206,0.));
#62139=CARTESIAN_POINT('Ctrl Pts',(43.5428052892483,-58.7351650559176,0.));
#62140=CARTESIAN_POINT('Ctrl Pts',(43.5650298615912,-58.7485957419296,0.));
#62141=CARTESIAN_POINT('Ctrl Pts',(43.5872996442343,-58.7620253252059,0.));
#62142=CARTESIAN_POINT('Ctrl Pts',(43.6096145796798,-58.7754537108672,0.));
#62143=CARTESIAN_POINT('Ctrl Pts',(43.6319746105488,-58.7888808043976,0.));
#62144=CARTESIAN_POINT('Ctrl Pts',(43.6543796795797,-58.8023065116446,0.));
#62145=CARTESIAN_POINT('Ctrl Pts',(43.6768297296403,-58.8157307388247,0.));
#62146=CARTESIAN_POINT('Ctrl Pts',(43.6993247037318,-58.8291533925299,0.));
#62147=CARTESIAN_POINT('Ctrl Pts',(43.7218645449921,-58.8425743797325,0.));
#62148=CARTESIAN_POINT('Ctrl Pts',(43.7444491966935,-58.8559936077933,0.));
#62149=CARTESIAN_POINT('Ctrl Pts',(43.7670786022392,-58.8694109844636,0.));
#62150=CARTESIAN_POINT('Ctrl Pts',(43.7897527051599,-58.882826417861,0.));
#62151=CARTESIAN_POINT('Ctrl Pts',(43.812471449107,-58.8962398164486,0.));
#62152=CARTESIAN_POINT('Ctrl Pts',(43.8352347778419,-58.9096510890128,0.));
#62153=CARTESIAN_POINT('Ctrl Pts',(43.8580426352236,-58.9230601446445,0.));
#62154=CARTESIAN_POINT('Ctrl Pts',(43.8808949651882,-58.9364668927132,0.));
#62155=CARTESIAN_POINT('Ctrl Pts',(43.9037917117749,-58.9498712429066,0.));
#62156=CARTESIAN_POINT('Ctrl Pts',(43.9267328191508,-58.9632731052704,0.));
#62157=CARTESIAN_POINT('Ctrl Pts',(43.9497182316333,-58.9766723902531,0.));
#62158=CARTESIAN_POINT('Ctrl Pts',(43.9727478937053,-58.9900690087404,0.));
#62159=CARTESIAN_POINT('Ctrl Pts',(43.9958217500364,-59.0034628721161,0.));
#62160=CARTESIAN_POINT('Ctrl Pts',(44.0189397454593,-59.0168538922087,0.));
#62161=CARTESIAN_POINT('Ctrl Pts',(44.0421018249219,-59.0302419811772,0.));
#62162=CARTESIAN_POINT('Ctrl Pts',(44.0653079334384,-59.0436270514085,0.));
#62163=CARTESIAN_POINT('Ctrl Pts',(44.0885580160433,-59.0570090154243,0.));
#62164=CARTESIAN_POINT('Ctrl Pts',(44.1118520177224,-59.0703877857529,0.));
#62165=CARTESIAN_POINT('Ctrl Pts',(44.1351898834057,-59.0837632749209,0.));
#62166=CARTESIAN_POINT('Ctrl Pts',(44.1585715581074,-59.0971353957218,0.));
#62167=CARTESIAN_POINT('Ctrl Pts',(44.1819969870314,-59.1105040614285,0.));
#62168=CARTESIAN_POINT('Ctrl Pts',(44.2054661156876,-59.1238691860307,0.));
#62169=CARTESIAN_POINT('Ctrl Pts',(44.2289788899962,-59.1372306844575,0.));
#62170=CARTESIAN_POINT('Ctrl Pts',(44.2525352563979,-59.1505884728194,0.));
#62171=CARTESIAN_POINT('Ctrl Pts',(44.2761351616027,-59.1639424678766,0.));
#62172=CARTESIAN_POINT('Ctrl Pts',(44.2997785523413,-59.1772925865191,0.));
#62173=CARTESIAN_POINT('Ctrl Pts',(44.3234653750877,-59.1906387451971,0.));
#62174=CARTESIAN_POINT('Ctrl Pts',(44.3471955758412,-59.2039808594765,0.));
#62175=CARTESIAN_POINT('Ctrl Pts',(44.3709690997495,-59.217318843283,0.));
#62176=CARTESIAN_POINT('Ctrl Pts',(44.394785891411,-59.2306526095175,0.));
#62177=CARTESIAN_POINT('Ctrl Pts',(44.4186458955486,-59.2439820714231,0.));
#62178=CARTESIAN_POINT('Ctrl Pts',(44.4425490575932,-59.2573071437801,0.));
#62179=CARTESIAN_POINT('Ctrl Pts',(44.4664953242373,-59.2706277440438,0.));
#62180=CARTESIAN_POINT('Ctrl Pts',(44.490484644147,-59.2839437938187,0.));
#62181=CARTESIAN_POINT('Ctrl Pts',(44.514516968128,-59.2972552192072,0.));
#62182=CARTESIAN_POINT('Ctrl Pts',(44.5351541478336,-59.3086616639392,0.));
#62183=CARTESIAN_POINT('Ctrl Pts',(44.5509994357954,-59.317404187219,0.));
#62184=CARTESIAN_POINT('Ctrl Pts',(44.5620338188487,-59.3234848865279,0.));
#62185=CARTESIAN_POINT('Ctrl Pts',(44.5682447395714,-59.3269051738223,0.));
#62186=CARTESIAN_POINT('Ctrl Pts',(44.5696260757422,-59.3276657444159,0.));
#62187=CARTESIAN_POINT('',(40.8467768343956,-56.8466430164621,12.));
#62188=CARTESIAN_POINT('',(40.8467768343956,-56.8466430164621,0.));
#62189=CARTESIAN_POINT('Ctrl Pts',(44.5696260757422,-59.3276657444159,12.));
#62190=CARTESIAN_POINT('Ctrl Pts',(44.5682447395714,-59.3269051738223,12.));
#62191=CARTESIAN_POINT('Ctrl Pts',(44.5620338188486,-59.3234848865279,12.));
#62192=CARTESIAN_POINT('Ctrl Pts',(44.5509994357954,-59.317404187219,12.));
#62193=CARTESIAN_POINT('Ctrl Pts',(44.5351541478336,-59.3086616639392,12.));
#62194=CARTESIAN_POINT('Ctrl Pts',(44.514516968128,-59.2972552192072,12.));
#62195=CARTESIAN_POINT('Ctrl Pts',(44.490484644147,-59.2839437938187,12.));
#62196=CARTESIAN_POINT('Ctrl Pts',(44.4664953242373,-59.2706277440438,12.));
#62197=CARTESIAN_POINT('Ctrl Pts',(44.4425490575932,-59.2573071437801,12.));
#62198=CARTESIAN_POINT('Ctrl Pts',(44.4186458955486,-59.2439820714231,12.));
#62199=CARTESIAN_POINT('Ctrl Pts',(44.394785891411,-59.2306526095175,12.));
#62200=CARTESIAN_POINT('Ctrl Pts',(44.3709690997495,-59.217318843283,12.));
#62201=CARTESIAN_POINT('Ctrl Pts',(44.3471955758412,-59.2039808594765,12.));
#62202=CARTESIAN_POINT('Ctrl Pts',(44.3234653750877,-59.1906387451971,12.));
#62203=CARTESIAN_POINT('Ctrl Pts',(44.2997785523413,-59.1772925865191,12.));
#62204=CARTESIAN_POINT('Ctrl Pts',(44.2761351616027,-59.1639424678766,12.));
#62205=CARTESIAN_POINT('Ctrl Pts',(44.2525352563979,-59.1505884728194,12.));
#62206=CARTESIAN_POINT('Ctrl Pts',(44.2289788899962,-59.1372306844575,12.));
#62207=CARTESIAN_POINT('Ctrl Pts',(44.2054661156876,-59.1238691860307,12.));
#62208=CARTESIAN_POINT('Ctrl Pts',(44.1819969870314,-59.1105040614285,12.));
#62209=CARTESIAN_POINT('Ctrl Pts',(44.1585715581074,-59.0971353957218,12.));
#62210=CARTESIAN_POINT('Ctrl Pts',(44.1351898834057,-59.0837632749209,12.));
#62211=CARTESIAN_POINT('Ctrl Pts',(44.1118520177224,-59.0703877857529,12.));
#62212=CARTESIAN_POINT('Ctrl Pts',(44.0885580160433,-59.0570090154243,12.));
#62213=CARTESIAN_POINT('Ctrl Pts',(44.0653079334384,-59.0436270514085,12.));
#62214=CARTESIAN_POINT('Ctrl Pts',(44.0421018249219,-59.0302419811772,12.));
#62215=CARTESIAN_POINT('Ctrl Pts',(44.0189397454593,-59.0168538922087,12.));
#62216=CARTESIAN_POINT('Ctrl Pts',(43.9958217500364,-59.0034628721161,12.));
#62217=CARTESIAN_POINT('Ctrl Pts',(43.9727478937053,-58.9900690087404,12.));
#62218=CARTESIAN_POINT('Ctrl Pts',(43.9497182316333,-58.9766723902531,12.));
#62219=CARTESIAN_POINT('Ctrl Pts',(43.9267328191508,-58.9632731052704,12.));
#62220=CARTESIAN_POINT('Ctrl Pts',(43.9037917117749,-58.9498712429066,12.));
#62221=CARTESIAN_POINT('Ctrl Pts',(43.8808949651882,-58.9364668927132,12.));
#62222=CARTESIAN_POINT('Ctrl Pts',(43.8580426352236,-58.9230601446445,12.));
#62223=CARTESIAN_POINT('Ctrl Pts',(43.8352347778419,-58.9096510890128,12.));
#62224=CARTESIAN_POINT('Ctrl Pts',(43.812471449107,-58.8962398164486,12.));
#62225=CARTESIAN_POINT('Ctrl Pts',(43.7897527051599,-58.882826417861,12.));
#62226=CARTESIAN_POINT('Ctrl Pts',(43.7670786022392,-58.8694109844636,12.));
#62227=CARTESIAN_POINT('Ctrl Pts',(43.7444491966935,-58.8559936077933,12.));
#62228=CARTESIAN_POINT('Ctrl Pts',(43.7218645449921,-58.8425743797325,12.));
#62229=CARTESIAN_POINT('Ctrl Pts',(43.6993247037318,-58.8291533925299,12.));
#62230=CARTESIAN_POINT('Ctrl Pts',(43.6768297296403,-58.8157307388247,12.));
#62231=CARTESIAN_POINT('Ctrl Pts',(43.6543796795797,-58.8023065116446,12.));
#62232=CARTESIAN_POINT('Ctrl Pts',(43.6319746105488,-58.7888808043976,12.));
#62233=CARTESIAN_POINT('Ctrl Pts',(43.6096145796798,-58.7754537108672,12.));
#62234=CARTESIAN_POINT('Ctrl Pts',(43.5872996442343,-58.7620253252059,12.));
#62235=CARTESIAN_POINT('Ctrl Pts',(43.5650298615912,-58.7485957419296,12.));
#62236=CARTESIAN_POINT('Ctrl Pts',(43.5428052892483,-58.7351650559176,12.));
#62237=CARTESIAN_POINT('Ctrl Pts',(43.5206259848333,-58.7217333624206,12.));
#62238=CARTESIAN_POINT('Ctrl Pts',(43.4984920061071,-58.708300757066,12.));
#62239=CARTESIAN_POINT('Ctrl Pts',(43.4764034109655,-58.6948673358639,12.));
#62240=CARTESIAN_POINT('Ctrl Pts',(43.4543602574352,-58.6814331952138,12.));
#62241=CARTESIAN_POINT('Ctrl Pts',(43.4323626036736,-58.6679984319095,12.));
#62242=CARTESIAN_POINT('Ctrl Pts',(43.4104105079766,-58.6545631431388,12.));
#62243=CARTESIAN_POINT('Ctrl Pts',(43.3885040287808,-58.6411274264854,12.));
#62244=CARTESIAN_POINT('Ctrl Pts',(43.3666432246635,-58.627691379929,12.));
#62245=CARTESIAN_POINT('Ctrl Pts',(43.3448281543375,-58.6142551018473,12.));
#62246=CARTESIAN_POINT('Ctrl Pts',(43.3230588766456,-58.6008186910166,12.));
#62247=CARTESIAN_POINT('Ctrl Pts',(43.3013354505708,-58.5873822466163,12.));
#62248=CARTESIAN_POINT('Ctrl Pts',(43.2796579352405,-58.5739458682317,12.));
#62249=CARTESIAN_POINT('Ctrl Pts',(43.2580263899278,-58.5605096558578,12.));
#62250=CARTESIAN_POINT('Ctrl Pts',(43.2364408740489,-58.5470737099027,12.));
#62251=CARTESIAN_POINT('Ctrl Pts',(43.214901447157,-58.5336381311911,12.));
#62252=CARTESIAN_POINT('Ctrl Pts',(43.1934081689504,-58.5202030209667,12.));
#62253=CARTESIAN_POINT('Ctrl Pts',(43.1719610992772,-58.5067684808946,12.));
#62254=CARTESIAN_POINT('Ctrl Pts',(43.1505602981366,-58.4933346130638,12.));
#62255=CARTESIAN_POINT('Ctrl Pts',(43.1292058256774,-58.4799015199904,12.));
#62256=CARTESIAN_POINT('Ctrl Pts',(43.1078977421908,-58.4664693046206,12.));
#62257=CARTESIAN_POINT('Ctrl Pts',(43.0866361081166,-58.4530380703335,12.));
#62258=CARTESIAN_POINT('Ctrl Pts',(43.0654209840502,-58.4396079209438,12.));
#62259=CARTESIAN_POINT('Ctrl Pts',(43.0442524307432,-58.4261789607055,12.));
#62260=CARTESIAN_POINT('Ctrl Pts',(43.0231305091033,-58.4127512943144,12.));
#62261=CARTESIAN_POINT('Ctrl Pts',(43.002055280187,-58.3993250269115,12.));
#62262=CARTESIAN_POINT('Ctrl Pts',(42.9810268052043,-58.3859002640871,12.));
#62263=CARTESIAN_POINT('Ctrl Pts',(42.9600451455267,-58.3724771118835,12.));
#62264=CARTESIAN_POINT('Ctrl Pts',(42.9391103626881,-58.3590556767981,12.));
#62265=CARTESIAN_POINT('Ctrl Pts',(42.9182225183851,-58.3456360657861,12.));
#62266=CARTESIAN_POINT('Ctrl Pts',(42.8973816744703,-58.3322183862647,12.));
#62267=CARTESIAN_POINT('Ctrl Pts',(42.8765878929545,-58.3188027461157,12.));
#62268=CARTESIAN_POINT('Ctrl Pts',(42.8558412360154,-58.305389253689,12.));
#62269=CARTESIAN_POINT('Ctrl Pts',(42.8351417659998,-58.2919780178063,12.));
#62270=CARTESIAN_POINT('Ctrl Pts',(42.8144895454234,-58.278569147764,12.));
#62271=CARTESIAN_POINT('Ctrl Pts',(42.7938846369651,-58.2651627533368,12.));
#62272=CARTESIAN_POINT('Ctrl Pts',(42.7733271034679,-58.2517589447818,12.));
#62273=CARTESIAN_POINT('Ctrl Pts',(42.7528170079482,-58.238357832842,12.));
#62274=CARTESIAN_POINT('Ctrl Pts',(42.7323544135983,-58.2249595287497,12.));
#62275=CARTESIAN_POINT('Ctrl Pts',(42.7119393837867,-58.2115641442302,12.));
#62276=CARTESIAN_POINT('Ctrl Pts',(42.6915719820517,-58.1981717915043,12.));
#62277=CARTESIAN_POINT('Ctrl Pts',(42.6712522721021,-58.1847825832932,12.));
#62278=CARTESIAN_POINT('Ctrl Pts',(42.650980317827,-58.1713966328217,12.));
#62279=CARTESIAN_POINT('Ctrl Pts',(42.6307561832978,-58.158014053823,12.));
#62280=CARTESIAN_POINT('Ctrl Pts',(42.6105799327697,-58.1446349605419,12.));
#62281=CARTESIAN_POINT('Ctrl Pts',(42.5904516306759,-58.1312594677383,12.));
#62282=CARTESIAN_POINT('Ctrl Pts',(42.5703713416263,-58.1178876906905,12.));
#62283=CARTESIAN_POINT('Ctrl Pts',(42.5503391304183,-58.1045197452003,12.));
#62284=CARTESIAN_POINT('Ctrl Pts',(42.5303550620388,-58.0911557475967,12.));
#62285=CARTESIAN_POINT('Ctrl Pts',(42.5104192016664,-58.0777958147404,12.));
#62286=CARTESIAN_POINT('Ctrl Pts',(42.490531614665,-58.064440064027,12.));
#62287=CARTESIAN_POINT('Ctrl Pts',(42.4706923665838,-58.0510886133917,12.));
#62288=CARTESIAN_POINT('Ctrl Pts',(42.4509015231668,-58.0377415813132,12.));
#62289=CARTESIAN_POINT('Ctrl Pts',(42.4311591503551,-58.0243990868175,12.));
#62290=CARTESIAN_POINT('Ctrl Pts',(42.4114653142891,-58.011061249483,12.));
#62291=CARTESIAN_POINT('Ctrl Pts',(42.3918200813025,-57.9977281894437,12.));
#62292=CARTESIAN_POINT('Ctrl Pts',(42.3722235179216,-57.9844000273936,12.));
#62293=CARTESIAN_POINT('Ctrl Pts',(42.3526756908764,-57.9710768845923,12.));
#62294=CARTESIAN_POINT('Ctrl Pts',(42.3331766671028,-57.9577588828693,12.));
#62295=CARTESIAN_POINT('Ctrl Pts',(42.3137265137446,-57.9444461446292,12.));
#62296=CARTESIAN_POINT('Ctrl Pts',(42.2943252981471,-57.9311387928541,12.));
#62297=CARTESIAN_POINT('Ctrl Pts',(42.274973087857,-57.9178369511084,12.));
#62298=CARTESIAN_POINT('Ctrl Pts',(42.2556699506332,-57.9045407435447,12.));
#62299=CARTESIAN_POINT('Ctrl Pts',(42.2364159544492,-57.8912502949084,12.));
#62300=CARTESIAN_POINT('Ctrl Pts',(42.2172111674946,-57.8779657305422,12.));
#62301=CARTESIAN_POINT('Ctrl Pts',(42.1980556581689,-57.86468717639,12.));
#62302=CARTESIAN_POINT('Ctrl Pts',(42.1789494950824,-57.8514147590012,12.));
#62303=CARTESIAN_POINT('Ctrl Pts',(42.1598927470671,-57.8381486055376,12.));
#62304=CARTESIAN_POINT('Ctrl Pts',(42.1408854831792,-57.8248888437787,12.));
#62305=CARTESIAN_POINT('Ctrl Pts',(42.121927772701,-57.8116356021274,12.));
#62306=CARTESIAN_POINT('Ctrl Pts',(42.1030196851344,-57.798389009613,12.));
#62307=CARTESIAN_POINT('Ctrl Pts',(42.0841612902018,-57.7851491958954,12.));
#62308=CARTESIAN_POINT('Ctrl Pts',(42.0653526578571,-57.7719162912721,12.));
#62309=CARTESIAN_POINT('Ctrl Pts',(42.0465938582878,-57.7586904266828,12.));
#62310=CARTESIAN_POINT('Ctrl Pts',(42.0278849619156,-57.7454717337151,12.));
#62311=CARTESIAN_POINT('Ctrl Pts',(42.0092260393911,-57.7322603446086,12.));
#62312=CARTESIAN_POINT('Ctrl Pts',(41.9906171615975,-57.7190563922614,12.));
#62313=CARTESIAN_POINT('Ctrl Pts',(41.9720583996601,-57.7058600102365,12.));
#62314=CARTESIAN_POINT('Ctrl Pts',(41.9535498249489,-57.6926713327674,12.));
#62315=CARTESIAN_POINT('Ctrl Pts',(41.9350915090791,-57.6794904947641,12.));
#62316=CARTESIAN_POINT('Ctrl Pts',(41.9166835239046,-57.6663176318176,12.));
#62317=CARTESIAN_POINT('Ctrl Pts',(41.8983259415245,-57.6531528802059,12.));
#62318=CARTESIAN_POINT('Ctrl Pts',(41.8800188342909,-57.6399963769003,12.));
#62319=CARTESIAN_POINT('Ctrl Pts',(41.8617622748108,-57.6268482595702,12.));
#62320=CARTESIAN_POINT('Ctrl Pts',(41.8435563359456,-57.6137086665882,12.));
#62321=CARTESIAN_POINT('Ctrl Pts',(41.8254010908051,-57.6005777370349,12.));
#62322=CARTESIAN_POINT('Ctrl Pts',(41.8072966127558,-57.5874556107056,12.));
#62323=CARTESIAN_POINT('Ctrl Pts',(41.7892429754297,-57.5743424281204,12.));
#62324=CARTESIAN_POINT('Ctrl Pts',(41.7712402527273,-57.561238330532,12.));
#62325=CARTESIAN_POINT('Ctrl Pts',(41.7532885188175,-57.5481434599335,12.));
#62326=CARTESIAN_POINT('Ctrl Pts',(41.7353878481337,-57.5350579590649,12.));
#62327=CARTESIAN_POINT('Ctrl Pts',(41.7175383153821,-57.5219819714171,12.));
#62328=CARTESIAN_POINT('Ctrl Pts',(41.6997399955447,-57.5089156412343,12.));
#62329=CARTESIAN_POINT('Ctrl Pts',(41.6819929638797,-57.4958591135165,12.));
#62330=CARTESIAN_POINT('Ctrl Pts',(41.6642972959165,-57.4828125340218,12.));
#62331=CARTESIAN_POINT('Ctrl Pts',(41.6466530674515,-57.4697760492683,12.));
#62332=CARTESIAN_POINT('Ctrl Pts',(41.6290603545666,-57.4567498065562,12.));
#62333=CARTESIAN_POINT('Ctrl Pts',(41.6115192336388,-57.4437339539841,12.));
#62334=CARTESIAN_POINT('Ctrl Pts',(41.5940297813477,-57.4307286404662,12.));
#62335=CARTESIAN_POINT('Ctrl Pts',(41.5765920746777,-57.4177340157508,12.));
#62336=CARTESIAN_POINT('Ctrl Pts',(41.5592061909176,-57.4047502304231,12.));
#62337=CARTESIAN_POINT('Ctrl Pts',(41.5418722076572,-57.3917774358863,12.));
#62338=CARTESIAN_POINT('Ctrl Pts',(41.5245902027771,-57.3788157843454,12.));
#62339=CARTESIAN_POINT('Ctrl Pts',(41.5073602544396,-57.3658654287937,12.));
#62340=CARTESIAN_POINT('Ctrl Pts',(41.4901824410637,-57.3529265229835,12.));
#62341=CARTESIAN_POINT('Ctrl Pts',(41.4730568413518,-57.3399992214717,12.));
#62342=CARTESIAN_POINT('Ctrl Pts',(41.4559835343328,-57.3270836796911,12.));
#62343=CARTESIAN_POINT('Ctrl Pts',(41.4389625993948,-57.3141800540137,12.));
#62344=CARTESIAN_POINT('Ctrl Pts',(41.4219941163163,-57.3012885018151,12.));
#62345=CARTESIAN_POINT('Ctrl Pts',(41.4050781652938,-57.2884091815406,12.));
#62346=CARTESIAN_POINT('Ctrl Pts',(41.3882148268814,-57.2755422525844,12.));
#62347=CARTESIAN_POINT('Ctrl Pts',(41.3714041819224,-57.2626878751596,12.));
#62348=CARTESIAN_POINT('Ctrl Pts',(41.3546463114885,-57.2498462101879,12.));
#62349=CARTESIAN_POINT('Ctrl Pts',(41.3379412967875,-57.2370174191401,12.));
#62350=CARTESIAN_POINT('Ctrl Pts',(41.321289219149,-57.2242016640198,12.));
#62351=CARTESIAN_POINT('Ctrl Pts',(41.3046901602293,-57.2113991077302,12.));
#62352=CARTESIAN_POINT('Ctrl Pts',(41.2881442021863,-57.1986099143983,12.));
#62353=CARTESIAN_POINT('Ctrl Pts',(41.2716514278276,-57.1858342496538,12.));
#62354=CARTESIAN_POINT('Ctrl Pts',(41.2552119208466,-57.17307228108,12.));
#62355=CARTESIAN_POINT('Ctrl Pts',(41.2388257656559,-57.1603241779077,12.));
#62356=CARTESIAN_POINT('Ctrl Pts',(41.222493046943,-57.147590110182,12.));
#62357=CARTESIAN_POINT('Ctrl Pts',(41.2062138492915,-57.1348702480647,12.));
#62358=CARTESIAN_POINT('Ctrl Pts',(41.1899882567923,-57.1221647611207,12.));
#62359=CARTESIAN_POINT('Ctrl Pts',(41.1738163525902,-57.1094738174957,12.));
#62360=CARTESIAN_POINT('Ctrl Pts',(41.1576982197375,-57.0967975854874,12.));
#62361=CARTESIAN_POINT('Ctrl Pts',(41.1416339422117,-57.084136235426,12.));
#62362=CARTESIAN_POINT('Ctrl Pts',(41.1256236057443,-57.0714899412099,12.));
#62363=CARTESIAN_POINT('Ctrl Pts',(41.1096672990148,-57.0588588825298,12.));
#62364=CARTESIAN_POINT('Ctrl Pts',(41.0937651137549,-57.046243245068,12.));
#62365=CARTESIAN_POINT('Ctrl Pts',(41.0779171422438,-57.0336432158536,12.));
#62366=CARTESIAN_POINT('Ctrl Pts',(41.0621234751007,-57.0210589791788,12.));
#62367=CARTESIAN_POINT('Ctrl Pts',(41.0463841993608,-57.008490713042,12.));
#62368=CARTESIAN_POINT('Ctrl Pts',(41.0306993953989,-56.995938583472,12.));
#62369=CARTESIAN_POINT('Ctrl Pts',(41.0150691398947,-56.9834027500117,12.));
#62370=CARTESIAN_POINT('Ctrl Pts',(40.9994935117276,-56.9708833766137,12.));
#62371=CARTESIAN_POINT('Ctrl Pts',(40.9839725967121,-56.9583806404069,12.));
#62372=CARTESIAN_POINT('Ctrl Pts',(40.9685064933074,-56.9458947422608,12.));
#62373=CARTESIAN_POINT('Ctrl Pts',(40.9530953165031,-56.9334259140049,12.));
#62374=CARTESIAN_POINT('Ctrl Pts',(40.9377391857129,-56.9209743960992,12.));
#62375=CARTESIAN_POINT('Ctrl Pts',(40.9224382132427,-56.9085404164502,12.));
#62376=CARTESIAN_POINT('Ctrl Pts',(40.9071924937508,-56.8961241708861,12.));
#62377=CARTESIAN_POINT('Ctrl Pts',(40.8920020903293,-56.8837257978343,12.));
#62378=CARTESIAN_POINT('Ctrl Pts',(40.8768670342052,-56.8713453764905,12.));
#62379=CARTESIAN_POINT('Ctrl Pts',(40.864803275942,-56.8614554317668,12.));
#62380=CARTESIAN_POINT('Ctrl Pts',(40.8557803680278,-56.8540460739472,12.));
#62381=CARTESIAN_POINT('Ctrl Pts',(40.8497761671036,-56.8491101022591,12.));
#62382=CARTESIAN_POINT('Ctrl Pts',(40.8467768343956,-56.8466430164621,12.));
#62383=CARTESIAN_POINT('Ctrl Pts',(45.7706564944895,-58.4060826907792,-5.55111512312578E-16));
#62384=CARTESIAN_POINT('Ctrl Pts',(45.7706564944895,-58.4060826907792,4.));
#62385=CARTESIAN_POINT('Ctrl Pts',(45.7706564944895,-58.4060826907792,8.));
#62386=CARTESIAN_POINT('Ctrl Pts',(45.7706564944895,-58.4060826907792,12.));
#62387=CARTESIAN_POINT('Ctrl Pts',(45.7969367893064,-58.5127761886842,-5.55111512312578E-16));
#62388=CARTESIAN_POINT('Ctrl Pts',(45.7969367893064,-58.5127761886842,4.));
#62389=CARTESIAN_POINT('Ctrl Pts',(45.7969367893065,-58.5127761886843,8.00000000000001));
#62390=CARTESIAN_POINT('Ctrl Pts',(45.7969367893065,-58.5127761886843,12.));
#62391=CARTESIAN_POINT('Ctrl Pts',(45.7788617791412,-58.7146322050558,-5.55111512312578E-16));
#62392=CARTESIAN_POINT('Ctrl Pts',(45.7788617791412,-58.7146322050558,4.));
#62393=CARTESIAN_POINT('Ctrl Pts',(45.7788617791413,-58.7146322050559,7.99999999999999));
#62394=CARTESIAN_POINT('Ctrl Pts',(45.7788617791413,-58.7146322050559,12.));
#62395=CARTESIAN_POINT('Ctrl Pts',(45.6563266621664,-58.870677144318,-5.55111512312578E-16));
#62396=CARTESIAN_POINT('Ctrl Pts',(45.6563266621664,-58.870677144318,4.));
#62397=CARTESIAN_POINT('Ctrl Pts',(45.6563266621664,-58.870677144318,8.00000000000001));
#62398=CARTESIAN_POINT('Ctrl Pts',(45.6563266621664,-58.870677144318,12.));
#62399=CARTESIAN_POINT('Ctrl Pts',(45.5911481700253,-58.9211100416379,-5.55111512312578E-16));
#62400=CARTESIAN_POINT('Ctrl Pts',(45.5911481700253,-58.9211100416379,4.));
#62401=CARTESIAN_POINT('Ctrl Pts',(45.5911481700253,-58.9211100416379,8.));
#62402=CARTESIAN_POINT('Ctrl Pts',(45.5911481700253,-58.9211100416379,12.));
#62403=CARTESIAN_POINT('',(45.7706564944895,-58.4060826907792,2.77555756156289E-16));
#62404=CARTESIAN_POINT('',(45.5911481700253,-58.9211100416379,0.));
#62405=CARTESIAN_POINT('Ctrl Pts',(45.7706564944895,-58.4060826907792,-1.38777878078145E-16));
#62406=CARTESIAN_POINT('Ctrl Pts',(45.7969367893064,-58.5127761886842,-1.38777878078145E-16));
#62407=CARTESIAN_POINT('Ctrl Pts',(45.7866082120692,-58.6281224837537,-1.38777878078144E-16));
#62408=CARTESIAN_POINT('Ctrl Pts',(45.7421702122002,-58.7285100597671,-1.38777878078145E-16));
#62409=CARTESIAN_POINT('Ctrl Pts',(45.7088417122985,-58.8038007417771,-1.38777878078145E-16));
#62410=CARTESIAN_POINT('Ctrl Pts',(45.6563266621664,-58.870677144318,-1.38777878078145E-16));
#62411=CARTESIAN_POINT('Ctrl Pts',(45.5911481700253,-58.9211100416379,-1.38777878078145E-16));
#62412=CARTESIAN_POINT('',(45.5911481700253,-58.9211100416379,12.));
#62413=CARTESIAN_POINT('Ctrl Pts',(45.5911481700253,-58.9211100416379,-5.55111512312578E-16));
#62414=CARTESIAN_POINT('Ctrl Pts',(45.5911481700253,-58.9211100416379,4.));
#62415=CARTESIAN_POINT('Ctrl Pts',(45.5911481700253,-58.9211100416379,8.));
#62416=CARTESIAN_POINT('Ctrl Pts',(45.5911481700253,-58.9211100416379,12.));
#62417=CARTESIAN_POINT('',(45.7706564944895,-58.4060826907792,12.));
#62418=CARTESIAN_POINT('Ctrl Pts',(45.5911481700253,-58.9211100416379,12.));
#62419=CARTESIAN_POINT('Ctrl Pts',(45.6563266621664,-58.870677144318,12.));
#62420=CARTESIAN_POINT('Ctrl Pts',(45.7088417122985,-58.8038007417771,12.));
#62421=CARTESIAN_POINT('Ctrl Pts',(45.7421702122002,-58.7285100597671,12.));
#62422=CARTESIAN_POINT('Ctrl Pts',(45.7866082120692,-58.6281224837538,12.));
#62423=CARTESIAN_POINT('Ctrl Pts',(45.7969367893065,-58.5127761886843,12.));
#62424=CARTESIAN_POINT('Ctrl Pts',(45.7706564944895,-58.4060826907792,12.));
#62425=CARTESIAN_POINT('Ctrl Pts',(45.7706564944895,-58.4060826907792,12.));
#62426=CARTESIAN_POINT('Ctrl Pts',(45.7706564944895,-58.4060826907792,8.));
#62427=CARTESIAN_POINT('Ctrl Pts',(45.7706564944895,-58.4060826907792,4.));
#62428=CARTESIAN_POINT('Ctrl Pts',(45.7706564944895,-58.4060826907792,-5.55111512312578E-16));
#62429=CARTESIAN_POINT('Origin',(2.28269173065022E-10,-2.97323128204029E-10,
0.));
#62430=CARTESIAN_POINT('Origin',(2.28269173065022E-10,-2.97323128204029E-10,
12.));
#62431=CARTESIAN_POINT('Origin',(2.28269173065022E-10,-2.97323128204029E-10,
0.));
#62432=CARTESIAN_POINT('Ctrl Pts',(39.7746412831502,-62.9938720098767,0.));
#62433=CARTESIAN_POINT('Ctrl Pts',(39.7746412831502,-62.9938720098767,4.));
#62434=CARTESIAN_POINT('Ctrl Pts',(39.7746412831501,-62.9938720098767,8.));
#62435=CARTESIAN_POINT('Ctrl Pts',(39.7746412831501,-62.9938720098767,12.));
#62436=CARTESIAN_POINT('Ctrl Pts',(39.681729578236,-63.0525369183203,0.));
#62437=CARTESIAN_POINT('Ctrl Pts',(39.681729578236,-63.0525369183203,4.));
#62438=CARTESIAN_POINT('Ctrl Pts',(39.6817295782359,-63.0525369183203,8.00000000000001));
#62439=CARTESIAN_POINT('Ctrl Pts',(39.6817295782359,-63.0525369183203,12.));
#62440=CARTESIAN_POINT('Ctrl Pts',(39.4845131830967,-63.0992090147608,-7.30833037966997E-17));
#62441=CARTESIAN_POINT('Ctrl Pts',(39.4845131830967,-63.0992090147608,4.00000000000001));
#62442=CARTESIAN_POINT('Ctrl Pts',(39.4845131830966,-63.0992090147609,7.99999999999999));
#62443=CARTESIAN_POINT('Ctrl Pts',(39.4845131830966,-63.0992090147609,12.));
#62444=CARTESIAN_POINT('Ctrl Pts',(39.2977314459981,-63.0322949727904,-2.46611180233029E-16));
#62445=CARTESIAN_POINT('Ctrl Pts',(39.2977314459981,-63.0322949727904,3.99999999999999));
#62446=CARTESIAN_POINT('Ctrl Pts',(39.2977314459979,-63.0322949727905,8.00000000000001));
#62447=CARTESIAN_POINT('Ctrl Pts',(39.2977314459979,-63.0322949727905,12.));
#62448=CARTESIAN_POINT('Ctrl Pts',(39.2292784191464,-62.9864049293629,-3.30265160470605E-16));
#62449=CARTESIAN_POINT('Ctrl Pts',(39.2292784191464,-62.9864049293629,4.));
#62450=CARTESIAN_POINT('Ctrl Pts',(39.2292784191463,-62.986404929363,8.));
#62451=CARTESIAN_POINT('Ctrl Pts',(39.2292784191463,-62.986404929363,12.));
#62452=CARTESIAN_POINT('',(39.7746412831502,-62.9938720098767,0.));
#62453=CARTESIAN_POINT('',(39.2292784191464,-62.9864049293629,0.));
#62454=CARTESIAN_POINT('Ctrl Pts',(39.7746412831502,-62.9938720098767,2.74425517504384E-17));
#62455=CARTESIAN_POINT('Ctrl Pts',(39.681729578236,-63.0525369183203,2.74425517504384E-17));
#62456=CARTESIAN_POINT('Ctrl Pts',(39.5690344952992,-63.0792066877149,-1.431933613339E-17));
#62457=CARTESIAN_POINT('Ctrl Pts',(39.4597466476411,-63.0687871057916,-8.88794518179137E-17));
#62458=CARTESIAN_POINT('Ctrl Pts',(39.3777807618975,-63.0609724193492,-1.44799538581306E-16));
#62459=CARTESIAN_POINT('Ctrl Pts',(39.2977314459981,-63.0322949727904,-2.1916862848259E-16));
#62460=CARTESIAN_POINT('Ctrl Pts',(39.2292784191464,-62.9864049293629,-3.02822608720167E-16));
#62461=CARTESIAN_POINT('',(39.2292784191464,-62.9864049293629,12.));
#62462=CARTESIAN_POINT('Ctrl Pts',(39.2292784191464,-62.9864049293629,-3.30265160470605E-16));
#62463=CARTESIAN_POINT('Ctrl Pts',(39.2292784191464,-62.9864049293629,4.));
#62464=CARTESIAN_POINT('Ctrl Pts',(39.2292784191463,-62.986404929363,8.));
#62465=CARTESIAN_POINT('Ctrl Pts',(39.2292784191463,-62.986404929363,12.));
#62466=CARTESIAN_POINT('',(39.7746412831501,-62.9938720098767,12.));
#62467=CARTESIAN_POINT('Ctrl Pts',(39.2292784191463,-62.986404929363,12.));
#62468=CARTESIAN_POINT('Ctrl Pts',(39.2977314459979,-63.0322949727905,12.));
#62469=CARTESIAN_POINT('Ctrl Pts',(39.3777807618974,-63.0609724193492,12.));
#62470=CARTESIAN_POINT('Ctrl Pts',(39.459746647641,-63.0687871057917,12.));
#62471=CARTESIAN_POINT('Ctrl Pts',(39.5690344952991,-63.079206687715,12.));
#62472=CARTESIAN_POINT('Ctrl Pts',(39.6817295782359,-63.0525369183203,12.));
#62473=CARTESIAN_POINT('Ctrl Pts',(39.7746412831501,-62.9938720098767,12.));
#62474=CARTESIAN_POINT('Ctrl Pts',(39.7746412831501,-62.9938720098767,12.));
#62475=CARTESIAN_POINT('Ctrl Pts',(39.7746412831501,-62.9938720098767,8.));
#62476=CARTESIAN_POINT('Ctrl Pts',(39.7746412831502,-62.9938720098767,4.));
#62477=CARTESIAN_POINT('Ctrl Pts',(39.7746412831502,-62.9938720098767,0.));
#62478=CARTESIAN_POINT('Ctrl Pts',(35.7368311217509,-60.1903555511633,0.));
#62479=CARTESIAN_POINT('Ctrl Pts',(35.7368311217509,-60.1903555511633,12.));
#62480=CARTESIAN_POINT('Ctrl Pts',(35.7396040203974,-60.1930746580239,0.));
#62481=CARTESIAN_POINT('Ctrl Pts',(35.7396040203974,-60.1930746580239,12.));
#62482=CARTESIAN_POINT('Ctrl Pts',(35.7451551752456,-60.1985151474406,0.));
#62483=CARTESIAN_POINT('Ctrl Pts',(35.7451551752456,-60.1985151474406,12.));
#62484=CARTESIAN_POINT('Ctrl Pts',(35.7534979801871,-60.2066827086579,0.));
#62485=CARTESIAN_POINT('Ctrl Pts',(35.7534979801871,-60.2066827086579,12.));
#62486=CARTESIAN_POINT('Ctrl Pts',(35.7646538667299,-60.2175864449678,0.));
#62487=CARTESIAN_POINT('Ctrl Pts',(35.7646538667299,-60.2175864449678,12.));
#62488=CARTESIAN_POINT('Ctrl Pts',(35.7786523045783,-60.2312388621286,0.));
#62489=CARTESIAN_POINT('Ctrl Pts',(35.7786523045783,-60.2312388621286,12.));
#62490=CARTESIAN_POINT('Ctrl Pts',(35.7927043145165,-60.2449139865206,0.));
#62491=CARTESIAN_POINT('Ctrl Pts',(35.7927043145165,-60.2449139865206,12.));
#62492=CARTESIAN_POINT('Ctrl Pts',(35.8068098723386,-60.2586117365278,0.));
#62493=CARTESIAN_POINT('Ctrl Pts',(35.8068098723386,-60.2586117365278,12.));
#62494=CARTESIAN_POINT('Ctrl Pts',(35.8209689272574,-60.2723319687507,0.));
#62495=CARTESIAN_POINT('Ctrl Pts',(35.8209689272574,-60.2723319687507,12.));
#62496=CARTESIAN_POINT('Ctrl Pts',(35.8351814020424,-60.2860744798563,0.));
#62497=CARTESIAN_POINT('Ctrl Pts',(35.8351814020424,-60.2860744798563,12.));
#62498=CARTESIAN_POINT('Ctrl Pts',(35.8494472046784,-60.2998390330173,0.));
#62499=CARTESIAN_POINT('Ctrl Pts',(35.8494472046784,-60.2998390330173,12.));
#62500=CARTESIAN_POINT('Ctrl Pts',(35.8637662371635,-60.313625378281,0.));
#62501=CARTESIAN_POINT('Ctrl Pts',(35.8637662371635,-60.313625378281,12.));
#62502=CARTESIAN_POINT('Ctrl Pts',(35.878138405151,-60.3274332746781,0.));
#62503=CARTESIAN_POINT('Ctrl Pts',(35.878138405151,-60.3274332746781,12.));
#62504=CARTESIAN_POINT('Ctrl Pts',(35.8925636280633,-60.3412625135223,0.));
#62505=CARTESIAN_POINT('Ctrl Pts',(35.8925636280633,-60.3412625135223,12.));
#62506=CARTESIAN_POINT('Ctrl Pts',(35.9070418358501,-60.3551129108794,0.));
#62507=CARTESIAN_POINT('Ctrl Pts',(35.9070418358501,-60.3551129108794,12.));
#62508=CARTESIAN_POINT('Ctrl Pts',(35.9215729642219,-60.368984296546,0.));
#62509=CARTESIAN_POINT('Ctrl Pts',(35.9215729642219,-60.368984296546,12.));
#62510=CARTESIAN_POINT('Ctrl Pts',(35.9361569506956,-60.3828765049031,0.));
#62511=CARTESIAN_POINT('Ctrl Pts',(35.9361569506956,-60.3828765049031,12.));
#62512=CARTESIAN_POINT('Ctrl Pts',(35.9507937296727,-60.3967893635487,0.));
#62513=CARTESIAN_POINT('Ctrl Pts',(35.9507937296727,-60.3967893635487,12.));
#62514=CARTESIAN_POINT('Ctrl Pts',(35.9654832299627,-60.4107226875759,0.));
#62515=CARTESIAN_POINT('Ctrl Pts',(35.9654832299627,-60.4107226875759,12.));
#62516=CARTESIAN_POINT('Ctrl Pts',(35.9802253773535,-60.424676285496,0.));
#62517=CARTESIAN_POINT('Ctrl Pts',(35.9802253773535,-60.424676285496,12.));
#62518=CARTESIAN_POINT('Ctrl Pts',(35.9950200962175,-60.438649962949,0.));
#62519=CARTESIAN_POINT('Ctrl Pts',(35.9950200962175,-60.438649962949,12.));
#62520=CARTESIAN_POINT('Ctrl Pts',(36.0098673113557,-60.452643526964,0.));
#62521=CARTESIAN_POINT('Ctrl Pts',(36.0098673113557,-60.452643526964,12.));
#62522=CARTESIAN_POINT('Ctrl Pts',(36.0247669500867,-60.4666567908053,0.));
#62523=CARTESIAN_POINT('Ctrl Pts',(36.0247669500867,-60.4666567908053,12.));
#62524=CARTESIAN_POINT('Ctrl Pts',(36.0397189421617,-60.4806895737643,0.));
#62525=CARTESIAN_POINT('Ctrl Pts',(36.0397189421617,-60.4806895737643,12.));
#62526=CARTESIAN_POINT('Ctrl Pts',(36.0547232187682,-60.4947416988396,0.));
#62527=CARTESIAN_POINT('Ctrl Pts',(36.0547232187682,-60.4947416988396,12.));
#62528=CARTESIAN_POINT('Ctrl Pts',(36.0697797118377,-60.5088129911357,0.));
#62529=CARTESIAN_POINT('Ctrl Pts',(36.0697797118377,-60.5088129911357,12.));
#62530=CARTESIAN_POINT('Ctrl Pts',(36.0848883531969,-60.5229032759001,0.));
#62531=CARTESIAN_POINT('Ctrl Pts',(36.0848883531969,-60.5229032759001,12.));
#62532=CARTESIAN_POINT('Ctrl Pts',(36.1000490738532,-60.5370123768841,0.));
#62533=CARTESIAN_POINT('Ctrl Pts',(36.1000490738532,-60.5370123768841,12.));
#62534=CARTESIAN_POINT('Ctrl Pts',(36.1152618043757,-60.5511401172014,0.));
#62535=CARTESIAN_POINT('Ctrl Pts',(36.1152618043757,-60.5511401172014,12.));
#62536=CARTESIAN_POINT('Ctrl Pts',(36.1305264752195,-60.5652863200732,0.));
#62537=CARTESIAN_POINT('Ctrl Pts',(36.1305264752195,-60.5652863200732,12.));
#62538=CARTESIAN_POINT('Ctrl Pts',(36.1458430170425,-60.5794508095555,0.));
#62539=CARTESIAN_POINT('Ctrl Pts',(36.1458430170425,-60.5794508095555,12.));
#62540=CARTESIAN_POINT('Ctrl Pts',(36.1612113610758,-60.5936334114082,0.));
#62541=CARTESIAN_POINT('Ctrl Pts',(36.1612113610758,-60.5936334114082,12.));
#62542=CARTESIAN_POINT('Ctrl Pts',(36.1766314392624,-60.6078339534151,0.));
#62543=CARTESIAN_POINT('Ctrl Pts',(36.1766314392624,-60.6078339534151,12.));
#62544=CARTESIAN_POINT('Ctrl Pts',(36.1921031840618,-60.6220522649129,0.));
#62545=CARTESIAN_POINT('Ctrl Pts',(36.1921031840618,-60.6220522649129,12.));
#62546=CARTESIAN_POINT('Ctrl Pts',(36.2076265283261,-60.6362881765014,0.));
#62547=CARTESIAN_POINT('Ctrl Pts',(36.2076265283261,-60.6362881765014,12.));
#62548=CARTESIAN_POINT('Ctrl Pts',(36.2232014051549,-60.6505415197054,0.));
#62549=CARTESIAN_POINT('Ctrl Pts',(36.2232014051549,-60.6505415197054,12.));
#62550=CARTESIAN_POINT('Ctrl Pts',(36.2388277477225,-60.6648121265907,0.));
#62551=CARTESIAN_POINT('Ctrl Pts',(36.2388277477225,-60.6648121265907,12.));
#62552=CARTESIAN_POINT('Ctrl Pts',(36.2545054892911,-60.6790998297823,0.));
#62553=CARTESIAN_POINT('Ctrl Pts',(36.2545054892911,-60.6790998297823,12.));
#62554=CARTESIAN_POINT('Ctrl Pts',(36.2702345632883,-60.6934044626304,0.));
#62555=CARTESIAN_POINT('Ctrl Pts',(36.2702345632883,-60.6934044626304,12.));
#62556=CARTESIAN_POINT('Ctrl Pts',(36.2860149033587,-60.7077258593268,0.));
#62557=CARTESIAN_POINT('Ctrl Pts',(36.2860149033587,-60.7077258593268,12.));
#62558=CARTESIAN_POINT('Ctrl Pts',(36.3018464434204,-60.7220638550396,0.));
#62559=CARTESIAN_POINT('Ctrl Pts',(36.3018464434204,-60.7220638550396,12.));
#62560=CARTESIAN_POINT('Ctrl Pts',(36.3177291177148,-60.7364182860388,0.));
#62561=CARTESIAN_POINT('Ctrl Pts',(36.3177291177148,-60.7364182860388,12.));
#62562=CARTESIAN_POINT('Ctrl Pts',(36.3336628607844,-60.7507889896283,0.));
#62563=CARTESIAN_POINT('Ctrl Pts',(36.3336628607844,-60.7507889896283,12.));
#62564=CARTESIAN_POINT('Ctrl Pts',(36.349647607448,-60.7651758040791,0.));
#62565=CARTESIAN_POINT('Ctrl Pts',(36.349647607448,-60.7651758040791,12.));
#62566=CARTESIAN_POINT('Ctrl Pts',(36.3656832927733,-60.779578568563,0.));
#62567=CARTESIAN_POINT('Ctrl Pts',(36.3656832927733,-60.779578568563,12.));
#62568=CARTESIAN_POINT('Ctrl Pts',(36.38176985204,-60.7939971230781,0.));
#62569=CARTESIAN_POINT('Ctrl Pts',(36.38176985204,-60.7939971230781,12.));
#62570=CARTESIAN_POINT('Ctrl Pts',(36.3979072207175,-60.8084313084009,0.));
#62571=CARTESIAN_POINT('Ctrl Pts',(36.3979072207175,-60.8084313084009,12.));
#62572=CARTESIAN_POINT('Ctrl Pts',(36.414095334487,-60.8228809661179,0.));
#62573=CARTESIAN_POINT('Ctrl Pts',(36.414095334487,-60.8228809661179,12.));
#62574=CARTESIAN_POINT('Ctrl Pts',(36.4303341292497,-60.8373459386397,0.));
#62575=CARTESIAN_POINT('Ctrl Pts',(36.4303341292497,-60.8373459386397,12.));
#62576=CARTESIAN_POINT('Ctrl Pts',(36.4466235411353,-60.851826069218,0.));
#62577=CARTESIAN_POINT('Ctrl Pts',(36.4466235411353,-60.851826069218,12.));
#62578=CARTESIAN_POINT('Ctrl Pts',(36.4629635065038,-60.8663212019645,0.));
#62579=CARTESIAN_POINT('Ctrl Pts',(36.4629635065038,-60.8663212019645,12.));
#62580=CARTESIAN_POINT('Ctrl Pts',(36.4793539619459,-60.8808311818488,0.));
#62581=CARTESIAN_POINT('Ctrl Pts',(36.4793539619459,-60.8808311818488,12.));
#62582=CARTESIAN_POINT('Ctrl Pts',(36.4957948442832,-60.8953558546791,0.));
#62583=CARTESIAN_POINT('Ctrl Pts',(36.4957948442832,-60.8953558546791,12.));
#62584=CARTESIAN_POINT('Ctrl Pts',(36.5122860905611,-60.9098950670847,0.));
#62585=CARTESIAN_POINT('Ctrl Pts',(36.5122860905611,-60.9098950670847,12.));
#62586=CARTESIAN_POINT('Ctrl Pts',(36.5288276380417,-60.9244486664989,0.));
#62587=CARTESIAN_POINT('Ctrl Pts',(36.5288276380417,-60.9244486664989,12.));
#62588=CARTESIAN_POINT('Ctrl Pts',(36.5454194241866,-60.9390165011357,0.));
#62589=CARTESIAN_POINT('Ctrl Pts',(36.5454194241866,-60.9390165011357,12.));
#62590=CARTESIAN_POINT('Ctrl Pts',(36.5620613866616,-60.9535984199874,0.));
#62591=CARTESIAN_POINT('Ctrl Pts',(36.5620613866616,-60.9535984199874,12.));
#62592=CARTESIAN_POINT('Ctrl Pts',(36.5787534633416,-60.9681942728237,0.));
#62593=CARTESIAN_POINT('Ctrl Pts',(36.5787534633416,-60.9681942728237,12.));
#62594=CARTESIAN_POINT('Ctrl Pts',(36.5954955923109,-60.9828039101887,0.));
#62595=CARTESIAN_POINT('Ctrl Pts',(36.5954955923109,-60.9828039101887,12.));
#62596=CARTESIAN_POINT('Ctrl Pts',(36.61228771186,-60.9974271833981,0.));
#62597=CARTESIAN_POINT('Ctrl Pts',(36.61228771186,-60.9974271833981,12.));
#62598=CARTESIAN_POINT('Ctrl Pts',(36.6291297604775,-61.012063944535,0.));
#62599=CARTESIAN_POINT('Ctrl Pts',(36.6291297604775,-61.012063944535,12.));
#62600=CARTESIAN_POINT('Ctrl Pts',(36.6460216768553,-61.0267140464434,0.));
#62601=CARTESIAN_POINT('Ctrl Pts',(36.6460216768553,-61.0267140464434,12.));
#62602=CARTESIAN_POINT('Ctrl Pts',(36.6629633998886,-61.0413773427204,0.));
#62603=CARTESIAN_POINT('Ctrl Pts',(36.6629633998886,-61.0413773427204,12.));
#62604=CARTESIAN_POINT('Ctrl Pts',(36.6799548686741,-61.0560536877084,0.));
#62605=CARTESIAN_POINT('Ctrl Pts',(36.6799548686741,-61.0560536877084,12.));
#62606=CARTESIAN_POINT('Ctrl Pts',(36.6969960225019,-61.0707429364841,0.));
#62607=CARTESIAN_POINT('Ctrl Pts',(36.6969960225019,-61.0707429364841,12.));
#62608=CARTESIAN_POINT('Ctrl Pts',(36.7140868008479,-61.085444944851,0.));
#62609=CARTESIAN_POINT('Ctrl Pts',(36.7140868008479,-61.085444944851,12.));
#62610=CARTESIAN_POINT('Ctrl Pts',(36.7312271433799,-61.1001595693357,0.));
#62611=CARTESIAN_POINT('Ctrl Pts',(36.7312271433799,-61.1001595693357,12.));
#62612=CARTESIAN_POINT('Ctrl Pts',(36.7484169899591,-61.114886667182,0.));
#62613=CARTESIAN_POINT('Ctrl Pts',(36.7484169899591,-61.114886667182,12.));
#62614=CARTESIAN_POINT('Ctrl Pts',(36.7656562806381,-61.1296260963468,0.));
#62615=CARTESIAN_POINT('Ctrl Pts',(36.7656562806381,-61.1296260963468,12.));
#62616=CARTESIAN_POINT('Ctrl Pts',(36.782944955654,-61.1443777154926,0.));
#62617=CARTESIAN_POINT('Ctrl Pts',(36.782944955654,-61.1443777154926,12.));
#62618=CARTESIAN_POINT('Ctrl Pts',(36.8002829554221,-61.1591413839809,0.));
#62619=CARTESIAN_POINT('Ctrl Pts',(36.8002829554221,-61.1591413839809,12.));
#62620=CARTESIAN_POINT('Ctrl Pts',(36.8176702205436,-61.1739169618688,0.));
#62621=CARTESIAN_POINT('Ctrl Pts',(36.8176702205436,-61.1739169618688,12.));
#62622=CARTESIAN_POINT('Ctrl Pts',(36.8351066918043,-61.1887043099026,0.));
#62623=CARTESIAN_POINT('Ctrl Pts',(36.8351066918043,-61.1887043099026,12.));
#62624=CARTESIAN_POINT('Ctrl Pts',(36.8525923101736,-61.2035032895121,0.));
#62625=CARTESIAN_POINT('Ctrl Pts',(36.8525923101736,-61.2035032895121,12.));
#62626=CARTESIAN_POINT('Ctrl Pts',(36.8701270167954,-61.2183137628031,0.));
#62627=CARTESIAN_POINT('Ctrl Pts',(36.8701270167954,-61.2183137628031,12.));
#62628=CARTESIAN_POINT('Ctrl Pts',(36.8877107529844,-61.2331355925513,0.));
#62629=CARTESIAN_POINT('Ctrl Pts',(36.8877107529844,-61.2331355925513,12.));
#62630=CARTESIAN_POINT('Ctrl Pts',(36.9053434602324,-61.2479686421979,0.));
#62631=CARTESIAN_POINT('Ctrl Pts',(36.9053434602324,-61.2479686421979,12.));
#62632=CARTESIAN_POINT('Ctrl Pts',(36.9230250802079,-61.2628127758443,0.));
#62633=CARTESIAN_POINT('Ctrl Pts',(36.9230250802079,-61.2628127758443,12.));
#62634=CARTESIAN_POINT('Ctrl Pts',(36.9407555547542,-61.2776678582473,0.));
#62635=CARTESIAN_POINT('Ctrl Pts',(36.9407555547542,-61.2776678582473,12.));
#62636=CARTESIAN_POINT('Ctrl Pts',(36.9585348258798,-61.2925337548113,0.));
#62637=CARTESIAN_POINT('Ctrl Pts',(36.9585348258798,-61.2925337548113,12.));
#62638=CARTESIAN_POINT('Ctrl Pts',(36.976362835757,-61.3074103315834,0.));
#62639=CARTESIAN_POINT('Ctrl Pts',(36.976362835757,-61.3074103315834,12.));
#62640=CARTESIAN_POINT('Ctrl Pts',(36.994239526729,-61.3222974552519,0.));
#62641=CARTESIAN_POINT('Ctrl Pts',(36.994239526729,-61.3222974552519,12.));
#62642=CARTESIAN_POINT('Ctrl Pts',(37.0121648413088,-61.3371949931396,0.));
#62643=CARTESIAN_POINT('Ctrl Pts',(37.0121648413088,-61.3371949931396,12.));
#62644=CARTESIAN_POINT('Ctrl Pts',(37.0301387221766,-61.352102813199,0.));
#62645=CARTESIAN_POINT('Ctrl Pts',(37.0301387221766,-61.352102813199,12.));
#62646=CARTESIAN_POINT('Ctrl Pts',(37.0481611121698,-61.367020784004,0.));
#62647=CARTESIAN_POINT('Ctrl Pts',(37.0481611121698,-61.367020784004,12.));
#62648=CARTESIAN_POINT('Ctrl Pts',(37.0662319542827,-61.3819487747458,0.));
#62649=CARTESIAN_POINT('Ctrl Pts',(37.0662319542827,-61.3819487747458,12.));
#62650=CARTESIAN_POINT('Ctrl Pts',(37.0843511916729,-61.3968866552294,0.));
#62651=CARTESIAN_POINT('Ctrl Pts',(37.0843511916729,-61.3968866552294,12.));
#62652=CARTESIAN_POINT('Ctrl Pts',(37.1025187676597,-61.411834295869,0.));
#62653=CARTESIAN_POINT('Ctrl Pts',(37.1025187676597,-61.411834295869,12.));
#62654=CARTESIAN_POINT('Ctrl Pts',(37.1207346257229,-61.4267915676833,0.));
#62655=CARTESIAN_POINT('Ctrl Pts',(37.1207346257229,-61.4267915676833,12.));
#62656=CARTESIAN_POINT('Ctrl Pts',(37.138998709492,-61.4417583422888,0.));
#62657=CARTESIAN_POINT('Ctrl Pts',(37.138998709492,-61.4417583422888,12.));
#62658=CARTESIAN_POINT('Ctrl Pts',(37.157310962747,-61.4567344918946,0.));
#62659=CARTESIAN_POINT('Ctrl Pts',(37.157310962747,-61.4567344918946,12.));
#62660=CARTESIAN_POINT('Ctrl Pts',(37.175671329425,-61.471719889301,0.));
#62661=CARTESIAN_POINT('Ctrl Pts',(37.175671329425,-61.471719889301,12.));
#62662=CARTESIAN_POINT('Ctrl Pts',(37.1940797536182,-61.4867144078939,0.));
#62663=CARTESIAN_POINT('Ctrl Pts',(37.1940797536182,-61.4867144078939,12.));
#62664=CARTESIAN_POINT('Ctrl Pts',(37.2125361795727,-61.5017179216404,0.));
#62665=CARTESIAN_POINT('Ctrl Pts',(37.2125361795727,-61.5017179216404,12.));
#62666=CARTESIAN_POINT('Ctrl Pts',(37.2310405516775,-61.5167303050823,0.));
#62667=CARTESIAN_POINT('Ctrl Pts',(37.2310405516775,-61.5167303050823,12.));
#62668=CARTESIAN_POINT('Ctrl Pts',(37.2495928144661,-61.5317514333319,0.));
#62669=CARTESIAN_POINT('Ctrl Pts',(37.2495928144661,-61.5317514333319,12.));
#62670=CARTESIAN_POINT('Ctrl Pts',(37.2681929126218,-61.5467811820685,0.));
#62671=CARTESIAN_POINT('Ctrl Pts',(37.2681929126218,-61.5467811820685,12.));
#62672=CARTESIAN_POINT('Ctrl Pts',(37.286840790977,-61.5618194275348,0.));
#62673=CARTESIAN_POINT('Ctrl Pts',(37.286840790977,-61.5618194275348,12.));
#62674=CARTESIAN_POINT('Ctrl Pts',(37.3055363945108,-61.5768660465313,0.));
#62675=CARTESIAN_POINT('Ctrl Pts',(37.3055363945108,-61.5768660465313,12.));
#62676=CARTESIAN_POINT('Ctrl Pts',(37.3242796683395,-61.591920916412,0.));
#62677=CARTESIAN_POINT('Ctrl Pts',(37.3242796683395,-61.591920916412,12.));
#62678=CARTESIAN_POINT('Ctrl Pts',(37.3430705577178,-61.6069839150804,0.));
#62679=CARTESIAN_POINT('Ctrl Pts',(37.3430705577178,-61.6069839150804,12.));
#62680=CARTESIAN_POINT('Ctrl Pts',(37.3619090080447,-61.6220549209862,0.));
#62681=CARTESIAN_POINT('Ctrl Pts',(37.3619090080447,-61.6220549209862,12.));
#62682=CARTESIAN_POINT('Ctrl Pts',(37.3807949648623,-61.6371338131208,0.));
#62683=CARTESIAN_POINT('Ctrl Pts',(37.3807949648623,-61.6371338131208,12.));
#62684=CARTESIAN_POINT('Ctrl Pts',(37.3997283738534,-61.6522204710133,0.));
#62685=CARTESIAN_POINT('Ctrl Pts',(37.3997283738534,-61.6522204710133,12.));
#62686=CARTESIAN_POINT('Ctrl Pts',(37.4187091808324,-61.6673147747249,0.));
#62687=CARTESIAN_POINT('Ctrl Pts',(37.4187091808324,-61.6673147747249,12.));
#62688=CARTESIAN_POINT('Ctrl Pts',(37.4377373317456,-61.6824166048453,0.));
#62689=CARTESIAN_POINT('Ctrl Pts',(37.4377373317456,-61.6824166048453,12.));
#62690=CARTESIAN_POINT('Ctrl Pts',(37.4568127726776,-61.69752584249,0.));
#62691=CARTESIAN_POINT('Ctrl Pts',(37.4568127726776,-61.69752584249,12.));
#62692=CARTESIAN_POINT('Ctrl Pts',(37.475935449851,-61.7126423692965,0.));
#62693=CARTESIAN_POINT('Ctrl Pts',(37.475935449851,-61.7126423692965,12.));
#62694=CARTESIAN_POINT('Ctrl Pts',(37.4951053096235,-61.7277660674203,0.));
#62695=CARTESIAN_POINT('Ctrl Pts',(37.4951053096235,-61.7277660674203,12.));
#62696=CARTESIAN_POINT('Ctrl Pts',(37.5143222984794,-61.7428968195295,0.));
#62697=CARTESIAN_POINT('Ctrl Pts',(37.5143222984794,-61.7428968195295,12.));
#62698=CARTESIAN_POINT('Ctrl Pts',(37.5335863630286,-61.7580345088013,0.));
#62699=CARTESIAN_POINT('Ctrl Pts',(37.5335863630286,-61.7580345088013,12.));
#62700=CARTESIAN_POINT('Ctrl Pts',(37.5528974500142,-61.7731790189191,0.));
#62701=CARTESIAN_POINT('Ctrl Pts',(37.5528974500142,-61.7731790189191,12.));
#62702=CARTESIAN_POINT('Ctrl Pts',(37.5722555063112,-61.7883302340689,0.));
#62703=CARTESIAN_POINT('Ctrl Pts',(37.5722555063112,-61.7883302340689,12.));
#62704=CARTESIAN_POINT('Ctrl Pts',(37.5916604789252,-61.8034880389362,0.));
#62705=CARTESIAN_POINT('Ctrl Pts',(37.5916604789252,-61.8034880389362,12.));
#62706=CARTESIAN_POINT('Ctrl Pts',(37.6111123149836,-61.8186523187011,0.));
#62707=CARTESIAN_POINT('Ctrl Pts',(37.6111123149836,-61.8186523187011,12.));
#62708=CARTESIAN_POINT('Ctrl Pts',(37.6306109617341,-61.8338229590345,0.));
#62709=CARTESIAN_POINT('Ctrl Pts',(37.6306109617341,-61.8338229590345,12.));
#62710=CARTESIAN_POINT('Ctrl Pts',(37.6501563665518,-61.848999846095,0.));
#62711=CARTESIAN_POINT('Ctrl Pts',(37.6501563665518,-61.848999846095,12.));
#62712=CARTESIAN_POINT('Ctrl Pts',(37.6697484769389,-61.8641828665257,0.));
#62713=CARTESIAN_POINT('Ctrl Pts',(37.6697484769389,-61.8641828665257,12.));
#62714=CARTESIAN_POINT('Ctrl Pts',(37.689387240523,-61.879371907451,0.));
#62715=CARTESIAN_POINT('Ctrl Pts',(37.689387240523,-61.879371907451,12.));
#62716=CARTESIAN_POINT('Ctrl Pts',(37.7090726050489,-61.8945668564714,0.));
#62717=CARTESIAN_POINT('Ctrl Pts',(37.7090726050489,-61.8945668564714,12.));
#62718=CARTESIAN_POINT('Ctrl Pts',(37.7288045183765,-61.9097676016616,0.));
#62719=CARTESIAN_POINT('Ctrl Pts',(37.7288045183765,-61.9097676016616,12.));
#62720=CARTESIAN_POINT('Ctrl Pts',(37.748582928488,-61.9249740315664,0.));
#62721=CARTESIAN_POINT('Ctrl Pts',(37.748582928488,-61.9249740315664,12.));
#62722=CARTESIAN_POINT('Ctrl Pts',(37.7684077834877,-61.940186035198,0.));
#62723=CARTESIAN_POINT('Ctrl Pts',(37.7684077834877,-61.940186035198,12.));
#62724=CARTESIAN_POINT('Ctrl Pts',(37.7882790316012,-61.9554035020334,0.));
#62725=CARTESIAN_POINT('Ctrl Pts',(37.7882790316012,-61.9554035020334,12.));
#62726=CARTESIAN_POINT('Ctrl Pts',(37.808196621168,-61.9706263220101,0.));
#62727=CARTESIAN_POINT('Ctrl Pts',(37.808196621168,-61.9706263220101,12.));
#62728=CARTESIAN_POINT('Ctrl Pts',(37.8281605006371,-61.9858543855221,0.));
#62729=CARTESIAN_POINT('Ctrl Pts',(37.8281605006371,-61.9858543855221,12.));
#62730=CARTESIAN_POINT('Ctrl Pts',(37.8481706185742,-62.0010875834176,0.));
#62731=CARTESIAN_POINT('Ctrl Pts',(37.8481706185742,-62.0010875834176,12.));
#62732=CARTESIAN_POINT('Ctrl Pts',(37.8682269236628,-62.0163258069954,0.));
#62733=CARTESIAN_POINT('Ctrl Pts',(37.8682269236628,-62.0163258069954,12.));
#62734=CARTESIAN_POINT('Ctrl Pts',(37.888329364703,-62.0315689480022,0.));
#62735=CARTESIAN_POINT('Ctrl Pts',(37.888329364703,-62.0315689480022,12.));
#62736=CARTESIAN_POINT('Ctrl Pts',(37.9084778906054,-62.0468168986289,0.));
#62737=CARTESIAN_POINT('Ctrl Pts',(37.9084778906054,-62.0468168986289,12.));
#62738=CARTESIAN_POINT('Ctrl Pts',(37.9286724503849,-62.0620695515072,0.));
#62739=CARTESIAN_POINT('Ctrl Pts',(37.9286724503849,-62.0620695515072,12.));
#62740=CARTESIAN_POINT('Ctrl Pts',(37.9489129931685,-62.0773267997072,0.));
#62741=CARTESIAN_POINT('Ctrl Pts',(37.9489129931685,-62.0773267997072,12.));
#62742=CARTESIAN_POINT('Ctrl Pts',(37.9691994681963,-62.0925885367346,0.));
#62743=CARTESIAN_POINT('Ctrl Pts',(37.9691994681963,-62.0925885367346,12.));
#62744=CARTESIAN_POINT('Ctrl Pts',(37.9895318248212,-62.107854656528,0.));
#62745=CARTESIAN_POINT('Ctrl Pts',(37.9895318248212,-62.107854656528,12.));
#62746=CARTESIAN_POINT('Ctrl Pts',(38.0099100125041,-62.1231250534558,0.));
#62747=CARTESIAN_POINT('Ctrl Pts',(38.0099100125041,-62.1231250534558,12.));
#62748=CARTESIAN_POINT('Ctrl Pts',(38.0303339808059,-62.1383996223136,0.));
#62749=CARTESIAN_POINT('Ctrl Pts',(38.0303339808059,-62.1383996223136,12.));
#62750=CARTESIAN_POINT('Ctrl Pts',(38.0508036793944,-62.153678258321,0.));
#62751=CARTESIAN_POINT('Ctrl Pts',(38.0508036793944,-62.153678258321,12.));
#62752=CARTESIAN_POINT('Ctrl Pts',(38.0713190580466,-62.1689608571182,0.));
#62753=CARTESIAN_POINT('Ctrl Pts',(38.0713190580466,-62.1689608571182,12.));
#62754=CARTESIAN_POINT('Ctrl Pts',(38.0918800666479,-62.1842473147626,0.));
#62755=CARTESIAN_POINT('Ctrl Pts',(38.0918800666479,-62.1842473147626,12.));
#62756=CARTESIAN_POINT('Ctrl Pts',(38.1124866551884,-62.1995375277253,0.));
#62757=CARTESIAN_POINT('Ctrl Pts',(38.1124866551884,-62.1995375277253,12.));
#62758=CARTESIAN_POINT('Ctrl Pts',(38.1331387737528,-62.2148313928859,0.));
#62759=CARTESIAN_POINT('Ctrl Pts',(38.1331387737528,-62.2148313928859,12.));
#62760=CARTESIAN_POINT('Ctrl Pts',(38.1538363725264,-62.2301288075318,0.));
#62761=CARTESIAN_POINT('Ctrl Pts',(38.1538363725264,-62.2301288075318,12.));
#62762=CARTESIAN_POINT('Ctrl Pts',(38.1745794017997,-62.245429669358,0.));
#62763=CARTESIAN_POINT('Ctrl Pts',(38.1745794017997,-62.245429669358,12.));
#62764=CARTESIAN_POINT('Ctrl Pts',(38.1953678119692,-62.2607338764655,0.));
#62765=CARTESIAN_POINT('Ctrl Pts',(38.1953678119692,-62.2607338764655,12.));
#62766=CARTESIAN_POINT('Ctrl Pts',(38.2162015535351,-62.2760413273601,0.));
#62767=CARTESIAN_POINT('Ctrl Pts',(38.2162015535351,-62.2760413273601,12.));
#62768=CARTESIAN_POINT('Ctrl Pts',(38.2370805770931,-62.2913519209517,0.));
#62769=CARTESIAN_POINT('Ctrl Pts',(38.2370805770931,-62.2913519209517,12.));
#62770=CARTESIAN_POINT('Ctrl Pts',(38.2580048333356,-62.3066655565497,0.));
#62771=CARTESIAN_POINT('Ctrl Pts',(38.2580048333356,-62.3066655565497,12.));
#62772=CARTESIAN_POINT('Ctrl Pts',(38.2789742730559,-62.3219821338564,0.));
#62773=CARTESIAN_POINT('Ctrl Pts',(38.2789742730559,-62.3219821338564,12.));
#62774=CARTESIAN_POINT('Ctrl Pts',(38.2999888471474,-62.337301552961,0.));
#62775=CARTESIAN_POINT('Ctrl Pts',(38.2999888471474,-62.337301552961,12.));
#62776=CARTESIAN_POINT('Ctrl Pts',(38.3210485066003,-62.3526237143338,0.));
#62777=CARTESIAN_POINT('Ctrl Pts',(38.3210485066003,-62.3526237143338,12.));
#62778=CARTESIAN_POINT('Ctrl Pts',(38.3421532024915,-62.3679485188178,0.));
#62779=CARTESIAN_POINT('Ctrl Pts',(38.3421532024915,-62.3679485188178,12.));
#62780=CARTESIAN_POINT('Ctrl Pts',(38.3633028859835,-62.3832758676281,0.));
#62781=CARTESIAN_POINT('Ctrl Pts',(38.3633028859835,-62.3832758676281,12.));
#62782=CARTESIAN_POINT('Ctrl Pts',(38.384497508335,-62.3986056623587,0.));
#62783=CARTESIAN_POINT('Ctrl Pts',(38.384497508335,-62.3986056623587,12.));
#62784=CARTESIAN_POINT('Ctrl Pts',(38.4057370209054,-62.4139378049891,0.));
#62785=CARTESIAN_POINT('Ctrl Pts',(38.4057370209054,-62.4139378049891,12.));
#62786=CARTESIAN_POINT('Ctrl Pts',(38.4270213751567,-62.42927219789,0.));
#62787=CARTESIAN_POINT('Ctrl Pts',(38.4270213751567,-62.42927219789,12.));
#62788=CARTESIAN_POINT('Ctrl Pts',(38.4483505226512,-62.4446087438304,0.));
#62789=CARTESIAN_POINT('Ctrl Pts',(38.4483505226512,-62.4446087438304,12.));
#62790=CARTESIAN_POINT('Ctrl Pts',(38.4697244150473,-62.4599473459799,0.));
#62791=CARTESIAN_POINT('Ctrl Pts',(38.4697244150473,-62.4599473459799,12.));
#62792=CARTESIAN_POINT('Ctrl Pts',(38.4911430040988,-62.4752879078842,0.));
#62793=CARTESIAN_POINT('Ctrl Pts',(38.4911430040988,-62.4752879078842,12.));
#62794=CARTESIAN_POINT('Ctrl Pts',(38.5126062416496,-62.4906303334435,0.));
#62795=CARTESIAN_POINT('Ctrl Pts',(38.5126062416496,-62.4906303334435,12.));
#62796=CARTESIAN_POINT('Ctrl Pts',(38.5341140796247,-62.5059745268899,0.));
#62797=CARTESIAN_POINT('Ctrl Pts',(38.5341140796247,-62.5059745268899,12.));
#62798=CARTESIAN_POINT('Ctrl Pts',(38.5556664700201,-62.5213203927672,0.));
#62799=CARTESIAN_POINT('Ctrl Pts',(38.5556664700201,-62.5213203927672,12.));
#62800=CARTESIAN_POINT('Ctrl Pts',(38.5772633648841,-62.5366678359035,0.));
#62801=CARTESIAN_POINT('Ctrl Pts',(38.5772633648841,-62.5366678359035,12.));
#62802=CARTESIAN_POINT('Ctrl Pts',(38.5989047163401,-62.5520167614529,0.));
#62803=CARTESIAN_POINT('Ctrl Pts',(38.5989047163401,-62.5520167614529,12.));
#62804=CARTESIAN_POINT('Ctrl Pts',(38.6205904766078,-62.567367074937,0.));
#62805=CARTESIAN_POINT('Ctrl Pts',(38.6205904766078,-62.567367074937,12.));
#62806=CARTESIAN_POINT('Ctrl Pts',(38.6423205980214,-62.5827186822923,0.));
#62807=CARTESIAN_POINT('Ctrl Pts',(38.6423205980214,-62.5827186822923,12.));
#62808=CARTESIAN_POINT('Ctrl Pts',(38.6640950330418,-62.5980714899048,0.));
#62809=CARTESIAN_POINT('Ctrl Pts',(38.6640950330418,-62.5980714899048,12.));
#62810=CARTESIAN_POINT('Ctrl Pts',(38.6859137342726,-62.6134254046731,0.));
#62811=CARTESIAN_POINT('Ctrl Pts',(38.6859137342726,-62.6134254046731,12.));
#62812=CARTESIAN_POINT('Ctrl Pts',(38.7077766544411,-62.6287803339534,0.));
#62813=CARTESIAN_POINT('Ctrl Pts',(38.7077766544411,-62.6287803339534,12.));
#62814=CARTESIAN_POINT('Ctrl Pts',(38.7296837463605,-62.6441361854406,0.));
#62815=CARTESIAN_POINT('Ctrl Pts',(38.7296837463605,-62.6441361854406,12.));
#62816=CARTESIAN_POINT('Ctrl Pts',(38.7516349628902,-62.6594928670626,0.));
#62817=CARTESIAN_POINT('Ctrl Pts',(38.7516349628902,-62.6594928670626,12.));
#62818=CARTESIAN_POINT('Ctrl Pts',(38.7736302568982,-62.6748502868836,0.));
#62819=CARTESIAN_POINT('Ctrl Pts',(38.7736302568982,-62.6748502868836,12.));
#62820=CARTESIAN_POINT('Ctrl Pts',(38.7956695812032,-62.6902083529698,0.));
#62821=CARTESIAN_POINT('Ctrl Pts',(38.7956695812032,-62.6902083529698,12.));
#62822=CARTESIAN_POINT('Ctrl Pts',(38.8177528885687,-62.7055669733811,0.));
#62823=CARTESIAN_POINT('Ctrl Pts',(38.8177528885687,-62.7055669733811,12.));
#62824=CARTESIAN_POINT('Ctrl Pts',(38.8398801318185,-62.7209260564505,0.));
#62825=CARTESIAN_POINT('Ctrl Pts',(38.8398801318185,-62.7209260564505,12.));
#62826=CARTESIAN_POINT('Ctrl Pts',(38.8620512639239,-62.7362855110052,0.));
#62827=CARTESIAN_POINT('Ctrl Pts',(38.8620512639239,-62.7362855110052,12.));
#62828=CARTESIAN_POINT('Ctrl Pts',(38.8842662380984,-62.7516452466129,0.));
#62829=CARTESIAN_POINT('Ctrl Pts',(38.8842662380984,-62.7516452466129,12.));
#62830=CARTESIAN_POINT('Ctrl Pts',(38.9065250078824,-62.7670051738131,0.));
#62831=CARTESIAN_POINT('Ctrl Pts',(38.9065250078824,-62.7670051738131,12.));
#62832=CARTESIAN_POINT('Ctrl Pts',(38.928827527232,-62.7823652043677,0.));
#62833=CARTESIAN_POINT('Ctrl Pts',(38.928827527232,-62.7823652043677,12.));
#62834=CARTESIAN_POINT('Ctrl Pts',(38.9511737503146,-62.797725250709,0.));
#62835=CARTESIAN_POINT('Ctrl Pts',(38.9511737503146,-62.797725250709,12.));
#62836=CARTESIAN_POINT('Ctrl Pts',(38.9735636313073,-62.8130852254004,0.));
#62837=CARTESIAN_POINT('Ctrl Pts',(38.9735636313073,-62.8130852254004,12.));
#62838=CARTESIAN_POINT('Ctrl Pts',(38.9959971241695,-62.8284450405451,0.));
#62839=CARTESIAN_POINT('Ctrl Pts',(38.9959971241695,-62.8284450405451,12.));
#62840=CARTESIAN_POINT('Ctrl Pts',(39.018474182465,-62.8438046073237,0.));
#62841=CARTESIAN_POINT('Ctrl Pts',(39.018474182465,-62.8438046073237,12.));
#62842=CARTESIAN_POINT('Ctrl Pts',(39.0409947590519,-62.859163835209,0.));
#62843=CARTESIAN_POINT('Ctrl Pts',(39.0409947590519,-62.859163835209,12.));
#62844=CARTESIAN_POINT('Ctrl Pts',(39.0635588063309,-62.8745226326046,0.));
#62845=CARTESIAN_POINT('Ctrl Pts',(39.0635588063309,-62.8745226326046,12.));
#62846=CARTESIAN_POINT('Ctrl Pts',(39.0861662767964,-62.8898809082658,0.));
#62847=CARTESIAN_POINT('Ctrl Pts',(39.0861662767964,-62.8898809082658,12.));
#62848=CARTESIAN_POINT('Ctrl Pts',(39.1088171235144,-62.9052385725416,0.));
#62849=CARTESIAN_POINT('Ctrl Pts',(39.1088171235144,-62.9052385725416,12.));
#62850=CARTESIAN_POINT('Ctrl Pts',(39.1315113005745,-62.9205955385551,0.));
#62851=CARTESIAN_POINT('Ctrl Pts',(39.1315113005745,-62.9205955385551,12.));
#62852=CARTESIAN_POINT('Ctrl Pts',(39.1542487636708,-62.9359517237352,0.));
#62853=CARTESIAN_POINT('Ctrl Pts',(39.1542487636708,-62.9359517237352,12.));
#62854=CARTESIAN_POINT('Ctrl Pts',(39.1770294702367,-62.9513070501777,0.));
#62855=CARTESIAN_POINT('Ctrl Pts',(39.1770294702367,-62.9513070501777,12.));
#62856=CARTESIAN_POINT('Ctrl Pts',(39.199853378159,-62.9666614412627,0.));
#62857=CARTESIAN_POINT('Ctrl Pts',(39.199853378159,-62.9666614412627,12.));
#62858=CARTESIAN_POINT('Ctrl Pts',(39.2227204447583,-62.9820148189849,0.));
#62859=CARTESIAN_POINT('Ctrl Pts',(39.2227204447583,-62.9820148189849,12.));
#62860=CARTESIAN_POINT('Ctrl Pts',(39.2456306256092,-62.9973671008685,0.));
#62861=CARTESIAN_POINT('Ctrl Pts',(39.2456306256092,-62.9973671008685,12.));
#62862=CARTESIAN_POINT('Ctrl Pts',(39.2685838735411,-63.0127181973702,0.));
#62863=CARTESIAN_POINT('Ctrl Pts',(39.2685838735411,-63.0127181973702,12.));
#62864=CARTESIAN_POINT('Ctrl Pts',(39.2915801372468,-63.0280680082522,0.));
#62865=CARTESIAN_POINT('Ctrl Pts',(39.2915801372468,-63.0280680082522,12.));
#62866=CARTESIAN_POINT('Ctrl Pts',(39.3146193632546,-63.0434164278221,0.));
#62867=CARTESIAN_POINT('Ctrl Pts',(39.3146193632546,-63.0434164278221,12.));
#62868=CARTESIAN_POINT('Ctrl Pts',(39.3377014983757,-63.0587633513993,0.));
#62869=CARTESIAN_POINT('Ctrl Pts',(39.3377014983757,-63.0587633513993,12.));
#62870=CARTESIAN_POINT('Ctrl Pts',(39.3608264920487,-63.0741086815957,0.));
#62871=CARTESIAN_POINT('Ctrl Pts',(39.3608264920487,-63.0741086815957,12.));
#62872=CARTESIAN_POINT('Ctrl Pts',(39.3839942985688,-63.0894523341238,0.));
#62873=CARTESIAN_POINT('Ctrl Pts',(39.3839942985688,-63.0894523341238,12.));
#62874=CARTESIAN_POINT('Ctrl Pts',(39.4072048797401,-63.1047942451583,0.));
#62875=CARTESIAN_POINT('Ctrl Pts',(39.4072048797401,-63.1047942451583,12.));
#62876=CARTESIAN_POINT('Ctrl Pts',(39.4304582059507,-63.1201343730643,0.));
#62877=CARTESIAN_POINT('Ctrl Pts',(39.4304582059507,-63.1201343730643,12.));
#62878=CARTESIAN_POINT('Ctrl Pts',(39.4537542551852,-63.1354726927781,0.));
#62879=CARTESIAN_POINT('Ctrl Pts',(39.4537542551852,-63.1354726927781,12.));
#62880=CARTESIAN_POINT('Ctrl Pts',(39.4724252610807,-63.1477418921889,0.));
#62881=CARTESIAN_POINT('Ctrl Pts',(39.4724252610807,-63.1477418921889,12.));
#62882=CARTESIAN_POINT('Ctrl Pts',(39.4864477303614,-63.1569429707564,0.));
#62883=CARTESIAN_POINT('Ctrl Pts',(39.4864477303614,-63.1569429707564,12.));
#62884=CARTESIAN_POINT('Ctrl Pts',(39.4958045828059,-63.1630766582674,0.));
#62885=CARTESIAN_POINT('Ctrl Pts',(39.4958045828059,-63.1630766582674,12.));
#62886=CARTESIAN_POINT('Ctrl Pts',(39.5004851439258,-63.1661434108059,0.));
#62887=CARTESIAN_POINT('Ctrl Pts',(39.5004851439258,-63.1661434108059,12.));
#62888=CARTESIAN_POINT('',(35.7368311217509,-60.1903555511633,0.));
#62889=CARTESIAN_POINT('Ctrl Pts',(35.7368311217509,-60.1903555511633,0.));
#62890=CARTESIAN_POINT('Ctrl Pts',(35.7396040203974,-60.1930746580239,0.));
#62891=CARTESIAN_POINT('Ctrl Pts',(35.7451551752456,-60.1985151474406,0.));
#62892=CARTESIAN_POINT('Ctrl Pts',(35.7534979801871,-60.2066827086579,0.));
#62893=CARTESIAN_POINT('Ctrl Pts',(35.7646538667299,-60.2175864449678,0.));
#62894=CARTESIAN_POINT('Ctrl Pts',(35.7786523045783,-60.2312388621286,0.));
#62895=CARTESIAN_POINT('Ctrl Pts',(35.7927043145165,-60.2449139865206,0.));
#62896=CARTESIAN_POINT('Ctrl Pts',(35.8068098723386,-60.2586117365278,0.));
#62897=CARTESIAN_POINT('Ctrl Pts',(35.8209689272574,-60.2723319687507,0.));
#62898=CARTESIAN_POINT('Ctrl Pts',(35.8351814020424,-60.2860744798563,0.));
#62899=CARTESIAN_POINT('Ctrl Pts',(35.8494472046784,-60.2998390330173,0.));
#62900=CARTESIAN_POINT('Ctrl Pts',(35.8637662371635,-60.313625378281,0.));
#62901=CARTESIAN_POINT('Ctrl Pts',(35.878138405151,-60.3274332746781,0.));
#62902=CARTESIAN_POINT('Ctrl Pts',(35.8925636280633,-60.3412625135223,0.));
#62903=CARTESIAN_POINT('Ctrl Pts',(35.9070418358501,-60.3551129108794,0.));
#62904=CARTESIAN_POINT('Ctrl Pts',(35.9215729642219,-60.368984296546,0.));
#62905=CARTESIAN_POINT('Ctrl Pts',(35.9361569506956,-60.3828765049031,0.));
#62906=CARTESIAN_POINT('Ctrl Pts',(35.9507937296727,-60.3967893635487,0.));
#62907=CARTESIAN_POINT('Ctrl Pts',(35.9654832299627,-60.4107226875759,0.));
#62908=CARTESIAN_POINT('Ctrl Pts',(35.9802253773535,-60.424676285496,0.));
#62909=CARTESIAN_POINT('Ctrl Pts',(35.9950200962175,-60.438649962949,0.));
#62910=CARTESIAN_POINT('Ctrl Pts',(36.0098673113557,-60.452643526964,0.));
#62911=CARTESIAN_POINT('Ctrl Pts',(36.0247669500867,-60.4666567908053,0.));
#62912=CARTESIAN_POINT('Ctrl Pts',(36.0397189421617,-60.4806895737643,0.));
#62913=CARTESIAN_POINT('Ctrl Pts',(36.0547232187682,-60.4947416988396,0.));
#62914=CARTESIAN_POINT('Ctrl Pts',(36.0697797118377,-60.5088129911357,0.));
#62915=CARTESIAN_POINT('Ctrl Pts',(36.0848883531969,-60.5229032759001,0.));
#62916=CARTESIAN_POINT('Ctrl Pts',(36.1000490738532,-60.5370123768841,0.));
#62917=CARTESIAN_POINT('Ctrl Pts',(36.1152618043757,-60.5511401172014,0.));
#62918=CARTESIAN_POINT('Ctrl Pts',(36.1305264752195,-60.5652863200732,0.));
#62919=CARTESIAN_POINT('Ctrl Pts',(36.1458430170425,-60.5794508095555,0.));
#62920=CARTESIAN_POINT('Ctrl Pts',(36.1612113610758,-60.5936334114082,0.));
#62921=CARTESIAN_POINT('Ctrl Pts',(36.1766314392624,-60.6078339534151,0.));
#62922=CARTESIAN_POINT('Ctrl Pts',(36.1921031840618,-60.6220522649129,0.));
#62923=CARTESIAN_POINT('Ctrl Pts',(36.2076265283261,-60.6362881765014,0.));
#62924=CARTESIAN_POINT('Ctrl Pts',(36.2232014051549,-60.6505415197054,0.));
#62925=CARTESIAN_POINT('Ctrl Pts',(36.2388277477225,-60.6648121265907,0.));
#62926=CARTESIAN_POINT('Ctrl Pts',(36.2545054892911,-60.6790998297823,0.));
#62927=CARTESIAN_POINT('Ctrl Pts',(36.2702345632883,-60.6934044626304,0.));
#62928=CARTESIAN_POINT('Ctrl Pts',(36.2860149033587,-60.7077258593268,0.));
#62929=CARTESIAN_POINT('Ctrl Pts',(36.3018464434204,-60.7220638550396,0.));
#62930=CARTESIAN_POINT('Ctrl Pts',(36.3177291177148,-60.7364182860388,0.));
#62931=CARTESIAN_POINT('Ctrl Pts',(36.3336628607844,-60.7507889896283,0.));
#62932=CARTESIAN_POINT('Ctrl Pts',(36.349647607448,-60.7651758040791,0.));
#62933=CARTESIAN_POINT('Ctrl Pts',(36.3656832927733,-60.779578568563,0.));
#62934=CARTESIAN_POINT('Ctrl Pts',(36.38176985204,-60.7939971230781,0.));
#62935=CARTESIAN_POINT('Ctrl Pts',(36.3979072207175,-60.8084313084009,0.));
#62936=CARTESIAN_POINT('Ctrl Pts',(36.414095334487,-60.8228809661179,0.));
#62937=CARTESIAN_POINT('Ctrl Pts',(36.4303341292497,-60.8373459386397,0.));
#62938=CARTESIAN_POINT('Ctrl Pts',(36.4466235411353,-60.851826069218,0.));
#62939=CARTESIAN_POINT('Ctrl Pts',(36.4629635065038,-60.8663212019645,0.));
#62940=CARTESIAN_POINT('Ctrl Pts',(36.4793539619459,-60.8808311818488,0.));
#62941=CARTESIAN_POINT('Ctrl Pts',(36.4957948442832,-60.8953558546791,0.));
#62942=CARTESIAN_POINT('Ctrl Pts',(36.5122860905611,-60.9098950670847,0.));
#62943=CARTESIAN_POINT('Ctrl Pts',(36.5288276380417,-60.9244486664989,0.));
#62944=CARTESIAN_POINT('Ctrl Pts',(36.5454194241866,-60.9390165011357,0.));
#62945=CARTESIAN_POINT('Ctrl Pts',(36.5620613866616,-60.9535984199874,0.));
#62946=CARTESIAN_POINT('Ctrl Pts',(36.5787534633416,-60.9681942728237,0.));
#62947=CARTESIAN_POINT('Ctrl Pts',(36.5954955923109,-60.9828039101887,0.));
#62948=CARTESIAN_POINT('Ctrl Pts',(36.61228771186,-60.9974271833981,0.));
#62949=CARTESIAN_POINT('Ctrl Pts',(36.6291297604775,-61.012063944535,0.));
#62950=CARTESIAN_POINT('Ctrl Pts',(36.6460216768553,-61.0267140464434,0.));
#62951=CARTESIAN_POINT('Ctrl Pts',(36.6629633998886,-61.0413773427204,0.));
#62952=CARTESIAN_POINT('Ctrl Pts',(36.6799548686741,-61.0560536877084,0.));
#62953=CARTESIAN_POINT('Ctrl Pts',(36.6969960225019,-61.0707429364841,0.));
#62954=CARTESIAN_POINT('Ctrl Pts',(36.7140868008479,-61.085444944851,0.));
#62955=CARTESIAN_POINT('Ctrl Pts',(36.7312271433799,-61.1001595693357,0.));
#62956=CARTESIAN_POINT('Ctrl Pts',(36.7484169899591,-61.114886667182,0.));
#62957=CARTESIAN_POINT('Ctrl Pts',(36.7656562806381,-61.1296260963468,0.));
#62958=CARTESIAN_POINT('Ctrl Pts',(36.782944955654,-61.1443777154926,0.));
#62959=CARTESIAN_POINT('Ctrl Pts',(36.8002829554221,-61.1591413839809,0.));
#62960=CARTESIAN_POINT('Ctrl Pts',(36.8176702205436,-61.1739169618688,0.));
#62961=CARTESIAN_POINT('Ctrl Pts',(36.8351066918043,-61.1887043099026,0.));
#62962=CARTESIAN_POINT('Ctrl Pts',(36.8525923101736,-61.2035032895121,0.));
#62963=CARTESIAN_POINT('Ctrl Pts',(36.8701270167954,-61.2183137628031,0.));
#62964=CARTESIAN_POINT('Ctrl Pts',(36.8877107529844,-61.2331355925513,0.));
#62965=CARTESIAN_POINT('Ctrl Pts',(36.9053434602324,-61.2479686421979,0.));
#62966=CARTESIAN_POINT('Ctrl Pts',(36.9230250802079,-61.2628127758443,0.));
#62967=CARTESIAN_POINT('Ctrl Pts',(36.9407555547542,-61.2776678582473,0.));
#62968=CARTESIAN_POINT('Ctrl Pts',(36.9585348258798,-61.2925337548113,0.));
#62969=CARTESIAN_POINT('Ctrl Pts',(36.976362835757,-61.3074103315834,0.));
#62970=CARTESIAN_POINT('Ctrl Pts',(36.994239526729,-61.3222974552519,0.));
#62971=CARTESIAN_POINT('Ctrl Pts',(37.0121648413088,-61.3371949931396,0.));
#62972=CARTESIAN_POINT('Ctrl Pts',(37.0301387221766,-61.352102813199,0.));
#62973=CARTESIAN_POINT('Ctrl Pts',(37.0481611121698,-61.367020784004,0.));
#62974=CARTESIAN_POINT('Ctrl Pts',(37.0662319542827,-61.3819487747458,0.));
#62975=CARTESIAN_POINT('Ctrl Pts',(37.0843511916729,-61.3968866552294,0.));
#62976=CARTESIAN_POINT('Ctrl Pts',(37.1025187676597,-61.411834295869,0.));
#62977=CARTESIAN_POINT('Ctrl Pts',(37.1207346257229,-61.4267915676833,0.));
#62978=CARTESIAN_POINT('Ctrl Pts',(37.138998709492,-61.4417583422888,0.));
#62979=CARTESIAN_POINT('Ctrl Pts',(37.157310962747,-61.4567344918946,0.));
#62980=CARTESIAN_POINT('Ctrl Pts',(37.175671329425,-61.471719889301,0.));
#62981=CARTESIAN_POINT('Ctrl Pts',(37.1940797536182,-61.4867144078939,0.));
#62982=CARTESIAN_POINT('Ctrl Pts',(37.2125361795727,-61.5017179216404,0.));
#62983=CARTESIAN_POINT('Ctrl Pts',(37.2310405516775,-61.5167303050823,0.));
#62984=CARTESIAN_POINT('Ctrl Pts',(37.2495928144661,-61.5317514333319,0.));
#62985=CARTESIAN_POINT('Ctrl Pts',(37.2681929126218,-61.5467811820685,0.));
#62986=CARTESIAN_POINT('Ctrl Pts',(37.286840790977,-61.5618194275348,0.));
#62987=CARTESIAN_POINT('Ctrl Pts',(37.3055363945108,-61.5768660465313,0.));
#62988=CARTESIAN_POINT('Ctrl Pts',(37.3242796683395,-61.591920916412,0.));
#62989=CARTESIAN_POINT('Ctrl Pts',(37.3430705577178,-61.6069839150804,0.));
#62990=CARTESIAN_POINT('Ctrl Pts',(37.3619090080447,-61.6220549209862,0.));
#62991=CARTESIAN_POINT('Ctrl Pts',(37.3807949648623,-61.6371338131208,0.));
#62992=CARTESIAN_POINT('Ctrl Pts',(37.3997283738534,-61.6522204710133,0.));
#62993=CARTESIAN_POINT('Ctrl Pts',(37.4187091808324,-61.6673147747249,0.));
#62994=CARTESIAN_POINT('Ctrl Pts',(37.4377373317456,-61.6824166048453,0.));
#62995=CARTESIAN_POINT('Ctrl Pts',(37.4568127726776,-61.69752584249,0.));
#62996=CARTESIAN_POINT('Ctrl Pts',(37.475935449851,-61.7126423692965,0.));
#62997=CARTESIAN_POINT('Ctrl Pts',(37.4951053096235,-61.7277660674203,0.));
#62998=CARTESIAN_POINT('Ctrl Pts',(37.5143222984794,-61.7428968195295,0.));
#62999=CARTESIAN_POINT('Ctrl Pts',(37.5335863630286,-61.7580345088013,0.));
#63000=CARTESIAN_POINT('Ctrl Pts',(37.5528974500142,-61.7731790189191,0.));
#63001=CARTESIAN_POINT('Ctrl Pts',(37.5722555063112,-61.7883302340689,0.));
#63002=CARTESIAN_POINT('Ctrl Pts',(37.5916604789252,-61.8034880389362,0.));
#63003=CARTESIAN_POINT('Ctrl Pts',(37.6111123149836,-61.8186523187011,0.));
#63004=CARTESIAN_POINT('Ctrl Pts',(37.6306109617341,-61.8338229590345,0.));
#63005=CARTESIAN_POINT('Ctrl Pts',(37.6501563665518,-61.848999846095,0.));
#63006=CARTESIAN_POINT('Ctrl Pts',(37.6697484769389,-61.8641828665257,0.));
#63007=CARTESIAN_POINT('Ctrl Pts',(37.689387240523,-61.879371907451,0.));
#63008=CARTESIAN_POINT('Ctrl Pts',(37.7090726050489,-61.8945668564714,0.));
#63009=CARTESIAN_POINT('Ctrl Pts',(37.7288045183765,-61.9097676016616,0.));
#63010=CARTESIAN_POINT('Ctrl Pts',(37.748582928488,-61.9249740315664,0.));
#63011=CARTESIAN_POINT('Ctrl Pts',(37.7684077834877,-61.940186035198,0.));
#63012=CARTESIAN_POINT('Ctrl Pts',(37.7882790316012,-61.9554035020334,0.));
#63013=CARTESIAN_POINT('Ctrl Pts',(37.808196621168,-61.9706263220101,0.));
#63014=CARTESIAN_POINT('Ctrl Pts',(37.8281605006371,-61.9858543855221,0.));
#63015=CARTESIAN_POINT('Ctrl Pts',(37.8481706185742,-62.0010875834176,0.));
#63016=CARTESIAN_POINT('Ctrl Pts',(37.8682269236628,-62.0163258069954,0.));
#63017=CARTESIAN_POINT('Ctrl Pts',(37.888329364703,-62.0315689480022,0.));
#63018=CARTESIAN_POINT('Ctrl Pts',(37.9084778906054,-62.0468168986289,0.));
#63019=CARTESIAN_POINT('Ctrl Pts',(37.9286724503849,-62.0620695515072,0.));
#63020=CARTESIAN_POINT('Ctrl Pts',(37.9489129931685,-62.0773267997072,0.));
#63021=CARTESIAN_POINT('Ctrl Pts',(37.9691994681963,-62.0925885367346,0.));
#63022=CARTESIAN_POINT('Ctrl Pts',(37.9895318248212,-62.107854656528,0.));
#63023=CARTESIAN_POINT('Ctrl Pts',(38.0099100125041,-62.1231250534558,0.));
#63024=CARTESIAN_POINT('Ctrl Pts',(38.0303339808059,-62.1383996223136,0.));
#63025=CARTESIAN_POINT('Ctrl Pts',(38.0508036793944,-62.153678258321,0.));
#63026=CARTESIAN_POINT('Ctrl Pts',(38.0713190580466,-62.1689608571182,0.));
#63027=CARTESIAN_POINT('Ctrl Pts',(38.0918800666479,-62.1842473147626,0.));
#63028=CARTESIAN_POINT('Ctrl Pts',(38.1124866551884,-62.1995375277253,0.));
#63029=CARTESIAN_POINT('Ctrl Pts',(38.1331387737528,-62.2148313928859,0.));
#63030=CARTESIAN_POINT('Ctrl Pts',(38.1538363725264,-62.2301288075318,0.));
#63031=CARTESIAN_POINT('Ctrl Pts',(38.1745794017997,-62.245429669358,0.));
#63032=CARTESIAN_POINT('Ctrl Pts',(38.1953678119692,-62.2607338764655,0.));
#63033=CARTESIAN_POINT('Ctrl Pts',(38.2162015535351,-62.2760413273601,0.));
#63034=CARTESIAN_POINT('Ctrl Pts',(38.2370805770931,-62.2913519209517,0.));
#63035=CARTESIAN_POINT('Ctrl Pts',(38.2580048333356,-62.3066655565497,0.));
#63036=CARTESIAN_POINT('Ctrl Pts',(38.2789742730559,-62.3219821338564,0.));
#63037=CARTESIAN_POINT('Ctrl Pts',(38.2999888471474,-62.337301552961,0.));
#63038=CARTESIAN_POINT('Ctrl Pts',(38.3210485066003,-62.3526237143338,0.));
#63039=CARTESIAN_POINT('Ctrl Pts',(38.3421532024915,-62.3679485188178,0.));
#63040=CARTESIAN_POINT('Ctrl Pts',(38.3633028859835,-62.3832758676281,0.));
#63041=CARTESIAN_POINT('Ctrl Pts',(38.384497508335,-62.3986056623587,0.));
#63042=CARTESIAN_POINT('Ctrl Pts',(38.4057370209054,-62.4139378049891,0.));
#63043=CARTESIAN_POINT('Ctrl Pts',(38.4270213751567,-62.42927219789,0.));
#63044=CARTESIAN_POINT('Ctrl Pts',(38.4483505226512,-62.4446087438304,0.));
#63045=CARTESIAN_POINT('Ctrl Pts',(38.4697244150473,-62.4599473459799,0.));
#63046=CARTESIAN_POINT('Ctrl Pts',(38.4911430040988,-62.4752879078842,0.));
#63047=CARTESIAN_POINT('Ctrl Pts',(38.5126062416496,-62.4906303334435,0.));
#63048=CARTESIAN_POINT('Ctrl Pts',(38.5341140796247,-62.5059745268899,0.));
#63049=CARTESIAN_POINT('Ctrl Pts',(38.5556664700201,-62.5213203927672,0.));
#63050=CARTESIAN_POINT('Ctrl Pts',(38.5772633648841,-62.5366678359035,0.));
#63051=CARTESIAN_POINT('Ctrl Pts',(38.5989047163401,-62.5520167614529,0.));
#63052=CARTESIAN_POINT('Ctrl Pts',(38.6205904766078,-62.567367074937,0.));
#63053=CARTESIAN_POINT('Ctrl Pts',(38.6423205980214,-62.5827186822923,0.));
#63054=CARTESIAN_POINT('Ctrl Pts',(38.6640950330418,-62.5980714899048,0.));
#63055=CARTESIAN_POINT('Ctrl Pts',(38.6859137342726,-62.6134254046731,0.));
#63056=CARTESIAN_POINT('Ctrl Pts',(38.7077766544411,-62.6287803339534,0.));
#63057=CARTESIAN_POINT('Ctrl Pts',(38.7296837463605,-62.6441361854406,0.));
#63058=CARTESIAN_POINT('Ctrl Pts',(38.7516349628902,-62.6594928670626,0.));
#63059=CARTESIAN_POINT('Ctrl Pts',(38.7736302568982,-62.6748502868836,0.));
#63060=CARTESIAN_POINT('Ctrl Pts',(38.7956695812032,-62.6902083529698,0.));
#63061=CARTESIAN_POINT('Ctrl Pts',(38.8177528885687,-62.7055669733811,0.));
#63062=CARTESIAN_POINT('Ctrl Pts',(38.8398801318185,-62.7209260564505,0.));
#63063=CARTESIAN_POINT('Ctrl Pts',(38.8620512639239,-62.7362855110052,0.));
#63064=CARTESIAN_POINT('Ctrl Pts',(38.8842662380984,-62.7516452466129,0.));
#63065=CARTESIAN_POINT('Ctrl Pts',(38.9065250078824,-62.7670051738131,0.));
#63066=CARTESIAN_POINT('Ctrl Pts',(38.928827527232,-62.7823652043677,0.));
#63067=CARTESIAN_POINT('Ctrl Pts',(38.9511737503146,-62.797725250709,0.));
#63068=CARTESIAN_POINT('Ctrl Pts',(38.9735636313073,-62.8130852254004,0.));
#63069=CARTESIAN_POINT('Ctrl Pts',(38.9959971241695,-62.8284450405451,0.));
#63070=CARTESIAN_POINT('Ctrl Pts',(39.018474182465,-62.8438046073237,0.));
#63071=CARTESIAN_POINT('Ctrl Pts',(39.0409947590519,-62.859163835209,0.));
#63072=CARTESIAN_POINT('Ctrl Pts',(39.0635588063309,-62.8745226326046,0.));
#63073=CARTESIAN_POINT('Ctrl Pts',(39.0861662767964,-62.8898809082658,0.));
#63074=CARTESIAN_POINT('Ctrl Pts',(39.1088171235144,-62.9052385725416,0.));
#63075=CARTESIAN_POINT('Ctrl Pts',(39.1315113005745,-62.9205955385551,0.));
#63076=CARTESIAN_POINT('Ctrl Pts',(39.1542487636708,-62.9359517237352,0.));
#63077=CARTESIAN_POINT('Ctrl Pts',(39.1770294702367,-62.9513070501777,0.));
#63078=CARTESIAN_POINT('Ctrl Pts',(39.1965939820803,-62.9644687386693,0.));
#63079=CARTESIAN_POINT('Ctrl Pts',(39.2116170128276,-62.9745590018499,0.));
#63080=CARTESIAN_POINT('Ctrl Pts',(39.2220794388572,-62.9815782721128,0.));
#63081=CARTESIAN_POINT('Ctrl Pts',(39.2279686274718,-62.9855268615901,0.));
#63082=CARTESIAN_POINT('Ctrl Pts',(39.2292784191464,-62.9864049293629,0.));
#63083=CARTESIAN_POINT('',(35.7368311217509,-60.1903555511633,12.));
#63084=CARTESIAN_POINT('',(35.7368311217509,-60.1903555511633,0.));
#63085=CARTESIAN_POINT('Ctrl Pts',(39.2292784191464,-62.9864049293629,12.));
#63086=CARTESIAN_POINT('Ctrl Pts',(39.2279686274718,-62.9855268615901,12.));
#63087=CARTESIAN_POINT('Ctrl Pts',(39.2220794388571,-62.9815782721128,12.));
#63088=CARTESIAN_POINT('Ctrl Pts',(39.2116170128275,-62.9745590018499,12.));
#63089=CARTESIAN_POINT('Ctrl Pts',(39.1965939820803,-62.9644687386693,12.));
#63090=CARTESIAN_POINT('Ctrl Pts',(39.1770294702367,-62.9513070501777,12.));
#63091=CARTESIAN_POINT('Ctrl Pts',(39.1542487636708,-62.9359517237352,12.));
#63092=CARTESIAN_POINT('Ctrl Pts',(39.1315113005745,-62.9205955385551,12.));
#63093=CARTESIAN_POINT('Ctrl Pts',(39.1088171235144,-62.9052385725416,12.));
#63094=CARTESIAN_POINT('Ctrl Pts',(39.0861662767964,-62.8898809082658,12.));
#63095=CARTESIAN_POINT('Ctrl Pts',(39.0635588063309,-62.8745226326046,12.));
#63096=CARTESIAN_POINT('Ctrl Pts',(39.0409947590519,-62.859163835209,12.));
#63097=CARTESIAN_POINT('Ctrl Pts',(39.018474182465,-62.8438046073237,12.));
#63098=CARTESIAN_POINT('Ctrl Pts',(38.9959971241695,-62.8284450405451,12.));
#63099=CARTESIAN_POINT('Ctrl Pts',(38.9735636313073,-62.8130852254004,12.));
#63100=CARTESIAN_POINT('Ctrl Pts',(38.9511737503146,-62.797725250709,12.));
#63101=CARTESIAN_POINT('Ctrl Pts',(38.928827527232,-62.7823652043677,12.));
#63102=CARTESIAN_POINT('Ctrl Pts',(38.9065250078824,-62.7670051738131,12.));
#63103=CARTESIAN_POINT('Ctrl Pts',(38.8842662380984,-62.7516452466129,12.));
#63104=CARTESIAN_POINT('Ctrl Pts',(38.8620512639239,-62.7362855110052,12.));
#63105=CARTESIAN_POINT('Ctrl Pts',(38.8398801318185,-62.7209260564505,12.));
#63106=CARTESIAN_POINT('Ctrl Pts',(38.8177528885687,-62.7055669733811,12.));
#63107=CARTESIAN_POINT('Ctrl Pts',(38.7956695812032,-62.6902083529698,12.));
#63108=CARTESIAN_POINT('Ctrl Pts',(38.7736302568982,-62.6748502868836,12.));
#63109=CARTESIAN_POINT('Ctrl Pts',(38.7516349628902,-62.6594928670626,12.));
#63110=CARTESIAN_POINT('Ctrl Pts',(38.7296837463605,-62.6441361854406,12.));
#63111=CARTESIAN_POINT('Ctrl Pts',(38.7077766544411,-62.6287803339534,12.));
#63112=CARTESIAN_POINT('Ctrl Pts',(38.6859137342726,-62.6134254046731,12.));
#63113=CARTESIAN_POINT('Ctrl Pts',(38.6640950330418,-62.5980714899048,12.));
#63114=CARTESIAN_POINT('Ctrl Pts',(38.6423205980214,-62.5827186822923,12.));
#63115=CARTESIAN_POINT('Ctrl Pts',(38.6205904766078,-62.567367074937,12.));
#63116=CARTESIAN_POINT('Ctrl Pts',(38.5989047163401,-62.5520167614529,12.));
#63117=CARTESIAN_POINT('Ctrl Pts',(38.5772633648841,-62.5366678359035,12.));
#63118=CARTESIAN_POINT('Ctrl Pts',(38.5556664700201,-62.5213203927672,12.));
#63119=CARTESIAN_POINT('Ctrl Pts',(38.5341140796247,-62.5059745268899,12.));
#63120=CARTESIAN_POINT('Ctrl Pts',(38.5126062416496,-62.4906303334435,12.));
#63121=CARTESIAN_POINT('Ctrl Pts',(38.4911430040988,-62.4752879078842,12.));
#63122=CARTESIAN_POINT('Ctrl Pts',(38.4697244150473,-62.4599473459799,12.));
#63123=CARTESIAN_POINT('Ctrl Pts',(38.4483505226512,-62.4446087438304,12.));
#63124=CARTESIAN_POINT('Ctrl Pts',(38.4270213751567,-62.42927219789,12.));
#63125=CARTESIAN_POINT('Ctrl Pts',(38.4057370209054,-62.4139378049891,12.));
#63126=CARTESIAN_POINT('Ctrl Pts',(38.384497508335,-62.3986056623587,12.));
#63127=CARTESIAN_POINT('Ctrl Pts',(38.3633028859835,-62.3832758676281,12.));
#63128=CARTESIAN_POINT('Ctrl Pts',(38.3421532024915,-62.3679485188178,12.));
#63129=CARTESIAN_POINT('Ctrl Pts',(38.3210485066003,-62.3526237143338,12.));
#63130=CARTESIAN_POINT('Ctrl Pts',(38.2999888471474,-62.337301552961,12.));
#63131=CARTESIAN_POINT('Ctrl Pts',(38.2789742730559,-62.3219821338564,12.));
#63132=CARTESIAN_POINT('Ctrl Pts',(38.2580048333356,-62.3066655565497,12.));
#63133=CARTESIAN_POINT('Ctrl Pts',(38.2370805770931,-62.2913519209517,12.));
#63134=CARTESIAN_POINT('Ctrl Pts',(38.2162015535351,-62.2760413273601,12.));
#63135=CARTESIAN_POINT('Ctrl Pts',(38.1953678119692,-62.2607338764655,12.));
#63136=CARTESIAN_POINT('Ctrl Pts',(38.1745794017997,-62.245429669358,12.));
#63137=CARTESIAN_POINT('Ctrl Pts',(38.1538363725264,-62.2301288075318,12.));
#63138=CARTESIAN_POINT('Ctrl Pts',(38.1331387737528,-62.2148313928859,12.));
#63139=CARTESIAN_POINT('Ctrl Pts',(38.1124866551884,-62.1995375277253,12.));
#63140=CARTESIAN_POINT('Ctrl Pts',(38.0918800666479,-62.1842473147626,12.));
#63141=CARTESIAN_POINT('Ctrl Pts',(38.0713190580466,-62.1689608571182,12.));
#63142=CARTESIAN_POINT('Ctrl Pts',(38.0508036793944,-62.153678258321,12.));
#63143=CARTESIAN_POINT('Ctrl Pts',(38.0303339808059,-62.1383996223136,12.));
#63144=CARTESIAN_POINT('Ctrl Pts',(38.0099100125041,-62.1231250534558,12.));
#63145=CARTESIAN_POINT('Ctrl Pts',(37.9895318248212,-62.107854656528,12.));
#63146=CARTESIAN_POINT('Ctrl Pts',(37.9691994681963,-62.0925885367346,12.));
#63147=CARTESIAN_POINT('Ctrl Pts',(37.9489129931685,-62.0773267997072,12.));
#63148=CARTESIAN_POINT('Ctrl Pts',(37.9286724503849,-62.0620695515072,12.));
#63149=CARTESIAN_POINT('Ctrl Pts',(37.9084778906054,-62.0468168986289,12.));
#63150=CARTESIAN_POINT('Ctrl Pts',(37.888329364703,-62.0315689480022,12.));
#63151=CARTESIAN_POINT('Ctrl Pts',(37.8682269236628,-62.0163258069954,12.));
#63152=CARTESIAN_POINT('Ctrl Pts',(37.8481706185742,-62.0010875834176,12.));
#63153=CARTESIAN_POINT('Ctrl Pts',(37.8281605006371,-61.9858543855221,12.));
#63154=CARTESIAN_POINT('Ctrl Pts',(37.808196621168,-61.9706263220101,12.));
#63155=CARTESIAN_POINT('Ctrl Pts',(37.7882790316012,-61.9554035020334,12.));
#63156=CARTESIAN_POINT('Ctrl Pts',(37.7684077834877,-61.940186035198,12.));
#63157=CARTESIAN_POINT('Ctrl Pts',(37.748582928488,-61.9249740315664,12.));
#63158=CARTESIAN_POINT('Ctrl Pts',(37.7288045183765,-61.9097676016616,12.));
#63159=CARTESIAN_POINT('Ctrl Pts',(37.7090726050489,-61.8945668564714,12.));
#63160=CARTESIAN_POINT('Ctrl Pts',(37.689387240523,-61.879371907451,12.));
#63161=CARTESIAN_POINT('Ctrl Pts',(37.6697484769389,-61.8641828665257,12.));
#63162=CARTESIAN_POINT('Ctrl Pts',(37.6501563665518,-61.848999846095,12.));
#63163=CARTESIAN_POINT('Ctrl Pts',(37.6306109617341,-61.8338229590345,12.));
#63164=CARTESIAN_POINT('Ctrl Pts',(37.6111123149836,-61.8186523187011,12.));
#63165=CARTESIAN_POINT('Ctrl Pts',(37.5916604789252,-61.8034880389362,12.));
#63166=CARTESIAN_POINT('Ctrl Pts',(37.5722555063112,-61.7883302340689,12.));
#63167=CARTESIAN_POINT('Ctrl Pts',(37.5528974500142,-61.7731790189191,12.));
#63168=CARTESIAN_POINT('Ctrl Pts',(37.5335863630286,-61.7580345088013,12.));
#63169=CARTESIAN_POINT('Ctrl Pts',(37.5143222984794,-61.7428968195295,12.));
#63170=CARTESIAN_POINT('Ctrl Pts',(37.4951053096235,-61.7277660674203,12.));
#63171=CARTESIAN_POINT('Ctrl Pts',(37.475935449851,-61.7126423692965,12.));
#63172=CARTESIAN_POINT('Ctrl Pts',(37.4568127726776,-61.69752584249,12.));
#63173=CARTESIAN_POINT('Ctrl Pts',(37.4377373317456,-61.6824166048453,12.));
#63174=CARTESIAN_POINT('Ctrl Pts',(37.4187091808324,-61.6673147747249,12.));
#63175=CARTESIAN_POINT('Ctrl Pts',(37.3997283738534,-61.6522204710133,12.));
#63176=CARTESIAN_POINT('Ctrl Pts',(37.3807949648623,-61.6371338131208,12.));
#63177=CARTESIAN_POINT('Ctrl Pts',(37.3619090080447,-61.6220549209862,12.));
#63178=CARTESIAN_POINT('Ctrl Pts',(37.3430705577178,-61.6069839150804,12.));
#63179=CARTESIAN_POINT('Ctrl Pts',(37.3242796683395,-61.591920916412,12.));
#63180=CARTESIAN_POINT('Ctrl Pts',(37.3055363945108,-61.5768660465313,12.));
#63181=CARTESIAN_POINT('Ctrl Pts',(37.286840790977,-61.5618194275348,12.));
#63182=CARTESIAN_POINT('Ctrl Pts',(37.2681929126218,-61.5467811820685,12.));
#63183=CARTESIAN_POINT('Ctrl Pts',(37.2495928144661,-61.5317514333319,12.));
#63184=CARTESIAN_POINT('Ctrl Pts',(37.2310405516775,-61.5167303050823,12.));
#63185=CARTESIAN_POINT('Ctrl Pts',(37.2125361795727,-61.5017179216404,12.));
#63186=CARTESIAN_POINT('Ctrl Pts',(37.1940797536182,-61.4867144078939,12.));
#63187=CARTESIAN_POINT('Ctrl Pts',(37.175671329425,-61.471719889301,12.));
#63188=CARTESIAN_POINT('Ctrl Pts',(37.157310962747,-61.4567344918946,12.));
#63189=CARTESIAN_POINT('Ctrl Pts',(37.138998709492,-61.4417583422888,12.));
#63190=CARTESIAN_POINT('Ctrl Pts',(37.1207346257229,-61.4267915676833,12.));
#63191=CARTESIAN_POINT('Ctrl Pts',(37.1025187676597,-61.411834295869,12.));
#63192=CARTESIAN_POINT('Ctrl Pts',(37.0843511916729,-61.3968866552294,12.));
#63193=CARTESIAN_POINT('Ctrl Pts',(37.0662319542827,-61.3819487747458,12.));
#63194=CARTESIAN_POINT('Ctrl Pts',(37.0481611121698,-61.367020784004,12.));
#63195=CARTESIAN_POINT('Ctrl Pts',(37.0301387221766,-61.352102813199,12.));
#63196=CARTESIAN_POINT('Ctrl Pts',(37.0121648413088,-61.3371949931396,12.));
#63197=CARTESIAN_POINT('Ctrl Pts',(36.994239526729,-61.3222974552519,12.));
#63198=CARTESIAN_POINT('Ctrl Pts',(36.976362835757,-61.3074103315834,12.));
#63199=CARTESIAN_POINT('Ctrl Pts',(36.9585348258798,-61.2925337548113,12.));
#63200=CARTESIAN_POINT('Ctrl Pts',(36.9407555547542,-61.2776678582473,12.));
#63201=CARTESIAN_POINT('Ctrl Pts',(36.9230250802079,-61.2628127758443,12.));
#63202=CARTESIAN_POINT('Ctrl Pts',(36.9053434602324,-61.2479686421979,12.));
#63203=CARTESIAN_POINT('Ctrl Pts',(36.8877107529844,-61.2331355925513,12.));
#63204=CARTESIAN_POINT('Ctrl Pts',(36.8701270167954,-61.2183137628031,12.));
#63205=CARTESIAN_POINT('Ctrl Pts',(36.8525923101736,-61.2035032895121,12.));
#63206=CARTESIAN_POINT('Ctrl Pts',(36.8351066918043,-61.1887043099026,12.));
#63207=CARTESIAN_POINT('Ctrl Pts',(36.8176702205436,-61.1739169618688,12.));
#63208=CARTESIAN_POINT('Ctrl Pts',(36.8002829554221,-61.1591413839809,12.));
#63209=CARTESIAN_POINT('Ctrl Pts',(36.782944955654,-61.1443777154926,12.));
#63210=CARTESIAN_POINT('Ctrl Pts',(36.7656562806381,-61.1296260963468,12.));
#63211=CARTESIAN_POINT('Ctrl Pts',(36.7484169899591,-61.114886667182,12.));
#63212=CARTESIAN_POINT('Ctrl Pts',(36.7312271433799,-61.1001595693357,12.));
#63213=CARTESIAN_POINT('Ctrl Pts',(36.7140868008479,-61.085444944851,12.));
#63214=CARTESIAN_POINT('Ctrl Pts',(36.6969960225019,-61.0707429364841,12.));
#63215=CARTESIAN_POINT('Ctrl Pts',(36.6799548686741,-61.0560536877084,12.));
#63216=CARTESIAN_POINT('Ctrl Pts',(36.6629633998886,-61.0413773427204,12.));
#63217=CARTESIAN_POINT('Ctrl Pts',(36.6460216768553,-61.0267140464434,12.));
#63218=CARTESIAN_POINT('Ctrl Pts',(36.6291297604775,-61.012063944535,12.));
#63219=CARTESIAN_POINT('Ctrl Pts',(36.61228771186,-60.9974271833981,12.));
#63220=CARTESIAN_POINT('Ctrl Pts',(36.5954955923109,-60.9828039101887,12.));
#63221=CARTESIAN_POINT('Ctrl Pts',(36.5787534633416,-60.9681942728237,12.));
#63222=CARTESIAN_POINT('Ctrl Pts',(36.5620613866616,-60.9535984199874,12.));
#63223=CARTESIAN_POINT('Ctrl Pts',(36.5454194241866,-60.9390165011357,12.));
#63224=CARTESIAN_POINT('Ctrl Pts',(36.5288276380417,-60.9244486664989,12.));
#63225=CARTESIAN_POINT('Ctrl Pts',(36.5122860905611,-60.9098950670847,12.));
#63226=CARTESIAN_POINT('Ctrl Pts',(36.4957948442832,-60.8953558546791,12.));
#63227=CARTESIAN_POINT('Ctrl Pts',(36.4793539619459,-60.8808311818488,12.));
#63228=CARTESIAN_POINT('Ctrl Pts',(36.4629635065038,-60.8663212019645,12.));
#63229=CARTESIAN_POINT('Ctrl Pts',(36.4466235411353,-60.851826069218,12.));
#63230=CARTESIAN_POINT('Ctrl Pts',(36.4303341292497,-60.8373459386397,12.));
#63231=CARTESIAN_POINT('Ctrl Pts',(36.414095334487,-60.8228809661179,12.));
#63232=CARTESIAN_POINT('Ctrl Pts',(36.3979072207175,-60.8084313084009,12.));
#63233=CARTESIAN_POINT('Ctrl Pts',(36.38176985204,-60.7939971230781,12.));
#63234=CARTESIAN_POINT('Ctrl Pts',(36.3656832927733,-60.779578568563,12.));
#63235=CARTESIAN_POINT('Ctrl Pts',(36.349647607448,-60.7651758040791,12.));
#63236=CARTESIAN_POINT('Ctrl Pts',(36.3336628607844,-60.7507889896283,12.));
#63237=CARTESIAN_POINT('Ctrl Pts',(36.3177291177148,-60.7364182860388,12.));
#63238=CARTESIAN_POINT('Ctrl Pts',(36.3018464434204,-60.7220638550396,12.));
#63239=CARTESIAN_POINT('Ctrl Pts',(36.2860149033587,-60.7077258593268,12.));
#63240=CARTESIAN_POINT('Ctrl Pts',(36.2702345632883,-60.6934044626304,12.));
#63241=CARTESIAN_POINT('Ctrl Pts',(36.2545054892911,-60.6790998297823,12.));
#63242=CARTESIAN_POINT('Ctrl Pts',(36.2388277477225,-60.6648121265907,12.));
#63243=CARTESIAN_POINT('Ctrl Pts',(36.2232014051549,-60.6505415197054,12.));
#63244=CARTESIAN_POINT('Ctrl Pts',(36.2076265283261,-60.6362881765014,12.));
#63245=CARTESIAN_POINT('Ctrl Pts',(36.1921031840618,-60.6220522649129,12.));
#63246=CARTESIAN_POINT('Ctrl Pts',(36.1766314392624,-60.6078339534151,12.));
#63247=CARTESIAN_POINT('Ctrl Pts',(36.1612113610758,-60.5936334114082,12.));
#63248=CARTESIAN_POINT('Ctrl Pts',(36.1458430170425,-60.5794508095555,12.));
#63249=CARTESIAN_POINT('Ctrl Pts',(36.1305264752195,-60.5652863200732,12.));
#63250=CARTESIAN_POINT('Ctrl Pts',(36.1152618043757,-60.5511401172014,12.));
#63251=CARTESIAN_POINT('Ctrl Pts',(36.1000490738532,-60.5370123768841,12.));
#63252=CARTESIAN_POINT('Ctrl Pts',(36.0848883531969,-60.5229032759001,12.));
#63253=CARTESIAN_POINT('Ctrl Pts',(36.0697797118377,-60.5088129911357,12.));
#63254=CARTESIAN_POINT('Ctrl Pts',(36.0547232187682,-60.4947416988396,12.));
#63255=CARTESIAN_POINT('Ctrl Pts',(36.0397189421617,-60.4806895737643,12.));
#63256=CARTESIAN_POINT('Ctrl Pts',(36.0247669500867,-60.4666567908053,12.));
#63257=CARTESIAN_POINT('Ctrl Pts',(36.0098673113557,-60.452643526964,12.));
#63258=CARTESIAN_POINT('Ctrl Pts',(35.9950200962175,-60.438649962949,12.));
#63259=CARTESIAN_POINT('Ctrl Pts',(35.9802253773535,-60.424676285496,12.));
#63260=CARTESIAN_POINT('Ctrl Pts',(35.9654832299627,-60.4107226875759,12.));
#63261=CARTESIAN_POINT('Ctrl Pts',(35.9507937296727,-60.3967893635487,12.));
#63262=CARTESIAN_POINT('Ctrl Pts',(35.9361569506956,-60.3828765049031,12.));
#63263=CARTESIAN_POINT('Ctrl Pts',(35.9215729642219,-60.368984296546,12.));
#63264=CARTESIAN_POINT('Ctrl Pts',(35.9070418358501,-60.3551129108794,12.));
#63265=CARTESIAN_POINT('Ctrl Pts',(35.8925636280633,-60.3412625135223,12.));
#63266=CARTESIAN_POINT('Ctrl Pts',(35.878138405151,-60.3274332746781,12.));
#63267=CARTESIAN_POINT('Ctrl Pts',(35.8637662371635,-60.313625378281,12.));
#63268=CARTESIAN_POINT('Ctrl Pts',(35.8494472046784,-60.2998390330173,12.));
#63269=CARTESIAN_POINT('Ctrl Pts',(35.8351814020424,-60.2860744798563,12.));
#63270=CARTESIAN_POINT('Ctrl Pts',(35.8209689272574,-60.2723319687507,12.));
#63271=CARTESIAN_POINT('Ctrl Pts',(35.8068098723386,-60.2586117365278,12.));
#63272=CARTESIAN_POINT('Ctrl Pts',(35.7927043145165,-60.2449139865206,12.));
#63273=CARTESIAN_POINT('Ctrl Pts',(35.7786523045783,-60.2312388621286,12.));
#63274=CARTESIAN_POINT('Ctrl Pts',(35.7646538667299,-60.2175864449678,12.));
#63275=CARTESIAN_POINT('Ctrl Pts',(35.7534979801871,-60.2066827086579,12.));
#63276=CARTESIAN_POINT('Ctrl Pts',(35.7451551752456,-60.1985151474406,12.));
#63277=CARTESIAN_POINT('Ctrl Pts',(35.7396040203974,-60.1930746580239,12.));
#63278=CARTESIAN_POINT('Ctrl Pts',(35.7368311217509,-60.1903555511633,12.));
#63279=CARTESIAN_POINT('Ctrl Pts',(40.506059810093,-62.1730054756874,-5.55111512312578E-16));
#63280=CARTESIAN_POINT('Ctrl Pts',(40.506059810093,-62.1730054756874,4.));
#63281=CARTESIAN_POINT('Ctrl Pts',(40.506059810093,-62.1730054756875,8.));
#63282=CARTESIAN_POINT('Ctrl Pts',(40.506059810093,-62.1730054756875,12.));
#63283=CARTESIAN_POINT('Ctrl Pts',(40.5229411493977,-62.2815834512357,-5.55111512312578E-16));
#63284=CARTESIAN_POINT('Ctrl Pts',(40.5229411493977,-62.2815834512357,4.));
#63285=CARTESIAN_POINT('Ctrl Pts',(40.5229411493977,-62.2815834512358,8.));
#63286=CARTESIAN_POINT('Ctrl Pts',(40.5229411493977,-62.2815834512358,12.));
#63287=CARTESIAN_POINT('Ctrl Pts',(40.4873422218647,-62.4810961163746,-5.55111512312578E-16));
#63288=CARTESIAN_POINT('Ctrl Pts',(40.4873422218647,-62.4810961163746,4.));
#63289=CARTESIAN_POINT('Ctrl Pts',(40.4873422218647,-62.4810961163747,7.99999999999999));
#63290=CARTESIAN_POINT('Ctrl Pts',(40.4873422218647,-62.4810961163747,12.));
#63291=CARTESIAN_POINT('Ctrl Pts',(40.3516729626244,-62.6258675056116,-5.55111512312578E-16));
#63292=CARTESIAN_POINT('Ctrl Pts',(40.3516729626244,-62.6258675056116,4.));
#63293=CARTESIAN_POINT('Ctrl Pts',(40.3516729626244,-62.6258675056116,8.00000000000001));
#63294=CARTESIAN_POINT('Ctrl Pts',(40.3516729626244,-62.6258675056116,12.));
#63295=CARTESIAN_POINT('Ctrl Pts',(40.282346977699,-62.6704278106373,-5.55111512312578E-16));
#63296=CARTESIAN_POINT('Ctrl Pts',(40.282346977699,-62.6704278106373,4.));
#63297=CARTESIAN_POINT('Ctrl Pts',(40.282346977699,-62.6704278106374,8.));
#63298=CARTESIAN_POINT('Ctrl Pts',(40.282346977699,-62.6704278106374,12.));
#63299=CARTESIAN_POINT('',(40.506059810093,-62.1730054756875,2.77555756156289E-16));
#63300=CARTESIAN_POINT('',(40.2823469776988,-62.6704278106371,0.));
#63301=CARTESIAN_POINT('Ctrl Pts',(40.506059810093,-62.1730054756874,-5.55111512312578E-16));
#63302=CARTESIAN_POINT('Ctrl Pts',(40.5229411493977,-62.2815834512357,-5.55111512312578E-16));
#63303=CARTESIAN_POINT('Ctrl Pts',(40.5025989050931,-62.395590688458,-5.55111512312578E-16));
#63304=CARTESIAN_POINT('Ctrl Pts',(40.4495806341086,-62.4917232233449,-5.55111512312578E-16));
#63305=CARTESIAN_POINT('Ctrl Pts',(40.4098169308703,-62.56382262451,-5.55111512312578E-16));
#63306=CARTESIAN_POINT('Ctrl Pts',(40.3516729626244,-62.6258675056116,-5.55111512312578E-16));
#63307=CARTESIAN_POINT('Ctrl Pts',(40.282346977699,-62.6704278106373,-5.55111512312578E-16));
#63308=CARTESIAN_POINT('',(40.2823469776988,-62.6704278106371,12.));
#63309=CARTESIAN_POINT('Ctrl Pts',(40.282346977699,-62.6704278106373,-5.55111512312578E-16));
#63310=CARTESIAN_POINT('Ctrl Pts',(40.282346977699,-62.6704278106373,4.));
#63311=CARTESIAN_POINT('Ctrl Pts',(40.282346977699,-62.6704278106374,8.));
#63312=CARTESIAN_POINT('Ctrl Pts',(40.282346977699,-62.6704278106374,12.));
#63313=CARTESIAN_POINT('',(40.506059810093,-62.1730054756875,12.));
#63314=CARTESIAN_POINT('Ctrl Pts',(40.282346977699,-62.6704278106374,12.));
#63315=CARTESIAN_POINT('Ctrl Pts',(40.3516729626244,-62.6258675056116,12.));
#63316=CARTESIAN_POINT('Ctrl Pts',(40.4098169308703,-62.5638226245101,12.));
#63317=CARTESIAN_POINT('Ctrl Pts',(40.4495806341086,-62.4917232233449,12.));
#63318=CARTESIAN_POINT('Ctrl Pts',(40.5025989050932,-62.395590688458,12.));
#63319=CARTESIAN_POINT('Ctrl Pts',(40.5229411493977,-62.2815834512358,12.));
#63320=CARTESIAN_POINT('Ctrl Pts',(40.506059810093,-62.1730054756875,12.));
#63321=CARTESIAN_POINT('Ctrl Pts',(40.506059810093,-62.1730054756875,12.));
#63322=CARTESIAN_POINT('Ctrl Pts',(40.506059810093,-62.1730054756875,8.));
#63323=CARTESIAN_POINT('Ctrl Pts',(40.506059810093,-62.1730054756874,4.));
#63324=CARTESIAN_POINT('Ctrl Pts',(40.506059810093,-62.1730054756874,-5.55111512312578E-16));
#63325=CARTESIAN_POINT('Origin',(2.01487121870483E-10,-3.16086693261782E-10,
0.));
#63326=CARTESIAN_POINT('Origin',(2.01487121870483E-10,-3.16086693261782E-10,
12.));
#63327=CARTESIAN_POINT('Origin',(2.01487121870483E-10,-3.16086693261782E-10,
0.));
#63328=CARTESIAN_POINT('Ctrl Pts',(34.1330090612035,-66.2207497120638,0.));
#63329=CARTESIAN_POINT('Ctrl Pts',(34.1330090612035,-66.2207497120638,4.));
#63330=CARTESIAN_POINT('Ctrl Pts',(34.1330090612035,-66.2207497120638,8.));
#63331=CARTESIAN_POINT('Ctrl Pts',(34.1330090612035,-66.2207497120638,12.));
#63332=CARTESIAN_POINT('Ctrl Pts',(34.0353379297088,-66.2710935941676,0.));
#63333=CARTESIAN_POINT('Ctrl Pts',(34.0353379297088,-66.2710935941676,4.));
#63334=CARTESIAN_POINT('Ctrl Pts',(34.0353379297088,-66.2710935941676,8.));
#63335=CARTESIAN_POINT('Ctrl Pts',(34.0353379297088,-66.2710935941676,12.));
#63336=CARTESIAN_POINT('Ctrl Pts',(33.8348041971631,-66.3003999311009,0.));
#63337=CARTESIAN_POINT('Ctrl Pts',(33.8348041971631,-66.3003999311009,4.00000000000001));
#63338=CARTESIAN_POINT('Ctrl Pts',(33.8348041971632,-66.3003999311009,8.));
#63339=CARTESIAN_POINT('Ctrl Pts',(33.8348041971632,-66.3003999311009,12.));
#63340=CARTESIAN_POINT('Ctrl Pts',(33.6545652280937,-66.2174610329229,0.));
#63341=CARTESIAN_POINT('Ctrl Pts',(33.6545652280937,-66.2174610329229,3.99999999999999));
#63342=CARTESIAN_POINT('Ctrl Pts',(33.6545652280938,-66.2174610329229,8.));
#63343=CARTESIAN_POINT('Ctrl Pts',(33.6545652280938,-66.2174610329229,12.));
#63344=CARTESIAN_POINT('Ctrl Pts',(33.5903722664954,-66.1657795405668,0.));
#63345=CARTESIAN_POINT('Ctrl Pts',(33.5903722664954,-66.1657795405668,4.));
#63346=CARTESIAN_POINT('Ctrl Pts',(33.5903722664955,-66.1657795405668,8.));
#63347=CARTESIAN_POINT('Ctrl Pts',(33.5903722664955,-66.1657795405668,12.));
#63348=CARTESIAN_POINT('',(34.1330090612035,-66.2207497120638,0.));
#63349=CARTESIAN_POINT('',(33.5903722664955,-66.1657795405667,0.));
#63350=CARTESIAN_POINT('Ctrl Pts',(34.1330090612035,-66.2207497120638,0.));
#63351=CARTESIAN_POINT('Ctrl Pts',(34.0353379297088,-66.2710935941676,0.));
#63352=CARTESIAN_POINT('Ctrl Pts',(33.920747225397,-66.2878400724152,0.));
#63353=CARTESIAN_POINT('Ctrl Pts',(33.8127833826284,-66.2679350453204,0.));
#63354=CARTESIAN_POINT('Ctrl Pts',(33.731810500552,-66.2530062749992,0.));
#63355=CARTESIAN_POINT('Ctrl Pts',(33.6545652280937,-66.2174610329229,0.));
#63356=CARTESIAN_POINT('Ctrl Pts',(33.5903722664954,-66.1657795405668,0.));
#63357=CARTESIAN_POINT('',(33.5903722664955,-66.1657795405668,12.));
#63358=CARTESIAN_POINT('Ctrl Pts',(33.5903722664954,-66.1657795405668,0.));
#63359=CARTESIAN_POINT('Ctrl Pts',(33.5903722664954,-66.1657795405668,4.));
#63360=CARTESIAN_POINT('Ctrl Pts',(33.5903722664955,-66.1657795405668,8.));
#63361=CARTESIAN_POINT('Ctrl Pts',(33.5903722664955,-66.1657795405668,12.));
#63362=CARTESIAN_POINT('',(34.1330090612035,-66.2207497120638,12.));
#63363=CARTESIAN_POINT('Ctrl Pts',(33.5903722664955,-66.1657795405668,12.));
#63364=CARTESIAN_POINT('Ctrl Pts',(33.6545652280938,-66.2174610329229,12.));
#63365=CARTESIAN_POINT('Ctrl Pts',(33.7318105005521,-66.2530062749992,12.));
#63366=CARTESIAN_POINT('Ctrl Pts',(33.8127833826285,-66.2679350453203,12.));
#63367=CARTESIAN_POINT('Ctrl Pts',(33.920747225397,-66.2878400724152,12.));
#63368=CARTESIAN_POINT('Ctrl Pts',(34.0353379297088,-66.2710935941676,12.));
#63369=CARTESIAN_POINT('Ctrl Pts',(34.1330090612035,-66.2207497120638,12.));
#63370=CARTESIAN_POINT('Ctrl Pts',(34.1330090612035,-66.2207497120638,12.));
#63371=CARTESIAN_POINT('Ctrl Pts',(34.1330090612035,-66.2207497120638,8.));
#63372=CARTESIAN_POINT('Ctrl Pts',(34.1330090612035,-66.2207497120638,4.));
#63373=CARTESIAN_POINT('Ctrl Pts',(34.1330090612035,-66.2207497120638,0.));
#63374=CARTESIAN_POINT('Ctrl Pts',(30.354906545781,-63.0759831361898,0.));
#63375=CARTESIAN_POINT('Ctrl Pts',(30.354906545781,-63.0759831361898,12.));
#63376=CARTESIAN_POINT('Ctrl Pts',(30.3574319069329,-63.078933570069,0.));
#63377=CARTESIAN_POINT('Ctrl Pts',(30.3574319069329,-63.078933570069,12.));
#63378=CARTESIAN_POINT('Ctrl Pts',(30.362487768065,-63.0848371718048,0.));
#63379=CARTESIAN_POINT('Ctrl Pts',(30.362487768065,-63.0848371718048,12.));
#63380=CARTESIAN_POINT('Ctrl Pts',(30.3700869762507,-63.0937007763471,0.));
#63381=CARTESIAN_POINT('Ctrl Pts',(30.3700869762507,-63.0937007763471,12.));
#63382=CARTESIAN_POINT('Ctrl Pts',(30.3802500880402,-63.105535320226,0.));
#63383=CARTESIAN_POINT('Ctrl Pts',(30.3802500880402,-63.105535320226,12.));
#63384=CARTESIAN_POINT('Ctrl Pts',(30.3930053710484,-63.1203558300657,0.));
#63385=CARTESIAN_POINT('Ctrl Pts',(30.3930053710484,-63.1203558300657,12.));
#63386=CARTESIAN_POINT('Ctrl Pts',(30.4058120432228,-63.1352036298441,0.));
#63387=CARTESIAN_POINT('Ctrl Pts',(30.4058120432228,-63.1352036298441,12.));
#63388=CARTESIAN_POINT('Ctrl Pts',(30.418670087563,-63.1500786361459,0.));
#63389=CARTESIAN_POINT('Ctrl Pts',(30.418670087563,-63.1500786361459,12.));
#63390=CARTESIAN_POINT('Ctrl Pts',(30.431579465973,-63.164980701691,0.));
#63391=CARTESIAN_POINT('Ctrl Pts',(30.431579465973,-63.164980701691,12.));
#63392=CARTESIAN_POINT('Ctrl Pts',(30.444540119238,-63.179909617189,0.));
#63393=CARTESIAN_POINT('Ctrl Pts',(30.444540119238,-63.179909617189,12.));
#63394=CARTESIAN_POINT('Ctrl Pts',(30.4575519763336,-63.1948651386942,0.));
#63395=CARTESIAN_POINT('Ctrl Pts',(30.4575519763336,-63.1948651386942,12.));
#63396=CARTESIAN_POINT('Ctrl Pts',(30.4706149614159,-63.2098470086636,0.));
#63397=CARTESIAN_POINT('Ctrl Pts',(30.4706149614159,-63.2098470086636,12.));
#63398=CARTESIAN_POINT('Ctrl Pts',(30.4837290014989,-63.2248549788222,0.));
#63399=CARTESIAN_POINT('Ctrl Pts',(30.4837290014989,-63.2248549788222,12.));
#63400=CARTESIAN_POINT('Ctrl Pts',(30.4968940344997,-63.2398888342546,0.));
#63401=CARTESIAN_POINT('Ctrl Pts',(30.4968940344997,-63.2398888342546,12.));
#63402=CARTESIAN_POINT('Ctrl Pts',(30.5101100066659,-63.2549483856215,0.));
#63403=CARTESIAN_POINT('Ctrl Pts',(30.5101100066659,-63.2549483856215,12.));
#63404=CARTESIAN_POINT('Ctrl Pts',(30.5233768687864,-63.2700334577639,0.));
#63405=CARTESIAN_POINT('Ctrl Pts',(30.5233768687864,-63.2700334577639,12.));
#63406=CARTESIAN_POINT('Ctrl Pts',(30.5366945730508,-63.2851438802474,0.));
#63407=CARTESIAN_POINT('Ctrl Pts',(30.5366945730508,-63.2851438802474,12.));
#63408=CARTESIAN_POINT('Ctrl Pts',(30.5500630691359,-63.3002794756086,0.));
#63409=CARTESIAN_POINT('Ctrl Pts',(30.5500630691359,-63.3002794756086,12.));
#63410=CARTESIAN_POINT('Ctrl Pts',(30.5634823022379,-63.3154400534397,0.));
#63411=CARTESIAN_POINT('Ctrl Pts',(30.5634823022379,-63.3154400534397,12.));
#63412=CARTESIAN_POINT('Ctrl Pts',(30.5769522151163,-63.3306254165126,0.));
#63413=CARTESIAN_POINT('Ctrl Pts',(30.5769522151163,-63.3306254165126,12.));
#63414=CARTESIAN_POINT('Ctrl Pts',(30.5904727493711,-63.3458353646154,0.));
#63415=CARTESIAN_POINT('Ctrl Pts',(30.5904727493711,-63.3458353646154,12.));
#63416=CARTESIAN_POINT('Ctrl Pts',(30.6040438469078,-63.3610696989577,0.));
#63417=CARTESIAN_POINT('Ctrl Pts',(30.6040438469078,-63.3610696989577,12.));
#63418=CARTESIAN_POINT('Ctrl Pts',(30.6176654515967,-63.3763282271796,0.));
#63419=CARTESIAN_POINT('Ctrl Pts',(30.6176654515967,-63.3763282271796,12.));
#63420=CARTESIAN_POINT('Ctrl Pts',(30.6313375092062,-63.3916107631376,0.));
#63421=CARTESIAN_POINT('Ctrl Pts',(30.6313375092062,-63.3916107631376,12.));
#63422=CARTESIAN_POINT('Ctrl Pts',(30.645059966612,-63.4069171245067,0.));
#63423=CARTESIAN_POINT('Ctrl Pts',(30.645059966612,-63.4069171245067,12.));
#63424=CARTESIAN_POINT('Ctrl Pts',(30.6588327712483,-63.422247131124,0.));
#63425=CARTESIAN_POINT('Ctrl Pts',(30.6588327712483,-63.422247131124,12.));
#63426=CARTESIAN_POINT('Ctrl Pts',(30.6726558704315,-63.4376006029604,0.));
#63427=CARTESIAN_POINT('Ctrl Pts',(30.6726558704315,-63.4376006029604,12.));
#63428=CARTESIAN_POINT('Ctrl Pts',(30.6865292107929,-63.4529773584249,0.));
#63429=CARTESIAN_POINT('Ctrl Pts',(30.6865292107929,-63.4529773584249,12.));
#63430=CARTESIAN_POINT('Ctrl Pts',(30.7004527385821,-63.468377215253,0.));
#63431=CARTESIAN_POINT('Ctrl Pts',(30.7004527385821,-63.468377215253,12.));
#63432=CARTESIAN_POINT('Ctrl Pts',(30.7144263999265,-63.4837999912772,0.));
#63433=CARTESIAN_POINT('Ctrl Pts',(30.7144263999265,-63.4837999912772,12.));
#63434=CARTESIAN_POINT('Ctrl Pts',(30.7284501410822,-63.4992455051795,0.));
#63435=CARTESIAN_POINT('Ctrl Pts',(30.7284501410822,-63.4992455051795,12.));
#63436=CARTESIAN_POINT('Ctrl Pts',(30.7425239087281,-63.5147135773894,0.));
#63437=CARTESIAN_POINT('Ctrl Pts',(30.7425239087281,-63.5147135773894,12.));
#63438=CARTESIAN_POINT('Ctrl Pts',(30.7566476500757,-63.5302040304142,0.));
#63439=CARTESIAN_POINT('Ctrl Pts',(30.7566476500757,-63.5302040304142,12.));
#63440=CARTESIAN_POINT('Ctrl Pts',(30.7708213127158,-63.5457166883537,0.));
#63441=CARTESIAN_POINT('Ctrl Pts',(30.7708213127158,-63.5457166883537,12.));
#63442=CARTESIAN_POINT('Ctrl Pts',(30.7850448445204,-63.5612513766,0.));
#63443=CARTESIAN_POINT('Ctrl Pts',(30.7850448445204,-63.5612513766,12.));
#63444=CARTESIAN_POINT('Ctrl Pts',(30.7993181935271,-63.5768079214882,0.));
#63445=CARTESIAN_POINT('Ctrl Pts',(30.7993181935271,-63.5768079214882,12.));
#63446=CARTESIAN_POINT('Ctrl Pts',(30.813641307801,-63.5923861498988,0.));
#63447=CARTESIAN_POINT('Ctrl Pts',(30.813641307801,-63.5923861498988,12.));
#63448=CARTESIAN_POINT('Ctrl Pts',(30.8280141354458,-63.6079858892771,0.));
#63449=CARTESIAN_POINT('Ctrl Pts',(30.8280141354458,-63.6079858892771,12.));
#63450=CARTESIAN_POINT('Ctrl Pts',(30.8424366246671,-63.6236069678055,0.));
#63451=CARTESIAN_POINT('Ctrl Pts',(30.8424366246671,-63.6236069678055,12.));
#63452=CARTESIAN_POINT('Ctrl Pts',(30.8569087238131,-63.6392492145233,0.));
#63453=CARTESIAN_POINT('Ctrl Pts',(30.8569087238131,-63.6392492145233,12.));
#63454=CARTESIAN_POINT('Ctrl Pts',(30.8714303814194,-63.6549124594666,0.));
#63455=CARTESIAN_POINT('Ctrl Pts',(30.8714303814194,-63.6549124594666,12.));
#63456=CARTESIAN_POINT('Ctrl Pts',(30.8860015462475,-63.6705965337971,0.));
#63457=CARTESIAN_POINT('Ctrl Pts',(30.8860015462475,-63.6705965337971,12.));
#63458=CARTESIAN_POINT('Ctrl Pts',(30.900622167269,-63.6863012697328,0.));
#63459=CARTESIAN_POINT('Ctrl Pts',(30.900622167269,-63.6863012697328,12.));
#63460=CARTESIAN_POINT('Ctrl Pts',(30.9152921936464,-63.7020265004792,0.));
#63461=CARTESIAN_POINT('Ctrl Pts',(30.9152921936464,-63.7020265004792,12.));
#63462=CARTESIAN_POINT('Ctrl Pts',(30.9300115747115,-63.717772060161,0.));
#63463=CARTESIAN_POINT('Ctrl Pts',(30.9300115747115,-63.717772060161,12.));
#63464=CARTESIAN_POINT('Ctrl Pts',(30.9447802599354,-63.7335377837441,0.));
#63465=CARTESIAN_POINT('Ctrl Pts',(30.9447802599354,-63.7335377837441,12.));
#63466=CARTESIAN_POINT('Ctrl Pts',(30.9595981989103,-63.7493235069871,0.));
#63467=CARTESIAN_POINT('Ctrl Pts',(30.9595981989103,-63.7493235069871,12.));
#63468=CARTESIAN_POINT('Ctrl Pts',(30.9744653413688,-63.7651290664733,0.));
#63469=CARTESIAN_POINT('Ctrl Pts',(30.9744653413688,-63.7651290664733,12.));
#63470=CARTESIAN_POINT('Ctrl Pts',(30.9893816371909,-63.7809542996264,0.));
#63471=CARTESIAN_POINT('Ctrl Pts',(30.9893816371909,-63.7809542996264,12.));
#63472=CARTESIAN_POINT('Ctrl Pts',(31.0043470364108,-63.796799044728,0.));
#63473=CARTESIAN_POINT('Ctrl Pts',(31.0043470364108,-63.796799044728,12.));
#63474=CARTESIAN_POINT('Ctrl Pts',(31.019361489217,-63.8126631409364,0.));
#63475=CARTESIAN_POINT('Ctrl Pts',(31.019361489217,-63.8126631409364,12.));
#63476=CARTESIAN_POINT('Ctrl Pts',(31.0344249459538,-63.8285464282846,0.));
#63477=CARTESIAN_POINT('Ctrl Pts',(31.0344249459538,-63.8285464282846,12.));
#63478=CARTESIAN_POINT('Ctrl Pts',(31.0495373571214,-63.8444487476611,0.));
#63479=CARTESIAN_POINT('Ctrl Pts',(31.0495373571214,-63.8444487476611,12.));
#63480=CARTESIAN_POINT('Ctrl Pts',(31.0646986733723,-63.8603699407922,0.));
#63481=CARTESIAN_POINT('Ctrl Pts',(31.0646986733723,-63.8603699407922,12.));
#63482=CARTESIAN_POINT('Ctrl Pts',(31.0799088455041,-63.8763098502237,0.));
#63483=CARTESIAN_POINT('Ctrl Pts',(31.0799088455041,-63.8763098502237,12.));
#63484=CARTESIAN_POINT('Ctrl Pts',(31.0951678244455,-63.8922683192965,0.));
#63485=CARTESIAN_POINT('Ctrl Pts',(31.0951678244455,-63.8922683192965,12.));
#63486=CARTESIAN_POINT('Ctrl Pts',(31.1104755612607,-63.9082451921448,0.));
#63487=CARTESIAN_POINT('Ctrl Pts',(31.1104755612607,-63.9082451921448,12.));
#63488=CARTESIAN_POINT('Ctrl Pts',(31.1258320071545,-63.9242403136955,0.));
#63489=CARTESIAN_POINT('Ctrl Pts',(31.1258320071545,-63.9242403136955,12.));
#63490=CARTESIAN_POINT('Ctrl Pts',(31.1412371134727,-63.9402535296651,0.));
#63491=CARTESIAN_POINT('Ctrl Pts',(31.1412371134727,-63.9402535296651,12.));
#63492=CARTESIAN_POINT('Ctrl Pts',(31.1566908316991,-63.9562846865567,0.));
#63493=CARTESIAN_POINT('Ctrl Pts',(31.1566908316991,-63.9562846865567,12.));
#63494=CARTESIAN_POINT('Ctrl Pts',(31.1721931134487,-63.9723336316551,0.));
#63495=CARTESIAN_POINT('Ctrl Pts',(31.1721931134487,-63.9723336316551,12.));
#63496=CARTESIAN_POINT('Ctrl Pts',(31.1877439104716,-63.9884002130211,0.));
#63497=CARTESIAN_POINT('Ctrl Pts',(31.1877439104716,-63.9884002130211,12.));
#63498=CARTESIAN_POINT('Ctrl Pts',(31.2033431746558,-64.0044842794832,0.));
#63499=CARTESIAN_POINT('Ctrl Pts',(31.2033431746558,-64.0044842794832,12.));
#63500=CARTESIAN_POINT('Ctrl Pts',(31.2189908580245,-64.02058568063,0.));
#63501=CARTESIAN_POINT('Ctrl Pts',(31.2189908580245,-64.02058568063,12.));
#63502=CARTESIAN_POINT('Ctrl Pts',(31.2346869127297,-64.0367042667984,0.));
#63503=CARTESIAN_POINT('Ctrl Pts',(31.2346869127297,-64.0367042667984,12.));
#63504=CARTESIAN_POINT('Ctrl Pts',(31.2504312910451,-64.0528398890657,0.));
#63505=CARTESIAN_POINT('Ctrl Pts',(31.2504312910451,-64.0528398890657,12.));
#63506=CARTESIAN_POINT('Ctrl Pts',(31.2662239453728,-64.0689923992461,0.));
#63507=CARTESIAN_POINT('Ctrl Pts',(31.2662239453728,-64.0689923992461,12.));
#63508=CARTESIAN_POINT('Ctrl Pts',(31.2820648282447,-64.0851616498853,0.));
#63509=CARTESIAN_POINT('Ctrl Pts',(31.2820648282447,-64.0851616498853,12.));
#63510=CARTESIAN_POINT('Ctrl Pts',(31.2979538923214,-64.1013474942557,0.));
#63511=CARTESIAN_POINT('Ctrl Pts',(31.2979538923214,-64.1013474942557,12.));
#63512=CARTESIAN_POINT('Ctrl Pts',(31.3138910903858,-64.1175497863491,0.));
#63513=CARTESIAN_POINT('Ctrl Pts',(31.3138910903858,-64.1175497863491,12.));
#63514=CARTESIAN_POINT('Ctrl Pts',(31.3298763753376,-64.1337683808691,0.));
#63515=CARTESIAN_POINT('Ctrl Pts',(31.3298763753376,-64.1337683808691,12.));
#63516=CARTESIAN_POINT('Ctrl Pts',(31.3459097002006,-64.1500031332282,0.));
#63517=CARTESIAN_POINT('Ctrl Pts',(31.3459097002006,-64.1500031332282,12.));
#63518=CARTESIAN_POINT('Ctrl Pts',(31.3619910181228,-64.166253899542,0.));
#63519=CARTESIAN_POINT('Ctrl Pts',(31.3619910181228,-64.166253899542,12.));
#63520=CARTESIAN_POINT('Ctrl Pts',(31.3781202823754,-64.1825205366225,0.));
#63521=CARTESIAN_POINT('Ctrl Pts',(31.3781202823754,-64.1825205366225,12.));
#63522=CARTESIAN_POINT('Ctrl Pts',(31.3942974463445,-64.1988029019707,0.));
#63523=CARTESIAN_POINT('Ctrl Pts',(31.3942974463445,-64.1988029019707,12.));
#63524=CARTESIAN_POINT('Ctrl Pts',(31.410522463528,-64.2151008537697,0.));
#63525=CARTESIAN_POINT('Ctrl Pts',(31.410522463528,-64.2151008537697,12.));
#63526=CARTESIAN_POINT('Ctrl Pts',(31.4267952875423,-64.231414250881,0.));
#63527=CARTESIAN_POINT('Ctrl Pts',(31.4267952875423,-64.231414250881,12.));
#63528=CARTESIAN_POINT('Ctrl Pts',(31.4431158721221,-64.2477429528393,0.));
#63529=CARTESIAN_POINT('Ctrl Pts',(31.4431158721221,-64.2477429528393,12.));
#63530=CARTESIAN_POINT('Ctrl Pts',(31.4594841711194,-64.2640868198473,0.));
#63531=CARTESIAN_POINT('Ctrl Pts',(31.4594841711194,-64.2640868198473,12.));
#63532=CARTESIAN_POINT('Ctrl Pts',(31.4759001384941,-64.2804457127671,0.));
#63533=CARTESIAN_POINT('Ctrl Pts',(31.4759001384941,-64.2804457127671,12.));
#63534=CARTESIAN_POINT('Ctrl Pts',(31.4923637283131,-64.2968194931158,0.));
#63535=CARTESIAN_POINT('Ctrl Pts',(31.4923637283131,-64.2968194931158,12.));
#63536=CARTESIAN_POINT('Ctrl Pts',(31.5088748947582,-64.3132080230637,0.));
#63537=CARTESIAN_POINT('Ctrl Pts',(31.5088748947582,-64.3132080230637,12.));
#63538=CARTESIAN_POINT('Ctrl Pts',(31.5254335921245,-64.3296111654283,0.));
#63539=CARTESIAN_POINT('Ctrl Pts',(31.5254335921245,-64.3296111654283,12.));
#63540=CARTESIAN_POINT('Ctrl Pts',(31.5420397748191,-64.3460287836687,0.));
#63541=CARTESIAN_POINT('Ctrl Pts',(31.5420397748191,-64.3460287836687,12.));
#63542=CARTESIAN_POINT('Ctrl Pts',(31.5586933973515,-64.3624607418769,0.));
#63543=CARTESIAN_POINT('Ctrl Pts',(31.5586933973515,-64.3624607418769,12.));
#63544=CARTESIAN_POINT('Ctrl Pts',(31.5753944143336,-64.3789069047734,0.));
#63545=CARTESIAN_POINT('Ctrl Pts',(31.5753944143336,-64.3789069047734,12.));
#63546=CARTESIAN_POINT('Ctrl Pts',(31.5921427804865,-64.3953671377046,0.));
#63547=CARTESIAN_POINT('Ctrl Pts',(31.5921427804865,-64.3953671377046,12.));
#63548=CARTESIAN_POINT('Ctrl Pts',(31.6089384506395,-64.4118413066378,0.));
#63549=CARTESIAN_POINT('Ctrl Pts',(31.6089384506395,-64.4118413066378,12.));
#63550=CARTESIAN_POINT('Ctrl Pts',(31.6257813797287,-64.4283292781565,0.));
#63551=CARTESIAN_POINT('Ctrl Pts',(31.6257813797287,-64.4283292781565,12.));
#63552=CARTESIAN_POINT('Ctrl Pts',(31.6426715227878,-64.4448309194525,0.));
#63553=CARTESIAN_POINT('Ctrl Pts',(31.6426715227878,-64.4448309194525,12.));
#63554=CARTESIAN_POINT('Ctrl Pts',(31.6596088349481,-64.4613460983214,0.));
#63555=CARTESIAN_POINT('Ctrl Pts',(31.6596088349481,-64.4613460983214,12.));
#63556=CARTESIAN_POINT('Ctrl Pts',(31.6765932714464,-64.4778746831614,0.));
#63557=CARTESIAN_POINT('Ctrl Pts',(31.6765932714464,-64.4778746831614,12.));
#63558=CARTESIAN_POINT('Ctrl Pts',(31.6936247876228,-64.4944165429675,0.));
#63559=CARTESIAN_POINT('Ctrl Pts',(31.6936247876228,-64.4944165429675,12.));
#63560=CARTESIAN_POINT('Ctrl Pts',(31.71070333892,-64.510971547327,0.));
#63561=CARTESIAN_POINT('Ctrl Pts',(31.71070333892,-64.510971547327,12.));
#63562=CARTESIAN_POINT('Ctrl Pts',(31.7278288808731,-64.5275395664124,0.));
#63563=CARTESIAN_POINT('Ctrl Pts',(31.7278288808731,-64.5275395664124,12.));
#63564=CARTESIAN_POINT('Ctrl Pts',(31.7450013691111,-64.544120470977,0.));
#63565=CARTESIAN_POINT('Ctrl Pts',(31.7450013691111,-64.544120470977,12.));
#63566=CARTESIAN_POINT('Ctrl Pts',(31.7622207593634,-64.5607141323521,0.));
#63567=CARTESIAN_POINT('Ctrl Pts',(31.7622207593634,-64.5607141323521,12.));
#63568=CARTESIAN_POINT('Ctrl Pts',(31.7794870074583,-64.5773204224429,0.));
#63569=CARTESIAN_POINT('Ctrl Pts',(31.7794870074583,-64.5773204224429,12.));
#63570=CARTESIAN_POINT('Ctrl Pts',(31.7968000693218,-64.5939392137235,0.));
#63571=CARTESIAN_POINT('Ctrl Pts',(31.7968000693218,-64.5939392137235,12.));
#63572=CARTESIAN_POINT('Ctrl Pts',(31.8141599009684,-64.6105703792312,0.));
#63573=CARTESIAN_POINT('Ctrl Pts',(31.8141599009684,-64.6105703792312,12.));
#63574=CARTESIAN_POINT('Ctrl Pts',(31.8315664585025,-64.6272137925627,0.));
#63575=CARTESIAN_POINT('Ctrl Pts',(31.8315664585025,-64.6272137925627,12.));
#63576=CARTESIAN_POINT('Ctrl Pts',(31.8490196981248,-64.6438693278714,0.));
#63577=CARTESIAN_POINT('Ctrl Pts',(31.8490196981248,-64.6438693278714,12.));
#63578=CARTESIAN_POINT('Ctrl Pts',(31.866519576131,-64.6605368598629,0.));
#63579=CARTESIAN_POINT('Ctrl Pts',(31.866519576131,-64.6605368598629,12.));
#63580=CARTESIAN_POINT('Ctrl Pts',(31.8840660489106,-64.6772162637907,0.));
#63581=CARTESIAN_POINT('Ctrl Pts',(31.8840660489106,-64.6772162637907,12.));
#63582=CARTESIAN_POINT('Ctrl Pts',(31.9016590729373,-64.6939074154498,0.));
#63583=CARTESIAN_POINT('Ctrl Pts',(31.9016590729373,-64.6939074154498,12.));
#63584=CARTESIAN_POINT('Ctrl Pts',(31.9192986047705,-64.7106101911732,0.));
#63585=CARTESIAN_POINT('Ctrl Pts',(31.9192986047705,-64.7106101911732,12.));
#63586=CARTESIAN_POINT('Ctrl Pts',(31.9369846010615,-64.7273244678297,0.));
#63587=CARTESIAN_POINT('Ctrl Pts',(31.9369846010615,-64.7273244678297,12.));
#63588=CARTESIAN_POINT('Ctrl Pts',(31.9547170185533,-64.7440501228203,0.));
#63589=CARTESIAN_POINT('Ctrl Pts',(31.9547170185533,-64.7440501228203,12.));
#63590=CARTESIAN_POINT('Ctrl Pts',(31.9724958140789,-64.7607870340735,0.));
#63591=CARTESIAN_POINT('Ctrl Pts',(31.9724958140789,-64.7607870340735,12.));
#63592=CARTESIAN_POINT('Ctrl Pts',(31.9903209445519,-64.7775350800401,0.));
#63593=CARTESIAN_POINT('Ctrl Pts',(31.9903209445519,-64.7775350800401,12.));
#63594=CARTESIAN_POINT('Ctrl Pts',(32.0081923669676,-64.7942941396881,0.));
#63595=CARTESIAN_POINT('Ctrl Pts',(32.0081923669676,-64.7942941396881,12.));
#63596=CARTESIAN_POINT('Ctrl Pts',(32.0261100384092,-64.8110640925021,0.));
#63597=CARTESIAN_POINT('Ctrl Pts',(32.0261100384092,-64.8110640925021,12.));
#63598=CARTESIAN_POINT('Ctrl Pts',(32.0440739160477,-64.8278448184787,0.));
#63599=CARTESIAN_POINT('Ctrl Pts',(32.0440739160477,-64.8278448184787,12.));
#63600=CARTESIAN_POINT('Ctrl Pts',(32.0620839571408,-64.8446361981234,0.));
#63601=CARTESIAN_POINT('Ctrl Pts',(32.0620839571408,-64.8446361981234,12.));
#63602=CARTESIAN_POINT('Ctrl Pts',(32.0801401190241,-64.861438112445,0.));
#63603=CARTESIAN_POINT('Ctrl Pts',(32.0801401190241,-64.861438112445,12.));
#63604=CARTESIAN_POINT('Ctrl Pts',(32.0982423591108,-64.878250442952,0.));
#63605=CARTESIAN_POINT('Ctrl Pts',(32.0982423591108,-64.878250442952,12.));
#63606=CARTESIAN_POINT('Ctrl Pts',(32.1163906348979,-64.8950730716493,0.));
#63607=CARTESIAN_POINT('Ctrl Pts',(32.1163906348979,-64.8950730716493,12.));
#63608=CARTESIAN_POINT('Ctrl Pts',(32.1345849039671,-64.9119058810362,0.));
#63609=CARTESIAN_POINT('Ctrl Pts',(32.1345849039671,-64.9119058810362,12.));
#63610=CARTESIAN_POINT('Ctrl Pts',(32.1528251239831,-64.9287487541019,0.));
#63611=CARTESIAN_POINT('Ctrl Pts',(32.1528251239831,-64.9287487541019,12.));
#63612=CARTESIAN_POINT('Ctrl Pts',(32.1711112526859,-64.9456015743203,0.));
#63613=CARTESIAN_POINT('Ctrl Pts',(32.1711112526859,-64.9456015743203,12.));
#63614=CARTESIAN_POINT('Ctrl Pts',(32.1894432478888,-64.9624642256478,0.));
#63615=CARTESIAN_POINT('Ctrl Pts',(32.1894432478888,-64.9624642256478,12.));
#63616=CARTESIAN_POINT('Ctrl Pts',(32.2078210674857,-64.9793365925194,0.));
#63617=CARTESIAN_POINT('Ctrl Pts',(32.2078210674857,-64.9793365925194,12.));
#63618=CARTESIAN_POINT('Ctrl Pts',(32.2262446694516,-64.996218559847,0.));
#63619=CARTESIAN_POINT('Ctrl Pts',(32.2262446694516,-64.996218559847,12.));
#63620=CARTESIAN_POINT('Ctrl Pts',(32.244714011842,-65.0131100130155,0.));
#63621=CARTESIAN_POINT('Ctrl Pts',(32.244714011842,-65.0131100130155,12.));
#63622=CARTESIAN_POINT('Ctrl Pts',(32.2632290527854,-65.0300108378786,0.));
#63623=CARTESIAN_POINT('Ctrl Pts',(32.2632290527854,-65.0300108378786,12.));
#63624=CARTESIAN_POINT('Ctrl Pts',(32.2817897504799,-65.0469209207548,0.));
#63625=CARTESIAN_POINT('Ctrl Pts',(32.2817897504799,-65.0469209207548,12.));
#63626=CARTESIAN_POINT('Ctrl Pts',(32.3003960632,-65.0638401484245,0.));
#63627=CARTESIAN_POINT('Ctrl Pts',(32.3003960632,-65.0638401484245,12.));
#63628=CARTESIAN_POINT('Ctrl Pts',(32.3190479492985,-65.0807684081278,0.));
#63629=CARTESIAN_POINT('Ctrl Pts',(32.3190479492985,-65.0807684081278,12.));
#63630=CARTESIAN_POINT('Ctrl Pts',(32.3377453672051,-65.097705587561,0.));
#63631=CARTESIAN_POINT('Ctrl Pts',(32.3377453672051,-65.097705587561,12.));
#63632=CARTESIAN_POINT('Ctrl Pts',(32.3564882754212,-65.1146515748723,0.));
#63633=CARTESIAN_POINT('Ctrl Pts',(32.3564882754212,-65.1146515748723,12.));
#63634=CARTESIAN_POINT('Ctrl Pts',(32.3752766325134,-65.1316062586586,0.));
#63635=CARTESIAN_POINT('Ctrl Pts',(32.3752766325134,-65.1316062586586,12.));
#63636=CARTESIAN_POINT('Ctrl Pts',(32.3941103971218,-65.1485695279628,0.));
#63637=CARTESIAN_POINT('Ctrl Pts',(32.3941103971218,-65.1485695279628,12.));
#63638=CARTESIAN_POINT('Ctrl Pts',(32.4129895279612,-65.165541272272,0.));
#63639=CARTESIAN_POINT('Ctrl Pts',(32.4129895279612,-65.165541272272,12.));
#63640=CARTESIAN_POINT('Ctrl Pts',(32.4319139838212,-65.182521381514,0.));
#63641=CARTESIAN_POINT('Ctrl Pts',(32.4319139838212,-65.182521381514,12.));
#63642=CARTESIAN_POINT('Ctrl Pts',(32.4508837235613,-65.1995097460546,0.));
#63643=CARTESIAN_POINT('Ctrl Pts',(32.4508837235613,-65.1995097460546,12.));
#63644=CARTESIAN_POINT('Ctrl Pts',(32.4698987061036,-65.2165062566936,0.));
#63645=CARTESIAN_POINT('Ctrl Pts',(32.4698987061036,-65.2165062566936,12.));
#63646=CARTESIAN_POINT('Ctrl Pts',(32.4889588904396,-65.2335108046625,0.));
#63647=CARTESIAN_POINT('Ctrl Pts',(32.4889588904396,-65.2335108046625,12.));
#63648=CARTESIAN_POINT('Ctrl Pts',(32.508064235633,-65.2505232816215,0.));
#63649=CARTESIAN_POINT('Ctrl Pts',(32.508064235633,-65.2505232816215,12.));
#63650=CARTESIAN_POINT('Ctrl Pts',(32.527214700819,-65.2675435796558,0.));
#63651=CARTESIAN_POINT('Ctrl Pts',(32.527214700819,-65.2675435796558,12.));
#63652=CARTESIAN_POINT('Ctrl Pts',(32.5464102452013,-65.2845715912717,0.));
#63653=CARTESIAN_POINT('Ctrl Pts',(32.5464102452013,-65.2845715912717,12.));
#63654=CARTESIAN_POINT('Ctrl Pts',(32.565650828042,-65.3016072093908,0.));
#63655=CARTESIAN_POINT('Ctrl Pts',(32.565650828042,-65.3016072093908,12.));
#63656=CARTESIAN_POINT('Ctrl Pts',(32.5849364086678,-65.3186503273498,0.));
#63657=CARTESIAN_POINT('Ctrl Pts',(32.5849364086678,-65.3186503273498,12.));
#63658=CARTESIAN_POINT('Ctrl Pts',(32.6042669464751,-65.3357008389005,0.));
#63659=CARTESIAN_POINT('Ctrl Pts',(32.6042669464751,-65.3357008389005,12.));
#63660=CARTESIAN_POINT('Ctrl Pts',(32.6236424009301,-65.3527586382082,0.));
#63661=CARTESIAN_POINT('Ctrl Pts',(32.6236424009301,-65.3527586382082,12.));
#63662=CARTESIAN_POINT('Ctrl Pts',(32.6430627315672,-65.3698236198512,0.));
#63663=CARTESIAN_POINT('Ctrl Pts',(32.6430627315672,-65.3698236198512,12.));
#63664=CARTESIAN_POINT('Ctrl Pts',(32.6625278979807,-65.3868956788178,0.));
#63665=CARTESIAN_POINT('Ctrl Pts',(32.6625278979807,-65.3868956788178,12.));
#63666=CARTESIAN_POINT('Ctrl Pts',(32.6820378598262,-65.4039747105033,0.));
#63667=CARTESIAN_POINT('Ctrl Pts',(32.6820378598262,-65.4039747105033,12.));
#63668=CARTESIAN_POINT('Ctrl Pts',(32.701592576826,-65.421060610703,0.));
#63669=CARTESIAN_POINT('Ctrl Pts',(32.701592576826,-65.421060610703,12.));
#63670=CARTESIAN_POINT('Ctrl Pts',(32.7211920087681,-65.4381532756063,0.));
#63671=CARTESIAN_POINT('Ctrl Pts',(32.7211920087681,-65.4381532756063,12.));
#63672=CARTESIAN_POINT('Ctrl Pts',(32.7408361155037,-65.4552526017907,0.));
#63673=CARTESIAN_POINT('Ctrl Pts',(32.7408361155037,-65.4552526017907,12.));
#63674=CARTESIAN_POINT('Ctrl Pts',(32.7605248569382,-65.4723584862129,0.));
#63675=CARTESIAN_POINT('Ctrl Pts',(32.7605248569382,-65.4723584862129,12.));
#63676=CARTESIAN_POINT('Ctrl Pts',(32.7802581930293,-65.4894708262071,0.));
#63677=CARTESIAN_POINT('Ctrl Pts',(32.7802581930293,-65.4894708262071,12.));
#63678=CARTESIAN_POINT('Ctrl Pts',(32.800036083798,-65.5065895194939,0.));
#63679=CARTESIAN_POINT('Ctrl Pts',(32.800036083798,-65.5065895194939,12.));
#63680=CARTESIAN_POINT('Ctrl Pts',(32.8198584893318,-65.5237144641864,0.));
#63681=CARTESIAN_POINT('Ctrl Pts',(32.8198584893318,-65.5237144641864,12.));
#63682=CARTESIAN_POINT('Ctrl Pts',(32.8397253697864,-65.5408455587963,0.));
#63683=CARTESIAN_POINT('Ctrl Pts',(32.8397253697864,-65.5408455587963,12.));
#63684=CARTESIAN_POINT('Ctrl Pts',(32.8596366853826,-65.5579827022413,0.));
#63685=CARTESIAN_POINT('Ctrl Pts',(32.8596366853826,-65.5579827022413,12.));
#63686=CARTESIAN_POINT('Ctrl Pts',(32.8795923964021,-65.575125793846,0.));
#63687=CARTESIAN_POINT('Ctrl Pts',(32.8795923964021,-65.575125793846,12.));
#63688=CARTESIAN_POINT('Ctrl Pts',(32.899592463189,-65.5922747333182,0.));
#63689=CARTESIAN_POINT('Ctrl Pts',(32.899592463189,-65.5922747333182,12.));
#63690=CARTESIAN_POINT('Ctrl Pts',(32.9196368461457,-65.6094294207267,0.));
#63691=CARTESIAN_POINT('Ctrl Pts',(32.9196368461457,-65.6094294207267,12.));
#63692=CARTESIAN_POINT('Ctrl Pts',(32.9397255057273,-65.6265897564782,0.));
#63693=CARTESIAN_POINT('Ctrl Pts',(32.9397255057273,-65.6265897564782,12.));
#63694=CARTESIAN_POINT('Ctrl Pts',(32.9598584024317,-65.6437556412956,0.));
#63695=CARTESIAN_POINT('Ctrl Pts',(32.9598584024317,-65.6437556412956,12.));
#63696=CARTESIAN_POINT('Ctrl Pts',(32.9800354967846,-65.6609269761902,0.));
#63697=CARTESIAN_POINT('Ctrl Pts',(32.9800354967846,-65.6609269761902,12.));
#63698=CARTESIAN_POINT('Ctrl Pts',(33.000256749358,-65.6781036625041,0.));
#63699=CARTESIAN_POINT('Ctrl Pts',(33.000256749358,-65.6781036625041,12.));
#63700=CARTESIAN_POINT('Ctrl Pts',(33.0205221207877,-65.6952856019542,0.));
#63701=CARTESIAN_POINT('Ctrl Pts',(33.0205221207877,-65.6952856019542,12.));
#63702=CARTESIAN_POINT('Ctrl Pts',(33.0408315717874,-65.7124726966805,0.));
#63703=CARTESIAN_POINT('Ctrl Pts',(33.0408315717874,-65.7124726966805,12.));
#63704=CARTESIAN_POINT('Ctrl Pts',(33.0611850631579,-65.729664849282,0.));
#63705=CARTESIAN_POINT('Ctrl Pts',(33.0611850631579,-65.729664849282,12.));
#63706=CARTESIAN_POINT('Ctrl Pts',(33.0815825557976,-65.7468619628808,0.));
#63707=CARTESIAN_POINT('Ctrl Pts',(33.0815825557976,-65.7468619628808,12.));
#63708=CARTESIAN_POINT('Ctrl Pts',(33.102024010688,-65.7640639410653,0.));
#63709=CARTESIAN_POINT('Ctrl Pts',(33.102024010688,-65.7640639410653,12.));
#63710=CARTESIAN_POINT('Ctrl Pts',(33.1225093888668,-65.7812706877691,0.));
#63711=CARTESIAN_POINT('Ctrl Pts',(33.1225093888668,-65.7812706877691,12.));
#63712=CARTESIAN_POINT('Ctrl Pts',(33.1430386513975,-65.7984821071622,0.));
#63713=CARTESIAN_POINT('Ctrl Pts',(33.1430386513975,-65.7984821071622,12.));
#63714=CARTESIAN_POINT('Ctrl Pts',(33.16361175934,-65.8156981035504,0.));
#63715=CARTESIAN_POINT('Ctrl Pts',(33.16361175934,-65.8156981035504,12.));
#63716=CARTESIAN_POINT('Ctrl Pts',(33.1842286737053,-65.8329185812379,0.));
#63717=CARTESIAN_POINT('Ctrl Pts',(33.1842286737053,-65.8329185812379,12.));
#63718=CARTESIAN_POINT('Ctrl Pts',(33.2048893554495,-65.8501434445174,0.));
#63719=CARTESIAN_POINT('Ctrl Pts',(33.2048893554495,-65.8501434445174,12.));
#63720=CARTESIAN_POINT('Ctrl Pts',(33.2255937655655,-65.8673725979591,0.));
#63721=CARTESIAN_POINT('Ctrl Pts',(33.2255937655655,-65.8673725979591,12.));
#63722=CARTESIAN_POINT('Ctrl Pts',(33.2463418651497,-65.8846059466382,0.));
#63723=CARTESIAN_POINT('Ctrl Pts',(33.2463418651497,-65.8846059466382,12.));
#63724=CARTESIAN_POINT('Ctrl Pts',(33.2671336154754,-65.901843396389,0.));
#63725=CARTESIAN_POINT('Ctrl Pts',(33.2671336154754,-65.901843396389,12.));
#63726=CARTESIAN_POINT('Ctrl Pts',(33.2879689780566,-65.9190848540422,0.));
#63727=CARTESIAN_POINT('Ctrl Pts',(33.2879689780566,-65.9190848540422,12.));
#63728=CARTESIAN_POINT('Ctrl Pts',(33.308847914715,-65.9363302276822,0.));
#63729=CARTESIAN_POINT('Ctrl Pts',(33.308847914715,-65.9363302276822,12.));
#63730=CARTESIAN_POINT('Ctrl Pts',(33.3297703874249,-65.9535794260802,0.));
#63731=CARTESIAN_POINT('Ctrl Pts',(33.3297703874249,-65.9535794260802,12.));
#63732=CARTESIAN_POINT('Ctrl Pts',(33.3507363581578,-65.9708323581386,0.));
#63733=CARTESIAN_POINT('Ctrl Pts',(33.3507363581578,-65.9708323581386,12.));
#63734=CARTESIAN_POINT('Ctrl Pts',(33.3717457887094,-65.9880889322822,0.));
#63735=CARTESIAN_POINT('Ctrl Pts',(33.3717457887094,-65.9880889322822,12.));
#63736=CARTESIAN_POINT('Ctrl Pts',(33.3927986405612,-66.0053490559826,0.));
#63737=CARTESIAN_POINT('Ctrl Pts',(33.3927986405612,-66.0053490559826,12.));
#63738=CARTESIAN_POINT('Ctrl Pts',(33.4138948746407,-66.0226126349482,0.));
#63739=CARTESIAN_POINT('Ctrl Pts',(33.4138948746407,-66.0226126349482,12.));
#63740=CARTESIAN_POINT('Ctrl Pts',(33.4350344515128,-66.0398795737827,0.));
#63741=CARTESIAN_POINT('Ctrl Pts',(33.4350344515128,-66.0398795737827,12.));
#63742=CARTESIAN_POINT('Ctrl Pts',(33.4562173318052,-66.0571497774484,0.));
#63743=CARTESIAN_POINT('Ctrl Pts',(33.4562173318052,-66.0571497774484,12.));
#63744=CARTESIAN_POINT('Ctrl Pts',(33.4774434765761,-66.0744231525445,0.));
#63745=CARTESIAN_POINT('Ctrl Pts',(33.4774434765761,-66.0744231525445,12.));
#63746=CARTESIAN_POINT('Ctrl Pts',(33.4987128476617,-66.0916996085237,0.));
#63747=CARTESIAN_POINT('Ctrl Pts',(33.4987128476617,-66.0916996085237,12.));
#63748=CARTESIAN_POINT('Ctrl Pts',(33.5200254081212,-66.1089790592673,0.));
#63749=CARTESIAN_POINT('Ctrl Pts',(33.5200254081212,-66.1089790592673,12.));
#63750=CARTESIAN_POINT('Ctrl Pts',(33.5413811223397,-66.1262614234579,0.));
#63751=CARTESIAN_POINT('Ctrl Pts',(33.5413811223397,-66.1262614234579,12.));
#63752=CARTESIAN_POINT('Ctrl Pts',(33.5627799550422,-66.1435466210967,0.));
#63753=CARTESIAN_POINT('Ctrl Pts',(33.5627799550422,-66.1435466210967,12.));
#63754=CARTESIAN_POINT('Ctrl Pts',(33.5842218705103,-66.1608345707552,0.));
#63755=CARTESIAN_POINT('Ctrl Pts',(33.5842218705103,-66.1608345707552,12.));
#63756=CARTESIAN_POINT('Ctrl Pts',(33.6057068316758,-66.1781251863998,0.));
#63757=CARTESIAN_POINT('Ctrl Pts',(33.6057068316758,-66.1781251863998,12.));
#63758=CARTESIAN_POINT('Ctrl Pts',(33.6272347993519,-66.1954183747167,0.));
#63759=CARTESIAN_POINT('Ctrl Pts',(33.6272347993519,-66.1954183747167,12.));
#63760=CARTESIAN_POINT('Ctrl Pts',(33.648805731163,-66.2127140313777,0.));
#63761=CARTESIAN_POINT('Ctrl Pts',(33.648805731163,-66.2127140313777,12.));
#63762=CARTESIAN_POINT('Ctrl Pts',(33.6704195830525,-66.2300120464323,0.));
#63763=CARTESIAN_POINT('Ctrl Pts',(33.6704195830525,-66.2300120464323,12.));
#63764=CARTESIAN_POINT('Ctrl Pts',(33.6920763111575,-66.2473123109627,0.));
#63765=CARTESIAN_POINT('Ctrl Pts',(33.6920763111575,-66.2473123109627,12.));
#63766=CARTESIAN_POINT('Ctrl Pts',(33.713775873597,-66.2646147235444,0.));
#63767=CARTESIAN_POINT('Ctrl Pts',(33.713775873597,-66.2646147235444,12.));
#63768=CARTESIAN_POINT('Ctrl Pts',(33.7355182321862,-66.2819191962273,0.));
#63769=CARTESIAN_POINT('Ctrl Pts',(33.7355182321862,-66.2819191962273,12.));
#63770=CARTESIAN_POINT('Ctrl Pts',(33.7573033544373,-66.2992256621001,0.));
#63771=CARTESIAN_POINT('Ctrl Pts',(33.7573033544373,-66.2992256621001,12.));
#63772=CARTESIAN_POINT('Ctrl Pts',(33.7791312144798,-66.3165340771053,0.));
#63773=CARTESIAN_POINT('Ctrl Pts',(33.7791312144798,-66.3165340771053,12.));
#63774=CARTESIAN_POINT('Ctrl Pts',(33.8010017925666,-66.333844414356,0.));
#63775=CARTESIAN_POINT('Ctrl Pts',(33.8010017925666,-66.333844414356,12.));
#63776=CARTESIAN_POINT('Ctrl Pts',(33.8185324184601,-66.3476942111456,0.));
#63777=CARTESIAN_POINT('Ctrl Pts',(33.8185324184601,-66.3476942111456,12.));
#63778=CARTESIAN_POINT('Ctrl Pts',(33.831699601175,-66.3580824155565,0.));
#63779=CARTESIAN_POINT('Ctrl Pts',(33.831699601175,-66.3580824155565,12.));
#63780=CARTESIAN_POINT('Ctrl Pts',(33.8404862618803,-66.3650082659593,0.));
#63781=CARTESIAN_POINT('Ctrl Pts',(33.8404862618803,-66.3650082659593,12.));
#63782=CARTESIAN_POINT('Ctrl Pts',(33.8448817269567,-66.3684712863594,0.));
#63783=CARTESIAN_POINT('Ctrl Pts',(33.8448817269567,-66.3684712863594,12.));
#63784=CARTESIAN_POINT('',(30.354906545781,-63.0759831361898,0.));
#63785=CARTESIAN_POINT('Ctrl Pts',(30.354906545781,-63.0759831361898,0.));
#63786=CARTESIAN_POINT('Ctrl Pts',(30.3574319069329,-63.078933570069,0.));
#63787=CARTESIAN_POINT('Ctrl Pts',(30.362487768065,-63.0848371718048,0.));
#63788=CARTESIAN_POINT('Ctrl Pts',(30.3700869762507,-63.0937007763471,0.));
#63789=CARTESIAN_POINT('Ctrl Pts',(30.3802500880402,-63.105535320226,0.));
#63790=CARTESIAN_POINT('Ctrl Pts',(30.3930053710484,-63.1203558300657,0.));
#63791=CARTESIAN_POINT('Ctrl Pts',(30.4058120432228,-63.1352036298441,0.));
#63792=CARTESIAN_POINT('Ctrl Pts',(30.418670087563,-63.1500786361459,0.));
#63793=CARTESIAN_POINT('Ctrl Pts',(30.431579465973,-63.164980701691,0.));
#63794=CARTESIAN_POINT('Ctrl Pts',(30.444540119238,-63.179909617189,0.));
#63795=CARTESIAN_POINT('Ctrl Pts',(30.4575519763336,-63.1948651386942,0.));
#63796=CARTESIAN_POINT('Ctrl Pts',(30.4706149614159,-63.2098470086636,0.));
#63797=CARTESIAN_POINT('Ctrl Pts',(30.4837290014989,-63.2248549788222,0.));
#63798=CARTESIAN_POINT('Ctrl Pts',(30.4968940344997,-63.2398888342546,0.));
#63799=CARTESIAN_POINT('Ctrl Pts',(30.5101100066659,-63.2549483856215,0.));
#63800=CARTESIAN_POINT('Ctrl Pts',(30.5233768687864,-63.2700334577639,0.));
#63801=CARTESIAN_POINT('Ctrl Pts',(30.5366945730508,-63.2851438802474,0.));
#63802=CARTESIAN_POINT('Ctrl Pts',(30.5500630691359,-63.3002794756086,0.));
#63803=CARTESIAN_POINT('Ctrl Pts',(30.5634823022379,-63.3154400534397,0.));
#63804=CARTESIAN_POINT('Ctrl Pts',(30.5769522151163,-63.3306254165126,0.));
#63805=CARTESIAN_POINT('Ctrl Pts',(30.5904727493711,-63.3458353646154,0.));
#63806=CARTESIAN_POINT('Ctrl Pts',(30.6040438469078,-63.3610696989577,0.));
#63807=CARTESIAN_POINT('Ctrl Pts',(30.6176654515967,-63.3763282271796,0.));
#63808=CARTESIAN_POINT('Ctrl Pts',(30.6313375092062,-63.3916107631376,0.));
#63809=CARTESIAN_POINT('Ctrl Pts',(30.645059966612,-63.4069171245067,0.));
#63810=CARTESIAN_POINT('Ctrl Pts',(30.6588327712483,-63.422247131124,0.));
#63811=CARTESIAN_POINT('Ctrl Pts',(30.6726558704315,-63.4376006029604,0.));
#63812=CARTESIAN_POINT('Ctrl Pts',(30.6865292107929,-63.4529773584249,0.));
#63813=CARTESIAN_POINT('Ctrl Pts',(30.7004527385821,-63.468377215253,0.));
#63814=CARTESIAN_POINT('Ctrl Pts',(30.7144263999265,-63.4837999912772,0.));
#63815=CARTESIAN_POINT('Ctrl Pts',(30.7284501410822,-63.4992455051795,0.));
#63816=CARTESIAN_POINT('Ctrl Pts',(30.7425239087281,-63.5147135773894,0.));
#63817=CARTESIAN_POINT('Ctrl Pts',(30.7566476500757,-63.5302040304142,0.));
#63818=CARTESIAN_POINT('Ctrl Pts',(30.7708213127158,-63.5457166883537,0.));
#63819=CARTESIAN_POINT('Ctrl Pts',(30.7850448445204,-63.5612513766,0.));
#63820=CARTESIAN_POINT('Ctrl Pts',(30.7993181935271,-63.5768079214882,0.));
#63821=CARTESIAN_POINT('Ctrl Pts',(30.813641307801,-63.5923861498988,0.));
#63822=CARTESIAN_POINT('Ctrl Pts',(30.8280141354458,-63.6079858892771,0.));
#63823=CARTESIAN_POINT('Ctrl Pts',(30.8424366246671,-63.6236069678055,0.));
#63824=CARTESIAN_POINT('Ctrl Pts',(30.8569087238131,-63.6392492145233,0.));
#63825=CARTESIAN_POINT('Ctrl Pts',(30.8714303814194,-63.6549124594666,0.));
#63826=CARTESIAN_POINT('Ctrl Pts',(30.8860015462475,-63.6705965337971,0.));
#63827=CARTESIAN_POINT('Ctrl Pts',(30.900622167269,-63.6863012697328,0.));
#63828=CARTESIAN_POINT('Ctrl Pts',(30.9152921936464,-63.7020265004792,0.));
#63829=CARTESIAN_POINT('Ctrl Pts',(30.9300115747115,-63.717772060161,0.));
#63830=CARTESIAN_POINT('Ctrl Pts',(30.9447802599354,-63.7335377837441,0.));
#63831=CARTESIAN_POINT('Ctrl Pts',(30.9595981989103,-63.7493235069871,0.));
#63832=CARTESIAN_POINT('Ctrl Pts',(30.9744653413688,-63.7651290664733,0.));
#63833=CARTESIAN_POINT('Ctrl Pts',(30.9893816371909,-63.7809542996264,0.));
#63834=CARTESIAN_POINT('Ctrl Pts',(31.0043470364108,-63.796799044728,0.));
#63835=CARTESIAN_POINT('Ctrl Pts',(31.019361489217,-63.8126631409364,0.));
#63836=CARTESIAN_POINT('Ctrl Pts',(31.0344249459538,-63.8285464282846,0.));
#63837=CARTESIAN_POINT('Ctrl Pts',(31.0495373571214,-63.8444487476611,0.));
#63838=CARTESIAN_POINT('Ctrl Pts',(31.0646986733723,-63.8603699407922,0.));
#63839=CARTESIAN_POINT('Ctrl Pts',(31.0799088455041,-63.8763098502237,0.));
#63840=CARTESIAN_POINT('Ctrl Pts',(31.0951678244455,-63.8922683192965,0.));
#63841=CARTESIAN_POINT('Ctrl Pts',(31.1104755612607,-63.9082451921448,0.));
#63842=CARTESIAN_POINT('Ctrl Pts',(31.1258320071545,-63.9242403136955,0.));
#63843=CARTESIAN_POINT('Ctrl Pts',(31.1412371134727,-63.9402535296651,0.));
#63844=CARTESIAN_POINT('Ctrl Pts',(31.1566908316991,-63.9562846865567,0.));
#63845=CARTESIAN_POINT('Ctrl Pts',(31.1721931134487,-63.9723336316551,0.));
#63846=CARTESIAN_POINT('Ctrl Pts',(31.1877439104716,-63.9884002130211,0.));
#63847=CARTESIAN_POINT('Ctrl Pts',(31.2033431746558,-64.0044842794832,0.));
#63848=CARTESIAN_POINT('Ctrl Pts',(31.2189908580245,-64.02058568063,0.));
#63849=CARTESIAN_POINT('Ctrl Pts',(31.2346869127297,-64.0367042667984,0.));
#63850=CARTESIAN_POINT('Ctrl Pts',(31.2504312910451,-64.0528398890657,0.));
#63851=CARTESIAN_POINT('Ctrl Pts',(31.2662239453728,-64.0689923992461,0.));
#63852=CARTESIAN_POINT('Ctrl Pts',(31.2820648282447,-64.0851616498853,0.));
#63853=CARTESIAN_POINT('Ctrl Pts',(31.2979538923214,-64.1013474942557,0.));
#63854=CARTESIAN_POINT('Ctrl Pts',(31.3138910903858,-64.1175497863491,0.));
#63855=CARTESIAN_POINT('Ctrl Pts',(31.3298763753376,-64.1337683808691,0.));
#63856=CARTESIAN_POINT('Ctrl Pts',(31.3459097002006,-64.1500031332282,0.));
#63857=CARTESIAN_POINT('Ctrl Pts',(31.3619910181228,-64.166253899542,0.));
#63858=CARTESIAN_POINT('Ctrl Pts',(31.3781202823754,-64.1825205366225,0.));
#63859=CARTESIAN_POINT('Ctrl Pts',(31.3942974463445,-64.1988029019707,0.));
#63860=CARTESIAN_POINT('Ctrl Pts',(31.410522463528,-64.2151008537697,0.));
#63861=CARTESIAN_POINT('Ctrl Pts',(31.4267952875423,-64.231414250881,0.));
#63862=CARTESIAN_POINT('Ctrl Pts',(31.4431158721221,-64.2477429528393,0.));
#63863=CARTESIAN_POINT('Ctrl Pts',(31.4594841711194,-64.2640868198473,0.));
#63864=CARTESIAN_POINT('Ctrl Pts',(31.4759001384941,-64.2804457127671,0.));
#63865=CARTESIAN_POINT('Ctrl Pts',(31.4923637283131,-64.2968194931158,0.));
#63866=CARTESIAN_POINT('Ctrl Pts',(31.5088748947582,-64.3132080230637,0.));
#63867=CARTESIAN_POINT('Ctrl Pts',(31.5254335921245,-64.3296111654283,0.));
#63868=CARTESIAN_POINT('Ctrl Pts',(31.5420397748191,-64.3460287836687,0.));
#63869=CARTESIAN_POINT('Ctrl Pts',(31.5586933973515,-64.3624607418769,0.));
#63870=CARTESIAN_POINT('Ctrl Pts',(31.5753944143336,-64.3789069047734,0.));
#63871=CARTESIAN_POINT('Ctrl Pts',(31.5921427804865,-64.3953671377046,0.));
#63872=CARTESIAN_POINT('Ctrl Pts',(31.6089384506395,-64.4118413066378,0.));
#63873=CARTESIAN_POINT('Ctrl Pts',(31.6257813797287,-64.4283292781565,0.));
#63874=CARTESIAN_POINT('Ctrl Pts',(31.6426715227878,-64.4448309194525,0.));
#63875=CARTESIAN_POINT('Ctrl Pts',(31.6596088349481,-64.4613460983214,0.));
#63876=CARTESIAN_POINT('Ctrl Pts',(31.6765932714464,-64.4778746831614,0.));
#63877=CARTESIAN_POINT('Ctrl Pts',(31.6936247876228,-64.4944165429675,0.));
#63878=CARTESIAN_POINT('Ctrl Pts',(31.71070333892,-64.510971547327,0.));
#63879=CARTESIAN_POINT('Ctrl Pts',(31.7278288808731,-64.5275395664124,0.));
#63880=CARTESIAN_POINT('Ctrl Pts',(31.7450013691111,-64.544120470977,0.));
#63881=CARTESIAN_POINT('Ctrl Pts',(31.7622207593634,-64.5607141323521,0.));
#63882=CARTESIAN_POINT('Ctrl Pts',(31.7794870074583,-64.5773204224429,0.));
#63883=CARTESIAN_POINT('Ctrl Pts',(31.7968000693218,-64.5939392137235,0.));
#63884=CARTESIAN_POINT('Ctrl Pts',(31.8141599009684,-64.6105703792312,0.));
#63885=CARTESIAN_POINT('Ctrl Pts',(31.8315664585025,-64.6272137925627,0.));
#63886=CARTESIAN_POINT('Ctrl Pts',(31.8490196981248,-64.6438693278714,0.));
#63887=CARTESIAN_POINT('Ctrl Pts',(31.866519576131,-64.6605368598629,0.));
#63888=CARTESIAN_POINT('Ctrl Pts',(31.8840660489106,-64.6772162637907,0.));
#63889=CARTESIAN_POINT('Ctrl Pts',(31.9016590729373,-64.6939074154498,0.));
#63890=CARTESIAN_POINT('Ctrl Pts',(31.9192986047705,-64.7106101911732,0.));
#63891=CARTESIAN_POINT('Ctrl Pts',(31.9369846010615,-64.7273244678297,0.));
#63892=CARTESIAN_POINT('Ctrl Pts',(31.9547170185533,-64.7440501228203,0.));
#63893=CARTESIAN_POINT('Ctrl Pts',(31.9724958140789,-64.7607870340735,0.));
#63894=CARTESIAN_POINT('Ctrl Pts',(31.9903209445519,-64.7775350800401,0.));
#63895=CARTESIAN_POINT('Ctrl Pts',(32.0081923669676,-64.7942941396881,0.));
#63896=CARTESIAN_POINT('Ctrl Pts',(32.0261100384092,-64.8110640925021,0.));
#63897=CARTESIAN_POINT('Ctrl Pts',(32.0440739160477,-64.8278448184787,0.));
#63898=CARTESIAN_POINT('Ctrl Pts',(32.0620839571408,-64.8446361981234,0.));
#63899=CARTESIAN_POINT('Ctrl Pts',(32.0801401190241,-64.861438112445,0.));
#63900=CARTESIAN_POINT('Ctrl Pts',(32.0982423591108,-64.878250442952,0.));
#63901=CARTESIAN_POINT('Ctrl Pts',(32.1163906348979,-64.8950730716493,0.));
#63902=CARTESIAN_POINT('Ctrl Pts',(32.1345849039671,-64.9119058810362,0.));
#63903=CARTESIAN_POINT('Ctrl Pts',(32.1528251239831,-64.9287487541019,0.));
#63904=CARTESIAN_POINT('Ctrl Pts',(32.1711112526859,-64.9456015743203,0.));
#63905=CARTESIAN_POINT('Ctrl Pts',(32.1894432478888,-64.9624642256478,0.));
#63906=CARTESIAN_POINT('Ctrl Pts',(32.2078210674857,-64.9793365925194,0.));
#63907=CARTESIAN_POINT('Ctrl Pts',(32.2262446694516,-64.996218559847,0.));
#63908=CARTESIAN_POINT('Ctrl Pts',(32.244714011842,-65.0131100130155,0.));
#63909=CARTESIAN_POINT('Ctrl Pts',(32.2632290527854,-65.0300108378786,0.));
#63910=CARTESIAN_POINT('Ctrl Pts',(32.2817897504799,-65.0469209207548,0.));
#63911=CARTESIAN_POINT('Ctrl Pts',(32.3003960632,-65.0638401484245,0.));
#63912=CARTESIAN_POINT('Ctrl Pts',(32.3190479492985,-65.0807684081278,0.));
#63913=CARTESIAN_POINT('Ctrl Pts',(32.3377453672051,-65.097705587561,0.));
#63914=CARTESIAN_POINT('Ctrl Pts',(32.3564882754212,-65.1146515748723,0.));
#63915=CARTESIAN_POINT('Ctrl Pts',(32.3752766325134,-65.1316062586586,0.));
#63916=CARTESIAN_POINT('Ctrl Pts',(32.3941103971218,-65.1485695279628,0.));
#63917=CARTESIAN_POINT('Ctrl Pts',(32.4129895279612,-65.165541272272,0.));
#63918=CARTESIAN_POINT('Ctrl Pts',(32.4319139838212,-65.182521381514,0.));
#63919=CARTESIAN_POINT('Ctrl Pts',(32.4508837235613,-65.1995097460546,0.));
#63920=CARTESIAN_POINT('Ctrl Pts',(32.4698987061036,-65.2165062566936,0.));
#63921=CARTESIAN_POINT('Ctrl Pts',(32.4889588904396,-65.2335108046625,0.));
#63922=CARTESIAN_POINT('Ctrl Pts',(32.508064235633,-65.2505232816215,0.));
#63923=CARTESIAN_POINT('Ctrl Pts',(32.527214700819,-65.2675435796558,0.));
#63924=CARTESIAN_POINT('Ctrl Pts',(32.5464102452013,-65.2845715912717,0.));
#63925=CARTESIAN_POINT('Ctrl Pts',(32.565650828042,-65.3016072093908,0.));
#63926=CARTESIAN_POINT('Ctrl Pts',(32.5849364086678,-65.3186503273498,0.));
#63927=CARTESIAN_POINT('Ctrl Pts',(32.6042669464751,-65.3357008389005,0.));
#63928=CARTESIAN_POINT('Ctrl Pts',(32.6236424009301,-65.3527586382082,0.));
#63929=CARTESIAN_POINT('Ctrl Pts',(32.6430627315672,-65.3698236198512,0.));
#63930=CARTESIAN_POINT('Ctrl Pts',(32.6625278979807,-65.3868956788178,0.));
#63931=CARTESIAN_POINT('Ctrl Pts',(32.6820378598262,-65.4039747105033,0.));
#63932=CARTESIAN_POINT('Ctrl Pts',(32.701592576826,-65.421060610703,0.));
#63933=CARTESIAN_POINT('Ctrl Pts',(32.7211920087681,-65.4381532756063,0.));
#63934=CARTESIAN_POINT('Ctrl Pts',(32.7408361155037,-65.4552526017907,0.));
#63935=CARTESIAN_POINT('Ctrl Pts',(32.7605248569382,-65.4723584862129,0.));
#63936=CARTESIAN_POINT('Ctrl Pts',(32.7802581930293,-65.4894708262071,0.));
#63937=CARTESIAN_POINT('Ctrl Pts',(32.800036083798,-65.5065895194939,0.));
#63938=CARTESIAN_POINT('Ctrl Pts',(32.8198584893318,-65.5237144641864,0.));
#63939=CARTESIAN_POINT('Ctrl Pts',(32.8397253697864,-65.5408455587963,0.));
#63940=CARTESIAN_POINT('Ctrl Pts',(32.8596366853826,-65.5579827022413,0.));
#63941=CARTESIAN_POINT('Ctrl Pts',(32.8795923964021,-65.575125793846,0.));
#63942=CARTESIAN_POINT('Ctrl Pts',(32.899592463189,-65.5922747333182,0.));
#63943=CARTESIAN_POINT('Ctrl Pts',(32.9196368461457,-65.6094294207267,0.));
#63944=CARTESIAN_POINT('Ctrl Pts',(32.9397255057273,-65.6265897564782,0.));
#63945=CARTESIAN_POINT('Ctrl Pts',(32.9598584024317,-65.6437556412956,0.));
#63946=CARTESIAN_POINT('Ctrl Pts',(32.9800354967846,-65.6609269761902,0.));
#63947=CARTESIAN_POINT('Ctrl Pts',(33.000256749358,-65.6781036625041,0.));
#63948=CARTESIAN_POINT('Ctrl Pts',(33.0205221207877,-65.6952856019542,0.));
#63949=CARTESIAN_POINT('Ctrl Pts',(33.0408315717874,-65.7124726966805,0.));
#63950=CARTESIAN_POINT('Ctrl Pts',(33.0611850631579,-65.729664849282,0.));
#63951=CARTESIAN_POINT('Ctrl Pts',(33.0815825557976,-65.7468619628808,0.));
#63952=CARTESIAN_POINT('Ctrl Pts',(33.102024010688,-65.7640639410653,0.));
#63953=CARTESIAN_POINT('Ctrl Pts',(33.1225093888668,-65.7812706877691,0.));
#63954=CARTESIAN_POINT('Ctrl Pts',(33.1430386513975,-65.7984821071622,0.));
#63955=CARTESIAN_POINT('Ctrl Pts',(33.16361175934,-65.8156981035504,0.));
#63956=CARTESIAN_POINT('Ctrl Pts',(33.1842286737053,-65.8329185812379,0.));
#63957=CARTESIAN_POINT('Ctrl Pts',(33.2048893554495,-65.8501434445174,0.));
#63958=CARTESIAN_POINT('Ctrl Pts',(33.2255937655655,-65.8673725979591,0.));
#63959=CARTESIAN_POINT('Ctrl Pts',(33.2463418651497,-65.8846059466382,0.));
#63960=CARTESIAN_POINT('Ctrl Pts',(33.2671336154754,-65.901843396389,0.));
#63961=CARTESIAN_POINT('Ctrl Pts',(33.2879689780566,-65.9190848540422,0.));
#63962=CARTESIAN_POINT('Ctrl Pts',(33.308847914715,-65.9363302276822,0.));
#63963=CARTESIAN_POINT('Ctrl Pts',(33.3297703874249,-65.9535794260802,0.));
#63964=CARTESIAN_POINT('Ctrl Pts',(33.3507363581578,-65.9708323581386,0.));
#63965=CARTESIAN_POINT('Ctrl Pts',(33.3717457887094,-65.9880889322822,0.));
#63966=CARTESIAN_POINT('Ctrl Pts',(33.3927986405612,-66.0053490559826,0.));
#63967=CARTESIAN_POINT('Ctrl Pts',(33.4138948746407,-66.0226126349482,0.));
#63968=CARTESIAN_POINT('Ctrl Pts',(33.4350344515128,-66.0398795737827,0.));
#63969=CARTESIAN_POINT('Ctrl Pts',(33.4562173318052,-66.0571497774484,0.));
#63970=CARTESIAN_POINT('Ctrl Pts',(33.4774434765761,-66.0744231525445,0.));
#63971=CARTESIAN_POINT('Ctrl Pts',(33.4987128476617,-66.0916996085237,0.));
#63972=CARTESIAN_POINT('Ctrl Pts',(33.5200254081212,-66.1089790592673,0.));
#63973=CARTESIAN_POINT('Ctrl Pts',(33.5413811223397,-66.1262614234579,0.));
#63974=CARTESIAN_POINT('Ctrl Pts',(33.5597240685728,-66.1410781873124,0.));
#63975=CARTESIAN_POINT('Ctrl Pts',(33.5738105077705,-66.1524393973985,0.));
#63976=CARTESIAN_POINT('Ctrl Pts',(33.5836213513971,-66.1603438177304,0.));
#63977=CARTESIAN_POINT('Ctrl Pts',(33.5891439876225,-66.1647906582406,0.));
#63978=CARTESIAN_POINT('Ctrl Pts',(33.5903722664954,-66.1657795405667,0.));
#63979=CARTESIAN_POINT('',(30.354906545781,-63.0759831361898,12.));
#63980=CARTESIAN_POINT('',(30.354906545781,-63.0759831361898,0.));
#63981=CARTESIAN_POINT('Ctrl Pts',(33.5903722664955,-66.1657795405668,12.));
#63982=CARTESIAN_POINT('Ctrl Pts',(33.5891439876225,-66.1647906582407,12.));
#63983=CARTESIAN_POINT('Ctrl Pts',(33.5836213513971,-66.1603438177305,12.));
#63984=CARTESIAN_POINT('Ctrl Pts',(33.5738105077705,-66.1524393973985,12.));
#63985=CARTESIAN_POINT('Ctrl Pts',(33.5597240685728,-66.1410781873124,12.));
#63986=CARTESIAN_POINT('Ctrl Pts',(33.5413811223397,-66.1262614234579,12.));
#63987=CARTESIAN_POINT('Ctrl Pts',(33.5200254081212,-66.1089790592673,12.));
#63988=CARTESIAN_POINT('Ctrl Pts',(33.4987128476617,-66.0916996085237,12.));
#63989=CARTESIAN_POINT('Ctrl Pts',(33.4774434765761,-66.0744231525445,12.));
#63990=CARTESIAN_POINT('Ctrl Pts',(33.4562173318052,-66.0571497774484,12.));
#63991=CARTESIAN_POINT('Ctrl Pts',(33.4350344515128,-66.0398795737827,12.));
#63992=CARTESIAN_POINT('Ctrl Pts',(33.4138948746407,-66.0226126349482,12.));
#63993=CARTESIAN_POINT('Ctrl Pts',(33.3927986405612,-66.0053490559826,12.));
#63994=CARTESIAN_POINT('Ctrl Pts',(33.3717457887094,-65.9880889322822,12.));
#63995=CARTESIAN_POINT('Ctrl Pts',(33.3507363581578,-65.9708323581386,12.));
#63996=CARTESIAN_POINT('Ctrl Pts',(33.3297703874249,-65.9535794260802,12.));
#63997=CARTESIAN_POINT('Ctrl Pts',(33.308847914715,-65.9363302276822,12.));
#63998=CARTESIAN_POINT('Ctrl Pts',(33.2879689780566,-65.9190848540422,12.));
#63999=CARTESIAN_POINT('Ctrl Pts',(33.2671336154754,-65.901843396389,12.));
#64000=CARTESIAN_POINT('Ctrl Pts',(33.2463418651497,-65.8846059466382,12.));
#64001=CARTESIAN_POINT('Ctrl Pts',(33.2255937655655,-65.8673725979591,12.));
#64002=CARTESIAN_POINT('Ctrl Pts',(33.2048893554495,-65.8501434445174,12.));
#64003=CARTESIAN_POINT('Ctrl Pts',(33.1842286737053,-65.8329185812379,12.));
#64004=CARTESIAN_POINT('Ctrl Pts',(33.16361175934,-65.8156981035504,12.));
#64005=CARTESIAN_POINT('Ctrl Pts',(33.1430386513975,-65.7984821071622,12.));
#64006=CARTESIAN_POINT('Ctrl Pts',(33.1225093888668,-65.7812706877691,12.));
#64007=CARTESIAN_POINT('Ctrl Pts',(33.102024010688,-65.7640639410653,12.));
#64008=CARTESIAN_POINT('Ctrl Pts',(33.0815825557976,-65.7468619628808,12.));
#64009=CARTESIAN_POINT('Ctrl Pts',(33.0611850631579,-65.729664849282,12.));
#64010=CARTESIAN_POINT('Ctrl Pts',(33.0408315717874,-65.7124726966805,12.));
#64011=CARTESIAN_POINT('Ctrl Pts',(33.0205221207877,-65.6952856019542,12.));
#64012=CARTESIAN_POINT('Ctrl Pts',(33.000256749358,-65.6781036625041,12.));
#64013=CARTESIAN_POINT('Ctrl Pts',(32.9800354967846,-65.6609269761902,12.));
#64014=CARTESIAN_POINT('Ctrl Pts',(32.9598584024317,-65.6437556412956,12.));
#64015=CARTESIAN_POINT('Ctrl Pts',(32.9397255057273,-65.6265897564782,12.));
#64016=CARTESIAN_POINT('Ctrl Pts',(32.9196368461457,-65.6094294207267,12.));
#64017=CARTESIAN_POINT('Ctrl Pts',(32.899592463189,-65.5922747333182,12.));
#64018=CARTESIAN_POINT('Ctrl Pts',(32.8795923964021,-65.575125793846,12.));
#64019=CARTESIAN_POINT('Ctrl Pts',(32.8596366853826,-65.5579827022413,12.));
#64020=CARTESIAN_POINT('Ctrl Pts',(32.8397253697864,-65.5408455587963,12.));
#64021=CARTESIAN_POINT('Ctrl Pts',(32.8198584893318,-65.5237144641864,12.));
#64022=CARTESIAN_POINT('Ctrl Pts',(32.800036083798,-65.5065895194939,12.));
#64023=CARTESIAN_POINT('Ctrl Pts',(32.7802581930293,-65.4894708262071,12.));
#64024=CARTESIAN_POINT('Ctrl Pts',(32.7605248569382,-65.4723584862129,12.));
#64025=CARTESIAN_POINT('Ctrl Pts',(32.7408361155037,-65.4552526017907,12.));
#64026=CARTESIAN_POINT('Ctrl Pts',(32.7211920087681,-65.4381532756063,12.));
#64027=CARTESIAN_POINT('Ctrl Pts',(32.701592576826,-65.421060610703,12.));
#64028=CARTESIAN_POINT('Ctrl Pts',(32.6820378598262,-65.4039747105033,12.));
#64029=CARTESIAN_POINT('Ctrl Pts',(32.6625278979807,-65.3868956788178,12.));
#64030=CARTESIAN_POINT('Ctrl Pts',(32.6430627315672,-65.3698236198512,12.));
#64031=CARTESIAN_POINT('Ctrl Pts',(32.6236424009301,-65.3527586382082,12.));
#64032=CARTESIAN_POINT('Ctrl Pts',(32.6042669464751,-65.3357008389005,12.));
#64033=CARTESIAN_POINT('Ctrl Pts',(32.5849364086678,-65.3186503273498,12.));
#64034=CARTESIAN_POINT('Ctrl Pts',(32.565650828042,-65.3016072093908,12.));
#64035=CARTESIAN_POINT('Ctrl Pts',(32.5464102452013,-65.2845715912717,12.));
#64036=CARTESIAN_POINT('Ctrl Pts',(32.527214700819,-65.2675435796558,12.));
#64037=CARTESIAN_POINT('Ctrl Pts',(32.508064235633,-65.2505232816215,12.));
#64038=CARTESIAN_POINT('Ctrl Pts',(32.4889588904396,-65.2335108046625,12.));
#64039=CARTESIAN_POINT('Ctrl Pts',(32.4698987061036,-65.2165062566936,12.));
#64040=CARTESIAN_POINT('Ctrl Pts',(32.4508837235613,-65.1995097460546,12.));
#64041=CARTESIAN_POINT('Ctrl Pts',(32.4319139838212,-65.182521381514,12.));
#64042=CARTESIAN_POINT('Ctrl Pts',(32.4129895279612,-65.165541272272,12.));
#64043=CARTESIAN_POINT('Ctrl Pts',(32.3941103971218,-65.1485695279628,12.));
#64044=CARTESIAN_POINT('Ctrl Pts',(32.3752766325134,-65.1316062586586,12.));
#64045=CARTESIAN_POINT('Ctrl Pts',(32.3564882754212,-65.1146515748723,12.));
#64046=CARTESIAN_POINT('Ctrl Pts',(32.3377453672051,-65.097705587561,12.));
#64047=CARTESIAN_POINT('Ctrl Pts',(32.3190479492985,-65.0807684081278,12.));
#64048=CARTESIAN_POINT('Ctrl Pts',(32.3003960632,-65.0638401484245,12.));
#64049=CARTESIAN_POINT('Ctrl Pts',(32.2817897504799,-65.0469209207548,12.));
#64050=CARTESIAN_POINT('Ctrl Pts',(32.2632290527854,-65.0300108378786,12.));
#64051=CARTESIAN_POINT('Ctrl Pts',(32.244714011842,-65.0131100130155,12.));
#64052=CARTESIAN_POINT('Ctrl Pts',(32.2262446694516,-64.996218559847,12.));
#64053=CARTESIAN_POINT('Ctrl Pts',(32.2078210674857,-64.9793365925194,12.));
#64054=CARTESIAN_POINT('Ctrl Pts',(32.1894432478888,-64.9624642256478,12.));
#64055=CARTESIAN_POINT('Ctrl Pts',(32.1711112526859,-64.9456015743203,12.));
#64056=CARTESIAN_POINT('Ctrl Pts',(32.1528251239831,-64.9287487541019,12.));
#64057=CARTESIAN_POINT('Ctrl Pts',(32.1345849039671,-64.9119058810362,12.));
#64058=CARTESIAN_POINT('Ctrl Pts',(32.1163906348979,-64.8950730716493,12.));
#64059=CARTESIAN_POINT('Ctrl Pts',(32.0982423591108,-64.878250442952,12.));
#64060=CARTESIAN_POINT('Ctrl Pts',(32.0801401190241,-64.861438112445,12.));
#64061=CARTESIAN_POINT('Ctrl Pts',(32.0620839571408,-64.8446361981234,12.));
#64062=CARTESIAN_POINT('Ctrl Pts',(32.0440739160477,-64.8278448184787,12.));
#64063=CARTESIAN_POINT('Ctrl Pts',(32.0261100384092,-64.8110640925021,12.));
#64064=CARTESIAN_POINT('Ctrl Pts',(32.0081923669676,-64.7942941396881,12.));
#64065=CARTESIAN_POINT('Ctrl Pts',(31.9903209445519,-64.7775350800401,12.));
#64066=CARTESIAN_POINT('Ctrl Pts',(31.9724958140789,-64.7607870340735,12.));
#64067=CARTESIAN_POINT('Ctrl Pts',(31.9547170185533,-64.7440501228203,12.));
#64068=CARTESIAN_POINT('Ctrl Pts',(31.9369846010615,-64.7273244678297,12.));
#64069=CARTESIAN_POINT('Ctrl Pts',(31.9192986047705,-64.7106101911732,12.));
#64070=CARTESIAN_POINT('Ctrl Pts',(31.9016590729373,-64.6939074154498,12.));
#64071=CARTESIAN_POINT('Ctrl Pts',(31.8840660489106,-64.6772162637907,12.));
#64072=CARTESIAN_POINT('Ctrl Pts',(31.866519576131,-64.6605368598629,12.));
#64073=CARTESIAN_POINT('Ctrl Pts',(31.8490196981248,-64.6438693278714,12.));
#64074=CARTESIAN_POINT('Ctrl Pts',(31.8315664585025,-64.6272137925627,12.));
#64075=CARTESIAN_POINT('Ctrl Pts',(31.8141599009684,-64.6105703792312,12.));
#64076=CARTESIAN_POINT('Ctrl Pts',(31.7968000693218,-64.5939392137235,12.));
#64077=CARTESIAN_POINT('Ctrl Pts',(31.7794870074583,-64.5773204224429,12.));
#64078=CARTESIAN_POINT('Ctrl Pts',(31.7622207593634,-64.5607141323521,12.));
#64079=CARTESIAN_POINT('Ctrl Pts',(31.7450013691111,-64.544120470977,12.));
#64080=CARTESIAN_POINT('Ctrl Pts',(31.7278288808731,-64.5275395664124,12.));
#64081=CARTESIAN_POINT('Ctrl Pts',(31.71070333892,-64.510971547327,12.));
#64082=CARTESIAN_POINT('Ctrl Pts',(31.6936247876228,-64.4944165429675,12.));
#64083=CARTESIAN_POINT('Ctrl Pts',(31.6765932714464,-64.4778746831614,12.));
#64084=CARTESIAN_POINT('Ctrl Pts',(31.6596088349481,-64.4613460983214,12.));
#64085=CARTESIAN_POINT('Ctrl Pts',(31.6426715227878,-64.4448309194525,12.));
#64086=CARTESIAN_POINT('Ctrl Pts',(31.6257813797287,-64.4283292781565,12.));
#64087=CARTESIAN_POINT('Ctrl Pts',(31.6089384506395,-64.4118413066378,12.));
#64088=CARTESIAN_POINT('Ctrl Pts',(31.5921427804865,-64.3953671377046,12.));
#64089=CARTESIAN_POINT('Ctrl Pts',(31.5753944143336,-64.3789069047734,12.));
#64090=CARTESIAN_POINT('Ctrl Pts',(31.5586933973515,-64.3624607418769,12.));
#64091=CARTESIAN_POINT('Ctrl Pts',(31.5420397748191,-64.3460287836687,12.));
#64092=CARTESIAN_POINT('Ctrl Pts',(31.5254335921245,-64.3296111654283,12.));
#64093=CARTESIAN_POINT('Ctrl Pts',(31.5088748947582,-64.3132080230637,12.));
#64094=CARTESIAN_POINT('Ctrl Pts',(31.4923637283131,-64.2968194931158,12.));
#64095=CARTESIAN_POINT('Ctrl Pts',(31.4759001384941,-64.2804457127671,12.));
#64096=CARTESIAN_POINT('Ctrl Pts',(31.4594841711194,-64.2640868198473,12.));
#64097=CARTESIAN_POINT('Ctrl Pts',(31.4431158721221,-64.2477429528393,12.));
#64098=CARTESIAN_POINT('Ctrl Pts',(31.4267952875423,-64.231414250881,12.));
#64099=CARTESIAN_POINT('Ctrl Pts',(31.410522463528,-64.2151008537697,12.));
#64100=CARTESIAN_POINT('Ctrl Pts',(31.3942974463445,-64.1988029019707,12.));
#64101=CARTESIAN_POINT('Ctrl Pts',(31.3781202823754,-64.1825205366225,12.));
#64102=CARTESIAN_POINT('Ctrl Pts',(31.3619910181228,-64.166253899542,12.));
#64103=CARTESIAN_POINT('Ctrl Pts',(31.3459097002006,-64.1500031332282,12.));
#64104=CARTESIAN_POINT('Ctrl Pts',(31.3298763753376,-64.1337683808691,12.));
#64105=CARTESIAN_POINT('Ctrl Pts',(31.3138910903858,-64.1175497863491,12.));
#64106=CARTESIAN_POINT('Ctrl Pts',(31.2979538923214,-64.1013474942557,12.));
#64107=CARTESIAN_POINT('Ctrl Pts',(31.2820648282447,-64.0851616498853,12.));
#64108=CARTESIAN_POINT('Ctrl Pts',(31.2662239453728,-64.0689923992461,12.));
#64109=CARTESIAN_POINT('Ctrl Pts',(31.2504312910451,-64.0528398890657,12.));
#64110=CARTESIAN_POINT('Ctrl Pts',(31.2346869127297,-64.0367042667984,12.));
#64111=CARTESIAN_POINT('Ctrl Pts',(31.2189908580245,-64.02058568063,12.));
#64112=CARTESIAN_POINT('Ctrl Pts',(31.2033431746558,-64.0044842794832,12.));
#64113=CARTESIAN_POINT('Ctrl Pts',(31.1877439104716,-63.9884002130211,12.));
#64114=CARTESIAN_POINT('Ctrl Pts',(31.1721931134487,-63.9723336316551,12.));
#64115=CARTESIAN_POINT('Ctrl Pts',(31.1566908316991,-63.9562846865567,12.));
#64116=CARTESIAN_POINT('Ctrl Pts',(31.1412371134727,-63.9402535296651,12.));
#64117=CARTESIAN_POINT('Ctrl Pts',(31.1258320071545,-63.9242403136955,12.));
#64118=CARTESIAN_POINT('Ctrl Pts',(31.1104755612607,-63.9082451921448,12.));
#64119=CARTESIAN_POINT('Ctrl Pts',(31.0951678244455,-63.8922683192965,12.));
#64120=CARTESIAN_POINT('Ctrl Pts',(31.0799088455041,-63.8763098502237,12.));
#64121=CARTESIAN_POINT('Ctrl Pts',(31.0646986733723,-63.8603699407922,12.));
#64122=CARTESIAN_POINT('Ctrl Pts',(31.0495373571214,-63.8444487476611,12.));
#64123=CARTESIAN_POINT('Ctrl Pts',(31.0344249459538,-63.8285464282846,12.));
#64124=CARTESIAN_POINT('Ctrl Pts',(31.019361489217,-63.8126631409364,12.));
#64125=CARTESIAN_POINT('Ctrl Pts',(31.0043470364108,-63.796799044728,12.));
#64126=CARTESIAN_POINT('Ctrl Pts',(30.9893816371909,-63.7809542996264,12.));
#64127=CARTESIAN_POINT('Ctrl Pts',(30.9744653413688,-63.7651290664733,12.));
#64128=CARTESIAN_POINT('Ctrl Pts',(30.9595981989103,-63.7493235069871,12.));
#64129=CARTESIAN_POINT('Ctrl Pts',(30.9447802599354,-63.7335377837441,12.));
#64130=CARTESIAN_POINT('Ctrl Pts',(30.9300115747115,-63.717772060161,12.));
#64131=CARTESIAN_POINT('Ctrl Pts',(30.9152921936464,-63.7020265004792,12.));
#64132=CARTESIAN_POINT('Ctrl Pts',(30.900622167269,-63.6863012697328,12.));
#64133=CARTESIAN_POINT('Ctrl Pts',(30.8860015462475,-63.6705965337971,12.));
#64134=CARTESIAN_POINT('Ctrl Pts',(30.8714303814194,-63.6549124594666,12.));
#64135=CARTESIAN_POINT('Ctrl Pts',(30.8569087238131,-63.6392492145233,12.));
#64136=CARTESIAN_POINT('Ctrl Pts',(30.8424366246671,-63.6236069678055,12.));
#64137=CARTESIAN_POINT('Ctrl Pts',(30.8280141354458,-63.6079858892771,12.));
#64138=CARTESIAN_POINT('Ctrl Pts',(30.813641307801,-63.5923861498988,12.));
#64139=CARTESIAN_POINT('Ctrl Pts',(30.7993181935271,-63.5768079214882,12.));
#64140=CARTESIAN_POINT('Ctrl Pts',(30.7850448445204,-63.5612513766,12.));
#64141=CARTESIAN_POINT('Ctrl Pts',(30.7708213127158,-63.5457166883537,12.));
#64142=CARTESIAN_POINT('Ctrl Pts',(30.7566476500757,-63.5302040304142,12.));
#64143=CARTESIAN_POINT('Ctrl Pts',(30.7425239087281,-63.5147135773894,12.));
#64144=CARTESIAN_POINT('Ctrl Pts',(30.7284501410822,-63.4992455051795,12.));
#64145=CARTESIAN_POINT('Ctrl Pts',(30.7144263999265,-63.4837999912772,12.));
#64146=CARTESIAN_POINT('Ctrl Pts',(30.7004527385821,-63.468377215253,12.));
#64147=CARTESIAN_POINT('Ctrl Pts',(30.6865292107929,-63.4529773584249,12.));
#64148=CARTESIAN_POINT('Ctrl Pts',(30.6726558704315,-63.4376006029604,12.));
#64149=CARTESIAN_POINT('Ctrl Pts',(30.6588327712483,-63.422247131124,12.));
#64150=CARTESIAN_POINT('Ctrl Pts',(30.645059966612,-63.4069171245067,12.));
#64151=CARTESIAN_POINT('Ctrl Pts',(30.6313375092062,-63.3916107631376,12.));
#64152=CARTESIAN_POINT('Ctrl Pts',(30.6176654515967,-63.3763282271796,12.));
#64153=CARTESIAN_POINT('Ctrl Pts',(30.6040438469078,-63.3610696989577,12.));
#64154=CARTESIAN_POINT('Ctrl Pts',(30.5904727493711,-63.3458353646154,12.));
#64155=CARTESIAN_POINT('Ctrl Pts',(30.5769522151163,-63.3306254165126,12.));
#64156=CARTESIAN_POINT('Ctrl Pts',(30.5634823022379,-63.3154400534397,12.));
#64157=CARTESIAN_POINT('Ctrl Pts',(30.5500630691359,-63.3002794756086,12.));
#64158=CARTESIAN_POINT('Ctrl Pts',(30.5366945730508,-63.2851438802474,12.));
#64159=CARTESIAN_POINT('Ctrl Pts',(30.5233768687864,-63.2700334577639,12.));
#64160=CARTESIAN_POINT('Ctrl Pts',(30.5101100066659,-63.2549483856215,12.));
#64161=CARTESIAN_POINT('Ctrl Pts',(30.4968940344997,-63.2398888342546,12.));
#64162=CARTESIAN_POINT('Ctrl Pts',(30.4837290014989,-63.2248549788222,12.));
#64163=CARTESIAN_POINT('Ctrl Pts',(30.4706149614159,-63.2098470086636,12.));
#64164=CARTESIAN_POINT('Ctrl Pts',(30.4575519763336,-63.1948651386942,12.));
#64165=CARTESIAN_POINT('Ctrl Pts',(30.444540119238,-63.179909617189,12.));
#64166=CARTESIAN_POINT('Ctrl Pts',(30.431579465973,-63.164980701691,12.));
#64167=CARTESIAN_POINT('Ctrl Pts',(30.418670087563,-63.1500786361459,12.));
#64168=CARTESIAN_POINT('Ctrl Pts',(30.4058120432228,-63.1352036298441,12.));
#64169=CARTESIAN_POINT('Ctrl Pts',(30.3930053710484,-63.1203558300657,12.));
#64170=CARTESIAN_POINT('Ctrl Pts',(30.3802500880402,-63.105535320226,12.));
#64171=CARTESIAN_POINT('Ctrl Pts',(30.3700869762507,-63.0937007763471,12.));
#64172=CARTESIAN_POINT('Ctrl Pts',(30.362487768065,-63.0848371718048,12.));
#64173=CARTESIAN_POINT('Ctrl Pts',(30.3574319069329,-63.078933570069,12.));
#64174=CARTESIAN_POINT('Ctrl Pts',(30.354906545781,-63.0759831361898,12.));
#64175=CARTESIAN_POINT('Ctrl Pts',(34.933187552314,-65.4667541478395,-5.55111512312578E-16));
#64176=CARTESIAN_POINT('Ctrl Pts',(34.933187552314,-65.4667541478395,4.));
#64177=CARTESIAN_POINT('Ctrl Pts',(34.933187552314,-65.4667541478394,8.));
#64178=CARTESIAN_POINT('Ctrl Pts',(34.933187552314,-65.4667541478394,12.));
#64179=CARTESIAN_POINT('Ctrl Pts',(34.940541458921,-65.5763902570758,-5.55111512312578E-16));
#64180=CARTESIAN_POINT('Ctrl Pts',(34.940541458921,-65.5763902570758,4.));
#64181=CARTESIAN_POINT('Ctrl Pts',(34.940541458921,-65.5763902570757,8.00000000000001));
#64182=CARTESIAN_POINT('Ctrl Pts',(34.940541458921,-65.5763902570757,12.));
#64183=CARTESIAN_POINT('Ctrl Pts',(34.8876896346298,-65.7720412680595,-5.55111512312578E-16));
#64184=CARTESIAN_POINT('Ctrl Pts',(34.8876896346298,-65.7720412680595,4.));
#64185=CARTESIAN_POINT('Ctrl Pts',(34.8876896346298,-65.7720412680595,7.99999999999999));
#64186=CARTESIAN_POINT('Ctrl Pts',(34.8876896346298,-65.7720412680595,12.));
#64187=CARTESIAN_POINT('Ctrl Pts',(34.7399186668304,-65.9044372006549,-5.55111512312578E-16));
#64188=CARTESIAN_POINT('Ctrl Pts',(34.7399186668304,-65.9044372006549,4.));
#64189=CARTESIAN_POINT('Ctrl Pts',(34.7399186668304,-65.9044372006548,8.00000000000001));
#64190=CARTESIAN_POINT('Ctrl Pts',(34.7399186668304,-65.9044372006548,12.));
#64191=CARTESIAN_POINT('Ctrl Pts',(34.6669728017261,-65.9427857825589,-5.55111512312578E-16));
#64192=CARTESIAN_POINT('Ctrl Pts',(34.6669728017261,-65.9427857825589,4.));
#64193=CARTESIAN_POINT('Ctrl Pts',(34.6669728017261,-65.9427857825589,8.));
#64194=CARTESIAN_POINT('Ctrl Pts',(34.6669728017261,-65.9427857825589,12.));
#64195=CARTESIAN_POINT('',(34.933187552314,-65.4667541478395,2.77555756156289E-16));
#64196=CARTESIAN_POINT('',(34.6669728017259,-65.9427857825585,0.));
#64197=CARTESIAN_POINT('Ctrl Pts',(34.933187552314,-65.4667541478395,-1.38777878078145E-16));
#64198=CARTESIAN_POINT('Ctrl Pts',(34.940541458921,-65.5763902570758,-1.38777878078145E-16));
#64199=CARTESIAN_POINT('Ctrl Pts',(34.9103404164689,-65.6881908347808,-1.38777878078144E-16));
#64200=CARTESIAN_POINT('Ctrl Pts',(34.8491453679733,-65.779336693012,-1.38777878078145E-16));
#64201=CARTESIAN_POINT('Ctrl Pts',(34.8032490816015,-65.8476960866854,-1.38777878078145E-16));
#64202=CARTESIAN_POINT('Ctrl Pts',(34.7399186668304,-65.9044372006549,-1.38777878078145E-16));
#64203=CARTESIAN_POINT('Ctrl Pts',(34.6669728017261,-65.9427857825589,-1.38777878078145E-16));
#64204=CARTESIAN_POINT('',(34.6669728017259,-65.9427857825585,12.));
#64205=CARTESIAN_POINT('Ctrl Pts',(34.6669728017261,-65.9427857825589,-5.55111512312578E-16));
#64206=CARTESIAN_POINT('Ctrl Pts',(34.6669728017261,-65.9427857825589,4.));
#64207=CARTESIAN_POINT('Ctrl Pts',(34.6669728017261,-65.9427857825589,8.));
#64208=CARTESIAN_POINT('Ctrl Pts',(34.6669728017261,-65.9427857825589,12.));
#64209=CARTESIAN_POINT('',(34.933187552314,-65.4667541478394,12.));
#64210=CARTESIAN_POINT('Ctrl Pts',(34.6669728017261,-65.9427857825589,12.));
#64211=CARTESIAN_POINT('Ctrl Pts',(34.7399186668304,-65.9044372006548,12.));
#64212=CARTESIAN_POINT('Ctrl Pts',(34.8032490816015,-65.8476960866854,12.));
#64213=CARTESIAN_POINT('Ctrl Pts',(34.8491453679733,-65.779336693012,12.));
#64214=CARTESIAN_POINT('Ctrl Pts',(34.9103404164689,-65.6881908347807,12.));
#64215=CARTESIAN_POINT('Ctrl Pts',(34.940541458921,-65.5763902570757,12.));
#64216=CARTESIAN_POINT('Ctrl Pts',(34.933187552314,-65.4667541478394,12.));
#64217=CARTESIAN_POINT('Ctrl Pts',(34.933187552314,-65.4667541478394,12.));
#64218=CARTESIAN_POINT('Ctrl Pts',(34.933187552314,-65.4667541478394,8.));
#64219=CARTESIAN_POINT('Ctrl Pts',(34.933187552314,-65.4667541478395,4.));
#64220=CARTESIAN_POINT('Ctrl Pts',(34.933187552314,-65.4667541478395,-5.55111512312578E-16));
#64221=CARTESIAN_POINT('Origin',(1.73171632017258E-10,-3.32444647725449E-10,
0.));
#64222=CARTESIAN_POINT('Origin',(1.73171632017258E-10,-3.32444647725449E-10,
12.));
#64223=CARTESIAN_POINT('Origin',(1.73171632017258E-10,-3.32444647725449E-10,
0.));
#64224=CARTESIAN_POINT('Ctrl Pts',(28.2316040302268,-68.9436475237602,0.));
#64225=CARTESIAN_POINT('Ctrl Pts',(28.2316040302268,-68.9436475237602,4.));
#64226=CARTESIAN_POINT('Ctrl Pts',(28.2316040302268,-68.9436475237602,8.));
#64227=CARTESIAN_POINT('Ctrl Pts',(28.2316040302268,-68.9436475237602,12.));
#64228=CARTESIAN_POINT('Ctrl Pts',(28.1299168084376,-68.9852872321829,0.));
#64229=CARTESIAN_POINT('Ctrl Pts',(28.1299168084376,-68.9852872321829,4.));
#64230=CARTESIAN_POINT('Ctrl Pts',(28.1299168084376,-68.9852872321829,8.));
#64231=CARTESIAN_POINT('Ctrl Pts',(28.1299168084376,-68.9852872321829,12.));
#64232=CARTESIAN_POINT('Ctrl Pts',(27.9275918177428,-68.9970049015576,0.));
#64233=CARTESIAN_POINT('Ctrl Pts',(27.9275918177428,-68.9970049015576,4.));
#64234=CARTESIAN_POINT('Ctrl Pts',(27.9275918177428,-68.9970049015576,7.99999999999999));
#64235=CARTESIAN_POINT('Ctrl Pts',(27.9275918177428,-68.9970049015576,12.));
#64236=CARTESIAN_POINT('Ctrl Pts',(27.7552674476217,-68.8986722313987,0.));
#64237=CARTESIAN_POINT('Ctrl Pts',(27.7552674476217,-68.8986722313987,4.));
#64238=CARTESIAN_POINT('Ctrl Pts',(27.7552674476217,-68.8986722313987,8.00000000000001));
#64239=CARTESIAN_POINT('Ctrl Pts',(27.7552674476217,-68.8986722313987,12.));
#64240=CARTESIAN_POINT('Ctrl Pts',(27.6958230984752,-68.8415926174768,0.));
#64241=CARTESIAN_POINT('Ctrl Pts',(27.6958230984752,-68.8415926174768,4.));
#64242=CARTESIAN_POINT('Ctrl Pts',(27.6958230984752,-68.8415926174768,8.));
#64243=CARTESIAN_POINT('Ctrl Pts',(27.6958230984752,-68.8415926174768,12.));
#64244=CARTESIAN_POINT('',(28.2316040302268,-68.9436475237602,0.));
#64245=CARTESIAN_POINT('',(27.6958230984751,-68.8415926174769,0.));
#64246=CARTESIAN_POINT('Ctrl Pts',(28.2316040302268,-68.9436475237602,0.));
#64247=CARTESIAN_POINT('Ctrl Pts',(28.1299168084376,-68.9852872321829,0.));
#64248=CARTESIAN_POINT('Ctrl Pts',(28.0143025280406,-68.9919830432541,0.));
#64249=CARTESIAN_POINT('Ctrl Pts',(27.9084843686472,-68.9627440495797,0.));
#64250=CARTESIAN_POINT('Ctrl Pts',(27.8291207491021,-68.9408148043239,0.));
#64251=CARTESIAN_POINT('Ctrl Pts',(27.7552674476217,-68.8986722313987,0.));
#64252=CARTESIAN_POINT('Ctrl Pts',(27.6958230984752,-68.8415926174768,0.));
#64253=CARTESIAN_POINT('',(27.6958230984751,-68.8415926174769,12.));
#64254=CARTESIAN_POINT('Ctrl Pts',(27.6958230984752,-68.8415926174768,0.));
#64255=CARTESIAN_POINT('Ctrl Pts',(27.6958230984752,-68.8415926174768,4.));
#64256=CARTESIAN_POINT('Ctrl Pts',(27.6958230984752,-68.8415926174768,8.));
#64257=CARTESIAN_POINT('Ctrl Pts',(27.6958230984752,-68.8415926174768,12.));
#64258=CARTESIAN_POINT('',(28.2316040302268,-68.9436475237602,12.));
#64259=CARTESIAN_POINT('Ctrl Pts',(27.6958230984752,-68.8415926174768,12.));
#64260=CARTESIAN_POINT('Ctrl Pts',(27.7552674476217,-68.8986722313987,12.));
#64261=CARTESIAN_POINT('Ctrl Pts',(27.8291207491021,-68.9408148043239,12.));
#64262=CARTESIAN_POINT('Ctrl Pts',(27.9084843686472,-68.9627440495797,12.));
#64263=CARTESIAN_POINT('Ctrl Pts',(28.0143025280406,-68.9919830432541,12.));
#64264=CARTESIAN_POINT('Ctrl Pts',(28.1299168084376,-68.9852872321829,12.));
#64265=CARTESIAN_POINT('Ctrl Pts',(28.2316040302268,-68.9436475237602,12.));
#64266=CARTESIAN_POINT('Ctrl Pts',(28.2316040302268,-68.9436475237602,12.));
#64267=CARTESIAN_POINT('Ctrl Pts',(28.2316040302268,-68.9436475237602,8.));
#64268=CARTESIAN_POINT('Ctrl Pts',(28.2316040302268,-68.9436475237602,4.));
#64269=CARTESIAN_POINT('Ctrl Pts',(28.2316040302268,-68.9436475237602,0.));
#64270=CARTESIAN_POINT('Ctrl Pts',(24.7419628022041,-65.4815644032299,0.));
#64271=CARTESIAN_POINT('Ctrl Pts',(24.7419628022041,-65.4815644032299,12.));
#64272=CARTESIAN_POINT('Ctrl Pts',(24.7442214063382,-65.4847237095443,0.));
#64273=CARTESIAN_POINT('Ctrl Pts',(24.7442214063382,-65.4847237095443,12.));
#64274=CARTESIAN_POINT('Ctrl Pts',(24.7487434955981,-65.4910454936254,0.));
#64275=CARTESIAN_POINT('Ctrl Pts',(24.7487434955981,-65.4910454936254,12.));
#64276=CARTESIAN_POINT('Ctrl Pts',(24.7555412724651,-65.5005376841101,0.));
#64277=CARTESIAN_POINT('Ctrl Pts',(24.7555412724651,-65.5005376841101,12.));
#64278=CARTESIAN_POINT('Ctrl Pts',(24.7646342620841,-65.5132129675333,0.));
#64279=CARTESIAN_POINT('Ctrl Pts',(24.7646342620841,-65.5132129675333,12.));
#64280=CARTESIAN_POINT('Ctrl Pts',(24.7760493148465,-65.5290887770232,0.));
#64281=CARTESIAN_POINT('Ctrl Pts',(24.7760493148465,-65.5290887770232,12.));
#64282=CARTESIAN_POINT('Ctrl Pts',(24.787513182749,-65.5449962514662,0.));
#64283=CARTESIAN_POINT('Ctrl Pts',(24.787513182749,-65.5449962514662,12.));
#64284=CARTESIAN_POINT('Ctrl Pts',(24.7990258561259,-65.5609353062829,0.));
#64285=CARTESIAN_POINT('Ctrl Pts',(24.7990258561259,-65.5609353062829,12.));
#64286=CARTESIAN_POINT('Ctrl Pts',(24.8105873098626,-65.5769057914333,0.));
#64287=CARTESIAN_POINT('Ctrl Pts',(24.8105873098626,-65.5769057914333,12.));
#64288=CARTESIAN_POINT('Ctrl Pts',(24.8221975032103,-65.5929074932624,0.));
#64289=CARTESIAN_POINT('Ctrl Pts',(24.8221975032103,-65.5929074932624,12.));
#64290=CARTESIAN_POINT('Ctrl Pts',(24.8338563866763,-65.6089401625628,0.));
#64291=CARTESIAN_POINT('Ctrl Pts',(24.8338563866763,-65.6089401625628,12.));
#64292=CARTESIAN_POINT('Ctrl Pts',(24.8455639071516,-65.6250035361612,0.));
#64293=CARTESIAN_POINT('Ctrl Pts',(24.8455639071516,-65.6250035361612,12.));
#64294=CARTESIAN_POINT('Ctrl Pts',(24.8573200135665,-65.6410973603661,0.));
#64295=CARTESIAN_POINT('Ctrl Pts',(24.8573200135665,-65.6410973603661,12.));
#64296=CARTESIAN_POINT('Ctrl Pts',(24.8691246628056,-65.6572214156692,0.));
#64297=CARTESIAN_POINT('Ctrl Pts',(24.8691246628056,-65.6572214156692,12.));
#64298=CARTESIAN_POINT('Ctrl Pts',(24.8809778178228,-65.6733755087669,0.));
#64299=CARTESIAN_POINT('Ctrl Pts',(24.8809778178228,-65.6733755087669,12.));
#64300=CARTESIAN_POINT('Ctrl Pts',(24.8928794448607,-65.6895594608776,0.));
#64301=CARTESIAN_POINT('Ctrl Pts',(24.8928794448607,-65.6895594608776,12.));
#64302=CARTESIAN_POINT('Ctrl Pts',(24.9048295111448,-65.7057730980483,0.));
#64303=CARTESIAN_POINT('Ctrl Pts',(24.9048295111448,-65.7057730980483,12.));
#64304=CARTESIAN_POINT('Ctrl Pts',(24.9168279820106,-65.7220162391054,0.));
#64305=CARTESIAN_POINT('Ctrl Pts',(24.9168279820106,-65.7220162391054,12.));
#64306=CARTESIAN_POINT('Ctrl Pts',(24.928874819458,-65.7382886895888,0.));
#64307=CARTESIAN_POINT('Ctrl Pts',(24.928874819458,-65.7382886895888,12.));
#64308=CARTESIAN_POINT('Ctrl Pts',(24.9409699836537,-65.7545902480323,0.));
#64309=CARTESIAN_POINT('Ctrl Pts',(24.9409699836537,-65.7545902480323,12.));
#64310=CARTESIAN_POINT('Ctrl Pts',(24.9531134338696,-65.7709207098959,0.));
#64311=CARTESIAN_POINT('Ctrl Pts',(24.9531134338696,-65.7709207098959,12.));
#64312=CARTESIAN_POINT('Ctrl Pts',(24.965305129558,-65.7872798720823,0.));
#64313=CARTESIAN_POINT('Ctrl Pts',(24.965305129558,-65.7872798720823,12.));
#64314=CARTESIAN_POINT('Ctrl Pts',(24.9775450315682,-65.8036675380718,0.));
#64315=CARTESIAN_POINT('Ctrl Pts',(24.9775450315682,-65.8036675380718,12.));
#64316=CARTESIAN_POINT('Ctrl Pts',(24.9898331020983,-65.8200835177024,0.));
#64317=CARTESIAN_POINT('Ctrl Pts',(24.9898331020983,-65.8200835177024,12.));
#64318=CARTESIAN_POINT('Ctrl Pts',(25.0021693041169,-65.8365276247128,0.));
#64319=CARTESIAN_POINT('Ctrl Pts',(25.0021693041169,-65.8365276247128,12.));
#64320=CARTESIAN_POINT('Ctrl Pts',(25.0145536009604,-65.8529996750445,0.));
#64321=CARTESIAN_POINT('Ctrl Pts',(25.0145536009604,-65.8529996750445,12.));
#64322=CARTESIAN_POINT('Ctrl Pts',(25.0269859558362,-65.8694994847617,0.));
#64323=CARTESIAN_POINT('Ctrl Pts',(25.0269859558362,-65.8694994847617,12.));
#64324=CARTESIAN_POINT('Ctrl Pts',(25.0394663314055,-65.8860268683128,0.));
#64325=CARTESIAN_POINT('Ctrl Pts',(25.0394663314055,-65.8860268683128,12.));
#64326=CARTESIAN_POINT('Ctrl Pts',(25.0519946900078,-65.9025816394424,0.));
#64327=CARTESIAN_POINT('Ctrl Pts',(25.0519946900078,-65.9025816394424,12.));
#64328=CARTESIAN_POINT('Ctrl Pts',(25.0645709938524,-65.919163611981,0.));
#64329=CARTESIAN_POINT('Ctrl Pts',(25.0645709938524,-65.919163611981,12.));
#64330=CARTESIAN_POINT('Ctrl Pts',(25.0771952052028,-65.9357726006163,0.));
#64331=CARTESIAN_POINT('Ctrl Pts',(25.0771952052028,-65.9357726006163,12.));
#64332=CARTESIAN_POINT('Ctrl Pts',(25.0898672865915,-65.952408421814,0.));
#64333=CARTESIAN_POINT('Ctrl Pts',(25.0898672865915,-65.952408421814,12.));
#64334=CARTESIAN_POINT('Ctrl Pts',(25.1025872009003,-65.9690708941558,0.));
#64335=CARTESIAN_POINT('Ctrl Pts',(25.1025872009003,-65.9690708941558,12.));
#64336=CARTESIAN_POINT('Ctrl Pts',(25.1153549112503,-65.9857598378433,0.));
#64337=CARTESIAN_POINT('Ctrl Pts',(25.1153549112503,-65.9857598378433,12.));
#64338=CARTESIAN_POINT('Ctrl Pts',(25.1281703809297,-66.0024750743897,0.));
#64339=CARTESIAN_POINT('Ctrl Pts',(25.1281703809297,-66.0024750743897,12.));
#64340=CARTESIAN_POINT('Ctrl Pts',(25.1410335733098,-66.0192164262621,0.));
#64341=CARTESIAN_POINT('Ctrl Pts',(25.1410335733098,-66.0192164262621,12.));
#64342=CARTESIAN_POINT('Ctrl Pts',(25.1539444517418,-66.0359837164734,0.));
#64343=CARTESIAN_POINT('Ctrl Pts',(25.1539444517418,-66.0359837164734,12.));
#64344=CARTESIAN_POINT('Ctrl Pts',(25.166902979566,-66.0527767686025,0.));
#64345=CARTESIAN_POINT('Ctrl Pts',(25.166902979566,-66.0527767686025,12.));
#64346=CARTESIAN_POINT('Ctrl Pts',(25.1799091201599,-66.0695954069713,0.));
#64347=CARTESIAN_POINT('Ctrl Pts',(25.1799091201599,-66.0695954069713,12.));
#64348=CARTESIAN_POINT('Ctrl Pts',(25.1929628369684,-66.086439456768,0.));
#64349=CARTESIAN_POINT('Ctrl Pts',(25.1929628369684,-66.086439456768,12.));
#64350=CARTESIAN_POINT('Ctrl Pts',(25.2060640935365,-66.10330874419,0.));
#64351=CARTESIAN_POINT('Ctrl Pts',(25.2060640935365,-66.10330874419,12.));
#64352=CARTESIAN_POINT('Ctrl Pts',(25.2192128535357,-66.1202030965759,0.));
#64353=CARTESIAN_POINT('Ctrl Pts',(25.2192128535357,-66.1202030965759,12.));
#64354=CARTESIAN_POINT('Ctrl Pts',(25.2324090807549,-66.1371223423345,0.));
#64355=CARTESIAN_POINT('Ctrl Pts',(25.2324090807549,-66.1371223423345,12.));
#64356=CARTESIAN_POINT('Ctrl Pts',(25.2456527390874,-66.1540663108754,0.));
#64357=CARTESIAN_POINT('Ctrl Pts',(25.2456527390874,-66.1540663108754,12.));
#64358=CARTESIAN_POINT('Ctrl Pts',(25.2589437925146,-66.1710348325384,0.));
#64359=CARTESIAN_POINT('Ctrl Pts',(25.2589437925146,-66.1710348325384,12.));
#64360=CARTESIAN_POINT('Ctrl Pts',(25.2722822050836,-66.1880277385136,0.));
#64361=CARTESIAN_POINT('Ctrl Pts',(25.2722822050836,-66.1880277385136,12.));
#64362=CARTESIAN_POINT('Ctrl Pts',(25.285667940893,-66.2050448607911,0.));
#64363=CARTESIAN_POINT('Ctrl Pts',(25.285667940893,-66.2050448607911,12.));
#64364=CARTESIAN_POINT('Ctrl Pts',(25.2991009641094,-66.2220860321952,0.));
#64365=CARTESIAN_POINT('Ctrl Pts',(25.2991009641094,-66.2220860321952,12.));
#64366=CARTESIAN_POINT('Ctrl Pts',(25.3125812389729,-66.2391510863998,0.));
#64367=CARTESIAN_POINT('Ctrl Pts',(25.3125812389729,-66.2391510863998,12.));
#64368=CARTESIAN_POINT('Ctrl Pts',(25.3261087298026,-66.2562398579471,0.));
#64369=CARTESIAN_POINT('Ctrl Pts',(25.3261087298026,-66.2562398579471,12.));
#64370=CARTESIAN_POINT('Ctrl Pts',(25.3396834009949,-66.2733521822662,0.));
#64371=CARTESIAN_POINT('Ctrl Pts',(25.3396834009949,-66.2733521822662,12.));
#64372=CARTESIAN_POINT('Ctrl Pts',(25.3533052170248,-66.290487895671,0.));
#64373=CARTESIAN_POINT('Ctrl Pts',(25.3533052170248,-66.290487895671,12.));
#64374=CARTESIAN_POINT('Ctrl Pts',(25.3669741424488,-66.3076468353413,0.));
#64375=CARTESIAN_POINT('Ctrl Pts',(25.3669741424488,-66.3076468353413,12.));
#64376=CARTESIAN_POINT('Ctrl Pts',(25.3806901419012,-66.3248288393046,0.));
#64377=CARTESIAN_POINT('Ctrl Pts',(25.3806901419012,-66.3248288393046,12.));
#64378=CARTESIAN_POINT('Ctrl Pts',(25.3944531800901,-66.3420337464178,0.));
#64379=CARTESIAN_POINT('Ctrl Pts',(25.3944531800901,-66.3420337464178,12.));
#64380=CARTESIAN_POINT('Ctrl Pts',(25.4082632217847,-66.359261396341,0.));
#64381=CARTESIAN_POINT('Ctrl Pts',(25.4082632217847,-66.359261396341,12.));
#64382=CARTESIAN_POINT('Ctrl Pts',(25.4221202318199,-66.3765116295365,0.));
#64383=CARTESIAN_POINT('Ctrl Pts',(25.4221202318199,-66.3765116295365,12.));
#64384=CARTESIAN_POINT('Ctrl Pts',(25.4360241751017,-66.3937842872685,0.));
#64385=CARTESIAN_POINT('Ctrl Pts',(25.4360241751017,-66.3937842872685,12.));
#64386=CARTESIAN_POINT('Ctrl Pts',(25.4499750166078,-66.4110792116,0.));
#64387=CARTESIAN_POINT('Ctrl Pts',(25.4499750166078,-66.4110792116,12.));
#64388=CARTESIAN_POINT('Ctrl Pts',(25.4639727213849,-66.4283962453899,0.));
#64389=CARTESIAN_POINT('Ctrl Pts',(25.4639727213849,-66.4283962453899,12.));
#64390=CARTESIAN_POINT('Ctrl Pts',(25.4780172545417,-66.4457352322871,0.));
#64391=CARTESIAN_POINT('Ctrl Pts',(25.4780172545417,-66.4457352322871,12.));
#64392=CARTESIAN_POINT('Ctrl Pts',(25.4921085812547,-66.4630960167252,0.));
#64393=CARTESIAN_POINT('Ctrl Pts',(25.4921085812547,-66.4630960167252,12.));
#64394=CARTESIAN_POINT('Ctrl Pts',(25.5062466667702,-66.4804784439148,0.));
#64395=CARTESIAN_POINT('Ctrl Pts',(25.5062466667702,-66.4804784439148,12.));
#64396=CARTESIAN_POINT('Ctrl Pts',(25.5204314764033,-66.4978823598354,0.));
#64397=CARTESIAN_POINT('Ctrl Pts',(25.5204314764033,-66.4978823598354,12.));
#64398=CARTESIAN_POINT('Ctrl Pts',(25.534662975532,-66.5153076112231,0.));
#64399=CARTESIAN_POINT('Ctrl Pts',(25.534662975532,-66.5153076112231,12.));
#64400=CARTESIAN_POINT('Ctrl Pts',(25.5489411295911,-66.5327540455624,0.));
#64401=CARTESIAN_POINT('Ctrl Pts',(25.5489411295911,-66.5327540455624,12.));
#64402=CARTESIAN_POINT('Ctrl Pts',(25.5632659040792,-66.5502215110829,0.));
#64403=CARTESIAN_POINT('Ctrl Pts',(25.5632659040792,-66.5502215110829,12.));
#64404=CARTESIAN_POINT('Ctrl Pts',(25.5776372645601,-66.5677098567542,0.));
#64405=CARTESIAN_POINT('Ctrl Pts',(25.5776372645601,-66.5677098567542,12.));
#64406=CARTESIAN_POINT('Ctrl Pts',(25.5920551766629,-66.5852189322813,0.));
#64407=CARTESIAN_POINT('Ctrl Pts',(25.5920551766629,-66.5852189322813,12.));
#64408=CARTESIAN_POINT('Ctrl Pts',(25.6065196060755,-66.6027485880963,0.));
#64409=CARTESIAN_POINT('Ctrl Pts',(25.6065196060755,-66.6027485880963,12.));
#64410=CARTESIAN_POINT('Ctrl Pts',(25.6210305185403,-66.6202986753507,0.));
#64411=CARTESIAN_POINT('Ctrl Pts',(25.6210305185403,-66.6202986753507,12.));
#64412=CARTESIAN_POINT('Ctrl Pts',(25.6355878798613,-66.6378690459129,0.));
#64413=CARTESIAN_POINT('Ctrl Pts',(25.6355878798613,-66.6378690459129,12.));
#64414=CARTESIAN_POINT('Ctrl Pts',(25.6501916559055,-66.6554595523624,0.));
#64415=CARTESIAN_POINT('Ctrl Pts',(25.6501916559055,-66.6554595523624,12.));
#64416=CARTESIAN_POINT('Ctrl Pts',(25.6648418126013,-66.6730700479837,0.));
#64417=CARTESIAN_POINT('Ctrl Pts',(25.6648418126013,-66.6730700479837,12.));
#64418=CARTESIAN_POINT('Ctrl Pts',(25.6795383159319,-66.6907003867572,0.));
#64419=CARTESIAN_POINT('Ctrl Pts',(25.6795383159319,-66.6907003867572,12.));
#64420=CARTESIAN_POINT('Ctrl Pts',(25.6942811319322,-66.7083504233529,0.));
#64421=CARTESIAN_POINT('Ctrl Pts',(25.6942811319322,-66.7083504233529,12.));
#64422=CARTESIAN_POINT('Ctrl Pts',(25.7090702266962,-66.7260200131266,0.));
#64423=CARTESIAN_POINT('Ctrl Pts',(25.7090702266962,-66.7260200131266,12.));
#64424=CARTESIAN_POINT('Ctrl Pts',(25.7239055663772,-66.7437090121153,0.));
#64425=CARTESIAN_POINT('Ctrl Pts',(25.7239055663772,-66.7437090121153,12.));
#64426=CARTESIAN_POINT('Ctrl Pts',(25.7387871171866,-66.7614172770316,0.));
#64427=CARTESIAN_POINT('Ctrl Pts',(25.7387871171866,-66.7614172770316,12.));
#64428=CARTESIAN_POINT('Ctrl Pts',(25.7537148453863,-66.7791446652545,0.));
#64429=CARTESIAN_POINT('Ctrl Pts',(25.7537148453863,-66.7791446652545,12.));
#64430=CARTESIAN_POINT('Ctrl Pts',(25.7686887172877,-66.7968910348245,0.));
#64431=CARTESIAN_POINT('Ctrl Pts',(25.7686887172877,-66.7968910348245,12.));
#64432=CARTESIAN_POINT('Ctrl Pts',(25.7837086992594,-66.8146562444433,0.));
#64433=CARTESIAN_POINT('Ctrl Pts',(25.7837086992594,-66.8146562444433,12.));
#64434=CARTESIAN_POINT('Ctrl Pts',(25.7987747577269,-66.8324401534668,0.));
#64435=CARTESIAN_POINT('Ctrl Pts',(25.7987747577269,-66.8324401534668,12.));
#64436=CARTESIAN_POINT('Ctrl Pts',(25.8138868591709,-66.8502426219001,0.));
#64437=CARTESIAN_POINT('Ctrl Pts',(25.8138868591709,-66.8502426219001,12.));
#64438=CARTESIAN_POINT('Ctrl Pts',(25.8290449701192,-66.8680635103876,0.));
#64439=CARTESIAN_POINT('Ctrl Pts',(25.8290449701192,-66.8680635103876,12.));
#64440=CARTESIAN_POINT('Ctrl Pts',(25.844249057147,-66.8859026802088,0.));
#64441=CARTESIAN_POINT('Ctrl Pts',(25.844249057147,-66.8859026802088,12.));
#64442=CARTESIAN_POINT('Ctrl Pts',(25.8594990868833,-66.9037599932761,0.));
#64443=CARTESIAN_POINT('Ctrl Pts',(25.8594990868833,-66.9037599932761,12.));
#64444=CARTESIAN_POINT('Ctrl Pts',(25.874795026011,-66.92163531213,0.));
#64445=CARTESIAN_POINT('Ctrl Pts',(25.874795026011,-66.92163531213,12.));
#64446=CARTESIAN_POINT('Ctrl Pts',(25.890136841266,-66.939528499934,0.));
#64447=CARTESIAN_POINT('Ctrl Pts',(25.890136841266,-66.939528499934,12.));
#64448=CARTESIAN_POINT('Ctrl Pts',(25.9055244994277,-66.9574394204663,0.));
#64449=CARTESIAN_POINT('Ctrl Pts',(25.9055244994277,-66.9574394204663,12.));
#64450=CARTESIAN_POINT('Ctrl Pts',(25.9209579673209,-66.975367938115,0.));
#64451=CARTESIAN_POINT('Ctrl Pts',(25.9209579673209,-66.975367938115,12.));
#64452=CARTESIAN_POINT('Ctrl Pts',(25.9364372118222,-66.9933139178778,0.));
#64453=CARTESIAN_POINT('Ctrl Pts',(25.9364372118222,-66.9933139178778,12.));
#64454=CARTESIAN_POINT('Ctrl Pts',(25.9519621998598,-67.0112772253556,0.));
#64455=CARTESIAN_POINT('Ctrl Pts',(25.9519621998598,-67.0112772253556,12.));
#64456=CARTESIAN_POINT('Ctrl Pts',(25.967532898412,-67.0292577267489,0.));
#64457=CARTESIAN_POINT('Ctrl Pts',(25.967532898412,-67.0292577267489,12.));
#64458=CARTESIAN_POINT('Ctrl Pts',(25.9831492744983,-67.0472552888485,0.));
#64459=CARTESIAN_POINT('Ctrl Pts',(25.9831492744983,-67.0472552888485,12.));
#64460=CARTESIAN_POINT('Ctrl Pts',(25.9988112951814,-67.0652697790325,0.));
#64461=CARTESIAN_POINT('Ctrl Pts',(25.9988112951814,-67.0652697790325,12.));
#64462=CARTESIAN_POINT('Ctrl Pts',(26.014518927573,-67.0833010652634,0.));
#64463=CARTESIAN_POINT('Ctrl Pts',(26.014518927573,-67.0833010652634,12.));
#64464=CARTESIAN_POINT('Ctrl Pts',(26.0302721388339,-67.101349016084,0.));
#64465=CARTESIAN_POINT('Ctrl Pts',(26.0302721388339,-67.101349016084,12.));
#64466=CARTESIAN_POINT('Ctrl Pts',(26.0460708961725,-67.1194135006124,0.));
#64467=CARTESIAN_POINT('Ctrl Pts',(26.0460708961725,-67.1194135006124,12.));
#64468=CARTESIAN_POINT('Ctrl Pts',(26.061915166836,-67.1374943885354,0.));
#64469=CARTESIAN_POINT('Ctrl Pts',(26.061915166836,-67.1374943885354,12.));
#64470=CARTESIAN_POINT('Ctrl Pts',(26.0778049181128,-67.1555915501049,0.));
#64471=CARTESIAN_POINT('Ctrl Pts',(26.0778049181128,-67.1555915501049,12.));
#64472=CARTESIAN_POINT('Ctrl Pts',(26.0937401173383,-67.173704856136,0.));
#64473=CARTESIAN_POINT('Ctrl Pts',(26.0937401173383,-67.173704856136,12.));
#64474=CARTESIAN_POINT('Ctrl Pts',(26.1097207318949,-67.1918341780018,0.));
#64475=CARTESIAN_POINT('Ctrl Pts',(26.1097207318949,-67.1918341780018,12.));
#64476=CARTESIAN_POINT('Ctrl Pts',(26.1257467292102,-67.2099793876297,0.));
#64477=CARTESIAN_POINT('Ctrl Pts',(26.1257467292102,-67.2099793876297,12.));
#64478=CARTESIAN_POINT('Ctrl Pts',(26.1418180767489,-67.2281403574938,0.));
#64479=CARTESIAN_POINT('Ctrl Pts',(26.1418180767489,-67.2281403574938,12.));
#64480=CARTESIAN_POINT('Ctrl Pts',(26.1579347420138,-67.2463169606115,0.));
#64481=CARTESIAN_POINT('Ctrl Pts',(26.1579347420138,-67.2463169606115,12.));
#64482=CARTESIAN_POINT('Ctrl Pts',(26.1740966925528,-67.2645090705421,0.));
#64483=CARTESIAN_POINT('Ctrl Pts',(26.1740966925528,-67.2645090705421,12.));
#64484=CARTESIAN_POINT('Ctrl Pts',(26.1903038959589,-67.282716561383,0.));
#64485=CARTESIAN_POINT('Ctrl Pts',(26.1903038959589,-67.282716561383,12.));
#64486=CARTESIAN_POINT('Ctrl Pts',(26.2065563198683,-67.3009393077652,0.));
#64487=CARTESIAN_POINT('Ctrl Pts',(26.2065563198683,-67.3009393077652,12.));
#64488=CARTESIAN_POINT('Ctrl Pts',(26.2228539319526,-67.3191771848464,0.));
#64489=CARTESIAN_POINT('Ctrl Pts',(26.2228539319526,-67.3191771848464,12.));
#64490=CARTESIAN_POINT('Ctrl Pts',(26.2391966999191,-67.3374300683074,0.));
#64491=CARTESIAN_POINT('Ctrl Pts',(26.2391966999191,-67.3374300683074,12.));
#64492=CARTESIAN_POINT('Ctrl Pts',(26.255584591518,-67.3556978343507,0.));
#64493=CARTESIAN_POINT('Ctrl Pts',(26.255584591518,-67.3556978343507,12.));
#64494=CARTESIAN_POINT('Ctrl Pts',(26.2720175745423,-67.3739803596969,0.));
#64495=CARTESIAN_POINT('Ctrl Pts',(26.2720175745423,-67.3739803596969,12.));
#64496=CARTESIAN_POINT('Ctrl Pts',(26.2884956168269,-67.392277521581,0.));
#64497=CARTESIAN_POINT('Ctrl Pts',(26.2884956168269,-67.392277521581,12.));
#64498=CARTESIAN_POINT('Ctrl Pts',(26.3050186862407,-67.4105891977461,0.));
#64499=CARTESIAN_POINT('Ctrl Pts',(26.3050186862407,-67.4105891977461,12.));
#64500=CARTESIAN_POINT('Ctrl Pts',(26.321586750686,-67.4289152664398,0.));
#64501=CARTESIAN_POINT('Ctrl Pts',(26.321586750686,-67.4289152664398,12.));
#64502=CARTESIAN_POINT('Ctrl Pts',(26.3381997781055,-67.4472556064119,0.));
#64503=CARTESIAN_POINT('Ctrl Pts',(26.3381997781055,-67.4472556064119,12.));
#64504=CARTESIAN_POINT('Ctrl Pts',(26.3548577364833,-67.4656100969116,0.));
#64505=CARTESIAN_POINT('Ctrl Pts',(26.3548577364833,-67.4656100969116,12.));
#64506=CARTESIAN_POINT('Ctrl Pts',(26.3715605938432,-67.4839786176836,0.));
#64507=CARTESIAN_POINT('Ctrl Pts',(26.3715605938432,-67.4839786176836,12.));
#64508=CARTESIAN_POINT('Ctrl Pts',(26.3883083182421,-67.5023610489622,0.));
#64509=CARTESIAN_POINT('Ctrl Pts',(26.3883083182421,-67.5023610489622,12.));
#64510=CARTESIAN_POINT('Ctrl Pts',(26.4051008777675,-67.5207572714683,0.));
#64511=CARTESIAN_POINT('Ctrl Pts',(26.4051008777675,-67.5207572714683,12.));
#64512=CARTESIAN_POINT('Ctrl Pts',(26.4219382405458,-67.5391671664072,0.));
#64513=CARTESIAN_POINT('Ctrl Pts',(26.4219382405458,-67.5391671664072,12.));
#64514=CARTESIAN_POINT('Ctrl Pts',(26.4388203747425,-67.5575906154657,0.));
#64515=CARTESIAN_POINT('Ctrl Pts',(26.4388203747425,-67.5575906154657,12.));
#64516=CARTESIAN_POINT('Ctrl Pts',(26.455747248562,-67.5760275008093,0.));
#64517=CARTESIAN_POINT('Ctrl Pts',(26.455747248562,-67.5760275008093,12.));
#64518=CARTESIAN_POINT('Ctrl Pts',(26.4727188302409,-67.5944777050768,0.));
#64519=CARTESIAN_POINT('Ctrl Pts',(26.4727188302409,-67.5944777050768,12.));
#64520=CARTESIAN_POINT('Ctrl Pts',(26.4897350880439,-67.6129411113758,0.));
#64521=CARTESIAN_POINT('Ctrl Pts',(26.4897350880439,-67.6129411113758,12.));
#64522=CARTESIAN_POINT('Ctrl Pts',(26.5067959902725,-67.6314176032811,0.));
#64523=CARTESIAN_POINT('Ctrl Pts',(26.5067959902725,-67.6314176032811,12.));
#64524=CARTESIAN_POINT('Ctrl Pts',(26.5239015052653,-67.649907064832,0.));
#64525=CARTESIAN_POINT('Ctrl Pts',(26.5239015052653,-67.649907064832,12.));
#64526=CARTESIAN_POINT('Ctrl Pts',(26.5410516013984,-67.6684093805291,0.));
#64527=CARTESIAN_POINT('Ctrl Pts',(26.5410516013984,-67.6684093805291,12.));
#64528=CARTESIAN_POINT('Ctrl Pts',(26.5582462470794,-67.6869244353294,0.));
#64529=CARTESIAN_POINT('Ctrl Pts',(26.5582462470794,-67.6869244353294,12.));
#64530=CARTESIAN_POINT('Ctrl Pts',(26.5754854107421,-67.7054521146425,0.));
#64531=CARTESIAN_POINT('Ctrl Pts',(26.5754854107421,-67.7054521146425,12.));
#64532=CARTESIAN_POINT('Ctrl Pts',(26.5927690608543,-67.7239923043288,0.));
#64533=CARTESIAN_POINT('Ctrl Pts',(26.5927690608543,-67.7239923043288,12.));
#64534=CARTESIAN_POINT('Ctrl Pts',(26.6100971659201,-67.7425448906977,0.));
#64535=CARTESIAN_POINT('Ctrl Pts',(26.6100971659201,-67.7425448906977,12.));
#64536=CARTESIAN_POINT('Ctrl Pts',(26.6274696944792,-67.7611097605042,0.));
#64537=CARTESIAN_POINT('Ctrl Pts',(26.6274696944792,-67.7611097605042,12.));
#64538=CARTESIAN_POINT('Ctrl Pts',(26.6448866151029,-67.7796868009455,0.));
#64539=CARTESIAN_POINT('Ctrl Pts',(26.6448866151029,-67.7796868009455,12.));
#64540=CARTESIAN_POINT('Ctrl Pts',(26.662347896387,-67.798275899657,0.));
#64541=CARTESIAN_POINT('Ctrl Pts',(26.662347896387,-67.798275899657,12.));
#64542=CARTESIAN_POINT('Ctrl Pts',(26.6798535069589,-67.8168769447098,0.));
#64543=CARTESIAN_POINT('Ctrl Pts',(26.6798535069589,-67.8168769447098,12.));
#64544=CARTESIAN_POINT('Ctrl Pts',(26.6974034154804,-67.8354898246086,0.));
#64545=CARTESIAN_POINT('Ctrl Pts',(26.6974034154804,-67.8354898246086,12.));
#64546=CARTESIAN_POINT('Ctrl Pts',(26.7149975906477,-67.8541144282875,0.));
#64547=CARTESIAN_POINT('Ctrl Pts',(26.7149975906477,-67.8541144282875,12.));
#64548=CARTESIAN_POINT('Ctrl Pts',(26.7326360011884,-67.8727506451064,0.));
#64549=CARTESIAN_POINT('Ctrl Pts',(26.7326360011884,-67.8727506451064,12.));
#64550=CARTESIAN_POINT('Ctrl Pts',(26.7503186158522,-67.8913983648437,0.));
#64551=CARTESIAN_POINT('Ctrl Pts',(26.7503186158522,-67.8913983648437,12.));
#64552=CARTESIAN_POINT('Ctrl Pts',(26.7680454034168,-67.9100574776972,0.));
#64553=CARTESIAN_POINT('Ctrl Pts',(26.7680454034168,-67.9100574776972,12.));
#64554=CARTESIAN_POINT('Ctrl Pts',(26.7858163326933,-67.928727874284,0.));
#64555=CARTESIAN_POINT('Ctrl Pts',(26.7858163326933,-67.928727874284,12.));
#64556=CARTESIAN_POINT('Ctrl Pts',(26.8036313725262,-67.9474094456396,0.));
#64557=CARTESIAN_POINT('Ctrl Pts',(26.8036313725262,-67.9474094456396,12.));
#64558=CARTESIAN_POINT('Ctrl Pts',(26.821490491792,-67.9661020832164,0.));
#64559=CARTESIAN_POINT('Ctrl Pts',(26.821490491792,-67.9661020832164,12.));
#64560=CARTESIAN_POINT('Ctrl Pts',(26.8393936593911,-67.9848056788809,0.));
#64561=CARTESIAN_POINT('Ctrl Pts',(26.8393936593911,-67.9848056788809,12.));
#64562=CARTESIAN_POINT('Ctrl Pts',(26.8573408442496,-68.0035201249102,0.));
#64563=CARTESIAN_POINT('Ctrl Pts',(26.8573408442496,-68.0035201249102,12.));
#64564=CARTESIAN_POINT('Ctrl Pts',(26.8753320153251,-68.0222453139856,0.));
#64565=CARTESIAN_POINT('Ctrl Pts',(26.8753320153251,-68.0222453139856,12.));
#64566=CARTESIAN_POINT('Ctrl Pts',(26.8933671416062,-68.0409811391869,0.));
#64567=CARTESIAN_POINT('Ctrl Pts',(26.8933671416062,-68.0409811391869,12.));
#64568=CARTESIAN_POINT('Ctrl Pts',(26.9114461921109,-68.0597274939859,0.));
#64569=CARTESIAN_POINT('Ctrl Pts',(26.9114461921109,-68.0597274939859,12.));
#64570=CARTESIAN_POINT('Ctrl Pts',(26.9295691358778,-68.0784842722369,0.));
#64571=CARTESIAN_POINT('Ctrl Pts',(26.9295691358778,-68.0784842722369,12.));
#64572=CARTESIAN_POINT('Ctrl Pts',(26.9477359419651,-68.0972513681751,0.));
#64573=CARTESIAN_POINT('Ctrl Pts',(26.9477359419651,-68.0972513681751,12.));
#64574=CARTESIAN_POINT('Ctrl Pts',(26.9659465794601,-68.1160286764255,0.));
#64575=CARTESIAN_POINT('Ctrl Pts',(26.9659465794601,-68.1160286764255,12.));
#64576=CARTESIAN_POINT('Ctrl Pts',(26.9842010174821,-68.1348160920107,0.));
#64577=CARTESIAN_POINT('Ctrl Pts',(26.9842010174821,-68.1348160920107,12.));
#64578=CARTESIAN_POINT('Ctrl Pts',(27.0024992251838,-68.1536135103557,0.));
#64579=CARTESIAN_POINT('Ctrl Pts',(27.0024992251838,-68.1536135103557,12.));
#64580=CARTESIAN_POINT('Ctrl Pts',(27.0208411717472,-68.1724208272958,0.));
#64581=CARTESIAN_POINT('Ctrl Pts',(27.0208411717472,-68.1724208272958,12.));
#64582=CARTESIAN_POINT('Ctrl Pts',(27.0392268263797,-68.1912379390773,0.));
#64583=CARTESIAN_POINT('Ctrl Pts',(27.0392268263797,-68.1912379390773,12.));
#64584=CARTESIAN_POINT('Ctrl Pts',(27.0576561583172,-68.2100647423332,0.));
#64585=CARTESIAN_POINT('Ctrl Pts',(27.0576561583172,-68.2100647423332,12.));
#64586=CARTESIAN_POINT('Ctrl Pts',(27.0761291368225,-68.2289011340615,0.));
#64587=CARTESIAN_POINT('Ctrl Pts',(27.0761291368225,-68.2289011340615,12.));
#64588=CARTESIAN_POINT('Ctrl Pts',(27.0946457311812,-68.2477470116013,0.));
#64589=CARTESIAN_POINT('Ctrl Pts',(27.0946457311812,-68.2477470116013,12.));
#64590=CARTESIAN_POINT('Ctrl Pts',(27.1132059106943,-68.2666022726104,0.));
#64591=CARTESIAN_POINT('Ctrl Pts',(27.1132059106943,-68.2666022726104,12.));
#64592=CARTESIAN_POINT('Ctrl Pts',(27.1318096446648,-68.2854668150364,0.));
#64593=CARTESIAN_POINT('Ctrl Pts',(27.1318096446648,-68.2854668150364,12.));
#64594=CARTESIAN_POINT('Ctrl Pts',(27.1504569024136,-68.3043405371603,0.));
#64595=CARTESIAN_POINT('Ctrl Pts',(27.1504569024136,-68.3043405371603,12.));
#64596=CARTESIAN_POINT('Ctrl Pts',(27.1691476532921,-68.3232233376425,0.));
#64597=CARTESIAN_POINT('Ctrl Pts',(27.1691476532921,-68.3232233376425,12.));
#64598=CARTESIAN_POINT('Ctrl Pts',(27.1878818666926,-68.3421151155711,0.));
#64599=CARTESIAN_POINT('Ctrl Pts',(27.1878818666926,-68.3421151155711,12.));
#64600=CARTESIAN_POINT('Ctrl Pts',(27.2066595120541,-68.3610157704994,0.));
#64601=CARTESIAN_POINT('Ctrl Pts',(27.2066595120541,-68.3610157704994,12.));
#64602=CARTESIAN_POINT('Ctrl Pts',(27.2254805588673,-68.3799252025102,0.));
#64603=CARTESIAN_POINT('Ctrl Pts',(27.2254805588673,-68.3799252025102,12.));
#64604=CARTESIAN_POINT('Ctrl Pts',(27.244344976665,-68.3988433121581,0.));
#64605=CARTESIAN_POINT('Ctrl Pts',(27.244344976665,-68.3988433121581,12.));
#64606=CARTESIAN_POINT('Ctrl Pts',(27.2632527350059,-68.4177700003465,0.));
#64607=CARTESIAN_POINT('Ctrl Pts',(27.2632527350059,-68.4177700003465,12.));
#64608=CARTESIAN_POINT('Ctrl Pts',(27.2822038034538,-68.4367051682164,0.));
#64609=CARTESIAN_POINT('Ctrl Pts',(27.2822038034538,-68.4367051682164,12.));
#64610=CARTESIAN_POINT('Ctrl Pts',(27.301198151557,-68.4556487170441,0.));
#64611=CARTESIAN_POINT('Ctrl Pts',(27.301198151557,-68.4556487170441,12.));
#64612=CARTESIAN_POINT('Ctrl Pts',(27.3202357488154,-68.4746005480997,0.));
#64613=CARTESIAN_POINT('Ctrl Pts',(27.3202357488154,-68.4746005480997,12.));
#64614=CARTESIAN_POINT('Ctrl Pts',(27.3393165646751,-68.4935605626372,0.));
#64615=CARTESIAN_POINT('Ctrl Pts',(27.3393165646751,-68.4935605626372,12.));
#64616=CARTESIAN_POINT('Ctrl Pts',(27.3584405685947,-68.5125286621902,0.));
#64617=CARTESIAN_POINT('Ctrl Pts',(27.3584405685947,-68.5125286621902,12.));
#64618=CARTESIAN_POINT('Ctrl Pts',(27.3776077300918,-68.5315047488046,0.));
#64619=CARTESIAN_POINT('Ctrl Pts',(27.3776077300918,-68.5315047488046,12.));
#64620=CARTESIAN_POINT('Ctrl Pts',(27.3968180187941,-68.5504887252976,0.));
#64621=CARTESIAN_POINT('Ctrl Pts',(27.3968180187941,-68.5504887252976,12.));
#64622=CARTESIAN_POINT('Ctrl Pts',(27.4160714044825,-68.5694804955002,0.));
#64623=CARTESIAN_POINT('Ctrl Pts',(27.4160714044825,-68.5694804955002,12.));
#64624=CARTESIAN_POINT('Ctrl Pts',(27.4353678571349,-68.5884799645193,0.));
#64625=CARTESIAN_POINT('Ctrl Pts',(27.4353678571349,-68.5884799645193,12.));
#64626=CARTESIAN_POINT('Ctrl Pts',(27.4547073468212,-68.6074870381588,0.));
#64627=CARTESIAN_POINT('Ctrl Pts',(27.4547073468212,-68.6074870381588,12.));
#64628=CARTESIAN_POINT('Ctrl Pts',(27.4740898435976,-68.6265016223536,0.));
#64629=CARTESIAN_POINT('Ctrl Pts',(27.4740898435976,-68.6265016223536,12.));
#64630=CARTESIAN_POINT('Ctrl Pts',(27.4935153173863,-68.6455236225471,0.));
#64631=CARTESIAN_POINT('Ctrl Pts',(27.4935153173863,-68.6455236225471,12.));
#64632=CARTESIAN_POINT('Ctrl Pts',(27.5129837378797,-68.664552943206,0.));
#64633=CARTESIAN_POINT('Ctrl Pts',(27.5129837378797,-68.664552943206,12.));
#64634=CARTESIAN_POINT('Ctrl Pts',(27.5324950743722,-68.683589486992,0.));
#64635=CARTESIAN_POINT('Ctrl Pts',(27.5324950743722,-68.683589486992,12.));
#64636=CARTESIAN_POINT('Ctrl Pts',(27.552049295893,-68.7026331554349,0.));
#64637=CARTESIAN_POINT('Ctrl Pts',(27.552049295893,-68.7026331554349,12.));
#64638=CARTESIAN_POINT('Ctrl Pts',(27.5716463715027,-68.721683850427,0.));
#64639=CARTESIAN_POINT('Ctrl Pts',(27.5716463715027,-68.721683850427,12.));
#64640=CARTESIAN_POINT('Ctrl Pts',(27.5912862705482,-68.7407414755291,0.));
#64641=CARTESIAN_POINT('Ctrl Pts',(27.5912862705482,-68.7407414755291,12.));
#64642=CARTESIAN_POINT('Ctrl Pts',(27.6109689629025,-68.7598059372121,0.));
#64643=CARTESIAN_POINT('Ctrl Pts',(27.6109689629025,-68.7598059372121,12.));
#64644=CARTESIAN_POINT('Ctrl Pts',(27.6306944192711,-68.7788771464655,0.));
#64645=CARTESIAN_POINT('Ctrl Pts',(27.6306944192711,-68.7788771464655,12.));
#64646=CARTESIAN_POINT('Ctrl Pts',(27.6504626112621,-68.7979550191773,0.));
#64647=CARTESIAN_POINT('Ctrl Pts',(27.6504626112621,-68.7979550191773,12.));
#64648=CARTESIAN_POINT('Ctrl Pts',(27.6702735107069,-68.8170394725786,0.));
#64649=CARTESIAN_POINT('Ctrl Pts',(27.6702735107069,-68.8170394725786,12.));
#64650=CARTESIAN_POINT('Ctrl Pts',(27.6901270891201,-68.8361304224378,0.));
#64651=CARTESIAN_POINT('Ctrl Pts',(27.6901270891201,-68.8361304224378,12.));
#64652=CARTESIAN_POINT('Ctrl Pts',(27.7100233170728,-68.8552277798181,0.));
#64653=CARTESIAN_POINT('Ctrl Pts',(27.7100233170728,-68.8552277798181,12.));
#64654=CARTESIAN_POINT('Ctrl Pts',(27.7299621636602,-68.8743314483451,0.));
#64655=CARTESIAN_POINT('Ctrl Pts',(27.7299621636602,-68.8743314483451,12.));
#64656=CARTESIAN_POINT('Ctrl Pts',(27.7499435957607,-68.8934413203945,0.));
#64657=CARTESIAN_POINT('Ctrl Pts',(27.7499435957607,-68.8934413203945,12.));
#64658=CARTESIAN_POINT('Ctrl Pts',(27.7699675790683,-68.9125572825946,0.));
#64659=CARTESIAN_POINT('Ctrl Pts',(27.7699675790683,-68.9125572825946,12.));
#64660=CARTESIAN_POINT('Ctrl Pts',(27.7900340793796,-68.9316792226187,0.));
#64661=CARTESIAN_POINT('Ctrl Pts',(27.7900340793796,-68.9316792226187,12.));
#64662=CARTESIAN_POINT('Ctrl Pts',(27.8101430638128,-68.9508070357786,0.));
#64663=CARTESIAN_POINT('Ctrl Pts',(27.8101430638128,-68.9508070357786,12.));
#64664=CARTESIAN_POINT('Ctrl Pts',(27.8302945019938,-68.9699406311305,0.));
#64665=CARTESIAN_POINT('Ctrl Pts',(27.8302945019938,-68.9699406311305,12.));
#64666=CARTESIAN_POINT('Ctrl Pts',(27.8504883673902,-68.9890799391863,0.));
#64667=CARTESIAN_POINT('Ctrl Pts',(27.8504883673902,-68.9890799391863,12.));
#64668=CARTESIAN_POINT('Ctrl Pts',(27.8707246380697,-69.0082249138015,0.));
#64669=CARTESIAN_POINT('Ctrl Pts',(27.8707246380697,-69.0082249138015,12.));
#64670=CARTESIAN_POINT('Ctrl Pts',(27.8910032967036,-69.0273755264702,0.));
#64671=CARTESIAN_POINT('Ctrl Pts',(27.8910032967036,-69.0273755264702,12.));
#64672=CARTESIAN_POINT('Ctrl Pts',(27.9072601239469,-69.0427005153223,0.));
#64673=CARTESIAN_POINT('Ctrl Pts',(27.9072601239469,-69.0427005153223,12.));
#64674=CARTESIAN_POINT('Ctrl Pts',(27.919471809885,-69.0541967850685,0.));
#64675=CARTESIAN_POINT('Ctrl Pts',(27.919471809885,-69.0541967850685,12.));
#64676=CARTESIAN_POINT('Ctrl Pts',(27.9276214070575,-69.0618620884596,0.));
#64677=CARTESIAN_POINT('Ctrl Pts',(27.9276214070575,-69.0618620884596,12.));
#64678=CARTESIAN_POINT('Ctrl Pts',(27.9316983239472,-69.065695021045,0.));
#64679=CARTESIAN_POINT('Ctrl Pts',(27.9316983239472,-69.065695021045,12.));
#64680=CARTESIAN_POINT('',(24.7419628022041,-65.4815644032299,0.));
#64681=CARTESIAN_POINT('Ctrl Pts',(24.7419628022041,-65.4815644032299,0.));
#64682=CARTESIAN_POINT('Ctrl Pts',(24.7442214063382,-65.4847237095443,0.));
#64683=CARTESIAN_POINT('Ctrl Pts',(24.7487434955981,-65.4910454936254,0.));
#64684=CARTESIAN_POINT('Ctrl Pts',(24.7555412724651,-65.5005376841101,0.));
#64685=CARTESIAN_POINT('Ctrl Pts',(24.7646342620841,-65.5132129675333,0.));
#64686=CARTESIAN_POINT('Ctrl Pts',(24.7760493148465,-65.5290887770232,0.));
#64687=CARTESIAN_POINT('Ctrl Pts',(24.787513182749,-65.5449962514662,0.));
#64688=CARTESIAN_POINT('Ctrl Pts',(24.7990258561259,-65.5609353062829,0.));
#64689=CARTESIAN_POINT('Ctrl Pts',(24.8105873098626,-65.5769057914333,0.));
#64690=CARTESIAN_POINT('Ctrl Pts',(24.8221975032103,-65.5929074932624,0.));
#64691=CARTESIAN_POINT('Ctrl Pts',(24.8338563866763,-65.6089401625628,0.));
#64692=CARTESIAN_POINT('Ctrl Pts',(24.8455639071516,-65.6250035361612,0.));
#64693=CARTESIAN_POINT('Ctrl Pts',(24.8573200135665,-65.6410973603661,0.));
#64694=CARTESIAN_POINT('Ctrl Pts',(24.8691246628056,-65.6572214156692,0.));
#64695=CARTESIAN_POINT('Ctrl Pts',(24.8809778178228,-65.6733755087669,0.));
#64696=CARTESIAN_POINT('Ctrl Pts',(24.8928794448607,-65.6895594608776,0.));
#64697=CARTESIAN_POINT('Ctrl Pts',(24.9048295111448,-65.7057730980483,0.));
#64698=CARTESIAN_POINT('Ctrl Pts',(24.9168279820106,-65.7220162391054,0.));
#64699=CARTESIAN_POINT('Ctrl Pts',(24.928874819458,-65.7382886895888,0.));
#64700=CARTESIAN_POINT('Ctrl Pts',(24.9409699836537,-65.7545902480323,0.));
#64701=CARTESIAN_POINT('Ctrl Pts',(24.9531134338696,-65.7709207098959,0.));
#64702=CARTESIAN_POINT('Ctrl Pts',(24.965305129558,-65.7872798720823,0.));
#64703=CARTESIAN_POINT('Ctrl Pts',(24.9775450315682,-65.8036675380718,0.));
#64704=CARTESIAN_POINT('Ctrl Pts',(24.9898331020983,-65.8200835177024,0.));
#64705=CARTESIAN_POINT('Ctrl Pts',(25.0021693041169,-65.8365276247128,0.));
#64706=CARTESIAN_POINT('Ctrl Pts',(25.0145536009604,-65.8529996750445,0.));
#64707=CARTESIAN_POINT('Ctrl Pts',(25.0269859558362,-65.8694994847617,0.));
#64708=CARTESIAN_POINT('Ctrl Pts',(25.0394663314055,-65.8860268683128,0.));
#64709=CARTESIAN_POINT('Ctrl Pts',(25.0519946900078,-65.9025816394424,0.));
#64710=CARTESIAN_POINT('Ctrl Pts',(25.0645709938524,-65.919163611981,0.));
#64711=CARTESIAN_POINT('Ctrl Pts',(25.0771952052028,-65.9357726006163,0.));
#64712=CARTESIAN_POINT('Ctrl Pts',(25.0898672865915,-65.952408421814,0.));
#64713=CARTESIAN_POINT('Ctrl Pts',(25.1025872009003,-65.9690708941558,0.));
#64714=CARTESIAN_POINT('Ctrl Pts',(25.1153549112503,-65.9857598378433,0.));
#64715=CARTESIAN_POINT('Ctrl Pts',(25.1281703809297,-66.0024750743897,0.));
#64716=CARTESIAN_POINT('Ctrl Pts',(25.1410335733098,-66.0192164262621,0.));
#64717=CARTESIAN_POINT('Ctrl Pts',(25.1539444517418,-66.0359837164734,0.));
#64718=CARTESIAN_POINT('Ctrl Pts',(25.166902979566,-66.0527767686025,0.));
#64719=CARTESIAN_POINT('Ctrl Pts',(25.1799091201599,-66.0695954069713,0.));
#64720=CARTESIAN_POINT('Ctrl Pts',(25.1929628369684,-66.086439456768,0.));
#64721=CARTESIAN_POINT('Ctrl Pts',(25.2060640935365,-66.10330874419,0.));
#64722=CARTESIAN_POINT('Ctrl Pts',(25.2192128535357,-66.1202030965759,0.));
#64723=CARTESIAN_POINT('Ctrl Pts',(25.2324090807549,-66.1371223423345,0.));
#64724=CARTESIAN_POINT('Ctrl Pts',(25.2456527390874,-66.1540663108754,0.));
#64725=CARTESIAN_POINT('Ctrl Pts',(25.2589437925146,-66.1710348325384,0.));
#64726=CARTESIAN_POINT('Ctrl Pts',(25.2722822050836,-66.1880277385136,0.));
#64727=CARTESIAN_POINT('Ctrl Pts',(25.285667940893,-66.2050448607911,0.));
#64728=CARTESIAN_POINT('Ctrl Pts',(25.2991009641094,-66.2220860321952,0.));
#64729=CARTESIAN_POINT('Ctrl Pts',(25.3125812389729,-66.2391510863998,0.));
#64730=CARTESIAN_POINT('Ctrl Pts',(25.3261087298026,-66.2562398579471,0.));
#64731=CARTESIAN_POINT('Ctrl Pts',(25.3396834009949,-66.2733521822662,0.));
#64732=CARTESIAN_POINT('Ctrl Pts',(25.3533052170248,-66.290487895671,0.));
#64733=CARTESIAN_POINT('Ctrl Pts',(25.3669741424488,-66.3076468353413,0.));
#64734=CARTESIAN_POINT('Ctrl Pts',(25.3806901419012,-66.3248288393046,0.));
#64735=CARTESIAN_POINT('Ctrl Pts',(25.3944531800901,-66.3420337464178,0.));
#64736=CARTESIAN_POINT('Ctrl Pts',(25.4082632217847,-66.359261396341,0.));
#64737=CARTESIAN_POINT('Ctrl Pts',(25.4221202318199,-66.3765116295365,0.));
#64738=CARTESIAN_POINT('Ctrl Pts',(25.4360241751017,-66.3937842872685,0.));
#64739=CARTESIAN_POINT('Ctrl Pts',(25.4499750166078,-66.4110792116,0.));
#64740=CARTESIAN_POINT('Ctrl Pts',(25.4639727213849,-66.4283962453899,0.));
#64741=CARTESIAN_POINT('Ctrl Pts',(25.4780172545417,-66.4457352322871,0.));
#64742=CARTESIAN_POINT('Ctrl Pts',(25.4921085812547,-66.4630960167252,0.));
#64743=CARTESIAN_POINT('Ctrl Pts',(25.5062466667702,-66.4804784439148,0.));
#64744=CARTESIAN_POINT('Ctrl Pts',(25.5204314764033,-66.4978823598354,0.));
#64745=CARTESIAN_POINT('Ctrl Pts',(25.534662975532,-66.5153076112231,0.));
#64746=CARTESIAN_POINT('Ctrl Pts',(25.5489411295911,-66.5327540455624,0.));
#64747=CARTESIAN_POINT('Ctrl Pts',(25.5632659040792,-66.5502215110829,0.));
#64748=CARTESIAN_POINT('Ctrl Pts',(25.5776372645601,-66.5677098567542,0.));
#64749=CARTESIAN_POINT('Ctrl Pts',(25.5920551766629,-66.5852189322813,0.));
#64750=CARTESIAN_POINT('Ctrl Pts',(25.6065196060755,-66.6027485880963,0.));
#64751=CARTESIAN_POINT('Ctrl Pts',(25.6210305185403,-66.6202986753507,0.));
#64752=CARTESIAN_POINT('Ctrl Pts',(25.6355878798613,-66.6378690459129,0.));
#64753=CARTESIAN_POINT('Ctrl Pts',(25.6501916559055,-66.6554595523624,0.));
#64754=CARTESIAN_POINT('Ctrl Pts',(25.6648418126013,-66.6730700479837,0.));
#64755=CARTESIAN_POINT('Ctrl Pts',(25.6795383159319,-66.6907003867572,0.));
#64756=CARTESIAN_POINT('Ctrl Pts',(25.6942811319322,-66.7083504233529,0.));
#64757=CARTESIAN_POINT('Ctrl Pts',(25.7090702266962,-66.7260200131266,0.));
#64758=CARTESIAN_POINT('Ctrl Pts',(25.7239055663772,-66.7437090121153,0.));
#64759=CARTESIAN_POINT('Ctrl Pts',(25.7387871171866,-66.7614172770316,0.));
#64760=CARTESIAN_POINT('Ctrl Pts',(25.7537148453863,-66.7791446652545,0.));
#64761=CARTESIAN_POINT('Ctrl Pts',(25.7686887172877,-66.7968910348245,0.));
#64762=CARTESIAN_POINT('Ctrl Pts',(25.7837086992594,-66.8146562444433,0.));
#64763=CARTESIAN_POINT('Ctrl Pts',(25.7987747577269,-66.8324401534668,0.));
#64764=CARTESIAN_POINT('Ctrl Pts',(25.8138868591709,-66.8502426219001,0.));
#64765=CARTESIAN_POINT('Ctrl Pts',(25.8290449701192,-66.8680635103876,0.));
#64766=CARTESIAN_POINT('Ctrl Pts',(25.844249057147,-66.8859026802088,0.));
#64767=CARTESIAN_POINT('Ctrl Pts',(25.8594990868833,-66.9037599932761,0.));
#64768=CARTESIAN_POINT('Ctrl Pts',(25.874795026011,-66.92163531213,0.));
#64769=CARTESIAN_POINT('Ctrl Pts',(25.890136841266,-66.939528499934,0.));
#64770=CARTESIAN_POINT('Ctrl Pts',(25.9055244994277,-66.9574394204663,0.));
#64771=CARTESIAN_POINT('Ctrl Pts',(25.9209579673209,-66.975367938115,0.));
#64772=CARTESIAN_POINT('Ctrl Pts',(25.9364372118222,-66.9933139178778,0.));
#64773=CARTESIAN_POINT('Ctrl Pts',(25.9519621998598,-67.0112772253556,0.));
#64774=CARTESIAN_POINT('Ctrl Pts',(25.967532898412,-67.0292577267489,0.));
#64775=CARTESIAN_POINT('Ctrl Pts',(25.9831492744983,-67.0472552888485,0.));
#64776=CARTESIAN_POINT('Ctrl Pts',(25.9988112951814,-67.0652697790325,0.));
#64777=CARTESIAN_POINT('Ctrl Pts',(26.014518927573,-67.0833010652634,0.));
#64778=CARTESIAN_POINT('Ctrl Pts',(26.0302721388339,-67.101349016084,0.));
#64779=CARTESIAN_POINT('Ctrl Pts',(26.0460708961725,-67.1194135006124,0.));
#64780=CARTESIAN_POINT('Ctrl Pts',(26.061915166836,-67.1374943885354,0.));
#64781=CARTESIAN_POINT('Ctrl Pts',(26.0778049181128,-67.1555915501049,0.));
#64782=CARTESIAN_POINT('Ctrl Pts',(26.0937401173383,-67.173704856136,0.));
#64783=CARTESIAN_POINT('Ctrl Pts',(26.1097207318949,-67.1918341780018,0.));
#64784=CARTESIAN_POINT('Ctrl Pts',(26.1257467292102,-67.2099793876297,0.));
#64785=CARTESIAN_POINT('Ctrl Pts',(26.1418180767489,-67.2281403574938,0.));
#64786=CARTESIAN_POINT('Ctrl Pts',(26.1579347420138,-67.2463169606115,0.));
#64787=CARTESIAN_POINT('Ctrl Pts',(26.1740966925528,-67.2645090705421,0.));
#64788=CARTESIAN_POINT('Ctrl Pts',(26.1903038959589,-67.282716561383,0.));
#64789=CARTESIAN_POINT('Ctrl Pts',(26.2065563198683,-67.3009393077652,0.));
#64790=CARTESIAN_POINT('Ctrl Pts',(26.2228539319526,-67.3191771848464,0.));
#64791=CARTESIAN_POINT('Ctrl Pts',(26.2391966999191,-67.3374300683074,0.));
#64792=CARTESIAN_POINT('Ctrl Pts',(26.255584591518,-67.3556978343507,0.));
#64793=CARTESIAN_POINT('Ctrl Pts',(26.2720175745423,-67.3739803596969,0.));
#64794=CARTESIAN_POINT('Ctrl Pts',(26.2884956168269,-67.392277521581,0.));
#64795=CARTESIAN_POINT('Ctrl Pts',(26.3050186862407,-67.4105891977461,0.));
#64796=CARTESIAN_POINT('Ctrl Pts',(26.321586750686,-67.4289152664398,0.));
#64797=CARTESIAN_POINT('Ctrl Pts',(26.3381997781055,-67.4472556064119,0.));
#64798=CARTESIAN_POINT('Ctrl Pts',(26.3548577364833,-67.4656100969116,0.));
#64799=CARTESIAN_POINT('Ctrl Pts',(26.3715605938432,-67.4839786176836,0.));
#64800=CARTESIAN_POINT('Ctrl Pts',(26.3883083182421,-67.5023610489622,0.));
#64801=CARTESIAN_POINT('Ctrl Pts',(26.4051008777675,-67.5207572714683,0.));
#64802=CARTESIAN_POINT('Ctrl Pts',(26.4219382405458,-67.5391671664072,0.));
#64803=CARTESIAN_POINT('Ctrl Pts',(26.4388203747425,-67.5575906154657,0.));
#64804=CARTESIAN_POINT('Ctrl Pts',(26.455747248562,-67.5760275008093,0.));
#64805=CARTESIAN_POINT('Ctrl Pts',(26.4727188302409,-67.5944777050768,0.));
#64806=CARTESIAN_POINT('Ctrl Pts',(26.4897350880439,-67.6129411113758,0.));
#64807=CARTESIAN_POINT('Ctrl Pts',(26.5067959902725,-67.6314176032811,0.));
#64808=CARTESIAN_POINT('Ctrl Pts',(26.5239015052653,-67.649907064832,0.));
#64809=CARTESIAN_POINT('Ctrl Pts',(26.5410516013984,-67.6684093805291,0.));
#64810=CARTESIAN_POINT('Ctrl Pts',(26.5582462470794,-67.6869244353294,0.));
#64811=CARTESIAN_POINT('Ctrl Pts',(26.5754854107421,-67.7054521146425,0.));
#64812=CARTESIAN_POINT('Ctrl Pts',(26.5927690608543,-67.7239923043288,0.));
#64813=CARTESIAN_POINT('Ctrl Pts',(26.6100971659201,-67.7425448906977,0.));
#64814=CARTESIAN_POINT('Ctrl Pts',(26.6274696944792,-67.7611097605042,0.));
#64815=CARTESIAN_POINT('Ctrl Pts',(26.6448866151029,-67.7796868009455,0.));
#64816=CARTESIAN_POINT('Ctrl Pts',(26.662347896387,-67.798275899657,0.));
#64817=CARTESIAN_POINT('Ctrl Pts',(26.6798535069589,-67.8168769447098,0.));
#64818=CARTESIAN_POINT('Ctrl Pts',(26.6974034154804,-67.8354898246086,0.));
#64819=CARTESIAN_POINT('Ctrl Pts',(26.7149975906477,-67.8541144282875,0.));
#64820=CARTESIAN_POINT('Ctrl Pts',(26.7326360011884,-67.8727506451064,0.));
#64821=CARTESIAN_POINT('Ctrl Pts',(26.7503186158522,-67.8913983648437,0.));
#64822=CARTESIAN_POINT('Ctrl Pts',(26.7680454034168,-67.9100574776972,0.));
#64823=CARTESIAN_POINT('Ctrl Pts',(26.7858163326933,-67.928727874284,0.));
#64824=CARTESIAN_POINT('Ctrl Pts',(26.8036313725262,-67.9474094456396,0.));
#64825=CARTESIAN_POINT('Ctrl Pts',(26.821490491792,-67.9661020832164,0.));
#64826=CARTESIAN_POINT('Ctrl Pts',(26.8393936593911,-67.9848056788809,0.));
#64827=CARTESIAN_POINT('Ctrl Pts',(26.8573408442496,-68.0035201249102,0.));
#64828=CARTESIAN_POINT('Ctrl Pts',(26.8753320153251,-68.0222453139856,0.));
#64829=CARTESIAN_POINT('Ctrl Pts',(26.8933671416062,-68.0409811391869,0.));
#64830=CARTESIAN_POINT('Ctrl Pts',(26.9114461921109,-68.0597274939859,0.));
#64831=CARTESIAN_POINT('Ctrl Pts',(26.9295691358778,-68.0784842722369,0.));
#64832=CARTESIAN_POINT('Ctrl Pts',(26.9477359419651,-68.0972513681751,0.));
#64833=CARTESIAN_POINT('Ctrl Pts',(26.9659465794601,-68.1160286764255,0.));
#64834=CARTESIAN_POINT('Ctrl Pts',(26.9842010174821,-68.1348160920107,0.));
#64835=CARTESIAN_POINT('Ctrl Pts',(27.0024992251838,-68.1536135103557,0.));
#64836=CARTESIAN_POINT('Ctrl Pts',(27.0208411717472,-68.1724208272958,0.));
#64837=CARTESIAN_POINT('Ctrl Pts',(27.0392268263797,-68.1912379390773,0.));
#64838=CARTESIAN_POINT('Ctrl Pts',(27.0576561583172,-68.2100647423332,0.));
#64839=CARTESIAN_POINT('Ctrl Pts',(27.0761291368225,-68.2289011340615,0.));
#64840=CARTESIAN_POINT('Ctrl Pts',(27.0946457311812,-68.2477470116013,0.));
#64841=CARTESIAN_POINT('Ctrl Pts',(27.1132059106943,-68.2666022726104,0.));
#64842=CARTESIAN_POINT('Ctrl Pts',(27.1318096446648,-68.2854668150364,0.));
#64843=CARTESIAN_POINT('Ctrl Pts',(27.1504569024136,-68.3043405371603,0.));
#64844=CARTESIAN_POINT('Ctrl Pts',(27.1691476532921,-68.3232233376425,0.));
#64845=CARTESIAN_POINT('Ctrl Pts',(27.1878818666926,-68.3421151155711,0.));
#64846=CARTESIAN_POINT('Ctrl Pts',(27.2066595120541,-68.3610157704994,0.));
#64847=CARTESIAN_POINT('Ctrl Pts',(27.2254805588673,-68.3799252025102,0.));
#64848=CARTESIAN_POINT('Ctrl Pts',(27.244344976665,-68.3988433121581,0.));
#64849=CARTESIAN_POINT('Ctrl Pts',(27.2632527350059,-68.4177700003465,0.));
#64850=CARTESIAN_POINT('Ctrl Pts',(27.2822038034538,-68.4367051682164,0.));
#64851=CARTESIAN_POINT('Ctrl Pts',(27.301198151557,-68.4556487170441,0.));
#64852=CARTESIAN_POINT('Ctrl Pts',(27.3202357488154,-68.4746005480997,0.));
#64853=CARTESIAN_POINT('Ctrl Pts',(27.3393165646751,-68.4935605626372,0.));
#64854=CARTESIAN_POINT('Ctrl Pts',(27.3584405685947,-68.5125286621902,0.));
#64855=CARTESIAN_POINT('Ctrl Pts',(27.3776077300918,-68.5315047488046,0.));
#64856=CARTESIAN_POINT('Ctrl Pts',(27.3968180187941,-68.5504887252976,0.));
#64857=CARTESIAN_POINT('Ctrl Pts',(27.4160714044825,-68.5694804955002,0.));
#64858=CARTESIAN_POINT('Ctrl Pts',(27.4353678571349,-68.5884799645193,0.));
#64859=CARTESIAN_POINT('Ctrl Pts',(27.4547073468212,-68.6074870381588,0.));
#64860=CARTESIAN_POINT('Ctrl Pts',(27.4740898435976,-68.6265016223536,0.));
#64861=CARTESIAN_POINT('Ctrl Pts',(27.4935153173863,-68.6455236225471,0.));
#64862=CARTESIAN_POINT('Ctrl Pts',(27.5129837378797,-68.664552943206,0.));
#64863=CARTESIAN_POINT('Ctrl Pts',(27.5324950743722,-68.683589486992,0.));
#64864=CARTESIAN_POINT('Ctrl Pts',(27.552049295893,-68.7026331554349,0.));
#64865=CARTESIAN_POINT('Ctrl Pts',(27.5716463715027,-68.721683850427,0.));
#64866=CARTESIAN_POINT('Ctrl Pts',(27.5912862705482,-68.7407414755291,0.));
#64867=CARTESIAN_POINT('Ctrl Pts',(27.6109689629025,-68.7598059372121,0.));
#64868=CARTESIAN_POINT('Ctrl Pts',(27.6306944192711,-68.7788771464655,0.));
#64869=CARTESIAN_POINT('Ctrl Pts',(27.6504626112621,-68.7979550191773,0.));
#64870=CARTESIAN_POINT('Ctrl Pts',(27.667444390988,-68.8143140938752,0.));
#64871=CARTESIAN_POINT('Ctrl Pts',(27.6804870323283,-68.8268597851978,0.));
#64872=CARTESIAN_POINT('Ctrl Pts',(27.689571627108,-68.8355891981874,0.));
#64873=CARTESIAN_POINT('Ctrl Pts',(27.6946856803477,-68.8405004465891,0.));
#64874=CARTESIAN_POINT('Ctrl Pts',(27.6958230984751,-68.8415926174769,0.));
#64875=CARTESIAN_POINT('',(24.7419628022041,-65.4815644032299,12.));
#64876=CARTESIAN_POINT('',(24.7419628022041,-65.4815644032299,0.));
#64877=CARTESIAN_POINT('Ctrl Pts',(27.6958230984751,-68.8415926174769,12.));
#64878=CARTESIAN_POINT('Ctrl Pts',(27.6946856803477,-68.8405004465891,12.));
#64879=CARTESIAN_POINT('Ctrl Pts',(27.689571627108,-68.8355891981874,12.));
#64880=CARTESIAN_POINT('Ctrl Pts',(27.6804870323283,-68.8268597851978,12.));
#64881=CARTESIAN_POINT('Ctrl Pts',(27.667444390988,-68.8143140938752,12.));
#64882=CARTESIAN_POINT('Ctrl Pts',(27.6504626112621,-68.7979550191773,12.));
#64883=CARTESIAN_POINT('Ctrl Pts',(27.6306944192711,-68.7788771464655,12.));
#64884=CARTESIAN_POINT('Ctrl Pts',(27.6109689629025,-68.7598059372121,12.));
#64885=CARTESIAN_POINT('Ctrl Pts',(27.5912862705482,-68.7407414755291,12.));
#64886=CARTESIAN_POINT('Ctrl Pts',(27.5716463715027,-68.721683850427,12.));
#64887=CARTESIAN_POINT('Ctrl Pts',(27.552049295893,-68.7026331554349,12.));
#64888=CARTESIAN_POINT('Ctrl Pts',(27.5324950743722,-68.683589486992,12.));
#64889=CARTESIAN_POINT('Ctrl Pts',(27.5129837378797,-68.664552943206,12.));
#64890=CARTESIAN_POINT('Ctrl Pts',(27.4935153173863,-68.6455236225471,12.));
#64891=CARTESIAN_POINT('Ctrl Pts',(27.4740898435976,-68.6265016223536,12.));
#64892=CARTESIAN_POINT('Ctrl Pts',(27.4547073468212,-68.6074870381588,12.));
#64893=CARTESIAN_POINT('Ctrl Pts',(27.4353678571349,-68.5884799645193,12.));
#64894=CARTESIAN_POINT('Ctrl Pts',(27.4160714044825,-68.5694804955002,12.));
#64895=CARTESIAN_POINT('Ctrl Pts',(27.3968180187941,-68.5504887252976,12.));
#64896=CARTESIAN_POINT('Ctrl Pts',(27.3776077300918,-68.5315047488046,12.));
#64897=CARTESIAN_POINT('Ctrl Pts',(27.3584405685947,-68.5125286621902,12.));
#64898=CARTESIAN_POINT('Ctrl Pts',(27.3393165646751,-68.4935605626372,12.));
#64899=CARTESIAN_POINT('Ctrl Pts',(27.3202357488154,-68.4746005480997,12.));
#64900=CARTESIAN_POINT('Ctrl Pts',(27.301198151557,-68.4556487170441,12.));
#64901=CARTESIAN_POINT('Ctrl Pts',(27.2822038034538,-68.4367051682164,12.));
#64902=CARTESIAN_POINT('Ctrl Pts',(27.2632527350059,-68.4177700003465,12.));
#64903=CARTESIAN_POINT('Ctrl Pts',(27.244344976665,-68.3988433121581,12.));
#64904=CARTESIAN_POINT('Ctrl Pts',(27.2254805588673,-68.3799252025102,12.));
#64905=CARTESIAN_POINT('Ctrl Pts',(27.2066595120541,-68.3610157704994,12.));
#64906=CARTESIAN_POINT('Ctrl Pts',(27.1878818666926,-68.3421151155711,12.));
#64907=CARTESIAN_POINT('Ctrl Pts',(27.1691476532921,-68.3232233376425,12.));
#64908=CARTESIAN_POINT('Ctrl Pts',(27.1504569024136,-68.3043405371603,12.));
#64909=CARTESIAN_POINT('Ctrl Pts',(27.1318096446648,-68.2854668150364,12.));
#64910=CARTESIAN_POINT('Ctrl Pts',(27.1132059106943,-68.2666022726104,12.));
#64911=CARTESIAN_POINT('Ctrl Pts',(27.0946457311812,-68.2477470116013,12.));
#64912=CARTESIAN_POINT('Ctrl Pts',(27.0761291368225,-68.2289011340615,12.));
#64913=CARTESIAN_POINT('Ctrl Pts',(27.0576561583172,-68.2100647423332,12.));
#64914=CARTESIAN_POINT('Ctrl Pts',(27.0392268263797,-68.1912379390773,12.));
#64915=CARTESIAN_POINT('Ctrl Pts',(27.0208411717472,-68.1724208272958,12.));
#64916=CARTESIAN_POINT('Ctrl Pts',(27.0024992251838,-68.1536135103557,12.));
#64917=CARTESIAN_POINT('Ctrl Pts',(26.9842010174821,-68.1348160920107,12.));
#64918=CARTESIAN_POINT('Ctrl Pts',(26.9659465794601,-68.1160286764255,12.));
#64919=CARTESIAN_POINT('Ctrl Pts',(26.9477359419651,-68.0972513681751,12.));
#64920=CARTESIAN_POINT('Ctrl Pts',(26.9295691358778,-68.0784842722369,12.));
#64921=CARTESIAN_POINT('Ctrl Pts',(26.9114461921109,-68.0597274939859,12.));
#64922=CARTESIAN_POINT('Ctrl Pts',(26.8933671416062,-68.0409811391869,12.));
#64923=CARTESIAN_POINT('Ctrl Pts',(26.8753320153251,-68.0222453139856,12.));
#64924=CARTESIAN_POINT('Ctrl Pts',(26.8573408442496,-68.0035201249102,12.));
#64925=CARTESIAN_POINT('Ctrl Pts',(26.8393936593911,-67.9848056788809,12.));
#64926=CARTESIAN_POINT('Ctrl Pts',(26.821490491792,-67.9661020832164,12.));
#64927=CARTESIAN_POINT('Ctrl Pts',(26.8036313725262,-67.9474094456396,12.));
#64928=CARTESIAN_POINT('Ctrl Pts',(26.7858163326933,-67.928727874284,12.));
#64929=CARTESIAN_POINT('Ctrl Pts',(26.7680454034168,-67.9100574776972,12.));
#64930=CARTESIAN_POINT('Ctrl Pts',(26.7503186158522,-67.8913983648437,12.));
#64931=CARTESIAN_POINT('Ctrl Pts',(26.7326360011884,-67.8727506451064,12.));
#64932=CARTESIAN_POINT('Ctrl Pts',(26.7149975906477,-67.8541144282875,12.));
#64933=CARTESIAN_POINT('Ctrl Pts',(26.6974034154804,-67.8354898246086,12.));
#64934=CARTESIAN_POINT('Ctrl Pts',(26.6798535069589,-67.8168769447098,12.));
#64935=CARTESIAN_POINT('Ctrl Pts',(26.662347896387,-67.798275899657,12.));
#64936=CARTESIAN_POINT('Ctrl Pts',(26.6448866151029,-67.7796868009455,12.));
#64937=CARTESIAN_POINT('Ctrl Pts',(26.6274696944792,-67.7611097605042,12.));
#64938=CARTESIAN_POINT('Ctrl Pts',(26.6100971659201,-67.7425448906977,12.));
#64939=CARTESIAN_POINT('Ctrl Pts',(26.5927690608543,-67.7239923043288,12.));
#64940=CARTESIAN_POINT('Ctrl Pts',(26.5754854107421,-67.7054521146425,12.));
#64941=CARTESIAN_POINT('Ctrl Pts',(26.5582462470794,-67.6869244353294,12.));
#64942=CARTESIAN_POINT('Ctrl Pts',(26.5410516013984,-67.6684093805291,12.));
#64943=CARTESIAN_POINT('Ctrl Pts',(26.5239015052653,-67.649907064832,12.));
#64944=CARTESIAN_POINT('Ctrl Pts',(26.5067959902725,-67.6314176032811,12.));
#64945=CARTESIAN_POINT('Ctrl Pts',(26.4897350880439,-67.6129411113758,12.));
#64946=CARTESIAN_POINT('Ctrl Pts',(26.4727188302409,-67.5944777050768,12.));
#64947=CARTESIAN_POINT('Ctrl Pts',(26.455747248562,-67.5760275008093,12.));
#64948=CARTESIAN_POINT('Ctrl Pts',(26.4388203747425,-67.5575906154657,12.));
#64949=CARTESIAN_POINT('Ctrl Pts',(26.4219382405458,-67.5391671664072,12.));
#64950=CARTESIAN_POINT('Ctrl Pts',(26.4051008777675,-67.5207572714683,12.));
#64951=CARTESIAN_POINT('Ctrl Pts',(26.3883083182421,-67.5023610489622,12.));
#64952=CARTESIAN_POINT('Ctrl Pts',(26.3715605938432,-67.4839786176836,12.));
#64953=CARTESIAN_POINT('Ctrl Pts',(26.3548577364833,-67.4656100969116,12.));
#64954=CARTESIAN_POINT('Ctrl Pts',(26.3381997781055,-67.4472556064119,12.));
#64955=CARTESIAN_POINT('Ctrl Pts',(26.321586750686,-67.4289152664398,12.));
#64956=CARTESIAN_POINT('Ctrl Pts',(26.3050186862407,-67.4105891977461,12.));
#64957=CARTESIAN_POINT('Ctrl Pts',(26.2884956168269,-67.392277521581,12.));
#64958=CARTESIAN_POINT('Ctrl Pts',(26.2720175745423,-67.3739803596969,12.));
#64959=CARTESIAN_POINT('Ctrl Pts',(26.255584591518,-67.3556978343507,12.));
#64960=CARTESIAN_POINT('Ctrl Pts',(26.2391966999191,-67.3374300683074,12.));
#64961=CARTESIAN_POINT('Ctrl Pts',(26.2228539319526,-67.3191771848464,12.));
#64962=CARTESIAN_POINT('Ctrl Pts',(26.2065563198683,-67.3009393077652,12.));
#64963=CARTESIAN_POINT('Ctrl Pts',(26.1903038959589,-67.282716561383,12.));
#64964=CARTESIAN_POINT('Ctrl Pts',(26.1740966925528,-67.2645090705421,12.));
#64965=CARTESIAN_POINT('Ctrl Pts',(26.1579347420138,-67.2463169606115,12.));
#64966=CARTESIAN_POINT('Ctrl Pts',(26.1418180767489,-67.2281403574938,12.));
#64967=CARTESIAN_POINT('Ctrl Pts',(26.1257467292102,-67.2099793876297,12.));
#64968=CARTESIAN_POINT('Ctrl Pts',(26.1097207318949,-67.1918341780018,12.));
#64969=CARTESIAN_POINT('Ctrl Pts',(26.0937401173383,-67.173704856136,12.));
#64970=CARTESIAN_POINT('Ctrl Pts',(26.0778049181128,-67.1555915501049,12.));
#64971=CARTESIAN_POINT('Ctrl Pts',(26.061915166836,-67.1374943885354,12.));
#64972=CARTESIAN_POINT('Ctrl Pts',(26.0460708961725,-67.1194135006124,12.));
#64973=CARTESIAN_POINT('Ctrl Pts',(26.0302721388339,-67.101349016084,12.));
#64974=CARTESIAN_POINT('Ctrl Pts',(26.014518927573,-67.0833010652634,12.));
#64975=CARTESIAN_POINT('Ctrl Pts',(25.9988112951814,-67.0652697790325,12.));
#64976=CARTESIAN_POINT('Ctrl Pts',(25.9831492744983,-67.0472552888485,12.));
#64977=CARTESIAN_POINT('Ctrl Pts',(25.967532898412,-67.0292577267489,12.));
#64978=CARTESIAN_POINT('Ctrl Pts',(25.9519621998598,-67.0112772253556,12.));
#64979=CARTESIAN_POINT('Ctrl Pts',(25.9364372118222,-66.9933139178778,12.));
#64980=CARTESIAN_POINT('Ctrl Pts',(25.9209579673209,-66.975367938115,12.));
#64981=CARTESIAN_POINT('Ctrl Pts',(25.9055244994277,-66.9574394204663,12.));
#64982=CARTESIAN_POINT('Ctrl Pts',(25.890136841266,-66.939528499934,12.));
#64983=CARTESIAN_POINT('Ctrl Pts',(25.874795026011,-66.92163531213,12.));
#64984=CARTESIAN_POINT('Ctrl Pts',(25.8594990868833,-66.9037599932761,12.));
#64985=CARTESIAN_POINT('Ctrl Pts',(25.844249057147,-66.8859026802088,12.));
#64986=CARTESIAN_POINT('Ctrl Pts',(25.8290449701192,-66.8680635103876,12.));
#64987=CARTESIAN_POINT('Ctrl Pts',(25.8138868591709,-66.8502426219001,12.));
#64988=CARTESIAN_POINT('Ctrl Pts',(25.7987747577269,-66.8324401534668,12.));
#64989=CARTESIAN_POINT('Ctrl Pts',(25.7837086992594,-66.8146562444433,12.));
#64990=CARTESIAN_POINT('Ctrl Pts',(25.7686887172877,-66.7968910348245,12.));
#64991=CARTESIAN_POINT('Ctrl Pts',(25.7537148453863,-66.7791446652545,12.));
#64992=CARTESIAN_POINT('Ctrl Pts',(25.7387871171866,-66.7614172770316,12.));
#64993=CARTESIAN_POINT('Ctrl Pts',(25.7239055663772,-66.7437090121153,12.));
#64994=CARTESIAN_POINT('Ctrl Pts',(25.7090702266962,-66.7260200131266,12.));
#64995=CARTESIAN_POINT('Ctrl Pts',(25.6942811319322,-66.7083504233529,12.));
#64996=CARTESIAN_POINT('Ctrl Pts',(25.6795383159319,-66.6907003867572,12.));
#64997=CARTESIAN_POINT('Ctrl Pts',(25.6648418126013,-66.6730700479837,12.));
#64998=CARTESIAN_POINT('Ctrl Pts',(25.6501916559055,-66.6554595523624,12.));
#64999=CARTESIAN_POINT('Ctrl Pts',(25.6355878798613,-66.6378690459129,12.));
#65000=CARTESIAN_POINT('Ctrl Pts',(25.6210305185403,-66.6202986753507,12.));
#65001=CARTESIAN_POINT('Ctrl Pts',(25.6065196060755,-66.6027485880963,12.));
#65002=CARTESIAN_POINT('Ctrl Pts',(25.5920551766629,-66.5852189322813,12.));
#65003=CARTESIAN_POINT('Ctrl Pts',(25.5776372645601,-66.5677098567542,12.));
#65004=CARTESIAN_POINT('Ctrl Pts',(25.5632659040792,-66.5502215110829,12.));
#65005=CARTESIAN_POINT('Ctrl Pts',(25.5489411295911,-66.5327540455624,12.));
#65006=CARTESIAN_POINT('Ctrl Pts',(25.534662975532,-66.5153076112231,12.));
#65007=CARTESIAN_POINT('Ctrl Pts',(25.5204314764033,-66.4978823598354,12.));
#65008=CARTESIAN_POINT('Ctrl Pts',(25.5062466667702,-66.4804784439148,12.));
#65009=CARTESIAN_POINT('Ctrl Pts',(25.4921085812547,-66.4630960167252,12.));
#65010=CARTESIAN_POINT('Ctrl Pts',(25.4780172545417,-66.4457352322871,12.));
#65011=CARTESIAN_POINT('Ctrl Pts',(25.4639727213849,-66.4283962453899,12.));
#65012=CARTESIAN_POINT('Ctrl Pts',(25.4499750166078,-66.4110792116,12.));
#65013=CARTESIAN_POINT('Ctrl Pts',(25.4360241751017,-66.3937842872685,12.));
#65014=CARTESIAN_POINT('Ctrl Pts',(25.4221202318199,-66.3765116295365,12.));
#65015=CARTESIAN_POINT('Ctrl Pts',(25.4082632217847,-66.359261396341,12.));
#65016=CARTESIAN_POINT('Ctrl Pts',(25.3944531800901,-66.3420337464178,12.));
#65017=CARTESIAN_POINT('Ctrl Pts',(25.3806901419012,-66.3248288393046,12.));
#65018=CARTESIAN_POINT('Ctrl Pts',(25.3669741424488,-66.3076468353413,12.));
#65019=CARTESIAN_POINT('Ctrl Pts',(25.3533052170248,-66.290487895671,12.));
#65020=CARTESIAN_POINT('Ctrl Pts',(25.3396834009949,-66.2733521822662,12.));
#65021=CARTESIAN_POINT('Ctrl Pts',(25.3261087298026,-66.2562398579471,12.));
#65022=CARTESIAN_POINT('Ctrl Pts',(25.3125812389729,-66.2391510863998,12.));
#65023=CARTESIAN_POINT('Ctrl Pts',(25.2991009641094,-66.2220860321952,12.));
#65024=CARTESIAN_POINT('Ctrl Pts',(25.285667940893,-66.2050448607911,12.));
#65025=CARTESIAN_POINT('Ctrl Pts',(25.2722822050836,-66.1880277385136,12.));
#65026=CARTESIAN_POINT('Ctrl Pts',(25.2589437925146,-66.1710348325384,12.));
#65027=CARTESIAN_POINT('Ctrl Pts',(25.2456527390874,-66.1540663108754,12.));
#65028=CARTESIAN_POINT('Ctrl Pts',(25.2324090807549,-66.1371223423345,12.));
#65029=CARTESIAN_POINT('Ctrl Pts',(25.2192128535357,-66.1202030965759,12.));
#65030=CARTESIAN_POINT('Ctrl Pts',(25.2060640935365,-66.10330874419,12.));
#65031=CARTESIAN_POINT('Ctrl Pts',(25.1929628369684,-66.086439456768,12.));
#65032=CARTESIAN_POINT('Ctrl Pts',(25.1799091201599,-66.0695954069713,12.));
#65033=CARTESIAN_POINT('Ctrl Pts',(25.166902979566,-66.0527767686025,12.));
#65034=CARTESIAN_POINT('Ctrl Pts',(25.1539444517418,-66.0359837164734,12.));
#65035=CARTESIAN_POINT('Ctrl Pts',(25.1410335733098,-66.0192164262621,12.));
#65036=CARTESIAN_POINT('Ctrl Pts',(25.1281703809297,-66.0024750743897,12.));
#65037=CARTESIAN_POINT('Ctrl Pts',(25.1153549112503,-65.9857598378433,12.));
#65038=CARTESIAN_POINT('Ctrl Pts',(25.1025872009003,-65.9690708941558,12.));
#65039=CARTESIAN_POINT('Ctrl Pts',(25.0898672865915,-65.952408421814,12.));
#65040=CARTESIAN_POINT('Ctrl Pts',(25.0771952052028,-65.9357726006163,12.));
#65041=CARTESIAN_POINT('Ctrl Pts',(25.0645709938524,-65.919163611981,12.));
#65042=CARTESIAN_POINT('Ctrl Pts',(25.0519946900078,-65.9025816394424,12.));
#65043=CARTESIAN_POINT('Ctrl Pts',(25.0394663314055,-65.8860268683128,12.));
#65044=CARTESIAN_POINT('Ctrl Pts',(25.0269859558362,-65.8694994847617,12.));
#65045=CARTESIAN_POINT('Ctrl Pts',(25.0145536009604,-65.8529996750445,12.));
#65046=CARTESIAN_POINT('Ctrl Pts',(25.0021693041169,-65.8365276247128,12.));
#65047=CARTESIAN_POINT('Ctrl Pts',(24.9898331020983,-65.8200835177024,12.));
#65048=CARTESIAN_POINT('Ctrl Pts',(24.9775450315682,-65.8036675380718,12.));
#65049=CARTESIAN_POINT('Ctrl Pts',(24.965305129558,-65.7872798720823,12.));
#65050=CARTESIAN_POINT('Ctrl Pts',(24.9531134338696,-65.7709207098959,12.));
#65051=CARTESIAN_POINT('Ctrl Pts',(24.9409699836537,-65.7545902480323,12.));
#65052=CARTESIAN_POINT('Ctrl Pts',(24.928874819458,-65.7382886895888,12.));
#65053=CARTESIAN_POINT('Ctrl Pts',(24.9168279820106,-65.7220162391054,12.));
#65054=CARTESIAN_POINT('Ctrl Pts',(24.9048295111448,-65.7057730980483,12.));
#65055=CARTESIAN_POINT('Ctrl Pts',(24.8928794448607,-65.6895594608776,12.));
#65056=CARTESIAN_POINT('Ctrl Pts',(24.8809778178228,-65.6733755087669,12.));
#65057=CARTESIAN_POINT('Ctrl Pts',(24.8691246628056,-65.6572214156692,12.));
#65058=CARTESIAN_POINT('Ctrl Pts',(24.8573200135665,-65.6410973603661,12.));
#65059=CARTESIAN_POINT('Ctrl Pts',(24.8455639071516,-65.6250035361612,12.));
#65060=CARTESIAN_POINT('Ctrl Pts',(24.8338563866763,-65.6089401625628,12.));
#65061=CARTESIAN_POINT('Ctrl Pts',(24.8221975032103,-65.5929074932624,12.));
#65062=CARTESIAN_POINT('Ctrl Pts',(24.8105873098626,-65.5769057914333,12.));
#65063=CARTESIAN_POINT('Ctrl Pts',(24.7990258561259,-65.5609353062829,12.));
#65064=CARTESIAN_POINT('Ctrl Pts',(24.787513182749,-65.5449962514662,12.));
#65065=CARTESIAN_POINT('Ctrl Pts',(24.7760493148465,-65.5290887770232,12.));
#65066=CARTESIAN_POINT('Ctrl Pts',(24.7646342620841,-65.5132129675333,12.));
#65067=CARTESIAN_POINT('Ctrl Pts',(24.7555412724651,-65.5005376841101,12.));
#65068=CARTESIAN_POINT('Ctrl Pts',(24.7487434955981,-65.4910454936254,12.));
#65069=CARTESIAN_POINT('Ctrl Pts',(24.7442214063382,-65.4847237095443,12.));
#65070=CARTESIAN_POINT('Ctrl Pts',(24.7419628022041,-65.4815644032299,12.));
#65071=CARTESIAN_POINT('Ctrl Pts',(29.0944526440265,-68.2622612910179,-1.11022302462516E-15));
#65072=CARTESIAN_POINT('Ctrl Pts',(29.0944526440265,-68.2622612910179,4.));
#65073=CARTESIAN_POINT('Ctrl Pts',(29.0944526440265,-68.2622612910179,8.));
#65074=CARTESIAN_POINT('Ctrl Pts',(29.0944526440265,-68.2622612910179,12.));
#65075=CARTESIAN_POINT('Ctrl Pts',(29.0922231502662,-68.3721211369509,-1.11022302462516E-15));
#65076=CARTESIAN_POINT('Ctrl Pts',(29.0922231502662,-68.3721211369509,4.));
#65077=CARTESIAN_POINT('Ctrl Pts',(29.0922231502662,-68.3721211369509,8.));
#65078=CARTESIAN_POINT('Ctrl Pts',(29.0922231502662,-68.3721211369509,12.));
#65079=CARTESIAN_POINT('Ctrl Pts',(29.0225207419379,-68.5624216146674,-1.11022302462516E-15));
#65080=CARTESIAN_POINT('Ctrl Pts',(29.0225207419379,-68.5624216146674,4.00000000000001));
#65081=CARTESIAN_POINT('Ctrl Pts',(29.0225207419379,-68.5624216146674,7.99999999999999));
#65082=CARTESIAN_POINT('Ctrl Pts',(29.0225207419379,-68.5624216146674,12.));
#65083=CARTESIAN_POINT('Ctrl Pts',(28.8637726134454,-68.6814343344129,-1.11022302462516E-15));
#65084=CARTESIAN_POINT('Ctrl Pts',(28.8637726134454,-68.6814343344129,4.));
#65085=CARTESIAN_POINT('Ctrl Pts',(28.8637726134454,-68.6814343344129,8.00000000000001));
#65086=CARTESIAN_POINT('Ctrl Pts',(28.8637726134454,-68.6814343344129,12.));
#65087=CARTESIAN_POINT('Ctrl Pts',(28.7877620302417,-68.7132793373315,-1.11022302462516E-15));
#65088=CARTESIAN_POINT('Ctrl Pts',(28.7877620302417,-68.7132793373315,4.));
#65089=CARTESIAN_POINT('Ctrl Pts',(28.7877620302417,-68.7132793373315,8.));
#65090=CARTESIAN_POINT('Ctrl Pts',(28.7877620302417,-68.7132793373315,12.));
#65091=CARTESIAN_POINT('',(29.0944526440265,-68.2622612910179,0.));
#65092=CARTESIAN_POINT('',(28.7877620302418,-68.7132793373317,0.));
#65093=CARTESIAN_POINT('Ctrl Pts',(29.0944526440265,-68.2622612910179,0.));
#65094=CARTESIAN_POINT('Ctrl Pts',(29.0922231502662,-68.3721211369509,-7.70371977754894E-31));
#65095=CARTESIAN_POINT('Ctrl Pts',(29.05239320265,-68.4808642670746,6.16297582203915E-31));
#65096=CARTESIAN_POINT('Ctrl Pts',(28.9834871015109,-68.5663297619425,3.08148791101958E-31));
#65097=CARTESIAN_POINT('Ctrl Pts',(28.9318075256565,-68.6304288830934,-6.16297582203912E-32));
#65098=CARTESIAN_POINT('Ctrl Pts',(28.8637726134454,-68.6814343344129,-1.4482993181792E-30));
#65099=CARTESIAN_POINT('Ctrl Pts',(28.7877620302417,-68.7132793373315,-6.16297582203914E-32));
#65100=CARTESIAN_POINT('',(28.7877620302418,-68.7132793373317,12.));
#65101=CARTESIAN_POINT('Ctrl Pts',(28.7877620302417,-68.7132793373315,-1.11022302462516E-15));
#65102=CARTESIAN_POINT('Ctrl Pts',(28.7877620302417,-68.7132793373315,4.));
#65103=CARTESIAN_POINT('Ctrl Pts',(28.7877620302417,-68.7132793373315,8.));
#65104=CARTESIAN_POINT('Ctrl Pts',(28.7877620302417,-68.7132793373315,12.));
#65105=CARTESIAN_POINT('',(29.0944526440265,-68.2622612910179,12.));
#65106=CARTESIAN_POINT('Ctrl Pts',(28.7877620302417,-68.7132793373315,12.));
#65107=CARTESIAN_POINT('Ctrl Pts',(28.8637726134454,-68.6814343344129,12.));
#65108=CARTESIAN_POINT('Ctrl Pts',(28.9318075256565,-68.6304288830934,12.));
#65109=CARTESIAN_POINT('Ctrl Pts',(28.9834871015109,-68.5663297619425,12.));
#65110=CARTESIAN_POINT('Ctrl Pts',(29.05239320265,-68.4808642670746,12.));
#65111=CARTESIAN_POINT('Ctrl Pts',(29.0922231502662,-68.3721211369509,12.));
#65112=CARTESIAN_POINT('Ctrl Pts',(29.0944526440265,-68.2622612910179,12.));
#65113=CARTESIAN_POINT('Ctrl Pts',(29.0944526440265,-68.2622612910179,12.));
#65114=CARTESIAN_POINT('Ctrl Pts',(29.0944526440265,-68.2622612910179,8.));
#65115=CARTESIAN_POINT('Ctrl Pts',(29.0944526440265,-68.2622612910179,4.));
#65116=CARTESIAN_POINT('Ctrl Pts',(29.0944526440265,-68.2622612910179,-1.11022302462516E-15));
#65117=CARTESIAN_POINT('Origin',(1.43538201480493E-10,-3.46272497684358E-10,
0.));
#65118=CARTESIAN_POINT('Origin',(1.43538201480493E-10,-3.46272497684358E-10,
12.));
#65119=CARTESIAN_POINT('Origin',(1.43538201480493E-10,-3.46272497684358E-10,
0.));
#65120=CARTESIAN_POINT('Ctrl Pts',(22.1153394458716,-71.1418425484881,0.));
#65121=CARTESIAN_POINT('Ctrl Pts',(22.1153394458716,-71.1418425484881,4.));
#65122=CARTESIAN_POINT('Ctrl Pts',(22.1153394458716,-71.1418425484881,8.));
#65123=CARTESIAN_POINT('Ctrl Pts',(22.1153394458716,-71.1418425484881,12.));
#65124=CARTESIAN_POINT('Ctrl Pts',(22.0104100349462,-71.1744611799059,0.));
#65125=CARTESIAN_POINT('Ctrl Pts',(22.0104100349462,-71.1744611799059,4.));
#65126=CARTESIAN_POINT('Ctrl Pts',(22.0104100349461,-71.1744611799059,8.));
#65127=CARTESIAN_POINT('Ctrl Pts',(22.0104100349461,-71.1744611799059,12.));
#65128=CARTESIAN_POINT('Ctrl Pts',(21.807833456103,-71.168501135194,-7.30818592425997E-17));
#65129=CARTESIAN_POINT('Ctrl Pts',(21.807833456103,-71.168501135194,4.00000000000001));
#65130=CARTESIAN_POINT('Ctrl Pts',(21.807833456103,-71.168501135194,7.99999999999999));
#65131=CARTESIAN_POINT('Ctrl Pts',(21.807833456103,-71.168501135194,12.));
#65132=CARTESIAN_POINT('Ctrl Pts',(21.6447353227843,-71.0555229320376,-2.46611180232746E-16));
#65133=CARTESIAN_POINT('Ctrl Pts',(21.6447353227843,-71.0555229320376,3.99999999999999));
#65134=CARTESIAN_POINT('Ctrl Pts',(21.6447353227843,-71.0555229320376,8.00000000000001));
#65135=CARTESIAN_POINT('Ctrl Pts',(21.6447353227843,-71.0555229320376,12.));
#65136=CARTESIAN_POINT('Ctrl Pts',(21.5904919934803,-70.9934796068775,-3.30265160470244E-16));
#65137=CARTESIAN_POINT('Ctrl Pts',(21.5904919934803,-70.9934796068775,4.));
#65138=CARTESIAN_POINT('Ctrl Pts',(21.5904919934803,-70.9934796068775,8.));
#65139=CARTESIAN_POINT('Ctrl Pts',(21.5904919934803,-70.9934796068775,12.));
#65140=CARTESIAN_POINT('',(22.1153394458716,-71.1418425484881,0.));
#65141=CARTESIAN_POINT('',(21.59049199348,-70.9934796068777,0.));
#65142=CARTESIAN_POINT('Ctrl Pts',(22.1153394458716,-71.1418425484881,2.74425517504379E-17));
#65143=CARTESIAN_POINT('Ctrl Pts',(22.0104100349462,-71.1744611799059,2.74425517504379E-17));
#65144=CARTESIAN_POINT('Ctrl Pts',(21.8946519898929,-71.1710554400705,-1.43185106739048E-17));
#65145=CARTESIAN_POINT('Ctrl Pts',(21.7917848658273,-71.1327049954369,-8.88787442811197E-17));
#65146=CARTESIAN_POINT('Ctrl Pts',(21.7146345227781,-71.1039421619618,-1.44798919486531E-16));
#65147=CARTESIAN_POINT('Ctrl Pts',(21.6447353227843,-71.0555229320376,-2.19168628482308E-16));
#65148=CARTESIAN_POINT('Ctrl Pts',(21.5904919934803,-70.9934796068775,-3.02822608719806E-16));
#65149=CARTESIAN_POINT('',(21.59049199348,-70.9934796068777,12.));
#65150=CARTESIAN_POINT('Ctrl Pts',(21.5904919934803,-70.9934796068775,-3.30265160470244E-16));
#65151=CARTESIAN_POINT('Ctrl Pts',(21.5904919934803,-70.9934796068775,4.));
#65152=CARTESIAN_POINT('Ctrl Pts',(21.5904919934803,-70.9934796068775,8.));
#65153=CARTESIAN_POINT('Ctrl Pts',(21.5904919934803,-70.9934796068775,12.));
#65154=CARTESIAN_POINT('',(22.1153394458716,-71.1418425484881,12.));
#65155=CARTESIAN_POINT('Ctrl Pts',(21.5904919934803,-70.9934796068775,12.));
#65156=CARTESIAN_POINT('Ctrl Pts',(21.6447353227843,-71.0555229320376,12.));
#65157=CARTESIAN_POINT('Ctrl Pts',(21.714634522778,-71.1039421619618,12.));
#65158=CARTESIAN_POINT('Ctrl Pts',(21.7917848658272,-71.132704995437,12.));
#65159=CARTESIAN_POINT('Ctrl Pts',(21.8946519898929,-71.1710554400705,12.));
#65160=CARTESIAN_POINT('Ctrl Pts',(22.0104100349461,-71.1744611799059,12.));
#65161=CARTESIAN_POINT('Ctrl Pts',(22.1153394458716,-71.1418425484881,12.));
#65162=CARTESIAN_POINT('Ctrl Pts',(22.1153394458716,-71.1418425484881,12.));
#65163=CARTESIAN_POINT('Ctrl Pts',(22.1153394458716,-71.1418425484881,8.));
#65164=CARTESIAN_POINT('Ctrl Pts',(22.1153394458716,-71.1418425484881,4.));
#65165=CARTESIAN_POINT('Ctrl Pts',(22.1153394458716,-71.1418425484881,0.));
#65166=CARTESIAN_POINT('Ctrl Pts',(18.9407177820968,-67.3887914263118,0.));
#65167=CARTESIAN_POINT('Ctrl Pts',(18.9407177820968,-67.3887914263118,12.));
#65168=CARTESIAN_POINT('Ctrl Pts',(18.9426924398719,-67.3921355608328,0.));
#65169=CARTESIAN_POINT('Ctrl Pts',(18.9426924398719,-67.3921355608328,12.));
#65170=CARTESIAN_POINT('Ctrl Pts',(18.9466463414299,-67.3988274146651,0.));
#65171=CARTESIAN_POINT('Ctrl Pts',(18.9466463414299,-67.3988274146651,12.));
#65172=CARTESIAN_POINT('Ctrl Pts',(18.9525909517915,-67.4088759497911,0.));
#65173=CARTESIAN_POINT('Ctrl Pts',(18.9525909517915,-67.4088759497911,12.));
#65174=CARTESIAN_POINT('Ctrl Pts',(18.9605446160985,-67.4222955061981,0.));
#65175=CARTESIAN_POINT('Ctrl Pts',(18.9605446160985,-67.4222955061981,12.));
#65176=CARTESIAN_POINT('Ctrl Pts',(18.970532563171,-67.4391057908418,0.));
#65177=CARTESIAN_POINT('Ctrl Pts',(18.970532563171,-67.4391057908418,12.));
#65178=CARTESIAN_POINT('Ctrl Pts',(18.9805663798448,-67.4559518744638,0.));
#65179=CARTESIAN_POINT('Ctrl Pts',(18.9805663798448,-67.4559518744638,12.));
#65180=CARTESIAN_POINT('Ctrl Pts',(18.9906460638625,-67.472833671964,0.));
#65181=CARTESIAN_POINT('Ctrl Pts',(18.9906460638625,-67.472833671964,12.));
#65182=CARTESIAN_POINT('Ctrl Pts',(19.0007716032819,-67.4897510316844,0.));
#65183=CARTESIAN_POINT('Ctrl Pts',(19.0007716032819,-67.4897510316844,12.));
#65184=CARTESIAN_POINT('Ctrl Pts',(19.0109429761306,-67.5067037372317,0.));
#65185=CARTESIAN_POINT('Ctrl Pts',(19.0109429761306,-67.5067037372317,12.));
#65186=CARTESIAN_POINT('Ctrl Pts',(19.021160154824,-67.5236915360331,0.));
#65187=CARTESIAN_POINT('Ctrl Pts',(19.021160154824,-67.5236915360331,12.));
#65188=CARTESIAN_POINT('Ctrl Pts',(19.0314231093923,-67.540714161288,0.));
#65189=CARTESIAN_POINT('Ctrl Pts',(19.0314231093923,-67.540714161288,12.));
#65190=CARTESIAN_POINT('Ctrl Pts',(19.0417318110708,-67.5577713558194,0.));
#65191=CARTESIAN_POINT('Ctrl Pts',(19.0417318110708,-67.5577713558194,12.));
#65192=CARTESIAN_POINT('Ctrl Pts',(19.0520862360395,-67.5748628971964,0.));
#65193=CARTESIAN_POINT('Ctrl Pts',(19.0520862360395,-67.5748628971964,12.));
#65194=CARTESIAN_POINT('Ctrl Pts',(19.062486364241,-67.5919885896222,0.));
#65195=CARTESIAN_POINT('Ctrl Pts',(19.062486364241,-67.5919885896222,12.));
#65196=CARTESIAN_POINT('Ctrl Pts',(19.072932177628,-67.6091482520534,0.));
#65197=CARTESIAN_POINT('Ctrl Pts',(19.072932177628,-67.6091482520534,12.));
#65198=CARTESIAN_POINT('Ctrl Pts',(19.0834236587118,-67.6263417083426,0.));
#65199=CARTESIAN_POINT('Ctrl Pts',(19.0834236587118,-67.6263417083426,12.));
#65200=CARTESIAN_POINT('Ctrl Pts',(19.0939607887501,-67.6435687749841,0.));
#65201=CARTESIAN_POINT('Ctrl Pts',(19.0939607887501,-67.6435687749841,12.));
#65202=CARTESIAN_POINT('Ctrl Pts',(19.1045435468358,-67.6608292549462,0.));
#65203=CARTESIAN_POINT('Ctrl Pts',(19.1045435468358,-67.6608292549462,12.));
#65204=CARTESIAN_POINT('Ctrl Pts',(19.115171910846,-67.6781229440573,0.));
#65205=CARTESIAN_POINT('Ctrl Pts',(19.115171910846,-67.6781229440573,12.));
#65206=CARTESIAN_POINT('Ctrl Pts',(19.1258458580345,-67.6954496350063,0.));
#65207=CARTESIAN_POINT('Ctrl Pts',(19.1258458580345,-67.6954496350063,12.));
#65208=CARTESIAN_POINT('Ctrl Pts',(19.136565365709,-67.7128091219348,0.));
#65209=CARTESIAN_POINT('Ctrl Pts',(19.136565365709,-67.7128091219348,12.));
#65210=CARTESIAN_POINT('Ctrl Pts',(19.1473304119955,-67.7302012056584,0.));
#65211=CARTESIAN_POINT('Ctrl Pts',(19.1473304119955,-67.7302012056584,12.));
#65212=CARTESIAN_POINT('Ctrl Pts',(19.1581409758097,-67.7476256934444,0.));
#65213=CARTESIAN_POINT('Ctrl Pts',(19.1581409758097,-67.7476256934444,12.));
#65214=CARTESIAN_POINT('Ctrl Pts',(19.1689970364949,-67.7650823965127,0.));
#65215=CARTESIAN_POINT('Ctrl Pts',(19.1689970364949,-67.7650823965127,12.));
#65216=CARTESIAN_POINT('Ctrl Pts',(19.1798985735687,-67.7825711283096,0.));
#65217=CARTESIAN_POINT('Ctrl Pts',(19.1798985735687,-67.7825711283096,12.));
#65218=CARTESIAN_POINT('Ctrl Pts',(19.1908455664097,-67.8000917023926,0.));
#65219=CARTESIAN_POINT('Ctrl Pts',(19.1908455664097,-67.8000917023926,12.));
#65220=CARTESIAN_POINT('Ctrl Pts',(19.201837993993,-67.8176439306621,0.));
#65221=CARTESIAN_POINT('Ctrl Pts',(19.201837993993,-67.8176439306621,12.));
#65222=CARTESIAN_POINT('Ctrl Pts',(19.2128758350345,-67.835227624289,0.));
#65223=CARTESIAN_POINT('Ctrl Pts',(19.2128758350345,-67.835227624289,12.));
#65224=CARTESIAN_POINT('Ctrl Pts',(19.2239590681133,-67.8528425945184,0.));
#65225=CARTESIAN_POINT('Ctrl Pts',(19.2239590681133,-67.8528425945184,12.));
#65226=CARTESIAN_POINT('Ctrl Pts',(19.2350876717874,-67.8704886534544,0.));
#65227=CARTESIAN_POINT('Ctrl Pts',(19.2350876717874,-67.8704886534544,12.));
#65228=CARTESIAN_POINT('Ctrl Pts',(19.2462616247279,-67.8881656149955,0.));
#65229=CARTESIAN_POINT('Ctrl Pts',(19.2462616247279,-67.8881656149955,12.));
#65230=CARTESIAN_POINT('Ctrl Pts',(19.2574809057696,-67.9058732951788,0.));
#65231=CARTESIAN_POINT('Ctrl Pts',(19.2574809057696,-67.9058732951788,12.));
#65232=CARTESIAN_POINT('Ctrl Pts',(19.2687454938442,-67.9236115116758,0.));
#65233=CARTESIAN_POINT('Ctrl Pts',(19.2687454938442,-67.9236115116758,12.));
#65234=CARTESIAN_POINT('Ctrl Pts',(19.280055367936,-67.9413800834793,0.));
#65235=CARTESIAN_POINT('Ctrl Pts',(19.280055367936,-67.9413800834793,12.));
#65236=CARTESIAN_POINT('Ctrl Pts',(19.2914105070286,-67.9591788305394,0.));
#65237=CARTESIAN_POINT('Ctrl Pts',(19.2914105070286,-67.9591788305394,12.));
#65238=CARTESIAN_POINT('Ctrl Pts',(19.302810890038,-67.9770075733485,0.));
#65239=CARTESIAN_POINT('Ctrl Pts',(19.302810890038,-67.9770075733485,12.));
#65240=CARTESIAN_POINT('Ctrl Pts',(19.3142564958202,-67.9948661329617,0.));
#65241=CARTESIAN_POINT('Ctrl Pts',(19.3142564958202,-67.9948661329617,12.));
#65242=CARTESIAN_POINT('Ctrl Pts',(19.3257473032034,-68.0127543311776,0.));
#65243=CARTESIAN_POINT('Ctrl Pts',(19.3257473032034,-68.0127543311776,12.));
#65244=CARTESIAN_POINT('Ctrl Pts',(19.3372832910076,-68.0306719906636,0.));
#65245=CARTESIAN_POINT('Ctrl Pts',(19.3372832910076,-68.0306719906636,12.));
#65246=CARTESIAN_POINT('Ctrl Pts',(19.3488644380641,-68.0486189351011,0.));
#65247=CARTESIAN_POINT('Ctrl Pts',(19.3488644380641,-68.0486189351011,12.));
#65248=CARTESIAN_POINT('Ctrl Pts',(19.3604907232313,-68.0665949893195,0.));
#65249=CARTESIAN_POINT('Ctrl Pts',(19.3604907232313,-68.0665949893195,12.));
#65250=CARTESIAN_POINT('Ctrl Pts',(19.3721621253912,-68.0845999792247,0.));
#65251=CARTESIAN_POINT('Ctrl Pts',(19.3721621253912,-68.0845999792247,12.));
#65252=CARTESIAN_POINT('Ctrl Pts',(19.3838786234421,-68.1026337317285,0.));
#65253=CARTESIAN_POINT('Ctrl Pts',(19.3838786234421,-68.1026337317285,12.));
#65254=CARTESIAN_POINT('Ctrl Pts',(19.3956401962894,-68.1206960746769,0.));
#65255=CARTESIAN_POINT('Ctrl Pts',(19.3956401962894,-68.1206960746769,12.));
#65256=CARTESIAN_POINT('Ctrl Pts',(19.4074468228299,-68.1387868367691,0.));
#65257=CARTESIAN_POINT('Ctrl Pts',(19.4074468228299,-68.1387868367691,12.));
#65258=CARTESIAN_POINT('Ctrl Pts',(19.4192984819418,-68.1569058475054,0.));
#65259=CARTESIAN_POINT('Ctrl Pts',(19.4192984819418,-68.1569058475054,12.));
#65260=CARTESIAN_POINT('Ctrl Pts',(19.4311951524983,-68.1750529372232,0.));
#65261=CARTESIAN_POINT('Ctrl Pts',(19.4311951524983,-68.1750529372232,12.));
#65262=CARTESIAN_POINT('Ctrl Pts',(19.4431368133719,-68.1932279371127,0.));
#65263=CARTESIAN_POINT('Ctrl Pts',(19.4431368133719,-68.1932279371127,12.));
#65264=CARTESIAN_POINT('Ctrl Pts',(19.455123443438,-68.2114306792358,0.));
#65265=CARTESIAN_POINT('Ctrl Pts',(19.455123443438,-68.2114306792358,12.));
#65266=CARTESIAN_POINT('Ctrl Pts',(19.467155021572,-68.2296609965448,0.));
#65267=CARTESIAN_POINT('Ctrl Pts',(19.467155021572,-68.2296609965448,12.));
#65268=CARTESIAN_POINT('Ctrl Pts',(19.4792315266501,-68.2479187228803,0.));
#65269=CARTESIAN_POINT('Ctrl Pts',(19.4792315266501,-68.2479187228803,12.));
#65270=CARTESIAN_POINT('Ctrl Pts',(19.4913529375543,-68.2662036929526,0.));
#65271=CARTESIAN_POINT('Ctrl Pts',(19.4913529375543,-68.2662036929526,12.));
#65272=CARTESIAN_POINT('Ctrl Pts',(19.5035192331705,-68.2845157423233,0.));
#65273=CARTESIAN_POINT('Ctrl Pts',(19.5035192331705,-68.2845157423233,12.));
#65274=CARTESIAN_POINT('Ctrl Pts',(19.5157303923856,-68.3028547073865,0.));
#65275=CARTESIAN_POINT('Ctrl Pts',(19.5157303923856,-68.3028547073865,12.));
#65276=CARTESIAN_POINT('Ctrl Pts',(19.5279863940773,-68.3212204253417,0.));
#65277=CARTESIAN_POINT('Ctrl Pts',(19.5279863940773,-68.3212204253417,12.));
#65278=CARTESIAN_POINT('Ctrl Pts',(19.540287217119,-68.3396127341938,0.));
#65279=CARTESIAN_POINT('Ctrl Pts',(19.540287217119,-68.3396127341938,12.));
#65280=CARTESIAN_POINT('Ctrl Pts',(19.5526328403852,-68.3580314727523,0.));
#65281=CARTESIAN_POINT('Ctrl Pts',(19.5526328403852,-68.3580314727523,12.));
#65282=CARTESIAN_POINT('Ctrl Pts',(19.5650232427515,-68.3764764806287,0.));
#65283=CARTESIAN_POINT('Ctrl Pts',(19.5650232427515,-68.3764764806287,12.));
#65284=CARTESIAN_POINT('Ctrl Pts',(19.5774584030937,-68.3949475982335,0.));
#65285=CARTESIAN_POINT('Ctrl Pts',(19.5774584030937,-68.3949475982335,12.));
#65286=CARTESIAN_POINT('Ctrl Pts',(19.5899383002802,-68.4134446667696,0.));
#65287=CARTESIAN_POINT('Ctrl Pts',(19.5899383002802,-68.4134446667696,12.));
#65288=CARTESIAN_POINT('Ctrl Pts',(19.6024629131784,-68.4319675282275,0.));
#65289=CARTESIAN_POINT('Ctrl Pts',(19.6024629131784,-68.4319675282275,12.));
#65290=CARTESIAN_POINT('Ctrl Pts',(19.6150322206577,-68.4505160253778,0.));
#65291=CARTESIAN_POINT('Ctrl Pts',(19.6150322206577,-68.4505160253778,12.));
#65292=CARTESIAN_POINT('Ctrl Pts',(19.6276462015888,-68.4690900017632,0.));
#65293=CARTESIAN_POINT('Ctrl Pts',(19.6276462015888,-68.4690900017632,12.));
#65294=CARTESIAN_POINT('Ctrl Pts',(19.6403048348395,-68.4876893016856,0.));
#65295=CARTESIAN_POINT('Ctrl Pts',(19.6403048348395,-68.4876893016856,12.));
#65296=CARTESIAN_POINT('Ctrl Pts',(19.6530080992686,-68.5063137701971,0.));
#65297=CARTESIAN_POINT('Ctrl Pts',(19.6530080992686,-68.5063137701971,12.));
#65298=CARTESIAN_POINT('Ctrl Pts',(19.6657559737336,-68.5249632530979,0.));
#65299=CARTESIAN_POINT('Ctrl Pts',(19.6657559737336,-68.5249632530979,12.));
#65300=CARTESIAN_POINT('Ctrl Pts',(19.6785484370926,-68.5436375969311,0.));
#65301=CARTESIAN_POINT('Ctrl Pts',(19.6785484370926,-68.5436375969311,12.));
#65302=CARTESIAN_POINT('Ctrl Pts',(19.6913854682046,-68.5623366489779,0.));
#65303=CARTESIAN_POINT('Ctrl Pts',(19.6913854682046,-68.5623366489779,12.));
#65304=CARTESIAN_POINT('Ctrl Pts',(19.7042670459237,-68.581060257249,0.));
#65305=CARTESIAN_POINT('Ctrl Pts',(19.7042670459237,-68.581060257249,12.));
#65306=CARTESIAN_POINT('Ctrl Pts',(19.7171931490956,-68.5998082704766,0.));
#65307=CARTESIAN_POINT('Ctrl Pts',(19.7171931490956,-68.5998082704766,12.));
#65308=CARTESIAN_POINT('Ctrl Pts',(19.7301637565652,-68.6185805381126,0.));
#65309=CARTESIAN_POINT('Ctrl Pts',(19.7301637565652,-68.6185805381126,12.));
#65310=CARTESIAN_POINT('Ctrl Pts',(19.7431788471775,-68.6373769103224,0.));
#65311=CARTESIAN_POINT('Ctrl Pts',(19.7431788471775,-68.6373769103224,12.));
#65312=CARTESIAN_POINT('Ctrl Pts',(19.7562383997781,-68.6561972379793,0.));
#65313=CARTESIAN_POINT('Ctrl Pts',(19.7562383997781,-68.6561972379793,12.));
#65314=CARTESIAN_POINT('Ctrl Pts',(19.7693423932058,-68.6750413726547,0.));
#65315=CARTESIAN_POINT('Ctrl Pts',(19.7693423932058,-68.6750413726547,12.));
#65316=CARTESIAN_POINT('Ctrl Pts',(19.7824908062913,-68.6939091666111,0.));
#65317=CARTESIAN_POINT('Ctrl Pts',(19.7824908062913,-68.6939091666111,12.));
#65318=CARTESIAN_POINT('Ctrl Pts',(19.795683617864,-68.7128004727998,0.));
#65319=CARTESIAN_POINT('Ctrl Pts',(19.795683617864,-68.7128004727998,12.));
#65320=CARTESIAN_POINT('Ctrl Pts',(19.8089208067532,-68.7317151448557,0.));
#65321=CARTESIAN_POINT('Ctrl Pts',(19.8089208067532,-68.7317151448557,12.));
#65322=CARTESIAN_POINT('Ctrl Pts',(19.8222023517874,-68.7506530370918,0.));
#65323=CARTESIAN_POINT('Ctrl Pts',(19.8222023517874,-68.7506530370918,12.));
#65324=CARTESIAN_POINT('Ctrl Pts',(19.835528231787,-68.7696140044892,0.));
#65325=CARTESIAN_POINT('Ctrl Pts',(19.835528231787,-68.7696140044892,12.));
#65326=CARTESIAN_POINT('Ctrl Pts',(19.8488984255641,-68.7885979026927,0.));
#65327=CARTESIAN_POINT('Ctrl Pts',(19.8488984255641,-68.7885979026927,12.));
#65328=CARTESIAN_POINT('Ctrl Pts',(19.8623129119304,-68.8076045880102,0.));
#65329=CARTESIAN_POINT('Ctrl Pts',(19.8623129119304,-68.8076045880102,12.));
#65330=CARTESIAN_POINT('Ctrl Pts',(19.8757716696968,-68.8266339174068,0.));
#65331=CARTESIAN_POINT('Ctrl Pts',(19.8757716696968,-68.8266339174068,12.));
#65332=CARTESIAN_POINT('Ctrl Pts',(19.8892746776733,-68.8456857484988,0.));
#65333=CARTESIAN_POINT('Ctrl Pts',(19.8892746776733,-68.8456857484988,12.));
#65334=CARTESIAN_POINT('Ctrl Pts',(19.9028219146606,-68.8647599395437,0.));
#65335=CARTESIAN_POINT('Ctrl Pts',(19.9028219146606,-68.8647599395437,12.));
#65336=CARTESIAN_POINT('Ctrl Pts',(19.9164133594512,-68.8838563494356,0.));
#65337=CARTESIAN_POINT('Ctrl Pts',(19.9164133594512,-68.8838563494356,12.));
#65338=CARTESIAN_POINT('Ctrl Pts',(19.9300489908364,-68.902974837704,0.));
#65339=CARTESIAN_POINT('Ctrl Pts',(19.9300489908364,-68.902974837704,12.));
#65340=CARTESIAN_POINT('Ctrl Pts',(19.9437287876063,-68.9221152645086,0.));
#65341=CARTESIAN_POINT('Ctrl Pts',(19.9437287876063,-68.9221152645086,12.));
#65342=CARTESIAN_POINT('Ctrl Pts',(19.9574527285492,-68.9412774906346,0.));
#65343=CARTESIAN_POINT('Ctrl Pts',(19.9574527285492,-68.9412774906346,12.));
#65344=CARTESIAN_POINT('Ctrl Pts',(19.9712207924436,-68.960461377483,0.));
#65345=CARTESIAN_POINT('Ctrl Pts',(19.9712207924436,-68.960461377483,12.));
#65346=CARTESIAN_POINT('Ctrl Pts',(19.9850329580599,-68.9796667870667,0.));
#65347=CARTESIAN_POINT('Ctrl Pts',(19.9850329580599,-68.9796667870667,12.));
#65348=CARTESIAN_POINT('Ctrl Pts',(19.9988892041671,-68.9988935820101,0.));
#65349=CARTESIAN_POINT('Ctrl Pts',(19.9988892041671,-68.9988935820101,12.));
#65350=CARTESIAN_POINT('Ctrl Pts',(20.0127895095326,-69.0181416255433,0.));
#65351=CARTESIAN_POINT('Ctrl Pts',(20.0127895095326,-69.0181416255433,12.));
#65352=CARTESIAN_POINT('Ctrl Pts',(20.026733852922,-69.0374107814977,0.));
#65353=CARTESIAN_POINT('Ctrl Pts',(20.026733852922,-69.0374107814977,12.));
#65354=CARTESIAN_POINT('Ctrl Pts',(20.0407222130902,-69.0567009142968,0.));
#65355=CARTESIAN_POINT('Ctrl Pts',(20.0407222130902,-69.0567009142968,12.));
#65356=CARTESIAN_POINT('Ctrl Pts',(20.0547545687839,-69.0760118889525,0.));
#65357=CARTESIAN_POINT('Ctrl Pts',(20.0547545687839,-69.0760118889525,12.));
#65358=CARTESIAN_POINT('Ctrl Pts',(20.0688308987478,-69.0953435710634,0.));
#65359=CARTESIAN_POINT('Ctrl Pts',(20.0688308987478,-69.0953435710634,12.));
#65360=CARTESIAN_POINT('Ctrl Pts',(20.082951181725,-69.1146958268104,0.));
#65361=CARTESIAN_POINT('Ctrl Pts',(20.082951181725,-69.1146958268104,12.));
#65362=CARTESIAN_POINT('Ctrl Pts',(20.0971153964557,-69.1340685229516,0.));
#65363=CARTESIAN_POINT('Ctrl Pts',(20.0971153964557,-69.1340685229516,12.));
#65364=CARTESIAN_POINT('Ctrl Pts',(20.1113235216693,-69.1534615268153,0.));
#65365=CARTESIAN_POINT('Ctrl Pts',(20.1113235216693,-69.1534615268153,12.));
#65366=CARTESIAN_POINT('Ctrl Pts',(20.125575536087,-69.172874706296,0.));
#65367=CARTESIAN_POINT('Ctrl Pts',(20.125575536087,-69.172874706296,12.));
#65368=CARTESIAN_POINT('Ctrl Pts',(20.1398714184278,-69.1923079298534,0.));
#65369=CARTESIAN_POINT('Ctrl Pts',(20.1398714184278,-69.1923079298534,12.));
#65370=CARTESIAN_POINT('Ctrl Pts',(20.1542111474086,-69.2117610665073,0.));
#65371=CARTESIAN_POINT('Ctrl Pts',(20.1542111474086,-69.2117610665073,12.));
#65372=CARTESIAN_POINT('Ctrl Pts',(20.1685947017433,-69.2312339858337,0.));
#65373=CARTESIAN_POINT('Ctrl Pts',(20.1685947017433,-69.2312339858337,12.));
#65374=CARTESIAN_POINT('Ctrl Pts',(20.183022060135,-69.2507265579562,0.));
#65375=CARTESIAN_POINT('Ctrl Pts',(20.183022060135,-69.2507265579562,12.));
#65376=CARTESIAN_POINT('Ctrl Pts',(20.1974932012775,-69.2702386535432,0.));
#65377=CARTESIAN_POINT('Ctrl Pts',(20.1974932012775,-69.2702386535432,12.));
#65378=CARTESIAN_POINT('Ctrl Pts',(20.2120081038621,-69.2897701438066,0.));
#65379=CARTESIAN_POINT('Ctrl Pts',(20.2120081038621,-69.2897701438066,12.));
#65380=CARTESIAN_POINT('Ctrl Pts',(20.2265667465783,-69.3093209004986,0.));
#65381=CARTESIAN_POINT('Ctrl Pts',(20.2265667465783,-69.3093209004986,12.));
#65382=CARTESIAN_POINT('Ctrl Pts',(20.2411691081122,-69.3288907959065,0.));
#65383=CARTESIAN_POINT('Ctrl Pts',(20.2411691081122,-69.3288907959065,12.));
#65384=CARTESIAN_POINT('Ctrl Pts',(20.255815167139,-69.3484797028454,0.));
#65385=CARTESIAN_POINT('Ctrl Pts',(20.255815167139,-69.3484797028454,12.));
#65386=CARTESIAN_POINT('Ctrl Pts',(20.270504902324,-69.3680874946548,0.));
#65387=CARTESIAN_POINT('Ctrl Pts',(20.270504902324,-69.3680874946548,12.));
#65388=CARTESIAN_POINT('Ctrl Pts',(20.2852382923299,-69.3877140451975,0.));
#65389=CARTESIAN_POINT('Ctrl Pts',(20.2852382923299,-69.3877140451975,12.));
#65390=CARTESIAN_POINT('Ctrl Pts',(20.3000153158167,-69.4073592288562,0.));
#65391=CARTESIAN_POINT('Ctrl Pts',(20.3000153158167,-69.4073592288562,12.));
#65392=CARTESIAN_POINT('Ctrl Pts',(20.3148359514414,-69.4270229205296,0.));
#65393=CARTESIAN_POINT('Ctrl Pts',(20.3148359514414,-69.4270229205296,12.));
#65394=CARTESIAN_POINT('Ctrl Pts',(20.3297001778505,-69.4467049956257,0.));
#65395=CARTESIAN_POINT('Ctrl Pts',(20.3297001778505,-69.4467049956257,12.));
#65396=CARTESIAN_POINT('Ctrl Pts',(20.3446079736798,-69.4664053300579,0.));
#65397=CARTESIAN_POINT('Ctrl Pts',(20.3446079736798,-69.4664053300579,12.));
#65398=CARTESIAN_POINT('Ctrl Pts',(20.3595593175619,-69.4861238002433,0.));
#65399=CARTESIAN_POINT('Ctrl Pts',(20.3595593175619,-69.4861238002433,12.));
#65400=CARTESIAN_POINT('Ctrl Pts',(20.3745541881266,-69.5058602831004,0.));
#65401=CARTESIAN_POINT('Ctrl Pts',(20.3745541881266,-69.5058602831004,12.));
#65402=CARTESIAN_POINT('Ctrl Pts',(20.3895925640006,-69.5256146560444,0.));
#65403=CARTESIAN_POINT('Ctrl Pts',(20.3895925640006,-69.5256146560444,12.));
#65404=CARTESIAN_POINT('Ctrl Pts',(20.4046744238002,-69.5453867969815,0.));
#65405=CARTESIAN_POINT('Ctrl Pts',(20.4046744238002,-69.5453867969815,12.));
#65406=CARTESIAN_POINT('Ctrl Pts',(20.4197997461305,-69.565176584305,0.));
#65407=CARTESIAN_POINT('Ctrl Pts',(20.4197997461305,-69.565176584305,12.));
#65408=CARTESIAN_POINT('Ctrl Pts',(20.4349685095928,-69.5849838968944,0.));
#65409=CARTESIAN_POINT('Ctrl Pts',(20.4349685095928,-69.5849838968944,12.));
#65410=CARTESIAN_POINT('Ctrl Pts',(20.4501806927854,-69.6048086141122,0.));
#65411=CARTESIAN_POINT('Ctrl Pts',(20.4501806927854,-69.6048086141122,12.));
#65412=CARTESIAN_POINT('Ctrl Pts',(20.4654362743036,-69.6246506158009,0.));
#65413=CARTESIAN_POINT('Ctrl Pts',(20.4654362743036,-69.6246506158009,12.));
#65414=CARTESIAN_POINT('Ctrl Pts',(20.4807352327335,-69.6445097822778,0.));
#65415=CARTESIAN_POINT('Ctrl Pts',(20.4807352327335,-69.6445097822778,12.));
#65416=CARTESIAN_POINT('Ctrl Pts',(20.4960775466486,-69.6643859943291,0.));
#65417=CARTESIAN_POINT('Ctrl Pts',(20.4960775466486,-69.6643859943291,12.));
#65418=CARTESIAN_POINT('Ctrl Pts',(20.511463194618,-69.6842791332102,0.));
#65419=CARTESIAN_POINT('Ctrl Pts',(20.511463194618,-69.6842791332102,12.));
#65420=CARTESIAN_POINT('Ctrl Pts',(20.5268921552075,-69.7041890806421,0.));
#65421=CARTESIAN_POINT('Ctrl Pts',(20.5268921552075,-69.7041890806421,12.));
#65422=CARTESIAN_POINT('Ctrl Pts',(20.5423644069799,-69.7241157188086,0.));
#65423=CARTESIAN_POINT('Ctrl Pts',(20.5423644069799,-69.7241157188086,12.));
#65424=CARTESIAN_POINT('Ctrl Pts',(20.5578799284897,-69.7440589303511,0.));
#65425=CARTESIAN_POINT('Ctrl Pts',(20.5578799284897,-69.7440589303511,12.));
#65426=CARTESIAN_POINT('Ctrl Pts',(20.5734386982781,-69.7640185983641,0.));
#65427=CARTESIAN_POINT('Ctrl Pts',(20.5734386982781,-69.7640185983641,12.));
#65428=CARTESIAN_POINT('Ctrl Pts',(20.5890406948808,-69.7839946063942,0.));
#65429=CARTESIAN_POINT('Ctrl Pts',(20.5890406948808,-69.7839946063942,12.));
#65430=CARTESIAN_POINT('Ctrl Pts',(20.6046858968305,-69.8039868384382,0.));
#65431=CARTESIAN_POINT('Ctrl Pts',(20.6046858968305,-69.8039868384382,12.));
#65432=CARTESIAN_POINT('Ctrl Pts',(20.6203742826565,-69.8239951789402,0.));
#65433=CARTESIAN_POINT('Ctrl Pts',(20.6203742826565,-69.8239951789402,12.));
#65434=CARTESIAN_POINT('Ctrl Pts',(20.6361058308812,-69.8440195127874,0.));
#65435=CARTESIAN_POINT('Ctrl Pts',(20.6361058308812,-69.8440195127874,12.));
#65436=CARTESIAN_POINT('Ctrl Pts',(20.6518805200131,-69.8640597253058,0.));
#65437=CARTESIAN_POINT('Ctrl Pts',(20.6518805200131,-69.8640597253058,12.));
#65438=CARTESIAN_POINT('Ctrl Pts',(20.6676983285542,-69.884115702258,0.));
#65439=CARTESIAN_POINT('Ctrl Pts',(20.6676983285542,-69.884115702258,12.));
#65440=CARTESIAN_POINT('Ctrl Pts',(20.683559235003,-69.9041873298416,0.));
#65441=CARTESIAN_POINT('Ctrl Pts',(20.683559235003,-69.9041873298416,12.));
#65442=CARTESIAN_POINT('Ctrl Pts',(20.6994632178551,-69.9242744946854,0.));
#65443=CARTESIAN_POINT('Ctrl Pts',(20.6994632178551,-69.9242744946854,12.));
#65444=CARTESIAN_POINT('Ctrl Pts',(20.7154102555996,-69.9443770838444,0.));
#65445=CARTESIAN_POINT('Ctrl Pts',(20.7154102555996,-69.9443770838444,12.));
#65446=CARTESIAN_POINT('Ctrl Pts',(20.7314003267118,-69.9644949847929,0.));
#65447=CARTESIAN_POINT('Ctrl Pts',(20.7314003267118,-69.9644949847929,12.));
#65448=CARTESIAN_POINT('Ctrl Pts',(20.7474334096581,-69.9846280854254,0.));
#65449=CARTESIAN_POINT('Ctrl Pts',(20.7474334096581,-69.9846280854254,12.));
#65450=CARTESIAN_POINT('Ctrl Pts',(20.7635094829016,-70.0047762740569,0.));
#65451=CARTESIAN_POINT('Ctrl Pts',(20.7635094829016,-70.0047762740569,12.));
#65452=CARTESIAN_POINT('Ctrl Pts',(20.7796285249022,-70.0249394394221,0.));
#65453=CARTESIAN_POINT('Ctrl Pts',(20.7796285249022,-70.0249394394221,12.));
#65454=CARTESIAN_POINT('Ctrl Pts',(20.7957905141155,-70.0451174706739,0.));
#65455=CARTESIAN_POINT('Ctrl Pts',(20.7957905141155,-70.0451174706739,12.));
#65456=CARTESIAN_POINT('Ctrl Pts',(20.8119954289845,-70.0653102573798,0.));
#65457=CARTESIAN_POINT('Ctrl Pts',(20.8119954289845,-70.0653102573798,12.));
#65458=CARTESIAN_POINT('Ctrl Pts',(20.8282432479425,-70.0855176895185,0.));
#65459=CARTESIAN_POINT('Ctrl Pts',(20.8282432479425,-70.0855176895185,12.));
#65460=CARTESIAN_POINT('Ctrl Pts',(20.8445339494184,-70.1057396574741,0.));
#65461=CARTESIAN_POINT('Ctrl Pts',(20.8445339494184,-70.1057396574741,12.));
#65462=CARTESIAN_POINT('Ctrl Pts',(20.8608675118377,-70.1259760520306,0.));
#65463=CARTESIAN_POINT('Ctrl Pts',(20.8608675118377,-70.1259760520306,12.));
#65464=CARTESIAN_POINT('Ctrl Pts',(20.8772439136206,-70.1462267643649,0.));
#65465=CARTESIAN_POINT('Ctrl Pts',(20.8772439136206,-70.1462267643649,12.));
#65466=CARTESIAN_POINT('Ctrl Pts',(20.893663133175,-70.1664916860366,0.));
#65467=CARTESIAN_POINT('Ctrl Pts',(20.893663133175,-70.1664916860366,12.));
#65468=CARTESIAN_POINT('Ctrl Pts',(20.9101251488948,-70.1867707089866,0.));
#65469=CARTESIAN_POINT('Ctrl Pts',(20.9101251488948,-70.1867707089866,12.));
#65470=CARTESIAN_POINT('Ctrl Pts',(20.9266299391687,-70.2070637255469,0.));
#65471=CARTESIAN_POINT('Ctrl Pts',(20.9266299391687,-70.2070637255469,12.));
#65472=CARTESIAN_POINT('Ctrl Pts',(20.9431774823833,-70.2273706284479,0.));
#65473=CARTESIAN_POINT('Ctrl Pts',(20.9431774823833,-70.2273706284479,12.));
#65474=CARTESIAN_POINT('Ctrl Pts',(20.9597677569227,-70.2476913108242,0.));
#65475=CARTESIAN_POINT('Ctrl Pts',(20.9597677569227,-70.2476913108242,12.));
#65476=CARTESIAN_POINT('Ctrl Pts',(20.9764007411648,-70.2680256662215,0.));
#65477=CARTESIAN_POINT('Ctrl Pts',(20.9764007411648,-70.2680256662215,12.));
#65478=CARTESIAN_POINT('Ctrl Pts',(20.993076413477,-70.2883735885971,0.));
#65479=CARTESIAN_POINT('Ctrl Pts',(20.993076413477,-70.2883735885971,12.));
#65480=CARTESIAN_POINT('Ctrl Pts',(21.0097947522212,-70.3087349722959,0.));
#65481=CARTESIAN_POINT('Ctrl Pts',(21.0097947522212,-70.3087349722959,12.));
#65482=CARTESIAN_POINT('Ctrl Pts',(21.0265557357544,-70.3291097120293,0.));
#65483=CARTESIAN_POINT('Ctrl Pts',(21.0265557357544,-70.3291097120293,12.));
#65484=CARTESIAN_POINT('Ctrl Pts',(21.0433593424265,-70.3494977028497,0.));
#65485=CARTESIAN_POINT('Ctrl Pts',(21.0433593424265,-70.3494977028497,12.));
#65486=CARTESIAN_POINT('Ctrl Pts',(21.0602055505751,-70.3698988401291,0.));
#65487=CARTESIAN_POINT('Ctrl Pts',(21.0602055505751,-70.3698988401291,12.));
#65488=CARTESIAN_POINT('Ctrl Pts',(21.0770943385145,-70.3903130195279,0.));
#65489=CARTESIAN_POINT('Ctrl Pts',(21.0770943385145,-70.3903130195279,12.));
#65490=CARTESIAN_POINT('Ctrl Pts',(21.0940256845477,-70.4107401370403,0.));
#65491=CARTESIAN_POINT('Ctrl Pts',(21.0940256845477,-70.4107401370403,12.));
#65492=CARTESIAN_POINT('Ctrl Pts',(21.110999566975,-70.4311800890411,0.));
#65493=CARTESIAN_POINT('Ctrl Pts',(21.110999566975,-70.4311800890411,12.));
#65494=CARTESIAN_POINT('Ctrl Pts',(21.1280159641003,-70.4516327723349,0.));
#65495=CARTESIAN_POINT('Ctrl Pts',(21.1280159641003,-70.4516327723349,12.));
#65496=CARTESIAN_POINT('Ctrl Pts',(21.1450748542334,-70.4720980841934,0.));
#65497=CARTESIAN_POINT('Ctrl Pts',(21.1450748542334,-70.4720980841934,12.));
#65498=CARTESIAN_POINT('Ctrl Pts',(21.1621762156894,-70.4925759224208,0.));
#65499=CARTESIAN_POINT('Ctrl Pts',(21.1621762156894,-70.4925759224208,12.));
#65500=CARTESIAN_POINT('Ctrl Pts',(21.1793200267843,-70.5130661852946,0.));
#65501=CARTESIAN_POINT('Ctrl Pts',(21.1793200267843,-70.5130661852946,12.));
#65502=CARTESIAN_POINT('Ctrl Pts',(21.1965062658295,-70.5335687714422,0.));
#65503=CARTESIAN_POINT('Ctrl Pts',(21.1965062658295,-70.5335687714422,12.));
#65504=CARTESIAN_POINT('Ctrl Pts',(21.2137349111207,-70.5540835797281,0.));
#65505=CARTESIAN_POINT('Ctrl Pts',(21.2137349111207,-70.5540835797281,12.));
#65506=CARTESIAN_POINT('Ctrl Pts',(21.2310059409265,-70.5746105091503,0.));
#65507=CARTESIAN_POINT('Ctrl Pts',(21.2310059409265,-70.5746105091503,12.));
#65508=CARTESIAN_POINT('Ctrl Pts',(21.2483193334676,-70.5951494586961,0.));
#65509=CARTESIAN_POINT('Ctrl Pts',(21.2483193334676,-70.5951494586961,12.));
#65510=CARTESIAN_POINT('Ctrl Pts',(21.2656750669129,-70.6157003273326,0.));
#65511=CARTESIAN_POINT('Ctrl Pts',(21.2656750669129,-70.6157003273326,12.));
#65512=CARTESIAN_POINT('Ctrl Pts',(21.2830731194187,-70.6362630143062,0.));
#65513=CARTESIAN_POINT('Ctrl Pts',(21.2830731194187,-70.6362630143062,12.));
#65514=CARTESIAN_POINT('Ctrl Pts',(21.3005134691563,-70.6568374193786,0.));
#65515=CARTESIAN_POINT('Ctrl Pts',(21.3005134691563,-70.6568374193786,12.));
#65516=CARTESIAN_POINT('Ctrl Pts',(21.3179960943388,-70.6774234430899,0.));
#65517=CARTESIAN_POINT('Ctrl Pts',(21.3179960943388,-70.6774234430899,12.));
#65518=CARTESIAN_POINT('Ctrl Pts',(21.3355209732438,-70.6980209870032,0.));
#65519=CARTESIAN_POINT('Ctrl Pts',(21.3355209732438,-70.6980209870032,12.));
#65520=CARTESIAN_POINT('Ctrl Pts',(21.353088084234,-70.7186299539698,0.));
#65521=CARTESIAN_POINT('Ctrl Pts',(21.353088084234,-70.7186299539698,12.));
#65522=CARTESIAN_POINT('Ctrl Pts',(21.3706974057028,-70.7392502475438,0.));
#65523=CARTESIAN_POINT('Ctrl Pts',(21.3706974057028,-70.7392502475438,12.));
#65524=CARTESIAN_POINT('Ctrl Pts',(21.3883489160187,-70.7598817714078,0.));
#65525=CARTESIAN_POINT('Ctrl Pts',(21.3883489160187,-70.7598817714078,12.));
#65526=CARTESIAN_POINT('Ctrl Pts',(21.4060425934594,-70.780524428744,0.));
#65527=CARTESIAN_POINT('Ctrl Pts',(21.4060425934594,-70.780524428744,12.));
#65528=CARTESIAN_POINT('Ctrl Pts',(21.4237784161592,-70.8011781217409,0.));
#65529=CARTESIAN_POINT('Ctrl Pts',(21.4237784161592,-70.8011781217409,12.));
#65530=CARTESIAN_POINT('Ctrl Pts',(21.4415563620127,-70.8218427507545,0.));
#65531=CARTESIAN_POINT('Ctrl Pts',(21.4415563620127,-70.8218427507545,12.));
#65532=CARTESIAN_POINT('Ctrl Pts',(21.4593764087492,-70.84251821499,0.));
#65533=CARTESIAN_POINT('Ctrl Pts',(21.4593764087492,-70.84251821499,12.));
#65534=CARTESIAN_POINT('Ctrl Pts',(21.4772385340978,-70.8632044140166,0.));
#65535=CARTESIAN_POINT('Ctrl Pts',(21.4772385340978,-70.8632044140166,12.));
#65536=CARTESIAN_POINT('Ctrl Pts',(21.4951427159272,-70.8839012490903,0.));
#65537=CARTESIAN_POINT('Ctrl Pts',(21.4951427159272,-70.8839012490903,12.));
#65538=CARTESIAN_POINT('Ctrl Pts',(21.5130889323766,-70.9046086244123,0.));
#65539=CARTESIAN_POINT('Ctrl Pts',(21.5130889323766,-70.9046086244123,12.));
#65540=CARTESIAN_POINT('Ctrl Pts',(21.5310771620209,-70.9253264487576,0.));
#65541=CARTESIAN_POINT('Ctrl Pts',(21.5310771620209,-70.9253264487576,12.));
#65542=CARTESIAN_POINT('Ctrl Pts',(21.549107383907,-70.9460546358597,0.));
#65543=CARTESIAN_POINT('Ctrl Pts',(21.549107383907,-70.9460546358597,12.));
#65544=CARTESIAN_POINT('Ctrl Pts',(21.5671795771872,-70.9667931008097,0.));
#65545=CARTESIAN_POINT('Ctrl Pts',(21.5671795771872,-70.9667931008097,12.));
#65546=CARTESIAN_POINT('Ctrl Pts',(21.5852937208258,-70.9875417572138,0.));
#65547=CARTESIAN_POINT('Ctrl Pts',(21.5852937208258,-70.9875417572138,12.));
#65548=CARTESIAN_POINT('Ctrl Pts',(21.6034497932573,-71.0083005139086,0.));
#65549=CARTESIAN_POINT('Ctrl Pts',(21.6034497932573,-71.0083005139086,12.));
#65550=CARTESIAN_POINT('Ctrl Pts',(21.6216477720941,-71.0290692721932,0.));
#65551=CARTESIAN_POINT('Ctrl Pts',(21.6216477720941,-71.0290692721932,12.));
#65552=CARTESIAN_POINT('Ctrl Pts',(21.6398876337206,-71.0498479219659,0.));
#65553=CARTESIAN_POINT('Ctrl Pts',(21.6398876337206,-71.0498479219659,12.));
#65554=CARTESIAN_POINT('Ctrl Pts',(21.6581693538424,-71.0706363472965,0.));
#65555=CARTESIAN_POINT('Ctrl Pts',(21.6581693538424,-71.0706363472965,12.));
#65556=CARTESIAN_POINT('Ctrl Pts',(21.6764929081762,-71.0914344333048,0.));
#65557=CARTESIAN_POINT('Ctrl Pts',(21.6764929081762,-71.0914344333048,12.));
#65558=CARTESIAN_POINT('Ctrl Pts',(21.6948582730895,-71.1122420728349,0.));
#65559=CARTESIAN_POINT('Ctrl Pts',(21.6948582730895,-71.1122420728349,12.));
#65560=CARTESIAN_POINT('Ctrl Pts',(21.7132654262501,-71.133059172642,0.));
#65561=CARTESIAN_POINT('Ctrl Pts',(21.7132654262501,-71.133059172642,12.));
#65562=CARTESIAN_POINT('Ctrl Pts',(21.7317143472826,-71.1538856611899,0.));
#65563=CARTESIAN_POINT('Ctrl Pts',(21.7317143472826,-71.1538856611899,12.));
#65564=CARTESIAN_POINT('Ctrl Pts',(21.7502050183602,-71.1747214905981,0.));
#65565=CARTESIAN_POINT('Ctrl Pts',(21.7502050183602,-71.1747214905981,12.));
#65566=CARTESIAN_POINT('Ctrl Pts',(21.7687374247045,-71.1955666309591,0.));
#65567=CARTESIAN_POINT('Ctrl Pts',(21.7687374247045,-71.1955666309591,12.));
#65568=CARTESIAN_POINT('Ctrl Pts',(21.7835967290261,-71.212250179455,0.));
#65569=CARTESIAN_POINT('Ctrl Pts',(21.7835967290261,-71.212250179455,12.));
#65570=CARTESIAN_POINT('Ctrl Pts',(21.7947599798838,-71.2247670209821,0.));
#65571=CARTESIAN_POINT('Ctrl Pts',(21.7947599798838,-71.2247670209821,12.));
#65572=CARTESIAN_POINT('Ctrl Pts',(21.8022104901682,-71.2331134397743,0.));
#65573=CARTESIAN_POINT('Ctrl Pts',(21.8022104901682,-71.2331134397743,12.));
#65574=CARTESIAN_POINT('Ctrl Pts',(21.8059378310718,-71.2372871136137,0.));
#65575=CARTESIAN_POINT('Ctrl Pts',(21.8059378310718,-71.2372871136137,12.));
#65576=CARTESIAN_POINT('',(18.9407177820968,-67.3887914263118,0.));
#65577=CARTESIAN_POINT('Ctrl Pts',(18.9407177820968,-67.3887914263118,0.));
#65578=CARTESIAN_POINT('Ctrl Pts',(18.9426924398719,-67.3921355608328,0.));
#65579=CARTESIAN_POINT('Ctrl Pts',(18.9466463414299,-67.3988274146651,0.));
#65580=CARTESIAN_POINT('Ctrl Pts',(18.9525909517915,-67.4088759497911,0.));
#65581=CARTESIAN_POINT('Ctrl Pts',(18.9605446160985,-67.4222955061981,0.));
#65582=CARTESIAN_POINT('Ctrl Pts',(18.970532563171,-67.4391057908418,0.));
#65583=CARTESIAN_POINT('Ctrl Pts',(18.9805663798448,-67.4559518744638,0.));
#65584=CARTESIAN_POINT('Ctrl Pts',(18.9906460638625,-67.472833671964,0.));
#65585=CARTESIAN_POINT('Ctrl Pts',(19.0007716032819,-67.4897510316844,0.));
#65586=CARTESIAN_POINT('Ctrl Pts',(19.0109429761306,-67.5067037372317,0.));
#65587=CARTESIAN_POINT('Ctrl Pts',(19.021160154824,-67.5236915360331,0.));
#65588=CARTESIAN_POINT('Ctrl Pts',(19.0314231093923,-67.540714161288,0.));
#65589=CARTESIAN_POINT('Ctrl Pts',(19.0417318110708,-67.5577713558194,0.));
#65590=CARTESIAN_POINT('Ctrl Pts',(19.0520862360395,-67.5748628971964,0.));
#65591=CARTESIAN_POINT('Ctrl Pts',(19.062486364241,-67.5919885896222,0.));
#65592=CARTESIAN_POINT('Ctrl Pts',(19.072932177628,-67.6091482520534,0.));
#65593=CARTESIAN_POINT('Ctrl Pts',(19.0834236587118,-67.6263417083426,0.));
#65594=CARTESIAN_POINT('Ctrl Pts',(19.0939607887501,-67.6435687749841,0.));
#65595=CARTESIAN_POINT('Ctrl Pts',(19.1045435468358,-67.6608292549462,0.));
#65596=CARTESIAN_POINT('Ctrl Pts',(19.115171910846,-67.6781229440573,0.));
#65597=CARTESIAN_POINT('Ctrl Pts',(19.1258458580345,-67.6954496350063,0.));
#65598=CARTESIAN_POINT('Ctrl Pts',(19.136565365709,-67.7128091219348,0.));
#65599=CARTESIAN_POINT('Ctrl Pts',(19.1473304119955,-67.7302012056584,0.));
#65600=CARTESIAN_POINT('Ctrl Pts',(19.1581409758097,-67.7476256934444,0.));
#65601=CARTESIAN_POINT('Ctrl Pts',(19.1689970364949,-67.7650823965127,0.));
#65602=CARTESIAN_POINT('Ctrl Pts',(19.1798985735687,-67.7825711283096,0.));
#65603=CARTESIAN_POINT('Ctrl Pts',(19.1908455664097,-67.8000917023926,0.));
#65604=CARTESIAN_POINT('Ctrl Pts',(19.201837993993,-67.8176439306621,0.));
#65605=CARTESIAN_POINT('Ctrl Pts',(19.2128758350345,-67.835227624289,0.));
#65606=CARTESIAN_POINT('Ctrl Pts',(19.2239590681133,-67.8528425945184,0.));
#65607=CARTESIAN_POINT('Ctrl Pts',(19.2350876717874,-67.8704886534544,0.));
#65608=CARTESIAN_POINT('Ctrl Pts',(19.2462616247279,-67.8881656149955,0.));
#65609=CARTESIAN_POINT('Ctrl Pts',(19.2574809057696,-67.9058732951788,0.));
#65610=CARTESIAN_POINT('Ctrl Pts',(19.2687454938442,-67.9236115116758,0.));
#65611=CARTESIAN_POINT('Ctrl Pts',(19.280055367936,-67.9413800834793,0.));
#65612=CARTESIAN_POINT('Ctrl Pts',(19.2914105070286,-67.9591788305394,0.));
#65613=CARTESIAN_POINT('Ctrl Pts',(19.302810890038,-67.9770075733485,0.));
#65614=CARTESIAN_POINT('Ctrl Pts',(19.3142564958202,-67.9948661329617,0.));
#65615=CARTESIAN_POINT('Ctrl Pts',(19.3257473032034,-68.0127543311776,0.));
#65616=CARTESIAN_POINT('Ctrl Pts',(19.3372832910076,-68.0306719906636,0.));
#65617=CARTESIAN_POINT('Ctrl Pts',(19.3488644380641,-68.0486189351011,0.));
#65618=CARTESIAN_POINT('Ctrl Pts',(19.3604907232313,-68.0665949893195,0.));
#65619=CARTESIAN_POINT('Ctrl Pts',(19.3721621253912,-68.0845999792247,0.));
#65620=CARTESIAN_POINT('Ctrl Pts',(19.3838786234421,-68.1026337317285,0.));
#65621=CARTESIAN_POINT('Ctrl Pts',(19.3956401962894,-68.1206960746769,0.));
#65622=CARTESIAN_POINT('Ctrl Pts',(19.4074468228299,-68.1387868367691,0.));
#65623=CARTESIAN_POINT('Ctrl Pts',(19.4192984819418,-68.1569058475054,0.));
#65624=CARTESIAN_POINT('Ctrl Pts',(19.4311951524983,-68.1750529372232,0.));
#65625=CARTESIAN_POINT('Ctrl Pts',(19.4431368133719,-68.1932279371127,0.));
#65626=CARTESIAN_POINT('Ctrl Pts',(19.455123443438,-68.2114306792358,0.));
#65627=CARTESIAN_POINT('Ctrl Pts',(19.467155021572,-68.2296609965448,0.));
#65628=CARTESIAN_POINT('Ctrl Pts',(19.4792315266501,-68.2479187228803,0.));
#65629=CARTESIAN_POINT('Ctrl Pts',(19.4913529375543,-68.2662036929526,0.));
#65630=CARTESIAN_POINT('Ctrl Pts',(19.5035192331705,-68.2845157423233,0.));
#65631=CARTESIAN_POINT('Ctrl Pts',(19.5157303923856,-68.3028547073865,0.));
#65632=CARTESIAN_POINT('Ctrl Pts',(19.5279863940773,-68.3212204253417,0.));
#65633=CARTESIAN_POINT('Ctrl Pts',(19.540287217119,-68.3396127341938,0.));
#65634=CARTESIAN_POINT('Ctrl Pts',(19.5526328403852,-68.3580314727523,0.));
#65635=CARTESIAN_POINT('Ctrl Pts',(19.5650232427515,-68.3764764806287,0.));
#65636=CARTESIAN_POINT('Ctrl Pts',(19.5774584030937,-68.3949475982335,0.));
#65637=CARTESIAN_POINT('Ctrl Pts',(19.5899383002802,-68.4134446667696,0.));
#65638=CARTESIAN_POINT('Ctrl Pts',(19.6024629131784,-68.4319675282275,0.));
#65639=CARTESIAN_POINT('Ctrl Pts',(19.6150322206577,-68.4505160253778,0.));
#65640=CARTESIAN_POINT('Ctrl Pts',(19.6276462015888,-68.4690900017632,0.));
#65641=CARTESIAN_POINT('Ctrl Pts',(19.6403048348395,-68.4876893016856,0.));
#65642=CARTESIAN_POINT('Ctrl Pts',(19.6530080992686,-68.5063137701971,0.));
#65643=CARTESIAN_POINT('Ctrl Pts',(19.6657559737336,-68.5249632530979,0.));
#65644=CARTESIAN_POINT('Ctrl Pts',(19.6785484370926,-68.5436375969311,0.));
#65645=CARTESIAN_POINT('Ctrl Pts',(19.6913854682046,-68.5623366489779,0.));
#65646=CARTESIAN_POINT('Ctrl Pts',(19.7042670459237,-68.581060257249,0.));
#65647=CARTESIAN_POINT('Ctrl Pts',(19.7171931490956,-68.5998082704766,0.));
#65648=CARTESIAN_POINT('Ctrl Pts',(19.7301637565652,-68.6185805381126,0.));
#65649=CARTESIAN_POINT('Ctrl Pts',(19.7431788471775,-68.6373769103224,0.));
#65650=CARTESIAN_POINT('Ctrl Pts',(19.7562383997781,-68.6561972379793,0.));
#65651=CARTESIAN_POINT('Ctrl Pts',(19.7693423932058,-68.6750413726547,0.));
#65652=CARTESIAN_POINT('Ctrl Pts',(19.7824908062913,-68.6939091666111,0.));
#65653=CARTESIAN_POINT('Ctrl Pts',(19.795683617864,-68.7128004727998,0.));
#65654=CARTESIAN_POINT('Ctrl Pts',(19.8089208067532,-68.7317151448557,0.));
#65655=CARTESIAN_POINT('Ctrl Pts',(19.8222023517874,-68.7506530370918,0.));
#65656=CARTESIAN_POINT('Ctrl Pts',(19.835528231787,-68.7696140044892,0.));
#65657=CARTESIAN_POINT('Ctrl Pts',(19.8488984255641,-68.7885979026927,0.));
#65658=CARTESIAN_POINT('Ctrl Pts',(19.8623129119304,-68.8076045880102,0.));
#65659=CARTESIAN_POINT('Ctrl Pts',(19.8757716696968,-68.8266339174068,0.));
#65660=CARTESIAN_POINT('Ctrl Pts',(19.8892746776733,-68.8456857484988,0.));
#65661=CARTESIAN_POINT('Ctrl Pts',(19.9028219146606,-68.8647599395437,0.));
#65662=CARTESIAN_POINT('Ctrl Pts',(19.9164133594512,-68.8838563494356,0.));
#65663=CARTESIAN_POINT('Ctrl Pts',(19.9300489908364,-68.902974837704,0.));
#65664=CARTESIAN_POINT('Ctrl Pts',(19.9437287876063,-68.9221152645086,0.));
#65665=CARTESIAN_POINT('Ctrl Pts',(19.9574527285492,-68.9412774906346,0.));
#65666=CARTESIAN_POINT('Ctrl Pts',(19.9712207924436,-68.960461377483,0.));
#65667=CARTESIAN_POINT('Ctrl Pts',(19.9850329580599,-68.9796667870667,0.));
#65668=CARTESIAN_POINT('Ctrl Pts',(19.9988892041671,-68.9988935820101,0.));
#65669=CARTESIAN_POINT('Ctrl Pts',(20.0127895095326,-69.0181416255433,0.));
#65670=CARTESIAN_POINT('Ctrl Pts',(20.026733852922,-69.0374107814977,0.));
#65671=CARTESIAN_POINT('Ctrl Pts',(20.0407222130902,-69.0567009142968,0.));
#65672=CARTESIAN_POINT('Ctrl Pts',(20.0547545687839,-69.0760118889525,0.));
#65673=CARTESIAN_POINT('Ctrl Pts',(20.0688308987478,-69.0953435710634,0.));
#65674=CARTESIAN_POINT('Ctrl Pts',(20.082951181725,-69.1146958268104,0.));
#65675=CARTESIAN_POINT('Ctrl Pts',(20.0971153964557,-69.1340685229516,0.));
#65676=CARTESIAN_POINT('Ctrl Pts',(20.1113235216693,-69.1534615268153,0.));
#65677=CARTESIAN_POINT('Ctrl Pts',(20.125575536087,-69.172874706296,0.));
#65678=CARTESIAN_POINT('Ctrl Pts',(20.1398714184278,-69.1923079298534,0.));
#65679=CARTESIAN_POINT('Ctrl Pts',(20.1542111474086,-69.2117610665073,0.));
#65680=CARTESIAN_POINT('Ctrl Pts',(20.1685947017433,-69.2312339858337,0.));
#65681=CARTESIAN_POINT('Ctrl Pts',(20.183022060135,-69.2507265579562,0.));
#65682=CARTESIAN_POINT('Ctrl Pts',(20.1974932012775,-69.2702386535432,0.));
#65683=CARTESIAN_POINT('Ctrl Pts',(20.2120081038621,-69.2897701438066,0.));
#65684=CARTESIAN_POINT('Ctrl Pts',(20.2265667465783,-69.3093209004986,0.));
#65685=CARTESIAN_POINT('Ctrl Pts',(20.2411691081122,-69.3288907959065,0.));
#65686=CARTESIAN_POINT('Ctrl Pts',(20.255815167139,-69.3484797028454,0.));
#65687=CARTESIAN_POINT('Ctrl Pts',(20.270504902324,-69.3680874946548,0.));
#65688=CARTESIAN_POINT('Ctrl Pts',(20.2852382923299,-69.3877140451975,0.));
#65689=CARTESIAN_POINT('Ctrl Pts',(20.3000153158167,-69.4073592288562,0.));
#65690=CARTESIAN_POINT('Ctrl Pts',(20.3148359514414,-69.4270229205296,0.));
#65691=CARTESIAN_POINT('Ctrl Pts',(20.3297001778505,-69.4467049956257,0.));
#65692=CARTESIAN_POINT('Ctrl Pts',(20.3446079736798,-69.4664053300579,0.));
#65693=CARTESIAN_POINT('Ctrl Pts',(20.3595593175619,-69.4861238002433,0.));
#65694=CARTESIAN_POINT('Ctrl Pts',(20.3745541881266,-69.5058602831004,0.));
#65695=CARTESIAN_POINT('Ctrl Pts',(20.3895925640006,-69.5256146560444,0.));
#65696=CARTESIAN_POINT('Ctrl Pts',(20.4046744238002,-69.5453867969815,0.));
#65697=CARTESIAN_POINT('Ctrl Pts',(20.4197997461305,-69.565176584305,0.));
#65698=CARTESIAN_POINT('Ctrl Pts',(20.4349685095928,-69.5849838968944,0.));
#65699=CARTESIAN_POINT('Ctrl Pts',(20.4501806927854,-69.6048086141122,0.));
#65700=CARTESIAN_POINT('Ctrl Pts',(20.4654362743036,-69.6246506158009,0.));
#65701=CARTESIAN_POINT('Ctrl Pts',(20.4807352327335,-69.6445097822778,0.));
#65702=CARTESIAN_POINT('Ctrl Pts',(20.4960775466486,-69.6643859943291,0.));
#65703=CARTESIAN_POINT('Ctrl Pts',(20.511463194618,-69.6842791332102,0.));
#65704=CARTESIAN_POINT('Ctrl Pts',(20.5268921552075,-69.7041890806421,0.));
#65705=CARTESIAN_POINT('Ctrl Pts',(20.5423644069799,-69.7241157188086,0.));
#65706=CARTESIAN_POINT('Ctrl Pts',(20.5578799284897,-69.7440589303511,0.));
#65707=CARTESIAN_POINT('Ctrl Pts',(20.5734386982781,-69.7640185983641,0.));
#65708=CARTESIAN_POINT('Ctrl Pts',(20.5890406948808,-69.7839946063942,0.));
#65709=CARTESIAN_POINT('Ctrl Pts',(20.6046858968305,-69.8039868384382,0.));
#65710=CARTESIAN_POINT('Ctrl Pts',(20.6203742826565,-69.8239951789402,0.));
#65711=CARTESIAN_POINT('Ctrl Pts',(20.6361058308812,-69.8440195127874,0.));
#65712=CARTESIAN_POINT('Ctrl Pts',(20.6518805200131,-69.8640597253058,0.));
#65713=CARTESIAN_POINT('Ctrl Pts',(20.6676983285542,-69.884115702258,0.));
#65714=CARTESIAN_POINT('Ctrl Pts',(20.683559235003,-69.9041873298416,0.));
#65715=CARTESIAN_POINT('Ctrl Pts',(20.6994632178551,-69.9242744946854,0.));
#65716=CARTESIAN_POINT('Ctrl Pts',(20.7154102555996,-69.9443770838444,0.));
#65717=CARTESIAN_POINT('Ctrl Pts',(20.7314003267118,-69.9644949847929,0.));
#65718=CARTESIAN_POINT('Ctrl Pts',(20.7474334096581,-69.9846280854254,0.));
#65719=CARTESIAN_POINT('Ctrl Pts',(20.7635094829016,-70.0047762740569,0.));
#65720=CARTESIAN_POINT('Ctrl Pts',(20.7796285249022,-70.0249394394221,0.));
#65721=CARTESIAN_POINT('Ctrl Pts',(20.7957905141155,-70.0451174706739,0.));
#65722=CARTESIAN_POINT('Ctrl Pts',(20.8119954289845,-70.0653102573798,0.));
#65723=CARTESIAN_POINT('Ctrl Pts',(20.8282432479425,-70.0855176895185,0.));
#65724=CARTESIAN_POINT('Ctrl Pts',(20.8445339494184,-70.1057396574741,0.));
#65725=CARTESIAN_POINT('Ctrl Pts',(20.8608675118377,-70.1259760520306,0.));
#65726=CARTESIAN_POINT('Ctrl Pts',(20.8772439136206,-70.1462267643649,0.));
#65727=CARTESIAN_POINT('Ctrl Pts',(20.893663133175,-70.1664916860366,0.));
#65728=CARTESIAN_POINT('Ctrl Pts',(20.9101251488948,-70.1867707089866,0.));
#65729=CARTESIAN_POINT('Ctrl Pts',(20.9266299391687,-70.2070637255469,0.));
#65730=CARTESIAN_POINT('Ctrl Pts',(20.9431774823833,-70.2273706284479,0.));
#65731=CARTESIAN_POINT('Ctrl Pts',(20.9597677569227,-70.2476913108242,0.));
#65732=CARTESIAN_POINT('Ctrl Pts',(20.9764007411648,-70.2680256662215,0.));
#65733=CARTESIAN_POINT('Ctrl Pts',(20.993076413477,-70.2883735885971,0.));
#65734=CARTESIAN_POINT('Ctrl Pts',(21.0097947522212,-70.3087349722959,0.));
#65735=CARTESIAN_POINT('Ctrl Pts',(21.0265557357544,-70.3291097120293,0.));
#65736=CARTESIAN_POINT('Ctrl Pts',(21.0433593424265,-70.3494977028497,0.));
#65737=CARTESIAN_POINT('Ctrl Pts',(21.0602055505751,-70.3698988401291,0.));
#65738=CARTESIAN_POINT('Ctrl Pts',(21.0770943385145,-70.3903130195279,0.));
#65739=CARTESIAN_POINT('Ctrl Pts',(21.0940256845477,-70.4107401370403,0.));
#65740=CARTESIAN_POINT('Ctrl Pts',(21.110999566975,-70.4311800890411,0.));
#65741=CARTESIAN_POINT('Ctrl Pts',(21.1280159641003,-70.4516327723349,0.));
#65742=CARTESIAN_POINT('Ctrl Pts',(21.1450748542334,-70.4720980841934,0.));
#65743=CARTESIAN_POINT('Ctrl Pts',(21.1621762156894,-70.4925759224208,0.));
#65744=CARTESIAN_POINT('Ctrl Pts',(21.1793200267843,-70.5130661852946,0.));
#65745=CARTESIAN_POINT('Ctrl Pts',(21.1965062658295,-70.5335687714422,0.));
#65746=CARTESIAN_POINT('Ctrl Pts',(21.2137349111207,-70.5540835797281,0.));
#65747=CARTESIAN_POINT('Ctrl Pts',(21.2310059409265,-70.5746105091503,0.));
#65748=CARTESIAN_POINT('Ctrl Pts',(21.2483193334676,-70.5951494586961,0.));
#65749=CARTESIAN_POINT('Ctrl Pts',(21.2656750669129,-70.6157003273326,0.));
#65750=CARTESIAN_POINT('Ctrl Pts',(21.2830731194187,-70.6362630143062,0.));
#65751=CARTESIAN_POINT('Ctrl Pts',(21.3005134691563,-70.6568374193786,0.));
#65752=CARTESIAN_POINT('Ctrl Pts',(21.3179960943388,-70.6774234430899,0.));
#65753=CARTESIAN_POINT('Ctrl Pts',(21.3355209732438,-70.6980209870032,0.));
#65754=CARTESIAN_POINT('Ctrl Pts',(21.353088084234,-70.7186299539698,0.));
#65755=CARTESIAN_POINT('Ctrl Pts',(21.3706974057028,-70.7392502475438,0.));
#65756=CARTESIAN_POINT('Ctrl Pts',(21.3883489160187,-70.7598817714078,0.));
#65757=CARTESIAN_POINT('Ctrl Pts',(21.4060425934594,-70.780524428744,0.));
#65758=CARTESIAN_POINT('Ctrl Pts',(21.4237784161592,-70.8011781217409,0.));
#65759=CARTESIAN_POINT('Ctrl Pts',(21.4415563620127,-70.8218427507545,0.));
#65760=CARTESIAN_POINT('Ctrl Pts',(21.4593764087492,-70.84251821499,0.));
#65761=CARTESIAN_POINT('Ctrl Pts',(21.4772385340978,-70.8632044140166,0.));
#65762=CARTESIAN_POINT('Ctrl Pts',(21.4951427159272,-70.8839012490903,0.));
#65763=CARTESIAN_POINT('Ctrl Pts',(21.5130889323766,-70.9046086244123,0.));
#65764=CARTESIAN_POINT('Ctrl Pts',(21.5310771620209,-70.9253264487576,0.));
#65765=CARTESIAN_POINT('Ctrl Pts',(21.549107383907,-70.9460546358597,0.));
#65766=CARTESIAN_POINT('Ctrl Pts',(21.5645987555282,-70.9638315189647,0.));
#65767=CARTESIAN_POINT('Ctrl Pts',(21.576498336635,-70.9774662112376,0.));
#65768=CARTESIAN_POINT('Ctrl Pts',(21.584787543316,-70.9869541807808,0.));
#65769=CARTESIAN_POINT('Ctrl Pts',(21.5894540925368,-70.9922924595081,0.));
#65770=CARTESIAN_POINT('Ctrl Pts',(21.59049199348,-70.9934796068777,0.));
#65771=CARTESIAN_POINT('',(18.9407177820968,-67.3887914263118,12.));
#65772=CARTESIAN_POINT('',(18.9407177820968,-67.3887914263118,0.));
#65773=CARTESIAN_POINT('Ctrl Pts',(21.59049199348,-70.9934796068777,12.));
#65774=CARTESIAN_POINT('Ctrl Pts',(21.5894540925368,-70.9922924595081,12.));
#65775=CARTESIAN_POINT('Ctrl Pts',(21.584787543316,-70.9869541807808,12.));
#65776=CARTESIAN_POINT('Ctrl Pts',(21.576498336635,-70.9774662112376,12.));
#65777=CARTESIAN_POINT('Ctrl Pts',(21.5645987555282,-70.9638315189647,12.));
#65778=CARTESIAN_POINT('Ctrl Pts',(21.549107383907,-70.9460546358597,12.));
#65779=CARTESIAN_POINT('Ctrl Pts',(21.5310771620209,-70.9253264487576,12.));
#65780=CARTESIAN_POINT('Ctrl Pts',(21.5130889323766,-70.9046086244123,12.));
#65781=CARTESIAN_POINT('Ctrl Pts',(21.4951427159272,-70.8839012490903,12.));
#65782=CARTESIAN_POINT('Ctrl Pts',(21.4772385340978,-70.8632044140166,12.));
#65783=CARTESIAN_POINT('Ctrl Pts',(21.4593764087492,-70.84251821499,12.));
#65784=CARTESIAN_POINT('Ctrl Pts',(21.4415563620127,-70.8218427507545,12.));
#65785=CARTESIAN_POINT('Ctrl Pts',(21.4237784161592,-70.8011781217409,12.));
#65786=CARTESIAN_POINT('Ctrl Pts',(21.4060425934594,-70.780524428744,12.));
#65787=CARTESIAN_POINT('Ctrl Pts',(21.3883489160187,-70.7598817714078,12.));
#65788=CARTESIAN_POINT('Ctrl Pts',(21.3706974057028,-70.7392502475438,12.));
#65789=CARTESIAN_POINT('Ctrl Pts',(21.353088084234,-70.7186299539698,12.));
#65790=CARTESIAN_POINT('Ctrl Pts',(21.3355209732438,-70.6980209870032,12.));
#65791=CARTESIAN_POINT('Ctrl Pts',(21.3179960943388,-70.6774234430899,12.));
#65792=CARTESIAN_POINT('Ctrl Pts',(21.3005134691563,-70.6568374193786,12.));
#65793=CARTESIAN_POINT('Ctrl Pts',(21.2830731194187,-70.6362630143062,12.));
#65794=CARTESIAN_POINT('Ctrl Pts',(21.2656750669129,-70.6157003273326,12.));
#65795=CARTESIAN_POINT('Ctrl Pts',(21.2483193334676,-70.5951494586961,12.));
#65796=CARTESIAN_POINT('Ctrl Pts',(21.2310059409265,-70.5746105091503,12.));
#65797=CARTESIAN_POINT('Ctrl Pts',(21.2137349111207,-70.5540835797281,12.));
#65798=CARTESIAN_POINT('Ctrl Pts',(21.1965062658295,-70.5335687714422,12.));
#65799=CARTESIAN_POINT('Ctrl Pts',(21.1793200267843,-70.5130661852946,12.));
#65800=CARTESIAN_POINT('Ctrl Pts',(21.1621762156894,-70.4925759224208,12.));
#65801=CARTESIAN_POINT('Ctrl Pts',(21.1450748542334,-70.4720980841934,12.));
#65802=CARTESIAN_POINT('Ctrl Pts',(21.1280159641003,-70.4516327723349,12.));
#65803=CARTESIAN_POINT('Ctrl Pts',(21.110999566975,-70.4311800890411,12.));
#65804=CARTESIAN_POINT('Ctrl Pts',(21.0940256845477,-70.4107401370403,12.));
#65805=CARTESIAN_POINT('Ctrl Pts',(21.0770943385145,-70.3903130195279,12.));
#65806=CARTESIAN_POINT('Ctrl Pts',(21.0602055505751,-70.3698988401291,12.));
#65807=CARTESIAN_POINT('Ctrl Pts',(21.0433593424265,-70.3494977028497,12.));
#65808=CARTESIAN_POINT('Ctrl Pts',(21.0265557357544,-70.3291097120293,12.));
#65809=CARTESIAN_POINT('Ctrl Pts',(21.0097947522212,-70.3087349722959,12.));
#65810=CARTESIAN_POINT('Ctrl Pts',(20.993076413477,-70.2883735885971,12.));
#65811=CARTESIAN_POINT('Ctrl Pts',(20.9764007411648,-70.2680256662215,12.));
#65812=CARTESIAN_POINT('Ctrl Pts',(20.9597677569227,-70.2476913108242,12.));
#65813=CARTESIAN_POINT('Ctrl Pts',(20.9431774823833,-70.2273706284479,12.));
#65814=CARTESIAN_POINT('Ctrl Pts',(20.9266299391687,-70.2070637255469,12.));
#65815=CARTESIAN_POINT('Ctrl Pts',(20.9101251488948,-70.1867707089866,12.));
#65816=CARTESIAN_POINT('Ctrl Pts',(20.893663133175,-70.1664916860366,12.));
#65817=CARTESIAN_POINT('Ctrl Pts',(20.8772439136206,-70.1462267643649,12.));
#65818=CARTESIAN_POINT('Ctrl Pts',(20.8608675118377,-70.1259760520306,12.));
#65819=CARTESIAN_POINT('Ctrl Pts',(20.8445339494184,-70.1057396574741,12.));
#65820=CARTESIAN_POINT('Ctrl Pts',(20.8282432479425,-70.0855176895185,12.));
#65821=CARTESIAN_POINT('Ctrl Pts',(20.8119954289845,-70.0653102573798,12.));
#65822=CARTESIAN_POINT('Ctrl Pts',(20.7957905141155,-70.0451174706739,12.));
#65823=CARTESIAN_POINT('Ctrl Pts',(20.7796285249022,-70.0249394394221,12.));
#65824=CARTESIAN_POINT('Ctrl Pts',(20.7635094829016,-70.0047762740569,12.));
#65825=CARTESIAN_POINT('Ctrl Pts',(20.7474334096581,-69.9846280854254,12.));
#65826=CARTESIAN_POINT('Ctrl Pts',(20.7314003267118,-69.9644949847929,12.));
#65827=CARTESIAN_POINT('Ctrl Pts',(20.7154102555996,-69.9443770838444,12.));
#65828=CARTESIAN_POINT('Ctrl Pts',(20.6994632178551,-69.9242744946854,12.));
#65829=CARTESIAN_POINT('Ctrl Pts',(20.683559235003,-69.9041873298416,12.));
#65830=CARTESIAN_POINT('Ctrl Pts',(20.6676983285542,-69.884115702258,12.));
#65831=CARTESIAN_POINT('Ctrl Pts',(20.6518805200131,-69.8640597253058,12.));
#65832=CARTESIAN_POINT('Ctrl Pts',(20.6361058308812,-69.8440195127874,12.));
#65833=CARTESIAN_POINT('Ctrl Pts',(20.6203742826565,-69.8239951789402,12.));
#65834=CARTESIAN_POINT('Ctrl Pts',(20.6046858968305,-69.8039868384382,12.));
#65835=CARTESIAN_POINT('Ctrl Pts',(20.5890406948808,-69.7839946063942,12.));
#65836=CARTESIAN_POINT('Ctrl Pts',(20.5734386982781,-69.7640185983641,12.));
#65837=CARTESIAN_POINT('Ctrl Pts',(20.5578799284897,-69.7440589303511,12.));
#65838=CARTESIAN_POINT('Ctrl Pts',(20.5423644069799,-69.7241157188086,12.));
#65839=CARTESIAN_POINT('Ctrl Pts',(20.5268921552075,-69.7041890806421,12.));
#65840=CARTESIAN_POINT('Ctrl Pts',(20.511463194618,-69.6842791332102,12.));
#65841=CARTESIAN_POINT('Ctrl Pts',(20.4960775466486,-69.6643859943291,12.));
#65842=CARTESIAN_POINT('Ctrl Pts',(20.4807352327335,-69.6445097822778,12.));
#65843=CARTESIAN_POINT('Ctrl Pts',(20.4654362743036,-69.6246506158009,12.));
#65844=CARTESIAN_POINT('Ctrl Pts',(20.4501806927854,-69.6048086141122,12.));
#65845=CARTESIAN_POINT('Ctrl Pts',(20.4349685095928,-69.5849838968944,12.));
#65846=CARTESIAN_POINT('Ctrl Pts',(20.4197997461305,-69.565176584305,12.));
#65847=CARTESIAN_POINT('Ctrl Pts',(20.4046744238002,-69.5453867969815,12.));
#65848=CARTESIAN_POINT('Ctrl Pts',(20.3895925640006,-69.5256146560444,12.));
#65849=CARTESIAN_POINT('Ctrl Pts',(20.3745541881266,-69.5058602831004,12.));
#65850=CARTESIAN_POINT('Ctrl Pts',(20.3595593175619,-69.4861238002433,12.));
#65851=CARTESIAN_POINT('Ctrl Pts',(20.3446079736798,-69.4664053300579,12.));
#65852=CARTESIAN_POINT('Ctrl Pts',(20.3297001778505,-69.4467049956257,12.));
#65853=CARTESIAN_POINT('Ctrl Pts',(20.3148359514414,-69.4270229205296,12.));
#65854=CARTESIAN_POINT('Ctrl Pts',(20.3000153158167,-69.4073592288562,12.));
#65855=CARTESIAN_POINT('Ctrl Pts',(20.2852382923299,-69.3877140451975,12.));
#65856=CARTESIAN_POINT('Ctrl Pts',(20.270504902324,-69.3680874946548,12.));
#65857=CARTESIAN_POINT('Ctrl Pts',(20.255815167139,-69.3484797028454,12.));
#65858=CARTESIAN_POINT('Ctrl Pts',(20.2411691081122,-69.3288907959065,12.));
#65859=CARTESIAN_POINT('Ctrl Pts',(20.2265667465783,-69.3093209004986,12.));
#65860=CARTESIAN_POINT('Ctrl Pts',(20.2120081038621,-69.2897701438066,12.));
#65861=CARTESIAN_POINT('Ctrl Pts',(20.1974932012775,-69.2702386535432,12.));
#65862=CARTESIAN_POINT('Ctrl Pts',(20.183022060135,-69.2507265579562,12.));
#65863=CARTESIAN_POINT('Ctrl Pts',(20.1685947017433,-69.2312339858337,12.));
#65864=CARTESIAN_POINT('Ctrl Pts',(20.1542111474086,-69.2117610665073,12.));
#65865=CARTESIAN_POINT('Ctrl Pts',(20.1398714184278,-69.1923079298534,12.));
#65866=CARTESIAN_POINT('Ctrl Pts',(20.125575536087,-69.172874706296,12.));
#65867=CARTESIAN_POINT('Ctrl Pts',(20.1113235216693,-69.1534615268153,12.));
#65868=CARTESIAN_POINT('Ctrl Pts',(20.0971153964557,-69.1340685229516,12.));
#65869=CARTESIAN_POINT('Ctrl Pts',(20.082951181725,-69.1146958268104,12.));
#65870=CARTESIAN_POINT('Ctrl Pts',(20.0688308987478,-69.0953435710634,12.));
#65871=CARTESIAN_POINT('Ctrl Pts',(20.0547545687839,-69.0760118889525,12.));
#65872=CARTESIAN_POINT('Ctrl Pts',(20.0407222130902,-69.0567009142968,12.));
#65873=CARTESIAN_POINT('Ctrl Pts',(20.026733852922,-69.0374107814977,12.));
#65874=CARTESIAN_POINT('Ctrl Pts',(20.0127895095326,-69.0181416255433,12.));
#65875=CARTESIAN_POINT('Ctrl Pts',(19.9988892041671,-68.9988935820101,12.));
#65876=CARTESIAN_POINT('Ctrl Pts',(19.9850329580599,-68.9796667870667,12.));
#65877=CARTESIAN_POINT('Ctrl Pts',(19.9712207924436,-68.960461377483,12.));
#65878=CARTESIAN_POINT('Ctrl Pts',(19.9574527285492,-68.9412774906346,12.));
#65879=CARTESIAN_POINT('Ctrl Pts',(19.9437287876063,-68.9221152645086,12.));
#65880=CARTESIAN_POINT('Ctrl Pts',(19.9300489908364,-68.902974837704,12.));
#65881=CARTESIAN_POINT('Ctrl Pts',(19.9164133594512,-68.8838563494356,12.));
#65882=CARTESIAN_POINT('Ctrl Pts',(19.9028219146606,-68.8647599395437,12.));
#65883=CARTESIAN_POINT('Ctrl Pts',(19.8892746776733,-68.8456857484988,12.));
#65884=CARTESIAN_POINT('Ctrl Pts',(19.8757716696968,-68.8266339174068,12.));
#65885=CARTESIAN_POINT('Ctrl Pts',(19.8623129119304,-68.8076045880102,12.));
#65886=CARTESIAN_POINT('Ctrl Pts',(19.8488984255641,-68.7885979026927,12.));
#65887=CARTESIAN_POINT('Ctrl Pts',(19.835528231787,-68.7696140044892,12.));
#65888=CARTESIAN_POINT('Ctrl Pts',(19.8222023517874,-68.7506530370918,12.));
#65889=CARTESIAN_POINT('Ctrl Pts',(19.8089208067532,-68.7317151448557,12.));
#65890=CARTESIAN_POINT('Ctrl Pts',(19.795683617864,-68.7128004727998,12.));
#65891=CARTESIAN_POINT('Ctrl Pts',(19.7824908062913,-68.6939091666111,12.));
#65892=CARTESIAN_POINT('Ctrl Pts',(19.7693423932058,-68.6750413726547,12.));
#65893=CARTESIAN_POINT('Ctrl Pts',(19.7562383997781,-68.6561972379793,12.));
#65894=CARTESIAN_POINT('Ctrl Pts',(19.7431788471775,-68.6373769103224,12.));
#65895=CARTESIAN_POINT('Ctrl Pts',(19.7301637565652,-68.6185805381126,12.));
#65896=CARTESIAN_POINT('Ctrl Pts',(19.7171931490956,-68.5998082704766,12.));
#65897=CARTESIAN_POINT('Ctrl Pts',(19.7042670459237,-68.581060257249,12.));
#65898=CARTESIAN_POINT('Ctrl Pts',(19.6913854682046,-68.5623366489779,12.));
#65899=CARTESIAN_POINT('Ctrl Pts',(19.6785484370926,-68.5436375969311,12.));
#65900=CARTESIAN_POINT('Ctrl Pts',(19.6657559737336,-68.5249632530979,12.));
#65901=CARTESIAN_POINT('Ctrl Pts',(19.6530080992686,-68.5063137701971,12.));
#65902=CARTESIAN_POINT('Ctrl Pts',(19.6403048348395,-68.4876893016856,12.));
#65903=CARTESIAN_POINT('Ctrl Pts',(19.6276462015888,-68.4690900017632,12.));
#65904=CARTESIAN_POINT('Ctrl Pts',(19.6150322206577,-68.4505160253778,12.));
#65905=CARTESIAN_POINT('Ctrl Pts',(19.6024629131784,-68.4319675282275,12.));
#65906=CARTESIAN_POINT('Ctrl Pts',(19.5899383002802,-68.4134446667696,12.));
#65907=CARTESIAN_POINT('Ctrl Pts',(19.5774584030937,-68.3949475982335,12.));
#65908=CARTESIAN_POINT('Ctrl Pts',(19.5650232427515,-68.3764764806287,12.));
#65909=CARTESIAN_POINT('Ctrl Pts',(19.5526328403852,-68.3580314727523,12.));
#65910=CARTESIAN_POINT('Ctrl Pts',(19.540287217119,-68.3396127341938,12.));
#65911=CARTESIAN_POINT('Ctrl Pts',(19.5279863940773,-68.3212204253417,12.));
#65912=CARTESIAN_POINT('Ctrl Pts',(19.5157303923856,-68.3028547073865,12.));
#65913=CARTESIAN_POINT('Ctrl Pts',(19.5035192331705,-68.2845157423233,12.));
#65914=CARTESIAN_POINT('Ctrl Pts',(19.4913529375543,-68.2662036929526,12.));
#65915=CARTESIAN_POINT('Ctrl Pts',(19.4792315266501,-68.2479187228803,12.));
#65916=CARTESIAN_POINT('Ctrl Pts',(19.467155021572,-68.2296609965448,12.));
#65917=CARTESIAN_POINT('Ctrl Pts',(19.455123443438,-68.2114306792358,12.));
#65918=CARTESIAN_POINT('Ctrl Pts',(19.4431368133719,-68.1932279371127,12.));
#65919=CARTESIAN_POINT('Ctrl Pts',(19.4311951524983,-68.1750529372232,12.));
#65920=CARTESIAN_POINT('Ctrl Pts',(19.4192984819418,-68.1569058475054,12.));
#65921=CARTESIAN_POINT('Ctrl Pts',(19.4074468228299,-68.1387868367691,12.));
#65922=CARTESIAN_POINT('Ctrl Pts',(19.3956401962894,-68.1206960746769,12.));
#65923=CARTESIAN_POINT('Ctrl Pts',(19.3838786234421,-68.1026337317285,12.));
#65924=CARTESIAN_POINT('Ctrl Pts',(19.3721621253912,-68.0845999792247,12.));
#65925=CARTESIAN_POINT('Ctrl Pts',(19.3604907232313,-68.0665949893195,12.));
#65926=CARTESIAN_POINT('Ctrl Pts',(19.3488644380641,-68.0486189351011,12.));
#65927=CARTESIAN_POINT('Ctrl Pts',(19.3372832910076,-68.0306719906636,12.));
#65928=CARTESIAN_POINT('Ctrl Pts',(19.3257473032034,-68.0127543311776,12.));
#65929=CARTESIAN_POINT('Ctrl Pts',(19.3142564958202,-67.9948661329617,12.));
#65930=CARTESIAN_POINT('Ctrl Pts',(19.302810890038,-67.9770075733485,12.));
#65931=CARTESIAN_POINT('Ctrl Pts',(19.2914105070286,-67.9591788305394,12.));
#65932=CARTESIAN_POINT('Ctrl Pts',(19.280055367936,-67.9413800834793,12.));
#65933=CARTESIAN_POINT('Ctrl Pts',(19.2687454938442,-67.9236115116758,12.));
#65934=CARTESIAN_POINT('Ctrl Pts',(19.2574809057696,-67.9058732951788,12.));
#65935=CARTESIAN_POINT('Ctrl Pts',(19.2462616247279,-67.8881656149955,12.));
#65936=CARTESIAN_POINT('Ctrl Pts',(19.2350876717874,-67.8704886534544,12.));
#65937=CARTESIAN_POINT('Ctrl Pts',(19.2239590681133,-67.8528425945184,12.));
#65938=CARTESIAN_POINT('Ctrl Pts',(19.2128758350345,-67.835227624289,12.));
#65939=CARTESIAN_POINT('Ctrl Pts',(19.201837993993,-67.8176439306621,12.));
#65940=CARTESIAN_POINT('Ctrl Pts',(19.1908455664097,-67.8000917023926,12.));
#65941=CARTESIAN_POINT('Ctrl Pts',(19.1798985735687,-67.7825711283096,12.));
#65942=CARTESIAN_POINT('Ctrl Pts',(19.1689970364949,-67.7650823965127,12.));
#65943=CARTESIAN_POINT('Ctrl Pts',(19.1581409758097,-67.7476256934444,12.));
#65944=CARTESIAN_POINT('Ctrl Pts',(19.1473304119955,-67.7302012056584,12.));
#65945=CARTESIAN_POINT('Ctrl Pts',(19.136565365709,-67.7128091219348,12.));
#65946=CARTESIAN_POINT('Ctrl Pts',(19.1258458580345,-67.6954496350063,12.));
#65947=CARTESIAN_POINT('Ctrl Pts',(19.115171910846,-67.6781229440573,12.));
#65948=CARTESIAN_POINT('Ctrl Pts',(19.1045435468358,-67.6608292549462,12.));
#65949=CARTESIAN_POINT('Ctrl Pts',(19.0939607887501,-67.6435687749841,12.));
#65950=CARTESIAN_POINT('Ctrl Pts',(19.0834236587118,-67.6263417083426,12.));
#65951=CARTESIAN_POINT('Ctrl Pts',(19.072932177628,-67.6091482520534,12.));
#65952=CARTESIAN_POINT('Ctrl Pts',(19.062486364241,-67.5919885896222,12.));
#65953=CARTESIAN_POINT('Ctrl Pts',(19.0520862360395,-67.5748628971964,12.));
#65954=CARTESIAN_POINT('Ctrl Pts',(19.0417318110708,-67.5577713558194,12.));
#65955=CARTESIAN_POINT('Ctrl Pts',(19.0314231093923,-67.540714161288,12.));
#65956=CARTESIAN_POINT('Ctrl Pts',(19.021160154824,-67.5236915360331,12.));
#65957=CARTESIAN_POINT('Ctrl Pts',(19.0109429761306,-67.5067037372317,12.));
#65958=CARTESIAN_POINT('Ctrl Pts',(19.0007716032819,-67.4897510316844,12.));
#65959=CARTESIAN_POINT('Ctrl Pts',(18.9906460638625,-67.472833671964,12.));
#65960=CARTESIAN_POINT('Ctrl Pts',(18.9805663798448,-67.4559518744638,12.));
#65961=CARTESIAN_POINT('Ctrl Pts',(18.970532563171,-67.4391057908418,12.));
#65962=CARTESIAN_POINT('Ctrl Pts',(18.9605446160985,-67.4222955061981,12.));
#65963=CARTESIAN_POINT('Ctrl Pts',(18.9525909517915,-67.4088759497911,12.));
#65964=CARTESIAN_POINT('Ctrl Pts',(18.9466463414299,-67.3988274146651,12.));
#65965=CARTESIAN_POINT('Ctrl Pts',(18.9426924398719,-67.3921355608328,12.));
#65966=CARTESIAN_POINT('Ctrl Pts',(18.9407177820968,-67.3887914263118,12.));
#65967=CARTESIAN_POINT('Ctrl Pts',(23.0342913834072,-70.538251407892,-5.55111512312578E-16));
#65968=CARTESIAN_POINT('Ctrl Pts',(23.0342913834072,-70.538251407892,4.));
#65969=CARTESIAN_POINT('Ctrl Pts',(23.0342913834072,-70.538251407892,8.));
#65970=CARTESIAN_POINT('Ctrl Pts',(23.0342913834072,-70.538251407892,12.));
#65971=CARTESIAN_POINT('Ctrl Pts',(23.0224954570734,-70.6474988907591,-5.55111512312578E-16));
#65972=CARTESIAN_POINT('Ctrl Pts',(23.0224954570734,-70.6474988907591,4.));
#65973=CARTESIAN_POINT('Ctrl Pts',(23.0224954570734,-70.6474988907591,8.00000000000001));
#65974=CARTESIAN_POINT('Ctrl Pts',(23.0224954570734,-70.6474988907591,12.));
#65975=CARTESIAN_POINT('Ctrl Pts',(22.9364730048789,-70.83100071469,-5.55111512312578E-16));
#65976=CARTESIAN_POINT('Ctrl Pts',(22.9364730048789,-70.83100071469,4.));
#65977=CARTESIAN_POINT('Ctrl Pts',(22.9364730048789,-70.83100071469,7.99999999999999));
#65978=CARTESIAN_POINT('Ctrl Pts',(22.9364730048789,-70.83100071469,12.));
#65979=CARTESIAN_POINT('Ctrl Pts',(22.7679558220498,-70.9357242819029,-5.55111512312578E-16));
#65980=CARTESIAN_POINT('Ctrl Pts',(22.7679558220498,-70.9357242819029,4.));
#65981=CARTESIAN_POINT('Ctrl Pts',(22.7679558220498,-70.9357242819029,8.00000000000001));
#65982=CARTESIAN_POINT('Ctrl Pts',(22.7679558220498,-70.9357242819029,12.));
#65983=CARTESIAN_POINT('Ctrl Pts',(22.6894590071812,-70.9608233461354,-5.55111512312578E-16));
#65984=CARTESIAN_POINT('Ctrl Pts',(22.6894590071812,-70.9608233461354,4.));
#65985=CARTESIAN_POINT('Ctrl Pts',(22.6894590071812,-70.9608233461354,8.));
#65986=CARTESIAN_POINT('Ctrl Pts',(22.6894590071812,-70.9608233461354,12.));
#65987=CARTESIAN_POINT('',(23.0342913834072,-70.538251407892,2.77555756156289E-16));
#65988=CARTESIAN_POINT('',(22.6894590071812,-70.9608233461355,0.));
#65989=CARTESIAN_POINT('Ctrl Pts',(23.0342913834072,-70.538251407892,-1.38777878078145E-16));
#65990=CARTESIAN_POINT('Ctrl Pts',(23.0224954570734,-70.6474988907591,-1.38777878078145E-16));
#65991=CARTESIAN_POINT('Ctrl Pts',(22.9733397701051,-70.7523570758625,-1.38777878078144E-16));
#65992=CARTESIAN_POINT('Ctrl Pts',(22.8972470282357,-70.8314917485681,-1.38777878078145E-16));
#65993=CARTESIAN_POINT('Ctrl Pts',(22.8401774718337,-70.8908427530974,-1.38777878078145E-16));
#65994=CARTESIAN_POINT('Ctrl Pts',(22.7679558220498,-70.9357242819029,-1.38777878078145E-16));
#65995=CARTESIAN_POINT('Ctrl Pts',(22.6894590071812,-70.9608233461354,-1.38777878078145E-16));
#65996=CARTESIAN_POINT('',(22.6894590071812,-70.9608233461355,12.));
#65997=CARTESIAN_POINT('Ctrl Pts',(22.6894590071812,-70.9608233461354,-5.55111512312578E-16));
#65998=CARTESIAN_POINT('Ctrl Pts',(22.6894590071812,-70.9608233461354,4.));
#65999=CARTESIAN_POINT('Ctrl Pts',(22.6894590071812,-70.9608233461354,8.));
#66000=CARTESIAN_POINT('Ctrl Pts',(22.6894590071812,-70.9608233461354,12.));
#66001=CARTESIAN_POINT('',(23.0342913834072,-70.538251407892,12.));
#66002=CARTESIAN_POINT('Ctrl Pts',(22.6894590071812,-70.9608233461354,12.));
#66003=CARTESIAN_POINT('Ctrl Pts',(22.7679558220498,-70.9357242819029,12.));
#66004=CARTESIAN_POINT('Ctrl Pts',(22.8401774718337,-70.8908427530974,12.));
#66005=CARTESIAN_POINT('Ctrl Pts',(22.8972470282357,-70.8314917485681,12.));
#66006=CARTESIAN_POINT('Ctrl Pts',(22.9733397701051,-70.7523570758625,12.));
#66007=CARTESIAN_POINT('Ctrl Pts',(23.0224954570734,-70.6474988907591,12.));
#66008=CARTESIAN_POINT('Ctrl Pts',(23.0342913834072,-70.538251407892,12.));
#66009=CARTESIAN_POINT('Ctrl Pts',(23.0342913834072,-70.538251407892,12.));
#66010=CARTESIAN_POINT('Ctrl Pts',(23.0342913834072,-70.538251407892,8.));
#66011=CARTESIAN_POINT('Ctrl Pts',(23.0342913834072,-70.538251407892,4.));
#66012=CARTESIAN_POINT('Ctrl Pts',(23.0342913834072,-70.538251407892,-5.55111512312578E-16));
#66013=CARTESIAN_POINT('Origin',(1.12812358559725E-10,-3.57465004850839E-10,
0.));
#66014=CARTESIAN_POINT('Origin',(1.12812358559725E-10,-3.57465004850839E-10,
12.));
#66015=CARTESIAN_POINT('Origin',(1.12812358559725E-10,-3.57465004850839E-10,
0.));
#66016=CARTESIAN_POINT('Ctrl Pts',(15.8307637747259,-72.7986051948032,-5.55111512312578E-16));
#66017=CARTESIAN_POINT('Ctrl Pts',(15.8307637747259,-72.7986051948032,4.));
#66018=CARTESIAN_POINT('Ctrl Pts',(15.830763774726,-72.7986051948032,8.));
#66019=CARTESIAN_POINT('Ctrl Pts',(15.830763774726,-72.7986051948032,12.));
#66020=CARTESIAN_POINT('Ctrl Pts',(15.7233907508395,-72.8219545017353,-5.55111512312578E-16));
#66021=CARTESIAN_POINT('Ctrl Pts',(15.7233907508395,-72.8219545017353,4.));
#66022=CARTESIAN_POINT('Ctrl Pts',(15.7233907508395,-72.8219545017353,8.));
#66023=CARTESIAN_POINT('Ctrl Pts',(15.7233907508395,-72.8219545017353,12.));
#66024=CARTESIAN_POINT('Ctrl Pts',(15.522104120072,-72.7983622347336,-5.55111512312578E-16));
#66025=CARTESIAN_POINT('Ctrl Pts',(15.522104120072,-72.7983622347336,4.00000000000001));
#66026=CARTESIAN_POINT('Ctrl Pts',(15.522104120072,-72.7983622347336,7.99999999999999));
#66027=CARTESIAN_POINT('Ctrl Pts',(15.522104120072,-72.7983622347336,12.));
#66028=CARTESIAN_POINT('Ctrl Pts',(15.3694736926916,-72.6715981986661,-5.55111512312578E-16));
#66029=CARTESIAN_POINT('Ctrl Pts',(15.3694736926916,-72.6715981986661,4.));
#66030=CARTESIAN_POINT('Ctrl Pts',(15.3694736926916,-72.6715981986661,8.00000000000001));
#66031=CARTESIAN_POINT('Ctrl Pts',(15.3694736926916,-72.6715981986661,12.));
#66032=CARTESIAN_POINT('Ctrl Pts',(15.3208442077189,-72.6050633494351,-5.55111512312578E-16));
#66033=CARTESIAN_POINT('Ctrl Pts',(15.3208442077189,-72.6050633494351,4.));
#66034=CARTESIAN_POINT('Ctrl Pts',(15.3208442077189,-72.605063349435,8.));
#66035=CARTESIAN_POINT('Ctrl Pts',(15.3208442077189,-72.605063349435,12.));
#66036=CARTESIAN_POINT('',(15.8307637747259,-72.7986051948032,0.));
#66037=CARTESIAN_POINT('',(15.3208442077189,-72.6050633494351,2.77555756156289E-16));
#66038=CARTESIAN_POINT('Ctrl Pts',(15.8307637747259,-72.7986051948032,-2.77555756156289E-16));
#66039=CARTESIAN_POINT('Ctrl Pts',(15.7233907508395,-72.8219545017353,-2.77555756156289E-16));
#66040=CARTESIAN_POINT('Ctrl Pts',(15.6083698189723,-72.8084732063058,-2.77555756156289E-16));
#66041=CARTESIAN_POINT('Ctrl Pts',(15.5092366269867,-72.7613031699568,-2.77555756156289E-16));
#66042=CARTESIAN_POINT('Ctrl Pts',(15.4348867329975,-72.7259256426951,-2.77555756156289E-16));
#66043=CARTESIAN_POINT('Ctrl Pts',(15.3694736926916,-72.6715981986661,-2.7755575615629E-16));
#66044=CARTESIAN_POINT('Ctrl Pts',(15.3208442077189,-72.6050633494351,-2.77555756156289E-16));
#66045=CARTESIAN_POINT('',(15.3208442077188,-72.6050633494351,12.));
#66046=CARTESIAN_POINT('Ctrl Pts',(15.3208442077189,-72.6050633494351,-5.55111512312578E-16));
#66047=CARTESIAN_POINT('Ctrl Pts',(15.3208442077189,-72.6050633494351,4.));
#66048=CARTESIAN_POINT('Ctrl Pts',(15.3208442077189,-72.605063349435,8.));
#66049=CARTESIAN_POINT('Ctrl Pts',(15.3208442077189,-72.605063349435,12.));
#66050=CARTESIAN_POINT('',(15.830763774726,-72.7986051948032,12.));
#66051=CARTESIAN_POINT('Ctrl Pts',(15.3208442077189,-72.605063349435,12.));
#66052=CARTESIAN_POINT('Ctrl Pts',(15.3694736926916,-72.6715981986661,12.));
#66053=CARTESIAN_POINT('Ctrl Pts',(15.4348867329975,-72.725925642695,12.));
#66054=CARTESIAN_POINT('Ctrl Pts',(15.5092366269867,-72.7613031699568,12.));
#66055=CARTESIAN_POINT('Ctrl Pts',(15.6083698189723,-72.8084732063058,12.));
#66056=CARTESIAN_POINT('Ctrl Pts',(15.7233907508395,-72.8219545017353,12.));
#66057=CARTESIAN_POINT('Ctrl Pts',(15.830763774726,-72.7986051948032,12.));
#66058=CARTESIAN_POINT('Ctrl Pts',(15.830763774726,-72.7986051948032,12.));
#66059=CARTESIAN_POINT('Ctrl Pts',(15.830763774726,-72.7986051948032,8.));
#66060=CARTESIAN_POINT('Ctrl Pts',(15.8307637747259,-72.7986051948032,4.));
#66061=CARTESIAN_POINT('Ctrl Pts',(15.8307637747259,-72.7986051948032,-5.55111512312578E-16));
#66062=CARTESIAN_POINT('Ctrl Pts',(12.9953224629497,-68.7831490561748,0.));
#66063=CARTESIAN_POINT('Ctrl Pts',(12.9953224629497,-68.7831490561748,12.));
#66064=CARTESIAN_POINT('Ctrl Pts',(12.9969981460277,-68.7866525680193,0.));
#66065=CARTESIAN_POINT('Ctrl Pts',(12.9969981460277,-68.7866525680193,12.));
#66066=CARTESIAN_POINT('Ctrl Pts',(13.0003537683054,-68.7936635625545,0.));
#66067=CARTESIAN_POINT('Ctrl Pts',(13.0003537683054,-68.7936635625545,12.));
#66068=CARTESIAN_POINT('Ctrl Pts',(13.0053999700875,-68.804191966902,0.));
#66069=CARTESIAN_POINT('Ctrl Pts',(13.0053999700875,-68.804191966902,12.));
#66070=CARTESIAN_POINT('Ctrl Pts',(13.0121537768945,-68.8182536653656,0.));
#66071=CARTESIAN_POINT('Ctrl Pts',(13.0121537768945,-68.8182536653656,12.));
#66072=CARTESIAN_POINT('Ctrl Pts',(13.0206386039691,-68.8358704887468,0.));
#66073=CARTESIAN_POINT('Ctrl Pts',(13.0206386039691,-68.8358704887468,12.));
#66074=CARTESIAN_POINT('Ctrl Pts',(13.0291660060107,-68.8535269726793,0.));
#66075=CARTESIAN_POINT('Ctrl Pts',(13.0291660060107,-68.8535269726793,12.));
#66076=CARTESIAN_POINT('Ctrl Pts',(13.0377359881875,-68.8712230321906,0.));
#66077=CARTESIAN_POINT('Ctrl Pts',(13.0377359881875,-68.8712230321906,12.));
#66078=CARTESIAN_POINT('Ctrl Pts',(13.0463485518206,-68.8889585151585,0.));
#66079=CARTESIAN_POINT('Ctrl Pts',(13.0463485518206,-68.8889585151585,12.));
#66080=CARTESIAN_POINT('Ctrl Pts',(13.0550036938813,-68.9067332040985,0.));
#66081=CARTESIAN_POINT('Ctrl Pts',(13.0550036938813,-68.9067332040985,12.));
#66082=CARTESIAN_POINT('Ctrl Pts',(13.0637014089029,-68.9245468449945,0.));
#66083=CARTESIAN_POINT('Ctrl Pts',(13.0637014089029,-68.9245468449945,12.));
#66084=CARTESIAN_POINT('Ctrl Pts',(13.072441690283,-68.9423991694492,0.));
#66085=CARTESIAN_POINT('Ctrl Pts',(13.072441690283,-68.9423991694492,12.));
#66086=CARTESIAN_POINT('Ctrl Pts',(13.0812245317807,-68.9602899187573,0.));
#66087=CARTESIAN_POINT('Ctrl Pts',(13.0812245317807,-68.9602899187573,12.));
#66088=CARTESIAN_POINT('Ctrl Pts',(13.090049929053,-68.9782188692581,0.));
#66089=CARTESIAN_POINT('Ctrl Pts',(13.090049929053,-68.9782188692581,12.));
#66090=CARTESIAN_POINT('Ctrl Pts',(13.0989178791833,-68.9961858241519,0.));
#66091=CARTESIAN_POINT('Ctrl Pts',(13.0989178791833,-68.9961858241519,12.));
#66092=CARTESIAN_POINT('Ctrl Pts',(13.1078283799722,-69.0141906015113,0.));
#66093=CARTESIAN_POINT('Ctrl Pts',(13.1078283799722,-69.0141906015113,12.));
#66094=CARTESIAN_POINT('Ctrl Pts',(13.1167814293497,-69.0322330243348,0.));
#66095=CARTESIAN_POINT('Ctrl Pts',(13.1167814293497,-69.0322330243348,12.));
#66096=CARTESIAN_POINT('Ctrl Pts',(13.1257770246385,-69.0503129081817,0.));
#66097=CARTESIAN_POINT('Ctrl Pts',(13.1257770246385,-69.0503129081817,12.));
#66098=CARTESIAN_POINT('Ctrl Pts',(13.1348151621834,-69.0684300549477,0.));
#66099=CARTESIAN_POINT('Ctrl Pts',(13.1348151621834,-69.0684300549477,12.));
#66100=CARTESIAN_POINT('Ctrl Pts',(13.1438958377404,-69.0865842593102,0.));
#66101=CARTESIAN_POINT('Ctrl Pts',(13.1438958377404,-69.0865842593102,12.));
#66102=CARTESIAN_POINT('Ctrl Pts',(13.1530190467183,-69.1047753127643,0.));
#66103=CARTESIAN_POINT('Ctrl Pts',(13.1530190467183,-69.1047753127643,12.));
#66104=CARTESIAN_POINT('Ctrl Pts',(13.1621847844528,-69.1230030082573,0.));
#66105=CARTESIAN_POINT('Ctrl Pts',(13.1621847844528,-69.1230030082573,12.));
#66106=CARTESIAN_POINT('Ctrl Pts',(13.1713930465132,-69.1412671454564,0.));
#66107=CARTESIAN_POINT('Ctrl Pts',(13.1713930465132,-69.1412671454564,12.));
#66108=CARTESIAN_POINT('Ctrl Pts',(13.1806438286934,-69.1595675305245,0.));
#66109=CARTESIAN_POINT('Ctrl Pts',(13.1806438286934,-69.1595675305245,12.));
#66110=CARTESIAN_POINT('Ctrl Pts',(13.1899371268683,-69.1779039735996,0.));
#66111=CARTESIAN_POINT('Ctrl Pts',(13.1899371268683,-69.1779039735996,12.));
#66112=CARTESIAN_POINT('Ctrl Pts',(13.1992729368928,-69.1962762870527,0.));
#66113=CARTESIAN_POINT('Ctrl Pts',(13.1992729368928,-69.1962762870527,12.));
#66114=CARTESIAN_POINT('Ctrl Pts',(13.2086512544735,-69.2146842833537,0.));
#66115=CARTESIAN_POINT('Ctrl Pts',(13.2086512544735,-69.2146842833537,12.));
#66116=CARTESIAN_POINT('Ctrl Pts',(13.2180720750594,-69.2331277732861,0.));
#66117=CARTESIAN_POINT('Ctrl Pts',(13.2180720750594,-69.2331277732861,12.));
#66118=CARTESIAN_POINT('Ctrl Pts',(13.2275353939051,-69.2516065668844,0.));
#66119=CARTESIAN_POINT('Ctrl Pts',(13.2275353939051,-69.2516065668844,12.));
#66120=CARTESIAN_POINT('Ctrl Pts',(13.237041206122,-69.2701204742449,0.));
#66121=CARTESIAN_POINT('Ctrl Pts',(13.237041206122,-69.2701204742449,12.));
#66122=CARTESIAN_POINT('Ctrl Pts',(13.2465895067262,-69.2886693063182,0.));
#66123=CARTESIAN_POINT('Ctrl Pts',(13.2465895067262,-69.2886693063182,12.));
#66124=CARTESIAN_POINT('Ctrl Pts',(13.2561802906896,-69.3072528758518,0.));
#66125=CARTESIAN_POINT('Ctrl Pts',(13.2561802906896,-69.3072528758518,12.));
#66126=CARTESIAN_POINT('Ctrl Pts',(13.265813552961,-69.3258709977382,0.));
#66127=CARTESIAN_POINT('Ctrl Pts',(13.265813552961,-69.3258709977382,12.));
#66128=CARTESIAN_POINT('Ctrl Pts',(13.2754892884433,-69.3445234885065,0.));
#66129=CARTESIAN_POINT('Ctrl Pts',(13.2754892884433,-69.3445234885065,12.));
#66130=CARTESIAN_POINT('Ctrl Pts',(13.2852074919765,-69.3632101660066,0.));
#66131=CARTESIAN_POINT('Ctrl Pts',(13.2852074919765,-69.3632101660066,12.));
#66132=CARTESIAN_POINT('Ctrl Pts',(13.2949681583167,-69.3819308490422,0.));
#66133=CARTESIAN_POINT('Ctrl Pts',(13.2949681583167,-69.3819308490422,12.));
#66134=CARTESIAN_POINT('Ctrl Pts',(13.3047712821051,-69.4006853569511,0.));
#66135=CARTESIAN_POINT('Ctrl Pts',(13.3047712821051,-69.4006853569511,12.));
#66136=CARTESIAN_POINT('Ctrl Pts',(13.3146168578743,-69.4194735096265,0.));
#66137=CARTESIAN_POINT('Ctrl Pts',(13.3146168578743,-69.4194735096265,12.));
#66138=CARTESIAN_POINT('Ctrl Pts',(13.3245048800643,-69.4382951276998,0.));
#66139=CARTESIAN_POINT('Ctrl Pts',(13.3245048800643,-69.4382951276998,12.));
#66140=CARTESIAN_POINT('Ctrl Pts',(13.3344353430313,-69.4571500326673,0.));
#66141=CARTESIAN_POINT('Ctrl Pts',(13.3344353430313,-69.4571500326673,12.));
#66142=CARTESIAN_POINT('Ctrl Pts',(13.3444082410543,-69.4760380470365,0.));
#66143=CARTESIAN_POINT('Ctrl Pts',(13.3444082410543,-69.4760380470365,12.));
#66144=CARTESIAN_POINT('Ctrl Pts',(13.3544235683393,-69.4949589944606,0.));
#66145=CARTESIAN_POINT('Ctrl Pts',(13.3544235683393,-69.4949589944606,12.));
#66146=CARTESIAN_POINT('Ctrl Pts',(13.3644813190219,-69.5139126996675,0.));
#66147=CARTESIAN_POINT('Ctrl Pts',(13.3644813190219,-69.5139126996675,12.));
#66148=CARTESIAN_POINT('Ctrl Pts',(13.3745814871664,-69.5328989883885,0.));
#66149=CARTESIAN_POINT('Ctrl Pts',(13.3745814871664,-69.5328989883885,12.));
#66150=CARTESIAN_POINT('Ctrl Pts',(13.3847240667627,-69.5519176872862,0.));
#66151=CARTESIAN_POINT('Ctrl Pts',(13.3847240667627,-69.5519176872862,12.));
#66152=CARTESIAN_POINT('Ctrl Pts',(13.3949090517177,-69.5709686238724,0.));
#66153=CARTESIAN_POINT('Ctrl Pts',(13.3949090517177,-69.5709686238724,12.));
#66154=CARTESIAN_POINT('Ctrl Pts',(13.4051364358499,-69.5900516264553,0.));
#66155=CARTESIAN_POINT('Ctrl Pts',(13.4051364358499,-69.5900516264553,12.));
#66156=CARTESIAN_POINT('Ctrl Pts',(13.4154062129002,-69.6091665241765,0.));
#66157=CARTESIAN_POINT('Ctrl Pts',(13.4154062129002,-69.6091665241765,12.));
#66158=CARTESIAN_POINT('Ctrl Pts',(13.4257183765341,-69.6283131470273,0.));
#66159=CARTESIAN_POINT('Ctrl Pts',(13.4257183765341,-69.6283131470273,12.));
#66160=CARTESIAN_POINT('Ctrl Pts',(13.4360729203442,-69.6474913258675,0.));
#66161=CARTESIAN_POINT('Ctrl Pts',(13.4360729203442,-69.6474913258675,12.));
#66162=CARTESIAN_POINT('Ctrl Pts',(13.4464698378453,-69.666700892444,0.));
#66163=CARTESIAN_POINT('Ctrl Pts',(13.4464698378453,-69.666700892444,12.));
#66164=CARTESIAN_POINT('Ctrl Pts',(13.456909122476,-69.6859416793886,0.));
#66165=CARTESIAN_POINT('Ctrl Pts',(13.456909122476,-69.6859416793886,12.));
#66166=CARTESIAN_POINT('Ctrl Pts',(13.4673907676044,-69.7052135201998,0.));
#66167=CARTESIAN_POINT('Ctrl Pts',(13.4673907676044,-69.7052135201998,12.));
#66168=CARTESIAN_POINT('Ctrl Pts',(13.4779147665285,-69.724516249225,0.));
#66169=CARTESIAN_POINT('Ctrl Pts',(13.4779147665285,-69.724516249225,12.));
#66170=CARTESIAN_POINT('Ctrl Pts',(13.4884811124748,-69.7438497016406,0.));
#66171=CARTESIAN_POINT('Ctrl Pts',(13.4884811124748,-69.7438497016406,12.));
#66172=CARTESIAN_POINT('Ctrl Pts',(13.4990897985904,-69.7632137134249,0.));
#66173=CARTESIAN_POINT('Ctrl Pts',(13.4990897985904,-69.7632137134249,12.));
#66174=CARTESIAN_POINT('Ctrl Pts',(13.5097408179479,-69.7826081213576,0.));
#66175=CARTESIAN_POINT('Ctrl Pts',(13.5097408179479,-69.7826081213576,12.));
#66176=CARTESIAN_POINT('Ctrl Pts',(13.5204341635507,-69.8020327630205,0.));
#66177=CARTESIAN_POINT('Ctrl Pts',(13.5204341635507,-69.8020327630205,12.));
#66178=CARTESIAN_POINT('Ctrl Pts',(13.5311698283339,-69.8214874767944,0.));
#66179=CARTESIAN_POINT('Ctrl Pts',(13.5311698283339,-69.8214874767944,12.));
#66180=CARTESIAN_POINT('Ctrl Pts',(13.5419478051625,-69.840972101856,0.));
#66181=CARTESIAN_POINT('Ctrl Pts',(13.5419478051625,-69.840972101856,12.));
#66182=CARTESIAN_POINT('Ctrl Pts',(13.5527680868255,-69.8604864781706,0.));
#66183=CARTESIAN_POINT('Ctrl Pts',(13.5527680868255,-69.8604864781706,12.));
#66184=CARTESIAN_POINT('Ctrl Pts',(13.5636306660421,-69.8800304464882,0.));
#66185=CARTESIAN_POINT('Ctrl Pts',(13.5636306660421,-69.8800304464882,12.));
#66186=CARTESIAN_POINT('Ctrl Pts',(13.5745355354656,-69.8996038483361,0.));
#66187=CARTESIAN_POINT('Ctrl Pts',(13.5745355354656,-69.8996038483361,12.));
#66188=CARTESIAN_POINT('Ctrl Pts',(13.5854826876834,-69.9192065260108,0.));
#66189=CARTESIAN_POINT('Ctrl Pts',(13.5854826876834,-69.9192065260108,12.));
#66190=CARTESIAN_POINT('Ctrl Pts',(13.5964721152135,-69.9388383225648,0.));
#66191=CARTESIAN_POINT('Ctrl Pts',(13.5964721152135,-69.9388383225648,12.));
#66192=CARTESIAN_POINT('Ctrl Pts',(13.6075038104998,-69.9584990817974,0.));
#66193=CARTESIAN_POINT('Ctrl Pts',(13.6075038104998,-69.9584990817974,12.));
#66194=CARTESIAN_POINT('Ctrl Pts',(13.6185777659198,-69.9781886482527,0.));
#66195=CARTESIAN_POINT('Ctrl Pts',(13.6185777659198,-69.9781886482527,12.));
#66196=CARTESIAN_POINT('Ctrl Pts',(13.6296939737865,-69.9979068672153,0.));
#66197=CARTESIAN_POINT('Ctrl Pts',(13.6296939737865,-69.9979068672153,12.));
#66198=CARTESIAN_POINT('Ctrl Pts',(13.6408524263496,-70.0176535847049,0.));
#66199=CARTESIAN_POINT('Ctrl Pts',(13.6408524263496,-70.0176535847049,12.));
#66200=CARTESIAN_POINT('Ctrl Pts',(13.6520531157907,-70.0374286474677,0.));
#66201=CARTESIAN_POINT('Ctrl Pts',(13.6520531157907,-70.0374286474677,12.));
#66202=CARTESIAN_POINT('Ctrl Pts',(13.6632960342196,-70.0572319029676,0.));
#66203=CARTESIAN_POINT('Ctrl Pts',(13.6632960342196,-70.0572319029676,12.));
#66204=CARTESIAN_POINT('Ctrl Pts',(13.6745811736829,-70.0770631993856,0.));
#66205=CARTESIAN_POINT('Ctrl Pts',(13.6745811736829,-70.0770631993856,12.));
#66206=CARTESIAN_POINT('Ctrl Pts',(13.6859085261653,-70.0969223856136,0.));
#66207=CARTESIAN_POINT('Ctrl Pts',(13.6859085261653,-70.0969223856136,12.));
#66208=CARTESIAN_POINT('Ctrl Pts',(13.6972780835897,-70.1168093112486,0.));
#66209=CARTESIAN_POINT('Ctrl Pts',(13.6972780835897,-70.1168093112486,12.));
#66210=CARTESIAN_POINT('Ctrl Pts',(13.7086898378121,-70.1367238265825,0.));
#66211=CARTESIAN_POINT('Ctrl Pts',(13.7086898378121,-70.1367238265825,12.));
#66212=CARTESIAN_POINT('Ctrl Pts',(13.7201437806199,-70.156665782595,0.));
#66213=CARTESIAN_POINT('Ctrl Pts',(13.7201437806199,-70.156665782595,12.));
#66214=CARTESIAN_POINT('Ctrl Pts',(13.7316399037392,-70.1766350309518,0.));
#66215=CARTESIAN_POINT('Ctrl Pts',(13.7316399037392,-70.1766350309518,12.));
#66216=CARTESIAN_POINT('Ctrl Pts',(13.7431781988364,-70.1966314239995,0.));
#66217=CARTESIAN_POINT('Ctrl Pts',(13.7431781988364,-70.1966314239995,12.));
#66218=CARTESIAN_POINT('Ctrl Pts',(13.754758657518,-70.2166548147604,0.));
#66219=CARTESIAN_POINT('Ctrl Pts',(13.754758657518,-70.2166548147604,12.));
#66220=CARTESIAN_POINT('Ctrl Pts',(13.7663812713243,-70.2367050569215,0.));
#66221=CARTESIAN_POINT('Ctrl Pts',(13.7663812713243,-70.2367050569215,12.));
#66222=CARTESIAN_POINT('Ctrl Pts',(13.7780460317294,-70.2567820048303,0.));
#66223=CARTESIAN_POINT('Ctrl Pts',(13.7780460317294,-70.2567820048303,12.));
#66224=CARTESIAN_POINT('Ctrl Pts',(13.7897529301491,-70.2768855134947,0.));
#66225=CARTESIAN_POINT('Ctrl Pts',(13.7897529301491,-70.2768855134947,12.));
#66226=CARTESIAN_POINT('Ctrl Pts',(13.8015019579414,-70.2970154385774,0.));
#66227=CARTESIAN_POINT('Ctrl Pts',(13.8015019579414,-70.2970154385774,12.));
#66228=CARTESIAN_POINT('Ctrl Pts',(13.8132931064063,-70.3171716363897,0.));
#66229=CARTESIAN_POINT('Ctrl Pts',(13.8132931064063,-70.3171716363897,12.));
#66230=CARTESIAN_POINT('Ctrl Pts',(13.825126366779,-70.3373539638809,0.));
#66231=CARTESIAN_POINT('Ctrl Pts',(13.825126366779,-70.3373539638809,12.));
#66232=CARTESIAN_POINT('Ctrl Pts',(13.8370017302309,-70.3575622786335,0.));
#66233=CARTESIAN_POINT('Ctrl Pts',(13.8370017302309,-70.3575622786335,12.));
#66234=CARTESIAN_POINT('Ctrl Pts',(13.8489191878767,-70.3777964388632,0.));
#66235=CARTESIAN_POINT('Ctrl Pts',(13.8489191878767,-70.3777964388632,12.));
#66236=CARTESIAN_POINT('Ctrl Pts',(13.8608787307751,-70.3980563034133,0.));
#66237=CARTESIAN_POINT('Ctrl Pts',(13.8608787307751,-70.3980563034133,12.));
#66238=CARTESIAN_POINT('Ctrl Pts',(13.8728803499287,-70.4183417317499,0.));
#66239=CARTESIAN_POINT('Ctrl Pts',(13.8728803499287,-70.4183417317499,12.));
#66240=CARTESIAN_POINT('Ctrl Pts',(13.8849240362763,-70.4386525839521,0.));
#66241=CARTESIAN_POINT('Ctrl Pts',(13.8849240362763,-70.4386525839521,12.));
#66242=CARTESIAN_POINT('Ctrl Pts',(13.8970097806953,-70.4589887207073,0.));
#66243=CARTESIAN_POINT('Ctrl Pts',(13.8970097806953,-70.4589887207073,12.));
#66244=CARTESIAN_POINT('Ctrl Pts',(13.9091375740088,-70.4793500033124,0.));
#66245=CARTESIAN_POINT('Ctrl Pts',(13.9091375740088,-70.4793500033124,12.));
#66246=CARTESIAN_POINT('Ctrl Pts',(13.9213074069852,-70.4997362936673,0.));
#66247=CARTESIAN_POINT('Ctrl Pts',(13.9213074069852,-70.4997362936673,12.));
#66248=CARTESIAN_POINT('Ctrl Pts',(13.9335192703388,-70.520147454271,0.));
#66249=CARTESIAN_POINT('Ctrl Pts',(13.9335192703388,-70.520147454271,12.));
#66250=CARTESIAN_POINT('Ctrl Pts',(13.9457731547215,-70.5405833482112,0.));
#66251=CARTESIAN_POINT('Ctrl Pts',(13.9457731547215,-70.5405833482112,12.));
#66252=CARTESIAN_POINT('Ctrl Pts',(13.958069050726,-70.5610438391612,0.));
#66253=CARTESIAN_POINT('Ctrl Pts',(13.958069050726,-70.5610438391612,12.));
#66254=CARTESIAN_POINT('Ctrl Pts',(13.9704069488917,-70.5815287913784,0.));
#66255=CARTESIAN_POINT('Ctrl Pts',(13.9704069488917,-70.5815287913784,12.));
#66256=CARTESIAN_POINT('Ctrl Pts',(13.9827868397057,-70.6020380697004,0.));
#66257=CARTESIAN_POINT('Ctrl Pts',(13.9827868397057,-70.6020380697004,12.));
#66258=CARTESIAN_POINT('Ctrl Pts',(13.9952087136018,-70.6225715395394,0.));
#66259=CARTESIAN_POINT('Ctrl Pts',(13.9952087136018,-70.6225715395394,12.));
#66260=CARTESIAN_POINT('Ctrl Pts',(14.0076725609536,-70.6431290668745,0.));
#66261=CARTESIAN_POINT('Ctrl Pts',(14.0076725609536,-70.6431290668745,12.));
#66262=CARTESIAN_POINT('Ctrl Pts',(14.0201783720769,-70.6637105182484,0.));
#66263=CARTESIAN_POINT('Ctrl Pts',(14.0201783720769,-70.6637105182484,12.));
#66264=CARTESIAN_POINT('Ctrl Pts',(14.0327261372362,-70.6843157607668,0.));
#66265=CARTESIAN_POINT('Ctrl Pts',(14.0327261372362,-70.6843157607668,12.));
#66266=CARTESIAN_POINT('Ctrl Pts',(14.0453158466451,-70.7049446620928,0.));
#66267=CARTESIAN_POINT('Ctrl Pts',(14.0453158466451,-70.7049446620928,12.));
#66268=CARTESIAN_POINT('Ctrl Pts',(14.0579474904657,-70.7255970904436,0.));
#66269=CARTESIAN_POINT('Ctrl Pts',(14.0579474904657,-70.7255970904436,12.));
#66270=CARTESIAN_POINT('Ctrl Pts',(14.0706210588016,-70.7462729145807,0.));
#66271=CARTESIAN_POINT('Ctrl Pts',(14.0706210588016,-70.7462729145807,12.));
#66272=CARTESIAN_POINT('Ctrl Pts',(14.0833365416996,-70.7669720038077,0.));
#66273=CARTESIAN_POINT('Ctrl Pts',(14.0833365416996,-70.7669720038077,12.));
#66274=CARTESIAN_POINT('Ctrl Pts',(14.0960939291569,-70.7876942279697,0.));
#66275=CARTESIAN_POINT('Ctrl Pts',(14.0960939291569,-70.7876942279697,12.));
#66276=CARTESIAN_POINT('Ctrl Pts',(14.1088932111214,-70.8084394574493,0.));
#66277=CARTESIAN_POINT('Ctrl Pts',(14.1088932111214,-70.8084394574493,12.));
#66278=CARTESIAN_POINT('Ctrl Pts',(14.1217343774913,-70.8292075631621,0.));
#66279=CARTESIAN_POINT('Ctrl Pts',(14.1217343774913,-70.8292075631621,12.));
#66280=CARTESIAN_POINT('Ctrl Pts',(14.1346174181078,-70.8499984165489,0.));
#66281=CARTESIAN_POINT('Ctrl Pts',(14.1346174181078,-70.8499984165489,12.));
#66282=CARTESIAN_POINT('Ctrl Pts',(14.1475423227568,-70.8708118895715,0.));
#66283=CARTESIAN_POINT('Ctrl Pts',(14.1475423227568,-70.8708118895715,12.));
#66284=CARTESIAN_POINT('Ctrl Pts',(14.1605090811754,-70.8916478547132,0.));
#66285=CARTESIAN_POINT('Ctrl Pts',(14.1605090811754,-70.8916478547132,12.));
#66286=CARTESIAN_POINT('Ctrl Pts',(14.1735176830533,-70.9125061849745,0.));
#66287=CARTESIAN_POINT('Ctrl Pts',(14.1735176830533,-70.9125061849745,12.));
#66288=CARTESIAN_POINT('Ctrl Pts',(14.186568118032,-70.9333867538704,0.));
#66289=CARTESIAN_POINT('Ctrl Pts',(14.186568118032,-70.9333867538704,12.));
#66290=CARTESIAN_POINT('Ctrl Pts',(14.1996603756982,-70.9542894354216,0.));
#66291=CARTESIAN_POINT('Ctrl Pts',(14.1996603756982,-70.9542894354216,12.));
#66292=CARTESIAN_POINT('Ctrl Pts',(14.2127944455838,-70.9752141041518,0.));
#66293=CARTESIAN_POINT('Ctrl Pts',(14.2127944455838,-70.9752141041518,12.));
#66294=CARTESIAN_POINT('Ctrl Pts',(14.2259703171737,-70.9961606350861,0.));
#66295=CARTESIAN_POINT('Ctrl Pts',(14.2259703171737,-70.9961606350861,12.));
#66296=CARTESIAN_POINT('Ctrl Pts',(14.2391879799061,-71.0171289037488,0.));
#66297=CARTESIAN_POINT('Ctrl Pts',(14.2391879799061,-71.0171289037488,12.));
#66298=CARTESIAN_POINT('Ctrl Pts',(14.2524474231732,-71.0381187861588,0.));
#66299=CARTESIAN_POINT('Ctrl Pts',(14.2524474231732,-71.0381187861588,12.));
#66300=CARTESIAN_POINT('Ctrl Pts',(14.2657486363139,-71.0591301588231,0.));
#66301=CARTESIAN_POINT('Ctrl Pts',(14.2657486363139,-71.0591301588231,12.));
#66302=CARTESIAN_POINT('Ctrl Pts',(14.2790916086133,-71.0801628987332,0.));
#66303=CARTESIAN_POINT('Ctrl Pts',(14.2790916086133,-71.0801628987332,12.));
#66304=CARTESIAN_POINT('Ctrl Pts',(14.2924763293105,-71.1012168833643,0.));
#66305=CARTESIAN_POINT('Ctrl Pts',(14.2924763293105,-71.1012168833643,12.));
#66306=CARTESIAN_POINT('Ctrl Pts',(14.3059027875994,-71.1222919906727,0.));
#66307=CARTESIAN_POINT('Ctrl Pts',(14.3059027875994,-71.1222919906727,12.));
#66308=CARTESIAN_POINT('Ctrl Pts',(14.3193709726294,-71.1433880990929,0.));
#66309=CARTESIAN_POINT('Ctrl Pts',(14.3193709726294,-71.1433880990929,12.));
#66310=CARTESIAN_POINT('Ctrl Pts',(14.3328808734989,-71.1645050875308,0.));
#66311=CARTESIAN_POINT('Ctrl Pts',(14.3328808734989,-71.1645050875308,12.));
#66312=CARTESIAN_POINT('Ctrl Pts',(14.3464324792533,-71.1856428353593,0.));
#66313=CARTESIAN_POINT('Ctrl Pts',(14.3464324792533,-71.1856428353593,12.));
#66314=CARTESIAN_POINT('Ctrl Pts',(14.3600257788924,-71.2068012224174,0.));
#66315=CARTESIAN_POINT('Ctrl Pts',(14.3600257788924,-71.2068012224174,12.));
#66316=CARTESIAN_POINT('Ctrl Pts',(14.3736607613722,-71.2279801290084,0.));
#66317=CARTESIAN_POINT('Ctrl Pts',(14.3736607613722,-71.2279801290084,12.));
#66318=CARTESIAN_POINT('Ctrl Pts',(14.3873374156056,-71.2491794358958,0.));
#66319=CARTESIAN_POINT('Ctrl Pts',(14.3873374156056,-71.2491794358958,12.));
#66320=CARTESIAN_POINT('Ctrl Pts',(14.401055730457,-71.2703990242988,0.));
#66321=CARTESIAN_POINT('Ctrl Pts',(14.401055730457,-71.2703990242988,12.));
#66322=CARTESIAN_POINT('Ctrl Pts',(14.4148156947383,-71.2916387758861,0.));
#66323=CARTESIAN_POINT('Ctrl Pts',(14.4148156947383,-71.2916387758861,12.));
#66324=CARTESIAN_POINT('Ctrl Pts',(14.4286172972166,-71.312898572777,0.));
#66325=CARTESIAN_POINT('Ctrl Pts',(14.4286172972166,-71.312898572777,12.));
#66326=CARTESIAN_POINT('Ctrl Pts',(14.4424605266165,-71.3341782975386,0.));
#66327=CARTESIAN_POINT('Ctrl Pts',(14.4424605266165,-71.3341782975386,12.));
#66328=CARTESIAN_POINT('Ctrl Pts',(14.4563453716204,-71.3554778331835,0.));
#66329=CARTESIAN_POINT('Ctrl Pts',(14.4563453716204,-71.3554778331835,12.));
#66330=CARTESIAN_POINT('Ctrl Pts',(14.4702718208651,-71.376797063165,0.));
#66331=CARTESIAN_POINT('Ctrl Pts',(14.4702718208651,-71.376797063165,12.));
#66332=CARTESIAN_POINT('Ctrl Pts',(14.4842398629355,-71.3981358713723,0.));
#66333=CARTESIAN_POINT('Ctrl Pts',(14.4842398629355,-71.3981358713723,12.));
#66334=CARTESIAN_POINT('Ctrl Pts',(14.4982494863718,-71.4194941421292,0.));
#66335=CARTESIAN_POINT('Ctrl Pts',(14.4982494863718,-71.4194941421292,12.));
#66336=CARTESIAN_POINT('Ctrl Pts',(14.5123006796728,-71.4408717601923,0.));
#66337=CARTESIAN_POINT('Ctrl Pts',(14.5123006796728,-71.4408717601923,12.));
#66338=CARTESIAN_POINT('Ctrl Pts',(14.5263934312969,-71.4622686107475,0.));
#66339=CARTESIAN_POINT('Ctrl Pts',(14.5263934312969,-71.4622686107475,12.));
#66340=CARTESIAN_POINT('Ctrl Pts',(14.540527729659,-71.4836845794048,0.));
#66341=CARTESIAN_POINT('Ctrl Pts',(14.540527729659,-71.4836845794048,12.));
#66342=CARTESIAN_POINT('Ctrl Pts',(14.5547035631233,-71.5051195521909,0.));
#66343=CARTESIAN_POINT('Ctrl Pts',(14.5547035631233,-71.5051195521909,12.));
#66344=CARTESIAN_POINT('Ctrl Pts',(14.5689209200091,-71.5265734155498,0.));
#66345=CARTESIAN_POINT('Ctrl Pts',(14.5689209200091,-71.5265734155498,12.));
#66346=CARTESIAN_POINT('Ctrl Pts',(14.5831797885952,-71.5480460563447,0.));
#66347=CARTESIAN_POINT('Ctrl Pts',(14.5831797885952,-71.5480460563447,12.));
#66348=CARTESIAN_POINT('Ctrl Pts',(14.597480157121,-71.5695373618562,0.));
#66349=CARTESIAN_POINT('Ctrl Pts',(14.597480157121,-71.5695373618562,12.));
#66350=CARTESIAN_POINT('Ctrl Pts',(14.6118220137849,-71.5910472197813,0.));
#66351=CARTESIAN_POINT('Ctrl Pts',(14.6118220137849,-71.5910472197813,12.));
#66352=CARTESIAN_POINT('Ctrl Pts',(14.626205346737,-71.612575518229,0.));
#66353=CARTESIAN_POINT('Ctrl Pts',(14.626205346737,-71.612575518229,12.));
#66354=CARTESIAN_POINT('Ctrl Pts',(14.6406301440814,-71.6341221457169,0.));
#66355=CARTESIAN_POINT('Ctrl Pts',(14.6406301440814,-71.6341221457169,12.));
#66356=CARTESIAN_POINT('Ctrl Pts',(14.6550963938829,-71.6556869911662,0.));
#66357=CARTESIAN_POINT('Ctrl Pts',(14.6550963938829,-71.6556869911662,12.));
#66358=CARTESIAN_POINT('Ctrl Pts',(14.6696040841678,-71.6772699438963,0.));
#66359=CARTESIAN_POINT('Ctrl Pts',(14.6696040841678,-71.6772699438963,12.));
#66360=CARTESIAN_POINT('Ctrl Pts',(14.6841532029232,-71.6988708936172,0.));
#66361=CARTESIAN_POINT('Ctrl Pts',(14.6841532029232,-71.6988708936172,12.));
#66362=CARTESIAN_POINT('Ctrl Pts',(14.69874373809,-71.7204897304194,0.));
#66363=CARTESIAN_POINT('Ctrl Pts',(14.69874373809,-71.7204897304194,12.));
#66364=CARTESIAN_POINT('Ctrl Pts',(14.7133756775625,-71.7421263447719,0.));
#66365=CARTESIAN_POINT('Ctrl Pts',(14.7133756775625,-71.7421263447719,12.));
#66366=CARTESIAN_POINT('Ctrl Pts',(14.7280490091957,-71.7637806275328,0.));
#66367=CARTESIAN_POINT('Ctrl Pts',(14.7280490091957,-71.7637806275328,12.));
#66368=CARTESIAN_POINT('Ctrl Pts',(14.7427637208072,-71.7854524699569,0.));
#66369=CARTESIAN_POINT('Ctrl Pts',(14.7427637208072,-71.7854524699569,12.));
#66370=CARTESIAN_POINT('Ctrl Pts',(14.7575198001776,-71.8071417637017,0.));
#66371=CARTESIAN_POINT('Ctrl Pts',(14.7575198001776,-71.8071417637017,12.));
#66372=CARTESIAN_POINT('Ctrl Pts',(14.7723172350451,-71.8288484008333,0.));
#66373=CARTESIAN_POINT('Ctrl Pts',(14.7723172350451,-71.8288484008333,12.));
#66374=CARTESIAN_POINT('Ctrl Pts',(14.7871560131016,-71.8505722738272,0.));
#66375=CARTESIAN_POINT('Ctrl Pts',(14.7871560131016,-71.8505722738272,12.));
#66376=CARTESIAN_POINT('Ctrl Pts',(14.8020361219998,-71.8723132755446,0.));
#66377=CARTESIAN_POINT('Ctrl Pts',(14.8020361219998,-71.8723132755446,12.));
#66378=CARTESIAN_POINT('Ctrl Pts',(14.8169575493557,-71.8940712992109,0.));
#66379=CARTESIAN_POINT('Ctrl Pts',(14.8169575493557,-71.8940712992109,12.));
#66380=CARTESIAN_POINT('Ctrl Pts',(14.8319202827482,-71.9158462383914,0.));
#66381=CARTESIAN_POINT('Ctrl Pts',(14.8319202827482,-71.9158462383914,12.));
#66382=CARTESIAN_POINT('Ctrl Pts',(14.8469243097162,-71.9376379869678,0.));
#66383=CARTESIAN_POINT('Ctrl Pts',(14.8469243097162,-71.9376379869678,12.));
#66384=CARTESIAN_POINT('Ctrl Pts',(14.8619696177506,-71.9594464391078,0.));
#66385=CARTESIAN_POINT('Ctrl Pts',(14.8619696177506,-71.9594464391078,12.));
#66386=CARTESIAN_POINT('Ctrl Pts',(14.8770561943014,-71.9812714893102,0.));
#66387=CARTESIAN_POINT('Ctrl Pts',(14.8770561943014,-71.9812714893102,12.));
#66388=CARTESIAN_POINT('Ctrl Pts',(14.8921840267832,-72.0031130324529,0.));
#66389=CARTESIAN_POINT('Ctrl Pts',(14.8921840267832,-72.0031130324529,12.));
#66390=CARTESIAN_POINT('Ctrl Pts',(14.9073531025764,-72.0249709638422,0.));
#66391=CARTESIAN_POINT('Ctrl Pts',(14.9073531025764,-72.0249709638422,12.));
#66392=CARTESIAN_POINT('Ctrl Pts',(14.9225634090268,-72.0468451792505,0.));
#66393=CARTESIAN_POINT('Ctrl Pts',(14.9225634090268,-72.0468451792505,12.));
#66394=CARTESIAN_POINT('Ctrl Pts',(14.9378149334388,-72.0687355749806,0.));
#66395=CARTESIAN_POINT('Ctrl Pts',(14.9378149334388,-72.0687355749806,12.));
#66396=CARTESIAN_POINT('Ctrl Pts',(14.9531076630767,-72.0906420478076,0.));
#66397=CARTESIAN_POINT('Ctrl Pts',(14.9531076630767,-72.0906420478076,12.));
#66398=CARTESIAN_POINT('Ctrl Pts',(14.9684415851698,-72.112564494854,0.));
#66399=CARTESIAN_POINT('Ctrl Pts',(14.9684415851698,-72.112564494854,12.));
#66400=CARTESIAN_POINT('Ctrl Pts',(14.9838166869107,-72.1345028134777,0.));
#66401=CARTESIAN_POINT('Ctrl Pts',(14.9838166869107,-72.1345028134777,12.));
#66402=CARTESIAN_POINT('Ctrl Pts',(14.9992329554537,-72.1564569011669,0.));
#66403=CARTESIAN_POINT('Ctrl Pts',(14.9992329554537,-72.1564569011669,12.));
#66404=CARTESIAN_POINT('Ctrl Pts',(15.0146903779062,-72.1784266553953,0.));
#66405=CARTESIAN_POINT('Ctrl Pts',(15.0146903779062,-72.1784266553953,12.));
#66406=CARTESIAN_POINT('Ctrl Pts',(15.0301889413257,-72.2004119736115,0.));
#66407=CARTESIAN_POINT('Ctrl Pts',(15.0301889413257,-72.2004119736115,12.));
#66408=CARTESIAN_POINT('Ctrl Pts',(15.0457286327331,-72.2224127535415,0.));
#66409=CARTESIAN_POINT('Ctrl Pts',(15.0457286327331,-72.2224127535415,12.));
#66410=CARTESIAN_POINT('Ctrl Pts',(15.0613094391189,-72.2444288934262,0.));
#66411=CARTESIAN_POINT('Ctrl Pts',(15.0613094391189,-72.2444288934262,12.));
#66412=CARTESIAN_POINT('Ctrl Pts',(15.0769313474476,-72.2664602922852,0.));
#66413=CARTESIAN_POINT('Ctrl Pts',(15.0769313474476,-72.2664602922852,12.));
#66414=CARTESIAN_POINT('Ctrl Pts',(15.0925943446589,-72.2885068501628,0.));
#66415=CARTESIAN_POINT('Ctrl Pts',(15.0925943446589,-72.2885068501628,12.));
#66416=CARTESIAN_POINT('Ctrl Pts',(15.1082984176649,-72.3105684683944,0.));
#66417=CARTESIAN_POINT('Ctrl Pts',(15.1082984176649,-72.3105684683944,12.));
#66418=CARTESIAN_POINT('Ctrl Pts',(15.124043553347,-72.3326450490177,0.));
#66419=CARTESIAN_POINT('Ctrl Pts',(15.124043553347,-72.3326450490177,12.));
#66420=CARTESIAN_POINT('Ctrl Pts',(15.1398297385506,-72.3547364941969,0.));
#66421=CARTESIAN_POINT('Ctrl Pts',(15.1398297385506,-72.3547364941969,12.));
#66422=CARTESIAN_POINT('Ctrl Pts',(15.1556569600744,-72.376842705589,0.));
#66423=CARTESIAN_POINT('Ctrl Pts',(15.1556569600744,-72.376842705589,12.));
#66424=CARTESIAN_POINT('Ctrl Pts',(15.1715252046606,-72.3989635838492,0.));
#66425=CARTESIAN_POINT('Ctrl Pts',(15.1715252046606,-72.3989635838492,12.));
#66426=CARTESIAN_POINT('Ctrl Pts',(15.1874344589725,-72.421099027786,0.));
#66427=CARTESIAN_POINT('Ctrl Pts',(15.1874344589725,-72.421099027786,12.));
#66428=CARTESIAN_POINT('Ctrl Pts',(15.2033847096091,-72.4432489350471,0.));
#66429=CARTESIAN_POINT('Ctrl Pts',(15.2033847096091,-72.4432489350471,12.));
#66430=CARTESIAN_POINT('Ctrl Pts',(15.2193759431372,-72.4654132036428,0.));
#66431=CARTESIAN_POINT('Ctrl Pts',(15.2193759431372,-72.4654132036428,12.));
#66432=CARTESIAN_POINT('Ctrl Pts',(15.235408146116,-72.4875917332761,0.));
#66433=CARTESIAN_POINT('Ctrl Pts',(15.235408146116,-72.4875917332761,12.));
#66434=CARTESIAN_POINT('Ctrl Pts',(15.2514813051172,-72.5097844266075,0.));
#66435=CARTESIAN_POINT('Ctrl Pts',(15.2514813051172,-72.5097844266075,12.));
#66436=CARTESIAN_POINT('Ctrl Pts',(15.2675954067479,-72.5319911908917,0.));
#66437=CARTESIAN_POINT('Ctrl Pts',(15.2675954067479,-72.5319911908917,12.));
#66438=CARTESIAN_POINT('Ctrl Pts',(15.2837504376535,-72.5542119383642,0.));
#66439=CARTESIAN_POINT('Ctrl Pts',(15.2837504376535,-72.5542119383642,12.));
#66440=CARTESIAN_POINT('Ctrl Pts',(15.299946384466,-72.5764465826224,0.));
#66441=CARTESIAN_POINT('Ctrl Pts',(15.299946384466,-72.5764465826224,12.));
#66442=CARTESIAN_POINT('Ctrl Pts',(15.3161832337594,-72.5986950357677,0.));
#66443=CARTESIAN_POINT('Ctrl Pts',(15.3161832337594,-72.5986950357677,12.));
#66444=CARTESIAN_POINT('Ctrl Pts',(15.3324609719955,-72.6209572051042,0.));
#66445=CARTESIAN_POINT('Ctrl Pts',(15.3324609719955,-72.6209572051042,12.));
#66446=CARTESIAN_POINT('Ctrl Pts',(15.3487795854745,-72.6432329903553,0.));
#66447=CARTESIAN_POINT('Ctrl Pts',(15.3487795854745,-72.6432329903553,12.));
#66448=CARTESIAN_POINT('Ctrl Pts',(15.3651390602665,-72.6655222797801,0.));
#66449=CARTESIAN_POINT('Ctrl Pts',(15.3651390602665,-72.6655222797801,12.));
#66450=CARTESIAN_POINT('Ctrl Pts',(15.3815393822736,-72.687824955772,0.));
#66451=CARTESIAN_POINT('Ctrl Pts',(15.3815393822736,-72.687824955772,12.));
#66452=CARTESIAN_POINT('Ctrl Pts',(15.3979805373174,-72.7101409017716,0.));
#66453=CARTESIAN_POINT('Ctrl Pts',(15.3979805373174,-72.7101409017716,12.));
#66454=CARTESIAN_POINT('Ctrl Pts',(15.4144625111944,-72.7324700089712,0.));
#66455=CARTESIAN_POINT('Ctrl Pts',(15.4144625111944,-72.7324700089712,12.));
#66456=CARTESIAN_POINT('Ctrl Pts',(15.4309852897844,-72.7548121825342,0.));
#66457=CARTESIAN_POINT('Ctrl Pts',(15.4309852897844,-72.7548121825342,12.));
#66458=CARTESIAN_POINT('Ctrl Pts',(15.4475488590243,-72.777167349421,0.));
#66459=CARTESIAN_POINT('Ctrl Pts',(15.4475488590243,-72.777167349421,12.));
#66460=CARTESIAN_POINT('Ctrl Pts',(15.4641532053281,-72.7995354603795,0.));
#66461=CARTESIAN_POINT('Ctrl Pts',(15.4641532053281,-72.7995354603795,12.));
#66462=CARTESIAN_POINT('Ctrl Pts',(15.4807983165804,-72.8219164843279,0.));
#66463=CARTESIAN_POINT('Ctrl Pts',(15.4807983165804,-72.8219164843279,12.));
#66464=CARTESIAN_POINT('Ctrl Pts',(15.494147009702,-72.8398316205897,0.));
#66465=CARTESIAN_POINT('Ctrl Pts',(15.494147009702,-72.8398316205897,12.));
#66466=CARTESIAN_POINT('Ctrl Pts',(15.5041768663998,-72.8532737731759,0.));
#66467=CARTESIAN_POINT('Ctrl Pts',(15.5041768663998,-72.8532737731759,12.));
#66468=CARTESIAN_POINT('Ctrl Pts',(15.5108715869141,-72.8622377860824,0.));
#66469=CARTESIAN_POINT('Ctrl Pts',(15.5108715869141,-72.8622377860824,12.));
#66470=CARTESIAN_POINT('Ctrl Pts',(15.5142209845168,-72.8667204369977,0.));
#66471=CARTESIAN_POINT('Ctrl Pts',(15.5142209845168,-72.8667204369977,12.));
#66472=CARTESIAN_POINT('',(12.9953224629497,-68.7831490561748,0.));
#66473=CARTESIAN_POINT('Ctrl Pts',(12.9953224629497,-68.7831490561748,0.));
#66474=CARTESIAN_POINT('Ctrl Pts',(12.9969981460277,-68.7866525680193,0.));
#66475=CARTESIAN_POINT('Ctrl Pts',(13.0003537683054,-68.7936635625545,0.));
#66476=CARTESIAN_POINT('Ctrl Pts',(13.0053999700875,-68.804191966902,0.));
#66477=CARTESIAN_POINT('Ctrl Pts',(13.0121537768945,-68.8182536653656,0.));
#66478=CARTESIAN_POINT('Ctrl Pts',(13.0206386039691,-68.8358704887468,0.));
#66479=CARTESIAN_POINT('Ctrl Pts',(13.0291660060107,-68.8535269726793,0.));
#66480=CARTESIAN_POINT('Ctrl Pts',(13.0377359881875,-68.8712230321906,0.));
#66481=CARTESIAN_POINT('Ctrl Pts',(13.0463485518206,-68.8889585151585,0.));
#66482=CARTESIAN_POINT('Ctrl Pts',(13.0550036938813,-68.9067332040985,0.));
#66483=CARTESIAN_POINT('Ctrl Pts',(13.0637014089029,-68.9245468449945,0.));
#66484=CARTESIAN_POINT('Ctrl Pts',(13.072441690283,-68.9423991694492,0.));
#66485=CARTESIAN_POINT('Ctrl Pts',(13.0812245317807,-68.9602899187573,0.));
#66486=CARTESIAN_POINT('Ctrl Pts',(13.090049929053,-68.9782188692581,0.));
#66487=CARTESIAN_POINT('Ctrl Pts',(13.0989178791833,-68.9961858241519,0.));
#66488=CARTESIAN_POINT('Ctrl Pts',(13.1078283799722,-69.0141906015113,0.));
#66489=CARTESIAN_POINT('Ctrl Pts',(13.1167814293497,-69.0322330243348,0.));
#66490=CARTESIAN_POINT('Ctrl Pts',(13.1257770246385,-69.0503129081817,0.));
#66491=CARTESIAN_POINT('Ctrl Pts',(13.1348151621834,-69.0684300549477,0.));
#66492=CARTESIAN_POINT('Ctrl Pts',(13.1438958377404,-69.0865842593102,0.));
#66493=CARTESIAN_POINT('Ctrl Pts',(13.1530190467183,-69.1047753127643,0.));
#66494=CARTESIAN_POINT('Ctrl Pts',(13.1621847844528,-69.1230030082573,0.));
#66495=CARTESIAN_POINT('Ctrl Pts',(13.1713930465132,-69.1412671454564,0.));
#66496=CARTESIAN_POINT('Ctrl Pts',(13.1806438286934,-69.1595675305245,0.));
#66497=CARTESIAN_POINT('Ctrl Pts',(13.1899371268683,-69.1779039735996,0.));
#66498=CARTESIAN_POINT('Ctrl Pts',(13.1992729368928,-69.1962762870527,0.));
#66499=CARTESIAN_POINT('Ctrl Pts',(13.2086512544735,-69.2146842833537,0.));
#66500=CARTESIAN_POINT('Ctrl Pts',(13.2180720750594,-69.2331277732861,0.));
#66501=CARTESIAN_POINT('Ctrl Pts',(13.2275353939051,-69.2516065668844,0.));
#66502=CARTESIAN_POINT('Ctrl Pts',(13.237041206122,-69.2701204742449,0.));
#66503=CARTESIAN_POINT('Ctrl Pts',(13.2465895067262,-69.2886693063182,0.));
#66504=CARTESIAN_POINT('Ctrl Pts',(13.2561802906896,-69.3072528758518,0.));
#66505=CARTESIAN_POINT('Ctrl Pts',(13.265813552961,-69.3258709977382,0.));
#66506=CARTESIAN_POINT('Ctrl Pts',(13.2754892884433,-69.3445234885065,0.));
#66507=CARTESIAN_POINT('Ctrl Pts',(13.2852074919765,-69.3632101660066,0.));
#66508=CARTESIAN_POINT('Ctrl Pts',(13.2949681583167,-69.3819308490422,0.));
#66509=CARTESIAN_POINT('Ctrl Pts',(13.3047712821051,-69.4006853569511,0.));
#66510=CARTESIAN_POINT('Ctrl Pts',(13.3146168578743,-69.4194735096265,0.));
#66511=CARTESIAN_POINT('Ctrl Pts',(13.3245048800643,-69.4382951276998,0.));
#66512=CARTESIAN_POINT('Ctrl Pts',(13.3344353430313,-69.4571500326673,0.));
#66513=CARTESIAN_POINT('Ctrl Pts',(13.3444082410543,-69.4760380470365,0.));
#66514=CARTESIAN_POINT('Ctrl Pts',(13.3544235683393,-69.4949589944606,0.));
#66515=CARTESIAN_POINT('Ctrl Pts',(13.3644813190219,-69.5139126996675,0.));
#66516=CARTESIAN_POINT('Ctrl Pts',(13.3745814871664,-69.5328989883885,0.));
#66517=CARTESIAN_POINT('Ctrl Pts',(13.3847240667627,-69.5519176872862,0.));
#66518=CARTESIAN_POINT('Ctrl Pts',(13.3949090517177,-69.5709686238724,0.));
#66519=CARTESIAN_POINT('Ctrl Pts',(13.4051364358499,-69.5900516264553,0.));
#66520=CARTESIAN_POINT('Ctrl Pts',(13.4154062129002,-69.6091665241765,0.));
#66521=CARTESIAN_POINT('Ctrl Pts',(13.4257183765341,-69.6283131470273,0.));
#66522=CARTESIAN_POINT('Ctrl Pts',(13.4360729203442,-69.6474913258675,0.));
#66523=CARTESIAN_POINT('Ctrl Pts',(13.4464698378453,-69.666700892444,0.));
#66524=CARTESIAN_POINT('Ctrl Pts',(13.456909122476,-69.6859416793886,0.));
#66525=CARTESIAN_POINT('Ctrl Pts',(13.4673907676044,-69.7052135201998,0.));
#66526=CARTESIAN_POINT('Ctrl Pts',(13.4779147665285,-69.724516249225,0.));
#66527=CARTESIAN_POINT('Ctrl Pts',(13.4884811124748,-69.7438497016406,0.));
#66528=CARTESIAN_POINT('Ctrl Pts',(13.4990897985904,-69.7632137134249,0.));
#66529=CARTESIAN_POINT('Ctrl Pts',(13.5097408179479,-69.7826081213576,0.));
#66530=CARTESIAN_POINT('Ctrl Pts',(13.5204341635507,-69.8020327630205,0.));
#66531=CARTESIAN_POINT('Ctrl Pts',(13.5311698283339,-69.8214874767944,0.));
#66532=CARTESIAN_POINT('Ctrl Pts',(13.5419478051625,-69.840972101856,0.));
#66533=CARTESIAN_POINT('Ctrl Pts',(13.5527680868255,-69.8604864781706,0.));
#66534=CARTESIAN_POINT('Ctrl Pts',(13.5636306660421,-69.8800304464882,0.));
#66535=CARTESIAN_POINT('Ctrl Pts',(13.5745355354656,-69.8996038483361,0.));
#66536=CARTESIAN_POINT('Ctrl Pts',(13.5854826876834,-69.9192065260108,0.));
#66537=CARTESIAN_POINT('Ctrl Pts',(13.5964721152135,-69.9388383225648,0.));
#66538=CARTESIAN_POINT('Ctrl Pts',(13.6075038104998,-69.9584990817974,0.));
#66539=CARTESIAN_POINT('Ctrl Pts',(13.6185777659198,-69.9781886482527,0.));
#66540=CARTESIAN_POINT('Ctrl Pts',(13.6296939737865,-69.9979068672153,0.));
#66541=CARTESIAN_POINT('Ctrl Pts',(13.6408524263496,-70.0176535847049,0.));
#66542=CARTESIAN_POINT('Ctrl Pts',(13.6520531157907,-70.0374286474677,0.));
#66543=CARTESIAN_POINT('Ctrl Pts',(13.6632960342196,-70.0572319029676,0.));
#66544=CARTESIAN_POINT('Ctrl Pts',(13.6745811736829,-70.0770631993856,0.));
#66545=CARTESIAN_POINT('Ctrl Pts',(13.6859085261653,-70.0969223856136,0.));
#66546=CARTESIAN_POINT('Ctrl Pts',(13.6972780835897,-70.1168093112486,0.));
#66547=CARTESIAN_POINT('Ctrl Pts',(13.7086898378121,-70.1367238265825,0.));
#66548=CARTESIAN_POINT('Ctrl Pts',(13.7201437806199,-70.156665782595,0.));
#66549=CARTESIAN_POINT('Ctrl Pts',(13.7316399037392,-70.1766350309518,0.));
#66550=CARTESIAN_POINT('Ctrl Pts',(13.7431781988364,-70.1966314239995,0.));
#66551=CARTESIAN_POINT('Ctrl Pts',(13.754758657518,-70.2166548147604,0.));
#66552=CARTESIAN_POINT('Ctrl Pts',(13.7663812713243,-70.2367050569215,0.));
#66553=CARTESIAN_POINT('Ctrl Pts',(13.7780460317294,-70.2567820048303,0.));
#66554=CARTESIAN_POINT('Ctrl Pts',(13.7897529301491,-70.2768855134947,0.));
#66555=CARTESIAN_POINT('Ctrl Pts',(13.8015019579414,-70.2970154385774,0.));
#66556=CARTESIAN_POINT('Ctrl Pts',(13.8132931064063,-70.3171716363897,0.));
#66557=CARTESIAN_POINT('Ctrl Pts',(13.825126366779,-70.3373539638809,0.));
#66558=CARTESIAN_POINT('Ctrl Pts',(13.8370017302309,-70.3575622786335,0.));
#66559=CARTESIAN_POINT('Ctrl Pts',(13.8489191878767,-70.3777964388632,0.));
#66560=CARTESIAN_POINT('Ctrl Pts',(13.8608787307751,-70.3980563034133,0.));
#66561=CARTESIAN_POINT('Ctrl Pts',(13.8728803499287,-70.4183417317499,0.));
#66562=CARTESIAN_POINT('Ctrl Pts',(13.8849240362763,-70.4386525839521,0.));
#66563=CARTESIAN_POINT('Ctrl Pts',(13.8970097806953,-70.4589887207073,0.));
#66564=CARTESIAN_POINT('Ctrl Pts',(13.9091375740088,-70.4793500033124,0.));
#66565=CARTESIAN_POINT('Ctrl Pts',(13.9213074069852,-70.4997362936673,0.));
#66566=CARTESIAN_POINT('Ctrl Pts',(13.9335192703388,-70.520147454271,0.));
#66567=CARTESIAN_POINT('Ctrl Pts',(13.9457731547215,-70.5405833482112,0.));
#66568=CARTESIAN_POINT('Ctrl Pts',(13.958069050726,-70.5610438391612,0.));
#66569=CARTESIAN_POINT('Ctrl Pts',(13.9704069488917,-70.5815287913784,0.));
#66570=CARTESIAN_POINT('Ctrl Pts',(13.9827868397057,-70.6020380697004,0.));
#66571=CARTESIAN_POINT('Ctrl Pts',(13.9952087136018,-70.6225715395394,0.));
#66572=CARTESIAN_POINT('Ctrl Pts',(14.0076725609536,-70.6431290668745,0.));
#66573=CARTESIAN_POINT('Ctrl Pts',(14.0201783720769,-70.6637105182484,0.));
#66574=CARTESIAN_POINT('Ctrl Pts',(14.0327261372362,-70.6843157607668,0.));
#66575=CARTESIAN_POINT('Ctrl Pts',(14.0453158466451,-70.7049446620928,0.));
#66576=CARTESIAN_POINT('Ctrl Pts',(14.0579474904657,-70.7255970904436,0.));
#66577=CARTESIAN_POINT('Ctrl Pts',(14.0706210588016,-70.7462729145807,0.));
#66578=CARTESIAN_POINT('Ctrl Pts',(14.0833365416996,-70.7669720038077,0.));
#66579=CARTESIAN_POINT('Ctrl Pts',(14.0960939291569,-70.7876942279697,0.));
#66580=CARTESIAN_POINT('Ctrl Pts',(14.1088932111214,-70.8084394574493,0.));
#66581=CARTESIAN_POINT('Ctrl Pts',(14.1217343774913,-70.8292075631621,0.));
#66582=CARTESIAN_POINT('Ctrl Pts',(14.1346174181078,-70.8499984165489,0.));
#66583=CARTESIAN_POINT('Ctrl Pts',(14.1475423227568,-70.8708118895715,0.));
#66584=CARTESIAN_POINT('Ctrl Pts',(14.1605090811754,-70.8916478547132,0.));
#66585=CARTESIAN_POINT('Ctrl Pts',(14.1735176830533,-70.9125061849745,0.));
#66586=CARTESIAN_POINT('Ctrl Pts',(14.186568118032,-70.9333867538704,0.));
#66587=CARTESIAN_POINT('Ctrl Pts',(14.1996603756982,-70.9542894354216,0.));
#66588=CARTESIAN_POINT('Ctrl Pts',(14.2127944455838,-70.9752141041518,0.));
#66589=CARTESIAN_POINT('Ctrl Pts',(14.2259703171737,-70.9961606350861,0.));
#66590=CARTESIAN_POINT('Ctrl Pts',(14.2391879799061,-71.0171289037488,0.));
#66591=CARTESIAN_POINT('Ctrl Pts',(14.2524474231732,-71.0381187861588,0.));
#66592=CARTESIAN_POINT('Ctrl Pts',(14.2657486363139,-71.0591301588231,0.));
#66593=CARTESIAN_POINT('Ctrl Pts',(14.2790916086133,-71.0801628987332,0.));
#66594=CARTESIAN_POINT('Ctrl Pts',(14.2924763293105,-71.1012168833643,0.));
#66595=CARTESIAN_POINT('Ctrl Pts',(14.3059027875994,-71.1222919906727,0.));
#66596=CARTESIAN_POINT('Ctrl Pts',(14.3193709726294,-71.1433880990929,0.));
#66597=CARTESIAN_POINT('Ctrl Pts',(14.3328808734989,-71.1645050875308,0.));
#66598=CARTESIAN_POINT('Ctrl Pts',(14.3464324792533,-71.1856428353593,0.));
#66599=CARTESIAN_POINT('Ctrl Pts',(14.3600257788924,-71.2068012224174,0.));
#66600=CARTESIAN_POINT('Ctrl Pts',(14.3736607613722,-71.2279801290084,0.));
#66601=CARTESIAN_POINT('Ctrl Pts',(14.3873374156056,-71.2491794358958,0.));
#66602=CARTESIAN_POINT('Ctrl Pts',(14.401055730457,-71.2703990242988,0.));
#66603=CARTESIAN_POINT('Ctrl Pts',(14.4148156947383,-71.2916387758861,0.));
#66604=CARTESIAN_POINT('Ctrl Pts',(14.4286172972166,-71.312898572777,0.));
#66605=CARTESIAN_POINT('Ctrl Pts',(14.4424605266165,-71.3341782975386,0.));
#66606=CARTESIAN_POINT('Ctrl Pts',(14.4563453716204,-71.3554778331835,0.));
#66607=CARTESIAN_POINT('Ctrl Pts',(14.4702718208651,-71.376797063165,0.));
#66608=CARTESIAN_POINT('Ctrl Pts',(14.4842398629355,-71.3981358713723,0.));
#66609=CARTESIAN_POINT('Ctrl Pts',(14.4982494863718,-71.4194941421292,0.));
#66610=CARTESIAN_POINT('Ctrl Pts',(14.5123006796728,-71.4408717601923,0.));
#66611=CARTESIAN_POINT('Ctrl Pts',(14.5263934312969,-71.4622686107475,0.));
#66612=CARTESIAN_POINT('Ctrl Pts',(14.540527729659,-71.4836845794048,0.));
#66613=CARTESIAN_POINT('Ctrl Pts',(14.5547035631233,-71.5051195521909,0.));
#66614=CARTESIAN_POINT('Ctrl Pts',(14.5689209200091,-71.5265734155498,0.));
#66615=CARTESIAN_POINT('Ctrl Pts',(14.5831797885952,-71.5480460563447,0.));
#66616=CARTESIAN_POINT('Ctrl Pts',(14.597480157121,-71.5695373618562,0.));
#66617=CARTESIAN_POINT('Ctrl Pts',(14.6118220137849,-71.5910472197813,0.));
#66618=CARTESIAN_POINT('Ctrl Pts',(14.626205346737,-71.612575518229,0.));
#66619=CARTESIAN_POINT('Ctrl Pts',(14.6406301440814,-71.6341221457169,0.));
#66620=CARTESIAN_POINT('Ctrl Pts',(14.6550963938829,-71.6556869911662,0.));
#66621=CARTESIAN_POINT('Ctrl Pts',(14.6696040841678,-71.6772699438963,0.));
#66622=CARTESIAN_POINT('Ctrl Pts',(14.6841532029232,-71.6988708936172,0.));
#66623=CARTESIAN_POINT('Ctrl Pts',(14.69874373809,-71.7204897304194,0.));
#66624=CARTESIAN_POINT('Ctrl Pts',(14.7133756775625,-71.7421263447719,0.));
#66625=CARTESIAN_POINT('Ctrl Pts',(14.7280490091957,-71.7637806275328,0.));
#66626=CARTESIAN_POINT('Ctrl Pts',(14.7427637208072,-71.7854524699569,0.));
#66627=CARTESIAN_POINT('Ctrl Pts',(14.7575198001776,-71.8071417637017,0.));
#66628=CARTESIAN_POINT('Ctrl Pts',(14.7723172350451,-71.8288484008333,0.));
#66629=CARTESIAN_POINT('Ctrl Pts',(14.7871560131016,-71.8505722738272,0.));
#66630=CARTESIAN_POINT('Ctrl Pts',(14.8020361219998,-71.8723132755446,0.));
#66631=CARTESIAN_POINT('Ctrl Pts',(14.8169575493557,-71.8940712992109,0.));
#66632=CARTESIAN_POINT('Ctrl Pts',(14.8319202827482,-71.9158462383914,0.));
#66633=CARTESIAN_POINT('Ctrl Pts',(14.8469243097162,-71.9376379869678,0.));
#66634=CARTESIAN_POINT('Ctrl Pts',(14.8619696177506,-71.9594464391078,0.));
#66635=CARTESIAN_POINT('Ctrl Pts',(14.8770561943014,-71.9812714893102,0.));
#66636=CARTESIAN_POINT('Ctrl Pts',(14.8921840267832,-72.0031130324529,0.));
#66637=CARTESIAN_POINT('Ctrl Pts',(14.9073531025764,-72.0249709638422,0.));
#66638=CARTESIAN_POINT('Ctrl Pts',(14.9225634090268,-72.0468451792505,0.));
#66639=CARTESIAN_POINT('Ctrl Pts',(14.9378149334388,-72.0687355749806,0.));
#66640=CARTESIAN_POINT('Ctrl Pts',(14.9531076630767,-72.0906420478076,0.));
#66641=CARTESIAN_POINT('Ctrl Pts',(14.9684415851698,-72.112564494854,0.));
#66642=CARTESIAN_POINT('Ctrl Pts',(14.9838166869107,-72.1345028134777,0.));
#66643=CARTESIAN_POINT('Ctrl Pts',(14.9992329554537,-72.1564569011669,0.));
#66644=CARTESIAN_POINT('Ctrl Pts',(15.0146903779062,-72.1784266553953,0.));
#66645=CARTESIAN_POINT('Ctrl Pts',(15.0301889413257,-72.2004119736115,0.));
#66646=CARTESIAN_POINT('Ctrl Pts',(15.0457286327331,-72.2224127535415,0.));
#66647=CARTESIAN_POINT('Ctrl Pts',(15.0613094391189,-72.2444288934262,0.));
#66648=CARTESIAN_POINT('Ctrl Pts',(15.0769313474476,-72.2664602922852,0.));
#66649=CARTESIAN_POINT('Ctrl Pts',(15.0925943446589,-72.2885068501628,0.));
#66650=CARTESIAN_POINT('Ctrl Pts',(15.1082984176649,-72.3105684683944,0.));
#66651=CARTESIAN_POINT('Ctrl Pts',(15.124043553347,-72.3326450490177,0.));
#66652=CARTESIAN_POINT('Ctrl Pts',(15.1398297385506,-72.3547364941969,0.));
#66653=CARTESIAN_POINT('Ctrl Pts',(15.1556569600744,-72.376842705589,0.));
#66654=CARTESIAN_POINT('Ctrl Pts',(15.1715252046606,-72.3989635838492,0.));
#66655=CARTESIAN_POINT('Ctrl Pts',(15.1874344589725,-72.421099027786,0.));
#66656=CARTESIAN_POINT('Ctrl Pts',(15.2033847096091,-72.4432489350471,0.));
#66657=CARTESIAN_POINT('Ctrl Pts',(15.2193759431372,-72.4654132036428,0.));
#66658=CARTESIAN_POINT('Ctrl Pts',(15.235408146116,-72.4875917332761,0.));
#66659=CARTESIAN_POINT('Ctrl Pts',(15.2514813051172,-72.5097844266075,0.));
#66660=CARTESIAN_POINT('Ctrl Pts',(15.2675954067479,-72.5319911908917,0.));
#66661=CARTESIAN_POINT('Ctrl Pts',(15.2837504376535,-72.5542119383642,0.));
#66662=CARTESIAN_POINT('Ctrl Pts',(15.297633502478,-72.5732713370618,0.));
#66663=CARTESIAN_POINT('Ctrl Pts',(15.3082994603539,-72.5878912620439,0.));
#66664=CARTESIAN_POINT('Ctrl Pts',(15.3157301930682,-72.5980655789635,0.));
#66665=CARTESIAN_POINT('Ctrl Pts',(15.3199137230129,-72.6037902604921,0.));
#66666=CARTESIAN_POINT('Ctrl Pts',(15.3208442077189,-72.6050633494351,0.));
#66667=CARTESIAN_POINT('',(12.9953224629497,-68.7831490561748,12.));
#66668=CARTESIAN_POINT('',(12.9953224629497,-68.7831490561748,0.));
#66669=CARTESIAN_POINT('Ctrl Pts',(15.3208442077188,-72.6050633494351,12.));
#66670=CARTESIAN_POINT('Ctrl Pts',(15.3199137230129,-72.603790260492,12.));
#66671=CARTESIAN_POINT('Ctrl Pts',(15.3157301930681,-72.5980655789635,12.));
#66672=CARTESIAN_POINT('Ctrl Pts',(15.3082994603539,-72.5878912620439,12.));
#66673=CARTESIAN_POINT('Ctrl Pts',(15.297633502478,-72.5732713370618,12.));
#66674=CARTESIAN_POINT('Ctrl Pts',(15.2837504376535,-72.5542119383642,12.));
#66675=CARTESIAN_POINT('Ctrl Pts',(15.2675954067479,-72.5319911908917,12.));
#66676=CARTESIAN_POINT('Ctrl Pts',(15.2514813051172,-72.5097844266075,12.));
#66677=CARTESIAN_POINT('Ctrl Pts',(15.235408146116,-72.4875917332761,12.));
#66678=CARTESIAN_POINT('Ctrl Pts',(15.2193759431372,-72.4654132036428,12.));
#66679=CARTESIAN_POINT('Ctrl Pts',(15.2033847096091,-72.4432489350471,12.));
#66680=CARTESIAN_POINT('Ctrl Pts',(15.1874344589725,-72.421099027786,12.));
#66681=CARTESIAN_POINT('Ctrl Pts',(15.1715252046606,-72.3989635838492,12.));
#66682=CARTESIAN_POINT('Ctrl Pts',(15.1556569600744,-72.376842705589,12.));
#66683=CARTESIAN_POINT('Ctrl Pts',(15.1398297385506,-72.3547364941969,12.));
#66684=CARTESIAN_POINT('Ctrl Pts',(15.124043553347,-72.3326450490177,12.));
#66685=CARTESIAN_POINT('Ctrl Pts',(15.1082984176649,-72.3105684683944,12.));
#66686=CARTESIAN_POINT('Ctrl Pts',(15.0925943446589,-72.2885068501628,12.));
#66687=CARTESIAN_POINT('Ctrl Pts',(15.0769313474476,-72.2664602922852,12.));
#66688=CARTESIAN_POINT('Ctrl Pts',(15.0613094391189,-72.2444288934262,12.));
#66689=CARTESIAN_POINT('Ctrl Pts',(15.0457286327331,-72.2224127535415,12.));
#66690=CARTESIAN_POINT('Ctrl Pts',(15.0301889413257,-72.2004119736115,12.));
#66691=CARTESIAN_POINT('Ctrl Pts',(15.0146903779062,-72.1784266553953,12.));
#66692=CARTESIAN_POINT('Ctrl Pts',(14.9992329554537,-72.1564569011669,12.));
#66693=CARTESIAN_POINT('Ctrl Pts',(14.9838166869107,-72.1345028134777,12.));
#66694=CARTESIAN_POINT('Ctrl Pts',(14.9684415851698,-72.112564494854,12.));
#66695=CARTESIAN_POINT('Ctrl Pts',(14.9531076630767,-72.0906420478076,12.));
#66696=CARTESIAN_POINT('Ctrl Pts',(14.9378149334388,-72.0687355749806,12.));
#66697=CARTESIAN_POINT('Ctrl Pts',(14.9225634090268,-72.0468451792505,12.));
#66698=CARTESIAN_POINT('Ctrl Pts',(14.9073531025764,-72.0249709638422,12.));
#66699=CARTESIAN_POINT('Ctrl Pts',(14.8921840267832,-72.0031130324529,12.));
#66700=CARTESIAN_POINT('Ctrl Pts',(14.8770561943014,-71.9812714893102,12.));
#66701=CARTESIAN_POINT('Ctrl Pts',(14.8619696177506,-71.9594464391078,12.));
#66702=CARTESIAN_POINT('Ctrl Pts',(14.8469243097162,-71.9376379869678,12.));
#66703=CARTESIAN_POINT('Ctrl Pts',(14.8319202827482,-71.9158462383914,12.));
#66704=CARTESIAN_POINT('Ctrl Pts',(14.8169575493557,-71.8940712992109,12.));
#66705=CARTESIAN_POINT('Ctrl Pts',(14.8020361219998,-71.8723132755446,12.));
#66706=CARTESIAN_POINT('Ctrl Pts',(14.7871560131016,-71.8505722738272,12.));
#66707=CARTESIAN_POINT('Ctrl Pts',(14.7723172350451,-71.8288484008333,12.));
#66708=CARTESIAN_POINT('Ctrl Pts',(14.7575198001776,-71.8071417637017,12.));
#66709=CARTESIAN_POINT('Ctrl Pts',(14.7427637208072,-71.7854524699569,12.));
#66710=CARTESIAN_POINT('Ctrl Pts',(14.7280490091957,-71.7637806275328,12.));
#66711=CARTESIAN_POINT('Ctrl Pts',(14.7133756775625,-71.7421263447719,12.));
#66712=CARTESIAN_POINT('Ctrl Pts',(14.69874373809,-71.7204897304194,12.));
#66713=CARTESIAN_POINT('Ctrl Pts',(14.6841532029232,-71.6988708936172,12.));
#66714=CARTESIAN_POINT('Ctrl Pts',(14.6696040841678,-71.6772699438963,12.));
#66715=CARTESIAN_POINT('Ctrl Pts',(14.6550963938829,-71.6556869911662,12.));
#66716=CARTESIAN_POINT('Ctrl Pts',(14.6406301440814,-71.6341221457169,12.));
#66717=CARTESIAN_POINT('Ctrl Pts',(14.626205346737,-71.612575518229,12.));
#66718=CARTESIAN_POINT('Ctrl Pts',(14.6118220137849,-71.5910472197813,12.));
#66719=CARTESIAN_POINT('Ctrl Pts',(14.597480157121,-71.5695373618562,12.));
#66720=CARTESIAN_POINT('Ctrl Pts',(14.5831797885952,-71.5480460563447,12.));
#66721=CARTESIAN_POINT('Ctrl Pts',(14.5689209200091,-71.5265734155498,12.));
#66722=CARTESIAN_POINT('Ctrl Pts',(14.5547035631233,-71.5051195521909,12.));
#66723=CARTESIAN_POINT('Ctrl Pts',(14.540527729659,-71.4836845794048,12.));
#66724=CARTESIAN_POINT('Ctrl Pts',(14.5263934312969,-71.4622686107475,12.));
#66725=CARTESIAN_POINT('Ctrl Pts',(14.5123006796728,-71.4408717601923,12.));
#66726=CARTESIAN_POINT('Ctrl Pts',(14.4982494863718,-71.4194941421292,12.));
#66727=CARTESIAN_POINT('Ctrl Pts',(14.4842398629355,-71.3981358713723,12.));
#66728=CARTESIAN_POINT('Ctrl Pts',(14.4702718208651,-71.376797063165,12.));
#66729=CARTESIAN_POINT('Ctrl Pts',(14.4563453716204,-71.3554778331835,12.));
#66730=CARTESIAN_POINT('Ctrl Pts',(14.4424605266165,-71.3341782975386,12.));
#66731=CARTESIAN_POINT('Ctrl Pts',(14.4286172972166,-71.312898572777,12.));
#66732=CARTESIAN_POINT('Ctrl Pts',(14.4148156947383,-71.2916387758861,12.));
#66733=CARTESIAN_POINT('Ctrl Pts',(14.401055730457,-71.2703990242988,12.));
#66734=CARTESIAN_POINT('Ctrl Pts',(14.3873374156056,-71.2491794358958,12.));
#66735=CARTESIAN_POINT('Ctrl Pts',(14.3736607613722,-71.2279801290084,12.));
#66736=CARTESIAN_POINT('Ctrl Pts',(14.3600257788924,-71.2068012224174,12.));
#66737=CARTESIAN_POINT('Ctrl Pts',(14.3464324792533,-71.1856428353593,12.));
#66738=CARTESIAN_POINT('Ctrl Pts',(14.3328808734989,-71.1645050875308,12.));
#66739=CARTESIAN_POINT('Ctrl Pts',(14.3193709726294,-71.1433880990929,12.));
#66740=CARTESIAN_POINT('Ctrl Pts',(14.3059027875994,-71.1222919906727,12.));
#66741=CARTESIAN_POINT('Ctrl Pts',(14.2924763293105,-71.1012168833643,12.));
#66742=CARTESIAN_POINT('Ctrl Pts',(14.2790916086133,-71.0801628987332,12.));
#66743=CARTESIAN_POINT('Ctrl Pts',(14.2657486363139,-71.0591301588231,12.));
#66744=CARTESIAN_POINT('Ctrl Pts',(14.2524474231732,-71.0381187861588,12.));
#66745=CARTESIAN_POINT('Ctrl Pts',(14.2391879799061,-71.0171289037488,12.));
#66746=CARTESIAN_POINT('Ctrl Pts',(14.2259703171737,-70.9961606350861,12.));
#66747=CARTESIAN_POINT('Ctrl Pts',(14.2127944455838,-70.9752141041518,12.));
#66748=CARTESIAN_POINT('Ctrl Pts',(14.1996603756982,-70.9542894354216,12.));
#66749=CARTESIAN_POINT('Ctrl Pts',(14.186568118032,-70.9333867538704,12.));
#66750=CARTESIAN_POINT('Ctrl Pts',(14.1735176830533,-70.9125061849745,12.));
#66751=CARTESIAN_POINT('Ctrl Pts',(14.1605090811754,-70.8916478547132,12.));
#66752=CARTESIAN_POINT('Ctrl Pts',(14.1475423227568,-70.8708118895715,12.));
#66753=CARTESIAN_POINT('Ctrl Pts',(14.1346174181078,-70.8499984165489,12.));
#66754=CARTESIAN_POINT('Ctrl Pts',(14.1217343774913,-70.8292075631621,12.));
#66755=CARTESIAN_POINT('Ctrl Pts',(14.1088932111214,-70.8084394574493,12.));
#66756=CARTESIAN_POINT('Ctrl Pts',(14.0960939291569,-70.7876942279697,12.));
#66757=CARTESIAN_POINT('Ctrl Pts',(14.0833365416996,-70.7669720038077,12.));
#66758=CARTESIAN_POINT('Ctrl Pts',(14.0706210588016,-70.7462729145807,12.));
#66759=CARTESIAN_POINT('Ctrl Pts',(14.0579474904657,-70.7255970904436,12.));
#66760=CARTESIAN_POINT('Ctrl Pts',(14.0453158466451,-70.7049446620928,12.));
#66761=CARTESIAN_POINT('Ctrl Pts',(14.0327261372362,-70.6843157607668,12.));
#66762=CARTESIAN_POINT('Ctrl Pts',(14.0201783720769,-70.6637105182484,12.));
#66763=CARTESIAN_POINT('Ctrl Pts',(14.0076725609536,-70.6431290668745,12.));
#66764=CARTESIAN_POINT('Ctrl Pts',(13.9952087136018,-70.6225715395394,12.));
#66765=CARTESIAN_POINT('Ctrl Pts',(13.9827868397057,-70.6020380697004,12.));
#66766=CARTESIAN_POINT('Ctrl Pts',(13.9704069488917,-70.5815287913784,12.));
#66767=CARTESIAN_POINT('Ctrl Pts',(13.958069050726,-70.5610438391612,12.));
#66768=CARTESIAN_POINT('Ctrl Pts',(13.9457731547215,-70.5405833482112,12.));
#66769=CARTESIAN_POINT('Ctrl Pts',(13.9335192703388,-70.520147454271,12.));
#66770=CARTESIAN_POINT('Ctrl Pts',(13.9213074069852,-70.4997362936673,12.));
#66771=CARTESIAN_POINT('Ctrl Pts',(13.9091375740088,-70.4793500033124,12.));
#66772=CARTESIAN_POINT('Ctrl Pts',(13.8970097806953,-70.4589887207073,12.));
#66773=CARTESIAN_POINT('Ctrl Pts',(13.8849240362763,-70.4386525839521,12.));
#66774=CARTESIAN_POINT('Ctrl Pts',(13.8728803499287,-70.4183417317499,12.));
#66775=CARTESIAN_POINT('Ctrl Pts',(13.8608787307751,-70.3980563034133,12.));
#66776=CARTESIAN_POINT('Ctrl Pts',(13.8489191878767,-70.3777964388632,12.));
#66777=CARTESIAN_POINT('Ctrl Pts',(13.8370017302309,-70.3575622786335,12.));
#66778=CARTESIAN_POINT('Ctrl Pts',(13.825126366779,-70.3373539638809,12.));
#66779=CARTESIAN_POINT('Ctrl Pts',(13.8132931064063,-70.3171716363897,12.));
#66780=CARTESIAN_POINT('Ctrl Pts',(13.8015019579414,-70.2970154385774,12.));
#66781=CARTESIAN_POINT('Ctrl Pts',(13.7897529301491,-70.2768855134947,12.));
#66782=CARTESIAN_POINT('Ctrl Pts',(13.7780460317294,-70.2567820048303,12.));
#66783=CARTESIAN_POINT('Ctrl Pts',(13.7663812713243,-70.2367050569215,12.));
#66784=CARTESIAN_POINT('Ctrl Pts',(13.754758657518,-70.2166548147604,12.));
#66785=CARTESIAN_POINT('Ctrl Pts',(13.7431781988364,-70.1966314239995,12.));
#66786=CARTESIAN_POINT('Ctrl Pts',(13.7316399037392,-70.1766350309518,12.));
#66787=CARTESIAN_POINT('Ctrl Pts',(13.7201437806199,-70.156665782595,12.));
#66788=CARTESIAN_POINT('Ctrl Pts',(13.7086898378121,-70.1367238265825,12.));
#66789=CARTESIAN_POINT('Ctrl Pts',(13.6972780835897,-70.1168093112486,12.));
#66790=CARTESIAN_POINT('Ctrl Pts',(13.6859085261653,-70.0969223856136,12.));
#66791=CARTESIAN_POINT('Ctrl Pts',(13.6745811736829,-70.0770631993856,12.));
#66792=CARTESIAN_POINT('Ctrl Pts',(13.6632960342196,-70.0572319029676,12.));
#66793=CARTESIAN_POINT('Ctrl Pts',(13.6520531157907,-70.0374286474677,12.));
#66794=CARTESIAN_POINT('Ctrl Pts',(13.6408524263496,-70.0176535847049,12.));
#66795=CARTESIAN_POINT('Ctrl Pts',(13.6296939737865,-69.9979068672153,12.));
#66796=CARTESIAN_POINT('Ctrl Pts',(13.6185777659198,-69.9781886482527,12.));
#66797=CARTESIAN_POINT('Ctrl Pts',(13.6075038104998,-69.9584990817974,12.));
#66798=CARTESIAN_POINT('Ctrl Pts',(13.5964721152135,-69.9388383225648,12.));
#66799=CARTESIAN_POINT('Ctrl Pts',(13.5854826876834,-69.9192065260108,12.));
#66800=CARTESIAN_POINT('Ctrl Pts',(13.5745355354656,-69.8996038483361,12.));
#66801=CARTESIAN_POINT('Ctrl Pts',(13.5636306660421,-69.8800304464882,12.));
#66802=CARTESIAN_POINT('Ctrl Pts',(13.5527680868255,-69.8604864781706,12.));
#66803=CARTESIAN_POINT('Ctrl Pts',(13.5419478051625,-69.840972101856,12.));
#66804=CARTESIAN_POINT('Ctrl Pts',(13.5311698283339,-69.8214874767944,12.));
#66805=CARTESIAN_POINT('Ctrl Pts',(13.5204341635507,-69.8020327630205,12.));
#66806=CARTESIAN_POINT('Ctrl Pts',(13.5097408179479,-69.7826081213576,12.));
#66807=CARTESIAN_POINT('Ctrl Pts',(13.4990897985904,-69.7632137134249,12.));
#66808=CARTESIAN_POINT('Ctrl Pts',(13.4884811124748,-69.7438497016406,12.));
#66809=CARTESIAN_POINT('Ctrl Pts',(13.4779147665285,-69.724516249225,12.));
#66810=CARTESIAN_POINT('Ctrl Pts',(13.4673907676044,-69.7052135201998,12.));
#66811=CARTESIAN_POINT('Ctrl Pts',(13.456909122476,-69.6859416793886,12.));
#66812=CARTESIAN_POINT('Ctrl Pts',(13.4464698378453,-69.666700892444,12.));
#66813=CARTESIAN_POINT('Ctrl Pts',(13.4360729203442,-69.6474913258675,12.));
#66814=CARTESIAN_POINT('Ctrl Pts',(13.4257183765341,-69.6283131470273,12.));
#66815=CARTESIAN_POINT('Ctrl Pts',(13.4154062129002,-69.6091665241765,12.));
#66816=CARTESIAN_POINT('Ctrl Pts',(13.4051364358499,-69.5900516264553,12.));
#66817=CARTESIAN_POINT('Ctrl Pts',(13.3949090517177,-69.5709686238724,12.));
#66818=CARTESIAN_POINT('Ctrl Pts',(13.3847240667627,-69.5519176872862,12.));
#66819=CARTESIAN_POINT('Ctrl Pts',(13.3745814871664,-69.5328989883885,12.));
#66820=CARTESIAN_POINT('Ctrl Pts',(13.3644813190219,-69.5139126996675,12.));
#66821=CARTESIAN_POINT('Ctrl Pts',(13.3544235683393,-69.4949589944606,12.));
#66822=CARTESIAN_POINT('Ctrl Pts',(13.3444082410543,-69.4760380470365,12.));
#66823=CARTESIAN_POINT('Ctrl Pts',(13.3344353430313,-69.4571500326673,12.));
#66824=CARTESIAN_POINT('Ctrl Pts',(13.3245048800643,-69.4382951276998,12.));
#66825=CARTESIAN_POINT('Ctrl Pts',(13.3146168578743,-69.4194735096265,12.));
#66826=CARTESIAN_POINT('Ctrl Pts',(13.3047712821051,-69.4006853569511,12.));
#66827=CARTESIAN_POINT('Ctrl Pts',(13.2949681583167,-69.3819308490422,12.));
#66828=CARTESIAN_POINT('Ctrl Pts',(13.2852074919765,-69.3632101660066,12.));
#66829=CARTESIAN_POINT('Ctrl Pts',(13.2754892884433,-69.3445234885065,12.));
#66830=CARTESIAN_POINT('Ctrl Pts',(13.265813552961,-69.3258709977382,12.));
#66831=CARTESIAN_POINT('Ctrl Pts',(13.2561802906896,-69.3072528758518,12.));
#66832=CARTESIAN_POINT('Ctrl Pts',(13.2465895067262,-69.2886693063182,12.));
#66833=CARTESIAN_POINT('Ctrl Pts',(13.237041206122,-69.2701204742449,12.));
#66834=CARTESIAN_POINT('Ctrl Pts',(13.2275353939051,-69.2516065668844,12.));
#66835=CARTESIAN_POINT('Ctrl Pts',(13.2180720750594,-69.2331277732861,12.));
#66836=CARTESIAN_POINT('Ctrl Pts',(13.2086512544735,-69.2146842833537,12.));
#66837=CARTESIAN_POINT('Ctrl Pts',(13.1992729368928,-69.1962762870527,12.));
#66838=CARTESIAN_POINT('Ctrl Pts',(13.1899371268683,-69.1779039735996,12.));
#66839=CARTESIAN_POINT('Ctrl Pts',(13.1806438286934,-69.1595675305245,12.));
#66840=CARTESIAN_POINT('Ctrl Pts',(13.1713930465132,-69.1412671454564,12.));
#66841=CARTESIAN_POINT('Ctrl Pts',(13.1621847844528,-69.1230030082573,12.));
#66842=CARTESIAN_POINT('Ctrl Pts',(13.1530190467183,-69.1047753127643,12.));
#66843=CARTESIAN_POINT('Ctrl Pts',(13.1438958377404,-69.0865842593102,12.));
#66844=CARTESIAN_POINT('Ctrl Pts',(13.1348151621834,-69.0684300549477,12.));
#66845=CARTESIAN_POINT('Ctrl Pts',(13.1257770246385,-69.0503129081817,12.));
#66846=CARTESIAN_POINT('Ctrl Pts',(13.1167814293497,-69.0322330243348,12.));
#66847=CARTESIAN_POINT('Ctrl Pts',(13.1078283799722,-69.0141906015113,12.));
#66848=CARTESIAN_POINT('Ctrl Pts',(13.0989178791833,-68.9961858241519,12.));
#66849=CARTESIAN_POINT('Ctrl Pts',(13.090049929053,-68.9782188692581,12.));
#66850=CARTESIAN_POINT('Ctrl Pts',(13.0812245317807,-68.9602899187573,12.));
#66851=CARTESIAN_POINT('Ctrl Pts',(13.072441690283,-68.9423991694492,12.));
#66852=CARTESIAN_POINT('Ctrl Pts',(13.0637014089029,-68.9245468449945,12.));
#66853=CARTESIAN_POINT('Ctrl Pts',(13.0550036938813,-68.9067332040985,12.));
#66854=CARTESIAN_POINT('Ctrl Pts',(13.0463485518206,-68.8889585151585,12.));
#66855=CARTESIAN_POINT('Ctrl Pts',(13.0377359881875,-68.8712230321906,12.));
#66856=CARTESIAN_POINT('Ctrl Pts',(13.0291660060107,-68.8535269726793,12.));
#66857=CARTESIAN_POINT('Ctrl Pts',(13.0206386039691,-68.8358704887468,12.));
#66858=CARTESIAN_POINT('Ctrl Pts',(13.0121537768945,-68.8182536653656,12.));
#66859=CARTESIAN_POINT('Ctrl Pts',(13.0053999700875,-68.804191966902,12.));
#66860=CARTESIAN_POINT('Ctrl Pts',(13.0003537683054,-68.7936635625545,12.));
#66861=CARTESIAN_POINT('Ctrl Pts',(12.9969981460277,-68.7866525680193,12.));
#66862=CARTESIAN_POINT('Ctrl Pts',(12.9953224629497,-68.7831490561748,12.));
#66863=CARTESIAN_POINT('Ctrl Pts',(16.7988252568748,-72.2774028393915,0.));
#66864=CARTESIAN_POINT('Ctrl Pts',(16.7988252568748,-72.2774028393915,4.));
#66865=CARTESIAN_POINT('Ctrl Pts',(16.7988252568748,-72.2774028393915,8.));
#66866=CARTESIAN_POINT('Ctrl Pts',(16.7988252568748,-72.2774028393915,12.));
#66867=CARTESIAN_POINT('Ctrl Pts',(16.7775526720893,-72.3852065198826,0.));
#66868=CARTESIAN_POINT('Ctrl Pts',(16.7775526720893,-72.3852065198826,4.));
#66869=CARTESIAN_POINT('Ctrl Pts',(16.7775526720893,-72.3852065198826,8.));
#66870=CARTESIAN_POINT('Ctrl Pts',(16.7775526720893,-72.3852065198826,12.));
#66871=CARTESIAN_POINT('Ctrl Pts',(16.6758649025558,-72.5605133546291,0.));
#66872=CARTESIAN_POINT('Ctrl Pts',(16.6758649025558,-72.5605133546291,4.));
#66873=CARTESIAN_POINT('Ctrl Pts',(16.6758649025558,-72.5605133546291,7.99999999999999));
#66874=CARTESIAN_POINT('Ctrl Pts',(16.6758649025558,-72.5605133546291,12.));
#66875=CARTESIAN_POINT('Ctrl Pts',(16.4988611391808,-72.6501505354464,0.));
#66876=CARTESIAN_POINT('Ctrl Pts',(16.4988611391808,-72.6501505354464,4.));
#66877=CARTESIAN_POINT('Ctrl Pts',(16.4988611391808,-72.6501505354464,8.00000000000001));
#66878=CARTESIAN_POINT('Ctrl Pts',(16.4988611391808,-72.6501505354464,12.));
#66879=CARTESIAN_POINT('Ctrl Pts',(16.4184755008061,-72.6683126419587,0.));
#66880=CARTESIAN_POINT('Ctrl Pts',(16.4184755008061,-72.6683126419587,4.));
#66881=CARTESIAN_POINT('Ctrl Pts',(16.4184755008061,-72.6683126419587,8.));
#66882=CARTESIAN_POINT('Ctrl Pts',(16.4184755008061,-72.6683126419587,12.));
#66883=CARTESIAN_POINT('',(16.7988252568748,-72.2774028393915,0.));
#66884=CARTESIAN_POINT('',(16.4184755008061,-72.6683126419586,0.));
#66885=CARTESIAN_POINT('Ctrl Pts',(16.7988252568748,-72.2774028393915,2.77555756156289E-16));
#66886=CARTESIAN_POINT('Ctrl Pts',(16.7775526720893,-72.3852065198826,2.77555756156289E-16));
#66887=CARTESIAN_POINT('Ctrl Pts',(16.719445375213,-72.4853818540234,2.77555756156289E-16));
#66888=CARTESIAN_POINT('Ctrl Pts',(16.6367451007558,-72.557583423616,2.77555756156289E-16));
#66889=CARTESIAN_POINT('Ctrl Pts',(16.5747198949129,-72.6117346008104,2.77555756156289E-16));
#66890=CARTESIAN_POINT('Ctrl Pts',(16.4988611391808,-72.6501505354464,2.77555756156289E-16));
#66891=CARTESIAN_POINT('Ctrl Pts',(16.4184755008061,-72.6683126419587,2.77555756156289E-16));
#66892=CARTESIAN_POINT('',(16.4184755008061,-72.6683126419586,12.));
#66893=CARTESIAN_POINT('Ctrl Pts',(16.4184755008061,-72.6683126419587,0.));
#66894=CARTESIAN_POINT('Ctrl Pts',(16.4184755008061,-72.6683126419587,4.));
#66895=CARTESIAN_POINT('Ctrl Pts',(16.4184755008061,-72.6683126419587,8.));
#66896=CARTESIAN_POINT('Ctrl Pts',(16.4184755008061,-72.6683126419587,12.));
#66897=CARTESIAN_POINT('',(16.7988252568748,-72.2774028393915,12.));
#66898=CARTESIAN_POINT('Ctrl Pts',(16.4184755008061,-72.6683126419587,12.));
#66899=CARTESIAN_POINT('Ctrl Pts',(16.4988611391808,-72.6501505354464,12.));
#66900=CARTESIAN_POINT('Ctrl Pts',(16.5747198949129,-72.6117346008104,12.));
#66901=CARTESIAN_POINT('Ctrl Pts',(16.6367451007558,-72.557583423616,12.));
#66902=CARTESIAN_POINT('Ctrl Pts',(16.7194453752131,-72.4853818540234,12.));
#66903=CARTESIAN_POINT('Ctrl Pts',(16.7775526720893,-72.3852065198826,12.));
#66904=CARTESIAN_POINT('Ctrl Pts',(16.7988252568748,-72.2774028393915,12.));
#66905=CARTESIAN_POINT('Ctrl Pts',(16.7988252568748,-72.2774028393915,12.));
#66906=CARTESIAN_POINT('Ctrl Pts',(16.7988252568748,-72.2774028393915,8.));
#66907=CARTESIAN_POINT('Ctrl Pts',(16.7988252568748,-72.2774028393915,4.));
#66908=CARTESIAN_POINT('Ctrl Pts',(16.7988252568748,-72.2774028393915,0.));
#66909=CARTESIAN_POINT('Origin',(8.12279454723525E-11,-3.65936987487134E-10,
0.));
#66910=CARTESIAN_POINT('Origin',(8.12279454723525E-11,-3.65936987487134E-10,
12.));
#66911=CARTESIAN_POINT('Origin',(8.12279454723525E-11,-3.65936987487134E-10,
0.));
#66912=CARTESIAN_POINT('Ctrl Pts',(9.42570643237823,-73.9013264985861,-5.55111512312578E-16));
#66913=CARTESIAN_POINT('Ctrl Pts',(9.42570643237823,-73.9013264985861,4.));
#66914=CARTESIAN_POINT('Ctrl Pts',(9.42570643237823,-73.9013264985861,8.));
#66915=CARTESIAN_POINT('Ctrl Pts',(9.42570643237823,-73.9013264985861,12.));
#66916=CARTESIAN_POINT('Ctrl Pts',(9.31670696907615,-73.9152287787081,-5.55111512312578E-16));
#66917=CARTESIAN_POINT('Ctrl Pts',(9.31670696907615,-73.9152287787081,4.));
#66918=CARTESIAN_POINT('Ctrl Pts',(9.31670696907615,-73.9152287787081,8.00000000000001));
#66919=CARTESIAN_POINT('Ctrl Pts',(9.31670696907615,-73.9152287787081,12.));
#66920=CARTESIAN_POINT('Ctrl Pts',(9.11824194722557,-73.8741839722668,-5.55111512312578E-16));
#66921=CARTESIAN_POINT('Ctrl Pts',(9.11824194722557,-73.8741839722668,4.));
#66922=CARTESIAN_POINT('Ctrl Pts',(9.11824194722557,-73.8741839722668,7.99999999999999));
#66923=CARTESIAN_POINT('Ctrl Pts',(9.11824194722557,-73.8741839722668,12.));
#66924=CARTESIAN_POINT('Ctrl Pts',(8.97724108745579,-73.734598722692,-5.55111512312578E-16));
#66925=CARTESIAN_POINT('Ctrl Pts',(8.97724108745579,-73.734598722692,4.));
#66926=CARTESIAN_POINT('Ctrl Pts',(8.97724108745578,-73.734598722692,8.00000000000001));
#66927=CARTESIAN_POINT('Ctrl Pts',(8.97724108745578,-73.734598722692,12.));
#66928=CARTESIAN_POINT('Ctrl Pts',(8.93459554655837,-73.6640787197675,-5.55111512312578E-16));
#66929=CARTESIAN_POINT('Ctrl Pts',(8.93459554655837,-73.6640787197675,4.));
#66930=CARTESIAN_POINT('Ctrl Pts',(8.93459554655836,-73.6640787197675,8.));
#66931=CARTESIAN_POINT('Ctrl Pts',(8.93459554655836,-73.6640787197675,12.));
#66932=CARTESIAN_POINT('',(9.42570643237823,-73.9013264985861,0.));
#66933=CARTESIAN_POINT('',(8.93459554655838,-73.6640787197675,0.));
#66934=CARTESIAN_POINT('Ctrl Pts',(9.42570643237823,-73.9013264985861,4.16333634234434E-16));
#66935=CARTESIAN_POINT('Ctrl Pts',(9.31670696907615,-73.9152287787081,4.16333634234434E-16));
#66936=CARTESIAN_POINT('Ctrl Pts',(9.20329838516153,-73.8917746035988,4.16333634234434E-16));
#66937=CARTESIAN_POINT('Ctrl Pts',(9.1086536092733,-73.8361439572622,4.16333634234434E-16));
#66938=CARTESIAN_POINT('Ctrl Pts',(9.03767002735712,-73.7944209725098,4.16333634234434E-16));
#66939=CARTESIAN_POINT('Ctrl Pts',(8.97724108745579,-73.734598722692,4.16333634234433E-16));
#66940=CARTESIAN_POINT('Ctrl Pts',(8.93459554655837,-73.6640787197675,4.16333634234434E-16));
#66941=CARTESIAN_POINT('',(8.93459554655838,-73.6640787197675,12.));
#66942=CARTESIAN_POINT('Ctrl Pts',(8.93459554655837,-73.6640787197675,-5.55111512312578E-16));
#66943=CARTESIAN_POINT('Ctrl Pts',(8.93459554655837,-73.6640787197675,4.));
#66944=CARTESIAN_POINT('Ctrl Pts',(8.93459554655836,-73.6640787197675,8.));
#66945=CARTESIAN_POINT('Ctrl Pts',(8.93459554655836,-73.6640787197675,12.));
#66946=CARTESIAN_POINT('',(9.42570643237823,-73.9013264985861,12.));
#66947=CARTESIAN_POINT('Ctrl Pts',(8.93459554655836,-73.6640787197675,12.));
#66948=CARTESIAN_POINT('Ctrl Pts',(8.97724108745578,-73.734598722692,12.));
#66949=CARTESIAN_POINT('Ctrl Pts',(9.03767002735712,-73.7944209725098,12.));
#66950=CARTESIAN_POINT('Ctrl Pts',(9.10865360927329,-73.8361439572622,12.));
#66951=CARTESIAN_POINT('Ctrl Pts',(9.20329838516153,-73.8917746035988,12.));
#66952=CARTESIAN_POINT('Ctrl Pts',(9.31670696907615,-73.9152287787081,12.));
#66953=CARTESIAN_POINT('Ctrl Pts',(9.42570643237823,-73.9013264985861,12.));
#66954=CARTESIAN_POINT('Ctrl Pts',(9.42570643237823,-73.9013264985861,12.));
#66955=CARTESIAN_POINT('Ctrl Pts',(9.42570643237823,-73.9013264985861,8.));
#66956=CARTESIAN_POINT('Ctrl Pts',(9.42570643237823,-73.9013264985861,4.));
#66957=CARTESIAN_POINT('Ctrl Pts',(9.42570643237823,-73.9013264985861,-5.55111512312578E-16));
#66958=CARTESIAN_POINT('Ctrl Pts',(6.95102489306925,-69.6540253893192,0.));
#66959=CARTESIAN_POINT('Ctrl Pts',(6.95102489306925,-69.6540253893192,12.));
#66960=CARTESIAN_POINT('Ctrl Pts',(6.95238884849024,-69.6576616146467,0.));
#66961=CARTESIAN_POINT('Ctrl Pts',(6.95238884849024,-69.6576616146467,12.));
#66962=CARTESIAN_POINT('Ctrl Pts',(6.95512065317599,-69.664938391983,0.));
#66963=CARTESIAN_POINT('Ctrl Pts',(6.95512065317599,-69.664938391983,12.));
#66964=CARTESIAN_POINT('Ctrl Pts',(6.9592300417359,-69.6758665380378,0.));
#66965=CARTESIAN_POINT('Ctrl Pts',(6.9592300417359,-69.6758665380378,12.));
#66966=CARTESIAN_POINT('Ctrl Pts',(6.96473259049512,-69.6904633605421,0.));
#66967=CARTESIAN_POINT('Ctrl Pts',(6.96473259049512,-69.6904633605421,12.));
#66968=CARTESIAN_POINT('Ctrl Pts',(6.97164972291439,-69.7087526479973,0.));
#66969=CARTESIAN_POINT('Ctrl Pts',(6.97164972291439,-69.7087526479973,12.));
#66970=CARTESIAN_POINT('Ctrl Pts',(6.97860581164526,-69.7270851557366,0.));
#66971=CARTESIAN_POINT('Ctrl Pts',(6.97860581164526,-69.7270851557366,12.));
#66972=CARTESIAN_POINT('Ctrl Pts',(6.98560086924213,-69.7454607995607,0.));
#66973=CARTESIAN_POINT('Ctrl Pts',(6.98560086924213,-69.7454607995607,12.));
#66974=CARTESIAN_POINT('Ctrl Pts',(6.9926349102794,-69.7638794280419,0.));
#66975=CARTESIAN_POINT('Ctrl Pts',(6.9926349102794,-69.7638794280419,12.));
#66976=CARTESIAN_POINT('Ctrl Pts',(6.99970795069475,-69.782340824259,0.));
#66977=CARTESIAN_POINT('Ctrl Pts',(6.99970795069475,-69.782340824259,12.));
#66978=CARTESIAN_POINT('Ctrl Pts',(7.0068200071815,-69.8008447346863,0.));
#66979=CARTESIAN_POINT('Ctrl Pts',(7.0068200071815,-69.8008447346863,12.));
#66980=CARTESIAN_POINT('Ctrl Pts',(7.01397109655454,-69.8193908913722,0.));
#66981=CARTESIAN_POINT('Ctrl Pts',(7.01397109655454,-69.8193908913722,12.));
#66982=CARTESIAN_POINT('Ctrl Pts',(7.02116123514451,-69.8379790360518,0.));
#66983=CARTESIAN_POINT('Ctrl Pts',(7.02116123514451,-69.8379790360518,12.));
#66984=CARTESIAN_POINT('Ctrl Pts',(7.02839043811812,-69.8566089455375,0.));
#66985=CARTESIAN_POINT('Ctrl Pts',(7.02839043811812,-69.8566089455375,12.));
#66986=CARTESIAN_POINT('Ctrl Pts',(7.0356587197222,-69.8752804235238,0.));
#66987=CARTESIAN_POINT('Ctrl Pts',(7.0356587197222,-69.8752804235238,12.));
#66988=CARTESIAN_POINT('Ctrl Pts',(7.04296609362165,-69.8939932885841,0.));
#66989=CARTESIAN_POINT('Ctrl Pts',(7.04296609362165,-69.8939932885841,12.));
#66990=CARTESIAN_POINT('Ctrl Pts',(7.05031257318115,-69.9127473642099,0.));
#66991=CARTESIAN_POINT('Ctrl Pts',(7.05031257318115,-69.9127473642099,12.));
#66992=CARTESIAN_POINT('Ctrl Pts',(7.05769817180856,-69.9315424664291,0.));
#66993=CARTESIAN_POINT('Ctrl Pts',(7.05769817180856,-69.9315424664291,12.));
#66994=CARTESIAN_POINT('Ctrl Pts',(7.06512290312849,-69.9503783975727,0.));
#66995=CARTESIAN_POINT('Ctrl Pts',(7.06512290312849,-69.9503783975727,12.));
#66996=CARTESIAN_POINT('Ctrl Pts',(7.0725867808083,-69.9692549527296,0.));
#66997=CARTESIAN_POINT('Ctrl Pts',(7.0725867808083,-69.9692549527296,12.));
#66998=CARTESIAN_POINT('Ctrl Pts',(7.08008981844651,-69.988171923788,0.));
#66999=CARTESIAN_POINT('Ctrl Pts',(7.08008981844651,-69.988171923788,12.));
#67000=CARTESIAN_POINT('Ctrl Pts',(7.08763202944245,-70.0071291040766,0.));
#67001=CARTESIAN_POINT('Ctrl Pts',(7.08763202944245,-70.0071291040766,12.));
#67002=CARTESIAN_POINT('Ctrl Pts',(7.09521342684248,-70.0261262936388,0.));
#67003=CARTESIAN_POINT('Ctrl Pts',(7.09521342684248,-70.0261262936388,12.));
#67004=CARTESIAN_POINT('Ctrl Pts',(7.10283402335033,-70.0451632990086,0.));
#67005=CARTESIAN_POINT('Ctrl Pts',(7.10283402335033,-70.0451632990086,12.));
#67006=CARTESIAN_POINT('Ctrl Pts',(7.11049383140445,-70.0642399306869,0.));
#67007=CARTESIAN_POINT('Ctrl Pts',(7.11049383140445,-70.0642399306869,12.));
#67008=CARTESIAN_POINT('Ctrl Pts',(7.11819286322825,-70.0833560013975,0.));
#67009=CARTESIAN_POINT('Ctrl Pts',(7.11819286322825,-70.0833560013975,12.));
#67010=CARTESIAN_POINT('Ctrl Pts',(7.12593113088903,-70.1025113239495,0.));
#67011=CARTESIAN_POINT('Ctrl Pts',(7.12593113088903,-70.1025113239495,12.));
#67012=CARTESIAN_POINT('Ctrl Pts',(7.13370864634442,-70.1217057094499,0.));
#67013=CARTESIAN_POINT('Ctrl Pts',(7.13370864634442,-70.1217057094499,12.));
#67014=CARTESIAN_POINT('Ctrl Pts',(7.14152542142373,-70.1409389682424,0.));
#67015=CARTESIAN_POINT('Ctrl Pts',(7.14152542142373,-70.1409389682424,12.));
#67016=CARTESIAN_POINT('Ctrl Pts',(7.14938146780813,-70.1602109107202,0.));
#67017=CARTESIAN_POINT('Ctrl Pts',(7.14938146780813,-70.1602109107202,12.));
#67018=CARTESIAN_POINT('Ctrl Pts',(7.15727679700932,-70.1795213481185,0.));
#67019=CARTESIAN_POINT('Ctrl Pts',(7.15727679700932,-70.1795213481185,12.));
#67020=CARTESIAN_POINT('Ctrl Pts',(7.16521142033863,-70.1988700934593,0.));
#67021=CARTESIAN_POINT('Ctrl Pts',(7.16521142033863,-70.1988700934593,12.));
#67022=CARTESIAN_POINT('Ctrl Pts',(7.17318534889715,-70.2182569618994,0.));
#67023=CARTESIAN_POINT('Ctrl Pts',(7.17318534889715,-70.2182569618994,12.));
#67024=CARTESIAN_POINT('Ctrl Pts',(7.18119859359777,-70.2376817702215,0.));
#67025=CARTESIAN_POINT('Ctrl Pts',(7.18119859359777,-70.2376817702215,12.));
#67026=CARTESIAN_POINT('Ctrl Pts',(7.18925116517554,-70.2571443365192,0.));
#67027=CARTESIAN_POINT('Ctrl Pts',(7.18925116517554,-70.2571443365192,12.));
#67028=CARTESIAN_POINT('Ctrl Pts',(7.19734307419872,-70.2766444798285,0.));
#67029=CARTESIAN_POINT('Ctrl Pts',(7.19734307419872,-70.2766444798285,12.));
#67030=CARTESIAN_POINT('Ctrl Pts',(7.20547433107482,-70.2961820197077,0.));
#67031=CARTESIAN_POINT('Ctrl Pts',(7.20547433107482,-70.2961820197077,12.));
#67032=CARTESIAN_POINT('Ctrl Pts',(7.21364494605449,-70.3157567762588,0.));
#67033=CARTESIAN_POINT('Ctrl Pts',(7.21364494605449,-70.3157567762588,12.));
#67034=CARTESIAN_POINT('Ctrl Pts',(7.2218549292319,-70.3353685703112,0.));
#67035=CARTESIAN_POINT('Ctrl Pts',(7.2218549292319,-70.3353685703112,12.));
#67036=CARTESIAN_POINT('Ctrl Pts',(7.23010429054228,-70.3550172235486,0.));
#67037=CARTESIAN_POINT('Ctrl Pts',(7.23010429054228,-70.3550172235486,12.));
#67038=CARTESIAN_POINT('Ctrl Pts',(7.23839303975606,-70.3747025586552,0.));
#67039=CARTESIAN_POINT('Ctrl Pts',(7.23839303975606,-70.3747025586552,12.));
#67040=CARTESIAN_POINT('Ctrl Pts',(7.24672118647084,-70.3944243994504,0.));
#67041=CARTESIAN_POINT('Ctrl Pts',(7.24672118647084,-70.3944243994504,12.));
#67042=CARTESIAN_POINT('Ctrl Pts',(7.25508874012042,-70.4141825708178,0.));
#67043=CARTESIAN_POINT('Ctrl Pts',(7.25508874012042,-70.4141825708178,12.));
#67044=CARTESIAN_POINT('Ctrl Pts',(7.26349570998032,-70.4339768986346,0.));
#67045=CARTESIAN_POINT('Ctrl Pts',(7.26349570998032,-70.4339768986346,12.));
#67046=CARTESIAN_POINT('Ctrl Pts',(7.27194210517062,-70.4538072096992,0.));
#67047=CARTESIAN_POINT('Ctrl Pts',(7.27194210517062,-70.4538072096992,12.));
#67048=CARTESIAN_POINT('Ctrl Pts',(7.2804279346547,-70.4736733316487,0.));
#67049=CARTESIAN_POINT('Ctrl Pts',(7.2804279346547,-70.4736733316487,12.));
#67050=CARTESIAN_POINT('Ctrl Pts',(7.28895320723861,-70.4935750929058,0.));
#67051=CARTESIAN_POINT('Ctrl Pts',(7.28895320723861,-70.4935750929058,12.));
#67052=CARTESIAN_POINT('Ctrl Pts',(7.29751793157822,-70.5135123227169,0.));
#67053=CARTESIAN_POINT('Ctrl Pts',(7.29751793157822,-70.5135123227169,12.));
#67054=CARTESIAN_POINT('Ctrl Pts',(7.30612211618052,-70.5334848511681,0.));
#67055=CARTESIAN_POINT('Ctrl Pts',(7.30612211618052,-70.5334848511681,12.));
#67056=CARTESIAN_POINT('Ctrl Pts',(7.31476576940391,-70.5534925092043,0.));
#67057=CARTESIAN_POINT('Ctrl Pts',(7.31476576940391,-70.5534925092043,12.));
#67058=CARTESIAN_POINT('Ctrl Pts',(7.32344889945219,-70.5735351286476,0.));
#67059=CARTESIAN_POINT('Ctrl Pts',(7.32344889945219,-70.5735351286476,12.));
#67060=CARTESIAN_POINT('Ctrl Pts',(7.3321715143759,-70.5936125421946,0.));
#67061=CARTESIAN_POINT('Ctrl Pts',(7.3321715143759,-70.5936125421946,12.));
#67062=CARTESIAN_POINT('Ctrl Pts',(7.34093362208007,-70.6137245833996,0.));
#67063=CARTESIAN_POINT('Ctrl Pts',(7.34093362208007,-70.6137245833996,12.));
#67064=CARTESIAN_POINT('Ctrl Pts',(7.34973523032577,-70.6338710866562,0.));
#67065=CARTESIAN_POINT('Ctrl Pts',(7.34973523032577,-70.6338710866562,12.));
#67066=CARTESIAN_POINT('Ctrl Pts',(7.35857634673054,-70.6540518871775,0.));
#67067=CARTESIAN_POINT('Ctrl Pts',(7.35857634673054,-70.6540518871775,12.));
#67068=CARTESIAN_POINT('Ctrl Pts',(7.367456978763,-70.6742668209687,0.));
#67069=CARTESIAN_POINT('Ctrl Pts',(7.367456978763,-70.6742668209687,12.));
#67070=CARTESIAN_POINT('Ctrl Pts',(7.37637713374767,-70.694515724827,0.));
#67071=CARTESIAN_POINT('Ctrl Pts',(7.37637713374767,-70.694515724827,12.));
#67072=CARTESIAN_POINT('Ctrl Pts',(7.38533681887032,-70.7147984363424,0.));
#67073=CARTESIAN_POINT('Ctrl Pts',(7.38533681887032,-70.7147984363424,12.));
#67074=CARTESIAN_POINT('Ctrl Pts',(7.3943360411789,-70.735114793895,0.));
#67075=CARTESIAN_POINT('Ctrl Pts',(7.3943360411789,-70.735114793895,12.));
#67076=CARTESIAN_POINT('Ctrl Pts',(7.40337480758229,-70.7554646366514,0.));
#67077=CARTESIAN_POINT('Ctrl Pts',(7.40337480758229,-70.7554646366514,12.));
#67078=CARTESIAN_POINT('Ctrl Pts',(7.41245312484486,-70.7758478045576,0.));
#67079=CARTESIAN_POINT('Ctrl Pts',(7.41245312484486,-70.7758478045576,12.));
#67080=CARTESIAN_POINT('Ctrl Pts',(7.42157099959315,-70.7962641383351,0.));
#67081=CARTESIAN_POINT('Ctrl Pts',(7.42157099959315,-70.7962641383351,12.));
#67082=CARTESIAN_POINT('Ctrl Pts',(7.43072843832007,-70.8167134794738,0.));
#67083=CARTESIAN_POINT('Ctrl Pts',(7.43072843832007,-70.8167134794738,12.));
#67084=CARTESIAN_POINT('Ctrl Pts',(7.43992544738606,-70.8371956702242,0.));
#67085=CARTESIAN_POINT('Ctrl Pts',(7.43992544738606,-70.8371956702242,12.));
#67086=CARTESIAN_POINT('Ctrl Pts',(7.44916203301644,-70.8577105535841,0.));
#67087=CARTESIAN_POINT('Ctrl Pts',(7.44916203301644,-70.8577105535841,12.));
#67088=CARTESIAN_POINT('Ctrl Pts',(7.45843820129775,-70.8782579732885,0.));
#67089=CARTESIAN_POINT('Ctrl Pts',(7.45843820129775,-70.8782579732885,12.));
#67090=CARTESIAN_POINT('Ctrl Pts',(7.46775395818518,-70.8988377738088,0.));
#67091=CARTESIAN_POINT('Ctrl Pts',(7.46775395818518,-70.8988377738088,12.));
#67092=CARTESIAN_POINT('Ctrl Pts',(7.47710930950553,-70.9194498003483,0.));
#67093=CARTESIAN_POINT('Ctrl Pts',(7.47710930950553,-70.9194498003483,12.));
#67094=CARTESIAN_POINT('Ctrl Pts',(7.48650426095822,-70.9400938988373,0.));
#67095=CARTESIAN_POINT('Ctrl Pts',(7.48650426095822,-70.9400938988373,12.));
#67096=CARTESIAN_POINT('Ctrl Pts',(7.49593881811141,-70.9607699159234,0.));
#67097=CARTESIAN_POINT('Ctrl Pts',(7.49593881811141,-70.9607699159234,12.));
#67098=CARTESIAN_POINT('Ctrl Pts',(7.50541298639948,-70.9814776989637,0.));
#67099=CARTESIAN_POINT('Ctrl Pts',(7.50541298639948,-70.9814776989637,12.));
#67100=CARTESIAN_POINT('Ctrl Pts',(7.51492677113111,-71.0022170960235,0.));
#67101=CARTESIAN_POINT('Ctrl Pts',(7.51492677113111,-71.0022170960235,12.));
#67102=CARTESIAN_POINT('Ctrl Pts',(7.52448017749135,-71.0229879558713,0.));
#67103=CARTESIAN_POINT('Ctrl Pts',(7.52448017749135,-71.0229879558713,12.));
#67104=CARTESIAN_POINT('Ctrl Pts',(7.53407321054253,-71.0437901279722,0.));
#67105=CARTESIAN_POINT('Ctrl Pts',(7.53407321054253,-71.0437901279722,12.));
#67106=CARTESIAN_POINT('Ctrl Pts',(7.54370587521947,-71.0646234624783,0.));
#67107=CARTESIAN_POINT('Ctrl Pts',(7.54370587521947,-71.0646234624783,12.));
#67108=CARTESIAN_POINT('Ctrl Pts',(7.55337817632872,-71.0854878102203,0.));
#67109=CARTESIAN_POINT('Ctrl Pts',(7.55337817632872,-71.0854878102203,12.));
#67110=CARTESIAN_POINT('Ctrl Pts',(7.56309011855616,-71.1063830227074,0.));
#67111=CARTESIAN_POINT('Ctrl Pts',(7.56309011855616,-71.1063830227074,12.));
#67112=CARTESIAN_POINT('Ctrl Pts',(7.57284170646865,-71.1273089521218,0.));
#67113=CARTESIAN_POINT('Ctrl Pts',(7.57284170646865,-71.1273089521218,12.));
#67114=CARTESIAN_POINT('Ctrl Pts',(7.58263294451465,-71.1482654513133,0.));
#67115=CARTESIAN_POINT('Ctrl Pts',(7.58263294451465,-71.1482654513133,12.));
#67116=CARTESIAN_POINT('Ctrl Pts',(7.59246383701859,-71.1692523737887,0.));
#67117=CARTESIAN_POINT('Ctrl Pts',(7.59246383701859,-71.1692523737887,12.));
#67118=CARTESIAN_POINT('Ctrl Pts',(7.60233438818156,-71.1902695737063,0.));
#67119=CARTESIAN_POINT('Ctrl Pts',(7.60233438818156,-71.1902695737063,12.));
#67120=CARTESIAN_POINT('Ctrl Pts',(7.61224460208886,-71.2113169058778,0.));
#67121=CARTESIAN_POINT('Ctrl Pts',(7.61224460208886,-71.2113169058778,12.));
#67122=CARTESIAN_POINT('Ctrl Pts',(7.62219448271124,-71.232394225762,0.));
#67123=CARTESIAN_POINT('Ctrl Pts',(7.62219448271124,-71.232394225762,12.));
#67124=CARTESIAN_POINT('Ctrl Pts',(7.63218403390514,-71.2535013894587,0.));
#67125=CARTESIAN_POINT('Ctrl Pts',(7.63218403390514,-71.2535013894587,12.));
#67126=CARTESIAN_POINT('Ctrl Pts',(7.64221325940671,-71.2746382536974,0.));
#67127=CARTESIAN_POINT('Ctrl Pts',(7.64221325940671,-71.2746382536974,12.));
#67128=CARTESIAN_POINT('Ctrl Pts',(7.65228216283342,-71.2958046758334,0.));
#67129=CARTESIAN_POINT('Ctrl Pts',(7.65228216283342,-71.2958046758334,12.));
#67130=CARTESIAN_POINT('Ctrl Pts',(7.66239074769118,-71.3170005138474,0.));
#67131=CARTESIAN_POINT('Ctrl Pts',(7.66239074769118,-71.3170005138474,12.));
#67132=CARTESIAN_POINT('Ctrl Pts',(7.67253901737539,-71.3382256263405,0.));
#67133=CARTESIAN_POINT('Ctrl Pts',(7.67253901737539,-71.3382256263405,12.));
#67134=CARTESIAN_POINT('Ctrl Pts',(7.68272697517102,-71.3594798725294,0.));
#67135=CARTESIAN_POINT('Ctrl Pts',(7.68272697517102,-71.3594798725294,12.));
#67136=CARTESIAN_POINT('Ctrl Pts',(7.69295462424646,-71.380763112236,0.));
#67137=CARTESIAN_POINT('Ctrl Pts',(7.69295462424646,-71.380763112236,12.));
#67138=CARTESIAN_POINT('Ctrl Pts',(7.70322196765572,-71.4020752058827,0.));
#67139=CARTESIAN_POINT('Ctrl Pts',(7.70322196765572,-71.4020752058827,12.));
#67140=CARTESIAN_POINT('Ctrl Pts',(7.71352900834537,-71.4234160144943,0.));
#67141=CARTESIAN_POINT('Ctrl Pts',(7.71352900834537,-71.4234160144943,12.));
#67142=CARTESIAN_POINT('Ctrl Pts',(7.72387574915544,-71.4447853996919,0.));
#67143=CARTESIAN_POINT('Ctrl Pts',(7.72387574915544,-71.4447853996919,12.));
#67144=CARTESIAN_POINT('Ctrl Pts',(7.73426219281931,-71.4661832236881,0.));
#67145=CARTESIAN_POINT('Ctrl Pts',(7.73426219281931,-71.4661832236881,12.));
#67146=CARTESIAN_POINT('Ctrl Pts',(7.74468834195734,-71.487609349277,0.));
#67147=CARTESIAN_POINT('Ctrl Pts',(7.74468834195734,-71.487609349277,12.));
#67148=CARTESIAN_POINT('Ctrl Pts',(7.75515419907954,-71.5090636398307,0.));
#67149=CARTESIAN_POINT('Ctrl Pts',(7.75515419907954,-71.5090636398307,12.));
#67150=CARTESIAN_POINT('Ctrl Pts',(7.76565976659218,-71.5305459592987,0.));
#67151=CARTESIAN_POINT('Ctrl Pts',(7.76565976659218,-71.5305459592987,12.));
#67152=CARTESIAN_POINT('Ctrl Pts',(7.77620504679867,-71.5520561722039,0.));
#67153=CARTESIAN_POINT('Ctrl Pts',(7.77620504679867,-71.5520561722039,12.));
#67154=CARTESIAN_POINT('Ctrl Pts',(7.78679004189934,-71.5735941436366,0.));
#67155=CARTESIAN_POINT('Ctrl Pts',(7.78679004189934,-71.5735941436366,12.));
#67156=CARTESIAN_POINT('Ctrl Pts',(7.79741475398511,-71.5951597392471,0.));
#67157=CARTESIAN_POINT('Ctrl Pts',(7.79741475398511,-71.5951597392471,12.));
#67158=CARTESIAN_POINT('Ctrl Pts',(7.80807918504016,-71.616752825242,0.));
#67159=CARTESIAN_POINT('Ctrl Pts',(7.80807918504016,-71.616752825242,12.));
#67160=CARTESIAN_POINT('Ctrl Pts',(7.81878333694855,-71.638373268384,0.));
#67161=CARTESIAN_POINT('Ctrl Pts',(7.81878333694855,-71.638373268384,12.));
#67162=CARTESIAN_POINT('Ctrl Pts',(7.82952721149503,-71.6600209359869,0.));
#67163=CARTESIAN_POINT('Ctrl Pts',(7.82952721149503,-71.6600209359869,12.));
#67164=CARTESIAN_POINT('Ctrl Pts',(7.84031081036488,-71.681695695912,0.));
#67165=CARTESIAN_POINT('Ctrl Pts',(7.84031081036488,-71.681695695912,12.));
#67166=CARTESIAN_POINT('Ctrl Pts',(7.85113413513738,-71.7033974165576,0.));
#67167=CARTESIAN_POINT('Ctrl Pts',(7.85113413513738,-71.7033974165576,12.));
#67168=CARTESIAN_POINT('Ctrl Pts',(7.86199718728829,-71.7251259668573,0.));
#67169=CARTESIAN_POINT('Ctrl Pts',(7.86199718728829,-71.7251259668573,12.));
#67170=CARTESIAN_POINT('Ctrl Pts',(7.87289996819653,-71.7468812162795,0.));
#67171=CARTESIAN_POINT('Ctrl Pts',(7.87289996819653,-71.7468812162795,12.));
#67172=CARTESIAN_POINT('Ctrl Pts',(7.88384247914521,-71.768663034824,0.));
#67173=CARTESIAN_POINT('Ctrl Pts',(7.88384247914521,-71.768663034824,12.));
#67174=CARTESIAN_POINT('Ctrl Pts',(7.89482472132134,-71.7904712930172,0.));
#67175=CARTESIAN_POINT('Ctrl Pts',(7.89482472132134,-71.7904712930172,12.));
#67176=CARTESIAN_POINT('Ctrl Pts',(7.90584669580955,-71.8123058619038,0.));
#67177=CARTESIAN_POINT('Ctrl Pts',(7.90584669580955,-71.8123058619038,12.));
#67178=CARTESIAN_POINT('Ctrl Pts',(7.9169084035937,-71.8341666130424,0.));
#67179=CARTESIAN_POINT('Ctrl Pts',(7.9169084035937,-71.8341666130424,12.));
#67180=CARTESIAN_POINT('Ctrl Pts',(7.92800984556399,-71.8560534185071,0.));
#67181=CARTESIAN_POINT('Ctrl Pts',(7.92800984556399,-71.8560534185071,12.));
#67182=CARTESIAN_POINT('Ctrl Pts',(7.93915102251795,-71.8779661508833,0.));
#67183=CARTESIAN_POINT('Ctrl Pts',(7.93915102251795,-71.8779661508833,12.));
#67184=CARTESIAN_POINT('Ctrl Pts',(7.95033193516045,-71.8999046832642,0.));
#67185=CARTESIAN_POINT('Ctrl Pts',(7.95033193516045,-71.8999046832642,12.));
#67186=CARTESIAN_POINT('Ctrl Pts',(7.96155258409751,-71.9218688892426,0.));
#67187=CARTESIAN_POINT('Ctrl Pts',(7.96155258409751,-71.9218688892426,12.));
#67188=CARTESIAN_POINT('Ctrl Pts',(7.97281296983701,-71.9438586429072,0.));
#67189=CARTESIAN_POINT('Ctrl Pts',(7.97281296983701,-71.9438586429072,12.));
#67190=CARTESIAN_POINT('Ctrl Pts',(7.98411309279597,-71.9658738188421,0.));
#67191=CARTESIAN_POINT('Ctrl Pts',(7.98411309279597,-71.9658738188421,12.));
#67192=CARTESIAN_POINT('Ctrl Pts',(7.99545295330181,-71.9879142921248,0.));
#67193=CARTESIAN_POINT('Ctrl Pts',(7.99545295330181,-71.9879142921248,12.));
#67194=CARTESIAN_POINT('Ctrl Pts',(8.00683255159249,-72.0099799383216,0.));
#67195=CARTESIAN_POINT('Ctrl Pts',(8.00683255159249,-72.0099799383216,12.));
#67196=CARTESIAN_POINT('Ctrl Pts',(8.01825188781069,-72.0320706334802,0.));
#67197=CARTESIAN_POINT('Ctrl Pts',(8.01825188781069,-72.0320706334802,12.));
#67198=CARTESIAN_POINT('Ctrl Pts',(8.02971096200327,-72.0541862541262,0.));
#67199=CARTESIAN_POINT('Ctrl Pts',(8.02971096200327,-72.0541862541262,12.));
#67200=CARTESIAN_POINT('Ctrl Pts',(8.04120977412891,-72.0763266772632,0.));
#67201=CARTESIAN_POINT('Ctrl Pts',(8.04120977412891,-72.0763266772632,12.));
#67202=CARTESIAN_POINT('Ctrl Pts',(8.05274832405956,-72.0984917803702,0.));
#67203=CARTESIAN_POINT('Ctrl Pts',(8.05274832405956,-72.0984917803702,12.));
#67204=CARTESIAN_POINT('Ctrl Pts',(8.06432661158088,-72.1206814413985,0.));
#67205=CARTESIAN_POINT('Ctrl Pts',(8.06432661158088,-72.1206814413985,12.));
#67206=CARTESIAN_POINT('Ctrl Pts',(8.07594463638699,-72.1428955387648,0.));
#67207=CARTESIAN_POINT('Ctrl Pts',(8.07594463638699,-72.1428955387648,12.));
#67208=CARTESIAN_POINT('Ctrl Pts',(8.08760239807814,-72.165133951346,0.));
#67209=CARTESIAN_POINT('Ctrl Pts',(8.08760239807814,-72.165133951346,12.));
#67210=CARTESIAN_POINT('Ctrl Pts',(8.09929989616873,-72.18739655848,0.));
#67211=CARTESIAN_POINT('Ctrl Pts',(8.09929989616873,-72.18739655848,12.));
#67212=CARTESIAN_POINT('Ctrl Pts',(8.11103713008921,-72.2096832399626,0.));
#67213=CARTESIAN_POINT('Ctrl Pts',(8.11103713008921,-72.2096832399626,12.));
#67214=CARTESIAN_POINT('Ctrl Pts',(8.12281409918661,-72.2319938760451,0.));
#67215=CARTESIAN_POINT('Ctrl Pts',(8.12281409918661,-72.2319938760451,12.));
#67216=CARTESIAN_POINT('Ctrl Pts',(8.13463080272028,-72.2543283474279,0.));
#67217=CARTESIAN_POINT('Ctrl Pts',(8.13463080272028,-72.2543283474279,12.));
#67218=CARTESIAN_POINT('Ctrl Pts',(8.14648723985792,-72.2766865352552,0.));
#67219=CARTESIAN_POINT('Ctrl Pts',(8.14648723985792,-72.2766865352552,12.));
#67220=CARTESIAN_POINT('Ctrl Pts',(8.15838340968327,-72.2990683211155,0.));
#67221=CARTESIAN_POINT('Ctrl Pts',(8.15838340968327,-72.2990683211155,12.));
#67222=CARTESIAN_POINT('Ctrl Pts',(8.17031931119881,-72.3214735870402,0.));
#67223=CARTESIAN_POINT('Ctrl Pts',(8.17031931119881,-72.3214735870402,12.));
#67224=CARTESIAN_POINT('Ctrl Pts',(8.18229494332621,-72.3439022155007,0.));
#67225=CARTESIAN_POINT('Ctrl Pts',(8.18229494332621,-72.3439022155007,12.));
#67226=CARTESIAN_POINT('Ctrl Pts',(8.19431030490318,-72.3663540894034,0.));
#67227=CARTESIAN_POINT('Ctrl Pts',(8.19431030490318,-72.3663540894034,12.));
#67228=CARTESIAN_POINT('Ctrl Pts',(8.20636539467781,-72.3888290920845,0.));
#67229=CARTESIAN_POINT('Ctrl Pts',(8.20636539467781,-72.3888290920845,12.));
#67230=CARTESIAN_POINT('Ctrl Pts',(8.21846021131563,-72.4113271073091,0.));
#67231=CARTESIAN_POINT('Ctrl Pts',(8.21846021131563,-72.4113271073091,12.));
#67232=CARTESIAN_POINT('Ctrl Pts',(8.23059475340354,-72.4338480192701,0.));
#67233=CARTESIAN_POINT('Ctrl Pts',(8.23059475340354,-72.4338480192701,12.));
#67234=CARTESIAN_POINT('Ctrl Pts',(8.24276901945036,-72.4563917125842,0.));
#67235=CARTESIAN_POINT('Ctrl Pts',(8.24276901945036,-72.4563917125842,12.));
#67236=CARTESIAN_POINT('Ctrl Pts',(8.25498300788492,-72.4789580722871,0.));
#67237=CARTESIAN_POINT('Ctrl Pts',(8.25498300788492,-72.4789580722871,12.));
#67238=CARTESIAN_POINT('Ctrl Pts',(8.26723671704923,-72.501546983825,0.));
#67239=CARTESIAN_POINT('Ctrl Pts',(8.26723671704923,-72.501546983825,12.));
#67240=CARTESIAN_POINT('Ctrl Pts',(8.27953014520384,-72.524158333056,0.));
#67241=CARTESIAN_POINT('Ctrl Pts',(8.27953014520384,-72.524158333056,12.));
#67242=CARTESIAN_POINT('Ctrl Pts',(8.29186329053288,-72.5467920062522,0.));
#67243=CARTESIAN_POINT('Ctrl Pts',(8.29186329053288,-72.5467920062522,12.));
#67244=CARTESIAN_POINT('Ctrl Pts',(8.30423615114454,-72.5694478900983,0.));
#67245=CARTESIAN_POINT('Ctrl Pts',(8.30423615114454,-72.5694478900983,12.));
#67246=CARTESIAN_POINT('Ctrl Pts',(8.31664872507007,-72.5921258716899,0.));
#67247=CARTESIAN_POINT('Ctrl Pts',(8.31664872507007,-72.5921258716899,12.));
#67248=CARTESIAN_POINT('Ctrl Pts',(8.32910101025652,-72.614825838529,0.));
#67249=CARTESIAN_POINT('Ctrl Pts',(8.32910101025652,-72.614825838529,12.));
#67250=CARTESIAN_POINT('Ctrl Pts',(8.34159300456964,-72.6375476785208,0.));
#67251=CARTESIAN_POINT('Ctrl Pts',(8.34159300456964,-72.6375476785208,12.));
#67252=CARTESIAN_POINT('Ctrl Pts',(8.35412470580082,-72.6602912799689,0.));
#67253=CARTESIAN_POINT('Ctrl Pts',(8.35412470580082,-72.6602912799689,12.));
#67254=CARTESIAN_POINT('Ctrl Pts',(8.36669611166833,-72.68305653157,0.));
#67255=CARTESIAN_POINT('Ctrl Pts',(8.36669611166833,-72.68305653157,12.));
#67256=CARTESIAN_POINT('Ctrl Pts',(8.37930721981734,-72.7058433224072,0.));
#67257=CARTESIAN_POINT('Ctrl Pts',(8.37930721981734,-72.7058433224072,12.));
#67258=CARTESIAN_POINT('Ctrl Pts',(8.39195802781406,-72.728651541938,0.));
#67259=CARTESIAN_POINT('Ctrl Pts',(8.39195802781406,-72.728651541938,12.));
#67260=CARTESIAN_POINT('Ctrl Pts',(8.40464853314492,-72.7514810799932,0.));
#67261=CARTESIAN_POINT('Ctrl Pts',(8.40464853314492,-72.7514810799932,12.));
#67262=CARTESIAN_POINT('Ctrl Pts',(8.41737873322352,-72.7743318267876,0.));
#67263=CARTESIAN_POINT('Ctrl Pts',(8.41737873322352,-72.7743318267876,12.));
#67264=CARTESIAN_POINT('Ctrl Pts',(8.4301486253917,-72.7972036729283,0.));
#67265=CARTESIAN_POINT('Ctrl Pts',(8.4301486253917,-72.7972036729283,12.));
#67266=CARTESIAN_POINT('Ctrl Pts',(8.44295820691906,-72.8200965094197,0.));
#67267=CARTESIAN_POINT('Ctrl Pts',(8.44295820691906,-72.8200965094197,12.));
#67268=CARTESIAN_POINT('Ctrl Pts',(8.4558074749977,-72.8430102276703,0.));
#67269=CARTESIAN_POINT('Ctrl Pts',(8.4558074749977,-72.8430102276703,12.));
#67270=CARTESIAN_POINT('Ctrl Pts',(8.46869642673762,-72.8659447194918,0.));
#67271=CARTESIAN_POINT('Ctrl Pts',(8.46869642673762,-72.8659447194918,12.));
#67272=CARTESIAN_POINT('Ctrl Pts',(8.48162505917627,-72.888899877077,0.));
#67273=CARTESIAN_POINT('Ctrl Pts',(8.48162505917627,-72.888899877077,12.));
#67274=CARTESIAN_POINT('Ctrl Pts',(8.49459336928275,-72.9118755929785,0.));
#67275=CARTESIAN_POINT('Ctrl Pts',(8.49459336928275,-72.9118755929785,12.));
#67276=CARTESIAN_POINT('Ctrl Pts',(8.50760135395978,-72.9348717600837,0.));
#67277=CARTESIAN_POINT('Ctrl Pts',(8.50760135395978,-72.9348717600837,12.));
#67278=CARTESIAN_POINT('Ctrl Pts',(8.52064901004243,-72.9578882715923,0.));
#67279=CARTESIAN_POINT('Ctrl Pts',(8.52064901004243,-72.9578882715923,12.));
#67280=CARTESIAN_POINT('Ctrl Pts',(8.53373633429302,-72.9809250209843,0.));
#67281=CARTESIAN_POINT('Ctrl Pts',(8.53373633429302,-72.9809250209843,12.));
#67282=CARTESIAN_POINT('Ctrl Pts',(8.54686332340438,-73.0039819020663,0.));
#67283=CARTESIAN_POINT('Ctrl Pts',(8.54686332340438,-73.0039819020663,12.));
#67284=CARTESIAN_POINT('Ctrl Pts',(8.56002997400095,-73.0270588090193,0.));
#67285=CARTESIAN_POINT('Ctrl Pts',(8.56002997400095,-73.0270588090193,12.));
#67286=CARTESIAN_POINT('Ctrl Pts',(8.57323628263594,-73.0501556364482,0.));
#67287=CARTESIAN_POINT('Ctrl Pts',(8.57323628263594,-73.0501556364482,12.));
#67288=CARTESIAN_POINT('Ctrl Pts',(8.58648224578722,-73.073272279419,0.));
#67289=CARTESIAN_POINT('Ctrl Pts',(8.58648224578722,-73.073272279419,12.));
#67290=CARTESIAN_POINT('Ctrl Pts',(8.59976785984538,-73.0964086335226,0.));
#67291=CARTESIAN_POINT('Ctrl Pts',(8.59976785984538,-73.0964086335226,12.));
#67292=CARTESIAN_POINT('Ctrl Pts',(8.61309312111988,-73.1195645948169,0.));
#67293=CARTESIAN_POINT('Ctrl Pts',(8.61309312111988,-73.1195645948169,12.));
#67294=CARTESIAN_POINT('Ctrl Pts',(8.62645802585474,-73.142740059703,0.));
#67295=CARTESIAN_POINT('Ctrl Pts',(8.62645802585474,-73.142740059703,12.));
#67296=CARTESIAN_POINT('Ctrl Pts',(8.63986257023734,-73.165934924813,0.));
#67297=CARTESIAN_POINT('Ctrl Pts',(8.63986257023734,-73.165934924813,12.));
#67298=CARTESIAN_POINT('Ctrl Pts',(8.65330675040535,-73.1891490869057,0.));
#67299=CARTESIAN_POINT('Ctrl Pts',(8.65330675040535,-73.1891490869057,12.));
#67300=CARTESIAN_POINT('Ctrl Pts',(8.66679056245095,-73.2123824427212,0.));
#67301=CARTESIAN_POINT('Ctrl Pts',(8.66679056245095,-73.2123824427212,12.));
#67302=CARTESIAN_POINT('Ctrl Pts',(8.68031400241883,-73.2356348889704,0.));
#67303=CARTESIAN_POINT('Ctrl Pts',(8.68031400241883,-73.2356348889704,12.));
#67304=CARTESIAN_POINT('Ctrl Pts',(8.69387706629303,-73.2589063226373,0.));
#67305=CARTESIAN_POINT('Ctrl Pts',(8.69387706629303,-73.2589063226373,12.));
#67306=CARTESIAN_POINT('Ctrl Pts',(8.70747974998244,-73.282196641216,0.));
#67307=CARTESIAN_POINT('Ctrl Pts',(8.70747974998244,-73.282196641216,12.));
#67308=CARTESIAN_POINT('Ctrl Pts',(8.72112204930231,-73.3055057429744,0.));
#67309=CARTESIAN_POINT('Ctrl Pts',(8.72112204930231,-73.3055057429744,12.));
#67310=CARTESIAN_POINT('Ctrl Pts',(8.73480395995359,-73.3288335271989,0.));
#67311=CARTESIAN_POINT('Ctrl Pts',(8.73480395995359,-73.3288335271989,12.));
#67312=CARTESIAN_POINT('Ctrl Pts',(8.74852547749735,-73.3521798944595,0.));
#67313=CARTESIAN_POINT('Ctrl Pts',(8.74852547749735,-73.3521798944595,12.));
#67314=CARTESIAN_POINT('Ctrl Pts',(8.76228659740304,-73.3755447460235,0.));
#67315=CARTESIAN_POINT('Ctrl Pts',(8.76228659740304,-73.3755447460235,12.));
#67316=CARTESIAN_POINT('Ctrl Pts',(8.77608731509303,-73.3989279832808,0.));
#67317=CARTESIAN_POINT('Ctrl Pts',(8.77608731509303,-73.3989279832808,12.));
#67318=CARTESIAN_POINT('Ctrl Pts',(8.78992762598737,-73.422329507112,0.));
#67319=CARTESIAN_POINT('Ctrl Pts',(8.78992762598737,-73.422329507112,12.));
#67320=CARTESIAN_POINT('Ctrl Pts',(8.80380752553713,-73.4457492173949,0.));
#67321=CARTESIAN_POINT('Ctrl Pts',(8.80380752553713,-73.4457492173949,12.));
#67322=CARTESIAN_POINT('Ctrl Pts',(8.81772700927592,-73.4691870121608,0.));
#67323=CARTESIAN_POINT('Ctrl Pts',(8.81772700927592,-73.4691870121608,12.));
#67324=CARTESIAN_POINT('Ctrl Pts',(8.83168607277414,-73.4926427882787,0.));
#67325=CARTESIAN_POINT('Ctrl Pts',(8.83168607277414,-73.4926427882787,12.));
#67326=CARTESIAN_POINT('Ctrl Pts',(8.84568471153893,-73.5161164429765,0.));
#67327=CARTESIAN_POINT('Ctrl Pts',(8.84568471153893,-73.5161164429765,12.));
#67328=CARTESIAN_POINT('Ctrl Pts',(8.85972292092182,-73.5396078751672,0.));
#67329=CARTESIAN_POINT('Ctrl Pts',(8.85972292092182,-73.5396078751672,12.));
#67330=CARTESIAN_POINT('Ctrl Pts',(8.87380069602954,-73.5631169867113,0.));
#67331=CARTESIAN_POINT('Ctrl Pts',(8.87380069602954,-73.5631169867113,12.));
#67332=CARTESIAN_POINT('Ctrl Pts',(8.8879180316034,-73.5866436840493,0.));
#67333=CARTESIAN_POINT('Ctrl Pts',(8.8879180316034,-73.5866436840493,12.));
#67334=CARTESIAN_POINT('Ctrl Pts',(8.9020749219887,-73.6101878785868,0.));
#67335=CARTESIAN_POINT('Ctrl Pts',(8.9020749219887,-73.6101878785868,12.));
#67336=CARTESIAN_POINT('Ctrl Pts',(8.91627136139886,-73.6337494830846,0.));
#67337=CARTESIAN_POINT('Ctrl Pts',(8.91627136139886,-73.6337494830846,12.));
#67338=CARTESIAN_POINT('Ctrl Pts',(8.9305073441197,-73.6573284088088,0.));
#67339=CARTESIAN_POINT('Ctrl Pts',(8.9305073441197,-73.6573284088088,12.));
#67340=CARTESIAN_POINT('Ctrl Pts',(8.94478286474382,-73.6809245622361,0.));
#67341=CARTESIAN_POINT('Ctrl Pts',(8.94478286474382,-73.6809245622361,12.));
#67342=CARTESIAN_POINT('Ctrl Pts',(8.95909791836289,-73.7045378422775,0.));
#67343=CARTESIAN_POINT('Ctrl Pts',(8.95909791836289,-73.7045378422775,12.));
#67344=CARTESIAN_POINT('Ctrl Pts',(8.97345250083917,-73.7281681364031,0.));
#67345=CARTESIAN_POINT('Ctrl Pts',(8.97345250083917,-73.7281681364031,12.));
#67346=CARTESIAN_POINT('Ctrl Pts',(8.98784660837827,-73.7518153262253,0.));
#67347=CARTESIAN_POINT('Ctrl Pts',(8.98784660837827,-73.7518153262253,12.));
#67348=CARTESIAN_POINT('Ctrl Pts',(9.00228023701466,-73.7754792943925,0.));
#67349=CARTESIAN_POINT('Ctrl Pts',(9.00228023701466,-73.7754792943925,12.));
#67350=CARTESIAN_POINT('Ctrl Pts',(9.01675338208221,-73.7991599312731,0.));
#67351=CARTESIAN_POINT('Ctrl Pts',(9.01675338208221,-73.7991599312731,12.));
#67352=CARTESIAN_POINT('Ctrl Pts',(9.0312660377798,-73.8228571411607,0.));
#67353=CARTESIAN_POINT('Ctrl Pts',(9.0312660377798,-73.8228571411607,12.));
#67354=CARTESIAN_POINT('Ctrl Pts',(9.04581819646384,-73.8465708500679,0.));
#67355=CARTESIAN_POINT('Ctrl Pts',(9.04581819646384,-73.8465708500679,12.));
#67356=CARTESIAN_POINT('Ctrl Pts',(9.06040984889249,-73.870301007746,0.));
#67357=CARTESIAN_POINT('Ctrl Pts',(9.06040984889249,-73.870301007746,12.));
#67358=CARTESIAN_POINT('Ctrl Pts',(9.07504098570546,-73.8940475821756,0.));
#67359=CARTESIAN_POINT('Ctrl Pts',(9.07504098570546,-73.8940475821756,12.));
#67360=CARTESIAN_POINT('Ctrl Pts',(9.08677747601237,-73.9130579611989,0.));
#67361=CARTESIAN_POINT('Ctrl Pts',(9.08677747601237,-73.9130579611989,12.));
#67362=CARTESIAN_POINT('Ctrl Pts',(9.09559760528458,-73.9273231219464,0.));
#67363=CARTESIAN_POINT('Ctrl Pts',(9.09559760528458,-73.9273231219464,12.));
#67364=CARTESIAN_POINT('Ctrl Pts',(9.10148558516323,-73.9368365074164,0.));
#67365=CARTESIAN_POINT('Ctrl Pts',(9.10148558516323,-73.9368365074164,12.));
#67366=CARTESIAN_POINT('Ctrl Pts',(9.10443154852686,-73.9415940197274,0.));
#67367=CARTESIAN_POINT('Ctrl Pts',(9.10443154852686,-73.9415940197274,12.));
#67368=CARTESIAN_POINT('',(6.95102489306925,-69.6540253893192,0.));
#67369=CARTESIAN_POINT('Ctrl Pts',(6.95102489306925,-69.6540253893192,0.));
#67370=CARTESIAN_POINT('Ctrl Pts',(6.95238884849024,-69.6576616146467,0.));
#67371=CARTESIAN_POINT('Ctrl Pts',(6.95512065317599,-69.664938391983,0.));
#67372=CARTESIAN_POINT('Ctrl Pts',(6.9592300417359,-69.6758665380378,0.));
#67373=CARTESIAN_POINT('Ctrl Pts',(6.96473259049512,-69.6904633605421,0.));
#67374=CARTESIAN_POINT('Ctrl Pts',(6.97164972291439,-69.7087526479973,0.));
#67375=CARTESIAN_POINT('Ctrl Pts',(6.97860581164526,-69.7270851557366,0.));
#67376=CARTESIAN_POINT('Ctrl Pts',(6.98560086924213,-69.7454607995607,0.));
#67377=CARTESIAN_POINT('Ctrl Pts',(6.9926349102794,-69.7638794280419,0.));
#67378=CARTESIAN_POINT('Ctrl Pts',(6.99970795069475,-69.782340824259,0.));
#67379=CARTESIAN_POINT('Ctrl Pts',(7.0068200071815,-69.8008447346863,0.));
#67380=CARTESIAN_POINT('Ctrl Pts',(7.01397109655454,-69.8193908913722,0.));
#67381=CARTESIAN_POINT('Ctrl Pts',(7.02116123514451,-69.8379790360518,0.));
#67382=CARTESIAN_POINT('Ctrl Pts',(7.02839043811812,-69.8566089455375,0.));
#67383=CARTESIAN_POINT('Ctrl Pts',(7.0356587197222,-69.8752804235238,0.));
#67384=CARTESIAN_POINT('Ctrl Pts',(7.04296609362165,-69.8939932885841,0.));
#67385=CARTESIAN_POINT('Ctrl Pts',(7.05031257318115,-69.9127473642099,0.));
#67386=CARTESIAN_POINT('Ctrl Pts',(7.05769817180856,-69.9315424664291,0.));
#67387=CARTESIAN_POINT('Ctrl Pts',(7.06512290312849,-69.9503783975727,0.));
#67388=CARTESIAN_POINT('Ctrl Pts',(7.0725867808083,-69.9692549527296,0.));
#67389=CARTESIAN_POINT('Ctrl Pts',(7.08008981844651,-69.988171923788,0.));
#67390=CARTESIAN_POINT('Ctrl Pts',(7.08763202944245,-70.0071291040766,0.));
#67391=CARTESIAN_POINT('Ctrl Pts',(7.09521342684248,-70.0261262936388,0.));
#67392=CARTESIAN_POINT('Ctrl Pts',(7.10283402335033,-70.0451632990086,0.));
#67393=CARTESIAN_POINT('Ctrl Pts',(7.11049383140445,-70.0642399306869,0.));
#67394=CARTESIAN_POINT('Ctrl Pts',(7.11819286322825,-70.0833560013975,0.));
#67395=CARTESIAN_POINT('Ctrl Pts',(7.12593113088903,-70.1025113239495,0.));
#67396=CARTESIAN_POINT('Ctrl Pts',(7.13370864634442,-70.1217057094499,0.));
#67397=CARTESIAN_POINT('Ctrl Pts',(7.14152542142373,-70.1409389682424,0.));
#67398=CARTESIAN_POINT('Ctrl Pts',(7.14938146780813,-70.1602109107202,0.));
#67399=CARTESIAN_POINT('Ctrl Pts',(7.15727679700932,-70.1795213481185,0.));
#67400=CARTESIAN_POINT('Ctrl Pts',(7.16521142033863,-70.1988700934593,0.));
#67401=CARTESIAN_POINT('Ctrl Pts',(7.17318534889715,-70.2182569618994,0.));
#67402=CARTESIAN_POINT('Ctrl Pts',(7.18119859359777,-70.2376817702215,0.));
#67403=CARTESIAN_POINT('Ctrl Pts',(7.18925116517554,-70.2571443365192,0.));
#67404=CARTESIAN_POINT('Ctrl Pts',(7.19734307419872,-70.2766444798285,0.));
#67405=CARTESIAN_POINT('Ctrl Pts',(7.20547433107482,-70.2961820197077,0.));
#67406=CARTESIAN_POINT('Ctrl Pts',(7.21364494605449,-70.3157567762588,0.));
#67407=CARTESIAN_POINT('Ctrl Pts',(7.2218549292319,-70.3353685703112,0.));
#67408=CARTESIAN_POINT('Ctrl Pts',(7.23010429054228,-70.3550172235486,0.));
#67409=CARTESIAN_POINT('Ctrl Pts',(7.23839303975606,-70.3747025586552,0.));
#67410=CARTESIAN_POINT('Ctrl Pts',(7.24672118647084,-70.3944243994504,0.));
#67411=CARTESIAN_POINT('Ctrl Pts',(7.25508874012042,-70.4141825708178,0.));
#67412=CARTESIAN_POINT('Ctrl Pts',(7.26349570998032,-70.4339768986346,0.));
#67413=CARTESIAN_POINT('Ctrl Pts',(7.27194210517062,-70.4538072096992,0.));
#67414=CARTESIAN_POINT('Ctrl Pts',(7.2804279346547,-70.4736733316487,0.));
#67415=CARTESIAN_POINT('Ctrl Pts',(7.28895320723861,-70.4935750929058,0.));
#67416=CARTESIAN_POINT('Ctrl Pts',(7.29751793157822,-70.5135123227169,0.));
#67417=CARTESIAN_POINT('Ctrl Pts',(7.30612211618052,-70.5334848511681,0.));
#67418=CARTESIAN_POINT('Ctrl Pts',(7.31476576940391,-70.5534925092043,0.));
#67419=CARTESIAN_POINT('Ctrl Pts',(7.32344889945219,-70.5735351286476,0.));
#67420=CARTESIAN_POINT('Ctrl Pts',(7.3321715143759,-70.5936125421946,0.));
#67421=CARTESIAN_POINT('Ctrl Pts',(7.34093362208007,-70.6137245833996,0.));
#67422=CARTESIAN_POINT('Ctrl Pts',(7.34973523032577,-70.6338710866562,0.));
#67423=CARTESIAN_POINT('Ctrl Pts',(7.35857634673054,-70.6540518871775,0.));
#67424=CARTESIAN_POINT('Ctrl Pts',(7.367456978763,-70.6742668209687,0.));
#67425=CARTESIAN_POINT('Ctrl Pts',(7.37637713374767,-70.694515724827,0.));
#67426=CARTESIAN_POINT('Ctrl Pts',(7.38533681887032,-70.7147984363424,0.));
#67427=CARTESIAN_POINT('Ctrl Pts',(7.3943360411789,-70.735114793895,0.));
#67428=CARTESIAN_POINT('Ctrl Pts',(7.40337480758229,-70.7554646366514,0.));
#67429=CARTESIAN_POINT('Ctrl Pts',(7.41245312484486,-70.7758478045576,0.));
#67430=CARTESIAN_POINT('Ctrl Pts',(7.42157099959315,-70.7962641383351,0.));
#67431=CARTESIAN_POINT('Ctrl Pts',(7.43072843832007,-70.8167134794738,0.));
#67432=CARTESIAN_POINT('Ctrl Pts',(7.43992544738606,-70.8371956702242,0.));
#67433=CARTESIAN_POINT('Ctrl Pts',(7.44916203301644,-70.8577105535841,0.));
#67434=CARTESIAN_POINT('Ctrl Pts',(7.45843820129775,-70.8782579732885,0.));
#67435=CARTESIAN_POINT('Ctrl Pts',(7.46775395818518,-70.8988377738088,0.));
#67436=CARTESIAN_POINT('Ctrl Pts',(7.47710930950553,-70.9194498003483,0.));
#67437=CARTESIAN_POINT('Ctrl Pts',(7.48650426095822,-70.9400938988373,0.));
#67438=CARTESIAN_POINT('Ctrl Pts',(7.49593881811141,-70.9607699159234,0.));
#67439=CARTESIAN_POINT('Ctrl Pts',(7.50541298639948,-70.9814776989637,0.));
#67440=CARTESIAN_POINT('Ctrl Pts',(7.51492677113111,-71.0022170960235,0.));
#67441=CARTESIAN_POINT('Ctrl Pts',(7.52448017749135,-71.0229879558713,0.));
#67442=CARTESIAN_POINT('Ctrl Pts',(7.53407321054253,-71.0437901279722,0.));
#67443=CARTESIAN_POINT('Ctrl Pts',(7.54370587521947,-71.0646234624783,0.));
#67444=CARTESIAN_POINT('Ctrl Pts',(7.55337817632872,-71.0854878102203,0.));
#67445=CARTESIAN_POINT('Ctrl Pts',(7.56309011855616,-71.1063830227074,0.));
#67446=CARTESIAN_POINT('Ctrl Pts',(7.57284170646865,-71.1273089521218,0.));
#67447=CARTESIAN_POINT('Ctrl Pts',(7.58263294451465,-71.1482654513133,0.));
#67448=CARTESIAN_POINT('Ctrl Pts',(7.59246383701859,-71.1692523737887,0.));
#67449=CARTESIAN_POINT('Ctrl Pts',(7.60233438818156,-71.1902695737063,0.));
#67450=CARTESIAN_POINT('Ctrl Pts',(7.61224460208886,-71.2113169058778,0.));
#67451=CARTESIAN_POINT('Ctrl Pts',(7.62219448271124,-71.232394225762,0.));
#67452=CARTESIAN_POINT('Ctrl Pts',(7.63218403390514,-71.2535013894587,0.));
#67453=CARTESIAN_POINT('Ctrl Pts',(7.64221325940671,-71.2746382536974,0.));
#67454=CARTESIAN_POINT('Ctrl Pts',(7.65228216283342,-71.2958046758334,0.));
#67455=CARTESIAN_POINT('Ctrl Pts',(7.66239074769118,-71.3170005138474,0.));
#67456=CARTESIAN_POINT('Ctrl Pts',(7.67253901737539,-71.3382256263405,0.));
#67457=CARTESIAN_POINT('Ctrl Pts',(7.68272697517102,-71.3594798725294,0.));
#67458=CARTESIAN_POINT('Ctrl Pts',(7.69295462424646,-71.380763112236,0.));
#67459=CARTESIAN_POINT('Ctrl Pts',(7.70322196765572,-71.4020752058827,0.));
#67460=CARTESIAN_POINT('Ctrl Pts',(7.71352900834537,-71.4234160144943,0.));
#67461=CARTESIAN_POINT('Ctrl Pts',(7.72387574915544,-71.4447853996919,0.));
#67462=CARTESIAN_POINT('Ctrl Pts',(7.73426219281931,-71.4661832236881,0.));
#67463=CARTESIAN_POINT('Ctrl Pts',(7.74468834195734,-71.487609349277,0.));
#67464=CARTESIAN_POINT('Ctrl Pts',(7.75515419907954,-71.5090636398307,0.));
#67465=CARTESIAN_POINT('Ctrl Pts',(7.76565976659218,-71.5305459592987,0.));
#67466=CARTESIAN_POINT('Ctrl Pts',(7.77620504679867,-71.5520561722039,0.));
#67467=CARTESIAN_POINT('Ctrl Pts',(7.78679004189934,-71.5735941436366,0.));
#67468=CARTESIAN_POINT('Ctrl Pts',(7.79741475398511,-71.5951597392471,0.));
#67469=CARTESIAN_POINT('Ctrl Pts',(7.80807918504016,-71.616752825242,0.));
#67470=CARTESIAN_POINT('Ctrl Pts',(7.81878333694855,-71.638373268384,0.));
#67471=CARTESIAN_POINT('Ctrl Pts',(7.82952721149503,-71.6600209359869,0.));
#67472=CARTESIAN_POINT('Ctrl Pts',(7.84031081036488,-71.681695695912,0.));
#67473=CARTESIAN_POINT('Ctrl Pts',(7.85113413513738,-71.7033974165576,0.));
#67474=CARTESIAN_POINT('Ctrl Pts',(7.86199718728829,-71.7251259668573,0.));
#67475=CARTESIAN_POINT('Ctrl Pts',(7.87289996819653,-71.7468812162795,0.));
#67476=CARTESIAN_POINT('Ctrl Pts',(7.88384247914521,-71.768663034824,0.));
#67477=CARTESIAN_POINT('Ctrl Pts',(7.89482472132134,-71.7904712930172,0.));
#67478=CARTESIAN_POINT('Ctrl Pts',(7.90584669580955,-71.8123058619038,0.));
#67479=CARTESIAN_POINT('Ctrl Pts',(7.9169084035937,-71.8341666130424,0.));
#67480=CARTESIAN_POINT('Ctrl Pts',(7.92800984556399,-71.8560534185071,0.));
#67481=CARTESIAN_POINT('Ctrl Pts',(7.93915102251795,-71.8779661508833,0.));
#67482=CARTESIAN_POINT('Ctrl Pts',(7.95033193516045,-71.8999046832642,0.));
#67483=CARTESIAN_POINT('Ctrl Pts',(7.96155258409751,-71.9218688892426,0.));
#67484=CARTESIAN_POINT('Ctrl Pts',(7.97281296983701,-71.9438586429072,0.));
#67485=CARTESIAN_POINT('Ctrl Pts',(7.98411309279597,-71.9658738188421,0.));
#67486=CARTESIAN_POINT('Ctrl Pts',(7.99545295330181,-71.9879142921248,0.));
#67487=CARTESIAN_POINT('Ctrl Pts',(8.00683255159249,-72.0099799383216,0.));
#67488=CARTESIAN_POINT('Ctrl Pts',(8.01825188781069,-72.0320706334802,0.));
#67489=CARTESIAN_POINT('Ctrl Pts',(8.02971096200327,-72.0541862541262,0.));
#67490=CARTESIAN_POINT('Ctrl Pts',(8.04120977412891,-72.0763266772632,0.));
#67491=CARTESIAN_POINT('Ctrl Pts',(8.05274832405956,-72.0984917803702,0.));
#67492=CARTESIAN_POINT('Ctrl Pts',(8.06432661158088,-72.1206814413985,0.));
#67493=CARTESIAN_POINT('Ctrl Pts',(8.07594463638699,-72.1428955387648,0.));
#67494=CARTESIAN_POINT('Ctrl Pts',(8.08760239807814,-72.165133951346,0.));
#67495=CARTESIAN_POINT('Ctrl Pts',(8.09929989616873,-72.18739655848,0.));
#67496=CARTESIAN_POINT('Ctrl Pts',(8.11103713008921,-72.2096832399626,0.));
#67497=CARTESIAN_POINT('Ctrl Pts',(8.12281409918661,-72.2319938760451,0.));
#67498=CARTESIAN_POINT('Ctrl Pts',(8.13463080272028,-72.2543283474279,0.));
#67499=CARTESIAN_POINT('Ctrl Pts',(8.14648723985792,-72.2766865352552,0.));
#67500=CARTESIAN_POINT('Ctrl Pts',(8.15838340968327,-72.2990683211155,0.));
#67501=CARTESIAN_POINT('Ctrl Pts',(8.17031931119881,-72.3214735870402,0.));
#67502=CARTESIAN_POINT('Ctrl Pts',(8.18229494332621,-72.3439022155007,0.));
#67503=CARTESIAN_POINT('Ctrl Pts',(8.19431030490318,-72.3663540894034,0.));
#67504=CARTESIAN_POINT('Ctrl Pts',(8.20636539467781,-72.3888290920845,0.));
#67505=CARTESIAN_POINT('Ctrl Pts',(8.21846021131563,-72.4113271073091,0.));
#67506=CARTESIAN_POINT('Ctrl Pts',(8.23059475340354,-72.4338480192701,0.));
#67507=CARTESIAN_POINT('Ctrl Pts',(8.24276901945036,-72.4563917125842,0.));
#67508=CARTESIAN_POINT('Ctrl Pts',(8.25498300788492,-72.4789580722871,0.));
#67509=CARTESIAN_POINT('Ctrl Pts',(8.26723671704923,-72.501546983825,0.));
#67510=CARTESIAN_POINT('Ctrl Pts',(8.27953014520384,-72.524158333056,0.));
#67511=CARTESIAN_POINT('Ctrl Pts',(8.29186329053288,-72.5467920062522,0.));
#67512=CARTESIAN_POINT('Ctrl Pts',(8.30423615114454,-72.5694478900983,0.));
#67513=CARTESIAN_POINT('Ctrl Pts',(8.31664872507007,-72.5921258716899,0.));
#67514=CARTESIAN_POINT('Ctrl Pts',(8.32910101025652,-72.614825838529,0.));
#67515=CARTESIAN_POINT('Ctrl Pts',(8.34159300456964,-72.6375476785208,0.));
#67516=CARTESIAN_POINT('Ctrl Pts',(8.35412470580082,-72.6602912799689,0.));
#67517=CARTESIAN_POINT('Ctrl Pts',(8.36669611166833,-72.68305653157,0.));
#67518=CARTESIAN_POINT('Ctrl Pts',(8.37930721981734,-72.7058433224072,0.));
#67519=CARTESIAN_POINT('Ctrl Pts',(8.39195802781406,-72.728651541938,0.));
#67520=CARTESIAN_POINT('Ctrl Pts',(8.40464853314492,-72.7514810799932,0.));
#67521=CARTESIAN_POINT('Ctrl Pts',(8.41737873322352,-72.7743318267876,0.));
#67522=CARTESIAN_POINT('Ctrl Pts',(8.4301486253917,-72.7972036729283,0.));
#67523=CARTESIAN_POINT('Ctrl Pts',(8.44295820691906,-72.8200965094197,0.));
#67524=CARTESIAN_POINT('Ctrl Pts',(8.4558074749977,-72.8430102276703,0.));
#67525=CARTESIAN_POINT('Ctrl Pts',(8.46869642673762,-72.8659447194918,0.));
#67526=CARTESIAN_POINT('Ctrl Pts',(8.48162505917627,-72.888899877077,0.));
#67527=CARTESIAN_POINT('Ctrl Pts',(8.49459336928275,-72.9118755929785,0.));
#67528=CARTESIAN_POINT('Ctrl Pts',(8.50760135395978,-72.9348717600837,0.));
#67529=CARTESIAN_POINT('Ctrl Pts',(8.52064901004243,-72.9578882715923,0.));
#67530=CARTESIAN_POINT('Ctrl Pts',(8.53373633429302,-72.9809250209843,0.));
#67531=CARTESIAN_POINT('Ctrl Pts',(8.54686332340438,-73.0039819020663,0.));
#67532=CARTESIAN_POINT('Ctrl Pts',(8.56002997400095,-73.0270588090193,0.));
#67533=CARTESIAN_POINT('Ctrl Pts',(8.57323628263594,-73.0501556364482,0.));
#67534=CARTESIAN_POINT('Ctrl Pts',(8.58648224578722,-73.073272279419,0.));
#67535=CARTESIAN_POINT('Ctrl Pts',(8.59976785984538,-73.0964086335226,0.));
#67536=CARTESIAN_POINT('Ctrl Pts',(8.61309312111988,-73.1195645948169,0.));
#67537=CARTESIAN_POINT('Ctrl Pts',(8.62645802585474,-73.142740059703,0.));
#67538=CARTESIAN_POINT('Ctrl Pts',(8.63986257023734,-73.165934924813,0.));
#67539=CARTESIAN_POINT('Ctrl Pts',(8.65330675040535,-73.1891490869057,0.));
#67540=CARTESIAN_POINT('Ctrl Pts',(8.66679056245095,-73.2123824427212,0.));
#67541=CARTESIAN_POINT('Ctrl Pts',(8.68031400241883,-73.2356348889704,0.));
#67542=CARTESIAN_POINT('Ctrl Pts',(8.69387706629303,-73.2589063226373,0.));
#67543=CARTESIAN_POINT('Ctrl Pts',(8.70747974998244,-73.282196641216,0.));
#67544=CARTESIAN_POINT('Ctrl Pts',(8.72112204930231,-73.3055057429744,0.));
#67545=CARTESIAN_POINT('Ctrl Pts',(8.73480395995359,-73.3288335271989,0.));
#67546=CARTESIAN_POINT('Ctrl Pts',(8.74852547749735,-73.3521798944595,0.));
#67547=CARTESIAN_POINT('Ctrl Pts',(8.76228659740304,-73.3755447460235,0.));
#67548=CARTESIAN_POINT('Ctrl Pts',(8.77608731509303,-73.3989279832808,0.));
#67549=CARTESIAN_POINT('Ctrl Pts',(8.78992762598737,-73.422329507112,0.));
#67550=CARTESIAN_POINT('Ctrl Pts',(8.80380752553713,-73.4457492173949,0.));
#67551=CARTESIAN_POINT('Ctrl Pts',(8.81772700927592,-73.4691870121608,0.));
#67552=CARTESIAN_POINT('Ctrl Pts',(8.83168607277414,-73.4926427882787,0.));
#67553=CARTESIAN_POINT('Ctrl Pts',(8.84568471153893,-73.5161164429765,0.));
#67554=CARTESIAN_POINT('Ctrl Pts',(8.85972292092182,-73.5396078751672,0.));
#67555=CARTESIAN_POINT('Ctrl Pts',(8.87380069602954,-73.5631169867113,0.));
#67556=CARTESIAN_POINT('Ctrl Pts',(8.8879180316034,-73.5866436840493,0.));
#67557=CARTESIAN_POINT('Ctrl Pts',(8.9020749219887,-73.6101878785868,0.));
#67558=CARTESIAN_POINT('Ctrl Pts',(8.91424402151027,-73.6303847393445,0.));
#67559=CARTESIAN_POINT('Ctrl Pts',(8.92359518177562,-73.645878630579,0.));
#67560=CARTESIAN_POINT('Ctrl Pts',(8.9301108881604,-73.6566618621799,0.));
#67561=CARTESIAN_POINT('Ctrl Pts',(8.93377955964004,-73.6627293782266,0.));
#67562=CARTESIAN_POINT('Ctrl Pts',(8.93459554655838,-73.6640787197675,0.));
#67563=CARTESIAN_POINT('',(6.95102489306925,-69.6540253893192,12.));
#67564=CARTESIAN_POINT('',(6.95102489306925,-69.6540253893192,0.));
#67565=CARTESIAN_POINT('Ctrl Pts',(8.93459554655838,-73.6640787197675,12.));
#67566=CARTESIAN_POINT('Ctrl Pts',(8.93377955964004,-73.6627293782266,12.));
#67567=CARTESIAN_POINT('Ctrl Pts',(8.9301108881604,-73.6566618621799,12.));
#67568=CARTESIAN_POINT('Ctrl Pts',(8.92359518177562,-73.645878630579,12.));
#67569=CARTESIAN_POINT('Ctrl Pts',(8.91424402151027,-73.6303847393445,12.));
#67570=CARTESIAN_POINT('Ctrl Pts',(8.9020749219887,-73.6101878785868,12.));
#67571=CARTESIAN_POINT('Ctrl Pts',(8.8879180316034,-73.5866436840493,12.));
#67572=CARTESIAN_POINT('Ctrl Pts',(8.87380069602954,-73.5631169867113,12.));
#67573=CARTESIAN_POINT('Ctrl Pts',(8.85972292092182,-73.5396078751672,12.));
#67574=CARTESIAN_POINT('Ctrl Pts',(8.84568471153893,-73.5161164429765,12.));
#67575=CARTESIAN_POINT('Ctrl Pts',(8.83168607277414,-73.4926427882787,12.));
#67576=CARTESIAN_POINT('Ctrl Pts',(8.81772700927592,-73.4691870121608,12.));
#67577=CARTESIAN_POINT('Ctrl Pts',(8.80380752553713,-73.4457492173949,12.));
#67578=CARTESIAN_POINT('Ctrl Pts',(8.78992762598737,-73.422329507112,12.));
#67579=CARTESIAN_POINT('Ctrl Pts',(8.77608731509303,-73.3989279832808,12.));
#67580=CARTESIAN_POINT('Ctrl Pts',(8.76228659740304,-73.3755447460235,12.));
#67581=CARTESIAN_POINT('Ctrl Pts',(8.74852547749735,-73.3521798944595,12.));
#67582=CARTESIAN_POINT('Ctrl Pts',(8.73480395995359,-73.3288335271989,12.));
#67583=CARTESIAN_POINT('Ctrl Pts',(8.72112204930231,-73.3055057429744,12.));
#67584=CARTESIAN_POINT('Ctrl Pts',(8.70747974998244,-73.282196641216,12.));
#67585=CARTESIAN_POINT('Ctrl Pts',(8.69387706629303,-73.2589063226373,12.));
#67586=CARTESIAN_POINT('Ctrl Pts',(8.68031400241883,-73.2356348889704,12.));
#67587=CARTESIAN_POINT('Ctrl Pts',(8.66679056245095,-73.2123824427212,12.));
#67588=CARTESIAN_POINT('Ctrl Pts',(8.65330675040535,-73.1891490869057,12.));
#67589=CARTESIAN_POINT('Ctrl Pts',(8.63986257023734,-73.165934924813,12.));
#67590=CARTESIAN_POINT('Ctrl Pts',(8.62645802585474,-73.142740059703,12.));
#67591=CARTESIAN_POINT('Ctrl Pts',(8.61309312111988,-73.1195645948169,12.));
#67592=CARTESIAN_POINT('Ctrl Pts',(8.59976785984538,-73.0964086335226,12.));
#67593=CARTESIAN_POINT('Ctrl Pts',(8.58648224578722,-73.073272279419,12.));
#67594=CARTESIAN_POINT('Ctrl Pts',(8.57323628263594,-73.0501556364482,12.));
#67595=CARTESIAN_POINT('Ctrl Pts',(8.56002997400095,-73.0270588090193,12.));
#67596=CARTESIAN_POINT('Ctrl Pts',(8.54686332340438,-73.0039819020663,12.));
#67597=CARTESIAN_POINT('Ctrl Pts',(8.53373633429302,-72.9809250209843,12.));
#67598=CARTESIAN_POINT('Ctrl Pts',(8.52064901004243,-72.9578882715923,12.));
#67599=CARTESIAN_POINT('Ctrl Pts',(8.50760135395978,-72.9348717600837,12.));
#67600=CARTESIAN_POINT('Ctrl Pts',(8.49459336928275,-72.9118755929785,12.));
#67601=CARTESIAN_POINT('Ctrl Pts',(8.48162505917627,-72.888899877077,12.));
#67602=CARTESIAN_POINT('Ctrl Pts',(8.46869642673762,-72.8659447194918,12.));
#67603=CARTESIAN_POINT('Ctrl Pts',(8.4558074749977,-72.8430102276703,12.));
#67604=CARTESIAN_POINT('Ctrl Pts',(8.44295820691906,-72.8200965094197,12.));
#67605=CARTESIAN_POINT('Ctrl Pts',(8.4301486253917,-72.7972036729283,12.));
#67606=CARTESIAN_POINT('Ctrl Pts',(8.41737873322352,-72.7743318267876,12.));
#67607=CARTESIAN_POINT('Ctrl Pts',(8.40464853314492,-72.7514810799932,12.));
#67608=CARTESIAN_POINT('Ctrl Pts',(8.39195802781406,-72.728651541938,12.));
#67609=CARTESIAN_POINT('Ctrl Pts',(8.37930721981734,-72.7058433224072,12.));
#67610=CARTESIAN_POINT('Ctrl Pts',(8.36669611166833,-72.68305653157,12.));
#67611=CARTESIAN_POINT('Ctrl Pts',(8.35412470580082,-72.6602912799689,12.));
#67612=CARTESIAN_POINT('Ctrl Pts',(8.34159300456964,-72.6375476785208,12.));
#67613=CARTESIAN_POINT('Ctrl Pts',(8.32910101025652,-72.614825838529,12.));
#67614=CARTESIAN_POINT('Ctrl Pts',(8.31664872507007,-72.5921258716899,12.));
#67615=CARTESIAN_POINT('Ctrl Pts',(8.30423615114454,-72.5694478900983,12.));
#67616=CARTESIAN_POINT('Ctrl Pts',(8.29186329053288,-72.5467920062522,12.));
#67617=CARTESIAN_POINT('Ctrl Pts',(8.27953014520384,-72.524158333056,12.));
#67618=CARTESIAN_POINT('Ctrl Pts',(8.26723671704923,-72.501546983825,12.));
#67619=CARTESIAN_POINT('Ctrl Pts',(8.25498300788492,-72.4789580722871,12.));
#67620=CARTESIAN_POINT('Ctrl Pts',(8.24276901945036,-72.4563917125842,12.));
#67621=CARTESIAN_POINT('Ctrl Pts',(8.23059475340354,-72.4338480192701,12.));
#67622=CARTESIAN_POINT('Ctrl Pts',(8.21846021131563,-72.4113271073091,12.));
#67623=CARTESIAN_POINT('Ctrl Pts',(8.20636539467781,-72.3888290920845,12.));
#67624=CARTESIAN_POINT('Ctrl Pts',(8.19431030490318,-72.3663540894034,12.));
#67625=CARTESIAN_POINT('Ctrl Pts',(8.18229494332621,-72.3439022155007,12.));
#67626=CARTESIAN_POINT('Ctrl Pts',(8.17031931119881,-72.3214735870402,12.));
#67627=CARTESIAN_POINT('Ctrl Pts',(8.15838340968327,-72.2990683211155,12.));
#67628=CARTESIAN_POINT('Ctrl Pts',(8.14648723985792,-72.2766865352552,12.));
#67629=CARTESIAN_POINT('Ctrl Pts',(8.13463080272028,-72.2543283474279,12.));
#67630=CARTESIAN_POINT('Ctrl Pts',(8.12281409918661,-72.2319938760451,12.));
#67631=CARTESIAN_POINT('Ctrl Pts',(8.11103713008921,-72.2096832399626,12.));
#67632=CARTESIAN_POINT('Ctrl Pts',(8.09929989616873,-72.18739655848,12.));
#67633=CARTESIAN_POINT('Ctrl Pts',(8.08760239807814,-72.165133951346,12.));
#67634=CARTESIAN_POINT('Ctrl Pts',(8.07594463638699,-72.1428955387648,12.));
#67635=CARTESIAN_POINT('Ctrl Pts',(8.06432661158088,-72.1206814413985,12.));
#67636=CARTESIAN_POINT('Ctrl Pts',(8.05274832405956,-72.0984917803702,12.));
#67637=CARTESIAN_POINT('Ctrl Pts',(8.04120977412891,-72.0763266772632,12.));
#67638=CARTESIAN_POINT('Ctrl Pts',(8.02971096200327,-72.0541862541262,12.));
#67639=CARTESIAN_POINT('Ctrl Pts',(8.01825188781069,-72.0320706334802,12.));
#67640=CARTESIAN_POINT('Ctrl Pts',(8.00683255159249,-72.0099799383216,12.));
#67641=CARTESIAN_POINT('Ctrl Pts',(7.99545295330181,-71.9879142921248,12.));
#67642=CARTESIAN_POINT('Ctrl Pts',(7.98411309279597,-71.9658738188421,12.));
#67643=CARTESIAN_POINT('Ctrl Pts',(7.97281296983701,-71.9438586429072,12.));
#67644=CARTESIAN_POINT('Ctrl Pts',(7.96155258409751,-71.9218688892426,12.));
#67645=CARTESIAN_POINT('Ctrl Pts',(7.95033193516045,-71.8999046832642,12.));
#67646=CARTESIAN_POINT('Ctrl Pts',(7.93915102251795,-71.8779661508833,12.));
#67647=CARTESIAN_POINT('Ctrl Pts',(7.92800984556399,-71.8560534185071,12.));
#67648=CARTESIAN_POINT('Ctrl Pts',(7.9169084035937,-71.8341666130424,12.));
#67649=CARTESIAN_POINT('Ctrl Pts',(7.90584669580955,-71.8123058619038,12.));
#67650=CARTESIAN_POINT('Ctrl Pts',(7.89482472132134,-71.7904712930172,12.));
#67651=CARTESIAN_POINT('Ctrl Pts',(7.88384247914521,-71.768663034824,12.));
#67652=CARTESIAN_POINT('Ctrl Pts',(7.87289996819653,-71.7468812162795,12.));
#67653=CARTESIAN_POINT('Ctrl Pts',(7.86199718728829,-71.7251259668573,12.));
#67654=CARTESIAN_POINT('Ctrl Pts',(7.85113413513738,-71.7033974165576,12.));
#67655=CARTESIAN_POINT('Ctrl Pts',(7.84031081036488,-71.681695695912,12.));
#67656=CARTESIAN_POINT('Ctrl Pts',(7.82952721149503,-71.6600209359869,12.));
#67657=CARTESIAN_POINT('Ctrl Pts',(7.81878333694855,-71.638373268384,12.));
#67658=CARTESIAN_POINT('Ctrl Pts',(7.80807918504016,-71.616752825242,12.));
#67659=CARTESIAN_POINT('Ctrl Pts',(7.79741475398511,-71.5951597392471,12.));
#67660=CARTESIAN_POINT('Ctrl Pts',(7.78679004189934,-71.5735941436366,12.));
#67661=CARTESIAN_POINT('Ctrl Pts',(7.77620504679867,-71.5520561722039,12.));
#67662=CARTESIAN_POINT('Ctrl Pts',(7.76565976659218,-71.5305459592987,12.));
#67663=CARTESIAN_POINT('Ctrl Pts',(7.75515419907954,-71.5090636398307,12.));
#67664=CARTESIAN_POINT('Ctrl Pts',(7.74468834195734,-71.487609349277,12.));
#67665=CARTESIAN_POINT('Ctrl Pts',(7.73426219281931,-71.4661832236881,12.));
#67666=CARTESIAN_POINT('Ctrl Pts',(7.72387574915544,-71.4447853996919,12.));
#67667=CARTESIAN_POINT('Ctrl Pts',(7.71352900834537,-71.4234160144943,12.));
#67668=CARTESIAN_POINT('Ctrl Pts',(7.70322196765572,-71.4020752058827,12.));
#67669=CARTESIAN_POINT('Ctrl Pts',(7.69295462424646,-71.380763112236,12.));
#67670=CARTESIAN_POINT('Ctrl Pts',(7.68272697517102,-71.3594798725294,12.));
#67671=CARTESIAN_POINT('Ctrl Pts',(7.67253901737539,-71.3382256263405,12.));
#67672=CARTESIAN_POINT('Ctrl Pts',(7.66239074769118,-71.3170005138474,12.));
#67673=CARTESIAN_POINT('Ctrl Pts',(7.65228216283342,-71.2958046758334,12.));
#67674=CARTESIAN_POINT('Ctrl Pts',(7.64221325940671,-71.2746382536974,12.));
#67675=CARTESIAN_POINT('Ctrl Pts',(7.63218403390514,-71.2535013894587,12.));
#67676=CARTESIAN_POINT('Ctrl Pts',(7.62219448271124,-71.232394225762,12.));
#67677=CARTESIAN_POINT('Ctrl Pts',(7.61224460208886,-71.2113169058778,12.));
#67678=CARTESIAN_POINT('Ctrl Pts',(7.60233438818156,-71.1902695737063,12.));
#67679=CARTESIAN_POINT('Ctrl Pts',(7.59246383701859,-71.1692523737887,12.));
#67680=CARTESIAN_POINT('Ctrl Pts',(7.58263294451465,-71.1482654513133,12.));
#67681=CARTESIAN_POINT('Ctrl Pts',(7.57284170646865,-71.1273089521218,12.));
#67682=CARTESIAN_POINT('Ctrl Pts',(7.56309011855616,-71.1063830227074,12.));
#67683=CARTESIAN_POINT('Ctrl Pts',(7.55337817632872,-71.0854878102203,12.));
#67684=CARTESIAN_POINT('Ctrl Pts',(7.54370587521947,-71.0646234624783,12.));
#67685=CARTESIAN_POINT('Ctrl Pts',(7.53407321054253,-71.0437901279722,12.));
#67686=CARTESIAN_POINT('Ctrl Pts',(7.52448017749135,-71.0229879558713,12.));
#67687=CARTESIAN_POINT('Ctrl Pts',(7.51492677113111,-71.0022170960235,12.));
#67688=CARTESIAN_POINT('Ctrl Pts',(7.50541298639948,-70.9814776989637,12.));
#67689=CARTESIAN_POINT('Ctrl Pts',(7.49593881811141,-70.9607699159234,12.));
#67690=CARTESIAN_POINT('Ctrl Pts',(7.48650426095822,-70.9400938988373,12.));
#67691=CARTESIAN_POINT('Ctrl Pts',(7.47710930950553,-70.9194498003483,12.));
#67692=CARTESIAN_POINT('Ctrl Pts',(7.46775395818518,-70.8988377738088,12.));
#67693=CARTESIAN_POINT('Ctrl Pts',(7.45843820129775,-70.8782579732885,12.));
#67694=CARTESIAN_POINT('Ctrl Pts',(7.44916203301644,-70.8577105535841,12.));
#67695=CARTESIAN_POINT('Ctrl Pts',(7.43992544738606,-70.8371956702242,12.));
#67696=CARTESIAN_POINT('Ctrl Pts',(7.43072843832007,-70.8167134794738,12.));
#67697=CARTESIAN_POINT('Ctrl Pts',(7.42157099959315,-70.7962641383351,12.));
#67698=CARTESIAN_POINT('Ctrl Pts',(7.41245312484486,-70.7758478045576,12.));
#67699=CARTESIAN_POINT('Ctrl Pts',(7.40337480758229,-70.7554646366514,12.));
#67700=CARTESIAN_POINT('Ctrl Pts',(7.3943360411789,-70.735114793895,12.));
#67701=CARTESIAN_POINT('Ctrl Pts',(7.38533681887032,-70.7147984363424,12.));
#67702=CARTESIAN_POINT('Ctrl Pts',(7.37637713374767,-70.694515724827,12.));
#67703=CARTESIAN_POINT('Ctrl Pts',(7.367456978763,-70.6742668209687,12.));
#67704=CARTESIAN_POINT('Ctrl Pts',(7.35857634673054,-70.6540518871775,12.));
#67705=CARTESIAN_POINT('Ctrl Pts',(7.34973523032577,-70.6338710866562,12.));
#67706=CARTESIAN_POINT('Ctrl Pts',(7.34093362208007,-70.6137245833996,12.));
#67707=CARTESIAN_POINT('Ctrl Pts',(7.3321715143759,-70.5936125421946,12.));
#67708=CARTESIAN_POINT('Ctrl Pts',(7.32344889945219,-70.5735351286476,12.));
#67709=CARTESIAN_POINT('Ctrl Pts',(7.31476576940391,-70.5534925092043,12.));
#67710=CARTESIAN_POINT('Ctrl Pts',(7.30612211618052,-70.5334848511681,12.));
#67711=CARTESIAN_POINT('Ctrl Pts',(7.29751793157822,-70.5135123227169,12.));
#67712=CARTESIAN_POINT('Ctrl Pts',(7.28895320723861,-70.4935750929058,12.));
#67713=CARTESIAN_POINT('Ctrl Pts',(7.2804279346547,-70.4736733316487,12.));
#67714=CARTESIAN_POINT('Ctrl Pts',(7.27194210517062,-70.4538072096992,12.));
#67715=CARTESIAN_POINT('Ctrl Pts',(7.26349570998032,-70.4339768986346,12.));
#67716=CARTESIAN_POINT('Ctrl Pts',(7.25508874012042,-70.4141825708178,12.));
#67717=CARTESIAN_POINT('Ctrl Pts',(7.24672118647084,-70.3944243994504,12.));
#67718=CARTESIAN_POINT('Ctrl Pts',(7.23839303975606,-70.3747025586552,12.));
#67719=CARTESIAN_POINT('Ctrl Pts',(7.23010429054228,-70.3550172235486,12.));
#67720=CARTESIAN_POINT('Ctrl Pts',(7.2218549292319,-70.3353685703112,12.));
#67721=CARTESIAN_POINT('Ctrl Pts',(7.21364494605449,-70.3157567762588,12.));
#67722=CARTESIAN_POINT('Ctrl Pts',(7.20547433107482,-70.2961820197077,12.));
#67723=CARTESIAN_POINT('Ctrl Pts',(7.19734307419872,-70.2766444798285,12.));
#67724=CARTESIAN_POINT('Ctrl Pts',(7.18925116517554,-70.2571443365192,12.));
#67725=CARTESIAN_POINT('Ctrl Pts',(7.18119859359777,-70.2376817702215,12.));
#67726=CARTESIAN_POINT('Ctrl Pts',(7.17318534889715,-70.2182569618994,12.));
#67727=CARTESIAN_POINT('Ctrl Pts',(7.16521142033863,-70.1988700934593,12.));
#67728=CARTESIAN_POINT('Ctrl Pts',(7.15727679700932,-70.1795213481185,12.));
#67729=CARTESIAN_POINT('Ctrl Pts',(7.14938146780813,-70.1602109107202,12.));
#67730=CARTESIAN_POINT('Ctrl Pts',(7.14152542142373,-70.1409389682424,12.));
#67731=CARTESIAN_POINT('Ctrl Pts',(7.13370864634442,-70.1217057094499,12.));
#67732=CARTESIAN_POINT('Ctrl Pts',(7.12593113088903,-70.1025113239495,12.));
#67733=CARTESIAN_POINT('Ctrl Pts',(7.11819286322825,-70.0833560013975,12.));
#67734=CARTESIAN_POINT('Ctrl Pts',(7.11049383140445,-70.0642399306869,12.));
#67735=CARTESIAN_POINT('Ctrl Pts',(7.10283402335033,-70.0451632990086,12.));
#67736=CARTESIAN_POINT('Ctrl Pts',(7.09521342684248,-70.0261262936388,12.));
#67737=CARTESIAN_POINT('Ctrl Pts',(7.08763202944245,-70.0071291040766,12.));
#67738=CARTESIAN_POINT('Ctrl Pts',(7.08008981844651,-69.988171923788,12.));
#67739=CARTESIAN_POINT('Ctrl Pts',(7.0725867808083,-69.9692549527296,12.));
#67740=CARTESIAN_POINT('Ctrl Pts',(7.06512290312849,-69.9503783975727,12.));
#67741=CARTESIAN_POINT('Ctrl Pts',(7.05769817180856,-69.9315424664291,12.));
#67742=CARTESIAN_POINT('Ctrl Pts',(7.05031257318115,-69.9127473642099,12.));
#67743=CARTESIAN_POINT('Ctrl Pts',(7.04296609362165,-69.8939932885841,12.));
#67744=CARTESIAN_POINT('Ctrl Pts',(7.0356587197222,-69.8752804235238,12.));
#67745=CARTESIAN_POINT('Ctrl Pts',(7.02839043811812,-69.8566089455375,12.));
#67746=CARTESIAN_POINT('Ctrl Pts',(7.02116123514451,-69.8379790360518,12.));
#67747=CARTESIAN_POINT('Ctrl Pts',(7.01397109655454,-69.8193908913722,12.));
#67748=CARTESIAN_POINT('Ctrl Pts',(7.0068200071815,-69.8008447346863,12.));
#67749=CARTESIAN_POINT('Ctrl Pts',(6.99970795069475,-69.782340824259,12.));
#67750=CARTESIAN_POINT('Ctrl Pts',(6.9926349102794,-69.7638794280419,12.));
#67751=CARTESIAN_POINT('Ctrl Pts',(6.98560086924213,-69.7454607995607,12.));
#67752=CARTESIAN_POINT('Ctrl Pts',(6.97860581164526,-69.7270851557366,12.));
#67753=CARTESIAN_POINT('Ctrl Pts',(6.97164972291439,-69.7087526479973,12.));
#67754=CARTESIAN_POINT('Ctrl Pts',(6.96473259049512,-69.6904633605421,12.));
#67755=CARTESIAN_POINT('Ctrl Pts',(6.9592300417359,-69.6758665380378,12.));
#67756=CARTESIAN_POINT('Ctrl Pts',(6.95512065317599,-69.664938391983,12.));
#67757=CARTESIAN_POINT('Ctrl Pts',(6.95238884849024,-69.6576616146467,12.));
#67758=CARTESIAN_POINT('Ctrl Pts',(6.95102489306925,-69.6540253893192,12.));
#67759=CARTESIAN_POINT('Ctrl Pts',(10.4355099267296,-73.4664795929938,-5.55111512312578E-16));
#67760=CARTESIAN_POINT('Ctrl Pts',(10.4355099267296,-73.4664795929938,4.));
#67761=CARTESIAN_POINT('Ctrl Pts',(10.4355099267296,-73.4664795929938,8.));
#67762=CARTESIAN_POINT('Ctrl Pts',(10.4355099267296,-73.4664795929938,12.));
#67763=CARTESIAN_POINT('Ctrl Pts',(10.4049225807075,-73.5720190200067,-5.55111512312578E-16));
#67764=CARTESIAN_POINT('Ctrl Pts',(10.4049225807075,-73.5720190200067,3.99999999999999));
#67765=CARTESIAN_POINT('Ctrl Pts',(10.4049225807075,-73.5720190200067,8.00000000000001));
#67766=CARTESIAN_POINT('Ctrl Pts',(10.4049225807075,-73.5720190200067,12.));
#67767=CARTESIAN_POINT('Ctrl Pts',(10.2883434191783,-73.7377969500798,-5.55111512312578E-16));
#67768=CARTESIAN_POINT('Ctrl Pts',(10.2883434191783,-73.7377969500798,4.00000000000001));
#67769=CARTESIAN_POINT('Ctrl Pts',(10.2883434191783,-73.7377969500798,7.99999999999999));
#67770=CARTESIAN_POINT('Ctrl Pts',(10.2883434191783,-73.7377969500798,12.));
#67771=CARTESIAN_POINT('Ctrl Pts',(10.1042001607579,-73.8116652760545,-5.55111512312578E-16));
#67772=CARTESIAN_POINT('Ctrl Pts',(10.1042001607579,-73.8116652760545,3.99999999999999));
#67773=CARTESIAN_POINT('Ctrl Pts',(10.1042001607579,-73.8116652760546,8.00000000000001));
#67774=CARTESIAN_POINT('Ctrl Pts',(10.1042001607579,-73.8116652760546,12.));
#67775=CARTESIAN_POINT('Ctrl Pts',(10.0225374821233,-73.8227522002495,-5.55111512312578E-16));
#67776=CARTESIAN_POINT('Ctrl Pts',(10.0225374821233,-73.8227522002495,4.));
#67777=CARTESIAN_POINT('Ctrl Pts',(10.0225374821233,-73.8227522002495,8.));
#67778=CARTESIAN_POINT('Ctrl Pts',(10.0225374821233,-73.8227522002495,12.));
#67779=CARTESIAN_POINT('',(10.4355099267296,-73.4664795929938,0.));
#67780=CARTESIAN_POINT('',(10.0225374821233,-73.8227522002494,0.));
#67781=CARTESIAN_POINT('Ctrl Pts',(10.4355099267296,-73.4664795929938,0.));
#67782=CARTESIAN_POINT('Ctrl Pts',(10.4049225807075,-73.5720190200067,-6.93334779979405E-31));
#67783=CARTESIAN_POINT('Ctrl Pts',(10.3383059169766,-73.6667492657628,3.85185988877447E-31));
#67784=CARTESIAN_POINT('Ctrl Pts',(10.2496275073219,-73.7314682122214,1.54074395550979E-31));
#67785=CARTESIAN_POINT('Ctrl Pts',(10.1831187000809,-73.7800074220654,-3.08148791101957E-32));
#67786=CARTESIAN_POINT('Ctrl Pts',(10.1042001607579,-73.8116652760545,-9.55261252416069E-31));
#67787=CARTESIAN_POINT('Ctrl Pts',(10.0225374821233,-73.8227522002495,4.62223186652938E-32));
#67788=CARTESIAN_POINT('',(10.0225374821233,-73.8227522002494,12.));
#67789=CARTESIAN_POINT('Ctrl Pts',(10.0225374821233,-73.8227522002495,-5.55111512312578E-16));
#67790=CARTESIAN_POINT('Ctrl Pts',(10.0225374821233,-73.8227522002495,4.));
#67791=CARTESIAN_POINT('Ctrl Pts',(10.0225374821233,-73.8227522002495,8.));
#67792=CARTESIAN_POINT('Ctrl Pts',(10.0225374821233,-73.8227522002495,12.));
#67793=CARTESIAN_POINT('',(10.4355099267296,-73.4664795929938,12.));
#67794=CARTESIAN_POINT('Ctrl Pts',(10.0225374821233,-73.8227522002495,12.));
#67795=CARTESIAN_POINT('Ctrl Pts',(10.1042001607579,-73.8116652760546,12.));
#67796=CARTESIAN_POINT('Ctrl Pts',(10.1831187000809,-73.7800074220654,12.));
#67797=CARTESIAN_POINT('Ctrl Pts',(10.2496275073219,-73.7314682122214,12.));
#67798=CARTESIAN_POINT('Ctrl Pts',(10.3383059169765,-73.6667492657628,12.));
#67799=CARTESIAN_POINT('Ctrl Pts',(10.4049225807075,-73.5720190200067,12.));
#67800=CARTESIAN_POINT('Ctrl Pts',(10.4355099267296,-73.4664795929938,12.));
#67801=CARTESIAN_POINT('Ctrl Pts',(10.4355099267296,-73.4664795929938,12.));
#67802=CARTESIAN_POINT('Ctrl Pts',(10.4355099267296,-73.4664795929938,8.));
#67803=CARTESIAN_POINT('Ctrl Pts',(10.4355099267296,-73.4664795929938,4.));
#67804=CARTESIAN_POINT('Ctrl Pts',(10.4355099267296,-73.4664795929938,-5.55111512312578E-16));
#67805=CARTESIAN_POINT('Origin',(4.90253386731613E-11,-3.71623968689858E-10,
0.));
#67806=CARTESIAN_POINT('Origin',(4.90253386731613E-11,-3.71623968689858E-10,
12.));
#67807=CARTESIAN_POINT('Origin',(4.90253386731613E-11,-3.71623968689858E-10,
0.));
#67808=CARTESIAN_POINT('Ctrl Pts',(2.94891377268305,-74.4416140848738,0.));
#67809=CARTESIAN_POINT('Ctrl Pts',(2.94891377268305,-74.4416140848738,4.));
#67810=CARTESIAN_POINT('Ctrl Pts',(2.94891377268299,-74.4416140848738,8.));
#67811=CARTESIAN_POINT('Ctrl Pts',(2.94891377268299,-74.4416140848738,12.));
#67812=CARTESIAN_POINT('Ctrl Pts',(2.83911742169683,-74.4459635334396,0.));
#67813=CARTESIAN_POINT('Ctrl Pts',(2.83911742169683,-74.4459635334396,4.));
#67814=CARTESIAN_POINT('Ctrl Pts',(2.83911742169676,-74.4459635334396,8.));
#67815=CARTESIAN_POINT('Ctrl Pts',(2.83911742169676,-74.4459635334396,12.));
#67816=CARTESIAN_POINT('Ctrl Pts',(2.64498412359382,-74.3877786926473,0.));
#67817=CARTESIAN_POINT('Ctrl Pts',(2.64498412359382,-74.3877786926473,4.));
#67818=CARTESIAN_POINT('Ctrl Pts',(2.64498412359375,-74.3877786926473,7.99999999999999));
#67819=CARTESIAN_POINT('Ctrl Pts',(2.64498412359375,-74.3877786926473,12.));
#67820=CARTESIAN_POINT('Ctrl Pts',(2.51668625693838,-74.2364344282704,0.));
#67821=CARTESIAN_POINT('Ctrl Pts',(2.51668625693838,-74.2364344282704,4.));
#67822=CARTESIAN_POINT('Ctrl Pts',(2.51668625693828,-74.2364344282705,8.00000000000001));
#67823=CARTESIAN_POINT('Ctrl Pts',(2.51668625693828,-74.2364344282705,12.));
#67824=CARTESIAN_POINT('Ctrl Pts',(2.48034921843256,-74.1624659714558,0.));
#67825=CARTESIAN_POINT('Ctrl Pts',(2.48034921843256,-74.1624659714558,4.));
#67826=CARTESIAN_POINT('Ctrl Pts',(2.48034921843243,-74.1624659714559,8.));
#67827=CARTESIAN_POINT('Ctrl Pts',(2.48034921843243,-74.1624659714559,12.));
#67828=CARTESIAN_POINT('',(2.94891377268305,-74.4416140848738,0.));
#67829=CARTESIAN_POINT('',(2.48034921843246,-74.1624659714559,0.));
#67830=CARTESIAN_POINT('Ctrl Pts',(2.94891377268305,-74.4416140848738,0.));
#67831=CARTESIAN_POINT('Ctrl Pts',(2.83911742169683,-74.4459635334396,0.));
#67832=CARTESIAN_POINT('Ctrl Pts',(2.72818410849511,-74.4127150529868,0.));
#67833=CARTESIAN_POINT('Ctrl Pts',(2.63874807903137,-74.3490471689147,0.));
#67834=CARTESIAN_POINT('Ctrl Pts',(2.57167105693357,-74.3012962558605,0.));
#67835=CARTESIAN_POINT('Ctrl Pts',(2.51668625693838,-74.2364344282704,0.));
#67836=CARTESIAN_POINT('Ctrl Pts',(2.48034921843256,-74.1624659714558,0.));
#67837=CARTESIAN_POINT('',(2.48034921843246,-74.1624659714559,12.));
#67838=CARTESIAN_POINT('Ctrl Pts',(2.48034921843256,-74.1624659714558,0.));
#67839=CARTESIAN_POINT('Ctrl Pts',(2.48034921843256,-74.1624659714558,4.));
#67840=CARTESIAN_POINT('Ctrl Pts',(2.48034921843243,-74.1624659714559,8.));
#67841=CARTESIAN_POINT('Ctrl Pts',(2.48034921843243,-74.1624659714559,12.));
#67842=CARTESIAN_POINT('',(2.94891377268299,-74.4416140848738,12.));
#67843=CARTESIAN_POINT('Ctrl Pts',(2.48034921843243,-74.1624659714559,12.));
#67844=CARTESIAN_POINT('Ctrl Pts',(2.51668625693828,-74.2364344282705,12.));
#67845=CARTESIAN_POINT('Ctrl Pts',(2.57167105693348,-74.3012962558605,12.));
#67846=CARTESIAN_POINT('Ctrl Pts',(2.63874807903129,-74.3490471689147,12.));
#67847=CARTESIAN_POINT('Ctrl Pts',(2.72818410849504,-74.4127150529869,12.));
#67848=CARTESIAN_POINT('Ctrl Pts',(2.83911742169676,-74.4459635334396,12.));
#67849=CARTESIAN_POINT('Ctrl Pts',(2.94891377268299,-74.4416140848738,12.));
#67850=CARTESIAN_POINT('Ctrl Pts',(2.94891377268299,-74.4416140848738,12.));
#67851=CARTESIAN_POINT('Ctrl Pts',(2.94891377268299,-74.4416140848738,8.));
#67852=CARTESIAN_POINT('Ctrl Pts',(2.94891377268305,-74.4416140848738,4.));
#67853=CARTESIAN_POINT('Ctrl Pts',(2.94891377268305,-74.4416140848738,0.));
#67854=CARTESIAN_POINT('Ctrl Pts',(0.853825826608976,-69.9947925310006,
0.));
#67855=CARTESIAN_POINT('Ctrl Pts',(0.853825826608976,-69.9947925310006,
12.));
#67856=CARTESIAN_POINT('Ctrl Pts',(0.854867673848587,-69.9985337959407,
0.));
#67857=CARTESIAN_POINT('Ctrl Pts',(0.854867673848587,-69.9985337959407,
12.));
#67858=CARTESIAN_POINT('Ctrl Pts',(0.856954870259198,-70.0060209754087,
0.));
#67859=CARTESIAN_POINT('Ctrl Pts',(0.856954870259198,-70.0060209754087,
12.));
#67860=CARTESIAN_POINT('Ctrl Pts',(0.860096170668728,-70.0172656933806,
0.));
#67861=CARTESIAN_POINT('Ctrl Pts',(0.860096170668728,-70.0172656933806,
12.));
#67862=CARTESIAN_POINT('Ctrl Pts',(0.864305583661538,-70.0322865492925,
0.));
#67863=CARTESIAN_POINT('Ctrl Pts',(0.864305583661538,-70.0322865492925,
12.));
#67864=CARTESIAN_POINT('Ctrl Pts',(0.869602377871117,-70.051109108301,0.));
#67865=CARTESIAN_POINT('Ctrl Pts',(0.869602377871117,-70.051109108301,12.));
#67866=CARTESIAN_POINT('Ctrl Pts',(0.874934213255831,-70.0699781183935,
0.));
#67867=CARTESIAN_POINT('Ctrl Pts',(0.874934213255831,-70.0699781183935,
12.));
#67868=CARTESIAN_POINT('Ctrl Pts',(0.880301109660721,-70.0888934967855,
0.));
#67869=CARTESIAN_POINT('Ctrl Pts',(0.880301109660721,-70.0888934967855,
12.));
#67870=CARTESIAN_POINT('Ctrl Pts',(0.885703094802528,-70.1078550938958,
0.));
#67871=CARTESIAN_POINT('Ctrl Pts',(0.885703094802528,-70.1078550938958,
12.));
#67872=CARTESIAN_POINT('Ctrl Pts',(0.891140203464235,-70.1268626950175,
0.));
#67873=CARTESIAN_POINT('Ctrl Pts',(0.891140203464235,-70.1268626950175,
12.));
#67874=CARTESIAN_POINT('Ctrl Pts',(0.896612474371837,-70.1459160490446,
0.));
#67875=CARTESIAN_POINT('Ctrl Pts',(0.896612474371837,-70.1459160490446,
12.));
#67876=CARTESIAN_POINT('Ctrl Pts',(0.902119947629764,-70.1650148905109,
0.));
#67877=CARTESIAN_POINT('Ctrl Pts',(0.902119947629764,-70.1650148905109,
12.));
#67878=CARTESIAN_POINT('Ctrl Pts',(0.907662662015778,-70.1841589635574,
0.));
#67879=CARTESIAN_POINT('Ctrl Pts',(0.907662662015778,-70.1841589635574,
12.));
#67880=CARTESIAN_POINT('Ctrl Pts',(0.913240652090973,-70.2033480471676,
0.));
#67881=CARTESIAN_POINT('Ctrl Pts',(0.913240652090973,-70.2033480471676,
12.));
#67882=CARTESIAN_POINT('Ctrl Pts',(0.918853949157111,-70.2225819470248,
0.));
#67883=CARTESIAN_POINT('Ctrl Pts',(0.918853949157111,-70.2225819470248,
12.));
#67884=CARTESIAN_POINT('Ctrl Pts',(0.924502582639448,-70.2418604835837,
0.));
#67885=CARTESIAN_POINT('Ctrl Pts',(0.924502582639448,-70.2418604835837,
12.));
#67886=CARTESIAN_POINT('Ctrl Pts',(0.93018658123554,-70.2611834821724,0.));
#67887=CARTESIAN_POINT('Ctrl Pts',(0.93018658123554,-70.2611834821724,12.));
#67888=CARTESIAN_POINT('Ctrl Pts',(0.935905974336473,-70.2805507606872,
0.));
#67889=CARTESIAN_POINT('Ctrl Pts',(0.935905974336473,-70.2805507606872,
12.));
#67890=CARTESIAN_POINT('Ctrl Pts',(0.941660792742972,-70.299962123399,0.));
#67891=CARTESIAN_POINT('Ctrl Pts',(0.941660792742972,-70.299962123399,12.));
#67892=CARTESIAN_POINT('Ctrl Pts',(0.947451067929597,-70.3194173673674,
0.));
#67893=CARTESIAN_POINT('Ctrl Pts',(0.947451067929597,-70.3194173673674,
12.));
#67894=CARTESIAN_POINT('Ctrl Pts',(0.953276831581235,-70.338916286458,0.));
#67895=CARTESIAN_POINT('Ctrl Pts',(0.953276831581235,-70.338916286458,12.));
#67896=CARTESIAN_POINT('Ctrl Pts',(0.959138115058824,-70.3584586759536,
0.));
#67897=CARTESIAN_POINT('Ctrl Pts',(0.959138115058824,-70.3584586759536,
12.));
#67898=CARTESIAN_POINT('Ctrl Pts',(0.965034948786442,-70.3780443377956,
0.));
#67899=CARTESIAN_POINT('Ctrl Pts',(0.965034948786442,-70.3780443377956,
12.));
#67900=CARTESIAN_POINT('Ctrl Pts',(0.970967362281167,-70.3976730803614,
0.));
#67901=CARTESIAN_POINT('Ctrl Pts',(0.970967362281167,-70.3976730803614,
12.));
#67902=CARTESIAN_POINT('Ctrl Pts',(0.976935384450034,-70.417344715957,0.));
#67903=CARTESIAN_POINT('Ctrl Pts',(0.976935384450034,-70.417344715957,12.));
#67904=CARTESIAN_POINT('Ctrl Pts',(0.982939043792148,-70.4370590590842,
0.));
#67905=CARTESIAN_POINT('Ctrl Pts',(0.982939043792148,-70.4370590590842,
12.));
#67906=CARTESIAN_POINT('Ctrl Pts',(0.988978368643642,-70.4568159243163,
0.));
#67907=CARTESIAN_POINT('Ctrl Pts',(0.988978368643642,-70.4568159243163,
12.));
#67908=CARTESIAN_POINT('Ctrl Pts',(0.995053387379748,-70.4766151245212,
0.));
#67909=CARTESIAN_POINT('Ctrl Pts',(0.995053387379748,-70.4766151245212,
12.));
#67910=CARTESIAN_POINT('Ctrl Pts',(1.00116412831442,-70.4964564717953,0.));
#67911=CARTESIAN_POINT('Ctrl Pts',(1.00116412831442,-70.4964564717953,12.));
#67912=CARTESIAN_POINT('Ctrl Pts',(1.00731061960967,-70.5163397782713,0.));
#67913=CARTESIAN_POINT('Ctrl Pts',(1.00731061960967,-70.5163397782713,12.));
#67914=CARTESIAN_POINT('Ctrl Pts',(1.01349288918536,-70.5362648569061,0.));
#67915=CARTESIAN_POINT('Ctrl Pts',(1.01349288918536,-70.5362648569061,12.));
#67916=CARTESIAN_POINT('Ctrl Pts',(1.01971096460596,-70.556231522419,0.));
#67917=CARTESIAN_POINT('Ctrl Pts',(1.01971096460596,-70.556231522419,12.));
#67918=CARTESIAN_POINT('Ctrl Pts',(1.02596487304048,-70.5762395916377,0.));
#67919=CARTESIAN_POINT('Ctrl Pts',(1.02596487304048,-70.5762395916377,12.));
#67920=CARTESIAN_POINT('Ctrl Pts',(1.0322546413287,-70.5962888829934,0.));
#67921=CARTESIAN_POINT('Ctrl Pts',(1.0322546413287,-70.5962888829934,12.));
#67922=CARTESIAN_POINT('Ctrl Pts',(1.03858029601903,-70.6163792162073,0.));
#67923=CARTESIAN_POINT('Ctrl Pts',(1.03858029601903,-70.6163792162073,12.));
#67924=CARTESIAN_POINT('Ctrl Pts',(1.04494186341155,-70.6365104119252,0.));
#67925=CARTESIAN_POINT('Ctrl Pts',(1.04494186341155,-70.6365104119252,12.));
#67926=CARTESIAN_POINT('Ctrl Pts',(1.05133936960071,-70.6566822912991,0.));
#67927=CARTESIAN_POINT('Ctrl Pts',(1.05133936960071,-70.6566822912991,12.));
#67928=CARTESIAN_POINT('Ctrl Pts',(1.05777284047729,-70.676894676009,0.));
#67929=CARTESIAN_POINT('Ctrl Pts',(1.05777284047729,-70.676894676009,12.));
#67930=CARTESIAN_POINT('Ctrl Pts',(1.0642423017128,-70.6971473884459,0.));
#67931=CARTESIAN_POINT('Ctrl Pts',(1.0642423017128,-70.6971473884459,12.));
#67932=CARTESIAN_POINT('Ctrl Pts',(1.07074777874595,-70.7174402518378,0.));
#67933=CARTESIAN_POINT('Ctrl Pts',(1.07074777874595,-70.7174402518378,12.));
#67934=CARTESIAN_POINT('Ctrl Pts',(1.07728929676408,-70.7377730903953,0.));
#67935=CARTESIAN_POINT('Ctrl Pts',(1.07728929676408,-70.7377730903953,12.));
#67936=CARTESIAN_POINT('Ctrl Pts',(1.08386688068342,-70.7581457294447,0.));
#67937=CARTESIAN_POINT('Ctrl Pts',(1.08386688068342,-70.7581457294447,12.));
#67938=CARTESIAN_POINT('Ctrl Pts',(1.09048055516426,-70.7785579953583,0.));
#67939=CARTESIAN_POINT('Ctrl Pts',(1.09048055516426,-70.7785579953583,12.));
#67940=CARTESIAN_POINT('Ctrl Pts',(1.09713034462265,-70.799009715484,0.));
#67941=CARTESIAN_POINT('Ctrl Pts',(1.09713034462265,-70.799009715484,12.));
#67942=CARTESIAN_POINT('Ctrl Pts',(1.10381627323946,-70.8195007180745,0.));
#67943=CARTESIAN_POINT('Ctrl Pts',(1.10381627323946,-70.8195007180745,12.));
#67944=CARTESIAN_POINT('Ctrl Pts',(1.11053836496639,-70.8400308322037,0.));
#67945=CARTESIAN_POINT('Ctrl Pts',(1.11053836496639,-70.8400308322037,12.));
#67946=CARTESIAN_POINT('Ctrl Pts',(1.11729664352992,-70.8605998877149,0.));
#67947=CARTESIAN_POINT('Ctrl Pts',(1.11729664352992,-70.8605998877149,12.));
#67948=CARTESIAN_POINT('Ctrl Pts',(1.12409113243513,-70.8812077152586,0.));
#67949=CARTESIAN_POINT('Ctrl Pts',(1.12409113243513,-70.8812077152586,12.));
#67950=CARTESIAN_POINT('Ctrl Pts',(1.13092185496564,-70.9018541463089,0.));
#67951=CARTESIAN_POINT('Ctrl Pts',(1.13092185496564,-70.9018541463089,12.));
#67952=CARTESIAN_POINT('Ctrl Pts',(1.13778883418213,-70.9225390131826,0.));
#67953=CARTESIAN_POINT('Ctrl Pts',(1.13778883418213,-70.9225390131826,12.));
#67954=CARTESIAN_POINT('Ctrl Pts',(1.14469209291488,-70.9432621490566,0.));
#67955=CARTESIAN_POINT('Ctrl Pts',(1.14469209291488,-70.9432621490566,12.));
#67956=CARTESIAN_POINT('Ctrl Pts',(1.15163165376523,-70.9640233879659,0.));
#67957=CARTESIAN_POINT('Ctrl Pts',(1.15163165376523,-70.9640233879659,12.));
#67958=CARTESIAN_POINT('Ctrl Pts',(1.15860753911484,-70.9848225647871,0.));
#67959=CARTESIAN_POINT('Ctrl Pts',(1.15860753911484,-70.9848225647871,12.));
#67960=CARTESIAN_POINT('Ctrl Pts',(1.1656197711288,-71.0056595152204,0.));
#67961=CARTESIAN_POINT('Ctrl Pts',(1.1656197711288,-71.0056595152204,12.));
#67962=CARTESIAN_POINT('Ctrl Pts',(1.17266837175776,-71.0265340757699,0.));
#67963=CARTESIAN_POINT('Ctrl Pts',(1.17266837175776,-71.0265340757699,12.));
#67964=CARTESIAN_POINT('Ctrl Pts',(1.17975336273503,-71.0474460837159,0.));
#67965=CARTESIAN_POINT('Ctrl Pts',(1.17975336273503,-71.0474460837159,12.));
#67966=CARTESIAN_POINT('Ctrl Pts',(1.18687476558132,-71.0683953771149,0.));
#67967=CARTESIAN_POINT('Ctrl Pts',(1.18687476558132,-71.0683953771149,12.));
#67968=CARTESIAN_POINT('Ctrl Pts',(1.19403260161001,-71.089381794801,0.));
#67969=CARTESIAN_POINT('Ctrl Pts',(1.19403260161001,-71.089381794801,12.));
#67970=CARTESIAN_POINT('Ctrl Pts',(1.20122689192835,-71.1104051763839,0.));
#67971=CARTESIAN_POINT('Ctrl Pts',(1.20122689192835,-71.1104051763839,12.));
#67972=CARTESIAN_POINT('Ctrl Pts',(1.20845765743647,-71.1314653622442,0.));
#67973=CARTESIAN_POINT('Ctrl Pts',(1.20845765743647,-71.1314653622442,12.));
#67974=CARTESIAN_POINT('Ctrl Pts',(1.21572491882262,-71.1525621935267,0.));
#67975=CARTESIAN_POINT('Ctrl Pts',(1.21572491882262,-71.1525621935267,12.));
#67976=CARTESIAN_POINT('Ctrl Pts',(1.22302869657017,-71.1736955121362,0.));
#67977=CARTESIAN_POINT('Ctrl Pts',(1.22302869657017,-71.1736955121362,12.));
#67978=CARTESIAN_POINT('Ctrl Pts',(1.23036901096238,-71.194865160732,0.));
#67979=CARTESIAN_POINT('Ctrl Pts',(1.23036901096238,-71.194865160732,12.));
#67980=CARTESIAN_POINT('Ctrl Pts',(1.23774588208426,-71.2160709827191,0.));
#67981=CARTESIAN_POINT('Ctrl Pts',(1.23774588208426,-71.2160709827191,12.));
#67982=CARTESIAN_POINT('Ctrl Pts',(1.24515932982112,-71.2373128222352,0.));
#67983=CARTESIAN_POINT('Ctrl Pts',(1.24515932982112,-71.2373128222352,12.));
#67984=CARTESIAN_POINT('Ctrl Pts',(1.25260937385568,-71.2585905241406,0.));
#67985=CARTESIAN_POINT('Ctrl Pts',(1.25260937385568,-71.2585905241406,12.));
#67986=CARTESIAN_POINT('Ctrl Pts',(1.2600960336757,-71.2799039340175,0.));
#67987=CARTESIAN_POINT('Ctrl Pts',(1.2600960336757,-71.2799039340175,12.));
#67988=CARTESIAN_POINT('Ctrl Pts',(1.26761932857724,-71.3012528981661,0.));
#67989=CARTESIAN_POINT('Ctrl Pts',(1.26761932857724,-71.3012528981661,12.));
#67990=CARTESIAN_POINT('Ctrl Pts',(1.27517927766607,-71.3226372635996,0.));
#67991=CARTESIAN_POINT('Ctrl Pts',(1.27517927766607,-71.3226372635996,12.));
#67992=CARTESIAN_POINT('Ctrl Pts',(1.28277589985471,-71.3440568780347,0.));
#67993=CARTESIAN_POINT('Ctrl Pts',(1.28277589985471,-71.3440568780347,12.));
#67994=CARTESIAN_POINT('Ctrl Pts',(1.29040921386058,-71.3655115898827,0.));
#67995=CARTESIAN_POINT('Ctrl Pts',(1.29040921386058,-71.3655115898827,12.));
#67996=CARTESIAN_POINT('Ctrl Pts',(1.29807923821413,-71.3870012482499,0.));
#67997=CARTESIAN_POINT('Ctrl Pts',(1.29807923821413,-71.3870012482499,12.));
#67998=CARTESIAN_POINT('Ctrl Pts',(1.30578599126139,-71.4085257029322,0.));
#67999=CARTESIAN_POINT('Ctrl Pts',(1.30578599126139,-71.4085257029322,12.));
#68000=CARTESIAN_POINT('Ctrl Pts',(1.31352949116536,-71.4300848044087,0.));
#68001=CARTESIAN_POINT('Ctrl Pts',(1.31352949116536,-71.4300848044087,12.));
#68002=CARTESIAN_POINT('Ctrl Pts',(1.32130975590225,-71.4516784038317,0.));
#68003=CARTESIAN_POINT('Ctrl Pts',(1.32130975590225,-71.4516784038317,12.));
#68004=CARTESIAN_POINT('Ctrl Pts',(1.32912680326123,-71.4733063530187,0.));
#68005=CARTESIAN_POINT('Ctrl Pts',(1.32912680326123,-71.4733063530187,12.));
#68006=CARTESIAN_POINT('Ctrl Pts',(1.33698065085219,-71.4949685044522,0.));
#68007=CARTESIAN_POINT('Ctrl Pts',(1.33698065085219,-71.4949685044522,12.));
#68008=CARTESIAN_POINT('Ctrl Pts',(1.3448713161078,-71.516664711275,0.));
#68009=CARTESIAN_POINT('Ctrl Pts',(1.3448713161078,-71.516664711275,12.));
#68010=CARTESIAN_POINT('Ctrl Pts',(1.35279881628454,-71.5383948272845,0.));
#68011=CARTESIAN_POINT('Ctrl Pts',(1.35279881628454,-71.5383948272845,12.));
#68012=CARTESIAN_POINT('Ctrl Pts',(1.36076316845815,-71.5601587069217,0.));
#68013=CARTESIAN_POINT('Ctrl Pts',(1.36076316845815,-71.5601587069217,12.));
#68014=CARTESIAN_POINT('Ctrl Pts',(1.36876438952465,-71.5819562052663,0.));
#68015=CARTESIAN_POINT('Ctrl Pts',(1.36876438952465,-71.5819562052663,12.));
#68016=CARTESIAN_POINT('Ctrl Pts',(1.37680249620779,-71.6037871780385,0.));
#68017=CARTESIAN_POINT('Ctrl Pts',(1.37680249620779,-71.6037871780385,12.));
#68018=CARTESIAN_POINT('Ctrl Pts',(1.38487750506081,-71.625651481593,0.));
#68019=CARTESIAN_POINT('Ctrl Pts',(1.38487750506081,-71.625651481593,12.));
#68020=CARTESIAN_POINT('Ctrl Pts',(1.39298943246721,-71.6475489729134,0.));
#68021=CARTESIAN_POINT('Ctrl Pts',(1.39298943246721,-71.6475489729134,12.));
#68022=CARTESIAN_POINT('Ctrl Pts',(1.40113829463576,-71.6694795096001,0.));
#68023=CARTESIAN_POINT('Ctrl Pts',(1.40113829463576,-71.6694795096001,12.));
#68024=CARTESIAN_POINT('Ctrl Pts',(1.40932410760247,-71.6914429498663,0.));
#68025=CARTESIAN_POINT('Ctrl Pts',(1.40932410760247,-71.6914429498663,12.));
#68026=CARTESIAN_POINT('Ctrl Pts',(1.41754688723772,-71.7134391525389,0.));
#68027=CARTESIAN_POINT('Ctrl Pts',(1.41754688723772,-71.7134391525389,12.));
#68028=CARTESIAN_POINT('Ctrl Pts',(1.42580664924769,-71.7354679770528,0.));
#68029=CARTESIAN_POINT('Ctrl Pts',(1.42580664924769,-71.7354679770528,12.));
#68030=CARTESIAN_POINT('Ctrl Pts',(1.43410340917495,-71.7575292834469,0.));
#68031=CARTESIAN_POINT('Ctrl Pts',(1.43410340917495,-71.7575292834469,12.));
#68032=CARTESIAN_POINT('Ctrl Pts',(1.44243718239314,-71.7796229323526,0.));
#68033=CARTESIAN_POINT('Ctrl Pts',(1.44243718239314,-71.7796229323526,12.));
#68034=CARTESIAN_POINT('Ctrl Pts',(1.45080798410964,-71.8017487849895,0.));
#68035=CARTESIAN_POINT('Ctrl Pts',(1.45080798410964,-71.8017487849895,12.));
#68036=CARTESIAN_POINT('Ctrl Pts',(1.45921582937231,-71.8239067031683,0.));
#68037=CARTESIAN_POINT('Ctrl Pts',(1.45921582937231,-71.8239067031683,12.));
#68038=CARTESIAN_POINT('Ctrl Pts',(1.46766073307087,-71.8460965492839,0.));
#68039=CARTESIAN_POINT('Ctrl Pts',(1.46766073307087,-71.8460965492839,12.));
#68040=CARTESIAN_POINT('Ctrl Pts',(1.47614270993728,-71.8683181863116,0.));
#68041=CARTESIAN_POINT('Ctrl Pts',(1.47614270993728,-71.8683181863116,12.));
#68042=CARTESIAN_POINT('Ctrl Pts',(1.48466177454019,-71.8905714777961,0.));
#68043=CARTESIAN_POINT('Ctrl Pts',(1.48466177454019,-71.8905714777961,12.));
#68044=CARTESIAN_POINT('Ctrl Pts',(1.49321794128798,-71.912856287848,0.));
#68045=CARTESIAN_POINT('Ctrl Pts',(1.49321794128798,-71.912856287848,12.));
#68046=CARTESIAN_POINT('Ctrl Pts',(1.50181122443533,-71.9351724811443,0.));
#68047=CARTESIAN_POINT('Ctrl Pts',(1.50181122443533,-71.9351724811443,12.));
#68048=CARTESIAN_POINT('Ctrl Pts',(1.51044163808453,-71.9575199229241,0.));
#68049=CARTESIAN_POINT('Ctrl Pts',(1.51044163808453,-71.9575199229241,12.));
#68050=CARTESIAN_POINT('Ctrl Pts',(1.51910919618565,-71.979898478983,0.));
#68051=CARTESIAN_POINT('Ctrl Pts',(1.51910919618565,-71.979898478983,12.));
#68052=CARTESIAN_POINT('Ctrl Pts',(1.52781391253101,-72.0023080156647,0.));
#68053=CARTESIAN_POINT('Ctrl Pts',(1.52781391253101,-72.0023080156647,12.));
#68054=CARTESIAN_POINT('Ctrl Pts',(1.53655580075812,-72.0247483998579,0.));
#68055=CARTESIAN_POINT('Ctrl Pts',(1.53655580075812,-72.0247483998579,12.));
#68056=CARTESIAN_POINT('Ctrl Pts',(1.54533487435625,-72.0472194989963,0.));
#68057=CARTESIAN_POINT('Ctrl Pts',(1.54533487435625,-72.0472194989963,12.));
#68058=CARTESIAN_POINT('Ctrl Pts',(1.55415114666773,-72.0697211810545,0.));
#68059=CARTESIAN_POINT('Ctrl Pts',(1.55415114666773,-72.0697211810545,12.));
#68060=CARTESIAN_POINT('Ctrl Pts',(1.56300463088808,-72.0922533145433,0.));
#68061=CARTESIAN_POINT('Ctrl Pts',(1.56300463088808,-72.0922533145433,12.));
#68062=CARTESIAN_POINT('Ctrl Pts',(1.5718953400604,-72.1148157684995,0.));
#68063=CARTESIAN_POINT('Ctrl Pts',(1.5718953400604,-72.1148157684995,12.));
#68064=CARTESIAN_POINT('Ctrl Pts',(1.58082328707802,-72.1374084124839,0.));
#68065=CARTESIAN_POINT('Ctrl Pts',(1.58082328707802,-72.1374084124839,12.));
#68066=CARTESIAN_POINT('Ctrl Pts',(1.58978848469122,-72.1600311165821,0.));
#68067=CARTESIAN_POINT('Ctrl Pts',(1.58978848469122,-72.1600311165821,12.));
#68068=CARTESIAN_POINT('Ctrl Pts',(1.59879094550846,-72.1826837514001,0.));
#68069=CARTESIAN_POINT('Ctrl Pts',(1.59879094550846,-72.1826837514001,12.));
#68070=CARTESIAN_POINT('Ctrl Pts',(1.60783068199662,-72.2053661880608,0.));
#68071=CARTESIAN_POINT('Ctrl Pts',(1.60783068199662,-72.2053661880608,12.));
#68072=CARTESIAN_POINT('Ctrl Pts',(1.61690770647539,-72.2280782981937,0.));
#68073=CARTESIAN_POINT('Ctrl Pts',(1.61690770647539,-72.2280782981937,12.));
#68074=CARTESIAN_POINT('Ctrl Pts',(1.62602203111929,-72.2508199539323,0.));
#68075=CARTESIAN_POINT('Ctrl Pts',(1.62602203111929,-72.2508199539323,12.));
#68076=CARTESIAN_POINT('Ctrl Pts',(1.63517366796462,-72.2735910279149,0.));
#68077=CARTESIAN_POINT('Ctrl Pts',(1.63517366796462,-72.2735910279149,12.));
#68078=CARTESIAN_POINT('Ctrl Pts',(1.64436262891078,-72.2963913932813,0.));
#68079=CARTESIAN_POINT('Ctrl Pts',(1.64436262891078,-72.2963913932813,12.));
#68080=CARTESIAN_POINT('Ctrl Pts',(1.65358892572062,-72.319220923669,0.));
#68081=CARTESIAN_POINT('Ctrl Pts',(1.65358892572062,-72.319220923669,12.));
#68082=CARTESIAN_POINT('Ctrl Pts',(1.66285257001496,-72.3420794932047,0.));
#68083=CARTESIAN_POINT('Ctrl Pts',(1.66285257001496,-72.3420794932047,12.));
#68084=CARTESIAN_POINT('Ctrl Pts',(1.67215357327364,-72.3649669765004,0.));
#68085=CARTESIAN_POINT('Ctrl Pts',(1.67215357327364,-72.3649669765004,12.));
#68086=CARTESIAN_POINT('Ctrl Pts',(1.68149194684281,-72.387883248654,0.));
#68087=CARTESIAN_POINT('Ctrl Pts',(1.68149194684281,-72.387883248654,12.));
#68088=CARTESIAN_POINT('Ctrl Pts',(1.69086770193636,-72.4108281852467,0.));
#68089=CARTESIAN_POINT('Ctrl Pts',(1.69086770193636,-72.4108281852467,12.));
#68090=CARTESIAN_POINT('Ctrl Pts',(1.70028084963647,-72.4338016623391,0.));
#68091=CARTESIAN_POINT('Ctrl Pts',(1.70028084963647,-72.4338016623391,12.));
#68092=CARTESIAN_POINT('Ctrl Pts',(1.70973140088841,-72.456803556463,0.));
#68093=CARTESIAN_POINT('Ctrl Pts',(1.70973140088841,-72.456803556463,12.));
#68094=CARTESIAN_POINT('Ctrl Pts',(1.71921936650037,-72.479833744618,0.));
#68095=CARTESIAN_POINT('Ctrl Pts',(1.71921936650037,-72.479833744618,12.));
#68096=CARTESIAN_POINT('Ctrl Pts',(1.72874475715102,-72.5028921042721,0.));
#68097=CARTESIAN_POINT('Ctrl Pts',(1.72874475715102,-72.5028921042721,12.));
#68098=CARTESIAN_POINT('Ctrl Pts',(1.73830758339124,-72.5259785133595,0.));
#68099=CARTESIAN_POINT('Ctrl Pts',(1.73830758339124,-72.5259785133595,12.));
#68100=CARTESIAN_POINT('Ctrl Pts',(1.74790785564473,-72.5490928502769,0.));
#68101=CARTESIAN_POINT('Ctrl Pts',(1.74790785564473,-72.5490928502769,12.));
#68102=CARTESIAN_POINT('Ctrl Pts',(1.75754558420343,-72.5722349938774,0.));
#68103=CARTESIAN_POINT('Ctrl Pts',(1.75754558420343,-72.5722349938774,12.));
#68104=CARTESIAN_POINT('Ctrl Pts',(1.76722077922574,-72.5954048234638,0.));
#68105=CARTESIAN_POINT('Ctrl Pts',(1.76722077922574,-72.5954048234638,12.));
#68106=CARTESIAN_POINT('Ctrl Pts',(1.77693345074426,-72.6186022187907,0.));
#68107=CARTESIAN_POINT('Ctrl Pts',(1.77693345074426,-72.6186022187907,12.));
#68108=CARTESIAN_POINT('Ctrl Pts',(1.7866836086681,-72.6418270600619,0.));
#68109=CARTESIAN_POINT('Ctrl Pts',(1.7866836086681,-72.6418270600619,12.));
#68110=CARTESIAN_POINT('Ctrl Pts',(1.79647126278358,-72.6650792279274,0.));
#68111=CARTESIAN_POINT('Ctrl Pts',(1.79647126278358,-72.6650792279274,12.));
#68112=CARTESIAN_POINT('Ctrl Pts',(1.8062964227505,-72.6883586034769,0.));
#68113=CARTESIAN_POINT('Ctrl Pts',(1.8062964227505,-72.6883586034769,12.));
#68114=CARTESIAN_POINT('Ctrl Pts',(1.8161590980987,-72.7116650682344,0.));
#68115=CARTESIAN_POINT('Ctrl Pts',(1.8161590980987,-72.7116650682344,12.));
#68116=CARTESIAN_POINT('Ctrl Pts',(1.82605929823564,-72.7349985041592,0.));
#68117=CARTESIAN_POINT('Ctrl Pts',(1.82605929823564,-72.7349985041592,12.));
#68118=CARTESIAN_POINT('Ctrl Pts',(1.83599703244924,-72.7583587936447,0.));
#68119=CARTESIAN_POINT('Ctrl Pts',(1.83599703244924,-72.7583587936447,12.));
#68120=CARTESIAN_POINT('Ctrl Pts',(1.84597230990856,-72.7817458195155,0.));
#68121=CARTESIAN_POINT('Ctrl Pts',(1.84597230990856,-72.7817458195155,12.));
#68122=CARTESIAN_POINT('Ctrl Pts',(1.85598513966113,-72.8051594650222,0.));
#68123=CARTESIAN_POINT('Ctrl Pts',(1.85598513966113,-72.8051594650222,12.));
#68124=CARTESIAN_POINT('Ctrl Pts',(1.8660355306277,-72.8285996138359,0.));
#68125=CARTESIAN_POINT('Ctrl Pts',(1.8660355306277,-72.8285996138359,12.));
#68126=CARTESIAN_POINT('Ctrl Pts',(1.87612349160944,-72.8520661500477,0.));
#68127=CARTESIAN_POINT('Ctrl Pts',(1.87612349160944,-72.8520661500477,12.));
#68128=CARTESIAN_POINT('Ctrl Pts',(1.88624903129187,-72.875558958168,0.));
#68129=CARTESIAN_POINT('Ctrl Pts',(1.88624903129187,-72.875558958168,12.));
#68130=CARTESIAN_POINT('Ctrl Pts',(1.89641215824581,-72.8990779231226,0.));
#68131=CARTESIAN_POINT('Ctrl Pts',(1.89641215824581,-72.8990779231226,12.));
#68132=CARTESIAN_POINT('Ctrl Pts',(1.90661288092586,-72.9226229302478,0.));
#68133=CARTESIAN_POINT('Ctrl Pts',(1.90661288092586,-72.9226229302478,12.));
#68134=CARTESIAN_POINT('Ctrl Pts',(1.91685120766436,-72.9461938652811,0.));
#68135=CARTESIAN_POINT('Ctrl Pts',(1.91685120766436,-72.9461938652811,12.));
#68136=CARTESIAN_POINT('Ctrl Pts',(1.9271271466766,-72.9697906143636,0.));
#68137=CARTESIAN_POINT('Ctrl Pts',(1.9271271466766,-72.9697906143636,12.));
#68138=CARTESIAN_POINT('Ctrl Pts',(1.93744070606565,-72.9934130640415,0.));
#68139=CARTESIAN_POINT('Ctrl Pts',(1.93744070606565,-72.9934130640415,12.));
#68140=CARTESIAN_POINT('Ctrl Pts',(1.94779189382301,-73.0170611012661,0.));
#68141=CARTESIAN_POINT('Ctrl Pts',(1.94779189382301,-73.0170611012661,12.));
#68142=CARTESIAN_POINT('Ctrl Pts',(1.95818071782766,-73.040734613391,0.));
#68143=CARTESIAN_POINT('Ctrl Pts',(1.95818071782766,-73.040734613391,12.));
#68144=CARTESIAN_POINT('Ctrl Pts',(1.96860718583931,-73.0644334881673,0.));
#68145=CARTESIAN_POINT('Ctrl Pts',(1.96860718583931,-73.0644334881673,12.));
#68146=CARTESIAN_POINT('Ctrl Pts',(1.97907130550157,-73.0881576137407,0.));
#68147=CARTESIAN_POINT('Ctrl Pts',(1.97907130550157,-73.0881576137407,12.));
#68148=CARTESIAN_POINT('Ctrl Pts',(1.98957308434917,-73.1119068786475,0.));
#68149=CARTESIAN_POINT('Ctrl Pts',(1.98957308434917,-73.1119068786475,12.));
#68150=CARTESIAN_POINT('Ctrl Pts',(2.00011252980981,-73.1356811718091,0.));
#68151=CARTESIAN_POINT('Ctrl Pts',(2.00011252980981,-73.1356811718091,12.));
#68152=CARTESIAN_POINT('Ctrl Pts',(2.01068964920466,-73.1594803825252,0.));
#68153=CARTESIAN_POINT('Ctrl Pts',(2.01068964920466,-73.1594803825252,12.));
#68154=CARTESIAN_POINT('Ctrl Pts',(2.02130444974361,-73.183304400462,0.));
#68155=CARTESIAN_POINT('Ctrl Pts',(2.02130444974361,-73.183304400462,12.));
#68156=CARTESIAN_POINT('Ctrl Pts',(2.03195693852454,-73.2071531156504,0.));
#68157=CARTESIAN_POINT('Ctrl Pts',(2.03195693852454,-73.2071531156504,12.));
#68158=CARTESIAN_POINT('Ctrl Pts',(2.04264712253928,-73.2310264184976,0.));
#68159=CARTESIAN_POINT('Ctrl Pts',(2.04264712253928,-73.2310264184976,12.));
#68160=CARTESIAN_POINT('Ctrl Pts',(2.05337500867402,-73.2549241997953,0.));
#68161=CARTESIAN_POINT('Ctrl Pts',(2.05337500867402,-73.2549241997953,12.));
#68162=CARTESIAN_POINT('Ctrl Pts',(2.06414060370834,-73.2788463507246,0.));
#68163=CARTESIAN_POINT('Ctrl Pts',(2.06414060370834,-73.2788463507246,12.));
#68164=CARTESIAN_POINT('Ctrl Pts',(2.0749439143094,-73.3027927628626,0.));
#68165=CARTESIAN_POINT('Ctrl Pts',(2.0749439143094,-73.3027927628626,12.));
#68166=CARTESIAN_POINT('Ctrl Pts',(2.08578494702743,-73.3267633281807,0.));
#68167=CARTESIAN_POINT('Ctrl Pts',(2.08578494702743,-73.3267633281807,12.));
#68168=CARTESIAN_POINT('Ctrl Pts',(2.09666370830715,-73.3507579390239,0.));
#68169=CARTESIAN_POINT('Ctrl Pts',(2.09666370830715,-73.3507579390239,12.));
#68170=CARTESIAN_POINT('Ctrl Pts',(2.10758020449389,-73.3747764880893,0.));
#68171=CARTESIAN_POINT('Ctrl Pts',(2.10758020449389,-73.3747764880893,12.));
#68172=CARTESIAN_POINT('Ctrl Pts',(2.11853444183761,-73.3988188684021,0.));
#68173=CARTESIAN_POINT('Ctrl Pts',(2.11853444183761,-73.3988188684021,12.));
#68174=CARTESIAN_POINT('Ctrl Pts',(2.12952642649367,-73.4228849732925,0.));
#68175=CARTESIAN_POINT('Ctrl Pts',(2.12952642649367,-73.4228849732925,12.));
#68176=CARTESIAN_POINT('Ctrl Pts',(2.14055616452057,-73.4469746963637,0.));
#68177=CARTESIAN_POINT('Ctrl Pts',(2.14055616452057,-73.4469746963637,12.));
#68178=CARTESIAN_POINT('Ctrl Pts',(2.15162366187906,-73.4710879315382,0.));
#68179=CARTESIAN_POINT('Ctrl Pts',(2.15162366187906,-73.4710879315382,12.));
#68180=CARTESIAN_POINT('Ctrl Pts',(2.16272892442919,-73.4952245731054,0.));
#68181=CARTESIAN_POINT('Ctrl Pts',(2.16272892442919,-73.4952245731054,12.));
#68182=CARTESIAN_POINT('Ctrl Pts',(2.17387195792305,-73.5193845157708,0.));
#68183=CARTESIAN_POINT('Ctrl Pts',(2.17387195792305,-73.5193845157708,12.));
#68184=CARTESIAN_POINT('Ctrl Pts',(2.18505276799752,-73.5435676546929,0.));
#68185=CARTESIAN_POINT('Ctrl Pts',(2.18505276799752,-73.5435676546929,12.));
#68186=CARTESIAN_POINT('Ctrl Pts',(2.19627136015677,-73.5677738855452,0.));
#68187=CARTESIAN_POINT('Ctrl Pts',(2.19627136015677,-73.5677738855452,12.));
#68188=CARTESIAN_POINT('Ctrl Pts',(2.20752773978348,-73.5920031044595,0.));
#68189=CARTESIAN_POINT('Ctrl Pts',(2.20752773978348,-73.5920031044595,12.));
#68190=CARTESIAN_POINT('Ctrl Pts',(2.21882191216517,-73.6162552079038,0.));
#68191=CARTESIAN_POINT('Ctrl Pts',(2.21882191216517,-73.6162552079038,12.));
#68192=CARTESIAN_POINT('Ctrl Pts',(2.23015388251287,-73.6405300925712,0.));
#68193=CARTESIAN_POINT('Ctrl Pts',(2.23015388251287,-73.6405300925712,12.));
#68194=CARTESIAN_POINT('Ctrl Pts',(2.24152365597697,-73.6648276552767,0.));
#68195=CARTESIAN_POINT('Ctrl Pts',(2.24152365597697,-73.6648276552767,12.));
#68196=CARTESIAN_POINT('Ctrl Pts',(2.25293123766424,-73.6891477928129,0.));
#68197=CARTESIAN_POINT('Ctrl Pts',(2.25293123766424,-73.6891477928129,12.));
#68198=CARTESIAN_POINT('Ctrl Pts',(2.26437663263666,-73.7134904019389,0.));
#68199=CARTESIAN_POINT('Ctrl Pts',(2.26437663263666,-73.7134904019389,12.));
#68200=CARTESIAN_POINT('Ctrl Pts',(2.27585984587198,-73.7378553796807,0.));
#68201=CARTESIAN_POINT('Ctrl Pts',(2.27585984587198,-73.7378553796807,12.));
#68202=CARTESIAN_POINT('Ctrl Pts',(2.28738088222863,-73.762242623566,0.));
#68203=CARTESIAN_POINT('Ctrl Pts',(2.28738088222863,-73.762242623566,12.));
#68204=CARTESIAN_POINT('Ctrl Pts',(2.29893974640434,-73.786652031885,0.));
#68205=CARTESIAN_POINT('Ctrl Pts',(2.29893974640434,-73.786652031885,12.));
#68206=CARTESIAN_POINT('Ctrl Pts',(2.31053644289416,-73.8110835039327,0.));
#68207=CARTESIAN_POINT('Ctrl Pts',(2.31053644289416,-73.8110835039327,12.));
#68208=CARTESIAN_POINT('Ctrl Pts',(2.32217097594197,-73.8355369402706,0.));
#68209=CARTESIAN_POINT('Ctrl Pts',(2.32217097594197,-73.8355369402706,12.));
#68210=CARTESIAN_POINT('Ctrl Pts',(2.33384334963957,-73.8600122421468,0.));
#68211=CARTESIAN_POINT('Ctrl Pts',(2.33384334963957,-73.8600122421468,12.));
#68212=CARTESIAN_POINT('Ctrl Pts',(2.3455535680212,-73.8845093109274,0.));
#68213=CARTESIAN_POINT('Ctrl Pts',(2.3455535680212,-73.8845093109274,12.));
#68214=CARTESIAN_POINT('Ctrl Pts',(2.35730163516315,-73.9090280474712,0.));
#68215=CARTESIAN_POINT('Ctrl Pts',(2.35730163516315,-73.9090280474712,12.));
#68216=CARTESIAN_POINT('Ctrl Pts',(2.36908755526003,-73.9335683516404,0.));
#68217=CARTESIAN_POINT('Ctrl Pts',(2.36908755526003,-73.9335683516404,12.));
#68218=CARTESIAN_POINT('Ctrl Pts',(2.3809113327496,-73.958130121465,0.));
#68219=CARTESIAN_POINT('Ctrl Pts',(2.3809113327496,-73.958130121465,12.));
#68220=CARTESIAN_POINT('Ctrl Pts',(2.39277297220756,-73.9827132538206,0.));
#68221=CARTESIAN_POINT('Ctrl Pts',(2.39277297220756,-73.9827132538206,12.));
#68222=CARTESIAN_POINT('Ctrl Pts',(2.40467247811536,-74.0073176459344,0.));
#68223=CARTESIAN_POINT('Ctrl Pts',(2.40467247811536,-74.0073176459344,12.));
#68224=CARTESIAN_POINT('Ctrl Pts',(2.41660985465251,-74.0319431966989,0.));
#68225=CARTESIAN_POINT('Ctrl Pts',(2.41660985465251,-74.0319431966989,12.));
#68226=CARTESIAN_POINT('Ctrl Pts',(2.42858510549778,-74.0565898079218,0.));
#68227=CARTESIAN_POINT('Ctrl Pts',(2.42858510549778,-74.0565898079218,12.));
#68228=CARTESIAN_POINT('Ctrl Pts',(2.44059823356675,-74.0812573859411,0.));
#68229=CARTESIAN_POINT('Ctrl Pts',(2.44059823356675,-74.0812573859411,12.));
#68230=CARTESIAN_POINT('Ctrl Pts',(2.45264924094774,-74.1059458420067,0.));
#68231=CARTESIAN_POINT('Ctrl Pts',(2.45264924094774,-74.1059458420067,12.));
#68232=CARTESIAN_POINT('Ctrl Pts',(2.46473812947959,-74.1306550887071,0.));
#68233=CARTESIAN_POINT('Ctrl Pts',(2.46473812947959,-74.1306550887071,12.));
#68234=CARTESIAN_POINT('Ctrl Pts',(2.47686490120353,-74.155385037148,0.));
#68235=CARTESIAN_POINT('Ctrl Pts',(2.47686490120353,-74.155385037148,12.));
#68236=CARTESIAN_POINT('Ctrl Pts',(2.48902955888384,-74.1801355936907,0.));
#68237=CARTESIAN_POINT('Ctrl Pts',(2.48902955888384,-74.1801355936907,12.));
#68238=CARTESIAN_POINT('Ctrl Pts',(2.50123210644134,-74.2049066572031,0.));
#68239=CARTESIAN_POINT('Ctrl Pts',(2.50123210644134,-74.2049066572031,12.));
#68240=CARTESIAN_POINT('Ctrl Pts',(2.51347254956166,-74.229698115223,0.));
#68241=CARTESIAN_POINT('Ctrl Pts',(2.51347254956166,-74.229698115223,12.));
#68242=CARTESIAN_POINT('Ctrl Pts',(2.52575089478303,-74.2545098494824,0.));
#68243=CARTESIAN_POINT('Ctrl Pts',(2.52575089478303,-74.2545098494824,12.));
#68244=CARTESIAN_POINT('Ctrl Pts',(2.53806714838285,-74.2793417427308,0.));
#68245=CARTESIAN_POINT('Ctrl Pts',(2.53806714838285,-74.2793417427308,12.));
#68246=CARTESIAN_POINT('Ctrl Pts',(2.5504213152678,-74.3041936853468,0.));
#68247=CARTESIAN_POINT('Ctrl Pts',(2.5504213152678,-74.3041936853468,12.));
#68248=CARTESIAN_POINT('Ctrl Pts',(2.56281339800017,-74.3290655814831,0.));
#68249=CARTESIAN_POINT('Ctrl Pts',(2.56281339800017,-74.3290655814831,12.));
#68250=CARTESIAN_POINT('Ctrl Pts',(2.57524339541389,-74.3539573567672,0.));
#68251=CARTESIAN_POINT('Ctrl Pts',(2.57524339541389,-74.3539573567672,12.));
#68252=CARTESIAN_POINT('Ctrl Pts',(2.58771130268175,-74.3788689603363,0.));
#68253=CARTESIAN_POINT('Ctrl Pts',(2.58771130268175,-74.3788689603363,12.));
#68254=CARTESIAN_POINT('Ctrl Pts',(2.60021711326976,-74.4038003594771,0.));
#68255=CARTESIAN_POINT('Ctrl Pts',(2.60021711326976,-74.4038003594771,12.));
#68256=CARTESIAN_POINT('Ctrl Pts',(2.61025207898402,-74.4237613007988,0.));
#68257=CARTESIAN_POINT('Ctrl Pts',(2.61025207898402,-74.4237613007988,12.));
#68258=CARTESIAN_POINT('Ctrl Pts',(2.61779535432111,-74.4387409032207,0.));
#68259=CARTESIAN_POINT('Ctrl Pts',(2.61779535432111,-74.4387409032207,12.));
#68260=CARTESIAN_POINT('Ctrl Pts',(2.62283178248202,-74.4487312586464,0.));
#68261=CARTESIAN_POINT('Ctrl Pts',(2.62283178248202,-74.4487312586464,12.));
#68262=CARTESIAN_POINT('Ctrl Pts',(2.62535189104655,-74.4537274248118,0.));
#68263=CARTESIAN_POINT('Ctrl Pts',(2.62535189104655,-74.4537274248118,12.));
#68264=CARTESIAN_POINT('',(0.853825826608976,-69.9947925310006,0.));
#68265=CARTESIAN_POINT('Ctrl Pts',(0.853825826608976,-69.9947925310006,
0.));
#68266=CARTESIAN_POINT('Ctrl Pts',(0.854867673848587,-69.9985337959407,
0.));
#68267=CARTESIAN_POINT('Ctrl Pts',(0.856954870259198,-70.0060209754087,
0.));
#68268=CARTESIAN_POINT('Ctrl Pts',(0.860096170668728,-70.0172656933806,
0.));
#68269=CARTESIAN_POINT('Ctrl Pts',(0.864305583661538,-70.0322865492925,
0.));
#68270=CARTESIAN_POINT('Ctrl Pts',(0.869602377871117,-70.051109108301,0.));
#68271=CARTESIAN_POINT('Ctrl Pts',(0.874934213255831,-70.0699781183935,
0.));
#68272=CARTESIAN_POINT('Ctrl Pts',(0.880301109660721,-70.0888934967855,
0.));
#68273=CARTESIAN_POINT('Ctrl Pts',(0.885703094802528,-70.1078550938958,
0.));
#68274=CARTESIAN_POINT('Ctrl Pts',(0.891140203464235,-70.1268626950175,
0.));
#68275=CARTESIAN_POINT('Ctrl Pts',(0.896612474371837,-70.1459160490446,
0.));
#68276=CARTESIAN_POINT('Ctrl Pts',(0.902119947629764,-70.1650148905109,
0.));
#68277=CARTESIAN_POINT('Ctrl Pts',(0.907662662015778,-70.1841589635574,
0.));
#68278=CARTESIAN_POINT('Ctrl Pts',(0.913240652090973,-70.2033480471676,
0.));
#68279=CARTESIAN_POINT('Ctrl Pts',(0.918853949157111,-70.2225819470248,
0.));
#68280=CARTESIAN_POINT('Ctrl Pts',(0.924502582639448,-70.2418604835837,
0.));
#68281=CARTESIAN_POINT('Ctrl Pts',(0.93018658123554,-70.2611834821724,0.));
#68282=CARTESIAN_POINT('Ctrl Pts',(0.935905974336473,-70.2805507606872,
0.));
#68283=CARTESIAN_POINT('Ctrl Pts',(0.941660792742972,-70.299962123399,0.));
#68284=CARTESIAN_POINT('Ctrl Pts',(0.947451067929597,-70.3194173673674,
0.));
#68285=CARTESIAN_POINT('Ctrl Pts',(0.953276831581235,-70.338916286458,0.));
#68286=CARTESIAN_POINT('Ctrl Pts',(0.959138115058824,-70.3584586759536,
0.));
#68287=CARTESIAN_POINT('Ctrl Pts',(0.965034948786442,-70.3780443377956,
0.));
#68288=CARTESIAN_POINT('Ctrl Pts',(0.970967362281167,-70.3976730803614,
0.));
#68289=CARTESIAN_POINT('Ctrl Pts',(0.976935384450034,-70.417344715957,0.));
#68290=CARTESIAN_POINT('Ctrl Pts',(0.982939043792148,-70.4370590590842,
0.));
#68291=CARTESIAN_POINT('Ctrl Pts',(0.988978368643642,-70.4568159243163,
0.));
#68292=CARTESIAN_POINT('Ctrl Pts',(0.995053387379748,-70.4766151245212,
0.));
#68293=CARTESIAN_POINT('Ctrl Pts',(1.00116412831442,-70.4964564717953,0.));
#68294=CARTESIAN_POINT('Ctrl Pts',(1.00731061960967,-70.5163397782713,0.));
#68295=CARTESIAN_POINT('Ctrl Pts',(1.01349288918536,-70.5362648569061,0.));
#68296=CARTESIAN_POINT('Ctrl Pts',(1.01971096460596,-70.556231522419,0.));
#68297=CARTESIAN_POINT('Ctrl Pts',(1.02596487304048,-70.5762395916377,0.));
#68298=CARTESIAN_POINT('Ctrl Pts',(1.0322546413287,-70.5962888829934,0.));
#68299=CARTESIAN_POINT('Ctrl Pts',(1.03858029601903,-70.6163792162073,0.));
#68300=CARTESIAN_POINT('Ctrl Pts',(1.04494186341155,-70.6365104119252,0.));
#68301=CARTESIAN_POINT('Ctrl Pts',(1.05133936960071,-70.6566822912991,0.));
#68302=CARTESIAN_POINT('Ctrl Pts',(1.05777284047729,-70.676894676009,0.));
#68303=CARTESIAN_POINT('Ctrl Pts',(1.0642423017128,-70.6971473884459,0.));
#68304=CARTESIAN_POINT('Ctrl Pts',(1.07074777874595,-70.7174402518378,0.));
#68305=CARTESIAN_POINT('Ctrl Pts',(1.07728929676408,-70.7377730903953,0.));
#68306=CARTESIAN_POINT('Ctrl Pts',(1.08386688068342,-70.7581457294447,0.));
#68307=CARTESIAN_POINT('Ctrl Pts',(1.09048055516426,-70.7785579953583,0.));
#68308=CARTESIAN_POINT('Ctrl Pts',(1.09713034462265,-70.799009715484,0.));
#68309=CARTESIAN_POINT('Ctrl Pts',(1.10381627323946,-70.8195007180745,0.));
#68310=CARTESIAN_POINT('Ctrl Pts',(1.11053836496639,-70.8400308322037,0.));
#68311=CARTESIAN_POINT('Ctrl Pts',(1.11729664352992,-70.8605998877149,0.));
#68312=CARTESIAN_POINT('Ctrl Pts',(1.12409113243513,-70.8812077152586,0.));
#68313=CARTESIAN_POINT('Ctrl Pts',(1.13092185496564,-70.9018541463089,0.));
#68314=CARTESIAN_POINT('Ctrl Pts',(1.13778883418213,-70.9225390131826,0.));
#68315=CARTESIAN_POINT('Ctrl Pts',(1.14469209291488,-70.9432621490566,0.));
#68316=CARTESIAN_POINT('Ctrl Pts',(1.15163165376523,-70.9640233879659,0.));
#68317=CARTESIAN_POINT('Ctrl Pts',(1.15860753911484,-70.9848225647871,0.));
#68318=CARTESIAN_POINT('Ctrl Pts',(1.1656197711288,-71.0056595152204,0.));
#68319=CARTESIAN_POINT('Ctrl Pts',(1.17266837175776,-71.0265340757699,0.));
#68320=CARTESIAN_POINT('Ctrl Pts',(1.17975336273503,-71.0474460837159,0.));
#68321=CARTESIAN_POINT('Ctrl Pts',(1.18687476558132,-71.0683953771149,0.));
#68322=CARTESIAN_POINT('Ctrl Pts',(1.19403260161001,-71.089381794801,0.));
#68323=CARTESIAN_POINT('Ctrl Pts',(1.20122689192835,-71.1104051763839,0.));
#68324=CARTESIAN_POINT('Ctrl Pts',(1.20845765743647,-71.1314653622442,0.));
#68325=CARTESIAN_POINT('Ctrl Pts',(1.21572491882262,-71.1525621935267,0.));
#68326=CARTESIAN_POINT('Ctrl Pts',(1.22302869657017,-71.1736955121362,0.));
#68327=CARTESIAN_POINT('Ctrl Pts',(1.23036901096238,-71.194865160732,0.));
#68328=CARTESIAN_POINT('Ctrl Pts',(1.23774588208426,-71.2160709827191,0.));
#68329=CARTESIAN_POINT('Ctrl Pts',(1.24515932982112,-71.2373128222352,0.));
#68330=CARTESIAN_POINT('Ctrl Pts',(1.25260937385568,-71.2585905241406,0.));
#68331=CARTESIAN_POINT('Ctrl Pts',(1.2600960336757,-71.2799039340175,0.));
#68332=CARTESIAN_POINT('Ctrl Pts',(1.26761932857724,-71.3012528981661,0.));
#68333=CARTESIAN_POINT('Ctrl Pts',(1.27517927766607,-71.3226372635996,0.));
#68334=CARTESIAN_POINT('Ctrl Pts',(1.28277589985471,-71.3440568780347,0.));
#68335=CARTESIAN_POINT('Ctrl Pts',(1.29040921386058,-71.3655115898827,0.));
#68336=CARTESIAN_POINT('Ctrl Pts',(1.29807923821413,-71.3870012482499,0.));
#68337=CARTESIAN_POINT('Ctrl Pts',(1.30578599126139,-71.4085257029322,0.));
#68338=CARTESIAN_POINT('Ctrl Pts',(1.31352949116536,-71.4300848044087,0.));
#68339=CARTESIAN_POINT('Ctrl Pts',(1.32130975590225,-71.4516784038317,0.));
#68340=CARTESIAN_POINT('Ctrl Pts',(1.32912680326123,-71.4733063530187,0.));
#68341=CARTESIAN_POINT('Ctrl Pts',(1.33698065085219,-71.4949685044522,0.));
#68342=CARTESIAN_POINT('Ctrl Pts',(1.3448713161078,-71.516664711275,0.));
#68343=CARTESIAN_POINT('Ctrl Pts',(1.35279881628454,-71.5383948272845,0.));
#68344=CARTESIAN_POINT('Ctrl Pts',(1.36076316845815,-71.5601587069217,0.));
#68345=CARTESIAN_POINT('Ctrl Pts',(1.36876438952465,-71.5819562052663,0.));
#68346=CARTESIAN_POINT('Ctrl Pts',(1.37680249620779,-71.6037871780385,0.));
#68347=CARTESIAN_POINT('Ctrl Pts',(1.38487750506081,-71.625651481593,0.));
#68348=CARTESIAN_POINT('Ctrl Pts',(1.39298943246721,-71.6475489729134,0.));
#68349=CARTESIAN_POINT('Ctrl Pts',(1.40113829463576,-71.6694795096001,0.));
#68350=CARTESIAN_POINT('Ctrl Pts',(1.40932410760247,-71.6914429498663,0.));
#68351=CARTESIAN_POINT('Ctrl Pts',(1.41754688723772,-71.7134391525389,0.));
#68352=CARTESIAN_POINT('Ctrl Pts',(1.42580664924769,-71.7354679770528,0.));
#68353=CARTESIAN_POINT('Ctrl Pts',(1.43410340917495,-71.7575292834469,0.));
#68354=CARTESIAN_POINT('Ctrl Pts',(1.44243718239314,-71.7796229323526,0.));
#68355=CARTESIAN_POINT('Ctrl Pts',(1.45080798410964,-71.8017487849895,0.));
#68356=CARTESIAN_POINT('Ctrl Pts',(1.45921582937231,-71.8239067031683,0.));
#68357=CARTESIAN_POINT('Ctrl Pts',(1.46766073307087,-71.8460965492839,0.));
#68358=CARTESIAN_POINT('Ctrl Pts',(1.47614270993728,-71.8683181863116,0.));
#68359=CARTESIAN_POINT('Ctrl Pts',(1.48466177454019,-71.8905714777961,0.));
#68360=CARTESIAN_POINT('Ctrl Pts',(1.49321794128798,-71.912856287848,0.));
#68361=CARTESIAN_POINT('Ctrl Pts',(1.50181122443533,-71.9351724811443,0.));
#68362=CARTESIAN_POINT('Ctrl Pts',(1.51044163808453,-71.9575199229241,0.));
#68363=CARTESIAN_POINT('Ctrl Pts',(1.51910919618565,-71.979898478983,0.));
#68364=CARTESIAN_POINT('Ctrl Pts',(1.52781391253101,-72.0023080156647,0.));
#68365=CARTESIAN_POINT('Ctrl Pts',(1.53655580075812,-72.0247483998579,0.));
#68366=CARTESIAN_POINT('Ctrl Pts',(1.54533487435625,-72.0472194989963,0.));
#68367=CARTESIAN_POINT('Ctrl Pts',(1.55415114666773,-72.0697211810545,0.));
#68368=CARTESIAN_POINT('Ctrl Pts',(1.56300463088808,-72.0922533145433,0.));
#68369=CARTESIAN_POINT('Ctrl Pts',(1.5718953400604,-72.1148157684995,0.));
#68370=CARTESIAN_POINT('Ctrl Pts',(1.58082328707802,-72.1374084124839,0.));
#68371=CARTESIAN_POINT('Ctrl Pts',(1.58978848469122,-72.1600311165821,0.));
#68372=CARTESIAN_POINT('Ctrl Pts',(1.59879094550846,-72.1826837514001,0.));
#68373=CARTESIAN_POINT('Ctrl Pts',(1.60783068199662,-72.2053661880608,0.));
#68374=CARTESIAN_POINT('Ctrl Pts',(1.61690770647539,-72.2280782981937,0.));
#68375=CARTESIAN_POINT('Ctrl Pts',(1.62602203111929,-72.2508199539323,0.));
#68376=CARTESIAN_POINT('Ctrl Pts',(1.63517366796462,-72.2735910279149,0.));
#68377=CARTESIAN_POINT('Ctrl Pts',(1.64436262891078,-72.2963913932813,0.));
#68378=CARTESIAN_POINT('Ctrl Pts',(1.65358892572062,-72.319220923669,0.));
#68379=CARTESIAN_POINT('Ctrl Pts',(1.66285257001496,-72.3420794932047,0.));
#68380=CARTESIAN_POINT('Ctrl Pts',(1.67215357327364,-72.3649669765004,0.));
#68381=CARTESIAN_POINT('Ctrl Pts',(1.68149194684281,-72.387883248654,0.));
#68382=CARTESIAN_POINT('Ctrl Pts',(1.69086770193636,-72.4108281852467,0.));
#68383=CARTESIAN_POINT('Ctrl Pts',(1.70028084963647,-72.4338016623391,0.));
#68384=CARTESIAN_POINT('Ctrl Pts',(1.70973140088841,-72.456803556463,0.));
#68385=CARTESIAN_POINT('Ctrl Pts',(1.71921936650037,-72.479833744618,0.));
#68386=CARTESIAN_POINT('Ctrl Pts',(1.72874475715102,-72.5028921042721,0.));
#68387=CARTESIAN_POINT('Ctrl Pts',(1.73830758339124,-72.5259785133595,0.));
#68388=CARTESIAN_POINT('Ctrl Pts',(1.74790785564473,-72.5490928502769,0.));
#68389=CARTESIAN_POINT('Ctrl Pts',(1.75754558420343,-72.5722349938774,0.));
#68390=CARTESIAN_POINT('Ctrl Pts',(1.76722077922574,-72.5954048234638,0.));
#68391=CARTESIAN_POINT('Ctrl Pts',(1.77693345074426,-72.6186022187907,0.));
#68392=CARTESIAN_POINT('Ctrl Pts',(1.7866836086681,-72.6418270600619,0.));
#68393=CARTESIAN_POINT('Ctrl Pts',(1.79647126278358,-72.6650792279274,0.));
#68394=CARTESIAN_POINT('Ctrl Pts',(1.8062964227505,-72.6883586034769,0.));
#68395=CARTESIAN_POINT('Ctrl Pts',(1.8161590980987,-72.7116650682344,0.));
#68396=CARTESIAN_POINT('Ctrl Pts',(1.82605929823564,-72.7349985041592,0.));
#68397=CARTESIAN_POINT('Ctrl Pts',(1.83599703244924,-72.7583587936447,0.));
#68398=CARTESIAN_POINT('Ctrl Pts',(1.84597230990856,-72.7817458195155,0.));
#68399=CARTESIAN_POINT('Ctrl Pts',(1.85598513966113,-72.8051594650222,0.));
#68400=CARTESIAN_POINT('Ctrl Pts',(1.8660355306277,-72.8285996138359,0.));
#68401=CARTESIAN_POINT('Ctrl Pts',(1.87612349160944,-72.8520661500477,0.));
#68402=CARTESIAN_POINT('Ctrl Pts',(1.88624903129187,-72.875558958168,0.));
#68403=CARTESIAN_POINT('Ctrl Pts',(1.89641215824581,-72.8990779231226,0.));
#68404=CARTESIAN_POINT('Ctrl Pts',(1.90661288092586,-72.9226229302478,0.));
#68405=CARTESIAN_POINT('Ctrl Pts',(1.91685120766436,-72.9461938652811,0.));
#68406=CARTESIAN_POINT('Ctrl Pts',(1.9271271466766,-72.9697906143636,0.));
#68407=CARTESIAN_POINT('Ctrl Pts',(1.93744070606565,-72.9934130640415,0.));
#68408=CARTESIAN_POINT('Ctrl Pts',(1.94779189382301,-73.0170611012661,0.));
#68409=CARTESIAN_POINT('Ctrl Pts',(1.95818071782766,-73.040734613391,0.));
#68410=CARTESIAN_POINT('Ctrl Pts',(1.96860718583931,-73.0644334881673,0.));
#68411=CARTESIAN_POINT('Ctrl Pts',(1.97907130550157,-73.0881576137407,0.));
#68412=CARTESIAN_POINT('Ctrl Pts',(1.98957308434917,-73.1119068786475,0.));
#68413=CARTESIAN_POINT('Ctrl Pts',(2.00011252980981,-73.1356811718091,0.));
#68414=CARTESIAN_POINT('Ctrl Pts',(2.01068964920466,-73.1594803825252,0.));
#68415=CARTESIAN_POINT('Ctrl Pts',(2.02130444974361,-73.183304400462,0.));
#68416=CARTESIAN_POINT('Ctrl Pts',(2.03195693852454,-73.2071531156504,0.));
#68417=CARTESIAN_POINT('Ctrl Pts',(2.04264712253928,-73.2310264184976,0.));
#68418=CARTESIAN_POINT('Ctrl Pts',(2.05337500867402,-73.2549241997953,0.));
#68419=CARTESIAN_POINT('Ctrl Pts',(2.06414060370834,-73.2788463507246,0.));
#68420=CARTESIAN_POINT('Ctrl Pts',(2.0749439143094,-73.3027927628626,0.));
#68421=CARTESIAN_POINT('Ctrl Pts',(2.08578494702743,-73.3267633281807,0.));
#68422=CARTESIAN_POINT('Ctrl Pts',(2.09666370830715,-73.3507579390239,0.));
#68423=CARTESIAN_POINT('Ctrl Pts',(2.10758020449389,-73.3747764880893,0.));
#68424=CARTESIAN_POINT('Ctrl Pts',(2.11853444183761,-73.3988188684021,0.));
#68425=CARTESIAN_POINT('Ctrl Pts',(2.12952642649367,-73.4228849732925,0.));
#68426=CARTESIAN_POINT('Ctrl Pts',(2.14055616452057,-73.4469746963637,0.));
#68427=CARTESIAN_POINT('Ctrl Pts',(2.15162366187906,-73.4710879315382,0.));
#68428=CARTESIAN_POINT('Ctrl Pts',(2.16272892442919,-73.4952245731054,0.));
#68429=CARTESIAN_POINT('Ctrl Pts',(2.17387195792305,-73.5193845157708,0.));
#68430=CARTESIAN_POINT('Ctrl Pts',(2.18505276799752,-73.5435676546929,0.));
#68431=CARTESIAN_POINT('Ctrl Pts',(2.19627136015677,-73.5677738855452,0.));
#68432=CARTESIAN_POINT('Ctrl Pts',(2.20752773978348,-73.5920031044595,0.));
#68433=CARTESIAN_POINT('Ctrl Pts',(2.21882191216517,-73.6162552079038,0.));
#68434=CARTESIAN_POINT('Ctrl Pts',(2.23015388251287,-73.6405300925712,0.));
#68435=CARTESIAN_POINT('Ctrl Pts',(2.24152365597697,-73.6648276552767,0.));
#68436=CARTESIAN_POINT('Ctrl Pts',(2.25293123766424,-73.6891477928129,0.));
#68437=CARTESIAN_POINT('Ctrl Pts',(2.26437663263666,-73.7134904019389,0.));
#68438=CARTESIAN_POINT('Ctrl Pts',(2.27585984587198,-73.7378553796807,0.));
#68439=CARTESIAN_POINT('Ctrl Pts',(2.28738088222863,-73.762242623566,0.));
#68440=CARTESIAN_POINT('Ctrl Pts',(2.29893974640434,-73.786652031885,0.));
#68441=CARTESIAN_POINT('Ctrl Pts',(2.31053644289416,-73.8110835039327,0.));
#68442=CARTESIAN_POINT('Ctrl Pts',(2.32217097594197,-73.8355369402706,0.));
#68443=CARTESIAN_POINT('Ctrl Pts',(2.33384334963957,-73.8600122421468,0.));
#68444=CARTESIAN_POINT('Ctrl Pts',(2.3455535680212,-73.8845093109274,0.));
#68445=CARTESIAN_POINT('Ctrl Pts',(2.35730163516315,-73.9090280474712,0.));
#68446=CARTESIAN_POINT('Ctrl Pts',(2.36908755526003,-73.9335683516404,0.));
#68447=CARTESIAN_POINT('Ctrl Pts',(2.3809113327496,-73.958130121465,0.));
#68448=CARTESIAN_POINT('Ctrl Pts',(2.39277297220756,-73.9827132538206,0.));
#68449=CARTESIAN_POINT('Ctrl Pts',(2.40467247811536,-74.0073176459344,0.));
#68450=CARTESIAN_POINT('Ctrl Pts',(2.41660985465251,-74.0319431966989,0.));
#68451=CARTESIAN_POINT('Ctrl Pts',(2.42858510549778,-74.0565898079218,0.));
#68452=CARTESIAN_POINT('Ctrl Pts',(2.44059823356675,-74.0812573859411,0.));
#68453=CARTESIAN_POINT('Ctrl Pts',(2.45264924094774,-74.1059458420067,0.));
#68454=CARTESIAN_POINT('Ctrl Pts',(2.46301176097121,-74.127126454519,0.));
#68455=CARTESIAN_POINT('Ctrl Pts',(2.47097695564999,-74.1433763941382,0.));
#68456=CARTESIAN_POINT('Ctrl Pts',(2.47652804724548,-74.1546864735169,0.));
#68457=CARTESIAN_POINT('Ctrl Pts',(2.47965393945489,-74.1610506466209,0.));
#68458=CARTESIAN_POINT('Ctrl Pts',(2.48034921843246,-74.1624659714559,0.));
#68459=CARTESIAN_POINT('',(0.853825826608976,-69.9947925310006,12.));
#68460=CARTESIAN_POINT('',(0.853825826608976,-69.9947925310006,0.));
#68461=CARTESIAN_POINT('Ctrl Pts',(2.48034921843246,-74.1624659714559,12.));
#68462=CARTESIAN_POINT('Ctrl Pts',(2.47965393945489,-74.1610506466209,12.));
#68463=CARTESIAN_POINT('Ctrl Pts',(2.47652804724548,-74.1546864735169,12.));
#68464=CARTESIAN_POINT('Ctrl Pts',(2.47097695565,-74.1433763941382,12.));
#68465=CARTESIAN_POINT('Ctrl Pts',(2.46301176097121,-74.127126454519,12.));
#68466=CARTESIAN_POINT('Ctrl Pts',(2.45264924094774,-74.1059458420067,12.));
#68467=CARTESIAN_POINT('Ctrl Pts',(2.44059823356675,-74.0812573859411,12.));
#68468=CARTESIAN_POINT('Ctrl Pts',(2.42858510549778,-74.0565898079218,12.));
#68469=CARTESIAN_POINT('Ctrl Pts',(2.41660985465251,-74.0319431966989,12.));
#68470=CARTESIAN_POINT('Ctrl Pts',(2.40467247811536,-74.0073176459344,12.));
#68471=CARTESIAN_POINT('Ctrl Pts',(2.39277297220756,-73.9827132538206,12.));
#68472=CARTESIAN_POINT('Ctrl Pts',(2.3809113327496,-73.958130121465,12.));
#68473=CARTESIAN_POINT('Ctrl Pts',(2.36908755526003,-73.9335683516404,12.));
#68474=CARTESIAN_POINT('Ctrl Pts',(2.35730163516315,-73.9090280474712,12.));
#68475=CARTESIAN_POINT('Ctrl Pts',(2.3455535680212,-73.8845093109274,12.));
#68476=CARTESIAN_POINT('Ctrl Pts',(2.33384334963957,-73.8600122421468,12.));
#68477=CARTESIAN_POINT('Ctrl Pts',(2.32217097594197,-73.8355369402706,12.));
#68478=CARTESIAN_POINT('Ctrl Pts',(2.31053644289416,-73.8110835039327,12.));
#68479=CARTESIAN_POINT('Ctrl Pts',(2.29893974640434,-73.786652031885,12.));
#68480=CARTESIAN_POINT('Ctrl Pts',(2.28738088222863,-73.762242623566,12.));
#68481=CARTESIAN_POINT('Ctrl Pts',(2.27585984587198,-73.7378553796807,12.));
#68482=CARTESIAN_POINT('Ctrl Pts',(2.26437663263666,-73.7134904019389,12.));
#68483=CARTESIAN_POINT('Ctrl Pts',(2.25293123766424,-73.6891477928129,12.));
#68484=CARTESIAN_POINT('Ctrl Pts',(2.24152365597697,-73.6648276552767,12.));
#68485=CARTESIAN_POINT('Ctrl Pts',(2.23015388251287,-73.6405300925712,12.));
#68486=CARTESIAN_POINT('Ctrl Pts',(2.21882191216517,-73.6162552079038,12.));
#68487=CARTESIAN_POINT('Ctrl Pts',(2.20752773978348,-73.5920031044595,12.));
#68488=CARTESIAN_POINT('Ctrl Pts',(2.19627136015677,-73.5677738855452,12.));
#68489=CARTESIAN_POINT('Ctrl Pts',(2.18505276799752,-73.5435676546929,12.));
#68490=CARTESIAN_POINT('Ctrl Pts',(2.17387195792305,-73.5193845157708,12.));
#68491=CARTESIAN_POINT('Ctrl Pts',(2.16272892442919,-73.4952245731054,12.));
#68492=CARTESIAN_POINT('Ctrl Pts',(2.15162366187906,-73.4710879315382,12.));
#68493=CARTESIAN_POINT('Ctrl Pts',(2.14055616452057,-73.4469746963637,12.));
#68494=CARTESIAN_POINT('Ctrl Pts',(2.12952642649367,-73.4228849732925,12.));
#68495=CARTESIAN_POINT('Ctrl Pts',(2.11853444183761,-73.3988188684021,12.));
#68496=CARTESIAN_POINT('Ctrl Pts',(2.10758020449389,-73.3747764880893,12.));
#68497=CARTESIAN_POINT('Ctrl Pts',(2.09666370830715,-73.3507579390239,12.));
#68498=CARTESIAN_POINT('Ctrl Pts',(2.08578494702743,-73.3267633281807,12.));
#68499=CARTESIAN_POINT('Ctrl Pts',(2.0749439143094,-73.3027927628626,12.));
#68500=CARTESIAN_POINT('Ctrl Pts',(2.06414060370834,-73.2788463507246,12.));
#68501=CARTESIAN_POINT('Ctrl Pts',(2.05337500867402,-73.2549241997953,12.));
#68502=CARTESIAN_POINT('Ctrl Pts',(2.04264712253928,-73.2310264184976,12.));
#68503=CARTESIAN_POINT('Ctrl Pts',(2.03195693852454,-73.2071531156504,12.));
#68504=CARTESIAN_POINT('Ctrl Pts',(2.02130444974361,-73.183304400462,12.));
#68505=CARTESIAN_POINT('Ctrl Pts',(2.01068964920466,-73.1594803825252,12.));
#68506=CARTESIAN_POINT('Ctrl Pts',(2.00011252980981,-73.1356811718091,12.));
#68507=CARTESIAN_POINT('Ctrl Pts',(1.98957308434917,-73.1119068786475,12.));
#68508=CARTESIAN_POINT('Ctrl Pts',(1.97907130550157,-73.0881576137407,12.));
#68509=CARTESIAN_POINT('Ctrl Pts',(1.96860718583931,-73.0644334881673,12.));
#68510=CARTESIAN_POINT('Ctrl Pts',(1.95818071782766,-73.040734613391,12.));
#68511=CARTESIAN_POINT('Ctrl Pts',(1.94779189382301,-73.0170611012661,12.));
#68512=CARTESIAN_POINT('Ctrl Pts',(1.93744070606565,-72.9934130640415,12.));
#68513=CARTESIAN_POINT('Ctrl Pts',(1.9271271466766,-72.9697906143636,12.));
#68514=CARTESIAN_POINT('Ctrl Pts',(1.91685120766436,-72.9461938652811,12.));
#68515=CARTESIAN_POINT('Ctrl Pts',(1.90661288092586,-72.9226229302478,12.));
#68516=CARTESIAN_POINT('Ctrl Pts',(1.89641215824581,-72.8990779231226,12.));
#68517=CARTESIAN_POINT('Ctrl Pts',(1.88624903129187,-72.875558958168,12.));
#68518=CARTESIAN_POINT('Ctrl Pts',(1.87612349160944,-72.8520661500477,12.));
#68519=CARTESIAN_POINT('Ctrl Pts',(1.8660355306277,-72.8285996138359,12.));
#68520=CARTESIAN_POINT('Ctrl Pts',(1.85598513966113,-72.8051594650222,12.));
#68521=CARTESIAN_POINT('Ctrl Pts',(1.84597230990856,-72.7817458195155,12.));
#68522=CARTESIAN_POINT('Ctrl Pts',(1.83599703244924,-72.7583587936447,12.));
#68523=CARTESIAN_POINT('Ctrl Pts',(1.82605929823564,-72.7349985041592,12.));
#68524=CARTESIAN_POINT('Ctrl Pts',(1.8161590980987,-72.7116650682344,12.));
#68525=CARTESIAN_POINT('Ctrl Pts',(1.8062964227505,-72.6883586034769,12.));
#68526=CARTESIAN_POINT('Ctrl Pts',(1.79647126278358,-72.6650792279274,12.));
#68527=CARTESIAN_POINT('Ctrl Pts',(1.7866836086681,-72.6418270600619,12.));
#68528=CARTESIAN_POINT('Ctrl Pts',(1.77693345074426,-72.6186022187907,12.));
#68529=CARTESIAN_POINT('Ctrl Pts',(1.76722077922574,-72.5954048234638,12.));
#68530=CARTESIAN_POINT('Ctrl Pts',(1.75754558420343,-72.5722349938774,12.));
#68531=CARTESIAN_POINT('Ctrl Pts',(1.74790785564473,-72.5490928502769,12.));
#68532=CARTESIAN_POINT('Ctrl Pts',(1.73830758339124,-72.5259785133595,12.));
#68533=CARTESIAN_POINT('Ctrl Pts',(1.72874475715102,-72.5028921042721,12.));
#68534=CARTESIAN_POINT('Ctrl Pts',(1.71921936650037,-72.479833744618,12.));
#68535=CARTESIAN_POINT('Ctrl Pts',(1.70973140088841,-72.456803556463,12.));
#68536=CARTESIAN_POINT('Ctrl Pts',(1.70028084963647,-72.4338016623391,12.));
#68537=CARTESIAN_POINT('Ctrl Pts',(1.69086770193636,-72.4108281852467,12.));
#68538=CARTESIAN_POINT('Ctrl Pts',(1.68149194684281,-72.387883248654,12.));
#68539=CARTESIAN_POINT('Ctrl Pts',(1.67215357327364,-72.3649669765004,12.));
#68540=CARTESIAN_POINT('Ctrl Pts',(1.66285257001496,-72.3420794932047,12.));
#68541=CARTESIAN_POINT('Ctrl Pts',(1.65358892572062,-72.319220923669,12.));
#68542=CARTESIAN_POINT('Ctrl Pts',(1.64436262891078,-72.2963913932813,12.));
#68543=CARTESIAN_POINT('Ctrl Pts',(1.63517366796462,-72.2735910279149,12.));
#68544=CARTESIAN_POINT('Ctrl Pts',(1.62602203111929,-72.2508199539323,12.));
#68545=CARTESIAN_POINT('Ctrl Pts',(1.61690770647539,-72.2280782981937,12.));
#68546=CARTESIAN_POINT('Ctrl Pts',(1.60783068199662,-72.2053661880608,12.));
#68547=CARTESIAN_POINT('Ctrl Pts',(1.59879094550846,-72.1826837514001,12.));
#68548=CARTESIAN_POINT('Ctrl Pts',(1.58978848469122,-72.1600311165821,12.));
#68549=CARTESIAN_POINT('Ctrl Pts',(1.58082328707802,-72.1374084124839,12.));
#68550=CARTESIAN_POINT('Ctrl Pts',(1.5718953400604,-72.1148157684995,12.));
#68551=CARTESIAN_POINT('Ctrl Pts',(1.56300463088808,-72.0922533145433,12.));
#68552=CARTESIAN_POINT('Ctrl Pts',(1.55415114666773,-72.0697211810545,12.));
#68553=CARTESIAN_POINT('Ctrl Pts',(1.54533487435625,-72.0472194989963,12.));
#68554=CARTESIAN_POINT('Ctrl Pts',(1.53655580075812,-72.0247483998579,12.));
#68555=CARTESIAN_POINT('Ctrl Pts',(1.52781391253101,-72.0023080156647,12.));
#68556=CARTESIAN_POINT('Ctrl Pts',(1.51910919618565,-71.979898478983,12.));
#68557=CARTESIAN_POINT('Ctrl Pts',(1.51044163808453,-71.9575199229241,12.));
#68558=CARTESIAN_POINT('Ctrl Pts',(1.50181122443533,-71.9351724811443,12.));
#68559=CARTESIAN_POINT('Ctrl Pts',(1.49321794128798,-71.912856287848,12.));
#68560=CARTESIAN_POINT('Ctrl Pts',(1.48466177454019,-71.8905714777961,12.));
#68561=CARTESIAN_POINT('Ctrl Pts',(1.47614270993728,-71.8683181863116,12.));
#68562=CARTESIAN_POINT('Ctrl Pts',(1.46766073307087,-71.8460965492839,12.));
#68563=CARTESIAN_POINT('Ctrl Pts',(1.45921582937231,-71.8239067031683,12.));
#68564=CARTESIAN_POINT('Ctrl Pts',(1.45080798410964,-71.8017487849895,12.));
#68565=CARTESIAN_POINT('Ctrl Pts',(1.44243718239314,-71.7796229323526,12.));
#68566=CARTESIAN_POINT('Ctrl Pts',(1.43410340917495,-71.7575292834469,12.));
#68567=CARTESIAN_POINT('Ctrl Pts',(1.42580664924769,-71.7354679770528,12.));
#68568=CARTESIAN_POINT('Ctrl Pts',(1.41754688723772,-71.7134391525389,12.));
#68569=CARTESIAN_POINT('Ctrl Pts',(1.40932410760247,-71.6914429498663,12.));
#68570=CARTESIAN_POINT('Ctrl Pts',(1.40113829463576,-71.6694795096001,12.));
#68571=CARTESIAN_POINT('Ctrl Pts',(1.39298943246721,-71.6475489729134,12.));
#68572=CARTESIAN_POINT('Ctrl Pts',(1.38487750506081,-71.625651481593,12.));
#68573=CARTESIAN_POINT('Ctrl Pts',(1.37680249620779,-71.6037871780385,12.));
#68574=CARTESIAN_POINT('Ctrl Pts',(1.36876438952465,-71.5819562052663,12.));
#68575=CARTESIAN_POINT('Ctrl Pts',(1.36076316845815,-71.5601587069217,12.));
#68576=CARTESIAN_POINT('Ctrl Pts',(1.35279881628454,-71.5383948272845,12.));
#68577=CARTESIAN_POINT('Ctrl Pts',(1.3448713161078,-71.516664711275,12.));
#68578=CARTESIAN_POINT('Ctrl Pts',(1.33698065085219,-71.4949685044522,12.));
#68579=CARTESIAN_POINT('Ctrl Pts',(1.32912680326123,-71.4733063530187,12.));
#68580=CARTESIAN_POINT('Ctrl Pts',(1.32130975590225,-71.4516784038317,12.));
#68581=CARTESIAN_POINT('Ctrl Pts',(1.31352949116536,-71.4300848044087,12.));
#68582=CARTESIAN_POINT('Ctrl Pts',(1.30578599126139,-71.4085257029322,12.));
#68583=CARTESIAN_POINT('Ctrl Pts',(1.29807923821413,-71.3870012482499,12.));
#68584=CARTESIAN_POINT('Ctrl Pts',(1.29040921386058,-71.3655115898827,12.));
#68585=CARTESIAN_POINT('Ctrl Pts',(1.28277589985471,-71.3440568780347,12.));
#68586=CARTESIAN_POINT('Ctrl Pts',(1.27517927766607,-71.3226372635996,12.));
#68587=CARTESIAN_POINT('Ctrl Pts',(1.26761932857724,-71.3012528981661,12.));
#68588=CARTESIAN_POINT('Ctrl Pts',(1.2600960336757,-71.2799039340175,12.));
#68589=CARTESIAN_POINT('Ctrl Pts',(1.25260937385568,-71.2585905241406,12.));
#68590=CARTESIAN_POINT('Ctrl Pts',(1.24515932982112,-71.2373128222352,12.));
#68591=CARTESIAN_POINT('Ctrl Pts',(1.23774588208426,-71.2160709827191,12.));
#68592=CARTESIAN_POINT('Ctrl Pts',(1.23036901096238,-71.194865160732,12.));
#68593=CARTESIAN_POINT('Ctrl Pts',(1.22302869657017,-71.1736955121362,12.));
#68594=CARTESIAN_POINT('Ctrl Pts',(1.21572491882262,-71.1525621935267,12.));
#68595=CARTESIAN_POINT('Ctrl Pts',(1.20845765743647,-71.1314653622442,12.));
#68596=CARTESIAN_POINT('Ctrl Pts',(1.20122689192835,-71.1104051763839,12.));
#68597=CARTESIAN_POINT('Ctrl Pts',(1.19403260161001,-71.089381794801,12.));
#68598=CARTESIAN_POINT('Ctrl Pts',(1.18687476558132,-71.0683953771149,12.));
#68599=CARTESIAN_POINT('Ctrl Pts',(1.17975336273503,-71.0474460837159,12.));
#68600=CARTESIAN_POINT('Ctrl Pts',(1.17266837175776,-71.0265340757699,12.));
#68601=CARTESIAN_POINT('Ctrl Pts',(1.1656197711288,-71.0056595152204,12.));
#68602=CARTESIAN_POINT('Ctrl Pts',(1.15860753911484,-70.9848225647871,12.));
#68603=CARTESIAN_POINT('Ctrl Pts',(1.15163165376523,-70.9640233879659,12.));
#68604=CARTESIAN_POINT('Ctrl Pts',(1.14469209291488,-70.9432621490566,12.));
#68605=CARTESIAN_POINT('Ctrl Pts',(1.13778883418213,-70.9225390131826,12.));
#68606=CARTESIAN_POINT('Ctrl Pts',(1.13092185496564,-70.9018541463089,12.));
#68607=CARTESIAN_POINT('Ctrl Pts',(1.12409113243513,-70.8812077152586,12.));
#68608=CARTESIAN_POINT('Ctrl Pts',(1.11729664352992,-70.8605998877149,12.));
#68609=CARTESIAN_POINT('Ctrl Pts',(1.11053836496639,-70.8400308322037,12.));
#68610=CARTESIAN_POINT('Ctrl Pts',(1.10381627323946,-70.8195007180745,12.));
#68611=CARTESIAN_POINT('Ctrl Pts',(1.09713034462265,-70.799009715484,12.));
#68612=CARTESIAN_POINT('Ctrl Pts',(1.09048055516426,-70.7785579953583,12.));
#68613=CARTESIAN_POINT('Ctrl Pts',(1.08386688068342,-70.7581457294447,12.));
#68614=CARTESIAN_POINT('Ctrl Pts',(1.07728929676408,-70.7377730903953,12.));
#68615=CARTESIAN_POINT('Ctrl Pts',(1.07074777874595,-70.7174402518378,12.));
#68616=CARTESIAN_POINT('Ctrl Pts',(1.0642423017128,-70.6971473884459,12.));
#68617=CARTESIAN_POINT('Ctrl Pts',(1.05777284047729,-70.676894676009,12.));
#68618=CARTESIAN_POINT('Ctrl Pts',(1.05133936960071,-70.6566822912991,12.));
#68619=CARTESIAN_POINT('Ctrl Pts',(1.04494186341155,-70.6365104119252,12.));
#68620=CARTESIAN_POINT('Ctrl Pts',(1.03858029601903,-70.6163792162073,12.));
#68621=CARTESIAN_POINT('Ctrl Pts',(1.0322546413287,-70.5962888829934,12.));
#68622=CARTESIAN_POINT('Ctrl Pts',(1.02596487304048,-70.5762395916377,12.));
#68623=CARTESIAN_POINT('Ctrl Pts',(1.01971096460596,-70.556231522419,12.));
#68624=CARTESIAN_POINT('Ctrl Pts',(1.01349288918536,-70.5362648569061,12.));
#68625=CARTESIAN_POINT('Ctrl Pts',(1.00731061960967,-70.5163397782713,12.));
#68626=CARTESIAN_POINT('Ctrl Pts',(1.00116412831442,-70.4964564717953,12.));
#68627=CARTESIAN_POINT('Ctrl Pts',(0.995053387379748,-70.4766151245212,
12.));
#68628=CARTESIAN_POINT('Ctrl Pts',(0.988978368643642,-70.4568159243163,
12.));
#68629=CARTESIAN_POINT('Ctrl Pts',(0.982939043792148,-70.4370590590842,
12.));
#68630=CARTESIAN_POINT('Ctrl Pts',(0.976935384450034,-70.417344715957,12.));
#68631=CARTESIAN_POINT('Ctrl Pts',(0.970967362281167,-70.3976730803614,
12.));
#68632=CARTESIAN_POINT('Ctrl Pts',(0.965034948786442,-70.3780443377956,
12.));
#68633=CARTESIAN_POINT('Ctrl Pts',(0.959138115058824,-70.3584586759536,
12.));
#68634=CARTESIAN_POINT('Ctrl Pts',(0.953276831581235,-70.338916286458,12.));
#68635=CARTESIAN_POINT('Ctrl Pts',(0.947451067929597,-70.3194173673674,
12.));
#68636=CARTESIAN_POINT('Ctrl Pts',(0.941660792742972,-70.299962123399,12.));
#68637=CARTESIAN_POINT('Ctrl Pts',(0.935905974336473,-70.2805507606872,
12.));
#68638=CARTESIAN_POINT('Ctrl Pts',(0.93018658123554,-70.2611834821724,12.));
#68639=CARTESIAN_POINT('Ctrl Pts',(0.924502582639448,-70.2418604835837,
12.));
#68640=CARTESIAN_POINT('Ctrl Pts',(0.918853949157111,-70.2225819470248,
12.));
#68641=CARTESIAN_POINT('Ctrl Pts',(0.913240652090973,-70.2033480471676,
12.));
#68642=CARTESIAN_POINT('Ctrl Pts',(0.907662662015778,-70.1841589635574,
12.));
#68643=CARTESIAN_POINT('Ctrl Pts',(0.902119947629764,-70.1650148905109,
12.));
#68644=CARTESIAN_POINT('Ctrl Pts',(0.896612474371837,-70.1459160490446,
12.));
#68645=CARTESIAN_POINT('Ctrl Pts',(0.891140203464235,-70.1268626950175,
12.));
#68646=CARTESIAN_POINT('Ctrl Pts',(0.885703094802528,-70.1078550938958,
12.));
#68647=CARTESIAN_POINT('Ctrl Pts',(0.880301109660721,-70.0888934967855,
12.));
#68648=CARTESIAN_POINT('Ctrl Pts',(0.874934213255831,-70.0699781183935,
12.));
#68649=CARTESIAN_POINT('Ctrl Pts',(0.869602377871117,-70.051109108301,12.));
#68650=CARTESIAN_POINT('Ctrl Pts',(0.864305583661538,-70.0322865492925,
12.));
#68651=CARTESIAN_POINT('Ctrl Pts',(0.860096170668728,-70.0172656933806,
12.));
#68652=CARTESIAN_POINT('Ctrl Pts',(0.856954870259198,-70.0060209754087,
12.));
#68653=CARTESIAN_POINT('Ctrl Pts',(0.854867673848587,-69.9985337959407,
12.));
#68654=CARTESIAN_POINT('Ctrl Pts',(0.853825826608976,-69.9947925310006,
12.));
#68655=CARTESIAN_POINT('Ctrl Pts',(3.99277406490873,-74.0964320766207,-5.55111512312578E-16));
#68656=CARTESIAN_POINT('Ctrl Pts',(3.99277406490873,-74.0964320766207,4.));
#68657=CARTESIAN_POINT('Ctrl Pts',(3.99277406490871,-74.0964320766207,8.));
#68658=CARTESIAN_POINT('Ctrl Pts',(3.99277406490871,-74.0964320766207,12.));
#68659=CARTESIAN_POINT('Ctrl Pts',(3.95310474582233,-74.1989040313892,-5.55111512312578E-16));
#68660=CARTESIAN_POINT('Ctrl Pts',(3.95310474582233,-74.1989040313892,4.));
#68661=CARTESIAN_POINT('Ctrl Pts',(3.95310474582231,-74.1989040313893,8.));
#68662=CARTESIAN_POINT('Ctrl Pts',(3.95310474582231,-74.1989040313893,12.));
#68663=CARTESIAN_POINT('Ctrl Pts',(3.82252142018535,-74.3538917248566,-5.55111512312578E-16));
#68664=CARTESIAN_POINT('Ctrl Pts',(3.82252142018535,-74.3538917248566,4.00000000000001));
#68665=CARTESIAN_POINT('Ctrl Pts',(3.82252142018533,-74.3538917248566,8.));
#68666=CARTESIAN_POINT('Ctrl Pts',(3.82252142018533,-74.3538917248566,12.));
#68667=CARTESIAN_POINT('Ctrl Pts',(3.63264011802873,-74.4114286752098,-5.55111512312578E-16));
#68668=CARTESIAN_POINT('Ctrl Pts',(3.63264011802873,-74.4114286752098,4.));
#68669=CARTESIAN_POINT('Ctrl Pts',(3.63264011802872,-74.4114286752098,8.00000000000001));
#68670=CARTESIAN_POINT('Ctrl Pts',(3.63264011802872,-74.4114286752098,12.));
#68671=CARTESIAN_POINT('Ctrl Pts',(3.55032190142808,-74.4153560388998,-5.55111512312578E-16));
#68672=CARTESIAN_POINT('Ctrl Pts',(3.55032190142808,-74.4153560388998,4.));
#68673=CARTESIAN_POINT('Ctrl Pts',(3.55032190142807,-74.4153560388998,8.));
#68674=CARTESIAN_POINT('Ctrl Pts',(3.55032190142807,-74.4153560388998,12.));
#68675=CARTESIAN_POINT('',(3.99277406490873,-74.0964320766207,-2.77555756156289E-16));
#68676=CARTESIAN_POINT('',(3.55032190142809,-74.4153560388999,0.));
#68677=CARTESIAN_POINT('Ctrl Pts',(3.99277406490873,-74.0964320766207,-1.38777878078145E-16));
#68678=CARTESIAN_POINT('Ctrl Pts',(3.95310474582233,-74.1989040313892,-1.38777878078145E-16));
#68679=CARTESIAN_POINT('Ctrl Pts',(3.8784857026012,-74.2874684276563,-1.38777878078144E-16));
#68680=CARTESIAN_POINT('Ctrl Pts',(3.78450405480223,-74.3442121731105,-1.38777878078144E-16));
#68681=CARTESIAN_POINT('Ctrl Pts',(3.714017818953,-74.3867699822013,-1.38777878078144E-16));
#68682=CARTESIAN_POINT('Ctrl Pts',(3.63264011802873,-74.4114286752098,-1.38777878078145E-16));
#68683=CARTESIAN_POINT('Ctrl Pts',(3.55032190142808,-74.4153560388998,-1.38777878078144E-16));
#68684=CARTESIAN_POINT('',(3.55032190142808,-74.4153560388999,12.));
#68685=CARTESIAN_POINT('Ctrl Pts',(3.55032190142808,-74.4153560388998,-5.55111512312578E-16));
#68686=CARTESIAN_POINT('Ctrl Pts',(3.55032190142808,-74.4153560388998,4.));
#68687=CARTESIAN_POINT('Ctrl Pts',(3.55032190142807,-74.4153560388998,8.));
#68688=CARTESIAN_POINT('Ctrl Pts',(3.55032190142807,-74.4153560388998,12.));
#68689=CARTESIAN_POINT('',(3.99277406490871,-74.0964320766207,12.));
#68690=CARTESIAN_POINT('Ctrl Pts',(3.55032190142807,-74.4153560388998,12.));
#68691=CARTESIAN_POINT('Ctrl Pts',(3.63264011802872,-74.4114286752098,12.));
#68692=CARTESIAN_POINT('Ctrl Pts',(3.71401781895298,-74.3867699822013,12.));
#68693=CARTESIAN_POINT('Ctrl Pts',(3.78450405480221,-74.3442121731106,12.));
#68694=CARTESIAN_POINT('Ctrl Pts',(3.87848570260118,-74.2874684276563,12.));
#68695=CARTESIAN_POINT('Ctrl Pts',(3.95310474582231,-74.1989040313893,12.));
#68696=CARTESIAN_POINT('Ctrl Pts',(3.99277406490871,-74.0964320766207,12.));
#68697=CARTESIAN_POINT('Ctrl Pts',(3.99277406490871,-74.0964320766207,12.));
#68698=CARTESIAN_POINT('Ctrl Pts',(3.99277406490871,-74.0964320766207,8.));
#68699=CARTESIAN_POINT('Ctrl Pts',(3.99277406490873,-74.0964320766207,4.));
#68700=CARTESIAN_POINT('Ctrl Pts',(3.99277406490873,-74.0964320766207,-5.55111512312578E-16));
#68701=CARTESIAN_POINT('Origin',(1.64496194443586E-11,-3.74482667098164E-10,
0.));
#68702=CARTESIAN_POINT('Origin',(1.64496194443586E-11,-3.74482667098164E-10,
12.));
#68703=CARTESIAN_POINT('Origin',(1.64496194443586E-11,-3.74482667098164E-10,
0.));
#68704=CARTESIAN_POINT('Ctrl Pts',(-3.55032190142517,-74.4153560389001,
0.));
#68705=CARTESIAN_POINT('Ctrl Pts',(-3.55032190142517,-74.4153560389001,
4.));
#68706=CARTESIAN_POINT('Ctrl Pts',(-3.55032190142517,-74.4153560389001,
8.));
#68707=CARTESIAN_POINT('Ctrl Pts',(-3.55032190142517,-74.4153560389001,
12.));
#68708=CARTESIAN_POINT('Ctrl Pts',(-3.66007952356784,-74.4101195539797,
0.));
#68709=CARTESIAN_POINT('Ctrl Pts',(-3.66007952356784,-74.4101195539797,
4.));
#68710=CARTESIAN_POINT('Ctrl Pts',(-3.66007952356784,-74.4101195539797,
8.));
#68711=CARTESIAN_POINT('Ctrl Pts',(-3.66007952356784,-74.4101195539797,
12.));
#68712=CARTESIAN_POINT('Ctrl Pts',(-3.84840282419245,-74.3352361483147,
0.));
#68713=CARTESIAN_POINT('Ctrl Pts',(-3.84840282419245,-74.3352361483147,
4.));
#68714=CARTESIAN_POINT('Ctrl Pts',(-3.84840282419245,-74.3352361483147,
7.99999999999999));
#68715=CARTESIAN_POINT('Ctrl Pts',(-3.84840282419245,-74.3352361483147,
12.));
#68716=CARTESIAN_POINT('Ctrl Pts',(-3.96302207561163,-74.1732860426646,
0.));
#68717=CARTESIAN_POINT('Ctrl Pts',(-3.96302207561163,-74.1732860426646,
4.));
#68718=CARTESIAN_POINT('Ctrl Pts',(-3.96302207561163,-74.1732860426646,
8.00000000000001));
#68719=CARTESIAN_POINT('Ctrl Pts',(-3.96302207561163,-74.1732860426646,
12.));
#68720=CARTESIAN_POINT('Ctrl Pts',(-3.99277406492189,-74.0964320765795,
0.));
#68721=CARTESIAN_POINT('Ctrl Pts',(-3.99277406492189,-74.0964320765795,
4.));
#68722=CARTESIAN_POINT('Ctrl Pts',(-3.99277406492189,-74.0964320765795,
8.));
#68723=CARTESIAN_POINT('Ctrl Pts',(-3.99277406492189,-74.0964320765795,
12.));
#68724=CARTESIAN_POINT('',(-3.55032190142517,-74.4153560389001,0.));
#68725=CARTESIAN_POINT('',(-3.99277406492187,-74.0964320765795,0.));
#68726=CARTESIAN_POINT('Ctrl Pts',(-3.55032190142517,-74.4153560389001,
0.));
#68727=CARTESIAN_POINT('Ctrl Pts',(-3.66007952356784,-74.4101195539797,
0.));
#68728=CARTESIAN_POINT('Ctrl Pts',(-3.76769283821047,-74.3673290364569,
0.));
#68729=CARTESIAN_POINT('Ctrl Pts',(-3.85123952454113,-74.2961085760817,
0.));
#68730=CARTESIAN_POINT('Ctrl Pts',(-3.91389953928912,-74.2426932308003,
0.));
#68731=CARTESIAN_POINT('Ctrl Pts',(-3.96302207561163,-74.1732860426646,
0.));
#68732=CARTESIAN_POINT('Ctrl Pts',(-3.99277406492189,-74.0964320765795,
0.));
#68733=CARTESIAN_POINT('',(-3.99277406492187,-74.0964320765795,12.));
#68734=CARTESIAN_POINT('Ctrl Pts',(-3.99277406492189,-74.0964320765795,
0.));
#68735=CARTESIAN_POINT('Ctrl Pts',(-3.99277406492189,-74.0964320765795,
4.));
#68736=CARTESIAN_POINT('Ctrl Pts',(-3.99277406492189,-74.0964320765795,
8.));
#68737=CARTESIAN_POINT('Ctrl Pts',(-3.99277406492189,-74.0964320765795,
12.));
#68738=CARTESIAN_POINT('',(-3.55032190142517,-74.4153560389001,12.));
#68739=CARTESIAN_POINT('Ctrl Pts',(-3.99277406492189,-74.0964320765795,
12.));
#68740=CARTESIAN_POINT('Ctrl Pts',(-3.96302207561163,-74.1732860426646,
12.));
#68741=CARTESIAN_POINT('Ctrl Pts',(-3.91389953928912,-74.2426932308003,
12.));
#68742=CARTESIAN_POINT('Ctrl Pts',(-3.85123952454113,-74.2961085760817,
12.));
#68743=CARTESIAN_POINT('Ctrl Pts',(-3.76769283821047,-74.3673290364569,
12.));
#68744=CARTESIAN_POINT('Ctrl Pts',(-3.66007952356784,-74.4101195539797,
12.));
#68745=CARTESIAN_POINT('Ctrl Pts',(-3.55032190142517,-74.4153560389001,
12.));
#68746=CARTESIAN_POINT('Ctrl Pts',(-3.55032190142517,-74.4153560389001,
12.));
#68747=CARTESIAN_POINT('Ctrl Pts',(-3.55032190142517,-74.4153560389001,
8.));
#68748=CARTESIAN_POINT('Ctrl Pts',(-3.55032190142517,-74.4153560389001,
4.));
#68749=CARTESIAN_POINT('Ctrl Pts',(-3.55032190142517,-74.4153560389001,
0.));
#68750=CARTESIAN_POINT('Ctrl Pts',(-5.24987136994592,-69.8028570375097,
0.));
#68751=CARTESIAN_POINT('Ctrl Pts',(-5.24987136994592,-69.8028570375097,
12.));
#68752=CARTESIAN_POINT('Ctrl Pts',(-5.24915955997427,-69.8066748687772,
0.));
#68753=CARTESIAN_POINT('Ctrl Pts',(-5.24915955997427,-69.8066748687772,
12.));
#68754=CARTESIAN_POINT('Ctrl Pts',(-5.24773285666376,-69.8143154684204,
0.));
#68755=CARTESIAN_POINT('Ctrl Pts',(-5.24773285666376,-69.8143154684204,
12.));
#68756=CARTESIAN_POINT('Ctrl Pts',(-5.2455835515975,-69.8257911792159,0.));
#68757=CARTESIAN_POINT('Ctrl Pts',(-5.2455835515975,-69.8257911792159,12.));
#68758=CARTESIAN_POINT('Ctrl Pts',(-5.24269931054569,-69.841121750752,0.));
#68759=CARTESIAN_POINT('Ctrl Pts',(-5.24269931054569,-69.841121750752,12.));
#68760=CARTESIAN_POINT('Ctrl Pts',(-5.23906316634803,-69.8603343302743,
0.));
#68761=CARTESIAN_POINT('Ctrl Pts',(-5.23906316634803,-69.8603343302743,
12.));
#68762=CARTESIAN_POINT('Ctrl Pts',(-5.2353961627962,-69.8795962381599,0.));
#68763=CARTESIAN_POINT('Ctrl Pts',(-5.2353961627962,-69.8795962381599,12.));
#68764=CARTESIAN_POINT('Ctrl Pts',(-5.23169827290555,-69.8989073936688,
0.));
#68765=CARTESIAN_POINT('Ctrl Pts',(-5.23169827290555,-69.8989073936688,
12.));
#68766=CARTESIAN_POINT('Ctrl Pts',(-5.22796945602794,-69.9182676502048,
0.));
#68767=CARTESIAN_POINT('Ctrl Pts',(-5.22796945602794,-69.9182676502048,
12.));
#68768=CARTESIAN_POINT('Ctrl Pts',(-5.22420965879981,-69.9376767969095,
0.));
#68769=CARTESIAN_POINT('Ctrl Pts',(-5.22420965879981,-69.9376767969095,
12.));
#68770=CARTESIAN_POINT('Ctrl Pts',(-5.22041882075721,-69.9571345870076,
0.));
#68771=CARTESIAN_POINT('Ctrl Pts',(-5.22041882075721,-69.9571345870076,
12.));
#68772=CARTESIAN_POINT('Ctrl Pts',(-5.21659687881139,-69.9766407595385,
0.));
#68773=CARTESIAN_POINT('Ctrl Pts',(-5.21659687881139,-69.9766407595385,
12.));
#68774=CARTESIAN_POINT('Ctrl Pts',(-5.21274377203259,-69.9961950629965,
0.));
#68775=CARTESIAN_POINT('Ctrl Pts',(-5.21274377203259,-69.9961950629965,
12.));
#68776=CARTESIAN_POINT('Ctrl Pts',(-5.20885944672836,-70.0157972802182,
0.));
#68777=CARTESIAN_POINT('Ctrl Pts',(-5.20885944672836,-70.0157972802182,
12.));
#68778=CARTESIAN_POINT('Ctrl Pts',(-5.20494385478025,-70.0354472203546,
0.));
#68779=CARTESIAN_POINT('Ctrl Pts',(-5.20494385478025,-70.0354472203546,
12.));
#68780=CARTESIAN_POINT('Ctrl Pts',(-5.20099695122656,-70.0551447071082,
0.));
#68781=CARTESIAN_POINT('Ctrl Pts',(-5.20099695122656,-70.0551447071082,
12.));
#68782=CARTESIAN_POINT('Ctrl Pts',(-5.19701869225528,-70.0748895689729,
0.));
#68783=CARTESIAN_POINT('Ctrl Pts',(-5.19701869225528,-70.0748895689729,
12.));
#68784=CARTESIAN_POINT('Ctrl Pts',(-5.1930090327158,-70.0946816270997,0.));
#68785=CARTESIAN_POINT('Ctrl Pts',(-5.1930090327158,-70.0946816270997,12.));
#68786=CARTESIAN_POINT('Ctrl Pts',(-5.18896792486565,-70.1145206891885,
0.));
#68787=CARTESIAN_POINT('Ctrl Pts',(-5.18896792486565,-70.1145206891885,
12.));
#68788=CARTESIAN_POINT('Ctrl Pts',(-5.18489531966265,-70.1344065558145,
0.));
#68789=CARTESIAN_POINT('Ctrl Pts',(-5.18489531966265,-70.1344065558145,
12.));
#68790=CARTESIAN_POINT('Ctrl Pts',(-5.18079116757666,-70.1543390243892,
0.));
#68791=CARTESIAN_POINT('Ctrl Pts',(-5.18079116757666,-70.1543390243892,
12.));
#68792=CARTESIAN_POINT('Ctrl Pts',(-5.17665541952383,-70.1743178937077,
0.));
#68793=CARTESIAN_POINT('Ctrl Pts',(-5.17665541952383,-70.1743178937077,
12.));
#68794=CARTESIAN_POINT('Ctrl Pts',(-5.17248802793389,-70.1943429691167,
0.));
#68795=CARTESIAN_POINT('Ctrl Pts',(-5.17248802793389,-70.1943429691167,
12.));
#68796=CARTESIAN_POINT('Ctrl Pts',(-5.16828894670108,-70.2144140622953,
0.));
#68797=CARTESIAN_POINT('Ctrl Pts',(-5.16828894670108,-70.2144140622953,
12.));
#68798=CARTESIAN_POINT('Ctrl Pts',(-5.16405813066976,-70.2345309887833,
0.));
#68799=CARTESIAN_POINT('Ctrl Pts',(-5.16405813066976,-70.2345309887833,
12.));
#68800=CARTESIAN_POINT('Ctrl Pts',(-5.15979553528203,-70.2546935662722,
0.));
#68801=CARTESIAN_POINT('Ctrl Pts',(-5.15979553528203,-70.2546935662722,
12.));
#68802=CARTESIAN_POINT('Ctrl Pts',(-5.15550111614859,-70.2749016125105,
0.));
#68803=CARTESIAN_POINT('Ctrl Pts',(-5.15550111614859,-70.2749016125105,
12.));
#68804=CARTESIAN_POINT('Ctrl Pts',(-5.15117482869254,-70.2951549435512,
0.));
#68805=CARTESIAN_POINT('Ctrl Pts',(-5.15117482869254,-70.2951549435512,
12.));
#68806=CARTESIAN_POINT('Ctrl Pts',(-5.1468166283308,-70.3154533746736,0.));
#68807=CARTESIAN_POINT('Ctrl Pts',(-5.1468166283308,-70.3154533746736,12.));
#68808=CARTESIAN_POINT('Ctrl Pts',(-5.14242647063479,-70.3357967211796,
0.));
#68809=CARTESIAN_POINT('Ctrl Pts',(-5.14242647063479,-70.3357967211796,
12.));
#68810=CARTESIAN_POINT('Ctrl Pts',(-5.13800431148904,-70.3561847991714,
0.));
#68811=CARTESIAN_POINT('Ctrl Pts',(-5.13800431148904,-70.3561847991714,
12.));
#68812=CARTESIAN_POINT('Ctrl Pts',(-5.13355010728567,-70.3766174264757,
0.));
#68813=CARTESIAN_POINT('Ctrl Pts',(-5.13355010728567,-70.3766174264757,
12.));
#68814=CARTESIAN_POINT('Ctrl Pts',(-5.12906381499456,-70.3970944229851,
0.));
#68815=CARTESIAN_POINT('Ctrl Pts',(-5.12906381499456,-70.3970944229851,
12.));
#68816=CARTESIAN_POINT('Ctrl Pts',(-5.12454539205328,-70.417615610161,0.));
#68817=CARTESIAN_POINT('Ctrl Pts',(-5.12454539205328,-70.417615610161,12.));
#68818=CARTESIAN_POINT('Ctrl Pts',(-5.11999479630212,-70.4381808107245,
0.));
#68819=CARTESIAN_POINT('Ctrl Pts',(-5.11999479630212,-70.4381808107245,
12.));
#68820=CARTESIAN_POINT('Ctrl Pts',(-5.11541198590932,-70.458789848296,0.));
#68821=CARTESIAN_POINT('Ctrl Pts',(-5.11541198590932,-70.458789848296,12.));
#68822=CARTESIAN_POINT('Ctrl Pts',(-5.11079691929213,-70.4794425469825,
0.));
#68823=CARTESIAN_POINT('Ctrl Pts',(-5.11079691929213,-70.4794425469825,
12.));
#68824=CARTESIAN_POINT('Ctrl Pts',(-5.10614955511664,-70.500138731399,0.));
#68825=CARTESIAN_POINT('Ctrl Pts',(-5.10614955511664,-70.500138731399,12.));
#68826=CARTESIAN_POINT('Ctrl Pts',(-5.10146985232941,-70.5208782268497,
0.));
#68827=CARTESIAN_POINT('Ctrl Pts',(-5.10146985232941,-70.5208782268497,
12.));
#68828=CARTESIAN_POINT('Ctrl Pts',(-5.09675777018183,-70.5416608594526,
0.));
#68829=CARTESIAN_POINT('Ctrl Pts',(-5.09675777018183,-70.5416608594526,
12.));
#68830=CARTESIAN_POINT('Ctrl Pts',(-5.09201326826134,-70.5624864562824,
0.));
#68831=CARTESIAN_POINT('Ctrl Pts',(-5.09201326826134,-70.5624864562824,
12.));
#68832=CARTESIAN_POINT('Ctrl Pts',(-5.08723630652273,-70.5833548455014,
0.));
#68833=CARTESIAN_POINT('Ctrl Pts',(-5.08723630652273,-70.5833548455014,
12.));
#68834=CARTESIAN_POINT('Ctrl Pts',(-5.08242684526687,-70.6042658562923,
0.));
#68835=CARTESIAN_POINT('Ctrl Pts',(-5.08242684526687,-70.6042658562923,
12.));
#68836=CARTESIAN_POINT('Ctrl Pts',(-5.07758484512302,-70.6252193187878,
0.));
#68837=CARTESIAN_POINT('Ctrl Pts',(-5.07758484512302,-70.6252193187878,
12.));
#68838=CARTESIAN_POINT('Ctrl Pts',(-5.07271026703355,-70.6462150640015,
0.));
#68839=CARTESIAN_POINT('Ctrl Pts',(-5.07271026703355,-70.6462150640015,
12.));
#68840=CARTESIAN_POINT('Ctrl Pts',(-5.06780307224072,-70.6672529237455,
0.));
#68841=CARTESIAN_POINT('Ctrl Pts',(-5.06780307224072,-70.6672529237455,
12.));
#68842=CARTESIAN_POINT('Ctrl Pts',(-5.0628632222782,-70.6883327305784,0.));
#68843=CARTESIAN_POINT('Ctrl Pts',(-5.0628632222782,-70.6883327305784,12.));
#68844=CARTESIAN_POINT('Ctrl Pts',(-5.05789067897057,-70.7094543178438,
0.));
#68845=CARTESIAN_POINT('Ctrl Pts',(-5.05789067897057,-70.7094543178438,
12.));
#68846=CARTESIAN_POINT('Ctrl Pts',(-5.05288540443482,-70.7306175196863,
0.));
#68847=CARTESIAN_POINT('Ctrl Pts',(-5.05288540443482,-70.7306175196863,
12.));
#68848=CARTESIAN_POINT('Ctrl Pts',(-5.04784736108346,-70.7518221710706,
0.));
#68849=CARTESIAN_POINT('Ctrl Pts',(-5.04784736108346,-70.7518221710706,
12.));
#68850=CARTESIAN_POINT('Ctrl Pts',(-5.0427765116335,-70.7730681077983,0.));
#68851=CARTESIAN_POINT('Ctrl Pts',(-5.0427765116335,-70.7730681077983,12.));
#68852=CARTESIAN_POINT('Ctrl Pts',(-5.03767281910479,-70.7943551665059,
0.));
#68853=CARTESIAN_POINT('Ctrl Pts',(-5.03767281910479,-70.7943551665059,
12.));
#68854=CARTESIAN_POINT('Ctrl Pts',(-5.03253624680941,-70.8156831846488,
0.));
#68855=CARTESIAN_POINT('Ctrl Pts',(-5.03253624680941,-70.8156831846488,
12.));
#68856=CARTESIAN_POINT('Ctrl Pts',(-5.02736675834693,-70.8370520004843,
0.));
#68857=CARTESIAN_POINT('Ctrl Pts',(-5.02736675834693,-70.8370520004843,
12.));
#68858=CARTESIAN_POINT('Ctrl Pts',(-5.02216431760061,-70.8584614530519,
0.));
#68859=CARTESIAN_POINT('Ctrl Pts',(-5.02216431760061,-70.8584614530519,
12.));
#68860=CARTESIAN_POINT('Ctrl Pts',(-5.0169288887379,-70.8799113821452,0.));
#68861=CARTESIAN_POINT('Ctrl Pts',(-5.0169288887379,-70.8799113821452,12.));
#68862=CARTESIAN_POINT('Ctrl Pts',(-5.01166043620568,-70.9014016283124,
0.));
#68863=CARTESIAN_POINT('Ctrl Pts',(-5.01166043620568,-70.9014016283124,
12.));
#68864=CARTESIAN_POINT('Ctrl Pts',(-5.00635892472513,-70.9229320328589,
0.));
#68865=CARTESIAN_POINT('Ctrl Pts',(-5.00635892472513,-70.9229320328589,
12.));
#68866=CARTESIAN_POINT('Ctrl Pts',(-5.00102431929039,-70.9445024378439,
0.));
#68867=CARTESIAN_POINT('Ctrl Pts',(-5.00102431929039,-70.9445024378439,
12.));
#68868=CARTESIAN_POINT('Ctrl Pts',(-4.99565658516913,-70.9661126860773,
0.));
#68869=CARTESIAN_POINT('Ctrl Pts',(-4.99565658516913,-70.9661126860773,
12.));
#68870=CARTESIAN_POINT('Ctrl Pts',(-4.99025568790664,-70.9877626211113,
0.));
#68871=CARTESIAN_POINT('Ctrl Pts',(-4.99025568790664,-70.9877626211113,
12.));
#68872=CARTESIAN_POINT('Ctrl Pts',(-4.98482159331863,-71.0094520872377,
0.));
#68873=CARTESIAN_POINT('Ctrl Pts',(-4.98482159331863,-71.0094520872377,
12.));
#68874=CARTESIAN_POINT('Ctrl Pts',(-4.97935426748585,-71.0311809294821,
0.));
#68875=CARTESIAN_POINT('Ctrl Pts',(-4.97935426748585,-71.0311809294821,
12.));
#68876=CARTESIAN_POINT('Ctrl Pts',(-4.97385367675159,-71.0529489935961,
0.));
#68877=CARTESIAN_POINT('Ctrl Pts',(-4.97385367675159,-71.0529489935961,
12.));
#68878=CARTESIAN_POINT('Ctrl Pts',(-4.96831978772191,-71.0747561260436,
0.));
#68879=CARTESIAN_POINT('Ctrl Pts',(-4.96831978772191,-71.0747561260436,
12.));
#68880=CARTESIAN_POINT('Ctrl Pts',(-4.96275256726766,-71.0966021739907,
0.));
#68881=CARTESIAN_POINT('Ctrl Pts',(-4.96275256726766,-71.0966021739907,
12.));
#68882=CARTESIAN_POINT('Ctrl Pts',(-4.95715198251685,-71.1184869853056,
0.));
#68883=CARTESIAN_POINT('Ctrl Pts',(-4.95715198251685,-71.1184869853056,
12.));
#68884=CARTESIAN_POINT('Ctrl Pts',(-4.95151800085101,-71.1404104085552,
0.));
#68885=CARTESIAN_POINT('Ctrl Pts',(-4.95151800085101,-71.1404104085552,
12.));
#68886=CARTESIAN_POINT('Ctrl Pts',(-4.94585058990341,-71.1623722930001,
0.));
#68887=CARTESIAN_POINT('Ctrl Pts',(-4.94585058990341,-71.1623722930001,
12.));
#68888=CARTESIAN_POINT('Ctrl Pts',(-4.94014971756115,-71.1843724885847,
0.));
#68889=CARTESIAN_POINT('Ctrl Pts',(-4.94014971756115,-71.1843724885847,
12.));
#68890=CARTESIAN_POINT('Ctrl Pts',(-4.93441535196617,-71.2064108459286,
0.));
#68891=CARTESIAN_POINT('Ctrl Pts',(-4.93441535196617,-71.2064108459286,
12.));
#68892=CARTESIAN_POINT('Ctrl Pts',(-4.92864746150732,-71.2284872163273,
0.));
#68893=CARTESIAN_POINT('Ctrl Pts',(-4.92864746150732,-71.2284872163273,
12.));
#68894=CARTESIAN_POINT('Ctrl Pts',(-4.92284601481721,-71.250601451747,0.));
#68895=CARTESIAN_POINT('Ctrl Pts',(-4.92284601481721,-71.250601451747,12.));
#68896=CARTESIAN_POINT('Ctrl Pts',(-4.91701098077036,-71.2727534048192,
0.));
#68897=CARTESIAN_POINT('Ctrl Pts',(-4.91701098077036,-71.2727534048192,
12.));
#68898=CARTESIAN_POINT('Ctrl Pts',(-4.91114232848603,-71.294942928829,0.));
#68899=CARTESIAN_POINT('Ctrl Pts',(-4.91114232848603,-71.294942928829,12.));
#68900=CARTESIAN_POINT('Ctrl Pts',(-4.90524002732779,-71.3171698777084,
0.));
#68901=CARTESIAN_POINT('Ctrl Pts',(-4.90524002732779,-71.3171698777084,
12.));
#68902=CARTESIAN_POINT('Ctrl Pts',(-4.89930404689575,-71.3394341060359,
0.));
#68903=CARTESIAN_POINT('Ctrl Pts',(-4.89930404689575,-71.3394341060359,
12.));
#68904=CARTESIAN_POINT('Ctrl Pts',(-4.89333435702414,-71.3617354690325,
0.));
#68905=CARTESIAN_POINT('Ctrl Pts',(-4.89333435702414,-71.3617354690325,
12.));
#68906=CARTESIAN_POINT('Ctrl Pts',(-4.88733092777975,-71.3840738225562,
0.));
#68907=CARTESIAN_POINT('Ctrl Pts',(-4.88733092777975,-71.3840738225562,
12.));
#68908=CARTESIAN_POINT('Ctrl Pts',(-4.88129372946551,-71.4064490230899,
0.));
#68909=CARTESIAN_POINT('Ctrl Pts',(-4.88129372946551,-71.4064490230899,
12.));
#68910=CARTESIAN_POINT('Ctrl Pts',(-4.87522273261908,-71.4288609277374,
0.));
#68911=CARTESIAN_POINT('Ctrl Pts',(-4.87522273261908,-71.4288609277374,
12.));
#68912=CARTESIAN_POINT('Ctrl Pts',(-4.8691179080055,-71.4513093942255,0.));
#68913=CARTESIAN_POINT('Ctrl Pts',(-4.8691179080055,-71.4513093942255,12.));
#68914=CARTESIAN_POINT('Ctrl Pts',(-4.86297922661503,-71.4737942808982,
0.));
#68915=CARTESIAN_POINT('Ctrl Pts',(-4.86297922661503,-71.4737942808982,
12.));
#68916=CARTESIAN_POINT('Ctrl Pts',(-4.8568066596618,-71.4963154467113,0.));
#68917=CARTESIAN_POINT('Ctrl Pts',(-4.8568066596618,-71.4963154467113,12.));
#68918=CARTESIAN_POINT('Ctrl Pts',(-4.8506001785878,-71.5188727512197,0.));
#68919=CARTESIAN_POINT('Ctrl Pts',(-4.8506001785878,-71.5188727512197,12.));
#68920=CARTESIAN_POINT('Ctrl Pts',(-4.84435975506048,-71.5414660545739,
0.));
#68921=CARTESIAN_POINT('Ctrl Pts',(-4.84435975506048,-71.5414660545739,
12.));
#68922=CARTESIAN_POINT('Ctrl Pts',(-4.83808536096583,-71.564095217521,0.));
#68923=CARTESIAN_POINT('Ctrl Pts',(-4.83808536096583,-71.564095217521,12.));
#68924=CARTESIAN_POINT('Ctrl Pts',(-4.83177696840637,-71.5867601014,0.));
#68925=CARTESIAN_POINT('Ctrl Pts',(-4.83177696840637,-71.5867601014,12.));
#68926=CARTESIAN_POINT('Ctrl Pts',(-4.82543454970027,-71.6094605681366,
0.));
#68927=CARTESIAN_POINT('Ctrl Pts',(-4.82543454970027,-71.6094605681366,
12.));
#68928=CARTESIAN_POINT('Ctrl Pts',(-4.81905807738557,-71.6321964802326,
0.));
#68929=CARTESIAN_POINT('Ctrl Pts',(-4.81905807738557,-71.6321964802326,
12.));
#68930=CARTESIAN_POINT('Ctrl Pts',(-4.81264752421732,-71.6549677007613,
0.));
#68931=CARTESIAN_POINT('Ctrl Pts',(-4.81264752421732,-71.6549677007613,
12.));
#68932=CARTESIAN_POINT('Ctrl Pts',(-4.80620286316088,-71.6777740933705,
0.));
#68933=CARTESIAN_POINT('Ctrl Pts',(-4.80620286316088,-71.6777740933705,
12.));
#68934=CARTESIAN_POINT('Ctrl Pts',(-4.79972406739014,-71.7006155222766,
0.));
#68935=CARTESIAN_POINT('Ctrl Pts',(-4.79972406739014,-71.7006155222766,
12.));
#68936=CARTESIAN_POINT('Ctrl Pts',(-4.79321111028672,-71.7234918522604,
0.));
#68937=CARTESIAN_POINT('Ctrl Pts',(-4.79321111028672,-71.7234918522604,
12.));
#68938=CARTESIAN_POINT('Ctrl Pts',(-4.7866639654445,-71.7464029486552,0.));
#68939=CARTESIAN_POINT('Ctrl Pts',(-4.7866639654445,-71.7464029486552,12.));
#68940=CARTESIAN_POINT('Ctrl Pts',(-4.78008260666642,-71.7693486773449,
0.));
#68941=CARTESIAN_POINT('Ctrl Pts',(-4.78008260666642,-71.7693486773449,
12.));
#68942=CARTESIAN_POINT('Ctrl Pts',(-4.77346700795787,-71.7923289047636,
0.));
#68943=CARTESIAN_POINT('Ctrl Pts',(-4.77346700795787,-71.7923289047636,
12.));
#68944=CARTESIAN_POINT('Ctrl Pts',(-4.76681714352503,-71.8153434978924,
0.));
#68945=CARTESIAN_POINT('Ctrl Pts',(-4.76681714352503,-71.8153434978924,
12.));
#68946=CARTESIAN_POINT('Ctrl Pts',(-4.76013298777422,-71.8383923242533,
0.));
#68947=CARTESIAN_POINT('Ctrl Pts',(-4.76013298777422,-71.8383923242533,
12.));
#68948=CARTESIAN_POINT('Ctrl Pts',(-4.75341451531671,-71.8614752519008,
0.));
#68949=CARTESIAN_POINT('Ctrl Pts',(-4.75341451531671,-71.8614752519008,
12.));
#68950=CARTESIAN_POINT('Ctrl Pts',(-4.74666170096545,-71.8845921494186,
0.));
#68951=CARTESIAN_POINT('Ctrl Pts',(-4.74666170096545,-71.8845921494186,
12.));
#68952=CARTESIAN_POINT('Ctrl Pts',(-4.7398745197286,-71.9077428859207,0.));
#68953=CARTESIAN_POINT('Ctrl Pts',(-4.7398745197286,-71.9077428859207,12.));
#68954=CARTESIAN_POINT('Ctrl Pts',(-4.73305294680784,-71.9309273310469,
0.));
#68955=CARTESIAN_POINT('Ctrl Pts',(-4.73305294680784,-71.9309273310469,
12.));
#68956=CARTESIAN_POINT('Ctrl Pts',(-4.72619695759778,-71.9541453549582,
0.));
#68957=CARTESIAN_POINT('Ctrl Pts',(-4.72619695759778,-71.9541453549582,
12.));
#68958=CARTESIAN_POINT('Ctrl Pts',(-4.7193065276908,-71.9773968283267,0.));
#68959=CARTESIAN_POINT('Ctrl Pts',(-4.7193065276908,-71.9773968283267,12.));
#68960=CARTESIAN_POINT('Ctrl Pts',(-4.7123816328741,-72.0006816223335,0.));
#68961=CARTESIAN_POINT('Ctrl Pts',(-4.7123816328741,-72.0006816223335,12.));
#68962=CARTESIAN_POINT('Ctrl Pts',(-4.70542224912312,-72.0239996086694,
0.));
#68963=CARTESIAN_POINT('Ctrl Pts',(-4.70542224912312,-72.0239996086694,
12.));
#68964=CARTESIAN_POINT('Ctrl Pts',(-4.69842835259997,-72.047350659532,0.));
#68965=CARTESIAN_POINT('Ctrl Pts',(-4.69842835259997,-72.047350659532,12.));
#68966=CARTESIAN_POINT('Ctrl Pts',(-4.6913999196528,-72.070734647621,0.));
#68967=CARTESIAN_POINT('Ctrl Pts',(-4.6913999196528,-72.070734647621,12.));
#68968=CARTESIAN_POINT('Ctrl Pts',(-4.6843369268206,-72.0941514461283,0.));
#68969=CARTESIAN_POINT('Ctrl Pts',(-4.6843369268206,-72.0941514461283,12.));
#68970=CARTESIAN_POINT('Ctrl Pts',(-4.67723935083087,-72.1176009287349,
0.));
#68971=CARTESIAN_POINT('Ctrl Pts',(-4.67723935083087,-72.1176009287349,
12.));
#68972=CARTESIAN_POINT('Ctrl Pts',(-4.67010716859281,-72.1410829696129,
0.));
#68973=CARTESIAN_POINT('Ctrl Pts',(-4.67010716859281,-72.1410829696129,
12.));
#68974=CARTESIAN_POINT('Ctrl Pts',(-4.6629403571957,-72.1645974434218,0.));
#68975=CARTESIAN_POINT('Ctrl Pts',(-4.6629403571957,-72.1645974434218,12.));
#68976=CARTESIAN_POINT('Ctrl Pts',(-4.65573889390824,-72.1881442253052,
0.));
#68977=CARTESIAN_POINT('Ctrl Pts',(-4.65573889390824,-72.1881442253052,
12.));
#68978=CARTESIAN_POINT('Ctrl Pts',(-4.64850275618325,-72.2117231908816,
0.));
#68979=CARTESIAN_POINT('Ctrl Pts',(-4.64850275618325,-72.2117231908816,
12.));
#68980=CARTESIAN_POINT('Ctrl Pts',(-4.64123192165627,-72.2353342162408,
0.));
#68981=CARTESIAN_POINT('Ctrl Pts',(-4.64123192165627,-72.2353342162408,
12.));
#68982=CARTESIAN_POINT('Ctrl Pts',(-4.63392636813842,-72.2589771779447,
0.));
#68983=CARTESIAN_POINT('Ctrl Pts',(-4.63392636813842,-72.2589771779447,
12.));
#68984=CARTESIAN_POINT('Ctrl Pts',(-4.62658607361465,-72.2826519530254,
0.));
#68985=CARTESIAN_POINT('Ctrl Pts',(-4.62658607361465,-72.2826519530254,
12.));
#68986=CARTESIAN_POINT('Ctrl Pts',(-4.61921101624294,-72.306358418981,0.));
#68987=CARTESIAN_POINT('Ctrl Pts',(-4.61921101624294,-72.306358418981,12.));
#68988=CARTESIAN_POINT('Ctrl Pts',(-4.61180117435868,-72.330096453767,0.));
#68989=CARTESIAN_POINT('Ctrl Pts',(-4.61180117435868,-72.330096453767,12.));
#68990=CARTESIAN_POINT('Ctrl Pts',(-4.60435652647463,-72.3538659357932,
0.));
#68991=CARTESIAN_POINT('Ctrl Pts',(-4.60435652647463,-72.3538659357932,
12.));
#68992=CARTESIAN_POINT('Ctrl Pts',(-4.5968770512734,-72.3776667439244,0.));
#68993=CARTESIAN_POINT('Ctrl Pts',(-4.5968770512734,-72.3776667439244,12.));
#68994=CARTESIAN_POINT('Ctrl Pts',(-4.58936272760551,-72.4014987574789,
0.));
#68995=CARTESIAN_POINT('Ctrl Pts',(-4.58936272760551,-72.4014987574789,
12.));
#68996=CARTESIAN_POINT('Ctrl Pts',(-4.58181353448851,-72.4253618562249,
0.));
#68997=CARTESIAN_POINT('Ctrl Pts',(-4.58181353448851,-72.4253618562249,
12.));
#68998=CARTESIAN_POINT('Ctrl Pts',(-4.57422945111094,-72.449255920373,0.));
#68999=CARTESIAN_POINT('Ctrl Pts',(-4.57422945111094,-72.449255920373,12.));
#69000=CARTESIAN_POINT('Ctrl Pts',(-4.56661045683366,-72.473180830571,0.));
#69001=CARTESIAN_POINT('Ctrl Pts',(-4.56661045683366,-72.473180830571,12.));
#69002=CARTESIAN_POINT('Ctrl Pts',(-4.55895653118213,-72.4971364679055,
0.));
#69003=CARTESIAN_POINT('Ctrl Pts',(-4.55895653118213,-72.4971364679055,
12.));
#69004=CARTESIAN_POINT('Ctrl Pts',(-4.55126765384403,-72.5211227138997,
0.));
#69005=CARTESIAN_POINT('Ctrl Pts',(-4.55126765384403,-72.5211227138997,
12.));
#69006=CARTESIAN_POINT('Ctrl Pts',(-4.54354380466825,-72.5451394505106,
0.));
#69007=CARTESIAN_POINT('Ctrl Pts',(-4.54354380466825,-72.5451394505106,
12.));
#69008=CARTESIAN_POINT('Ctrl Pts',(-4.53578496366802,-72.5691865601225,
0.));
#69009=CARTESIAN_POINT('Ctrl Pts',(-4.53578496366802,-72.5691865601225,
12.));
#69010=CARTESIAN_POINT('Ctrl Pts',(-4.5279911110239,-72.5932639255406,0.));
#69011=CARTESIAN_POINT('Ctrl Pts',(-4.5279911110239,-72.5932639255406,12.));
#69012=CARTESIAN_POINT('Ctrl Pts',(-4.52016222707632,-72.6173714299935,
0.));
#69013=CARTESIAN_POINT('Ctrl Pts',(-4.52016222707632,-72.6173714299935,
12.));
#69014=CARTESIAN_POINT('Ctrl Pts',(-4.5122982923226,-72.6415089571314,0.));
#69015=CARTESIAN_POINT('Ctrl Pts',(-4.5122982923226,-72.6415089571314,12.));
#69016=CARTESIAN_POINT('Ctrl Pts',(-4.50439928741605,-72.6656763910241,
0.));
#69017=CARTESIAN_POINT('Ctrl Pts',(-4.50439928741605,-72.6656763910241,
12.));
#69018=CARTESIAN_POINT('Ctrl Pts',(-4.49646519316822,-72.689873616155,0.));
#69019=CARTESIAN_POINT('Ctrl Pts',(-4.49646519316822,-72.689873616155,12.));
#69020=CARTESIAN_POINT('Ctrl Pts',(-4.48849599055354,-72.7141005174153,
0.));
#69021=CARTESIAN_POINT('Ctrl Pts',(-4.48849599055354,-72.7141005174153,
12.));
#69022=CARTESIAN_POINT('Ctrl Pts',(-4.48049166070223,-72.7383569801042,
0.));
#69023=CARTESIAN_POINT('Ctrl Pts',(-4.48049166070223,-72.7383569801042,
12.));
#69024=CARTESIAN_POINT('Ctrl Pts',(-4.47245218489623,-72.7626428899287,
0.));
#69025=CARTESIAN_POINT('Ctrl Pts',(-4.47245218489623,-72.7626428899287,
12.));
#69026=CARTESIAN_POINT('Ctrl Pts',(-4.46437754456795,-72.7869581329994,
0.));
#69027=CARTESIAN_POINT('Ctrl Pts',(-4.46437754456795,-72.7869581329994,
12.));
#69028=CARTESIAN_POINT('Ctrl Pts',(-4.45626772130138,-72.8113025958258,
0.));
#69029=CARTESIAN_POINT('Ctrl Pts',(-4.45626772130138,-72.8113025958258,
12.));
#69030=CARTESIAN_POINT('Ctrl Pts',(-4.44812269683724,-72.8356761653064,
0.));
#69031=CARTESIAN_POINT('Ctrl Pts',(-4.44812269683724,-72.8356761653064,
12.));
#69032=CARTESIAN_POINT('Ctrl Pts',(-4.43994245306805,-72.8600787287316,
0.));
#69033=CARTESIAN_POINT('Ctrl Pts',(-4.43994245306805,-72.8600787287316,
12.));
#69034=CARTESIAN_POINT('Ctrl Pts',(-4.43172697203341,-72.8845101737856,
0.));
#69035=CARTESIAN_POINT('Ctrl Pts',(-4.43172697203341,-72.8845101737856,
12.));
#69036=CARTESIAN_POINT('Ctrl Pts',(-4.42347623591941,-72.9089703885463,
0.));
#69037=CARTESIAN_POINT('Ctrl Pts',(-4.42347623591941,-72.9089703885463,
12.));
#69038=CARTESIAN_POINT('Ctrl Pts',(-4.41519022705926,-72.9334592614828,
0.));
#69039=CARTESIAN_POINT('Ctrl Pts',(-4.41519022705926,-72.9334592614828,
12.));
#69040=CARTESIAN_POINT('Ctrl Pts',(-4.40686892793965,-72.9579766814495,
0.));
#69041=CARTESIAN_POINT('Ctrl Pts',(-4.40686892793965,-72.9579766814495,
12.));
#69042=CARTESIAN_POINT('Ctrl Pts',(-4.3985123211973,-72.9825225376839,0.));
#69043=CARTESIAN_POINT('Ctrl Pts',(-4.3985123211973,-72.9825225376839,12.));
#69044=CARTESIAN_POINT('Ctrl Pts',(-4.39012038961145,-73.0070967198033,
0.));
#69045=CARTESIAN_POINT('Ctrl Pts',(-4.39012038961145,-73.0070967198033,
12.));
#69046=CARTESIAN_POINT('Ctrl Pts',(-4.38169311610153,-73.031699117799,0.));
#69047=CARTESIAN_POINT('Ctrl Pts',(-4.38169311610153,-73.031699117799,12.));
#69048=CARTESIAN_POINT('Ctrl Pts',(-4.37323048372607,-73.0563296220301,
0.));
#69049=CARTESIAN_POINT('Ctrl Pts',(-4.37323048372607,-73.0563296220301,
12.));
#69050=CARTESIAN_POINT('Ctrl Pts',(-4.36473247568638,-73.0809881232111,
0.));
#69051=CARTESIAN_POINT('Ctrl Pts',(-4.36473247568638,-73.0809881232111,
12.));
#69052=CARTESIAN_POINT('Ctrl Pts',(-4.35619907532716,-73.1056745124099,
0.));
#69053=CARTESIAN_POINT('Ctrl Pts',(-4.35619907532716,-73.1056745124099,
12.));
#69054=CARTESIAN_POINT('Ctrl Pts',(-4.34763026613154,-73.1303886810602,
0.));
#69055=CARTESIAN_POINT('Ctrl Pts',(-4.34763026613154,-73.1303886810602,
12.));
#69056=CARTESIAN_POINT('Ctrl Pts',(-4.33902603172139,-73.1551305209692,
0.));
#69057=CARTESIAN_POINT('Ctrl Pts',(-4.33902603172139,-73.1551305209692,
12.));
#69058=CARTESIAN_POINT('Ctrl Pts',(-4.33038635585878,-73.1798999243234,
0.));
#69059=CARTESIAN_POINT('Ctrl Pts',(-4.33038635585878,-73.1798999243234,
12.));
#69060=CARTESIAN_POINT('Ctrl Pts',(-4.32171122245218,-73.204696783693,0.));
#69061=CARTESIAN_POINT('Ctrl Pts',(-4.32171122245218,-73.204696783693,12.));
#69062=CARTESIAN_POINT('Ctrl Pts',(-4.31300061556103,-73.2295209920319,
0.));
#69063=CARTESIAN_POINT('Ctrl Pts',(-4.31300061556103,-73.2295209920319,
12.));
#69064=CARTESIAN_POINT('Ctrl Pts',(-4.30425451938234,-73.2543724426562,
0.));
#69065=CARTESIAN_POINT('Ctrl Pts',(-4.30425451938234,-73.2543724426562,
12.));
#69066=CARTESIAN_POINT('Ctrl Pts',(-4.29547291824289,-73.2792510292243,
0.));
#69067=CARTESIAN_POINT('Ctrl Pts',(-4.29547291824289,-73.2792510292243,
12.));
#69068=CARTESIAN_POINT('Ctrl Pts',(-4.28665579659302,-73.3041566457134,
0.));
#69069=CARTESIAN_POINT('Ctrl Pts',(-4.28665579659302,-73.3041566457134,
12.));
#69070=CARTESIAN_POINT('Ctrl Pts',(-4.27780313900392,-73.3290891863959,
0.));
#69071=CARTESIAN_POINT('Ctrl Pts',(-4.27780313900392,-73.3290891863959,
12.));
#69072=CARTESIAN_POINT('Ctrl Pts',(-4.26891493016703,-73.354048545808,0.));
#69073=CARTESIAN_POINT('Ctrl Pts',(-4.26891493016703,-73.354048545808,12.));
#69074=CARTESIAN_POINT('Ctrl Pts',(-4.25999115489904,-73.3790346187953,
0.));
#69075=CARTESIAN_POINT('Ctrl Pts',(-4.25999115489904,-73.3790346187953,
12.));
#69076=CARTESIAN_POINT('Ctrl Pts',(-4.25103179814892,-73.4040473005603,
0.));
#69077=CARTESIAN_POINT('Ctrl Pts',(-4.25103179814892,-73.4040473005603,
12.));
#69078=CARTESIAN_POINT('Ctrl Pts',(-4.24203684500941,-73.4290864867103,
0.));
#69079=CARTESIAN_POINT('Ctrl Pts',(-4.24203684500941,-73.4290864867103,
12.));
#69080=CARTESIAN_POINT('Ctrl Pts',(-4.23300628072757,-73.4541520732943,
0.));
#69081=CARTESIAN_POINT('Ctrl Pts',(-4.23300628072757,-73.4541520732943,
12.));
#69082=CARTESIAN_POINT('Ctrl Pts',(-4.22394009072753,-73.4792439568624,
0.));
#69083=CARTESIAN_POINT('Ctrl Pts',(-4.22394009072753,-73.4792439568624,
12.));
#69084=CARTESIAN_POINT('Ctrl Pts',(-4.21483826059436,-73.5043620344107,
0.));
#69085=CARTESIAN_POINT('Ctrl Pts',(-4.21483826059436,-73.5043620344107,
12.));
#69086=CARTESIAN_POINT('Ctrl Pts',(-4.20570077603727,-73.5295062032621,
0.));
#69087=CARTESIAN_POINT('Ctrl Pts',(-4.20570077603727,-73.5295062032621,
12.));
#69088=CARTESIAN_POINT('Ctrl Pts',(-4.19652762286126,-73.554676360957,0.));
#69089=CARTESIAN_POINT('Ctrl Pts',(-4.19652762286126,-73.554676360957,12.));
#69090=CARTESIAN_POINT('Ctrl Pts',(-4.18731878694238,-73.5798724051519,
0.));
#69091=CARTESIAN_POINT('Ctrl Pts',(-4.18731878694238,-73.5798724051519,
12.));
#69092=CARTESIAN_POINT('Ctrl Pts',(-4.17807425419816,-73.6050942334773,
0.));
#69093=CARTESIAN_POINT('Ctrl Pts',(-4.17807425419816,-73.6050942334773,
12.));
#69094=CARTESIAN_POINT('Ctrl Pts',(-4.16879401058786,-73.6303417435262,
0.));
#69095=CARTESIAN_POINT('Ctrl Pts',(-4.16879401058786,-73.6303417435262,
12.));
#69096=CARTESIAN_POINT('Ctrl Pts',(-4.1594780421779,-73.6556148331504,0.));
#69097=CARTESIAN_POINT('Ctrl Pts',(-4.1594780421779,-73.6556148331504,12.));
#69098=CARTESIAN_POINT('Ctrl Pts',(-4.15012633519728,-73.6809134006909,
0.));
#69099=CARTESIAN_POINT('Ctrl Pts',(-4.15012633519728,-73.6809134006909,
12.));
#69100=CARTESIAN_POINT('Ctrl Pts',(-4.14073887610155,-73.7062373452344,
0.));
#69101=CARTESIAN_POINT('Ctrl Pts',(-4.14073887610155,-73.7062373452344,
12.));
#69102=CARTESIAN_POINT('Ctrl Pts',(-4.13131565163575,-73.7315865668508,
0.));
#69103=CARTESIAN_POINT('Ctrl Pts',(-4.13131565163575,-73.7315865668508,
12.));
#69104=CARTESIAN_POINT('Ctrl Pts',(-4.12185664890551,-73.7569609668501,
0.));
#69105=CARTESIAN_POINT('Ctrl Pts',(-4.12185664890551,-73.7569609668501,
12.));
#69106=CARTESIAN_POINT('Ctrl Pts',(-4.1123618552278,-73.7823604472126,0.));
#69107=CARTESIAN_POINT('Ctrl Pts',(-4.1123618552278,-73.7823604472126,12.));
#69108=CARTESIAN_POINT('Ctrl Pts',(-4.10283125798724,-73.8077849100314,
0.));
#69109=CARTESIAN_POINT('Ctrl Pts',(-4.10283125798724,-73.8077849100314,
12.));
#69110=CARTESIAN_POINT('Ctrl Pts',(-4.09326484448231,-73.8332342568978,
0.));
#69111=CARTESIAN_POINT('Ctrl Pts',(-4.09326484448231,-73.8332342568978,
12.));
#69112=CARTESIAN_POINT('Ctrl Pts',(-4.08366260180679,-73.8587083884208,
0.));
#69113=CARTESIAN_POINT('Ctrl Pts',(-4.08366260180679,-73.8587083884208,
12.));
#69114=CARTESIAN_POINT('Ctrl Pts',(-4.07402451665253,-73.884207203405,0.));
#69115=CARTESIAN_POINT('Ctrl Pts',(-4.07402451665253,-73.884207203405,12.));
#69116=CARTESIAN_POINT('Ctrl Pts',(-4.06435057547335,-73.9097305995173,
0.));
#69117=CARTESIAN_POINT('Ctrl Pts',(-4.06435057547335,-73.9097305995173,
12.));
#69118=CARTESIAN_POINT('Ctrl Pts',(-4.05464076484761,-73.9352784747665,
0.));
#69119=CARTESIAN_POINT('Ctrl Pts',(-4.05464076484761,-73.9352784747665,
12.));
#69120=CARTESIAN_POINT('Ctrl Pts',(-4.04489507179964,-73.9608507287943,
0.));
#69121=CARTESIAN_POINT('Ctrl Pts',(-4.04489507179964,-73.9608507287943,
12.));
#69122=CARTESIAN_POINT('Ctrl Pts',(-4.0351134841066,-73.9864472641025,0.));
#69123=CARTESIAN_POINT('Ctrl Pts',(-4.0351134841066,-73.9864472641025,12.));
#69124=CARTESIAN_POINT('Ctrl Pts',(-4.02529599070085,-74.0120679876396,
0.));
#69125=CARTESIAN_POINT('Ctrl Pts',(-4.02529599070085,-74.0120679876396,
12.));
#69126=CARTESIAN_POINT('Ctrl Pts',(-4.01544258176693,-74.0377128111754,
0.));
#69127=CARTESIAN_POINT('Ctrl Pts',(-4.01544258176693,-74.0377128111754,
12.));
#69128=CARTESIAN_POINT('Ctrl Pts',(-4.00555324785459,-74.0633816477912,
0.));
#69129=CARTESIAN_POINT('Ctrl Pts',(-4.00555324785459,-74.0633816477912,
12.));
#69130=CARTESIAN_POINT('Ctrl Pts',(-3.99562797918271,-74.0890744091088,
0.));
#69131=CARTESIAN_POINT('Ctrl Pts',(-3.99562797918271,-74.0890744091088,
12.));
#69132=CARTESIAN_POINT('Ctrl Pts',(-3.98566676483639,-74.1147910020869,
0.));
#69133=CARTESIAN_POINT('Ctrl Pts',(-3.98566676483639,-74.1147910020869,
12.));
#69134=CARTESIAN_POINT('Ctrl Pts',(-3.97566959209546,-74.1405313263198,
0.));
#69135=CARTESIAN_POINT('Ctrl Pts',(-3.97566959209546,-74.1405313263198,
12.));
#69136=CARTESIAN_POINT('Ctrl Pts',(-3.96563644549422,-74.1662952702689,
0.));
#69137=CARTESIAN_POINT('Ctrl Pts',(-3.96563644549422,-74.1662952702689,
12.));
#69138=CARTESIAN_POINT('Ctrl Pts',(-3.9555673082116,-74.1920827166861,0.));
#69139=CARTESIAN_POINT('Ctrl Pts',(-3.9555673082116,-74.1920827166861,12.));
#69140=CARTESIAN_POINT('Ctrl Pts',(-3.94546216377498,-74.217893549314,0.));
#69141=CARTESIAN_POINT('Ctrl Pts',(-3.94546216377498,-74.217893549314,12.));
#69142=CARTESIAN_POINT('Ctrl Pts',(-3.93532099774229,-74.2437276593763,
0.));
#69143=CARTESIAN_POINT('Ctrl Pts',(-3.93532099774229,-74.2437276593763,
12.));
#69144=CARTESIAN_POINT('Ctrl Pts',(-3.92514379920729,-74.2695849516134,
0.));
#69145=CARTESIAN_POINT('Ctrl Pts',(-3.92514379920729,-74.2695849516134,
12.));
#69146=CARTESIAN_POINT('Ctrl Pts',(-3.91493056284964,-74.2954653518345,
0.));
#69147=CARTESIAN_POINT('Ctrl Pts',(-3.91493056284964,-74.2954653518345,
12.));
#69148=CARTESIAN_POINT('Ctrl Pts',(-3.9046812890452,-74.3213688089495,0.));
#69149=CARTESIAN_POINT('Ctrl Pts',(-3.9046812890452,-74.3213688089495,12.));
#69150=CARTESIAN_POINT('Ctrl Pts',(-3.89439598145193,-74.3472952898,0.));
#69151=CARTESIAN_POINT('Ctrl Pts',(-3.89439598145193,-74.3472952898,12.));
#69152=CARTESIAN_POINT('Ctrl Pts',(-3.88613891247869,-74.3680548786039,
0.));
#69153=CARTESIAN_POINT('Ctrl Pts',(-3.88613891247869,-74.3680548786039,
12.));
#69154=CARTESIAN_POINT('Ctrl Pts',(-3.87992989995678,-74.3836349188809,
0.));
#69155=CARTESIAN_POINT('Ctrl Pts',(-3.87992989995678,-74.3836349188809,
12.));
#69156=CARTESIAN_POINT('Ctrl Pts',(-3.87578335377301,-74.3940262116251,
0.));
#69157=CARTESIAN_POINT('Ctrl Pts',(-3.87578335377301,-74.3940262116251,
12.));
#69158=CARTESIAN_POINT('Ctrl Pts',(-3.87370827955545,-74.3992230078037,
0.));
#69159=CARTESIAN_POINT('Ctrl Pts',(-3.87370827955545,-74.3992230078037,
12.));
#69160=CARTESIAN_POINT('',(-5.24987136994592,-69.8028570375097,0.));
#69161=CARTESIAN_POINT('Ctrl Pts',(-5.24987136994592,-69.8028570375097,
0.));
#69162=CARTESIAN_POINT('Ctrl Pts',(-5.24915955997427,-69.8066748687772,
0.));
#69163=CARTESIAN_POINT('Ctrl Pts',(-5.24773285666376,-69.8143154684204,
0.));
#69164=CARTESIAN_POINT('Ctrl Pts',(-5.2455835515975,-69.8257911792159,0.));
#69165=CARTESIAN_POINT('Ctrl Pts',(-5.24269931054569,-69.841121750752,0.));
#69166=CARTESIAN_POINT('Ctrl Pts',(-5.23906316634803,-69.8603343302743,
0.));
#69167=CARTESIAN_POINT('Ctrl Pts',(-5.2353961627962,-69.8795962381599,0.));
#69168=CARTESIAN_POINT('Ctrl Pts',(-5.23169827290555,-69.8989073936688,
0.));
#69169=CARTESIAN_POINT('Ctrl Pts',(-5.22796945602794,-69.9182676502048,
0.));
#69170=CARTESIAN_POINT('Ctrl Pts',(-5.22420965879981,-69.9376767969095,
0.));
#69171=CARTESIAN_POINT('Ctrl Pts',(-5.22041882075721,-69.9571345870076,
0.));
#69172=CARTESIAN_POINT('Ctrl Pts',(-5.21659687881139,-69.9766407595385,
0.));
#69173=CARTESIAN_POINT('Ctrl Pts',(-5.21274377203259,-69.9961950629965,
0.));
#69174=CARTESIAN_POINT('Ctrl Pts',(-5.20885944672836,-70.0157972802182,
0.));
#69175=CARTESIAN_POINT('Ctrl Pts',(-5.20494385478025,-70.0354472203546,
0.));
#69176=CARTESIAN_POINT('Ctrl Pts',(-5.20099695122656,-70.0551447071082,
0.));
#69177=CARTESIAN_POINT('Ctrl Pts',(-5.19701869225528,-70.0748895689729,
0.));
#69178=CARTESIAN_POINT('Ctrl Pts',(-5.1930090327158,-70.0946816270997,0.));
#69179=CARTESIAN_POINT('Ctrl Pts',(-5.18896792486565,-70.1145206891885,
0.));
#69180=CARTESIAN_POINT('Ctrl Pts',(-5.18489531966265,-70.1344065558145,
0.));
#69181=CARTESIAN_POINT('Ctrl Pts',(-5.18079116757666,-70.1543390243892,
0.));
#69182=CARTESIAN_POINT('Ctrl Pts',(-5.17665541952383,-70.1743178937077,
0.));
#69183=CARTESIAN_POINT('Ctrl Pts',(-5.17248802793389,-70.1943429691167,
0.));
#69184=CARTESIAN_POINT('Ctrl Pts',(-5.16828894670108,-70.2144140622953,
0.));
#69185=CARTESIAN_POINT('Ctrl Pts',(-5.16405813066976,-70.2345309887833,
0.));
#69186=CARTESIAN_POINT('Ctrl Pts',(-5.15979553528203,-70.2546935662722,
0.));
#69187=CARTESIAN_POINT('Ctrl Pts',(-5.15550111614859,-70.2749016125105,
0.));
#69188=CARTESIAN_POINT('Ctrl Pts',(-5.15117482869254,-70.2951549435512,
0.));
#69189=CARTESIAN_POINT('Ctrl Pts',(-5.1468166283308,-70.3154533746736,0.));
#69190=CARTESIAN_POINT('Ctrl Pts',(-5.14242647063479,-70.3357967211796,
0.));
#69191=CARTESIAN_POINT('Ctrl Pts',(-5.13800431148904,-70.3561847991714,
0.));
#69192=CARTESIAN_POINT('Ctrl Pts',(-5.13355010728567,-70.3766174264757,
0.));
#69193=CARTESIAN_POINT('Ctrl Pts',(-5.12906381499456,-70.3970944229851,
0.));
#69194=CARTESIAN_POINT('Ctrl Pts',(-5.12454539205328,-70.417615610161,0.));
#69195=CARTESIAN_POINT('Ctrl Pts',(-5.11999479630212,-70.4381808107245,
0.));
#69196=CARTESIAN_POINT('Ctrl Pts',(-5.11541198590932,-70.458789848296,0.));
#69197=CARTESIAN_POINT('Ctrl Pts',(-5.11079691929213,-70.4794425469825,
0.));
#69198=CARTESIAN_POINT('Ctrl Pts',(-5.10614955511664,-70.500138731399,0.));
#69199=CARTESIAN_POINT('Ctrl Pts',(-5.10146985232941,-70.5208782268497,
0.));
#69200=CARTESIAN_POINT('Ctrl Pts',(-5.09675777018183,-70.5416608594526,
0.));
#69201=CARTESIAN_POINT('Ctrl Pts',(-5.09201326826134,-70.5624864562824,
0.));
#69202=CARTESIAN_POINT('Ctrl Pts',(-5.08723630652273,-70.5833548455014,
0.));
#69203=CARTESIAN_POINT('Ctrl Pts',(-5.08242684526687,-70.6042658562923,
0.));
#69204=CARTESIAN_POINT('Ctrl Pts',(-5.07758484512302,-70.6252193187878,
0.));
#69205=CARTESIAN_POINT('Ctrl Pts',(-5.07271026703355,-70.6462150640015,
0.));
#69206=CARTESIAN_POINT('Ctrl Pts',(-5.06780307224072,-70.6672529237455,
0.));
#69207=CARTESIAN_POINT('Ctrl Pts',(-5.0628632222782,-70.6883327305784,0.));
#69208=CARTESIAN_POINT('Ctrl Pts',(-5.05789067897057,-70.7094543178438,
0.));
#69209=CARTESIAN_POINT('Ctrl Pts',(-5.05288540443482,-70.7306175196863,
0.));
#69210=CARTESIAN_POINT('Ctrl Pts',(-5.04784736108346,-70.7518221710706,
0.));
#69211=CARTESIAN_POINT('Ctrl Pts',(-5.0427765116335,-70.7730681077983,0.));
#69212=CARTESIAN_POINT('Ctrl Pts',(-5.03767281910479,-70.7943551665059,
0.));
#69213=CARTESIAN_POINT('Ctrl Pts',(-5.03253624680941,-70.8156831846488,
0.));
#69214=CARTESIAN_POINT('Ctrl Pts',(-5.02736675834693,-70.8370520004843,
0.));
#69215=CARTESIAN_POINT('Ctrl Pts',(-5.02216431760061,-70.8584614530519,
0.));
#69216=CARTESIAN_POINT('Ctrl Pts',(-5.0169288887379,-70.8799113821452,0.));
#69217=CARTESIAN_POINT('Ctrl Pts',(-5.01166043620568,-70.9014016283124,
0.));
#69218=CARTESIAN_POINT('Ctrl Pts',(-5.00635892472513,-70.9229320328589,
0.));
#69219=CARTESIAN_POINT('Ctrl Pts',(-5.00102431929039,-70.9445024378439,
0.));
#69220=CARTESIAN_POINT('Ctrl Pts',(-4.99565658516913,-70.9661126860773,
0.));
#69221=CARTESIAN_POINT('Ctrl Pts',(-4.99025568790664,-70.9877626211113,
0.));
#69222=CARTESIAN_POINT('Ctrl Pts',(-4.98482159331863,-71.0094520872377,
0.));
#69223=CARTESIAN_POINT('Ctrl Pts',(-4.97935426748585,-71.0311809294821,
0.));
#69224=CARTESIAN_POINT('Ctrl Pts',(-4.97385367675159,-71.0529489935961,
0.));
#69225=CARTESIAN_POINT('Ctrl Pts',(-4.96831978772191,-71.0747561260436,
0.));
#69226=CARTESIAN_POINT('Ctrl Pts',(-4.96275256726766,-71.0966021739907,
0.));
#69227=CARTESIAN_POINT('Ctrl Pts',(-4.95715198251685,-71.1184869853056,
0.));
#69228=CARTESIAN_POINT('Ctrl Pts',(-4.95151800085101,-71.1404104085552,
0.));
#69229=CARTESIAN_POINT('Ctrl Pts',(-4.94585058990341,-71.1623722930001,
0.));
#69230=CARTESIAN_POINT('Ctrl Pts',(-4.94014971756115,-71.1843724885847,
0.));
#69231=CARTESIAN_POINT('Ctrl Pts',(-4.93441535196617,-71.2064108459286,
0.));
#69232=CARTESIAN_POINT('Ctrl Pts',(-4.92864746150732,-71.2284872163273,
0.));
#69233=CARTESIAN_POINT('Ctrl Pts',(-4.92284601481721,-71.250601451747,0.));
#69234=CARTESIAN_POINT('Ctrl Pts',(-4.91701098077036,-71.2727534048192,
0.));
#69235=CARTESIAN_POINT('Ctrl Pts',(-4.91114232848603,-71.294942928829,0.));
#69236=CARTESIAN_POINT('Ctrl Pts',(-4.90524002732779,-71.3171698777084,
0.));
#69237=CARTESIAN_POINT('Ctrl Pts',(-4.89930404689575,-71.3394341060359,
0.));
#69238=CARTESIAN_POINT('Ctrl Pts',(-4.89333435702414,-71.3617354690325,
0.));
#69239=CARTESIAN_POINT('Ctrl Pts',(-4.88733092777975,-71.3840738225562,
0.));
#69240=CARTESIAN_POINT('Ctrl Pts',(-4.88129372946551,-71.4064490230899,
0.));
#69241=CARTESIAN_POINT('Ctrl Pts',(-4.87522273261908,-71.4288609277374,
0.));
#69242=CARTESIAN_POINT('Ctrl Pts',(-4.8691179080055,-71.4513093942255,0.));
#69243=CARTESIAN_POINT('Ctrl Pts',(-4.86297922661503,-71.4737942808982,
0.));
#69244=CARTESIAN_POINT('Ctrl Pts',(-4.8568066596618,-71.4963154467113,0.));
#69245=CARTESIAN_POINT('Ctrl Pts',(-4.8506001785878,-71.5188727512197,0.));
#69246=CARTESIAN_POINT('Ctrl Pts',(-4.84435975506048,-71.5414660545739,
0.));
#69247=CARTESIAN_POINT('Ctrl Pts',(-4.83808536096583,-71.564095217521,0.));
#69248=CARTESIAN_POINT('Ctrl Pts',(-4.83177696840637,-71.5867601014,0.));
#69249=CARTESIAN_POINT('Ctrl Pts',(-4.82543454970027,-71.6094605681366,
0.));
#69250=CARTESIAN_POINT('Ctrl Pts',(-4.81905807738557,-71.6321964802326,
0.));
#69251=CARTESIAN_POINT('Ctrl Pts',(-4.81264752421732,-71.6549677007613,
0.));
#69252=CARTESIAN_POINT('Ctrl Pts',(-4.80620286316088,-71.6777740933705,
0.));
#69253=CARTESIAN_POINT('Ctrl Pts',(-4.79972406739014,-71.7006155222766,
0.));
#69254=CARTESIAN_POINT('Ctrl Pts',(-4.79321111028672,-71.7234918522604,
0.));
#69255=CARTESIAN_POINT('Ctrl Pts',(-4.7866639654445,-71.7464029486552,0.));
#69256=CARTESIAN_POINT('Ctrl Pts',(-4.78008260666642,-71.7693486773449,
0.));
#69257=CARTESIAN_POINT('Ctrl Pts',(-4.77346700795787,-71.7923289047636,
0.));
#69258=CARTESIAN_POINT('Ctrl Pts',(-4.76681714352503,-71.8153434978924,
0.));
#69259=CARTESIAN_POINT('Ctrl Pts',(-4.76013298777422,-71.8383923242533,
0.));
#69260=CARTESIAN_POINT('Ctrl Pts',(-4.75341451531671,-71.8614752519008,
0.));
#69261=CARTESIAN_POINT('Ctrl Pts',(-4.74666170096545,-71.8845921494186,
0.));
#69262=CARTESIAN_POINT('Ctrl Pts',(-4.7398745197286,-71.9077428859207,0.));
#69263=CARTESIAN_POINT('Ctrl Pts',(-4.73305294680784,-71.9309273310469,
0.));
#69264=CARTESIAN_POINT('Ctrl Pts',(-4.72619695759778,-71.9541453549582,
0.));
#69265=CARTESIAN_POINT('Ctrl Pts',(-4.7193065276908,-71.9773968283267,0.));
#69266=CARTESIAN_POINT('Ctrl Pts',(-4.7123816328741,-72.0006816223335,0.));
#69267=CARTESIAN_POINT('Ctrl Pts',(-4.70542224912312,-72.0239996086694,
0.));
#69268=CARTESIAN_POINT('Ctrl Pts',(-4.69842835259997,-72.047350659532,0.));
#69269=CARTESIAN_POINT('Ctrl Pts',(-4.6913999196528,-72.070734647621,0.));
#69270=CARTESIAN_POINT('Ctrl Pts',(-4.6843369268206,-72.0941514461283,0.));
#69271=CARTESIAN_POINT('Ctrl Pts',(-4.67723935083087,-72.1176009287349,
0.));
#69272=CARTESIAN_POINT('Ctrl Pts',(-4.67010716859281,-72.1410829696129,
0.));
#69273=CARTESIAN_POINT('Ctrl Pts',(-4.6629403571957,-72.1645974434218,0.));
#69274=CARTESIAN_POINT('Ctrl Pts',(-4.65573889390824,-72.1881442253052,
0.));
#69275=CARTESIAN_POINT('Ctrl Pts',(-4.64850275618325,-72.2117231908816,
0.));
#69276=CARTESIAN_POINT('Ctrl Pts',(-4.64123192165627,-72.2353342162408,
0.));
#69277=CARTESIAN_POINT('Ctrl Pts',(-4.63392636813842,-72.2589771779447,
0.));
#69278=CARTESIAN_POINT('Ctrl Pts',(-4.62658607361465,-72.2826519530254,
0.));
#69279=CARTESIAN_POINT('Ctrl Pts',(-4.61921101624294,-72.306358418981,0.));
#69280=CARTESIAN_POINT('Ctrl Pts',(-4.61180117435868,-72.330096453767,0.));
#69281=CARTESIAN_POINT('Ctrl Pts',(-4.60435652647463,-72.3538659357932,
0.));
#69282=CARTESIAN_POINT('Ctrl Pts',(-4.5968770512734,-72.3776667439244,0.));
#69283=CARTESIAN_POINT('Ctrl Pts',(-4.58936272760551,-72.4014987574789,
0.));
#69284=CARTESIAN_POINT('Ctrl Pts',(-4.58181353448851,-72.4253618562249,
0.));
#69285=CARTESIAN_POINT('Ctrl Pts',(-4.57422945111094,-72.449255920373,0.));
#69286=CARTESIAN_POINT('Ctrl Pts',(-4.56661045683366,-72.473180830571,0.));
#69287=CARTESIAN_POINT('Ctrl Pts',(-4.55895653118213,-72.4971364679055,
0.));
#69288=CARTESIAN_POINT('Ctrl Pts',(-4.55126765384403,-72.5211227138997,
0.));
#69289=CARTESIAN_POINT('Ctrl Pts',(-4.54354380466825,-72.5451394505106,
0.));
#69290=CARTESIAN_POINT('Ctrl Pts',(-4.53578496366802,-72.5691865601225,
0.));
#69291=CARTESIAN_POINT('Ctrl Pts',(-4.5279911110239,-72.5932639255406,0.));
#69292=CARTESIAN_POINT('Ctrl Pts',(-4.52016222707632,-72.6173714299935,
0.));
#69293=CARTESIAN_POINT('Ctrl Pts',(-4.5122982923226,-72.6415089571314,0.));
#69294=CARTESIAN_POINT('Ctrl Pts',(-4.50439928741605,-72.6656763910241,
0.));
#69295=CARTESIAN_POINT('Ctrl Pts',(-4.49646519316822,-72.689873616155,0.));
#69296=CARTESIAN_POINT('Ctrl Pts',(-4.48849599055354,-72.7141005174153,
0.));
#69297=CARTESIAN_POINT('Ctrl Pts',(-4.48049166070223,-72.7383569801042,
0.));
#69298=CARTESIAN_POINT('Ctrl Pts',(-4.47245218489623,-72.7626428899287,
0.));
#69299=CARTESIAN_POINT('Ctrl Pts',(-4.46437754456795,-72.7869581329994,
0.));
#69300=CARTESIAN_POINT('Ctrl Pts',(-4.45626772130138,-72.8113025958258,
0.));
#69301=CARTESIAN_POINT('Ctrl Pts',(-4.44812269683724,-72.8356761653064,
0.));
#69302=CARTESIAN_POINT('Ctrl Pts',(-4.43994245306805,-72.8600787287316,
0.));
#69303=CARTESIAN_POINT('Ctrl Pts',(-4.43172697203341,-72.8845101737856,
0.));
#69304=CARTESIAN_POINT('Ctrl Pts',(-4.42347623591941,-72.9089703885463,
0.));
#69305=CARTESIAN_POINT('Ctrl Pts',(-4.41519022705926,-72.9334592614828,
0.));
#69306=CARTESIAN_POINT('Ctrl Pts',(-4.40686892793965,-72.9579766814495,
0.));
#69307=CARTESIAN_POINT('Ctrl Pts',(-4.3985123211973,-72.9825225376839,0.));
#69308=CARTESIAN_POINT('Ctrl Pts',(-4.39012038961145,-73.0070967198033,
0.));
#69309=CARTESIAN_POINT('Ctrl Pts',(-4.38169311610153,-73.031699117799,0.));
#69310=CARTESIAN_POINT('Ctrl Pts',(-4.37323048372607,-73.0563296220301,
0.));
#69311=CARTESIAN_POINT('Ctrl Pts',(-4.36473247568638,-73.0809881232111,
0.));
#69312=CARTESIAN_POINT('Ctrl Pts',(-4.35619907532716,-73.1056745124099,
0.));
#69313=CARTESIAN_POINT('Ctrl Pts',(-4.34763026613154,-73.1303886810602,
0.));
#69314=CARTESIAN_POINT('Ctrl Pts',(-4.33902603172139,-73.1551305209692,
0.));
#69315=CARTESIAN_POINT('Ctrl Pts',(-4.33038635585878,-73.1798999243234,
0.));
#69316=CARTESIAN_POINT('Ctrl Pts',(-4.32171122245218,-73.204696783693,0.));
#69317=CARTESIAN_POINT('Ctrl Pts',(-4.31300061556103,-73.2295209920319,
0.));
#69318=CARTESIAN_POINT('Ctrl Pts',(-4.30425451938234,-73.2543724426562,
0.));
#69319=CARTESIAN_POINT('Ctrl Pts',(-4.29547291824289,-73.2792510292243,
0.));
#69320=CARTESIAN_POINT('Ctrl Pts',(-4.28665579659302,-73.3041566457134,
0.));
#69321=CARTESIAN_POINT('Ctrl Pts',(-4.27780313900392,-73.3290891863959,
0.));
#69322=CARTESIAN_POINT('Ctrl Pts',(-4.26891493016703,-73.354048545808,0.));
#69323=CARTESIAN_POINT('Ctrl Pts',(-4.25999115489904,-73.3790346187953,
0.));
#69324=CARTESIAN_POINT('Ctrl Pts',(-4.25103179814892,-73.4040473005603,
0.));
#69325=CARTESIAN_POINT('Ctrl Pts',(-4.24203684500941,-73.4290864867103,
0.));
#69326=CARTESIAN_POINT('Ctrl Pts',(-4.23300628072757,-73.4541520732943,
0.));
#69327=CARTESIAN_POINT('Ctrl Pts',(-4.22394009072753,-73.4792439568624,
0.));
#69328=CARTESIAN_POINT('Ctrl Pts',(-4.21483826059436,-73.5043620344107,
0.));
#69329=CARTESIAN_POINT('Ctrl Pts',(-4.20570077603727,-73.5295062032621,
0.));
#69330=CARTESIAN_POINT('Ctrl Pts',(-4.19652762286126,-73.554676360957,0.));
#69331=CARTESIAN_POINT('Ctrl Pts',(-4.18731878694238,-73.5798724051519,
0.));
#69332=CARTESIAN_POINT('Ctrl Pts',(-4.17807425419816,-73.6050942334773,
0.));
#69333=CARTESIAN_POINT('Ctrl Pts',(-4.16879401058786,-73.6303417435262,
0.));
#69334=CARTESIAN_POINT('Ctrl Pts',(-4.1594780421779,-73.6556148331504,0.));
#69335=CARTESIAN_POINT('Ctrl Pts',(-4.15012633519728,-73.6809134006909,
0.));
#69336=CARTESIAN_POINT('Ctrl Pts',(-4.14073887610155,-73.7062373452344,
0.));
#69337=CARTESIAN_POINT('Ctrl Pts',(-4.13131565163575,-73.7315865668508,
0.));
#69338=CARTESIAN_POINT('Ctrl Pts',(-4.12185664890551,-73.7569609668501,
0.));
#69339=CARTESIAN_POINT('Ctrl Pts',(-4.1123618552278,-73.7823604472126,0.));
#69340=CARTESIAN_POINT('Ctrl Pts',(-4.10283125798724,-73.8077849100314,
0.));
#69341=CARTESIAN_POINT('Ctrl Pts',(-4.09326484448231,-73.8332342568978,
0.));
#69342=CARTESIAN_POINT('Ctrl Pts',(-4.08366260180679,-73.8587083884208,
0.));
#69343=CARTESIAN_POINT('Ctrl Pts',(-4.07402451665253,-73.884207203405,0.));
#69344=CARTESIAN_POINT('Ctrl Pts',(-4.06435057547335,-73.9097305995173,
0.));
#69345=CARTESIAN_POINT('Ctrl Pts',(-4.05464076484761,-73.9352784747665,
0.));
#69346=CARTESIAN_POINT('Ctrl Pts',(-4.04489507179964,-73.9608507287943,
0.));
#69347=CARTESIAN_POINT('Ctrl Pts',(-4.0351134841066,-73.9864472641025,0.));
#69348=CARTESIAN_POINT('Ctrl Pts',(-4.02529599070085,-74.0120679876396,
0.));
#69349=CARTESIAN_POINT('Ctrl Pts',(-4.01544258176693,-74.0377128111754,
0.));
#69350=CARTESIAN_POINT('Ctrl Pts',(-4.00696550627608,-74.0597159781918,
0.));
#69351=CARTESIAN_POINT('Ctrl Pts',(-4.00044689712494,-74.076598294343,0.));
#69352=CARTESIAN_POINT('Ctrl Pts',(-3.99590266747771,-74.0883491449661,
0.));
#69353=CARTESIAN_POINT('Ctrl Pts',(-3.99334334446578,-74.0949615399272,
0.));
#69354=CARTESIAN_POINT('Ctrl Pts',(-3.99277406492187,-74.0964320765795,
0.));
#69355=CARTESIAN_POINT('',(-5.24987136994592,-69.8028570375097,12.));
#69356=CARTESIAN_POINT('',(-5.24987136994592,-69.8028570375097,0.));
#69357=CARTESIAN_POINT('Ctrl Pts',(-3.99277406492187,-74.0964320765795,
12.));
#69358=CARTESIAN_POINT('Ctrl Pts',(-3.99334334446578,-74.0949615399272,
12.));
#69359=CARTESIAN_POINT('Ctrl Pts',(-3.99590266747771,-74.0883491449661,
12.));
#69360=CARTESIAN_POINT('Ctrl Pts',(-4.00044689712494,-74.076598294343,12.));
#69361=CARTESIAN_POINT('Ctrl Pts',(-4.00696550627608,-74.0597159781918,
12.));
#69362=CARTESIAN_POINT('Ctrl Pts',(-4.01544258176693,-74.0377128111754,
12.));
#69363=CARTESIAN_POINT('Ctrl Pts',(-4.02529599070085,-74.0120679876396,
12.));
#69364=CARTESIAN_POINT('Ctrl Pts',(-4.0351134841066,-73.9864472641025,12.));
#69365=CARTESIAN_POINT('Ctrl Pts',(-4.04489507179964,-73.9608507287943,
12.));
#69366=CARTESIAN_POINT('Ctrl Pts',(-4.05464076484761,-73.9352784747665,
12.));
#69367=CARTESIAN_POINT('Ctrl Pts',(-4.06435057547335,-73.9097305995173,
12.));
#69368=CARTESIAN_POINT('Ctrl Pts',(-4.07402451665253,-73.884207203405,12.));
#69369=CARTESIAN_POINT('Ctrl Pts',(-4.08366260180679,-73.8587083884208,
12.));
#69370=CARTESIAN_POINT('Ctrl Pts',(-4.09326484448231,-73.8332342568978,
12.));
#69371=CARTESIAN_POINT('Ctrl Pts',(-4.10283125798724,-73.8077849100314,
12.));
#69372=CARTESIAN_POINT('Ctrl Pts',(-4.1123618552278,-73.7823604472126,12.));
#69373=CARTESIAN_POINT('Ctrl Pts',(-4.12185664890551,-73.7569609668501,
12.));
#69374=CARTESIAN_POINT('Ctrl Pts',(-4.13131565163575,-73.7315865668508,
12.));
#69375=CARTESIAN_POINT('Ctrl Pts',(-4.14073887610155,-73.7062373452344,
12.));
#69376=CARTESIAN_POINT('Ctrl Pts',(-4.15012633519728,-73.6809134006909,
12.));
#69377=CARTESIAN_POINT('Ctrl Pts',(-4.1594780421779,-73.6556148331504,12.));
#69378=CARTESIAN_POINT('Ctrl Pts',(-4.16879401058786,-73.6303417435262,
12.));
#69379=CARTESIAN_POINT('Ctrl Pts',(-4.17807425419816,-73.6050942334773,
12.));
#69380=CARTESIAN_POINT('Ctrl Pts',(-4.18731878694238,-73.5798724051519,
12.));
#69381=CARTESIAN_POINT('Ctrl Pts',(-4.19652762286126,-73.554676360957,12.));
#69382=CARTESIAN_POINT('Ctrl Pts',(-4.20570077603727,-73.5295062032621,
12.));
#69383=CARTESIAN_POINT('Ctrl Pts',(-4.21483826059436,-73.5043620344107,
12.));
#69384=CARTESIAN_POINT('Ctrl Pts',(-4.22394009072753,-73.4792439568624,
12.));
#69385=CARTESIAN_POINT('Ctrl Pts',(-4.23300628072757,-73.4541520732943,
12.));
#69386=CARTESIAN_POINT('Ctrl Pts',(-4.24203684500941,-73.4290864867103,
12.));
#69387=CARTESIAN_POINT('Ctrl Pts',(-4.25103179814892,-73.4040473005603,
12.));
#69388=CARTESIAN_POINT('Ctrl Pts',(-4.25999115489904,-73.3790346187953,
12.));
#69389=CARTESIAN_POINT('Ctrl Pts',(-4.26891493016703,-73.354048545808,12.));
#69390=CARTESIAN_POINT('Ctrl Pts',(-4.27780313900392,-73.3290891863959,
12.));
#69391=CARTESIAN_POINT('Ctrl Pts',(-4.28665579659302,-73.3041566457134,
12.));
#69392=CARTESIAN_POINT('Ctrl Pts',(-4.29547291824289,-73.2792510292243,
12.));
#69393=CARTESIAN_POINT('Ctrl Pts',(-4.30425451938234,-73.2543724426562,
12.));
#69394=CARTESIAN_POINT('Ctrl Pts',(-4.31300061556103,-73.2295209920319,
12.));
#69395=CARTESIAN_POINT('Ctrl Pts',(-4.32171122245218,-73.204696783693,12.));
#69396=CARTESIAN_POINT('Ctrl Pts',(-4.33038635585878,-73.1798999243234,
12.));
#69397=CARTESIAN_POINT('Ctrl Pts',(-4.33902603172139,-73.1551305209692,
12.));
#69398=CARTESIAN_POINT('Ctrl Pts',(-4.34763026613154,-73.1303886810602,
12.));
#69399=CARTESIAN_POINT('Ctrl Pts',(-4.35619907532716,-73.1056745124099,
12.));
#69400=CARTESIAN_POINT('Ctrl Pts',(-4.36473247568638,-73.0809881232111,
12.));
#69401=CARTESIAN_POINT('Ctrl Pts',(-4.37323048372607,-73.0563296220301,
12.));
#69402=CARTESIAN_POINT('Ctrl Pts',(-4.38169311610153,-73.031699117799,12.));
#69403=CARTESIAN_POINT('Ctrl Pts',(-4.39012038961145,-73.0070967198033,
12.));
#69404=CARTESIAN_POINT('Ctrl Pts',(-4.3985123211973,-72.9825225376839,12.));
#69405=CARTESIAN_POINT('Ctrl Pts',(-4.40686892793965,-72.9579766814495,
12.));
#69406=CARTESIAN_POINT('Ctrl Pts',(-4.41519022705926,-72.9334592614828,
12.));
#69407=CARTESIAN_POINT('Ctrl Pts',(-4.42347623591941,-72.9089703885463,
12.));
#69408=CARTESIAN_POINT('Ctrl Pts',(-4.43172697203341,-72.8845101737856,
12.));
#69409=CARTESIAN_POINT('Ctrl Pts',(-4.43994245306805,-72.8600787287316,
12.));
#69410=CARTESIAN_POINT('Ctrl Pts',(-4.44812269683724,-72.8356761653064,
12.));
#69411=CARTESIAN_POINT('Ctrl Pts',(-4.45626772130138,-72.8113025958258,
12.));
#69412=CARTESIAN_POINT('Ctrl Pts',(-4.46437754456795,-72.7869581329994,
12.));
#69413=CARTESIAN_POINT('Ctrl Pts',(-4.47245218489623,-72.7626428899287,
12.));
#69414=CARTESIAN_POINT('Ctrl Pts',(-4.48049166070223,-72.7383569801042,
12.));
#69415=CARTESIAN_POINT('Ctrl Pts',(-4.48849599055354,-72.7141005174153,
12.));
#69416=CARTESIAN_POINT('Ctrl Pts',(-4.49646519316822,-72.689873616155,12.));
#69417=CARTESIAN_POINT('Ctrl Pts',(-4.50439928741605,-72.6656763910241,
12.));
#69418=CARTESIAN_POINT('Ctrl Pts',(-4.5122982923226,-72.6415089571314,12.));
#69419=CARTESIAN_POINT('Ctrl Pts',(-4.52016222707632,-72.6173714299935,
12.));
#69420=CARTESIAN_POINT('Ctrl Pts',(-4.5279911110239,-72.5932639255406,12.));
#69421=CARTESIAN_POINT('Ctrl Pts',(-4.53578496366802,-72.5691865601225,
12.));
#69422=CARTESIAN_POINT('Ctrl Pts',(-4.54354380466825,-72.5451394505106,
12.));
#69423=CARTESIAN_POINT('Ctrl Pts',(-4.55126765384403,-72.5211227138997,
12.));
#69424=CARTESIAN_POINT('Ctrl Pts',(-4.55895653118213,-72.4971364679055,
12.));
#69425=CARTESIAN_POINT('Ctrl Pts',(-4.56661045683366,-72.473180830571,12.));
#69426=CARTESIAN_POINT('Ctrl Pts',(-4.57422945111094,-72.449255920373,12.));
#69427=CARTESIAN_POINT('Ctrl Pts',(-4.58181353448851,-72.4253618562249,
12.));
#69428=CARTESIAN_POINT('Ctrl Pts',(-4.58936272760551,-72.4014987574789,
12.));
#69429=CARTESIAN_POINT('Ctrl Pts',(-4.5968770512734,-72.3776667439244,12.));
#69430=CARTESIAN_POINT('Ctrl Pts',(-4.60435652647463,-72.3538659357932,
12.));
#69431=CARTESIAN_POINT('Ctrl Pts',(-4.61180117435868,-72.330096453767,12.));
#69432=CARTESIAN_POINT('Ctrl Pts',(-4.61921101624294,-72.306358418981,12.));
#69433=CARTESIAN_POINT('Ctrl Pts',(-4.62658607361465,-72.2826519530254,
12.));
#69434=CARTESIAN_POINT('Ctrl Pts',(-4.63392636813842,-72.2589771779447,
12.));
#69435=CARTESIAN_POINT('Ctrl Pts',(-4.64123192165627,-72.2353342162408,
12.));
#69436=CARTESIAN_POINT('Ctrl Pts',(-4.64850275618325,-72.2117231908816,
12.));
#69437=CARTESIAN_POINT('Ctrl Pts',(-4.65573889390824,-72.1881442253052,
12.));
#69438=CARTESIAN_POINT('Ctrl Pts',(-4.6629403571957,-72.1645974434218,12.));
#69439=CARTESIAN_POINT('Ctrl Pts',(-4.67010716859281,-72.1410829696129,
12.));
#69440=CARTESIAN_POINT('Ctrl Pts',(-4.67723935083087,-72.1176009287349,
12.));
#69441=CARTESIAN_POINT('Ctrl Pts',(-4.6843369268206,-72.0941514461283,12.));
#69442=CARTESIAN_POINT('Ctrl Pts',(-4.6913999196528,-72.070734647621,12.));
#69443=CARTESIAN_POINT('Ctrl Pts',(-4.69842835259997,-72.047350659532,12.));
#69444=CARTESIAN_POINT('Ctrl Pts',(-4.70542224912312,-72.0239996086694,
12.));
#69445=CARTESIAN_POINT('Ctrl Pts',(-4.7123816328741,-72.0006816223335,12.));
#69446=CARTESIAN_POINT('Ctrl Pts',(-4.7193065276908,-71.9773968283267,12.));
#69447=CARTESIAN_POINT('Ctrl Pts',(-4.72619695759778,-71.9541453549582,
12.));
#69448=CARTESIAN_POINT('Ctrl Pts',(-4.73305294680784,-71.9309273310469,
12.));
#69449=CARTESIAN_POINT('Ctrl Pts',(-4.7398745197286,-71.9077428859207,12.));
#69450=CARTESIAN_POINT('Ctrl Pts',(-4.74666170096545,-71.8845921494186,
12.));
#69451=CARTESIAN_POINT('Ctrl Pts',(-4.75341451531671,-71.8614752519008,
12.));
#69452=CARTESIAN_POINT('Ctrl Pts',(-4.76013298777422,-71.8383923242533,
12.));
#69453=CARTESIAN_POINT('Ctrl Pts',(-4.76681714352503,-71.8153434978924,
12.));
#69454=CARTESIAN_POINT('Ctrl Pts',(-4.77346700795787,-71.7923289047636,
12.));
#69455=CARTESIAN_POINT('Ctrl Pts',(-4.78008260666642,-71.7693486773449,
12.));
#69456=CARTESIAN_POINT('Ctrl Pts',(-4.7866639654445,-71.7464029486552,12.));
#69457=CARTESIAN_POINT('Ctrl Pts',(-4.79321111028672,-71.7234918522604,
12.));
#69458=CARTESIAN_POINT('Ctrl Pts',(-4.79972406739014,-71.7006155222766,
12.));
#69459=CARTESIAN_POINT('Ctrl Pts',(-4.80620286316088,-71.6777740933705,
12.));
#69460=CARTESIAN_POINT('Ctrl Pts',(-4.81264752421732,-71.6549677007613,
12.));
#69461=CARTESIAN_POINT('Ctrl Pts',(-4.81905807738557,-71.6321964802326,
12.));
#69462=CARTESIAN_POINT('Ctrl Pts',(-4.82543454970027,-71.6094605681366,
12.));
#69463=CARTESIAN_POINT('Ctrl Pts',(-4.83177696840637,-71.5867601014,12.));
#69464=CARTESIAN_POINT('Ctrl Pts',(-4.83808536096583,-71.564095217521,12.));
#69465=CARTESIAN_POINT('Ctrl Pts',(-4.84435975506048,-71.5414660545739,
12.));
#69466=CARTESIAN_POINT('Ctrl Pts',(-4.8506001785878,-71.5188727512197,12.));
#69467=CARTESIAN_POINT('Ctrl Pts',(-4.8568066596618,-71.4963154467113,12.));
#69468=CARTESIAN_POINT('Ctrl Pts',(-4.86297922661503,-71.4737942808982,
12.));
#69469=CARTESIAN_POINT('Ctrl Pts',(-4.8691179080055,-71.4513093942255,12.));
#69470=CARTESIAN_POINT('Ctrl Pts',(-4.87522273261908,-71.4288609277374,
12.));
#69471=CARTESIAN_POINT('Ctrl Pts',(-4.88129372946551,-71.4064490230899,
12.));
#69472=CARTESIAN_POINT('Ctrl Pts',(-4.88733092777975,-71.3840738225562,
12.));
#69473=CARTESIAN_POINT('Ctrl Pts',(-4.89333435702414,-71.3617354690325,
12.));
#69474=CARTESIAN_POINT('Ctrl Pts',(-4.89930404689575,-71.3394341060359,
12.));
#69475=CARTESIAN_POINT('Ctrl Pts',(-4.90524002732779,-71.3171698777084,
12.));
#69476=CARTESIAN_POINT('Ctrl Pts',(-4.91114232848603,-71.294942928829,12.));
#69477=CARTESIAN_POINT('Ctrl Pts',(-4.91701098077036,-71.2727534048192,
12.));
#69478=CARTESIAN_POINT('Ctrl Pts',(-4.92284601481721,-71.250601451747,12.));
#69479=CARTESIAN_POINT('Ctrl Pts',(-4.92864746150732,-71.2284872163273,
12.));
#69480=CARTESIAN_POINT('Ctrl Pts',(-4.93441535196617,-71.2064108459286,
12.));
#69481=CARTESIAN_POINT('Ctrl Pts',(-4.94014971756115,-71.1843724885847,
12.));
#69482=CARTESIAN_POINT('Ctrl Pts',(-4.94585058990341,-71.1623722930001,
12.));
#69483=CARTESIAN_POINT('Ctrl Pts',(-4.95151800085101,-71.1404104085552,
12.));
#69484=CARTESIAN_POINT('Ctrl Pts',(-4.95715198251685,-71.1184869853056,
12.));
#69485=CARTESIAN_POINT('Ctrl Pts',(-4.96275256726766,-71.0966021739907,
12.));
#69486=CARTESIAN_POINT('Ctrl Pts',(-4.96831978772191,-71.0747561260436,
12.));
#69487=CARTESIAN_POINT('Ctrl Pts',(-4.97385367675159,-71.0529489935961,
12.));
#69488=CARTESIAN_POINT('Ctrl Pts',(-4.97935426748585,-71.0311809294821,
12.));
#69489=CARTESIAN_POINT('Ctrl Pts',(-4.98482159331863,-71.0094520872377,
12.));
#69490=CARTESIAN_POINT('Ctrl Pts',(-4.99025568790664,-70.9877626211113,
12.));
#69491=CARTESIAN_POINT('Ctrl Pts',(-4.99565658516913,-70.9661126860773,
12.));
#69492=CARTESIAN_POINT('Ctrl Pts',(-5.00102431929039,-70.9445024378439,
12.));
#69493=CARTESIAN_POINT('Ctrl Pts',(-5.00635892472513,-70.9229320328589,
12.));
#69494=CARTESIAN_POINT('Ctrl Pts',(-5.01166043620568,-70.9014016283124,
12.));
#69495=CARTESIAN_POINT('Ctrl Pts',(-5.0169288887379,-70.8799113821452,12.));
#69496=CARTESIAN_POINT('Ctrl Pts',(-5.02216431760061,-70.8584614530519,
12.));
#69497=CARTESIAN_POINT('Ctrl Pts',(-5.02736675834693,-70.8370520004843,
12.));
#69498=CARTESIAN_POINT('Ctrl Pts',(-5.03253624680941,-70.8156831846488,
12.));
#69499=CARTESIAN_POINT('Ctrl Pts',(-5.03767281910479,-70.7943551665059,
12.));
#69500=CARTESIAN_POINT('Ctrl Pts',(-5.0427765116335,-70.7730681077983,12.));
#69501=CARTESIAN_POINT('Ctrl Pts',(-5.04784736108346,-70.7518221710706,
12.));
#69502=CARTESIAN_POINT('Ctrl Pts',(-5.05288540443482,-70.7306175196863,
12.));
#69503=CARTESIAN_POINT('Ctrl Pts',(-5.05789067897057,-70.7094543178438,
12.));
#69504=CARTESIAN_POINT('Ctrl Pts',(-5.0628632222782,-70.6883327305784,12.));
#69505=CARTESIAN_POINT('Ctrl Pts',(-5.06780307224072,-70.6672529237455,
12.));
#69506=CARTESIAN_POINT('Ctrl Pts',(-5.07271026703355,-70.6462150640015,
12.));
#69507=CARTESIAN_POINT('Ctrl Pts',(-5.07758484512302,-70.6252193187878,
12.));
#69508=CARTESIAN_POINT('Ctrl Pts',(-5.08242684526687,-70.6042658562923,
12.));
#69509=CARTESIAN_POINT('Ctrl Pts',(-5.08723630652273,-70.5833548455014,
12.));
#69510=CARTESIAN_POINT('Ctrl Pts',(-5.09201326826134,-70.5624864562824,
12.));
#69511=CARTESIAN_POINT('Ctrl Pts',(-5.09675777018183,-70.5416608594526,
12.));
#69512=CARTESIAN_POINT('Ctrl Pts',(-5.10146985232941,-70.5208782268497,
12.));
#69513=CARTESIAN_POINT('Ctrl Pts',(-5.10614955511664,-70.500138731399,12.));
#69514=CARTESIAN_POINT('Ctrl Pts',(-5.11079691929213,-70.4794425469825,
12.));
#69515=CARTESIAN_POINT('Ctrl Pts',(-5.11541198590932,-70.458789848296,12.));
#69516=CARTESIAN_POINT('Ctrl Pts',(-5.11999479630212,-70.4381808107245,
12.));
#69517=CARTESIAN_POINT('Ctrl Pts',(-5.12454539205328,-70.417615610161,12.));
#69518=CARTESIAN_POINT('Ctrl Pts',(-5.12906381499456,-70.3970944229851,
12.));
#69519=CARTESIAN_POINT('Ctrl Pts',(-5.13355010728567,-70.3766174264757,
12.));
#69520=CARTESIAN_POINT('Ctrl Pts',(-5.13800431148904,-70.3561847991714,
12.));
#69521=CARTESIAN_POINT('Ctrl Pts',(-5.14242647063479,-70.3357967211796,
12.));
#69522=CARTESIAN_POINT('Ctrl Pts',(-5.1468166283308,-70.3154533746736,12.));
#69523=CARTESIAN_POINT('Ctrl Pts',(-5.15117482869254,-70.2951549435512,
12.));
#69524=CARTESIAN_POINT('Ctrl Pts',(-5.15550111614859,-70.2749016125105,
12.));
#69525=CARTESIAN_POINT('Ctrl Pts',(-5.15979553528203,-70.2546935662722,
12.));
#69526=CARTESIAN_POINT('Ctrl Pts',(-5.16405813066976,-70.2345309887833,
12.));
#69527=CARTESIAN_POINT('Ctrl Pts',(-5.16828894670108,-70.2144140622953,
12.));
#69528=CARTESIAN_POINT('Ctrl Pts',(-5.17248802793389,-70.1943429691167,
12.));
#69529=CARTESIAN_POINT('Ctrl Pts',(-5.17665541952383,-70.1743178937077,
12.));
#69530=CARTESIAN_POINT('Ctrl Pts',(-5.18079116757666,-70.1543390243892,
12.));
#69531=CARTESIAN_POINT('Ctrl Pts',(-5.18489531966265,-70.1344065558145,
12.));
#69532=CARTESIAN_POINT('Ctrl Pts',(-5.18896792486565,-70.1145206891885,
12.));
#69533=CARTESIAN_POINT('Ctrl Pts',(-5.1930090327158,-70.0946816270997,12.));
#69534=CARTESIAN_POINT('Ctrl Pts',(-5.19701869225528,-70.0748895689729,
12.));
#69535=CARTESIAN_POINT('Ctrl Pts',(-5.20099695122656,-70.0551447071082,
12.));
#69536=CARTESIAN_POINT('Ctrl Pts',(-5.20494385478025,-70.0354472203546,
12.));
#69537=CARTESIAN_POINT('Ctrl Pts',(-5.20885944672836,-70.0157972802182,
12.));
#69538=CARTESIAN_POINT('Ctrl Pts',(-5.21274377203259,-69.9961950629965,
12.));
#69539=CARTESIAN_POINT('Ctrl Pts',(-5.21659687881139,-69.9766407595385,
12.));
#69540=CARTESIAN_POINT('Ctrl Pts',(-5.22041882075721,-69.9571345870076,
12.));
#69541=CARTESIAN_POINT('Ctrl Pts',(-5.22420965879981,-69.9376767969095,
12.));
#69542=CARTESIAN_POINT('Ctrl Pts',(-5.22796945602794,-69.9182676502048,
12.));
#69543=CARTESIAN_POINT('Ctrl Pts',(-5.23169827290555,-69.8989073936688,
12.));
#69544=CARTESIAN_POINT('Ctrl Pts',(-5.2353961627962,-69.8795962381599,12.));
#69545=CARTESIAN_POINT('Ctrl Pts',(-5.23906316634803,-69.8603343302743,
12.));
#69546=CARTESIAN_POINT('Ctrl Pts',(-5.24269931054569,-69.841121750752,12.));
#69547=CARTESIAN_POINT('Ctrl Pts',(-5.2455835515975,-69.8257911792159,12.));
#69548=CARTESIAN_POINT('Ctrl Pts',(-5.24773285666376,-69.8143154684204,
12.));
#69549=CARTESIAN_POINT('Ctrl Pts',(-5.24915955997427,-69.8066748687772,
12.));
#69550=CARTESIAN_POINT('Ctrl Pts',(-5.24987136994592,-69.8028570375097,
12.));
#69551=CARTESIAN_POINT('Ctrl Pts',(-2.480349218449,-74.1624659714954,0.));
#69552=CARTESIAN_POINT('Ctrl Pts',(-2.480349218449,-74.1624659714954,4.));
#69553=CARTESIAN_POINT('Ctrl Pts',(-2.480349218449,-74.1624659714954,8.));
#69554=CARTESIAN_POINT('Ctrl Pts',(-2.480349218449,-74.1624659714954,12.));
#69555=CARTESIAN_POINT('Ctrl Pts',(-2.52879860312845,-74.2610905805697,
0.));
#69556=CARTESIAN_POINT('Ctrl Pts',(-2.52879860312845,-74.2610905805697,
4.));
#69557=CARTESIAN_POINT('Ctrl Pts',(-2.52879860312844,-74.2610905805697,
8.));
#69558=CARTESIAN_POINT('Ctrl Pts',(-2.52879860312844,-74.2610905805697,
12.));
#69559=CARTESIAN_POINT('Ctrl Pts',(-2.67239300265255,-74.4041075779818,
-7.30788408099537E-17));
#69560=CARTESIAN_POINT('Ctrl Pts',(-2.67239300265255,-74.4041075779818,
4.));
#69561=CARTESIAN_POINT('Ctrl Pts',(-2.67239300265254,-74.4041075779819,
7.99999999999999));
#69562=CARTESIAN_POINT('Ctrl Pts',(-2.67239300265254,-74.4041075779819,
12.));
#69563=CARTESIAN_POINT('Ctrl Pts',(-2.86656650944673,-74.4448761712979,
-2.46611180197105E-16));
#69564=CARTESIAN_POINT('Ctrl Pts',(-2.86656650944673,-74.4448761712979,
4.));
#69565=CARTESIAN_POINT('Ctrl Pts',(-2.86656650944675,-74.444876171298,8.00000000000001));
#69566=CARTESIAN_POINT('Ctrl Pts',(-2.86656650944675,-74.444876171298,12.));
#69567=CARTESIAN_POINT('Ctrl Pts',(-2.94891377268011,-74.4416140848738,
-3.30265160424791E-16));
#69568=CARTESIAN_POINT('Ctrl Pts',(-2.94891377268011,-74.4416140848738,
4.));
#69569=CARTESIAN_POINT('Ctrl Pts',(-2.94891377268014,-74.4416140848739,
8.));
#69570=CARTESIAN_POINT('Ctrl Pts',(-2.94891377268014,-74.4416140848739,
12.));
#69571=CARTESIAN_POINT('',(-2.480349218449,-74.1624659714954,0.));
#69572=CARTESIAN_POINT('',(-2.94891377268011,-74.4416140848739,0.));
#69573=CARTESIAN_POINT('Ctrl Pts',(-2.480349218449,-74.1624659714954,2.74425517504386E-17));
#69574=CARTESIAN_POINT('Ctrl Pts',(-2.52879860312845,-74.2610905805697,
2.74425517504386E-17));
#69575=CARTESIAN_POINT('Ctrl Pts',(-2.61085254571365,-74.3428145790909,
-1.43167858552492E-17));
#69576=CARTESIAN_POINT('Ctrl Pts',(-2.70942211516255,-74.3911513436216,
-8.88772658534914E-17));
#69577=CARTESIAN_POINT('Ctrl Pts',(-2.78334929224922,-74.4274039170196,
-1.44797625852173E-16));
#69578=CARTESIAN_POINT('Ctrl Pts',(-2.86656650944673,-74.4448761712979,
-2.19168628446667E-16));
#69579=CARTESIAN_POINT('Ctrl Pts',(-2.94891377268011,-74.4416140848738,
-3.02822608674353E-16));
#69580=CARTESIAN_POINT('',(-2.94891377268014,-74.4416140848739,12.));
#69581=CARTESIAN_POINT('Ctrl Pts',(-2.94891377268011,-74.4416140848738,
-3.30265160424791E-16));
#69582=CARTESIAN_POINT('Ctrl Pts',(-2.94891377268011,-74.4416140848738,
4.));
#69583=CARTESIAN_POINT('Ctrl Pts',(-2.94891377268014,-74.4416140848739,
8.));
#69584=CARTESIAN_POINT('Ctrl Pts',(-2.94891377268014,-74.4416140848739,
12.));
#69585=CARTESIAN_POINT('',(-2.480349218449,-74.1624659714954,12.));
#69586=CARTESIAN_POINT('Ctrl Pts',(-2.94891377268014,-74.4416140848739,
12.));
#69587=CARTESIAN_POINT('Ctrl Pts',(-2.86656650944675,-74.444876171298,12.));
#69588=CARTESIAN_POINT('Ctrl Pts',(-2.78334929224923,-74.4274039170196,
12.));
#69589=CARTESIAN_POINT('Ctrl Pts',(-2.70942211516255,-74.3911513436216,
12.));
#69590=CARTESIAN_POINT('Ctrl Pts',(-2.61085254571364,-74.342814579091,12.));
#69591=CARTESIAN_POINT('Ctrl Pts',(-2.52879860312844,-74.2610905805697,
12.));
#69592=CARTESIAN_POINT('Ctrl Pts',(-2.480349218449,-74.1624659714954,12.));
#69593=CARTESIAN_POINT('Ctrl Pts',(-2.480349218449,-74.1624659714954,12.));
#69594=CARTESIAN_POINT('Ctrl Pts',(-2.480349218449,-74.1624659714954,8.));
#69595=CARTESIAN_POINT('Ctrl Pts',(-2.480349218449,-74.1624659714954,4.));
#69596=CARTESIAN_POINT('Ctrl Pts',(-2.480349218449,-74.1624659714954,0.));
#69597=CARTESIAN_POINT('Origin',(-1.62512913209675E-11,-3.74491326291036E-10,
0.));
#69598=CARTESIAN_POINT('Origin',(-1.62512913209675E-11,-3.74491326291036E-10,
12.));
#69599=CARTESIAN_POINT('Origin',(-1.62512913209675E-11,-3.74491326291036E-10,
0.));
#69600=CARTESIAN_POINT('Ctrl Pts',(-10.0225374821204,-73.8227522002498,
-5.55111512312578E-16));
#69601=CARTESIAN_POINT('Ctrl Pts',(-10.0225374821204,-73.8227522002498,
4.));
#69602=CARTESIAN_POINT('Ctrl Pts',(-10.0225374821204,-73.8227522002498,
8.));
#69603=CARTESIAN_POINT('Ctrl Pts',(-10.0225374821204,-73.8227522002498,
12.));
#69604=CARTESIAN_POINT('Ctrl Pts',(-10.1314210536414,-73.8079696346555,
-5.55111512312578E-16));
#69605=CARTESIAN_POINT('Ctrl Pts',(-10.1314210536414,-73.8079696346555,
4.));
#69606=CARTESIAN_POINT('Ctrl Pts',(-10.1314210536414,-73.8079696346555,
8.00000000000001));
#69607=CARTESIAN_POINT('Ctrl Pts',(-10.1314210536414,-73.8079696346555,
12.));
#69608=CARTESIAN_POINT('Ctrl Pts',(-10.3125002643516,-73.7169567649192,
-6.28191717183155E-16));
#69609=CARTESIAN_POINT('Ctrl Pts',(-10.3125002643516,-73.7169567649192,
4.00000000000001));
#69610=CARTESIAN_POINT('Ctrl Pts',(-10.3125002643516,-73.7169567649192,
8.));
#69611=CARTESIAN_POINT('Ctrl Pts',(-10.3125002643516,-73.7169567649192,
12.));
#69612=CARTESIAN_POINT('Ctrl Pts',(-10.4125694172275,-73.5456341632196,
-8.01722692545273E-16));
#69613=CARTESIAN_POINT('Ctrl Pts',(-10.4125694172275,-73.5456341632196,
4.));
#69614=CARTESIAN_POINT('Ctrl Pts',(-10.4125694172275,-73.5456341632196,
8.00000000000001));
#69615=CARTESIAN_POINT('Ctrl Pts',(-10.4125694172275,-73.5456341632196,
12.));
#69616=CARTESIAN_POINT('Ctrl Pts',(-10.4355099267388,-73.4664795929518,
-8.85376672782757E-16));
#69617=CARTESIAN_POINT('Ctrl Pts',(-10.4355099267388,-73.4664795929518,
4.));
#69618=CARTESIAN_POINT('Ctrl Pts',(-10.4355099267388,-73.4664795929518,
8.));
#69619=CARTESIAN_POINT('Ctrl Pts',(-10.4355099267388,-73.4664795929518,
12.));
#69620=CARTESIAN_POINT('',(-10.0225374821204,-73.8227522002498,0.));
#69621=CARTESIAN_POINT('',(-10.4355099267391,-73.4664795929519,0.));
#69622=CARTESIAN_POINT('Ctrl Pts',(-10.0225374821204,-73.8227522002498,
-5.27668960562141E-16));
#69623=CARTESIAN_POINT('Ctrl Pts',(-10.1314210536414,-73.8079696346555,
-5.27668960562141E-16));
#69624=CARTESIAN_POINT('Ctrl Pts',(-10.234894888333,-73.7559622805204,-5.69429077631042E-16));
#69625=CARTESIAN_POINT('Ctrl Pts',(-10.3119164592419,-73.6777313404382,
-6.43989446289017E-16));
#69626=CARTESIAN_POINT('Ctrl Pts',(-10.3696826374235,-73.6190581353765,
-6.99909722782499E-16));
#69627=CARTESIAN_POINT('Ctrl Pts',(-10.4125694172275,-73.5456341632196,
-7.74280140794835E-16));
#69628=CARTESIAN_POINT('Ctrl Pts',(-10.4355099267388,-73.4664795929518,
-8.5793412103232E-16));
#69629=CARTESIAN_POINT('',(-10.4355099267391,-73.4664795929519,12.));
#69630=CARTESIAN_POINT('Ctrl Pts',(-10.4355099267388,-73.4664795929518,
-8.85376672782757E-16));
#69631=CARTESIAN_POINT('Ctrl Pts',(-10.4355099267388,-73.4664795929518,
4.));
#69632=CARTESIAN_POINT('Ctrl Pts',(-10.4355099267388,-73.4664795929518,
8.));
#69633=CARTESIAN_POINT('Ctrl Pts',(-10.4355099267388,-73.4664795929518,
12.));
#69634=CARTESIAN_POINT('',(-10.0225374821204,-73.8227522002498,12.));
#69635=CARTESIAN_POINT('Ctrl Pts',(-10.4355099267388,-73.4664795929518,
12.));
#69636=CARTESIAN_POINT('Ctrl Pts',(-10.4125694172275,-73.5456341632196,
12.));
#69637=CARTESIAN_POINT('Ctrl Pts',(-10.3696826374235,-73.6190581353765,
12.));
#69638=CARTESIAN_POINT('Ctrl Pts',(-10.3119164592419,-73.6777313404382,
12.));
#69639=CARTESIAN_POINT('Ctrl Pts',(-10.234894888333,-73.7559622805204,12.));
#69640=CARTESIAN_POINT('Ctrl Pts',(-10.1314210536414,-73.8079696346555,
12.));
#69641=CARTESIAN_POINT('Ctrl Pts',(-10.0225374821204,-73.8227522002498,
12.));
#69642=CARTESIAN_POINT('Ctrl Pts',(-10.0225374821204,-73.8227522002498,
12.));
#69643=CARTESIAN_POINT('Ctrl Pts',(-10.0225374821204,-73.8227522002498,
8.));
#69644=CARTESIAN_POINT('Ctrl Pts',(-10.0225374821204,-73.8227522002498,
4.));
#69645=CARTESIAN_POINT('Ctrl Pts',(-10.0225374821204,-73.8227522002498,
-5.55111512312578E-16));
#69646=CARTESIAN_POINT('Ctrl Pts',(-11.3136138754165,-69.079679653846,0.));
#69647=CARTESIAN_POINT('Ctrl Pts',(-11.3136138754165,-69.079679653846,12.));
#69648=CARTESIAN_POINT('Ctrl Pts',(-11.3132375200165,-69.0835449954396,
0.));
#69649=CARTESIAN_POINT('Ctrl Pts',(-11.3132375200165,-69.0835449954396,
12.));
#69650=CARTESIAN_POINT('Ctrl Pts',(-11.3124821678798,-69.0912808656811,
0.));
#69651=CARTESIAN_POINT('Ctrl Pts',(-11.3124821678798,-69.0912808656811,
12.));
#69652=CARTESIAN_POINT('Ctrl Pts',(-11.3113412156661,-69.1029002322118,
0.));
#69653=CARTESIAN_POINT('Ctrl Pts',(-11.3113412156661,-69.1029002322118,
12.));
#69654=CARTESIAN_POINT('Ctrl Pts',(-11.3098040973713,-69.118423844466,0.));
#69655=CARTESIAN_POINT('Ctrl Pts',(-11.3098040973713,-69.118423844466,12.));
#69656=CARTESIAN_POINT('Ctrl Pts',(-11.3078562764384,-69.1378802251711,
0.));
#69657=CARTESIAN_POINT('Ctrl Pts',(-11.3078562764384,-69.1378802251711,
12.));
#69658=CARTESIAN_POINT('Ctrl Pts',(-11.3058820128307,-69.1573884361,0.));
#69659=CARTESIAN_POINT('Ctrl Pts',(-11.3058820128307,-69.1573884361,12.));
#69660=CARTESIAN_POINT('Ctrl Pts',(-11.3038812726292,-69.1769483991721,
0.));
#69661=CARTESIAN_POINT('Ctrl Pts',(-11.3038812726292,-69.1769483991721,
12.));
#69662=CARTESIAN_POINT('Ctrl Pts',(-11.3018540025638,-69.1965599718914,
0.));
#69663=CARTESIAN_POINT('Ctrl Pts',(-11.3018540025638,-69.1965599718914,
12.));
#69664=CARTESIAN_POINT('Ctrl Pts',(-11.2998001310964,-69.2162229488531,
0.));
#69665=CARTESIAN_POINT('Ctrl Pts',(-11.2998001310964,-69.2162229488531,
12.));
#69666=CARTESIAN_POINT('Ctrl Pts',(-11.2977195764852,-69.2359370894907,
0.));
#69667=CARTESIAN_POINT('Ctrl Pts',(-11.2977195764852,-69.2359370894907,
12.));
#69668=CARTESIAN_POINT('Ctrl Pts',(-11.2956122531375,-69.255702139335,0.));
#69669=CARTESIAN_POINT('Ctrl Pts',(-11.2956122531375,-69.255702139335,12.));
#69670=CARTESIAN_POINT('Ctrl Pts',(-11.2934780784351,-69.275517853148,0.));
#69671=CARTESIAN_POINT('Ctrl Pts',(-11.2934780784351,-69.275517853148,12.));
#69672=CARTESIAN_POINT('Ctrl Pts',(-11.2913169799628,-69.295384019272,0.));
#69673=CARTESIAN_POINT('Ctrl Pts',(-11.2913169799628,-69.295384019272,12.));
#69674=CARTESIAN_POINT('Ctrl Pts',(-11.2891288931517,-69.3153004517783,
0.));
#69675=CARTESIAN_POINT('Ctrl Pts',(-11.2891288931517,-69.3153004517783,
12.));
#69676=CARTESIAN_POINT('Ctrl Pts',(-11.2869137578459,-69.3352669789587,
0.));
#69677=CARTESIAN_POINT('Ctrl Pts',(-11.2869137578459,-69.3352669789587,
12.));
#69678=CARTESIAN_POINT('Ctrl Pts',(-11.2846715154524,-69.3552834337784,
0.));
#69679=CARTESIAN_POINT('Ctrl Pts',(-11.2846715154524,-69.3552834337784,
12.));
#69680=CARTESIAN_POINT('Ctrl Pts',(-11.2824021054045,-69.3753496420039,
0.));
#69681=CARTESIAN_POINT('Ctrl Pts',(-11.2824021054045,-69.3753496420039,
12.));
#69682=CARTESIAN_POINT('Ctrl Pts',(-11.2801054633815,-69.3954654162281,
0.));
#69683=CARTESIAN_POINT('Ctrl Pts',(-11.2801054633815,-69.3954654162281,
12.));
#69684=CARTESIAN_POINT('Ctrl Pts',(-11.2777815231469,-69.4156305620593,
0.));
#69685=CARTESIAN_POINT('Ctrl Pts',(-11.2777815231469,-69.4156305620593,
12.));
#69686=CARTESIAN_POINT('Ctrl Pts',(-11.2754302177021,-69.4358448819967,
0.));
#69687=CARTESIAN_POINT('Ctrl Pts',(-11.2754302177021,-69.4358448819967,
12.));
#69688=CARTESIAN_POINT('Ctrl Pts',(-11.2730514806139,-69.456108179879,0.));
#69689=CARTESIAN_POINT('Ctrl Pts',(-11.2730514806139,-69.456108179879,12.));
#69690=CARTESIAN_POINT('Ctrl Pts',(-11.270645247528,-69.4764202659397,0.));
#69691=CARTESIAN_POINT('Ctrl Pts',(-11.270645247528,-69.4764202659397,12.));
#69692=CARTESIAN_POINT('Ctrl Pts',(-11.2682114561007,-69.4967809565929,
0.));
#69693=CARTESIAN_POINT('Ctrl Pts',(-11.2682114561007,-69.4967809565929,
12.));
#69694=CARTESIAN_POINT('Ctrl Pts',(-11.2657500452716,-69.5171900720158,
0.));
#69695=CARTESIAN_POINT('Ctrl Pts',(-11.2657500452716,-69.5171900720158,
12.));
#69696=CARTESIAN_POINT('Ctrl Pts',(-11.263260954763,-69.5376474344771,0.));
#69697=CARTESIAN_POINT('Ctrl Pts',(-11.263260954763,-69.5376474344771,12.));
#69698=CARTESIAN_POINT('Ctrl Pts',(-11.2607441244702,-69.5581528662877,
0.));
#69699=CARTESIAN_POINT('Ctrl Pts',(-11.2607441244702,-69.5581528662877,
12.));
#69700=CARTESIAN_POINT('Ctrl Pts',(-11.2581994939541,-69.5787061880857,
0.));
#69701=CARTESIAN_POINT('Ctrl Pts',(-11.2581994939541,-69.5787061880857,
12.));
#69702=CARTESIAN_POINT('Ctrl Pts',(-11.2556270027016,-69.599307219739,0.));
#69703=CARTESIAN_POINT('Ctrl Pts',(-11.2556270027016,-69.599307219739,12.));
#69704=CARTESIAN_POINT('Ctrl Pts',(-11.2530265903557,-69.6199557811245,
0.));
#69705=CARTESIAN_POINT('Ctrl Pts',(-11.2530265903557,-69.6199557811245,
12.));
#69706=CARTESIAN_POINT('Ctrl Pts',(-11.2503981969412,-69.6406516928891,
0.));
#69707=CARTESIAN_POINT('Ctrl Pts',(-11.2503981969412,-69.6406516928891,
12.));
#69708=CARTESIAN_POINT('Ctrl Pts',(-11.2477417631386,-69.6613947773534,
0.));
#69709=CARTESIAN_POINT('Ctrl Pts',(-11.2477417631386,-69.6613947773534,
12.));
#69710=CARTESIAN_POINT('Ctrl Pts',(-11.2450572303841,-69.6821848588457,
0.));
#69711=CARTESIAN_POINT('Ctrl Pts',(-11.2450572303841,-69.6821848588457,
12.));
#69712=CARTESIAN_POINT('Ctrl Pts',(-11.2423445407166,-69.7030217632164,
0.));
#69713=CARTESIAN_POINT('Ctrl Pts',(-11.2423445407166,-69.7030217632164,
12.));
#69714=CARTESIAN_POINT('Ctrl Pts',(-11.239603636686,-69.7239053175356,0.));
#69715=CARTESIAN_POINT('Ctrl Pts',(-11.239603636686,-69.7239053175356,12.));
#69716=CARTESIAN_POINT('Ctrl Pts',(-11.2368344612472,-69.7448353497408,
0.));
#69717=CARTESIAN_POINT('Ctrl Pts',(-11.2368344612472,-69.7448353497408,
12.));
#69718=CARTESIAN_POINT('Ctrl Pts',(-11.2340369576456,-69.7658116882324,
0.));
#69719=CARTESIAN_POINT('Ctrl Pts',(-11.2340369576456,-69.7658116882324,
12.));
#69720=CARTESIAN_POINT('Ctrl Pts',(-11.2312110694187,-69.7868341618954,
0.));
#69721=CARTESIAN_POINT('Ctrl Pts',(-11.2312110694187,-69.7868341618954,
12.));
#69722=CARTESIAN_POINT('Ctrl Pts',(-11.2283567404437,-69.8079026002768,
0.));
#69723=CARTESIAN_POINT('Ctrl Pts',(-11.2283567404437,-69.8079026002768,
12.));
#69724=CARTESIAN_POINT('Ctrl Pts',(-11.225473914972,-69.8290168337076,0.));
#69725=CARTESIAN_POINT('Ctrl Pts',(-11.225473914972,-69.8290168337076,12.));
#69726=CARTESIAN_POINT('Ctrl Pts',(-11.2225625376736,-69.8501766934428,
0.));
#69727=CARTESIAN_POINT('Ctrl Pts',(-11.2225625376736,-69.8501766934428,
12.));
#69728=CARTESIAN_POINT('Ctrl Pts',(-11.219622553679,-69.871382011789,0.));
#69729=CARTESIAN_POINT('Ctrl Pts',(-11.219622553679,-69.871382011789,12.));
#69730=CARTESIAN_POINT('Ctrl Pts',(-11.2166539085523,-69.8926326220385,
0.));
#69731=CARTESIAN_POINT('Ctrl Pts',(-11.2166539085523,-69.8926326220385,
12.));
#69732=CARTESIAN_POINT('Ctrl Pts',(-11.2136565482677,-69.9139283584022,
0.));
#69733=CARTESIAN_POINT('Ctrl Pts',(-11.2136565482677,-69.9139283584022,
12.));
#69734=CARTESIAN_POINT('Ctrl Pts',(-11.2106304191882,-69.9352690559405,
0.));
#69735=CARTESIAN_POINT('Ctrl Pts',(-11.2106304191882,-69.9352690559405,
12.));
#69736=CARTESIAN_POINT('Ctrl Pts',(-11.2075754680449,-69.9566545504837,
0.));
#69737=CARTESIAN_POINT('Ctrl Pts',(-11.2075754680449,-69.9566545504837,
12.));
#69738=CARTESIAN_POINT('Ctrl Pts',(-11.2044916419244,-69.97808467858,0.));
#69739=CARTESIAN_POINT('Ctrl Pts',(-11.2044916419244,-69.97808467858,12.));
#69740=CARTESIAN_POINT('Ctrl Pts',(-11.2013788882714,-69.9995592775343,
0.));
#69741=CARTESIAN_POINT('Ctrl Pts',(-11.2013788882714,-69.9995592775343,
12.));
#69742=CARTESIAN_POINT('Ctrl Pts',(-11.1982371548919,-70.0210781854243,
0.));
#69743=CARTESIAN_POINT('Ctrl Pts',(-11.1982371548919,-70.0210781854243,
12.));
#69744=CARTESIAN_POINT('Ctrl Pts',(-11.1950663899576,-70.0426412411185,
0.));
#69745=CARTESIAN_POINT('Ctrl Pts',(-11.1950663899576,-70.0426412411185,
12.));
#69746=CARTESIAN_POINT('Ctrl Pts',(-11.1918665420166,-70.0642482842928,
0.));
#69747=CARTESIAN_POINT('Ctrl Pts',(-11.1918665420166,-70.0642482842928,
12.));
#69748=CARTESIAN_POINT('Ctrl Pts',(-11.1886375599914,-70.0858991554283,
0.));
#69749=CARTESIAN_POINT('Ctrl Pts',(-11.1886375599914,-70.0858991554283,
12.));
#69750=CARTESIAN_POINT('Ctrl Pts',(-11.185379393167,-70.1075936957968,0.));
#69751=CARTESIAN_POINT('Ctrl Pts',(-11.185379393167,-70.1075936957968,12.));
#69752=CARTESIAN_POINT('Ctrl Pts',(-11.1820919911846,-70.1293317474432,
0.));
#69753=CARTESIAN_POINT('Ctrl Pts',(-11.1820919911846,-70.1293317474432,
12.));
#69754=CARTESIAN_POINT('Ctrl Pts',(-11.1787753040363,-70.1511131531674,
0.));
#69755=CARTESIAN_POINT('Ctrl Pts',(-11.1787753040363,-70.1511131531674,
12.));
#69756=CARTESIAN_POINT('Ctrl Pts',(-11.1754292820631,-70.1729377564956,
0.));
#69757=CARTESIAN_POINT('Ctrl Pts',(-11.1754292820631,-70.1729377564956,
12.));
#69758=CARTESIAN_POINT('Ctrl Pts',(-11.1720538759498,-70.1948054016817,
0.));
#69759=CARTESIAN_POINT('Ctrl Pts',(-11.1720538759498,-70.1948054016817,
12.));
#69760=CARTESIAN_POINT('Ctrl Pts',(-11.168649036721,-70.2167159337095,0.));
#69761=CARTESIAN_POINT('Ctrl Pts',(-11.168649036721,-70.2167159337095,12.));
#69762=CARTESIAN_POINT('Ctrl Pts',(-11.1652147157383,-70.2386691982902,
0.));
#69763=CARTESIAN_POINT('Ctrl Pts',(-11.1652147157383,-70.2386691982902,
12.));
#69764=CARTESIAN_POINT('Ctrl Pts',(-11.1617508647017,-70.2606650418589,
0.));
#69765=CARTESIAN_POINT('Ctrl Pts',(-11.1617508647017,-70.2606650418589,
12.));
#69766=CARTESIAN_POINT('Ctrl Pts',(-11.1582574356522,-70.2827033115662,
0.));
#69767=CARTESIAN_POINT('Ctrl Pts',(-11.1582574356522,-70.2827033115662,
12.));
#69768=CARTESIAN_POINT('Ctrl Pts',(-11.1547343809647,-70.3047838552758,
0.));
#69769=CARTESIAN_POINT('Ctrl Pts',(-11.1547343809647,-70.3047838552758,
12.));
#69770=CARTESIAN_POINT('Ctrl Pts',(-11.1511816533422,-70.3269065215591,
0.));
#69771=CARTESIAN_POINT('Ctrl Pts',(-11.1511816533422,-70.3269065215591,
12.));
#69772=CARTESIAN_POINT('Ctrl Pts',(-11.1475992058124,-70.3490711596882,
0.));
#69773=CARTESIAN_POINT('Ctrl Pts',(-11.1475992058124,-70.3490711596882,
12.));
#69774=CARTESIAN_POINT('Ctrl Pts',(-11.1439869917269,-70.3712776196216,
0.));
#69775=CARTESIAN_POINT('Ctrl Pts',(-11.1439869917269,-70.3712776196216,
12.));
#69776=CARTESIAN_POINT('Ctrl Pts',(-11.1403449647622,-70.3935257519945,
0.));
#69777=CARTESIAN_POINT('Ctrl Pts',(-11.1403449647622,-70.3935257519945,
12.));
#69778=CARTESIAN_POINT('Ctrl Pts',(-11.1366730789122,-70.415815408119,0.));
#69779=CARTESIAN_POINT('Ctrl Pts',(-11.1366730789122,-70.415815408119,12.));
#69780=CARTESIAN_POINT('Ctrl Pts',(-11.1329712884845,-70.438146439981,0.));
#69781=CARTESIAN_POINT('Ctrl Pts',(-11.1329712884845,-70.438146439981,12.));
#69782=CARTESIAN_POINT('Ctrl Pts',(-11.1292395480975,-70.4605187002356,
0.));
#69783=CARTESIAN_POINT('Ctrl Pts',(-11.1292395480975,-70.4605187002356,
12.));
#69784=CARTESIAN_POINT('Ctrl Pts',(-11.1254778126824,-70.4829320421973,
0.));
#69785=CARTESIAN_POINT('Ctrl Pts',(-11.1254778126824,-70.4829320421973,
12.));
#69786=CARTESIAN_POINT('Ctrl Pts',(-11.121686037483,-70.5053863198306,0.));
#69787=CARTESIAN_POINT('Ctrl Pts',(-11.121686037483,-70.5053863198306,12.));
#69788=CARTESIAN_POINT('Ctrl Pts',(-11.117864178048,-70.5278813877519,0.));
#69789=CARTESIAN_POINT('Ctrl Pts',(-11.117864178048,-70.5278813877519,12.));
#69790=CARTESIAN_POINT('Ctrl Pts',(-11.1140121902274,-70.5504171012247,
0.));
#69791=CARTESIAN_POINT('Ctrl Pts',(-11.1140121902274,-70.5504171012247,
12.));
#69792=CARTESIAN_POINT('Ctrl Pts',(-11.11013003017,-70.5729933161538,0.));
#69793=CARTESIAN_POINT('Ctrl Pts',(-11.11013003017,-70.5729933161538,12.));
#69794=CARTESIAN_POINT('Ctrl Pts',(-11.1062176543257,-70.5956098890744,
0.));
#69795=CARTESIAN_POINT('Ctrl Pts',(-11.1062176543257,-70.5956098890744,
12.));
#69796=CARTESIAN_POINT('Ctrl Pts',(-11.1022750194439,-70.6182666771441,
0.));
#69797=CARTESIAN_POINT('Ctrl Pts',(-11.1022750194439,-70.6182666771441,
12.));
#69798=CARTESIAN_POINT('Ctrl Pts',(-11.0983020825662,-70.6409635381446,
0.));
#69799=CARTESIAN_POINT('Ctrl Pts',(-11.0983020825662,-70.6409635381446,
12.));
#69800=CARTESIAN_POINT('Ctrl Pts',(-11.0942988010231,-70.6637003304768,
0.));
#69801=CARTESIAN_POINT('Ctrl Pts',(-11.0942988010231,-70.6637003304768,
12.));
#69802=CARTESIAN_POINT('Ctrl Pts',(-11.0902651324325,-70.686476913156,0.));
#69803=CARTESIAN_POINT('Ctrl Pts',(-11.0902651324325,-70.686476913156,12.));
#69804=CARTESIAN_POINT('Ctrl Pts',(-11.0862010347022,-70.7092931457996,
0.));
#69805=CARTESIAN_POINT('Ctrl Pts',(-11.0862010347022,-70.7092931457996,
12.));
#69806=CARTESIAN_POINT('Ctrl Pts',(-11.0821064660276,-70.7321488886229,
0.));
#69807=CARTESIAN_POINT('Ctrl Pts',(-11.0821064660276,-70.7321488886229,
12.));
#69808=CARTESIAN_POINT('Ctrl Pts',(-11.0779813848851,-70.7550440024422,
0.));
#69809=CARTESIAN_POINT('Ctrl Pts',(-11.0779813848851,-70.7550440024422,
12.));
#69810=CARTESIAN_POINT('Ctrl Pts',(-11.0738257500292,-70.7779783486689,
0.));
#69811=CARTESIAN_POINT('Ctrl Pts',(-11.0738257500292,-70.7779783486689,
12.));
#69812=CARTESIAN_POINT('Ctrl Pts',(-11.0696395204907,-70.8009517893042,
0.));
#69813=CARTESIAN_POINT('Ctrl Pts',(-11.0696395204907,-70.8009517893042,
12.));
#69814=CARTESIAN_POINT('Ctrl Pts',(-11.0654226555798,-70.8239641869266,
0.));
#69815=CARTESIAN_POINT('Ctrl Pts',(-11.0654226555798,-70.8239641869266,
12.));
#69816=CARTESIAN_POINT('Ctrl Pts',(-11.061175114883,-70.847015404688,0.));
#69817=CARTESIAN_POINT('Ctrl Pts',(-11.061175114883,-70.847015404688,12.));
#69818=CARTESIAN_POINT('Ctrl Pts',(-11.0568968582566,-70.8701053063158,
0.));
#69819=CARTESIAN_POINT('Ctrl Pts',(-11.0568968582566,-70.8701053063158,
12.));
#69820=CARTESIAN_POINT('Ctrl Pts',(-11.0525878458242,-70.8932337561078,
0.));
#69821=CARTESIAN_POINT('Ctrl Pts',(-11.0525878458242,-70.8932337561078,
12.));
#69822=CARTESIAN_POINT('Ctrl Pts',(-11.0482480379752,-70.9164006189283,
0.));
#69823=CARTESIAN_POINT('Ctrl Pts',(-11.0482480379752,-70.9164006189283,
12.));
#69824=CARTESIAN_POINT('Ctrl Pts',(-11.0438773953686,-70.9396057601953,
0.));
#69825=CARTESIAN_POINT('Ctrl Pts',(-11.0438773953686,-70.9396057601953,
12.));
#69826=CARTESIAN_POINT('Ctrl Pts',(-11.039475878929,-70.9628490458779,0.));
#69827=CARTESIAN_POINT('Ctrl Pts',(-11.039475878929,-70.9628490458779,12.));
#69828=CARTESIAN_POINT('Ctrl Pts',(-11.0350434498408,-70.9861303424989,
0.));
#69829=CARTESIAN_POINT('Ctrl Pts',(-11.0350434498408,-70.9861303424989,
12.));
#69830=CARTESIAN_POINT('Ctrl Pts',(-11.0305800695457,-71.0094495171295,
0.));
#69831=CARTESIAN_POINT('Ctrl Pts',(-11.0305800695457,-71.0094495171295,
12.));
#69832=CARTESIAN_POINT('Ctrl Pts',(-11.0260856997414,-71.0328064373849,
0.));
#69833=CARTESIAN_POINT('Ctrl Pts',(-11.0260856997414,-71.0328064373849,
12.));
#69834=CARTESIAN_POINT('Ctrl Pts',(-11.0215603023854,-71.0562009714125,
0.));
#69835=CARTESIAN_POINT('Ctrl Pts',(-11.0215603023854,-71.0562009714125,
12.));
#69836=CARTESIAN_POINT('Ctrl Pts',(-11.0170038396913,-71.0796329878896,
0.));
#69837=CARTESIAN_POINT('Ctrl Pts',(-11.0170038396913,-71.0796329878896,
12.));
#69838=CARTESIAN_POINT('Ctrl Pts',(-11.0124162741223,-71.1031023560243,
0.));
#69839=CARTESIAN_POINT('Ctrl Pts',(-11.0124162741223,-71.1031023560243,
12.));
#69840=CARTESIAN_POINT('Ctrl Pts',(-11.0077975683895,-71.1266089455517,
0.));
#69841=CARTESIAN_POINT('Ctrl Pts',(-11.0077975683895,-71.1266089455517,
12.));
#69842=CARTESIAN_POINT('Ctrl Pts',(-11.0031476854503,-71.1501526267288,
0.));
#69843=CARTESIAN_POINT('Ctrl Pts',(-11.0031476854503,-71.1501526267288,
12.));
#69844=CARTESIAN_POINT('Ctrl Pts',(-10.9984665885127,-71.1737332703248,
0.));
#69845=CARTESIAN_POINT('Ctrl Pts',(-10.9984665885127,-71.1737332703248,
12.));
#69846=CARTESIAN_POINT('Ctrl Pts',(-10.993754241032,-71.1973507476188,0.));
#69847=CARTESIAN_POINT('Ctrl Pts',(-10.993754241032,-71.1973507476188,12.));
#69848=CARTESIAN_POINT('Ctrl Pts',(-10.9890106067038,-71.221004930401,0.));
#69849=CARTESIAN_POINT('Ctrl Pts',(-10.9890106067038,-71.221004930401,12.));
#69850=CARTESIAN_POINT('Ctrl Pts',(-10.9842356494627,-71.2446956909685,
0.));
#69851=CARTESIAN_POINT('Ctrl Pts',(-10.9842356494627,-71.2446956909685,
12.));
#69852=CARTESIAN_POINT('Ctrl Pts',(-10.9794293334806,-71.2684229021209,
0.));
#69853=CARTESIAN_POINT('Ctrl Pts',(-10.9794293334806,-71.2684229021209,
12.));
#69854=CARTESIAN_POINT('Ctrl Pts',(-10.9745916231711,-71.2921864371499,
0.));
#69855=CARTESIAN_POINT('Ctrl Pts',(-10.9745916231711,-71.2921864371499,
12.));
#69856=CARTESIAN_POINT('Ctrl Pts',(-10.9697224831862,-71.3159861698368,
0.));
#69857=CARTESIAN_POINT('Ctrl Pts',(-10.9697224831862,-71.3159861698368,
12.));
#69858=CARTESIAN_POINT('Ctrl Pts',(-10.96482187841,-71.3398219744547,0.));
#69859=CARTESIAN_POINT('Ctrl Pts',(-10.96482187841,-71.3398219744547,12.));
#69860=CARTESIAN_POINT('Ctrl Pts',(-10.9598897739565,-71.3636937257651,
0.));
#69861=CARTESIAN_POINT('Ctrl Pts',(-10.9598897739565,-71.3636937257651,
12.));
#69862=CARTESIAN_POINT('Ctrl Pts',(-10.9549261351689,-71.3876012990135,
0.));
#69863=CARTESIAN_POINT('Ctrl Pts',(-10.9549261351689,-71.3876012990135,
12.));
#69864=CARTESIAN_POINT('Ctrl Pts',(-10.9499309276235,-71.411544569919,0.));
#69865=CARTESIAN_POINT('Ctrl Pts',(-10.9499309276235,-71.411544569919,12.));
#69866=CARTESIAN_POINT('Ctrl Pts',(-10.9449041171269,-71.4355234146718,
0.));
#69867=CARTESIAN_POINT('Ctrl Pts',(-10.9449041171269,-71.4355234146718,
12.));
#69868=CARTESIAN_POINT('Ctrl Pts',(-10.9398456697094,-71.4595377099352,
0.));
#69869=CARTESIAN_POINT('Ctrl Pts',(-10.9398456697094,-71.4595377099352,
12.));
#69870=CARTESIAN_POINT('Ctrl Pts',(-10.9347555516236,-71.4835873328425,
0.));
#69871=CARTESIAN_POINT('Ctrl Pts',(-10.9347555516236,-71.4835873328425,
12.));
#69872=CARTESIAN_POINT('Ctrl Pts',(-10.9296337293425,-71.5076721609936,
0.));
#69873=CARTESIAN_POINT('Ctrl Pts',(-10.9296337293425,-71.5076721609936,
12.));
#69874=CARTESIAN_POINT('Ctrl Pts',(-10.9244801695642,-71.5317920724453,
0.));
#69875=CARTESIAN_POINT('Ctrl Pts',(-10.9244801695642,-71.5317920724453,
12.));
#69876=CARTESIAN_POINT('Ctrl Pts',(-10.9192948392099,-71.5559469457082,
0.));
#69877=CARTESIAN_POINT('Ctrl Pts',(-10.9192948392099,-71.5559469457082,
12.));
#69878=CARTESIAN_POINT('Ctrl Pts',(-10.9140777054169,-71.5801366597479,
0.));
#69879=CARTESIAN_POINT('Ctrl Pts',(-10.9140777054169,-71.5801366597479,
12.));
#69880=CARTESIAN_POINT('Ctrl Pts',(-10.9088287355364,-71.604361093983,0.));
#69881=CARTESIAN_POINT('Ctrl Pts',(-10.9088287355364,-71.604361093983,12.));
#69882=CARTESIAN_POINT('Ctrl Pts',(-10.9035478971329,-71.6286201282815,
0.));
#69883=CARTESIAN_POINT('Ctrl Pts',(-10.9035478971329,-71.6286201282815,
12.));
#69884=CARTESIAN_POINT('Ctrl Pts',(-10.8982351579872,-71.6529136429515,
0.));
#69885=CARTESIAN_POINT('Ctrl Pts',(-10.8982351579872,-71.6529136429515,
12.));
#69886=CARTESIAN_POINT('Ctrl Pts',(-10.8928904860967,-71.6772415187382,
0.));
#69887=CARTESIAN_POINT('Ctrl Pts',(-10.8928904860967,-71.6772415187382,
12.));
#69888=CARTESIAN_POINT('Ctrl Pts',(-10.8875138496674,-71.7016036368254,
0.));
#69889=CARTESIAN_POINT('Ctrl Pts',(-10.8875138496674,-71.7016036368254,
12.));
#69890=CARTESIAN_POINT('Ctrl Pts',(-10.8821052171122,-71.7259998788337,
0.));
#69891=CARTESIAN_POINT('Ctrl Pts',(-10.8821052171122,-71.7259998788337,
12.));
#69892=CARTESIAN_POINT('Ctrl Pts',(-10.8766645570496,-71.7504301268177,
0.));
#69893=CARTESIAN_POINT('Ctrl Pts',(-10.8766645570496,-71.7504301268177,
12.));
#69894=CARTESIAN_POINT('Ctrl Pts',(-10.8711918383071,-71.7748942632578,
0.));
#69895=CARTESIAN_POINT('Ctrl Pts',(-10.8711918383071,-71.7748942632578,
12.));
#69896=CARTESIAN_POINT('Ctrl Pts',(-10.8656870299218,-71.7993921710546,
0.));
#69897=CARTESIAN_POINT('Ctrl Pts',(-10.8656870299218,-71.7993921710546,
12.));
#69898=CARTESIAN_POINT('Ctrl Pts',(-10.860150101133,-71.8239237335318,0.));
#69899=CARTESIAN_POINT('Ctrl Pts',(-10.860150101133,-71.8239237335318,12.));
#69900=CARTESIAN_POINT('Ctrl Pts',(-10.8545810213799,-71.8484888344335,
0.));
#69901=CARTESIAN_POINT('Ctrl Pts',(-10.8545810213799,-71.8484888344335,
12.));
#69902=CARTESIAN_POINT('Ctrl Pts',(-10.8489797602998,-71.8730873579226,
0.));
#69903=CARTESIAN_POINT('Ctrl Pts',(-10.8489797602998,-71.8730873579226,
12.));
#69904=CARTESIAN_POINT('Ctrl Pts',(-10.8433462877312,-71.8977191885726,
0.));
#69905=CARTESIAN_POINT('Ctrl Pts',(-10.8433462877312,-71.8977191885726,
12.));
#69906=CARTESIAN_POINT('Ctrl Pts',(-10.8376805737158,-71.9223842113622,
0.));
#69907=CARTESIAN_POINT('Ctrl Pts',(-10.8376805737158,-71.9223842113622,
12.));
#69908=CARTESIAN_POINT('Ctrl Pts',(-10.8319825884917,-71.9470823116777,
0.));
#69909=CARTESIAN_POINT('Ctrl Pts',(-10.8319825884917,-71.9470823116777,
12.));
#69910=CARTESIAN_POINT('Ctrl Pts',(-10.8262523024897,-71.971813375312,0.));
#69911=CARTESIAN_POINT('Ctrl Pts',(-10.8262523024897,-71.971813375312,12.));
#69912=CARTESIAN_POINT('Ctrl Pts',(-10.8204896863328,-71.9965772884619,
0.));
#69913=CARTESIAN_POINT('Ctrl Pts',(-10.8204896863328,-71.9965772884619,
12.));
#69914=CARTESIAN_POINT('Ctrl Pts',(-10.8146947108376,-72.0213739377231,
0.));
#69915=CARTESIAN_POINT('Ctrl Pts',(-10.8146947108376,-72.0213739377231,
12.));
#69916=CARTESIAN_POINT('Ctrl Pts',(-10.8088673470187,-72.0462032100828,
0.));
#69917=CARTESIAN_POINT('Ctrl Pts',(-10.8088673470187,-72.0462032100828,
12.));
#69918=CARTESIAN_POINT('Ctrl Pts',(-10.8030075660811,-72.0710649929214,
0.));
#69919=CARTESIAN_POINT('Ctrl Pts',(-10.8030075660811,-72.0710649929214,
12.));
#69920=CARTESIAN_POINT('Ctrl Pts',(-10.7971153394168,-72.095959174012,0.));
#69921=CARTESIAN_POINT('Ctrl Pts',(-10.7971153394168,-72.095959174012,12.));
#69922=CARTESIAN_POINT('Ctrl Pts',(-10.7911906386027,-72.1208856415171,
0.));
#69923=CARTESIAN_POINT('Ctrl Pts',(-10.7911906386027,-72.1208856415171,
12.));
#69924=CARTESIAN_POINT('Ctrl Pts',(-10.7852334354015,-72.145844283983,0.));
#69925=CARTESIAN_POINT('Ctrl Pts',(-10.7852334354015,-72.145844283983,12.));
#69926=CARTESIAN_POINT('Ctrl Pts',(-10.779243701766,-72.17083499033,0.));
#69927=CARTESIAN_POINT('Ctrl Pts',(-10.779243701766,-72.17083499033,12.));
#69928=CARTESIAN_POINT('Ctrl Pts',(-10.7732214098343,-72.1958576498556,
0.));
#69929=CARTESIAN_POINT('Ctrl Pts',(-10.7732214098343,-72.1958576498556,
12.));
#69930=CARTESIAN_POINT('Ctrl Pts',(-10.7671665319254,-72.2209121522367,
0.));
#69931=CARTESIAN_POINT('Ctrl Pts',(-10.7671665319254,-72.2209121522367,
12.));
#69932=CARTESIAN_POINT('Ctrl Pts',(-10.7610790405385,-72.2459983875298,
0.));
#69933=CARTESIAN_POINT('Ctrl Pts',(-10.7610790405385,-72.2459983875298,
12.));
#69934=CARTESIAN_POINT('Ctrl Pts',(-10.7549589083535,-72.2711162461679,
0.));
#69935=CARTESIAN_POINT('Ctrl Pts',(-10.7549589083535,-72.2711162461679,
12.));
#69936=CARTESIAN_POINT('Ctrl Pts',(-10.7488061082368,-72.296265618955,0.));
#69937=CARTESIAN_POINT('Ctrl Pts',(-10.7488061082368,-72.296265618955,12.));
#69938=CARTESIAN_POINT('Ctrl Pts',(-10.7426206132375,-72.3214463970634,
0.));
#69939=CARTESIAN_POINT('Ctrl Pts',(-10.7426206132375,-72.3214463970634,
12.));
#69940=CARTESIAN_POINT('Ctrl Pts',(-10.73640239658,-72.3466584720311,0.));
#69941=CARTESIAN_POINT('Ctrl Pts',(-10.73640239658,-72.3466584720311,12.));
#69942=CARTESIAN_POINT('Ctrl Pts',(-10.7301514316607,-72.3719017357568,
0.));
#69943=CARTESIAN_POINT('Ctrl Pts',(-10.7301514316607,-72.3719017357568,
12.));
#69944=CARTESIAN_POINT('Ctrl Pts',(-10.7238676920469,-72.3971760804935,
0.));
#69945=CARTESIAN_POINT('Ctrl Pts',(-10.7238676920469,-72.3971760804935,
12.));
#69946=CARTESIAN_POINT('Ctrl Pts',(-10.7175511514789,-72.4224813988355,
0.));
#69947=CARTESIAN_POINT('Ctrl Pts',(-10.7175511514789,-72.4224813988355,
12.));
#69948=CARTESIAN_POINT('Ctrl Pts',(-10.7112017838707,-72.4478175837168,
0.));
#69949=CARTESIAN_POINT('Ctrl Pts',(-10.7112017838707,-72.4478175837168,
12.));
#69950=CARTESIAN_POINT('Ctrl Pts',(-10.7048195633062,-72.4731845284238,
0.));
#69951=CARTESIAN_POINT('Ctrl Pts',(-10.7048195633062,-72.4731845284238,
12.));
#69952=CARTESIAN_POINT('Ctrl Pts',(-10.6984044640399,-72.4985821266031,
0.));
#69953=CARTESIAN_POINT('Ctrl Pts',(-10.6984044640399,-72.4985821266031,
12.));
#69954=CARTESIAN_POINT('Ctrl Pts',(-10.691956460499,-72.5240102722662,0.));
#69955=CARTESIAN_POINT('Ctrl Pts',(-10.691956460499,-72.5240102722662,12.));
#69956=CARTESIAN_POINT('Ctrl Pts',(-10.6854755272903,-72.5494688597951,
0.));
#69957=CARTESIAN_POINT('Ctrl Pts',(-10.6854755272903,-72.5494688597951,
12.));
#69958=CARTESIAN_POINT('Ctrl Pts',(-10.6789616392041,-72.57495778394,0.));
#69959=CARTESIAN_POINT('Ctrl Pts',(-10.6789616392041,-72.57495778394,12.));
#69960=CARTESIAN_POINT('Ctrl Pts',(-10.6724147711994,-72.6004769398004,
0.));
#69961=CARTESIAN_POINT('Ctrl Pts',(-10.6724147711994,-72.6004769398004,
12.));
#69962=CARTESIAN_POINT('Ctrl Pts',(-10.6658348983944,-72.6260262228055,
0.));
#69963=CARTESIAN_POINT('Ctrl Pts',(-10.6658348983944,-72.6260262228055,
12.));
#69964=CARTESIAN_POINT('Ctrl Pts',(-10.659221996058,-72.6516055286908,0.));
#69965=CARTESIAN_POINT('Ctrl Pts',(-10.659221996058,-72.6516055286908,12.));
#69966=CARTESIAN_POINT('Ctrl Pts',(-10.6525760396055,-72.6772147534762,
0.));
#69967=CARTESIAN_POINT('Ctrl Pts',(-10.6525760396055,-72.6772147534762,
12.));
#69968=CARTESIAN_POINT('Ctrl Pts',(-10.6458970045948,-72.7028537934332,
0.));
#69969=CARTESIAN_POINT('Ctrl Pts',(-10.6458970045948,-72.7028537934332,
12.));
#69970=CARTESIAN_POINT('Ctrl Pts',(-10.6391848667354,-72.7285225451309,
0.));
#69971=CARTESIAN_POINT('Ctrl Pts',(-10.6391848667354,-72.7285225451309,
12.));
#69972=CARTESIAN_POINT('Ctrl Pts',(-10.6324396018999,-72.7542209054823,
0.));
#69973=CARTESIAN_POINT('Ctrl Pts',(-10.6324396018999,-72.7542209054823,
12.));
#69974=CARTESIAN_POINT('Ctrl Pts',(-10.6256611861395,-72.7799487717914,
0.));
#69975=CARTESIAN_POINT('Ctrl Pts',(-10.6256611861395,-72.7799487717914,
12.));
#69976=CARTESIAN_POINT('Ctrl Pts',(-10.6188495956973,-72.8057060417882,
0.));
#69977=CARTESIAN_POINT('Ctrl Pts',(-10.6188495956973,-72.8057060417882,
12.));
#69978=CARTESIAN_POINT('Ctrl Pts',(-10.6120048070366,-72.8314926136872,
0.));
#69979=CARTESIAN_POINT('Ctrl Pts',(-10.6120048070366,-72.8314926136872,
12.));
#69980=CARTESIAN_POINT('Ctrl Pts',(-10.6051267968202,-72.8573083861328,
0.));
#69981=CARTESIAN_POINT('Ctrl Pts',(-10.6051267968202,-72.8573083861328,
12.));
#69982=CARTESIAN_POINT('Ctrl Pts',(-10.5982155418625,-72.8831532580839,
0.));
#69983=CARTESIAN_POINT('Ctrl Pts',(-10.5982155418625,-72.8831532580839,
12.));
#69984=CARTESIAN_POINT('Ctrl Pts',(-10.5912710190928,-72.9090271287081,
0.));
#69985=CARTESIAN_POINT('Ctrl Pts',(-10.5912710190928,-72.9090271287081,
12.));
#69986=CARTESIAN_POINT('Ctrl Pts',(-10.5842932055209,-72.9349298972823,
0.));
#69987=CARTESIAN_POINT('Ctrl Pts',(-10.5842932055209,-72.9349298972823,
12.));
#69988=CARTESIAN_POINT('Ctrl Pts',(-10.5772820781959,-72.9608614630539,
0.));
#69989=CARTESIAN_POINT('Ctrl Pts',(-10.5772820781959,-72.9608614630539,
12.));
#69990=CARTESIAN_POINT('Ctrl Pts',(-10.5702376142052,-72.9868217252293,
0.));
#69991=CARTESIAN_POINT('Ctrl Pts',(-10.5702376142052,-72.9868217252293,
12.));
#69992=CARTESIAN_POINT('Ctrl Pts',(-10.5631597907653,-73.0128105832635,
0.));
#69993=CARTESIAN_POINT('Ctrl Pts',(-10.5631597907653,-73.0128105832635,
12.));
#69994=CARTESIAN_POINT('Ctrl Pts',(-10.5560485852975,-73.0388279370845,
0.));
#69995=CARTESIAN_POINT('Ctrl Pts',(-10.5560485852975,-73.0388279370845,
12.));
#69996=CARTESIAN_POINT('Ctrl Pts',(-10.5489039755138,-73.0648736873435,
0.));
#69997=CARTESIAN_POINT('Ctrl Pts',(-10.5489039755138,-73.0648736873435,
12.));
#69998=CARTESIAN_POINT('Ctrl Pts',(-10.5417259395001,-73.090947735646,0.));
#69999=CARTESIAN_POINT('Ctrl Pts',(-10.5417259395001,-73.090947735646,12.));
#70000=CARTESIAN_POINT('Ctrl Pts',(-10.5345144558097,-73.1170499848012,
0.));
#70001=CARTESIAN_POINT('Ctrl Pts',(-10.5345144558097,-73.1170499848012,
12.));
#70002=CARTESIAN_POINT('Ctrl Pts',(-10.5272695032649,-73.1431803382677,
0.));
#70003=CARTESIAN_POINT('Ctrl Pts',(-10.5272695032649,-73.1431803382677,
12.));
#70004=CARTESIAN_POINT('Ctrl Pts',(-10.5199910607652,-73.169338699611,0.));
#70005=CARTESIAN_POINT('Ctrl Pts',(-10.5199910607652,-73.169338699611,12.));
#70006=CARTESIAN_POINT('Ctrl Pts',(-10.5126791070804,-73.1955249719037,
0.));
#70007=CARTESIAN_POINT('Ctrl Pts',(-10.5126791070804,-73.1955249719037,
12.));
#70008=CARTESIAN_POINT('Ctrl Pts',(-10.505333620691,-73.2217390572578,0.));
#70009=CARTESIAN_POINT('Ctrl Pts',(-10.505333620691,-73.2217390572578,12.));
#70010=CARTESIAN_POINT('Ctrl Pts',(-10.4979545795197,-73.247980856023,0.));
#70011=CARTESIAN_POINT('Ctrl Pts',(-10.4979545795197,-73.247980856023,12.));
#70012=CARTESIAN_POINT('Ctrl Pts',(-10.4905419611529,-73.2742502674361,
0.));
#70013=CARTESIAN_POINT('Ctrl Pts',(-10.4905419611529,-73.2742502674361,
12.));
#70014=CARTESIAN_POINT('Ctrl Pts',(-10.4830957433311,-73.3005471910639,
0.));
#70015=CARTESIAN_POINT('Ctrl Pts',(-10.4830957433311,-73.3005471910639,
12.));
#70016=CARTESIAN_POINT('Ctrl Pts',(-10.475615904381,-73.3268715280609,0.));
#70017=CARTESIAN_POINT('Ctrl Pts',(-10.475615904381,-73.3268715280609,12.));
#70018=CARTESIAN_POINT('Ctrl Pts',(-10.4681024236288,-73.353223182365,0.));
#70019=CARTESIAN_POINT('Ctrl Pts',(-10.4681024236288,-73.353223182365,12.));
#70020=CARTESIAN_POINT('Ctrl Pts',(-10.460555281939,-73.3796020622437,0.));
#70021=CARTESIAN_POINT('Ctrl Pts',(-10.460555281939,-73.3796020622437,12.));
#70022=CARTESIAN_POINT('Ctrl Pts',(-10.4529744618438,-73.4060080806577,
0.));
#70023=CARTESIAN_POINT('Ctrl Pts',(-10.4529744618438,-73.4060080806577,
12.));
#70024=CARTESIAN_POINT('Ctrl Pts',(-10.4453599463534,-73.432441151843,0.));
#70025=CARTESIAN_POINT('Ctrl Pts',(-10.4453599463534,-73.432441151843,12.));
#70026=CARTESIAN_POINT('Ctrl Pts',(-10.4377117180212,-73.45890118861,0.));
#70027=CARTESIAN_POINT('Ctrl Pts',(-10.4377117180212,-73.45890118861,12.));
#70028=CARTESIAN_POINT('Ctrl Pts',(-10.4300297578648,-73.4853880992228,
0.));
#70029=CARTESIAN_POINT('Ctrl Pts',(-10.4300297578648,-73.4853880992228,
12.));
#70030=CARTESIAN_POINT('Ctrl Pts',(-10.4223140444615,-73.5119017847664,
0.));
#70031=CARTESIAN_POINT('Ctrl Pts',(-10.4223140444615,-73.5119017847664,
12.));
#70032=CARTESIAN_POINT('Ctrl Pts',(-10.4145645526831,-73.5384421354746,
0.));
#70033=CARTESIAN_POINT('Ctrl Pts',(-10.4145645526831,-73.5384421354746,
12.));
#70034=CARTESIAN_POINT('Ctrl Pts',(-10.4067812555539,-73.5650090360114,
0.));
#70035=CARTESIAN_POINT('Ctrl Pts',(-10.4067812555539,-73.5650090360114,
12.));
#70036=CARTESIAN_POINT('Ctrl Pts',(-10.3989641265313,-73.5916023719976,
0.));
#70037=CARTESIAN_POINT('Ctrl Pts',(-10.3989641265313,-73.5916023719976,
12.));
#70038=CARTESIAN_POINT('Ctrl Pts',(-10.3911131417478,-73.6182220363295,
0.));
#70039=CARTESIAN_POINT('Ctrl Pts',(-10.3911131417478,-73.6182220363295,
12.));
#70040=CARTESIAN_POINT('Ctrl Pts',(-10.3832282820361,-73.6448679350605,
0.));
#70041=CARTESIAN_POINT('Ctrl Pts',(-10.3832282820361,-73.6448679350605,
12.));
#70042=CARTESIAN_POINT('Ctrl Pts',(-10.3753095356302,-73.6715399947459,
0.));
#70043=CARTESIAN_POINT('Ctrl Pts',(-10.3753095356302,-73.6715399947459,
12.));
#70044=CARTESIAN_POINT('Ctrl Pts',(-10.3673568984515,-73.6982381644571,
0.));
#70045=CARTESIAN_POINT('Ctrl Pts',(-10.3673568984515,-73.6982381644571,
12.));
#70046=CARTESIAN_POINT('Ctrl Pts',(-10.3593703712542,-73.7249624108433,
0.));
#70047=CARTESIAN_POINT('Ctrl Pts',(-10.3593703712542,-73.7249624108433,
12.));
#70048=CARTESIAN_POINT('Ctrl Pts',(-10.3529540403026,-73.7463626541235,
0.));
#70049=CARTESIAN_POINT('Ctrl Pts',(-10.3529540403026,-73.7463626541235,
12.));
#70050=CARTESIAN_POINT('Ctrl Pts',(-10.3481265449303,-73.7624245587416,
0.));
#70051=CARTESIAN_POINT('Ctrl Pts',(-10.3481265449303,-73.7624245587416,
12.));
#70052=CARTESIAN_POINT('Ctrl Pts',(-10.3449014384438,-73.7731377047922,
0.));
#70053=CARTESIAN_POINT('Ctrl Pts',(-10.3449014384438,-73.7731377047922,
12.));
#70054=CARTESIAN_POINT('Ctrl Pts',(-10.343287191141,-73.778495580227,0.));
#70055=CARTESIAN_POINT('Ctrl Pts',(-10.343287191141,-73.778495580227,12.));
#70056=CARTESIAN_POINT('',(-11.3136138754165,-69.079679653846,0.));
#70057=CARTESIAN_POINT('Ctrl Pts',(-11.3136138754165,-69.079679653846,0.));
#70058=CARTESIAN_POINT('Ctrl Pts',(-11.3132375200165,-69.0835449954396,
0.));
#70059=CARTESIAN_POINT('Ctrl Pts',(-11.3124821678798,-69.0912808656811,
0.));
#70060=CARTESIAN_POINT('Ctrl Pts',(-11.3113412156661,-69.1029002322118,
0.));
#70061=CARTESIAN_POINT('Ctrl Pts',(-11.3098040973713,-69.118423844466,0.));
#70062=CARTESIAN_POINT('Ctrl Pts',(-11.3078562764384,-69.1378802251711,
0.));
#70063=CARTESIAN_POINT('Ctrl Pts',(-11.3058820128307,-69.1573884361,0.));
#70064=CARTESIAN_POINT('Ctrl Pts',(-11.3038812726292,-69.1769483991721,
0.));
#70065=CARTESIAN_POINT('Ctrl Pts',(-11.3018540025638,-69.1965599718914,
0.));
#70066=CARTESIAN_POINT('Ctrl Pts',(-11.2998001310964,-69.2162229488531,
0.));
#70067=CARTESIAN_POINT('Ctrl Pts',(-11.2977195764852,-69.2359370894907,
0.));
#70068=CARTESIAN_POINT('Ctrl Pts',(-11.2956122531375,-69.255702139335,0.));
#70069=CARTESIAN_POINT('Ctrl Pts',(-11.2934780784351,-69.275517853148,0.));
#70070=CARTESIAN_POINT('Ctrl Pts',(-11.2913169799628,-69.295384019272,0.));
#70071=CARTESIAN_POINT('Ctrl Pts',(-11.2891288931517,-69.3153004517783,
0.));
#70072=CARTESIAN_POINT('Ctrl Pts',(-11.2869137578459,-69.3352669789587,
0.));
#70073=CARTESIAN_POINT('Ctrl Pts',(-11.2846715154524,-69.3552834337784,
0.));
#70074=CARTESIAN_POINT('Ctrl Pts',(-11.2824021054045,-69.3753496420039,
0.));
#70075=CARTESIAN_POINT('Ctrl Pts',(-11.2801054633815,-69.3954654162281,
0.));
#70076=CARTESIAN_POINT('Ctrl Pts',(-11.2777815231469,-69.4156305620593,
0.));
#70077=CARTESIAN_POINT('Ctrl Pts',(-11.2754302177021,-69.4358448819967,
0.));
#70078=CARTESIAN_POINT('Ctrl Pts',(-11.2730514806139,-69.456108179879,0.));
#70079=CARTESIAN_POINT('Ctrl Pts',(-11.270645247528,-69.4764202659397,0.));
#70080=CARTESIAN_POINT('Ctrl Pts',(-11.2682114561007,-69.4967809565929,
0.));
#70081=CARTESIAN_POINT('Ctrl Pts',(-11.2657500452716,-69.5171900720158,
0.));
#70082=CARTESIAN_POINT('Ctrl Pts',(-11.263260954763,-69.5376474344771,0.));
#70083=CARTESIAN_POINT('Ctrl Pts',(-11.2607441244702,-69.5581528662877,
0.));
#70084=CARTESIAN_POINT('Ctrl Pts',(-11.2581994939541,-69.5787061880857,
0.));
#70085=CARTESIAN_POINT('Ctrl Pts',(-11.2556270027016,-69.599307219739,0.));
#70086=CARTESIAN_POINT('Ctrl Pts',(-11.2530265903557,-69.6199557811245,
0.));
#70087=CARTESIAN_POINT('Ctrl Pts',(-11.2503981969412,-69.6406516928891,
0.));
#70088=CARTESIAN_POINT('Ctrl Pts',(-11.2477417631386,-69.6613947773534,
0.));
#70089=CARTESIAN_POINT('Ctrl Pts',(-11.2450572303841,-69.6821848588457,
0.));
#70090=CARTESIAN_POINT('Ctrl Pts',(-11.2423445407166,-69.7030217632164,
0.));
#70091=CARTESIAN_POINT('Ctrl Pts',(-11.239603636686,-69.7239053175356,0.));
#70092=CARTESIAN_POINT('Ctrl Pts',(-11.2368344612472,-69.7448353497408,
0.));
#70093=CARTESIAN_POINT('Ctrl Pts',(-11.2340369576456,-69.7658116882324,
0.));
#70094=CARTESIAN_POINT('Ctrl Pts',(-11.2312110694187,-69.7868341618954,
0.));
#70095=CARTESIAN_POINT('Ctrl Pts',(-11.2283567404437,-69.8079026002768,
0.));
#70096=CARTESIAN_POINT('Ctrl Pts',(-11.225473914972,-69.8290168337076,0.));
#70097=CARTESIAN_POINT('Ctrl Pts',(-11.2225625376736,-69.8501766934428,
0.));
#70098=CARTESIAN_POINT('Ctrl Pts',(-11.219622553679,-69.871382011789,0.));
#70099=CARTESIAN_POINT('Ctrl Pts',(-11.2166539085523,-69.8926326220385,
0.));
#70100=CARTESIAN_POINT('Ctrl Pts',(-11.2136565482677,-69.9139283584022,
0.));
#70101=CARTESIAN_POINT('Ctrl Pts',(-11.2106304191882,-69.9352690559405,
0.));
#70102=CARTESIAN_POINT('Ctrl Pts',(-11.2075754680449,-69.9566545504837,
0.));
#70103=CARTESIAN_POINT('Ctrl Pts',(-11.2044916419244,-69.97808467858,0.));
#70104=CARTESIAN_POINT('Ctrl Pts',(-11.2013788882714,-69.9995592775343,
0.));
#70105=CARTESIAN_POINT('Ctrl Pts',(-11.1982371548919,-70.0210781854243,
0.));
#70106=CARTESIAN_POINT('Ctrl Pts',(-11.1950663899576,-70.0426412411185,
0.));
#70107=CARTESIAN_POINT('Ctrl Pts',(-11.1918665420166,-70.0642482842928,
0.));
#70108=CARTESIAN_POINT('Ctrl Pts',(-11.1886375599914,-70.0858991554283,
0.));
#70109=CARTESIAN_POINT('Ctrl Pts',(-11.185379393167,-70.1075936957968,0.));
#70110=CARTESIAN_POINT('Ctrl Pts',(-11.1820919911846,-70.1293317474432,
0.));
#70111=CARTESIAN_POINT('Ctrl Pts',(-11.1787753040363,-70.1511131531674,
0.));
#70112=CARTESIAN_POINT('Ctrl Pts',(-11.1754292820631,-70.1729377564956,
0.));
#70113=CARTESIAN_POINT('Ctrl Pts',(-11.1720538759498,-70.1948054016817,
0.));
#70114=CARTESIAN_POINT('Ctrl Pts',(-11.168649036721,-70.2167159337095,0.));
#70115=CARTESIAN_POINT('Ctrl Pts',(-11.1652147157383,-70.2386691982902,
0.));
#70116=CARTESIAN_POINT('Ctrl Pts',(-11.1617508647017,-70.2606650418589,
0.));
#70117=CARTESIAN_POINT('Ctrl Pts',(-11.1582574356522,-70.2827033115662,
0.));
#70118=CARTESIAN_POINT('Ctrl Pts',(-11.1547343809647,-70.3047838552758,
0.));
#70119=CARTESIAN_POINT('Ctrl Pts',(-11.1511816533422,-70.3269065215591,
0.));
#70120=CARTESIAN_POINT('Ctrl Pts',(-11.1475992058124,-70.3490711596882,
0.));
#70121=CARTESIAN_POINT('Ctrl Pts',(-11.1439869917269,-70.3712776196216,
0.));
#70122=CARTESIAN_POINT('Ctrl Pts',(-11.1403449647622,-70.3935257519945,
0.));
#70123=CARTESIAN_POINT('Ctrl Pts',(-11.1366730789122,-70.415815408119,0.));
#70124=CARTESIAN_POINT('Ctrl Pts',(-11.1329712884845,-70.438146439981,0.));
#70125=CARTESIAN_POINT('Ctrl Pts',(-11.1292395480975,-70.4605187002356,
0.));
#70126=CARTESIAN_POINT('Ctrl Pts',(-11.1254778126824,-70.4829320421973,
0.));
#70127=CARTESIAN_POINT('Ctrl Pts',(-11.121686037483,-70.5053863198306,0.));
#70128=CARTESIAN_POINT('Ctrl Pts',(-11.117864178048,-70.5278813877519,0.));
#70129=CARTESIAN_POINT('Ctrl Pts',(-11.1140121902274,-70.5504171012247,
0.));
#70130=CARTESIAN_POINT('Ctrl Pts',(-11.11013003017,-70.5729933161538,0.));
#70131=CARTESIAN_POINT('Ctrl Pts',(-11.1062176543257,-70.5956098890744,
0.));
#70132=CARTESIAN_POINT('Ctrl Pts',(-11.1022750194439,-70.6182666771441,
0.));
#70133=CARTESIAN_POINT('Ctrl Pts',(-11.0983020825662,-70.6409635381446,
0.));
#70134=CARTESIAN_POINT('Ctrl Pts',(-11.0942988010231,-70.6637003304768,
0.));
#70135=CARTESIAN_POINT('Ctrl Pts',(-11.0902651324325,-70.686476913156,0.));
#70136=CARTESIAN_POINT('Ctrl Pts',(-11.0862010347022,-70.7092931457996,
0.));
#70137=CARTESIAN_POINT('Ctrl Pts',(-11.0821064660276,-70.7321488886229,
0.));
#70138=CARTESIAN_POINT('Ctrl Pts',(-11.0779813848851,-70.7550440024422,
0.));
#70139=CARTESIAN_POINT('Ctrl Pts',(-11.0738257500292,-70.7779783486689,
0.));
#70140=CARTESIAN_POINT('Ctrl Pts',(-11.0696395204907,-70.8009517893042,
0.));
#70141=CARTESIAN_POINT('Ctrl Pts',(-11.0654226555798,-70.8239641869266,
0.));
#70142=CARTESIAN_POINT('Ctrl Pts',(-11.061175114883,-70.847015404688,0.));
#70143=CARTESIAN_POINT('Ctrl Pts',(-11.0568968582566,-70.8701053063158,
0.));
#70144=CARTESIAN_POINT('Ctrl Pts',(-11.0525878458242,-70.8932337561078,
0.));
#70145=CARTESIAN_POINT('Ctrl Pts',(-11.0482480379752,-70.9164006189283,
0.));
#70146=CARTESIAN_POINT('Ctrl Pts',(-11.0438773953686,-70.9396057601953,
0.));
#70147=CARTESIAN_POINT('Ctrl Pts',(-11.039475878929,-70.9628490458779,0.));
#70148=CARTESIAN_POINT('Ctrl Pts',(-11.0350434498408,-70.9861303424989,
0.));
#70149=CARTESIAN_POINT('Ctrl Pts',(-11.0305800695457,-71.0094495171295,
0.));
#70150=CARTESIAN_POINT('Ctrl Pts',(-11.0260856997414,-71.0328064373849,
0.));
#70151=CARTESIAN_POINT('Ctrl Pts',(-11.0215603023854,-71.0562009714125,
0.));
#70152=CARTESIAN_POINT('Ctrl Pts',(-11.0170038396913,-71.0796329878896,
0.));
#70153=CARTESIAN_POINT('Ctrl Pts',(-11.0124162741223,-71.1031023560243,
0.));
#70154=CARTESIAN_POINT('Ctrl Pts',(-11.0077975683895,-71.1266089455517,
0.));
#70155=CARTESIAN_POINT('Ctrl Pts',(-11.0031476854503,-71.1501526267288,
0.));
#70156=CARTESIAN_POINT('Ctrl Pts',(-10.9984665885127,-71.1737332703248,
0.));
#70157=CARTESIAN_POINT('Ctrl Pts',(-10.993754241032,-71.1973507476188,0.));
#70158=CARTESIAN_POINT('Ctrl Pts',(-10.9890106067038,-71.221004930401,0.));
#70159=CARTESIAN_POINT('Ctrl Pts',(-10.9842356494627,-71.2446956909685,
0.));
#70160=CARTESIAN_POINT('Ctrl Pts',(-10.9794293334806,-71.2684229021209,
0.));
#70161=CARTESIAN_POINT('Ctrl Pts',(-10.9745916231711,-71.2921864371499,
0.));
#70162=CARTESIAN_POINT('Ctrl Pts',(-10.9697224831862,-71.3159861698368,
0.));
#70163=CARTESIAN_POINT('Ctrl Pts',(-10.96482187841,-71.3398219744547,0.));
#70164=CARTESIAN_POINT('Ctrl Pts',(-10.9598897739565,-71.3636937257651,
0.));
#70165=CARTESIAN_POINT('Ctrl Pts',(-10.9549261351689,-71.3876012990135,
0.));
#70166=CARTESIAN_POINT('Ctrl Pts',(-10.9499309276235,-71.411544569919,0.));
#70167=CARTESIAN_POINT('Ctrl Pts',(-10.9449041171269,-71.4355234146718,
0.));
#70168=CARTESIAN_POINT('Ctrl Pts',(-10.9398456697094,-71.4595377099352,
0.));
#70169=CARTESIAN_POINT('Ctrl Pts',(-10.9347555516236,-71.4835873328425,
0.));
#70170=CARTESIAN_POINT('Ctrl Pts',(-10.9296337293425,-71.5076721609936,
0.));
#70171=CARTESIAN_POINT('Ctrl Pts',(-10.9244801695642,-71.5317920724453,
0.));
#70172=CARTESIAN_POINT('Ctrl Pts',(-10.9192948392099,-71.5559469457082,
0.));
#70173=CARTESIAN_POINT('Ctrl Pts',(-10.9140777054169,-71.5801366597479,
0.));
#70174=CARTESIAN_POINT('Ctrl Pts',(-10.9088287355364,-71.604361093983,0.));
#70175=CARTESIAN_POINT('Ctrl Pts',(-10.9035478971329,-71.6286201282815,
0.));
#70176=CARTESIAN_POINT('Ctrl Pts',(-10.8982351579872,-71.6529136429515,
0.));
#70177=CARTESIAN_POINT('Ctrl Pts',(-10.8928904860967,-71.6772415187382,
0.));
#70178=CARTESIAN_POINT('Ctrl Pts',(-10.8875138496674,-71.7016036368254,
0.));
#70179=CARTESIAN_POINT('Ctrl Pts',(-10.8821052171122,-71.7259998788337,
0.));
#70180=CARTESIAN_POINT('Ctrl Pts',(-10.8766645570496,-71.7504301268177,
0.));
#70181=CARTESIAN_POINT('Ctrl Pts',(-10.8711918383071,-71.7748942632578,
0.));
#70182=CARTESIAN_POINT('Ctrl Pts',(-10.8656870299218,-71.7993921710546,
0.));
#70183=CARTESIAN_POINT('Ctrl Pts',(-10.860150101133,-71.8239237335318,0.));
#70184=CARTESIAN_POINT('Ctrl Pts',(-10.8545810213799,-71.8484888344335,
0.));
#70185=CARTESIAN_POINT('Ctrl Pts',(-10.8489797602998,-71.8730873579226,
0.));
#70186=CARTESIAN_POINT('Ctrl Pts',(-10.8433462877312,-71.8977191885726,
0.));
#70187=CARTESIAN_POINT('Ctrl Pts',(-10.8376805737158,-71.9223842113622,
0.));
#70188=CARTESIAN_POINT('Ctrl Pts',(-10.8319825884917,-71.9470823116777,
0.));
#70189=CARTESIAN_POINT('Ctrl Pts',(-10.8262523024897,-71.971813375312,0.));
#70190=CARTESIAN_POINT('Ctrl Pts',(-10.8204896863328,-71.9965772884619,
0.));
#70191=CARTESIAN_POINT('Ctrl Pts',(-10.8146947108376,-72.0213739377231,
0.));
#70192=CARTESIAN_POINT('Ctrl Pts',(-10.8088673470187,-72.0462032100828,
0.));
#70193=CARTESIAN_POINT('Ctrl Pts',(-10.8030075660811,-72.0710649929214,
0.));
#70194=CARTESIAN_POINT('Ctrl Pts',(-10.7971153394168,-72.095959174012,0.));
#70195=CARTESIAN_POINT('Ctrl Pts',(-10.7911906386027,-72.1208856415171,
0.));
#70196=CARTESIAN_POINT('Ctrl Pts',(-10.7852334354015,-72.145844283983,0.));
#70197=CARTESIAN_POINT('Ctrl Pts',(-10.779243701766,-72.17083499033,0.));
#70198=CARTESIAN_POINT('Ctrl Pts',(-10.7732214098343,-72.1958576498556,
0.));
#70199=CARTESIAN_POINT('Ctrl Pts',(-10.7671665319254,-72.2209121522367,
0.));
#70200=CARTESIAN_POINT('Ctrl Pts',(-10.7610790405385,-72.2459983875298,
0.));
#70201=CARTESIAN_POINT('Ctrl Pts',(-10.7549589083535,-72.2711162461679,
0.));
#70202=CARTESIAN_POINT('Ctrl Pts',(-10.7488061082368,-72.296265618955,0.));
#70203=CARTESIAN_POINT('Ctrl Pts',(-10.7426206132375,-72.3214463970634,
0.));
#70204=CARTESIAN_POINT('Ctrl Pts',(-10.73640239658,-72.3466584720311,0.));
#70205=CARTESIAN_POINT('Ctrl Pts',(-10.7301514316607,-72.3719017357568,
0.));
#70206=CARTESIAN_POINT('Ctrl Pts',(-10.7238676920469,-72.3971760804935,
0.));
#70207=CARTESIAN_POINT('Ctrl Pts',(-10.7175511514789,-72.4224813988355,
0.));
#70208=CARTESIAN_POINT('Ctrl Pts',(-10.7112017838707,-72.4478175837168,
0.));
#70209=CARTESIAN_POINT('Ctrl Pts',(-10.7048195633062,-72.4731845284238,
0.));
#70210=CARTESIAN_POINT('Ctrl Pts',(-10.6984044640399,-72.4985821266031,
0.));
#70211=CARTESIAN_POINT('Ctrl Pts',(-10.691956460499,-72.5240102722662,0.));
#70212=CARTESIAN_POINT('Ctrl Pts',(-10.6854755272903,-72.5494688597951,
0.));
#70213=CARTESIAN_POINT('Ctrl Pts',(-10.6789616392041,-72.57495778394,0.));
#70214=CARTESIAN_POINT('Ctrl Pts',(-10.6724147711994,-72.6004769398004,
0.));
#70215=CARTESIAN_POINT('Ctrl Pts',(-10.6658348983944,-72.6260262228055,
0.));
#70216=CARTESIAN_POINT('Ctrl Pts',(-10.659221996058,-72.6516055286908,0.));
#70217=CARTESIAN_POINT('Ctrl Pts',(-10.6525760396055,-72.6772147534762,
0.));
#70218=CARTESIAN_POINT('Ctrl Pts',(-10.6458970045948,-72.7028537934332,
0.));
#70219=CARTESIAN_POINT('Ctrl Pts',(-10.6391848667354,-72.7285225451309,
0.));
#70220=CARTESIAN_POINT('Ctrl Pts',(-10.6324396018999,-72.7542209054823,
0.));
#70221=CARTESIAN_POINT('Ctrl Pts',(-10.6256611861395,-72.7799487717914,
0.));
#70222=CARTESIAN_POINT('Ctrl Pts',(-10.6188495956973,-72.8057060417882,
0.));
#70223=CARTESIAN_POINT('Ctrl Pts',(-10.6120048070366,-72.8314926136872,
0.));
#70224=CARTESIAN_POINT('Ctrl Pts',(-10.6051267968202,-72.8573083861328,
0.));
#70225=CARTESIAN_POINT('Ctrl Pts',(-10.5982155418625,-72.8831532580839,
0.));
#70226=CARTESIAN_POINT('Ctrl Pts',(-10.5912710190928,-72.9090271287081,
0.));
#70227=CARTESIAN_POINT('Ctrl Pts',(-10.5842932055209,-72.9349298972823,
0.));
#70228=CARTESIAN_POINT('Ctrl Pts',(-10.5772820781959,-72.9608614630539,
0.));
#70229=CARTESIAN_POINT('Ctrl Pts',(-10.5702376142052,-72.9868217252293,
0.));
#70230=CARTESIAN_POINT('Ctrl Pts',(-10.5631597907653,-73.0128105832635,
0.));
#70231=CARTESIAN_POINT('Ctrl Pts',(-10.5560485852975,-73.0388279370845,
0.));
#70232=CARTESIAN_POINT('Ctrl Pts',(-10.5489039755138,-73.0648736873435,
0.));
#70233=CARTESIAN_POINT('Ctrl Pts',(-10.5417259395001,-73.090947735646,0.));
#70234=CARTESIAN_POINT('Ctrl Pts',(-10.5345144558097,-73.1170499848012,
0.));
#70235=CARTESIAN_POINT('Ctrl Pts',(-10.5272695032649,-73.1431803382677,
0.));
#70236=CARTESIAN_POINT('Ctrl Pts',(-10.5199910607652,-73.169338699611,0.));
#70237=CARTESIAN_POINT('Ctrl Pts',(-10.5126791070804,-73.1955249719037,
0.));
#70238=CARTESIAN_POINT('Ctrl Pts',(-10.505333620691,-73.2217390572578,0.));
#70239=CARTESIAN_POINT('Ctrl Pts',(-10.4979545795197,-73.247980856023,0.));
#70240=CARTESIAN_POINT('Ctrl Pts',(-10.4905419611529,-73.2742502674361,
0.));
#70241=CARTESIAN_POINT('Ctrl Pts',(-10.4830957433311,-73.3005471910639,
0.));
#70242=CARTESIAN_POINT('Ctrl Pts',(-10.475615904381,-73.3268715280609,0.));
#70243=CARTESIAN_POINT('Ctrl Pts',(-10.4681024236288,-73.353223182365,0.));
#70244=CARTESIAN_POINT('Ctrl Pts',(-10.460555281939,-73.3796020622437,0.));
#70245=CARTESIAN_POINT('Ctrl Pts',(-10.4529744618438,-73.4060080806577,
0.));
#70246=CARTESIAN_POINT('Ctrl Pts',(-10.4464473465486,-73.4286663447915,
0.));
#70247=CARTESIAN_POINT('Ctrl Pts',(-10.4414249334768,-73.4460525528551,
0.));
#70248=CARTESIAN_POINT('Ctrl Pts',(-10.4379221501093,-73.458154743654,0.));
#70249=CARTESIAN_POINT('Ctrl Pts',(-10.4359488742883,-73.464965036154,0.));
#70250=CARTESIAN_POINT('Ctrl Pts',(-10.4355099267391,-73.4664795929519,
0.));
#70251=CARTESIAN_POINT('',(-11.3136138754165,-69.079679653846,12.));
#70252=CARTESIAN_POINT('',(-11.3136138754165,-69.079679653846,0.));
#70253=CARTESIAN_POINT('Ctrl Pts',(-10.4355099267391,-73.4664795929519,
12.));
#70254=CARTESIAN_POINT('Ctrl Pts',(-10.4359488742883,-73.464965036154,12.));
#70255=CARTESIAN_POINT('Ctrl Pts',(-10.4379221501093,-73.458154743654,12.));
#70256=CARTESIAN_POINT('Ctrl Pts',(-10.4414249334768,-73.4460525528551,
12.));
#70257=CARTESIAN_POINT('Ctrl Pts',(-10.4464473465486,-73.4286663447915,
12.));
#70258=CARTESIAN_POINT('Ctrl Pts',(-10.4529744618438,-73.4060080806577,
12.));
#70259=CARTESIAN_POINT('Ctrl Pts',(-10.460555281939,-73.3796020622437,12.));
#70260=CARTESIAN_POINT('Ctrl Pts',(-10.4681024236288,-73.353223182365,12.));
#70261=CARTESIAN_POINT('Ctrl Pts',(-10.475615904381,-73.3268715280609,12.));
#70262=CARTESIAN_POINT('Ctrl Pts',(-10.4830957433311,-73.3005471910639,
12.));
#70263=CARTESIAN_POINT('Ctrl Pts',(-10.4905419611529,-73.2742502674361,
12.));
#70264=CARTESIAN_POINT('Ctrl Pts',(-10.4979545795197,-73.247980856023,12.));
#70265=CARTESIAN_POINT('Ctrl Pts',(-10.505333620691,-73.2217390572578,12.));
#70266=CARTESIAN_POINT('Ctrl Pts',(-10.5126791070804,-73.1955249719037,
12.));
#70267=CARTESIAN_POINT('Ctrl Pts',(-10.5199910607652,-73.169338699611,12.));
#70268=CARTESIAN_POINT('Ctrl Pts',(-10.5272695032649,-73.1431803382677,
12.));
#70269=CARTESIAN_POINT('Ctrl Pts',(-10.5345144558097,-73.1170499848012,
12.));
#70270=CARTESIAN_POINT('Ctrl Pts',(-10.5417259395001,-73.090947735646,12.));
#70271=CARTESIAN_POINT('Ctrl Pts',(-10.5489039755138,-73.0648736873435,
12.));
#70272=CARTESIAN_POINT('Ctrl Pts',(-10.5560485852975,-73.0388279370845,
12.));
#70273=CARTESIAN_POINT('Ctrl Pts',(-10.5631597907653,-73.0128105832635,
12.));
#70274=CARTESIAN_POINT('Ctrl Pts',(-10.5702376142052,-72.9868217252293,
12.));
#70275=CARTESIAN_POINT('Ctrl Pts',(-10.5772820781959,-72.9608614630539,
12.));
#70276=CARTESIAN_POINT('Ctrl Pts',(-10.5842932055209,-72.9349298972823,
12.));
#70277=CARTESIAN_POINT('Ctrl Pts',(-10.5912710190928,-72.9090271287081,
12.));
#70278=CARTESIAN_POINT('Ctrl Pts',(-10.5982155418625,-72.8831532580839,
12.));
#70279=CARTESIAN_POINT('Ctrl Pts',(-10.6051267968202,-72.8573083861328,
12.));
#70280=CARTESIAN_POINT('Ctrl Pts',(-10.6120048070366,-72.8314926136872,
12.));
#70281=CARTESIAN_POINT('Ctrl Pts',(-10.6188495956973,-72.8057060417882,
12.));
#70282=CARTESIAN_POINT('Ctrl Pts',(-10.6256611861395,-72.7799487717914,
12.));
#70283=CARTESIAN_POINT('Ctrl Pts',(-10.6324396018999,-72.7542209054823,
12.));
#70284=CARTESIAN_POINT('Ctrl Pts',(-10.6391848667354,-72.7285225451309,
12.));
#70285=CARTESIAN_POINT('Ctrl Pts',(-10.6458970045948,-72.7028537934332,
12.));
#70286=CARTESIAN_POINT('Ctrl Pts',(-10.6525760396055,-72.6772147534762,
12.));
#70287=CARTESIAN_POINT('Ctrl Pts',(-10.659221996058,-72.6516055286908,12.));
#70288=CARTESIAN_POINT('Ctrl Pts',(-10.6658348983944,-72.6260262228055,
12.));
#70289=CARTESIAN_POINT('Ctrl Pts',(-10.6724147711994,-72.6004769398004,
12.));
#70290=CARTESIAN_POINT('Ctrl Pts',(-10.6789616392041,-72.57495778394,12.));
#70291=CARTESIAN_POINT('Ctrl Pts',(-10.6854755272903,-72.5494688597951,
12.));
#70292=CARTESIAN_POINT('Ctrl Pts',(-10.691956460499,-72.5240102722662,12.));
#70293=CARTESIAN_POINT('Ctrl Pts',(-10.6984044640399,-72.4985821266031,
12.));
#70294=CARTESIAN_POINT('Ctrl Pts',(-10.7048195633062,-72.4731845284238,
12.));
#70295=CARTESIAN_POINT('Ctrl Pts',(-10.7112017838707,-72.4478175837168,
12.));
#70296=CARTESIAN_POINT('Ctrl Pts',(-10.7175511514789,-72.4224813988355,
12.));
#70297=CARTESIAN_POINT('Ctrl Pts',(-10.7238676920469,-72.3971760804935,
12.));
#70298=CARTESIAN_POINT('Ctrl Pts',(-10.7301514316607,-72.3719017357568,
12.));
#70299=CARTESIAN_POINT('Ctrl Pts',(-10.73640239658,-72.3466584720311,12.));
#70300=CARTESIAN_POINT('Ctrl Pts',(-10.7426206132375,-72.3214463970634,
12.));
#70301=CARTESIAN_POINT('Ctrl Pts',(-10.7488061082368,-72.296265618955,12.));
#70302=CARTESIAN_POINT('Ctrl Pts',(-10.7549589083535,-72.2711162461679,
12.));
#70303=CARTESIAN_POINT('Ctrl Pts',(-10.7610790405385,-72.2459983875298,
12.));
#70304=CARTESIAN_POINT('Ctrl Pts',(-10.7671665319254,-72.2209121522367,
12.));
#70305=CARTESIAN_POINT('Ctrl Pts',(-10.7732214098343,-72.1958576498556,
12.));
#70306=CARTESIAN_POINT('Ctrl Pts',(-10.779243701766,-72.17083499033,12.));
#70307=CARTESIAN_POINT('Ctrl Pts',(-10.7852334354015,-72.145844283983,12.));
#70308=CARTESIAN_POINT('Ctrl Pts',(-10.7911906386027,-72.1208856415171,
12.));
#70309=CARTESIAN_POINT('Ctrl Pts',(-10.7971153394168,-72.095959174012,12.));
#70310=CARTESIAN_POINT('Ctrl Pts',(-10.8030075660811,-72.0710649929214,
12.));
#70311=CARTESIAN_POINT('Ctrl Pts',(-10.8088673470187,-72.0462032100828,
12.));
#70312=CARTESIAN_POINT('Ctrl Pts',(-10.8146947108376,-72.0213739377231,
12.));
#70313=CARTESIAN_POINT('Ctrl Pts',(-10.8204896863328,-71.9965772884619,
12.));
#70314=CARTESIAN_POINT('Ctrl Pts',(-10.8262523024897,-71.971813375312,12.));
#70315=CARTESIAN_POINT('Ctrl Pts',(-10.8319825884917,-71.9470823116777,
12.));
#70316=CARTESIAN_POINT('Ctrl Pts',(-10.8376805737158,-71.9223842113622,
12.));
#70317=CARTESIAN_POINT('Ctrl Pts',(-10.8433462877312,-71.8977191885726,
12.));
#70318=CARTESIAN_POINT('Ctrl Pts',(-10.8489797602998,-71.8730873579226,
12.));
#70319=CARTESIAN_POINT('Ctrl Pts',(-10.8545810213799,-71.8484888344335,
12.));
#70320=CARTESIAN_POINT('Ctrl Pts',(-10.860150101133,-71.8239237335318,12.));
#70321=CARTESIAN_POINT('Ctrl Pts',(-10.8656870299218,-71.7993921710546,
12.));
#70322=CARTESIAN_POINT('Ctrl Pts',(-10.8711918383071,-71.7748942632578,
12.));
#70323=CARTESIAN_POINT('Ctrl Pts',(-10.8766645570496,-71.7504301268177,
12.));
#70324=CARTESIAN_POINT('Ctrl Pts',(-10.8821052171122,-71.7259998788337,
12.));
#70325=CARTESIAN_POINT('Ctrl Pts',(-10.8875138496674,-71.7016036368254,
12.));
#70326=CARTESIAN_POINT('Ctrl Pts',(-10.8928904860967,-71.6772415187382,
12.));
#70327=CARTESIAN_POINT('Ctrl Pts',(-10.8982351579872,-71.6529136429515,
12.));
#70328=CARTESIAN_POINT('Ctrl Pts',(-10.9035478971329,-71.6286201282815,
12.));
#70329=CARTESIAN_POINT('Ctrl Pts',(-10.9088287355364,-71.604361093983,12.));
#70330=CARTESIAN_POINT('Ctrl Pts',(-10.9140777054169,-71.5801366597479,
12.));
#70331=CARTESIAN_POINT('Ctrl Pts',(-10.9192948392099,-71.5559469457082,
12.));
#70332=CARTESIAN_POINT('Ctrl Pts',(-10.9244801695642,-71.5317920724453,
12.));
#70333=CARTESIAN_POINT('Ctrl Pts',(-10.9296337293425,-71.5076721609936,
12.));
#70334=CARTESIAN_POINT('Ctrl Pts',(-10.9347555516236,-71.4835873328425,
12.));
#70335=CARTESIAN_POINT('Ctrl Pts',(-10.9398456697094,-71.4595377099352,
12.));
#70336=CARTESIAN_POINT('Ctrl Pts',(-10.9449041171269,-71.4355234146718,
12.));
#70337=CARTESIAN_POINT('Ctrl Pts',(-10.9499309276235,-71.411544569919,12.));
#70338=CARTESIAN_POINT('Ctrl Pts',(-10.9549261351689,-71.3876012990135,
12.));
#70339=CARTESIAN_POINT('Ctrl Pts',(-10.9598897739565,-71.3636937257651,
12.));
#70340=CARTESIAN_POINT('Ctrl Pts',(-10.96482187841,-71.3398219744547,12.));
#70341=CARTESIAN_POINT('Ctrl Pts',(-10.9697224831862,-71.3159861698368,
12.));
#70342=CARTESIAN_POINT('Ctrl Pts',(-10.9745916231711,-71.2921864371499,
12.));
#70343=CARTESIAN_POINT('Ctrl Pts',(-10.9794293334806,-71.2684229021209,
12.));
#70344=CARTESIAN_POINT('Ctrl Pts',(-10.9842356494627,-71.2446956909685,
12.));
#70345=CARTESIAN_POINT('Ctrl Pts',(-10.9890106067038,-71.221004930401,12.));
#70346=CARTESIAN_POINT('Ctrl Pts',(-10.993754241032,-71.1973507476188,12.));
#70347=CARTESIAN_POINT('Ctrl Pts',(-10.9984665885127,-71.1737332703248,
12.));
#70348=CARTESIAN_POINT('Ctrl Pts',(-11.0031476854503,-71.1501526267288,
12.));
#70349=CARTESIAN_POINT('Ctrl Pts',(-11.0077975683895,-71.1266089455517,
12.));
#70350=CARTESIAN_POINT('Ctrl Pts',(-11.0124162741223,-71.1031023560243,
12.));
#70351=CARTESIAN_POINT('Ctrl Pts',(-11.0170038396913,-71.0796329878896,
12.));
#70352=CARTESIAN_POINT('Ctrl Pts',(-11.0215603023854,-71.0562009714125,
12.));
#70353=CARTESIAN_POINT('Ctrl Pts',(-11.0260856997414,-71.0328064373849,
12.));
#70354=CARTESIAN_POINT('Ctrl Pts',(-11.0305800695457,-71.0094495171295,
12.));
#70355=CARTESIAN_POINT('Ctrl Pts',(-11.0350434498408,-70.9861303424989,
12.));
#70356=CARTESIAN_POINT('Ctrl Pts',(-11.039475878929,-70.9628490458779,12.));
#70357=CARTESIAN_POINT('Ctrl Pts',(-11.0438773953686,-70.9396057601953,
12.));
#70358=CARTESIAN_POINT('Ctrl Pts',(-11.0482480379752,-70.9164006189283,
12.));
#70359=CARTESIAN_POINT('Ctrl Pts',(-11.0525878458242,-70.8932337561078,
12.));
#70360=CARTESIAN_POINT('Ctrl Pts',(-11.0568968582566,-70.8701053063158,
12.));
#70361=CARTESIAN_POINT('Ctrl Pts',(-11.061175114883,-70.847015404688,12.));
#70362=CARTESIAN_POINT('Ctrl Pts',(-11.0654226555798,-70.8239641869266,
12.));
#70363=CARTESIAN_POINT('Ctrl Pts',(-11.0696395204907,-70.8009517893042,
12.));
#70364=CARTESIAN_POINT('Ctrl Pts',(-11.0738257500292,-70.7779783486689,
12.));
#70365=CARTESIAN_POINT('Ctrl Pts',(-11.0779813848851,-70.7550440024422,
12.));
#70366=CARTESIAN_POINT('Ctrl Pts',(-11.0821064660276,-70.7321488886229,
12.));
#70367=CARTESIAN_POINT('Ctrl Pts',(-11.0862010347022,-70.7092931457996,
12.));
#70368=CARTESIAN_POINT('Ctrl Pts',(-11.0902651324325,-70.686476913156,12.));
#70369=CARTESIAN_POINT('Ctrl Pts',(-11.0942988010231,-70.6637003304768,
12.));
#70370=CARTESIAN_POINT('Ctrl Pts',(-11.0983020825662,-70.6409635381446,
12.));
#70371=CARTESIAN_POINT('Ctrl Pts',(-11.1022750194439,-70.6182666771441,
12.));
#70372=CARTESIAN_POINT('Ctrl Pts',(-11.1062176543257,-70.5956098890744,
12.));
#70373=CARTESIAN_POINT('Ctrl Pts',(-11.11013003017,-70.5729933161538,12.));
#70374=CARTESIAN_POINT('Ctrl Pts',(-11.1140121902274,-70.5504171012247,
12.));
#70375=CARTESIAN_POINT('Ctrl Pts',(-11.117864178048,-70.5278813877519,12.));
#70376=CARTESIAN_POINT('Ctrl Pts',(-11.121686037483,-70.5053863198306,12.));
#70377=CARTESIAN_POINT('Ctrl Pts',(-11.1254778126824,-70.4829320421973,
12.));
#70378=CARTESIAN_POINT('Ctrl Pts',(-11.1292395480975,-70.4605187002356,
12.));
#70379=CARTESIAN_POINT('Ctrl Pts',(-11.1329712884845,-70.438146439981,12.));
#70380=CARTESIAN_POINT('Ctrl Pts',(-11.1366730789122,-70.415815408119,12.));
#70381=CARTESIAN_POINT('Ctrl Pts',(-11.1403449647622,-70.3935257519945,
12.));
#70382=CARTESIAN_POINT('Ctrl Pts',(-11.1439869917269,-70.3712776196216,
12.));
#70383=CARTESIAN_POINT('Ctrl Pts',(-11.1475992058124,-70.3490711596882,
12.));
#70384=CARTESIAN_POINT('Ctrl Pts',(-11.1511816533422,-70.3269065215591,
12.));
#70385=CARTESIAN_POINT('Ctrl Pts',(-11.1547343809647,-70.3047838552758,
12.));
#70386=CARTESIAN_POINT('Ctrl Pts',(-11.1582574356522,-70.2827033115662,
12.));
#70387=CARTESIAN_POINT('Ctrl Pts',(-11.1617508647017,-70.2606650418589,
12.));
#70388=CARTESIAN_POINT('Ctrl Pts',(-11.1652147157383,-70.2386691982902,
12.));
#70389=CARTESIAN_POINT('Ctrl Pts',(-11.168649036721,-70.2167159337095,12.));
#70390=CARTESIAN_POINT('Ctrl Pts',(-11.1720538759498,-70.1948054016817,
12.));
#70391=CARTESIAN_POINT('Ctrl Pts',(-11.1754292820631,-70.1729377564956,
12.));
#70392=CARTESIAN_POINT('Ctrl Pts',(-11.1787753040363,-70.1511131531674,
12.));
#70393=CARTESIAN_POINT('Ctrl Pts',(-11.1820919911846,-70.1293317474432,
12.));
#70394=CARTESIAN_POINT('Ctrl Pts',(-11.185379393167,-70.1075936957968,12.));
#70395=CARTESIAN_POINT('Ctrl Pts',(-11.1886375599914,-70.0858991554283,
12.));
#70396=CARTESIAN_POINT('Ctrl Pts',(-11.1918665420166,-70.0642482842928,
12.));
#70397=CARTESIAN_POINT('Ctrl Pts',(-11.1950663899576,-70.0426412411185,
12.));
#70398=CARTESIAN_POINT('Ctrl Pts',(-11.1982371548919,-70.0210781854243,
12.));
#70399=CARTESIAN_POINT('Ctrl Pts',(-11.2013788882714,-69.9995592775343,
12.));
#70400=CARTESIAN_POINT('Ctrl Pts',(-11.2044916419244,-69.97808467858,12.));
#70401=CARTESIAN_POINT('Ctrl Pts',(-11.2075754680449,-69.9566545504837,
12.));
#70402=CARTESIAN_POINT('Ctrl Pts',(-11.2106304191882,-69.9352690559405,
12.));
#70403=CARTESIAN_POINT('Ctrl Pts',(-11.2136565482677,-69.9139283584022,
12.));
#70404=CARTESIAN_POINT('Ctrl Pts',(-11.2166539085523,-69.8926326220385,
12.));
#70405=CARTESIAN_POINT('Ctrl Pts',(-11.219622553679,-69.871382011789,12.));
#70406=CARTESIAN_POINT('Ctrl Pts',(-11.2225625376736,-69.8501766934428,
12.));
#70407=CARTESIAN_POINT('Ctrl Pts',(-11.225473914972,-69.8290168337076,12.));
#70408=CARTESIAN_POINT('Ctrl Pts',(-11.2283567404437,-69.8079026002768,
12.));
#70409=CARTESIAN_POINT('Ctrl Pts',(-11.2312110694187,-69.7868341618954,
12.));
#70410=CARTESIAN_POINT('Ctrl Pts',(-11.2340369576456,-69.7658116882324,
12.));
#70411=CARTESIAN_POINT('Ctrl Pts',(-11.2368344612472,-69.7448353497408,
12.));
#70412=CARTESIAN_POINT('Ctrl Pts',(-11.239603636686,-69.7239053175356,12.));
#70413=CARTESIAN_POINT('Ctrl Pts',(-11.2423445407166,-69.7030217632164,
12.));
#70414=CARTESIAN_POINT('Ctrl Pts',(-11.2450572303841,-69.6821848588457,
12.));
#70415=CARTESIAN_POINT('Ctrl Pts',(-11.2477417631386,-69.6613947773534,
12.));
#70416=CARTESIAN_POINT('Ctrl Pts',(-11.2503981969412,-69.6406516928891,
12.));
#70417=CARTESIAN_POINT('Ctrl Pts',(-11.2530265903557,-69.6199557811245,
12.));
#70418=CARTESIAN_POINT('Ctrl Pts',(-11.2556270027016,-69.599307219739,12.));
#70419=CARTESIAN_POINT('Ctrl Pts',(-11.2581994939541,-69.5787061880857,
12.));
#70420=CARTESIAN_POINT('Ctrl Pts',(-11.2607441244702,-69.5581528662877,
12.));
#70421=CARTESIAN_POINT('Ctrl Pts',(-11.263260954763,-69.5376474344771,12.));
#70422=CARTESIAN_POINT('Ctrl Pts',(-11.2657500452716,-69.5171900720158,
12.));
#70423=CARTESIAN_POINT('Ctrl Pts',(-11.2682114561007,-69.4967809565929,
12.));
#70424=CARTESIAN_POINT('Ctrl Pts',(-11.270645247528,-69.4764202659397,12.));
#70425=CARTESIAN_POINT('Ctrl Pts',(-11.2730514806139,-69.456108179879,12.));
#70426=CARTESIAN_POINT('Ctrl Pts',(-11.2754302177021,-69.4358448819967,
12.));
#70427=CARTESIAN_POINT('Ctrl Pts',(-11.2777815231469,-69.4156305620593,
12.));
#70428=CARTESIAN_POINT('Ctrl Pts',(-11.2801054633815,-69.3954654162281,
12.));
#70429=CARTESIAN_POINT('Ctrl Pts',(-11.2824021054045,-69.3753496420039,
12.));
#70430=CARTESIAN_POINT('Ctrl Pts',(-11.2846715154524,-69.3552834337784,
12.));
#70431=CARTESIAN_POINT('Ctrl Pts',(-11.2869137578459,-69.3352669789587,
12.));
#70432=CARTESIAN_POINT('Ctrl Pts',(-11.2891288931517,-69.3153004517783,
12.));
#70433=CARTESIAN_POINT('Ctrl Pts',(-11.2913169799628,-69.295384019272,12.));
#70434=CARTESIAN_POINT('Ctrl Pts',(-11.2934780784351,-69.275517853148,12.));
#70435=CARTESIAN_POINT('Ctrl Pts',(-11.2956122531375,-69.255702139335,12.));
#70436=CARTESIAN_POINT('Ctrl Pts',(-11.2977195764852,-69.2359370894907,
12.));
#70437=CARTESIAN_POINT('Ctrl Pts',(-11.2998001310964,-69.2162229488531,
12.));
#70438=CARTESIAN_POINT('Ctrl Pts',(-11.3018540025638,-69.1965599718914,
12.));
#70439=CARTESIAN_POINT('Ctrl Pts',(-11.3038812726292,-69.1769483991721,
12.));
#70440=CARTESIAN_POINT('Ctrl Pts',(-11.3058820128307,-69.1573884361,12.));
#70441=CARTESIAN_POINT('Ctrl Pts',(-11.3078562764384,-69.1378802251711,
12.));
#70442=CARTESIAN_POINT('Ctrl Pts',(-11.3098040973713,-69.118423844466,12.));
#70443=CARTESIAN_POINT('Ctrl Pts',(-11.3113412156661,-69.1029002322118,
12.));
#70444=CARTESIAN_POINT('Ctrl Pts',(-11.3124821678798,-69.0912808656811,
12.));
#70445=CARTESIAN_POINT('Ctrl Pts',(-11.3132375200165,-69.0835449954396,
12.));
#70446=CARTESIAN_POINT('Ctrl Pts',(-11.3136138754165,-69.079679653846,12.));
#70447=CARTESIAN_POINT('Ctrl Pts',(-8.93459554657871,-73.6640787198061,
-5.55111512312578E-16));
#70448=CARTESIAN_POINT('Ctrl Pts',(-8.93459554657871,-73.6640787198061,
4.));
#70449=CARTESIAN_POINT('Ctrl Pts',(-8.93459554657871,-73.6640787198061,
8.));
#70450=CARTESIAN_POINT('Ctrl Pts',(-8.93459554657871,-73.6640787198061,
12.));
#70451=CARTESIAN_POINT('Ctrl Pts',(-8.9914562677793,-73.7581053903597,-5.55111512312578E-16));
#70452=CARTESIAN_POINT('Ctrl Pts',(-8.9914562677793,-73.7581053903597,4.));
#70453=CARTESIAN_POINT('Ctrl Pts',(-8.9914562677793,-73.7581053903597,8.));
#70454=CARTESIAN_POINT('Ctrl Pts',(-8.9914562677793,-73.7581053903597,12.));
#70455=CARTESIAN_POINT('Ctrl Pts',(-9.14696952162315,-73.8880618019207,
-5.55111512312578E-16));
#70456=CARTESIAN_POINT('Ctrl Pts',(-9.14696952162315,-73.8880618019207,
4.00000000000001));
#70457=CARTESIAN_POINT('Ctrl Pts',(-9.14696952162315,-73.8880618019207,
7.99999999999999));
#70458=CARTESIAN_POINT('Ctrl Pts',(-9.14696952162315,-73.8880618019207,
12.));
#70459=CARTESIAN_POINT('Ctrl Pts',(-9.3439568349051,-73.911753208677,-5.55111512312578E-16));
#70460=CARTESIAN_POINT('Ctrl Pts',(-9.3439568349051,-73.911753208677,4.));
#70461=CARTESIAN_POINT('Ctrl Pts',(-9.3439568349051,-73.911753208677,8.00000000000001));
#70462=CARTESIAN_POINT('Ctrl Pts',(-9.3439568349051,-73.911753208677,12.));
#70463=CARTESIAN_POINT('Ctrl Pts',(-9.42570643237529,-73.9013264985863,
-5.55111512312578E-16));
#70464=CARTESIAN_POINT('Ctrl Pts',(-9.42570643237529,-73.9013264985863,
4.));
#70465=CARTESIAN_POINT('Ctrl Pts',(-9.42570643237529,-73.9013264985863,
8.));
#70466=CARTESIAN_POINT('Ctrl Pts',(-9.42570643237529,-73.9013264985863,
12.));
#70467=CARTESIAN_POINT('',(-8.93459554657871,-73.6640787198061,-2.77555756156289E-16));
#70468=CARTESIAN_POINT('',(-9.42570643237531,-73.9013264985865,2.77555756156289E-16));
#70469=CARTESIAN_POINT('Ctrl Pts',(-8.93459554657871,-73.6640787198061,
1.23259516440783E-31));
#70470=CARTESIAN_POINT('Ctrl Pts',(-8.9914562677793,-73.7581053903597,-2.61926472436664E-31));
#70471=CARTESIAN_POINT('Ctrl Pts',(-9.0803209842615,-73.832366196966,4.93038065763132E-31));
#70472=CARTESIAN_POINT('Ctrl Pts',(-9.1827282507643,-73.8719282264932,3.23556230657056E-31));
#70473=CARTESIAN_POINT('Ctrl Pts',(-9.25953370064141,-73.9015997486385,
1.54074395550979E-31));
#70474=CARTESIAN_POINT('Ctrl Pts',(-9.3439568349051,-73.911753208677,-5.23852944873328E-31));
#70475=CARTESIAN_POINT('Ctrl Pts',(-9.42570643237529,-73.9013264985863,
1.69481835106077E-31));
#70476=CARTESIAN_POINT('',(-9.42570643237531,-73.9013264985865,12.));
#70477=CARTESIAN_POINT('Ctrl Pts',(-9.42570643237529,-73.9013264985863,
-5.55111512312578E-16));
#70478=CARTESIAN_POINT('Ctrl Pts',(-9.42570643237529,-73.9013264985863,
4.));
#70479=CARTESIAN_POINT('Ctrl Pts',(-9.42570643237529,-73.9013264985863,
8.));
#70480=CARTESIAN_POINT('Ctrl Pts',(-9.42570643237529,-73.9013264985863,
12.));
#70481=CARTESIAN_POINT('',(-8.93459554657871,-73.6640787198061,12.));
#70482=CARTESIAN_POINT('Ctrl Pts',(-9.42570643237529,-73.9013264985863,
12.));
#70483=CARTESIAN_POINT('Ctrl Pts',(-9.3439568349051,-73.911753208677,12.));
#70484=CARTESIAN_POINT('Ctrl Pts',(-9.25953370064141,-73.9015997486385,
12.));
#70485=CARTESIAN_POINT('Ctrl Pts',(-9.1827282507643,-73.8719282264932,12.));
#70486=CARTESIAN_POINT('Ctrl Pts',(-9.0803209842615,-73.832366196966,12.));
#70487=CARTESIAN_POINT('Ctrl Pts',(-8.9914562677793,-73.7581053903597,12.));
#70488=CARTESIAN_POINT('Ctrl Pts',(-8.93459554657871,-73.6640787198061,
12.));
#70489=CARTESIAN_POINT('Ctrl Pts',(-8.93459554657871,-73.6640787198061,
12.));
#70490=CARTESIAN_POINT('Ctrl Pts',(-8.93459554657871,-73.6640787198061,
8.));
#70491=CARTESIAN_POINT('Ctrl Pts',(-8.93459554657871,-73.6640787198061,
4.));
#70492=CARTESIAN_POINT('Ctrl Pts',(-8.93459554657871,-73.6640787198061,
-5.55111512312578E-16));
#70493=CARTESIAN_POINT('Origin',(-4.88285199465431E-11,-3.71649880366789E-10,
0.));
#70494=CARTESIAN_POINT('Origin',(-4.88285199465431E-11,-3.71649880366789E-10,
12.));
#70495=CARTESIAN_POINT('Origin',(-4.88285199465431E-11,-3.71649880366789E-10,
0.));
#70496=CARTESIAN_POINT('Ctrl Pts',(-16.4184755008033,-72.6683126419592,
-5.55111512312578E-16));
#70497=CARTESIAN_POINT('Ctrl Pts',(-16.4184755008033,-72.6683126419592,
4.));
#70498=CARTESIAN_POINT('Ctrl Pts',(-16.4184755008033,-72.6683126419592,
8.));
#70499=CARTESIAN_POINT('Ctrl Pts',(-16.4184755008033,-72.6683126419592,
12.));
#70500=CARTESIAN_POINT('Ctrl Pts',(-16.5256563519778,-72.6440964999409,
-5.55111512312578E-16));
#70501=CARTESIAN_POINT('Ctrl Pts',(-16.5256563519778,-72.6440964999409,
4.));
#70502=CARTESIAN_POINT('Ctrl Pts',(-16.5256563519778,-72.6440964999409,
8.00000000000001));
#70503=CARTESIAN_POINT('Ctrl Pts',(-16.5256563519778,-72.6440964999409,
12.));
#70504=CARTESIAN_POINT('Ctrl Pts',(-16.6981133841326,-72.5376471652844,
-5.55111512312578E-16));
#70505=CARTESIAN_POINT('Ctrl Pts',(-16.6981133841326,-72.5376471652844,
4.));
#70506=CARTESIAN_POINT('Ctrl Pts',(-16.6981133841326,-72.5376471652844,
7.99999999999999));
#70507=CARTESIAN_POINT('Ctrl Pts',(-16.6981133841326,-72.5376471652844,
12.));
#70508=CARTESIAN_POINT('Ctrl Pts',(-16.7828708182974,-72.3582555997246,
-5.55111512312578E-16));
#70509=CARTESIAN_POINT('Ctrl Pts',(-16.7828708182974,-72.3582555997246,
4.));
#70510=CARTESIAN_POINT('Ctrl Pts',(-16.7828708182974,-72.3582555997246,
8.00000000000001));
#70511=CARTESIAN_POINT('Ctrl Pts',(-16.7828708182974,-72.3582555997246,
12.));
#70512=CARTESIAN_POINT('Ctrl Pts',(-16.7988252568806,-72.2774028393486,
-5.55111512312578E-16));
#70513=CARTESIAN_POINT('Ctrl Pts',(-16.7988252568806,-72.2774028393486,
4.));
#70514=CARTESIAN_POINT('Ctrl Pts',(-16.7988252568806,-72.2774028393486,
8.));
#70515=CARTESIAN_POINT('Ctrl Pts',(-16.7988252568806,-72.2774028393486,
12.));
#70516=CARTESIAN_POINT('',(-16.4184755008033,-72.6683126419592,0.));
#70517=CARTESIAN_POINT('',(-16.7988252568806,-72.2774028393486,0.));
#70518=CARTESIAN_POINT('Ctrl Pts',(-16.4184755008033,-72.6683126419592,
4.16333634234434E-16));
#70519=CARTESIAN_POINT('Ctrl Pts',(-16.5256563519778,-72.6440964999409,
4.16333634234433E-16));
#70520=CARTESIAN_POINT('Ctrl Pts',(-16.6242032274948,-72.5832683087087,
4.16333634234434E-16));
#70521=CARTESIAN_POINT('Ctrl Pts',(-16.6941134995865,-72.498622246161,4.16333634234434E-16));
#70522=CARTESIAN_POINT('Ctrl Pts',(-16.7465462036553,-72.4351376992502,
4.16333634234434E-16));
#70523=CARTESIAN_POINT('Ctrl Pts',(-16.7828708182974,-72.3582555997246,
4.16333634234433E-16));
#70524=CARTESIAN_POINT('Ctrl Pts',(-16.7988252568806,-72.2774028393486,
4.16333634234434E-16));
#70525=CARTESIAN_POINT('',(-16.7988252568806,-72.2774028393486,12.));
#70526=CARTESIAN_POINT('Ctrl Pts',(-16.7988252568806,-72.2774028393486,
-5.55111512312578E-16));
#70527=CARTESIAN_POINT('Ctrl Pts',(-16.7988252568806,-72.2774028393486,
4.));
#70528=CARTESIAN_POINT('Ctrl Pts',(-16.7988252568806,-72.2774028393486,
8.));
#70529=CARTESIAN_POINT('Ctrl Pts',(-16.7988252568806,-72.2774028393486,
12.));
#70530=CARTESIAN_POINT('',(-16.4184755008033,-72.6683126419592,12.));
#70531=CARTESIAN_POINT('Ctrl Pts',(-16.7988252568806,-72.2774028393486,
12.));
#70532=CARTESIAN_POINT('Ctrl Pts',(-16.7828708182974,-72.3582555997246,
12.));
#70533=CARTESIAN_POINT('Ctrl Pts',(-16.7465462036554,-72.4351376992502,
12.));
#70534=CARTESIAN_POINT('Ctrl Pts',(-16.6941134995865,-72.498622246161,12.));
#70535=CARTESIAN_POINT('Ctrl Pts',(-16.6242032274948,-72.5832683087087,
12.));
#70536=CARTESIAN_POINT('Ctrl Pts',(-16.5256563519778,-72.6440964999409,
12.));
#70537=CARTESIAN_POINT('Ctrl Pts',(-16.4184755008033,-72.6683126419592,
12.));
#70538=CARTESIAN_POINT('Ctrl Pts',(-16.4184755008033,-72.6683126419592,
12.));
#70539=CARTESIAN_POINT('Ctrl Pts',(-16.4184755008033,-72.6683126419592,
8.));
#70540=CARTESIAN_POINT('Ctrl Pts',(-16.4184755008033,-72.6683126419592,
4.));
#70541=CARTESIAN_POINT('Ctrl Pts',(-16.4184755008033,-72.6683126419592,
-5.55111512312578E-16));
#70542=CARTESIAN_POINT('Ctrl Pts',(-17.2912529479484,-67.8307641965655,
0.));
#70543=CARTESIAN_POINT('Ctrl Pts',(-17.2912529479484,-67.8307641965655,
12.));
#70544=CARTESIAN_POINT('Ctrl Pts',(-17.2912149114119,-67.8346476309018,
0.));
#70545=CARTESIAN_POINT('Ctrl Pts',(-17.2912149114119,-67.8346476309018,
12.));
#70546=CARTESIAN_POINT('Ctrl Pts',(-17.2911366591347,-67.842419897098,0.));
#70547=CARTESIAN_POINT('Ctrl Pts',(-17.2911366591347,-67.842419897098,12.));
#70548=CARTESIAN_POINT('Ctrl Pts',(-17.291012743109,-67.8540944889687,0.));
#70549=CARTESIAN_POINT('Ctrl Pts',(-17.291012743109,-67.8540944889687,12.));
#70550=CARTESIAN_POINT('Ctrl Pts',(-17.2908344459694,-67.8696929978782,
0.));
#70551=CARTESIAN_POINT('Ctrl Pts',(-17.2908344459694,-67.8696929978782,
12.));
#70552=CARTESIAN_POINT('Ctrl Pts',(-17.2905897723948,-67.8892451049608,
0.));
#70553=CARTESIAN_POINT('Ctrl Pts',(-17.2905897723948,-67.8892451049608,
12.));
#70554=CARTESIAN_POINT('Ctrl Pts',(-17.2903232740694,-67.9088511496686,
0.));
#70555=CARTESIAN_POINT('Ctrl Pts',(-17.2903232740694,-67.9088511496686,
12.));
#70556=CARTESIAN_POINT('Ctrl Pts',(-17.2900349103981,-67.9285110571741,
0.));
#70557=CARTESIAN_POINT('Ctrl Pts',(-17.2900349103981,-67.9285110571741,
12.));
#70558=CARTESIAN_POINT('Ctrl Pts',(-17.2897246158941,-67.9482246901667,
0.));
#70559=CARTESIAN_POINT('Ctrl Pts',(-17.2897246158941,-67.9482246901667,
12.));
#70560=CARTESIAN_POINT('Ctrl Pts',(-17.2893923013894,-67.9679918502579,
0.));
#70561=CARTESIAN_POINT('Ctrl Pts',(-17.2893923013894,-67.9679918502579,
12.));
#70562=CARTESIAN_POINT('Ctrl Pts',(-17.2890378644866,-67.987812304921,0.));
#70563=CARTESIAN_POINT('Ctrl Pts',(-17.2890378644866,-67.987812304921,12.));
#70564=CARTESIAN_POINT('Ctrl Pts',(-17.28866119774,-68.007685808115,0.));
#70565=CARTESIAN_POINT('Ctrl Pts',(-17.28866119774,-68.007685808115,12.));
#70566=CARTESIAN_POINT('Ctrl Pts',(-17.2882621974721,-68.0276121227356,
0.));
#70567=CARTESIAN_POINT('Ctrl Pts',(-17.2882621974721,-68.0276121227356,
12.));
#70568=CARTESIAN_POINT('Ctrl Pts',(-17.2878407730961,-68.0475910442424,
0.));
#70569=CARTESIAN_POINT('Ctrl Pts',(-17.2878407730961,-68.0475910442424,
12.));
#70570=CARTESIAN_POINT('Ctrl Pts',(-17.2873968440839,-68.0676223930412,
0.));
#70571=CARTESIAN_POINT('Ctrl Pts',(-17.2873968440839,-68.0676223930412,
12.));
#70572=CARTESIAN_POINT('Ctrl Pts',(-17.2869303355432,-68.0877060033205,
0.));
#70573=CARTESIAN_POINT('Ctrl Pts',(-17.2869303355432,-68.0877060033205,
12.));
#70574=CARTESIAN_POINT('Ctrl Pts',(-17.2864411745459,-68.1078417137877,
0.));
#70575=CARTESIAN_POINT('Ctrl Pts',(-17.2864411745459,-68.1078417137877,
12.));
#70576=CARTESIAN_POINT('Ctrl Pts',(-17.2859292855705,-68.1280293561511,
0.));
#70577=CARTESIAN_POINT('Ctrl Pts',(-17.2859292855705,-68.1280293561511,
12.));
#70578=CARTESIAN_POINT('Ctrl Pts',(-17.2853945882072,-68.1482687493226,
0.));
#70579=CARTESIAN_POINT('Ctrl Pts',(-17.2853945882072,-68.1482687493226,
12.));
#70580=CARTESIAN_POINT('Ctrl Pts',(-17.2848369995293,-68.1685597054232,
0.));
#70581=CARTESIAN_POINT('Ctrl Pts',(-17.2848369995293,-68.1685597054232,
12.));
#70582=CARTESIAN_POINT('Ctrl Pts',(-17.2842564355799,-68.1889020335427,
0.));
#70583=CARTESIAN_POINT('Ctrl Pts',(-17.2842564355799,-68.1889020335427,
12.));
#70584=CARTESIAN_POINT('Ctrl Pts',(-17.2836528130819,-68.2092955440567,
0.));
#70585=CARTESIAN_POINT('Ctrl Pts',(-17.2836528130819,-68.2092955440567,
12.));
#70586=CARTESIAN_POINT('Ctrl Pts',(-17.2830260513867,-68.2297400535294,
0.));
#70587=CARTESIAN_POINT('Ctrl Pts',(-17.2830260513867,-68.2297400535294,
12.));
#70588=CARTESIAN_POINT('Ctrl Pts',(-17.2823760723874,-68.2502353845071,
0.));
#70589=CARTESIAN_POINT('Ctrl Pts',(-17.2823760723874,-68.2502353845071,
12.));
#70590=CARTESIAN_POINT('Ctrl Pts',(-17.2817027995831,-68.2707813631731,
0.));
#70591=CARTESIAN_POINT('Ctrl Pts',(-17.2817027995831,-68.2707813631731,
12.));
#70592=CARTESIAN_POINT('Ctrl Pts',(-17.2810061574353,-68.2913778177261,
0.));
#70593=CARTESIAN_POINT('Ctrl Pts',(-17.2810061574353,-68.2913778177261,
12.));
#70594=CARTESIAN_POINT('Ctrl Pts',(-17.2802860705815,-68.3120245763914,
0.));
#70595=CARTESIAN_POINT('Ctrl Pts',(-17.2802860705815,-68.3120245763914,
12.));
#70596=CARTESIAN_POINT('Ctrl Pts',(-17.2795424631799,-68.3327214657575,
0.));
#70597=CARTESIAN_POINT('Ctrl Pts',(-17.2795424631799,-68.3327214657575,
12.));
#70598=CARTESIAN_POINT('Ctrl Pts',(-17.2787752592484,-68.3534683116515,
0.));
#70599=CARTESIAN_POINT('Ctrl Pts',(-17.2787752592484,-68.3534683116515,
12.));
#70600=CARTESIAN_POINT('Ctrl Pts',(-17.2779843829608,-68.3742649398964,
0.));
#70601=CARTESIAN_POINT('Ctrl Pts',(-17.2779843829608,-68.3742649398964,
12.));
#70602=CARTESIAN_POINT('Ctrl Pts',(-17.2771697589384,-68.3951111770487,
0.));
#70603=CARTESIAN_POINT('Ctrl Pts',(-17.2771697589384,-68.3951111770487,
12.));
#70604=CARTESIAN_POINT('Ctrl Pts',(-17.2763313126018,-68.4160068512753,
0.));
#70605=CARTESIAN_POINT('Ctrl Pts',(-17.2763313126018,-68.4160068512753,
12.));
#70606=CARTESIAN_POINT('Ctrl Pts',(-17.2754689702992,-68.436951792677,0.));
#70607=CARTESIAN_POINT('Ctrl Pts',(-17.2754689702992,-68.436951792677,12.));
#70608=CARTESIAN_POINT('Ctrl Pts',(-17.2745826591119,-68.4579458328185,
0.));
#70609=CARTESIAN_POINT('Ctrl Pts',(-17.2745826591119,-68.4579458328185,
12.));
#70610=CARTESIAN_POINT('Ctrl Pts',(-17.2736723067365,-68.4789888044351,
0.));
#70611=CARTESIAN_POINT('Ctrl Pts',(-17.2736723067365,-68.4789888044351,
12.));
#70612=CARTESIAN_POINT('Ctrl Pts',(-17.2727378413489,-68.5000805410911,
0.));
#70613=CARTESIAN_POINT('Ctrl Pts',(-17.2727378413489,-68.5000805410911,
12.));
#70614=CARTESIAN_POINT('Ctrl Pts',(-17.2717791914544,-68.521220876786,0.));
#70615=CARTESIAN_POINT('Ctrl Pts',(-17.2717791914544,-68.521220876786,12.));
#70616=CARTESIAN_POINT('Ctrl Pts',(-17.2707962858919,-68.5424096459772,
0.));
#70617=CARTESIAN_POINT('Ctrl Pts',(-17.2707962858919,-68.5424096459772,
12.));
#70618=CARTESIAN_POINT('Ctrl Pts',(-17.269789053896,-68.5636466837517,0.));
#70619=CARTESIAN_POINT('Ctrl Pts',(-17.269789053896,-68.5636466837517,12.));
#70620=CARTESIAN_POINT('Ctrl Pts',(-17.2687574251428,-68.5849318259449,
0.));
#70621=CARTESIAN_POINT('Ctrl Pts',(-17.2687574251428,-68.5849318259449,
12.));
#70622=CARTESIAN_POINT('Ctrl Pts',(-17.2677013298057,-68.6062649092764,
0.));
#70623=CARTESIAN_POINT('Ctrl Pts',(-17.2677013298057,-68.6062649092764,
12.));
#70624=CARTESIAN_POINT('Ctrl Pts',(-17.2666206986084,-68.6276457714729,
0.));
#70625=CARTESIAN_POINT('Ctrl Pts',(-17.2666206986084,-68.6276457714729,
12.));
#70626=CARTESIAN_POINT('Ctrl Pts',(-17.2655154627928,-68.6490742512057,
0.));
#70627=CARTESIAN_POINT('Ctrl Pts',(-17.2655154627928,-68.6490742512057,
12.));
#70628=CARTESIAN_POINT('Ctrl Pts',(-17.2643855540892,-68.6705501880249,
0.));
#70629=CARTESIAN_POINT('Ctrl Pts',(-17.2643855540892,-68.6705501880249,
12.));
#70630=CARTESIAN_POINT('Ctrl Pts',(-17.2632309046892,-68.6920734222938,
0.));
#70631=CARTESIAN_POINT('Ctrl Pts',(-17.2632309046892,-68.6920734222938,
12.));
#70632=CARTESIAN_POINT('Ctrl Pts',(-17.2620514472182,-68.7136437951097,
0.));
#70633=CARTESIAN_POINT('Ctrl Pts',(-17.2620514472182,-68.7136437951097,
12.));
#70634=CARTESIAN_POINT('Ctrl Pts',(-17.2608471147185,-68.7352611482547,
0.));
#70635=CARTESIAN_POINT('Ctrl Pts',(-17.2608471147185,-68.7352611482547,
12.));
#70636=CARTESIAN_POINT('Ctrl Pts',(-17.259617840655,-68.7569253242333,0.));
#70637=CARTESIAN_POINT('Ctrl Pts',(-17.259617840655,-68.7569253242333,12.));
#70638=CARTESIAN_POINT('Ctrl Pts',(-17.2583635589198,-68.7786361662882,
0.));
#70639=CARTESIAN_POINT('Ctrl Pts',(-17.2583635589198,-68.7786361662882,
12.));
#70640=CARTESIAN_POINT('Ctrl Pts',(-17.2570842038383,-68.8003935184184,
0.));
#70641=CARTESIAN_POINT('Ctrl Pts',(-17.2570842038383,-68.8003935184184,
12.));
#70642=CARTESIAN_POINT('Ctrl Pts',(-17.2557797101812,-68.8221972253941,
0.));
#70643=CARTESIAN_POINT('Ctrl Pts',(-17.2557797101812,-68.8221972253941,
12.));
#70644=CARTESIAN_POINT('Ctrl Pts',(-17.2544500131624,-68.844047132755,0.));
#70645=CARTESIAN_POINT('Ctrl Pts',(-17.2544500131624,-68.844047132755,12.));
#70646=CARTESIAN_POINT('Ctrl Pts',(-17.2530950484258,-68.8659430867972,
0.));
#70647=CARTESIAN_POINT('Ctrl Pts',(-17.2530950484258,-68.8659430867972,
12.));
#70648=CARTESIAN_POINT('Ctrl Pts',(-17.2517147520376,-68.8878849345557,
0.));
#70649=CARTESIAN_POINT('Ctrl Pts',(-17.2517147520376,-68.8878849345557,
12.));
#70650=CARTESIAN_POINT('Ctrl Pts',(-17.2503090604792,-68.909872523787,0.));
#70651=CARTESIAN_POINT('Ctrl Pts',(-17.2503090604792,-68.909872523787,12.));
#70652=CARTESIAN_POINT('Ctrl Pts',(-17.248877910643,-68.9319057029409,0.));
#70653=CARTESIAN_POINT('Ctrl Pts',(-17.248877910643,-68.9319057029409,12.));
#70654=CARTESIAN_POINT('Ctrl Pts',(-17.2474212398275,-68.9539843211619,
0.));
#70655=CARTESIAN_POINT('Ctrl Pts',(-17.2474212398275,-68.9539843211619,
12.));
#70656=CARTESIAN_POINT('Ctrl Pts',(-17.2459389857327,-68.9761082282922,
0.));
#70657=CARTESIAN_POINT('Ctrl Pts',(-17.2459389857327,-68.9761082282922,
12.));
#70658=CARTESIAN_POINT('Ctrl Pts',(-17.2444310864585,-68.9982772748694,
0.));
#70659=CARTESIAN_POINT('Ctrl Pts',(-17.2444310864585,-68.9982772748694,
12.));
#70660=CARTESIAN_POINT('Ctrl Pts',(-17.2428974805044,-69.0204913121225,
0.));
#70661=CARTESIAN_POINT('Ctrl Pts',(-17.2428974805044,-69.0204913121225,
12.));
#70662=CARTESIAN_POINT('Ctrl Pts',(-17.2413381067723,-69.0427501919636,
0.));
#70663=CARTESIAN_POINT('Ctrl Pts',(-17.2413381067723,-69.0427501919636,
12.));
#70664=CARTESIAN_POINT('Ctrl Pts',(-17.2397529045589,-69.065053766986,0.));
#70665=CARTESIAN_POINT('Ctrl Pts',(-17.2397529045589,-69.065053766986,12.));
#70666=CARTESIAN_POINT('Ctrl Pts',(-17.238141813549,-69.0874018904599,0.));
#70667=CARTESIAN_POINT('Ctrl Pts',(-17.238141813549,-69.0874018904599,12.));
#70668=CARTESIAN_POINT('Ctrl Pts',(-17.2365047738125,-69.1097944163245,
0.));
#70669=CARTESIAN_POINT('Ctrl Pts',(-17.2365047738125,-69.1097944163245,
12.));
#70670=CARTESIAN_POINT('Ctrl Pts',(-17.2348417258015,-69.1322311991752,
0.));
#70671=CARTESIAN_POINT('Ctrl Pts',(-17.2348417258015,-69.1322311991752,
12.));
#70672=CARTESIAN_POINT('Ctrl Pts',(-17.2331526103506,-69.1547120942527,
0.));
#70673=CARTESIAN_POINT('Ctrl Pts',(-17.2331526103506,-69.1547120942527,
12.));
#70674=CARTESIAN_POINT('Ctrl Pts',(-17.23143736867,-69.1772369574447,0.));
#70675=CARTESIAN_POINT('Ctrl Pts',(-17.23143736867,-69.1772369574447,12.));
#70676=CARTESIAN_POINT('Ctrl Pts',(-17.2296959423407,-69.1998056452828,
0.));
#70677=CARTESIAN_POINT('Ctrl Pts',(-17.2296959423407,-69.1998056452828,
12.));
#70678=CARTESIAN_POINT('Ctrl Pts',(-17.227928273312,-69.222418014938,0.));
#70679=CARTESIAN_POINT('Ctrl Pts',(-17.227928273312,-69.222418014938,12.));
#70680=CARTESIAN_POINT('Ctrl Pts',(-17.226134303902,-69.2450739242109,0.));
#70681=CARTESIAN_POINT('Ctrl Pts',(-17.226134303902,-69.2450739242109,12.));
#70682=CARTESIAN_POINT('Ctrl Pts',(-17.224313976797,-69.2677732315224,0.));
#70683=CARTESIAN_POINT('Ctrl Pts',(-17.224313976797,-69.2677732315224,12.));
#70684=CARTESIAN_POINT('Ctrl Pts',(-17.2224672350438,-69.2905157959166,
0.));
#70685=CARTESIAN_POINT('Ctrl Pts',(-17.2224672350438,-69.2905157959166,
12.));
#70686=CARTESIAN_POINT('Ctrl Pts',(-17.2205940220459,-69.3133014770555,
0.));
#70687=CARTESIAN_POINT('Ctrl Pts',(-17.2205940220459,-69.3133014770555,
12.));
#70688=CARTESIAN_POINT('Ctrl Pts',(-17.2186942815602,-69.3361301352141,
0.));
#70689=CARTESIAN_POINT('Ctrl Pts',(-17.2186942815602,-69.3361301352141,
12.));
#70690=CARTESIAN_POINT('Ctrl Pts',(-17.2167679576984,-69.3590016312692,
0.));
#70691=CARTESIAN_POINT('Ctrl Pts',(-17.2167679576984,-69.3590016312692,
12.));
#70692=CARTESIAN_POINT('Ctrl Pts',(-17.2148149949252,-69.3819158266916,
0.));
#70693=CARTESIAN_POINT('Ctrl Pts',(-17.2148149949252,-69.3819158266916,
12.));
#70694=CARTESIAN_POINT('Ctrl Pts',(-17.2128353380502,-69.404872583548,0.));
#70695=CARTESIAN_POINT('Ctrl Pts',(-17.2128353380502,-69.404872583548,12.));
#70696=CARTESIAN_POINT('Ctrl Pts',(-17.2108289322254,-69.4278717644973,
0.));
#70697=CARTESIAN_POINT('Ctrl Pts',(-17.2108289322254,-69.4278717644973,
12.));
#70698=CARTESIAN_POINT('Ctrl Pts',(-17.2087957229423,-69.450913232785,0.));
#70699=CARTESIAN_POINT('Ctrl Pts',(-17.2087957229423,-69.450913232785,12.));
#70700=CARTESIAN_POINT('Ctrl Pts',(-17.2067356560336,-69.4739968522313,
0.));
#70701=CARTESIAN_POINT('Ctrl Pts',(-17.2067356560336,-69.4739968522313,
12.));
#70702=CARTESIAN_POINT('Ctrl Pts',(-17.2046486776708,-69.4971224872269,
0.));
#70703=CARTESIAN_POINT('Ctrl Pts',(-17.2046486776708,-69.4971224872269,
12.));
#70704=CARTESIAN_POINT('Ctrl Pts',(-17.2025347343577,-69.5202900027367,
0.));
#70705=CARTESIAN_POINT('Ctrl Pts',(-17.2025347343577,-69.5202900027367,
12.));
#70706=CARTESIAN_POINT('Ctrl Pts',(-17.2003937729268,-69.5434992642944,
0.));
#70707=CARTESIAN_POINT('Ctrl Pts',(-17.2003937729268,-69.5434992642944,
12.));
#70708=CARTESIAN_POINT('Ctrl Pts',(-17.1982257405377,-69.5667501379969,
0.));
#70709=CARTESIAN_POINT('Ctrl Pts',(-17.1982257405377,-69.5667501379969,
12.));
#70710=CARTESIAN_POINT('Ctrl Pts',(-17.196030584678,-69.5900424904921,0.));
#70711=CARTESIAN_POINT('Ctrl Pts',(-17.196030584678,-69.5900424904921,12.));
#70712=CARTESIAN_POINT('Ctrl Pts',(-17.1938082531612,-69.6133761889748,
0.));
#70713=CARTESIAN_POINT('Ctrl Pts',(-17.1938082531612,-69.6133761889748,
12.));
#70714=CARTESIAN_POINT('Ctrl Pts',(-17.1915586941192,-69.6367511011898,
0.));
#70715=CARTESIAN_POINT('Ctrl Pts',(-17.1915586941192,-69.6367511011898,
12.));
#70716=CARTESIAN_POINT('Ctrl Pts',(-17.1892818560002,-69.6601670954269,
0.));
#70717=CARTESIAN_POINT('Ctrl Pts',(-17.1892818560002,-69.6601670954269,
12.));
#70718=CARTESIAN_POINT('Ctrl Pts',(-17.1869776875666,-69.6836240405164,
0.));
#70719=CARTESIAN_POINT('Ctrl Pts',(-17.1869776875666,-69.6836240405164,
12.));
#70720=CARTESIAN_POINT('Ctrl Pts',(-17.1846461378973,-69.7071218058178,
0.));
#70721=CARTESIAN_POINT('Ctrl Pts',(-17.1846461378973,-69.7071218058178,
12.));
#70722=CARTESIAN_POINT('Ctrl Pts',(-17.1822871563842,-69.7306602612155,
0.));
#70723=CARTESIAN_POINT('Ctrl Pts',(-17.1822871563842,-69.7306602612155,
12.));
#70724=CARTESIAN_POINT('Ctrl Pts',(-17.179900692726,-69.7542392771234,0.));
#70725=CARTESIAN_POINT('Ctrl Pts',(-17.179900692726,-69.7542392771234,12.));
#70726=CARTESIAN_POINT('Ctrl Pts',(-17.1774866969256,-69.777858724479,0.));
#70727=CARTESIAN_POINT('Ctrl Pts',(-17.1774866969256,-69.777858724479,12.));
#70728=CARTESIAN_POINT('Ctrl Pts',(-17.1750451192885,-69.8015184747398,
0.));
#70729=CARTESIAN_POINT('Ctrl Pts',(-17.1750451192885,-69.8015184747398,
12.));
#70730=CARTESIAN_POINT('Ctrl Pts',(-17.1725759104251,-69.8252183998702,
0.));
#70731=CARTESIAN_POINT('Ctrl Pts',(-17.1725759104251,-69.8252183998702,
12.));
#70732=CARTESIAN_POINT('Ctrl Pts',(-17.1700790212473,-69.8489583723407,
0.));
#70733=CARTESIAN_POINT('Ctrl Pts',(-17.1700790212473,-69.8489583723407,
12.));
#70734=CARTESIAN_POINT('Ctrl Pts',(-17.167554402962,-69.8727382651286,0.));
#70735=CARTESIAN_POINT('Ctrl Pts',(-17.167554402962,-69.8727382651286,12.));
#70736=CARTESIAN_POINT('Ctrl Pts',(-17.1650020070686,-69.8965579517147,
0.));
#70737=CARTESIAN_POINT('Ctrl Pts',(-17.1650020070686,-69.8965579517147,
12.));
#70738=CARTESIAN_POINT('Ctrl Pts',(-17.1624217853578,-69.9204173060781,
0.));
#70739=CARTESIAN_POINT('Ctrl Pts',(-17.1624217853578,-69.9204173060781,
12.));
#70740=CARTESIAN_POINT('Ctrl Pts',(-17.1598136899144,-69.9443162026865,
0.));
#70741=CARTESIAN_POINT('Ctrl Pts',(-17.1598136899144,-69.9443162026865,
12.));
#70742=CARTESIAN_POINT('Ctrl Pts',(-17.1571776731139,-69.9682545164939,
0.));
#70743=CARTESIAN_POINT('Ctrl Pts',(-17.1571776731139,-69.9682545164939,
12.));
#70744=CARTESIAN_POINT('Ctrl Pts',(-17.154513687616,-69.9922321229424,0.));
#70745=CARTESIAN_POINT('Ctrl Pts',(-17.154513687616,-69.9922321229424,12.));
#70746=CARTESIAN_POINT('Ctrl Pts',(-17.1518216863623,-70.0162488979584,
0.));
#70747=CARTESIAN_POINT('Ctrl Pts',(-17.1518216863623,-70.0162488979584,
12.));
#70748=CARTESIAN_POINT('Ctrl Pts',(-17.1491016225749,-70.0403047179483,
0.));
#70749=CARTESIAN_POINT('Ctrl Pts',(-17.1491016225749,-70.0403047179483,
12.));
#70750=CARTESIAN_POINT('Ctrl Pts',(-17.1463534497594,-70.0643994597873,
0.));
#70751=CARTESIAN_POINT('Ctrl Pts',(-17.1463534497594,-70.0643994597873,
12.));
#70752=CARTESIAN_POINT('Ctrl Pts',(-17.1435771217018,-70.0885330008179,
0.));
#70753=CARTESIAN_POINT('Ctrl Pts',(-17.1435771217018,-70.0885330008179,
12.));
#70754=CARTESIAN_POINT('Ctrl Pts',(-17.1407725924617,-70.1127052188522,
0.));
#70755=CARTESIAN_POINT('Ctrl Pts',(-17.1407725924617,-70.1127052188522,
12.));
#70756=CARTESIAN_POINT('Ctrl Pts',(-17.1379398163709,-70.1369159921687,
0.));
#70757=CARTESIAN_POINT('Ctrl Pts',(-17.1379398163709,-70.1369159921687,
12.));
#70758=CARTESIAN_POINT('Ctrl Pts',(-17.1350787480312,-70.1611651995083,
0.));
#70759=CARTESIAN_POINT('Ctrl Pts',(-17.1350787480312,-70.1611651995083,
12.));
#70760=CARTESIAN_POINT('Ctrl Pts',(-17.1321893423182,-70.1854527200631,
0.));
#70761=CARTESIAN_POINT('Ctrl Pts',(-17.1321893423182,-70.1854527200631,
12.));
#70762=CARTESIAN_POINT('Ctrl Pts',(-17.1292715543778,-70.2097784334747,
0.));
#70763=CARTESIAN_POINT('Ctrl Pts',(-17.1292715543778,-70.2097784334747,
12.));
#70764=CARTESIAN_POINT('Ctrl Pts',(-17.1263253396202,-70.2341422198363,
0.));
#70765=CARTESIAN_POINT('Ctrl Pts',(-17.1263253396202,-70.2341422198363,
12.));
#70766=CARTESIAN_POINT('Ctrl Pts',(-17.1233506537176,-70.2585439596901,
0.));
#70767=CARTESIAN_POINT('Ctrl Pts',(-17.1233506537176,-70.2585439596901,
12.));
#70768=CARTESIAN_POINT('Ctrl Pts',(-17.1203474526031,-70.2829835340238,
0.));
#70769=CARTESIAN_POINT('Ctrl Pts',(-17.1203474526031,-70.2829835340238,
12.));
#70770=CARTESIAN_POINT('Ctrl Pts',(-17.1173156924733,-70.3074608242608,
0.));
#70771=CARTESIAN_POINT('Ctrl Pts',(-17.1173156924733,-70.3074608242608,
12.));
#70772=CARTESIAN_POINT('Ctrl Pts',(-17.1142553297867,-70.3319757122568,
0.));
#70773=CARTESIAN_POINT('Ctrl Pts',(-17.1142553297867,-70.3319757122568,
12.));
#70774=CARTESIAN_POINT('Ctrl Pts',(-17.1111663212568,-70.3565280803022,
0.));
#70775=CARTESIAN_POINT('Ctrl Pts',(-17.1111663212568,-70.3565280803022,
12.));
#70776=CARTESIAN_POINT('Ctrl Pts',(-17.1080486238499,-70.3811178111201,
0.));
#70777=CARTESIAN_POINT('Ctrl Pts',(-17.1080486238499,-70.3811178111201,
12.));
#70778=CARTESIAN_POINT('Ctrl Pts',(-17.1049021947834,-70.4057447878624,
0.));
#70779=CARTESIAN_POINT('Ctrl Pts',(-17.1049021947834,-70.4057447878624,
12.));
#70780=CARTESIAN_POINT('Ctrl Pts',(-17.1017269915292,-70.430408894101,0.));
#70781=CARTESIAN_POINT('Ctrl Pts',(-17.1017269915292,-70.430408894101,12.));
#70782=CARTESIAN_POINT('Ctrl Pts',(-17.0985229718124,-70.4551100138238,
0.));
#70783=CARTESIAN_POINT('Ctrl Pts',(-17.0985229718124,-70.4551100138238,
12.));
#70784=CARTESIAN_POINT('Ctrl Pts',(-17.0952900936048,-70.4798480314381,
0.));
#70785=CARTESIAN_POINT('Ctrl Pts',(-17.0952900936048,-70.4798480314381,
12.));
#70786=CARTESIAN_POINT('Ctrl Pts',(-17.0920283151219,-70.5046228317677,
0.));
#70787=CARTESIAN_POINT('Ctrl Pts',(-17.0920283151219,-70.5046228317677,
12.));
#70788=CARTESIAN_POINT('Ctrl Pts',(-17.088737594822,-70.5294343000513,0.));
#70789=CARTESIAN_POINT('Ctrl Pts',(-17.088737594822,-70.5294343000513,12.));
#70790=CARTESIAN_POINT('Ctrl Pts',(-17.0854178914087,-70.5542823219331,
0.));
#70791=CARTESIAN_POINT('Ctrl Pts',(-17.0854178914087,-70.5542823219331,
12.));
#70792=CARTESIAN_POINT('Ctrl Pts',(-17.082069163831,-70.5791667834582,0.));
#70793=CARTESIAN_POINT('Ctrl Pts',(-17.082069163831,-70.5791667834582,12.));
#70794=CARTESIAN_POINT('Ctrl Pts',(-17.0786913712763,-70.6040875710749,
0.));
#70795=CARTESIAN_POINT('Ctrl Pts',(-17.0786913712763,-70.6040875710749,
12.));
#70796=CARTESIAN_POINT('Ctrl Pts',(-17.0752844731678,-70.6290445716337,
0.));
#70797=CARTESIAN_POINT('Ctrl Pts',(-17.0752844731678,-70.6290445716337,
12.));
#70798=CARTESIAN_POINT('Ctrl Pts',(-17.0718484291624,-70.6540376723841,
0.));
#70799=CARTESIAN_POINT('Ctrl Pts',(-17.0718484291624,-70.6540376723841,
12.));
#70800=CARTESIAN_POINT('Ctrl Pts',(-17.0683831991532,-70.6790667609679,
0.));
#70801=CARTESIAN_POINT('Ctrl Pts',(-17.0683831991532,-70.6790667609679,
12.));
#70802=CARTESIAN_POINT('Ctrl Pts',(-17.0648887432713,-70.7041317254125,
0.));
#70803=CARTESIAN_POINT('Ctrl Pts',(-17.0648887432713,-70.7041317254125,
12.));
#70804=CARTESIAN_POINT('Ctrl Pts',(-17.0613650218787,-70.7292324541341,
0.));
#70805=CARTESIAN_POINT('Ctrl Pts',(-17.0613650218787,-70.7292324541341,
12.));
#70806=CARTESIAN_POINT('Ctrl Pts',(-17.0578119955649,-70.7543688359374,
0.));
#70807=CARTESIAN_POINT('Ctrl Pts',(-17.0578119955649,-70.7543688359374,
12.));
#70808=CARTESIAN_POINT('Ctrl Pts',(-17.0542296251462,-70.7795407600127,
0.));
#70809=CARTESIAN_POINT('Ctrl Pts',(-17.0542296251462,-70.7795407600127,
12.));
#70810=CARTESIAN_POINT('Ctrl Pts',(-17.0506178716664,-70.8047481159306,
0.));
#70811=CARTESIAN_POINT('Ctrl Pts',(-17.0506178716664,-70.8047481159306,
12.));
#70812=CARTESIAN_POINT('Ctrl Pts',(-17.0469766964005,-70.8299907936346,
0.));
#70813=CARTESIAN_POINT('Ctrl Pts',(-17.0469766964005,-70.8299907936346,
12.));
#70814=CARTESIAN_POINT('Ctrl Pts',(-17.0433060608478,-70.8552686834435,
0.));
#70815=CARTESIAN_POINT('Ctrl Pts',(-17.0433060608478,-70.8552686834435,
12.));
#70816=CARTESIAN_POINT('Ctrl Pts',(-17.0396059267279,-70.8805816760507,
0.));
#70817=CARTESIAN_POINT('Ctrl Pts',(-17.0396059267279,-70.8805816760507,
12.));
#70818=CARTESIAN_POINT('Ctrl Pts',(-17.0358762559786,-70.9059296625214,
0.));
#70819=CARTESIAN_POINT('Ctrl Pts',(-17.0358762559786,-70.9059296625214,
12.));
#70820=CARTESIAN_POINT('Ctrl Pts',(-17.0321170107562,-70.9313125342872,
0.));
#70821=CARTESIAN_POINT('Ctrl Pts',(-17.0321170107562,-70.9313125342872,
12.));
#70822=CARTESIAN_POINT('Ctrl Pts',(-17.028328153439,-70.9567301831355,0.));
#70823=CARTESIAN_POINT('Ctrl Pts',(-17.028328153439,-70.9567301831355,12.));
#70824=CARTESIAN_POINT('Ctrl Pts',(-17.0245096466228,-70.9821825012134,
0.));
#70825=CARTESIAN_POINT('Ctrl Pts',(-17.0245096466228,-70.9821825012134,
12.));
#70826=CARTESIAN_POINT('Ctrl Pts',(-17.0206614531165,-71.0076693810303,
0.));
#70827=CARTESIAN_POINT('Ctrl Pts',(-17.0206614531165,-71.0076693810303,
12.));
#70828=CARTESIAN_POINT('Ctrl Pts',(-17.0167835359419,-71.0331907154575,
0.));
#70829=CARTESIAN_POINT('Ctrl Pts',(-17.0167835359419,-71.0331907154575,
12.));
#70830=CARTESIAN_POINT('Ctrl Pts',(-17.0128758583335,-71.0587463977266,
0.));
#70831=CARTESIAN_POINT('Ctrl Pts',(-17.0128758583335,-71.0587463977266,
12.));
#70832=CARTESIAN_POINT('Ctrl Pts',(-17.0089383837436,-71.0843363214216,
0.));
#70833=CARTESIAN_POINT('Ctrl Pts',(-17.0089383837436,-71.0843363214216,
12.));
#70834=CARTESIAN_POINT('Ctrl Pts',(-17.0049710758393,-71.1099603804779,
0.));
#70835=CARTESIAN_POINT('Ctrl Pts',(-17.0049710758393,-71.1099603804779,
12.));
#70836=CARTESIAN_POINT('Ctrl Pts',(-17.0009738984935,-71.1356184691799,
0.));
#70837=CARTESIAN_POINT('Ctrl Pts',(-17.0009738984935,-71.1356184691799,
12.));
#70838=CARTESIAN_POINT('Ctrl Pts',(-16.9969468157824,-71.1613104821565,
0.));
#70839=CARTESIAN_POINT('Ctrl Pts',(-16.9969468157824,-71.1613104821565,
12.));
#70840=CARTESIAN_POINT('Ctrl Pts',(-16.9928897919829,-71.1870363143742,
0.));
#70841=CARTESIAN_POINT('Ctrl Pts',(-16.9928897919829,-71.1870363143742,
12.));
#70842=CARTESIAN_POINT('Ctrl Pts',(-16.9888027915743,-71.2127958611248,
0.));
#70843=CARTESIAN_POINT('Ctrl Pts',(-16.9888027915743,-71.2127958611248,
12.));
#70844=CARTESIAN_POINT('Ctrl Pts',(-16.9846857792385,-71.2385890180233,
0.));
#70845=CARTESIAN_POINT('Ctrl Pts',(-16.9846857792385,-71.2385890180233,
12.));
#70846=CARTESIAN_POINT('Ctrl Pts',(-16.9805387198573,-71.2644156810209,
0.));
#70847=CARTESIAN_POINT('Ctrl Pts',(-16.9805387198573,-71.2644156810209,
12.));
#70848=CARTESIAN_POINT('Ctrl Pts',(-16.9763615785137,-71.2902757464127,
0.));
#70849=CARTESIAN_POINT('Ctrl Pts',(-16.9763615785137,-71.2902757464127,
12.));
#70850=CARTESIAN_POINT('Ctrl Pts',(-16.9721543204951,-71.3161691108425,
0.));
#70851=CARTESIAN_POINT('Ctrl Pts',(-16.9721543204951,-71.3161691108425,
12.));
#70852=CARTESIAN_POINT('Ctrl Pts',(-16.9679169112993,-71.3420956713072,
0.));
#70853=CARTESIAN_POINT('Ctrl Pts',(-16.9679169112993,-71.3420956713072,
12.));
#70854=CARTESIAN_POINT('Ctrl Pts',(-16.9636493166395,-71.3680553251548,
0.));
#70855=CARTESIAN_POINT('Ctrl Pts',(-16.9636493166395,-71.3680553251548,
12.));
#70856=CARTESIAN_POINT('Ctrl Pts',(-16.9593515024274,-71.3940479700663,
0.));
#70857=CARTESIAN_POINT('Ctrl Pts',(-16.9593515024274,-71.3940479700663,
12.));
#70858=CARTESIAN_POINT('Ctrl Pts',(-16.9550234347619,-71.4200735040374,
0.));
#70859=CARTESIAN_POINT('Ctrl Pts',(-16.9550234347619,-71.4200735040374,
12.));
#70860=CARTESIAN_POINT('Ctrl Pts',(-16.9506650799188,-71.4461318253561,
0.));
#70861=CARTESIAN_POINT('Ctrl Pts',(-16.9506650799188,-71.4461318253561,
12.));
#70862=CARTESIAN_POINT('Ctrl Pts',(-16.9462764043445,-71.4722228325805,
0.));
#70863=CARTESIAN_POINT('Ctrl Pts',(-16.9462764043445,-71.4722228325805,
12.));
#70864=CARTESIAN_POINT('Ctrl Pts',(-16.9418573746492,-71.498346424507,0.));
#70865=CARTESIAN_POINT('Ctrl Pts',(-16.9418573746492,-71.498346424507,12.));
#70866=CARTESIAN_POINT('Ctrl Pts',(-16.9374079576204,-71.5245025002154,
0.));
#70867=CARTESIAN_POINT('Ctrl Pts',(-16.9374079576204,-71.5245025002154,
12.));
#70868=CARTESIAN_POINT('Ctrl Pts',(-16.9329281202379,-71.5506909591139,
0.));
#70869=CARTESIAN_POINT('Ctrl Pts',(-16.9329281202379,-71.5506909591139,
12.));
#70870=CARTESIAN_POINT('Ctrl Pts',(-16.9284178296934,-71.5769117009844,
0.));
#70871=CARTESIAN_POINT('Ctrl Pts',(-16.9284178296934,-71.5769117009844,
12.));
#70872=CARTESIAN_POINT('Ctrl Pts',(-16.923877053407,-71.6031646260169,0.));
#70873=CARTESIAN_POINT('Ctrl Pts',(-16.923877053407,-71.6031646260169,12.));
#70874=CARTESIAN_POINT('Ctrl Pts',(-16.9193057590605,-71.6294496348644,
0.));
#70875=CARTESIAN_POINT('Ctrl Pts',(-16.9193057590605,-71.6294496348644,
12.));
#70876=CARTESIAN_POINT('Ctrl Pts',(-16.9147039145715,-71.6557666285908,
0.));
#70877=CARTESIAN_POINT('Ctrl Pts',(-16.9147039145715,-71.6557666285908,
12.));
#70878=CARTESIAN_POINT('Ctrl Pts',(-16.9100714880367,-71.6821155085605,
0.));
#70879=CARTESIAN_POINT('Ctrl Pts',(-16.9100714880367,-71.6821155085605,
12.));
#70880=CARTESIAN_POINT('Ctrl Pts',(-16.9054084476847,-71.7084961763355,
0.));
#70881=CARTESIAN_POINT('Ctrl Pts',(-16.9054084476847,-71.7084961763355,
12.));
#70882=CARTESIAN_POINT('Ctrl Pts',(-16.9007147618344,-71.7349085335796,
0.));
#70883=CARTESIAN_POINT('Ctrl Pts',(-16.9007147618344,-71.7349085335796,
12.));
#70884=CARTESIAN_POINT('Ctrl Pts',(-16.895990398841,-71.761352481924,0.));
#70885=CARTESIAN_POINT('Ctrl Pts',(-16.895990398841,-71.761352481924,12.));
#70886=CARTESIAN_POINT('Ctrl Pts',(-16.8912353270944,-71.7878279229556,
0.));
#70887=CARTESIAN_POINT('Ctrl Pts',(-16.8912353270944,-71.7878279229556,
12.));
#70888=CARTESIAN_POINT('Ctrl Pts',(-16.8864495151347,-71.8143347584977,
0.));
#70889=CARTESIAN_POINT('Ctrl Pts',(-16.8864495151347,-71.8143347584977,
12.));
#70890=CARTESIAN_POINT('Ctrl Pts',(-16.8816329317473,-71.8408728908269,
0.));
#70891=CARTESIAN_POINT('Ctrl Pts',(-16.8816329317473,-71.8408728908269,
12.));
#70892=CARTESIAN_POINT('Ctrl Pts',(-16.87678554607,-71.8674422229151,0.));
#70893=CARTESIAN_POINT('Ctrl Pts',(-16.87678554607,-71.8674422229151,12.));
#70894=CARTESIAN_POINT('Ctrl Pts',(-16.8719073276967,-71.8940426586521,
0.));
#70895=CARTESIAN_POINT('Ctrl Pts',(-16.8719073276967,-71.8940426586521,
12.));
#70896=CARTESIAN_POINT('Ctrl Pts',(-16.8669982467915,-71.920674103086,0.));
#70897=CARTESIAN_POINT('Ctrl Pts',(-16.8669982467915,-71.920674103086,12.));
#70898=CARTESIAN_POINT('Ctrl Pts',(-16.862058273843,-71.9473364618889,0.));
#70899=CARTESIAN_POINT('Ctrl Pts',(-16.862058273843,-71.9473364618889,12.));
#70900=CARTESIAN_POINT('Ctrl Pts',(-16.8570873794264,-71.9740296408319,
0.));
#70901=CARTESIAN_POINT('Ctrl Pts',(-16.8570873794264,-71.9740296408319,
12.));
#70902=CARTESIAN_POINT('Ctrl Pts',(-16.8520855339444,-72.0007535452071,
0.));
#70903=CARTESIAN_POINT('Ctrl Pts',(-16.8520855339444,-72.0007535452071,
12.));
#70904=CARTESIAN_POINT('Ctrl Pts',(-16.8470527074278,-72.0275080793742,
0.));
#70905=CARTESIAN_POINT('Ctrl Pts',(-16.8470527074278,-72.0275080793742,
12.));
#70906=CARTESIAN_POINT('Ctrl Pts',(-16.8419888691984,-72.0542931459865,
0.));
#70907=CARTESIAN_POINT('Ctrl Pts',(-16.8419888691984,-72.0542931459865,
12.));
#70908=CARTESIAN_POINT('Ctrl Pts',(-16.8368939881457,-72.0811086466177,
0.));
#70909=CARTESIAN_POINT('Ctrl Pts',(-16.8368939881457,-72.0811086466177,
12.));
#70910=CARTESIAN_POINT('Ctrl Pts',(-16.8317680333415,-72.1079544831568,
0.));
#70911=CARTESIAN_POINT('Ctrl Pts',(-16.8317680333415,-72.1079544831568,
12.));
#70912=CARTESIAN_POINT('Ctrl Pts',(-16.8266109745801,-72.1348305590233,
0.));
#70913=CARTESIAN_POINT('Ctrl Pts',(-16.8266109745801,-72.1348305590233,
12.));
#70914=CARTESIAN_POINT('Ctrl Pts',(-16.8214227828941,-72.1617367803226,
0.));
#70915=CARTESIAN_POINT('Ctrl Pts',(-16.8214227828941,-72.1617367803226,
12.));
#70916=CARTESIAN_POINT('Ctrl Pts',(-16.8162034312257,-72.1886730573389,
0.));
#70917=CARTESIAN_POINT('Ctrl Pts',(-16.8162034312257,-72.1886730573389,
12.));
#70918=CARTESIAN_POINT('Ctrl Pts',(-16.8109528945876,-72.2156393048868,
0.));
#70919=CARTESIAN_POINT('Ctrl Pts',(-16.8109528945876,-72.2156393048868,
12.));
#70920=CARTESIAN_POINT('Ctrl Pts',(-16.8056711485797,-72.242635439009,0.));
#70921=CARTESIAN_POINT('Ctrl Pts',(-16.8056711485797,-72.242635439009,12.));
#70922=CARTESIAN_POINT('Ctrl Pts',(-16.800358168223,-72.2696613743687,0.));
#70923=CARTESIAN_POINT('Ctrl Pts',(-16.800358168223,-72.2696613743687,12.));
#70924=CARTESIAN_POINT('Ctrl Pts',(-16.7950139266117,-72.2967170212331,
0.));
#70925=CARTESIAN_POINT('Ctrl Pts',(-16.7950139266117,-72.2967170212331,
12.));
#70926=CARTESIAN_POINT('Ctrl Pts',(-16.7896383937839,-72.323802282931,0.));
#70927=CARTESIAN_POINT('Ctrl Pts',(-16.7896383937839,-72.323802282931,12.));
#70928=CARTESIAN_POINT('Ctrl Pts',(-16.7842315351401,-72.3509170523038,
0.));
#70929=CARTESIAN_POINT('Ctrl Pts',(-16.7842315351401,-72.3509170523038,
12.));
#70930=CARTESIAN_POINT('Ctrl Pts',(-16.7787933137551,-72.3780612168057,
0.));
#70931=CARTESIAN_POINT('Ctrl Pts',(-16.7787933137551,-72.3780612168057,
12.));
#70932=CARTESIAN_POINT('Ctrl Pts',(-16.7733236932185,-72.4052346648058,
0.));
#70933=CARTESIAN_POINT('Ctrl Pts',(-16.7733236932185,-72.4052346648058,
12.));
#70934=CARTESIAN_POINT('Ctrl Pts',(-16.7678226404189,-72.4324372916884,
0.));
#70935=CARTESIAN_POINT('Ctrl Pts',(-16.7678226404189,-72.4324372916884,
12.));
#70936=CARTESIAN_POINT('Ctrl Pts',(-16.7622901280741,-72.4596690055347,
0.));
#70937=CARTESIAN_POINT('Ctrl Pts',(-16.7622901280741,-72.4596690055347,
12.));
#70938=CARTESIAN_POINT('Ctrl Pts',(-16.7567261380614,-72.4869297342051,
0.));
#70939=CARTESIAN_POINT('Ctrl Pts',(-16.7567261380614,-72.4869297342051,
12.));
#70940=CARTESIAN_POINT('Ctrl Pts',(-16.7511306618793,-72.5142194273203,
0.));
#70941=CARTESIAN_POINT('Ctrl Pts',(-16.7511306618793,-72.5142194273203,
12.));
#70942=CARTESIAN_POINT('Ctrl Pts',(-16.7455036973724,-72.5415380515905,
0.));
#70943=CARTESIAN_POINT('Ctrl Pts',(-16.7455036973724,-72.5415380515905,
12.));
#70944=CARTESIAN_POINT('Ctrl Pts',(-16.7409769365953,-72.563416080574,0.));
#70945=CARTESIAN_POINT('Ctrl Pts',(-16.7409769365953,-72.563416080574,12.));
#70946=CARTESIAN_POINT('Ctrl Pts',(-16.7375676985272,-72.5798376087406,
0.));
#70947=CARTESIAN_POINT('Ctrl Pts',(-16.7375676985272,-72.5798376087406,
12.));
#70948=CARTESIAN_POINT('Ctrl Pts',(-16.7352885767459,-72.5907910745874,
0.));
#70949=CARTESIAN_POINT('Ctrl Pts',(-16.7352885767459,-72.5907910745874,
12.));
#70950=CARTESIAN_POINT('Ctrl Pts',(-16.7341474417544,-72.5962692526112,
0.));
#70951=CARTESIAN_POINT('Ctrl Pts',(-16.7341474417544,-72.5962692526112,
12.));
#70952=CARTESIAN_POINT('',(-17.2912529479484,-67.8307641965655,0.));
#70953=CARTESIAN_POINT('Ctrl Pts',(-17.2912529479484,-67.8307641965655,
0.));
#70954=CARTESIAN_POINT('Ctrl Pts',(-17.2912149114119,-67.8346476309018,
0.));
#70955=CARTESIAN_POINT('Ctrl Pts',(-17.2911366591347,-67.842419897098,0.));
#70956=CARTESIAN_POINT('Ctrl Pts',(-17.291012743109,-67.8540944889687,0.));
#70957=CARTESIAN_POINT('Ctrl Pts',(-17.2908344459694,-67.8696929978782,
0.));
#70958=CARTESIAN_POINT('Ctrl Pts',(-17.2905897723948,-67.8892451049608,
0.));
#70959=CARTESIAN_POINT('Ctrl Pts',(-17.2903232740694,-67.9088511496686,
0.));
#70960=CARTESIAN_POINT('Ctrl Pts',(-17.2900349103981,-67.9285110571741,
0.));
#70961=CARTESIAN_POINT('Ctrl Pts',(-17.2897246158941,-67.9482246901667,
0.));
#70962=CARTESIAN_POINT('Ctrl Pts',(-17.2893923013894,-67.9679918502579,
0.));
#70963=CARTESIAN_POINT('Ctrl Pts',(-17.2890378644866,-67.987812304921,0.));
#70964=CARTESIAN_POINT('Ctrl Pts',(-17.28866119774,-68.007685808115,0.));
#70965=CARTESIAN_POINT('Ctrl Pts',(-17.2882621974721,-68.0276121227356,
0.));
#70966=CARTESIAN_POINT('Ctrl Pts',(-17.2878407730961,-68.0475910442424,
0.));
#70967=CARTESIAN_POINT('Ctrl Pts',(-17.2873968440839,-68.0676223930412,
0.));
#70968=CARTESIAN_POINT('Ctrl Pts',(-17.2869303355432,-68.0877060033205,
0.));
#70969=CARTESIAN_POINT('Ctrl Pts',(-17.2864411745459,-68.1078417137877,
0.));
#70970=CARTESIAN_POINT('Ctrl Pts',(-17.2859292855705,-68.1280293561511,
0.));
#70971=CARTESIAN_POINT('Ctrl Pts',(-17.2853945882072,-68.1482687493226,
0.));
#70972=CARTESIAN_POINT('Ctrl Pts',(-17.2848369995293,-68.1685597054232,
0.));
#70973=CARTESIAN_POINT('Ctrl Pts',(-17.2842564355799,-68.1889020335427,
0.));
#70974=CARTESIAN_POINT('Ctrl Pts',(-17.2836528130819,-68.2092955440567,
0.));
#70975=CARTESIAN_POINT('Ctrl Pts',(-17.2830260513867,-68.2297400535294,
0.));
#70976=CARTESIAN_POINT('Ctrl Pts',(-17.2823760723874,-68.2502353845071,
0.));
#70977=CARTESIAN_POINT('Ctrl Pts',(-17.2817027995831,-68.2707813631731,
0.));
#70978=CARTESIAN_POINT('Ctrl Pts',(-17.2810061574353,-68.2913778177261,
0.));
#70979=CARTESIAN_POINT('Ctrl Pts',(-17.2802860705815,-68.3120245763914,
0.));
#70980=CARTESIAN_POINT('Ctrl Pts',(-17.2795424631799,-68.3327214657575,
0.));
#70981=CARTESIAN_POINT('Ctrl Pts',(-17.2787752592484,-68.3534683116515,
0.));
#70982=CARTESIAN_POINT('Ctrl Pts',(-17.2779843829608,-68.3742649398964,
0.));
#70983=CARTESIAN_POINT('Ctrl Pts',(-17.2771697589384,-68.3951111770487,
0.));
#70984=CARTESIAN_POINT('Ctrl Pts',(-17.2763313126018,-68.4160068512753,
0.));
#70985=CARTESIAN_POINT('Ctrl Pts',(-17.2754689702992,-68.436951792677,0.));
#70986=CARTESIAN_POINT('Ctrl Pts',(-17.2745826591119,-68.4579458328185,
0.));
#70987=CARTESIAN_POINT('Ctrl Pts',(-17.2736723067365,-68.4789888044351,
0.));
#70988=CARTESIAN_POINT('Ctrl Pts',(-17.2727378413489,-68.5000805410911,
0.));
#70989=CARTESIAN_POINT('Ctrl Pts',(-17.2717791914544,-68.521220876786,0.));
#70990=CARTESIAN_POINT('Ctrl Pts',(-17.2707962858919,-68.5424096459772,
0.));
#70991=CARTESIAN_POINT('Ctrl Pts',(-17.269789053896,-68.5636466837517,0.));
#70992=CARTESIAN_POINT('Ctrl Pts',(-17.2687574251428,-68.5849318259449,
0.));
#70993=CARTESIAN_POINT('Ctrl Pts',(-17.2677013298057,-68.6062649092764,
0.));
#70994=CARTESIAN_POINT('Ctrl Pts',(-17.2666206986084,-68.6276457714729,
0.));
#70995=CARTESIAN_POINT('Ctrl Pts',(-17.2655154627928,-68.6490742512057,
0.));
#70996=CARTESIAN_POINT('Ctrl Pts',(-17.2643855540892,-68.6705501880249,
0.));
#70997=CARTESIAN_POINT('Ctrl Pts',(-17.2632309046892,-68.6920734222938,
0.));
#70998=CARTESIAN_POINT('Ctrl Pts',(-17.2620514472182,-68.7136437951097,
0.));
#70999=CARTESIAN_POINT('Ctrl Pts',(-17.2608471147185,-68.7352611482547,
0.));
#71000=CARTESIAN_POINT('Ctrl Pts',(-17.259617840655,-68.7569253242333,0.));
#71001=CARTESIAN_POINT('Ctrl Pts',(-17.2583635589198,-68.7786361662882,
0.));
#71002=CARTESIAN_POINT('Ctrl Pts',(-17.2570842038383,-68.8003935184184,
0.));
#71003=CARTESIAN_POINT('Ctrl Pts',(-17.2557797101812,-68.8221972253941,
0.));
#71004=CARTESIAN_POINT('Ctrl Pts',(-17.2544500131624,-68.844047132755,0.));
#71005=CARTESIAN_POINT('Ctrl Pts',(-17.2530950484258,-68.8659430867972,
0.));
#71006=CARTESIAN_POINT('Ctrl Pts',(-17.2517147520376,-68.8878849345557,
0.));
#71007=CARTESIAN_POINT('Ctrl Pts',(-17.2503090604792,-68.909872523787,0.));
#71008=CARTESIAN_POINT('Ctrl Pts',(-17.248877910643,-68.9319057029409,0.));
#71009=CARTESIAN_POINT('Ctrl Pts',(-17.2474212398275,-68.9539843211619,
0.));
#71010=CARTESIAN_POINT('Ctrl Pts',(-17.2459389857327,-68.9761082282922,
0.));
#71011=CARTESIAN_POINT('Ctrl Pts',(-17.2444310864585,-68.9982772748694,
0.));
#71012=CARTESIAN_POINT('Ctrl Pts',(-17.2428974805044,-69.0204913121225,
0.));
#71013=CARTESIAN_POINT('Ctrl Pts',(-17.2413381067723,-69.0427501919636,
0.));
#71014=CARTESIAN_POINT('Ctrl Pts',(-17.2397529045589,-69.065053766986,0.));
#71015=CARTESIAN_POINT('Ctrl Pts',(-17.238141813549,-69.0874018904599,0.));
#71016=CARTESIAN_POINT('Ctrl Pts',(-17.2365047738125,-69.1097944163245,
0.));
#71017=CARTESIAN_POINT('Ctrl Pts',(-17.2348417258015,-69.1322311991752,
0.));
#71018=CARTESIAN_POINT('Ctrl Pts',(-17.2331526103506,-69.1547120942527,
0.));
#71019=CARTESIAN_POINT('Ctrl Pts',(-17.23143736867,-69.1772369574447,0.));
#71020=CARTESIAN_POINT('Ctrl Pts',(-17.2296959423407,-69.1998056452828,
0.));
#71021=CARTESIAN_POINT('Ctrl Pts',(-17.227928273312,-69.222418014938,0.));
#71022=CARTESIAN_POINT('Ctrl Pts',(-17.226134303902,-69.2450739242109,0.));
#71023=CARTESIAN_POINT('Ctrl Pts',(-17.224313976797,-69.2677732315224,0.));
#71024=CARTESIAN_POINT('Ctrl Pts',(-17.2224672350438,-69.2905157959166,
0.));
#71025=CARTESIAN_POINT('Ctrl Pts',(-17.2205940220459,-69.3133014770555,
0.));
#71026=CARTESIAN_POINT('Ctrl Pts',(-17.2186942815602,-69.3361301352141,
0.));
#71027=CARTESIAN_POINT('Ctrl Pts',(-17.2167679576984,-69.3590016312692,
0.));
#71028=CARTESIAN_POINT('Ctrl Pts',(-17.2148149949252,-69.3819158266916,
0.));
#71029=CARTESIAN_POINT('Ctrl Pts',(-17.2128353380502,-69.404872583548,0.));
#71030=CARTESIAN_POINT('Ctrl Pts',(-17.2108289322254,-69.4278717644973,
0.));
#71031=CARTESIAN_POINT('Ctrl Pts',(-17.2087957229423,-69.450913232785,0.));
#71032=CARTESIAN_POINT('Ctrl Pts',(-17.2067356560336,-69.4739968522313,
0.));
#71033=CARTESIAN_POINT('Ctrl Pts',(-17.2046486776708,-69.4971224872269,
0.));
#71034=CARTESIAN_POINT('Ctrl Pts',(-17.2025347343577,-69.5202900027367,
0.));
#71035=CARTESIAN_POINT('Ctrl Pts',(-17.2003937729268,-69.5434992642944,
0.));
#71036=CARTESIAN_POINT('Ctrl Pts',(-17.1982257405377,-69.5667501379969,
0.));
#71037=CARTESIAN_POINT('Ctrl Pts',(-17.196030584678,-69.5900424904921,0.));
#71038=CARTESIAN_POINT('Ctrl Pts',(-17.1938082531612,-69.6133761889748,
0.));
#71039=CARTESIAN_POINT('Ctrl Pts',(-17.1915586941192,-69.6367511011898,
0.));
#71040=CARTESIAN_POINT('Ctrl Pts',(-17.1892818560002,-69.6601670954269,
0.));
#71041=CARTESIAN_POINT('Ctrl Pts',(-17.1869776875666,-69.6836240405164,
0.));
#71042=CARTESIAN_POINT('Ctrl Pts',(-17.1846461378973,-69.7071218058178,
0.));
#71043=CARTESIAN_POINT('Ctrl Pts',(-17.1822871563842,-69.7306602612155,
0.));
#71044=CARTESIAN_POINT('Ctrl Pts',(-17.179900692726,-69.7542392771234,0.));
#71045=CARTESIAN_POINT('Ctrl Pts',(-17.1774866969256,-69.777858724479,0.));
#71046=CARTESIAN_POINT('Ctrl Pts',(-17.1750451192885,-69.8015184747398,
0.));
#71047=CARTESIAN_POINT('Ctrl Pts',(-17.1725759104251,-69.8252183998702,
0.));
#71048=CARTESIAN_POINT('Ctrl Pts',(-17.1700790212473,-69.8489583723407,
0.));
#71049=CARTESIAN_POINT('Ctrl Pts',(-17.167554402962,-69.8727382651286,0.));
#71050=CARTESIAN_POINT('Ctrl Pts',(-17.1650020070686,-69.8965579517147,
0.));
#71051=CARTESIAN_POINT('Ctrl Pts',(-17.1624217853578,-69.9204173060781,
0.));
#71052=CARTESIAN_POINT('Ctrl Pts',(-17.1598136899144,-69.9443162026865,
0.));
#71053=CARTESIAN_POINT('Ctrl Pts',(-17.1571776731139,-69.9682545164939,
0.));
#71054=CARTESIAN_POINT('Ctrl Pts',(-17.154513687616,-69.9922321229424,0.));
#71055=CARTESIAN_POINT('Ctrl Pts',(-17.1518216863623,-70.0162488979584,
0.));
#71056=CARTESIAN_POINT('Ctrl Pts',(-17.1491016225749,-70.0403047179483,
0.));
#71057=CARTESIAN_POINT('Ctrl Pts',(-17.1463534497594,-70.0643994597873,
0.));
#71058=CARTESIAN_POINT('Ctrl Pts',(-17.1435771217018,-70.0885330008179,
0.));
#71059=CARTESIAN_POINT('Ctrl Pts',(-17.1407725924617,-70.1127052188522,
0.));
#71060=CARTESIAN_POINT('Ctrl Pts',(-17.1379398163709,-70.1369159921687,
0.));
#71061=CARTESIAN_POINT('Ctrl Pts',(-17.1350787480312,-70.1611651995083,
0.));
#71062=CARTESIAN_POINT('Ctrl Pts',(-17.1321893423182,-70.1854527200631,
0.));
#71063=CARTESIAN_POINT('Ctrl Pts',(-17.1292715543778,-70.2097784334747,
0.));
#71064=CARTESIAN_POINT('Ctrl Pts',(-17.1263253396202,-70.2341422198363,
0.));
#71065=CARTESIAN_POINT('Ctrl Pts',(-17.1233506537176,-70.2585439596901,
0.));
#71066=CARTESIAN_POINT('Ctrl Pts',(-17.1203474526031,-70.2829835340238,
0.));
#71067=CARTESIAN_POINT('Ctrl Pts',(-17.1173156924733,-70.3074608242608,
0.));
#71068=CARTESIAN_POINT('Ctrl Pts',(-17.1142553297867,-70.3319757122568,
0.));
#71069=CARTESIAN_POINT('Ctrl Pts',(-17.1111663212568,-70.3565280803022,
0.));
#71070=CARTESIAN_POINT('Ctrl Pts',(-17.1080486238499,-70.3811178111201,
0.));
#71071=CARTESIAN_POINT('Ctrl Pts',(-17.1049021947834,-70.4057447878624,
0.));
#71072=CARTESIAN_POINT('Ctrl Pts',(-17.1017269915292,-70.430408894101,0.));
#71073=CARTESIAN_POINT('Ctrl Pts',(-17.0985229718124,-70.4551100138238,
0.));
#71074=CARTESIAN_POINT('Ctrl Pts',(-17.0952900936048,-70.4798480314381,
0.));
#71075=CARTESIAN_POINT('Ctrl Pts',(-17.0920283151219,-70.5046228317677,
0.));
#71076=CARTESIAN_POINT('Ctrl Pts',(-17.088737594822,-70.5294343000513,0.));
#71077=CARTESIAN_POINT('Ctrl Pts',(-17.0854178914087,-70.5542823219331,
0.));
#71078=CARTESIAN_POINT('Ctrl Pts',(-17.082069163831,-70.5791667834582,0.));
#71079=CARTESIAN_POINT('Ctrl Pts',(-17.0786913712763,-70.6040875710749,
0.));
#71080=CARTESIAN_POINT('Ctrl Pts',(-17.0752844731678,-70.6290445716337,
0.));
#71081=CARTESIAN_POINT('Ctrl Pts',(-17.0718484291624,-70.6540376723841,
0.));
#71082=CARTESIAN_POINT('Ctrl Pts',(-17.0683831991532,-70.6790667609679,
0.));
#71083=CARTESIAN_POINT('Ctrl Pts',(-17.0648887432713,-70.7041317254125,
0.));
#71084=CARTESIAN_POINT('Ctrl Pts',(-17.0613650218787,-70.7292324541341,
0.));
#71085=CARTESIAN_POINT('Ctrl Pts',(-17.0578119955649,-70.7543688359374,
0.));
#71086=CARTESIAN_POINT('Ctrl Pts',(-17.0542296251462,-70.7795407600127,
0.));
#71087=CARTESIAN_POINT('Ctrl Pts',(-17.0506178716664,-70.8047481159306,
0.));
#71088=CARTESIAN_POINT('Ctrl Pts',(-17.0469766964005,-70.8299907936346,
0.));
#71089=CARTESIAN_POINT('Ctrl Pts',(-17.0433060608478,-70.8552686834435,
0.));
#71090=CARTESIAN_POINT('Ctrl Pts',(-17.0396059267279,-70.8805816760507,
0.));
#71091=CARTESIAN_POINT('Ctrl Pts',(-17.0358762559786,-70.9059296625214,
0.));
#71092=CARTESIAN_POINT('Ctrl Pts',(-17.0321170107562,-70.9313125342872,
0.));
#71093=CARTESIAN_POINT('Ctrl Pts',(-17.028328153439,-70.9567301831355,0.));
#71094=CARTESIAN_POINT('Ctrl Pts',(-17.0245096466228,-70.9821825012134,
0.));
#71095=CARTESIAN_POINT('Ctrl Pts',(-17.0206614531165,-71.0076693810303,
0.));
#71096=CARTESIAN_POINT('Ctrl Pts',(-17.0167835359419,-71.0331907154575,
0.));
#71097=CARTESIAN_POINT('Ctrl Pts',(-17.0128758583335,-71.0587463977266,
0.));
#71098=CARTESIAN_POINT('Ctrl Pts',(-17.0089383837436,-71.0843363214216,
0.));
#71099=CARTESIAN_POINT('Ctrl Pts',(-17.0049710758393,-71.1099603804779,
0.));
#71100=CARTESIAN_POINT('Ctrl Pts',(-17.0009738984935,-71.1356184691799,
0.));
#71101=CARTESIAN_POINT('Ctrl Pts',(-16.9969468157824,-71.1613104821565,
0.));
#71102=CARTESIAN_POINT('Ctrl Pts',(-16.9928897919829,-71.1870363143742,
0.));
#71103=CARTESIAN_POINT('Ctrl Pts',(-16.9888027915743,-71.2127958611248,
0.));
#71104=CARTESIAN_POINT('Ctrl Pts',(-16.9846857792385,-71.2385890180233,
0.));
#71105=CARTESIAN_POINT('Ctrl Pts',(-16.9805387198573,-71.2644156810209,
0.));
#71106=CARTESIAN_POINT('Ctrl Pts',(-16.9763615785137,-71.2902757464127,
0.));
#71107=CARTESIAN_POINT('Ctrl Pts',(-16.9721543204951,-71.3161691108425,
0.));
#71108=CARTESIAN_POINT('Ctrl Pts',(-16.9679169112993,-71.3420956713072,
0.));
#71109=CARTESIAN_POINT('Ctrl Pts',(-16.9636493166395,-71.3680553251548,
0.));
#71110=CARTESIAN_POINT('Ctrl Pts',(-16.9593515024274,-71.3940479700663,
0.));
#71111=CARTESIAN_POINT('Ctrl Pts',(-16.9550234347619,-71.4200735040374,
0.));
#71112=CARTESIAN_POINT('Ctrl Pts',(-16.9506650799188,-71.4461318253561,
0.));
#71113=CARTESIAN_POINT('Ctrl Pts',(-16.9462764043445,-71.4722228325805,
0.));
#71114=CARTESIAN_POINT('Ctrl Pts',(-16.9418573746492,-71.498346424507,0.));
#71115=CARTESIAN_POINT('Ctrl Pts',(-16.9374079576204,-71.5245025002154,
0.));
#71116=CARTESIAN_POINT('Ctrl Pts',(-16.9329281202379,-71.5506909591139,
0.));
#71117=CARTESIAN_POINT('Ctrl Pts',(-16.9284178296934,-71.5769117009844,
0.));
#71118=CARTESIAN_POINT('Ctrl Pts',(-16.923877053407,-71.6031646260169,0.));
#71119=CARTESIAN_POINT('Ctrl Pts',(-16.9193057590605,-71.6294496348644,
0.));
#71120=CARTESIAN_POINT('Ctrl Pts',(-16.9147039145715,-71.6557666285908,
0.));
#71121=CARTESIAN_POINT('Ctrl Pts',(-16.9100714880367,-71.6821155085605,
0.));
#71122=CARTESIAN_POINT('Ctrl Pts',(-16.9054084476847,-71.7084961763355,
0.));
#71123=CARTESIAN_POINT('Ctrl Pts',(-16.9007147618344,-71.7349085335796,
0.));
#71124=CARTESIAN_POINT('Ctrl Pts',(-16.895990398841,-71.761352481924,0.));
#71125=CARTESIAN_POINT('Ctrl Pts',(-16.8912353270944,-71.7878279229556,
0.));
#71126=CARTESIAN_POINT('Ctrl Pts',(-16.8864495151347,-71.8143347584977,
0.));
#71127=CARTESIAN_POINT('Ctrl Pts',(-16.8816329317473,-71.8408728908269,
0.));
#71128=CARTESIAN_POINT('Ctrl Pts',(-16.87678554607,-71.8674422229151,0.));
#71129=CARTESIAN_POINT('Ctrl Pts',(-16.8719073276967,-71.8940426586521,
0.));
#71130=CARTESIAN_POINT('Ctrl Pts',(-16.8669982467915,-71.920674103086,0.));
#71131=CARTESIAN_POINT('Ctrl Pts',(-16.862058273843,-71.9473364618889,0.));
#71132=CARTESIAN_POINT('Ctrl Pts',(-16.8570873794264,-71.9740296408319,
0.));
#71133=CARTESIAN_POINT('Ctrl Pts',(-16.8520855339444,-72.0007535452071,
0.));
#71134=CARTESIAN_POINT('Ctrl Pts',(-16.8470527074278,-72.0275080793742,
0.));
#71135=CARTESIAN_POINT('Ctrl Pts',(-16.8419888691984,-72.0542931459865,
0.));
#71136=CARTESIAN_POINT('Ctrl Pts',(-16.8368939881457,-72.0811086466177,
0.));
#71137=CARTESIAN_POINT('Ctrl Pts',(-16.8317680333415,-72.1079544831568,
0.));
#71138=CARTESIAN_POINT('Ctrl Pts',(-16.8266109745801,-72.1348305590233,
0.));
#71139=CARTESIAN_POINT('Ctrl Pts',(-16.8214227828941,-72.1617367803226,
0.));
#71140=CARTESIAN_POINT('Ctrl Pts',(-16.8162034312257,-72.1886730573389,
0.));
#71141=CARTESIAN_POINT('Ctrl Pts',(-16.8109528945876,-72.2156393048868,
0.));
#71142=CARTESIAN_POINT('Ctrl Pts',(-16.8064254147766,-72.2387802230663,
0.));
#71143=CARTESIAN_POINT('Ctrl Pts',(-16.8029374213802,-72.2565380035009,
0.));
#71144=CARTESIAN_POINT('Ctrl Pts',(-16.8005027425888,-72.2688994294961,
0.));
#71145=CARTESIAN_POINT('Ctrl Pts',(-16.7991305317792,-72.275855789097,0.));
#71146=CARTESIAN_POINT('Ctrl Pts',(-16.7988252568806,-72.2774028393486,
0.));
#71147=CARTESIAN_POINT('',(-17.2912529479484,-67.8307641965655,12.));
#71148=CARTESIAN_POINT('',(-17.2912529479484,-67.8307641965655,0.));
#71149=CARTESIAN_POINT('Ctrl Pts',(-16.7988252568806,-72.2774028393486,
12.));
#71150=CARTESIAN_POINT('Ctrl Pts',(-16.7991305317792,-72.275855789097,12.));
#71151=CARTESIAN_POINT('Ctrl Pts',(-16.8005027425888,-72.2688994294961,
12.));
#71152=CARTESIAN_POINT('Ctrl Pts',(-16.8029374213802,-72.2565380035009,
12.));
#71153=CARTESIAN_POINT('Ctrl Pts',(-16.8064254147766,-72.2387802230663,
12.));
#71154=CARTESIAN_POINT('Ctrl Pts',(-16.8109528945876,-72.2156393048868,
12.));
#71155=CARTESIAN_POINT('Ctrl Pts',(-16.8162034312257,-72.1886730573389,
12.));
#71156=CARTESIAN_POINT('Ctrl Pts',(-16.8214227828941,-72.1617367803226,
12.));
#71157=CARTESIAN_POINT('Ctrl Pts',(-16.8266109745801,-72.1348305590233,
12.));
#71158=CARTESIAN_POINT('Ctrl Pts',(-16.8317680333415,-72.1079544831568,
12.));
#71159=CARTESIAN_POINT('Ctrl Pts',(-16.8368939881457,-72.0811086466177,
12.));
#71160=CARTESIAN_POINT('Ctrl Pts',(-16.8419888691984,-72.0542931459865,
12.));
#71161=CARTESIAN_POINT('Ctrl Pts',(-16.8470527074278,-72.0275080793742,
12.));
#71162=CARTESIAN_POINT('Ctrl Pts',(-16.8520855339444,-72.0007535452071,
12.));
#71163=CARTESIAN_POINT('Ctrl Pts',(-16.8570873794264,-71.9740296408319,
12.));
#71164=CARTESIAN_POINT('Ctrl Pts',(-16.862058273843,-71.9473364618889,12.));
#71165=CARTESIAN_POINT('Ctrl Pts',(-16.8669982467915,-71.920674103086,12.));
#71166=CARTESIAN_POINT('Ctrl Pts',(-16.8719073276967,-71.8940426586521,
12.));
#71167=CARTESIAN_POINT('Ctrl Pts',(-16.87678554607,-71.8674422229151,12.));
#71168=CARTESIAN_POINT('Ctrl Pts',(-16.8816329317473,-71.8408728908269,
12.));
#71169=CARTESIAN_POINT('Ctrl Pts',(-16.8864495151347,-71.8143347584977,
12.));
#71170=CARTESIAN_POINT('Ctrl Pts',(-16.8912353270944,-71.7878279229556,
12.));
#71171=CARTESIAN_POINT('Ctrl Pts',(-16.895990398841,-71.761352481924,12.));
#71172=CARTESIAN_POINT('Ctrl Pts',(-16.9007147618344,-71.7349085335796,
12.));
#71173=CARTESIAN_POINT('Ctrl Pts',(-16.9054084476847,-71.7084961763355,
12.));
#71174=CARTESIAN_POINT('Ctrl Pts',(-16.9100714880367,-71.6821155085605,
12.));
#71175=CARTESIAN_POINT('Ctrl Pts',(-16.9147039145715,-71.6557666285908,
12.));
#71176=CARTESIAN_POINT('Ctrl Pts',(-16.9193057590605,-71.6294496348644,
12.));
#71177=CARTESIAN_POINT('Ctrl Pts',(-16.923877053407,-71.6031646260169,12.));
#71178=CARTESIAN_POINT('Ctrl Pts',(-16.9284178296934,-71.5769117009844,
12.));
#71179=CARTESIAN_POINT('Ctrl Pts',(-16.9329281202379,-71.5506909591139,
12.));
#71180=CARTESIAN_POINT('Ctrl Pts',(-16.9374079576204,-71.5245025002154,
12.));
#71181=CARTESIAN_POINT('Ctrl Pts',(-16.9418573746492,-71.498346424507,12.));
#71182=CARTESIAN_POINT('Ctrl Pts',(-16.9462764043445,-71.4722228325805,
12.));
#71183=CARTESIAN_POINT('Ctrl Pts',(-16.9506650799188,-71.4461318253561,
12.));
#71184=CARTESIAN_POINT('Ctrl Pts',(-16.9550234347619,-71.4200735040374,
12.));
#71185=CARTESIAN_POINT('Ctrl Pts',(-16.9593515024274,-71.3940479700663,
12.));
#71186=CARTESIAN_POINT('Ctrl Pts',(-16.9636493166395,-71.3680553251548,
12.));
#71187=CARTESIAN_POINT('Ctrl Pts',(-16.9679169112993,-71.3420956713072,
12.));
#71188=CARTESIAN_POINT('Ctrl Pts',(-16.9721543204951,-71.3161691108425,
12.));
#71189=CARTESIAN_POINT('Ctrl Pts',(-16.9763615785137,-71.2902757464127,
12.));
#71190=CARTESIAN_POINT('Ctrl Pts',(-16.9805387198573,-71.2644156810209,
12.));
#71191=CARTESIAN_POINT('Ctrl Pts',(-16.9846857792385,-71.2385890180233,
12.));
#71192=CARTESIAN_POINT('Ctrl Pts',(-16.9888027915743,-71.2127958611248,
12.));
#71193=CARTESIAN_POINT('Ctrl Pts',(-16.9928897919829,-71.1870363143742,
12.));
#71194=CARTESIAN_POINT('Ctrl Pts',(-16.9969468157824,-71.1613104821565,
12.));
#71195=CARTESIAN_POINT('Ctrl Pts',(-17.0009738984935,-71.1356184691799,
12.));
#71196=CARTESIAN_POINT('Ctrl Pts',(-17.0049710758393,-71.1099603804779,
12.));
#71197=CARTESIAN_POINT('Ctrl Pts',(-17.0089383837436,-71.0843363214216,
12.));
#71198=CARTESIAN_POINT('Ctrl Pts',(-17.0128758583335,-71.0587463977266,
12.));
#71199=CARTESIAN_POINT('Ctrl Pts',(-17.0167835359419,-71.0331907154575,
12.));
#71200=CARTESIAN_POINT('Ctrl Pts',(-17.0206614531165,-71.0076693810303,
12.));
#71201=CARTESIAN_POINT('Ctrl Pts',(-17.0245096466228,-70.9821825012134,
12.));
#71202=CARTESIAN_POINT('Ctrl Pts',(-17.028328153439,-70.9567301831355,12.));
#71203=CARTESIAN_POINT('Ctrl Pts',(-17.0321170107562,-70.9313125342872,
12.));
#71204=CARTESIAN_POINT('Ctrl Pts',(-17.0358762559786,-70.9059296625214,
12.));
#71205=CARTESIAN_POINT('Ctrl Pts',(-17.0396059267279,-70.8805816760507,
12.));
#71206=CARTESIAN_POINT('Ctrl Pts',(-17.0433060608478,-70.8552686834435,
12.));
#71207=CARTESIAN_POINT('Ctrl Pts',(-17.0469766964005,-70.8299907936346,
12.));
#71208=CARTESIAN_POINT('Ctrl Pts',(-17.0506178716664,-70.8047481159306,
12.));
#71209=CARTESIAN_POINT('Ctrl Pts',(-17.0542296251462,-70.7795407600127,
12.));
#71210=CARTESIAN_POINT('Ctrl Pts',(-17.0578119955649,-70.7543688359374,
12.));
#71211=CARTESIAN_POINT('Ctrl Pts',(-17.0613650218787,-70.7292324541341,
12.));
#71212=CARTESIAN_POINT('Ctrl Pts',(-17.0648887432713,-70.7041317254125,
12.));
#71213=CARTESIAN_POINT('Ctrl Pts',(-17.0683831991532,-70.6790667609679,
12.));
#71214=CARTESIAN_POINT('Ctrl Pts',(-17.0718484291624,-70.6540376723841,
12.));
#71215=CARTESIAN_POINT('Ctrl Pts',(-17.0752844731678,-70.6290445716337,
12.));
#71216=CARTESIAN_POINT('Ctrl Pts',(-17.0786913712763,-70.6040875710749,
12.));
#71217=CARTESIAN_POINT('Ctrl Pts',(-17.082069163831,-70.5791667834582,12.));
#71218=CARTESIAN_POINT('Ctrl Pts',(-17.0854178914087,-70.5542823219331,
12.));
#71219=CARTESIAN_POINT('Ctrl Pts',(-17.088737594822,-70.5294343000513,12.));
#71220=CARTESIAN_POINT('Ctrl Pts',(-17.0920283151219,-70.5046228317677,
12.));
#71221=CARTESIAN_POINT('Ctrl Pts',(-17.0952900936048,-70.4798480314381,
12.));
#71222=CARTESIAN_POINT('Ctrl Pts',(-17.0985229718124,-70.4551100138238,
12.));
#71223=CARTESIAN_POINT('Ctrl Pts',(-17.1017269915292,-70.430408894101,12.));
#71224=CARTESIAN_POINT('Ctrl Pts',(-17.1049021947834,-70.4057447878624,
12.));
#71225=CARTESIAN_POINT('Ctrl Pts',(-17.1080486238499,-70.3811178111201,
12.));
#71226=CARTESIAN_POINT('Ctrl Pts',(-17.1111663212568,-70.3565280803022,
12.));
#71227=CARTESIAN_POINT('Ctrl Pts',(-17.1142553297867,-70.3319757122568,
12.));
#71228=CARTESIAN_POINT('Ctrl Pts',(-17.1173156924733,-70.3074608242608,
12.));
#71229=CARTESIAN_POINT('Ctrl Pts',(-17.1203474526031,-70.2829835340238,
12.));
#71230=CARTESIAN_POINT('Ctrl Pts',(-17.1233506537176,-70.2585439596901,
12.));
#71231=CARTESIAN_POINT('Ctrl Pts',(-17.1263253396202,-70.2341422198363,
12.));
#71232=CARTESIAN_POINT('Ctrl Pts',(-17.1292715543778,-70.2097784334747,
12.));
#71233=CARTESIAN_POINT('Ctrl Pts',(-17.1321893423182,-70.1854527200631,
12.));
#71234=CARTESIAN_POINT('Ctrl Pts',(-17.1350787480312,-70.1611651995083,
12.));
#71235=CARTESIAN_POINT('Ctrl Pts',(-17.1379398163709,-70.1369159921687,
12.));
#71236=CARTESIAN_POINT('Ctrl Pts',(-17.1407725924617,-70.1127052188522,
12.));
#71237=CARTESIAN_POINT('Ctrl Pts',(-17.1435771217018,-70.0885330008179,
12.));
#71238=CARTESIAN_POINT('Ctrl Pts',(-17.1463534497594,-70.0643994597873,
12.));
#71239=CARTESIAN_POINT('Ctrl Pts',(-17.1491016225749,-70.0403047179483,
12.));
#71240=CARTESIAN_POINT('Ctrl Pts',(-17.1518216863623,-70.0162488979584,
12.));
#71241=CARTESIAN_POINT('Ctrl Pts',(-17.154513687616,-69.9922321229424,12.));
#71242=CARTESIAN_POINT('Ctrl Pts',(-17.1571776731139,-69.9682545164939,
12.));
#71243=CARTESIAN_POINT('Ctrl Pts',(-17.1598136899144,-69.9443162026865,
12.));
#71244=CARTESIAN_POINT('Ctrl Pts',(-17.1624217853578,-69.9204173060781,
12.));
#71245=CARTESIAN_POINT('Ctrl Pts',(-17.1650020070686,-69.8965579517147,
12.));
#71246=CARTESIAN_POINT('Ctrl Pts',(-17.167554402962,-69.8727382651286,12.));
#71247=CARTESIAN_POINT('Ctrl Pts',(-17.1700790212473,-69.8489583723407,
12.));
#71248=CARTESIAN_POINT('Ctrl Pts',(-17.1725759104251,-69.8252183998702,
12.));
#71249=CARTESIAN_POINT('Ctrl Pts',(-17.1750451192885,-69.8015184747398,
12.));
#71250=CARTESIAN_POINT('Ctrl Pts',(-17.1774866969256,-69.777858724479,12.));
#71251=CARTESIAN_POINT('Ctrl Pts',(-17.179900692726,-69.7542392771234,12.));
#71252=CARTESIAN_POINT('Ctrl Pts',(-17.1822871563842,-69.7306602612155,
12.));
#71253=CARTESIAN_POINT('Ctrl Pts',(-17.1846461378973,-69.7071218058178,
12.));
#71254=CARTESIAN_POINT('Ctrl Pts',(-17.1869776875666,-69.6836240405164,
12.));
#71255=CARTESIAN_POINT('Ctrl Pts',(-17.1892818560002,-69.6601670954269,
12.));
#71256=CARTESIAN_POINT('Ctrl Pts',(-17.1915586941192,-69.6367511011898,
12.));
#71257=CARTESIAN_POINT('Ctrl Pts',(-17.1938082531612,-69.6133761889748,
12.));
#71258=CARTESIAN_POINT('Ctrl Pts',(-17.196030584678,-69.5900424904921,12.));
#71259=CARTESIAN_POINT('Ctrl Pts',(-17.1982257405377,-69.5667501379969,
12.));
#71260=CARTESIAN_POINT('Ctrl Pts',(-17.2003937729268,-69.5434992642944,
12.));
#71261=CARTESIAN_POINT('Ctrl Pts',(-17.2025347343577,-69.5202900027367,
12.));
#71262=CARTESIAN_POINT('Ctrl Pts',(-17.2046486776708,-69.4971224872269,
12.));
#71263=CARTESIAN_POINT('Ctrl Pts',(-17.2067356560336,-69.4739968522313,
12.));
#71264=CARTESIAN_POINT('Ctrl Pts',(-17.2087957229423,-69.450913232785,12.));
#71265=CARTESIAN_POINT('Ctrl Pts',(-17.2108289322254,-69.4278717644973,
12.));
#71266=CARTESIAN_POINT('Ctrl Pts',(-17.2128353380502,-69.404872583548,12.));
#71267=CARTESIAN_POINT('Ctrl Pts',(-17.2148149949252,-69.3819158266916,
12.));
#71268=CARTESIAN_POINT('Ctrl Pts',(-17.2167679576984,-69.3590016312692,
12.));
#71269=CARTESIAN_POINT('Ctrl Pts',(-17.2186942815602,-69.3361301352141,
12.));
#71270=CARTESIAN_POINT('Ctrl Pts',(-17.2205940220459,-69.3133014770555,
12.));
#71271=CARTESIAN_POINT('Ctrl Pts',(-17.2224672350438,-69.2905157959166,
12.));
#71272=CARTESIAN_POINT('Ctrl Pts',(-17.224313976797,-69.2677732315224,12.));
#71273=CARTESIAN_POINT('Ctrl Pts',(-17.226134303902,-69.2450739242109,12.));
#71274=CARTESIAN_POINT('Ctrl Pts',(-17.227928273312,-69.222418014938,12.));
#71275=CARTESIAN_POINT('Ctrl Pts',(-17.2296959423407,-69.1998056452828,
12.));
#71276=CARTESIAN_POINT('Ctrl Pts',(-17.23143736867,-69.1772369574447,12.));
#71277=CARTESIAN_POINT('Ctrl Pts',(-17.2331526103506,-69.1547120942527,
12.));
#71278=CARTESIAN_POINT('Ctrl Pts',(-17.2348417258015,-69.1322311991752,
12.));
#71279=CARTESIAN_POINT('Ctrl Pts',(-17.2365047738125,-69.1097944163245,
12.));
#71280=CARTESIAN_POINT('Ctrl Pts',(-17.238141813549,-69.0874018904599,12.));
#71281=CARTESIAN_POINT('Ctrl Pts',(-17.2397529045589,-69.065053766986,12.));
#71282=CARTESIAN_POINT('Ctrl Pts',(-17.2413381067723,-69.0427501919636,
12.));
#71283=CARTESIAN_POINT('Ctrl Pts',(-17.2428974805044,-69.0204913121225,
12.));
#71284=CARTESIAN_POINT('Ctrl Pts',(-17.2444310864585,-68.9982772748694,
12.));
#71285=CARTESIAN_POINT('Ctrl Pts',(-17.2459389857327,-68.9761082282922,
12.));
#71286=CARTESIAN_POINT('Ctrl Pts',(-17.2474212398275,-68.9539843211619,
12.));
#71287=CARTESIAN_POINT('Ctrl Pts',(-17.248877910643,-68.9319057029409,12.));
#71288=CARTESIAN_POINT('Ctrl Pts',(-17.2503090604792,-68.909872523787,12.));
#71289=CARTESIAN_POINT('Ctrl Pts',(-17.2517147520376,-68.8878849345557,
12.));
#71290=CARTESIAN_POINT('Ctrl Pts',(-17.2530950484258,-68.8659430867972,
12.));
#71291=CARTESIAN_POINT('Ctrl Pts',(-17.2544500131624,-68.844047132755,12.));
#71292=CARTESIAN_POINT('Ctrl Pts',(-17.2557797101812,-68.8221972253941,
12.));
#71293=CARTESIAN_POINT('Ctrl Pts',(-17.2570842038383,-68.8003935184184,
12.));
#71294=CARTESIAN_POINT('Ctrl Pts',(-17.2583635589198,-68.7786361662882,
12.));
#71295=CARTESIAN_POINT('Ctrl Pts',(-17.259617840655,-68.7569253242333,12.));
#71296=CARTESIAN_POINT('Ctrl Pts',(-17.2608471147185,-68.7352611482547,
12.));
#71297=CARTESIAN_POINT('Ctrl Pts',(-17.2620514472182,-68.7136437951097,
12.));
#71298=CARTESIAN_POINT('Ctrl Pts',(-17.2632309046892,-68.6920734222938,
12.));
#71299=CARTESIAN_POINT('Ctrl Pts',(-17.2643855540892,-68.6705501880249,
12.));
#71300=CARTESIAN_POINT('Ctrl Pts',(-17.2655154627928,-68.6490742512057,
12.));
#71301=CARTESIAN_POINT('Ctrl Pts',(-17.2666206986084,-68.6276457714729,
12.));
#71302=CARTESIAN_POINT('Ctrl Pts',(-17.2677013298057,-68.6062649092764,
12.));
#71303=CARTESIAN_POINT('Ctrl Pts',(-17.2687574251428,-68.5849318259449,
12.));
#71304=CARTESIAN_POINT('Ctrl Pts',(-17.269789053896,-68.5636466837517,12.));
#71305=CARTESIAN_POINT('Ctrl Pts',(-17.2707962858919,-68.5424096459772,
12.));
#71306=CARTESIAN_POINT('Ctrl Pts',(-17.2717791914544,-68.521220876786,12.));
#71307=CARTESIAN_POINT('Ctrl Pts',(-17.2727378413489,-68.5000805410911,
12.));
#71308=CARTESIAN_POINT('Ctrl Pts',(-17.2736723067365,-68.4789888044351,
12.));
#71309=CARTESIAN_POINT('Ctrl Pts',(-17.2745826591119,-68.4579458328185,
12.));
#71310=CARTESIAN_POINT('Ctrl Pts',(-17.2754689702992,-68.436951792677,12.));
#71311=CARTESIAN_POINT('Ctrl Pts',(-17.2763313126018,-68.4160068512753,
12.));
#71312=CARTESIAN_POINT('Ctrl Pts',(-17.2771697589384,-68.3951111770487,
12.));
#71313=CARTESIAN_POINT('Ctrl Pts',(-17.2779843829608,-68.3742649398964,
12.));
#71314=CARTESIAN_POINT('Ctrl Pts',(-17.2787752592484,-68.3534683116515,
12.));
#71315=CARTESIAN_POINT('Ctrl Pts',(-17.2795424631799,-68.3327214657575,
12.));
#71316=CARTESIAN_POINT('Ctrl Pts',(-17.2802860705815,-68.3120245763914,
12.));
#71317=CARTESIAN_POINT('Ctrl Pts',(-17.2810061574353,-68.2913778177261,
12.));
#71318=CARTESIAN_POINT('Ctrl Pts',(-17.2817027995831,-68.2707813631731,
12.));
#71319=CARTESIAN_POINT('Ctrl Pts',(-17.2823760723874,-68.2502353845071,
12.));
#71320=CARTESIAN_POINT('Ctrl Pts',(-17.2830260513867,-68.2297400535294,
12.));
#71321=CARTESIAN_POINT('Ctrl Pts',(-17.2836528130819,-68.2092955440567,
12.));
#71322=CARTESIAN_POINT('Ctrl Pts',(-17.2842564355799,-68.1889020335427,
12.));
#71323=CARTESIAN_POINT('Ctrl Pts',(-17.2848369995293,-68.1685597054232,
12.));
#71324=CARTESIAN_POINT('Ctrl Pts',(-17.2853945882072,-68.1482687493226,
12.));
#71325=CARTESIAN_POINT('Ctrl Pts',(-17.2859292855705,-68.1280293561511,
12.));
#71326=CARTESIAN_POINT('Ctrl Pts',(-17.2864411745459,-68.1078417137877,
12.));
#71327=CARTESIAN_POINT('Ctrl Pts',(-17.2869303355432,-68.0877060033205,
12.));
#71328=CARTESIAN_POINT('Ctrl Pts',(-17.2873968440839,-68.0676223930412,
12.));
#71329=CARTESIAN_POINT('Ctrl Pts',(-17.2878407730961,-68.0475910442424,
12.));
#71330=CARTESIAN_POINT('Ctrl Pts',(-17.2882621974721,-68.0276121227356,
12.));
#71331=CARTESIAN_POINT('Ctrl Pts',(-17.28866119774,-68.007685808115,12.));
#71332=CARTESIAN_POINT('Ctrl Pts',(-17.2890378644866,-67.987812304921,12.));
#71333=CARTESIAN_POINT('Ctrl Pts',(-17.2893923013894,-67.9679918502579,
12.));
#71334=CARTESIAN_POINT('Ctrl Pts',(-17.2897246158941,-67.9482246901667,
12.));
#71335=CARTESIAN_POINT('Ctrl Pts',(-17.2900349103981,-67.9285110571741,
12.));
#71336=CARTESIAN_POINT('Ctrl Pts',(-17.2903232740694,-67.9088511496686,
12.));
#71337=CARTESIAN_POINT('Ctrl Pts',(-17.2905897723948,-67.8892451049608,
12.));
#71338=CARTESIAN_POINT('Ctrl Pts',(-17.2908344459694,-67.8696929978782,
12.));
#71339=CARTESIAN_POINT('Ctrl Pts',(-17.291012743109,-67.8540944889687,12.));
#71340=CARTESIAN_POINT('Ctrl Pts',(-17.2911366591347,-67.842419897098,12.));
#71341=CARTESIAN_POINT('Ctrl Pts',(-17.2912149114119,-67.8346476309018,
12.));
#71342=CARTESIAN_POINT('Ctrl Pts',(-17.2912529479484,-67.8307641965655,
12.));
#71343=CARTESIAN_POINT('Ctrl Pts',(-15.3208442077421,-72.6050633494713,
0.));
#71344=CARTESIAN_POINT('Ctrl Pts',(-15.3208442077421,-72.6050633494713,
4.));
#71345=CARTESIAN_POINT('Ctrl Pts',(-15.3208442077421,-72.6050633494713,
8.));
#71346=CARTESIAN_POINT('Ctrl Pts',(-15.3208442077421,-72.6050633494713,
12.));
#71347=CARTESIAN_POINT('Ctrl Pts',(-15.385683521042,-72.6937764817669,0.));
#71348=CARTESIAN_POINT('Ctrl Pts',(-15.385683521042,-72.6937764817669,4.));
#71349=CARTESIAN_POINT('Ctrl Pts',(-15.385683521042,-72.6937764817669,8.));
#71350=CARTESIAN_POINT('Ctrl Pts',(-15.385683521042,-72.6937764817669,12.));
#71351=CARTESIAN_POINT('Ctrl Pts',(-15.5519317750287,-72.809683430771,0.));
#71352=CARTESIAN_POINT('Ctrl Pts',(-15.5519317750287,-72.809683430771,4.00000000000001));
#71353=CARTESIAN_POINT('Ctrl Pts',(-15.5519317750287,-72.809683430771,7.99999999999999));
#71354=CARTESIAN_POINT('Ctrl Pts',(-15.5519317750287,-72.809683430771,12.));
#71355=CARTESIAN_POINT('Ctrl Pts',(-15.7502340068145,-72.8161171750016,
0.));
#71356=CARTESIAN_POINT('Ctrl Pts',(-15.7502340068145,-72.8161171750016,
4.));
#71357=CARTESIAN_POINT('Ctrl Pts',(-15.7502340068145,-72.8161171750016,
8.00000000000001));
#71358=CARTESIAN_POINT('Ctrl Pts',(-15.7502340068145,-72.8161171750016,
12.));
#71359=CARTESIAN_POINT('Ctrl Pts',(-15.8307637747231,-72.7986051948038,
0.));
#71360=CARTESIAN_POINT('Ctrl Pts',(-15.8307637747231,-72.7986051948038,
4.));
#71361=CARTESIAN_POINT('Ctrl Pts',(-15.8307637747231,-72.7986051948038,
8.));
#71362=CARTESIAN_POINT('Ctrl Pts',(-15.8307637747231,-72.7986051948038,
12.));
#71363=CARTESIAN_POINT('',(-15.3208442077421,-72.6050633494713,0.));
#71364=CARTESIAN_POINT('',(-15.8307637747231,-72.7986051948038,0.));
#71365=CARTESIAN_POINT('Ctrl Pts',(-15.3208442077421,-72.6050633494713,
2.77555756156289E-16));
#71366=CARTESIAN_POINT('Ctrl Pts',(-15.385683521042,-72.6937764817669,2.77555756156289E-16));
#71367=CARTESIAN_POINT('Ctrl Pts',(-15.4806825233201,-72.760009024055,2.77555756156289E-16));
#71368=CARTESIAN_POINT('Ctrl Pts',(-15.5861481305938,-72.7904952137639,
2.77555756156289E-16));
#71369=CARTESIAN_POINT('Ctrl Pts',(-15.6652473360491,-72.8133598560456,
2.77555756156289E-16));
#71370=CARTESIAN_POINT('Ctrl Pts',(-15.7502340068145,-72.8161171750016,
2.77555756156289E-16));
#71371=CARTESIAN_POINT('Ctrl Pts',(-15.8307637747231,-72.7986051948038,
2.77555756156289E-16));
#71372=CARTESIAN_POINT('',(-15.8307637747231,-72.7986051948038,12.));
#71373=CARTESIAN_POINT('Ctrl Pts',(-15.8307637747231,-72.7986051948038,
0.));
#71374=CARTESIAN_POINT('Ctrl Pts',(-15.8307637747231,-72.7986051948038,
4.));
#71375=CARTESIAN_POINT('Ctrl Pts',(-15.8307637747231,-72.7986051948038,
8.));
#71376=CARTESIAN_POINT('Ctrl Pts',(-15.8307637747231,-72.7986051948038,
12.));
#71377=CARTESIAN_POINT('',(-15.3208442077421,-72.6050633494713,12.));
#71378=CARTESIAN_POINT('Ctrl Pts',(-15.8307637747231,-72.7986051948038,
12.));
#71379=CARTESIAN_POINT('Ctrl Pts',(-15.7502340068145,-72.8161171750016,
12.));
#71380=CARTESIAN_POINT('Ctrl Pts',(-15.6652473360491,-72.8133598560456,
12.));
#71381=CARTESIAN_POINT('Ctrl Pts',(-15.5861481305938,-72.7904952137639,
12.));
#71382=CARTESIAN_POINT('Ctrl Pts',(-15.4806825233201,-72.760009024055,12.));
#71383=CARTESIAN_POINT('Ctrl Pts',(-15.385683521042,-72.6937764817669,12.));
#71384=CARTESIAN_POINT('Ctrl Pts',(-15.3208442077421,-72.6050633494713,
12.));
#71385=CARTESIAN_POINT('Ctrl Pts',(-15.3208442077421,-72.6050633494713,
12.));
#71386=CARTESIAN_POINT('Ctrl Pts',(-15.3208442077421,-72.6050633494713,
8.));
#71387=CARTESIAN_POINT('Ctrl Pts',(-15.3208442077421,-72.6050633494713,
4.));
#71388=CARTESIAN_POINT('Ctrl Pts',(-15.3208442077421,-72.6050633494713,
0.));
#71389=CARTESIAN_POINT('Origin',(-8.1034134051859E-11,-3.65979954444617E-10,
0.));
#71390=CARTESIAN_POINT('Origin',(-8.1034134051859E-11,-3.65979954444617E-10,
12.));
#71391=CARTESIAN_POINT('Origin',(-8.1034134051859E-11,-3.65979954444617E-10,
0.));
#71392=CARTESIAN_POINT('Ctrl Pts',(-22.6894590071785,-70.9608233461364,
0.));
#71393=CARTESIAN_POINT('Ctrl Pts',(-22.6894590071785,-70.9608233461364,
4.));
#71394=CARTESIAN_POINT('Ctrl Pts',(-22.6894590071785,-70.9608233461363,
8.));
#71395=CARTESIAN_POINT('Ctrl Pts',(-22.6894590071785,-70.9608233461363,
12.));
#71396=CARTESIAN_POINT('Ctrl Pts',(-22.7941214270114,-70.9273579271571,
0.));
#71397=CARTESIAN_POINT('Ctrl Pts',(-22.7941214270114,-70.9273579271571,
4.));
#71398=CARTESIAN_POINT('Ctrl Pts',(-22.7941214270114,-70.9273579271571,
8.00000000000001));
#71399=CARTESIAN_POINT('Ctrl Pts',(-22.7941214270114,-70.9273579271571,
12.));
#71400=CARTESIAN_POINT('Ctrl Pts',(-22.9566438338674,-70.8062825417802,
0.));
#71401=CARTESIAN_POINT('Ctrl Pts',(-22.9566438338674,-70.8062825417802,
4.));
#71402=CARTESIAN_POINT('Ctrl Pts',(-22.9566438338675,-70.8062825417802,
8.));
#71403=CARTESIAN_POINT('Ctrl Pts',(-22.9566438338675,-70.8062825417802,
12.));
#71404=CARTESIAN_POINT('Ctrl Pts',(-23.0254444386655,-70.6201870200063,
0.));
#71405=CARTESIAN_POINT('Ctrl Pts',(-23.0254444386655,-70.6201870200063,
4.));
#71406=CARTESIAN_POINT('Ctrl Pts',(-23.0254444386655,-70.6201870200063,
8.00000000000001));
#71407=CARTESIAN_POINT('Ctrl Pts',(-23.0254444386655,-70.6201870200063,
12.));
#71408=CARTESIAN_POINT('Ctrl Pts',(-23.0342913834093,-70.5382514078489,
0.));
#71409=CARTESIAN_POINT('Ctrl Pts',(-23.0342913834093,-70.5382514078489,
4.));
#71410=CARTESIAN_POINT('Ctrl Pts',(-23.0342913834093,-70.5382514078489,
8.));
#71411=CARTESIAN_POINT('Ctrl Pts',(-23.0342913834093,-70.5382514078489,
12.));
#71412=CARTESIAN_POINT('',(-22.6894590071785,-70.9608233461364,0.));
#71413=CARTESIAN_POINT('',(-23.0342913834093,-70.5382514078489,0.));
#71414=CARTESIAN_POINT('Ctrl Pts',(-22.6894590071785,-70.9608233461364,
1.38777878078145E-16));
#71415=CARTESIAN_POINT('Ctrl Pts',(-22.7941214270114,-70.9273579271571,
1.38777878078145E-16));
#71416=CARTESIAN_POINT('Ctrl Pts',(-22.8869913737863,-70.858171992656,1.38777878078145E-16));
#71417=CARTESIAN_POINT('Ctrl Pts',(-22.9492582831545,-70.767754993209,1.38777878078145E-16));
#71418=CARTESIAN_POINT('Ctrl Pts',(-22.9959584651806,-70.6999422436237,
1.38777878078145E-16));
#71419=CARTESIAN_POINT('Ctrl Pts',(-23.0254444386655,-70.6201870200063,
1.38777878078144E-16));
#71420=CARTESIAN_POINT('Ctrl Pts',(-23.0342913834093,-70.5382514078489,
1.38777878078145E-16));
#71421=CARTESIAN_POINT('',(-23.0342913834093,-70.5382514078489,12.));
#71422=CARTESIAN_POINT('Ctrl Pts',(-23.0342913834093,-70.5382514078489,
0.));
#71423=CARTESIAN_POINT('Ctrl Pts',(-23.0342913834093,-70.5382514078489,
4.));
#71424=CARTESIAN_POINT('Ctrl Pts',(-23.0342913834093,-70.5382514078489,
8.));
#71425=CARTESIAN_POINT('Ctrl Pts',(-23.0342913834093,-70.5382514078489,
12.));
#71426=CARTESIAN_POINT('',(-22.6894590071785,-70.9608233461363,12.));
#71427=CARTESIAN_POINT('Ctrl Pts',(-23.0342913834093,-70.5382514078489,
12.));
#71428=CARTESIAN_POINT('Ctrl Pts',(-23.0254444386655,-70.6201870200063,
12.));
#71429=CARTESIAN_POINT('Ctrl Pts',(-22.9959584651806,-70.6999422436237,
12.));
#71430=CARTESIAN_POINT('Ctrl Pts',(-22.9492582831545,-70.767754993209,12.));
#71431=CARTESIAN_POINT('Ctrl Pts',(-22.8869913737863,-70.858171992656,12.));
#71432=CARTESIAN_POINT('Ctrl Pts',(-22.7941214270114,-70.9273579271571,
12.));
#71433=CARTESIAN_POINT('Ctrl Pts',(-22.6894590071785,-70.9608233461363,
12.));
#71434=CARTESIAN_POINT('Ctrl Pts',(-22.6894590071785,-70.9608233461363,
12.));
#71435=CARTESIAN_POINT('Ctrl Pts',(-22.6894590071785,-70.9608233461363,
8.));
#71436=CARTESIAN_POINT('Ctrl Pts',(-22.6894590071785,-70.9608233461364,
4.));
#71437=CARTESIAN_POINT('Ctrl Pts',(-22.6894590071785,-70.9608233461364,
0.));
#71438=CARTESIAN_POINT('Ctrl Pts',(-23.1372951448024,-66.0656156664138,
0.));
#71439=CARTESIAN_POINT('Ctrl Pts',(-23.1372951448024,-66.0656156664138,
12.));
#71440=CARTESIAN_POINT('Ctrl Pts',(-23.1375957166104,-66.0694876382127,
0.));
#71441=CARTESIAN_POINT('Ctrl Pts',(-23.1375957166104,-66.0694876382127,
12.));
#71442=CARTESIAN_POINT('Ctrl Pts',(-23.13819515974,-66.0772371487248,0.));
#71443=CARTESIAN_POINT('Ctrl Pts',(-23.13819515974,-66.0772371487248,12.));
#71444=CARTESIAN_POINT('Ctrl Pts',(-23.1390892229779,-66.088878115242,0.));
#71445=CARTESIAN_POINT('Ctrl Pts',(-23.1390892229779,-66.088878115242,12.));
#71446=CARTESIAN_POINT('Ctrl Pts',(-23.1402711039425,-66.1044328067355,
0.));
#71447=CARTESIAN_POINT('Ctrl Pts',(-23.1402711039425,-66.1044328067355,
12.));
#71448=CARTESIAN_POINT('Ctrl Pts',(-23.1417314398398,-66.1239318368548,
0.));
#71449=CARTESIAN_POINT('Ctrl Pts',(-23.1417314398398,-66.1239318368548,
12.));
#71450=CARTESIAN_POINT('Ctrl Pts',(-23.1431747350098,-66.1434865015027,
0.));
#71451=CARTESIAN_POINT('Ctrl Pts',(-23.1431747350098,-66.1434865015027,
12.));
#71452=CARTESIAN_POINT('Ctrl Pts',(-23.1446009424903,-66.1630967296747,
0.));
#71453=CARTESIAN_POINT('Ctrl Pts',(-23.1446009424903,-66.1630967296747,
12.));
#71454=CARTESIAN_POINT('Ctrl Pts',(-23.1460099850763,-66.18276239029,0.));
#71455=CARTESIAN_POINT('Ctrl Pts',(-23.1460099850763,-66.18276239029,12.));
#71456=CARTESIAN_POINT('Ctrl Pts',(-23.1474017566484,-66.2024832934866,
0.));
#71457=CARTESIAN_POINT('Ctrl Pts',(-23.1474017566484,-66.2024832934866,
12.));
#71458=CARTESIAN_POINT('Ctrl Pts',(-23.1487761349328,-66.2222592165473,
0.));
#71459=CARTESIAN_POINT('Ctrl Pts',(-23.1487761349328,-66.2222592165473,
12.));
#71460=CARTESIAN_POINT('Ctrl Pts',(-23.1501329914488,-66.2420899237317,
0.));
#71461=CARTESIAN_POINT('Ctrl Pts',(-23.1501329914488,-66.2420899237317,
12.));
#71462=CARTESIAN_POINT('Ctrl Pts',(-23.1514722022483,-66.2619751878741,
0.));
#71463=CARTESIAN_POINT('Ctrl Pts',(-23.1514722022483,-66.2619751878741,
12.));
#71464=CARTESIAN_POINT('Ctrl Pts',(-23.1527936592625,-66.2819148131072,
0.));
#71465=CARTESIAN_POINT('Ctrl Pts',(-23.1527936592625,-66.2819148131072,
12.));
#71466=CARTESIAN_POINT('Ctrl Pts',(-23.154097266617,-66.301908627539,0.));
#71467=CARTESIAN_POINT('Ctrl Pts',(-23.154097266617,-66.301908627539,12.));
#71468=CARTESIAN_POINT('Ctrl Pts',(-23.1553829352531,-66.3219564725161,
0.));
#71469=CARTESIAN_POINT('Ctrl Pts',(-23.1553829352531,-66.3219564725161,
12.));
#71470=CARTESIAN_POINT('Ctrl Pts',(-23.1566505784626,-66.3420581937159,
0.));
#71471=CARTESIAN_POINT('Ctrl Pts',(-23.1566505784626,-66.3420581937159,
12.));
#71472=CARTESIAN_POINT('Ctrl Pts',(-23.1579001063438,-66.3622136300692,
0.));
#71473=CARTESIAN_POINT('Ctrl Pts',(-23.1579001063438,-66.3622136300692,
12.));
#71474=CARTESIAN_POINT('Ctrl Pts',(-23.1591314230101,-66.382422608185,0.));
#71475=CARTESIAN_POINT('Ctrl Pts',(-23.1591314230101,-66.382422608185,12.));
#71476=CARTESIAN_POINT('Ctrl Pts',(-23.1603444294754,-66.402684948127,0.));
#71477=CARTESIAN_POINT('Ctrl Pts',(-23.1603444294754,-66.402684948127,12.));
#71478=CARTESIAN_POINT('Ctrl Pts',(-23.1615390254635,-66.4230004670288,
0.));
#71479=CARTESIAN_POINT('Ctrl Pts',(-23.1615390254635,-66.4230004670288,
12.));
#71480=CARTESIAN_POINT('Ctrl Pts',(-23.1627151114875,-66.4433689832454,
0.));
#71481=CARTESIAN_POINT('Ctrl Pts',(-23.1627151114875,-66.4433689832454,
12.));
#71482=CARTESIAN_POINT('Ctrl Pts',(-23.163872591218,-66.4637903210682,0.));
#71483=CARTESIAN_POINT('Ctrl Pts',(-23.163872591218,-66.4637903210682,12.));
#71484=CARTESIAN_POINT('Ctrl Pts',(-23.1650113713792,-66.4842643105263,
0.));
#71485=CARTESIAN_POINT('Ctrl Pts',(-23.1650113713792,-66.4842643105263,
12.));
#71486=CARTESIAN_POINT('Ctrl Pts',(-23.1661313606123,-66.5047907851319,
0.));
#71487=CARTESIAN_POINT('Ctrl Pts',(-23.1661313606123,-66.5047907851319,
12.));
#71488=CARTESIAN_POINT('Ctrl Pts',(-23.1672324686928,-66.5253695803209,
0.));
#71489=CARTESIAN_POINT('Ctrl Pts',(-23.1672324686928,-66.5253695803209,
12.));
#71490=CARTESIAN_POINT('Ctrl Pts',(-23.1683146055736,-66.5460005315406,
0.));
#71491=CARTESIAN_POINT('Ctrl Pts',(-23.1683146055736,-66.5460005315406,
12.));
#71492=CARTESIAN_POINT('Ctrl Pts',(-23.169377680588,-66.5666834726494,0.));
#71493=CARTESIAN_POINT('Ctrl Pts',(-23.169377680588,-66.5666834726494,12.));
#71494=CARTESIAN_POINT('Ctrl Pts',(-23.1704216028626,-66.5874182367596,
0.));
#71495=CARTESIAN_POINT('Ctrl Pts',(-23.1704216028626,-66.5874182367596,
12.));
#71496=CARTESIAN_POINT('Ctrl Pts',(-23.1714462816794,-66.6082046569657,
0.));
#71497=CARTESIAN_POINT('Ctrl Pts',(-23.1714462816794,-66.6082046569657,
12.));
#71498=CARTESIAN_POINT('Ctrl Pts',(-23.1724516268299,-66.6290425670538,
0.));
#71499=CARTESIAN_POINT('Ctrl Pts',(-23.1724516268299,-66.6290425670538,
12.));
#71500=CARTESIAN_POINT('Ctrl Pts',(-23.1734375490421,-66.6499318023445,
0.));
#71501=CARTESIAN_POINT('Ctrl Pts',(-23.1734375490421,-66.6499318023445,
12.));
#71502=CARTESIAN_POINT('Ctrl Pts',(-23.174403960137,-66.6708722000046,0.));
#71503=CARTESIAN_POINT('Ctrl Pts',(-23.174403960137,-66.6708722000046,12.));
#71504=CARTESIAN_POINT('Ctrl Pts',(-23.1753507727932,-66.691863598595,0.));
#71505=CARTESIAN_POINT('Ctrl Pts',(-23.1753507727932,-66.691863598595,12.));
#71506=CARTESIAN_POINT('Ctrl Pts',(-23.1762779004043,-66.712905837789,0.));
#71507=CARTESIAN_POINT('Ctrl Pts',(-23.1762779004043,-66.712905837789,12.));
#71508=CARTESIAN_POINT('Ctrl Pts',(-23.1771852569137,-66.7339987580441,
0.));
#71509=CARTESIAN_POINT('Ctrl Pts',(-23.1771852569137,-66.7339987580441,
12.));
#71510=CARTESIAN_POINT('Ctrl Pts',(-23.1780727566309,-66.7551422002229,
0.));
#71511=CARTESIAN_POINT('Ctrl Pts',(-23.1780727566309,-66.7551422002229,
12.));
#71512=CARTESIAN_POINT('Ctrl Pts',(-23.1789403142376,-66.7763360056146,
0.));
#71513=CARTESIAN_POINT('Ctrl Pts',(-23.1789403142376,-66.7763360056146,
12.));
#71514=CARTESIAN_POINT('Ctrl Pts',(-23.1797878448645,-66.7975800161014,
0.));
#71515=CARTESIAN_POINT('Ctrl Pts',(-23.1797878448645,-66.7975800161014,
12.));
#71516=CARTESIAN_POINT('Ctrl Pts',(-23.1806152641475,-66.8188740742727,
0.));
#71517=CARTESIAN_POINT('Ctrl Pts',(-23.1806152641475,-66.8188740742727,
12.));
#71518=CARTESIAN_POINT('Ctrl Pts',(-23.1814224882948,-66.8402180235549,
0.));
#71519=CARTESIAN_POINT('Ctrl Pts',(-23.1814224882948,-66.8402180235549,
12.));
#71520=CARTESIAN_POINT('Ctrl Pts',(-23.1822094341508,-66.8616117083304,
0.));
#71521=CARTESIAN_POINT('Ctrl Pts',(-23.1822094341508,-66.8616117083304,
12.));
#71522=CARTESIAN_POINT('Ctrl Pts',(-23.1829760191583,-66.8830549738768,
0.));
#71523=CARTESIAN_POINT('Ctrl Pts',(-23.1829760191583,-66.8830549738768,
12.));
#71524=CARTESIAN_POINT('Ctrl Pts',(-23.1837221613231,-66.904547666305,0.));
#71525=CARTESIAN_POINT('Ctrl Pts',(-23.1837221613231,-66.904547666305,12.));
#71526=CARTESIAN_POINT('Ctrl Pts',(-23.1844477791816,-66.9260896324955,
0.));
#71527=CARTESIAN_POINT('Ctrl Pts',(-23.1844477791816,-66.9260896324955,
12.));
#71528=CARTESIAN_POINT('Ctrl Pts',(-23.1851527917666,-66.9476807200225,
0.));
#71529=CARTESIAN_POINT('Ctrl Pts',(-23.1851527917666,-66.9476807200225,
12.));
#71530=CARTESIAN_POINT('Ctrl Pts',(-23.1858371185852,-66.9693207771058,
0.));
#71531=CARTESIAN_POINT('Ctrl Pts',(-23.1858371185852,-66.9693207771058,
12.));
#71532=CARTESIAN_POINT('Ctrl Pts',(-23.1865006796291,-66.9910096526483,
0.));
#71533=CARTESIAN_POINT('Ctrl Pts',(-23.1865006796291,-66.9910096526483,
12.));
#71534=CARTESIAN_POINT('Ctrl Pts',(-23.1871433953795,-67.0127471962507,
0.));
#71535=CARTESIAN_POINT('Ctrl Pts',(-23.1871433953795,-67.0127471962507,
12.));
#71536=CARTESIAN_POINT('Ctrl Pts',(-23.1877651868155,-67.0345332582297,
0.));
#71537=CARTESIAN_POINT('Ctrl Pts',(-23.1877651868155,-67.0345332582297,
12.));
#71538=CARTESIAN_POINT('Ctrl Pts',(-23.1883659754268,-67.0563676896312,
0.));
#71539=CARTESIAN_POINT('Ctrl Pts',(-23.1883659754268,-67.0563676896312,
12.));
#71540=CARTESIAN_POINT('Ctrl Pts',(-23.1889456832116,-67.0782503422293,
0.));
#71541=CARTESIAN_POINT('Ctrl Pts',(-23.1889456832116,-67.0782503422293,
12.));
#71542=CARTESIAN_POINT('Ctrl Pts',(-23.1895042326626,-67.1001810685138,
0.));
#71543=CARTESIAN_POINT('Ctrl Pts',(-23.1895042326626,-67.1001810685138,
12.));
#71544=CARTESIAN_POINT('Ctrl Pts',(-23.1900415467575,-67.122159721674,0.));
#71545=CARTESIAN_POINT('Ctrl Pts',(-23.1900415467575,-67.122159721674,12.));
#71546=CARTESIAN_POINT('Ctrl Pts',(-23.1905575489506,-67.1441861555819,
0.));
#71547=CARTESIAN_POINT('Ctrl Pts',(-23.1905575489506,-67.1441861555819,
12.));
#71548=CARTESIAN_POINT('Ctrl Pts',(-23.1910521631658,-67.1662602247641,
0.));
#71549=CARTESIAN_POINT('Ctrl Pts',(-23.1910521631658,-67.1662602247641,
12.));
#71550=CARTESIAN_POINT('Ctrl Pts',(-23.1915253137924,-67.1883817844039,
0.));
#71551=CARTESIAN_POINT('Ctrl Pts',(-23.1915253137924,-67.1883817844039,
12.));
#71552=CARTESIAN_POINT('Ctrl Pts',(-23.1919769256803,-67.2105506903448,
0.));
#71553=CARTESIAN_POINT('Ctrl Pts',(-23.1919769256803,-67.2105506903448,
12.));
#71554=CARTESIAN_POINT('Ctrl Pts',(-23.1924069241386,-67.232766799088,0.));
#71555=CARTESIAN_POINT('Ctrl Pts',(-23.1924069241386,-67.232766799088,12.));
#71556=CARTESIAN_POINT('Ctrl Pts',(-23.1928152349344,-67.2550299677888,
0.));
#71557=CARTESIAN_POINT('Ctrl Pts',(-23.1928152349344,-67.2550299677888,
12.));
#71558=CARTESIAN_POINT('Ctrl Pts',(-23.1932017842954,-67.2773400542477,
0.));
#71559=CARTESIAN_POINT('Ctrl Pts',(-23.1932017842954,-67.2773400542477,
12.));
#71560=CARTESIAN_POINT('Ctrl Pts',(-23.193566498902,-67.2996969169099,0.));
#71561=CARTESIAN_POINT('Ctrl Pts',(-23.193566498902,-67.2996969169099,12.));
#71562=CARTESIAN_POINT('Ctrl Pts',(-23.1939093058802,-67.3221004148604,
0.));
#71563=CARTESIAN_POINT('Ctrl Pts',(-23.1939093058802,-67.3221004148604,
12.));
#71564=CARTESIAN_POINT('Ctrl Pts',(-23.1942301327979,-67.3445504078178,
0.));
#71565=CARTESIAN_POINT('Ctrl Pts',(-23.1942301327979,-67.3445504078178,
12.));
#71566=CARTESIAN_POINT('Ctrl Pts',(-23.1945289076608,-67.3670467561205,
0.));
#71567=CARTESIAN_POINT('Ctrl Pts',(-23.1945289076608,-67.3670467561205,
12.));
#71568=CARTESIAN_POINT('Ctrl Pts',(-23.1948055589123,-67.3895893207168,
0.));
#71569=CARTESIAN_POINT('Ctrl Pts',(-23.1948055589123,-67.3895893207168,
12.));
#71570=CARTESIAN_POINT('Ctrl Pts',(-23.195060015426,-67.4121779631666,0.));
#71571=CARTESIAN_POINT('Ctrl Pts',(-23.195060015426,-67.4121779631666,12.));
#71572=CARTESIAN_POINT('Ctrl Pts',(-23.1952922065009,-67.4348125456389,
0.));
#71573=CARTESIAN_POINT('Ctrl Pts',(-23.1952922065009,-67.4348125456389,
12.));
#71574=CARTESIAN_POINT('Ctrl Pts',(-23.1955020618591,-67.4574929309078,
0.));
#71575=CARTESIAN_POINT('Ctrl Pts',(-23.1955020618591,-67.4574929309078,
12.));
#71576=CARTESIAN_POINT('Ctrl Pts',(-23.1956895116446,-67.4802189823423,
0.));
#71577=CARTESIAN_POINT('Ctrl Pts',(-23.1956895116446,-67.4802189823423,
12.));
#71578=CARTESIAN_POINT('Ctrl Pts',(-23.1958544864224,-67.5029905638973,
0.));
#71579=CARTESIAN_POINT('Ctrl Pts',(-23.1958544864224,-67.5029905638973,
12.));
#71580=CARTESIAN_POINT('Ctrl Pts',(-23.195996917171,-67.525807540117,0.));
#71581=CARTESIAN_POINT('Ctrl Pts',(-23.195996917171,-67.525807540117,12.));
#71582=CARTESIAN_POINT('Ctrl Pts',(-23.1961167352777,-67.5486697761301,
0.));
#71583=CARTESIAN_POINT('Ctrl Pts',(-23.1961167352777,-67.5486697761301,
12.));
#71584=CARTESIAN_POINT('Ctrl Pts',(-23.1962138725358,-67.5715771376454,
0.));
#71585=CARTESIAN_POINT('Ctrl Pts',(-23.1962138725358,-67.5715771376454,
12.));
#71586=CARTESIAN_POINT('Ctrl Pts',(-23.1962882611444,-67.5945294909398,
0.));
#71587=CARTESIAN_POINT('Ctrl Pts',(-23.1962882611444,-67.5945294909398,
12.));
#71588=CARTESIAN_POINT('Ctrl Pts',(-23.1963398337056,-67.6175267028516,
0.));
#71589=CARTESIAN_POINT('Ctrl Pts',(-23.1963398337056,-67.6175267028516,
12.));
#71590=CARTESIAN_POINT('Ctrl Pts',(-23.1963685232176,-67.6405686407828,
0.));
#71591=CARTESIAN_POINT('Ctrl Pts',(-23.1963685232176,-67.6405686407828,
12.));
#71592=CARTESIAN_POINT('Ctrl Pts',(-23.196374263071,-67.6636551726948,0.));
#71593=CARTESIAN_POINT('Ctrl Pts',(-23.196374263071,-67.6636551726948,12.));
#71594=CARTESIAN_POINT('Ctrl Pts',(-23.1963569870457,-67.6867861671044,
0.));
#71595=CARTESIAN_POINT('Ctrl Pts',(-23.1963569870457,-67.6867861671044,
12.));
#71596=CARTESIAN_POINT('Ctrl Pts',(-23.1963166293116,-67.7099614930712,
0.));
#71597=CARTESIAN_POINT('Ctrl Pts',(-23.1963166293116,-67.7099614930712,
12.));
#71598=CARTESIAN_POINT('Ctrl Pts',(-23.1962531244261,-67.7331810201931,
0.));
#71599=CARTESIAN_POINT('Ctrl Pts',(-23.1962531244261,-67.7331810201931,
12.));
#71600=CARTESIAN_POINT('Ctrl Pts',(-23.1961664073274,-67.7564446186115,
0.));
#71601=CARTESIAN_POINT('Ctrl Pts',(-23.1961664073274,-67.7564446186115,
12.));
#71602=CARTESIAN_POINT('Ctrl Pts',(-23.1960564133308,-67.7797521590056,
0.));
#71603=CARTESIAN_POINT('Ctrl Pts',(-23.1960564133308,-67.7797521590056,
12.));
#71604=CARTESIAN_POINT('Ctrl Pts',(-23.1959230781265,-67.8031035125873,
0.));
#71605=CARTESIAN_POINT('Ctrl Pts',(-23.1959230781265,-67.8031035125873,
12.));
#71606=CARTESIAN_POINT('Ctrl Pts',(-23.1957663377798,-67.8264985510884,
0.));
#71607=CARTESIAN_POINT('Ctrl Pts',(-23.1957663377798,-67.8264985510884,
12.));
#71608=CARTESIAN_POINT('Ctrl Pts',(-23.1955861287276,-67.8499371467578,
0.));
#71609=CARTESIAN_POINT('Ctrl Pts',(-23.1955861287276,-67.8499371467578,
12.));
#71610=CARTESIAN_POINT('Ctrl Pts',(-23.1953823877727,-67.8734191723639,
0.));
#71611=CARTESIAN_POINT('Ctrl Pts',(-23.1953823877727,-67.8734191723639,
12.));
#71612=CARTESIAN_POINT('Ctrl Pts',(-23.19515505208,-67.8969445011908,0.));
#71613=CARTESIAN_POINT('Ctrl Pts',(-23.19515505208,-67.8969445011908,12.));
#71614=CARTESIAN_POINT('Ctrl Pts',(-23.1949040591748,-67.9205130070337,
0.));
#71615=CARTESIAN_POINT('Ctrl Pts',(-23.1949040591748,-67.9205130070337,
12.));
#71616=CARTESIAN_POINT('Ctrl Pts',(-23.1946293469437,-67.944124564187,0.));
#71617=CARTESIAN_POINT('Ctrl Pts',(-23.1946293469437,-67.944124564187,12.));
#71618=CARTESIAN_POINT('Ctrl Pts',(-23.1943308536307,-67.9677790474414,
0.));
#71619=CARTESIAN_POINT('Ctrl Pts',(-23.1943308536307,-67.9677790474414,
12.));
#71620=CARTESIAN_POINT('Ctrl Pts',(-23.194008517832,-67.9914763320878,0.));
#71621=CARTESIAN_POINT('Ctrl Pts',(-23.194008517832,-67.9914763320878,12.));
#71622=CARTESIAN_POINT('Ctrl Pts',(-23.193662278492,-68.0152162939123,0.));
#71623=CARTESIAN_POINT('Ctrl Pts',(-23.193662278492,-68.0152162939123,12.));
#71624=CARTESIAN_POINT('Ctrl Pts',(-23.1932920749021,-68.0389988091926,
0.));
#71625=CARTESIAN_POINT('Ctrl Pts',(-23.1932920749021,-68.0389988091926,
12.));
#71626=CARTESIAN_POINT('Ctrl Pts',(-23.1928978467018,-68.0628237546852,
0.));
#71627=CARTESIAN_POINT('Ctrl Pts',(-23.1928978467018,-68.0628237546852,
12.));
#71628=CARTESIAN_POINT('Ctrl Pts',(-23.1924795338746,-68.086691007624,0.));
#71629=CARTESIAN_POINT('Ctrl Pts',(-23.1924795338746,-68.086691007624,12.));
#71630=CARTESIAN_POINT('Ctrl Pts',(-23.1920370767424,-68.1106004457223,
0.));
#71631=CARTESIAN_POINT('Ctrl Pts',(-23.1920370767424,-68.1106004457223,
12.));
#71632=CARTESIAN_POINT('Ctrl Pts',(-23.1915704159624,-68.1345519471695,
0.));
#71633=CARTESIAN_POINT('Ctrl Pts',(-23.1915704159624,-68.1345519471695,
12.));
#71634=CARTESIAN_POINT('Ctrl Pts',(-23.1910794925252,-68.1585453906259,
0.));
#71635=CARTESIAN_POINT('Ctrl Pts',(-23.1910794925252,-68.1585453906259,
12.));
#71636=CARTESIAN_POINT('Ctrl Pts',(-23.1905642477572,-68.182580655213,0.));
#71637=CARTESIAN_POINT('Ctrl Pts',(-23.1905642477572,-68.182580655213,12.));
#71638=CARTESIAN_POINT('Ctrl Pts',(-23.1900246233165,-68.2066576205113,
0.));
#71639=CARTESIAN_POINT('Ctrl Pts',(-23.1900246233165,-68.2066576205113,
12.));
#71640=CARTESIAN_POINT('Ctrl Pts',(-23.189460561187,-68.2307761665629,0.));
#71641=CARTESIAN_POINT('Ctrl Pts',(-23.189460561187,-68.2307761665629,12.));
#71642=CARTESIAN_POINT('Ctrl Pts',(-23.1888720036757,-68.2549361738679,
0.));
#71643=CARTESIAN_POINT('Ctrl Pts',(-23.1888720036757,-68.2549361738679,
12.));
#71644=CARTESIAN_POINT('Ctrl Pts',(-23.1882588934108,-68.2791375233798,
0.));
#71645=CARTESIAN_POINT('Ctrl Pts',(-23.1882588934108,-68.2791375233798,
12.));
#71646=CARTESIAN_POINT('Ctrl Pts',(-23.1876211733439,-68.3033800964946,
0.));
#71647=CARTESIAN_POINT('Ctrl Pts',(-23.1876211733439,-68.3033800964946,
12.));
#71648=CARTESIAN_POINT('Ctrl Pts',(-23.1869587867463,-68.3276637750494,
0.));
#71649=CARTESIAN_POINT('Ctrl Pts',(-23.1869587867463,-68.3276637750494,
12.));
#71650=CARTESIAN_POINT('Ctrl Pts',(-23.1862716772034,-68.3519884413253,
0.));
#71651=CARTESIAN_POINT('Ctrl Pts',(-23.1862716772034,-68.3519884413253,
12.));
#71652=CARTESIAN_POINT('Ctrl Pts',(-23.1855597886117,-68.3763539780442,
0.));
#71653=CARTESIAN_POINT('Ctrl Pts',(-23.1855597886117,-68.3763539780442,
12.));
#71654=CARTESIAN_POINT('Ctrl Pts',(-23.1848230651776,-68.4007602683649,
0.));
#71655=CARTESIAN_POINT('Ctrl Pts',(-23.1848230651776,-68.4007602683649,
12.));
#71656=CARTESIAN_POINT('Ctrl Pts',(-23.1840614514191,-68.4252071958725,
0.));
#71657=CARTESIAN_POINT('Ctrl Pts',(-23.1840614514191,-68.4252071958725,
12.));
#71658=CARTESIAN_POINT('Ctrl Pts',(-23.1832748921629,-68.4496946445756,
0.));
#71659=CARTESIAN_POINT('Ctrl Pts',(-23.1832748921629,-68.4496946445756,
12.));
#71660=CARTESIAN_POINT('Ctrl Pts',(-23.1824633325385,-68.4742224989099,
0.));
#71661=CARTESIAN_POINT('Ctrl Pts',(-23.1824633325385,-68.4742224989099,
12.));
#71662=CARTESIAN_POINT('Ctrl Pts',(-23.1816267179752,-68.4987906437357,
0.));
#71663=CARTESIAN_POINT('Ctrl Pts',(-23.1816267179752,-68.4987906437357,
12.));
#71664=CARTESIAN_POINT('Ctrl Pts',(-23.1807649942011,-68.5233989643344,
0.));
#71665=CARTESIAN_POINT('Ctrl Pts',(-23.1807649942011,-68.5233989643344,
12.));
#71666=CARTESIAN_POINT('Ctrl Pts',(-23.1798781072449,-68.548047346398,0.));
#71667=CARTESIAN_POINT('Ctrl Pts',(-23.1798781072449,-68.548047346398,12.));
#71668=CARTESIAN_POINT('Ctrl Pts',(-23.178966003434,-68.572735676027,0.));
#71669=CARTESIAN_POINT('Ctrl Pts',(-23.178966003434,-68.572735676027,12.));
#71670=CARTESIAN_POINT('Ctrl Pts',(-23.1780286293873,-68.5974638397322,
0.));
#71671=CARTESIAN_POINT('Ctrl Pts',(-23.1780286293873,-68.5974638397322,
12.));
#71672=CARTESIAN_POINT('Ctrl Pts',(-23.1770659320137,-68.6222317244336,
0.));
#71673=CARTESIAN_POINT('Ctrl Pts',(-23.1770659320137,-68.6222317244336,
12.));
#71674=CARTESIAN_POINT('Ctrl Pts',(-23.1760778585094,-68.6470392174567,
0.));
#71675=CARTESIAN_POINT('Ctrl Pts',(-23.1760778585094,-68.6470392174567,
12.));
#71676=CARTESIAN_POINT('Ctrl Pts',(-23.1750643563606,-68.6718862065227,
0.));
#71677=CARTESIAN_POINT('Ctrl Pts',(-23.1750643563606,-68.6718862065227,
12.));
#71678=CARTESIAN_POINT('Ctrl Pts',(-23.1740253733423,-68.6967725797457,
0.));
#71679=CARTESIAN_POINT('Ctrl Pts',(-23.1740253733423,-68.6967725797457,
12.));
#71680=CARTESIAN_POINT('Ctrl Pts',(-23.1729608575115,-68.7216982256357,
0.));
#71681=CARTESIAN_POINT('Ctrl Pts',(-23.1729608575115,-68.7216982256357,
12.));
#71682=CARTESIAN_POINT('Ctrl Pts',(-23.1718707572047,-68.7466630330968,
0.));
#71683=CARTESIAN_POINT('Ctrl Pts',(-23.1718707572047,-68.7466630330968,
12.));
#71684=CARTESIAN_POINT('Ctrl Pts',(-23.1707550210359,-68.7716668914246,
0.));
#71685=CARTESIAN_POINT('Ctrl Pts',(-23.1707550210359,-68.7716668914246,
12.));
#71686=CARTESIAN_POINT('Ctrl Pts',(-23.1696135978993,-68.7967096902981,
0.));
#71687=CARTESIAN_POINT('Ctrl Pts',(-23.1696135978993,-68.7967096902981,
12.));
#71688=CARTESIAN_POINT('Ctrl Pts',(-23.1684464369681,-68.8217913197735,
0.));
#71689=CARTESIAN_POINT('Ctrl Pts',(-23.1684464369681,-68.8217913197735,
12.));
#71690=CARTESIAN_POINT('Ctrl Pts',(-23.1672534876885,-68.8469116702885,
0.));
#71691=CARTESIAN_POINT('Ctrl Pts',(-23.1672534876885,-68.8469116702885,
12.));
#71692=CARTESIAN_POINT('Ctrl Pts',(-23.1660346997763,-68.8720706326606,
0.));
#71693=CARTESIAN_POINT('Ctrl Pts',(-23.1660346997763,-68.8720706326606,
12.));
#71694=CARTESIAN_POINT('Ctrl Pts',(-23.1647900232152,-68.8972680980844,
0.));
#71695=CARTESIAN_POINT('Ctrl Pts',(-23.1647900232152,-68.8972680980844,
12.));
#71696=CARTESIAN_POINT('Ctrl Pts',(-23.1635194082582,-68.9225039581249,
0.));
#71697=CARTESIAN_POINT('Ctrl Pts',(-23.1635194082582,-68.9225039581249,
12.));
#71698=CARTESIAN_POINT('Ctrl Pts',(-23.162222805429,-68.9477781047103,0.));
#71699=CARTESIAN_POINT('Ctrl Pts',(-23.162222805429,-68.9477781047103,12.));
#71700=CARTESIAN_POINT('Ctrl Pts',(-23.1609001655154,-68.9730904301362,
0.));
#71701=CARTESIAN_POINT('Ctrl Pts',(-23.1609001655154,-68.9730904301362,
12.));
#71702=CARTESIAN_POINT('Ctrl Pts',(-23.1595514395655,-68.9984408270652,
0.));
#71703=CARTESIAN_POINT('Ctrl Pts',(-23.1595514395655,-68.9984408270652,
12.));
#71704=CARTESIAN_POINT('Ctrl Pts',(-23.1581765788869,-69.0238291885245,
0.));
#71705=CARTESIAN_POINT('Ctrl Pts',(-23.1581765788869,-69.0238291885245,
12.));
#71706=CARTESIAN_POINT('Ctrl Pts',(-23.1567755350472,-69.0492554078999,
0.));
#71707=CARTESIAN_POINT('Ctrl Pts',(-23.1567755350472,-69.0492554078999,
12.));
#71708=CARTESIAN_POINT('Ctrl Pts',(-23.1553482598768,-69.0747193789291,
0.));
#71709=CARTESIAN_POINT('Ctrl Pts',(-23.1553482598768,-69.0747193789291,
12.));
#71710=CARTESIAN_POINT('Ctrl Pts',(-23.153894705462,-69.1002209957036,0.));
#71711=CARTESIAN_POINT('Ctrl Pts',(-23.153894705462,-69.1002209957036,12.));
#71712=CARTESIAN_POINT('Ctrl Pts',(-23.1524148241413,-69.1257601526692,
0.));
#71713=CARTESIAN_POINT('Ctrl Pts',(-23.1524148241413,-69.1257601526692,
12.));
#71714=CARTESIAN_POINT('Ctrl Pts',(-23.1509085685033,-69.1513367446231,
0.));
#71715=CARTESIAN_POINT('Ctrl Pts',(-23.1509085685033,-69.1513367446231,
12.));
#71716=CARTESIAN_POINT('Ctrl Pts',(-23.1493758913857,-69.176950666708,0.));
#71717=CARTESIAN_POINT('Ctrl Pts',(-23.1493758913857,-69.176950666708,12.));
#71718=CARTESIAN_POINT('Ctrl Pts',(-23.1478167458787,-69.2026018144023,
0.));
#71719=CARTESIAN_POINT('Ctrl Pts',(-23.1478167458787,-69.2026018144023,
12.));
#71720=CARTESIAN_POINT('Ctrl Pts',(-23.1462310853205,-69.2282900835234,
0.));
#71721=CARTESIAN_POINT('Ctrl Pts',(-23.1462310853205,-69.2282900835234,
12.));
#71722=CARTESIAN_POINT('Ctrl Pts',(-23.1446188632931,-69.2540153702311,
0.));
#71723=CARTESIAN_POINT('Ctrl Pts',(-23.1446188632931,-69.2540153702311,
12.));
#71724=CARTESIAN_POINT('Ctrl Pts',(-23.1429800336221,-69.2797775710275,
0.));
#71725=CARTESIAN_POINT('Ctrl Pts',(-23.1429800336221,-69.2797775710275,
12.));
#71726=CARTESIAN_POINT('Ctrl Pts',(-23.1413145503762,-69.3055765827544,
0.));
#71727=CARTESIAN_POINT('Ctrl Pts',(-23.1413145503762,-69.3055765827544,
12.));
#71728=CARTESIAN_POINT('Ctrl Pts',(-23.1396223678725,-69.3314123025863,
0.));
#71729=CARTESIAN_POINT('Ctrl Pts',(-23.1396223678725,-69.3314123025863,
12.));
#71730=CARTESIAN_POINT('Ctrl Pts',(-23.1379034406718,-69.3572846280289,
0.));
#71731=CARTESIAN_POINT('Ctrl Pts',(-23.1379034406718,-69.3572846280289,
12.));
#71732=CARTESIAN_POINT('Ctrl Pts',(-23.1361577235708,-69.3831934569176,
0.));
#71733=CARTESIAN_POINT('Ctrl Pts',(-23.1361577235708,-69.3831934569176,
12.));
#71734=CARTESIAN_POINT('Ctrl Pts',(-23.1343851715989,-69.4091386874129,
0.));
#71735=CARTESIAN_POINT('Ctrl Pts',(-23.1343851715989,-69.4091386874129,
12.));
#71736=CARTESIAN_POINT('Ctrl Pts',(-23.1325857400145,-69.4351202179948,
0.));
#71737=CARTESIAN_POINT('Ctrl Pts',(-23.1325857400145,-69.4351202179948,
12.));
#71738=CARTESIAN_POINT('Ctrl Pts',(-23.1307593843063,-69.4611379474492,
0.));
#71739=CARTESIAN_POINT('Ctrl Pts',(-23.1307593843063,-69.4611379474492,
12.));
#71740=CARTESIAN_POINT('Ctrl Pts',(-23.1289060601927,-69.4871917748665,
0.));
#71741=CARTESIAN_POINT('Ctrl Pts',(-23.1289060601927,-69.4871917748665,
12.));
#71742=CARTESIAN_POINT('Ctrl Pts',(-23.1270257236207,-69.5132815996548,
0.));
#71743=CARTESIAN_POINT('Ctrl Pts',(-23.1270257236207,-69.5132815996548,
12.));
#71744=CARTESIAN_POINT('Ctrl Pts',(-23.1251183307678,-69.5394073215467,
0.));
#71745=CARTESIAN_POINT('Ctrl Pts',(-23.1251183307678,-69.5394073215467,
12.));
#71746=CARTESIAN_POINT('Ctrl Pts',(-23.1231838380452,-69.565568840605,0.));
#71747=CARTESIAN_POINT('Ctrl Pts',(-23.1231838380452,-69.565568840605,12.));
#71748=CARTESIAN_POINT('Ctrl Pts',(-23.1212222021049,-69.5917660572255,
0.));
#71749=CARTESIAN_POINT('Ctrl Pts',(-23.1212222021049,-69.5917660572255,
12.));
#71750=CARTESIAN_POINT('Ctrl Pts',(-23.1192333798438,-69.617998872135,0.));
#71751=CARTESIAN_POINT('Ctrl Pts',(-23.1192333798438,-69.617998872135,12.));
#71752=CARTESIAN_POINT('Ctrl Pts',(-23.1172173283856,-69.6442671863751,
0.));
#71753=CARTESIAN_POINT('Ctrl Pts',(-23.1172173283856,-69.6442671863751,
12.));
#71754=CARTESIAN_POINT('Ctrl Pts',(-23.1151740050679,-69.6705709012842,
0.));
#71755=CARTESIAN_POINT('Ctrl Pts',(-23.1151740050679,-69.6705709012842,
12.));
#71756=CARTESIAN_POINT('Ctrl Pts',(-23.1131033674301,-69.6969099184766,
0.));
#71757=CARTESIAN_POINT('Ctrl Pts',(-23.1131033674301,-69.6969099184766,
12.));
#71758=CARTESIAN_POINT('Ctrl Pts',(-23.111005373205,-69.7232841398207,0.));
#71759=CARTESIAN_POINT('Ctrl Pts',(-23.111005373205,-69.7232841398207,12.));
#71760=CARTESIAN_POINT('Ctrl Pts',(-23.1088799803094,-69.7496934674083,
0.));
#71761=CARTESIAN_POINT('Ctrl Pts',(-23.1088799803094,-69.7496934674083,
12.));
#71762=CARTESIAN_POINT('Ctrl Pts',(-23.1067271468614,-69.7761378035979,
0.));
#71763=CARTESIAN_POINT('Ctrl Pts',(-23.1067271468614,-69.7761378035979,
12.));
#71764=CARTESIAN_POINT('Ctrl Pts',(-23.1045468311994,-69.8026170510582,
0.));
#71765=CARTESIAN_POINT('Ctrl Pts',(-23.1045468311994,-69.8026170510582,
12.));
#71766=CARTESIAN_POINT('Ctrl Pts',(-23.1023389919052,-69.8291311128121,
0.));
#71767=CARTESIAN_POINT('Ctrl Pts',(-23.1023389919052,-69.8291311128121,
12.));
#71768=CARTESIAN_POINT('Ctrl Pts',(-23.100103587824,-69.8556798922688,0.));
#71769=CARTESIAN_POINT('Ctrl Pts',(-23.100103587824,-69.8556798922688,12.));
#71770=CARTESIAN_POINT('Ctrl Pts',(-23.0978405781018,-69.8822632932759,
0.));
#71771=CARTESIAN_POINT('Ctrl Pts',(-23.0978405781018,-69.8822632932759,
12.));
#71772=CARTESIAN_POINT('Ctrl Pts',(-23.0955499221556,-69.9088812200703,
0.));
#71773=CARTESIAN_POINT('Ctrl Pts',(-23.0955499221556,-69.9088812200703,
12.));
#71774=CARTESIAN_POINT('Ctrl Pts',(-23.0932315796066,-69.9355335771722,
0.));
#71775=CARTESIAN_POINT('Ctrl Pts',(-23.0932315796066,-69.9355335771722,
12.));
#71776=CARTESIAN_POINT('Ctrl Pts',(-23.0908855102251,-69.9622202692871,
0.));
#71777=CARTESIAN_POINT('Ctrl Pts',(-23.0908855102251,-69.9622202692871,
12.));
#71778=CARTESIAN_POINT('Ctrl Pts',(-23.0885116738798,-69.9889412012143,
0.));
#71779=CARTESIAN_POINT('Ctrl Pts',(-23.0885116738798,-69.9889412012143,
12.));
#71780=CARTESIAN_POINT('Ctrl Pts',(-23.0861100304731,-70.0156962777173,
0.));
#71781=CARTESIAN_POINT('Ctrl Pts',(-23.0861100304731,-70.0156962777173,
12.));
#71782=CARTESIAN_POINT('Ctrl Pts',(-23.0836805399378,-70.0424854035125,
0.));
#71783=CARTESIAN_POINT('Ctrl Pts',(-23.0836805399378,-70.0424854035125,
12.));
#71784=CARTESIAN_POINT('Ctrl Pts',(-23.081223162377,-70.0693084835387,0.));
#71785=CARTESIAN_POINT('Ctrl Pts',(-23.081223162377,-70.0693084835387,12.));
#71786=CARTESIAN_POINT('Ctrl Pts',(-23.0787378581778,-70.096165423165,0.));
#71787=CARTESIAN_POINT('Ctrl Pts',(-23.0787378581778,-70.096165423165,12.));
#71788=CARTESIAN_POINT('Ctrl Pts',(-23.076224588139,-70.1230561284222,0.));
#71789=CARTESIAN_POINT('Ctrl Pts',(-23.076224588139,-70.1230561284222,12.));
#71790=CARTESIAN_POINT('Ctrl Pts',(-23.0736833135934,-70.1499805062159,
0.));
#71791=CARTESIAN_POINT('Ctrl Pts',(-23.0736833135934,-70.1499805062159,
12.));
#71792=CARTESIAN_POINT('Ctrl Pts',(-23.0711139965432,-70.176938464556,0.));
#71793=CARTESIAN_POINT('Ctrl Pts',(-23.0711139965432,-70.176938464556,12.));
#71794=CARTESIAN_POINT('Ctrl Pts',(-23.0685165993681,-70.2039299120456,
0.));
#71795=CARTESIAN_POINT('Ctrl Pts',(-23.0685165993681,-70.2039299120456,
12.));
#71796=CARTESIAN_POINT('Ctrl Pts',(-23.0658910845425,-70.2309547573788,
0.));
#71797=CARTESIAN_POINT('Ctrl Pts',(-23.0658910845425,-70.2309547573788,
12.));
#71798=CARTESIAN_POINT('Ctrl Pts',(-23.0632374143276,-70.2580129087877,
0.));
#71799=CARTESIAN_POINT('Ctrl Pts',(-23.0632374143276,-70.2580129087877,
12.));
#71800=CARTESIAN_POINT('Ctrl Pts',(-23.0605555505326,-70.2851042736081,
0.));
#71801=CARTESIAN_POINT('Ctrl Pts',(-23.0605555505326,-70.2851042736081,
12.));
#71802=CARTESIAN_POINT('Ctrl Pts',(-23.0578454541116,-70.3122287575374,
0.));
#71803=CARTESIAN_POINT('Ctrl Pts',(-23.0578454541116,-70.3122287575374,
12.));
#71804=CARTESIAN_POINT('Ctrl Pts',(-23.0551070854942,-70.3393862652353,
0.));
#71805=CARTESIAN_POINT('Ctrl Pts',(-23.0551070854942,-70.3393862652353,
12.));
#71806=CARTESIAN_POINT('Ctrl Pts',(-23.0523404053188,-70.3665767016596,
0.));
#71807=CARTESIAN_POINT('Ctrl Pts',(-23.0523404053188,-70.3665767016596,
12.));
#71808=CARTESIAN_POINT('Ctrl Pts',(-23.0495453750773,-70.39379997323,0.));
#71809=CARTESIAN_POINT('Ctrl Pts',(-23.0495453750773,-70.39379997323,12.));
#71810=CARTESIAN_POINT('Ctrl Pts',(-23.0467219577289,-70.421055988934,0.));
#71811=CARTESIAN_POINT('Ctrl Pts',(-23.0467219577289,-70.421055988934,12.));
#71812=CARTESIAN_POINT('Ctrl Pts',(-23.0438701184995,-70.4483446617553,
0.));
#71813=CARTESIAN_POINT('Ctrl Pts',(-23.0438701184995,-70.4483446617553,
12.));
#71814=CARTESIAN_POINT('Ctrl Pts',(-23.0409898250726,-70.4756659090104,
0.));
#71815=CARTESIAN_POINT('Ctrl Pts',(-23.0409898250726,-70.4756659090104,
12.));
#71816=CARTESIAN_POINT('Ctrl Pts',(-23.0380810458237,-70.5030196491883,
0.));
#71817=CARTESIAN_POINT('Ctrl Pts',(-23.0380810458237,-70.5030196491883,
12.));
#71818=CARTESIAN_POINT('Ctrl Pts',(-23.035143748431,-70.5304057994537,0.));
#71819=CARTESIAN_POINT('Ctrl Pts',(-23.035143748431,-70.5304057994537,12.));
#71820=CARTESIAN_POINT('Ctrl Pts',(-23.0321778982705,-70.5578242727606,
0.));
#71821=CARTESIAN_POINT('Ctrl Pts',(-23.0321778982705,-70.5578242727606,
12.));
#71822=CARTESIAN_POINT('Ctrl Pts',(-23.0291834570688,-70.5852749754167,
0.));
#71823=CARTESIAN_POINT('Ctrl Pts',(-23.0291834570688,-70.5852749754167,
12.));
#71824=CARTESIAN_POINT('Ctrl Pts',(-23.0261603810187,-70.6127578036869,
0.));
#71825=CARTESIAN_POINT('Ctrl Pts',(-23.0261603810187,-70.6127578036869,
12.));
#71826=CARTESIAN_POINT('Ctrl Pts',(-23.0231086235263,-70.6402726486718,
0.));
#71827=CARTESIAN_POINT('Ctrl Pts',(-23.0231086235263,-70.6402726486718,
12.));
#71828=CARTESIAN_POINT('Ctrl Pts',(-23.0200281385906,-70.6678194023389,
0.));
#71829=CARTESIAN_POINT('Ctrl Pts',(-23.0200281385906,-70.6678194023389,
12.));
#71830=CARTESIAN_POINT('Ctrl Pts',(-23.0169188841084,-70.6953979633561,
0.));
#71831=CARTESIAN_POINT('Ctrl Pts',(-23.0169188841084,-70.6953979633561,
12.));
#71832=CARTESIAN_POINT('Ctrl Pts',(-23.0137808248899,-70.7230082425324,
0.));
#71833=CARTESIAN_POINT('Ctrl Pts',(-23.0137808248899,-70.7230082425324,
12.));
#71834=CARTESIAN_POINT('Ctrl Pts',(-23.0106139365941,-70.7506501695822,
0.));
#71835=CARTESIAN_POINT('Ctrl Pts',(-23.0106139365941,-70.7506501695822,
12.));
#71836=CARTESIAN_POINT('Ctrl Pts',(-23.0074182063611,-70.7783236950588,
0.));
#71837=CARTESIAN_POINT('Ctrl Pts',(-23.0074182063611,-70.7783236950588,
12.));
#71838=CARTESIAN_POINT('Ctrl Pts',(-23.004193629142,-70.806028785987,0.));
#71839=CARTESIAN_POINT('Ctrl Pts',(-23.004193629142,-70.806028785987,12.));
#71840=CARTESIAN_POINT('Ctrl Pts',(-23.0015908899222,-70.8282180956627,
0.));
#71841=CARTESIAN_POINT('Ctrl Pts',(-23.0015908899222,-70.8282180956627,
12.));
#71842=CARTESIAN_POINT('Ctrl Pts',(-22.9996258555187,-70.8448742696329,
0.));
#71843=CARTESIAN_POINT('Ctrl Pts',(-22.9996258555187,-70.8448742696329,
12.));
#71844=CARTESIAN_POINT('Ctrl Pts',(-22.9983100639354,-70.8559846927868,
0.));
#71845=CARTESIAN_POINT('Ctrl Pts',(-22.9983100639354,-70.8559846927868,
12.));
#71846=CARTESIAN_POINT('Ctrl Pts',(-22.9976507259817,-70.8615414811571,
0.));
#71847=CARTESIAN_POINT('Ctrl Pts',(-22.9976507259817,-70.8615414811571,
12.));
#71848=CARTESIAN_POINT('',(-23.1372951448024,-66.0656156664138,0.));
#71849=CARTESIAN_POINT('Ctrl Pts',(-23.1372951448024,-66.0656156664138,
0.));
#71850=CARTESIAN_POINT('Ctrl Pts',(-23.1375957166104,-66.0694876382127,
0.));
#71851=CARTESIAN_POINT('Ctrl Pts',(-23.13819515974,-66.0772371487248,0.));
#71852=CARTESIAN_POINT('Ctrl Pts',(-23.1390892229779,-66.088878115242,0.));
#71853=CARTESIAN_POINT('Ctrl Pts',(-23.1402711039425,-66.1044328067355,
0.));
#71854=CARTESIAN_POINT('Ctrl Pts',(-23.1417314398398,-66.1239318368548,
0.));
#71855=CARTESIAN_POINT('Ctrl Pts',(-23.1431747350098,-66.1434865015027,
0.));
#71856=CARTESIAN_POINT('Ctrl Pts',(-23.1446009424903,-66.1630967296747,
0.));
#71857=CARTESIAN_POINT('Ctrl Pts',(-23.1460099850763,-66.18276239029,0.));
#71858=CARTESIAN_POINT('Ctrl Pts',(-23.1474017566484,-66.2024832934866,
0.));
#71859=CARTESIAN_POINT('Ctrl Pts',(-23.1487761349328,-66.2222592165473,
0.));
#71860=CARTESIAN_POINT('Ctrl Pts',(-23.1501329914488,-66.2420899237317,
0.));
#71861=CARTESIAN_POINT('Ctrl Pts',(-23.1514722022483,-66.2619751878741,
0.));
#71862=CARTESIAN_POINT('Ctrl Pts',(-23.1527936592625,-66.2819148131072,
0.));
#71863=CARTESIAN_POINT('Ctrl Pts',(-23.154097266617,-66.301908627539,0.));
#71864=CARTESIAN_POINT('Ctrl Pts',(-23.1553829352531,-66.3219564725161,
0.));
#71865=CARTESIAN_POINT('Ctrl Pts',(-23.1566505784626,-66.3420581937159,
0.));
#71866=CARTESIAN_POINT('Ctrl Pts',(-23.1579001063438,-66.3622136300692,
0.));
#71867=CARTESIAN_POINT('Ctrl Pts',(-23.1591314230101,-66.382422608185,0.));
#71868=CARTESIAN_POINT('Ctrl Pts',(-23.1603444294754,-66.402684948127,0.));
#71869=CARTESIAN_POINT('Ctrl Pts',(-23.1615390254635,-66.4230004670288,
0.));
#71870=CARTESIAN_POINT('Ctrl Pts',(-23.1627151114875,-66.4433689832454,
0.));
#71871=CARTESIAN_POINT('Ctrl Pts',(-23.163872591218,-66.4637903210682,0.));
#71872=CARTESIAN_POINT('Ctrl Pts',(-23.1650113713792,-66.4842643105263,
0.));
#71873=CARTESIAN_POINT('Ctrl Pts',(-23.1661313606123,-66.5047907851319,
0.));
#71874=CARTESIAN_POINT('Ctrl Pts',(-23.1672324686928,-66.5253695803209,
0.));
#71875=CARTESIAN_POINT('Ctrl Pts',(-23.1683146055736,-66.5460005315406,
0.));
#71876=CARTESIAN_POINT('Ctrl Pts',(-23.169377680588,-66.5666834726494,0.));
#71877=CARTESIAN_POINT('Ctrl Pts',(-23.1704216028626,-66.5874182367596,
0.));
#71878=CARTESIAN_POINT('Ctrl Pts',(-23.1714462816794,-66.6082046569657,
0.));
#71879=CARTESIAN_POINT('Ctrl Pts',(-23.1724516268299,-66.6290425670538,
0.));
#71880=CARTESIAN_POINT('Ctrl Pts',(-23.1734375490421,-66.6499318023445,
0.));
#71881=CARTESIAN_POINT('Ctrl Pts',(-23.174403960137,-66.6708722000046,0.));
#71882=CARTESIAN_POINT('Ctrl Pts',(-23.1753507727932,-66.691863598595,0.));
#71883=CARTESIAN_POINT('Ctrl Pts',(-23.1762779004043,-66.712905837789,0.));
#71884=CARTESIAN_POINT('Ctrl Pts',(-23.1771852569137,-66.7339987580441,
0.));
#71885=CARTESIAN_POINT('Ctrl Pts',(-23.1780727566309,-66.7551422002229,
0.));
#71886=CARTESIAN_POINT('Ctrl Pts',(-23.1789403142376,-66.7763360056146,
0.));
#71887=CARTESIAN_POINT('Ctrl Pts',(-23.1797878448645,-66.7975800161014,
0.));
#71888=CARTESIAN_POINT('Ctrl Pts',(-23.1806152641475,-66.8188740742727,
0.));
#71889=CARTESIAN_POINT('Ctrl Pts',(-23.1814224882948,-66.8402180235549,
0.));
#71890=CARTESIAN_POINT('Ctrl Pts',(-23.1822094341508,-66.8616117083304,
0.));
#71891=CARTESIAN_POINT('Ctrl Pts',(-23.1829760191583,-66.8830549738768,
0.));
#71892=CARTESIAN_POINT('Ctrl Pts',(-23.1837221613231,-66.904547666305,0.));
#71893=CARTESIAN_POINT('Ctrl Pts',(-23.1844477791816,-66.9260896324955,
0.));
#71894=CARTESIAN_POINT('Ctrl Pts',(-23.1851527917666,-66.9476807200225,
0.));
#71895=CARTESIAN_POINT('Ctrl Pts',(-23.1858371185852,-66.9693207771058,
0.));
#71896=CARTESIAN_POINT('Ctrl Pts',(-23.1865006796291,-66.9910096526483,
0.));
#71897=CARTESIAN_POINT('Ctrl Pts',(-23.1871433953795,-67.0127471962507,
0.));
#71898=CARTESIAN_POINT('Ctrl Pts',(-23.1877651868155,-67.0345332582297,
0.));
#71899=CARTESIAN_POINT('Ctrl Pts',(-23.1883659754268,-67.0563676896312,
0.));
#71900=CARTESIAN_POINT('Ctrl Pts',(-23.1889456832116,-67.0782503422293,
0.));
#71901=CARTESIAN_POINT('Ctrl Pts',(-23.1895042326626,-67.1001810685138,
0.));
#71902=CARTESIAN_POINT('Ctrl Pts',(-23.1900415467575,-67.122159721674,0.));
#71903=CARTESIAN_POINT('Ctrl Pts',(-23.1905575489506,-67.1441861555819,
0.));
#71904=CARTESIAN_POINT('Ctrl Pts',(-23.1910521631658,-67.1662602247641,
0.));
#71905=CARTESIAN_POINT('Ctrl Pts',(-23.1915253137924,-67.1883817844039,
0.));
#71906=CARTESIAN_POINT('Ctrl Pts',(-23.1919769256803,-67.2105506903448,
0.));
#71907=CARTESIAN_POINT('Ctrl Pts',(-23.1924069241386,-67.232766799088,0.));
#71908=CARTESIAN_POINT('Ctrl Pts',(-23.1928152349344,-67.2550299677888,
0.));
#71909=CARTESIAN_POINT('Ctrl Pts',(-23.1932017842954,-67.2773400542477,
0.));
#71910=CARTESIAN_POINT('Ctrl Pts',(-23.193566498902,-67.2996969169099,0.));
#71911=CARTESIAN_POINT('Ctrl Pts',(-23.1939093058802,-67.3221004148604,
0.));
#71912=CARTESIAN_POINT('Ctrl Pts',(-23.1942301327979,-67.3445504078178,
0.));
#71913=CARTESIAN_POINT('Ctrl Pts',(-23.1945289076608,-67.3670467561205,
0.));
#71914=CARTESIAN_POINT('Ctrl Pts',(-23.1948055589123,-67.3895893207168,
0.));
#71915=CARTESIAN_POINT('Ctrl Pts',(-23.195060015426,-67.4121779631666,0.));
#71916=CARTESIAN_POINT('Ctrl Pts',(-23.1952922065009,-67.4348125456389,
0.));
#71917=CARTESIAN_POINT('Ctrl Pts',(-23.1955020618591,-67.4574929309078,
0.));
#71918=CARTESIAN_POINT('Ctrl Pts',(-23.1956895116446,-67.4802189823423,
0.));
#71919=CARTESIAN_POINT('Ctrl Pts',(-23.1958544864224,-67.5029905638973,
0.));
#71920=CARTESIAN_POINT('Ctrl Pts',(-23.195996917171,-67.525807540117,0.));
#71921=CARTESIAN_POINT('Ctrl Pts',(-23.1961167352777,-67.5486697761301,
0.));
#71922=CARTESIAN_POINT('Ctrl Pts',(-23.1962138725358,-67.5715771376454,
0.));
#71923=CARTESIAN_POINT('Ctrl Pts',(-23.1962882611444,-67.5945294909398,
0.));
#71924=CARTESIAN_POINT('Ctrl Pts',(-23.1963398337056,-67.6175267028516,
0.));
#71925=CARTESIAN_POINT('Ctrl Pts',(-23.1963685232176,-67.6405686407828,
0.));
#71926=CARTESIAN_POINT('Ctrl Pts',(-23.196374263071,-67.6636551726948,0.));
#71927=CARTESIAN_POINT('Ctrl Pts',(-23.1963569870457,-67.6867861671044,
0.));
#71928=CARTESIAN_POINT('Ctrl Pts',(-23.1963166293116,-67.7099614930712,
0.));
#71929=CARTESIAN_POINT('Ctrl Pts',(-23.1962531244261,-67.7331810201931,
0.));
#71930=CARTESIAN_POINT('Ctrl Pts',(-23.1961664073274,-67.7564446186115,
0.));
#71931=CARTESIAN_POINT('Ctrl Pts',(-23.1960564133308,-67.7797521590056,
0.));
#71932=CARTESIAN_POINT('Ctrl Pts',(-23.1959230781265,-67.8031035125873,
0.));
#71933=CARTESIAN_POINT('Ctrl Pts',(-23.1957663377798,-67.8264985510884,
0.));
#71934=CARTESIAN_POINT('Ctrl Pts',(-23.1955861287276,-67.8499371467578,
0.));
#71935=CARTESIAN_POINT('Ctrl Pts',(-23.1953823877727,-67.8734191723639,
0.));
#71936=CARTESIAN_POINT('Ctrl Pts',(-23.19515505208,-67.8969445011908,0.));
#71937=CARTESIAN_POINT('Ctrl Pts',(-23.1949040591748,-67.9205130070337,
0.));
#71938=CARTESIAN_POINT('Ctrl Pts',(-23.1946293469437,-67.944124564187,0.));
#71939=CARTESIAN_POINT('Ctrl Pts',(-23.1943308536307,-67.9677790474414,
0.));
#71940=CARTESIAN_POINT('Ctrl Pts',(-23.194008517832,-67.9914763320878,0.));
#71941=CARTESIAN_POINT('Ctrl Pts',(-23.193662278492,-68.0152162939123,0.));
#71942=CARTESIAN_POINT('Ctrl Pts',(-23.1932920749021,-68.0389988091926,
0.));
#71943=CARTESIAN_POINT('Ctrl Pts',(-23.1928978467018,-68.0628237546852,
0.));
#71944=CARTESIAN_POINT('Ctrl Pts',(-23.1924795338746,-68.086691007624,0.));
#71945=CARTESIAN_POINT('Ctrl Pts',(-23.1920370767424,-68.1106004457223,
0.));
#71946=CARTESIAN_POINT('Ctrl Pts',(-23.1915704159624,-68.1345519471695,
0.));
#71947=CARTESIAN_POINT('Ctrl Pts',(-23.1910794925252,-68.1585453906259,
0.));
#71948=CARTESIAN_POINT('Ctrl Pts',(-23.1905642477572,-68.182580655213,0.));
#71949=CARTESIAN_POINT('Ctrl Pts',(-23.1900246233165,-68.2066576205113,
0.));
#71950=CARTESIAN_POINT('Ctrl Pts',(-23.189460561187,-68.2307761665629,0.));
#71951=CARTESIAN_POINT('Ctrl Pts',(-23.1888720036757,-68.2549361738679,
0.));
#71952=CARTESIAN_POINT('Ctrl Pts',(-23.1882588934108,-68.2791375233798,
0.));
#71953=CARTESIAN_POINT('Ctrl Pts',(-23.1876211733439,-68.3033800964946,
0.));
#71954=CARTESIAN_POINT('Ctrl Pts',(-23.1869587867463,-68.3276637750494,
0.));
#71955=CARTESIAN_POINT('Ctrl Pts',(-23.1862716772034,-68.3519884413253,
0.));
#71956=CARTESIAN_POINT('Ctrl Pts',(-23.1855597886117,-68.3763539780442,
0.));
#71957=CARTESIAN_POINT('Ctrl Pts',(-23.1848230651776,-68.4007602683649,
0.));
#71958=CARTESIAN_POINT('Ctrl Pts',(-23.1840614514191,-68.4252071958725,
0.));
#71959=CARTESIAN_POINT('Ctrl Pts',(-23.1832748921629,-68.4496946445756,
0.));
#71960=CARTESIAN_POINT('Ctrl Pts',(-23.1824633325385,-68.4742224989099,
0.));
#71961=CARTESIAN_POINT('Ctrl Pts',(-23.1816267179752,-68.4987906437357,
0.));
#71962=CARTESIAN_POINT('Ctrl Pts',(-23.1807649942011,-68.5233989643344,
0.));
#71963=CARTESIAN_POINT('Ctrl Pts',(-23.1798781072449,-68.548047346398,0.));
#71964=CARTESIAN_POINT('Ctrl Pts',(-23.178966003434,-68.572735676027,0.));
#71965=CARTESIAN_POINT('Ctrl Pts',(-23.1780286293873,-68.5974638397322,
0.));
#71966=CARTESIAN_POINT('Ctrl Pts',(-23.1770659320137,-68.6222317244336,
0.));
#71967=CARTESIAN_POINT('Ctrl Pts',(-23.1760778585094,-68.6470392174567,
0.));
#71968=CARTESIAN_POINT('Ctrl Pts',(-23.1750643563606,-68.6718862065227,
0.));
#71969=CARTESIAN_POINT('Ctrl Pts',(-23.1740253733423,-68.6967725797457,
0.));
#71970=CARTESIAN_POINT('Ctrl Pts',(-23.1729608575115,-68.7216982256357,
0.));
#71971=CARTESIAN_POINT('Ctrl Pts',(-23.1718707572047,-68.7466630330968,
0.));
#71972=CARTESIAN_POINT('Ctrl Pts',(-23.1707550210359,-68.7716668914246,
0.));
#71973=CARTESIAN_POINT('Ctrl Pts',(-23.1696135978993,-68.7967096902981,
0.));
#71974=CARTESIAN_POINT('Ctrl Pts',(-23.1684464369681,-68.8217913197735,
0.));
#71975=CARTESIAN_POINT('Ctrl Pts',(-23.1672534876885,-68.8469116702885,
0.));
#71976=CARTESIAN_POINT('Ctrl Pts',(-23.1660346997763,-68.8720706326606,
0.));
#71977=CARTESIAN_POINT('Ctrl Pts',(-23.1647900232152,-68.8972680980844,
0.));
#71978=CARTESIAN_POINT('Ctrl Pts',(-23.1635194082582,-68.9225039581249,
0.));
#71979=CARTESIAN_POINT('Ctrl Pts',(-23.162222805429,-68.9477781047103,0.));
#71980=CARTESIAN_POINT('Ctrl Pts',(-23.1609001655154,-68.9730904301362,
0.));
#71981=CARTESIAN_POINT('Ctrl Pts',(-23.1595514395655,-68.9984408270652,
0.));
#71982=CARTESIAN_POINT('Ctrl Pts',(-23.1581765788869,-69.0238291885245,
0.));
#71983=CARTESIAN_POINT('Ctrl Pts',(-23.1567755350472,-69.0492554078999,
0.));
#71984=CARTESIAN_POINT('Ctrl Pts',(-23.1553482598768,-69.0747193789291,
0.));
#71985=CARTESIAN_POINT('Ctrl Pts',(-23.153894705462,-69.1002209957036,0.));
#71986=CARTESIAN_POINT('Ctrl Pts',(-23.1524148241413,-69.1257601526692,
0.));
#71987=CARTESIAN_POINT('Ctrl Pts',(-23.1509085685033,-69.1513367446231,
0.));
#71988=CARTESIAN_POINT('Ctrl Pts',(-23.1493758913857,-69.176950666708,0.));
#71989=CARTESIAN_POINT('Ctrl Pts',(-23.1478167458787,-69.2026018144023,
0.));
#71990=CARTESIAN_POINT('Ctrl Pts',(-23.1462310853205,-69.2282900835234,
0.));
#71991=CARTESIAN_POINT('Ctrl Pts',(-23.1446188632931,-69.2540153702311,
0.));
#71992=CARTESIAN_POINT('Ctrl Pts',(-23.1429800336221,-69.2797775710275,
0.));
#71993=CARTESIAN_POINT('Ctrl Pts',(-23.1413145503762,-69.3055765827544,
0.));
#71994=CARTESIAN_POINT('Ctrl Pts',(-23.1396223678725,-69.3314123025863,
0.));
#71995=CARTESIAN_POINT('Ctrl Pts',(-23.1379034406718,-69.3572846280289,
0.));
#71996=CARTESIAN_POINT('Ctrl Pts',(-23.1361577235708,-69.3831934569176,
0.));
#71997=CARTESIAN_POINT('Ctrl Pts',(-23.1343851715989,-69.4091386874129,
0.));
#71998=CARTESIAN_POINT('Ctrl Pts',(-23.1325857400145,-69.4351202179948,
0.));
#71999=CARTESIAN_POINT('Ctrl Pts',(-23.1307593843063,-69.4611379474492,
0.));
#72000=CARTESIAN_POINT('Ctrl Pts',(-23.1289060601927,-69.4871917748665,
0.));
#72001=CARTESIAN_POINT('Ctrl Pts',(-23.1270257236207,-69.5132815996548,
0.));
#72002=CARTESIAN_POINT('Ctrl Pts',(-23.1251183307678,-69.5394073215467,
0.));
#72003=CARTESIAN_POINT('Ctrl Pts',(-23.1231838380452,-69.565568840605,0.));
#72004=CARTESIAN_POINT('Ctrl Pts',(-23.1212222021049,-69.5917660572255,
0.));
#72005=CARTESIAN_POINT('Ctrl Pts',(-23.1192333798438,-69.617998872135,0.));
#72006=CARTESIAN_POINT('Ctrl Pts',(-23.1172173283856,-69.6442671863751,
0.));
#72007=CARTESIAN_POINT('Ctrl Pts',(-23.1151740050679,-69.6705709012842,
0.));
#72008=CARTESIAN_POINT('Ctrl Pts',(-23.1131033674301,-69.6969099184766,
0.));
#72009=CARTESIAN_POINT('Ctrl Pts',(-23.111005373205,-69.7232841398207,0.));
#72010=CARTESIAN_POINT('Ctrl Pts',(-23.1088799803094,-69.7496934674083,
0.));
#72011=CARTESIAN_POINT('Ctrl Pts',(-23.1067271468614,-69.7761378035979,
0.));
#72012=CARTESIAN_POINT('Ctrl Pts',(-23.1045468311994,-69.8026170510582,
0.));
#72013=CARTESIAN_POINT('Ctrl Pts',(-23.1023389919052,-69.8291311128121,
0.));
#72014=CARTESIAN_POINT('Ctrl Pts',(-23.100103587824,-69.8556798922688,0.));
#72015=CARTESIAN_POINT('Ctrl Pts',(-23.0978405781018,-69.8822632932759,
0.));
#72016=CARTESIAN_POINT('Ctrl Pts',(-23.0955499221556,-69.9088812200703,
0.));
#72017=CARTESIAN_POINT('Ctrl Pts',(-23.0932315796066,-69.9355335771722,
0.));
#72018=CARTESIAN_POINT('Ctrl Pts',(-23.0908855102251,-69.9622202692871,
0.));
#72019=CARTESIAN_POINT('Ctrl Pts',(-23.0885116738798,-69.9889412012143,
0.));
#72020=CARTESIAN_POINT('Ctrl Pts',(-23.0861100304731,-70.0156962777173,
0.));
#72021=CARTESIAN_POINT('Ctrl Pts',(-23.0836805399378,-70.0424854035125,
0.));
#72022=CARTESIAN_POINT('Ctrl Pts',(-23.081223162377,-70.0693084835387,0.));
#72023=CARTESIAN_POINT('Ctrl Pts',(-23.0787378581778,-70.096165423165,0.));
#72024=CARTESIAN_POINT('Ctrl Pts',(-23.076224588139,-70.1230561284222,0.));
#72025=CARTESIAN_POINT('Ctrl Pts',(-23.0736833135934,-70.1499805062159,
0.));
#72026=CARTESIAN_POINT('Ctrl Pts',(-23.0711139965432,-70.176938464556,0.));
#72027=CARTESIAN_POINT('Ctrl Pts',(-23.0685165993681,-70.2039299120456,
0.));
#72028=CARTESIAN_POINT('Ctrl Pts',(-23.0658910845425,-70.2309547573788,
0.));
#72029=CARTESIAN_POINT('Ctrl Pts',(-23.0632374143276,-70.2580129087877,
0.));
#72030=CARTESIAN_POINT('Ctrl Pts',(-23.0605555505326,-70.2851042736081,
0.));
#72031=CARTESIAN_POINT('Ctrl Pts',(-23.0578454541116,-70.3122287575374,
0.));
#72032=CARTESIAN_POINT('Ctrl Pts',(-23.0551070854942,-70.3393862652353,
0.));
#72033=CARTESIAN_POINT('Ctrl Pts',(-23.0523404053188,-70.3665767016596,
0.));
#72034=CARTESIAN_POINT('Ctrl Pts',(-23.0495453750773,-70.39379997323,0.));
#72035=CARTESIAN_POINT('Ctrl Pts',(-23.0467219577289,-70.421055988934,0.));
#72036=CARTESIAN_POINT('Ctrl Pts',(-23.0438701184995,-70.4483446617553,
0.));
#72037=CARTESIAN_POINT('Ctrl Pts',(-23.0409898250726,-70.4756659090104,
0.));
#72038=CARTESIAN_POINT('Ctrl Pts',(-23.0384964376011,-70.4991133648756,
0.));
#72039=CARTESIAN_POINT('Ctrl Pts',(-23.0365694096158,-70.5171075702495,
0.));
#72040=CARTESIAN_POINT('Ctrl Pts',(-23.0352213647764,-70.5296341535252,
0.));
#72041=CARTESIAN_POINT('Ctrl Pts',(-23.034460662331,-70.5366836381299,0.));
#72042=CARTESIAN_POINT('Ctrl Pts',(-23.0342913834093,-70.5382514078489,
0.));
#72043=CARTESIAN_POINT('',(-23.1372951448024,-66.0656156664138,12.));
#72044=CARTESIAN_POINT('',(-23.1372951448024,-66.0656156664138,0.));
#72045=CARTESIAN_POINT('Ctrl Pts',(-23.0342913834093,-70.5382514078489,
12.));
#72046=CARTESIAN_POINT('Ctrl Pts',(-23.034460662331,-70.5366836381299,12.));
#72047=CARTESIAN_POINT('Ctrl Pts',(-23.0352213647764,-70.5296341535252,
12.));
#72048=CARTESIAN_POINT('Ctrl Pts',(-23.0365694096158,-70.5171075702495,
12.));
#72049=CARTESIAN_POINT('Ctrl Pts',(-23.0384964376011,-70.4991133648756,
12.));
#72050=CARTESIAN_POINT('Ctrl Pts',(-23.0409898250726,-70.4756659090104,
12.));
#72051=CARTESIAN_POINT('Ctrl Pts',(-23.0438701184995,-70.4483446617553,
12.));
#72052=CARTESIAN_POINT('Ctrl Pts',(-23.0467219577289,-70.421055988934,12.));
#72053=CARTESIAN_POINT('Ctrl Pts',(-23.0495453750773,-70.39379997323,12.));
#72054=CARTESIAN_POINT('Ctrl Pts',(-23.0523404053188,-70.3665767016596,
12.));
#72055=CARTESIAN_POINT('Ctrl Pts',(-23.0551070854942,-70.3393862652353,
12.));
#72056=CARTESIAN_POINT('Ctrl Pts',(-23.0578454541116,-70.3122287575374,
12.));
#72057=CARTESIAN_POINT('Ctrl Pts',(-23.0605555505326,-70.2851042736081,
12.));
#72058=CARTESIAN_POINT('Ctrl Pts',(-23.0632374143276,-70.2580129087877,
12.));
#72059=CARTESIAN_POINT('Ctrl Pts',(-23.0658910845425,-70.2309547573788,
12.));
#72060=CARTESIAN_POINT('Ctrl Pts',(-23.0685165993681,-70.2039299120456,
12.));
#72061=CARTESIAN_POINT('Ctrl Pts',(-23.0711139965432,-70.176938464556,12.));
#72062=CARTESIAN_POINT('Ctrl Pts',(-23.0736833135934,-70.1499805062159,
12.));
#72063=CARTESIAN_POINT('Ctrl Pts',(-23.076224588139,-70.1230561284222,12.));
#72064=CARTESIAN_POINT('Ctrl Pts',(-23.0787378581778,-70.096165423165,12.));
#72065=CARTESIAN_POINT('Ctrl Pts',(-23.081223162377,-70.0693084835387,12.));
#72066=CARTESIAN_POINT('Ctrl Pts',(-23.0836805399378,-70.0424854035125,
12.));
#72067=CARTESIAN_POINT('Ctrl Pts',(-23.0861100304731,-70.0156962777173,
12.));
#72068=CARTESIAN_POINT('Ctrl Pts',(-23.0885116738798,-69.9889412012143,
12.));
#72069=CARTESIAN_POINT('Ctrl Pts',(-23.0908855102251,-69.9622202692871,
12.));
#72070=CARTESIAN_POINT('Ctrl Pts',(-23.0932315796066,-69.9355335771722,
12.));
#72071=CARTESIAN_POINT('Ctrl Pts',(-23.0955499221556,-69.9088812200703,
12.));
#72072=CARTESIAN_POINT('Ctrl Pts',(-23.0978405781018,-69.8822632932759,
12.));
#72073=CARTESIAN_POINT('Ctrl Pts',(-23.100103587824,-69.8556798922688,12.));
#72074=CARTESIAN_POINT('Ctrl Pts',(-23.1023389919052,-69.8291311128121,
12.));
#72075=CARTESIAN_POINT('Ctrl Pts',(-23.1045468311994,-69.8026170510582,
12.));
#72076=CARTESIAN_POINT('Ctrl Pts',(-23.1067271468614,-69.7761378035979,
12.));
#72077=CARTESIAN_POINT('Ctrl Pts',(-23.1088799803094,-69.7496934674083,
12.));
#72078=CARTESIAN_POINT('Ctrl Pts',(-23.111005373205,-69.7232841398207,12.));
#72079=CARTESIAN_POINT('Ctrl Pts',(-23.1131033674301,-69.6969099184766,
12.));
#72080=CARTESIAN_POINT('Ctrl Pts',(-23.1151740050679,-69.6705709012842,
12.));
#72081=CARTESIAN_POINT('Ctrl Pts',(-23.1172173283856,-69.6442671863751,
12.));
#72082=CARTESIAN_POINT('Ctrl Pts',(-23.1192333798438,-69.617998872135,12.));
#72083=CARTESIAN_POINT('Ctrl Pts',(-23.1212222021049,-69.5917660572255,
12.));
#72084=CARTESIAN_POINT('Ctrl Pts',(-23.1231838380452,-69.565568840605,12.));
#72085=CARTESIAN_POINT('Ctrl Pts',(-23.1251183307678,-69.5394073215467,
12.));
#72086=CARTESIAN_POINT('Ctrl Pts',(-23.1270257236207,-69.5132815996548,
12.));
#72087=CARTESIAN_POINT('Ctrl Pts',(-23.1289060601927,-69.4871917748665,
12.));
#72088=CARTESIAN_POINT('Ctrl Pts',(-23.1307593843063,-69.4611379474492,
12.));
#72089=CARTESIAN_POINT('Ctrl Pts',(-23.1325857400145,-69.4351202179948,
12.));
#72090=CARTESIAN_POINT('Ctrl Pts',(-23.1343851715989,-69.4091386874129,
12.));
#72091=CARTESIAN_POINT('Ctrl Pts',(-23.1361577235708,-69.3831934569176,
12.));
#72092=CARTESIAN_POINT('Ctrl Pts',(-23.1379034406718,-69.3572846280289,
12.));
#72093=CARTESIAN_POINT('Ctrl Pts',(-23.1396223678725,-69.3314123025863,
12.));
#72094=CARTESIAN_POINT('Ctrl Pts',(-23.1413145503762,-69.3055765827544,
12.));
#72095=CARTESIAN_POINT('Ctrl Pts',(-23.1429800336221,-69.2797775710275,
12.));
#72096=CARTESIAN_POINT('Ctrl Pts',(-23.1446188632931,-69.2540153702311,
12.));
#72097=CARTESIAN_POINT('Ctrl Pts',(-23.1462310853205,-69.2282900835234,
12.));
#72098=CARTESIAN_POINT('Ctrl Pts',(-23.1478167458787,-69.2026018144023,
12.));
#72099=CARTESIAN_POINT('Ctrl Pts',(-23.1493758913857,-69.176950666708,12.));
#72100=CARTESIAN_POINT('Ctrl Pts',(-23.1509085685033,-69.1513367446231,
12.));
#72101=CARTESIAN_POINT('Ctrl Pts',(-23.1524148241413,-69.1257601526692,
12.));
#72102=CARTESIAN_POINT('Ctrl Pts',(-23.153894705462,-69.1002209957036,12.));
#72103=CARTESIAN_POINT('Ctrl Pts',(-23.1553482598768,-69.0747193789291,
12.));
#72104=CARTESIAN_POINT('Ctrl Pts',(-23.1567755350472,-69.0492554078999,
12.));
#72105=CARTESIAN_POINT('Ctrl Pts',(-23.1581765788869,-69.0238291885245,
12.));
#72106=CARTESIAN_POINT('Ctrl Pts',(-23.1595514395655,-68.9984408270652,
12.));
#72107=CARTESIAN_POINT('Ctrl Pts',(-23.1609001655154,-68.9730904301362,
12.));
#72108=CARTESIAN_POINT('Ctrl Pts',(-23.162222805429,-68.9477781047103,12.));
#72109=CARTESIAN_POINT('Ctrl Pts',(-23.1635194082582,-68.9225039581249,
12.));
#72110=CARTESIAN_POINT('Ctrl Pts',(-23.1647900232152,-68.8972680980844,
12.));
#72111=CARTESIAN_POINT('Ctrl Pts',(-23.1660346997763,-68.8720706326606,
12.));
#72112=CARTESIAN_POINT('Ctrl Pts',(-23.1672534876885,-68.8469116702885,
12.));
#72113=CARTESIAN_POINT('Ctrl Pts',(-23.1684464369681,-68.8217913197735,
12.));
#72114=CARTESIAN_POINT('Ctrl Pts',(-23.1696135978993,-68.7967096902981,
12.));
#72115=CARTESIAN_POINT('Ctrl Pts',(-23.1707550210359,-68.7716668914246,
12.));
#72116=CARTESIAN_POINT('Ctrl Pts',(-23.1718707572047,-68.7466630330968,
12.));
#72117=CARTESIAN_POINT('Ctrl Pts',(-23.1729608575115,-68.7216982256357,
12.));
#72118=CARTESIAN_POINT('Ctrl Pts',(-23.1740253733423,-68.6967725797457,
12.));
#72119=CARTESIAN_POINT('Ctrl Pts',(-23.1750643563606,-68.6718862065227,
12.));
#72120=CARTESIAN_POINT('Ctrl Pts',(-23.1760778585094,-68.6470392174567,
12.));
#72121=CARTESIAN_POINT('Ctrl Pts',(-23.1770659320137,-68.6222317244336,
12.));
#72122=CARTESIAN_POINT('Ctrl Pts',(-23.1780286293873,-68.5974638397322,
12.));
#72123=CARTESIAN_POINT('Ctrl Pts',(-23.178966003434,-68.572735676027,12.));
#72124=CARTESIAN_POINT('Ctrl Pts',(-23.1798781072449,-68.548047346398,12.));
#72125=CARTESIAN_POINT('Ctrl Pts',(-23.1807649942011,-68.5233989643344,
12.));
#72126=CARTESIAN_POINT('Ctrl Pts',(-23.1816267179752,-68.4987906437357,
12.));
#72127=CARTESIAN_POINT('Ctrl Pts',(-23.1824633325385,-68.4742224989099,
12.));
#72128=CARTESIAN_POINT('Ctrl Pts',(-23.1832748921629,-68.4496946445756,
12.));
#72129=CARTESIAN_POINT('Ctrl Pts',(-23.1840614514191,-68.4252071958725,
12.));
#72130=CARTESIAN_POINT('Ctrl Pts',(-23.1848230651776,-68.4007602683649,
12.));
#72131=CARTESIAN_POINT('Ctrl Pts',(-23.1855597886117,-68.3763539780442,
12.));
#72132=CARTESIAN_POINT('Ctrl Pts',(-23.1862716772034,-68.3519884413253,
12.));
#72133=CARTESIAN_POINT('Ctrl Pts',(-23.1869587867463,-68.3276637750494,
12.));
#72134=CARTESIAN_POINT('Ctrl Pts',(-23.1876211733439,-68.3033800964946,
12.));
#72135=CARTESIAN_POINT('Ctrl Pts',(-23.1882588934108,-68.2791375233798,
12.));
#72136=CARTESIAN_POINT('Ctrl Pts',(-23.1888720036757,-68.2549361738679,
12.));
#72137=CARTESIAN_POINT('Ctrl Pts',(-23.189460561187,-68.2307761665629,12.));
#72138=CARTESIAN_POINT('Ctrl Pts',(-23.1900246233165,-68.2066576205113,
12.));
#72139=CARTESIAN_POINT('Ctrl Pts',(-23.1905642477572,-68.182580655213,12.));
#72140=CARTESIAN_POINT('Ctrl Pts',(-23.1910794925252,-68.1585453906259,
12.));
#72141=CARTESIAN_POINT('Ctrl Pts',(-23.1915704159624,-68.1345519471695,
12.));
#72142=CARTESIAN_POINT('Ctrl Pts',(-23.1920370767424,-68.1106004457223,
12.));
#72143=CARTESIAN_POINT('Ctrl Pts',(-23.1924795338746,-68.086691007624,12.));
#72144=CARTESIAN_POINT('Ctrl Pts',(-23.1928978467018,-68.0628237546852,
12.));
#72145=CARTESIAN_POINT('Ctrl Pts',(-23.1932920749021,-68.0389988091926,
12.));
#72146=CARTESIAN_POINT('Ctrl Pts',(-23.193662278492,-68.0152162939123,12.));
#72147=CARTESIAN_POINT('Ctrl Pts',(-23.194008517832,-67.9914763320878,12.));
#72148=CARTESIAN_POINT('Ctrl Pts',(-23.1943308536307,-67.9677790474414,
12.));
#72149=CARTESIAN_POINT('Ctrl Pts',(-23.1946293469437,-67.944124564187,12.));
#72150=CARTESIAN_POINT('Ctrl Pts',(-23.1949040591748,-67.9205130070337,
12.));
#72151=CARTESIAN_POINT('Ctrl Pts',(-23.19515505208,-67.8969445011908,12.));
#72152=CARTESIAN_POINT('Ctrl Pts',(-23.1953823877727,-67.8734191723639,
12.));
#72153=CARTESIAN_POINT('Ctrl Pts',(-23.1955861287276,-67.8499371467578,
12.));
#72154=CARTESIAN_POINT('Ctrl Pts',(-23.1957663377798,-67.8264985510884,
12.));
#72155=CARTESIAN_POINT('Ctrl Pts',(-23.1959230781265,-67.8031035125873,
12.));
#72156=CARTESIAN_POINT('Ctrl Pts',(-23.1960564133308,-67.7797521590056,
12.));
#72157=CARTESIAN_POINT('Ctrl Pts',(-23.1961664073274,-67.7564446186115,
12.));
#72158=CARTESIAN_POINT('Ctrl Pts',(-23.1962531244261,-67.7331810201931,
12.));
#72159=CARTESIAN_POINT('Ctrl Pts',(-23.1963166293116,-67.7099614930712,
12.));
#72160=CARTESIAN_POINT('Ctrl Pts',(-23.1963569870457,-67.6867861671044,
12.));
#72161=CARTESIAN_POINT('Ctrl Pts',(-23.196374263071,-67.6636551726948,12.));
#72162=CARTESIAN_POINT('Ctrl Pts',(-23.1963685232176,-67.6405686407828,
12.));
#72163=CARTESIAN_POINT('Ctrl Pts',(-23.1963398337056,-67.6175267028516,
12.));
#72164=CARTESIAN_POINT('Ctrl Pts',(-23.1962882611444,-67.5945294909398,
12.));
#72165=CARTESIAN_POINT('Ctrl Pts',(-23.1962138725358,-67.5715771376454,
12.));
#72166=CARTESIAN_POINT('Ctrl Pts',(-23.1961167352777,-67.5486697761301,
12.));
#72167=CARTESIAN_POINT('Ctrl Pts',(-23.195996917171,-67.525807540117,12.));
#72168=CARTESIAN_POINT('Ctrl Pts',(-23.1958544864224,-67.5029905638973,
12.));
#72169=CARTESIAN_POINT('Ctrl Pts',(-23.1956895116446,-67.4802189823423,
12.));
#72170=CARTESIAN_POINT('Ctrl Pts',(-23.1955020618591,-67.4574929309078,
12.));
#72171=CARTESIAN_POINT('Ctrl Pts',(-23.1952922065009,-67.4348125456389,
12.));
#72172=CARTESIAN_POINT('Ctrl Pts',(-23.195060015426,-67.4121779631666,12.));
#72173=CARTESIAN_POINT('Ctrl Pts',(-23.1948055589123,-67.3895893207168,
12.));
#72174=CARTESIAN_POINT('Ctrl Pts',(-23.1945289076608,-67.3670467561205,
12.));
#72175=CARTESIAN_POINT('Ctrl Pts',(-23.1942301327979,-67.3445504078178,
12.));
#72176=CARTESIAN_POINT('Ctrl Pts',(-23.1939093058802,-67.3221004148604,
12.));
#72177=CARTESIAN_POINT('Ctrl Pts',(-23.193566498902,-67.2996969169099,12.));
#72178=CARTESIAN_POINT('Ctrl Pts',(-23.1932017842954,-67.2773400542477,
12.));
#72179=CARTESIAN_POINT('Ctrl Pts',(-23.1928152349344,-67.2550299677888,
12.));
#72180=CARTESIAN_POINT('Ctrl Pts',(-23.1924069241386,-67.232766799088,12.));
#72181=CARTESIAN_POINT('Ctrl Pts',(-23.1919769256803,-67.2105506903448,
12.));
#72182=CARTESIAN_POINT('Ctrl Pts',(-23.1915253137924,-67.1883817844039,
12.));
#72183=CARTESIAN_POINT('Ctrl Pts',(-23.1910521631658,-67.1662602247641,
12.));
#72184=CARTESIAN_POINT('Ctrl Pts',(-23.1905575489506,-67.1441861555819,
12.));
#72185=CARTESIAN_POINT('Ctrl Pts',(-23.1900415467575,-67.122159721674,12.));
#72186=CARTESIAN_POINT('Ctrl Pts',(-23.1895042326626,-67.1001810685138,
12.));
#72187=CARTESIAN_POINT('Ctrl Pts',(-23.1889456832116,-67.0782503422293,
12.));
#72188=CARTESIAN_POINT('Ctrl Pts',(-23.1883659754268,-67.0563676896312,
12.));
#72189=CARTESIAN_POINT('Ctrl Pts',(-23.1877651868155,-67.0345332582297,
12.));
#72190=CARTESIAN_POINT('Ctrl Pts',(-23.1871433953795,-67.0127471962507,
12.));
#72191=CARTESIAN_POINT('Ctrl Pts',(-23.1865006796291,-66.9910096526483,
12.));
#72192=CARTESIAN_POINT('Ctrl Pts',(-23.1858371185852,-66.9693207771058,
12.));
#72193=CARTESIAN_POINT('Ctrl Pts',(-23.1851527917666,-66.9476807200225,
12.));
#72194=CARTESIAN_POINT('Ctrl Pts',(-23.1844477791816,-66.9260896324955,
12.));
#72195=CARTESIAN_POINT('Ctrl Pts',(-23.1837221613231,-66.904547666305,12.));
#72196=CARTESIAN_POINT('Ctrl Pts',(-23.1829760191583,-66.8830549738768,
12.));
#72197=CARTESIAN_POINT('Ctrl Pts',(-23.1822094341508,-66.8616117083304,
12.));
#72198=CARTESIAN_POINT('Ctrl Pts',(-23.1814224882948,-66.8402180235549,
12.));
#72199=CARTESIAN_POINT('Ctrl Pts',(-23.1806152641475,-66.8188740742727,
12.));
#72200=CARTESIAN_POINT('Ctrl Pts',(-23.1797878448645,-66.7975800161014,
12.));
#72201=CARTESIAN_POINT('Ctrl Pts',(-23.1789403142376,-66.7763360056146,
12.));
#72202=CARTESIAN_POINT('Ctrl Pts',(-23.1780727566309,-66.7551422002229,
12.));
#72203=CARTESIAN_POINT('Ctrl Pts',(-23.1771852569137,-66.7339987580441,
12.));
#72204=CARTESIAN_POINT('Ctrl Pts',(-23.1762779004043,-66.712905837789,12.));
#72205=CARTESIAN_POINT('Ctrl Pts',(-23.1753507727932,-66.691863598595,12.));
#72206=CARTESIAN_POINT('Ctrl Pts',(-23.174403960137,-66.6708722000046,12.));
#72207=CARTESIAN_POINT('Ctrl Pts',(-23.1734375490421,-66.6499318023445,
12.));
#72208=CARTESIAN_POINT('Ctrl Pts',(-23.1724516268299,-66.6290425670538,
12.));
#72209=CARTESIAN_POINT('Ctrl Pts',(-23.1714462816794,-66.6082046569657,
12.));
#72210=CARTESIAN_POINT('Ctrl Pts',(-23.1704216028626,-66.5874182367596,
12.));
#72211=CARTESIAN_POINT('Ctrl Pts',(-23.169377680588,-66.5666834726494,12.));
#72212=CARTESIAN_POINT('Ctrl Pts',(-23.1683146055736,-66.5460005315406,
12.));
#72213=CARTESIAN_POINT('Ctrl Pts',(-23.1672324686928,-66.5253695803209,
12.));
#72214=CARTESIAN_POINT('Ctrl Pts',(-23.1661313606123,-66.5047907851319,
12.));
#72215=CARTESIAN_POINT('Ctrl Pts',(-23.1650113713792,-66.4842643105263,
12.));
#72216=CARTESIAN_POINT('Ctrl Pts',(-23.163872591218,-66.4637903210682,12.));
#72217=CARTESIAN_POINT('Ctrl Pts',(-23.1627151114875,-66.4433689832454,
12.));
#72218=CARTESIAN_POINT('Ctrl Pts',(-23.1615390254635,-66.4230004670288,
12.));
#72219=CARTESIAN_POINT('Ctrl Pts',(-23.1603444294754,-66.402684948127,12.));
#72220=CARTESIAN_POINT('Ctrl Pts',(-23.1591314230101,-66.382422608185,12.));
#72221=CARTESIAN_POINT('Ctrl Pts',(-23.1579001063438,-66.3622136300692,
12.));
#72222=CARTESIAN_POINT('Ctrl Pts',(-23.1566505784626,-66.3420581937159,
12.));
#72223=CARTESIAN_POINT('Ctrl Pts',(-23.1553829352531,-66.3219564725161,
12.));
#72224=CARTESIAN_POINT('Ctrl Pts',(-23.154097266617,-66.301908627539,12.));
#72225=CARTESIAN_POINT('Ctrl Pts',(-23.1527936592625,-66.2819148131072,
12.));
#72226=CARTESIAN_POINT('Ctrl Pts',(-23.1514722022483,-66.2619751878741,
12.));
#72227=CARTESIAN_POINT('Ctrl Pts',(-23.1501329914488,-66.2420899237317,
12.));
#72228=CARTESIAN_POINT('Ctrl Pts',(-23.1487761349328,-66.2222592165473,
12.));
#72229=CARTESIAN_POINT('Ctrl Pts',(-23.1474017566484,-66.2024832934866,
12.));
#72230=CARTESIAN_POINT('Ctrl Pts',(-23.1460099850763,-66.18276239029,12.));
#72231=CARTESIAN_POINT('Ctrl Pts',(-23.1446009424903,-66.1630967296747,
12.));
#72232=CARTESIAN_POINT('Ctrl Pts',(-23.1431747350098,-66.1434865015027,
12.));
#72233=CARTESIAN_POINT('Ctrl Pts',(-23.1417314398398,-66.1239318368548,
12.));
#72234=CARTESIAN_POINT('Ctrl Pts',(-23.1402711039425,-66.1044328067355,
12.));
#72235=CARTESIAN_POINT('Ctrl Pts',(-23.1390892229779,-66.088878115242,12.));
#72236=CARTESIAN_POINT('Ctrl Pts',(-23.13819515974,-66.0772371487248,12.));
#72237=CARTESIAN_POINT('Ctrl Pts',(-23.1375957166104,-66.0694876382127,
12.));
#72238=CARTESIAN_POINT('Ctrl Pts',(-23.1372951448024,-66.0656156664138,
12.));
#72239=CARTESIAN_POINT('Ctrl Pts',(-21.5904919935066,-70.993479606912,-5.55111512312578E-16));
#72240=CARTESIAN_POINT('Ctrl Pts',(-21.5904919935066,-70.993479606912,4.));
#72241=CARTESIAN_POINT('Ctrl Pts',(-21.5904919935066,-70.993479606912,8.));
#72242=CARTESIAN_POINT('Ctrl Pts',(-21.5904919935066,-70.993479606912,12.));
#72243=CARTESIAN_POINT('Ctrl Pts',(-21.6628164325805,-71.0762040404459,
-5.55111512312578E-16));
#72244=CARTESIAN_POINT('Ctrl Pts',(-21.6628164325805,-71.0762040404459,
4.));
#72245=CARTESIAN_POINT('Ctrl Pts',(-21.6628164325805,-71.076204040446,8.));
#72246=CARTESIAN_POINT('Ctrl Pts',(-21.6628164325805,-71.076204040446,12.));
#72247=CARTESIAN_POINT('Ctrl Pts',(-21.8385342042359,-71.1771795679079,
-5.55111512312578E-16));
#72248=CARTESIAN_POINT('Ctrl Pts',(-21.8385342042359,-71.1771795679079,
4.00000000000001));
#72249=CARTESIAN_POINT('Ctrl Pts',(-21.8385342042359,-71.177179567908,7.99999999999999));
#72250=CARTESIAN_POINT('Ctrl Pts',(-21.8385342042359,-71.177179567908,12.));
#72251=CARTESIAN_POINT('Ctrl Pts',(-22.0366423876806,-71.1663065220503,
-5.55111512312578E-16));
#72252=CARTESIAN_POINT('Ctrl Pts',(-22.0366423876806,-71.1663065220503,
3.99999999999999));
#72253=CARTESIAN_POINT('Ctrl Pts',(-22.0366423876807,-71.1663065220504,
8.00000000000001));
#72254=CARTESIAN_POINT('Ctrl Pts',(-22.0366423876807,-71.1663065220504,
12.));
#72255=CARTESIAN_POINT('Ctrl Pts',(-22.1153394458686,-71.1418425484889,
-5.55111512312578E-16));
#72256=CARTESIAN_POINT('Ctrl Pts',(-22.1153394458686,-71.1418425484889,
4.));
#72257=CARTESIAN_POINT('Ctrl Pts',(-22.1153394458687,-71.141842548489,8.));
#72258=CARTESIAN_POINT('Ctrl Pts',(-22.1153394458687,-71.141842548489,12.));
#72259=CARTESIAN_POINT('',(-21.5904919935066,-70.993479606912,-2.77555756156289E-16));
#72260=CARTESIAN_POINT('',(-22.1153394458687,-71.1418425484891,2.77555756156289E-16));
#72261=CARTESIAN_POINT('Ctrl Pts',(-21.5904919935066,-70.993479606912,0.));
#72262=CARTESIAN_POINT('Ctrl Pts',(-21.6628164325805,-71.0762040404459,
-6.93334779979405E-31));
#72263=CARTESIAN_POINT('Ctrl Pts',(-21.7632265878122,-71.1339043418528,
5.23852944873328E-31));
#72264=CARTESIAN_POINT('Ctrl Pts',(-21.8709478979138,-71.1550826601349,
1.54074395550979E-31));
#72265=CARTESIAN_POINT('Ctrl Pts',(-21.95173888049,-71.1709663988464,9.24446373305873E-32));
#72266=CARTESIAN_POINT('Ctrl Pts',(-22.0366423876806,-71.1663065220503,
-8.32001735975286E-31));
#72267=CARTESIAN_POINT('Ctrl Pts',(-22.1153394458686,-71.1418425484889,
1.69481835106077E-31));
#72268=CARTESIAN_POINT('',(-22.1153394458687,-71.1418425484891,12.));
#72269=CARTESIAN_POINT('Ctrl Pts',(-22.1153394458686,-71.1418425484889,
-5.55111512312578E-16));
#72270=CARTESIAN_POINT('Ctrl Pts',(-22.1153394458686,-71.1418425484889,
4.));
#72271=CARTESIAN_POINT('Ctrl Pts',(-22.1153394458687,-71.141842548489,8.));
#72272=CARTESIAN_POINT('Ctrl Pts',(-22.1153394458687,-71.141842548489,12.));
#72273=CARTESIAN_POINT('',(-21.5904919935066,-70.993479606912,12.));
#72274=CARTESIAN_POINT('Ctrl Pts',(-22.1153394458687,-71.141842548489,12.));
#72275=CARTESIAN_POINT('Ctrl Pts',(-22.0366423876807,-71.1663065220504,
12.));
#72276=CARTESIAN_POINT('Ctrl Pts',(-21.9517388804901,-71.1709663988466,
12.));
#72277=CARTESIAN_POINT('Ctrl Pts',(-21.8709478979138,-71.155082660135,12.));
#72278=CARTESIAN_POINT('Ctrl Pts',(-21.7632265878122,-71.1339043418528,
12.));
#72279=CARTESIAN_POINT('Ctrl Pts',(-21.6628164325805,-71.076204040446,12.));
#72280=CARTESIAN_POINT('Ctrl Pts',(-21.5904919935066,-70.993479606912,12.));
#72281=CARTESIAN_POINT('Ctrl Pts',(-21.5904919935066,-70.993479606912,12.));
#72282=CARTESIAN_POINT('Ctrl Pts',(-21.5904919935066,-70.993479606912,8.));
#72283=CARTESIAN_POINT('Ctrl Pts',(-21.5904919935066,-70.993479606912,4.));
#72284=CARTESIAN_POINT('Ctrl Pts',(-21.5904919935066,-70.993479606912,-5.55111512312578E-16));
#72285=CARTESIAN_POINT('Origin',(-1.12623029467293E-10,-3.57524700084383E-10,
0.));
#72286=CARTESIAN_POINT('Origin',(-1.12623029467293E-10,-3.57524700084383E-10,
12.));
#72287=CARTESIAN_POINT('Origin',(-1.12623029467293E-10,-3.57524700084383E-10,
0.));
#72288=CARTESIAN_POINT('Ctrl Pts',(-28.7877620302392,-68.7132793373328,
0.));
#72289=CARTESIAN_POINT('Ctrl Pts',(-28.7877620302392,-68.7132793373328,
4.));
#72290=CARTESIAN_POINT('Ctrl Pts',(-28.7877620302391,-68.7132793373328,
8.));
#72291=CARTESIAN_POINT('Ctrl Pts',(-28.7877620302391,-68.7132793373328,
12.));
#72292=CARTESIAN_POINT('Ctrl Pts',(-28.8891094745187,-68.6708193334379,
0.));
#72293=CARTESIAN_POINT('Ctrl Pts',(-28.8891094745187,-68.6708193334379,
4.));
#72294=CARTESIAN_POINT('Ctrl Pts',(-28.8891094745187,-68.6708193334379,
8.));
#72295=CARTESIAN_POINT('Ctrl Pts',(-28.8891094745187,-68.6708193334379,
12.));
#72296=CARTESIAN_POINT('Ctrl Pts',(-29.0404604348958,-68.5360395709811,
0.));
#72297=CARTESIAN_POINT('Ctrl Pts',(-29.0404604348958,-68.5360395709811,
4.));
#72298=CARTESIAN_POINT('Ctrl Pts',(-29.0404604348958,-68.5360395709811,
8.));
#72299=CARTESIAN_POINT('Ctrl Pts',(-29.0404604348958,-68.5360395709811,
12.));
#72300=CARTESIAN_POINT('Ctrl Pts',(-29.092780523712,-68.3446561754307,0.));
#72301=CARTESIAN_POINT('Ctrl Pts',(-29.092780523712,-68.3446561754307,4.));
#72302=CARTESIAN_POINT('Ctrl Pts',(-29.0927805237119,-68.3446561754307,
8.));
#72303=CARTESIAN_POINT('Ctrl Pts',(-29.0927805237119,-68.3446561754307,
12.));
#72304=CARTESIAN_POINT('Ctrl Pts',(-29.094452644025,-68.2622612909743,0.));
#72305=CARTESIAN_POINT('Ctrl Pts',(-29.094452644025,-68.2622612909743,4.));
#72306=CARTESIAN_POINT('Ctrl Pts',(-29.0944526440249,-68.2622612909743,
8.));
#72307=CARTESIAN_POINT('Ctrl Pts',(-29.0944526440249,-68.2622612909743,
12.));
#72308=CARTESIAN_POINT('',(-28.7877620302392,-68.7132793373328,0.));
#72309=CARTESIAN_POINT('',(-29.0944526440249,-68.2622612909743,2.77555756156289E-16));
#72310=CARTESIAN_POINT('Ctrl Pts',(-28.7877620302392,-68.7132793373328,
2.08166817117217E-16));
#72311=CARTESIAN_POINT('Ctrl Pts',(-28.8891094745187,-68.6708193334379,
2.08166817117217E-16));
#72312=CARTESIAN_POINT('Ctrl Pts',(-28.9755957375913,-68.5938023263197,
2.08166817117217E-16));
#72313=CARTESIAN_POINT('Ctrl Pts',(-29.029745389542,-68.4983025002322,2.08166817117217E-16));
#72314=CARTESIAN_POINT('Ctrl Pts',(-29.070357628505,-68.4266776306666,2.08166817117217E-16));
#72315=CARTESIAN_POINT('Ctrl Pts',(-29.092780523712,-68.3446561754307,2.08166817117217E-16));
#72316=CARTESIAN_POINT('Ctrl Pts',(-29.094452644025,-68.2622612909743,2.08166817117217E-16));
#72317=CARTESIAN_POINT('',(-29.0944526440249,-68.2622612909743,12.));
#72318=CARTESIAN_POINT('Ctrl Pts',(-29.094452644025,-68.2622612909743,0.));
#72319=CARTESIAN_POINT('Ctrl Pts',(-29.094452644025,-68.2622612909743,4.));
#72320=CARTESIAN_POINT('Ctrl Pts',(-29.0944526440249,-68.2622612909743,
8.));
#72321=CARTESIAN_POINT('Ctrl Pts',(-29.0944526440249,-68.2622612909743,
12.));
#72322=CARTESIAN_POINT('',(-28.7877620302391,-68.7132793373328,12.));
#72323=CARTESIAN_POINT('Ctrl Pts',(-29.0944526440249,-68.2622612909743,
12.));
#72324=CARTESIAN_POINT('Ctrl Pts',(-29.0927805237119,-68.3446561754307,
12.));
#72325=CARTESIAN_POINT('Ctrl Pts',(-29.070357628505,-68.4266776306666,12.));
#72326=CARTESIAN_POINT('Ctrl Pts',(-29.029745389542,-68.4983025002322,12.));
#72327=CARTESIAN_POINT('Ctrl Pts',(-28.9755957375913,-68.5938023263197,
12.));
#72328=CARTESIAN_POINT('Ctrl Pts',(-28.8891094745187,-68.6708193334379,
12.));
#72329=CARTESIAN_POINT('Ctrl Pts',(-28.7877620302391,-68.7132793373328,
12.));
#72330=CARTESIAN_POINT('Ctrl Pts',(-28.7877620302391,-68.7132793373328,
12.));
#72331=CARTESIAN_POINT('Ctrl Pts',(-28.7877620302391,-68.7132793373328,
8.));
#72332=CARTESIAN_POINT('Ctrl Pts',(-28.7877620302392,-68.7132793373328,
4.));
#72333=CARTESIAN_POINT('Ctrl Pts',(-28.7877620302392,-68.7132793373328,
0.));
#72334=CARTESIAN_POINT('Ctrl Pts',(-28.8072485549237,-63.7976679095314,
0.));
#72335=CARTESIAN_POINT('Ctrl Pts',(-28.8072485549237,-63.7976679095314,
12.));
#72336=CARTESIAN_POINT('Ctrl Pts',(-28.8078854475432,-63.8014989507494,
0.));
#72337=CARTESIAN_POINT('Ctrl Pts',(-28.8078854475432,-63.8014989507494,
12.));
#72338=CARTESIAN_POINT('Ctrl Pts',(-28.8091580239553,-63.8091667271231,
0.));
#72339=CARTESIAN_POINT('Ctrl Pts',(-28.8091580239553,-63.8091667271231,
12.));
#72340=CARTESIAN_POINT('Ctrl Pts',(-28.8110632620958,-63.8206854735027,
0.));
#72341=CARTESIAN_POINT('Ctrl Pts',(-28.8110632620958,-63.8206854735027,
12.));
#72342=CARTESIAN_POINT('Ctrl Pts',(-28.8135963263369,-63.8360779669856,
0.));
#72343=CARTESIAN_POINT('Ctrl Pts',(-28.8135963263369,-63.8360779669856,
12.));
#72344=CARTESIAN_POINT('Ctrl Pts',(-28.8167505576681,-63.8553755207486,
0.));
#72345=CARTESIAN_POINT('Ctrl Pts',(-28.8167505576681,-63.8553755207486,
12.));
#72346=CARTESIAN_POINT('Ctrl Pts',(-28.8198926619858,-63.8747299825313,
0.));
#72347=CARTESIAN_POINT('Ctrl Pts',(-28.8198926619858,-63.8747299825313,
12.));
#72348=CARTESIAN_POINT('Ctrl Pts',(-28.823022586318,-63.8941412856923,0.));
#72349=CARTESIAN_POINT('Ctrl Pts',(-28.823022586318,-63.8941412856923,12.));
#72350=CARTESIAN_POINT('Ctrl Pts',(-28.8261402423291,-63.9136093063786,
0.));
#72351=CARTESIAN_POINT('Ctrl Pts',(-28.8261402423291,-63.9136093063786,
12.));
#72352=CARTESIAN_POINT('Ctrl Pts',(-28.8292455077559,-63.9331338646996,
0.));
#72353=CARTESIAN_POINT('Ctrl Pts',(-28.8292455077559,-63.9331338646996,
12.));
#72354=CARTESIAN_POINT('Ctrl Pts',(-28.8323382413789,-63.9527147494423,
0.));
#72355=CARTESIAN_POINT('Ctrl Pts',(-28.8323382413789,-63.9527147494423,
12.));
#72356=CARTESIAN_POINT('Ctrl Pts',(-28.8354182946601,-63.9723517369614,
0.));
#72357=CARTESIAN_POINT('Ctrl Pts',(-28.8354182946601,-63.9723517369614,
12.));
#72358=CARTESIAN_POINT('Ctrl Pts',(-28.8384855243243,-63.9920446117582,
0.));
#72359=CARTESIAN_POINT('Ctrl Pts',(-28.8384855243243,-63.9920446117582,
12.));
#72360=CARTESIAN_POINT('Ctrl Pts',(-28.8415398056428,-64.0117931881298,
0.));
#72361=CARTESIAN_POINT('Ctrl Pts',(-28.8415398056428,-64.0117931881298,
12.));
#72362=CARTESIAN_POINT('Ctrl Pts',(-28.844581028125,-64.0315973031942,0.));
#72363=CARTESIAN_POINT('Ctrl Pts',(-28.844581028125,-64.0315973031942,12.));
#72364=CARTESIAN_POINT('Ctrl Pts',(-28.8476090892232,-64.0514568066637,
0.));
#72365=CARTESIAN_POINT('Ctrl Pts',(-28.8476090892232,-64.0514568066637,
12.));
#72366=CARTESIAN_POINT('Ctrl Pts',(-28.8506238891093,-64.0713715523599,
0.));
#72367=CARTESIAN_POINT('Ctrl Pts',(-28.8506238891093,-64.0713715523599,
12.));
#72368=CARTESIAN_POINT('Ctrl Pts',(-28.8536253241854,-64.0913413876622,
0.));
#72369=CARTESIAN_POINT('Ctrl Pts',(-28.8536253241854,-64.0913413876622,
12.));
#72370=CARTESIAN_POINT('Ctrl Pts',(-28.8566132838179,-64.1113661481965,
0.));
#72371=CARTESIAN_POINT('Ctrl Pts',(-28.8566132838179,-64.1113661481965,
12.));
#72372=CARTESIAN_POINT('Ctrl Pts',(-28.8595876537148,-64.1314456633381,
0.));
#72373=CARTESIAN_POINT('Ctrl Pts',(-28.8595876537148,-64.1314456633381,
12.));
#72374=CARTESIAN_POINT('Ctrl Pts',(-28.8625483180438,-64.1515797596564,
0.));
#72375=CARTESIAN_POINT('Ctrl Pts',(-28.8625483180438,-64.1515797596564,
12.));
#72376=CARTESIAN_POINT('Ctrl Pts',(-28.8654951618649,-64.1717682648685,
0.));
#72377=CARTESIAN_POINT('Ctrl Pts',(-28.8654951618649,-64.1717682648685,
12.));
#72378=CARTESIAN_POINT('Ctrl Pts',(-28.8684280739014,-64.1920110123299,
0.));
#72379=CARTESIAN_POINT('Ctrl Pts',(-28.8684280739014,-64.1920110123299,
12.));
#72380=CARTESIAN_POINT('Ctrl Pts',(-28.8713469464185,-64.2123078408461,
0.));
#72381=CARTESIAN_POINT('Ctrl Pts',(-28.8713469464185,-64.2123078408461,
12.));
#72382=CARTESIAN_POINT('Ctrl Pts',(-28.8742516738947,-64.2326585925252,
0.));
#72383=CARTESIAN_POINT('Ctrl Pts',(-28.8742516738947,-64.2326585925252,
12.));
#72384=CARTESIAN_POINT('Ctrl Pts',(-28.877142152106,-64.2530631112929,0.));
#72385=CARTESIAN_POINT('Ctrl Pts',(-28.877142152106,-64.2530631112929,12.));
#72386=CARTESIAN_POINT('Ctrl Pts',(-28.8800182770065,-64.273521241071,0.));
#72387=CARTESIAN_POINT('Ctrl Pts',(-28.8800182770065,-64.273521241071,12.));
#72388=CARTESIAN_POINT('Ctrl Pts',(-28.882879943794,-64.2940328242521,0.));
#72389=CARTESIAN_POINT('Ctrl Pts',(-28.882879943794,-64.2940328242521,12.));
#72390=CARTESIAN_POINT('Ctrl Pts',(-28.8857270473959,-64.3145977025037,
0.));
#72391=CARTESIAN_POINT('Ctrl Pts',(-28.8857270473959,-64.3145977025037,
12.));
#72392=CARTESIAN_POINT('Ctrl Pts',(-28.8885594828926,-64.3352157174619,
0.));
#72393=CARTESIAN_POINT('Ctrl Pts',(-28.8885594828926,-64.3352157174619,
12.));
#72394=CARTESIAN_POINT('Ctrl Pts',(-28.8913771459323,-64.3558867114076,
0.));
#72395=CARTESIAN_POINT('Ctrl Pts',(-28.8913771459323,-64.3558867114076,
12.));
#72396=CARTESIAN_POINT('Ctrl Pts',(-28.89417993323,-64.3766105280688,0.));
#72397=CARTESIAN_POINT('Ctrl Pts',(-28.89417993323,-64.3766105280688,12.));
#72398=CARTESIAN_POINT('Ctrl Pts',(-28.8969677427504,-64.3973870129169,
0.));
#72399=CARTESIAN_POINT('Ctrl Pts',(-28.8969677427504,-64.3973870129169,
12.));
#72400=CARTESIAN_POINT('Ctrl Pts',(-28.899740473434,-64.4182160127379,0.));
#72401=CARTESIAN_POINT('Ctrl Pts',(-28.899740473434,-64.4182160127379,12.));
#72402=CARTESIAN_POINT('Ctrl Pts',(-28.9024980250307,-64.4390973753634,
0.));
#72403=CARTESIAN_POINT('Ctrl Pts',(-28.9024980250307,-64.4390973753634,
12.));
#72404=CARTESIAN_POINT('Ctrl Pts',(-28.9052402979062,-64.4600309493583,
0.));
#72405=CARTESIAN_POINT('Ctrl Pts',(-28.9052402979062,-64.4600309493583,
12.));
#72406=CARTESIAN_POINT('Ctrl Pts',(-28.9079671928264,-64.4810165836592,
0.));
#72407=CARTESIAN_POINT('Ctrl Pts',(-28.9079671928264,-64.4810165836592,
12.));
#72408=CARTESIAN_POINT('Ctrl Pts',(-28.910678610965,-64.5020541275951,0.));
#72409=CARTESIAN_POINT('Ctrl Pts',(-28.910678610965,-64.5020541275951,12.));
#72410=CARTESIAN_POINT('Ctrl Pts',(-28.9133744539949,-64.523143431047,0.));
#72411=CARTESIAN_POINT('Ctrl Pts',(-28.9133744539949,-64.523143431047,12.));
#72412=CARTESIAN_POINT('Ctrl Pts',(-28.9160546241538,-64.5442843445559,
0.));
#72413=CARTESIAN_POINT('Ctrl Pts',(-28.9160546241538,-64.5442843445559,
12.));
#72414=CARTESIAN_POINT('Ctrl Pts',(-28.9187190243224,-64.5654767194471,
0.));
#72415=CARTESIAN_POINT('Ctrl Pts',(-28.9187190243224,-64.5654767194471,
12.));
#72416=CARTESIAN_POINT('Ctrl Pts',(-28.9213675580985,-64.5867204079426,
0.));
#72417=CARTESIAN_POINT('Ctrl Pts',(-28.9213675580985,-64.5867204079426,
12.));
#72418=CARTESIAN_POINT('Ctrl Pts',(-28.9240001297542,-64.6080152631039,
0.));
#72419=CARTESIAN_POINT('Ctrl Pts',(-28.9240001297542,-64.6080152631039,
12.));
#72420=CARTESIAN_POINT('Ctrl Pts',(-28.9266166441951,-64.629361138774,0.));
#72421=CARTESIAN_POINT('Ctrl Pts',(-28.9266166441951,-64.629361138774,12.));
#72422=CARTESIAN_POINT('Ctrl Pts',(-28.9292170069222,-64.6507578895161,
0.));
#72423=CARTESIAN_POINT('Ctrl Pts',(-28.9292170069222,-64.6507578895161,
12.));
#72424=CARTESIAN_POINT('Ctrl Pts',(-28.9318011239915,-64.672205370541,0.));
#72425=CARTESIAN_POINT('Ctrl Pts',(-28.9318011239915,-64.672205370541,12.));
#72426=CARTESIAN_POINT('Ctrl Pts',(-28.9343689019882,-64.6937034376617,
0.));
#72427=CARTESIAN_POINT('Ctrl Pts',(-28.9343689019882,-64.6937034376617,
12.));
#72428=CARTESIAN_POINT('Ctrl Pts',(-28.9369202480393,-64.715251947329,0.));
#72429=CARTESIAN_POINT('Ctrl Pts',(-28.9369202480393,-64.715251947329,12.));
#72430=CARTESIAN_POINT('Ctrl Pts',(-28.9394550698204,-64.7368507566467,
0.));
#72431=CARTESIAN_POINT('Ctrl Pts',(-28.9394550698204,-64.7368507566467,
12.));
#72432=CARTESIAN_POINT('Ctrl Pts',(-28.9419732755656,-64.758499723388,0.));
#72433=CARTESIAN_POINT('Ctrl Pts',(-28.9419732755656,-64.758499723388,12.));
#72434=CARTESIAN_POINT('Ctrl Pts',(-28.944474774081,-64.7801987060084,0.));
#72435=CARTESIAN_POINT('Ctrl Pts',(-28.944474774081,-64.7801987060084,12.));
#72436=CARTESIAN_POINT('Ctrl Pts',(-28.9469594747432,-64.8019475636442,
0.));
#72437=CARTESIAN_POINT('Ctrl Pts',(-28.9469594747432,-64.8019475636442,
12.));
#72438=CARTESIAN_POINT('Ctrl Pts',(-28.9494272874832,-64.8237461561018,
0.));
#72439=CARTESIAN_POINT('Ctrl Pts',(-28.9494272874832,-64.8237461561018,
12.));
#72440=CARTESIAN_POINT('Ctrl Pts',(-28.9518781227765,-64.8455943438423,
0.));
#72441=CARTESIAN_POINT('Ctrl Pts',(-28.9518781227765,-64.8455943438423,
12.));
#72442=CARTESIAN_POINT('Ctrl Pts',(-28.9543118916328,-64.8674919879648,
0.));
#72443=CARTESIAN_POINT('Ctrl Pts',(-28.9543118916328,-64.8674919879648,
12.));
#72444=CARTESIAN_POINT('Ctrl Pts',(-28.9567285055867,-64.8894389501801,
0.));
#72445=CARTESIAN_POINT('Ctrl Pts',(-28.9567285055867,-64.8894389501801,
12.));
#72446=CARTESIAN_POINT('Ctrl Pts',(-28.9591278766934,-64.9114350928125,
0.));
#72447=CARTESIAN_POINT('Ctrl Pts',(-28.9591278766934,-64.9114350928125,
12.));
#72448=CARTESIAN_POINT('Ctrl Pts',(-28.961509917525,-64.9334802788038,0.));
#72449=CARTESIAN_POINT('Ctrl Pts',(-28.961509917525,-64.9334802788038,12.));
#72450=CARTESIAN_POINT('Ctrl Pts',(-28.9638745411677,-64.9555743717109,
0.));
#72451=CARTESIAN_POINT('Ctrl Pts',(-28.9638745411677,-64.9555743717109,
12.));
#72452=CARTESIAN_POINT('Ctrl Pts',(-28.9662216612217,-64.9777172357027,
0.));
#72453=CARTESIAN_POINT('Ctrl Pts',(-28.9662216612217,-64.9777172357027,
12.));
#72454=CARTESIAN_POINT('Ctrl Pts',(-28.9685511918018,-64.9999087355504,
0.));
#72455=CARTESIAN_POINT('Ctrl Pts',(-28.9685511918018,-64.9999087355504,
12.));
#72456=CARTESIAN_POINT('Ctrl Pts',(-28.97086304753,-65.022148736628,0.));
#72457=CARTESIAN_POINT('Ctrl Pts',(-28.97086304753,-65.022148736628,12.));
#72458=CARTESIAN_POINT('Ctrl Pts',(-28.9731571435283,-65.0444371049082,
0.));
#72459=CARTESIAN_POINT('Ctrl Pts',(-28.9731571435283,-65.0444371049082,
12.));
#72460=CARTESIAN_POINT('Ctrl Pts',(-28.9754333954135,-65.0667737069563,
0.));
#72461=CARTESIAN_POINT('Ctrl Pts',(-28.9754333954135,-65.0667737069563,
12.));
#72462=CARTESIAN_POINT('Ctrl Pts',(-28.9776917192933,-65.0891584099168,
0.));
#72463=CARTESIAN_POINT('Ctrl Pts',(-28.9776917192933,-65.0891584099168,
12.));
#72464=CARTESIAN_POINT('Ctrl Pts',(-28.9799320317641,-65.1115910815037,
0.));
#72465=CARTESIAN_POINT('Ctrl Pts',(-28.9799320317641,-65.1115910815037,
12.));
#72466=CARTESIAN_POINT('Ctrl Pts',(-28.9821542499043,-65.1340715900028,
0.));
#72467=CARTESIAN_POINT('Ctrl Pts',(-28.9821542499043,-65.1340715900028,
12.));
#72468=CARTESIAN_POINT('Ctrl Pts',(-28.9843582912693,-65.1565998042697,
0.));
#72469=CARTESIAN_POINT('Ctrl Pts',(-28.9843582912693,-65.1565998042697,
12.));
#72470=CARTESIAN_POINT('Ctrl Pts',(-28.9865440738884,-65.1791755937256,
0.));
#72471=CARTESIAN_POINT('Ctrl Pts',(-28.9865440738884,-65.1791755937256,
12.));
#72472=CARTESIAN_POINT('Ctrl Pts',(-28.9887115162634,-65.2017988283479,
0.));
#72473=CARTESIAN_POINT('Ctrl Pts',(-28.9887115162634,-65.2017988283479,
12.));
#72474=CARTESIAN_POINT('Ctrl Pts',(-28.9908605373663,-65.2244693786609,
0.));
#72475=CARTESIAN_POINT('Ctrl Pts',(-28.9908605373663,-65.2244693786609,
12.));
#72476=CARTESIAN_POINT('Ctrl Pts',(-28.9929910566325,-65.2471871157397,
0.));
#72477=CARTESIAN_POINT('Ctrl Pts',(-28.9929910566325,-65.2471871157397,
12.));
#72478=CARTESIAN_POINT('Ctrl Pts',(-28.9951029939557,-65.2699519112064,
0.));
#72479=CARTESIAN_POINT('Ctrl Pts',(-28.9951029939557,-65.2699519112064,
12.));
#72480=CARTESIAN_POINT('Ctrl Pts',(-28.9971962696845,-65.2927636372253,
0.));
#72481=CARTESIAN_POINT('Ctrl Pts',(-28.9971962696845,-65.2927636372253,
12.));
#72482=CARTESIAN_POINT('Ctrl Pts',(-28.9992708046212,-65.3156221664916,
0.));
#72483=CARTESIAN_POINT('Ctrl Pts',(-28.9992708046212,-65.3156221664916,
12.));
#72484=CARTESIAN_POINT('Ctrl Pts',(-29.0013265200185,-65.3385273722241,
0.));
#72485=CARTESIAN_POINT('Ctrl Pts',(-29.0013265200185,-65.3385273722241,
12.));
#72486=CARTESIAN_POINT('Ctrl Pts',(-29.003363337573,-65.3614791281692,0.));
#72487=CARTESIAN_POINT('Ctrl Pts',(-29.003363337573,-65.3614791281692,12.));
#72488=CARTESIAN_POINT('Ctrl Pts',(-29.0053811794207,-65.3844773085961,
0.));
#72489=CARTESIAN_POINT('Ctrl Pts',(-29.0053811794207,-65.3844773085961,
12.));
#72490=CARTESIAN_POINT('Ctrl Pts',(-29.0073799681342,-65.4075217882934,
0.));
#72491=CARTESIAN_POINT('Ctrl Pts',(-29.0073799681342,-65.4075217882934,
12.));
#72492=CARTESIAN_POINT('Ctrl Pts',(-29.0093596267216,-65.4306124425562,
0.));
#72493=CARTESIAN_POINT('Ctrl Pts',(-29.0093596267216,-65.4306124425562,
12.));
#72494=CARTESIAN_POINT('Ctrl Pts',(-29.0113200786239,-65.4537491471828,
0.));
#72495=CARTESIAN_POINT('Ctrl Pts',(-29.0113200786239,-65.4537491471828,
12.));
#72496=CARTESIAN_POINT('Ctrl Pts',(-29.013261247709,-65.4769317784789,0.));
#72497=CARTESIAN_POINT('Ctrl Pts',(-29.013261247709,-65.4769317784789,12.));
#72498=CARTESIAN_POINT('Ctrl Pts',(-29.0151830582675,-65.5001602132535,
0.));
#72499=CARTESIAN_POINT('Ctrl Pts',(-29.0151830582675,-65.5001602132535,
12.));
#72500=CARTESIAN_POINT('Ctrl Pts',(-29.0170854350095,-65.5234343288136,
0.));
#72501=CARTESIAN_POINT('Ctrl Pts',(-29.0170854350095,-65.5234343288136,
12.));
#72502=CARTESIAN_POINT('Ctrl Pts',(-29.0189683030642,-65.5467540029514,
0.));
#72503=CARTESIAN_POINT('Ctrl Pts',(-29.0189683030642,-65.5467540029514,
12.));
#72504=CARTESIAN_POINT('Ctrl Pts',(-29.0208315879764,-65.5701191139418,
0.));
#72505=CARTESIAN_POINT('Ctrl Pts',(-29.0208315879764,-65.5701191139418,
12.));
#72506=CARTESIAN_POINT('Ctrl Pts',(-29.0226752157003,-65.5935295405453,
0.));
#72507=CARTESIAN_POINT('Ctrl Pts',(-29.0226752157003,-65.5935295405453,
12.));
#72508=CARTESIAN_POINT('Ctrl Pts',(-29.0244991125959,-65.6169851620046,
0.));
#72509=CARTESIAN_POINT('Ctrl Pts',(-29.0244991125959,-65.6169851620046,
12.));
#72510=CARTESIAN_POINT('Ctrl Pts',(-29.0263032054266,-65.6404858580403,
0.));
#72511=CARTESIAN_POINT('Ctrl Pts',(-29.0263032054266,-65.6404858580403,
12.));
#72512=CARTESIAN_POINT('Ctrl Pts',(-29.0280874213596,-65.6640315088388,
0.));
#72513=CARTESIAN_POINT('Ctrl Pts',(-29.0280874213596,-65.6640315088388,
12.));
#72514=CARTESIAN_POINT('Ctrl Pts',(-29.0298516879612,-65.6876219950493,
0.));
#72515=CARTESIAN_POINT('Ctrl Pts',(-29.0298516879612,-65.6876219950493,
12.));
#72516=CARTESIAN_POINT('Ctrl Pts',(-29.0315959331919,-65.7112571977891,
0.));
#72517=CARTESIAN_POINT('Ctrl Pts',(-29.0315959331919,-65.7112571977891,
12.));
#72518=CARTESIAN_POINT('Ctrl Pts',(-29.0333200854028,-65.7349369986384,
0.));
#72519=CARTESIAN_POINT('Ctrl Pts',(-29.0333200854028,-65.7349369986384,
12.));
#72520=CARTESIAN_POINT('Ctrl Pts',(-29.035024073333,-65.7586612796368,0.));
#72521=CARTESIAN_POINT('Ctrl Pts',(-29.035024073333,-65.7586612796368,12.));
#72522=CARTESIAN_POINT('Ctrl Pts',(-29.0367078261103,-65.7824299232705,
0.));
#72523=CARTESIAN_POINT('Ctrl Pts',(-29.0367078261103,-65.7824299232705,
12.));
#72524=CARTESIAN_POINT('Ctrl Pts',(-29.0383712732469,-65.8062428124713,
0.));
#72525=CARTESIAN_POINT('Ctrl Pts',(-29.0383712732469,-65.8062428124713,
12.));
#72526=CARTESIAN_POINT('Ctrl Pts',(-29.0400143446338,-65.8300998306191,
0.));
#72527=CARTESIAN_POINT('Ctrl Pts',(-29.0400143446338,-65.8300998306191,
12.));
#72528=CARTESIAN_POINT('Ctrl Pts',(-29.0416369705375,-65.854000861539,0.));
#72529=CARTESIAN_POINT('Ctrl Pts',(-29.0416369705375,-65.854000861539,12.));
#72530=CARTESIAN_POINT('Ctrl Pts',(-29.0432390815978,-65.8779457894961,
0.));
#72531=CARTESIAN_POINT('Ctrl Pts',(-29.0432390815978,-65.8779457894961,
12.));
#72532=CARTESIAN_POINT('Ctrl Pts',(-29.0448206088289,-65.9019344991854,
0.));
#72533=CARTESIAN_POINT('Ctrl Pts',(-29.0448206088289,-65.9019344991854,
12.));
#72534=CARTESIAN_POINT('Ctrl Pts',(-29.0463814836157,-65.9259668757306,
0.));
#72535=CARTESIAN_POINT('Ctrl Pts',(-29.0463814836157,-65.9259668757306,
12.));
#72536=CARTESIAN_POINT('Ctrl Pts',(-29.0479216377081,-65.9500428046868,
0.));
#72537=CARTESIAN_POINT('Ctrl Pts',(-29.0479216377081,-65.9500428046868,
12.));
#72538=CARTESIAN_POINT('Ctrl Pts',(-29.0494410032173,-65.9741621720369,
0.));
#72539=CARTESIAN_POINT('Ctrl Pts',(-29.0494410032173,-65.9741621720369,
12.));
#72540=CARTESIAN_POINT('Ctrl Pts',(-29.0509395126143,-65.9983248641879,
0.));
#72541=CARTESIAN_POINT('Ctrl Pts',(-29.0509395126143,-65.9983248641879,
12.));
#72542=CARTESIAN_POINT('Ctrl Pts',(-29.0524170987307,-66.0225307679591,
0.));
#72543=CARTESIAN_POINT('Ctrl Pts',(-29.0524170987307,-66.0225307679591,
12.));
#72544=CARTESIAN_POINT('Ctrl Pts',(-29.0538736947552,-66.0467797705815,
0.));
#72545=CARTESIAN_POINT('Ctrl Pts',(-29.0538736947552,-66.0467797705815,
12.));
#72546=CARTESIAN_POINT('Ctrl Pts',(-29.0553092342279,-66.0710717597009,
0.));
#72547=CARTESIAN_POINT('Ctrl Pts',(-29.0553092342279,-66.0710717597009,
12.));
#72548=CARTESIAN_POINT('Ctrl Pts',(-29.0567236510374,-66.0954066233754,
0.));
#72549=CARTESIAN_POINT('Ctrl Pts',(-29.0567236510374,-66.0954066233754,
12.));
#72550=CARTESIAN_POINT('Ctrl Pts',(-29.058116879419,-66.1197842500711,0.));
#72551=CARTESIAN_POINT('Ctrl Pts',(-29.058116879419,-66.1197842500711,12.));
#72552=CARTESIAN_POINT('Ctrl Pts',(-29.0594888539556,-66.1442045286516,
0.));
#72553=CARTESIAN_POINT('Ctrl Pts',(-29.0594888539556,-66.1442045286516,
12.));
#72554=CARTESIAN_POINT('Ctrl Pts',(-29.0608395095746,-66.1686673483755,
0.));
#72555=CARTESIAN_POINT('Ctrl Pts',(-29.0608395095746,-66.1686673483755,
12.));
#72556=CARTESIAN_POINT('Ctrl Pts',(-29.062168781542,-66.1931725989008,0.));
#72557=CARTESIAN_POINT('Ctrl Pts',(-29.062168781542,-66.1931725989008,12.));
#72558=CARTESIAN_POINT('Ctrl Pts',(-29.0634766054599,-66.2177201702819,
0.));
#72559=CARTESIAN_POINT('Ctrl Pts',(-29.0634766054599,-66.2177201702819,
12.));
#72560=CARTESIAN_POINT('Ctrl Pts',(-29.0647629172645,-66.2423099529668,
0.));
#72561=CARTESIAN_POINT('Ctrl Pts',(-29.0647629172645,-66.2423099529668,
12.));
#72562=CARTESIAN_POINT('Ctrl Pts',(-29.0660276532272,-66.2669418377865,
0.));
#72563=CARTESIAN_POINT('Ctrl Pts',(-29.0660276532272,-66.2669418377865,
12.));
#72564=CARTESIAN_POINT('Ctrl Pts',(-29.0672707499527,-66.2916157159527,
0.));
#72565=CARTESIAN_POINT('Ctrl Pts',(-29.0672707499527,-66.2916157159527,
12.));
#72566=CARTESIAN_POINT('Ctrl Pts',(-29.0684921443718,-66.3163314790607,
0.));
#72567=CARTESIAN_POINT('Ctrl Pts',(-29.0684921443718,-66.3163314790607,
12.));
#72568=CARTESIAN_POINT('Ctrl Pts',(-29.0696917737398,-66.3410890190879,
0.));
#72569=CARTESIAN_POINT('Ctrl Pts',(-29.0696917737398,-66.3410890190879,
12.));
#72570=CARTESIAN_POINT('Ctrl Pts',(-29.0708695756336,-66.3658882283906,
0.));
#72571=CARTESIAN_POINT('Ctrl Pts',(-29.0708695756336,-66.3658882283906,
12.));
#72572=CARTESIAN_POINT('Ctrl Pts',(-29.0720254879535,-66.3907289996942,
0.));
#72573=CARTESIAN_POINT('Ctrl Pts',(-29.0720254879535,-66.3907289996942,
12.));
#72574=CARTESIAN_POINT('Ctrl Pts',(-29.0731594489219,-66.4156112260904,
0.));
#72575=CARTESIAN_POINT('Ctrl Pts',(-29.0731594489219,-66.4156112260904,
12.));
#72576=CARTESIAN_POINT('Ctrl Pts',(-29.0742713970762,-66.4405348010404,
0.));
#72577=CARTESIAN_POINT('Ctrl Pts',(-29.0742713970762,-66.4405348010404,
12.));
#72578=CARTESIAN_POINT('Ctrl Pts',(-29.075361271267,-66.4654996183739,0.));
#72579=CARTESIAN_POINT('Ctrl Pts',(-29.075361271267,-66.4654996183739,12.));
#72580=CARTESIAN_POINT('Ctrl Pts',(-29.0764290106553,-66.4905055722864,
0.));
#72581=CARTESIAN_POINT('Ctrl Pts',(-29.0764290106553,-66.4905055722864,
12.));
#72582=CARTESIAN_POINT('Ctrl Pts',(-29.0774745547146,-66.5155525573308,
0.));
#72583=CARTESIAN_POINT('Ctrl Pts',(-29.0774745547146,-66.5155525573308,
12.));
#72584=CARTESIAN_POINT('Ctrl Pts',(-29.0784978432294,-66.5406404684116,
0.));
#72585=CARTESIAN_POINT('Ctrl Pts',(-29.0784978432294,-66.5406404684116,
12.));
#72586=CARTESIAN_POINT('Ctrl Pts',(-29.0794988162892,-66.5657692007894,
0.));
#72587=CARTESIAN_POINT('Ctrl Pts',(-29.0794988162892,-66.5657692007894,
12.));
#72588=CARTESIAN_POINT('Ctrl Pts',(-29.0804774142852,-66.5909386500796,
0.));
#72589=CARTESIAN_POINT('Ctrl Pts',(-29.0804774142852,-66.5909386500796,
12.));
#72590=CARTESIAN_POINT('Ctrl Pts',(-29.0814335779086,-66.6161487122504,
0.));
#72591=CARTESIAN_POINT('Ctrl Pts',(-29.0814335779086,-66.6161487122504,
12.));
#72592=CARTESIAN_POINT('Ctrl Pts',(-29.0823672481508,-66.6413992836148,
0.));
#72593=CARTESIAN_POINT('Ctrl Pts',(-29.0823672481508,-66.6413992836148,
12.));
#72594=CARTESIAN_POINT('Ctrl Pts',(-29.0832783663049,-66.6666902608246,
0.));
#72595=CARTESIAN_POINT('Ctrl Pts',(-29.0832783663049,-66.6666902608246,
12.));
#72596=CARTESIAN_POINT('Ctrl Pts',(-29.0841668739585,-66.6920215408744,
0.));
#72597=CARTESIAN_POINT('Ctrl Pts',(-29.0841668739585,-66.6920215408744,
12.));
#72598=CARTESIAN_POINT('Ctrl Pts',(-29.0850327129914,-66.7173930211015,
0.));
#72599=CARTESIAN_POINT('Ctrl Pts',(-29.0850327129914,-66.7173930211015,
12.));
#72600=CARTESIAN_POINT('Ctrl Pts',(-29.0858758255729,-66.742804599184,0.));
#72601=CARTESIAN_POINT('Ctrl Pts',(-29.0858758255729,-66.742804599184,12.));
#72602=CARTESIAN_POINT('Ctrl Pts',(-29.086696154163,-66.7682561731348,0.));
#72603=CARTESIAN_POINT('Ctrl Pts',(-29.086696154163,-66.7682561731348,12.));
#72604=CARTESIAN_POINT('Ctrl Pts',(-29.0874936415138,-66.7937476412941,
0.));
#72605=CARTESIAN_POINT('Ctrl Pts',(-29.0874936415138,-66.7937476412941,
12.));
#72606=CARTESIAN_POINT('Ctrl Pts',(-29.0882682306636,-66.8192789023323,
0.));
#72607=CARTESIAN_POINT('Ctrl Pts',(-29.0882682306636,-66.8192789023323,
12.));
#72608=CARTESIAN_POINT('Ctrl Pts',(-29.0890198649327,-66.8448498552508,
0.));
#72609=CARTESIAN_POINT('Ctrl Pts',(-29.0890198649327,-66.8448498552508,
12.));
#72610=CARTESIAN_POINT('Ctrl Pts',(-29.0897484879208,-66.8704603993794,
0.));
#72611=CARTESIAN_POINT('Ctrl Pts',(-29.0897484879208,-66.8704603993794,
12.));
#72612=CARTESIAN_POINT('Ctrl Pts',(-29.0904540435063,-66.8961104343703,
0.));
#72613=CARTESIAN_POINT('Ctrl Pts',(-29.0904540435063,-66.8961104343703,
12.));
#72614=CARTESIAN_POINT('Ctrl Pts',(-29.0911364758484,-66.9217998601881,
0.));
#72615=CARTESIAN_POINT('Ctrl Pts',(-29.0911364758484,-66.9217998601881,
12.));
#72616=CARTESIAN_POINT('Ctrl Pts',(-29.0917957293824,-66.9475285771133,
0.));
#72617=CARTESIAN_POINT('Ctrl Pts',(-29.0917957293824,-66.9475285771133,
12.));
#72618=CARTESIAN_POINT('Ctrl Pts',(-29.092431748817,-66.9732964857467,0.));
#72619=CARTESIAN_POINT('Ctrl Pts',(-29.092431748817,-66.9732964857467,12.));
#72620=CARTESIAN_POINT('Ctrl Pts',(-29.0930444791329,-66.9991034870084,
0.));
#72621=CARTESIAN_POINT('Ctrl Pts',(-29.0930444791329,-66.9991034870084,
12.));
#72622=CARTESIAN_POINT('Ctrl Pts',(-29.0936338655828,-67.0249494821361,
0.));
#72623=CARTESIAN_POINT('Ctrl Pts',(-29.0936338655828,-67.0249494821361,
12.));
#72624=CARTESIAN_POINT('Ctrl Pts',(-29.0941998536958,-67.0508343726771,
0.));
#72625=CARTESIAN_POINT('Ctrl Pts',(-29.0941998536958,-67.0508343726771,
12.));
#72626=CARTESIAN_POINT('Ctrl Pts',(-29.0947423892725,-67.0767580604872,
0.));
#72627=CARTESIAN_POINT('Ctrl Pts',(-29.0947423892725,-67.0767580604872,
12.));
#72628=CARTESIAN_POINT('Ctrl Pts',(-29.0952614183777,-67.1027204477304,
0.));
#72629=CARTESIAN_POINT('Ctrl Pts',(-29.0952614183777,-67.1027204477304,
12.));
#72630=CARTESIAN_POINT('Ctrl Pts',(-29.0957568873358,-67.1287214368743,
0.));
#72631=CARTESIAN_POINT('Ctrl Pts',(-29.0957568873358,-67.1287214368743,
12.));
#72632=CARTESIAN_POINT('Ctrl Pts',(-29.0962287427274,-67.1547609306845,
0.));
#72633=CARTESIAN_POINT('Ctrl Pts',(-29.0962287427274,-67.1547609306845,
12.));
#72634=CARTESIAN_POINT('Ctrl Pts',(-29.0966769313893,-67.1808388322116,
0.));
#72635=CARTESIAN_POINT('Ctrl Pts',(-29.0966769313893,-67.1808388322116,
12.));
#72636=CARTESIAN_POINT('Ctrl Pts',(-29.0971014004135,-67.2069550447895,
0.));
#72637=CARTESIAN_POINT('Ctrl Pts',(-29.0971014004135,-67.2069550447895,
12.));
#72638=CARTESIAN_POINT('Ctrl Pts',(-29.0975020971474,-67.2331094720482,
0.));
#72639=CARTESIAN_POINT('Ctrl Pts',(-29.0975020971474,-67.2331094720482,
12.));
#72640=CARTESIAN_POINT('Ctrl Pts',(-29.0978789691965,-67.2593020179216,
0.));
#72641=CARTESIAN_POINT('Ctrl Pts',(-29.0978789691965,-67.2593020179216,
12.));
#72642=CARTESIAN_POINT('Ctrl Pts',(-29.0982319644277,-67.2855325866516,
0.));
#72643=CARTESIAN_POINT('Ctrl Pts',(-29.0982319644277,-67.2855325866516,
12.));
#72644=CARTESIAN_POINT('Ctrl Pts',(-29.0985610309768,-67.311801082791,0.));
#72645=CARTESIAN_POINT('Ctrl Pts',(-29.0985610309768,-67.311801082791,12.));
#72646=CARTESIAN_POINT('Ctrl Pts',(-29.0988661172526,-67.3381074112013,
0.));
#72647=CARTESIAN_POINT('Ctrl Pts',(-29.0988661172526,-67.3381074112013,
12.));
#72648=CARTESIAN_POINT('Ctrl Pts',(-29.0991471719172,-67.3644514770373,
0.));
#72649=CARTESIAN_POINT('Ctrl Pts',(-29.0991471719172,-67.3644514770373,
12.));
#72650=CARTESIAN_POINT('Ctrl Pts',(-29.0994041438715,-67.3908331857313,
0.));
#72651=CARTESIAN_POINT('Ctrl Pts',(-29.0994041438715,-67.3908331857313,
12.));
#72652=CARTESIAN_POINT('Ctrl Pts',(-29.0996369822418,-67.4172524429726,
0.));
#72653=CARTESIAN_POINT('Ctrl Pts',(-29.0996369822418,-67.4172524429726,
12.));
#72654=CARTESIAN_POINT('Ctrl Pts',(-29.0998456363687,-67.4437091546869,
0.));
#72655=CARTESIAN_POINT('Ctrl Pts',(-29.0998456363687,-67.4437091546869,
12.));
#72656=CARTESIAN_POINT('Ctrl Pts',(-29.1000300557961,-67.4702032270062,
0.));
#72657=CARTESIAN_POINT('Ctrl Pts',(-29.1000300557961,-67.4702032270062,
12.));
#72658=CARTESIAN_POINT('Ctrl Pts',(-29.1001901902915,-67.496734566311,0.));
#72659=CARTESIAN_POINT('Ctrl Pts',(-29.1001901902915,-67.496734566311,12.));
#72660=CARTESIAN_POINT('Ctrl Pts',(-29.1003259898686,-67.5233030792714,
0.));
#72661=CARTESIAN_POINT('Ctrl Pts',(-29.1003259898686,-67.5233030792714,
12.));
#72662=CARTESIAN_POINT('Ctrl Pts',(-29.1004374048149,-67.5499086728891,
0.));
#72663=CARTESIAN_POINT('Ctrl Pts',(-29.1004374048149,-67.5499086728891,
12.));
#72664=CARTESIAN_POINT('Ctrl Pts',(-29.1005243857137,-67.5765512545276,
0.));
#72665=CARTESIAN_POINT('Ctrl Pts',(-29.1005243857137,-67.5765512545276,
12.));
#72666=CARTESIAN_POINT('Ctrl Pts',(-29.1005868834863,-67.6032307319614,
0.));
#72667=CARTESIAN_POINT('Ctrl Pts',(-29.1005868834863,-67.6032307319614,
12.));
#72668=CARTESIAN_POINT('Ctrl Pts',(-29.1006248493577,-67.6299470133286,
0.));
#72669=CARTESIAN_POINT('Ctrl Pts',(-29.1006248493577,-67.6299470133286,
12.));
#72670=CARTESIAN_POINT('Ctrl Pts',(-29.1006382347812,-67.6567000070319,
0.));
#72671=CARTESIAN_POINT('Ctrl Pts',(-29.1006382347812,-67.6567000070319,
12.));
#72672=CARTESIAN_POINT('Ctrl Pts',(-29.1006269913747,-67.6834896216458,
0.));
#72673=CARTESIAN_POINT('Ctrl Pts',(-29.1006269913747,-67.6834896216458,
12.));
#72674=CARTESIAN_POINT('Ctrl Pts',(-29.1005910708625,-67.7103157658296,
0.));
#72675=CARTESIAN_POINT('Ctrl Pts',(-29.1005910708625,-67.7103157658296,
12.));
#72676=CARTESIAN_POINT('Ctrl Pts',(-29.1005304249989,-67.7371783482038,
0.));
#72677=CARTESIAN_POINT('Ctrl Pts',(-29.1005304249989,-67.7371783482038,
12.));
#72678=CARTESIAN_POINT('Ctrl Pts',(-29.1004450055647,-67.7640772773397,
0.));
#72679=CARTESIAN_POINT('Ctrl Pts',(-29.1004450055647,-67.7640772773397,
12.));
#72680=CARTESIAN_POINT('Ctrl Pts',(-29.10033476453,-67.7910124620148,0.));
#72681=CARTESIAN_POINT('Ctrl Pts',(-29.10033476453,-67.7910124620148,12.));
#72682=CARTESIAN_POINT('Ctrl Pts',(-29.1001996541847,-67.8179838114109,
0.));
#72683=CARTESIAN_POINT('Ctrl Pts',(-29.1001996541847,-67.8179838114109,
12.));
#72684=CARTESIAN_POINT('Ctrl Pts',(-29.1000396272868,-67.844991235333,0.));
#72685=CARTESIAN_POINT('Ctrl Pts',(-29.1000396272868,-67.844991235333,12.));
#72686=CARTESIAN_POINT('Ctrl Pts',(-29.0998546372027,-67.8720346444111,
0.));
#72687=CARTESIAN_POINT('Ctrl Pts',(-29.0998546372027,-67.8720346444111,
12.));
#72688=CARTESIAN_POINT('Ctrl Pts',(-29.0996446380617,-67.8991139503168,
0.));
#72689=CARTESIAN_POINT('Ctrl Pts',(-29.0996446380617,-67.8991139503168,
12.));
#72690=CARTESIAN_POINT('Ctrl Pts',(-29.0994095844208,-67.9262290652797,
0.));
#72691=CARTESIAN_POINT('Ctrl Pts',(-29.0994095844208,-67.9262290652797,
12.));
#72692=CARTESIAN_POINT('Ctrl Pts',(-29.0991494309395,-67.9533799016122,
0.));
#72693=CARTESIAN_POINT('Ctrl Pts',(-29.0991494309395,-67.9533799016122,
12.));
#72694=CARTESIAN_POINT('Ctrl Pts',(-29.0988641320243,-67.9805663711845,
0.));
#72695=CARTESIAN_POINT('Ctrl Pts',(-29.0988641320243,-67.9805663711845,
12.));
#72696=CARTESIAN_POINT('Ctrl Pts',(-29.0985536415537,-68.0077883850136,
0.));
#72697=CARTESIAN_POINT('Ctrl Pts',(-29.0985536415537,-68.0077883850136,
12.));
#72698=CARTESIAN_POINT('Ctrl Pts',(-29.0982179124113,-68.0350458525589,
0.));
#72699=CARTESIAN_POINT('Ctrl Pts',(-29.0982179124113,-68.0350458525589,
12.));
#72700=CARTESIAN_POINT('Ctrl Pts',(-29.0978568968678,-68.0623386822917,
0.));
#72701=CARTESIAN_POINT('Ctrl Pts',(-29.0978568968678,-68.0623386822917,
12.));
#72702=CARTESIAN_POINT('Ctrl Pts',(-29.0974705474279,-68.089666782962,0.));
#72703=CARTESIAN_POINT('Ctrl Pts',(-29.0974705474279,-68.089666782962,12.));
#72704=CARTESIAN_POINT('Ctrl Pts',(-29.0970588175741,-68.1170300647019,
0.));
#72705=CARTESIAN_POINT('Ctrl Pts',(-29.0970588175741,-68.1170300647019,
12.));
#72706=CARTESIAN_POINT('Ctrl Pts',(-29.0966216624741,-68.1444284400734,
0.));
#72707=CARTESIAN_POINT('Ctrl Pts',(-29.0966216624741,-68.1444284400734,
12.));
#72708=CARTESIAN_POINT('Ctrl Pts',(-29.0961590399023,-68.1718618254221,
0.));
#72709=CARTESIAN_POINT('Ctrl Pts',(-29.0961590399023,-68.1718618254221,
12.));
#72710=CARTESIAN_POINT('Ctrl Pts',(-29.0956709104588,-68.1993301411959,
0.));
#72711=CARTESIAN_POINT('Ctrl Pts',(-29.0956709104588,-68.1993301411959,
12.));
#72712=CARTESIAN_POINT('Ctrl Pts',(-29.0951572355353,-68.22683330895,0.));
#72713=CARTESIAN_POINT('Ctrl Pts',(-29.0951572355353,-68.22683330895,12.));
#72714=CARTESIAN_POINT('Ctrl Pts',(-29.0946179757133,-68.2543712489815,
0.));
#72715=CARTESIAN_POINT('Ctrl Pts',(-29.0946179757133,-68.2543712489815,
12.));
#72716=CARTESIAN_POINT('Ctrl Pts',(-29.0940530889142,-68.2819438775932,
0.));
#72717=CARTESIAN_POINT('Ctrl Pts',(-29.0940530889142,-68.2819438775932,
12.));
#72718=CARTESIAN_POINT('Ctrl Pts',(-29.0934625288442,-68.3095511047852,
0.));
#72719=CARTESIAN_POINT('Ctrl Pts',(-29.0934625288442,-68.3095511047852,
12.));
#72720=CARTESIAN_POINT('Ctrl Pts',(-29.0928462428218,-68.3371928310351,
0.));
#72721=CARTESIAN_POINT('Ctrl Pts',(-29.0928462428218,-68.3371928310351,
12.));
#72722=CARTESIAN_POINT('Ctrl Pts',(-29.0922041749393,-68.3648689519188,
0.));
#72723=CARTESIAN_POINT('Ctrl Pts',(-29.0922041749393,-68.3648689519188,
12.));
#72724=CARTESIAN_POINT('Ctrl Pts',(-29.091536269955,-68.3925793638241,0.));
#72725=CARTESIAN_POINT('Ctrl Pts',(-29.091536269955,-68.3925793638241,12.));
#72726=CARTESIAN_POINT('Ctrl Pts',(-29.0908424770941,-68.4203239694742,
0.));
#72727=CARTESIAN_POINT('Ctrl Pts',(-29.0908424770941,-68.4203239694742,
12.));
#72728=CARTESIAN_POINT('Ctrl Pts',(-29.0901227535274,-68.4481026830845,
0.));
#72729=CARTESIAN_POINT('Ctrl Pts',(-29.0901227535274,-68.4481026830845,
12.));
#72730=CARTESIAN_POINT('Ctrl Pts',(-29.0893770688808,-68.4759154367582,
0.));
#72731=CARTESIAN_POINT('Ctrl Pts',(-29.0893770688808,-68.4759154367582,
12.));
#72732=CARTESIAN_POINT('Ctrl Pts',(-29.0886054060334,-68.5037621823575,
0.));
#72733=CARTESIAN_POINT('Ctrl Pts',(-29.0886054060334,-68.5037621823575,
12.));
#72734=CARTESIAN_POINT('Ctrl Pts',(-29.0878077570819,-68.5316428874729,
0.));
#72735=CARTESIAN_POINT('Ctrl Pts',(-29.0878077570819,-68.5316428874729,
12.));
#72736=CARTESIAN_POINT('Ctrl Pts',(-29.0871488478365,-68.5539746037961,
0.));
#72737=CARTESIAN_POINT('Ctrl Pts',(-29.0871488478365,-68.5539746037961,
12.));
#72738=CARTESIAN_POINT('Ctrl Pts',(-29.0866429721959,-68.5707386600286,
0.));
#72739=CARTESIAN_POINT('Ctrl Pts',(-29.0866429721959,-68.5707386600286,
12.));
#72740=CARTESIAN_POINT('Ctrl Pts',(-29.086300524779,-68.5819214834609,0.));
#72741=CARTESIAN_POINT('Ctrl Pts',(-29.086300524779,-68.5819214834609,12.));
#72742=CARTESIAN_POINT('Ctrl Pts',(-29.086128001823,-68.5875145916629,0.));
#72743=CARTESIAN_POINT('Ctrl Pts',(-29.086128001823,-68.5875145916629,12.));
#72744=CARTESIAN_POINT('',(-28.8072485549237,-63.7976679095314,0.));
#72745=CARTESIAN_POINT('Ctrl Pts',(-28.8072485549237,-63.7976679095314,
0.));
#72746=CARTESIAN_POINT('Ctrl Pts',(-28.8078854475432,-63.8014989507494,
0.));
#72747=CARTESIAN_POINT('Ctrl Pts',(-28.8091580239553,-63.8091667271231,
0.));
#72748=CARTESIAN_POINT('Ctrl Pts',(-28.8110632620958,-63.8206854735027,
0.));
#72749=CARTESIAN_POINT('Ctrl Pts',(-28.8135963263369,-63.8360779669856,
0.));
#72750=CARTESIAN_POINT('Ctrl Pts',(-28.8167505576681,-63.8553755207486,
0.));
#72751=CARTESIAN_POINT('Ctrl Pts',(-28.8198926619858,-63.8747299825313,
0.));
#72752=CARTESIAN_POINT('Ctrl Pts',(-28.823022586318,-63.8941412856923,0.));
#72753=CARTESIAN_POINT('Ctrl Pts',(-28.8261402423291,-63.9136093063786,
0.));
#72754=CARTESIAN_POINT('Ctrl Pts',(-28.8292455077559,-63.9331338646996,
0.));
#72755=CARTESIAN_POINT('Ctrl Pts',(-28.8323382413789,-63.9527147494423,
0.));
#72756=CARTESIAN_POINT('Ctrl Pts',(-28.8354182946601,-63.9723517369614,
0.));
#72757=CARTESIAN_POINT('Ctrl Pts',(-28.8384855243243,-63.9920446117582,
0.));
#72758=CARTESIAN_POINT('Ctrl Pts',(-28.8415398056428,-64.0117931881298,
0.));
#72759=CARTESIAN_POINT('Ctrl Pts',(-28.844581028125,-64.0315973031942,0.));
#72760=CARTESIAN_POINT('Ctrl Pts',(-28.8476090892232,-64.0514568066637,
0.));
#72761=CARTESIAN_POINT('Ctrl Pts',(-28.8506238891093,-64.0713715523599,
0.));
#72762=CARTESIAN_POINT('Ctrl Pts',(-28.8536253241854,-64.0913413876622,
0.));
#72763=CARTESIAN_POINT('Ctrl Pts',(-28.8566132838179,-64.1113661481965,
0.));
#72764=CARTESIAN_POINT('Ctrl Pts',(-28.8595876537148,-64.1314456633381,
0.));
#72765=CARTESIAN_POINT('Ctrl Pts',(-28.8625483180438,-64.1515797596564,
0.));
#72766=CARTESIAN_POINT('Ctrl Pts',(-28.8654951618649,-64.1717682648685,
0.));
#72767=CARTESIAN_POINT('Ctrl Pts',(-28.8684280739014,-64.1920110123299,
0.));
#72768=CARTESIAN_POINT('Ctrl Pts',(-28.8713469464185,-64.2123078408461,
0.));
#72769=CARTESIAN_POINT('Ctrl Pts',(-28.8742516738947,-64.2326585925252,
0.));
#72770=CARTESIAN_POINT('Ctrl Pts',(-28.877142152106,-64.2530631112929,0.));
#72771=CARTESIAN_POINT('Ctrl Pts',(-28.8800182770065,-64.273521241071,0.));
#72772=CARTESIAN_POINT('Ctrl Pts',(-28.882879943794,-64.2940328242521,0.));
#72773=CARTESIAN_POINT('Ctrl Pts',(-28.8857270473959,-64.3145977025037,
0.));
#72774=CARTESIAN_POINT('Ctrl Pts',(-28.8885594828926,-64.3352157174619,
0.));
#72775=CARTESIAN_POINT('Ctrl Pts',(-28.8913771459323,-64.3558867114076,
0.));
#72776=CARTESIAN_POINT('Ctrl Pts',(-28.89417993323,-64.3766105280688,0.));
#72777=CARTESIAN_POINT('Ctrl Pts',(-28.8969677427504,-64.3973870129169,
0.));
#72778=CARTESIAN_POINT('Ctrl Pts',(-28.899740473434,-64.4182160127379,0.));
#72779=CARTESIAN_POINT('Ctrl Pts',(-28.9024980250307,-64.4390973753634,
0.));
#72780=CARTESIAN_POINT('Ctrl Pts',(-28.9052402979062,-64.4600309493583,
0.));
#72781=CARTESIAN_POINT('Ctrl Pts',(-28.9079671928264,-64.4810165836592,
0.));
#72782=CARTESIAN_POINT('Ctrl Pts',(-28.910678610965,-64.5020541275951,0.));
#72783=CARTESIAN_POINT('Ctrl Pts',(-28.9133744539949,-64.523143431047,0.));
#72784=CARTESIAN_POINT('Ctrl Pts',(-28.9160546241538,-64.5442843445559,
0.));
#72785=CARTESIAN_POINT('Ctrl Pts',(-28.9187190243224,-64.5654767194471,
0.));
#72786=CARTESIAN_POINT('Ctrl Pts',(-28.9213675580985,-64.5867204079426,
0.));
#72787=CARTESIAN_POINT('Ctrl Pts',(-28.9240001297542,-64.6080152631039,
0.));
#72788=CARTESIAN_POINT('Ctrl Pts',(-28.9266166441951,-64.629361138774,0.));
#72789=CARTESIAN_POINT('Ctrl Pts',(-28.9292170069222,-64.6507578895161,
0.));
#72790=CARTESIAN_POINT('Ctrl Pts',(-28.9318011239915,-64.672205370541,0.));
#72791=CARTESIAN_POINT('Ctrl Pts',(-28.9343689019882,-64.6937034376617,
0.));
#72792=CARTESIAN_POINT('Ctrl Pts',(-28.9369202480393,-64.715251947329,0.));
#72793=CARTESIAN_POINT('Ctrl Pts',(-28.9394550698204,-64.7368507566467,
0.));
#72794=CARTESIAN_POINT('Ctrl Pts',(-28.9419732755656,-64.758499723388,0.));
#72795=CARTESIAN_POINT('Ctrl Pts',(-28.944474774081,-64.7801987060084,0.));
#72796=CARTESIAN_POINT('Ctrl Pts',(-28.9469594747432,-64.8019475636442,
0.));
#72797=CARTESIAN_POINT('Ctrl Pts',(-28.9494272874832,-64.8237461561018,
0.));
#72798=CARTESIAN_POINT('Ctrl Pts',(-28.9518781227765,-64.8455943438423,
0.));
#72799=CARTESIAN_POINT('Ctrl Pts',(-28.9543118916328,-64.8674919879648,
0.));
#72800=CARTESIAN_POINT('Ctrl Pts',(-28.9567285055867,-64.8894389501801,
0.));
#72801=CARTESIAN_POINT('Ctrl Pts',(-28.9591278766934,-64.9114350928125,
0.));
#72802=CARTESIAN_POINT('Ctrl Pts',(-28.961509917525,-64.9334802788038,0.));
#72803=CARTESIAN_POINT('Ctrl Pts',(-28.9638745411677,-64.9555743717109,
0.));
#72804=CARTESIAN_POINT('Ctrl Pts',(-28.9662216612217,-64.9777172357027,
0.));
#72805=CARTESIAN_POINT('Ctrl Pts',(-28.9685511918018,-64.9999087355504,
0.));
#72806=CARTESIAN_POINT('Ctrl Pts',(-28.97086304753,-65.022148736628,0.));
#72807=CARTESIAN_POINT('Ctrl Pts',(-28.9731571435283,-65.0444371049082,
0.));
#72808=CARTESIAN_POINT('Ctrl Pts',(-28.9754333954135,-65.0667737069563,
0.));
#72809=CARTESIAN_POINT('Ctrl Pts',(-28.9776917192933,-65.0891584099168,
0.));
#72810=CARTESIAN_POINT('Ctrl Pts',(-28.9799320317641,-65.1115910815037,
0.));
#72811=CARTESIAN_POINT('Ctrl Pts',(-28.9821542499043,-65.1340715900028,
0.));
#72812=CARTESIAN_POINT('Ctrl Pts',(-28.9843582912693,-65.1565998042697,
0.));
#72813=CARTESIAN_POINT('Ctrl Pts',(-28.9865440738884,-65.1791755937256,
0.));
#72814=CARTESIAN_POINT('Ctrl Pts',(-28.9887115162634,-65.2017988283479,
0.));
#72815=CARTESIAN_POINT('Ctrl Pts',(-28.9908605373663,-65.2244693786609,
0.));
#72816=CARTESIAN_POINT('Ctrl Pts',(-28.9929910566325,-65.2471871157397,
0.));
#72817=CARTESIAN_POINT('Ctrl Pts',(-28.9951029939557,-65.2699519112064,
0.));
#72818=CARTESIAN_POINT('Ctrl Pts',(-28.9971962696845,-65.2927636372253,
0.));
#72819=CARTESIAN_POINT('Ctrl Pts',(-28.9992708046212,-65.3156221664916,
0.));
#72820=CARTESIAN_POINT('Ctrl Pts',(-29.0013265200185,-65.3385273722241,
0.));
#72821=CARTESIAN_POINT('Ctrl Pts',(-29.003363337573,-65.3614791281692,0.));
#72822=CARTESIAN_POINT('Ctrl Pts',(-29.0053811794207,-65.3844773085961,
0.));
#72823=CARTESIAN_POINT('Ctrl Pts',(-29.0073799681342,-65.4075217882934,
0.));
#72824=CARTESIAN_POINT('Ctrl Pts',(-29.0093596267216,-65.4306124425562,
0.));
#72825=CARTESIAN_POINT('Ctrl Pts',(-29.0113200786239,-65.4537491471828,
0.));
#72826=CARTESIAN_POINT('Ctrl Pts',(-29.013261247709,-65.4769317784789,0.));
#72827=CARTESIAN_POINT('Ctrl Pts',(-29.0151830582675,-65.5001602132535,
0.));
#72828=CARTESIAN_POINT('Ctrl Pts',(-29.0170854350095,-65.5234343288136,
0.));
#72829=CARTESIAN_POINT('Ctrl Pts',(-29.0189683030642,-65.5467540029514,
0.));
#72830=CARTESIAN_POINT('Ctrl Pts',(-29.0208315879764,-65.5701191139418,
0.));
#72831=CARTESIAN_POINT('Ctrl Pts',(-29.0226752157003,-65.5935295405453,
0.));
#72832=CARTESIAN_POINT('Ctrl Pts',(-29.0244991125959,-65.6169851620046,
0.));
#72833=CARTESIAN_POINT('Ctrl Pts',(-29.0263032054266,-65.6404858580403,
0.));
#72834=CARTESIAN_POINT('Ctrl Pts',(-29.0280874213596,-65.6640315088388,
0.));
#72835=CARTESIAN_POINT('Ctrl Pts',(-29.0298516879612,-65.6876219950493,
0.));
#72836=CARTESIAN_POINT('Ctrl Pts',(-29.0315959331919,-65.7112571977891,
0.));
#72837=CARTESIAN_POINT('Ctrl Pts',(-29.0333200854028,-65.7349369986384,
0.));
#72838=CARTESIAN_POINT('Ctrl Pts',(-29.035024073333,-65.7586612796368,0.));
#72839=CARTESIAN_POINT('Ctrl Pts',(-29.0367078261103,-65.7824299232705,
0.));
#72840=CARTESIAN_POINT('Ctrl Pts',(-29.0383712732469,-65.8062428124713,
0.));
#72841=CARTESIAN_POINT('Ctrl Pts',(-29.0400143446338,-65.8300998306191,
0.));
#72842=CARTESIAN_POINT('Ctrl Pts',(-29.0416369705375,-65.854000861539,0.));
#72843=CARTESIAN_POINT('Ctrl Pts',(-29.0432390815978,-65.8779457894961,
0.));
#72844=CARTESIAN_POINT('Ctrl Pts',(-29.0448206088289,-65.9019344991854,
0.));
#72845=CARTESIAN_POINT('Ctrl Pts',(-29.0463814836157,-65.9259668757306,
0.));
#72846=CARTESIAN_POINT('Ctrl Pts',(-29.0479216377081,-65.9500428046868,
0.));
#72847=CARTESIAN_POINT('Ctrl Pts',(-29.0494410032173,-65.9741621720369,
0.));
#72848=CARTESIAN_POINT('Ctrl Pts',(-29.0509395126143,-65.9983248641879,
0.));
#72849=CARTESIAN_POINT('Ctrl Pts',(-29.0524170987307,-66.0225307679591,
0.));
#72850=CARTESIAN_POINT('Ctrl Pts',(-29.0538736947552,-66.0467797705815,
0.));
#72851=CARTESIAN_POINT('Ctrl Pts',(-29.0553092342279,-66.0710717597009,
0.));
#72852=CARTESIAN_POINT('Ctrl Pts',(-29.0567236510374,-66.0954066233754,
0.));
#72853=CARTESIAN_POINT('Ctrl Pts',(-29.058116879419,-66.1197842500711,0.));
#72854=CARTESIAN_POINT('Ctrl Pts',(-29.0594888539556,-66.1442045286516,
0.));
#72855=CARTESIAN_POINT('Ctrl Pts',(-29.0608395095746,-66.1686673483755,
0.));
#72856=CARTESIAN_POINT('Ctrl Pts',(-29.062168781542,-66.1931725989008,0.));
#72857=CARTESIAN_POINT('Ctrl Pts',(-29.0634766054599,-66.2177201702819,
0.));
#72858=CARTESIAN_POINT('Ctrl Pts',(-29.0647629172645,-66.2423099529668,
0.));
#72859=CARTESIAN_POINT('Ctrl Pts',(-29.0660276532272,-66.2669418377865,
0.));
#72860=CARTESIAN_POINT('Ctrl Pts',(-29.0672707499527,-66.2916157159527,
0.));
#72861=CARTESIAN_POINT('Ctrl Pts',(-29.0684921443718,-66.3163314790607,
0.));
#72862=CARTESIAN_POINT('Ctrl Pts',(-29.0696917737398,-66.3410890190879,
0.));
#72863=CARTESIAN_POINT('Ctrl Pts',(-29.0708695756336,-66.3658882283906,
0.));
#72864=CARTESIAN_POINT('Ctrl Pts',(-29.0720254879535,-66.3907289996942,
0.));
#72865=CARTESIAN_POINT('Ctrl Pts',(-29.0731594489219,-66.4156112260904,
0.));
#72866=CARTESIAN_POINT('Ctrl Pts',(-29.0742713970762,-66.4405348010404,
0.));
#72867=CARTESIAN_POINT('Ctrl Pts',(-29.075361271267,-66.4654996183739,0.));
#72868=CARTESIAN_POINT('Ctrl Pts',(-29.0764290106553,-66.4905055722864,
0.));
#72869=CARTESIAN_POINT('Ctrl Pts',(-29.0774745547146,-66.5155525573308,
0.));
#72870=CARTESIAN_POINT('Ctrl Pts',(-29.0784978432294,-66.5406404684116,
0.));
#72871=CARTESIAN_POINT('Ctrl Pts',(-29.0794988162892,-66.5657692007894,
0.));
#72872=CARTESIAN_POINT('Ctrl Pts',(-29.0804774142852,-66.5909386500796,
0.));
#72873=CARTESIAN_POINT('Ctrl Pts',(-29.0814335779086,-66.6161487122504,
0.));
#72874=CARTESIAN_POINT('Ctrl Pts',(-29.0823672481508,-66.6413992836148,
0.));
#72875=CARTESIAN_POINT('Ctrl Pts',(-29.0832783663049,-66.6666902608246,
0.));
#72876=CARTESIAN_POINT('Ctrl Pts',(-29.0841668739585,-66.6920215408744,
0.));
#72877=CARTESIAN_POINT('Ctrl Pts',(-29.0850327129914,-66.7173930211015,
0.));
#72878=CARTESIAN_POINT('Ctrl Pts',(-29.0858758255729,-66.742804599184,0.));
#72879=CARTESIAN_POINT('Ctrl Pts',(-29.086696154163,-66.7682561731348,0.));
#72880=CARTESIAN_POINT('Ctrl Pts',(-29.0874936415138,-66.7937476412941,
0.));
#72881=CARTESIAN_POINT('Ctrl Pts',(-29.0882682306636,-66.8192789023323,
0.));
#72882=CARTESIAN_POINT('Ctrl Pts',(-29.0890198649327,-66.8448498552508,
0.));
#72883=CARTESIAN_POINT('Ctrl Pts',(-29.0897484879208,-66.8704603993794,
0.));
#72884=CARTESIAN_POINT('Ctrl Pts',(-29.0904540435063,-66.8961104343703,
0.));
#72885=CARTESIAN_POINT('Ctrl Pts',(-29.0911364758484,-66.9217998601881,
0.));
#72886=CARTESIAN_POINT('Ctrl Pts',(-29.0917957293824,-66.9475285771133,
0.));
#72887=CARTESIAN_POINT('Ctrl Pts',(-29.092431748817,-66.9732964857467,0.));
#72888=CARTESIAN_POINT('Ctrl Pts',(-29.0930444791329,-66.9991034870084,
0.));
#72889=CARTESIAN_POINT('Ctrl Pts',(-29.0936338655828,-67.0249494821361,
0.));
#72890=CARTESIAN_POINT('Ctrl Pts',(-29.0941998536958,-67.0508343726771,
0.));
#72891=CARTESIAN_POINT('Ctrl Pts',(-29.0947423892725,-67.0767580604872,
0.));
#72892=CARTESIAN_POINT('Ctrl Pts',(-29.0952614183777,-67.1027204477304,
0.));
#72893=CARTESIAN_POINT('Ctrl Pts',(-29.0957568873358,-67.1287214368743,
0.));
#72894=CARTESIAN_POINT('Ctrl Pts',(-29.0962287427274,-67.1547609306845,
0.));
#72895=CARTESIAN_POINT('Ctrl Pts',(-29.0966769313893,-67.1808388322116,
0.));
#72896=CARTESIAN_POINT('Ctrl Pts',(-29.0971014004135,-67.2069550447895,
0.));
#72897=CARTESIAN_POINT('Ctrl Pts',(-29.0975020971474,-67.2331094720482,
0.));
#72898=CARTESIAN_POINT('Ctrl Pts',(-29.0978789691965,-67.2593020179216,
0.));
#72899=CARTESIAN_POINT('Ctrl Pts',(-29.0982319644277,-67.2855325866516,
0.));
#72900=CARTESIAN_POINT('Ctrl Pts',(-29.0985610309768,-67.311801082791,0.));
#72901=CARTESIAN_POINT('Ctrl Pts',(-29.0988661172526,-67.3381074112013,
0.));
#72902=CARTESIAN_POINT('Ctrl Pts',(-29.0991471719172,-67.3644514770373,
0.));
#72903=CARTESIAN_POINT('Ctrl Pts',(-29.0994041438715,-67.3908331857313,
0.));
#72904=CARTESIAN_POINT('Ctrl Pts',(-29.0996369822418,-67.4172524429726,
0.));
#72905=CARTESIAN_POINT('Ctrl Pts',(-29.0998456363687,-67.4437091546869,
0.));
#72906=CARTESIAN_POINT('Ctrl Pts',(-29.1000300557961,-67.4702032270062,
0.));
#72907=CARTESIAN_POINT('Ctrl Pts',(-29.1001901902915,-67.496734566311,0.));
#72908=CARTESIAN_POINT('Ctrl Pts',(-29.1003259898686,-67.5233030792714,
0.));
#72909=CARTESIAN_POINT('Ctrl Pts',(-29.1004374048149,-67.5499086728891,
0.));
#72910=CARTESIAN_POINT('Ctrl Pts',(-29.1005243857137,-67.5765512545276,
0.));
#72911=CARTESIAN_POINT('Ctrl Pts',(-29.1005868834863,-67.6032307319614,
0.));
#72912=CARTESIAN_POINT('Ctrl Pts',(-29.1006248493577,-67.6299470133286,
0.));
#72913=CARTESIAN_POINT('Ctrl Pts',(-29.1006382347812,-67.6567000070319,
0.));
#72914=CARTESIAN_POINT('Ctrl Pts',(-29.1006269913747,-67.6834896216458,
0.));
#72915=CARTESIAN_POINT('Ctrl Pts',(-29.1005910708625,-67.7103157658296,
0.));
#72916=CARTESIAN_POINT('Ctrl Pts',(-29.1005304249989,-67.7371783482038,
0.));
#72917=CARTESIAN_POINT('Ctrl Pts',(-29.1004450055647,-67.7640772773397,
0.));
#72918=CARTESIAN_POINT('Ctrl Pts',(-29.10033476453,-67.7910124620148,0.));
#72919=CARTESIAN_POINT('Ctrl Pts',(-29.1001996541847,-67.8179838114109,
0.));
#72920=CARTESIAN_POINT('Ctrl Pts',(-29.1000396272868,-67.844991235333,0.));
#72921=CARTESIAN_POINT('Ctrl Pts',(-29.0998546372027,-67.8720346444111,
0.));
#72922=CARTESIAN_POINT('Ctrl Pts',(-29.0996446380617,-67.8991139503168,
0.));
#72923=CARTESIAN_POINT('Ctrl Pts',(-29.0994095844208,-67.9262290652797,
0.));
#72924=CARTESIAN_POINT('Ctrl Pts',(-29.0991494309395,-67.9533799016122,
0.));
#72925=CARTESIAN_POINT('Ctrl Pts',(-29.0988641320243,-67.9805663711845,
0.));
#72926=CARTESIAN_POINT('Ctrl Pts',(-29.0985536415537,-68.0077883850136,
0.));
#72927=CARTESIAN_POINT('Ctrl Pts',(-29.0982179124113,-68.0350458525589,
0.));
#72928=CARTESIAN_POINT('Ctrl Pts',(-29.0978568968678,-68.0623386822917,
0.));
#72929=CARTESIAN_POINT('Ctrl Pts',(-29.0974705474279,-68.089666782962,0.));
#72930=CARTESIAN_POINT('Ctrl Pts',(-29.0970588175741,-68.1170300647019,
0.));
#72931=CARTESIAN_POINT('Ctrl Pts',(-29.0966216624741,-68.1444284400734,
0.));
#72932=CARTESIAN_POINT('Ctrl Pts',(-29.0961590399023,-68.1718618254221,
0.));
#72933=CARTESIAN_POINT('Ctrl Pts',(-29.0956709104588,-68.1993301411959,
0.));
#72934=CARTESIAN_POINT('Ctrl Pts',(-29.0952305915108,-68.2229056854495,
0.));
#72935=CARTESIAN_POINT('Ctrl Pts',(-29.0948791947834,-68.2409993689947,
0.));
#72936=CARTESIAN_POINT('Ctrl Pts',(-29.094628043331,-68.2535957746883,0.));
#72937=CARTESIAN_POINT('Ctrl Pts',(-29.0944846386549,-68.2606847334624,
0.));
#72938=CARTESIAN_POINT('Ctrl Pts',(-29.0944526440249,-68.2622612909743,
0.));
#72939=CARTESIAN_POINT('',(-28.8072485549237,-63.7976679095314,12.));
#72940=CARTESIAN_POINT('',(-28.8072485549237,-63.7976679095314,0.));
#72941=CARTESIAN_POINT('Ctrl Pts',(-29.0944526440249,-68.2622612909743,
12.));
#72942=CARTESIAN_POINT('Ctrl Pts',(-29.0944846386549,-68.2606847334624,
12.));
#72943=CARTESIAN_POINT('Ctrl Pts',(-29.094628043331,-68.2535957746883,12.));
#72944=CARTESIAN_POINT('Ctrl Pts',(-29.0948791947834,-68.2409993689947,
12.));
#72945=CARTESIAN_POINT('Ctrl Pts',(-29.0952305915108,-68.2229056854495,
12.));
#72946=CARTESIAN_POINT('Ctrl Pts',(-29.0956709104588,-68.1993301411959,
12.));
#72947=CARTESIAN_POINT('Ctrl Pts',(-29.0961590399023,-68.1718618254221,
12.));
#72948=CARTESIAN_POINT('Ctrl Pts',(-29.0966216624741,-68.1444284400734,
12.));
#72949=CARTESIAN_POINT('Ctrl Pts',(-29.0970588175741,-68.1170300647019,
12.));
#72950=CARTESIAN_POINT('Ctrl Pts',(-29.0974705474279,-68.089666782962,12.));
#72951=CARTESIAN_POINT('Ctrl Pts',(-29.0978568968678,-68.0623386822917,
12.));
#72952=CARTESIAN_POINT('Ctrl Pts',(-29.0982179124113,-68.0350458525589,
12.));
#72953=CARTESIAN_POINT('Ctrl Pts',(-29.0985536415537,-68.0077883850136,
12.));
#72954=CARTESIAN_POINT('Ctrl Pts',(-29.0988641320243,-67.9805663711845,
12.));
#72955=CARTESIAN_POINT('Ctrl Pts',(-29.0991494309395,-67.9533799016122,
12.));
#72956=CARTESIAN_POINT('Ctrl Pts',(-29.0994095844208,-67.9262290652797,
12.));
#72957=CARTESIAN_POINT('Ctrl Pts',(-29.0996446380617,-67.8991139503168,
12.));
#72958=CARTESIAN_POINT('Ctrl Pts',(-29.0998546372027,-67.8720346444111,
12.));
#72959=CARTESIAN_POINT('Ctrl Pts',(-29.1000396272868,-67.844991235333,12.));
#72960=CARTESIAN_POINT('Ctrl Pts',(-29.1001996541847,-67.8179838114109,
12.));
#72961=CARTESIAN_POINT('Ctrl Pts',(-29.10033476453,-67.7910124620148,12.));
#72962=CARTESIAN_POINT('Ctrl Pts',(-29.1004450055647,-67.7640772773397,
12.));
#72963=CARTESIAN_POINT('Ctrl Pts',(-29.1005304249989,-67.7371783482038,
12.));
#72964=CARTESIAN_POINT('Ctrl Pts',(-29.1005910708625,-67.7103157658296,
12.));
#72965=CARTESIAN_POINT('Ctrl Pts',(-29.1006269913747,-67.6834896216458,
12.));
#72966=CARTESIAN_POINT('Ctrl Pts',(-29.1006382347812,-67.6567000070319,
12.));
#72967=CARTESIAN_POINT('Ctrl Pts',(-29.1006248493577,-67.6299470133286,
12.));
#72968=CARTESIAN_POINT('Ctrl Pts',(-29.1005868834863,-67.6032307319614,
12.));
#72969=CARTESIAN_POINT('Ctrl Pts',(-29.1005243857137,-67.5765512545276,
12.));
#72970=CARTESIAN_POINT('Ctrl Pts',(-29.1004374048149,-67.5499086728891,
12.));
#72971=CARTESIAN_POINT('Ctrl Pts',(-29.1003259898686,-67.5233030792714,
12.));
#72972=CARTESIAN_POINT('Ctrl Pts',(-29.1001901902915,-67.496734566311,12.));
#72973=CARTESIAN_POINT('Ctrl Pts',(-29.1000300557961,-67.4702032270062,
12.));
#72974=CARTESIAN_POINT('Ctrl Pts',(-29.0998456363687,-67.4437091546869,
12.));
#72975=CARTESIAN_POINT('Ctrl Pts',(-29.0996369822418,-67.4172524429726,
12.));
#72976=CARTESIAN_POINT('Ctrl Pts',(-29.0994041438715,-67.3908331857313,
12.));
#72977=CARTESIAN_POINT('Ctrl Pts',(-29.0991471719172,-67.3644514770373,
12.));
#72978=CARTESIAN_POINT('Ctrl Pts',(-29.0988661172526,-67.3381074112013,
12.));
#72979=CARTESIAN_POINT('Ctrl Pts',(-29.0985610309768,-67.311801082791,12.));
#72980=CARTESIAN_POINT('Ctrl Pts',(-29.0982319644277,-67.2855325866516,
12.));
#72981=CARTESIAN_POINT('Ctrl Pts',(-29.0978789691965,-67.2593020179216,
12.));
#72982=CARTESIAN_POINT('Ctrl Pts',(-29.0975020971474,-67.2331094720482,
12.));
#72983=CARTESIAN_POINT('Ctrl Pts',(-29.0971014004135,-67.2069550447895,
12.));
#72984=CARTESIAN_POINT('Ctrl Pts',(-29.0966769313893,-67.1808388322116,
12.));
#72985=CARTESIAN_POINT('Ctrl Pts',(-29.0962287427274,-67.1547609306845,
12.));
#72986=CARTESIAN_POINT('Ctrl Pts',(-29.0957568873358,-67.1287214368743,
12.));
#72987=CARTESIAN_POINT('Ctrl Pts',(-29.0952614183777,-67.1027204477304,
12.));
#72988=CARTESIAN_POINT('Ctrl Pts',(-29.0947423892725,-67.0767580604872,
12.));
#72989=CARTESIAN_POINT('Ctrl Pts',(-29.0941998536958,-67.0508343726771,
12.));
#72990=CARTESIAN_POINT('Ctrl Pts',(-29.0936338655828,-67.0249494821361,
12.));
#72991=CARTESIAN_POINT('Ctrl Pts',(-29.0930444791329,-66.9991034870084,
12.));
#72992=CARTESIAN_POINT('Ctrl Pts',(-29.092431748817,-66.9732964857467,12.));
#72993=CARTESIAN_POINT('Ctrl Pts',(-29.0917957293824,-66.9475285771133,
12.));
#72994=CARTESIAN_POINT('Ctrl Pts',(-29.0911364758484,-66.9217998601881,
12.));
#72995=CARTESIAN_POINT('Ctrl Pts',(-29.0904540435063,-66.8961104343703,
12.));
#72996=CARTESIAN_POINT('Ctrl Pts',(-29.0897484879208,-66.8704603993794,
12.));
#72997=CARTESIAN_POINT('Ctrl Pts',(-29.0890198649327,-66.8448498552508,
12.));
#72998=CARTESIAN_POINT('Ctrl Pts',(-29.0882682306636,-66.8192789023323,
12.));
#72999=CARTESIAN_POINT('Ctrl Pts',(-29.0874936415138,-66.7937476412941,
12.));
#73000=CARTESIAN_POINT('Ctrl Pts',(-29.086696154163,-66.7682561731348,12.));
#73001=CARTESIAN_POINT('Ctrl Pts',(-29.0858758255729,-66.742804599184,12.));
#73002=CARTESIAN_POINT('Ctrl Pts',(-29.0850327129914,-66.7173930211015,
12.));
#73003=CARTESIAN_POINT('Ctrl Pts',(-29.0841668739585,-66.6920215408744,
12.));
#73004=CARTESIAN_POINT('Ctrl Pts',(-29.0832783663049,-66.6666902608246,
12.));
#73005=CARTESIAN_POINT('Ctrl Pts',(-29.0823672481508,-66.6413992836148,
12.));
#73006=CARTESIAN_POINT('Ctrl Pts',(-29.0814335779086,-66.6161487122504,
12.));
#73007=CARTESIAN_POINT('Ctrl Pts',(-29.0804774142852,-66.5909386500796,
12.));
#73008=CARTESIAN_POINT('Ctrl Pts',(-29.0794988162892,-66.5657692007894,
12.));
#73009=CARTESIAN_POINT('Ctrl Pts',(-29.0784978432294,-66.5406404684116,
12.));
#73010=CARTESIAN_POINT('Ctrl Pts',(-29.0774745547146,-66.5155525573308,
12.));
#73011=CARTESIAN_POINT('Ctrl Pts',(-29.0764290106553,-66.4905055722864,
12.));
#73012=CARTESIAN_POINT('Ctrl Pts',(-29.075361271267,-66.4654996183739,12.));
#73013=CARTESIAN_POINT('Ctrl Pts',(-29.0742713970762,-66.4405348010404,
12.));
#73014=CARTESIAN_POINT('Ctrl Pts',(-29.0731594489219,-66.4156112260904,
12.));
#73015=CARTESIAN_POINT('Ctrl Pts',(-29.0720254879535,-66.3907289996942,
12.));
#73016=CARTESIAN_POINT('Ctrl Pts',(-29.0708695756336,-66.3658882283906,
12.));
#73017=CARTESIAN_POINT('Ctrl Pts',(-29.0696917737398,-66.3410890190879,
12.));
#73018=CARTESIAN_POINT('Ctrl Pts',(-29.0684921443718,-66.3163314790607,
12.));
#73019=CARTESIAN_POINT('Ctrl Pts',(-29.0672707499527,-66.2916157159527,
12.));
#73020=CARTESIAN_POINT('Ctrl Pts',(-29.0660276532272,-66.2669418377865,
12.));
#73021=CARTESIAN_POINT('Ctrl Pts',(-29.0647629172645,-66.2423099529668,
12.));
#73022=CARTESIAN_POINT('Ctrl Pts',(-29.0634766054599,-66.2177201702819,
12.));
#73023=CARTESIAN_POINT('Ctrl Pts',(-29.062168781542,-66.1931725989008,12.));
#73024=CARTESIAN_POINT('Ctrl Pts',(-29.0608395095746,-66.1686673483755,
12.));
#73025=CARTESIAN_POINT('Ctrl Pts',(-29.0594888539556,-66.1442045286516,
12.));
#73026=CARTESIAN_POINT('Ctrl Pts',(-29.058116879419,-66.1197842500711,12.));
#73027=CARTESIAN_POINT('Ctrl Pts',(-29.0567236510374,-66.0954066233754,
12.));
#73028=CARTESIAN_POINT('Ctrl Pts',(-29.0553092342279,-66.0710717597009,
12.));
#73029=CARTESIAN_POINT('Ctrl Pts',(-29.0538736947552,-66.0467797705815,
12.));
#73030=CARTESIAN_POINT('Ctrl Pts',(-29.0524170987307,-66.0225307679591,
12.));
#73031=CARTESIAN_POINT('Ctrl Pts',(-29.0509395126143,-65.9983248641879,
12.));
#73032=CARTESIAN_POINT('Ctrl Pts',(-29.0494410032173,-65.9741621720369,
12.));
#73033=CARTESIAN_POINT('Ctrl Pts',(-29.0479216377081,-65.9500428046868,
12.));
#73034=CARTESIAN_POINT('Ctrl Pts',(-29.0463814836157,-65.9259668757306,
12.));
#73035=CARTESIAN_POINT('Ctrl Pts',(-29.0448206088289,-65.9019344991854,
12.));
#73036=CARTESIAN_POINT('Ctrl Pts',(-29.0432390815978,-65.8779457894961,
12.));
#73037=CARTESIAN_POINT('Ctrl Pts',(-29.0416369705375,-65.854000861539,12.));
#73038=CARTESIAN_POINT('Ctrl Pts',(-29.0400143446338,-65.8300998306191,
12.));
#73039=CARTESIAN_POINT('Ctrl Pts',(-29.0383712732469,-65.8062428124713,
12.));
#73040=CARTESIAN_POINT('Ctrl Pts',(-29.0367078261103,-65.7824299232705,
12.));
#73041=CARTESIAN_POINT('Ctrl Pts',(-29.035024073333,-65.7586612796368,12.));
#73042=CARTESIAN_POINT('Ctrl Pts',(-29.0333200854028,-65.7349369986384,
12.));
#73043=CARTESIAN_POINT('Ctrl Pts',(-29.0315959331919,-65.7112571977891,
12.));
#73044=CARTESIAN_POINT('Ctrl Pts',(-29.0298516879612,-65.6876219950493,
12.));
#73045=CARTESIAN_POINT('Ctrl Pts',(-29.0280874213596,-65.6640315088388,
12.));
#73046=CARTESIAN_POINT('Ctrl Pts',(-29.0263032054266,-65.6404858580403,
12.));
#73047=CARTESIAN_POINT('Ctrl Pts',(-29.0244991125959,-65.6169851620046,
12.));
#73048=CARTESIAN_POINT('Ctrl Pts',(-29.0226752157003,-65.5935295405453,
12.));
#73049=CARTESIAN_POINT('Ctrl Pts',(-29.0208315879764,-65.5701191139418,
12.));
#73050=CARTESIAN_POINT('Ctrl Pts',(-29.0189683030642,-65.5467540029514,
12.));
#73051=CARTESIAN_POINT('Ctrl Pts',(-29.0170854350095,-65.5234343288136,
12.));
#73052=CARTESIAN_POINT('Ctrl Pts',(-29.0151830582675,-65.5001602132535,
12.));
#73053=CARTESIAN_POINT('Ctrl Pts',(-29.013261247709,-65.4769317784789,12.));
#73054=CARTESIAN_POINT('Ctrl Pts',(-29.0113200786239,-65.4537491471828,
12.));
#73055=CARTESIAN_POINT('Ctrl Pts',(-29.0093596267216,-65.4306124425562,
12.));
#73056=CARTESIAN_POINT('Ctrl Pts',(-29.0073799681342,-65.4075217882934,
12.));
#73057=CARTESIAN_POINT('Ctrl Pts',(-29.0053811794207,-65.3844773085961,
12.));
#73058=CARTESIAN_POINT('Ctrl Pts',(-29.003363337573,-65.3614791281692,12.));
#73059=CARTESIAN_POINT('Ctrl Pts',(-29.0013265200185,-65.3385273722241,
12.));
#73060=CARTESIAN_POINT('Ctrl Pts',(-28.9992708046212,-65.3156221664916,
12.));
#73061=CARTESIAN_POINT('Ctrl Pts',(-28.9971962696845,-65.2927636372253,
12.));
#73062=CARTESIAN_POINT('Ctrl Pts',(-28.9951029939557,-65.2699519112064,
12.));
#73063=CARTESIAN_POINT('Ctrl Pts',(-28.9929910566325,-65.2471871157397,
12.));
#73064=CARTESIAN_POINT('Ctrl Pts',(-28.9908605373663,-65.2244693786609,
12.));
#73065=CARTESIAN_POINT('Ctrl Pts',(-28.9887115162634,-65.2017988283479,
12.));
#73066=CARTESIAN_POINT('Ctrl Pts',(-28.9865440738884,-65.1791755937256,
12.));
#73067=CARTESIAN_POINT('Ctrl Pts',(-28.9843582912693,-65.1565998042697,
12.));
#73068=CARTESIAN_POINT('Ctrl Pts',(-28.9821542499043,-65.1340715900028,
12.));
#73069=CARTESIAN_POINT('Ctrl Pts',(-28.9799320317641,-65.1115910815037,
12.));
#73070=CARTESIAN_POINT('Ctrl Pts',(-28.9776917192933,-65.0891584099168,
12.));
#73071=CARTESIAN_POINT('Ctrl Pts',(-28.9754333954135,-65.0667737069563,
12.));
#73072=CARTESIAN_POINT('Ctrl Pts',(-28.9731571435283,-65.0444371049082,
12.));
#73073=CARTESIAN_POINT('Ctrl Pts',(-28.97086304753,-65.022148736628,12.));
#73074=CARTESIAN_POINT('Ctrl Pts',(-28.9685511918018,-64.9999087355504,
12.));
#73075=CARTESIAN_POINT('Ctrl Pts',(-28.9662216612217,-64.9777172357027,
12.));
#73076=CARTESIAN_POINT('Ctrl Pts',(-28.9638745411677,-64.9555743717109,
12.));
#73077=CARTESIAN_POINT('Ctrl Pts',(-28.961509917525,-64.9334802788038,12.));
#73078=CARTESIAN_POINT('Ctrl Pts',(-28.9591278766934,-64.9114350928125,
12.));
#73079=CARTESIAN_POINT('Ctrl Pts',(-28.9567285055867,-64.8894389501801,
12.));
#73080=CARTESIAN_POINT('Ctrl Pts',(-28.9543118916328,-64.8674919879648,
12.));
#73081=CARTESIAN_POINT('Ctrl Pts',(-28.9518781227765,-64.8455943438423,
12.));
#73082=CARTESIAN_POINT('Ctrl Pts',(-28.9494272874832,-64.8237461561018,
12.));
#73083=CARTESIAN_POINT('Ctrl Pts',(-28.9469594747432,-64.8019475636442,
12.));
#73084=CARTESIAN_POINT('Ctrl Pts',(-28.944474774081,-64.7801987060084,12.));
#73085=CARTESIAN_POINT('Ctrl Pts',(-28.9419732755656,-64.758499723388,12.));
#73086=CARTESIAN_POINT('Ctrl Pts',(-28.9394550698204,-64.7368507566467,
12.));
#73087=CARTESIAN_POINT('Ctrl Pts',(-28.9369202480393,-64.715251947329,12.));
#73088=CARTESIAN_POINT('Ctrl Pts',(-28.9343689019882,-64.6937034376617,
12.));
#73089=CARTESIAN_POINT('Ctrl Pts',(-28.9318011239915,-64.672205370541,12.));
#73090=CARTESIAN_POINT('Ctrl Pts',(-28.9292170069222,-64.6507578895161,
12.));
#73091=CARTESIAN_POINT('Ctrl Pts',(-28.9266166441951,-64.629361138774,12.));
#73092=CARTESIAN_POINT('Ctrl Pts',(-28.9240001297542,-64.6080152631039,
12.));
#73093=CARTESIAN_POINT('Ctrl Pts',(-28.9213675580985,-64.5867204079426,
12.));
#73094=CARTESIAN_POINT('Ctrl Pts',(-28.9187190243224,-64.5654767194471,
12.));
#73095=CARTESIAN_POINT('Ctrl Pts',(-28.9160546241538,-64.5442843445559,
12.));
#73096=CARTESIAN_POINT('Ctrl Pts',(-28.9133744539949,-64.523143431047,12.));
#73097=CARTESIAN_POINT('Ctrl Pts',(-28.910678610965,-64.5020541275951,12.));
#73098=CARTESIAN_POINT('Ctrl Pts',(-28.9079671928264,-64.4810165836592,
12.));
#73099=CARTESIAN_POINT('Ctrl Pts',(-28.9052402979062,-64.4600309493583,
12.));
#73100=CARTESIAN_POINT('Ctrl Pts',(-28.9024980250307,-64.4390973753634,
12.));
#73101=CARTESIAN_POINT('Ctrl Pts',(-28.899740473434,-64.4182160127379,12.));
#73102=CARTESIAN_POINT('Ctrl Pts',(-28.8969677427504,-64.3973870129169,
12.));
#73103=CARTESIAN_POINT('Ctrl Pts',(-28.89417993323,-64.3766105280688,12.));
#73104=CARTESIAN_POINT('Ctrl Pts',(-28.8913771459323,-64.3558867114076,
12.));
#73105=CARTESIAN_POINT('Ctrl Pts',(-28.8885594828926,-64.3352157174619,
12.));
#73106=CARTESIAN_POINT('Ctrl Pts',(-28.8857270473959,-64.3145977025037,
12.));
#73107=CARTESIAN_POINT('Ctrl Pts',(-28.882879943794,-64.2940328242521,12.));
#73108=CARTESIAN_POINT('Ctrl Pts',(-28.8800182770065,-64.273521241071,12.));
#73109=CARTESIAN_POINT('Ctrl Pts',(-28.877142152106,-64.2530631112929,12.));
#73110=CARTESIAN_POINT('Ctrl Pts',(-28.8742516738947,-64.2326585925252,
12.));
#73111=CARTESIAN_POINT('Ctrl Pts',(-28.8713469464185,-64.2123078408461,
12.));
#73112=CARTESIAN_POINT('Ctrl Pts',(-28.8684280739014,-64.1920110123299,
12.));
#73113=CARTESIAN_POINT('Ctrl Pts',(-28.8654951618649,-64.1717682648685,
12.));
#73114=CARTESIAN_POINT('Ctrl Pts',(-28.8625483180438,-64.1515797596564,
12.));
#73115=CARTESIAN_POINT('Ctrl Pts',(-28.8595876537148,-64.1314456633381,
12.));
#73116=CARTESIAN_POINT('Ctrl Pts',(-28.8566132838179,-64.1113661481965,
12.));
#73117=CARTESIAN_POINT('Ctrl Pts',(-28.8536253241854,-64.0913413876622,
12.));
#73118=CARTESIAN_POINT('Ctrl Pts',(-28.8506238891093,-64.0713715523599,
12.));
#73119=CARTESIAN_POINT('Ctrl Pts',(-28.8476090892232,-64.0514568066637,
12.));
#73120=CARTESIAN_POINT('Ctrl Pts',(-28.844581028125,-64.0315973031942,12.));
#73121=CARTESIAN_POINT('Ctrl Pts',(-28.8415398056428,-64.0117931881298,
12.));
#73122=CARTESIAN_POINT('Ctrl Pts',(-28.8384855243243,-63.9920446117582,
12.));
#73123=CARTESIAN_POINT('Ctrl Pts',(-28.8354182946601,-63.9723517369614,
12.));
#73124=CARTESIAN_POINT('Ctrl Pts',(-28.8323382413789,-63.9527147494423,
12.));
#73125=CARTESIAN_POINT('Ctrl Pts',(-28.8292455077559,-63.9331338646996,
12.));
#73126=CARTESIAN_POINT('Ctrl Pts',(-28.8261402423291,-63.9136093063786,
12.));
#73127=CARTESIAN_POINT('Ctrl Pts',(-28.823022586318,-63.8941412856923,12.));
#73128=CARTESIAN_POINT('Ctrl Pts',(-28.8198926619858,-63.8747299825313,
12.));
#73129=CARTESIAN_POINT('Ctrl Pts',(-28.8167505576681,-63.8553755207486,
12.));
#73130=CARTESIAN_POINT('Ctrl Pts',(-28.8135963263369,-63.8360779669856,
12.));
#73131=CARTESIAN_POINT('Ctrl Pts',(-28.8110632620958,-63.8206854735027,
12.));
#73132=CARTESIAN_POINT('Ctrl Pts',(-28.8091580239553,-63.8091667271231,
12.));
#73133=CARTESIAN_POINT('Ctrl Pts',(-28.8078854475432,-63.8014989507494,
12.));
#73134=CARTESIAN_POINT('Ctrl Pts',(-28.8072485549237,-63.7976679095314,
12.));
#73135=CARTESIAN_POINT('Ctrl Pts',(-27.6958230985045,-68.8415926175086,
-5.55111512312578E-16));
#73136=CARTESIAN_POINT('Ctrl Pts',(-27.6958230985045,-68.8415926175086,
4.));
#73137=CARTESIAN_POINT('Ctrl Pts',(-27.6958230985045,-68.8415926175086,
8.));
#73138=CARTESIAN_POINT('Ctrl Pts',(-27.6958230985045,-68.8415926175086,
12.));
#73139=CARTESIAN_POINT('Ctrl Pts',(-27.7750822307004,-68.9176987693915,
-5.55111512312578E-16));
#73140=CARTESIAN_POINT('Ctrl Pts',(-27.7750822307004,-68.9176987693915,
3.99999999999999));
#73141=CARTESIAN_POINT('Ctrl Pts',(-27.7750822307004,-68.9176987693915,
8.));
#73142=CARTESIAN_POINT('Ctrl Pts',(-27.7750822307004,-68.9176987693915,
12.));
#73143=CARTESIAN_POINT('Ctrl Pts',(-27.9589320265198,-69.0029745467578,
-5.55111512312578E-16));
#73144=CARTESIAN_POINT('Ctrl Pts',(-27.9589320265198,-69.0029745467578,
4.00000000000001));
#73145=CARTESIAN_POINT('Ctrl Pts',(-27.9589320265198,-69.0029745467578,
7.99999999999999));
#73146=CARTESIAN_POINT('Ctrl Pts',(-27.9589320265198,-69.0029745467578,
12.));
#73147=CARTESIAN_POINT('Ctrl Pts',(-28.155338613888,-68.9748773050757,-5.55111512312578E-16));
#73148=CARTESIAN_POINT('Ctrl Pts',(-28.155338613888,-68.9748773050757,3.99999999999999));
#73149=CARTESIAN_POINT('Ctrl Pts',(-28.155338613888,-68.9748773050757,8.00000000000001));
#73150=CARTESIAN_POINT('Ctrl Pts',(-28.155338613888,-68.9748773050757,12.));
#73151=CARTESIAN_POINT('Ctrl Pts',(-28.231604030224,-68.9436475237611,-5.55111512312578E-16));
#73152=CARTESIAN_POINT('Ctrl Pts',(-28.231604030224,-68.9436475237611,4.));
#73153=CARTESIAN_POINT('Ctrl Pts',(-28.231604030224,-68.9436475237611,8.));
#73154=CARTESIAN_POINT('Ctrl Pts',(-28.231604030224,-68.9436475237611,12.));
#73155=CARTESIAN_POINT('',(-27.6958230985045,-68.8415926175086,-2.77555756156289E-16));
#73156=CARTESIAN_POINT('',(-28.2316040302241,-68.9436475237613,2.77555756156289E-16));
#73157=CARTESIAN_POINT('Ctrl Pts',(-27.6958230985045,-68.8415926175086,
-5.55111512312578E-16));
#73158=CARTESIAN_POINT('Ctrl Pts',(-27.7750822307004,-68.9176987693915,
-5.55111512312578E-16));
#73159=CARTESIAN_POINT('Ctrl Pts',(-27.8801392568829,-68.9664277850294,
-5.55111512312578E-16));
#73160=CARTESIAN_POINT('Ctrl Pts',(-27.9892964598977,-68.9781370393453,
-5.55111512312578E-16));
#73161=CARTESIAN_POINT('Ctrl Pts',(-28.0711643621588,-68.9869189800823,
-5.55111512312578E-16));
#73162=CARTESIAN_POINT('Ctrl Pts',(-28.155338613888,-68.9748773050757,-5.55111512312578E-16));
#73163=CARTESIAN_POINT('Ctrl Pts',(-28.231604030224,-68.9436475237611,-5.55111512312578E-16));
#73164=CARTESIAN_POINT('',(-28.2316040302241,-68.9436475237613,12.));
#73165=CARTESIAN_POINT('Ctrl Pts',(-28.231604030224,-68.9436475237611,-5.55111512312578E-16));
#73166=CARTESIAN_POINT('Ctrl Pts',(-28.231604030224,-68.9436475237611,4.));
#73167=CARTESIAN_POINT('Ctrl Pts',(-28.231604030224,-68.9436475237611,8.));
#73168=CARTESIAN_POINT('Ctrl Pts',(-28.231604030224,-68.9436475237611,12.));
#73169=CARTESIAN_POINT('',(-27.6958230985045,-68.8415926175086,12.));
#73170=CARTESIAN_POINT('Ctrl Pts',(-28.231604030224,-68.9436475237611,12.));
#73171=CARTESIAN_POINT('Ctrl Pts',(-28.155338613888,-68.9748773050757,12.));
#73172=CARTESIAN_POINT('Ctrl Pts',(-28.0711643621588,-68.9869189800823,
12.));
#73173=CARTESIAN_POINT('Ctrl Pts',(-27.9892964598977,-68.9781370393453,
12.));
#73174=CARTESIAN_POINT('Ctrl Pts',(-27.8801392568829,-68.9664277850294,
12.));
#73175=CARTESIAN_POINT('Ctrl Pts',(-27.7750822307004,-68.9176987693915,
12.));
#73176=CARTESIAN_POINT('Ctrl Pts',(-27.6958230985045,-68.8415926175086,
12.));
#73177=CARTESIAN_POINT('Ctrl Pts',(-27.6958230985045,-68.8415926175086,
12.));
#73178=CARTESIAN_POINT('Ctrl Pts',(-27.6958230985045,-68.8415926175086,
8.));
#73179=CARTESIAN_POINT('Ctrl Pts',(-27.6958230985045,-68.8415926175086,
4.));
#73180=CARTESIAN_POINT('Ctrl Pts',(-27.6958230985045,-68.8415926175086,
-5.55111512312578E-16));
#73181=CARTESIAN_POINT('Origin',(-1.43354795624835E-10,-3.4634846687719E-10,
0.));
#73182=CARTESIAN_POINT('Origin',(-1.43354795624835E-10,-3.4634846687719E-10,
12.));
#73183=CARTESIAN_POINT('Origin',(-1.43354795624835E-10,-3.4634846687719E-10,
0.));
#73184=CARTESIAN_POINT('Ctrl Pts',(-34.6669728017237,-65.9427857825597,
-5.55111512312578E-16));
#73185=CARTESIAN_POINT('Ctrl Pts',(-34.6669728017237,-65.9427857825597,
4.));
#73186=CARTESIAN_POINT('Ctrl Pts',(-34.6669728017237,-65.9427857825597,
8.));
#73187=CARTESIAN_POINT('Ctrl Pts',(-34.6669728017237,-65.9427857825597,
12.));
#73188=CARTESIAN_POINT('Ctrl Pts',(-34.7642339552035,-65.8916543400169,
-5.55111512312578E-16));
#73189=CARTESIAN_POINT('Ctrl Pts',(-34.7642339552035,-65.8916543400169,
4.));
#73190=CARTESIAN_POINT('Ctrl Pts',(-34.7642339552036,-65.8916543400169,
8.));
#73191=CARTESIAN_POINT('Ctrl Pts',(-34.7642339552036,-65.8916543400169,
12.));
#73192=CARTESIAN_POINT('Ctrl Pts',(-34.9032616822024,-65.7441961270804,
-5.55111512312578E-16));
#73193=CARTESIAN_POINT('Ctrl Pts',(-34.9032616822024,-65.7441961270804,
4.));
#73194=CARTESIAN_POINT('Ctrl Pts',(-34.9032616822024,-65.7441961270804,
8.));
#73195=CARTESIAN_POINT('Ctrl Pts',(-34.9032616822024,-65.7441961270804,
12.));
#73196=CARTESIAN_POINT('Ctrl Pts',(-34.9387029822717,-65.5489812297286,
-5.55111512312578E-16));
#73197=CARTESIAN_POINT('Ctrl Pts',(-34.9387029822717,-65.5489812297286,
4.));
#73198=CARTESIAN_POINT('Ctrl Pts',(-34.9387029822717,-65.5489812297286,
8.));
#73199=CARTESIAN_POINT('Ctrl Pts',(-34.9387029822717,-65.5489812297286,
12.));
#73200=CARTESIAN_POINT('Ctrl Pts',(-34.9331875523087,-65.4667541477954,
-5.55111512312578E-16));
#73201=CARTESIAN_POINT('Ctrl Pts',(-34.9331875523087,-65.4667541477954,
4.));
#73202=CARTESIAN_POINT('Ctrl Pts',(-34.9331875523087,-65.4667541477954,
8.));
#73203=CARTESIAN_POINT('Ctrl Pts',(-34.9331875523087,-65.4667541477954,
12.));
#73204=CARTESIAN_POINT('',(-34.6669728017237,-65.9427857825597,0.));
#73205=CARTESIAN_POINT('',(-34.9331875523085,-65.4667541477955,2.77555756156289E-16));
#73206=CARTESIAN_POINT('Ctrl Pts',(-34.6669728017237,-65.9427857825597,
-1.38777878078145E-16));
#73207=CARTESIAN_POINT('Ctrl Pts',(-34.7642339552035,-65.8916543400169,
-1.38777878078145E-16));
#73208=CARTESIAN_POINT('Ctrl Pts',(-34.8436783706315,-65.8073925040532,
-1.38777878078144E-16));
#73209=CARTESIAN_POINT('Ctrl Pts',(-34.8892986466538,-65.7075366486885,
-1.38777878078145E-16));
#73210=CARTESIAN_POINT('Ctrl Pts',(-34.9235138536706,-65.6326447571651,
-1.38777878078145E-16));
#73211=CARTESIAN_POINT('Ctrl Pts',(-34.9387029822717,-65.5489812297286,
-1.38777878078145E-16));
#73212=CARTESIAN_POINT('Ctrl Pts',(-34.9331875523087,-65.4667541477954,
-1.38777878078145E-16));
#73213=CARTESIAN_POINT('',(-34.9331875523085,-65.4667541477955,12.));
#73214=CARTESIAN_POINT('Ctrl Pts',(-34.9331875523087,-65.4667541477954,
-5.55111512312578E-16));
#73215=CARTESIAN_POINT('Ctrl Pts',(-34.9331875523087,-65.4667541477954,
4.));
#73216=CARTESIAN_POINT('Ctrl Pts',(-34.9331875523087,-65.4667541477954,
8.));
#73217=CARTESIAN_POINT('Ctrl Pts',(-34.9331875523087,-65.4667541477954,
12.));
#73218=CARTESIAN_POINT('',(-34.6669728017237,-65.9427857825597,12.));
#73219=CARTESIAN_POINT('Ctrl Pts',(-34.9331875523087,-65.4667541477954,
12.));
#73220=CARTESIAN_POINT('Ctrl Pts',(-34.9387029822717,-65.5489812297286,
12.));
#73221=CARTESIAN_POINT('Ctrl Pts',(-34.9235138536706,-65.6326447571651,
12.));
#73222=CARTESIAN_POINT('Ctrl Pts',(-34.8892986466538,-65.7075366486885,
12.));
#73223=CARTESIAN_POINT('Ctrl Pts',(-34.8436783706315,-65.8073925040532,
12.));
#73224=CARTESIAN_POINT('Ctrl Pts',(-34.7642339552036,-65.8916543400169,
12.));
#73225=CARTESIAN_POINT('Ctrl Pts',(-34.6669728017237,-65.9427857825597,
12.));
#73226=CARTESIAN_POINT('Ctrl Pts',(-34.6669728017237,-65.9427857825597,
12.));
#73227=CARTESIAN_POINT('Ctrl Pts',(-34.6669728017237,-65.9427857825597,
8.));
#73228=CARTESIAN_POINT('Ctrl Pts',(-34.6669728017237,-65.9427857825597,
4.));
#73229=CARTESIAN_POINT('Ctrl Pts',(-34.6669728017237,-65.9427857825597,
-5.55111512312578E-16));
#73230=CARTESIAN_POINT('Ctrl Pts',(-34.2579614092497,-61.0441813777723,
0.));
#73231=CARTESIAN_POINT('Ctrl Pts',(-34.2579614092497,-61.0441813777723,
12.));
#73232=CARTESIAN_POINT('Ctrl Pts',(-34.2589297755434,-61.0479423318725,
0.));
#73233=CARTESIAN_POINT('Ctrl Pts',(-34.2589297755434,-61.0479423318725,
12.));
#73234=CARTESIAN_POINT('Ctrl Pts',(-34.2608658001631,-61.0554700176998,
0.));
#73235=CARTESIAN_POINT('Ctrl Pts',(-34.2608658001631,-61.0554700176998,
12.));
#73236=CARTESIAN_POINT('Ctrl Pts',(-34.2637677131935,-61.0667788793266,
0.));
#73237=CARTESIAN_POINT('Ctrl Pts',(-34.2637677131935,-61.0667788793266,
12.));
#73238=CARTESIAN_POINT('Ctrl Pts',(-34.2676326825626,-61.0818920286293,
0.));
#73239=CARTESIAN_POINT('Ctrl Pts',(-34.2676326825626,-61.0818920286293,
12.));
#73240=CARTESIAN_POINT('Ctrl Pts',(-34.2724568037228,-61.1008412399997,
0.));
#73241=CARTESIAN_POINT('Ctrl Pts',(-34.2724568037228,-61.1008412399997,
12.));
#73242=CARTESIAN_POINT('Ctrl Pts',(-34.2772738038771,-61.1198481997764,
0.));
#73243=CARTESIAN_POINT('Ctrl Pts',(-34.2772738038771,-61.1198481997764,
12.));
#73244=CARTESIAN_POINT('Ctrl Pts',(-34.282083624447,-61.1389128461885,0.));
#73245=CARTESIAN_POINT('Ctrl Pts',(-34.282083624447,-61.1389128461885,12.));
#73246=CARTESIAN_POINT('Ctrl Pts',(-34.2868861666384,-61.1580350635532,
0.));
#73247=CARTESIAN_POINT('Ctrl Pts',(-34.2868861666384,-61.1580350635532,
12.));
#73248=CARTESIAN_POINT('Ctrl Pts',(-34.2916812929751,-61.1772146833205,
0.));
#73249=CARTESIAN_POINT('Ctrl Pts',(-34.2916812929751,-61.1772146833205,
12.));
#73250=CARTESIAN_POINT('Ctrl Pts',(-34.2964688443663,-61.1964515073891,
0.));
#73251=CARTESIAN_POINT('Ctrl Pts',(-34.2964688443663,-61.1964515073891,
12.));
#73252=CARTESIAN_POINT('Ctrl Pts',(-34.3012486533474,-61.2157453259107,
0.));
#73253=CARTESIAN_POINT('Ctrl Pts',(-34.3012486533474,-61.2157453259107,
12.));
#73254=CARTESIAN_POINT('Ctrl Pts',(-34.3060205584065,-61.2350959366939,
0.));
#73255=CARTESIAN_POINT('Ctrl Pts',(-34.3060205584065,-61.2350959366939,
12.));
#73256=CARTESIAN_POINT('Ctrl Pts',(-34.3107844191044,-61.2545031656133,
0.));
#73257=CARTESIAN_POINT('Ctrl Pts',(-34.3107844191044,-61.2545031656133,
12.));
#73258=CARTESIAN_POINT('Ctrl Pts',(-34.3155401111747,-61.2739668600365,
0.));
#73259=CARTESIAN_POINT('Ctrl Pts',(-34.3155401111747,-61.2739668600365,
12.));
#73260=CARTESIAN_POINT('Ctrl Pts',(-34.3202875193618,-61.2934868791854,
0.));
#73261=CARTESIAN_POINT('Ctrl Pts',(-34.3202875193618,-61.2934868791854,
12.));
#73262=CARTESIAN_POINT('Ctrl Pts',(-34.3250265314768,-61.3130630861386,
0.));
#73263=CARTESIAN_POINT('Ctrl Pts',(-34.3250265314768,-61.3130630861386,
12.));
#73264=CARTESIAN_POINT('Ctrl Pts',(-34.3297570310146,-61.3326953378851,
0.));
#73265=CARTESIAN_POINT('Ctrl Pts',(-34.3297570310146,-61.3326953378851,
12.));
#73266=CARTESIAN_POINT('Ctrl Pts',(-34.3344788934363,-61.3523834803188,
0.));
#73267=CARTESIAN_POINT('Ctrl Pts',(-34.3344788934363,-61.3523834803188,
12.));
#73268=CARTESIAN_POINT('Ctrl Pts',(-34.339191990014,-61.3721273534256,0.));
#73269=CARTESIAN_POINT('Ctrl Pts',(-34.339191990014,-61.3721273534256,12.));
#73270=CARTESIAN_POINT('Ctrl Pts',(-34.3438961902405,-61.3919267945302,
0.));
#73271=CARTESIAN_POINT('Ctrl Pts',(-34.3438961902405,-61.3919267945302,
12.));
#73272=CARTESIAN_POINT('Ctrl Pts',(-34.3485913645979,-61.4117816420228,
0.));
#73273=CARTESIAN_POINT('Ctrl Pts',(-34.3485913645979,-61.4117816420228,
12.));
#73274=CARTESIAN_POINT('Ctrl Pts',(-34.3532773877089,-61.4316917395918,
0.));
#73275=CARTESIAN_POINT('Ctrl Pts',(-34.3532773877089,-61.4316917395918,
12.));
#73276=CARTESIAN_POINT('Ctrl Pts',(-34.3579541381996,-61.4516569360454,
0.));
#73277=CARTESIAN_POINT('Ctrl Pts',(-34.3579541381996,-61.4516569360454,
12.));
#73278=CARTESIAN_POINT('Ctrl Pts',(-34.3626214971889,-61.4716770832896,
0.));
#73279=CARTESIAN_POINT('Ctrl Pts',(-34.3626214971889,-61.4716770832896,
12.));
#73280=CARTESIAN_POINT('Ctrl Pts',(-34.3672793472466,-61.4917520349278,
0.));
#73281=CARTESIAN_POINT('Ctrl Pts',(-34.3672793472466,-61.4917520349278,
12.));
#73282=CARTESIAN_POINT('Ctrl Pts',(-34.3719275711195,-61.5118816445437,
0.));
#73283=CARTESIAN_POINT('Ctrl Pts',(-34.3719275711195,-61.5118816445437,
12.));
#73284=CARTESIAN_POINT('Ctrl Pts',(-34.376566050668,-61.5320657642638,0.));
#73285=CARTESIAN_POINT('Ctrl Pts',(-34.376566050668,-61.5320657642638,12.));
#73286=CARTESIAN_POINT('Ctrl Pts',(-34.3811946674197,-61.5523042455158,
0.));
#73287=CARTESIAN_POINT('Ctrl Pts',(-34.3811946674197,-61.5523042455158,
12.));
#73288=CARTESIAN_POINT('Ctrl Pts',(-34.3858133030518,-61.5725969396829,
0.));
#73289=CARTESIAN_POINT('Ctrl Pts',(-34.3858133030518,-61.5725969396829,
12.));
#73290=CARTESIAN_POINT('Ctrl Pts',(-34.3904218398637,-61.5929436987409,
0.));
#73291=CARTESIAN_POINT('Ctrl Pts',(-34.3904218398637,-61.5929436987409,
12.));
#73292=CARTESIAN_POINT('Ctrl Pts',(-34.3950201613432,-61.6133443760142,
0.));
#73293=CARTESIAN_POINT('Ctrl Pts',(-34.3950201613432,-61.6133443760142,
12.));
#73294=CARTESIAN_POINT('Ctrl Pts',(-34.3996081523753,-61.6337988264556,
0.));
#73295=CARTESIAN_POINT('Ctrl Pts',(-34.3996081523753,-61.6337988264556,
12.));
#73296=CARTESIAN_POINT('Ctrl Pts',(-34.4041856989317,-61.6543069062416,
0.));
#73297=CARTESIAN_POINT('Ctrl Pts',(-34.4041856989317,-61.6543069062416,
12.));
#73298=CARTESIAN_POINT('Ctrl Pts',(-34.4087526878812,-61.6748684725205,
0.));
#73299=CARTESIAN_POINT('Ctrl Pts',(-34.4087526878812,-61.6748684725205,
12.));
#73300=CARTESIAN_POINT('Ctrl Pts',(-34.4133090067704,-61.695483383117,0.));
#73301=CARTESIAN_POINT('Ctrl Pts',(-34.4133090067704,-61.695483383117,12.));
#73302=CARTESIAN_POINT('Ctrl Pts',(-34.4178545435767,-61.7161514961914,
0.));
#73303=CARTESIAN_POINT('Ctrl Pts',(-34.4178545435767,-61.7161514961914,
12.));
#73304=CARTESIAN_POINT('Ctrl Pts',(-34.422389186718,-61.7368726702596,0.));
#73305=CARTESIAN_POINT('Ctrl Pts',(-34.422389186718,-61.7368726702596,12.));
#73306=CARTESIAN_POINT('Ctrl Pts',(-34.4269128251577,-61.7576467643432,
0.));
#73307=CARTESIAN_POINT('Ctrl Pts',(-34.4269128251577,-61.7576467643432,
12.));
#73308=CARTESIAN_POINT('Ctrl Pts',(-34.4314253484792,-61.7784736380727,
0.));
#73309=CARTESIAN_POINT('Ctrl Pts',(-34.4314253484792,-61.7784736380727,
12.));
#73310=CARTESIAN_POINT('Ctrl Pts',(-34.4359266469749,-61.7993531518036,
0.));
#73311=CARTESIAN_POINT('Ctrl Pts',(-34.4359266469749,-61.7993531518036,
12.));
#73312=CARTESIAN_POINT('Ctrl Pts',(-34.4404166117299,-61.8202851667222,
0.));
#73313=CARTESIAN_POINT('Ctrl Pts',(-34.4404166117299,-61.8202851667222,
12.));
#73314=CARTESIAN_POINT('Ctrl Pts',(-34.444895134574,-61.8412695447926,0.));
#73315=CARTESIAN_POINT('Ctrl Pts',(-34.444895134574,-61.8412695447926,12.));
#73316=CARTESIAN_POINT('Ctrl Pts',(-34.4493621080361,-61.8623061487018,
0.));
#73317=CARTESIAN_POINT('Ctrl Pts',(-34.4493621080361,-61.8623061487018,
12.));
#73318=CARTESIAN_POINT('Ctrl Pts',(-34.4538174253012,-61.8833948418025,
0.));
#73319=CARTESIAN_POINT('Ctrl Pts',(-34.4538174253012,-61.8833948418025,
12.));
#73320=CARTESIAN_POINT('Ctrl Pts',(-34.4582609801637,-61.9045354880444,
0.));
#73321=CARTESIAN_POINT('Ctrl Pts',(-34.4582609801637,-61.9045354880444,
12.));
#73322=CARTESIAN_POINT('Ctrl Pts',(-34.4626926669975,-61.9257279519308,
0.));
#73323=CARTESIAN_POINT('Ctrl Pts',(-34.4626926669975,-61.9257279519308,
12.));
#73324=CARTESIAN_POINT('Ctrl Pts',(-34.4671123807717,-61.9469720985531,
0.));
#73325=CARTESIAN_POINT('Ctrl Pts',(-34.4671123807717,-61.9469720985531,
12.));
#73326=CARTESIAN_POINT('Ctrl Pts',(-34.4715200170592,-61.9682677936053,
0.));
#73327=CARTESIAN_POINT('Ctrl Pts',(-34.4715200170592,-61.9682677936053,
12.));
#73328=CARTESIAN_POINT('Ctrl Pts',(-34.4759154720473,-61.9896149034001,
0.));
#73329=CARTESIAN_POINT('Ctrl Pts',(-34.4759154720473,-61.9896149034001,
12.));
#73330=CARTESIAN_POINT('Ctrl Pts',(-34.4802986425528,-62.0110132948794,
0.));
#73331=CARTESIAN_POINT('Ctrl Pts',(-34.4802986425528,-62.0110132948794,
12.));
#73332=CARTESIAN_POINT('Ctrl Pts',(-34.48466942602,-62.0324628356141,0.));
#73333=CARTESIAN_POINT('Ctrl Pts',(-34.48466942602,-62.0324628356141,12.));
#73334=CARTESIAN_POINT('Ctrl Pts',(-34.489027720504,-62.0539633937939,0.));
#73335=CARTESIAN_POINT('Ctrl Pts',(-34.489027720504,-62.0539633937939,12.));
#73336=CARTESIAN_POINT('Ctrl Pts',(-34.4933734246593,-62.0755148382135,
0.));
#73337=CARTESIAN_POINT('Ctrl Pts',(-34.4933734246593,-62.0755148382135,
12.));
#73338=CARTESIAN_POINT('Ctrl Pts',(-34.4977064377282,-62.0971170382567,
0.));
#73339=CARTESIAN_POINT('Ctrl Pts',(-34.4977064377282,-62.0971170382567,
12.));
#73340=CARTESIAN_POINT('Ctrl Pts',(-34.5020266595293,-62.1187698638707,
0.));
#73341=CARTESIAN_POINT('Ctrl Pts',(-34.5020266595293,-62.1187698638707,
12.));
#73342=CARTESIAN_POINT('Ctrl Pts',(-34.5063339904533,-62.1404731855687,
0.));
#73343=CARTESIAN_POINT('Ctrl Pts',(-34.5063339904533,-62.1404731855687,
12.));
#73344=CARTESIAN_POINT('Ctrl Pts',(-34.5106283314594,-62.1622268744337,
0.));
#73345=CARTESIAN_POINT('Ctrl Pts',(-34.5106283314594,-62.1622268744337,
12.));
#73346=CARTESIAN_POINT('Ctrl Pts',(-34.514909584073,-62.184030802117,0.));
#73347=CARTESIAN_POINT('Ctrl Pts',(-34.514909584073,-62.184030802117,12.));
#73348=CARTESIAN_POINT('Ctrl Pts',(-34.5191776503843,-62.2058848408346,
0.));
#73349=CARTESIAN_POINT('Ctrl Pts',(-34.5191776503843,-62.2058848408346,
12.));
#73350=CARTESIAN_POINT('Ctrl Pts',(-34.5234324330492,-62.2277888633576,
0.));
#73351=CARTESIAN_POINT('Ctrl Pts',(-34.5234324330492,-62.2277888633576,
12.));
#73352=CARTESIAN_POINT('Ctrl Pts',(-34.527673835281,-62.2497427430136,0.));
#73353=CARTESIAN_POINT('Ctrl Pts',(-34.527673835281,-62.2497427430136,12.));
#73354=CARTESIAN_POINT('Ctrl Pts',(-34.5319017608435,-62.2717463536828,
0.));
#73355=CARTESIAN_POINT('Ctrl Pts',(-34.5319017608435,-62.2717463536828,
12.));
#73356=CARTESIAN_POINT('Ctrl Pts',(-34.536116114045,-62.2937995697927,0.));
#73357=CARTESIAN_POINT('Ctrl Pts',(-34.536116114045,-62.2937995697927,12.));
#73358=CARTESIAN_POINT('Ctrl Pts',(-34.5403167997333,-62.3159022663052,
0.));
#73359=CARTESIAN_POINT('Ctrl Pts',(-34.5403167997333,-62.3159022663052,
12.));
#73360=CARTESIAN_POINT('Ctrl Pts',(-34.5445037232928,-62.3380543187067,
0.));
#73361=CARTESIAN_POINT('Ctrl Pts',(-34.5445037232928,-62.3380543187067,
12.));
#73362=CARTESIAN_POINT('Ctrl Pts',(-34.5486767906376,-62.3602556030114,
0.));
#73363=CARTESIAN_POINT('Ctrl Pts',(-34.5486767906376,-62.3602556030114,
12.));
#73364=CARTESIAN_POINT('Ctrl Pts',(-34.552835908207,-62.3825059957593,0.));
#73365=CARTESIAN_POINT('Ctrl Pts',(-34.552835908207,-62.3825059957593,12.));
#73366=CARTESIAN_POINT('Ctrl Pts',(-34.5569809829615,-62.4048053740129,
0.));
#73367=CARTESIAN_POINT('Ctrl Pts',(-34.5569809829615,-62.4048053740129,
12.));
#73368=CARTESIAN_POINT('Ctrl Pts',(-34.5611119223807,-62.4271536153473,
0.));
#73369=CARTESIAN_POINT('Ctrl Pts',(-34.5611119223807,-62.4271536153473,
12.));
#73370=CARTESIAN_POINT('Ctrl Pts',(-34.5652286344606,-62.4495505978415,
0.));
#73371=CARTESIAN_POINT('Ctrl Pts',(-34.5652286344606,-62.4495505978415,
12.));
#73372=CARTESIAN_POINT('Ctrl Pts',(-34.5693310277064,-62.4719962000829,
0.));
#73373=CARTESIAN_POINT('Ctrl Pts',(-34.5693310277064,-62.4719962000829,
12.));
#73374=CARTESIAN_POINT('Ctrl Pts',(-34.5734190111279,-62.494490301164,0.));
#73375=CARTESIAN_POINT('Ctrl Pts',(-34.5734190111279,-62.494490301164,12.));
#73376=CARTESIAN_POINT('Ctrl Pts',(-34.5774924942351,-62.5170327806774,
0.));
#73377=CARTESIAN_POINT('Ctrl Pts',(-34.5774924942351,-62.5170327806774,
12.));
#73378=CARTESIAN_POINT('Ctrl Pts',(-34.5815513870363,-62.5396235187053,
0.));
#73379=CARTESIAN_POINT('Ctrl Pts',(-34.5815513870363,-62.5396235187053,
12.));
#73380=CARTESIAN_POINT('Ctrl Pts',(-34.5855956000344,-62.5622623958125,
0.));
#73381=CARTESIAN_POINT('Ctrl Pts',(-34.5855956000344,-62.5622623958125,
12.));
#73382=CARTESIAN_POINT('Ctrl Pts',(-34.5896250442199,-62.5849492930501,
0.));
#73383=CARTESIAN_POINT('Ctrl Pts',(-34.5896250442199,-62.5849492930501,
12.));
#73384=CARTESIAN_POINT('Ctrl Pts',(-34.5936396310671,-62.6076840919521,
0.));
#73385=CARTESIAN_POINT('Ctrl Pts',(-34.5936396310671,-62.6076840919521,
12.));
#73386=CARTESIAN_POINT('Ctrl Pts',(-34.5976392725303,-62.6304666745319,
0.));
#73387=CARTESIAN_POINT('Ctrl Pts',(-34.5976392725303,-62.6304666745319,
12.));
#73388=CARTESIAN_POINT('Ctrl Pts',(-34.6016238810419,-62.6532969232695,
0.));
#73389=CARTESIAN_POINT('Ctrl Pts',(-34.6016238810419,-62.6532969232695,
12.));
#73390=CARTESIAN_POINT('Ctrl Pts',(-34.6055933695093,-62.6761747211081,
0.));
#73391=CARTESIAN_POINT('Ctrl Pts',(-34.6055933695093,-62.6761747211081,
12.));
#73392=CARTESIAN_POINT('Ctrl Pts',(-34.6095476513095,-62.6990999514597,
0.));
#73393=CARTESIAN_POINT('Ctrl Pts',(-34.6095476513095,-62.6990999514597,
12.));
#73394=CARTESIAN_POINT('Ctrl Pts',(-34.6134866402842,-62.7220724982005,
0.));
#73395=CARTESIAN_POINT('Ctrl Pts',(-34.6134866402842,-62.7220724982005,
12.));
#73396=CARTESIAN_POINT('Ctrl Pts',(-34.6174102507368,-62.7450922456662,
0.));
#73397=CARTESIAN_POINT('Ctrl Pts',(-34.6174102507368,-62.7450922456662,
12.));
#73398=CARTESIAN_POINT('Ctrl Pts',(-34.6213183974303,-62.7681590786398,
0.));
#73399=CARTESIAN_POINT('Ctrl Pts',(-34.6213183974303,-62.7681590786398,
12.));
#73400=CARTESIAN_POINT('Ctrl Pts',(-34.6252109955836,-62.7912728823482,
0.));
#73401=CARTESIAN_POINT('Ctrl Pts',(-34.6252109955836,-62.7912728823482,
12.));
#73402=CARTESIAN_POINT('Ctrl Pts',(-34.629087960866,-62.8144335424671,0.));
#73403=CARTESIAN_POINT('Ctrl Pts',(-34.629087960866,-62.8144335424671,12.));
#73404=CARTESIAN_POINT('Ctrl Pts',(-34.6329492093932,-62.8376409451167,
0.));
#73405=CARTESIAN_POINT('Ctrl Pts',(-34.6329492093932,-62.8376409451167,
12.));
#73406=CARTESIAN_POINT('Ctrl Pts',(-34.6367946577241,-62.8608949768583,
0.));
#73407=CARTESIAN_POINT('Ctrl Pts',(-34.6367946577241,-62.8608949768583,
12.));
#73408=CARTESIAN_POINT('Ctrl Pts',(-34.6406242228606,-62.8841955246819,
0.));
#73409=CARTESIAN_POINT('Ctrl Pts',(-34.6406242228606,-62.8841955246819,
12.));
#73410=CARTESIAN_POINT('Ctrl Pts',(-34.6444378222425,-62.9075424760042,
0.));
#73411=CARTESIAN_POINT('Ctrl Pts',(-34.6444378222425,-62.9075424760042,
12.));
#73412=CARTESIAN_POINT('Ctrl Pts',(-34.6482353737434,-62.9309357186733,
0.));
#73413=CARTESIAN_POINT('Ctrl Pts',(-34.6482353737434,-62.9309357186733,
12.));
#73414=CARTESIAN_POINT('Ctrl Pts',(-34.6520167956657,-62.9543751409647,
0.));
#73415=CARTESIAN_POINT('Ctrl Pts',(-34.6520167956657,-62.9543751409647,
12.));
#73416=CARTESIAN_POINT('Ctrl Pts',(-34.655782006739,-62.9778606315777,0.));
#73417=CARTESIAN_POINT('Ctrl Pts',(-34.655782006739,-62.9778606315777,12.));
#73418=CARTESIAN_POINT('Ctrl Pts',(-34.6595309261186,-63.0013920796225,
0.));
#73419=CARTESIAN_POINT('Ctrl Pts',(-34.6595309261186,-63.0013920796225,
12.));
#73420=CARTESIAN_POINT('Ctrl Pts',(-34.6632634733819,-63.0249693746198,
0.));
#73421=CARTESIAN_POINT('Ctrl Pts',(-34.6632634733819,-63.0249693746198,
12.));
#73422=CARTESIAN_POINT('Ctrl Pts',(-34.6669795685225,-63.0485924065039,
0.));
#73423=CARTESIAN_POINT('Ctrl Pts',(-34.6669795685225,-63.0485924065039,
12.));
#73424=CARTESIAN_POINT('Ctrl Pts',(-34.6706791319471,-63.0722610656194,
0.));
#73425=CARTESIAN_POINT('Ctrl Pts',(-34.6706791319471,-63.0722610656194,
12.));
#73426=CARTESIAN_POINT('Ctrl Pts',(-34.6743620844722,-63.0959752427169,
0.));
#73427=CARTESIAN_POINT('Ctrl Pts',(-34.6743620844722,-63.0959752427169,
12.));
#73428=CARTESIAN_POINT('Ctrl Pts',(-34.6780283473252,-63.119734828943,0.));
#73429=CARTESIAN_POINT('Ctrl Pts',(-34.6780283473252,-63.119734828943,12.));
#73430=CARTESIAN_POINT('Ctrl Pts',(-34.6816778421401,-63.1435397158385,
0.));
#73431=CARTESIAN_POINT('Ctrl Pts',(-34.6816778421401,-63.1435397158385,
12.));
#73432=CARTESIAN_POINT('Ctrl Pts',(-34.6853104909516,-63.1673897953425,
0.));
#73433=CARTESIAN_POINT('Ctrl Pts',(-34.6853104909516,-63.1673897953425,
12.));
#73434=CARTESIAN_POINT('Ctrl Pts',(-34.6889262161923,-63.1912849597885,
0.));
#73435=CARTESIAN_POINT('Ctrl Pts',(-34.6889262161923,-63.1912849597885,
12.));
#73436=CARTESIAN_POINT('Ctrl Pts',(-34.6925249406899,-63.2152251019014,
0.));
#73437=CARTESIAN_POINT('Ctrl Pts',(-34.6925249406899,-63.2152251019014,
12.));
#73438=CARTESIAN_POINT('Ctrl Pts',(-34.6961065876671,-63.2392101147853,
0.));
#73439=CARTESIAN_POINT('Ctrl Pts',(-34.6961065876671,-63.2392101147853,
12.));
#73440=CARTESIAN_POINT('Ctrl Pts',(-34.6996710807384,-63.2632398919234,
0.));
#73441=CARTESIAN_POINT('Ctrl Pts',(-34.6996710807384,-63.2632398919234,
12.));
#73442=CARTESIAN_POINT('Ctrl Pts',(-34.7032183439045,-63.2873143271812,
0.));
#73443=CARTESIAN_POINT('Ctrl Pts',(-34.7032183439045,-63.2873143271812,
12.));
#73444=CARTESIAN_POINT('Ctrl Pts',(-34.7067483015492,-63.311433314805,0.));
#73445=CARTESIAN_POINT('Ctrl Pts',(-34.7067483015492,-63.311433314805,12.));
#73446=CARTESIAN_POINT('Ctrl Pts',(-34.7102608784373,-63.3355967494169,
0.));
#73447=CARTESIAN_POINT('Ctrl Pts',(-34.7102608784373,-63.3355967494169,
12.));
#73448=CARTESIAN_POINT('Ctrl Pts',(-34.7137559997143,-63.3598045260049,
0.));
#73449=CARTESIAN_POINT('Ctrl Pts',(-34.7137559997143,-63.3598045260049,
12.));
#73450=CARTESIAN_POINT('Ctrl Pts',(-34.7172335909037,-63.3840565399206,
0.));
#73451=CARTESIAN_POINT('Ctrl Pts',(-34.7172335909037,-63.3840565399206,
12.));
#73452=CARTESIAN_POINT('Ctrl Pts',(-34.7206935779007,-63.4083526868837,
0.));
#73453=CARTESIAN_POINT('Ctrl Pts',(-34.7206935779007,-63.4083526868837,
12.));
#73454=CARTESIAN_POINT('Ctrl Pts',(-34.7241358869702,-63.4326928629796,
0.));
#73455=CARTESIAN_POINT('Ctrl Pts',(-34.7241358869702,-63.4326928629796,
12.));
#73456=CARTESIAN_POINT('Ctrl Pts',(-34.7275604447439,-63.4570769646568,
0.));
#73457=CARTESIAN_POINT('Ctrl Pts',(-34.7275604447439,-63.4570769646568,
12.));
#73458=CARTESIAN_POINT('Ctrl Pts',(-34.7309671782212,-63.481504888716,0.));
#73459=CARTESIAN_POINT('Ctrl Pts',(-34.7309671782212,-63.481504888716,12.));
#73460=CARTESIAN_POINT('Ctrl Pts',(-34.7343560147663,-63.5059765323082,
0.));
#73461=CARTESIAN_POINT('Ctrl Pts',(-34.7343560147663,-63.5059765323082,
12.));
#73462=CARTESIAN_POINT('Ctrl Pts',(-34.7377268821022,-63.5304917929378,
0.));
#73463=CARTESIAN_POINT('Ctrl Pts',(-34.7377268821022,-63.5304917929378,
12.));
#73464=CARTESIAN_POINT('Ctrl Pts',(-34.7410797083079,-63.5550505684621,
0.));
#73465=CARTESIAN_POINT('Ctrl Pts',(-34.7410797083079,-63.5550505684621,
12.));
#73466=CARTESIAN_POINT('Ctrl Pts',(-34.7444144218162,-63.5796527570874,
0.));
#73467=CARTESIAN_POINT('Ctrl Pts',(-34.7444144218162,-63.5796527570874,
12.));
#73468=CARTESIAN_POINT('Ctrl Pts',(-34.7477309514142,-63.6042982573598,
0.));
#73469=CARTESIAN_POINT('Ctrl Pts',(-34.7477309514142,-63.6042982573598,
12.));
#73470=CARTESIAN_POINT('Ctrl Pts',(-34.7510292262415,-63.628986968162,0.));
#73471=CARTESIAN_POINT('Ctrl Pts',(-34.7510292262415,-63.628986968162,12.));
#73472=CARTESIAN_POINT('Ctrl Pts',(-34.7543091757842,-63.6537187887174,
0.));
#73473=CARTESIAN_POINT('Ctrl Pts',(-34.7543091757842,-63.6537187887174,
12.));
#73474=CARTESIAN_POINT('Ctrl Pts',(-34.7575707298718,-63.6784936185893,
0.));
#73475=CARTESIAN_POINT('Ctrl Pts',(-34.7575707298718,-63.6784936185893,
12.));
#73476=CARTESIAN_POINT('Ctrl Pts',(-34.7608138186758,-63.7033113576782,
0.));
#73477=CARTESIAN_POINT('Ctrl Pts',(-34.7608138186758,-63.7033113576782,
12.));
#73478=CARTESIAN_POINT('Ctrl Pts',(-34.7640383727094,-63.7281719062135,
0.));
#73479=CARTESIAN_POINT('Ctrl Pts',(-34.7640383727094,-63.7281719062135,
12.));
#73480=CARTESIAN_POINT('Ctrl Pts',(-34.7672443228267,-63.7530751647478,
0.));
#73481=CARTESIAN_POINT('Ctrl Pts',(-34.7672443228267,-63.7530751647478,
12.));
#73482=CARTESIAN_POINT('Ctrl Pts',(-34.7704316002165,-63.7780210341618,
0.));
#73483=CARTESIAN_POINT('Ctrl Pts',(-34.7704316002165,-63.7780210341618,
12.));
#73484=CARTESIAN_POINT('Ctrl Pts',(-34.7736001363991,-63.8030094156635,
0.));
#73485=CARTESIAN_POINT('Ctrl Pts',(-34.7736001363991,-63.8030094156635,
12.));
#73486=CARTESIAN_POINT('Ctrl Pts',(-34.7767498632244,-63.8280402107858,
0.));
#73487=CARTESIAN_POINT('Ctrl Pts',(-34.7767498632244,-63.8280402107858,
12.));
#73488=CARTESIAN_POINT('Ctrl Pts',(-34.7798807128716,-63.8531133213794,
0.));
#73489=CARTESIAN_POINT('Ctrl Pts',(-34.7798807128716,-63.8531133213794,
12.));
#73490=CARTESIAN_POINT('Ctrl Pts',(-34.7829926178495,-63.8782286496059,
0.));
#73491=CARTESIAN_POINT('Ctrl Pts',(-34.7829926178495,-63.8782286496059,
12.));
#73492=CARTESIAN_POINT('Ctrl Pts',(-34.7860855109908,-63.9033860979428,
0.));
#73493=CARTESIAN_POINT('Ctrl Pts',(-34.7860855109908,-63.9033860979428,
12.));
#73494=CARTESIAN_POINT('Ctrl Pts',(-34.7891593254485,-63.9285855691838,
0.));
#73495=CARTESIAN_POINT('Ctrl Pts',(-34.7891593254485,-63.9285855691838,
12.));
#73496=CARTESIAN_POINT('Ctrl Pts',(-34.7922139946943,-63.9538269664365,
0.));
#73497=CARTESIAN_POINT('Ctrl Pts',(-34.7922139946943,-63.9538269664365,
12.));
#73498=CARTESIAN_POINT('Ctrl Pts',(-34.7952494525182,-63.9791101931169,
0.));
#73499=CARTESIAN_POINT('Ctrl Pts',(-34.7952494525182,-63.9791101931169,
12.));
#73500=CARTESIAN_POINT('Ctrl Pts',(-34.79826563303,-64.0044351529413,0.));
#73501=CARTESIAN_POINT('Ctrl Pts',(-34.79826563303,-64.0044351529413,12.));
#73502=CARTESIAN_POINT('Ctrl Pts',(-34.8012624706534,-64.0298017499304,
0.));
#73503=CARTESIAN_POINT('Ctrl Pts',(-34.8012624706534,-64.0298017499304,
12.));
#73504=CARTESIAN_POINT('Ctrl Pts',(-34.8042399001215,-64.05520988841,0.));
#73505=CARTESIAN_POINT('Ctrl Pts',(-34.8042399001215,-64.05520988841,12.));
#73506=CARTESIAN_POINT('Ctrl Pts',(-34.8071978564748,-64.0806594730084,
0.));
#73507=CARTESIAN_POINT('Ctrl Pts',(-34.8071978564748,-64.0806594730084,
12.));
#73508=CARTESIAN_POINT('Ctrl Pts',(-34.8101362750595,-64.1061504086512,
0.));
#73509=CARTESIAN_POINT('Ctrl Pts',(-34.8101362750595,-64.1061504086512,
12.));
#73510=CARTESIAN_POINT('Ctrl Pts',(-34.8130550915284,-64.1316826005502,
0.));
#73511=CARTESIAN_POINT('Ctrl Pts',(-34.8130550915284,-64.1316826005502,
12.));
#73512=CARTESIAN_POINT('Ctrl Pts',(-34.8159542418372,-64.1572559542084,
0.));
#73513=CARTESIAN_POINT('Ctrl Pts',(-34.8159542418372,-64.1572559542084,
12.));
#73514=CARTESIAN_POINT('Ctrl Pts',(-34.8188336622419,-64.1828703754237,
0.));
#73515=CARTESIAN_POINT('Ctrl Pts',(-34.8188336622419,-64.1828703754237,
12.));
#73516=CARTESIAN_POINT('Ctrl Pts',(-34.8216932892969,-64.2085257702885,
0.));
#73517=CARTESIAN_POINT('Ctrl Pts',(-34.8216932892969,-64.2085257702885,
12.));
#73518=CARTESIAN_POINT('Ctrl Pts',(-34.8245330598559,-64.2342220451878,
0.));
#73519=CARTESIAN_POINT('Ctrl Pts',(-34.8245330598559,-64.2342220451878,
12.));
#73520=CARTESIAN_POINT('Ctrl Pts',(-34.8273529110742,-64.259959106791,0.));
#73521=CARTESIAN_POINT('Ctrl Pts',(-34.8273529110742,-64.259959106791,12.));
#73522=CARTESIAN_POINT('Ctrl Pts',(-34.8301527804052,-64.2857368620513,
0.));
#73523=CARTESIAN_POINT('Ctrl Pts',(-34.8301527804052,-64.2857368620513,
12.));
#73524=CARTESIAN_POINT('Ctrl Pts',(-34.8329326055916,-64.3115552182056,
0.));
#73525=CARTESIAN_POINT('Ctrl Pts',(-34.8329326055916,-64.3115552182056,
12.));
#73526=CARTESIAN_POINT('Ctrl Pts',(-34.8356923246617,-64.3374140827708,
0.));
#73527=CARTESIAN_POINT('Ctrl Pts',(-34.8356923246617,-64.3374140827708,
12.));
#73528=CARTESIAN_POINT('Ctrl Pts',(-34.838431875925,-64.3633133635384,0.));
#73529=CARTESIAN_POINT('Ctrl Pts',(-34.838431875925,-64.3633133635384,12.));
#73530=CARTESIAN_POINT('Ctrl Pts',(-34.8411511979705,-64.3892529685614,
0.));
#73531=CARTESIAN_POINT('Ctrl Pts',(-34.8411511979705,-64.3892529685614,
12.));
#73532=CARTESIAN_POINT('Ctrl Pts',(-34.8438502296669,-64.4152328061526,
0.));
#73533=CARTESIAN_POINT('Ctrl Pts',(-34.8438502296669,-64.4152328061526,
12.));
#73534=CARTESIAN_POINT('Ctrl Pts',(-34.8465289101626,-64.4412527848979,
0.));
#73535=CARTESIAN_POINT('Ctrl Pts',(-34.8465289101626,-64.4412527848979,
12.));
#73536=CARTESIAN_POINT('Ctrl Pts',(-34.8491871788899,-64.4673128136631,
0.));
#73537=CARTESIAN_POINT('Ctrl Pts',(-34.8491871788899,-64.4673128136631,
12.));
#73538=CARTESIAN_POINT('Ctrl Pts',(-34.851824975568,-64.4934128015983,0.));
#73539=CARTESIAN_POINT('Ctrl Pts',(-34.851824975568,-64.4934128015983,12.));
#73540=CARTESIAN_POINT('Ctrl Pts',(-34.8544422402114,-64.5195526581398,
0.));
#73541=CARTESIAN_POINT('Ctrl Pts',(-34.8544422402114,-64.5195526581398,
12.));
#73542=CARTESIAN_POINT('Ctrl Pts',(-34.8570389131334,-64.5457322930074,
0.));
#73543=CARTESIAN_POINT('Ctrl Pts',(-34.8570389131334,-64.5457322930074,
12.));
#73544=CARTESIAN_POINT('Ctrl Pts',(-34.8596149349251,-64.5719516161913,
0.));
#73545=CARTESIAN_POINT('Ctrl Pts',(-34.8596149349251,-64.5719516161913,
12.));
#73546=CARTESIAN_POINT('Ctrl Pts',(-34.8621702464397,-64.5982105379374,
0.));
#73547=CARTESIAN_POINT('Ctrl Pts',(-34.8621702464397,-64.5982105379374,
12.));
#73548=CARTESIAN_POINT('Ctrl Pts',(-34.8647047887774,-64.6245089687276,
0.));
#73549=CARTESIAN_POINT('Ctrl Pts',(-34.8647047887774,-64.6245089687276,
12.));
#73550=CARTESIAN_POINT('Ctrl Pts',(-34.8672185032725,-64.6508468192609,
0.));
#73551=CARTESIAN_POINT('Ctrl Pts',(-34.8672185032725,-64.6508468192609,
12.));
#73552=CARTESIAN_POINT('Ctrl Pts',(-34.8697113314797,-64.6772240004241,
0.));
#73553=CARTESIAN_POINT('Ctrl Pts',(-34.8697113314797,-64.6772240004241,
12.));
#73554=CARTESIAN_POINT('Ctrl Pts',(-34.8721832151982,-64.7036404233319,
0.));
#73555=CARTESIAN_POINT('Ctrl Pts',(-34.8721832151982,-64.7036404233319,
12.));
#73556=CARTESIAN_POINT('Ctrl Pts',(-34.8746340964977,-64.7300959993662,
0.));
#73557=CARTESIAN_POINT('Ctrl Pts',(-34.8746340964977,-64.7300959993662,
12.));
#73558=CARTESIAN_POINT('Ctrl Pts',(-34.8770639177494,-64.7565906402153,
0.));
#73559=CARTESIAN_POINT('Ctrl Pts',(-34.8770639177494,-64.7565906402153,
12.));
#73560=CARTESIAN_POINT('Ctrl Pts',(-34.8794726216511,-64.7831242579023,
0.));
#73561=CARTESIAN_POINT('Ctrl Pts',(-34.8794726216511,-64.7831242579023,
12.));
#73562=CARTESIAN_POINT('Ctrl Pts',(-34.8818601512726,-64.8096967648299,
0.));
#73563=CARTESIAN_POINT('Ctrl Pts',(-34.8818601512726,-64.8096967648299,
12.));
#73564=CARTESIAN_POINT('Ctrl Pts',(-34.8842264500184,-64.8363080737369,
0.));
#73565=CARTESIAN_POINT('Ctrl Pts',(-34.8842264500184,-64.8363080737369,
12.));
#73566=CARTESIAN_POINT('Ctrl Pts',(-34.8865714615433,-64.8629580976057,
0.));
#73567=CARTESIAN_POINT('Ctrl Pts',(-34.8865714615433,-64.8629580976057,
12.));
#73568=CARTESIAN_POINT('Ctrl Pts',(-34.888895129681,-64.8896467495754,0.));
#73569=CARTESIAN_POINT('Ctrl Pts',(-34.888895129681,-64.8896467495754,12.));
#73570=CARTESIAN_POINT('Ctrl Pts',(-34.8911973983785,-64.9163739428606,
0.));
#73571=CARTESIAN_POINT('Ctrl Pts',(-34.8911973983785,-64.9163739428606,
12.));
#73572=CARTESIAN_POINT('Ctrl Pts',(-34.8934782116097,-64.943139590634,0.));
#73573=CARTESIAN_POINT('Ctrl Pts',(-34.8934782116097,-64.943139590634,12.));
#73574=CARTESIAN_POINT('Ctrl Pts',(-34.8957375133702,-64.9699436060178,
0.));
#73575=CARTESIAN_POINT('Ctrl Pts',(-34.8957375133702,-64.9699436060178,
12.));
#73576=CARTESIAN_POINT('Ctrl Pts',(-34.8979752478623,-64.9967859023225,
0.));
#73577=CARTESIAN_POINT('Ctrl Pts',(-34.8979752478623,-64.9967859023225,
12.));
#73578=CARTESIAN_POINT('Ctrl Pts',(-34.9001913596422,-65.0236663932338,
0.));
#73579=CARTESIAN_POINT('Ctrl Pts',(-34.9001913596422,-65.0236663932338,
12.));
#73580=CARTESIAN_POINT('Ctrl Pts',(-34.9023857937866,-65.0505849930172,
0.));
#73581=CARTESIAN_POINT('Ctrl Pts',(-34.9023857937866,-65.0505849930172,
12.));
#73582=CARTESIAN_POINT('Ctrl Pts',(-34.9045584960503,-65.0775416167073,
0.));
#73583=CARTESIAN_POINT('Ctrl Pts',(-34.9045584960503,-65.0775416167073,
12.));
#73584=CARTESIAN_POINT('Ctrl Pts',(-34.9067094130387,-65.1045361803097,
0.));
#73585=CARTESIAN_POINT('Ctrl Pts',(-34.9067094130387,-65.1045361803097,
12.));
#73586=CARTESIAN_POINT('Ctrl Pts',(-34.9088384918322,-65.1315686003485,
0.));
#73587=CARTESIAN_POINT('Ctrl Pts',(-34.9088384918322,-65.1315686003485,
12.));
#73588=CARTESIAN_POINT('Ctrl Pts',(-34.9109456796201,-65.1586387934216,
0.));
#73589=CARTESIAN_POINT('Ctrl Pts',(-34.9109456796201,-65.1586387934216,
12.));
#73590=CARTESIAN_POINT('Ctrl Pts',(-34.9130309233017,-65.1857466757082,
0.));
#73591=CARTESIAN_POINT('Ctrl Pts',(-34.9130309233017,-65.1857466757082,
12.));
#73592=CARTESIAN_POINT('Ctrl Pts',(-34.9150941691754,-65.2128921625837,
0.));
#73593=CARTESIAN_POINT('Ctrl Pts',(-34.9150941691754,-65.2128921625837,
12.));
#73594=CARTESIAN_POINT('Ctrl Pts',(-34.9171353624131,-65.2400751679586,
0.));
#73595=CARTESIAN_POINT('Ctrl Pts',(-34.9171353624131,-65.2400751679586,
12.));
#73596=CARTESIAN_POINT('Ctrl Pts',(-34.9191544474898,-65.2672956048121,
0.));
#73597=CARTESIAN_POINT('Ctrl Pts',(-34.9191544474898,-65.2672956048121,
12.));
#73598=CARTESIAN_POINT('Ctrl Pts',(-34.921151369138,-65.2945533863812,0.));
#73599=CARTESIAN_POINT('Ctrl Pts',(-34.921151369138,-65.2945533863812,12.));
#73600=CARTESIAN_POINT('Ctrl Pts',(-34.9231260731846,-65.3218484271941,
0.));
#73601=CARTESIAN_POINT('Ctrl Pts',(-34.9231260731846,-65.3218484271941,
12.));
#73602=CARTESIAN_POINT('Ctrl Pts',(-34.9250785073473,-65.3491806440529,
0.));
#73603=CARTESIAN_POINT('Ctrl Pts',(-34.9250785073473,-65.3491806440529,
12.));
#73604=CARTESIAN_POINT('Ctrl Pts',(-34.9270086222703,-65.3765499573019,
0.));
#73605=CARTESIAN_POINT('Ctrl Pts',(-34.9270086222703,-65.3765499573019,
12.));
#73606=CARTESIAN_POINT('Ctrl Pts',(-34.92891637177,-65.4039562911254,0.));
#73607=CARTESIAN_POINT('Ctrl Pts',(-34.92891637177,-65.4039562911254,12.));
#73608=CARTESIAN_POINT('Ctrl Pts',(-34.9308017105481,-65.4313995707423,
0.));
#73609=CARTESIAN_POINT('Ctrl Pts',(-34.9308017105481,-65.4313995707423,
12.));
#73610=CARTESIAN_POINT('Ctrl Pts',(-34.9326645923897,-65.4588797201884,
0.));
#73611=CARTESIAN_POINT('Ctrl Pts',(-34.9326645923897,-65.4588797201884,
12.));
#73612=CARTESIAN_POINT('Ctrl Pts',(-34.9345049680816,-65.4863966597523,
0.));
#73613=CARTESIAN_POINT('Ctrl Pts',(-34.9345049680816,-65.4863966597523,
12.));
#73614=CARTESIAN_POINT('Ctrl Pts',(-34.9363227836621,-65.5139503038116,
0.));
#73615=CARTESIAN_POINT('Ctrl Pts',(-34.9363227836621,-65.5139503038116,
12.));
#73616=CARTESIAN_POINT('Ctrl Pts',(-34.9381179779763,-65.5415405578138,
0.));
#73617=CARTESIAN_POINT('Ctrl Pts',(-34.9381179779763,-65.5415405578138,
12.));
#73618=CARTESIAN_POINT('Ctrl Pts',(-34.9398904862279,-65.5691673226051,
0.));
#73619=CARTESIAN_POINT('Ctrl Pts',(-34.9398904862279,-65.5691673226051,
12.));
#73620=CARTESIAN_POINT('Ctrl Pts',(-34.9416402443551,-65.5968304997821,
0.));
#73621=CARTESIAN_POINT('Ctrl Pts',(-34.9416402443551,-65.5968304997821,
12.));
#73622=CARTESIAN_POINT('Ctrl Pts',(-34.9433671932982,-65.6245299968635,
0.));
#73623=CARTESIAN_POINT('Ctrl Pts',(-34.9433671932982,-65.6245299968635,
12.));
#73624=CARTESIAN_POINT('Ctrl Pts',(-34.9450712829143,-65.6522657321239,
0.));
#73625=CARTESIAN_POINT('Ctrl Pts',(-34.9450712829143,-65.6522657321239,
12.));
#73626=CARTESIAN_POINT('Ctrl Pts',(-34.9467524770271,-65.6800376405722,
0.));
#73627=CARTESIAN_POINT('Ctrl Pts',(-34.9467524770271,-65.6800376405722,
12.));
#73628=CARTESIAN_POINT('Ctrl Pts',(-34.9484107543857,-65.707845675746,0.));
#73629=CARTESIAN_POINT('Ctrl Pts',(-34.9484107543857,-65.707845675746,12.));
#73630=CARTESIAN_POINT('Ctrl Pts',(-34.9500461042919,-65.7356898060478,
0.));
#73631=CARTESIAN_POINT('Ctrl Pts',(-34.9500461042919,-65.7356898060478,
12.));
#73632=CARTESIAN_POINT('Ctrl Pts',(-34.9513360397181,-65.757993971173,0.));
#73633=CARTESIAN_POINT('Ctrl Pts',(-34.9513360397181,-65.757993971173,12.));
#73634=CARTESIAN_POINT('Ctrl Pts',(-34.9522931728594,-65.7747383250775,
0.));
#73635=CARTESIAN_POINT('Ctrl Pts',(-34.9522931728594,-65.7747383250775,
12.));
#73636=CARTESIAN_POINT('Ctrl Pts',(-34.9529266758406,-65.7859084407494,
0.));
#73637=CARTESIAN_POINT('Ctrl Pts',(-34.9529266758406,-65.7859084407494,
12.));
#73638=CARTESIAN_POINT('Ctrl Pts',(-34.9532422808861,-65.7914953018524,
0.));
#73639=CARTESIAN_POINT('Ctrl Pts',(-34.9532422808861,-65.7914953018524,
12.));
#73640=CARTESIAN_POINT('',(-34.2579614092497,-61.0441813777723,0.));
#73641=CARTESIAN_POINT('Ctrl Pts',(-34.2579614092497,-61.0441813777723,
0.));
#73642=CARTESIAN_POINT('Ctrl Pts',(-34.2589297755434,-61.0479423318725,
0.));
#73643=CARTESIAN_POINT('Ctrl Pts',(-34.2608658001631,-61.0554700176998,
0.));
#73644=CARTESIAN_POINT('Ctrl Pts',(-34.2637677131935,-61.0667788793266,
0.));
#73645=CARTESIAN_POINT('Ctrl Pts',(-34.2676326825626,-61.0818920286293,
0.));
#73646=CARTESIAN_POINT('Ctrl Pts',(-34.2724568037228,-61.1008412399997,
0.));
#73647=CARTESIAN_POINT('Ctrl Pts',(-34.2772738038771,-61.1198481997764,
0.));
#73648=CARTESIAN_POINT('Ctrl Pts',(-34.282083624447,-61.1389128461885,0.));
#73649=CARTESIAN_POINT('Ctrl Pts',(-34.2868861666384,-61.1580350635532,
0.));
#73650=CARTESIAN_POINT('Ctrl Pts',(-34.2916812929751,-61.1772146833205,
0.));
#73651=CARTESIAN_POINT('Ctrl Pts',(-34.2964688443663,-61.1964515073891,
0.));
#73652=CARTESIAN_POINT('Ctrl Pts',(-34.3012486533474,-61.2157453259107,
0.));
#73653=CARTESIAN_POINT('Ctrl Pts',(-34.3060205584065,-61.2350959366939,
0.));
#73654=CARTESIAN_POINT('Ctrl Pts',(-34.3107844191044,-61.2545031656133,
0.));
#73655=CARTESIAN_POINT('Ctrl Pts',(-34.3155401111747,-61.2739668600365,
0.));
#73656=CARTESIAN_POINT('Ctrl Pts',(-34.3202875193618,-61.2934868791854,
0.));
#73657=CARTESIAN_POINT('Ctrl Pts',(-34.3250265314768,-61.3130630861386,
0.));
#73658=CARTESIAN_POINT('Ctrl Pts',(-34.3297570310146,-61.3326953378851,
0.));
#73659=CARTESIAN_POINT('Ctrl Pts',(-34.3344788934363,-61.3523834803188,
0.));
#73660=CARTESIAN_POINT('Ctrl Pts',(-34.339191990014,-61.3721273534256,0.));
#73661=CARTESIAN_POINT('Ctrl Pts',(-34.3438961902405,-61.3919267945302,
0.));
#73662=CARTESIAN_POINT('Ctrl Pts',(-34.3485913645979,-61.4117816420228,
0.));
#73663=CARTESIAN_POINT('Ctrl Pts',(-34.3532773877089,-61.4316917395918,
0.));
#73664=CARTESIAN_POINT('Ctrl Pts',(-34.3579541381996,-61.4516569360454,
0.));
#73665=CARTESIAN_POINT('Ctrl Pts',(-34.3626214971889,-61.4716770832896,
0.));
#73666=CARTESIAN_POINT('Ctrl Pts',(-34.3672793472466,-61.4917520349278,
0.));
#73667=CARTESIAN_POINT('Ctrl Pts',(-34.3719275711195,-61.5118816445437,
0.));
#73668=CARTESIAN_POINT('Ctrl Pts',(-34.376566050668,-61.5320657642638,0.));
#73669=CARTESIAN_POINT('Ctrl Pts',(-34.3811946674197,-61.5523042455158,
0.));
#73670=CARTESIAN_POINT('Ctrl Pts',(-34.3858133030518,-61.5725969396829,
0.));
#73671=CARTESIAN_POINT('Ctrl Pts',(-34.3904218398637,-61.5929436987409,
0.));
#73672=CARTESIAN_POINT('Ctrl Pts',(-34.3950201613432,-61.6133443760142,
0.));
#73673=CARTESIAN_POINT('Ctrl Pts',(-34.3996081523753,-61.6337988264556,
0.));
#73674=CARTESIAN_POINT('Ctrl Pts',(-34.4041856989317,-61.6543069062416,
0.));
#73675=CARTESIAN_POINT('Ctrl Pts',(-34.4087526878812,-61.6748684725205,
0.));
#73676=CARTESIAN_POINT('Ctrl Pts',(-34.4133090067704,-61.695483383117,0.));
#73677=CARTESIAN_POINT('Ctrl Pts',(-34.4178545435767,-61.7161514961914,
0.));
#73678=CARTESIAN_POINT('Ctrl Pts',(-34.422389186718,-61.7368726702596,0.));
#73679=CARTESIAN_POINT('Ctrl Pts',(-34.4269128251577,-61.7576467643432,
0.));
#73680=CARTESIAN_POINT('Ctrl Pts',(-34.4314253484792,-61.7784736380727,
0.));
#73681=CARTESIAN_POINT('Ctrl Pts',(-34.4359266469749,-61.7993531518036,
0.));
#73682=CARTESIAN_POINT('Ctrl Pts',(-34.4404166117299,-61.8202851667222,
0.));
#73683=CARTESIAN_POINT('Ctrl Pts',(-34.444895134574,-61.8412695447926,0.));
#73684=CARTESIAN_POINT('Ctrl Pts',(-34.4493621080361,-61.8623061487018,
0.));
#73685=CARTESIAN_POINT('Ctrl Pts',(-34.4538174253012,-61.8833948418025,
0.));
#73686=CARTESIAN_POINT('Ctrl Pts',(-34.4582609801637,-61.9045354880444,
0.));
#73687=CARTESIAN_POINT('Ctrl Pts',(-34.4626926669975,-61.9257279519308,
0.));
#73688=CARTESIAN_POINT('Ctrl Pts',(-34.4671123807717,-61.9469720985531,
0.));
#73689=CARTESIAN_POINT('Ctrl Pts',(-34.4715200170592,-61.9682677936053,
0.));
#73690=CARTESIAN_POINT('Ctrl Pts',(-34.4759154720473,-61.9896149034001,
0.));
#73691=CARTESIAN_POINT('Ctrl Pts',(-34.4802986425528,-62.0110132948794,
0.));
#73692=CARTESIAN_POINT('Ctrl Pts',(-34.48466942602,-62.0324628356141,0.));
#73693=CARTESIAN_POINT('Ctrl Pts',(-34.489027720504,-62.0539633937939,0.));
#73694=CARTESIAN_POINT('Ctrl Pts',(-34.4933734246593,-62.0755148382135,
0.));
#73695=CARTESIAN_POINT('Ctrl Pts',(-34.4977064377282,-62.0971170382567,
0.));
#73696=CARTESIAN_POINT('Ctrl Pts',(-34.5020266595293,-62.1187698638707,
0.));
#73697=CARTESIAN_POINT('Ctrl Pts',(-34.5063339904533,-62.1404731855687,
0.));
#73698=CARTESIAN_POINT('Ctrl Pts',(-34.5106283314594,-62.1622268744337,
0.));
#73699=CARTESIAN_POINT('Ctrl Pts',(-34.514909584073,-62.184030802117,0.));
#73700=CARTESIAN_POINT('Ctrl Pts',(-34.5191776503843,-62.2058848408346,
0.));
#73701=CARTESIAN_POINT('Ctrl Pts',(-34.5234324330492,-62.2277888633576,
0.));
#73702=CARTESIAN_POINT('Ctrl Pts',(-34.527673835281,-62.2497427430136,0.));
#73703=CARTESIAN_POINT('Ctrl Pts',(-34.5319017608435,-62.2717463536828,
0.));
#73704=CARTESIAN_POINT('Ctrl Pts',(-34.536116114045,-62.2937995697927,0.));
#73705=CARTESIAN_POINT('Ctrl Pts',(-34.5403167997333,-62.3159022663052,
0.));
#73706=CARTESIAN_POINT('Ctrl Pts',(-34.5445037232928,-62.3380543187067,
0.));
#73707=CARTESIAN_POINT('Ctrl Pts',(-34.5486767906376,-62.3602556030114,
0.));
#73708=CARTESIAN_POINT('Ctrl Pts',(-34.552835908207,-62.3825059957593,0.));
#73709=CARTESIAN_POINT('Ctrl Pts',(-34.5569809829615,-62.4048053740129,
0.));
#73710=CARTESIAN_POINT('Ctrl Pts',(-34.5611119223807,-62.4271536153473,
0.));
#73711=CARTESIAN_POINT('Ctrl Pts',(-34.5652286344606,-62.4495505978415,
0.));
#73712=CARTESIAN_POINT('Ctrl Pts',(-34.5693310277064,-62.4719962000829,
0.));
#73713=CARTESIAN_POINT('Ctrl Pts',(-34.5734190111279,-62.494490301164,0.));
#73714=CARTESIAN_POINT('Ctrl Pts',(-34.5774924942351,-62.5170327806774,
0.));
#73715=CARTESIAN_POINT('Ctrl Pts',(-34.5815513870363,-62.5396235187053,
0.));
#73716=CARTESIAN_POINT('Ctrl Pts',(-34.5855956000344,-62.5622623958125,
0.));
#73717=CARTESIAN_POINT('Ctrl Pts',(-34.5896250442199,-62.5849492930501,
0.));
#73718=CARTESIAN_POINT('Ctrl Pts',(-34.5936396310671,-62.6076840919521,
0.));
#73719=CARTESIAN_POINT('Ctrl Pts',(-34.5976392725303,-62.6304666745319,
0.));
#73720=CARTESIAN_POINT('Ctrl Pts',(-34.6016238810419,-62.6532969232695,
0.));
#73721=CARTESIAN_POINT('Ctrl Pts',(-34.6055933695093,-62.6761747211081,
0.));
#73722=CARTESIAN_POINT('Ctrl Pts',(-34.6095476513095,-62.6990999514597,
0.));
#73723=CARTESIAN_POINT('Ctrl Pts',(-34.6134866402842,-62.7220724982005,
0.));
#73724=CARTESIAN_POINT('Ctrl Pts',(-34.6174102507368,-62.7450922456662,
0.));
#73725=CARTESIAN_POINT('Ctrl Pts',(-34.6213183974303,-62.7681590786398,
0.));
#73726=CARTESIAN_POINT('Ctrl Pts',(-34.6252109955836,-62.7912728823482,
0.));
#73727=CARTESIAN_POINT('Ctrl Pts',(-34.629087960866,-62.8144335424671,0.));
#73728=CARTESIAN_POINT('Ctrl Pts',(-34.6329492093932,-62.8376409451167,
0.));
#73729=CARTESIAN_POINT('Ctrl Pts',(-34.6367946577241,-62.8608949768583,
0.));
#73730=CARTESIAN_POINT('Ctrl Pts',(-34.6406242228606,-62.8841955246819,
0.));
#73731=CARTESIAN_POINT('Ctrl Pts',(-34.6444378222425,-62.9075424760042,
0.));
#73732=CARTESIAN_POINT('Ctrl Pts',(-34.6482353737434,-62.9309357186733,
0.));
#73733=CARTESIAN_POINT('Ctrl Pts',(-34.6520167956657,-62.9543751409647,
0.));
#73734=CARTESIAN_POINT('Ctrl Pts',(-34.655782006739,-62.9778606315777,0.));
#73735=CARTESIAN_POINT('Ctrl Pts',(-34.6595309261186,-63.0013920796225,
0.));
#73736=CARTESIAN_POINT('Ctrl Pts',(-34.6632634733819,-63.0249693746198,
0.));
#73737=CARTESIAN_POINT('Ctrl Pts',(-34.6669795685225,-63.0485924065039,
0.));
#73738=CARTESIAN_POINT('Ctrl Pts',(-34.6706791319471,-63.0722610656194,
0.));
#73739=CARTESIAN_POINT('Ctrl Pts',(-34.6743620844722,-63.0959752427169,
0.));
#73740=CARTESIAN_POINT('Ctrl Pts',(-34.6780283473252,-63.119734828943,0.));
#73741=CARTESIAN_POINT('Ctrl Pts',(-34.6816778421401,-63.1435397158385,
0.));
#73742=CARTESIAN_POINT('Ctrl Pts',(-34.6853104909516,-63.1673897953425,
0.));
#73743=CARTESIAN_POINT('Ctrl Pts',(-34.6889262161923,-63.1912849597885,
0.));
#73744=CARTESIAN_POINT('Ctrl Pts',(-34.6925249406899,-63.2152251019014,
0.));
#73745=CARTESIAN_POINT('Ctrl Pts',(-34.6961065876671,-63.2392101147853,
0.));
#73746=CARTESIAN_POINT('Ctrl Pts',(-34.6996710807384,-63.2632398919234,
0.));
#73747=CARTESIAN_POINT('Ctrl Pts',(-34.7032183439045,-63.2873143271812,
0.));
#73748=CARTESIAN_POINT('Ctrl Pts',(-34.7067483015492,-63.311433314805,0.));
#73749=CARTESIAN_POINT('Ctrl Pts',(-34.7102608784373,-63.3355967494169,
0.));
#73750=CARTESIAN_POINT('Ctrl Pts',(-34.7137559997143,-63.3598045260049,
0.));
#73751=CARTESIAN_POINT('Ctrl Pts',(-34.7172335909037,-63.3840565399206,
0.));
#73752=CARTESIAN_POINT('Ctrl Pts',(-34.7206935779007,-63.4083526868837,
0.));
#73753=CARTESIAN_POINT('Ctrl Pts',(-34.7241358869702,-63.4326928629796,
0.));
#73754=CARTESIAN_POINT('Ctrl Pts',(-34.7275604447439,-63.4570769646568,
0.));
#73755=CARTESIAN_POINT('Ctrl Pts',(-34.7309671782212,-63.481504888716,0.));
#73756=CARTESIAN_POINT('Ctrl Pts',(-34.7343560147663,-63.5059765323082,
0.));
#73757=CARTESIAN_POINT('Ctrl Pts',(-34.7377268821022,-63.5304917929378,
0.));
#73758=CARTESIAN_POINT('Ctrl Pts',(-34.7410797083079,-63.5550505684621,
0.));
#73759=CARTESIAN_POINT('Ctrl Pts',(-34.7444144218162,-63.5796527570874,
0.));
#73760=CARTESIAN_POINT('Ctrl Pts',(-34.7477309514142,-63.6042982573598,
0.));
#73761=CARTESIAN_POINT('Ctrl Pts',(-34.7510292262415,-63.628986968162,0.));
#73762=CARTESIAN_POINT('Ctrl Pts',(-34.7543091757842,-63.6537187887174,
0.));
#73763=CARTESIAN_POINT('Ctrl Pts',(-34.7575707298718,-63.6784936185893,
0.));
#73764=CARTESIAN_POINT('Ctrl Pts',(-34.7608138186758,-63.7033113576782,
0.));
#73765=CARTESIAN_POINT('Ctrl Pts',(-34.7640383727094,-63.7281719062135,
0.));
#73766=CARTESIAN_POINT('Ctrl Pts',(-34.7672443228267,-63.7530751647478,
0.));
#73767=CARTESIAN_POINT('Ctrl Pts',(-34.7704316002165,-63.7780210341618,
0.));
#73768=CARTESIAN_POINT('Ctrl Pts',(-34.7736001363991,-63.8030094156635,
0.));
#73769=CARTESIAN_POINT('Ctrl Pts',(-34.7767498632244,-63.8280402107858,
0.));
#73770=CARTESIAN_POINT('Ctrl Pts',(-34.7798807128716,-63.8531133213794,
0.));
#73771=CARTESIAN_POINT('Ctrl Pts',(-34.7829926178495,-63.8782286496059,
0.));
#73772=CARTESIAN_POINT('Ctrl Pts',(-34.7860855109908,-63.9033860979428,
0.));
#73773=CARTESIAN_POINT('Ctrl Pts',(-34.7891593254485,-63.9285855691838,
0.));
#73774=CARTESIAN_POINT('Ctrl Pts',(-34.7922139946943,-63.9538269664365,
0.));
#73775=CARTESIAN_POINT('Ctrl Pts',(-34.7952494525182,-63.9791101931169,
0.));
#73776=CARTESIAN_POINT('Ctrl Pts',(-34.79826563303,-64.0044351529413,0.));
#73777=CARTESIAN_POINT('Ctrl Pts',(-34.8012624706534,-64.0298017499304,
0.));
#73778=CARTESIAN_POINT('Ctrl Pts',(-34.8042399001215,-64.05520988841,0.));
#73779=CARTESIAN_POINT('Ctrl Pts',(-34.8071978564748,-64.0806594730084,
0.));
#73780=CARTESIAN_POINT('Ctrl Pts',(-34.8101362750595,-64.1061504086512,
0.));
#73781=CARTESIAN_POINT('Ctrl Pts',(-34.8130550915284,-64.1316826005502,
0.));
#73782=CARTESIAN_POINT('Ctrl Pts',(-34.8159542418372,-64.1572559542084,
0.));
#73783=CARTESIAN_POINT('Ctrl Pts',(-34.8188336622419,-64.1828703754237,
0.));
#73784=CARTESIAN_POINT('Ctrl Pts',(-34.8216932892969,-64.2085257702885,
0.));
#73785=CARTESIAN_POINT('Ctrl Pts',(-34.8245330598559,-64.2342220451878,
0.));
#73786=CARTESIAN_POINT('Ctrl Pts',(-34.8273529110742,-64.259959106791,0.));
#73787=CARTESIAN_POINT('Ctrl Pts',(-34.8301527804052,-64.2857368620513,
0.));
#73788=CARTESIAN_POINT('Ctrl Pts',(-34.8329326055916,-64.3115552182056,
0.));
#73789=CARTESIAN_POINT('Ctrl Pts',(-34.8356923246617,-64.3374140827708,
0.));
#73790=CARTESIAN_POINT('Ctrl Pts',(-34.838431875925,-64.3633133635384,0.));
#73791=CARTESIAN_POINT('Ctrl Pts',(-34.8411511979705,-64.3892529685614,
0.));
#73792=CARTESIAN_POINT('Ctrl Pts',(-34.8438502296669,-64.4152328061526,
0.));
#73793=CARTESIAN_POINT('Ctrl Pts',(-34.8465289101626,-64.4412527848979,
0.));
#73794=CARTESIAN_POINT('Ctrl Pts',(-34.8491871788899,-64.4673128136631,
0.));
#73795=CARTESIAN_POINT('Ctrl Pts',(-34.851824975568,-64.4934128015983,0.));
#73796=CARTESIAN_POINT('Ctrl Pts',(-34.8544422402114,-64.5195526581398,
0.));
#73797=CARTESIAN_POINT('Ctrl Pts',(-34.8570389131334,-64.5457322930074,
0.));
#73798=CARTESIAN_POINT('Ctrl Pts',(-34.8596149349251,-64.5719516161913,
0.));
#73799=CARTESIAN_POINT('Ctrl Pts',(-34.8621702464397,-64.5982105379374,
0.));
#73800=CARTESIAN_POINT('Ctrl Pts',(-34.8647047887774,-64.6245089687276,
0.));
#73801=CARTESIAN_POINT('Ctrl Pts',(-34.8672185032725,-64.6508468192609,
0.));
#73802=CARTESIAN_POINT('Ctrl Pts',(-34.8697113314797,-64.6772240004241,
0.));
#73803=CARTESIAN_POINT('Ctrl Pts',(-34.8721832151982,-64.7036404233319,
0.));
#73804=CARTESIAN_POINT('Ctrl Pts',(-34.8746340964977,-64.7300959993662,
0.));
#73805=CARTESIAN_POINT('Ctrl Pts',(-34.8770639177494,-64.7565906402153,
0.));
#73806=CARTESIAN_POINT('Ctrl Pts',(-34.8794726216511,-64.7831242579023,
0.));
#73807=CARTESIAN_POINT('Ctrl Pts',(-34.8818601512726,-64.8096967648299,
0.));
#73808=CARTESIAN_POINT('Ctrl Pts',(-34.8842264500184,-64.8363080737369,
0.));
#73809=CARTESIAN_POINT('Ctrl Pts',(-34.8865714615433,-64.8629580976057,
0.));
#73810=CARTESIAN_POINT('Ctrl Pts',(-34.888895129681,-64.8896467495754,0.));
#73811=CARTESIAN_POINT('Ctrl Pts',(-34.8911973983785,-64.9163739428606,
0.));
#73812=CARTESIAN_POINT('Ctrl Pts',(-34.8934782116097,-64.943139590634,0.));
#73813=CARTESIAN_POINT('Ctrl Pts',(-34.8957375133702,-64.9699436060178,
0.));
#73814=CARTESIAN_POINT('Ctrl Pts',(-34.8979752478623,-64.9967859023225,
0.));
#73815=CARTESIAN_POINT('Ctrl Pts',(-34.9001913596422,-65.0236663932338,
0.));
#73816=CARTESIAN_POINT('Ctrl Pts',(-34.9023857937866,-65.0505849930172,
0.));
#73817=CARTESIAN_POINT('Ctrl Pts',(-34.9045584960503,-65.0775416167073,
0.));
#73818=CARTESIAN_POINT('Ctrl Pts',(-34.9067094130387,-65.1045361803097,
0.));
#73819=CARTESIAN_POINT('Ctrl Pts',(-34.9088384918322,-65.1315686003485,
0.));
#73820=CARTESIAN_POINT('Ctrl Pts',(-34.9109456796201,-65.1586387934216,
0.));
#73821=CARTESIAN_POINT('Ctrl Pts',(-34.9130309233017,-65.1857466757082,
0.));
#73822=CARTESIAN_POINT('Ctrl Pts',(-34.9150941691754,-65.2128921625837,
0.));
#73823=CARTESIAN_POINT('Ctrl Pts',(-34.9171353624131,-65.2400751679586,
0.));
#73824=CARTESIAN_POINT('Ctrl Pts',(-34.9191544474898,-65.2672956048121,
0.));
#73825=CARTESIAN_POINT('Ctrl Pts',(-34.921151369138,-65.2945533863812,0.));
#73826=CARTESIAN_POINT('Ctrl Pts',(-34.9231260731846,-65.3218484271941,
0.));
#73827=CARTESIAN_POINT('Ctrl Pts',(-34.9250785073473,-65.3491806440529,
0.));
#73828=CARTESIAN_POINT('Ctrl Pts',(-34.9270086222703,-65.3765499573019,
0.));
#73829=CARTESIAN_POINT('Ctrl Pts',(-34.92891637177,-65.4039562911254,0.));
#73830=CARTESIAN_POINT('Ctrl Pts',(-34.9305324724386,-65.4274804996405,
0.));
#73831=CARTESIAN_POINT('Ctrl Pts',(-34.9317593813103,-65.4455359574999,
0.));
#73832=CARTESIAN_POINT('Ctrl Pts',(-34.9326070346592,-65.4581063193583,
0.));
#73833=CARTESIAN_POINT('Ctrl Pts',(-34.9330820191484,-65.4651808010451,
0.));
#73834=CARTESIAN_POINT('Ctrl Pts',(-34.9331875523085,-65.4667541477954,
0.));
#73835=CARTESIAN_POINT('',(-34.2579614092497,-61.0441813777723,12.));
#73836=CARTESIAN_POINT('',(-34.2579614092497,-61.0441813777723,0.));
#73837=CARTESIAN_POINT('Ctrl Pts',(-34.9331875523085,-65.4667541477954,
12.));
#73838=CARTESIAN_POINT('Ctrl Pts',(-34.9330820191484,-65.4651808010451,
12.));
#73839=CARTESIAN_POINT('Ctrl Pts',(-34.9326070346592,-65.4581063193583,
12.));
#73840=CARTESIAN_POINT('Ctrl Pts',(-34.9317593813103,-65.4455359574999,
12.));
#73841=CARTESIAN_POINT('Ctrl Pts',(-34.9305324724386,-65.4274804996405,
12.));
#73842=CARTESIAN_POINT('Ctrl Pts',(-34.92891637177,-65.4039562911254,12.));
#73843=CARTESIAN_POINT('Ctrl Pts',(-34.9270086222703,-65.3765499573019,
12.));
#73844=CARTESIAN_POINT('Ctrl Pts',(-34.9250785073473,-65.3491806440529,
12.));
#73845=CARTESIAN_POINT('Ctrl Pts',(-34.9231260731846,-65.3218484271941,
12.));
#73846=CARTESIAN_POINT('Ctrl Pts',(-34.921151369138,-65.2945533863812,12.));
#73847=CARTESIAN_POINT('Ctrl Pts',(-34.9191544474898,-65.2672956048121,
12.));
#73848=CARTESIAN_POINT('Ctrl Pts',(-34.9171353624131,-65.2400751679586,
12.));
#73849=CARTESIAN_POINT('Ctrl Pts',(-34.9150941691754,-65.2128921625837,
12.));
#73850=CARTESIAN_POINT('Ctrl Pts',(-34.9130309233017,-65.1857466757082,
12.));
#73851=CARTESIAN_POINT('Ctrl Pts',(-34.9109456796201,-65.1586387934216,
12.));
#73852=CARTESIAN_POINT('Ctrl Pts',(-34.9088384918322,-65.1315686003485,
12.));
#73853=CARTESIAN_POINT('Ctrl Pts',(-34.9067094130387,-65.1045361803097,
12.));
#73854=CARTESIAN_POINT('Ctrl Pts',(-34.9045584960503,-65.0775416167073,
12.));
#73855=CARTESIAN_POINT('Ctrl Pts',(-34.9023857937866,-65.0505849930172,
12.));
#73856=CARTESIAN_POINT('Ctrl Pts',(-34.9001913596422,-65.0236663932338,
12.));
#73857=CARTESIAN_POINT('Ctrl Pts',(-34.8979752478623,-64.9967859023225,
12.));
#73858=CARTESIAN_POINT('Ctrl Pts',(-34.8957375133702,-64.9699436060178,
12.));
#73859=CARTESIAN_POINT('Ctrl Pts',(-34.8934782116097,-64.943139590634,12.));
#73860=CARTESIAN_POINT('Ctrl Pts',(-34.8911973983785,-64.9163739428606,
12.));
#73861=CARTESIAN_POINT('Ctrl Pts',(-34.888895129681,-64.8896467495754,12.));
#73862=CARTESIAN_POINT('Ctrl Pts',(-34.8865714615433,-64.8629580976057,
12.));
#73863=CARTESIAN_POINT('Ctrl Pts',(-34.8842264500184,-64.8363080737369,
12.));
#73864=CARTESIAN_POINT('Ctrl Pts',(-34.8818601512726,-64.8096967648299,
12.));
#73865=CARTESIAN_POINT('Ctrl Pts',(-34.8794726216511,-64.7831242579023,
12.));
#73866=CARTESIAN_POINT('Ctrl Pts',(-34.8770639177494,-64.7565906402153,
12.));
#73867=CARTESIAN_POINT('Ctrl Pts',(-34.8746340964977,-64.7300959993662,
12.));
#73868=CARTESIAN_POINT('Ctrl Pts',(-34.8721832151982,-64.7036404233319,
12.));
#73869=CARTESIAN_POINT('Ctrl Pts',(-34.8697113314797,-64.6772240004241,
12.));
#73870=CARTESIAN_POINT('Ctrl Pts',(-34.8672185032725,-64.6508468192609,
12.));
#73871=CARTESIAN_POINT('Ctrl Pts',(-34.8647047887774,-64.6245089687276,
12.));
#73872=CARTESIAN_POINT('Ctrl Pts',(-34.8621702464397,-64.5982105379374,
12.));
#73873=CARTESIAN_POINT('Ctrl Pts',(-34.8596149349251,-64.5719516161913,
12.));
#73874=CARTESIAN_POINT('Ctrl Pts',(-34.8570389131334,-64.5457322930074,
12.));
#73875=CARTESIAN_POINT('Ctrl Pts',(-34.8544422402114,-64.5195526581398,
12.));
#73876=CARTESIAN_POINT('Ctrl Pts',(-34.851824975568,-64.4934128015983,12.));
#73877=CARTESIAN_POINT('Ctrl Pts',(-34.8491871788899,-64.4673128136631,
12.));
#73878=CARTESIAN_POINT('Ctrl Pts',(-34.8465289101626,-64.4412527848979,
12.));
#73879=CARTESIAN_POINT('Ctrl Pts',(-34.8438502296669,-64.4152328061526,
12.));
#73880=CARTESIAN_POINT('Ctrl Pts',(-34.8411511979705,-64.3892529685614,
12.));
#73881=CARTESIAN_POINT('Ctrl Pts',(-34.838431875925,-64.3633133635384,12.));
#73882=CARTESIAN_POINT('Ctrl Pts',(-34.8356923246617,-64.3374140827708,
12.));
#73883=CARTESIAN_POINT('Ctrl Pts',(-34.8329326055916,-64.3115552182056,
12.));
#73884=CARTESIAN_POINT('Ctrl Pts',(-34.8301527804052,-64.2857368620513,
12.));
#73885=CARTESIAN_POINT('Ctrl Pts',(-34.8273529110742,-64.259959106791,12.));
#73886=CARTESIAN_POINT('Ctrl Pts',(-34.8245330598559,-64.2342220451878,
12.));
#73887=CARTESIAN_POINT('Ctrl Pts',(-34.8216932892969,-64.2085257702885,
12.));
#73888=CARTESIAN_POINT('Ctrl Pts',(-34.8188336622419,-64.1828703754237,
12.));
#73889=CARTESIAN_POINT('Ctrl Pts',(-34.8159542418372,-64.1572559542084,
12.));
#73890=CARTESIAN_POINT('Ctrl Pts',(-34.8130550915284,-64.1316826005502,
12.));
#73891=CARTESIAN_POINT('Ctrl Pts',(-34.8101362750595,-64.1061504086512,
12.));
#73892=CARTESIAN_POINT('Ctrl Pts',(-34.8071978564748,-64.0806594730084,
12.));
#73893=CARTESIAN_POINT('Ctrl Pts',(-34.8042399001215,-64.05520988841,12.));
#73894=CARTESIAN_POINT('Ctrl Pts',(-34.8012624706534,-64.0298017499304,
12.));
#73895=CARTESIAN_POINT('Ctrl Pts',(-34.79826563303,-64.0044351529413,12.));
#73896=CARTESIAN_POINT('Ctrl Pts',(-34.7952494525182,-63.9791101931169,
12.));
#73897=CARTESIAN_POINT('Ctrl Pts',(-34.7922139946943,-63.9538269664365,
12.));
#73898=CARTESIAN_POINT('Ctrl Pts',(-34.7891593254485,-63.9285855691838,
12.));
#73899=CARTESIAN_POINT('Ctrl Pts',(-34.7860855109908,-63.9033860979428,
12.));
#73900=CARTESIAN_POINT('Ctrl Pts',(-34.7829926178495,-63.8782286496059,
12.));
#73901=CARTESIAN_POINT('Ctrl Pts',(-34.7798807128716,-63.8531133213794,
12.));
#73902=CARTESIAN_POINT('Ctrl Pts',(-34.7767498632244,-63.8280402107858,
12.));
#73903=CARTESIAN_POINT('Ctrl Pts',(-34.7736001363991,-63.8030094156635,
12.));
#73904=CARTESIAN_POINT('Ctrl Pts',(-34.7704316002165,-63.7780210341618,
12.));
#73905=CARTESIAN_POINT('Ctrl Pts',(-34.7672443228267,-63.7530751647478,
12.));
#73906=CARTESIAN_POINT('Ctrl Pts',(-34.7640383727094,-63.7281719062135,
12.));
#73907=CARTESIAN_POINT('Ctrl Pts',(-34.7608138186758,-63.7033113576782,
12.));
#73908=CARTESIAN_POINT('Ctrl Pts',(-34.7575707298718,-63.6784936185893,
12.));
#73909=CARTESIAN_POINT('Ctrl Pts',(-34.7543091757842,-63.6537187887174,
12.));
#73910=CARTESIAN_POINT('Ctrl Pts',(-34.7510292262415,-63.628986968162,12.));
#73911=CARTESIAN_POINT('Ctrl Pts',(-34.7477309514142,-63.6042982573598,
12.));
#73912=CARTESIAN_POINT('Ctrl Pts',(-34.7444144218162,-63.5796527570874,
12.));
#73913=CARTESIAN_POINT('Ctrl Pts',(-34.7410797083079,-63.5550505684621,
12.));
#73914=CARTESIAN_POINT('Ctrl Pts',(-34.7377268821022,-63.5304917929378,
12.));
#73915=CARTESIAN_POINT('Ctrl Pts',(-34.7343560147663,-63.5059765323082,
12.));
#73916=CARTESIAN_POINT('Ctrl Pts',(-34.7309671782212,-63.481504888716,12.));
#73917=CARTESIAN_POINT('Ctrl Pts',(-34.7275604447439,-63.4570769646568,
12.));
#73918=CARTESIAN_POINT('Ctrl Pts',(-34.7241358869702,-63.4326928629796,
12.));
#73919=CARTESIAN_POINT('Ctrl Pts',(-34.7206935779007,-63.4083526868837,
12.));
#73920=CARTESIAN_POINT('Ctrl Pts',(-34.7172335909037,-63.3840565399206,
12.));
#73921=CARTESIAN_POINT('Ctrl Pts',(-34.7137559997143,-63.3598045260049,
12.));
#73922=CARTESIAN_POINT('Ctrl Pts',(-34.7102608784373,-63.3355967494169,
12.));
#73923=CARTESIAN_POINT('Ctrl Pts',(-34.7067483015492,-63.311433314805,12.));
#73924=CARTESIAN_POINT('Ctrl Pts',(-34.7032183439045,-63.2873143271812,
12.));
#73925=CARTESIAN_POINT('Ctrl Pts',(-34.6996710807384,-63.2632398919234,
12.));
#73926=CARTESIAN_POINT('Ctrl Pts',(-34.6961065876671,-63.2392101147853,
12.));
#73927=CARTESIAN_POINT('Ctrl Pts',(-34.6925249406899,-63.2152251019014,
12.));
#73928=CARTESIAN_POINT('Ctrl Pts',(-34.6889262161923,-63.1912849597885,
12.));
#73929=CARTESIAN_POINT('Ctrl Pts',(-34.6853104909516,-63.1673897953425,
12.));
#73930=CARTESIAN_POINT('Ctrl Pts',(-34.6816778421401,-63.1435397158385,
12.));
#73931=CARTESIAN_POINT('Ctrl Pts',(-34.6780283473252,-63.119734828943,12.));
#73932=CARTESIAN_POINT('Ctrl Pts',(-34.6743620844722,-63.0959752427169,
12.));
#73933=CARTESIAN_POINT('Ctrl Pts',(-34.6706791319471,-63.0722610656194,
12.));
#73934=CARTESIAN_POINT('Ctrl Pts',(-34.6669795685225,-63.0485924065039,
12.));
#73935=CARTESIAN_POINT('Ctrl Pts',(-34.6632634733819,-63.0249693746198,
12.));
#73936=CARTESIAN_POINT('Ctrl Pts',(-34.6595309261186,-63.0013920796225,
12.));
#73937=CARTESIAN_POINT('Ctrl Pts',(-34.655782006739,-62.9778606315777,12.));
#73938=CARTESIAN_POINT('Ctrl Pts',(-34.6520167956657,-62.9543751409647,
12.));
#73939=CARTESIAN_POINT('Ctrl Pts',(-34.6482353737434,-62.9309357186733,
12.));
#73940=CARTESIAN_POINT('Ctrl Pts',(-34.6444378222425,-62.9075424760042,
12.));
#73941=CARTESIAN_POINT('Ctrl Pts',(-34.6406242228606,-62.8841955246819,
12.));
#73942=CARTESIAN_POINT('Ctrl Pts',(-34.6367946577241,-62.8608949768583,
12.));
#73943=CARTESIAN_POINT('Ctrl Pts',(-34.6329492093932,-62.8376409451167,
12.));
#73944=CARTESIAN_POINT('Ctrl Pts',(-34.629087960866,-62.8144335424671,12.));
#73945=CARTESIAN_POINT('Ctrl Pts',(-34.6252109955836,-62.7912728823482,
12.));
#73946=CARTESIAN_POINT('Ctrl Pts',(-34.6213183974303,-62.7681590786398,
12.));
#73947=CARTESIAN_POINT('Ctrl Pts',(-34.6174102507368,-62.7450922456662,
12.));
#73948=CARTESIAN_POINT('Ctrl Pts',(-34.6134866402842,-62.7220724982005,
12.));
#73949=CARTESIAN_POINT('Ctrl Pts',(-34.6095476513095,-62.6990999514597,
12.));
#73950=CARTESIAN_POINT('Ctrl Pts',(-34.6055933695093,-62.6761747211081,
12.));
#73951=CARTESIAN_POINT('Ctrl Pts',(-34.6016238810419,-62.6532969232695,
12.));
#73952=CARTESIAN_POINT('Ctrl Pts',(-34.5976392725303,-62.6304666745319,
12.));
#73953=CARTESIAN_POINT('Ctrl Pts',(-34.5936396310671,-62.6076840919521,
12.));
#73954=CARTESIAN_POINT('Ctrl Pts',(-34.5896250442199,-62.5849492930501,
12.));
#73955=CARTESIAN_POINT('Ctrl Pts',(-34.5855956000344,-62.5622623958125,
12.));
#73956=CARTESIAN_POINT('Ctrl Pts',(-34.5815513870363,-62.5396235187053,
12.));
#73957=CARTESIAN_POINT('Ctrl Pts',(-34.5774924942351,-62.5170327806774,
12.));
#73958=CARTESIAN_POINT('Ctrl Pts',(-34.5734190111279,-62.494490301164,12.));
#73959=CARTESIAN_POINT('Ctrl Pts',(-34.5693310277064,-62.4719962000829,
12.));
#73960=CARTESIAN_POINT('Ctrl Pts',(-34.5652286344606,-62.4495505978415,
12.));
#73961=CARTESIAN_POINT('Ctrl Pts',(-34.5611119223807,-62.4271536153473,
12.));
#73962=CARTESIAN_POINT('Ctrl Pts',(-34.5569809829615,-62.4048053740129,
12.));
#73963=CARTESIAN_POINT('Ctrl Pts',(-34.552835908207,-62.3825059957593,12.));
#73964=CARTESIAN_POINT('Ctrl Pts',(-34.5486767906376,-62.3602556030114,
12.));
#73965=CARTESIAN_POINT('Ctrl Pts',(-34.5445037232928,-62.3380543187067,
12.));
#73966=CARTESIAN_POINT('Ctrl Pts',(-34.5403167997333,-62.3159022663052,
12.));
#73967=CARTESIAN_POINT('Ctrl Pts',(-34.536116114045,-62.2937995697927,12.));
#73968=CARTESIAN_POINT('Ctrl Pts',(-34.5319017608435,-62.2717463536828,
12.));
#73969=CARTESIAN_POINT('Ctrl Pts',(-34.527673835281,-62.2497427430136,12.));
#73970=CARTESIAN_POINT('Ctrl Pts',(-34.5234324330492,-62.2277888633576,
12.));
#73971=CARTESIAN_POINT('Ctrl Pts',(-34.5191776503843,-62.2058848408346,
12.));
#73972=CARTESIAN_POINT('Ctrl Pts',(-34.514909584073,-62.184030802117,12.));
#73973=CARTESIAN_POINT('Ctrl Pts',(-34.5106283314594,-62.1622268744337,
12.));
#73974=CARTESIAN_POINT('Ctrl Pts',(-34.5063339904533,-62.1404731855687,
12.));
#73975=CARTESIAN_POINT('Ctrl Pts',(-34.5020266595293,-62.1187698638707,
12.));
#73976=CARTESIAN_POINT('Ctrl Pts',(-34.4977064377282,-62.0971170382567,
12.));
#73977=CARTESIAN_POINT('Ctrl Pts',(-34.4933734246593,-62.0755148382135,
12.));
#73978=CARTESIAN_POINT('Ctrl Pts',(-34.489027720504,-62.0539633937939,12.));
#73979=CARTESIAN_POINT('Ctrl Pts',(-34.48466942602,-62.0324628356141,12.));
#73980=CARTESIAN_POINT('Ctrl Pts',(-34.4802986425528,-62.0110132948794,
12.));
#73981=CARTESIAN_POINT('Ctrl Pts',(-34.4759154720473,-61.9896149034001,
12.));
#73982=CARTESIAN_POINT('Ctrl Pts',(-34.4715200170592,-61.9682677936053,
12.));
#73983=CARTESIAN_POINT('Ctrl Pts',(-34.4671123807717,-61.9469720985531,
12.));
#73984=CARTESIAN_POINT('Ctrl Pts',(-34.4626926669975,-61.9257279519308,
12.));
#73985=CARTESIAN_POINT('Ctrl Pts',(-34.4582609801637,-61.9045354880444,
12.));
#73986=CARTESIAN_POINT('Ctrl Pts',(-34.4538174253012,-61.8833948418025,
12.));
#73987=CARTESIAN_POINT('Ctrl Pts',(-34.4493621080361,-61.8623061487018,
12.));
#73988=CARTESIAN_POINT('Ctrl Pts',(-34.444895134574,-61.8412695447926,12.));
#73989=CARTESIAN_POINT('Ctrl Pts',(-34.4404166117299,-61.8202851667222,
12.));
#73990=CARTESIAN_POINT('Ctrl Pts',(-34.4359266469749,-61.7993531518036,
12.));
#73991=CARTESIAN_POINT('Ctrl Pts',(-34.4314253484792,-61.7784736380727,
12.));
#73992=CARTESIAN_POINT('Ctrl Pts',(-34.4269128251577,-61.7576467643432,
12.));
#73993=CARTESIAN_POINT('Ctrl Pts',(-34.422389186718,-61.7368726702596,12.));
#73994=CARTESIAN_POINT('Ctrl Pts',(-34.4178545435767,-61.7161514961914,
12.));
#73995=CARTESIAN_POINT('Ctrl Pts',(-34.4133090067704,-61.695483383117,12.));
#73996=CARTESIAN_POINT('Ctrl Pts',(-34.4087526878812,-61.6748684725205,
12.));
#73997=CARTESIAN_POINT('Ctrl Pts',(-34.4041856989317,-61.6543069062416,
12.));
#73998=CARTESIAN_POINT('Ctrl Pts',(-34.3996081523753,-61.6337988264556,
12.));
#73999=CARTESIAN_POINT('Ctrl Pts',(-34.3950201613432,-61.6133443760142,
12.));
#74000=CARTESIAN_POINT('Ctrl Pts',(-34.3904218398637,-61.5929436987409,
12.));
#74001=CARTESIAN_POINT('Ctrl Pts',(-34.3858133030518,-61.5725969396829,
12.));
#74002=CARTESIAN_POINT('Ctrl Pts',(-34.3811946674197,-61.5523042455158,
12.));
#74003=CARTESIAN_POINT('Ctrl Pts',(-34.376566050668,-61.5320657642638,12.));
#74004=CARTESIAN_POINT('Ctrl Pts',(-34.3719275711195,-61.5118816445437,
12.));
#74005=CARTESIAN_POINT('Ctrl Pts',(-34.3672793472466,-61.4917520349278,
12.));
#74006=CARTESIAN_POINT('Ctrl Pts',(-34.3626214971889,-61.4716770832896,
12.));
#74007=CARTESIAN_POINT('Ctrl Pts',(-34.3579541381996,-61.4516569360454,
12.));
#74008=CARTESIAN_POINT('Ctrl Pts',(-34.3532773877089,-61.4316917395918,
12.));
#74009=CARTESIAN_POINT('Ctrl Pts',(-34.3485913645979,-61.4117816420228,
12.));
#74010=CARTESIAN_POINT('Ctrl Pts',(-34.3438961902405,-61.3919267945302,
12.));
#74011=CARTESIAN_POINT('Ctrl Pts',(-34.339191990014,-61.3721273534256,12.));
#74012=CARTESIAN_POINT('Ctrl Pts',(-34.3344788934363,-61.3523834803188,
12.));
#74013=CARTESIAN_POINT('Ctrl Pts',(-34.3297570310146,-61.3326953378851,
12.));
#74014=CARTESIAN_POINT('Ctrl Pts',(-34.3250265314768,-61.3130630861386,
12.));
#74015=CARTESIAN_POINT('Ctrl Pts',(-34.3202875193618,-61.2934868791854,
12.));
#74016=CARTESIAN_POINT('Ctrl Pts',(-34.3155401111747,-61.2739668600365,
12.));
#74017=CARTESIAN_POINT('Ctrl Pts',(-34.3107844191044,-61.2545031656133,
12.));
#74018=CARTESIAN_POINT('Ctrl Pts',(-34.3060205584065,-61.2350959366939,
12.));
#74019=CARTESIAN_POINT('Ctrl Pts',(-34.3012486533474,-61.2157453259107,
12.));
#74020=CARTESIAN_POINT('Ctrl Pts',(-34.2964688443663,-61.1964515073891,
12.));
#74021=CARTESIAN_POINT('Ctrl Pts',(-34.2916812929751,-61.1772146833205,
12.));
#74022=CARTESIAN_POINT('Ctrl Pts',(-34.2868861666384,-61.1580350635532,
12.));
#74023=CARTESIAN_POINT('Ctrl Pts',(-34.282083624447,-61.1389128461885,12.));
#74024=CARTESIAN_POINT('Ctrl Pts',(-34.2772738038771,-61.1198481997764,
12.));
#74025=CARTESIAN_POINT('Ctrl Pts',(-34.2724568037228,-61.1008412399997,
12.));
#74026=CARTESIAN_POINT('Ctrl Pts',(-34.2676326825626,-61.0818920286293,
12.));
#74027=CARTESIAN_POINT('Ctrl Pts',(-34.2637677131935,-61.0667788793266,
12.));
#74028=CARTESIAN_POINT('Ctrl Pts',(-34.2608658001631,-61.0554700176998,
12.));
#74029=CARTESIAN_POINT('Ctrl Pts',(-34.2589297755434,-61.0479423318725,
12.));
#74030=CARTESIAN_POINT('Ctrl Pts',(-34.2579614092497,-61.0441813777723,
12.));
#74031=CARTESIAN_POINT('Ctrl Pts',(-33.590372266528,-66.1657795405962,-5.55111512312578E-16));
#74032=CARTESIAN_POINT('Ctrl Pts',(-33.590372266528,-66.1657795405962,4.));
#74033=CARTESIAN_POINT('Ctrl Pts',(-33.590372266528,-66.1657795405962,8.));
#74034=CARTESIAN_POINT('Ctrl Pts',(-33.590372266528,-66.1657795405962,12.));
#74035=CARTESIAN_POINT('Ctrl Pts',(-33.6759628819919,-66.2346881970582,
-5.55111512312578E-16));
#74036=CARTESIAN_POINT('Ctrl Pts',(-33.6759628819919,-66.2346881970582,
4.));
#74037=CARTESIAN_POINT('Ctrl Pts',(-33.675962881992,-66.2346881970582,8.));
#74038=CARTESIAN_POINT('Ctrl Pts',(-33.675962881992,-66.2346881970582,12.));
#74039=CARTESIAN_POINT('Ctrl Pts',(-33.8665453669335,-66.3036153738448,
-5.55111512312578E-16));
#74040=CARTESIAN_POINT('Ctrl Pts',(-33.8665453669335,-66.3036153738448,
4.));
#74041=CARTESIAN_POINT('Ctrl Pts',(-33.8665453669334,-66.3036153738447,
8.));
#74042=CARTESIAN_POINT('Ctrl Pts',(-33.8665453669334,-66.3036153738447,
12.));
#74043=CARTESIAN_POINT('Ctrl Pts',(-34.0597557125863,-66.2585076236406,
-5.55111512312578E-16));
#74044=CARTESIAN_POINT('Ctrl Pts',(-34.0597557125863,-66.2585076236406,
4.));
#74045=CARTESIAN_POINT('Ctrl Pts',(-34.0597557125862,-66.2585076236405,
8.));
#74046=CARTESIAN_POINT('Ctrl Pts',(-34.0597557125862,-66.2585076236405,
12.));
#74047=CARTESIAN_POINT('Ctrl Pts',(-34.1330090612018,-66.2207497120656,
-5.55111512312578E-16));
#74048=CARTESIAN_POINT('Ctrl Pts',(-34.1330090612018,-66.2207497120656,
4.));
#74049=CARTESIAN_POINT('Ctrl Pts',(-34.1330090612017,-66.2207497120656,
8.));
#74050=CARTESIAN_POINT('Ctrl Pts',(-34.1330090612017,-66.2207497120656,
12.));
#74051=CARTESIAN_POINT('',(-33.590372266528,-66.1657795405962,-2.77555756156289E-16));
#74052=CARTESIAN_POINT('',(-34.1330090612014,-66.2207497120649,2.77555756156289E-16));
#74053=CARTESIAN_POINT('Ctrl Pts',(-33.590372266528,-66.1657795405962,-5.44214888274584E-16));
#74054=CARTESIAN_POINT('Ctrl Pts',(-33.6759628819919,-66.2346881970582,
-5.44214888274584E-16));
#74055=CARTESIAN_POINT('Ctrl Pts',(-33.7848671591014,-66.274075155222,-5.44214888274584E-16));
#74056=CARTESIAN_POINT('Ctrl Pts',(-33.8946295131778,-66.2762262188581,
-5.44214888274584E-16));
#74057=CARTESIAN_POINT('Ctrl Pts',(-33.9769512787351,-66.2778395165852,
-5.44214888274584E-16));
#74058=CARTESIAN_POINT('Ctrl Pts',(-34.0597557125863,-66.2585076236406,
-5.44214888274584E-16));
#74059=CARTESIAN_POINT('Ctrl Pts',(-34.1330090612018,-66.2207497120656,
-5.44214888274584E-16));
#74060=CARTESIAN_POINT('',(-34.1330090612013,-66.2207497120649,12.));
#74061=CARTESIAN_POINT('Ctrl Pts',(-34.1330090612018,-66.2207497120656,
-5.55111512312578E-16));
#74062=CARTESIAN_POINT('Ctrl Pts',(-34.1330090612018,-66.2207497120656,
4.));
#74063=CARTESIAN_POINT('Ctrl Pts',(-34.1330090612017,-66.2207497120656,
8.));
#74064=CARTESIAN_POINT('Ctrl Pts',(-34.1330090612017,-66.2207497120656,
12.));
#74065=CARTESIAN_POINT('',(-33.590372266528,-66.1657795405962,12.));
#74066=CARTESIAN_POINT('Ctrl Pts',(-34.1330090612017,-66.2207497120656,
12.));
#74067=CARTESIAN_POINT('Ctrl Pts',(-34.0597557125862,-66.2585076236405,
12.));
#74068=CARTESIAN_POINT('Ctrl Pts',(-33.976951278735,-66.2778395165851,12.));
#74069=CARTESIAN_POINT('Ctrl Pts',(-33.8946295131777,-66.2762262188581,
12.));
#74070=CARTESIAN_POINT('Ctrl Pts',(-33.7848671591014,-66.2740751552219,
12.));
#74071=CARTESIAN_POINT('Ctrl Pts',(-33.675962881992,-66.2346881970582,12.));
#74072=CARTESIAN_POINT('Ctrl Pts',(-33.590372266528,-66.1657795405962,12.));
#74073=CARTESIAN_POINT('Ctrl Pts',(-33.590372266528,-66.1657795405962,12.));
#74074=CARTESIAN_POINT('Ctrl Pts',(-33.590372266528,-66.1657795405962,8.));
#74075=CARTESIAN_POINT('Ctrl Pts',(-33.590372266528,-66.1657795405962,4.));
#74076=CARTESIAN_POINT('Ctrl Pts',(-33.590372266528,-66.1657795405962,-5.55111512312578E-16));
#74077=CARTESIAN_POINT('Origin',(-1.72995545227681E-10,-3.3253631270614E-10,
0.));
#74078=CARTESIAN_POINT('Origin',(-1.72995545227681E-10,-3.3253631270614E-10,
12.));
#74079=CARTESIAN_POINT('Origin',(-1.72995545227681E-10,-3.3253631270614E-10,
0.));
#74080=CARTESIAN_POINT('Ctrl Pts',(-40.2823469776966,-62.6704278106386,
0.));
#74081=CARTESIAN_POINT('Ctrl Pts',(-40.2823469776966,-62.6704278106386,
4.));
#74082=CARTESIAN_POINT('Ctrl Pts',(-40.2823469776966,-62.6704278106386,
8.));
#74083=CARTESIAN_POINT('Ctrl Pts',(-40.2823469776966,-62.6704278106386,
12.));
#74084=CARTESIAN_POINT('Ctrl Pts',(-40.3747816242709,-62.6110140705996,
0.));
#74085=CARTESIAN_POINT('Ctrl Pts',(-40.3747816242709,-62.6110140705996,
4.));
#74086=CARTESIAN_POINT('Ctrl Pts',(-40.3747816242709,-62.6110140705997,
8.00000000000001));
#74087=CARTESIAN_POINT('Ctrl Pts',(-40.3747816242709,-62.6110140705997,
12.));
#74088=CARTESIAN_POINT('Ctrl Pts',(-40.5004281293558,-62.4519997852061,
0.));
#74089=CARTESIAN_POINT('Ctrl Pts',(-40.5004281293558,-62.4519997852061,
4.));
#74090=CARTESIAN_POINT('Ctrl Pts',(-40.5004281293557,-62.4519997852062,
7.99999999999999));
#74091=CARTESIAN_POINT('Ctrl Pts',(-40.5004281293557,-62.4519997852062,
12.));
#74092=CARTESIAN_POINT('Ctrl Pts',(-40.5187208145706,-62.2544389573114,
0.));
#74093=CARTESIAN_POINT('Ctrl Pts',(-40.5187208145706,-62.2544389573114,
4.));
#74094=CARTESIAN_POINT('Ctrl Pts',(-40.5187208145705,-62.2544389573115,
8.00000000000001));
#74095=CARTESIAN_POINT('Ctrl Pts',(-40.5187208145705,-62.2544389573115,
12.));
#74096=CARTESIAN_POINT('Ctrl Pts',(-40.506059810084,-62.173005475645,0.));
#74097=CARTESIAN_POINT('Ctrl Pts',(-40.506059810084,-62.173005475645,4.));
#74098=CARTESIAN_POINT('Ctrl Pts',(-40.5060598100839,-62.1730054756452,
8.));
#74099=CARTESIAN_POINT('Ctrl Pts',(-40.5060598100839,-62.1730054756452,
12.));
#74100=CARTESIAN_POINT('',(-40.2823469776966,-62.6704278106386,0.));
#74101=CARTESIAN_POINT('',(-40.5060598100838,-62.1730054756451,0.));
#74102=CARTESIAN_POINT('Ctrl Pts',(-40.2823469776966,-62.6704278106386,
0.));
#74103=CARTESIAN_POINT('Ctrl Pts',(-40.3747816242709,-62.6110140705996,
0.));
#74104=CARTESIAN_POINT('Ctrl Pts',(-40.4465796271766,-62.5201487646605,
0.));
#74105=CARTESIAN_POINT('Ctrl Pts',(-40.4833233215532,-62.4166968325985,
0.));
#74106=CARTESIAN_POINT('Ctrl Pts',(-40.5108810923357,-62.339107883552,0.));
#74107=CARTESIAN_POINT('Ctrl Pts',(-40.5187208145706,-62.2544389573114,
0.));
#74108=CARTESIAN_POINT('Ctrl Pts',(-40.506059810084,-62.173005475645,0.));
#74109=CARTESIAN_POINT('',(-40.5060598100838,-62.1730054756452,12.));
#74110=CARTESIAN_POINT('Ctrl Pts',(-40.506059810084,-62.173005475645,0.));
#74111=CARTESIAN_POINT('Ctrl Pts',(-40.506059810084,-62.173005475645,4.));
#74112=CARTESIAN_POINT('Ctrl Pts',(-40.5060598100839,-62.1730054756452,
8.));
#74113=CARTESIAN_POINT('Ctrl Pts',(-40.5060598100839,-62.1730054756452,
12.));
#74114=CARTESIAN_POINT('',(-40.2823469776966,-62.6704278106386,12.));
#74115=CARTESIAN_POINT('Ctrl Pts',(-40.5060598100839,-62.1730054756452,
12.));
#74116=CARTESIAN_POINT('Ctrl Pts',(-40.5187208145705,-62.2544389573115,
12.));
#74117=CARTESIAN_POINT('Ctrl Pts',(-40.5108810923356,-62.3391078835521,
12.));
#74118=CARTESIAN_POINT('Ctrl Pts',(-40.4833233215531,-62.4166968325986,
12.));
#74119=CARTESIAN_POINT('Ctrl Pts',(-40.4465796271765,-62.5201487646605,
12.));
#74120=CARTESIAN_POINT('Ctrl Pts',(-40.3747816242709,-62.6110140705997,
12.));
#74121=CARTESIAN_POINT('Ctrl Pts',(-40.2823469776966,-62.6704278106386,
12.));
#74122=CARTESIAN_POINT('Ctrl Pts',(-40.2823469776966,-62.6704278106386,
12.));
#74123=CARTESIAN_POINT('Ctrl Pts',(-40.2823469776966,-62.6704278106386,
8.));
#74124=CARTESIAN_POINT('Ctrl Pts',(-40.2823469776966,-62.6704278106386,
4.));
#74125=CARTESIAN_POINT('Ctrl Pts',(-40.2823469776966,-62.6704278106386,
0.));
#74126=CARTESIAN_POINT('Ctrl Pts',(-39.4479504917287,-57.8261117662438,
0.));
#74127=CARTESIAN_POINT('Ctrl Pts',(-39.4479504917287,-57.8261117662438,
12.));
#74128=CARTESIAN_POINT('Ctrl Pts',(-39.4492429618443,-57.8297740100947,
0.));
#74129=CARTESIAN_POINT('Ctrl Pts',(-39.4492429618443,-57.8297740100947,
12.));
#74130=CARTESIAN_POINT('Ctrl Pts',(-39.4518277003553,-57.837104315141,0.));
#74131=CARTESIAN_POINT('Ctrl Pts',(-39.4518277003553,-57.837104315141,12.));
#74132=CARTESIAN_POINT('Ctrl Pts',(-39.4557042029652,-57.8481172247495,
0.));
#74133=CARTESIAN_POINT('Ctrl Pts',(-39.4557042029652,-57.8481172247495,
12.));
#74134=CARTESIAN_POINT('Ctrl Pts',(-39.4608716627118,-57.8628360096803,
0.));
#74135=CARTESIAN_POINT('Ctrl Pts',(-39.4608716627118,-57.8628360096803,
12.));
#74136=CARTESIAN_POINT('Ctrl Pts',(-39.4673289592259,-57.8812926637177,
0.));
#74137=CARTESIAN_POINT('Ctrl Pts',(-39.4673289592259,-57.8812926637177,
12.));
#74138=CARTESIAN_POINT('Ctrl Pts',(-39.473784194937,-57.8998074670478,0.));
#74139=CARTESIAN_POINT('Ctrl Pts',(-39.473784194937,-57.8998074670478,12.));
#74140=CARTESIAN_POINT('Ctrl Pts',(-39.4802373061058,-57.9183803632403,
0.));
#74141=CARTESIAN_POINT('Ctrl Pts',(-39.4802373061058,-57.9183803632403,
12.));
#74142=CARTESIAN_POINT('Ctrl Pts',(-39.4866881842317,-57.937011245663,0.));
#74143=CARTESIAN_POINT('Ctrl Pts',(-39.4866881842317,-57.937011245663,12.));
#74144=CARTESIAN_POINT('Ctrl Pts',(-39.4931366776714,-57.9556999583892,
0.));
#74145=CARTESIAN_POINT('Ctrl Pts',(-39.4931366776714,-57.9556999583892,
12.));
#74146=CARTESIAN_POINT('Ctrl Pts',(-39.499582610674,-57.974446317937,0.));
#74147=CARTESIAN_POINT('Ctrl Pts',(-39.499582610674,-57.974446317937,12.));
#74148=CARTESIAN_POINT('Ctrl Pts',(-39.5060257981225,-57.9932501298522,
0.));
#74149=CARTESIAN_POINT('Ctrl Pts',(-39.5060257981225,-57.9932501298522,
12.));
#74150=CARTESIAN_POINT('Ctrl Pts',(-39.5124660614976,-58.0121112067895,
0.));
#74151=CARTESIAN_POINT('Ctrl Pts',(-39.5124660614976,-58.0121112067895,
12.));
#74152=CARTESIAN_POINT('Ctrl Pts',(-39.5189032457184,-58.0310293875262,
0.));
#74153=CARTESIAN_POINT('Ctrl Pts',(-39.5189032457184,-58.0310293875262,
12.));
#74154=CARTESIAN_POINT('Ctrl Pts',(-39.5253372136887,-58.0500045308412,
0.));
#74155=CARTESIAN_POINT('Ctrl Pts',(-39.5253372136887,-58.0500045308412,
12.));
#74156=CARTESIAN_POINT('Ctrl Pts',(-39.5317678383217,-58.0690365065374,
0.));
#74157=CARTESIAN_POINT('Ctrl Pts',(-39.5317678383217,-58.0690365065374,
12.));
#74158=CARTESIAN_POINT('Ctrl Pts',(-39.5381949959221,-58.088125187992,0.));
#74159=CARTESIAN_POINT('Ctrl Pts',(-39.5381949959221,-58.088125187992,12.));
#74160=CARTESIAN_POINT('Ctrl Pts',(-39.5446185579638,-58.1072704428928,
0.));
#74161=CARTESIAN_POINT('Ctrl Pts',(-39.5446185579638,-58.1072704428928,
12.));
#74162=CARTESIAN_POINT('Ctrl Pts',(-39.5510383869505,-58.126472128574,0.));
#74163=CARTESIAN_POINT('Ctrl Pts',(-39.5510383869505,-58.126472128574,12.));
#74164=CARTESIAN_POINT('Ctrl Pts',(-39.5574543406982,-58.1457300968499,
0.));
#74165=CARTESIAN_POINT('Ctrl Pts',(-39.5574543406982,-58.1457300968499,
12.));
#74166=CARTESIAN_POINT('Ctrl Pts',(-39.563866275018,-58.1650441970387,0.));
#74167=CARTESIAN_POINT('Ctrl Pts',(-39.563866275018,-58.1650441970387,12.));
#74168=CARTESIAN_POINT('Ctrl Pts',(-39.5702740467999,-58.1844142794338,
0.));
#74169=CARTESIAN_POINT('Ctrl Pts',(-39.5702740467999,-58.1844142794338,
12.));
#74170=CARTESIAN_POINT('Ctrl Pts',(-39.57667751752,-58.2038401992457,0.));
#74171=CARTESIAN_POINT('Ctrl Pts',(-39.57667751752,-58.2038401992457,12.));
#74172=CARTESIAN_POINT('Ctrl Pts',(-39.5830765530891,-58.2233218164365,
0.));
#74173=CARTESIAN_POINT('Ctrl Pts',(-39.5830765530891,-58.2233218164365,
12.));
#74174=CARTESIAN_POINT('Ctrl Pts',(-39.5894710221713,-58.2428589938369,
0.));
#74175=CARTESIAN_POINT('Ctrl Pts',(-39.5894710221713,-58.2428589938369,
12.));
#74176=CARTESIAN_POINT('Ctrl Pts',(-39.5958607950239,-58.2624515958419,
0.));
#74177=CARTESIAN_POINT('Ctrl Pts',(-39.5958607950239,-58.2624515958419,
12.));
#74178=CARTESIAN_POINT('Ctrl Pts',(-39.602245742079,-58.2820994868118,0.));
#74179=CARTESIAN_POINT('Ctrl Pts',(-39.602245742079,-58.2820994868118,12.));
#74180=CARTESIAN_POINT('Ctrl Pts',(-39.6086257327583,-58.3018025297323,
0.));
#74181=CARTESIAN_POINT('Ctrl Pts',(-39.6086257327583,-58.3018025297323,
12.));
#74182=CARTESIAN_POINT('Ctrl Pts',(-39.6150006360914,-58.3215605869221,
0.));
#74183=CARTESIAN_POINT('Ctrl Pts',(-39.6150006360914,-58.3215605869221,
12.));
#74184=CARTESIAN_POINT('Ctrl Pts',(-39.6213703212531,-58.3413735206423,
0.));
#74185=CARTESIAN_POINT('Ctrl Pts',(-39.6213703212531,-58.3413735206423,
12.));
#74186=CARTESIAN_POINT('Ctrl Pts',(-39.6277346580892,-58.3612411936904,
0.));
#74187=CARTESIAN_POINT('Ctrl Pts',(-39.6277346580892,-58.3612411936904,
12.));
#74188=CARTESIAN_POINT('Ctrl Pts',(-39.6340935177476,-58.3811634701037,
0.));
#74189=CARTESIAN_POINT('Ctrl Pts',(-39.6340935177476,-58.3811634701037,
12.));
#74190=CARTESIAN_POINT('Ctrl Pts',(-39.6404467729094,-58.4011402154196,
0.));
#74191=CARTESIAN_POINT('Ctrl Pts',(-39.6404467729094,-58.4011402154196,
12.));
#74192=CARTESIAN_POINT('Ctrl Pts',(-39.6467942974451,-58.4211712963004,
0.));
#74193=CARTESIAN_POINT('Ctrl Pts',(-39.6467942974451,-58.4211712963004,
12.));
#74194=CARTESIAN_POINT('Ctrl Pts',(-39.653135966204,-58.4412565802979,0.));
#74195=CARTESIAN_POINT('Ctrl Pts',(-39.653135966204,-58.4412565802979,12.));
#74196=CARTESIAN_POINT('Ctrl Pts',(-39.6594716547689,-58.4613959355788,
0.));
#74197=CARTESIAN_POINT('Ctrl Pts',(-39.6594716547689,-58.4613959355788,
12.));
#74198=CARTESIAN_POINT('Ctrl Pts',(-39.6658012391815,-58.4815892306066,
0.));
#74199=CARTESIAN_POINT('Ctrl Pts',(-39.6658012391815,-58.4815892306066,
12.));
#74200=CARTESIAN_POINT('Ctrl Pts',(-39.6721245959531,-58.5018363341604,
0.));
#74201=CARTESIAN_POINT('Ctrl Pts',(-39.6721245959531,-58.5018363341604,
12.));
#74202=CARTESIAN_POINT('Ctrl Pts',(-39.6784416021826,-58.522137115476,0.));
#74203=CARTESIAN_POINT('Ctrl Pts',(-39.6784416021826,-58.522137115476,12.));
#74204=CARTESIAN_POINT('Ctrl Pts',(-39.6847521356395,-58.5424914443415,
0.));
#74205=CARTESIAN_POINT('Ctrl Pts',(-39.6847521356395,-58.5424914443415,
12.));
#74206=CARTESIAN_POINT('Ctrl Pts',(-39.6910560748629,-58.5628991912052,
0.));
#74207=CARTESIAN_POINT('Ctrl Pts',(-39.6910560748629,-58.5628991912052,
12.));
#74208=CARTESIAN_POINT('Ctrl Pts',(-39.6973532992539,-58.5833602272743,
0.));
#74209=CARTESIAN_POINT('Ctrl Pts',(-39.6973532992539,-58.5833602272743,
12.));
#74210=CARTESIAN_POINT('Ctrl Pts',(-39.7036436890233,-58.6038744244659,
0.));
#74211=CARTESIAN_POINT('Ctrl Pts',(-39.7036436890233,-58.6038744244659,
12.));
#74212=CARTESIAN_POINT('Ctrl Pts',(-39.7099271251413,-58.6244416553562,
0.));
#74213=CARTESIAN_POINT('Ctrl Pts',(-39.7099271251413,-58.6244416553562,
12.));
#74214=CARTESIAN_POINT('Ctrl Pts',(-39.7162034892899,-58.6450617931274,
0.));
#74215=CARTESIAN_POINT('Ctrl Pts',(-39.7162034892899,-58.6450617931274,
12.));
#74216=CARTESIAN_POINT('Ctrl Pts',(-39.7224726638101,-58.6657347115034,
0.));
#74217=CARTESIAN_POINT('Ctrl Pts',(-39.7224726638101,-58.6657347115034,
12.));
#74218=CARTESIAN_POINT('Ctrl Pts',(-39.7287345316681,-58.6864602847088,
0.));
#74219=CARTESIAN_POINT('Ctrl Pts',(-39.7287345316681,-58.6864602847088,
12.));
#74220=CARTESIAN_POINT('Ctrl Pts',(-39.734988976475,-58.7072383875027,0.));
#74221=CARTESIAN_POINT('Ctrl Pts',(-39.734988976475,-58.7072383875027,12.));
#74222=CARTESIAN_POINT('Ctrl Pts',(-39.7412358824953,-58.7280688951916,
0.));
#74223=CARTESIAN_POINT('Ctrl Pts',(-39.7412358824953,-58.7280688951916,
12.));
#74224=CARTESIAN_POINT('Ctrl Pts',(-39.7474751346598,-58.7489516836445,
0.));
#74225=CARTESIAN_POINT('Ctrl Pts',(-39.7474751346598,-58.7489516836445,
12.));
#74226=CARTESIAN_POINT('Ctrl Pts',(-39.7537066185813,-58.7698866293029,
0.));
#74227=CARTESIAN_POINT('Ctrl Pts',(-39.7537066185813,-58.7698866293029,
12.));
#74228=CARTESIAN_POINT('Ctrl Pts',(-39.7599302205521,-58.7908736091798,
0.));
#74229=CARTESIAN_POINT('Ctrl Pts',(-39.7599302205521,-58.7908736091798,
12.));
#74230=CARTESIAN_POINT('Ctrl Pts',(-39.7661458275274,-58.8119125008517,
0.));
#74231=CARTESIAN_POINT('Ctrl Pts',(-39.7661458275274,-58.8119125008517,
12.));
#74232=CARTESIAN_POINT('Ctrl Pts',(-39.772353327112,-58.8330031824453,0.));
#74233=CARTESIAN_POINT('Ctrl Pts',(-39.772353327112,-58.8330031824453,12.));
#74234=CARTESIAN_POINT('Ctrl Pts',(-39.7785526075478,-58.8541455326231,
0.));
#74235=CARTESIAN_POINT('Ctrl Pts',(-39.7785526075478,-58.8541455326231,
12.));
#74236=CARTESIAN_POINT('Ctrl Pts',(-39.7847435576996,-58.8753394305585,
0.));
#74237=CARTESIAN_POINT('Ctrl Pts',(-39.7847435576996,-58.8753394305585,
12.));
#74238=CARTESIAN_POINT('Ctrl Pts',(-39.7909260670517,-58.8965847559391,
0.));
#74239=CARTESIAN_POINT('Ctrl Pts',(-39.7909260670517,-58.8965847559391,
12.));
#74240=CARTESIAN_POINT('Ctrl Pts',(-39.7971000257044,-58.9178813889703,
0.));
#74241=CARTESIAN_POINT('Ctrl Pts',(-39.7971000257044,-58.9178813889703,
12.));
#74242=CARTESIAN_POINT('Ctrl Pts',(-39.8032653243712,-58.9392292103747,
0.));
#74243=CARTESIAN_POINT('Ctrl Pts',(-39.8032653243712,-58.9392292103747,
12.));
#74244=CARTESIAN_POINT('Ctrl Pts',(-39.8094218543782,-58.9606281013875,
0.));
#74245=CARTESIAN_POINT('Ctrl Pts',(-39.8094218543782,-58.9606281013875,
12.));
#74246=CARTESIAN_POINT('Ctrl Pts',(-39.8155695076626,-58.9820779437484,
0.));
#74247=CARTESIAN_POINT('Ctrl Pts',(-39.8155695076626,-58.9820779437484,
12.));
#74248=CARTESIAN_POINT('Ctrl Pts',(-39.821708176766,-59.0035786197024,0.));
#74249=CARTESIAN_POINT('Ctrl Pts',(-39.821708176766,-59.0035786197024,12.));
#74250=CARTESIAN_POINT('Ctrl Pts',(-39.8278377548262,-59.0251300119973,
0.));
#74251=CARTESIAN_POINT('Ctrl Pts',(-39.8278377548262,-59.0251300119973,
12.));
#74252=CARTESIAN_POINT('Ctrl Pts',(-39.8339581355716,-59.0467320038784,
0.));
#74253=CARTESIAN_POINT('Ctrl Pts',(-39.8339581355716,-59.0467320038784,
12.));
#74254=CARTESIAN_POINT('Ctrl Pts',(-39.8400692133139,-59.0683844790764,
0.));
#74255=CARTESIAN_POINT('Ctrl Pts',(-39.8400692133139,-59.0683844790764,
12.));
#74256=CARTESIAN_POINT('Ctrl Pts',(-39.8461708829456,-59.090087321798,0.));
#74257=CARTESIAN_POINT('Ctrl Pts',(-39.8461708829456,-59.090087321798,12.));
#74258=CARTESIAN_POINT('Ctrl Pts',(-39.8522630399328,-59.1118404167292,
0.));
#74259=CARTESIAN_POINT('Ctrl Pts',(-39.8522630399328,-59.1118404167292,
12.));
#74260=CARTESIAN_POINT('Ctrl Pts',(-39.8583455803105,-59.1336436490342,
0.));
#74261=CARTESIAN_POINT('Ctrl Pts',(-39.8583455803105,-59.1336436490342,
12.));
#74262=CARTESIAN_POINT('Ctrl Pts',(-39.8644184006787,-59.1554969043522,
0.));
#74263=CARTESIAN_POINT('Ctrl Pts',(-39.8644184006787,-59.1554969043522,
12.));
#74264=CARTESIAN_POINT('Ctrl Pts',(-39.8704813981988,-59.1774000687879,
0.));
#74265=CARTESIAN_POINT('Ctrl Pts',(-39.8704813981988,-59.1774000687879,
12.));
#74266=CARTESIAN_POINT('Ctrl Pts',(-39.876534470591,-59.1993530289028,0.));
#74267=CARTESIAN_POINT('Ctrl Pts',(-39.876534470591,-59.1993530289028,12.));
#74268=CARTESIAN_POINT('Ctrl Pts',(-39.8825775161267,-59.2213556717209,
0.));
#74269=CARTESIAN_POINT('Ctrl Pts',(-39.8825775161267,-59.2213556717209,
12.));
#74270=CARTESIAN_POINT('Ctrl Pts',(-39.8886104336242,-59.2434078847247,
0.));
#74271=CARTESIAN_POINT('Ctrl Pts',(-39.8886104336242,-59.2434078847247,
12.));
#74272=CARTESIAN_POINT('Ctrl Pts',(-39.8946331224438,-59.2655095558521,
0.));
#74273=CARTESIAN_POINT('Ctrl Pts',(-39.8946331224438,-59.2655095558521,
12.));
#74274=CARTESIAN_POINT('Ctrl Pts',(-39.9006454824845,-59.2876605734846,
0.));
#74275=CARTESIAN_POINT('Ctrl Pts',(-39.9006454824845,-59.2876605734846,
12.));
#74276=CARTESIAN_POINT('Ctrl Pts',(-39.9066474141803,-59.3098608264419,
0.));
#74277=CARTESIAN_POINT('Ctrl Pts',(-39.9066474141803,-59.3098608264419,
12.));
#74278=CARTESIAN_POINT('Ctrl Pts',(-39.9126388184936,-59.3321102039852,
0.));
#74279=CARTESIAN_POINT('Ctrl Pts',(-39.9126388184936,-59.3321102039852,
12.));
#74280=CARTESIAN_POINT('Ctrl Pts',(-39.9186195969104,-59.3544085958151,
0.));
#74281=CARTESIAN_POINT('Ctrl Pts',(-39.9186195969104,-59.3544085958151,
12.));
#74282=CARTESIAN_POINT('Ctrl Pts',(-39.9245896514367,-59.3767558920675,
0.));
#74283=CARTESIAN_POINT('Ctrl Pts',(-39.9245896514367,-59.3767558920675,
12.));
#74284=CARTESIAN_POINT('Ctrl Pts',(-39.9305488845958,-59.3991519833016,
0.));
#74285=CARTESIAN_POINT('Ctrl Pts',(-39.9305488845958,-59.3991519833016,
12.));
#74286=CARTESIAN_POINT('Ctrl Pts',(-39.9364971994242,-59.4215967604967,
0.));
#74287=CARTESIAN_POINT('Ctrl Pts',(-39.9364971994242,-59.4215967604967,
12.));
#74288=CARTESIAN_POINT('Ctrl Pts',(-39.9424344994672,-59.4440901150582,
0.));
#74289=CARTESIAN_POINT('Ctrl Pts',(-39.9424344994672,-59.4440901150582,
12.));
#74290=CARTESIAN_POINT('Ctrl Pts',(-39.9483606887737,-59.4666319388133,
0.));
#74291=CARTESIAN_POINT('Ctrl Pts',(-39.9483606887737,-59.4666319388133,
12.));
#74292=CARTESIAN_POINT('Ctrl Pts',(-39.9542756718922,-59.4892221240068,
0.));
#74293=CARTESIAN_POINT('Ctrl Pts',(-39.9542756718922,-59.4892221240068,
12.));
#74294=CARTESIAN_POINT('Ctrl Pts',(-39.9601793538682,-59.511860563289,0.));
#74295=CARTESIAN_POINT('Ctrl Pts',(-39.9601793538682,-59.511860563289,12.));
#74296=CARTESIAN_POINT('Ctrl Pts',(-39.9660716402403,-59.5345471497128,
0.));
#74297=CARTESIAN_POINT('Ctrl Pts',(-39.9660716402403,-59.5345471497128,
12.));
#74298=CARTESIAN_POINT('Ctrl Pts',(-39.9719524370345,-59.5572817767388,
0.));
#74299=CARTESIAN_POINT('Ctrl Pts',(-39.9719524370345,-59.5572817767388,
12.));
#74300=CARTESIAN_POINT('Ctrl Pts',(-39.9778216507605,-59.5800643382314,
0.));
#74301=CARTESIAN_POINT('Ctrl Pts',(-39.9778216507605,-59.5800643382314,
12.));
#74302=CARTESIAN_POINT('Ctrl Pts',(-39.9836791884079,-59.6028947284562,
0.));
#74303=CARTESIAN_POINT('Ctrl Pts',(-39.9836791884079,-59.6028947284562,
12.));
#74304=CARTESIAN_POINT('Ctrl Pts',(-39.9895249574448,-59.6257728420669,
0.));
#74305=CARTESIAN_POINT('Ctrl Pts',(-39.9895249574448,-59.6257728420669,
12.));
#74306=CARTESIAN_POINT('Ctrl Pts',(-39.9953588658132,-59.6486985741041,
0.));
#74307=CARTESIAN_POINT('Ctrl Pts',(-39.9953588658132,-59.6486985741041,
12.));
#74308=CARTESIAN_POINT('Ctrl Pts',(-40.0011808219241,-59.6716718200005,
0.));
#74309=CARTESIAN_POINT('Ctrl Pts',(-40.0011808219241,-59.6716718200005,
12.));
#74310=CARTESIAN_POINT('Ctrl Pts',(-40.0069907346537,-59.6946924755773,
0.));
#74311=CARTESIAN_POINT('Ctrl Pts',(-40.0069907346537,-59.6946924755773,
12.));
#74312=CARTESIAN_POINT('Ctrl Pts',(-40.0127885133403,-59.7177604370403,
0.));
#74313=CARTESIAN_POINT('Ctrl Pts',(-40.0127885133403,-59.7177604370403,
12.));
#74314=CARTESIAN_POINT('Ctrl Pts',(-40.0185740677821,-59.7408756009679,
0.));
#74315=CARTESIAN_POINT('Ctrl Pts',(-40.0185740677821,-59.7408756009679,
12.));
#74316=CARTESIAN_POINT('Ctrl Pts',(-40.0243473082337,-59.7640378643106,
0.));
#74317=CARTESIAN_POINT('Ctrl Pts',(-40.0243473082337,-59.7640378643106,
12.));
#74318=CARTESIAN_POINT('Ctrl Pts',(-40.0301081454002,-59.7872471243942,
0.));
#74319=CARTESIAN_POINT('Ctrl Pts',(-40.0301081454002,-59.7872471243942,
12.));
#74320=CARTESIAN_POINT('Ctrl Pts',(-40.0358564904341,-59.8105032789179,
0.));
#74321=CARTESIAN_POINT('Ctrl Pts',(-40.0358564904341,-59.8105032789179,
12.));
#74322=CARTESIAN_POINT('Ctrl Pts',(-40.0415922549315,-59.8338062259492,
0.));
#74323=CARTESIAN_POINT('Ctrl Pts',(-40.0415922549315,-59.8338062259492,
12.));
#74324=CARTESIAN_POINT('Ctrl Pts',(-40.0473153509324,-59.8571558639145,
0.));
#74325=CARTESIAN_POINT('Ctrl Pts',(-40.0473153509324,-59.8571558639145,
12.));
#74326=CARTESIAN_POINT('Ctrl Pts',(-40.0530256909161,-59.8805520915972,
0.));
#74327=CARTESIAN_POINT('Ctrl Pts',(-40.0530256909161,-59.8805520915972,
12.));
#74328=CARTESIAN_POINT('Ctrl Pts',(-40.0587231877959,-59.9039948081428,
0.));
#74329=CARTESIAN_POINT('Ctrl Pts',(-40.0587231877959,-59.9039948081428,
12.));
#74330=CARTESIAN_POINT('Ctrl Pts',(-40.0644077549158,-59.927483913055,0.));
#74331=CARTESIAN_POINT('Ctrl Pts',(-40.0644077549158,-59.927483913055,12.));
#74332=CARTESIAN_POINT('Ctrl Pts',(-40.0700793060475,-59.9510193061929,
0.));
#74333=CARTESIAN_POINT('Ctrl Pts',(-40.0700793060475,-59.9510193061929,
12.));
#74334=CARTESIAN_POINT('Ctrl Pts',(-40.0757377553893,-59.974600887759,0.));
#74335=CARTESIAN_POINT('Ctrl Pts',(-40.0757377553893,-59.974600887759,12.));
#74336=CARTESIAN_POINT('Ctrl Pts',(-40.0813830175629,-59.9982285582991,
0.));
#74337=CARTESIAN_POINT('Ctrl Pts',(-40.0813830175629,-59.9982285582991,
12.));
#74338=CARTESIAN_POINT('Ctrl Pts',(-40.0870150076078,-60.0219022187066,
0.));
#74339=CARTESIAN_POINT('Ctrl Pts',(-40.0870150076078,-60.0219022187066,
12.));
#74340=CARTESIAN_POINT('Ctrl Pts',(-40.0926336409787,-60.0456217702203,
0.));
#74341=CARTESIAN_POINT('Ctrl Pts',(-40.0926336409787,-60.0456217702203,
12.));
#74342=CARTESIAN_POINT('Ctrl Pts',(-40.0982388335421,-60.0693871144207,
0.));
#74343=CARTESIAN_POINT('Ctrl Pts',(-40.0982388335421,-60.0693871144207,
12.));
#74344=CARTESIAN_POINT('Ctrl Pts',(-40.1038305015763,-60.0931981532194,
0.));
#74345=CARTESIAN_POINT('Ctrl Pts',(-40.1038305015763,-60.0931981532194,
12.));
#74346=CARTESIAN_POINT('Ctrl Pts',(-40.1094085617672,-60.1170547888572,
0.));
#74347=CARTESIAN_POINT('Ctrl Pts',(-40.1094085617672,-60.1170547888572,
12.));
#74348=CARTESIAN_POINT('Ctrl Pts',(-40.1149729312036,-60.1409569239092,
0.));
#74349=CARTESIAN_POINT('Ctrl Pts',(-40.1149729312036,-60.1409569239092,
12.));
#74350=CARTESIAN_POINT('Ctrl Pts',(-40.120523527374,-60.1649044612829,0.));
#74351=CARTESIAN_POINT('Ctrl Pts',(-40.120523527374,-60.1649044612829,12.));
#74352=CARTESIAN_POINT('Ctrl Pts',(-40.1260602681644,-60.1888973042151,
0.));
#74353=CARTESIAN_POINT('Ctrl Pts',(-40.1260602681644,-60.1888973042151,
12.));
#74354=CARTESIAN_POINT('Ctrl Pts',(-40.1315830718575,-60.2129353562617,
0.));
#74355=CARTESIAN_POINT('Ctrl Pts',(-40.1315830718575,-60.2129353562617,
12.));
#74356=CARTESIAN_POINT('Ctrl Pts',(-40.13709185713,-60.2370185212957,0.));
#74357=CARTESIAN_POINT('Ctrl Pts',(-40.13709185713,-60.2370185212957,12.));
#74358=CARTESIAN_POINT('Ctrl Pts',(-40.1425865430468,-60.2611467035109,
0.));
#74359=CARTESIAN_POINT('Ctrl Pts',(-40.1425865430468,-60.2611467035109,
12.));
#74360=CARTESIAN_POINT('Ctrl Pts',(-40.1480670490583,-60.2853198074215,
0.));
#74361=CARTESIAN_POINT('Ctrl Pts',(-40.1480670490583,-60.2853198074215,
12.));
#74362=CARTESIAN_POINT('Ctrl Pts',(-40.1535332949978,-60.3095377378589,
0.));
#74363=CARTESIAN_POINT('Ctrl Pts',(-40.1535332949978,-60.3095377378589,
12.));
#74364=CARTESIAN_POINT('Ctrl Pts',(-40.1589852010811,-60.3338003999616,
0.));
#74365=CARTESIAN_POINT('Ctrl Pts',(-40.1589852010811,-60.3338003999616,
12.));
#74366=CARTESIAN_POINT('Ctrl Pts',(-40.1644226879043,-60.3581076991731,
0.));
#74367=CARTESIAN_POINT('Ctrl Pts',(-40.1644226879043,-60.3581076991731,
12.));
#74368=CARTESIAN_POINT('Ctrl Pts',(-40.1698456764387,-60.382459541246,0.));
#74369=CARTESIAN_POINT('Ctrl Pts',(-40.1698456764387,-60.382459541246,12.));
#74370=CARTESIAN_POINT('Ctrl Pts',(-40.1752540880273,-60.4068558322414,
0.));
#74371=CARTESIAN_POINT('Ctrl Pts',(-40.1752540880273,-60.4068558322414,
12.));
#74372=CARTESIAN_POINT('Ctrl Pts',(-40.1806478443828,-60.4312964785269,
0.));
#74373=CARTESIAN_POINT('Ctrl Pts',(-40.1806478443828,-60.4312964785269,
12.));
#74374=CARTESIAN_POINT('Ctrl Pts',(-40.1860268675875,-60.4557813867677,
0.));
#74375=CARTESIAN_POINT('Ctrl Pts',(-40.1860268675875,-60.4557813867677,
12.));
#74376=CARTESIAN_POINT('Ctrl Pts',(-40.1913910800911,-60.4803104639211,
0.));
#74377=CARTESIAN_POINT('Ctrl Pts',(-40.1913910800911,-60.4803104639211,
12.));
#74378=CARTESIAN_POINT('Ctrl Pts',(-40.1967404047055,-60.5048836172423,
0.));
#74379=CARTESIAN_POINT('Ctrl Pts',(-40.1967404047055,-60.5048836172423,
12.));
#74380=CARTESIAN_POINT('Ctrl Pts',(-40.2020747646012,-60.5295007542838,
0.));
#74381=CARTESIAN_POINT('Ctrl Pts',(-40.2020747646012,-60.5295007542838,
12.));
#74382=CARTESIAN_POINT('Ctrl Pts',(-40.2073940833054,-60.5541617828927,
0.));
#74383=CARTESIAN_POINT('Ctrl Pts',(-40.2073940833054,-60.5541617828927,
12.));
#74384=CARTESIAN_POINT('Ctrl Pts',(-40.2126982847012,-60.5788666112043,
0.));
#74385=CARTESIAN_POINT('Ctrl Pts',(-40.2126982847012,-60.5788666112043,
12.));
#74386=CARTESIAN_POINT('Ctrl Pts',(-40.2179872930272,-60.6036151476347,
0.));
#74387=CARTESIAN_POINT('Ctrl Pts',(-40.2179872930272,-60.6036151476347,
12.));
#74388=CARTESIAN_POINT('Ctrl Pts',(-40.2232610328717,-60.6284073008865,
0.));
#74389=CARTESIAN_POINT('Ctrl Pts',(-40.2232610328717,-60.6284073008865,
12.));
#74390=CARTESIAN_POINT('Ctrl Pts',(-40.2285194291702,-60.6532429799493,
0.));
#74391=CARTESIAN_POINT('Ctrl Pts',(-40.2285194291702,-60.6532429799493,
12.));
#74392=CARTESIAN_POINT('Ctrl Pts',(-40.2337624072029,-60.6781220940979,
0.));
#74393=CARTESIAN_POINT('Ctrl Pts',(-40.2337624072029,-60.6781220940979,
12.));
#74394=CARTESIAN_POINT('Ctrl Pts',(-40.2389898925937,-60.7030445528863,
0.));
#74395=CARTESIAN_POINT('Ctrl Pts',(-40.2389898925937,-60.7030445528863,
12.));
#74396=CARTESIAN_POINT('Ctrl Pts',(-40.2442018113116,-60.72801026614,0.));
#74397=CARTESIAN_POINT('Ctrl Pts',(-40.2442018113116,-60.72801026614,12.));
#74398=CARTESIAN_POINT('Ctrl Pts',(-40.2493980896646,-60.7530191439603,
0.));
#74399=CARTESIAN_POINT('Ctrl Pts',(-40.2493980896646,-60.7530191439603,
12.));
#74400=CARTESIAN_POINT('Ctrl Pts',(-40.2545786542957,-60.7780710967253,
0.));
#74401=CARTESIAN_POINT('Ctrl Pts',(-40.2545786542957,-60.7780710967253,
12.));
#74402=CARTESIAN_POINT('Ctrl Pts',(-40.2597434321804,-60.8031660350878,
0.));
#74403=CARTESIAN_POINT('Ctrl Pts',(-40.2597434321804,-60.8031660350878,
12.));
#74404=CARTESIAN_POINT('Ctrl Pts',(-40.2648923506245,-60.8283038699703,
0.));
#74405=CARTESIAN_POINT('Ctrl Pts',(-40.2648923506245,-60.8283038699703,
12.));
#74406=CARTESIAN_POINT('Ctrl Pts',(-40.2700253372644,-60.8534845125535,
0.));
#74407=CARTESIAN_POINT('Ctrl Pts',(-40.2700253372644,-60.8534845125535,
12.));
#74408=CARTESIAN_POINT('Ctrl Pts',(-40.2751423200637,-60.8787078742817,
0.));
#74409=CARTESIAN_POINT('Ctrl Pts',(-40.2751423200637,-60.8787078742817,
12.));
#74410=CARTESIAN_POINT('Ctrl Pts',(-40.2802432273105,-60.903973866867,0.));
#74411=CARTESIAN_POINT('Ctrl Pts',(-40.2802432273105,-60.903973866867,12.));
#74412=CARTESIAN_POINT('Ctrl Pts',(-40.2853279876162,-60.9292824022888,
0.));
#74413=CARTESIAN_POINT('Ctrl Pts',(-40.2853279876162,-60.9292824022888,
12.));
#74414=CARTESIAN_POINT('Ctrl Pts',(-40.2903965299155,-60.9546333927919,
0.));
#74415=CARTESIAN_POINT('Ctrl Pts',(-40.2903965299155,-60.9546333927919,
12.));
#74416=CARTESIAN_POINT('Ctrl Pts',(-40.2954487834688,-60.9800267508781,
0.));
#74417=CARTESIAN_POINT('Ctrl Pts',(-40.2954487834688,-60.9800267508781,
12.));
#74418=CARTESIAN_POINT('Ctrl Pts',(-40.3004846778577,-61.0054623893059,
0.));
#74419=CARTESIAN_POINT('Ctrl Pts',(-40.3004846778577,-61.0054623893059,
12.));
#74420=CARTESIAN_POINT('Ctrl Pts',(-40.3055041429772,-61.0309402210915,
0.));
#74421=CARTESIAN_POINT('Ctrl Pts',(-40.3055041429772,-61.0309402210915,
12.));
#74422=CARTESIAN_POINT('Ctrl Pts',(-40.3105071090308,-61.0564601595047,
0.));
#74423=CARTESIAN_POINT('Ctrl Pts',(-40.3105071090308,-61.0564601595047,
12.));
#74424=CARTESIAN_POINT('Ctrl Pts',(-40.3154935065264,-61.0820221180646,
0.));
#74425=CARTESIAN_POINT('Ctrl Pts',(-40.3154935065264,-61.0820221180646,
12.));
#74426=CARTESIAN_POINT('Ctrl Pts',(-40.3204632662729,-61.1076260105265,
0.));
#74427=CARTESIAN_POINT('Ctrl Pts',(-40.3204632662729,-61.1076260105265,
12.));
#74428=CARTESIAN_POINT('Ctrl Pts',(-40.3254163193806,-61.1332717508799,
0.));
#74429=CARTESIAN_POINT('Ctrl Pts',(-40.3254163193806,-61.1332717508799,
12.));
#74430=CARTESIAN_POINT('Ctrl Pts',(-40.3303525972621,-61.1589592533623,
0.));
#74431=CARTESIAN_POINT('Ctrl Pts',(-40.3303525972621,-61.1589592533623,
12.));
#74432=CARTESIAN_POINT('Ctrl Pts',(-40.3352720316373,-61.184688432465,0.));
#74433=CARTESIAN_POINT('Ctrl Pts',(-40.3352720316373,-61.184688432465,12.));
#74434=CARTESIAN_POINT('Ctrl Pts',(-40.3401745545369,-61.2104592029375,
0.));
#74435=CARTESIAN_POINT('Ctrl Pts',(-40.3401745545369,-61.2104592029375,
12.));
#74436=CARTESIAN_POINT('Ctrl Pts',(-40.3450600983104,-61.236271479789,0.));
#74437=CARTESIAN_POINT('Ctrl Pts',(-40.3450600983104,-61.236271479789,12.));
#74438=CARTESIAN_POINT('Ctrl Pts',(-40.3499285956297,-61.2621251782849,
0.));
#74439=CARTESIAN_POINT('Ctrl Pts',(-40.3499285956297,-61.2621251782849,
12.));
#74440=CARTESIAN_POINT('Ctrl Pts',(-40.3547799794672,-61.2880202139358,
0.));
#74441=CARTESIAN_POINT('Ctrl Pts',(-40.3547799794672,-61.2880202139358,
12.));
#74442=CARTESIAN_POINT('Ctrl Pts',(-40.3596141830786,-61.3139565024838,
0.));
#74443=CARTESIAN_POINT('Ctrl Pts',(-40.3596141830786,-61.3139565024838,
12.));
#74444=CARTESIAN_POINT('Ctrl Pts',(-40.3644311399861,-61.3399339598851,
0.));
#74445=CARTESIAN_POINT('Ctrl Pts',(-40.3644311399861,-61.3399339598851,
12.));
#74446=CARTESIAN_POINT('Ctrl Pts',(-40.3692307839642,-61.3659525022917,
0.));
#74447=CARTESIAN_POINT('Ctrl Pts',(-40.3692307839642,-61.3659525022917,
12.));
#74448=CARTESIAN_POINT('Ctrl Pts',(-40.3740130490233,-61.3920120460232,
0.));
#74449=CARTESIAN_POINT('Ctrl Pts',(-40.3740130490233,-61.3920120460232,
12.));
#74450=CARTESIAN_POINT('Ctrl Pts',(-40.3787778694373,-61.418112507605,0.));
#74451=CARTESIAN_POINT('Ctrl Pts',(-40.3787778694373,-61.418112507605,12.));
#74452=CARTESIAN_POINT('Ctrl Pts',(-40.3835251797725,-61.4442538038053,
0.));
#74453=CARTESIAN_POINT('Ctrl Pts',(-40.3835251797725,-61.4442538038053,
12.));
#74454=CARTESIAN_POINT('Ctrl Pts',(-40.3882549149229,-61.4704358516711,
0.));
#74455=CARTESIAN_POINT('Ctrl Pts',(-40.3882549149229,-61.4704358516711,
12.));
#74456=CARTESIAN_POINT('Ctrl Pts',(-40.3929670101363,-61.4966585685544,
0.));
#74457=CARTESIAN_POINT('Ctrl Pts',(-40.3929670101363,-61.4966585685544,
12.));
#74458=CARTESIAN_POINT('Ctrl Pts',(-40.3976614010648,-61.5229218721532,
0.));
#74459=CARTESIAN_POINT('Ctrl Pts',(-40.3976614010648,-61.5229218721532,
12.));
#74460=CARTESIAN_POINT('Ctrl Pts',(-40.4023380237227,-61.5492256804709,
0.));
#74461=CARTESIAN_POINT('Ctrl Pts',(-40.4023380237227,-61.5492256804709,
12.));
#74462=CARTESIAN_POINT('Ctrl Pts',(-40.4069968143953,-61.5755699117318,
0.));
#74463=CARTESIAN_POINT('Ctrl Pts',(-40.4069968143953,-61.5755699117318,
12.));
#74464=CARTESIAN_POINT('Ctrl Pts',(-40.4116377095595,-61.6019544843008,
0.));
#74465=CARTESIAN_POINT('Ctrl Pts',(-40.4116377095595,-61.6019544843008,
12.));
#74466=CARTESIAN_POINT('Ctrl Pts',(-40.4162606458119,-61.628379316608,0.));
#74467=CARTESIAN_POINT('Ctrl Pts',(-40.4162606458119,-61.628379316608,12.));
#74468=CARTESIAN_POINT('Ctrl Pts',(-40.420865559772,-61.6548443270397,0.));
#74469=CARTESIAN_POINT('Ctrl Pts',(-40.420865559772,-61.6548443270397,12.));
#74470=CARTESIAN_POINT('Ctrl Pts',(-40.4254523880766,-61.6813494339295,
0.));
#74471=CARTESIAN_POINT('Ctrl Pts',(-40.4254523880766,-61.6813494339295,
12.));
#74472=CARTESIAN_POINT('Ctrl Pts',(-40.4300210675848,-61.7078945557812,
0.));
#74473=CARTESIAN_POINT('Ctrl Pts',(-40.4300210675848,-61.7078945557812,
12.));
#74474=CARTESIAN_POINT('Ctrl Pts',(-40.4345715355411,-61.7344796114409,
0.));
#74475=CARTESIAN_POINT('Ctrl Pts',(-40.4345715355411,-61.7344796114409,
12.));
#74476=CARTESIAN_POINT('Ctrl Pts',(-40.439103729759,-61.7611045202875,0.));
#74477=CARTESIAN_POINT('Ctrl Pts',(-40.439103729759,-61.7611045202875,12.));
#74478=CARTESIAN_POINT('Ctrl Pts',(-40.4436175887943,-61.7877692024064,
0.));
#74479=CARTESIAN_POINT('Ctrl Pts',(-40.4436175887943,-61.7877692024064,
12.));
#74480=CARTESIAN_POINT('Ctrl Pts',(-40.448113052135,-61.8144735787767,0.));
#74481=CARTESIAN_POINT('Ctrl Pts',(-40.448113052135,-61.8144735787767,12.));
#74482=CARTESIAN_POINT('Ctrl Pts',(-40.4525900597877,-61.8412175708523,
0.));
#74483=CARTESIAN_POINT('Ctrl Pts',(-40.4525900597877,-61.8412175708523,
12.));
#74484=CARTESIAN_POINT('Ctrl Pts',(-40.4570485518735,-61.8680011001513,
0.));
#74485=CARTESIAN_POINT('Ctrl Pts',(-40.4570485518735,-61.8680011001513,
12.));
#74486=CARTESIAN_POINT('Ctrl Pts',(-40.4614884681884,-61.8948240877998,
0.));
#74487=CARTESIAN_POINT('Ctrl Pts',(-40.4614884681884,-61.8948240877998,
12.));
#74488=CARTESIAN_POINT('Ctrl Pts',(-40.4659097478595,-61.9216864541758,
0.));
#74489=CARTESIAN_POINT('Ctrl Pts',(-40.4659097478595,-61.9216864541758,
12.));
#74490=CARTESIAN_POINT('Ctrl Pts',(-40.4703123287642,-61.9485881182957,
0.));
#74491=CARTESIAN_POINT('Ctrl Pts',(-40.4703123287642,-61.9485881182957,
12.));
#74492=CARTESIAN_POINT('Ctrl Pts',(-40.4746961480045,-61.9755289983093,
0.));
#74493=CARTESIAN_POINT('Ctrl Pts',(-40.4746961480045,-61.9755289983093,
12.));
#74494=CARTESIAN_POINT('Ctrl Pts',(-40.4790611429613,-62.0025090126008,
0.));
#74495=CARTESIAN_POINT('Ctrl Pts',(-40.4790611429613,-62.0025090126008,
12.));
#74496=CARTESIAN_POINT('Ctrl Pts',(-40.4834072522181,-62.0295280807449,
0.));
#74497=CARTESIAN_POINT('Ctrl Pts',(-40.4834072522181,-62.0295280807449,
12.));
#74498=CARTESIAN_POINT('Ctrl Pts',(-40.4877344164407,-62.0565861244171,
0.));
#74499=CARTESIAN_POINT('Ctrl Pts',(-40.4877344164407,-62.0565861244171,
12.));
#74500=CARTESIAN_POINT('Ctrl Pts',(-40.4920425795184,-62.0836830685665,
0.));
#74501=CARTESIAN_POINT('Ctrl Pts',(-40.4920425795184,-62.0836830685665,
12.));
#74502=CARTESIAN_POINT('Ctrl Pts',(-40.4963316888357,-62.110818841691,0.));
#74503=CARTESIAN_POINT('Ctrl Pts',(-40.4963316888357,-62.110818841691,12.));
#74504=CARTESIAN_POINT('Ctrl Pts',(-40.5006016927489,-62.137993373242,0.));
#74505=CARTESIAN_POINT('Ctrl Pts',(-40.5006016927489,-62.137993373242,12.));
#74506=CARTESIAN_POINT('Ctrl Pts',(-40.5048525385985,-62.1652065915724,
0.));
#74507=CARTESIAN_POINT('Ctrl Pts',(-40.5048525385985,-62.1652065915724,
12.));
#74508=CARTESIAN_POINT('Ctrl Pts',(-40.5090841704111,-62.1924584215634,
0.));
#74509=CARTESIAN_POINT('Ctrl Pts',(-40.5090841704111,-62.1924584215634,
12.));
#74510=CARTESIAN_POINT('Ctrl Pts',(-40.5132965269679,-62.2197487826212,
0.));
#74511=CARTESIAN_POINT('Ctrl Pts',(-40.5132965269679,-62.2197487826212,
12.));
#74512=CARTESIAN_POINT('Ctrl Pts',(-40.5174895391059,-62.2470775858834,
0.));
#74513=CARTESIAN_POINT('Ctrl Pts',(-40.5174895391059,-62.2470775858834,
12.));
#74514=CARTESIAN_POINT('Ctrl Pts',(-40.5216631336335,-62.2744447382207,
0.));
#74515=CARTESIAN_POINT('Ctrl Pts',(-40.5216631336335,-62.2744447382207,
12.));
#74516=CARTESIAN_POINT('Ctrl Pts',(-40.5258172381565,-62.3018501471876,
0.));
#74517=CARTESIAN_POINT('Ctrl Pts',(-40.5258172381565,-62.3018501471876,
12.));
#74518=CARTESIAN_POINT('Ctrl Pts',(-40.5299517857793,-62.3292937258021,
0.));
#74519=CARTESIAN_POINT('Ctrl Pts',(-40.5299517857793,-62.3292937258021,
12.));
#74520=CARTESIAN_POINT('Ctrl Pts',(-40.5340667194272,-62.35677539702,0.));
#74521=CARTESIAN_POINT('Ctrl Pts',(-40.5340667194272,-62.35677539702,12.));
#74522=CARTESIAN_POINT('Ctrl Pts',(-40.5381619973972,-62.3842950992504,
0.));
#74523=CARTESIAN_POINT('Ctrl Pts',(-40.5381619973972,-62.3842950992504,
12.));
#74524=CARTESIAN_POINT('Ctrl Pts',(-40.5422375944697,-62.4118527880601,
0.));
#74525=CARTESIAN_POINT('Ctrl Pts',(-40.5422375944697,-62.4118527880601,
12.));
#74526=CARTESIAN_POINT('Ctrl Pts',(-40.5462934972334,-62.439448432904,0.));
#74527=CARTESIAN_POINT('Ctrl Pts',(-40.5462934972334,-62.439448432904,12.));
#74528=CARTESIAN_POINT('Ctrl Pts',(-40.5495224601437,-62.4615552986668,
0.));
#74529=CARTESIAN_POINT('Ctrl Pts',(-40.5495224601437,-62.4615552986668,
12.));
#74530=CARTESIAN_POINT('Ctrl Pts',(-40.5519353177058,-62.4781525155997,
0.));
#74531=CARTESIAN_POINT('Ctrl Pts',(-40.5519353177058,-62.4781525155997,
12.));
#74532=CARTESIAN_POINT('Ctrl Pts',(-40.5535399497449,-62.4892249121863,
0.));
#74533=CARTESIAN_POINT('Ctrl Pts',(-40.5535399497449,-62.4892249121863,
12.));
#74534=CARTESIAN_POINT('Ctrl Pts',(-40.554341280847,-62.4947630068039,0.));
#74535=CARTESIAN_POINT('Ctrl Pts',(-40.554341280847,-62.4947630068039,12.));
#74536=CARTESIAN_POINT('',(-39.4479504917287,-57.8261117662438,0.));
#74537=CARTESIAN_POINT('Ctrl Pts',(-39.4479504917287,-57.8261117662438,
0.));
#74538=CARTESIAN_POINT('Ctrl Pts',(-39.4492429618443,-57.8297740100947,
0.));
#74539=CARTESIAN_POINT('Ctrl Pts',(-39.4518277003553,-57.837104315141,0.));
#74540=CARTESIAN_POINT('Ctrl Pts',(-39.4557042029652,-57.8481172247495,
0.));
#74541=CARTESIAN_POINT('Ctrl Pts',(-39.4608716627118,-57.8628360096803,
0.));
#74542=CARTESIAN_POINT('Ctrl Pts',(-39.4673289592259,-57.8812926637177,
0.));
#74543=CARTESIAN_POINT('Ctrl Pts',(-39.473784194937,-57.8998074670478,0.));
#74544=CARTESIAN_POINT('Ctrl Pts',(-39.4802373061058,-57.9183803632403,
0.));
#74545=CARTESIAN_POINT('Ctrl Pts',(-39.4866881842317,-57.937011245663,0.));
#74546=CARTESIAN_POINT('Ctrl Pts',(-39.4931366776714,-57.9556999583892,
0.));
#74547=CARTESIAN_POINT('Ctrl Pts',(-39.499582610674,-57.974446317937,0.));
#74548=CARTESIAN_POINT('Ctrl Pts',(-39.5060257981225,-57.9932501298522,
0.));
#74549=CARTESIAN_POINT('Ctrl Pts',(-39.5124660614976,-58.0121112067895,
0.));
#74550=CARTESIAN_POINT('Ctrl Pts',(-39.5189032457184,-58.0310293875262,
0.));
#74551=CARTESIAN_POINT('Ctrl Pts',(-39.5253372136887,-58.0500045308412,
0.));
#74552=CARTESIAN_POINT('Ctrl Pts',(-39.5317678383217,-58.0690365065374,
0.));
#74553=CARTESIAN_POINT('Ctrl Pts',(-39.5381949959221,-58.088125187992,0.));
#74554=CARTESIAN_POINT('Ctrl Pts',(-39.5446185579638,-58.1072704428928,
0.));
#74555=CARTESIAN_POINT('Ctrl Pts',(-39.5510383869505,-58.126472128574,0.));
#74556=CARTESIAN_POINT('Ctrl Pts',(-39.5574543406982,-58.1457300968499,
0.));
#74557=CARTESIAN_POINT('Ctrl Pts',(-39.563866275018,-58.1650441970387,0.));
#74558=CARTESIAN_POINT('Ctrl Pts',(-39.5702740467999,-58.1844142794338,
0.));
#74559=CARTESIAN_POINT('Ctrl Pts',(-39.57667751752,-58.2038401992457,0.));
#74560=CARTESIAN_POINT('Ctrl Pts',(-39.5830765530891,-58.2233218164365,
0.));
#74561=CARTESIAN_POINT('Ctrl Pts',(-39.5894710221713,-58.2428589938369,
0.));
#74562=CARTESIAN_POINT('Ctrl Pts',(-39.5958607950239,-58.2624515958419,
0.));
#74563=CARTESIAN_POINT('Ctrl Pts',(-39.602245742079,-58.2820994868118,0.));
#74564=CARTESIAN_POINT('Ctrl Pts',(-39.6086257327583,-58.3018025297323,
0.));
#74565=CARTESIAN_POINT('Ctrl Pts',(-39.6150006360914,-58.3215605869221,
0.));
#74566=CARTESIAN_POINT('Ctrl Pts',(-39.6213703212531,-58.3413735206423,
0.));
#74567=CARTESIAN_POINT('Ctrl Pts',(-39.6277346580892,-58.3612411936904,
0.));
#74568=CARTESIAN_POINT('Ctrl Pts',(-39.6340935177476,-58.3811634701037,
0.));
#74569=CARTESIAN_POINT('Ctrl Pts',(-39.6404467729094,-58.4011402154196,
0.));
#74570=CARTESIAN_POINT('Ctrl Pts',(-39.6467942974451,-58.4211712963004,
0.));
#74571=CARTESIAN_POINT('Ctrl Pts',(-39.653135966204,-58.4412565802979,0.));
#74572=CARTESIAN_POINT('Ctrl Pts',(-39.6594716547689,-58.4613959355788,
0.));
#74573=CARTESIAN_POINT('Ctrl Pts',(-39.6658012391815,-58.4815892306066,
0.));
#74574=CARTESIAN_POINT('Ctrl Pts',(-39.6721245959531,-58.5018363341604,
0.));
#74575=CARTESIAN_POINT('Ctrl Pts',(-39.6784416021826,-58.522137115476,0.));
#74576=CARTESIAN_POINT('Ctrl Pts',(-39.6847521356395,-58.5424914443415,
0.));
#74577=CARTESIAN_POINT('Ctrl Pts',(-39.6910560748629,-58.5628991912052,
0.));
#74578=CARTESIAN_POINT('Ctrl Pts',(-39.6973532992539,-58.5833602272743,
0.));
#74579=CARTESIAN_POINT('Ctrl Pts',(-39.7036436890233,-58.6038744244659,
0.));
#74580=CARTESIAN_POINT('Ctrl Pts',(-39.7099271251413,-58.6244416553562,
0.));
#74581=CARTESIAN_POINT('Ctrl Pts',(-39.7162034892899,-58.6450617931274,
0.));
#74582=CARTESIAN_POINT('Ctrl Pts',(-39.7224726638101,-58.6657347115034,
0.));
#74583=CARTESIAN_POINT('Ctrl Pts',(-39.7287345316681,-58.6864602847088,
0.));
#74584=CARTESIAN_POINT('Ctrl Pts',(-39.734988976475,-58.7072383875027,0.));
#74585=CARTESIAN_POINT('Ctrl Pts',(-39.7412358824953,-58.7280688951916,
0.));
#74586=CARTESIAN_POINT('Ctrl Pts',(-39.7474751346598,-58.7489516836445,
0.));
#74587=CARTESIAN_POINT('Ctrl Pts',(-39.7537066185813,-58.7698866293029,
0.));
#74588=CARTESIAN_POINT('Ctrl Pts',(-39.7599302205521,-58.7908736091798,
0.));
#74589=CARTESIAN_POINT('Ctrl Pts',(-39.7661458275274,-58.8119125008517,
0.));
#74590=CARTESIAN_POINT('Ctrl Pts',(-39.772353327112,-58.8330031824453,0.));
#74591=CARTESIAN_POINT('Ctrl Pts',(-39.7785526075478,-58.8541455326231,
0.));
#74592=CARTESIAN_POINT('Ctrl Pts',(-39.7847435576996,-58.8753394305585,
0.));
#74593=CARTESIAN_POINT('Ctrl Pts',(-39.7909260670517,-58.8965847559391,
0.));
#74594=CARTESIAN_POINT('Ctrl Pts',(-39.7971000257044,-58.9178813889703,
0.));
#74595=CARTESIAN_POINT('Ctrl Pts',(-39.8032653243712,-58.9392292103747,
0.));
#74596=CARTESIAN_POINT('Ctrl Pts',(-39.8094218543782,-58.9606281013875,
0.));
#74597=CARTESIAN_POINT('Ctrl Pts',(-39.8155695076626,-58.9820779437484,
0.));
#74598=CARTESIAN_POINT('Ctrl Pts',(-39.821708176766,-59.0035786197024,0.));
#74599=CARTESIAN_POINT('Ctrl Pts',(-39.8278377548262,-59.0251300119973,
0.));
#74600=CARTESIAN_POINT('Ctrl Pts',(-39.8339581355716,-59.0467320038784,
0.));
#74601=CARTESIAN_POINT('Ctrl Pts',(-39.8400692133139,-59.0683844790764,
0.));
#74602=CARTESIAN_POINT('Ctrl Pts',(-39.8461708829456,-59.090087321798,0.));
#74603=CARTESIAN_POINT('Ctrl Pts',(-39.8522630399328,-59.1118404167292,
0.));
#74604=CARTESIAN_POINT('Ctrl Pts',(-39.8583455803105,-59.1336436490342,
0.));
#74605=CARTESIAN_POINT('Ctrl Pts',(-39.8644184006787,-59.1554969043522,
0.));
#74606=CARTESIAN_POINT('Ctrl Pts',(-39.8704813981988,-59.1774000687879,
0.));
#74607=CARTESIAN_POINT('Ctrl Pts',(-39.876534470591,-59.1993530289028,0.));
#74608=CARTESIAN_POINT('Ctrl Pts',(-39.8825775161267,-59.2213556717209,
0.));
#74609=CARTESIAN_POINT('Ctrl Pts',(-39.8886104336242,-59.2434078847247,
0.));
#74610=CARTESIAN_POINT('Ctrl Pts',(-39.8946331224438,-59.2655095558521,
0.));
#74611=CARTESIAN_POINT('Ctrl Pts',(-39.9006454824845,-59.2876605734846,
0.));
#74612=CARTESIAN_POINT('Ctrl Pts',(-39.9066474141803,-59.3098608264419,
0.));
#74613=CARTESIAN_POINT('Ctrl Pts',(-39.9126388184936,-59.3321102039852,
0.));
#74614=CARTESIAN_POINT('Ctrl Pts',(-39.9186195969104,-59.3544085958151,
0.));
#74615=CARTESIAN_POINT('Ctrl Pts',(-39.9245896514367,-59.3767558920675,
0.));
#74616=CARTESIAN_POINT('Ctrl Pts',(-39.9305488845958,-59.3991519833016,
0.));
#74617=CARTESIAN_POINT('Ctrl Pts',(-39.9364971994242,-59.4215967604967,
0.));
#74618=CARTESIAN_POINT('Ctrl Pts',(-39.9424344994672,-59.4440901150582,
0.));
#74619=CARTESIAN_POINT('Ctrl Pts',(-39.9483606887737,-59.4666319388133,
0.));
#74620=CARTESIAN_POINT('Ctrl Pts',(-39.9542756718922,-59.4892221240068,
0.));
#74621=CARTESIAN_POINT('Ctrl Pts',(-39.9601793538682,-59.511860563289,0.));
#74622=CARTESIAN_POINT('Ctrl Pts',(-39.9660716402403,-59.5345471497128,
0.));
#74623=CARTESIAN_POINT('Ctrl Pts',(-39.9719524370345,-59.5572817767388,
0.));
#74624=CARTESIAN_POINT('Ctrl Pts',(-39.9778216507605,-59.5800643382314,
0.));
#74625=CARTESIAN_POINT('Ctrl Pts',(-39.9836791884079,-59.6028947284562,
0.));
#74626=CARTESIAN_POINT('Ctrl Pts',(-39.9895249574448,-59.6257728420669,
0.));
#74627=CARTESIAN_POINT('Ctrl Pts',(-39.9953588658132,-59.6486985741041,
0.));
#74628=CARTESIAN_POINT('Ctrl Pts',(-40.0011808219241,-59.6716718200005,
0.));
#74629=CARTESIAN_POINT('Ctrl Pts',(-40.0069907346537,-59.6946924755773,
0.));
#74630=CARTESIAN_POINT('Ctrl Pts',(-40.0127885133403,-59.7177604370403,
0.));
#74631=CARTESIAN_POINT('Ctrl Pts',(-40.0185740677821,-59.7408756009679,
0.));
#74632=CARTESIAN_POINT('Ctrl Pts',(-40.0243473082337,-59.7640378643106,
0.));
#74633=CARTESIAN_POINT('Ctrl Pts',(-40.0301081454002,-59.7872471243942,
0.));
#74634=CARTESIAN_POINT('Ctrl Pts',(-40.0358564904341,-59.8105032789179,
0.));
#74635=CARTESIAN_POINT('Ctrl Pts',(-40.0415922549315,-59.8338062259492,
0.));
#74636=CARTESIAN_POINT('Ctrl Pts',(-40.0473153509324,-59.8571558639145,
0.));
#74637=CARTESIAN_POINT('Ctrl Pts',(-40.0530256909161,-59.8805520915972,
0.));
#74638=CARTESIAN_POINT('Ctrl Pts',(-40.0587231877959,-59.9039948081428,
0.));
#74639=CARTESIAN_POINT('Ctrl Pts',(-40.0644077549158,-59.927483913055,0.));
#74640=CARTESIAN_POINT('Ctrl Pts',(-40.0700793060475,-59.9510193061929,
0.));
#74641=CARTESIAN_POINT('Ctrl Pts',(-40.0757377553893,-59.974600887759,0.));
#74642=CARTESIAN_POINT('Ctrl Pts',(-40.0813830175629,-59.9982285582991,
0.));
#74643=CARTESIAN_POINT('Ctrl Pts',(-40.0870150076078,-60.0219022187066,
0.));
#74644=CARTESIAN_POINT('Ctrl Pts',(-40.0926336409787,-60.0456217702203,
0.));
#74645=CARTESIAN_POINT('Ctrl Pts',(-40.0982388335421,-60.0693871144207,
0.));
#74646=CARTESIAN_POINT('Ctrl Pts',(-40.1038305015763,-60.0931981532194,
0.));
#74647=CARTESIAN_POINT('Ctrl Pts',(-40.1094085617672,-60.1170547888572,
0.));
#74648=CARTESIAN_POINT('Ctrl Pts',(-40.1149729312036,-60.1409569239092,
0.));
#74649=CARTESIAN_POINT('Ctrl Pts',(-40.120523527374,-60.1649044612829,0.));
#74650=CARTESIAN_POINT('Ctrl Pts',(-40.1260602681644,-60.1888973042151,
0.));
#74651=CARTESIAN_POINT('Ctrl Pts',(-40.1315830718575,-60.2129353562617,
0.));
#74652=CARTESIAN_POINT('Ctrl Pts',(-40.13709185713,-60.2370185212957,0.));
#74653=CARTESIAN_POINT('Ctrl Pts',(-40.1425865430468,-60.2611467035109,
0.));
#74654=CARTESIAN_POINT('Ctrl Pts',(-40.1480670490583,-60.2853198074215,
0.));
#74655=CARTESIAN_POINT('Ctrl Pts',(-40.1535332949978,-60.3095377378589,
0.));
#74656=CARTESIAN_POINT('Ctrl Pts',(-40.1589852010811,-60.3338003999616,
0.));
#74657=CARTESIAN_POINT('Ctrl Pts',(-40.1644226879043,-60.3581076991731,
0.));
#74658=CARTESIAN_POINT('Ctrl Pts',(-40.1698456764387,-60.382459541246,0.));
#74659=CARTESIAN_POINT('Ctrl Pts',(-40.1752540880273,-60.4068558322414,
0.));
#74660=CARTESIAN_POINT('Ctrl Pts',(-40.1806478443828,-60.4312964785269,
0.));
#74661=CARTESIAN_POINT('Ctrl Pts',(-40.1860268675875,-60.4557813867677,
0.));
#74662=CARTESIAN_POINT('Ctrl Pts',(-40.1913910800911,-60.4803104639211,
0.));
#74663=CARTESIAN_POINT('Ctrl Pts',(-40.1967404047055,-60.5048836172423,
0.));
#74664=CARTESIAN_POINT('Ctrl Pts',(-40.2020747646012,-60.5295007542838,
0.));
#74665=CARTESIAN_POINT('Ctrl Pts',(-40.2073940833054,-60.5541617828927,
0.));
#74666=CARTESIAN_POINT('Ctrl Pts',(-40.2126982847012,-60.5788666112043,
0.));
#74667=CARTESIAN_POINT('Ctrl Pts',(-40.2179872930272,-60.6036151476347,
0.));
#74668=CARTESIAN_POINT('Ctrl Pts',(-40.2232610328717,-60.6284073008865,
0.));
#74669=CARTESIAN_POINT('Ctrl Pts',(-40.2285194291702,-60.6532429799493,
0.));
#74670=CARTESIAN_POINT('Ctrl Pts',(-40.2337624072029,-60.6781220940979,
0.));
#74671=CARTESIAN_POINT('Ctrl Pts',(-40.2389898925937,-60.7030445528863,
0.));
#74672=CARTESIAN_POINT('Ctrl Pts',(-40.2442018113116,-60.72801026614,0.));
#74673=CARTESIAN_POINT('Ctrl Pts',(-40.2493980896646,-60.7530191439603,
0.));
#74674=CARTESIAN_POINT('Ctrl Pts',(-40.2545786542957,-60.7780710967253,
0.));
#74675=CARTESIAN_POINT('Ctrl Pts',(-40.2597434321804,-60.8031660350878,
0.));
#74676=CARTESIAN_POINT('Ctrl Pts',(-40.2648923506245,-60.8283038699703,
0.));
#74677=CARTESIAN_POINT('Ctrl Pts',(-40.2700253372644,-60.8534845125535,
0.));
#74678=CARTESIAN_POINT('Ctrl Pts',(-40.2751423200637,-60.8787078742817,
0.));
#74679=CARTESIAN_POINT('Ctrl Pts',(-40.2802432273105,-60.903973866867,0.));
#74680=CARTESIAN_POINT('Ctrl Pts',(-40.2853279876162,-60.9292824022888,
0.));
#74681=CARTESIAN_POINT('Ctrl Pts',(-40.2903965299155,-60.9546333927919,
0.));
#74682=CARTESIAN_POINT('Ctrl Pts',(-40.2954487834688,-60.9800267508781,
0.));
#74683=CARTESIAN_POINT('Ctrl Pts',(-40.3004846778577,-61.0054623893059,
0.));
#74684=CARTESIAN_POINT('Ctrl Pts',(-40.3055041429772,-61.0309402210915,
0.));
#74685=CARTESIAN_POINT('Ctrl Pts',(-40.3105071090308,-61.0564601595047,
0.));
#74686=CARTESIAN_POINT('Ctrl Pts',(-40.3154935065264,-61.0820221180646,
0.));
#74687=CARTESIAN_POINT('Ctrl Pts',(-40.3204632662729,-61.1076260105265,
0.));
#74688=CARTESIAN_POINT('Ctrl Pts',(-40.3254163193806,-61.1332717508799,
0.));
#74689=CARTESIAN_POINT('Ctrl Pts',(-40.3303525972621,-61.1589592533623,
0.));
#74690=CARTESIAN_POINT('Ctrl Pts',(-40.3352720316373,-61.184688432465,0.));
#74691=CARTESIAN_POINT('Ctrl Pts',(-40.3401745545369,-61.2104592029375,
0.));
#74692=CARTESIAN_POINT('Ctrl Pts',(-40.3450600983104,-61.236271479789,0.));
#74693=CARTESIAN_POINT('Ctrl Pts',(-40.3499285956297,-61.2621251782849,
0.));
#74694=CARTESIAN_POINT('Ctrl Pts',(-40.3547799794672,-61.2880202139358,
0.));
#74695=CARTESIAN_POINT('Ctrl Pts',(-40.3596141830786,-61.3139565024838,
0.));
#74696=CARTESIAN_POINT('Ctrl Pts',(-40.3644311399861,-61.3399339598851,
0.));
#74697=CARTESIAN_POINT('Ctrl Pts',(-40.3692307839642,-61.3659525022917,
0.));
#74698=CARTESIAN_POINT('Ctrl Pts',(-40.3740130490233,-61.3920120460232,
0.));
#74699=CARTESIAN_POINT('Ctrl Pts',(-40.3787778694373,-61.418112507605,0.));
#74700=CARTESIAN_POINT('Ctrl Pts',(-40.3835251797725,-61.4442538038053,
0.));
#74701=CARTESIAN_POINT('Ctrl Pts',(-40.3882549149229,-61.4704358516711,
0.));
#74702=CARTESIAN_POINT('Ctrl Pts',(-40.3929670101363,-61.4966585685544,
0.));
#74703=CARTESIAN_POINT('Ctrl Pts',(-40.3976614010648,-61.5229218721532,
0.));
#74704=CARTESIAN_POINT('Ctrl Pts',(-40.4023380237227,-61.5492256804709,
0.));
#74705=CARTESIAN_POINT('Ctrl Pts',(-40.4069968143953,-61.5755699117318,
0.));
#74706=CARTESIAN_POINT('Ctrl Pts',(-40.4116377095595,-61.6019544843008,
0.));
#74707=CARTESIAN_POINT('Ctrl Pts',(-40.4162606458119,-61.628379316608,0.));
#74708=CARTESIAN_POINT('Ctrl Pts',(-40.420865559772,-61.6548443270397,0.));
#74709=CARTESIAN_POINT('Ctrl Pts',(-40.4254523880766,-61.6813494339295,
0.));
#74710=CARTESIAN_POINT('Ctrl Pts',(-40.4300210675848,-61.7078945557812,
0.));
#74711=CARTESIAN_POINT('Ctrl Pts',(-40.4345715355411,-61.7344796114409,
0.));
#74712=CARTESIAN_POINT('Ctrl Pts',(-40.439103729759,-61.7611045202875,0.));
#74713=CARTESIAN_POINT('Ctrl Pts',(-40.4436175887943,-61.7877692024064,
0.));
#74714=CARTESIAN_POINT('Ctrl Pts',(-40.448113052135,-61.8144735787767,0.));
#74715=CARTESIAN_POINT('Ctrl Pts',(-40.4525900597877,-61.8412175708523,
0.));
#74716=CARTESIAN_POINT('Ctrl Pts',(-40.4570485518735,-61.8680011001513,
0.));
#74717=CARTESIAN_POINT('Ctrl Pts',(-40.4614884681884,-61.8948240877998,
0.));
#74718=CARTESIAN_POINT('Ctrl Pts',(-40.4659097478595,-61.9216864541758,
0.));
#74719=CARTESIAN_POINT('Ctrl Pts',(-40.4703123287642,-61.9485881182957,
0.));
#74720=CARTESIAN_POINT('Ctrl Pts',(-40.4746961480045,-61.9755289983093,
0.));
#74721=CARTESIAN_POINT('Ctrl Pts',(-40.4790611429613,-62.0025090126008,
0.));
#74722=CARTESIAN_POINT('Ctrl Pts',(-40.4834072522181,-62.0295280807449,
0.));
#74723=CARTESIAN_POINT('Ctrl Pts',(-40.4877344164407,-62.0565861244171,
0.));
#74724=CARTESIAN_POINT('Ctrl Pts',(-40.4920425795184,-62.0836830685665,
0.));
#74725=CARTESIAN_POINT('Ctrl Pts',(-40.4963316888357,-62.110818841691,0.));
#74726=CARTESIAN_POINT('Ctrl Pts',(-40.499991909619,-62.1341126810364,0.));
#74727=CARTESIAN_POINT('Ctrl Pts',(-40.5027877865723,-62.1519925002736,
0.));
#74728=CARTESIAN_POINT('Ctrl Pts',(-40.5047277935687,-62.1644411502528,
0.));
#74729=CARTESIAN_POINT('Ctrl Pts',(-40.5058175523045,-62.171447313775,0.));
#74730=CARTESIAN_POINT('Ctrl Pts',(-40.5060598100838,-62.1730054756451,
0.));
#74731=CARTESIAN_POINT('',(-39.4479504917287,-57.8261117662438,12.));
#74732=CARTESIAN_POINT('',(-39.4479504917287,-57.8261117662438,0.));
#74733=CARTESIAN_POINT('Ctrl Pts',(-40.5060598100838,-62.1730054756452,
12.));
#74734=CARTESIAN_POINT('Ctrl Pts',(-40.5058175523045,-62.1714473137751,
12.));
#74735=CARTESIAN_POINT('Ctrl Pts',(-40.5047277935688,-62.1644411502529,
12.));
#74736=CARTESIAN_POINT('Ctrl Pts',(-40.5027877865724,-62.1519925002736,
12.));
#74737=CARTESIAN_POINT('Ctrl Pts',(-40.499991909619,-62.1341126810364,12.));
#74738=CARTESIAN_POINT('Ctrl Pts',(-40.4963316888357,-62.110818841691,12.));
#74739=CARTESIAN_POINT('Ctrl Pts',(-40.4920425795184,-62.0836830685665,
12.));
#74740=CARTESIAN_POINT('Ctrl Pts',(-40.4877344164407,-62.0565861244171,
12.));
#74741=CARTESIAN_POINT('Ctrl Pts',(-40.4834072522181,-62.0295280807449,
12.));
#74742=CARTESIAN_POINT('Ctrl Pts',(-40.4790611429613,-62.0025090126008,
12.));
#74743=CARTESIAN_POINT('Ctrl Pts',(-40.4746961480045,-61.9755289983093,
12.));
#74744=CARTESIAN_POINT('Ctrl Pts',(-40.4703123287642,-61.9485881182957,
12.));
#74745=CARTESIAN_POINT('Ctrl Pts',(-40.4659097478595,-61.9216864541758,
12.));
#74746=CARTESIAN_POINT('Ctrl Pts',(-40.4614884681884,-61.8948240877998,
12.));
#74747=CARTESIAN_POINT('Ctrl Pts',(-40.4570485518735,-61.8680011001513,
12.));
#74748=CARTESIAN_POINT('Ctrl Pts',(-40.4525900597877,-61.8412175708523,
12.));
#74749=CARTESIAN_POINT('Ctrl Pts',(-40.448113052135,-61.8144735787767,12.));
#74750=CARTESIAN_POINT('Ctrl Pts',(-40.4436175887943,-61.7877692024064,
12.));
#74751=CARTESIAN_POINT('Ctrl Pts',(-40.439103729759,-61.7611045202875,12.));
#74752=CARTESIAN_POINT('Ctrl Pts',(-40.4345715355411,-61.7344796114409,
12.));
#74753=CARTESIAN_POINT('Ctrl Pts',(-40.4300210675848,-61.7078945557812,
12.));
#74754=CARTESIAN_POINT('Ctrl Pts',(-40.4254523880766,-61.6813494339295,
12.));
#74755=CARTESIAN_POINT('Ctrl Pts',(-40.420865559772,-61.6548443270397,12.));
#74756=CARTESIAN_POINT('Ctrl Pts',(-40.4162606458119,-61.628379316608,12.));
#74757=CARTESIAN_POINT('Ctrl Pts',(-40.4116377095595,-61.6019544843008,
12.));
#74758=CARTESIAN_POINT('Ctrl Pts',(-40.4069968143953,-61.5755699117318,
12.));
#74759=CARTESIAN_POINT('Ctrl Pts',(-40.4023380237227,-61.5492256804709,
12.));
#74760=CARTESIAN_POINT('Ctrl Pts',(-40.3976614010648,-61.5229218721532,
12.));
#74761=CARTESIAN_POINT('Ctrl Pts',(-40.3929670101363,-61.4966585685544,
12.));
#74762=CARTESIAN_POINT('Ctrl Pts',(-40.3882549149229,-61.4704358516711,
12.));
#74763=CARTESIAN_POINT('Ctrl Pts',(-40.3835251797725,-61.4442538038053,
12.));
#74764=CARTESIAN_POINT('Ctrl Pts',(-40.3787778694373,-61.418112507605,12.));
#74765=CARTESIAN_POINT('Ctrl Pts',(-40.3740130490233,-61.3920120460232,
12.));
#74766=CARTESIAN_POINT('Ctrl Pts',(-40.3692307839642,-61.3659525022917,
12.));
#74767=CARTESIAN_POINT('Ctrl Pts',(-40.3644311399861,-61.3399339598851,
12.));
#74768=CARTESIAN_POINT('Ctrl Pts',(-40.3596141830786,-61.3139565024838,
12.));
#74769=CARTESIAN_POINT('Ctrl Pts',(-40.3547799794672,-61.2880202139358,
12.));
#74770=CARTESIAN_POINT('Ctrl Pts',(-40.3499285956297,-61.2621251782849,
12.));
#74771=CARTESIAN_POINT('Ctrl Pts',(-40.3450600983104,-61.236271479789,12.));
#74772=CARTESIAN_POINT('Ctrl Pts',(-40.3401745545369,-61.2104592029375,
12.));
#74773=CARTESIAN_POINT('Ctrl Pts',(-40.3352720316373,-61.184688432465,12.));
#74774=CARTESIAN_POINT('Ctrl Pts',(-40.3303525972621,-61.1589592533623,
12.));
#74775=CARTESIAN_POINT('Ctrl Pts',(-40.3254163193806,-61.1332717508799,
12.));
#74776=CARTESIAN_POINT('Ctrl Pts',(-40.3204632662729,-61.1076260105265,
12.));
#74777=CARTESIAN_POINT('Ctrl Pts',(-40.3154935065264,-61.0820221180646,
12.));
#74778=CARTESIAN_POINT('Ctrl Pts',(-40.3105071090308,-61.0564601595047,
12.));
#74779=CARTESIAN_POINT('Ctrl Pts',(-40.3055041429772,-61.0309402210915,
12.));
#74780=CARTESIAN_POINT('Ctrl Pts',(-40.3004846778577,-61.0054623893059,
12.));
#74781=CARTESIAN_POINT('Ctrl Pts',(-40.2954487834688,-60.9800267508781,
12.));
#74782=CARTESIAN_POINT('Ctrl Pts',(-40.2903965299155,-60.9546333927919,
12.));
#74783=CARTESIAN_POINT('Ctrl Pts',(-40.2853279876162,-60.9292824022888,
12.));
#74784=CARTESIAN_POINT('Ctrl Pts',(-40.2802432273105,-60.903973866867,12.));
#74785=CARTESIAN_POINT('Ctrl Pts',(-40.2751423200637,-60.8787078742817,
12.));
#74786=CARTESIAN_POINT('Ctrl Pts',(-40.2700253372644,-60.8534845125535,
12.));
#74787=CARTESIAN_POINT('Ctrl Pts',(-40.2648923506245,-60.8283038699703,
12.));
#74788=CARTESIAN_POINT('Ctrl Pts',(-40.2597434321804,-60.8031660350878,
12.));
#74789=CARTESIAN_POINT('Ctrl Pts',(-40.2545786542957,-60.7780710967253,
12.));
#74790=CARTESIAN_POINT('Ctrl Pts',(-40.2493980896646,-60.7530191439603,
12.));
#74791=CARTESIAN_POINT('Ctrl Pts',(-40.2442018113116,-60.72801026614,12.));
#74792=CARTESIAN_POINT('Ctrl Pts',(-40.2389898925937,-60.7030445528863,
12.));
#74793=CARTESIAN_POINT('Ctrl Pts',(-40.2337624072029,-60.6781220940979,
12.));
#74794=CARTESIAN_POINT('Ctrl Pts',(-40.2285194291702,-60.6532429799493,
12.));
#74795=CARTESIAN_POINT('Ctrl Pts',(-40.2232610328717,-60.6284073008865,
12.));
#74796=CARTESIAN_POINT('Ctrl Pts',(-40.2179872930272,-60.6036151476347,
12.));
#74797=CARTESIAN_POINT('Ctrl Pts',(-40.2126982847012,-60.5788666112043,
12.));
#74798=CARTESIAN_POINT('Ctrl Pts',(-40.2073940833054,-60.5541617828927,
12.));
#74799=CARTESIAN_POINT('Ctrl Pts',(-40.2020747646012,-60.5295007542838,
12.));
#74800=CARTESIAN_POINT('Ctrl Pts',(-40.1967404047055,-60.5048836172423,
12.));
#74801=CARTESIAN_POINT('Ctrl Pts',(-40.1913910800911,-60.4803104639211,
12.));
#74802=CARTESIAN_POINT('Ctrl Pts',(-40.1860268675875,-60.4557813867677,
12.));
#74803=CARTESIAN_POINT('Ctrl Pts',(-40.1806478443828,-60.4312964785269,
12.));
#74804=CARTESIAN_POINT('Ctrl Pts',(-40.1752540880273,-60.4068558322414,
12.));
#74805=CARTESIAN_POINT('Ctrl Pts',(-40.1698456764387,-60.382459541246,12.));
#74806=CARTESIAN_POINT('Ctrl Pts',(-40.1644226879043,-60.3581076991731,
12.));
#74807=CARTESIAN_POINT('Ctrl Pts',(-40.1589852010811,-60.3338003999616,
12.));
#74808=CARTESIAN_POINT('Ctrl Pts',(-40.1535332949978,-60.3095377378589,
12.));
#74809=CARTESIAN_POINT('Ctrl Pts',(-40.1480670490583,-60.2853198074215,
12.));
#74810=CARTESIAN_POINT('Ctrl Pts',(-40.1425865430468,-60.2611467035109,
12.));
#74811=CARTESIAN_POINT('Ctrl Pts',(-40.13709185713,-60.2370185212957,12.));
#74812=CARTESIAN_POINT('Ctrl Pts',(-40.1315830718575,-60.2129353562617,
12.));
#74813=CARTESIAN_POINT('Ctrl Pts',(-40.1260602681644,-60.1888973042151,
12.));
#74814=CARTESIAN_POINT('Ctrl Pts',(-40.120523527374,-60.1649044612829,12.));
#74815=CARTESIAN_POINT('Ctrl Pts',(-40.1149729312036,-60.1409569239092,
12.));
#74816=CARTESIAN_POINT('Ctrl Pts',(-40.1094085617672,-60.1170547888572,
12.));
#74817=CARTESIAN_POINT('Ctrl Pts',(-40.1038305015763,-60.0931981532194,
12.));
#74818=CARTESIAN_POINT('Ctrl Pts',(-40.0982388335421,-60.0693871144207,
12.));
#74819=CARTESIAN_POINT('Ctrl Pts',(-40.0926336409787,-60.0456217702203,
12.));
#74820=CARTESIAN_POINT('Ctrl Pts',(-40.0870150076078,-60.0219022187066,
12.));
#74821=CARTESIAN_POINT('Ctrl Pts',(-40.0813830175629,-59.9982285582991,
12.));
#74822=CARTESIAN_POINT('Ctrl Pts',(-40.0757377553893,-59.974600887759,12.));
#74823=CARTESIAN_POINT('Ctrl Pts',(-40.0700793060475,-59.9510193061929,
12.));
#74824=CARTESIAN_POINT('Ctrl Pts',(-40.0644077549158,-59.927483913055,12.));
#74825=CARTESIAN_POINT('Ctrl Pts',(-40.0587231877959,-59.9039948081428,
12.));
#74826=CARTESIAN_POINT('Ctrl Pts',(-40.0530256909161,-59.8805520915972,
12.));
#74827=CARTESIAN_POINT('Ctrl Pts',(-40.0473153509324,-59.8571558639145,
12.));
#74828=CARTESIAN_POINT('Ctrl Pts',(-40.0415922549315,-59.8338062259492,
12.));
#74829=CARTESIAN_POINT('Ctrl Pts',(-40.0358564904341,-59.8105032789179,
12.));
#74830=CARTESIAN_POINT('Ctrl Pts',(-40.0301081454002,-59.7872471243942,
12.));
#74831=CARTESIAN_POINT('Ctrl Pts',(-40.0243473082337,-59.7640378643106,
12.));
#74832=CARTESIAN_POINT('Ctrl Pts',(-40.0185740677821,-59.7408756009679,
12.));
#74833=CARTESIAN_POINT('Ctrl Pts',(-40.0127885133403,-59.7177604370403,
12.));
#74834=CARTESIAN_POINT('Ctrl Pts',(-40.0069907346537,-59.6946924755773,
12.));
#74835=CARTESIAN_POINT('Ctrl Pts',(-40.0011808219241,-59.6716718200005,
12.));
#74836=CARTESIAN_POINT('Ctrl Pts',(-39.9953588658132,-59.6486985741041,
12.));
#74837=CARTESIAN_POINT('Ctrl Pts',(-39.9895249574448,-59.6257728420669,
12.));
#74838=CARTESIAN_POINT('Ctrl Pts',(-39.9836791884079,-59.6028947284562,
12.));
#74839=CARTESIAN_POINT('Ctrl Pts',(-39.9778216507605,-59.5800643382314,
12.));
#74840=CARTESIAN_POINT('Ctrl Pts',(-39.9719524370345,-59.5572817767388,
12.));
#74841=CARTESIAN_POINT('Ctrl Pts',(-39.9660716402403,-59.5345471497128,
12.));
#74842=CARTESIAN_POINT('Ctrl Pts',(-39.9601793538682,-59.511860563289,12.));
#74843=CARTESIAN_POINT('Ctrl Pts',(-39.9542756718922,-59.4892221240068,
12.));
#74844=CARTESIAN_POINT('Ctrl Pts',(-39.9483606887737,-59.4666319388133,
12.));
#74845=CARTESIAN_POINT('Ctrl Pts',(-39.9424344994672,-59.4440901150582,
12.));
#74846=CARTESIAN_POINT('Ctrl Pts',(-39.9364971994242,-59.4215967604967,
12.));
#74847=CARTESIAN_POINT('Ctrl Pts',(-39.9305488845958,-59.3991519833016,
12.));
#74848=CARTESIAN_POINT('Ctrl Pts',(-39.9245896514367,-59.3767558920675,
12.));
#74849=CARTESIAN_POINT('Ctrl Pts',(-39.9186195969104,-59.3544085958151,
12.));
#74850=CARTESIAN_POINT('Ctrl Pts',(-39.9126388184936,-59.3321102039852,
12.));
#74851=CARTESIAN_POINT('Ctrl Pts',(-39.9066474141803,-59.3098608264419,
12.));
#74852=CARTESIAN_POINT('Ctrl Pts',(-39.9006454824845,-59.2876605734846,
12.));
#74853=CARTESIAN_POINT('Ctrl Pts',(-39.8946331224438,-59.2655095558521,
12.));
#74854=CARTESIAN_POINT('Ctrl Pts',(-39.8886104336242,-59.2434078847247,
12.));
#74855=CARTESIAN_POINT('Ctrl Pts',(-39.8825775161267,-59.2213556717209,
12.));
#74856=CARTESIAN_POINT('Ctrl Pts',(-39.876534470591,-59.1993530289028,12.));
#74857=CARTESIAN_POINT('Ctrl Pts',(-39.8704813981988,-59.1774000687879,
12.));
#74858=CARTESIAN_POINT('Ctrl Pts',(-39.8644184006787,-59.1554969043522,
12.));
#74859=CARTESIAN_POINT('Ctrl Pts',(-39.8583455803105,-59.1336436490342,
12.));
#74860=CARTESIAN_POINT('Ctrl Pts',(-39.8522630399328,-59.1118404167292,
12.));
#74861=CARTESIAN_POINT('Ctrl Pts',(-39.8461708829456,-59.090087321798,12.));
#74862=CARTESIAN_POINT('Ctrl Pts',(-39.8400692133139,-59.0683844790764,
12.));
#74863=CARTESIAN_POINT('Ctrl Pts',(-39.8339581355716,-59.0467320038784,
12.));
#74864=CARTESIAN_POINT('Ctrl Pts',(-39.8278377548262,-59.0251300119973,
12.));
#74865=CARTESIAN_POINT('Ctrl Pts',(-39.821708176766,-59.0035786197024,12.));
#74866=CARTESIAN_POINT('Ctrl Pts',(-39.8155695076626,-58.9820779437484,
12.));
#74867=CARTESIAN_POINT('Ctrl Pts',(-39.8094218543782,-58.9606281013875,
12.));
#74868=CARTESIAN_POINT('Ctrl Pts',(-39.8032653243712,-58.9392292103747,
12.));
#74869=CARTESIAN_POINT('Ctrl Pts',(-39.7971000257044,-58.9178813889703,
12.));
#74870=CARTESIAN_POINT('Ctrl Pts',(-39.7909260670517,-58.8965847559391,
12.));
#74871=CARTESIAN_POINT('Ctrl Pts',(-39.7847435576996,-58.8753394305585,
12.));
#74872=CARTESIAN_POINT('Ctrl Pts',(-39.7785526075478,-58.8541455326231,
12.));
#74873=CARTESIAN_POINT('Ctrl Pts',(-39.772353327112,-58.8330031824453,12.));
#74874=CARTESIAN_POINT('Ctrl Pts',(-39.7661458275274,-58.8119125008517,
12.));
#74875=CARTESIAN_POINT('Ctrl Pts',(-39.7599302205521,-58.7908736091798,
12.));
#74876=CARTESIAN_POINT('Ctrl Pts',(-39.7537066185813,-58.7698866293029,
12.));
#74877=CARTESIAN_POINT('Ctrl Pts',(-39.7474751346598,-58.7489516836445,
12.));
#74878=CARTESIAN_POINT('Ctrl Pts',(-39.7412358824953,-58.7280688951916,
12.));
#74879=CARTESIAN_POINT('Ctrl Pts',(-39.734988976475,-58.7072383875027,12.));
#74880=CARTESIAN_POINT('Ctrl Pts',(-39.7287345316681,-58.6864602847088,
12.));
#74881=CARTESIAN_POINT('Ctrl Pts',(-39.7224726638101,-58.6657347115034,
12.));
#74882=CARTESIAN_POINT('Ctrl Pts',(-39.7162034892899,-58.6450617931274,
12.));
#74883=CARTESIAN_POINT('Ctrl Pts',(-39.7099271251413,-58.6244416553562,
12.));
#74884=CARTESIAN_POINT('Ctrl Pts',(-39.7036436890233,-58.6038744244659,
12.));
#74885=CARTESIAN_POINT('Ctrl Pts',(-39.6973532992539,-58.5833602272743,
12.));
#74886=CARTESIAN_POINT('Ctrl Pts',(-39.6910560748629,-58.5628991912052,
12.));
#74887=CARTESIAN_POINT('Ctrl Pts',(-39.6847521356395,-58.5424914443415,
12.));
#74888=CARTESIAN_POINT('Ctrl Pts',(-39.6784416021826,-58.522137115476,12.));
#74889=CARTESIAN_POINT('Ctrl Pts',(-39.6721245959531,-58.5018363341604,
12.));
#74890=CARTESIAN_POINT('Ctrl Pts',(-39.6658012391815,-58.4815892306066,
12.));
#74891=CARTESIAN_POINT('Ctrl Pts',(-39.6594716547689,-58.4613959355788,
12.));
#74892=CARTESIAN_POINT('Ctrl Pts',(-39.653135966204,-58.4412565802979,12.));
#74893=CARTESIAN_POINT('Ctrl Pts',(-39.6467942974451,-58.4211712963004,
12.));
#74894=CARTESIAN_POINT('Ctrl Pts',(-39.6404467729094,-58.4011402154196,
12.));
#74895=CARTESIAN_POINT('Ctrl Pts',(-39.6340935177476,-58.3811634701037,
12.));
#74896=CARTESIAN_POINT('Ctrl Pts',(-39.6277346580892,-58.3612411936904,
12.));
#74897=CARTESIAN_POINT('Ctrl Pts',(-39.6213703212531,-58.3413735206423,
12.));
#74898=CARTESIAN_POINT('Ctrl Pts',(-39.6150006360914,-58.3215605869221,
12.));
#74899=CARTESIAN_POINT('Ctrl Pts',(-39.6086257327583,-58.3018025297323,
12.));
#74900=CARTESIAN_POINT('Ctrl Pts',(-39.602245742079,-58.2820994868118,12.));
#74901=CARTESIAN_POINT('Ctrl Pts',(-39.5958607950239,-58.2624515958419,
12.));
#74902=CARTESIAN_POINT('Ctrl Pts',(-39.5894710221713,-58.2428589938369,
12.));
#74903=CARTESIAN_POINT('Ctrl Pts',(-39.5830765530891,-58.2233218164365,
12.));
#74904=CARTESIAN_POINT('Ctrl Pts',(-39.57667751752,-58.2038401992457,12.));
#74905=CARTESIAN_POINT('Ctrl Pts',(-39.5702740467999,-58.1844142794338,
12.));
#74906=CARTESIAN_POINT('Ctrl Pts',(-39.563866275018,-58.1650441970387,12.));
#74907=CARTESIAN_POINT('Ctrl Pts',(-39.5574543406982,-58.1457300968499,
12.));
#74908=CARTESIAN_POINT('Ctrl Pts',(-39.5510383869505,-58.126472128574,12.));
#74909=CARTESIAN_POINT('Ctrl Pts',(-39.5446185579638,-58.1072704428928,
12.));
#74910=CARTESIAN_POINT('Ctrl Pts',(-39.5381949959221,-58.088125187992,12.));
#74911=CARTESIAN_POINT('Ctrl Pts',(-39.5317678383217,-58.0690365065374,
12.));
#74912=CARTESIAN_POINT('Ctrl Pts',(-39.5253372136887,-58.0500045308412,
12.));
#74913=CARTESIAN_POINT('Ctrl Pts',(-39.5189032457184,-58.0310293875262,
12.));
#74914=CARTESIAN_POINT('Ctrl Pts',(-39.5124660614976,-58.0121112067895,
12.));
#74915=CARTESIAN_POINT('Ctrl Pts',(-39.5060257981225,-57.9932501298522,
12.));
#74916=CARTESIAN_POINT('Ctrl Pts',(-39.499582610674,-57.974446317937,12.));
#74917=CARTESIAN_POINT('Ctrl Pts',(-39.4931366776714,-57.9556999583892,
12.));
#74918=CARTESIAN_POINT('Ctrl Pts',(-39.4866881842317,-57.937011245663,12.));
#74919=CARTESIAN_POINT('Ctrl Pts',(-39.4802373061058,-57.9183803632403,
12.));
#74920=CARTESIAN_POINT('Ctrl Pts',(-39.473784194937,-57.8998074670478,12.));
#74921=CARTESIAN_POINT('Ctrl Pts',(-39.4673289592259,-57.8812926637177,
12.));
#74922=CARTESIAN_POINT('Ctrl Pts',(-39.4608716627118,-57.8628360096803,
12.));
#74923=CARTESIAN_POINT('Ctrl Pts',(-39.4557042029652,-57.8481172247495,
12.));
#74924=CARTESIAN_POINT('Ctrl Pts',(-39.4518277003553,-57.837104315141,12.));
#74925=CARTESIAN_POINT('Ctrl Pts',(-39.4492429618443,-57.8297740100947,
12.));
#74926=CARTESIAN_POINT('Ctrl Pts',(-39.4479504917287,-57.8261117662438,
12.));
#74927=CARTESIAN_POINT('Ctrl Pts',(-39.2292784191817,-62.9864049293897,
0.));
#74928=CARTESIAN_POINT('Ctrl Pts',(-39.2292784191817,-62.9864049293897,
4.));
#74929=CARTESIAN_POINT('Ctrl Pts',(-39.2292784191818,-62.9864049293897,
8.));
#74930=CARTESIAN_POINT('Ctrl Pts',(-39.2292784191818,-62.9864049293897,
12.));
#74931=CARTESIAN_POINT('Ctrl Pts',(-39.3205491216489,-63.0475916539463,
0.));
#74932=CARTESIAN_POINT('Ctrl Pts',(-39.3205491216489,-63.0475916539463,
4.));
#74933=CARTESIAN_POINT('Ctrl Pts',(-39.320549121649,-63.0475916539464,8.));
#74934=CARTESIAN_POINT('Ctrl Pts',(-39.320549121649,-63.0475916539464,12.));
#74935=CARTESIAN_POINT('Ctrl Pts',(-39.5164137621549,-63.0996457958578,
0.));
#74936=CARTESIAN_POINT('Ctrl Pts',(-39.5164137621549,-63.0996457958578,
4.00000000000001));
#74937=CARTESIAN_POINT('Ctrl Pts',(-39.516413762155,-63.0996457958578,7.99999999999999));
#74938=CARTESIAN_POINT('Ctrl Pts',(-39.516413762155,-63.0996457958578,12.));
#74939=CARTESIAN_POINT('Ctrl Pts',(-39.7049575044671,-63.037870691207,0.));
#74940=CARTESIAN_POINT('Ctrl Pts',(-39.7049575044671,-63.037870691207,3.99999999999999));
#74941=CARTESIAN_POINT('Ctrl Pts',(-39.7049575044672,-63.0378706912071,
8.00000000000001));
#74942=CARTESIAN_POINT('Ctrl Pts',(-39.7049575044672,-63.0378706912071,
12.));
#74943=CARTESIAN_POINT('Ctrl Pts',(-39.7746412831472,-62.9938720098778,
0.));
#74944=CARTESIAN_POINT('Ctrl Pts',(-39.7746412831472,-62.9938720098778,
4.));
#74945=CARTESIAN_POINT('Ctrl Pts',(-39.7746412831473,-62.9938720098779,
8.));
#74946=CARTESIAN_POINT('Ctrl Pts',(-39.7746412831473,-62.9938720098779,
12.));
#74947=CARTESIAN_POINT('',(-39.2292784191817,-62.9864049293897,0.));
#74948=CARTESIAN_POINT('',(-39.7746412831476,-62.9938720098783,0.));
#74949=CARTESIAN_POINT('Ctrl Pts',(-39.2292784191817,-62.9864049293897,
0.));
#74950=CARTESIAN_POINT('Ctrl Pts',(-39.3205491216489,-63.0475916539463,
0.));
#74951=CARTESIAN_POINT('Ctrl Pts',(-39.4324717733666,-63.0773368778958,
0.));
#74952=CARTESIAN_POINT('Ctrl Pts',(-39.5420039277149,-63.0699133682738,
0.));
#74953=CARTESIAN_POINT('Ctrl Pts',(-39.6241530434762,-63.0643457360574,
0.));
#74954=CARTESIAN_POINT('Ctrl Pts',(-39.7049575044671,-63.037870691207,0.));
#74955=CARTESIAN_POINT('Ctrl Pts',(-39.7746412831472,-62.9938720098778,
0.));
#74956=CARTESIAN_POINT('',(-39.7746412831476,-62.9938720098783,12.));
#74957=CARTESIAN_POINT('Ctrl Pts',(-39.7746412831472,-62.9938720098778,
0.));
#74958=CARTESIAN_POINT('Ctrl Pts',(-39.7746412831472,-62.9938720098778,
4.));
#74959=CARTESIAN_POINT('Ctrl Pts',(-39.7746412831473,-62.9938720098779,
8.));
#74960=CARTESIAN_POINT('Ctrl Pts',(-39.7746412831473,-62.9938720098779,
12.));
#74961=CARTESIAN_POINT('',(-39.2292784191818,-62.9864049293897,12.));
#74962=CARTESIAN_POINT('Ctrl Pts',(-39.7746412831473,-62.9938720098779,
12.));
#74963=CARTESIAN_POINT('Ctrl Pts',(-39.7049575044672,-63.0378706912071,
12.));
#74964=CARTESIAN_POINT('Ctrl Pts',(-39.6241530434763,-63.0643457360574,
12.));
#74965=CARTESIAN_POINT('Ctrl Pts',(-39.542003927715,-63.0699133682739,12.));
#74966=CARTESIAN_POINT('Ctrl Pts',(-39.4324717733667,-63.0773368778958,
12.));
#74967=CARTESIAN_POINT('Ctrl Pts',(-39.320549121649,-63.0475916539464,12.));
#74968=CARTESIAN_POINT('Ctrl Pts',(-39.2292784191818,-62.9864049293897,
12.));
#74969=CARTESIAN_POINT('Ctrl Pts',(-39.2292784191818,-62.9864049293897,
12.));
#74970=CARTESIAN_POINT('Ctrl Pts',(-39.2292784191818,-62.9864049293897,
8.));
#74971=CARTESIAN_POINT('Ctrl Pts',(-39.2292784191817,-62.9864049293897,
4.));
#74972=CARTESIAN_POINT('Ctrl Pts',(-39.2292784191817,-62.9864049293897,
0.));
#74973=CARTESIAN_POINT('Origin',(-2.01319694273778E-10,-3.16193356404481E-10,
0.));
#74974=CARTESIAN_POINT('Origin',(-2.01319694273778E-10,-3.16193356404481E-10,
12.));
#74975=CARTESIAN_POINT('Origin',(-2.01319694273778E-10,-3.16193356404481E-10,
0.));
#74976=CARTESIAN_POINT('Ctrl Pts',(-45.591148170023,-58.9211100416396,0.));
#74977=CARTESIAN_POINT('Ctrl Pts',(-45.591148170023,-58.9211100416396,4.));
#74978=CARTESIAN_POINT('Ctrl Pts',(-45.5911481700231,-58.9211100416396,
8.));
#74979=CARTESIAN_POINT('Ctrl Pts',(-45.5911481700231,-58.9211100416396,
12.));
#74980=CARTESIAN_POINT('Ctrl Pts',(-45.6780528262179,-58.8538661785413,
0.));
#74981=CARTESIAN_POINT('Ctrl Pts',(-45.6780528262179,-58.8538661785413,
4.));
#74982=CARTESIAN_POINT('Ctrl Pts',(-45.6780528262179,-58.8538661785413,
8.));
#74983=CARTESIAN_POINT('Ctrl Pts',(-45.6780528262179,-58.8538661785413,
12.));
#74984=CARTESIAN_POINT('Ctrl Pts',(-45.7893619681937,-58.6845061116499,
0.));
#74985=CARTESIAN_POINT('Ctrl Pts',(-45.7893619681937,-58.6845061116499,
4.00000000000001));
#74986=CARTESIAN_POINT('Ctrl Pts',(-45.7893619681937,-58.6845061116498,
7.99999999999999));
#74987=CARTESIAN_POINT('Ctrl Pts',(-45.7893619681937,-58.6845061116498,
12.));
#74988=CARTESIAN_POINT('Ctrl Pts',(-45.790366715598,-58.486102814171,0.));
#74989=CARTESIAN_POINT('Ctrl Pts',(-45.790366715598,-58.486102814171,4.));
#74990=CARTESIAN_POINT('Ctrl Pts',(-45.7903667155981,-58.486102814171,8.00000000000001));
#74991=CARTESIAN_POINT('Ctrl Pts',(-45.7903667155981,-58.486102814171,12.));
#74992=CARTESIAN_POINT('Ctrl Pts',(-45.7706564944768,-58.4060826907379,
0.));
#74993=CARTESIAN_POINT('Ctrl Pts',(-45.7706564944768,-58.4060826907379,
4.));
#74994=CARTESIAN_POINT('Ctrl Pts',(-45.7706564944768,-58.4060826907378,
8.));
#74995=CARTESIAN_POINT('Ctrl Pts',(-45.7706564944768,-58.4060826907378,
12.));
#74996=CARTESIAN_POINT('',(-45.591148170023,-58.9211100416396,0.));
#74997=CARTESIAN_POINT('',(-45.7706564944767,-58.4060826907379,0.));
#74998=CARTESIAN_POINT('Ctrl Pts',(-45.591148170023,-58.9211100416396,0.));
#74999=CARTESIAN_POINT('Ctrl Pts',(-45.6780528262179,-58.8538661785413,
0.));
#75000=CARTESIAN_POINT('Ctrl Pts',(-45.741658050204,-58.7570889974605,0.));
#75001=CARTESIAN_POINT('Ctrl Pts',(-45.7692455126975,-58.6508283125144,
0.));
#75002=CARTESIAN_POINT('Ctrl Pts',(-45.7899361095676,-58.5711327988048,
0.));
#75003=CARTESIAN_POINT('Ctrl Pts',(-45.790366715598,-58.486102814171,0.));
#75004=CARTESIAN_POINT('Ctrl Pts',(-45.7706564944768,-58.4060826907379,
0.));
#75005=CARTESIAN_POINT('',(-45.7706564944767,-58.4060826907378,12.));
#75006=CARTESIAN_POINT('Ctrl Pts',(-45.7706564944768,-58.4060826907379,
0.));
#75007=CARTESIAN_POINT('Ctrl Pts',(-45.7706564944768,-58.4060826907379,
4.));
#75008=CARTESIAN_POINT('Ctrl Pts',(-45.7706564944768,-58.4060826907378,
8.));
#75009=CARTESIAN_POINT('Ctrl Pts',(-45.7706564944768,-58.4060826907378,
12.));
#75010=CARTESIAN_POINT('',(-45.5911481700231,-58.9211100416396,12.));
#75011=CARTESIAN_POINT('Ctrl Pts',(-45.7706564944768,-58.4060826907378,
12.));
#75012=CARTESIAN_POINT('Ctrl Pts',(-45.7903667155981,-58.486102814171,12.));
#75013=CARTESIAN_POINT('Ctrl Pts',(-45.7899361095676,-58.5711327988048,
12.));
#75014=CARTESIAN_POINT('Ctrl Pts',(-45.7692455126975,-58.6508283125143,
12.));
#75015=CARTESIAN_POINT('Ctrl Pts',(-45.7416580502041,-58.7570889974604,
12.));
#75016=CARTESIAN_POINT('Ctrl Pts',(-45.6780528262179,-58.8538661785413,
12.));
#75017=CARTESIAN_POINT('Ctrl Pts',(-45.5911481700231,-58.9211100416396,
12.));
#75018=CARTESIAN_POINT('Ctrl Pts',(-45.5911481700231,-58.9211100416396,
12.));
#75019=CARTESIAN_POINT('Ctrl Pts',(-45.5911481700231,-58.9211100416396,
8.));
#75020=CARTESIAN_POINT('Ctrl Pts',(-45.591148170023,-58.9211100416396,4.));
#75021=CARTESIAN_POINT('Ctrl Pts',(-45.591148170023,-58.9211100416396,0.));
#75022=CARTESIAN_POINT('Ctrl Pts',(-44.3377168516418,-54.1679505278134,
0.));
#75023=CARTESIAN_POINT('Ctrl Pts',(-44.3377168516418,-54.1679505278134,
12.));
#75024=CARTESIAN_POINT('Ctrl Pts',(-44.3393235891014,-54.1714861895278,
0.));
#75025=CARTESIAN_POINT('Ctrl Pts',(-44.3393235891014,-54.1714861895278,
12.));
#75026=CARTESIAN_POINT('Ctrl Pts',(-44.3425373700829,-54.1785633257456,
0.));
#75027=CARTESIAN_POINT('Ctrl Pts',(-44.3425373700829,-54.1785633257456,
12.));
#75028=CARTESIAN_POINT('Ctrl Pts',(-44.3473589597468,-54.1891964684439,
0.));
#75029=CARTESIAN_POINT('Ctrl Pts',(-44.3473589597468,-54.1891964684439,
12.));
#75030=CARTESIAN_POINT('Ctrl Pts',(-44.3537895823819,-54.203408870162,0.));
#75031=CARTESIAN_POINT('Ctrl Pts',(-44.3537895823819,-54.203408870162,12.));
#75032=CARTESIAN_POINT('Ctrl Pts',(-44.3618309103245,-54.2212325005847,
0.));
#75033=CARTESIAN_POINT('Ctrl Pts',(-44.3618309103245,-54.2212325005847,
12.));
#75034=CARTESIAN_POINT('Ctrl Pts',(-44.369875253351,-54.2391142386354,0.));
#75035=CARTESIAN_POINT('Ctrl Pts',(-44.369875253351,-54.2391142386354,12.));
#75036=CARTESIAN_POINT('Ctrl Pts',(-44.3779225430461,-54.2570540336536,
0.));
#75037=CARTESIAN_POINT('Ctrl Pts',(-44.3779225430461,-54.2570540336536,
12.));
#75038=CARTESIAN_POINT('Ctrl Pts',(-44.3859726620288,-54.2750517888695,
0.));
#75039=CARTESIAN_POINT('Ctrl Pts',(-44.3859726620288,-54.2750517888695,
12.));
#75040=CARTESIAN_POINT('Ctrl Pts',(-44.3940254456427,-54.2931073621661,
0.));
#75041=CARTESIAN_POINT('Ctrl Pts',(-44.3940254456427,-54.2931073621661,
12.));
#75042=CARTESIAN_POINT('Ctrl Pts',(-44.4020807028144,-54.3112205860776,
0.));
#75043=CARTESIAN_POINT('Ctrl Pts',(-44.4020807028144,-54.3112205860776,
12.));
#75044=CARTESIAN_POINT('Ctrl Pts',(-44.4101382321834,-54.3293912830237,
0.));
#75045=CARTESIAN_POINT('Ctrl Pts',(-44.4101382321834,-54.3293912830237,
12.));
#75046=CARTESIAN_POINT('Ctrl Pts',(-44.4181978395814,-54.347619281931,0.));
#75047=CARTESIAN_POINT('Ctrl Pts',(-44.4181978395814,-54.347619281931,12.));
#75048=CARTESIAN_POINT('Ctrl Pts',(-44.4262593564664,-54.3659044357064,
0.));
#75049=CARTESIAN_POINT('Ctrl Pts',(-44.4262593564664,-54.3659044357064,
12.));
#75050=CARTESIAN_POINT('Ctrl Pts',(-44.4343226339555,-54.3842466156151,
0.));
#75051=CARTESIAN_POINT('Ctrl Pts',(-44.4343226339555,-54.3842466156151,
12.));
#75052=CARTESIAN_POINT('Ctrl Pts',(-44.442387534098,-54.4026457030316,0.));
#75053=CARTESIAN_POINT('Ctrl Pts',(-44.442387534098,-54.4026457030316,12.));
#75054=CARTESIAN_POINT('Ctrl Pts',(-44.4504539226336,-54.4211015825959,
0.));
#75055=CARTESIAN_POINT('Ctrl Pts',(-44.4504539226336,-54.4211015825959,
12.));
#75056=CARTESIAN_POINT('Ctrl Pts',(-44.4585216599933,-54.4396141337008,
0.));
#75057=CARTESIAN_POINT('Ctrl Pts',(-44.4585216599933,-54.4396141337008,
12.));
#75058=CARTESIAN_POINT('Ctrl Pts',(-44.4665905967701,-54.4581832262072,
0.));
#75059=CARTESIAN_POINT('Ctrl Pts',(-44.4665905967701,-54.4581832262072,
12.));
#75060=CARTESIAN_POINT('Ctrl Pts',(-44.4746605784056,-54.4768087248854,
0.));
#75061=CARTESIAN_POINT('Ctrl Pts',(-44.4746605784056,-54.4768087248854,
12.));
#75062=CARTESIAN_POINT('Ctrl Pts',(-44.482731448127,-54.4954904921938,0.));
#75063=CARTESIAN_POINT('Ctrl Pts',(-44.482731448127,-54.4954904921938,12.));
#75064=CARTESIAN_POINT('Ctrl Pts',(-44.4908030503209,-54.5142283914684,
0.));
#75065=CARTESIAN_POINT('Ctrl Pts',(-44.4908030503209,-54.5142283914684,
12.));
#75066=CARTESIAN_POINT('Ctrl Pts',(-44.4988752343715,-54.5330222905438,
0.));
#75067=CARTESIAN_POINT('Ctrl Pts',(-44.4988752343715,-54.5330222905438,
12.));
#75068=CARTESIAN_POINT('Ctrl Pts',(-44.5069478544945,-54.5518720616016,
0.));
#75069=CARTESIAN_POINT('Ctrl Pts',(-44.5069478544945,-54.5518720616016,
12.));
#75070=CARTESIAN_POINT('Ctrl Pts',(-44.5150207678988,-54.5707775794412,
0.));
#75071=CARTESIAN_POINT('Ctrl Pts',(-44.5150207678988,-54.5707775794412,
12.));
#75072=CARTESIAN_POINT('Ctrl Pts',(-44.5230938335167,-54.5897387202815,
0.));
#75073=CARTESIAN_POINT('Ctrl Pts',(-44.5230938335167,-54.5897387202815,
12.));
#75074=CARTESIAN_POINT('Ctrl Pts',(-44.5311669104515,-54.6087553602914,
0.));
#75075=CARTESIAN_POINT('Ctrl Pts',(-44.5311669104515,-54.6087553602914,
12.));
#75076=CARTESIAN_POINT('Ctrl Pts',(-44.5392398566802,-54.6278273743587,
0.));
#75077=CARTESIAN_POINT('Ctrl Pts',(-44.5392398566802,-54.6278273743587,
12.));
#75078=CARTESIAN_POINT('Ctrl Pts',(-44.5473125297311,-54.6469546367408,
0.));
#75079=CARTESIAN_POINT('Ctrl Pts',(-44.5473125297311,-54.6469546367408,
12.));
#75080=CARTESIAN_POINT('Ctrl Pts',(-44.5553847872721,-54.6661370216252,
0.));
#75081=CARTESIAN_POINT('Ctrl Pts',(-44.5553847872721,-54.6661370216252,
12.));
#75082=CARTESIAN_POINT('Ctrl Pts',(-44.5634564876863,-54.6853744036751,
0.));
#75083=CARTESIAN_POINT('Ctrl Pts',(-44.5634564876863,-54.6853744036751,
12.));
#75084=CARTESIAN_POINT('Ctrl Pts',(-44.5715274907619,-54.7046666586754,
0.));
#75085=CARTESIAN_POINT('Ctrl Pts',(-44.5715274907619,-54.7046666586754,
12.));
#75086=CARTESIAN_POINT('Ctrl Pts',(-44.5795976579454,-54.7240136637717,
0.));
#75087=CARTESIAN_POINT('Ctrl Pts',(-44.5795976579454,-54.7240136637717,
12.));
#75088=CARTESIAN_POINT('Ctrl Pts',(-44.5876668519661,-54.7434152971267,
0.));
#75089=CARTESIAN_POINT('Ctrl Pts',(-44.5876668519661,-54.7434152971267,
12.));
#75090=CARTESIAN_POINT('Ctrl Pts',(-44.5957349366059,-54.7628714377037,
0.));
#75091=CARTESIAN_POINT('Ctrl Pts',(-44.5957349366059,-54.7628714377037,
12.));
#75092=CARTESIAN_POINT('Ctrl Pts',(-44.6038017764309,-54.7823819650149,
0.));
#75093=CARTESIAN_POINT('Ctrl Pts',(-44.6038017764309,-54.7823819650149,
12.));
#75094=CARTESIAN_POINT('Ctrl Pts',(-44.6118672364906,-54.8019467588278,
0.));
#75095=CARTESIAN_POINT('Ctrl Pts',(-44.6118672364906,-54.8019467588278,
12.));
#75096=CARTESIAN_POINT('Ctrl Pts',(-44.6199311823293,-54.8215656991837,
0.));
#75097=CARTESIAN_POINT('Ctrl Pts',(-44.6199311823293,-54.8215656991837,
12.));
#75098=CARTESIAN_POINT('Ctrl Pts',(-44.6279934801169,-54.8412386665276,
0.));
#75099=CARTESIAN_POINT('Ctrl Pts',(-44.6279934801169,-54.8412386665276,
12.));
#75100=CARTESIAN_POINT('Ctrl Pts',(-44.6360539967392,-54.860965541796,0.));
#75101=CARTESIAN_POINT('Ctrl Pts',(-44.6360539967392,-54.860965541796,12.));
#75102=CARTESIAN_POINT('Ctrl Pts',(-44.6441125999063,-54.8807462065164,
0.));
#75103=CARTESIAN_POINT('Ctrl Pts',(-44.6441125999063,-54.8807462065164,
12.));
#75104=CARTESIAN_POINT('Ctrl Pts',(-44.6521691582533,-54.9005805428969,
0.));
#75105=CARTESIAN_POINT('Ctrl Pts',(-44.6521691582533,-54.9005805428969,
12.));
#75106=CARTESIAN_POINT('Ctrl Pts',(-44.6602235412836,-54.9204684337822,
0.));
#75107=CARTESIAN_POINT('Ctrl Pts',(-44.6602235412836,-54.9204684337822,
12.));
#75108=CARTESIAN_POINT('Ctrl Pts',(-44.6682756193147,-54.9404097626077,
0.));
#75109=CARTESIAN_POINT('Ctrl Pts',(-44.6682756193147,-54.9404097626077,
12.));
#75110=CARTESIAN_POINT('Ctrl Pts',(-44.6763252634258,-54.9604044133501,
0.));
#75111=CARTESIAN_POINT('Ctrl Pts',(-44.6763252634258,-54.9604044133501,
12.));
#75112=CARTESIAN_POINT('Ctrl Pts',(-44.6843723454,-54.9804522704686,0.));
#75113=CARTESIAN_POINT('Ctrl Pts',(-44.6843723454,-54.9804522704686,12.));
#75114=CARTESIAN_POINT('Ctrl Pts',(-44.6924167376869,-55.0005532188667,
0.));
#75115=CARTESIAN_POINT('Ctrl Pts',(-44.6924167376869,-55.0005532188667,
12.));
#75116=CARTESIAN_POINT('Ctrl Pts',(-44.7004583134249,-55.0207071439237,
0.));
#75117=CARTESIAN_POINT('Ctrl Pts',(-44.7004583134249,-55.0207071439237,
12.));
#75118=CARTESIAN_POINT('Ctrl Pts',(-44.7084969464513,-55.0409139315078,
0.));
#75119=CARTESIAN_POINT('Ctrl Pts',(-44.7084969464513,-55.0409139315078,
12.));
#75120=CARTESIAN_POINT('Ctrl Pts',(-44.7165325113159,-55.0611734679894,
0.));
#75121=CARTESIAN_POINT('Ctrl Pts',(-44.7165325113159,-55.0611734679894,
12.));
#75122=CARTESIAN_POINT('Ctrl Pts',(-44.7245648832979,-55.0814856402496,
0.));
#75123=CARTESIAN_POINT('Ctrl Pts',(-44.7245648832979,-55.0814856402496,
12.));
#75124=CARTESIAN_POINT('Ctrl Pts',(-44.7325939384035,-55.1018503356796,
0.));
#75125=CARTESIAN_POINT('Ctrl Pts',(-44.7325939384035,-55.1018503356796,
12.));
#75126=CARTESIAN_POINT('Ctrl Pts',(-44.740619553348,-55.1222674421743,0.));
#75127=CARTESIAN_POINT('Ctrl Pts',(-44.740619553348,-55.1222674421743,12.));
#75128=CARTESIAN_POINT('Ctrl Pts',(-44.748641605542,-55.14273684812,0.));
#75129=CARTESIAN_POINT('Ctrl Pts',(-44.748641605542,-55.14273684812,12.));
#75130=CARTESIAN_POINT('Ctrl Pts',(-44.7566599730773,-55.1632584423815,
0.));
#75131=CARTESIAN_POINT('Ctrl Pts',(-44.7566599730773,-55.1632584423815,
12.));
#75132=CARTESIAN_POINT('Ctrl Pts',(-44.7646745347109,-55.1838321142779,
0.));
#75133=CARTESIAN_POINT('Ctrl Pts',(-44.7646745347109,-55.1838321142779,
12.));
#75134=CARTESIAN_POINT('Ctrl Pts',(-44.7726851698619,-55.2044577535866,
0.));
#75135=CARTESIAN_POINT('Ctrl Pts',(-44.7726851698619,-55.2044577535866,
12.));
#75136=CARTESIAN_POINT('Ctrl Pts',(-44.7806917586077,-55.2251352505475,
0.));
#75137=CARTESIAN_POINT('Ctrl Pts',(-44.7806917586077,-55.2251352505475,
12.));
#75138=CARTESIAN_POINT('Ctrl Pts',(-44.7886941816823,-55.2458644958617,
0.));
#75139=CARTESIAN_POINT('Ctrl Pts',(-44.7886941816823,-55.2458644958617,
12.));
#75140=CARTESIAN_POINT('Ctrl Pts',(-44.7966923204741,-55.2666453806883,
0.));
#75141=CARTESIAN_POINT('Ctrl Pts',(-44.7966923204741,-55.2666453806883,
12.));
#75142=CARTESIAN_POINT('Ctrl Pts',(-44.8046860570245,-55.287477796635,0.));
#75143=CARTESIAN_POINT('Ctrl Pts',(-44.8046860570245,-55.287477796635,12.));
#75144=CARTESIAN_POINT('Ctrl Pts',(-44.812675274021,-55.3083616357605,0.));
#75145=CARTESIAN_POINT('Ctrl Pts',(-44.812675274021,-55.3083616357605,12.));
#75146=CARTESIAN_POINT('Ctrl Pts',(-44.8206598547889,-55.3292967905726,
0.));
#75147=CARTESIAN_POINT('Ctrl Pts',(-44.8206598547889,-55.3292967905726,
12.));
#75148=CARTESIAN_POINT('Ctrl Pts',(-44.8286396832849,-55.350283154023,0.));
#75149=CARTESIAN_POINT('Ctrl Pts',(-44.8286396832849,-55.350283154023,12.));
#75150=CARTESIAN_POINT('Ctrl Pts',(-44.8366146440896,-55.3713206194962,
0.));
#75151=CARTESIAN_POINT('Ctrl Pts',(-44.8366146440896,-55.3713206194962,
12.));
#75152=CARTESIAN_POINT('Ctrl Pts',(-44.8445846224034,-55.3924090808002,
0.));
#75153=CARTESIAN_POINT('Ctrl Pts',(-44.8445846224034,-55.3924090808002,
12.));
#75154=CARTESIAN_POINT('Ctrl Pts',(-44.8525495040397,-55.4135484321706,
0.));
#75155=CARTESIAN_POINT('Ctrl Pts',(-44.8525495040397,-55.4135484321706,
12.));
#75156=CARTESIAN_POINT('Ctrl Pts',(-44.8605091754208,-55.4347385682697,
0.));
#75157=CARTESIAN_POINT('Ctrl Pts',(-44.8605091754208,-55.4347385682697,
12.));
#75158=CARTESIAN_POINT('Ctrl Pts',(-44.8684635235727,-55.4559793841838,
0.));
#75159=CARTESIAN_POINT('Ctrl Pts',(-44.8684635235727,-55.4559793841838,
12.));
#75160=CARTESIAN_POINT('Ctrl Pts',(-44.8764124361218,-55.4772707754139,
0.));
#75161=CARTESIAN_POINT('Ctrl Pts',(-44.8764124361218,-55.4772707754139,
12.));
#75162=CARTESIAN_POINT('Ctrl Pts',(-44.8843558012903,-55.4986126378676,
0.));
#75163=CARTESIAN_POINT('Ctrl Pts',(-44.8843558012903,-55.4986126378676,
12.));
#75164=CARTESIAN_POINT('Ctrl Pts',(-44.8922935078905,-55.5200048678648,
0.));
#75165=CARTESIAN_POINT('Ctrl Pts',(-44.8922935078905,-55.5200048678648,
12.));
#75166=CARTESIAN_POINT('Ctrl Pts',(-44.9002254453192,-55.541447362135,0.));
#75167=CARTESIAN_POINT('Ctrl Pts',(-44.9002254453192,-55.541447362135,12.));
#75168=CARTESIAN_POINT('Ctrl Pts',(-44.9081515035525,-55.5629400178136,
0.));
#75169=CARTESIAN_POINT('Ctrl Pts',(-44.9081515035525,-55.5629400178136,
12.));
#75170=CARTESIAN_POINT('Ctrl Pts',(-44.9160715731425,-55.5844827324315,
0.));
#75171=CARTESIAN_POINT('Ctrl Pts',(-44.9160715731425,-55.5844827324315,
12.));
#75172=CARTESIAN_POINT('Ctrl Pts',(-44.9239855452119,-55.6060754039089,
0.));
#75173=CARTESIAN_POINT('Ctrl Pts',(-44.9239855452119,-55.6060754039089,
12.));
#75174=CARTESIAN_POINT('Ctrl Pts',(-44.9318933114483,-55.6277179305604,
0.));
#75175=CARTESIAN_POINT('Ctrl Pts',(-44.9318933114483,-55.6277179305604,
12.));
#75176=CARTESIAN_POINT('Ctrl Pts',(-44.9397947640996,-55.6494102110922,
0.));
#75177=CARTESIAN_POINT('Ctrl Pts',(-44.9397947640996,-55.6494102110922,
12.));
#75178=CARTESIAN_POINT('Ctrl Pts',(-44.9476897959694,-55.671152144599,0.));
#75179=CARTESIAN_POINT('Ctrl Pts',(-44.9476897959694,-55.671152144599,12.));
#75180=CARTESIAN_POINT('Ctrl Pts',(-44.9555783004133,-55.6929436305522,
0.));
#75181=CARTESIAN_POINT('Ctrl Pts',(-44.9555783004133,-55.6929436305522,
12.));
#75182=CARTESIAN_POINT('Ctrl Pts',(-44.9634601713352,-55.7147845687969,
0.));
#75183=CARTESIAN_POINT('Ctrl Pts',(-44.9634601713352,-55.7147845687969,
12.));
#75184=CARTESIAN_POINT('Ctrl Pts',(-44.9713353031827,-55.7366748595582,
0.));
#75185=CARTESIAN_POINT('Ctrl Pts',(-44.9713353031827,-55.7366748595582,
12.));
#75186=CARTESIAN_POINT('Ctrl Pts',(-44.979203590942,-55.7586144034376,0.));
#75187=CARTESIAN_POINT('Ctrl Pts',(-44.979203590942,-55.7586144034376,12.));
#75188=CARTESIAN_POINT('Ctrl Pts',(-44.9870649301333,-55.7806031014093,
0.));
#75189=CARTESIAN_POINT('Ctrl Pts',(-44.9870649301333,-55.7806031014093,
12.));
#75190=CARTESIAN_POINT('Ctrl Pts',(-44.9949192168073,-55.8026408548078,
0.));
#75191=CARTESIAN_POINT('Ctrl Pts',(-44.9949192168073,-55.8026408548078,
12.));
#75192=CARTESIAN_POINT('Ctrl Pts',(-45.002766347541,-55.8247275653257,0.));
#75193=CARTESIAN_POINT('Ctrl Pts',(-45.002766347541,-55.8247275653257,12.));
#75194=CARTESIAN_POINT('Ctrl Pts',(-45.0106062194325,-55.8468631350195,
0.));
#75195=CARTESIAN_POINT('Ctrl Pts',(-45.0106062194325,-55.8468631350195,
12.));
#75196=CARTESIAN_POINT('Ctrl Pts',(-45.0184387300968,-55.8690474663058,
0.));
#75197=CARTESIAN_POINT('Ctrl Pts',(-45.0184387300968,-55.8690474663058,
12.));
#75198=CARTESIAN_POINT('Ctrl Pts',(-45.0262637776623,-55.8912804619588,
0.));
#75199=CARTESIAN_POINT('Ctrl Pts',(-45.0262637776623,-55.8912804619588,
12.));
#75200=CARTESIAN_POINT('Ctrl Pts',(-45.0340812607676,-55.9135620250977,
0.));
#75201=CARTESIAN_POINT('Ctrl Pts',(-45.0340812607676,-55.9135620250977,
12.));
#75202=CARTESIAN_POINT('Ctrl Pts',(-45.041891078557,-55.9358920591861,0.));
#75203=CARTESIAN_POINT('Ctrl Pts',(-45.041891078557,-55.9358920591861,12.));
#75204=CARTESIAN_POINT('Ctrl Pts',(-45.0496931306766,-55.958270468037,0.));
#75205=CARTESIAN_POINT('Ctrl Pts',(-45.0496931306766,-55.958270468037,12.));
#75206=CARTESIAN_POINT('Ctrl Pts',(-45.0574873172696,-55.9806971558099,
0.));
#75207=CARTESIAN_POINT('Ctrl Pts',(-45.0574873172696,-55.9806971558099,
12.));
#75208=CARTESIAN_POINT('Ctrl Pts',(-45.0652735389729,-56.0031720270074,
0.));
#75209=CARTESIAN_POINT('Ctrl Pts',(-45.0652735389729,-56.0031720270074,
12.));
#75210=CARTESIAN_POINT('Ctrl Pts',(-45.0730516969142,-56.025694986463,0.));
#75211=CARTESIAN_POINT('Ctrl Pts',(-45.0730516969142,-56.025694986463,12.));
#75212=CARTESIAN_POINT('Ctrl Pts',(-45.0808216927082,-56.0482659393412,
0.));
#75213=CARTESIAN_POINT('Ctrl Pts',(-45.0808216927082,-56.0482659393412,
12.));
#75214=CARTESIAN_POINT('Ctrl Pts',(-45.0885834284513,-56.070884791141,0.));
#75215=CARTESIAN_POINT('Ctrl Pts',(-45.0885834284513,-56.070884791141,12.));
#75216=CARTESIAN_POINT('Ctrl Pts',(-45.0963368067177,-56.0935514476945,
0.));
#75217=CARTESIAN_POINT('Ctrl Pts',(-45.0963368067177,-56.0935514476945,
12.));
#75218=CARTESIAN_POINT('Ctrl Pts',(-45.1040817305563,-56.1162658151621,
0.));
#75219=CARTESIAN_POINT('Ctrl Pts',(-45.1040817305563,-56.1162658151621,
12.));
#75220=CARTESIAN_POINT('Ctrl Pts',(-45.1118181034888,-56.1390278000226,
0.));
#75221=CARTESIAN_POINT('Ctrl Pts',(-45.1118181034888,-56.1390278000226,
12.));
#75222=CARTESIAN_POINT('Ctrl Pts',(-45.119545829506,-56.1618373090729,0.));
#75223=CARTESIAN_POINT('Ctrl Pts',(-45.119545829506,-56.1618373090729,12.));
#75224=CARTESIAN_POINT('Ctrl Pts',(-45.1272648130627,-56.1846942494321,
0.));
#75225=CARTESIAN_POINT('Ctrl Pts',(-45.1272648130627,-56.1846942494321,
12.));
#75226=CARTESIAN_POINT('Ctrl Pts',(-45.1349749590736,-56.2075985285391,
0.));
#75227=CARTESIAN_POINT('Ctrl Pts',(-45.1349749590736,-56.2075985285391,
12.));
#75228=CARTESIAN_POINT('Ctrl Pts',(-45.1426761729107,-56.2305500541491,
0.));
#75229=CARTESIAN_POINT('Ctrl Pts',(-45.1426761729107,-56.2305500541491,
12.));
#75230=CARTESIAN_POINT('Ctrl Pts',(-45.150368360401,-56.2535487343227,0.));
#75231=CARTESIAN_POINT('Ctrl Pts',(-45.150368360401,-56.2535487343227,12.));
#75232=CARTESIAN_POINT('Ctrl Pts',(-45.158051427823,-56.2765944774252,0.));
#75233=CARTESIAN_POINT('Ctrl Pts',(-45.158051427823,-56.2765944774252,12.));
#75234=CARTESIAN_POINT('Ctrl Pts',(-45.1657252819018,-56.2996871921321,
0.));
#75235=CARTESIAN_POINT('Ctrl Pts',(-45.1657252819018,-56.2996871921321,
12.));
#75236=CARTESIAN_POINT('Ctrl Pts',(-45.1733898298062,-56.3228267874265,
0.));
#75237=CARTESIAN_POINT('Ctrl Pts',(-45.1733898298062,-56.3228267874265,
12.));
#75238=CARTESIAN_POINT('Ctrl Pts',(-45.1810449791451,-56.3460131725962,
0.));
#75239=CARTESIAN_POINT('Ctrl Pts',(-45.1810449791451,-56.3460131725962,
12.));
#75240=CARTESIAN_POINT('Ctrl Pts',(-45.1886906379664,-56.3692462572228,
0.));
#75241=CARTESIAN_POINT('Ctrl Pts',(-45.1886906379664,-56.3692462572228,
12.));
#75242=CARTESIAN_POINT('Ctrl Pts',(-45.1963267147527,-56.3925259511804,
0.));
#75243=CARTESIAN_POINT('Ctrl Pts',(-45.1963267147527,-56.3925259511804,
12.));
#75244=CARTESIAN_POINT('Ctrl Pts',(-45.2039531184172,-56.4158521646412,
0.));
#75245=CARTESIAN_POINT('Ctrl Pts',(-45.2039531184172,-56.4158521646412,
12.));
#75246=CARTESIAN_POINT('Ctrl Pts',(-45.2115697583002,-56.4392248080733,
0.));
#75247=CARTESIAN_POINT('Ctrl Pts',(-45.2115697583002,-56.4392248080733,
12.));
#75248=CARTESIAN_POINT('Ctrl Pts',(-45.2191765441666,-56.4626437922385,
0.));
#75249=CARTESIAN_POINT('Ctrl Pts',(-45.2191765441666,-56.4626437922385,
12.));
#75250=CARTESIAN_POINT('Ctrl Pts',(-45.2267733862046,-56.4861090281819,
0.));
#75251=CARTESIAN_POINT('Ctrl Pts',(-45.2267733862046,-56.4861090281819,
12.));
#75252=CARTESIAN_POINT('Ctrl Pts',(-45.2343601950222,-56.5096204272299,
0.));
#75253=CARTESIAN_POINT('Ctrl Pts',(-45.2343601950222,-56.5096204272299,
12.));
#75254=CARTESIAN_POINT('Ctrl Pts',(-45.2419368816423,-56.533177900995,0.));
#75255=CARTESIAN_POINT('Ctrl Pts',(-45.2419368816423,-56.533177900995,12.));
#75256=CARTESIAN_POINT('Ctrl Pts',(-45.2495033574997,-56.5567813613752,
0.));
#75257=CARTESIAN_POINT('Ctrl Pts',(-45.2495033574997,-56.5567813613752,
12.));
#75258=CARTESIAN_POINT('Ctrl Pts',(-45.2570595344382,-56.5804307205507,
0.));
#75259=CARTESIAN_POINT('Ctrl Pts',(-45.2570595344382,-56.5804307205507,
12.));
#75260=CARTESIAN_POINT('Ctrl Pts',(-45.2646053247094,-56.604125890975,0.));
#75261=CARTESIAN_POINT('Ctrl Pts',(-45.2646053247094,-56.604125890975,12.));
#75262=CARTESIAN_POINT('Ctrl Pts',(-45.2721406409706,-56.6278667853716,
0.));
#75263=CARTESIAN_POINT('Ctrl Pts',(-45.2721406409706,-56.6278667853716,
12.));
#75264=CARTESIAN_POINT('Ctrl Pts',(-45.2796653962796,-56.6516533167398,
0.));
#75265=CARTESIAN_POINT('Ctrl Pts',(-45.2796653962796,-56.6516533167398,
12.));
#75266=CARTESIAN_POINT('Ctrl Pts',(-45.2871795040912,-56.6754853983535,
0.));
#75267=CARTESIAN_POINT('Ctrl Pts',(-45.2871795040912,-56.6754853983535,
12.));
#75268=CARTESIAN_POINT('Ctrl Pts',(-45.2946828782557,-56.6993629437596,
0.));
#75269=CARTESIAN_POINT('Ctrl Pts',(-45.2946828782557,-56.6993629437596,
12.));
#75270=CARTESIAN_POINT('Ctrl Pts',(-45.3021754330169,-56.7232858667697,
0.));
#75271=CARTESIAN_POINT('Ctrl Pts',(-45.3021754330169,-56.7232858667697,
12.));
#75272=CARTESIAN_POINT('Ctrl Pts',(-45.3096570830107,-56.747254081454,0.));
#75273=CARTESIAN_POINT('Ctrl Pts',(-45.3096570830107,-56.747254081454,12.));
#75274=CARTESIAN_POINT('Ctrl Pts',(-45.3171277432592,-56.771267502148,0.));
#75275=CARTESIAN_POINT('Ctrl Pts',(-45.3171277432592,-56.771267502148,12.));
#75276=CARTESIAN_POINT('Ctrl Pts',(-45.3245873291682,-56.7953260434521,
0.));
#75277=CARTESIAN_POINT('Ctrl Pts',(-45.3245873291682,-56.7953260434521,
12.));
#75278=CARTESIAN_POINT('Ctrl Pts',(-45.3320357565241,-56.8194296202293,
0.));
#75279=CARTESIAN_POINT('Ctrl Pts',(-45.3320357565241,-56.8194296202293,
12.));
#75280=CARTESIAN_POINT('Ctrl Pts',(-45.3394729414932,-56.8435781475982,
0.));
#75281=CARTESIAN_POINT('Ctrl Pts',(-45.3394729414932,-56.8435781475982,
12.));
#75282=CARTESIAN_POINT('Ctrl Pts',(-45.3468988006202,-56.8677715409266,
0.));
#75283=CARTESIAN_POINT('Ctrl Pts',(-45.3468988006202,-56.8677715409266,
12.));
#75284=CARTESIAN_POINT('Ctrl Pts',(-45.3543132508234,-56.8920097158371,
0.));
#75285=CARTESIAN_POINT('Ctrl Pts',(-45.3543132508234,-56.8920097158371,
12.));
#75286=CARTESIAN_POINT('Ctrl Pts',(-45.3617162093918,-56.916292588208,0.));
#75287=CARTESIAN_POINT('Ctrl Pts',(-45.3617162093918,-56.916292588208,12.));
#75288=CARTESIAN_POINT('Ctrl Pts',(-45.3691075939827,-56.9406200741714,
0.));
#75289=CARTESIAN_POINT('Ctrl Pts',(-45.3691075939827,-56.9406200741714,
12.));
#75290=CARTESIAN_POINT('Ctrl Pts',(-45.3764873226202,-56.9649920901079,
0.));
#75291=CARTESIAN_POINT('Ctrl Pts',(-45.3764873226202,-56.9649920901079,
12.));
#75292=CARTESIAN_POINT('Ctrl Pts',(-45.3838553136957,-56.9894085526383,
0.));
#75293=CARTESIAN_POINT('Ctrl Pts',(-45.3838553136957,-56.9894085526383,
12.));
#75294=CARTESIAN_POINT('Ctrl Pts',(-45.3912114859625,-57.0138693786287,
0.));
#75295=CARTESIAN_POINT('Ctrl Pts',(-45.3912114859625,-57.0138693786287,
12.));
#75296=CARTESIAN_POINT('Ctrl Pts',(-45.3985557585316,-57.0383744851917,
0.));
#75297=CARTESIAN_POINT('Ctrl Pts',(-45.3985557585316,-57.0383744851917,
12.));
#75298=CARTESIAN_POINT('Ctrl Pts',(-45.4058880508693,-57.0629237896848,
0.));
#75299=CARTESIAN_POINT('Ctrl Pts',(-45.4058880508693,-57.0629237896848,
12.));
#75300=CARTESIAN_POINT('Ctrl Pts',(-45.4132082827945,-57.0875172097048,
0.));
#75301=CARTESIAN_POINT('Ctrl Pts',(-45.4132082827945,-57.0875172097048,
12.));
#75302=CARTESIAN_POINT('Ctrl Pts',(-45.4205163744778,-57.1121546630776,
0.));
#75303=CARTESIAN_POINT('Ctrl Pts',(-45.4205163744778,-57.1121546630776,
12.));
#75304=CARTESIAN_POINT('Ctrl Pts',(-45.4278122464387,-57.1368360678629,
0.));
#75305=CARTESIAN_POINT('Ctrl Pts',(-45.4278122464387,-57.1368360678629,
12.));
#75306=CARTESIAN_POINT('Ctrl Pts',(-45.4350958195434,-57.1615613423586,
0.));
#75307=CARTESIAN_POINT('Ctrl Pts',(-45.4350958195434,-57.1615613423586,
12.));
#75308=CARTESIAN_POINT('Ctrl Pts',(-45.4423670150035,-57.1863304051011,
0.));
#75309=CARTESIAN_POINT('Ctrl Pts',(-45.4423670150035,-57.1863304051011,
12.));
#75310=CARTESIAN_POINT('Ctrl Pts',(-45.4496257543759,-57.2111431748629,
0.));
#75311=CARTESIAN_POINT('Ctrl Pts',(-45.4496257543759,-57.2111431748629,
12.));
#75312=CARTESIAN_POINT('Ctrl Pts',(-45.4568719595639,-57.2359995706441,
0.));
#75313=CARTESIAN_POINT('Ctrl Pts',(-45.4568719595639,-57.2359995706441,
12.));
#75314=CARTESIAN_POINT('Ctrl Pts',(-45.4641055528138,-57.2608995116727,
0.));
#75315=CARTESIAN_POINT('Ctrl Pts',(-45.4641055528138,-57.2608995116727,
12.));
#75316=CARTESIAN_POINT('Ctrl Pts',(-45.4713264567059,-57.2858429174056,
0.));
#75317=CARTESIAN_POINT('Ctrl Pts',(-45.4713264567059,-57.2858429174056,
12.));
#75318=CARTESIAN_POINT('Ctrl Pts',(-45.4785345941505,-57.3108297075262,
0.));
#75319=CARTESIAN_POINT('Ctrl Pts',(-45.4785345941505,-57.3108297075262,
12.));
#75320=CARTESIAN_POINT('Ctrl Pts',(-45.4857298883826,-57.3358598019391,
0.));
#75321=CARTESIAN_POINT('Ctrl Pts',(-45.4857298883826,-57.3358598019391,
12.));
#75322=CARTESIAN_POINT('Ctrl Pts',(-45.4929122629576,-57.360933120758,0.));
#75323=CARTESIAN_POINT('Ctrl Pts',(-45.4929122629576,-57.360933120758,12.));
#75324=CARTESIAN_POINT('Ctrl Pts',(-45.5000816417516,-57.3860495843043,
0.));
#75325=CARTESIAN_POINT('Ctrl Pts',(-45.5000816417516,-57.3860495843043,
12.));
#75326=CARTESIAN_POINT('Ctrl Pts',(-45.5072379489637,-57.4112091131193,
0.));
#75327=CARTESIAN_POINT('Ctrl Pts',(-45.5072379489637,-57.4112091131193,
12.));
#75328=CARTESIAN_POINT('Ctrl Pts',(-45.5143811091209,-57.4364116279708,
0.));
#75329=CARTESIAN_POINT('Ctrl Pts',(-45.5143811091209,-57.4364116279708,
12.));
#75330=CARTESIAN_POINT('Ctrl Pts',(-45.5215110470825,-57.4616570498566,
0.));
#75331=CARTESIAN_POINT('Ctrl Pts',(-45.5215110470825,-57.4616570498566,
12.));
#75332=CARTESIAN_POINT('Ctrl Pts',(-45.5286276880479,-57.4869453000055,
0.));
#75333=CARTESIAN_POINT('Ctrl Pts',(-45.5286276880479,-57.4869453000055,
12.));
#75334=CARTESIAN_POINT('Ctrl Pts',(-45.5357309575603,-57.5122762998732,
0.));
#75335=CARTESIAN_POINT('Ctrl Pts',(-45.5357309575603,-57.5122762998732,
12.));
#75336=CARTESIAN_POINT('Ctrl Pts',(-45.5428207814832,-57.5376499711338,
0.));
#75337=CARTESIAN_POINT('Ctrl Pts',(-45.5428207814832,-57.5376499711338,
12.));
#75338=CARTESIAN_POINT('Ctrl Pts',(-45.5498970859829,-57.5630662356671,
0.));
#75339=CARTESIAN_POINT('Ctrl Pts',(-45.5498970859829,-57.5630662356671,
12.));
#75340=CARTESIAN_POINT('Ctrl Pts',(-45.5569597975096,-57.5885250155432,
0.));
#75341=CARTESIAN_POINT('Ctrl Pts',(-45.5569597975096,-57.5885250155432,
12.));
#75342=CARTESIAN_POINT('Ctrl Pts',(-45.5640088427819,-57.6140262330048,
0.));
#75343=CARTESIAN_POINT('Ctrl Pts',(-45.5640088427819,-57.6140262330048,
12.));
#75344=CARTESIAN_POINT('Ctrl Pts',(-45.5710441487683,-57.6395698104416,
0.));
#75345=CARTESIAN_POINT('Ctrl Pts',(-45.5710441487683,-57.6395698104416,
12.));
#75346=CARTESIAN_POINT('Ctrl Pts',(-45.5780656427172,-57.6651556704249,
0.));
#75347=CARTESIAN_POINT('Ctrl Pts',(-45.5780656427172,-57.6651556704249,
12.));
#75348=CARTESIAN_POINT('Ctrl Pts',(-45.5850732521902,-57.6907837357425,
0.));
#75349=CARTESIAN_POINT('Ctrl Pts',(-45.5850732521902,-57.6907837357425,
12.));
#75350=CARTESIAN_POINT('Ctrl Pts',(-45.5920669050988,-57.7164539294316,
0.));
#75351=CARTESIAN_POINT('Ctrl Pts',(-45.5920669050988,-57.7164539294316,
12.));
#75352=CARTESIAN_POINT('Ctrl Pts',(-45.5990465297341,-57.7421661748022,
0.));
#75353=CARTESIAN_POINT('Ctrl Pts',(-45.5990465297341,-57.7421661748022,
12.));
#75354=CARTESIAN_POINT('Ctrl Pts',(-45.6060120548199,-57.7679203954735,
0.));
#75355=CARTESIAN_POINT('Ctrl Pts',(-45.6060120548199,-57.7679203954735,
12.));
#75356=CARTESIAN_POINT('Ctrl Pts',(-45.6129634094677,-57.7937165153379,
0.));
#75357=CARTESIAN_POINT('Ctrl Pts',(-45.6129634094677,-57.7937165153379,
12.));
#75358=CARTESIAN_POINT('Ctrl Pts',(-45.619900523078,-57.819554458484,0.));
#75359=CARTESIAN_POINT('Ctrl Pts',(-45.619900523078,-57.819554458484,12.));
#75360=CARTESIAN_POINT('Ctrl Pts',(-45.6268233252543,-57.8454341491236,
0.));
#75361=CARTESIAN_POINT('Ctrl Pts',(-45.6268233252543,-57.8454341491236,
12.));
#75362=CARTESIAN_POINT('Ctrl Pts',(-45.6337317457253,-57.8713555115232,
0.));
#75363=CARTESIAN_POINT('Ctrl Pts',(-45.6337317457253,-57.8713555115232,
12.));
#75364=CARTESIAN_POINT('Ctrl Pts',(-45.6406257142385,-57.8973184699037,
0.));
#75365=CARTESIAN_POINT('Ctrl Pts',(-45.6406257142385,-57.8973184699037,
12.));
#75366=CARTESIAN_POINT('Ctrl Pts',(-45.6475051605542,-57.923322948432,0.));
#75367=CARTESIAN_POINT('Ctrl Pts',(-45.6475051605542,-57.923322948432,12.));
#75368=CARTESIAN_POINT('Ctrl Pts',(-45.6543700146689,-57.9493688714249,
0.));
#75369=CARTESIAN_POINT('Ctrl Pts',(-45.6543700146689,-57.9493688714249,
12.));
#75370=CARTESIAN_POINT('Ctrl Pts',(-45.6612202069927,-57.975456163507,0.));
#75371=CARTESIAN_POINT('Ctrl Pts',(-45.6612202069927,-57.975456163507,12.));
#75372=CARTESIAN_POINT('Ctrl Pts',(-45.6680556685494,-58.0015847497838,
0.));
#75373=CARTESIAN_POINT('Ctrl Pts',(-45.6680556685494,-58.0015847497838,
12.));
#75374=CARTESIAN_POINT('Ctrl Pts',(-45.6748763311635,-58.0277545560001,
0.));
#75375=CARTESIAN_POINT('Ctrl Pts',(-45.6748763311635,-58.0277545560001,
12.));
#75376=CARTESIAN_POINT('Ctrl Pts',(-45.6816821276662,-58.0539655087095,
0.));
#75377=CARTESIAN_POINT('Ctrl Pts',(-45.6816821276662,-58.0539655087095,
12.));
#75378=CARTESIAN_POINT('Ctrl Pts',(-45.6884729914465,-58.0802175348939,
0.));
#75379=CARTESIAN_POINT('Ctrl Pts',(-45.6884729914465,-58.0802175348939,
12.));
#75380=CARTESIAN_POINT('Ctrl Pts',(-45.6952488560133,-58.1065105615884,
0.));
#75381=CARTESIAN_POINT('Ctrl Pts',(-45.6952488560133,-58.1065105615884,
12.));
#75382=CARTESIAN_POINT('Ctrl Pts',(-45.7020096545174,-58.1328445154667,
0.));
#75383=CARTESIAN_POINT('Ctrl Pts',(-45.7020096545174,-58.1328445154667,
12.));
#75384=CARTESIAN_POINT('Ctrl Pts',(-45.708755319378,-58.159219322515,0.));
#75385=CARTESIAN_POINT('Ctrl Pts',(-45.708755319378,-58.159219322515,12.));
#75386=CARTESIAN_POINT('Ctrl Pts',(-45.7154857816507,-58.1856349074723,
0.));
#75387=CARTESIAN_POINT('Ctrl Pts',(-45.7154857816507,-58.1856349074723,
12.));
#75388=CARTESIAN_POINT('Ctrl Pts',(-45.7222009715431,-58.2120911942819,
0.));
#75389=CARTESIAN_POINT('Ctrl Pts',(-45.7222009715431,-58.2120911942819,
12.));
#75390=CARTESIAN_POINT('Ctrl Pts',(-45.7289008195612,-58.2385881070959,
0.));
#75391=CARTESIAN_POINT('Ctrl Pts',(-45.7289008195612,-58.2385881070959,
12.));
#75392=CARTESIAN_POINT('Ctrl Pts',(-45.7355852575127,-58.2651255711481,
0.));
#75393=CARTESIAN_POINT('Ctrl Pts',(-45.7355852575127,-58.2651255711481,
12.));
#75394=CARTESIAN_POINT('Ctrl Pts',(-45.7422542194625,-58.2917035135833,
0.));
#75395=CARTESIAN_POINT('Ctrl Pts',(-45.7422542194625,-58.2917035135833,
12.));
#75396=CARTESIAN_POINT('Ctrl Pts',(-45.7489076429725,-58.3183218645265,
0.));
#75397=CARTESIAN_POINT('Ctrl Pts',(-45.7489076429725,-58.3183218645265,
12.));
#75398=CARTESIAN_POINT('Ctrl Pts',(-45.7555454693956,-58.3449805573335,
0.));
#75399=CARTESIAN_POINT('Ctrl Pts',(-45.7555454693956,-58.3449805573335,
12.));
#75400=CARTESIAN_POINT('Ctrl Pts',(-45.762167641136,-58.3716795262251,0.));
#75401=CARTESIAN_POINT('Ctrl Pts',(-45.762167641136,-58.3716795262251,12.));
#75402=CARTESIAN_POINT('Ctrl Pts',(-45.7687740994899,-58.3984187044166,
0.));
#75403=CARTESIAN_POINT('Ctrl Pts',(-45.7687740994899,-58.3984187044166,
12.));
#75404=CARTESIAN_POINT('Ctrl Pts',(-45.77536478215,-58.4251980219532,0.));
#75405=CARTESIAN_POINT('Ctrl Pts',(-45.77536478215,-58.4251980219532,12.));
#75406=CARTESIAN_POINT('Ctrl Pts',(-45.7819396211062,-58.4520174038836,
0.));
#75407=CARTESIAN_POINT('Ctrl Pts',(-45.7819396211062,-58.4520174038836,
12.));
#75408=CARTESIAN_POINT('Ctrl Pts',(-45.7884985397138,-58.4788767677114,
0.));
#75409=CARTESIAN_POINT('Ctrl Pts',(-45.7884985397138,-58.4788767677114,
12.));
#75410=CARTESIAN_POINT('Ctrl Pts',(-45.7950414569431,-58.5057760270407,
0.));
#75411=CARTESIAN_POINT('Ctrl Pts',(-45.7950414569431,-58.5057760270407,
12.));
#75412=CARTESIAN_POINT('Ctrl Pts',(-45.801568292618,-58.5327150960874,0.));
#75413=CARTESIAN_POINT('Ctrl Pts',(-45.801568292618,-58.5327150960874,12.));
#75414=CARTESIAN_POINT('Ctrl Pts',(-45.8080789725167,-58.5596938940308,
0.));
#75415=CARTESIAN_POINT('Ctrl Pts',(-45.8080789725167,-58.5596938940308,
12.));
#75416=CARTESIAN_POINT('Ctrl Pts',(-45.8145734330666,-58.5867123490943,
0.));
#75417=CARTESIAN_POINT('Ctrl Pts',(-45.8145734330666,-58.5867123490943,
12.));
#75418=CARTESIAN_POINT('Ctrl Pts',(-45.8210516273556,-58.6137704035561,
0.));
#75419=CARTESIAN_POINT('Ctrl Pts',(-45.8210516273556,-58.6137704035561,
12.));
#75420=CARTESIAN_POINT('Ctrl Pts',(-45.8275135263874,-58.64086801535,0.));
#75421=CARTESIAN_POINT('Ctrl Pts',(-45.8275135263874,-58.64086801535,12.));
#75422=CARTESIAN_POINT('Ctrl Pts',(-45.8339591141396,-58.668005155216,0.));
#75423=CARTESIAN_POINT('Ctrl Pts',(-45.8339591141396,-58.668005155216,12.));
#75424=CARTESIAN_POINT('Ctrl Pts',(-45.8391025301766,-58.6897464750196,
0.));
#75425=CARTESIAN_POINT('Ctrl Pts',(-45.8391025301766,-58.6897464750196,
12.));
#75426=CARTESIAN_POINT('Ctrl Pts',(-45.8429527488565,-58.7060702401382,
0.));
#75427=CARTESIAN_POINT('Ctrl Pts',(-45.8429527488565,-58.7060702401382,
12.));
#75428=CARTESIAN_POINT('Ctrl Pts',(-45.8455162977347,-58.7169606500157,
0.));
#75429=CARTESIAN_POINT('Ctrl Pts',(-45.8455162977347,-58.7169606500157,
12.));
#75430=CARTESIAN_POINT('Ctrl Pts',(-45.8467972562798,-58.722407829904,0.));
#75431=CARTESIAN_POINT('Ctrl Pts',(-45.8467972562798,-58.722407829904,12.));
#75432=CARTESIAN_POINT('',(-44.3377168516418,-54.1679505278134,0.));
#75433=CARTESIAN_POINT('Ctrl Pts',(-44.3377168516418,-54.1679505278134,
0.));
#75434=CARTESIAN_POINT('Ctrl Pts',(-44.3393235891014,-54.1714861895278,
0.));
#75435=CARTESIAN_POINT('Ctrl Pts',(-44.3425373700829,-54.1785633257456,
0.));
#75436=CARTESIAN_POINT('Ctrl Pts',(-44.3473589597468,-54.1891964684439,
0.));
#75437=CARTESIAN_POINT('Ctrl Pts',(-44.3537895823819,-54.203408870162,0.));
#75438=CARTESIAN_POINT('Ctrl Pts',(-44.3618309103245,-54.2212325005847,
0.));
#75439=CARTESIAN_POINT('Ctrl Pts',(-44.369875253351,-54.2391142386354,0.));
#75440=CARTESIAN_POINT('Ctrl Pts',(-44.3779225430461,-54.2570540336536,
0.));
#75441=CARTESIAN_POINT('Ctrl Pts',(-44.3859726620288,-54.2750517888695,
0.));
#75442=CARTESIAN_POINT('Ctrl Pts',(-44.3940254456427,-54.2931073621661,
0.));
#75443=CARTESIAN_POINT('Ctrl Pts',(-44.4020807028144,-54.3112205860776,
0.));
#75444=CARTESIAN_POINT('Ctrl Pts',(-44.4101382321834,-54.3293912830237,
0.));
#75445=CARTESIAN_POINT('Ctrl Pts',(-44.4181978395814,-54.347619281931,0.));
#75446=CARTESIAN_POINT('Ctrl Pts',(-44.4262593564664,-54.3659044357064,
0.));
#75447=CARTESIAN_POINT('Ctrl Pts',(-44.4343226339555,-54.3842466156151,
0.));
#75448=CARTESIAN_POINT('Ctrl Pts',(-44.442387534098,-54.4026457030316,0.));
#75449=CARTESIAN_POINT('Ctrl Pts',(-44.4504539226336,-54.4211015825959,
0.));
#75450=CARTESIAN_POINT('Ctrl Pts',(-44.4585216599933,-54.4396141337008,
0.));
#75451=CARTESIAN_POINT('Ctrl Pts',(-44.4665905967701,-54.4581832262072,
0.));
#75452=CARTESIAN_POINT('Ctrl Pts',(-44.4746605784056,-54.4768087248854,
0.));
#75453=CARTESIAN_POINT('Ctrl Pts',(-44.482731448127,-54.4954904921938,0.));
#75454=CARTESIAN_POINT('Ctrl Pts',(-44.4908030503209,-54.5142283914684,
0.));
#75455=CARTESIAN_POINT('Ctrl Pts',(-44.4988752343715,-54.5330222905438,
0.));
#75456=CARTESIAN_POINT('Ctrl Pts',(-44.5069478544945,-54.5518720616016,
0.));
#75457=CARTESIAN_POINT('Ctrl Pts',(-44.5150207678988,-54.5707775794412,
0.));
#75458=CARTESIAN_POINT('Ctrl Pts',(-44.5230938335167,-54.5897387202815,
0.));
#75459=CARTESIAN_POINT('Ctrl Pts',(-44.5311669104515,-54.6087553602914,
0.));
#75460=CARTESIAN_POINT('Ctrl Pts',(-44.5392398566802,-54.6278273743587,
0.));
#75461=CARTESIAN_POINT('Ctrl Pts',(-44.5473125297311,-54.6469546367408,
0.));
#75462=CARTESIAN_POINT('Ctrl Pts',(-44.5553847872721,-54.6661370216252,
0.));
#75463=CARTESIAN_POINT('Ctrl Pts',(-44.5634564876863,-54.6853744036751,
0.));
#75464=CARTESIAN_POINT('Ctrl Pts',(-44.5715274907619,-54.7046666586754,
0.));
#75465=CARTESIAN_POINT('Ctrl Pts',(-44.5795976579454,-54.7240136637717,
0.));
#75466=CARTESIAN_POINT('Ctrl Pts',(-44.5876668519661,-54.7434152971267,
0.));
#75467=CARTESIAN_POINT('Ctrl Pts',(-44.5957349366059,-54.7628714377037,
0.));
#75468=CARTESIAN_POINT('Ctrl Pts',(-44.6038017764309,-54.7823819650149,
0.));
#75469=CARTESIAN_POINT('Ctrl Pts',(-44.6118672364906,-54.8019467588278,
0.));
#75470=CARTESIAN_POINT('Ctrl Pts',(-44.6199311823293,-54.8215656991837,
0.));
#75471=CARTESIAN_POINT('Ctrl Pts',(-44.6279934801169,-54.8412386665276,
0.));
#75472=CARTESIAN_POINT('Ctrl Pts',(-44.6360539967392,-54.860965541796,0.));
#75473=CARTESIAN_POINT('Ctrl Pts',(-44.6441125999063,-54.8807462065164,
0.));
#75474=CARTESIAN_POINT('Ctrl Pts',(-44.6521691582533,-54.9005805428969,
0.));
#75475=CARTESIAN_POINT('Ctrl Pts',(-44.6602235412836,-54.9204684337822,
0.));
#75476=CARTESIAN_POINT('Ctrl Pts',(-44.6682756193147,-54.9404097626077,
0.));
#75477=CARTESIAN_POINT('Ctrl Pts',(-44.6763252634258,-54.9604044133501,
0.));
#75478=CARTESIAN_POINT('Ctrl Pts',(-44.6843723454,-54.9804522704686,0.));
#75479=CARTESIAN_POINT('Ctrl Pts',(-44.6924167376869,-55.0005532188667,
0.));
#75480=CARTESIAN_POINT('Ctrl Pts',(-44.7004583134249,-55.0207071439237,
0.));
#75481=CARTESIAN_POINT('Ctrl Pts',(-44.7084969464513,-55.0409139315078,
0.));
#75482=CARTESIAN_POINT('Ctrl Pts',(-44.7165325113159,-55.0611734679894,
0.));
#75483=CARTESIAN_POINT('Ctrl Pts',(-44.7245648832979,-55.0814856402496,
0.));
#75484=CARTESIAN_POINT('Ctrl Pts',(-44.7325939384035,-55.1018503356796,
0.));
#75485=CARTESIAN_POINT('Ctrl Pts',(-44.740619553348,-55.1222674421743,0.));
#75486=CARTESIAN_POINT('Ctrl Pts',(-44.748641605542,-55.14273684812,0.));
#75487=CARTESIAN_POINT('Ctrl Pts',(-44.7566599730773,-55.1632584423815,
0.));
#75488=CARTESIAN_POINT('Ctrl Pts',(-44.7646745347109,-55.1838321142779,
0.));
#75489=CARTESIAN_POINT('Ctrl Pts',(-44.7726851698619,-55.2044577535866,
0.));
#75490=CARTESIAN_POINT('Ctrl Pts',(-44.7806917586077,-55.2251352505475,
0.));
#75491=CARTESIAN_POINT('Ctrl Pts',(-44.7886941816823,-55.2458644958617,
0.));
#75492=CARTESIAN_POINT('Ctrl Pts',(-44.7966923204741,-55.2666453806883,
0.));
#75493=CARTESIAN_POINT('Ctrl Pts',(-44.8046860570245,-55.287477796635,0.));
#75494=CARTESIAN_POINT('Ctrl Pts',(-44.812675274021,-55.3083616357605,0.));
#75495=CARTESIAN_POINT('Ctrl Pts',(-44.8206598547889,-55.3292967905726,
0.));
#75496=CARTESIAN_POINT('Ctrl Pts',(-44.8286396832849,-55.350283154023,0.));
#75497=CARTESIAN_POINT('Ctrl Pts',(-44.8366146440896,-55.3713206194962,
0.));
#75498=CARTESIAN_POINT('Ctrl Pts',(-44.8445846224034,-55.3924090808002,
0.));
#75499=CARTESIAN_POINT('Ctrl Pts',(-44.8525495040397,-55.4135484321706,
0.));
#75500=CARTESIAN_POINT('Ctrl Pts',(-44.8605091754208,-55.4347385682697,
0.));
#75501=CARTESIAN_POINT('Ctrl Pts',(-44.8684635235727,-55.4559793841838,
0.));
#75502=CARTESIAN_POINT('Ctrl Pts',(-44.8764124361218,-55.4772707754139,
0.));
#75503=CARTESIAN_POINT('Ctrl Pts',(-44.8843558012903,-55.4986126378676,
0.));
#75504=CARTESIAN_POINT('Ctrl Pts',(-44.8922935078905,-55.5200048678648,
0.));
#75505=CARTESIAN_POINT('Ctrl Pts',(-44.9002254453192,-55.541447362135,0.));
#75506=CARTESIAN_POINT('Ctrl Pts',(-44.9081515035525,-55.5629400178136,
0.));
#75507=CARTESIAN_POINT('Ctrl Pts',(-44.9160715731425,-55.5844827324315,
0.));
#75508=CARTESIAN_POINT('Ctrl Pts',(-44.9239855452119,-55.6060754039089,
0.));
#75509=CARTESIAN_POINT('Ctrl Pts',(-44.9318933114483,-55.6277179305604,
0.));
#75510=CARTESIAN_POINT('Ctrl Pts',(-44.9397947640996,-55.6494102110922,
0.));
#75511=CARTESIAN_POINT('Ctrl Pts',(-44.9476897959694,-55.671152144599,0.));
#75512=CARTESIAN_POINT('Ctrl Pts',(-44.9555783004133,-55.6929436305522,
0.));
#75513=CARTESIAN_POINT('Ctrl Pts',(-44.9634601713352,-55.7147845687969,
0.));
#75514=CARTESIAN_POINT('Ctrl Pts',(-44.9713353031827,-55.7366748595582,
0.));
#75515=CARTESIAN_POINT('Ctrl Pts',(-44.979203590942,-55.7586144034376,0.));
#75516=CARTESIAN_POINT('Ctrl Pts',(-44.9870649301333,-55.7806031014093,
0.));
#75517=CARTESIAN_POINT('Ctrl Pts',(-44.9949192168073,-55.8026408548078,
0.));
#75518=CARTESIAN_POINT('Ctrl Pts',(-45.002766347541,-55.8247275653257,0.));
#75519=CARTESIAN_POINT('Ctrl Pts',(-45.0106062194325,-55.8468631350195,
0.));
#75520=CARTESIAN_POINT('Ctrl Pts',(-45.0184387300968,-55.8690474663058,
0.));
#75521=CARTESIAN_POINT('Ctrl Pts',(-45.0262637776623,-55.8912804619588,
0.));
#75522=CARTESIAN_POINT('Ctrl Pts',(-45.0340812607676,-55.9135620250977,
0.));
#75523=CARTESIAN_POINT('Ctrl Pts',(-45.041891078557,-55.9358920591861,0.));
#75524=CARTESIAN_POINT('Ctrl Pts',(-45.0496931306766,-55.958270468037,0.));
#75525=CARTESIAN_POINT('Ctrl Pts',(-45.0574873172696,-55.9806971558099,
0.));
#75526=CARTESIAN_POINT('Ctrl Pts',(-45.0652735389729,-56.0031720270074,
0.));
#75527=CARTESIAN_POINT('Ctrl Pts',(-45.0730516969142,-56.025694986463,0.));
#75528=CARTESIAN_POINT('Ctrl Pts',(-45.0808216927082,-56.0482659393412,
0.));
#75529=CARTESIAN_POINT('Ctrl Pts',(-45.0885834284513,-56.070884791141,0.));
#75530=CARTESIAN_POINT('Ctrl Pts',(-45.0963368067177,-56.0935514476945,
0.));
#75531=CARTESIAN_POINT('Ctrl Pts',(-45.1040817305563,-56.1162658151621,
0.));
#75532=CARTESIAN_POINT('Ctrl Pts',(-45.1118181034888,-56.1390278000226,
0.));
#75533=CARTESIAN_POINT('Ctrl Pts',(-45.119545829506,-56.1618373090729,0.));
#75534=CARTESIAN_POINT('Ctrl Pts',(-45.1272648130627,-56.1846942494321,
0.));
#75535=CARTESIAN_POINT('Ctrl Pts',(-45.1349749590736,-56.2075985285391,
0.));
#75536=CARTESIAN_POINT('Ctrl Pts',(-45.1426761729107,-56.2305500541491,
0.));
#75537=CARTESIAN_POINT('Ctrl Pts',(-45.150368360401,-56.2535487343227,0.));
#75538=CARTESIAN_POINT('Ctrl Pts',(-45.158051427823,-56.2765944774252,0.));
#75539=CARTESIAN_POINT('Ctrl Pts',(-45.1657252819018,-56.2996871921321,
0.));
#75540=CARTESIAN_POINT('Ctrl Pts',(-45.1733898298062,-56.3228267874265,
0.));
#75541=CARTESIAN_POINT('Ctrl Pts',(-45.1810449791451,-56.3460131725962,
0.));
#75542=CARTESIAN_POINT('Ctrl Pts',(-45.1886906379664,-56.3692462572228,
0.));
#75543=CARTESIAN_POINT('Ctrl Pts',(-45.1963267147527,-56.3925259511804,
0.));
#75544=CARTESIAN_POINT('Ctrl Pts',(-45.2039531184172,-56.4158521646412,
0.));
#75545=CARTESIAN_POINT('Ctrl Pts',(-45.2115697583002,-56.4392248080733,
0.));
#75546=CARTESIAN_POINT('Ctrl Pts',(-45.2191765441666,-56.4626437922385,
0.));
#75547=CARTESIAN_POINT('Ctrl Pts',(-45.2267733862046,-56.4861090281819,
0.));
#75548=CARTESIAN_POINT('Ctrl Pts',(-45.2343601950222,-56.5096204272299,
0.));
#75549=CARTESIAN_POINT('Ctrl Pts',(-45.2419368816423,-56.533177900995,0.));
#75550=CARTESIAN_POINT('Ctrl Pts',(-45.2495033574997,-56.5567813613752,
0.));
#75551=CARTESIAN_POINT('Ctrl Pts',(-45.2570595344382,-56.5804307205507,
0.));
#75552=CARTESIAN_POINT('Ctrl Pts',(-45.2646053247094,-56.604125890975,0.));
#75553=CARTESIAN_POINT('Ctrl Pts',(-45.2721406409706,-56.6278667853716,
0.));
#75554=CARTESIAN_POINT('Ctrl Pts',(-45.2796653962796,-56.6516533167398,
0.));
#75555=CARTESIAN_POINT('Ctrl Pts',(-45.2871795040912,-56.6754853983535,
0.));
#75556=CARTESIAN_POINT('Ctrl Pts',(-45.2946828782557,-56.6993629437596,
0.));
#75557=CARTESIAN_POINT('Ctrl Pts',(-45.3021754330169,-56.7232858667697,
0.));
#75558=CARTESIAN_POINT('Ctrl Pts',(-45.3096570830107,-56.747254081454,0.));
#75559=CARTESIAN_POINT('Ctrl Pts',(-45.3171277432592,-56.771267502148,0.));
#75560=CARTESIAN_POINT('Ctrl Pts',(-45.3245873291682,-56.7953260434521,
0.));
#75561=CARTESIAN_POINT('Ctrl Pts',(-45.3320357565241,-56.8194296202293,
0.));
#75562=CARTESIAN_POINT('Ctrl Pts',(-45.3394729414932,-56.8435781475982,
0.));
#75563=CARTESIAN_POINT('Ctrl Pts',(-45.3468988006202,-56.8677715409266,
0.));
#75564=CARTESIAN_POINT('Ctrl Pts',(-45.3543132508234,-56.8920097158371,
0.));
#75565=CARTESIAN_POINT('Ctrl Pts',(-45.3617162093918,-56.916292588208,0.));
#75566=CARTESIAN_POINT('Ctrl Pts',(-45.3691075939827,-56.9406200741714,
0.));
#75567=CARTESIAN_POINT('Ctrl Pts',(-45.3764873226202,-56.9649920901079,
0.));
#75568=CARTESIAN_POINT('Ctrl Pts',(-45.3838553136957,-56.9894085526383,
0.));
#75569=CARTESIAN_POINT('Ctrl Pts',(-45.3912114859625,-57.0138693786287,
0.));
#75570=CARTESIAN_POINT('Ctrl Pts',(-45.3985557585316,-57.0383744851917,
0.));
#75571=CARTESIAN_POINT('Ctrl Pts',(-45.4058880508693,-57.0629237896848,
0.));
#75572=CARTESIAN_POINT('Ctrl Pts',(-45.4132082827945,-57.0875172097048,
0.));
#75573=CARTESIAN_POINT('Ctrl Pts',(-45.4205163744778,-57.1121546630776,
0.));
#75574=CARTESIAN_POINT('Ctrl Pts',(-45.4278122464387,-57.1368360678629,
0.));
#75575=CARTESIAN_POINT('Ctrl Pts',(-45.4350958195434,-57.1615613423586,
0.));
#75576=CARTESIAN_POINT('Ctrl Pts',(-45.4423670150035,-57.1863304051011,
0.));
#75577=CARTESIAN_POINT('Ctrl Pts',(-45.4496257543759,-57.2111431748629,
0.));
#75578=CARTESIAN_POINT('Ctrl Pts',(-45.4568719595639,-57.2359995706441,
0.));
#75579=CARTESIAN_POINT('Ctrl Pts',(-45.4641055528138,-57.2608995116727,
0.));
#75580=CARTESIAN_POINT('Ctrl Pts',(-45.4713264567059,-57.2858429174056,
0.));
#75581=CARTESIAN_POINT('Ctrl Pts',(-45.4785345941505,-57.3108297075262,
0.));
#75582=CARTESIAN_POINT('Ctrl Pts',(-45.4857298883826,-57.3358598019391,
0.));
#75583=CARTESIAN_POINT('Ctrl Pts',(-45.4929122629576,-57.360933120758,0.));
#75584=CARTESIAN_POINT('Ctrl Pts',(-45.5000816417516,-57.3860495843043,
0.));
#75585=CARTESIAN_POINT('Ctrl Pts',(-45.5072379489637,-57.4112091131193,
0.));
#75586=CARTESIAN_POINT('Ctrl Pts',(-45.5143811091209,-57.4364116279708,
0.));
#75587=CARTESIAN_POINT('Ctrl Pts',(-45.5215110470825,-57.4616570498566,
0.));
#75588=CARTESIAN_POINT('Ctrl Pts',(-45.5286276880479,-57.4869453000055,
0.));
#75589=CARTESIAN_POINT('Ctrl Pts',(-45.5357309575603,-57.5122762998732,
0.));
#75590=CARTESIAN_POINT('Ctrl Pts',(-45.5428207814832,-57.5376499711338,
0.));
#75591=CARTESIAN_POINT('Ctrl Pts',(-45.5498970859829,-57.5630662356671,
0.));
#75592=CARTESIAN_POINT('Ctrl Pts',(-45.5569597975096,-57.5885250155432,
0.));
#75593=CARTESIAN_POINT('Ctrl Pts',(-45.5640088427819,-57.6140262330048,
0.));
#75594=CARTESIAN_POINT('Ctrl Pts',(-45.5710441487683,-57.6395698104416,
0.));
#75595=CARTESIAN_POINT('Ctrl Pts',(-45.5780656427172,-57.6651556704249,
0.));
#75596=CARTESIAN_POINT('Ctrl Pts',(-45.5850732521902,-57.6907837357425,
0.));
#75597=CARTESIAN_POINT('Ctrl Pts',(-45.5920669050988,-57.7164539294316,
0.));
#75598=CARTESIAN_POINT('Ctrl Pts',(-45.5990465297341,-57.7421661748022,
0.));
#75599=CARTESIAN_POINT('Ctrl Pts',(-45.6060120548199,-57.7679203954735,
0.));
#75600=CARTESIAN_POINT('Ctrl Pts',(-45.6129634094677,-57.7937165153379,
0.));
#75601=CARTESIAN_POINT('Ctrl Pts',(-45.619900523078,-57.819554458484,0.));
#75602=CARTESIAN_POINT('Ctrl Pts',(-45.6268233252543,-57.8454341491236,
0.));
#75603=CARTESIAN_POINT('Ctrl Pts',(-45.6337317457253,-57.8713555115232,
0.));
#75604=CARTESIAN_POINT('Ctrl Pts',(-45.6406257142385,-57.8973184699037,
0.));
#75605=CARTESIAN_POINT('Ctrl Pts',(-45.6475051605542,-57.923322948432,0.));
#75606=CARTESIAN_POINT('Ctrl Pts',(-45.6543700146689,-57.9493688714249,
0.));
#75607=CARTESIAN_POINT('Ctrl Pts',(-45.6612202069927,-57.975456163507,0.));
#75608=CARTESIAN_POINT('Ctrl Pts',(-45.6680556685494,-58.0015847497838,
0.));
#75609=CARTESIAN_POINT('Ctrl Pts',(-45.6748763311635,-58.0277545560001,
0.));
#75610=CARTESIAN_POINT('Ctrl Pts',(-45.6816821276662,-58.0539655087095,
0.));
#75611=CARTESIAN_POINT('Ctrl Pts',(-45.6884729914465,-58.0802175348939,
0.));
#75612=CARTESIAN_POINT('Ctrl Pts',(-45.6952488560133,-58.1065105615884,
0.));
#75613=CARTESIAN_POINT('Ctrl Pts',(-45.7020096545174,-58.1328445154667,
0.));
#75614=CARTESIAN_POINT('Ctrl Pts',(-45.708755319378,-58.159219322515,0.));
#75615=CARTESIAN_POINT('Ctrl Pts',(-45.7154857816507,-58.1856349074723,
0.));
#75616=CARTESIAN_POINT('Ctrl Pts',(-45.7222009715431,-58.2120911942819,
0.));
#75617=CARTESIAN_POINT('Ctrl Pts',(-45.7289008195612,-58.2385881070959,
0.));
#75618=CARTESIAN_POINT('Ctrl Pts',(-45.7355852575127,-58.2651255711481,
0.));
#75619=CARTESIAN_POINT('Ctrl Pts',(-45.7422542194625,-58.2917035135833,
0.));
#75620=CARTESIAN_POINT('Ctrl Pts',(-45.7489076429725,-58.3183218645265,
0.));
#75621=CARTESIAN_POINT('Ctrl Pts',(-45.7555454693956,-58.3449805573335,
0.));
#75622=CARTESIAN_POINT('Ctrl Pts',(-45.7612219538034,-58.3678667473266,
0.));
#75623=CARTESIAN_POINT('Ctrl Pts',(-45.7655655205267,-58.385434851721,0.));
#75624=CARTESIAN_POINT('Ctrl Pts',(-45.7685831165459,-58.3976670480781,
0.));
#75625=CARTESIAN_POINT('Ctrl Pts',(-45.7702793558063,-58.4045515723008,
0.));
#75626=CARTESIAN_POINT('Ctrl Pts',(-45.7706564944767,-58.4060826907379,
0.));
#75627=CARTESIAN_POINT('',(-44.3377168516418,-54.1679505278134,12.));
#75628=CARTESIAN_POINT('',(-44.3377168516418,-54.1679505278134,0.));
#75629=CARTESIAN_POINT('Ctrl Pts',(-45.7706564944767,-58.4060826907378,
12.));
#75630=CARTESIAN_POINT('Ctrl Pts',(-45.7702793558063,-58.4045515723008,
12.));
#75631=CARTESIAN_POINT('Ctrl Pts',(-45.7685831165459,-58.397667048078,12.));
#75632=CARTESIAN_POINT('Ctrl Pts',(-45.7655655205267,-58.385434851721,12.));
#75633=CARTESIAN_POINT('Ctrl Pts',(-45.7612219538034,-58.3678667473265,
12.));
#75634=CARTESIAN_POINT('Ctrl Pts',(-45.7555454693956,-58.3449805573335,
12.));
#75635=CARTESIAN_POINT('Ctrl Pts',(-45.7489076429725,-58.3183218645265,
12.));
#75636=CARTESIAN_POINT('Ctrl Pts',(-45.7422542194625,-58.2917035135833,
12.));
#75637=CARTESIAN_POINT('Ctrl Pts',(-45.7355852575127,-58.2651255711481,
12.));
#75638=CARTESIAN_POINT('Ctrl Pts',(-45.7289008195612,-58.2385881070959,
12.));
#75639=CARTESIAN_POINT('Ctrl Pts',(-45.7222009715431,-58.2120911942819,
12.));
#75640=CARTESIAN_POINT('Ctrl Pts',(-45.7154857816507,-58.1856349074723,
12.));
#75641=CARTESIAN_POINT('Ctrl Pts',(-45.708755319378,-58.159219322515,12.));
#75642=CARTESIAN_POINT('Ctrl Pts',(-45.7020096545174,-58.1328445154667,
12.));
#75643=CARTESIAN_POINT('Ctrl Pts',(-45.6952488560133,-58.1065105615884,
12.));
#75644=CARTESIAN_POINT('Ctrl Pts',(-45.6884729914465,-58.0802175348939,
12.));
#75645=CARTESIAN_POINT('Ctrl Pts',(-45.6816821276662,-58.0539655087095,
12.));
#75646=CARTESIAN_POINT('Ctrl Pts',(-45.6748763311635,-58.0277545560001,
12.));
#75647=CARTESIAN_POINT('Ctrl Pts',(-45.6680556685494,-58.0015847497838,
12.));
#75648=CARTESIAN_POINT('Ctrl Pts',(-45.6612202069927,-57.975456163507,12.));
#75649=CARTESIAN_POINT('Ctrl Pts',(-45.6543700146689,-57.9493688714249,
12.));
#75650=CARTESIAN_POINT('Ctrl Pts',(-45.6475051605542,-57.923322948432,12.));
#75651=CARTESIAN_POINT('Ctrl Pts',(-45.6406257142385,-57.8973184699037,
12.));
#75652=CARTESIAN_POINT('Ctrl Pts',(-45.6337317457253,-57.8713555115232,
12.));
#75653=CARTESIAN_POINT('Ctrl Pts',(-45.6268233252543,-57.8454341491236,
12.));
#75654=CARTESIAN_POINT('Ctrl Pts',(-45.619900523078,-57.819554458484,12.));
#75655=CARTESIAN_POINT('Ctrl Pts',(-45.6129634094677,-57.7937165153379,
12.));
#75656=CARTESIAN_POINT('Ctrl Pts',(-45.6060120548199,-57.7679203954735,
12.));
#75657=CARTESIAN_POINT('Ctrl Pts',(-45.5990465297341,-57.7421661748022,
12.));
#75658=CARTESIAN_POINT('Ctrl Pts',(-45.5920669050988,-57.7164539294316,
12.));
#75659=CARTESIAN_POINT('Ctrl Pts',(-45.5850732521902,-57.6907837357425,
12.));
#75660=CARTESIAN_POINT('Ctrl Pts',(-45.5780656427172,-57.6651556704249,
12.));
#75661=CARTESIAN_POINT('Ctrl Pts',(-45.5710441487683,-57.6395698104416,
12.));
#75662=CARTESIAN_POINT('Ctrl Pts',(-45.5640088427819,-57.6140262330048,
12.));
#75663=CARTESIAN_POINT('Ctrl Pts',(-45.5569597975096,-57.5885250155432,
12.));
#75664=CARTESIAN_POINT('Ctrl Pts',(-45.5498970859829,-57.5630662356671,
12.));
#75665=CARTESIAN_POINT('Ctrl Pts',(-45.5428207814832,-57.5376499711338,
12.));
#75666=CARTESIAN_POINT('Ctrl Pts',(-45.5357309575603,-57.5122762998732,
12.));
#75667=CARTESIAN_POINT('Ctrl Pts',(-45.5286276880479,-57.4869453000055,
12.));
#75668=CARTESIAN_POINT('Ctrl Pts',(-45.5215110470825,-57.4616570498566,
12.));
#75669=CARTESIAN_POINT('Ctrl Pts',(-45.5143811091209,-57.4364116279708,
12.));
#75670=CARTESIAN_POINT('Ctrl Pts',(-45.5072379489637,-57.4112091131193,
12.));
#75671=CARTESIAN_POINT('Ctrl Pts',(-45.5000816417516,-57.3860495843043,
12.));
#75672=CARTESIAN_POINT('Ctrl Pts',(-45.4929122629576,-57.360933120758,12.));
#75673=CARTESIAN_POINT('Ctrl Pts',(-45.4857298883826,-57.3358598019391,
12.));
#75674=CARTESIAN_POINT('Ctrl Pts',(-45.4785345941505,-57.3108297075262,
12.));
#75675=CARTESIAN_POINT('Ctrl Pts',(-45.4713264567059,-57.2858429174056,
12.));
#75676=CARTESIAN_POINT('Ctrl Pts',(-45.4641055528138,-57.2608995116727,
12.));
#75677=CARTESIAN_POINT('Ctrl Pts',(-45.4568719595639,-57.2359995706441,
12.));
#75678=CARTESIAN_POINT('Ctrl Pts',(-45.4496257543759,-57.2111431748629,
12.));
#75679=CARTESIAN_POINT('Ctrl Pts',(-45.4423670150035,-57.1863304051011,
12.));
#75680=CARTESIAN_POINT('Ctrl Pts',(-45.4350958195434,-57.1615613423586,
12.));
#75681=CARTESIAN_POINT('Ctrl Pts',(-45.4278122464387,-57.1368360678629,
12.));
#75682=CARTESIAN_POINT('Ctrl Pts',(-45.4205163744778,-57.1121546630776,
12.));
#75683=CARTESIAN_POINT('Ctrl Pts',(-45.4132082827945,-57.0875172097048,
12.));
#75684=CARTESIAN_POINT('Ctrl Pts',(-45.4058880508693,-57.0629237896848,
12.));
#75685=CARTESIAN_POINT('Ctrl Pts',(-45.3985557585316,-57.0383744851917,
12.));
#75686=CARTESIAN_POINT('Ctrl Pts',(-45.3912114859625,-57.0138693786287,
12.));
#75687=CARTESIAN_POINT('Ctrl Pts',(-45.3838553136957,-56.9894085526383,
12.));
#75688=CARTESIAN_POINT('Ctrl Pts',(-45.3764873226202,-56.9649920901079,
12.));
#75689=CARTESIAN_POINT('Ctrl Pts',(-45.3691075939827,-56.9406200741714,
12.));
#75690=CARTESIAN_POINT('Ctrl Pts',(-45.3617162093918,-56.916292588208,12.));
#75691=CARTESIAN_POINT('Ctrl Pts',(-45.3543132508234,-56.8920097158371,
12.));
#75692=CARTESIAN_POINT('Ctrl Pts',(-45.3468988006202,-56.8677715409266,
12.));
#75693=CARTESIAN_POINT('Ctrl Pts',(-45.3394729414932,-56.8435781475982,
12.));
#75694=CARTESIAN_POINT('Ctrl Pts',(-45.3320357565241,-56.8194296202293,
12.));
#75695=CARTESIAN_POINT('Ctrl Pts',(-45.3245873291682,-56.7953260434521,
12.));
#75696=CARTESIAN_POINT('Ctrl Pts',(-45.3171277432592,-56.771267502148,12.));
#75697=CARTESIAN_POINT('Ctrl Pts',(-45.3096570830107,-56.747254081454,12.));
#75698=CARTESIAN_POINT('Ctrl Pts',(-45.3021754330169,-56.7232858667697,
12.));
#75699=CARTESIAN_POINT('Ctrl Pts',(-45.2946828782557,-56.6993629437596,
12.));
#75700=CARTESIAN_POINT('Ctrl Pts',(-45.2871795040912,-56.6754853983535,
12.));
#75701=CARTESIAN_POINT('Ctrl Pts',(-45.2796653962796,-56.6516533167398,
12.));
#75702=CARTESIAN_POINT('Ctrl Pts',(-45.2721406409706,-56.6278667853716,
12.));
#75703=CARTESIAN_POINT('Ctrl Pts',(-45.2646053247094,-56.604125890975,12.));
#75704=CARTESIAN_POINT('Ctrl Pts',(-45.2570595344382,-56.5804307205507,
12.));
#75705=CARTESIAN_POINT('Ctrl Pts',(-45.2495033574997,-56.5567813613752,
12.));
#75706=CARTESIAN_POINT('Ctrl Pts',(-45.2419368816423,-56.533177900995,12.));
#75707=CARTESIAN_POINT('Ctrl Pts',(-45.2343601950222,-56.5096204272299,
12.));
#75708=CARTESIAN_POINT('Ctrl Pts',(-45.2267733862046,-56.4861090281819,
12.));
#75709=CARTESIAN_POINT('Ctrl Pts',(-45.2191765441666,-56.4626437922385,
12.));
#75710=CARTESIAN_POINT('Ctrl Pts',(-45.2115697583002,-56.4392248080733,
12.));
#75711=CARTESIAN_POINT('Ctrl Pts',(-45.2039531184172,-56.4158521646412,
12.));
#75712=CARTESIAN_POINT('Ctrl Pts',(-45.1963267147527,-56.3925259511804,
12.));
#75713=CARTESIAN_POINT('Ctrl Pts',(-45.1886906379664,-56.3692462572228,
12.));
#75714=CARTESIAN_POINT('Ctrl Pts',(-45.1810449791451,-56.3460131725962,
12.));
#75715=CARTESIAN_POINT('Ctrl Pts',(-45.1733898298062,-56.3228267874265,
12.));
#75716=CARTESIAN_POINT('Ctrl Pts',(-45.1657252819018,-56.2996871921321,
12.));
#75717=CARTESIAN_POINT('Ctrl Pts',(-45.158051427823,-56.2765944774252,12.));
#75718=CARTESIAN_POINT('Ctrl Pts',(-45.150368360401,-56.2535487343227,12.));
#75719=CARTESIAN_POINT('Ctrl Pts',(-45.1426761729107,-56.2305500541491,
12.));
#75720=CARTESIAN_POINT('Ctrl Pts',(-45.1349749590736,-56.2075985285391,
12.));
#75721=CARTESIAN_POINT('Ctrl Pts',(-45.1272648130627,-56.1846942494321,
12.));
#75722=CARTESIAN_POINT('Ctrl Pts',(-45.119545829506,-56.1618373090729,12.));
#75723=CARTESIAN_POINT('Ctrl Pts',(-45.1118181034888,-56.1390278000226,
12.));
#75724=CARTESIAN_POINT('Ctrl Pts',(-45.1040817305563,-56.1162658151621,
12.));
#75725=CARTESIAN_POINT('Ctrl Pts',(-45.0963368067177,-56.0935514476945,
12.));
#75726=CARTESIAN_POINT('Ctrl Pts',(-45.0885834284513,-56.070884791141,12.));
#75727=CARTESIAN_POINT('Ctrl Pts',(-45.0808216927082,-56.0482659393412,
12.));
#75728=CARTESIAN_POINT('Ctrl Pts',(-45.0730516969142,-56.025694986463,12.));
#75729=CARTESIAN_POINT('Ctrl Pts',(-45.0652735389729,-56.0031720270074,
12.));
#75730=CARTESIAN_POINT('Ctrl Pts',(-45.0574873172696,-55.9806971558099,
12.));
#75731=CARTESIAN_POINT('Ctrl Pts',(-45.0496931306766,-55.958270468037,12.));
#75732=CARTESIAN_POINT('Ctrl Pts',(-45.041891078557,-55.9358920591861,12.));
#75733=CARTESIAN_POINT('Ctrl Pts',(-45.0340812607676,-55.9135620250977,
12.));
#75734=CARTESIAN_POINT('Ctrl Pts',(-45.0262637776623,-55.8912804619588,
12.));
#75735=CARTESIAN_POINT('Ctrl Pts',(-45.0184387300968,-55.8690474663058,
12.));
#75736=CARTESIAN_POINT('Ctrl Pts',(-45.0106062194325,-55.8468631350195,
12.));
#75737=CARTESIAN_POINT('Ctrl Pts',(-45.002766347541,-55.8247275653257,12.));
#75738=CARTESIAN_POINT('Ctrl Pts',(-44.9949192168073,-55.8026408548078,
12.));
#75739=CARTESIAN_POINT('Ctrl Pts',(-44.9870649301333,-55.7806031014093,
12.));
#75740=CARTESIAN_POINT('Ctrl Pts',(-44.979203590942,-55.7586144034376,12.));
#75741=CARTESIAN_POINT('Ctrl Pts',(-44.9713353031827,-55.7366748595582,
12.));
#75742=CARTESIAN_POINT('Ctrl Pts',(-44.9634601713352,-55.7147845687969,
12.));
#75743=CARTESIAN_POINT('Ctrl Pts',(-44.9555783004133,-55.6929436305522,
12.));
#75744=CARTESIAN_POINT('Ctrl Pts',(-44.9476897959694,-55.671152144599,12.));
#75745=CARTESIAN_POINT('Ctrl Pts',(-44.9397947640996,-55.6494102110922,
12.));
#75746=CARTESIAN_POINT('Ctrl Pts',(-44.9318933114483,-55.6277179305604,
12.));
#75747=CARTESIAN_POINT('Ctrl Pts',(-44.9239855452119,-55.6060754039089,
12.));
#75748=CARTESIAN_POINT('Ctrl Pts',(-44.9160715731425,-55.5844827324315,
12.));
#75749=CARTESIAN_POINT('Ctrl Pts',(-44.9081515035525,-55.5629400178136,
12.));
#75750=CARTESIAN_POINT('Ctrl Pts',(-44.9002254453192,-55.541447362135,12.));
#75751=CARTESIAN_POINT('Ctrl Pts',(-44.8922935078905,-55.5200048678648,
12.));
#75752=CARTESIAN_POINT('Ctrl Pts',(-44.8843558012903,-55.4986126378676,
12.));
#75753=CARTESIAN_POINT('Ctrl Pts',(-44.8764124361218,-55.4772707754139,
12.));
#75754=CARTESIAN_POINT('Ctrl Pts',(-44.8684635235727,-55.4559793841838,
12.));
#75755=CARTESIAN_POINT('Ctrl Pts',(-44.8605091754208,-55.4347385682697,
12.));
#75756=CARTESIAN_POINT('Ctrl Pts',(-44.8525495040397,-55.4135484321706,
12.));
#75757=CARTESIAN_POINT('Ctrl Pts',(-44.8445846224034,-55.3924090808002,
12.));
#75758=CARTESIAN_POINT('Ctrl Pts',(-44.8366146440896,-55.3713206194962,
12.));
#75759=CARTESIAN_POINT('Ctrl Pts',(-44.8286396832849,-55.350283154023,12.));
#75760=CARTESIAN_POINT('Ctrl Pts',(-44.8206598547889,-55.3292967905726,
12.));
#75761=CARTESIAN_POINT('Ctrl Pts',(-44.812675274021,-55.3083616357605,12.));
#75762=CARTESIAN_POINT('Ctrl Pts',(-44.8046860570245,-55.287477796635,12.));
#75763=CARTESIAN_POINT('Ctrl Pts',(-44.7966923204741,-55.2666453806883,
12.));
#75764=CARTESIAN_POINT('Ctrl Pts',(-44.7886941816823,-55.2458644958617,
12.));
#75765=CARTESIAN_POINT('Ctrl Pts',(-44.7806917586077,-55.2251352505475,
12.));
#75766=CARTESIAN_POINT('Ctrl Pts',(-44.7726851698619,-55.2044577535866,
12.));
#75767=CARTESIAN_POINT('Ctrl Pts',(-44.7646745347109,-55.1838321142779,
12.));
#75768=CARTESIAN_POINT('Ctrl Pts',(-44.7566599730773,-55.1632584423815,
12.));
#75769=CARTESIAN_POINT('Ctrl Pts',(-44.748641605542,-55.14273684812,12.));
#75770=CARTESIAN_POINT('Ctrl Pts',(-44.740619553348,-55.1222674421743,12.));
#75771=CARTESIAN_POINT('Ctrl Pts',(-44.7325939384035,-55.1018503356796,
12.));
#75772=CARTESIAN_POINT('Ctrl Pts',(-44.7245648832979,-55.0814856402496,
12.));
#75773=CARTESIAN_POINT('Ctrl Pts',(-44.7165325113159,-55.0611734679894,
12.));
#75774=CARTESIAN_POINT('Ctrl Pts',(-44.7084969464513,-55.0409139315078,
12.));
#75775=CARTESIAN_POINT('Ctrl Pts',(-44.7004583134249,-55.0207071439237,
12.));
#75776=CARTESIAN_POINT('Ctrl Pts',(-44.6924167376869,-55.0005532188667,
12.));
#75777=CARTESIAN_POINT('Ctrl Pts',(-44.6843723454,-54.9804522704686,12.));
#75778=CARTESIAN_POINT('Ctrl Pts',(-44.6763252634258,-54.9604044133501,
12.));
#75779=CARTESIAN_POINT('Ctrl Pts',(-44.6682756193147,-54.9404097626077,
12.));
#75780=CARTESIAN_POINT('Ctrl Pts',(-44.6602235412836,-54.9204684337822,
12.));
#75781=CARTESIAN_POINT('Ctrl Pts',(-44.6521691582533,-54.9005805428969,
12.));
#75782=CARTESIAN_POINT('Ctrl Pts',(-44.6441125999063,-54.8807462065164,
12.));
#75783=CARTESIAN_POINT('Ctrl Pts',(-44.6360539967392,-54.860965541796,12.));
#75784=CARTESIAN_POINT('Ctrl Pts',(-44.6279934801169,-54.8412386665276,
12.));
#75785=CARTESIAN_POINT('Ctrl Pts',(-44.6199311823293,-54.8215656991837,
12.));
#75786=CARTESIAN_POINT('Ctrl Pts',(-44.6118672364906,-54.8019467588278,
12.));
#75787=CARTESIAN_POINT('Ctrl Pts',(-44.6038017764309,-54.7823819650149,
12.));
#75788=CARTESIAN_POINT('Ctrl Pts',(-44.5957349366059,-54.7628714377037,
12.));
#75789=CARTESIAN_POINT('Ctrl Pts',(-44.5876668519661,-54.7434152971267,
12.));
#75790=CARTESIAN_POINT('Ctrl Pts',(-44.5795976579454,-54.7240136637717,
12.));
#75791=CARTESIAN_POINT('Ctrl Pts',(-44.5715274907619,-54.7046666586754,
12.));
#75792=CARTESIAN_POINT('Ctrl Pts',(-44.5634564876863,-54.6853744036751,
12.));
#75793=CARTESIAN_POINT('Ctrl Pts',(-44.5553847872721,-54.6661370216252,
12.));
#75794=CARTESIAN_POINT('Ctrl Pts',(-44.5473125297311,-54.6469546367408,
12.));
#75795=CARTESIAN_POINT('Ctrl Pts',(-44.5392398566802,-54.6278273743587,
12.));
#75796=CARTESIAN_POINT('Ctrl Pts',(-44.5311669104515,-54.6087553602914,
12.));
#75797=CARTESIAN_POINT('Ctrl Pts',(-44.5230938335167,-54.5897387202815,
12.));
#75798=CARTESIAN_POINT('Ctrl Pts',(-44.5150207678988,-54.5707775794412,
12.));
#75799=CARTESIAN_POINT('Ctrl Pts',(-44.5069478544945,-54.5518720616016,
12.));
#75800=CARTESIAN_POINT('Ctrl Pts',(-44.4988752343715,-54.5330222905438,
12.));
#75801=CARTESIAN_POINT('Ctrl Pts',(-44.4908030503209,-54.5142283914684,
12.));
#75802=CARTESIAN_POINT('Ctrl Pts',(-44.482731448127,-54.4954904921938,12.));
#75803=CARTESIAN_POINT('Ctrl Pts',(-44.4746605784056,-54.4768087248854,
12.));
#75804=CARTESIAN_POINT('Ctrl Pts',(-44.4665905967701,-54.4581832262072,
12.));
#75805=CARTESIAN_POINT('Ctrl Pts',(-44.4585216599933,-54.4396141337008,
12.));
#75806=CARTESIAN_POINT('Ctrl Pts',(-44.4504539226336,-54.4211015825959,
12.));
#75807=CARTESIAN_POINT('Ctrl Pts',(-44.442387534098,-54.4026457030316,12.));
#75808=CARTESIAN_POINT('Ctrl Pts',(-44.4343226339555,-54.3842466156151,
12.));
#75809=CARTESIAN_POINT('Ctrl Pts',(-44.4262593564664,-54.3659044357064,
12.));
#75810=CARTESIAN_POINT('Ctrl Pts',(-44.4181978395814,-54.347619281931,12.));
#75811=CARTESIAN_POINT('Ctrl Pts',(-44.4101382321834,-54.3293912830237,
12.));
#75812=CARTESIAN_POINT('Ctrl Pts',(-44.4020807028144,-54.3112205860776,
12.));
#75813=CARTESIAN_POINT('Ctrl Pts',(-44.3940254456427,-54.2931073621661,
12.));
#75814=CARTESIAN_POINT('Ctrl Pts',(-44.3859726620288,-54.2750517888695,
12.));
#75815=CARTESIAN_POINT('Ctrl Pts',(-44.3779225430461,-54.2570540336536,
12.));
#75816=CARTESIAN_POINT('Ctrl Pts',(-44.369875253351,-54.2391142386354,12.));
#75817=CARTESIAN_POINT('Ctrl Pts',(-44.3618309103245,-54.2212325005847,
12.));
#75818=CARTESIAN_POINT('Ctrl Pts',(-44.3537895823819,-54.203408870162,12.));
#75819=CARTESIAN_POINT('Ctrl Pts',(-44.3473589597468,-54.1891964684439,
12.));
#75820=CARTESIAN_POINT('Ctrl Pts',(-44.3425373700829,-54.1785633257456,
12.));
#75821=CARTESIAN_POINT('Ctrl Pts',(-44.3393235891014,-54.1714861895278,
12.));
#75822=CARTESIAN_POINT('Ctrl Pts',(-44.3377168516418,-54.1679505278134,
12.));
#75823=CARTESIAN_POINT('Ctrl Pts',(-44.5696260757792,-59.3276657444392,
-1.11022302462516E-15));
#75824=CARTESIAN_POINT('Ctrl Pts',(-44.5696260757792,-59.3276657444392,
4.));
#75825=CARTESIAN_POINT('Ctrl Pts',(-44.5696260757792,-59.3276657444392,
8.));
#75826=CARTESIAN_POINT('Ctrl Pts',(-44.5696260757792,-59.3276657444392,
12.));
#75827=CARTESIAN_POINT('Ctrl Pts',(-44.6658822400933,-59.3806648691719,
-1.11022302462516E-15));
#75828=CARTESIAN_POINT('Ctrl Pts',(-44.6658822400933,-59.3806648691719,
4.));
#75829=CARTESIAN_POINT('Ctrl Pts',(-44.6658822400933,-59.3806648691719,
8.));
#75830=CARTESIAN_POINT('Ctrl Pts',(-44.6658822400933,-59.3806648691719,
12.));
#75831=CARTESIAN_POINT('Ctrl Pts',(-44.8655383388341,-59.4154499491518,
-1.03713949455603E-15));
#75832=CARTESIAN_POINT('Ctrl Pts',(-44.8655383388341,-59.4154499491518,
4.));
#75833=CARTESIAN_POINT('Ctrl Pts',(-44.8655383388341,-59.4154499491518,
7.99999999999999));
#75834=CARTESIAN_POINT('Ctrl Pts',(-44.8655383388341,-59.4154499491518,
12.));
#75835=CARTESIAN_POINT('Ctrl Pts',(-45.047980595232,-59.3374774995081,-8.63611844427577E-16));
#75836=CARTESIAN_POINT('Ctrl Pts',(-45.047980595232,-59.3374774995081,4.));
#75837=CARTESIAN_POINT('Ctrl Pts',(-45.0479805952321,-59.3374774995081,
8.00000000000001));
#75838=CARTESIAN_POINT('Ctrl Pts',(-45.0479805952321,-59.3374774995081,
12.));
#75839=CARTESIAN_POINT('Ctrl Pts',(-45.1135644683452,-59.2875729049565,
-7.79957864199761E-16));
#75840=CARTESIAN_POINT('Ctrl Pts',(-45.1135644683452,-59.2875729049565,
4.));
#75841=CARTESIAN_POINT('Ctrl Pts',(-45.1135644683452,-59.2875729049565,
8.));
#75842=CARTESIAN_POINT('Ctrl Pts',(-45.1135644683452,-59.2875729049565,
12.));
#75843=CARTESIAN_POINT('',(-44.5696260757792,-59.3276657444392,2.77555756156289E-16));
#75844=CARTESIAN_POINT('',(-45.1135644683449,-59.2875729049561,2.77555756156289E-16));
#75845=CARTESIAN_POINT('Ctrl Pts',(-44.5696260757792,-59.3276657444392,
-3.21795698712167E-17));
#75846=CARTESIAN_POINT('Ctrl Pts',(-44.6658822400933,-59.3806648691719,
-3.2179569871217E-17));
#75847=CARTESIAN_POINT('Ctrl Pts',(-44.7799714393737,-59.4005420577319,
9.58244731114085E-18));
#75848=CARTESIAN_POINT('Ctrl Pts',(-44.8884397921749,-59.3836004611086,
8.41425445128705E-17));
#75849=CARTESIAN_POINT('Ctrl Pts',(-44.9697910567758,-59.3708942636411,
1.40062617414167E-16));
#75850=CARTESIAN_POINT('Ctrl Pts',(-45.047980595232,-59.3374774995081,2.14431610326361E-16));
#75851=CARTESIAN_POINT('Ctrl Pts',(-45.1135644683452,-59.2875729049565,
2.98085590554179E-16));
#75852=CARTESIAN_POINT('',(-45.1135644683449,-59.2875729049561,12.));
#75853=CARTESIAN_POINT('Ctrl Pts',(-45.1135644683452,-59.2875729049565,
-7.79957864199761E-16));
#75854=CARTESIAN_POINT('Ctrl Pts',(-45.1135644683452,-59.2875729049565,
4.));
#75855=CARTESIAN_POINT('Ctrl Pts',(-45.1135644683452,-59.2875729049565,
8.));
#75856=CARTESIAN_POINT('Ctrl Pts',(-45.1135644683452,-59.2875729049565,
12.));
#75857=CARTESIAN_POINT('',(-44.5696260757792,-59.3276657444392,12.));
#75858=CARTESIAN_POINT('Ctrl Pts',(-45.1135644683452,-59.2875729049565,
12.));
#75859=CARTESIAN_POINT('Ctrl Pts',(-45.0479805952321,-59.3374774995081,
12.));
#75860=CARTESIAN_POINT('Ctrl Pts',(-44.9697910567758,-59.3708942636412,
12.));
#75861=CARTESIAN_POINT('Ctrl Pts',(-44.8884397921749,-59.3836004611086,
12.));
#75862=CARTESIAN_POINT('Ctrl Pts',(-44.7799714393738,-59.4005420577319,
12.));
#75863=CARTESIAN_POINT('Ctrl Pts',(-44.6658822400933,-59.3806648691719,
12.));
#75864=CARTESIAN_POINT('Ctrl Pts',(-44.5696260757792,-59.3276657444392,
12.));
#75865=CARTESIAN_POINT('Ctrl Pts',(-44.5696260757792,-59.3276657444392,
12.));
#75866=CARTESIAN_POINT('Ctrl Pts',(-44.5696260757792,-59.3276657444392,
8.));
#75867=CARTESIAN_POINT('Ctrl Pts',(-44.5696260757792,-59.3276657444392,
4.));
#75868=CARTESIAN_POINT('Ctrl Pts',(-44.5696260757792,-59.3276657444392,
-1.11022302462516E-15));
#75869=CARTESIAN_POINT('Origin',(-2.28111678886296E-10,-2.97443977737815E-10,
0.));
#75870=CARTESIAN_POINT('Origin',(-2.28111678886296E-10,-2.97443977737815E-10,
12.));
#75871=CARTESIAN_POINT('Origin',(-2.28111678886296E-10,-2.97443977737815E-10,
0.));
#75872=CARTESIAN_POINT('Ctrl Pts',(-50.5529731960877,-54.7233670476848,
0.));
#75873=CARTESIAN_POINT('Ctrl Pts',(-50.5529731960877,-54.7233670476848,
4.));
#75874=CARTESIAN_POINT('Ctrl Pts',(-50.5529731960877,-54.7233670476848,
8.));
#75875=CARTESIAN_POINT('Ctrl Pts',(-50.5529731960877,-54.7233670476848,
12.));
#75876=CARTESIAN_POINT('Ctrl Pts',(-50.6336864649948,-54.6488048279282,
0.));
#75877=CARTESIAN_POINT('Ctrl Pts',(-50.6336864649948,-54.6488048279282,
4.));
#75878=CARTESIAN_POINT('Ctrl Pts',(-50.6336864649948,-54.6488048279283,
8.));
#75879=CARTESIAN_POINT('Ctrl Pts',(-50.6336864649948,-54.6488048279283,
12.));
#75880=CARTESIAN_POINT('Ctrl Pts',(-50.7298112257546,-54.4703879751554,
0.));
#75881=CARTESIAN_POINT('Ctrl Pts',(-50.7298112257546,-54.4703879751554,
4.00000000000001));
#75882=CARTESIAN_POINT('Ctrl Pts',(-50.7298112257546,-54.4703879751553,
8.));
#75883=CARTESIAN_POINT('Ctrl Pts',(-50.7298112257546,-54.4703879751553,
12.));
#75884=CARTESIAN_POINT('Ctrl Pts',(-50.7135202769404,-54.2726521137409,
0.));
#75885=CARTESIAN_POINT('Ctrl Pts',(-50.7135202769404,-54.2726521137409,
4.));
#75886=CARTESIAN_POINT('Ctrl Pts',(-50.7135202769404,-54.2726521137408,
8.00000000000001));
#75887=CARTESIAN_POINT('Ctrl Pts',(-50.7135202769404,-54.2726521137408,
12.));
#75888=CARTESIAN_POINT('Ctrl Pts',(-50.6869108458687,-54.1946543499977,
0.));
#75889=CARTESIAN_POINT('Ctrl Pts',(-50.6869108458687,-54.1946543499977,
4.));
#75890=CARTESIAN_POINT('Ctrl Pts',(-50.6869108458687,-54.1946543499977,
8.));
#75891=CARTESIAN_POINT('Ctrl Pts',(-50.6869108458687,-54.1946543499977,
12.));
#75892=CARTESIAN_POINT('',(-50.5529731960877,-54.7233670476848,0.));
#75893=CARTESIAN_POINT('',(-50.6869108458688,-54.1946543499977,0.));
#75894=CARTESIAN_POINT('Ctrl Pts',(-50.5529731960877,-54.7233670476848,
0.));
#75895=CARTESIAN_POINT('Ctrl Pts',(-50.6336864649948,-54.6488048279282,
0.));
#75896=CARTESIAN_POINT('Ctrl Pts',(-50.6886148997147,-54.5468523406295,
0.));
#75897=CARTESIAN_POINT('Ctrl Pts',(-50.7068361639614,-54.438591605611,0.));
#75898=CARTESIAN_POINT('Ctrl Pts',(-50.7205021121465,-54.3573960543471,
0.));
#75899=CARTESIAN_POINT('Ctrl Pts',(-50.7135202769404,-54.2726521137409,
0.));
#75900=CARTESIAN_POINT('Ctrl Pts',(-50.6869108458687,-54.1946543499977,
0.));
#75901=CARTESIAN_POINT('',(-50.6869108458688,-54.1946543499976,12.));
#75902=CARTESIAN_POINT('Ctrl Pts',(-50.6869108458687,-54.1946543499977,
0.));
#75903=CARTESIAN_POINT('Ctrl Pts',(-50.6869108458687,-54.1946543499977,
4.));
#75904=CARTESIAN_POINT('Ctrl Pts',(-50.6869108458687,-54.1946543499977,
8.));
#75905=CARTESIAN_POINT('Ctrl Pts',(-50.6869108458687,-54.1946543499977,
12.));
#75906=CARTESIAN_POINT('',(-50.5529731960877,-54.7233670476848,12.));
#75907=CARTESIAN_POINT('Ctrl Pts',(-50.6869108458687,-54.1946543499977,
12.));
#75908=CARTESIAN_POINT('Ctrl Pts',(-50.7135202769404,-54.2726521137408,
12.));
#75909=CARTESIAN_POINT('Ctrl Pts',(-50.7205021121465,-54.357396054347,12.));
#75910=CARTESIAN_POINT('Ctrl Pts',(-50.7068361639614,-54.4385916056109,
12.));
#75911=CARTESIAN_POINT('Ctrl Pts',(-50.6886148997147,-54.5468523406294,
12.));
#75912=CARTESIAN_POINT('Ctrl Pts',(-50.6336864649948,-54.6488048279283,
12.));
#75913=CARTESIAN_POINT('Ctrl Pts',(-50.5529731960877,-54.7233670476848,
12.));
#75914=CARTESIAN_POINT('Ctrl Pts',(-50.5529731960877,-54.7233670476848,
12.));
#75915=CARTESIAN_POINT('Ctrl Pts',(-50.5529731960877,-54.7233670476848,
8.));
#75916=CARTESIAN_POINT('Ctrl Pts',(-50.5529731960877,-54.7233670476848,
4.));
#75917=CARTESIAN_POINT('Ctrl Pts',(-50.5529731960877,-54.7233670476848,
0.));
#75918=CARTESIAN_POINT('Ctrl Pts',(-48.8900464144686,-50.0975384783634,
0.));
#75919=CARTESIAN_POINT('Ctrl Pts',(-48.8900464144686,-50.0975384783634,
12.));
#75920=CARTESIAN_POINT('Ctrl Pts',(-48.8919551910299,-50.1009206494209,
0.));
#75921=CARTESIAN_POINT('Ctrl Pts',(-48.8919551910299,-50.1009206494209,
12.));
#75922=CARTESIAN_POINT('Ctrl Pts',(-48.8957735556681,-50.1076907555303,
0.));
#75923=CARTESIAN_POINT('Ctrl Pts',(-48.8957735556681,-50.1076907555303,
12.));
#75924=CARTESIAN_POINT('Ctrl Pts',(-48.9015035371772,-50.1178632066821,
0.));
#75925=CARTESIAN_POINT('Ctrl Pts',(-48.9015035371772,-50.1178632066821,
12.));
#75926=CARTESIAN_POINT('Ctrl Pts',(-48.9091483817797,-50.1314610602286,
0.));
#75927=CARTESIAN_POINT('Ctrl Pts',(-48.9091483817797,-50.1314610602286,
12.));
#75928=CARTESIAN_POINT('Ctrl Pts',(-48.9187125417897,-50.148516018447,0.));
#75929=CARTESIAN_POINT('Ctrl Pts',(-48.9187125417897,-50.148516018447,12.));
#75930=CARTESIAN_POINT('Ctrl Pts',(-48.9282847698237,-50.1656286003943,
0.));
#75931=CARTESIAN_POINT('Ctrl Pts',(-48.9282847698237,-50.1656286003943,
12.));
#75932=CARTESIAN_POINT('Ctrl Pts',(-48.9378649933116,-50.1827987615659,
0.));
#75933=CARTESIAN_POINT('Ctrl Pts',(-48.9378649933116,-50.1827987615659,
12.));
#75934=CARTESIAN_POINT('Ctrl Pts',(-48.9474530868847,-50.2000264157903,
0.));
#75935=CARTESIAN_POINT('Ctrl Pts',(-48.9474530868847,-50.2000264157903,
12.));
#75936=CARTESIAN_POINT('Ctrl Pts',(-48.9570488741273,-50.2173114358423,
0.));
#75937=CARTESIAN_POINT('Ctrl Pts',(-48.9570488741273,-50.2173114358423,
12.));
#75938=CARTESIAN_POINT('Ctrl Pts',(-48.9666521500969,-50.2346536715465,
0.));
#75939=CARTESIAN_POINT('Ctrl Pts',(-48.9666521500969,-50.2346536715465,
12.));
#75940=CARTESIAN_POINT('Ctrl Pts',(-48.9762626987227,-50.252052963548,0.));
#75941=CARTESIAN_POINT('Ctrl Pts',(-48.9762626987227,-50.252052963548,12.));
#75942=CARTESIAN_POINT('Ctrl Pts',(-48.9858803116649,-50.2695091583473,
0.));
#75943=CARTESIAN_POINT('Ctrl Pts',(-48.9858803116649,-50.2695091583473,
12.));
#75944=CARTESIAN_POINT('Ctrl Pts',(-48.9955048082028,-50.2870221241003,
0.));
#75945=CARTESIAN_POINT('Ctrl Pts',(-48.9955048082028,-50.2870221241003,
12.));
#75946=CARTESIAN_POINT('Ctrl Pts',(-49.0051360288002,-50.3045917455383,
0.));
#75947=CARTESIAN_POINT('Ctrl Pts',(-49.0051360288002,-50.3045917455383,
12.));
#75948=CARTESIAN_POINT('Ctrl Pts',(-49.0147738256925,-50.3222179165102,
0.));
#75949=CARTESIAN_POINT('Ctrl Pts',(-49.0147738256925,-50.3222179165102,
12.));
#75950=CARTESIAN_POINT('Ctrl Pts',(-49.0244180550759,-50.3399005337967,
0.));
#75951=CARTESIAN_POINT('Ctrl Pts',(-49.0244180550759,-50.3399005337967,
12.));
#75952=CARTESIAN_POINT('Ctrl Pts',(-49.034068567401,-50.3576394894136,0.));
#75953=CARTESIAN_POINT('Ctrl Pts',(-49.034068567401,-50.3576394894136,12.));
#75954=CARTESIAN_POINT('Ctrl Pts',(-49.0437252024868,-50.3754346667389,
0.));
#75955=CARTESIAN_POINT('Ctrl Pts',(-49.0437252024868,-50.3754346667389,
12.));
#75956=CARTESIAN_POINT('Ctrl Pts',(-49.0533877945771,-50.393285944528,0.));
#75957=CARTESIAN_POINT('Ctrl Pts',(-49.0533877945771,-50.393285944528,12.));
#75958=CARTESIAN_POINT('Ctrl Pts',(-49.0630561755082,-50.4111931994264,
0.));
#75959=CARTESIAN_POINT('Ctrl Pts',(-49.0630561755082,-50.4111931994264,
12.));
#75960=CARTESIAN_POINT('Ctrl Pts',(-49.0727301783477,-50.4291563088528,
0.));
#75961=CARTESIAN_POINT('Ctrl Pts',(-49.0727301783477,-50.4291563088528,
12.));
#75962=CARTESIAN_POINT('Ctrl Pts',(-49.0824096415339,-50.4471751542717,
0.));
#75963=CARTESIAN_POINT('Ctrl Pts',(-49.0824096415339,-50.4471751542717,
12.));
#75964=CARTESIAN_POINT('Ctrl Pts',(-49.0920944086973,-50.465249621057,0.));
#75965=CARTESIAN_POINT('Ctrl Pts',(-49.0920944086973,-50.465249621057,12.));
#75966=CARTESIAN_POINT('Ctrl Pts',(-49.1017843266782,-50.4833795969296,
0.));
#75967=CARTESIAN_POINT('Ctrl Pts',(-49.1017843266782,-50.4833795969296,
12.));
#75968=CARTESIAN_POINT('Ctrl Pts',(-49.1114792441573,-50.5015649708742,
0.));
#75969=CARTESIAN_POINT('Ctrl Pts',(-49.1114792441573,-50.5015649708742,
12.));
#75970=CARTESIAN_POINT('Ctrl Pts',(-49.1211790099817,-50.5198056318111,
0.));
#75971=CARTESIAN_POINT('Ctrl Pts',(-49.1211790099817,-50.5198056318111,
12.));
#75972=CARTESIAN_POINT('Ctrl Pts',(-49.1308834717645,-50.5381014674822,
0.));
#75973=CARTESIAN_POINT('Ctrl Pts',(-49.1308834717645,-50.5381014674822,
12.));
#75974=CARTESIAN_POINT('Ctrl Pts',(-49.1405924766169,-50.5564523650406,
0.));
#75975=CARTESIAN_POINT('Ctrl Pts',(-49.1405924766169,-50.5564523650406,
12.));
#75976=CARTESIAN_POINT('Ctrl Pts',(-49.1503058717831,-50.5748582115575,
0.));
#75977=CARTESIAN_POINT('Ctrl Pts',(-49.1503058717831,-50.5748582115575,
12.));
#75978=CARTESIAN_POINT('Ctrl Pts',(-49.1600235052613,-50.593318894516,0.));
#75979=CARTESIAN_POINT('Ctrl Pts',(-49.1600235052613,-50.593318894516,12.));
#75980=CARTESIAN_POINT('Ctrl Pts',(-49.1697452265473,-50.6118343023937,
0.));
#75981=CARTESIAN_POINT('Ctrl Pts',(-49.1697452265473,-50.6118343023937,
12.));
#75982=CARTESIAN_POINT('Ctrl Pts',(-49.1794708869074,-50.6304043248796,
0.));
#75983=CARTESIAN_POINT('Ctrl Pts',(-49.1794708869074,-50.6304043248796,
12.));
#75984=CARTESIAN_POINT('Ctrl Pts',(-49.1892003389743,-50.6490288525639,
0.));
#75985=CARTESIAN_POINT('Ctrl Pts',(-49.1892003389743,-50.6490288525639,
12.));
#75986=CARTESIAN_POINT('Ctrl Pts',(-49.1989334364992,-50.6677077767427,
0.));
#75987=CARTESIAN_POINT('Ctrl Pts',(-49.1989334364992,-50.6677077767427,
12.));
#75988=CARTESIAN_POINT('Ctrl Pts',(-49.2086700340625,-50.6864409891905,
0.));
#75989=CARTESIAN_POINT('Ctrl Pts',(-49.2086700340625,-50.6864409891905,
12.));
#75990=CARTESIAN_POINT('Ctrl Pts',(-49.218409986748,-50.7052283818941,0.));
#75991=CARTESIAN_POINT('Ctrl Pts',(-49.218409986748,-50.7052283818941,12.));
#75992=CARTESIAN_POINT('Ctrl Pts',(-49.2281531501569,-50.7240698470698,
0.));
#75993=CARTESIAN_POINT('Ctrl Pts',(-49.2281531501569,-50.7240698470698,
12.));
#75994=CARTESIAN_POINT('Ctrl Pts',(-49.2378993805482,-50.7429652772816,
0.));
#75995=CARTESIAN_POINT('Ctrl Pts',(-49.2378993805482,-50.7429652772816,
12.));
#75996=CARTESIAN_POINT('Ctrl Pts',(-49.2476485349373,-50.7619145655207,
0.));
#75997=CARTESIAN_POINT('Ctrl Pts',(-49.2476485349373,-50.7619145655207,
12.));
#75998=CARTESIAN_POINT('Ctrl Pts',(-49.2574004712122,-50.7809176052954,
0.));
#75999=CARTESIAN_POINT('Ctrl Pts',(-49.2574004712122,-50.7809176052954,
12.));
#76000=CARTESIAN_POINT('Ctrl Pts',(-49.2671550482415,-50.7999742907111,
0.));
#76001=CARTESIAN_POINT('Ctrl Pts',(-49.2671550482415,-50.7999742907111,
12.));
#76002=CARTESIAN_POINT('Ctrl Pts',(-49.2769121258144,-50.8190845164319,
0.));
#76003=CARTESIAN_POINT('Ctrl Pts',(-49.2769121258144,-50.8190845164319,
12.));
#76004=CARTESIAN_POINT('Ctrl Pts',(-49.2866715645828,-50.8382481776392,
0.));
#76005=CARTESIAN_POINT('Ctrl Pts',(-49.2866715645828,-50.8382481776392,
12.));
#76006=CARTESIAN_POINT('Ctrl Pts',(-49.2964332260043,-50.8574651699877,
0.));
#76007=CARTESIAN_POINT('Ctrl Pts',(-49.2964332260043,-50.8574651699877,
12.));
#76008=CARTESIAN_POINT('Ctrl Pts',(-49.3061969722798,-50.8767353895509,
0.));
#76009=CARTESIAN_POINT('Ctrl Pts',(-49.3061969722798,-50.8767353895509,
12.));
#76010=CARTESIAN_POINT('Ctrl Pts',(-49.3159626663129,-50.8960587327869,
0.));
#76011=CARTESIAN_POINT('Ctrl Pts',(-49.3159626663129,-50.8960587327869,
12.));
#76012=CARTESIAN_POINT('Ctrl Pts',(-49.325730171735,-50.9154350965681,0.));
#76013=CARTESIAN_POINT('Ctrl Pts',(-49.325730171735,-50.9154350965681,12.));
#76014=CARTESIAN_POINT('Ctrl Pts',(-49.3354993529163,-50.9348643781928,
0.));
#76015=CARTESIAN_POINT('Ctrl Pts',(-49.3354993529163,-50.9348643781928,
12.));
#76016=CARTESIAN_POINT('Ctrl Pts',(-49.3452700749804,-50.9543464753974,
0.));
#76017=CARTESIAN_POINT('Ctrl Pts',(-49.3452700749804,-50.9543464753974,
12.));
#76018=CARTESIAN_POINT('Ctrl Pts',(-49.3550422038221,-50.9738812863636,
0.));
#76019=CARTESIAN_POINT('Ctrl Pts',(-49.3550422038221,-50.9738812863636,
12.));
#76020=CARTESIAN_POINT('Ctrl Pts',(-49.3648156061049,-50.9934687097179,
0.));
#76021=CARTESIAN_POINT('Ctrl Pts',(-49.3648156061049,-50.9934687097179,
12.));
#76022=CARTESIAN_POINT('Ctrl Pts',(-49.3745901492429,-51.0131086445268,
0.));
#76023=CARTESIAN_POINT('Ctrl Pts',(-49.3745901492429,-51.0131086445268,
12.));
#76024=CARTESIAN_POINT('Ctrl Pts',(-49.3843657013851,-51.0328009902857,
0.));
#76025=CARTESIAN_POINT('Ctrl Pts',(-49.3843657013851,-51.0328009902857,
12.));
#76026=CARTESIAN_POINT('Ctrl Pts',(-49.3941421314014,-51.0525456469072,
0.));
#76027=CARTESIAN_POINT('Ctrl Pts',(-49.3941421314014,-51.0525456469072,
12.));
#76028=CARTESIAN_POINT('Ctrl Pts',(-49.4039193088636,-51.0723425146987,
0.));
#76029=CARTESIAN_POINT('Ctrl Pts',(-49.4039193088636,-51.0723425146987,
12.));
#76030=CARTESIAN_POINT('Ctrl Pts',(-49.4136971040428,-51.0921914943663,
0.));
#76031=CARTESIAN_POINT('Ctrl Pts',(-49.4136971040428,-51.0921914943663,
12.));
#76032=CARTESIAN_POINT('Ctrl Pts',(-49.4234753879071,-51.1120924870196,
0.));
#76033=CARTESIAN_POINT('Ctrl Pts',(-49.4234753879071,-51.1120924870196,
12.));
#76034=CARTESIAN_POINT('Ctrl Pts',(-49.4332540321178,-51.1320453941702,
0.));
#76035=CARTESIAN_POINT('Ctrl Pts',(-49.4332540321178,-51.1320453941702,
12.));
#76036=CARTESIAN_POINT('Ctrl Pts',(-49.4430329090288,-51.1520501177291,
0.));
#76037=CARTESIAN_POINT('Ctrl Pts',(-49.4430329090288,-51.1520501177291,
12.));
#76038=CARTESIAN_POINT('Ctrl Pts',(-49.4528118916833,-51.1721065599972,
0.));
#76039=CARTESIAN_POINT('Ctrl Pts',(-49.4528118916833,-51.1721065599972,
12.));
#76040=CARTESIAN_POINT('Ctrl Pts',(-49.4625908538076,-51.1922146236686,
0.));
#76041=CARTESIAN_POINT('Ctrl Pts',(-49.4625908538076,-51.1922146236686,
12.));
#76042=CARTESIAN_POINT('Ctrl Pts',(-49.4723696698022,-51.2123742118288,
0.));
#76043=CARTESIAN_POINT('Ctrl Pts',(-49.4723696698022,-51.2123742118288,
12.));
#76044=CARTESIAN_POINT('Ctrl Pts',(-49.4821482147357,-51.2325852279507,
0.));
#76045=CARTESIAN_POINT('Ctrl Pts',(-49.4821482147357,-51.2325852279507,
12.));
#76046=CARTESIAN_POINT('Ctrl Pts',(-49.4919263643357,-51.2528475758841,
0.));
#76047=CARTESIAN_POINT('Ctrl Pts',(-49.4919263643357,-51.2528475758841,
12.));
#76048=CARTESIAN_POINT('Ctrl Pts',(-49.5017039949841,-51.2731611598465,
0.));
#76049=CARTESIAN_POINT('Ctrl Pts',(-49.5017039949841,-51.2731611598465,
12.));
#76050=CARTESIAN_POINT('Ctrl Pts',(-49.5114809837111,-51.2935258844278,
0.));
#76051=CARTESIAN_POINT('Ctrl Pts',(-49.5114809837111,-51.2935258844278,
12.));
#76052=CARTESIAN_POINT('Ctrl Pts',(-49.5212572081901,-51.3139416545903,
0.));
#76053=CARTESIAN_POINT('Ctrl Pts',(-49.5212572081901,-51.3139416545903,
12.));
#76054=CARTESIAN_POINT('Ctrl Pts',(-49.5310325467334,-51.3344083756659,
0.));
#76055=CARTESIAN_POINT('Ctrl Pts',(-49.5310325467334,-51.3344083756659,
12.));
#76056=CARTESIAN_POINT('Ctrl Pts',(-49.5408068782871,-51.354925953347,0.));
#76057=CARTESIAN_POINT('Ctrl Pts',(-49.5408068782871,-51.354925953347,12.));
#76058=CARTESIAN_POINT('Ctrl Pts',(-49.5505800824268,-51.3754942936796,
0.));
#76059=CARTESIAN_POINT('Ctrl Pts',(-49.5505800824268,-51.3754942936796,
12.));
#76060=CARTESIAN_POINT('Ctrl Pts',(-49.5603520393514,-51.3961133030688,
0.));
#76061=CARTESIAN_POINT('Ctrl Pts',(-49.5603520393514,-51.3961133030688,
12.));
#76062=CARTESIAN_POINT('Ctrl Pts',(-49.5701226298779,-51.4167828882765,
0.));
#76063=CARTESIAN_POINT('Ctrl Pts',(-49.5701226298779,-51.4167828882765,
12.));
#76064=CARTESIAN_POINT('Ctrl Pts',(-49.579891735436,-51.4375029564191,0.));
#76065=CARTESIAN_POINT('Ctrl Pts',(-49.579891735436,-51.4375029564191,12.));
#76066=CARTESIAN_POINT('Ctrl Pts',(-49.5896592380634,-51.4582734149562,
0.));
#76067=CARTESIAN_POINT('Ctrl Pts',(-49.5896592380634,-51.4582734149562,
12.));
#76068=CARTESIAN_POINT('Ctrl Pts',(-49.5994250204003,-51.4790941716859,
0.));
#76069=CARTESIAN_POINT('Ctrl Pts',(-49.5994250204003,-51.4790941716859,
12.));
#76070=CARTESIAN_POINT('Ctrl Pts',(-49.609188965684,-51.4999651347496,0.));
#76071=CARTESIAN_POINT('Ctrl Pts',(-49.609188965684,-51.4999651347496,12.));
#76072=CARTESIAN_POINT('Ctrl Pts',(-49.6189509577441,-51.5208862126303,
0.));
#76073=CARTESIAN_POINT('Ctrl Pts',(-49.6189509577441,-51.5208862126303,
12.));
#76074=CARTESIAN_POINT('Ctrl Pts',(-49.6287108809975,-51.5418573141494,
0.));
#76075=CARTESIAN_POINT('Ctrl Pts',(-49.6287108809975,-51.5418573141494,
12.));
#76076=CARTESIAN_POINT('Ctrl Pts',(-49.6384686204443,-51.5628783484556,
0.));
#76077=CARTESIAN_POINT('Ctrl Pts',(-49.6384686204443,-51.5628783484556,
12.));
#76078=CARTESIAN_POINT('Ctrl Pts',(-49.6482240616627,-51.5839492250218,
0.));
#76079=CARTESIAN_POINT('Ctrl Pts',(-49.6482240616627,-51.5839492250218,
12.));
#76080=CARTESIAN_POINT('Ctrl Pts',(-49.6579770908063,-51.6050698536525,
0.));
#76081=CARTESIAN_POINT('Ctrl Pts',(-49.6579770908063,-51.6050698536525,
12.));
#76082=CARTESIAN_POINT('Ctrl Pts',(-49.6677275945975,-51.6262401444799,
0.));
#76083=CARTESIAN_POINT('Ctrl Pts',(-49.6677275945975,-51.6262401444799,
12.));
#76084=CARTESIAN_POINT('Ctrl Pts',(-49.6774754603235,-51.6474600079611,
0.));
#76085=CARTESIAN_POINT('Ctrl Pts',(-49.6774754603235,-51.6474600079611,
12.));
#76086=CARTESIAN_POINT('Ctrl Pts',(-49.6872205758314,-51.6687293548656,
0.));
#76087=CARTESIAN_POINT('Ctrl Pts',(-49.6872205758314,-51.6687293548656,
12.));
#76088=CARTESIAN_POINT('Ctrl Pts',(-49.6969628295236,-51.6900480962744,
0.));
#76089=CARTESIAN_POINT('Ctrl Pts',(-49.6969628295236,-51.6900480962744,
12.));
#76090=CARTESIAN_POINT('Ctrl Pts',(-49.7067021103534,-51.7114161435848,
0.));
#76091=CARTESIAN_POINT('Ctrl Pts',(-49.7067021103534,-51.7114161435848,
12.));
#76092=CARTESIAN_POINT('Ctrl Pts',(-49.7164383078206,-51.7328334085084,
0.));
#76093=CARTESIAN_POINT('Ctrl Pts',(-49.7164383078206,-51.7328334085084,
12.));
#76094=CARTESIAN_POINT('Ctrl Pts',(-49.7261713119672,-51.754299803068,0.));
#76095=CARTESIAN_POINT('Ctrl Pts',(-49.7261713119672,-51.754299803068,12.));
#76096=CARTESIAN_POINT('Ctrl Pts',(-49.7359010133741,-51.7758152395857,
0.));
#76097=CARTESIAN_POINT('Ctrl Pts',(-49.7359010133741,-51.7758152395857,
12.));
#76098=CARTESIAN_POINT('Ctrl Pts',(-49.7456273031555,-51.7973796306826,
0.));
#76099=CARTESIAN_POINT('Ctrl Pts',(-49.7456273031555,-51.7973796306826,
12.));
#76100=CARTESIAN_POINT('Ctrl Pts',(-49.7553500729563,-51.8189928892841,
0.));
#76101=CARTESIAN_POINT('Ctrl Pts',(-49.7553500729563,-51.8189928892841,
12.));
#76102=CARTESIAN_POINT('Ctrl Pts',(-49.7650692149464,-51.8406549286177,
0.));
#76103=CARTESIAN_POINT('Ctrl Pts',(-49.7650692149464,-51.8406549286177,
12.));
#76104=CARTESIAN_POINT('Ctrl Pts',(-49.7747846218177,-51.8623656622092,
0.));
#76105=CARTESIAN_POINT('Ctrl Pts',(-49.7747846218177,-51.8623656622092,
12.));
#76106=CARTESIAN_POINT('Ctrl Pts',(-49.78449618678,-51.8841250038716,0.));
#76107=CARTESIAN_POINT('Ctrl Pts',(-49.78449618678,-51.8841250038716,12.));
#76108=CARTESIAN_POINT('Ctrl Pts',(-49.7942038035568,-51.9059328677051,
0.));
#76109=CARTESIAN_POINT('Ctrl Pts',(-49.7942038035568,-51.9059328677051,
12.));
#76110=CARTESIAN_POINT('Ctrl Pts',(-49.8039073663808,-51.9277891681014,
0.));
#76111=CARTESIAN_POINT('Ctrl Pts',(-49.8039073663808,-51.9277891681014,
12.));
#76112=CARTESIAN_POINT('Ctrl Pts',(-49.8136067699896,-51.9496938197418,
0.));
#76113=CARTESIAN_POINT('Ctrl Pts',(-49.8136067699896,-51.9496938197418,
12.));
#76114=CARTESIAN_POINT('Ctrl Pts',(-49.8233019096224,-51.9716467375938,
0.));
#76115=CARTESIAN_POINT('Ctrl Pts',(-49.8233019096224,-51.9716467375938,
12.));
#76116=CARTESIAN_POINT('Ctrl Pts',(-49.8329926810172,-51.9936478369008,
0.));
#76117=CARTESIAN_POINT('Ctrl Pts',(-49.8329926810172,-51.9936478369008,
12.));
#76118=CARTESIAN_POINT('Ctrl Pts',(-49.8426789804068,-52.015697033182,0.));
#76119=CARTESIAN_POINT('Ctrl Pts',(-49.8426789804068,-52.015697033182,12.));
#76120=CARTESIAN_POINT('Ctrl Pts',(-49.8523607045146,-52.0377942422373,
0.));
#76121=CARTESIAN_POINT('Ctrl Pts',(-49.8523607045146,-52.0377942422373,
12.));
#76122=CARTESIAN_POINT('Ctrl Pts',(-49.8620377505498,-52.059939380145,0.));
#76123=CARTESIAN_POINT('Ctrl Pts',(-49.8620377505498,-52.059939380145,12.));
#76124=CARTESIAN_POINT('Ctrl Pts',(-49.871710016205,-52.0821323632588,0.));
#76125=CARTESIAN_POINT('Ctrl Pts',(-49.871710016205,-52.0821323632588,12.));
#76126=CARTESIAN_POINT('Ctrl Pts',(-49.8813773996523,-52.1043731081968,
0.));
#76127=CARTESIAN_POINT('Ctrl Pts',(-49.8813773996523,-52.1043731081968,
12.));
#76128=CARTESIAN_POINT('Ctrl Pts',(-49.8910397995404,-52.1266615318414,
0.));
#76129=CARTESIAN_POINT('Ctrl Pts',(-49.8910397995404,-52.1266615318414,
12.));
#76130=CARTESIAN_POINT('Ctrl Pts',(-49.90069711499,-52.1489975513449,0.));
#76131=CARTESIAN_POINT('Ctrl Pts',(-49.90069711499,-52.1489975513449,12.));
#76132=CARTESIAN_POINT('Ctrl Pts',(-49.9103492455904,-52.1713810841277,
0.));
#76133=CARTESIAN_POINT('Ctrl Pts',(-49.9103492455904,-52.1713810841277,
12.));
#76134=CARTESIAN_POINT('Ctrl Pts',(-49.919996091396,-52.1938120478752,0.));
#76135=CARTESIAN_POINT('Ctrl Pts',(-49.919996091396,-52.1938120478752,12.));
#76136=CARTESIAN_POINT('Ctrl Pts',(-49.9296375529241,-52.2162903605272,
0.));
#76137=CARTESIAN_POINT('Ctrl Pts',(-49.9296375529241,-52.2162903605272,
12.));
#76138=CARTESIAN_POINT('Ctrl Pts',(-49.9392735311507,-52.238815940277,0.));
#76139=CARTESIAN_POINT('Ctrl Pts',(-49.9392735311507,-52.238815940277,12.));
#76140=CARTESIAN_POINT('Ctrl Pts',(-49.9489039275064,-52.2613887055773,
0.));
#76141=CARTESIAN_POINT('Ctrl Pts',(-49.9489039275064,-52.2613887055773,
12.));
#76142=CARTESIAN_POINT('Ctrl Pts',(-49.9585286438734,-52.2840085751385,
0.));
#76143=CARTESIAN_POINT('Ctrl Pts',(-49.9585286438734,-52.2840085751385,
12.));
#76144=CARTESIAN_POINT('Ctrl Pts',(-49.9681475825824,-52.3066754679265,
0.));
#76145=CARTESIAN_POINT('Ctrl Pts',(-49.9681475825824,-52.3066754679265,
12.));
#76146=CARTESIAN_POINT('Ctrl Pts',(-49.9777606464103,-52.3293893031524,
0.));
#76147=CARTESIAN_POINT('Ctrl Pts',(-49.9777606464103,-52.3293893031524,
12.));
#76148=CARTESIAN_POINT('Ctrl Pts',(-49.9873677385769,-52.3521500002711,
0.));
#76149=CARTESIAN_POINT('Ctrl Pts',(-49.9873677385769,-52.3521500002711,
12.));
#76150=CARTESIAN_POINT('Ctrl Pts',(-49.9969687627402,-52.3749574789865,
0.));
#76151=CARTESIAN_POINT('Ctrl Pts',(-49.9969687627402,-52.3749574789865,
12.));
#76152=CARTESIAN_POINT('Ctrl Pts',(-50.0065636229934,-52.3978116592505,
0.));
#76153=CARTESIAN_POINT('Ctrl Pts',(-50.0065636229934,-52.3978116592505,
12.));
#76154=CARTESIAN_POINT('Ctrl Pts',(-50.0161522238619,-52.420712461261,0.));
#76155=CARTESIAN_POINT('Ctrl Pts',(-50.0161522238619,-52.420712461261,12.));
#76156=CARTESIAN_POINT('Ctrl Pts',(-50.0257344703008,-52.4436598054523,
0.));
#76157=CARTESIAN_POINT('Ctrl Pts',(-50.0257344703008,-52.4436598054523,
12.));
#76158=CARTESIAN_POINT('Ctrl Pts',(-50.0353102676933,-52.4666536124926,
0.));
#76159=CARTESIAN_POINT('Ctrl Pts',(-50.0353102676933,-52.4666536124926,
12.));
#76160=CARTESIAN_POINT('Ctrl Pts',(-50.0448795218453,-52.4896938032896,
0.));
#76161=CARTESIAN_POINT('Ctrl Pts',(-50.0448795218453,-52.4896938032896,
12.));
#76162=CARTESIAN_POINT('Ctrl Pts',(-50.0544421389824,-52.5127802989903,
0.));
#76163=CARTESIAN_POINT('Ctrl Pts',(-50.0544421389824,-52.5127802989903,
12.));
#76164=CARTESIAN_POINT('Ctrl Pts',(-50.0639980257477,-52.5359130209789,
0.));
#76165=CARTESIAN_POINT('Ctrl Pts',(-50.0639980257477,-52.5359130209789,
12.));
#76166=CARTESIAN_POINT('Ctrl Pts',(-50.0735470891996,-52.5590918908691,
0.));
#76167=CARTESIAN_POINT('Ctrl Pts',(-50.0735470891996,-52.5590918908691,
12.));
#76168=CARTESIAN_POINT('Ctrl Pts',(-50.0830892368095,-52.5823168304981,
0.));
#76169=CARTESIAN_POINT('Ctrl Pts',(-50.0830892368095,-52.5823168304981,
12.));
#76170=CARTESIAN_POINT('Ctrl Pts',(-50.0926243764569,-52.6055877619338,
0.));
#76171=CARTESIAN_POINT('Ctrl Pts',(-50.0926243764569,-52.6055877619338,
12.));
#76172=CARTESIAN_POINT('Ctrl Pts',(-50.1021524164261,-52.6289046074743,
0.));
#76173=CARTESIAN_POINT('Ctrl Pts',(-50.1021524164261,-52.6289046074743,
12.));
#76174=CARTESIAN_POINT('Ctrl Pts',(-50.1116732654041,-52.6522672896462,
0.));
#76175=CARTESIAN_POINT('Ctrl Pts',(-50.1116732654041,-52.6522672896462,
12.));
#76176=CARTESIAN_POINT('Ctrl Pts',(-50.1211868324781,-52.6756757311979,
0.));
#76177=CARTESIAN_POINT('Ctrl Pts',(-50.1211868324781,-52.6756757311979,
12.));
#76178=CARTESIAN_POINT('Ctrl Pts',(-50.1306930271343,-52.6991298550928,
0.));
#76179=CARTESIAN_POINT('Ctrl Pts',(-50.1306930271343,-52.6991298550928,
12.));
#76180=CARTESIAN_POINT('Ctrl Pts',(-50.1401917592532,-52.7226295845156,
0.));
#76181=CARTESIAN_POINT('Ctrl Pts',(-50.1401917592532,-52.7226295845156,
12.));
#76182=CARTESIAN_POINT('Ctrl Pts',(-50.1496829391068,-52.7461748428733,
0.));
#76183=CARTESIAN_POINT('Ctrl Pts',(-50.1496829391068,-52.7461748428733,
12.));
#76184=CARTESIAN_POINT('Ctrl Pts',(-50.1591664773561,-52.769765553794,0.));
#76185=CARTESIAN_POINT('Ctrl Pts',(-50.1591664773561,-52.769765553794,12.));
#76186=CARTESIAN_POINT('Ctrl Pts',(-50.1686422850493,-52.793401641121,0.));
#76187=CARTESIAN_POINT('Ctrl Pts',(-50.1686422850493,-52.793401641121,12.));
#76188=CARTESIAN_POINT('Ctrl Pts',(-50.1781102736215,-52.8170830289052,
0.));
#76189=CARTESIAN_POINT('Ctrl Pts',(-50.1781102736215,-52.8170830289052,
12.));
#76190=CARTESIAN_POINT('Ctrl Pts',(-50.1875703548893,-52.8408096414101,
0.));
#76191=CARTESIAN_POINT('Ctrl Pts',(-50.1875703548893,-52.8408096414101,
12.));
#76192=CARTESIAN_POINT('Ctrl Pts',(-50.1970224410476,-52.8645814031137,
0.));
#76193=CARTESIAN_POINT('Ctrl Pts',(-50.1970224410476,-52.8645814031137,
12.));
#76194=CARTESIAN_POINT('Ctrl Pts',(-50.2064664446663,-52.8883982387068,
0.));
#76195=CARTESIAN_POINT('Ctrl Pts',(-50.2064664446663,-52.8883982387068,
12.));
#76196=CARTESIAN_POINT('Ctrl Pts',(-50.2159022786876,-52.9122600730882,
0.));
#76197=CARTESIAN_POINT('Ctrl Pts',(-50.2159022786876,-52.9122600730882,
12.));
#76198=CARTESIAN_POINT('Ctrl Pts',(-50.2253298564237,-52.9361668313539,
0.));
#76199=CARTESIAN_POINT('Ctrl Pts',(-50.2253298564237,-52.9361668313539,
12.));
#76200=CARTESIAN_POINT('Ctrl Pts',(-50.2347490915553,-52.9601184388027,
0.));
#76201=CARTESIAN_POINT('Ctrl Pts',(-50.2347490915553,-52.9601184388027,
12.));
#76202=CARTESIAN_POINT('Ctrl Pts',(-50.2441598981286,-52.9841148209404,
0.));
#76203=CARTESIAN_POINT('Ctrl Pts',(-50.2441598981286,-52.9841148209404,
12.));
#76204=CARTESIAN_POINT('Ctrl Pts',(-50.2535621905553,-53.0081559034802,
0.));
#76205=CARTESIAN_POINT('Ctrl Pts',(-50.2535621905553,-53.0081559034802,
12.));
#76206=CARTESIAN_POINT('Ctrl Pts',(-50.262955883611,-53.0322416123404,0.));
#76207=CARTESIAN_POINT('Ctrl Pts',(-50.262955883611,-53.0322416123404,12.));
#76208=CARTESIAN_POINT('Ctrl Pts',(-50.272340892437,-53.0563718736361,0.));
#76209=CARTESIAN_POINT('Ctrl Pts',(-50.272340892437,-53.0563718736361,12.));
#76210=CARTESIAN_POINT('Ctrl Pts',(-50.2817171325354,-53.0805466136791,
0.));
#76211=CARTESIAN_POINT('Ctrl Pts',(-50.2817171325354,-53.0805466136791,
12.));
#76212=CARTESIAN_POINT('Ctrl Pts',(-50.2910845197615,-53.1047657589806,
0.));
#76213=CARTESIAN_POINT('Ctrl Pts',(-50.2910845197615,-53.1047657589806,
12.));
#76214=CARTESIAN_POINT('Ctrl Pts',(-50.3004429703188,-53.1290292362482,
0.));
#76215=CARTESIAN_POINT('Ctrl Pts',(-50.3004429703188,-53.1290292362482,
12.));
#76216=CARTESIAN_POINT('Ctrl Pts',(-50.3097924007536,-53.153336972382,0.));
#76217=CARTESIAN_POINT('Ctrl Pts',(-50.3097924007536,-53.153336972382,12.));
#76218=CARTESIAN_POINT('Ctrl Pts',(-50.3191327279497,-53.1776888944622,
0.));
#76219=CARTESIAN_POINT('Ctrl Pts',(-50.3191327279497,-53.1776888944622,
12.));
#76220=CARTESIAN_POINT('Ctrl Pts',(-50.3284638691285,-53.202084929748,0.));
#76221=CARTESIAN_POINT('Ctrl Pts',(-50.3284638691285,-53.202084929748,12.));
#76222=CARTESIAN_POINT('Ctrl Pts',(-50.3377857418522,-53.2265250056896,
0.));
#76223=CARTESIAN_POINT('Ctrl Pts',(-50.3377857418522,-53.2265250056896,
12.));
#76224=CARTESIAN_POINT('Ctrl Pts',(-50.3470982640294,-53.2510090499341,
0.));
#76225=CARTESIAN_POINT('Ctrl Pts',(-50.3470982640294,-53.2510090499341,
12.));
#76226=CARTESIAN_POINT('Ctrl Pts',(-50.3564013539198,-53.2755369903291,
0.));
#76227=CARTESIAN_POINT('Ctrl Pts',(-50.3564013539198,-53.2755369903291,
12.));
#76228=CARTESIAN_POINT('Ctrl Pts',(-50.3656949301424,-53.3001087549222,
0.));
#76229=CARTESIAN_POINT('Ctrl Pts',(-50.3656949301424,-53.3001087549222,
12.));
#76230=CARTESIAN_POINT('Ctrl Pts',(-50.3749789116777,-53.3247242719575,
0.));
#76231=CARTESIAN_POINT('Ctrl Pts',(-50.3749789116777,-53.3247242719575,
12.));
#76232=CARTESIAN_POINT('Ctrl Pts',(-50.3842532178451,-53.3493834698685,
0.));
#76233=CARTESIAN_POINT('Ctrl Pts',(-50.3842532178451,-53.3493834698685,
12.));
#76234=CARTESIAN_POINT('Ctrl Pts',(-50.393517768283,-53.3740862772673,0.));
#76235=CARTESIAN_POINT('Ctrl Pts',(-50.393517768283,-53.3740862772673,12.));
#76236=CARTESIAN_POINT('Ctrl Pts',(-50.4027724829296,-53.3988326229308,
0.));
#76237=CARTESIAN_POINT('Ctrl Pts',(-50.4027724829296,-53.3988326229308,
12.));
#76238=CARTESIAN_POINT('Ctrl Pts',(-50.4120172820054,-53.4236224357846,
0.));
#76239=CARTESIAN_POINT('Ctrl Pts',(-50.4120172820054,-53.4236224357846,
12.));
#76240=CARTESIAN_POINT('Ctrl Pts',(-50.4212520859924,-53.4484556448787,
0.));
#76241=CARTESIAN_POINT('Ctrl Pts',(-50.4212520859924,-53.4484556448787,
12.));
#76242=CARTESIAN_POINT('Ctrl Pts',(-50.4304768156677,-53.4733321794199,
0.));
#76243=CARTESIAN_POINT('Ctrl Pts',(-50.4304768156677,-53.4733321794199,
12.));
#76244=CARTESIAN_POINT('Ctrl Pts',(-50.4396913921389,-53.4982519688032,
0.));
#76245=CARTESIAN_POINT('Ctrl Pts',(-50.4396913921389,-53.4982519688032,
12.));
#76246=CARTESIAN_POINT('Ctrl Pts',(-50.4488957368841,-53.5232149426415,
0.));
#76247=CARTESIAN_POINT('Ctrl Pts',(-50.4488957368841,-53.5232149426415,
12.));
#76248=CARTESIAN_POINT('Ctrl Pts',(-50.4580897717835,-53.5482210307864,
0.));
#76249=CARTESIAN_POINT('Ctrl Pts',(-50.4580897717835,-53.5482210307864,
12.));
#76250=CARTESIAN_POINT('Ctrl Pts',(-50.467273419175,-53.5732701633603,0.));
#76251=CARTESIAN_POINT('Ctrl Pts',(-50.467273419175,-53.5732701633603,12.));
#76252=CARTESIAN_POINT('Ctrl Pts',(-50.4764466018064,-53.5983622707231,
0.));
#76253=CARTESIAN_POINT('Ctrl Pts',(-50.4764466018064,-53.5983622707231,
12.));
#76254=CARTESIAN_POINT('Ctrl Pts',(-50.485609242731,-53.6234972834055,0.));
#76255=CARTESIAN_POINT('Ctrl Pts',(-50.485609242731,-53.6234972834055,12.));
#76256=CARTESIAN_POINT('Ctrl Pts',(-50.4947612652147,-53.6486751320434,
0.));
#76257=CARTESIAN_POINT('Ctrl Pts',(-50.4947612652147,-53.6486751320434,
12.));
#76258=CARTESIAN_POINT('Ctrl Pts',(-50.5039025926531,-53.6738957473158,
0.));
#76259=CARTESIAN_POINT('Ctrl Pts',(-50.5039025926531,-53.6738957473158,
12.));
#76260=CARTESIAN_POINT('Ctrl Pts',(-50.5130331484563,-53.6991590598551,
0.));
#76261=CARTESIAN_POINT('Ctrl Pts',(-50.5130331484563,-53.6991590598551,
12.));
#76262=CARTESIAN_POINT('Ctrl Pts',(-50.5221528560427,-53.7244650002382,
0.));
#76263=CARTESIAN_POINT('Ctrl Pts',(-50.5221528560427,-53.7244650002382,
12.));
#76264=CARTESIAN_POINT('Ctrl Pts',(-50.5312616390789,-53.7498134991714,
0.));
#76265=CARTESIAN_POINT('Ctrl Pts',(-50.5312616390789,-53.7498134991714,
12.));
#76266=CARTESIAN_POINT('Ctrl Pts',(-50.5403594216706,-53.7752044876313,
0.));
#76267=CARTESIAN_POINT('Ctrl Pts',(-50.5403594216706,-53.7752044876313,
12.));
#76268=CARTESIAN_POINT('Ctrl Pts',(-50.5494461285762,-53.8006378970198,
0.));
#76269=CARTESIAN_POINT('Ctrl Pts',(-50.5494461285762,-53.8006378970198,
12.));
#76270=CARTESIAN_POINT('Ctrl Pts',(-50.5585216854082,-53.8261136593064,
0.));
#76271=CARTESIAN_POINT('Ctrl Pts',(-50.5585216854082,-53.8261136593064,
12.));
#76272=CARTESIAN_POINT('Ctrl Pts',(-50.567586018852,-53.8516317071783,0.));
#76273=CARTESIAN_POINT('Ctrl Pts',(-50.567586018852,-53.8516317071783,12.));
#76274=CARTESIAN_POINT('Ctrl Pts',(-50.5766390561861,-53.8771919737007,
0.));
#76275=CARTESIAN_POINT('Ctrl Pts',(-50.5766390561861,-53.8771919737007,
12.));
#76276=CARTESIAN_POINT('Ctrl Pts',(-50.5856807248133,-53.9027943919814,
0.));
#76277=CARTESIAN_POINT('Ctrl Pts',(-50.5856807248133,-53.9027943919814,
12.));
#76278=CARTESIAN_POINT('Ctrl Pts',(-50.5947109517476,-53.9284388947996,
0.));
#76279=CARTESIAN_POINT('Ctrl Pts',(-50.5947109517476,-53.9284388947996,
12.));
#76280=CARTESIAN_POINT('Ctrl Pts',(-50.603729663215,-53.9541254143131,0.));
#76281=CARTESIAN_POINT('Ctrl Pts',(-50.603729663215,-53.9541254143131,12.));
#76282=CARTESIAN_POINT('Ctrl Pts',(-50.6127367839738,-53.9798538815561,
0.));
#76283=CARTESIAN_POINT('Ctrl Pts',(-50.6127367839738,-53.9798538815561,
12.));
#76284=CARTESIAN_POINT('Ctrl Pts',(-50.6217322378686,-54.0056242268443,
0.));
#76285=CARTESIAN_POINT('Ctrl Pts',(-50.6217322378686,-54.0056242268443,
12.));
#76286=CARTESIAN_POINT('Ctrl Pts',(-50.630715949059,-54.0314363806751,0.));
#76287=CARTESIAN_POINT('Ctrl Pts',(-50.630715949059,-54.0314363806751,12.));
#76288=CARTESIAN_POINT('Ctrl Pts',(-50.6396878430961,-54.0572902745101,
0.));
#76289=CARTESIAN_POINT('Ctrl Pts',(-50.6396878430961,-54.0572902745101,
12.));
#76290=CARTESIAN_POINT('Ctrl Pts',(-50.6486478479459,-54.0831858415182,
0.));
#76291=CARTESIAN_POINT('Ctrl Pts',(-50.6486478479459,-54.0831858415182,
12.));
#76292=CARTESIAN_POINT('Ctrl Pts',(-50.657595895318,-54.1091230175319,0.));
#76293=CARTESIAN_POINT('Ctrl Pts',(-50.657595895318,-54.1091230175319,12.));
#76294=CARTESIAN_POINT('Ctrl Pts',(-50.6665319209798,-54.1351017412722,
0.));
#76295=CARTESIAN_POINT('Ctrl Pts',(-50.6665319209798,-54.1351017412722,
12.));
#76296=CARTESIAN_POINT('Ctrl Pts',(-50.6754558618218,-54.1611219522299,
0.));
#76297=CARTESIAN_POINT('Ctrl Pts',(-50.6754558618218,-54.1611219522299,
12.));
#76298=CARTESIAN_POINT('Ctrl Pts',(-50.6843676535428,-54.1871835889908,
0.));
#76299=CARTESIAN_POINT('Ctrl Pts',(-50.6843676535428,-54.1871835889908,
12.));
#76300=CARTESIAN_POINT('Ctrl Pts',(-50.6932672279758,-54.2132865872968,
0.));
#76301=CARTESIAN_POINT('Ctrl Pts',(-50.6932672279758,-54.2132865872968,
12.));
#76302=CARTESIAN_POINT('Ctrl Pts',(-50.7021545108369,-54.2394308784093,
0.));
#76303=CARTESIAN_POINT('Ctrl Pts',(-50.7021545108369,-54.2394308784093,
12.));
#76304=CARTESIAN_POINT('Ctrl Pts',(-50.7110294185832,-54.2656163868258,
0.));
#76305=CARTESIAN_POINT('Ctrl Pts',(-50.7110294185832,-54.2656163868258,
12.));
#76306=CARTESIAN_POINT('Ctrl Pts',(-50.7198918629632,-54.2918430335414,
0.));
#76307=CARTESIAN_POINT('Ctrl Pts',(-50.7198918629632,-54.2918430335414,
12.));
#76308=CARTESIAN_POINT('Ctrl Pts',(-50.7287417566296,-54.3181107400862,
0.));
#76309=CARTESIAN_POINT('Ctrl Pts',(-50.7287417566296,-54.3181107400862,
12.));
#76310=CARTESIAN_POINT('Ctrl Pts',(-50.7375790185988,-54.344419432416,0.));
#76311=CARTESIAN_POINT('Ctrl Pts',(-50.7375790185988,-54.344419432416,12.));
#76312=CARTESIAN_POINT('Ctrl Pts',(-50.7464035792846,-54.3707690445679,
0.));
#76313=CARTESIAN_POINT('Ctrl Pts',(-50.7464035792846,-54.3707690445679,
12.));
#76314=CARTESIAN_POINT('Ctrl Pts',(-50.7552153869224,-54.3971595231285,
0.));
#76315=CARTESIAN_POINT('Ctrl Pts',(-50.7552153869224,-54.3971595231285,
12.));
#76316=CARTESIAN_POINT('Ctrl Pts',(-50.7640144089601,-54.4235908287188,
0.));
#76317=CARTESIAN_POINT('Ctrl Pts',(-50.7640144089601,-54.4235908287188,
12.));
#76318=CARTESIAN_POINT('Ctrl Pts',(-50.772800626886,-54.4500629335867,0.));
#76319=CARTESIAN_POINT('Ctrl Pts',(-50.772800626886,-54.4500629335867,12.));
#76320=CARTESIAN_POINT('Ctrl Pts',(-50.7798193515479,-54.4712732428597,
0.));
#76321=CARTESIAN_POINT('Ctrl Pts',(-50.7798193515479,-54.4712732428597,
12.));
#76322=CARTESIAN_POINT('Ctrl Pts',(-50.7850776288567,-54.4871993224549,
0.));
#76323=CARTESIAN_POINT('Ctrl Pts',(-50.7850776288567,-54.4871993224549,
12.));
#76324=CARTESIAN_POINT('Ctrl Pts',(-50.7885805844191,-54.4978248630284,
0.));
#76325=CARTESIAN_POINT('Ctrl Pts',(-50.7885805844191,-54.4978248630284,
12.));
#76326=CARTESIAN_POINT('Ctrl Pts',(-50.7903314215393,-54.5031396718592,
0.));
#76327=CARTESIAN_POINT('Ctrl Pts',(-50.7903314215393,-54.5031396718592,
12.));
#76328=CARTESIAN_POINT('',(-48.8900464144686,-50.0975384783634,0.));
#76329=CARTESIAN_POINT('Ctrl Pts',(-48.8900464144686,-50.0975384783634,
0.));
#76330=CARTESIAN_POINT('Ctrl Pts',(-48.8919551910299,-50.1009206494209,
0.));
#76331=CARTESIAN_POINT('Ctrl Pts',(-48.8957735556681,-50.1076907555303,
0.));
#76332=CARTESIAN_POINT('Ctrl Pts',(-48.9015035371772,-50.1178632066821,
0.));
#76333=CARTESIAN_POINT('Ctrl Pts',(-48.9091483817797,-50.1314610602286,
0.));
#76334=CARTESIAN_POINT('Ctrl Pts',(-48.9187125417897,-50.148516018447,0.));
#76335=CARTESIAN_POINT('Ctrl Pts',(-48.9282847698237,-50.1656286003943,
0.));
#76336=CARTESIAN_POINT('Ctrl Pts',(-48.9378649933116,-50.1827987615659,
0.));
#76337=CARTESIAN_POINT('Ctrl Pts',(-48.9474530868847,-50.2000264157903,
0.));
#76338=CARTESIAN_POINT('Ctrl Pts',(-48.9570488741273,-50.2173114358423,
0.));
#76339=CARTESIAN_POINT('Ctrl Pts',(-48.9666521500969,-50.2346536715465,
0.));
#76340=CARTESIAN_POINT('Ctrl Pts',(-48.9762626987227,-50.252052963548,0.));
#76341=CARTESIAN_POINT('Ctrl Pts',(-48.9858803116649,-50.2695091583473,
0.));
#76342=CARTESIAN_POINT('Ctrl Pts',(-48.9955048082028,-50.2870221241003,
0.));
#76343=CARTESIAN_POINT('Ctrl Pts',(-49.0051360288002,-50.3045917455383,
0.));
#76344=CARTESIAN_POINT('Ctrl Pts',(-49.0147738256925,-50.3222179165102,
0.));
#76345=CARTESIAN_POINT('Ctrl Pts',(-49.0244180550759,-50.3399005337967,
0.));
#76346=CARTESIAN_POINT('Ctrl Pts',(-49.034068567401,-50.3576394894136,0.));
#76347=CARTESIAN_POINT('Ctrl Pts',(-49.0437252024868,-50.3754346667389,
0.));
#76348=CARTESIAN_POINT('Ctrl Pts',(-49.0533877945771,-50.393285944528,0.));
#76349=CARTESIAN_POINT('Ctrl Pts',(-49.0630561755082,-50.4111931994264,
0.));
#76350=CARTESIAN_POINT('Ctrl Pts',(-49.0727301783477,-50.4291563088528,
0.));
#76351=CARTESIAN_POINT('Ctrl Pts',(-49.0824096415339,-50.4471751542717,
0.));
#76352=CARTESIAN_POINT('Ctrl Pts',(-49.0920944086973,-50.465249621057,0.));
#76353=CARTESIAN_POINT('Ctrl Pts',(-49.1017843266782,-50.4833795969296,
0.));
#76354=CARTESIAN_POINT('Ctrl Pts',(-49.1114792441573,-50.5015649708742,
0.));
#76355=CARTESIAN_POINT('Ctrl Pts',(-49.1211790099817,-50.5198056318111,
0.));
#76356=CARTESIAN_POINT('Ctrl Pts',(-49.1308834717645,-50.5381014674822,
0.));
#76357=CARTESIAN_POINT('Ctrl Pts',(-49.1405924766169,-50.5564523650406,
0.));
#76358=CARTESIAN_POINT('Ctrl Pts',(-49.1503058717831,-50.5748582115575,
0.));
#76359=CARTESIAN_POINT('Ctrl Pts',(-49.1600235052613,-50.593318894516,0.));
#76360=CARTESIAN_POINT('Ctrl Pts',(-49.1697452265473,-50.6118343023937,
0.));
#76361=CARTESIAN_POINT('Ctrl Pts',(-49.1794708869074,-50.6304043248796,
0.));
#76362=CARTESIAN_POINT('Ctrl Pts',(-49.1892003389743,-50.6490288525639,
0.));
#76363=CARTESIAN_POINT('Ctrl Pts',(-49.1989334364992,-50.6677077767427,
0.));
#76364=CARTESIAN_POINT('Ctrl Pts',(-49.2086700340625,-50.6864409891905,
0.));
#76365=CARTESIAN_POINT('Ctrl Pts',(-49.218409986748,-50.7052283818941,0.));
#76366=CARTESIAN_POINT('Ctrl Pts',(-49.2281531501569,-50.7240698470698,
0.));
#76367=CARTESIAN_POINT('Ctrl Pts',(-49.2378993805482,-50.7429652772816,
0.));
#76368=CARTESIAN_POINT('Ctrl Pts',(-49.2476485349373,-50.7619145655207,
0.));
#76369=CARTESIAN_POINT('Ctrl Pts',(-49.2574004712122,-50.7809176052954,
0.));
#76370=CARTESIAN_POINT('Ctrl Pts',(-49.2671550482415,-50.7999742907111,
0.));
#76371=CARTESIAN_POINT('Ctrl Pts',(-49.2769121258144,-50.8190845164319,
0.));
#76372=CARTESIAN_POINT('Ctrl Pts',(-49.2866715645828,-50.8382481776392,
0.));
#76373=CARTESIAN_POINT('Ctrl Pts',(-49.2964332260043,-50.8574651699877,
0.));
#76374=CARTESIAN_POINT('Ctrl Pts',(-49.3061969722798,-50.8767353895509,
0.));
#76375=CARTESIAN_POINT('Ctrl Pts',(-49.3159626663129,-50.8960587327869,
0.));
#76376=CARTESIAN_POINT('Ctrl Pts',(-49.325730171735,-50.9154350965681,0.));
#76377=CARTESIAN_POINT('Ctrl Pts',(-49.3354993529163,-50.9348643781928,
0.));
#76378=CARTESIAN_POINT('Ctrl Pts',(-49.3452700749804,-50.9543464753974,
0.));
#76379=CARTESIAN_POINT('Ctrl Pts',(-49.3550422038221,-50.9738812863636,
0.));
#76380=CARTESIAN_POINT('Ctrl Pts',(-49.3648156061049,-50.9934687097179,
0.));
#76381=CARTESIAN_POINT('Ctrl Pts',(-49.3745901492429,-51.0131086445268,
0.));
#76382=CARTESIAN_POINT('Ctrl Pts',(-49.3843657013851,-51.0328009902857,
0.));
#76383=CARTESIAN_POINT('Ctrl Pts',(-49.3941421314014,-51.0525456469072,
0.));
#76384=CARTESIAN_POINT('Ctrl Pts',(-49.4039193088636,-51.0723425146987,
0.));
#76385=CARTESIAN_POINT('Ctrl Pts',(-49.4136971040428,-51.0921914943663,
0.));
#76386=CARTESIAN_POINT('Ctrl Pts',(-49.4234753879071,-51.1120924870196,
0.));
#76387=CARTESIAN_POINT('Ctrl Pts',(-49.4332540321178,-51.1320453941702,
0.));
#76388=CARTESIAN_POINT('Ctrl Pts',(-49.4430329090288,-51.1520501177291,
0.));
#76389=CARTESIAN_POINT('Ctrl Pts',(-49.4528118916833,-51.1721065599972,
0.));
#76390=CARTESIAN_POINT('Ctrl Pts',(-49.4625908538076,-51.1922146236686,
0.));
#76391=CARTESIAN_POINT('Ctrl Pts',(-49.4723696698022,-51.2123742118288,
0.));
#76392=CARTESIAN_POINT('Ctrl Pts',(-49.4821482147357,-51.2325852279507,
0.));
#76393=CARTESIAN_POINT('Ctrl Pts',(-49.4919263643357,-51.2528475758841,
0.));
#76394=CARTESIAN_POINT('Ctrl Pts',(-49.5017039949841,-51.2731611598465,
0.));
#76395=CARTESIAN_POINT('Ctrl Pts',(-49.5114809837111,-51.2935258844278,
0.));
#76396=CARTESIAN_POINT('Ctrl Pts',(-49.5212572081901,-51.3139416545903,
0.));
#76397=CARTESIAN_POINT('Ctrl Pts',(-49.5310325467334,-51.3344083756659,
0.));
#76398=CARTESIAN_POINT('Ctrl Pts',(-49.5408068782871,-51.354925953347,0.));
#76399=CARTESIAN_POINT('Ctrl Pts',(-49.5505800824268,-51.3754942936796,
0.));
#76400=CARTESIAN_POINT('Ctrl Pts',(-49.5603520393514,-51.3961133030688,
0.));
#76401=CARTESIAN_POINT('Ctrl Pts',(-49.5701226298779,-51.4167828882765,
0.));
#76402=CARTESIAN_POINT('Ctrl Pts',(-49.579891735436,-51.4375029564191,0.));
#76403=CARTESIAN_POINT('Ctrl Pts',(-49.5896592380634,-51.4582734149562,
0.));
#76404=CARTESIAN_POINT('Ctrl Pts',(-49.5994250204003,-51.4790941716859,
0.));
#76405=CARTESIAN_POINT('Ctrl Pts',(-49.609188965684,-51.4999651347496,0.));
#76406=CARTESIAN_POINT('Ctrl Pts',(-49.6189509577441,-51.5208862126303,
0.));
#76407=CARTESIAN_POINT('Ctrl Pts',(-49.6287108809975,-51.5418573141494,
0.));
#76408=CARTESIAN_POINT('Ctrl Pts',(-49.6384686204443,-51.5628783484556,
0.));
#76409=CARTESIAN_POINT('Ctrl Pts',(-49.6482240616627,-51.5839492250218,
0.));
#76410=CARTESIAN_POINT('Ctrl Pts',(-49.6579770908063,-51.6050698536525,
0.));
#76411=CARTESIAN_POINT('Ctrl Pts',(-49.6677275945975,-51.6262401444799,
0.));
#76412=CARTESIAN_POINT('Ctrl Pts',(-49.6774754603235,-51.6474600079611,
0.));
#76413=CARTESIAN_POINT('Ctrl Pts',(-49.6872205758314,-51.6687293548656,
0.));
#76414=CARTESIAN_POINT('Ctrl Pts',(-49.6969628295236,-51.6900480962744,
0.));
#76415=CARTESIAN_POINT('Ctrl Pts',(-49.7067021103534,-51.7114161435848,
0.));
#76416=CARTESIAN_POINT('Ctrl Pts',(-49.7164383078206,-51.7328334085084,
0.));
#76417=CARTESIAN_POINT('Ctrl Pts',(-49.7261713119672,-51.754299803068,0.));
#76418=CARTESIAN_POINT('Ctrl Pts',(-49.7359010133741,-51.7758152395857,
0.));
#76419=CARTESIAN_POINT('Ctrl Pts',(-49.7456273031555,-51.7973796306826,
0.));
#76420=CARTESIAN_POINT('Ctrl Pts',(-49.7553500729563,-51.8189928892841,
0.));
#76421=CARTESIAN_POINT('Ctrl Pts',(-49.7650692149464,-51.8406549286177,
0.));
#76422=CARTESIAN_POINT('Ctrl Pts',(-49.7747846218177,-51.8623656622092,
0.));
#76423=CARTESIAN_POINT('Ctrl Pts',(-49.78449618678,-51.8841250038716,0.));
#76424=CARTESIAN_POINT('Ctrl Pts',(-49.7942038035568,-51.9059328677051,
0.));
#76425=CARTESIAN_POINT('Ctrl Pts',(-49.8039073663808,-51.9277891681014,
0.));
#76426=CARTESIAN_POINT('Ctrl Pts',(-49.8136067699896,-51.9496938197418,
0.));
#76427=CARTESIAN_POINT('Ctrl Pts',(-49.8233019096224,-51.9716467375938,
0.));
#76428=CARTESIAN_POINT('Ctrl Pts',(-49.8329926810172,-51.9936478369008,
0.));
#76429=CARTESIAN_POINT('Ctrl Pts',(-49.8426789804068,-52.015697033182,0.));
#76430=CARTESIAN_POINT('Ctrl Pts',(-49.8523607045146,-52.0377942422373,
0.));
#76431=CARTESIAN_POINT('Ctrl Pts',(-49.8620377505498,-52.059939380145,0.));
#76432=CARTESIAN_POINT('Ctrl Pts',(-49.871710016205,-52.0821323632588,0.));
#76433=CARTESIAN_POINT('Ctrl Pts',(-49.8813773996523,-52.1043731081968,
0.));
#76434=CARTESIAN_POINT('Ctrl Pts',(-49.8910397995404,-52.1266615318414,
0.));
#76435=CARTESIAN_POINT('Ctrl Pts',(-49.90069711499,-52.1489975513449,0.));
#76436=CARTESIAN_POINT('Ctrl Pts',(-49.9103492455904,-52.1713810841277,
0.));
#76437=CARTESIAN_POINT('Ctrl Pts',(-49.919996091396,-52.1938120478752,0.));
#76438=CARTESIAN_POINT('Ctrl Pts',(-49.9296375529241,-52.2162903605272,
0.));
#76439=CARTESIAN_POINT('Ctrl Pts',(-49.9392735311507,-52.238815940277,0.));
#76440=CARTESIAN_POINT('Ctrl Pts',(-49.9489039275064,-52.2613887055773,
0.));
#76441=CARTESIAN_POINT('Ctrl Pts',(-49.9585286438734,-52.2840085751385,
0.));
#76442=CARTESIAN_POINT('Ctrl Pts',(-49.9681475825824,-52.3066754679265,
0.));
#76443=CARTESIAN_POINT('Ctrl Pts',(-49.9777606464103,-52.3293893031524,
0.));
#76444=CARTESIAN_POINT('Ctrl Pts',(-49.9873677385769,-52.3521500002711,
0.));
#76445=CARTESIAN_POINT('Ctrl Pts',(-49.9969687627402,-52.3749574789865,
0.));
#76446=CARTESIAN_POINT('Ctrl Pts',(-50.0065636229934,-52.3978116592505,
0.));
#76447=CARTESIAN_POINT('Ctrl Pts',(-50.0161522238619,-52.420712461261,0.));
#76448=CARTESIAN_POINT('Ctrl Pts',(-50.0257344703008,-52.4436598054523,
0.));
#76449=CARTESIAN_POINT('Ctrl Pts',(-50.0353102676933,-52.4666536124926,
0.));
#76450=CARTESIAN_POINT('Ctrl Pts',(-50.0448795218453,-52.4896938032896,
0.));
#76451=CARTESIAN_POINT('Ctrl Pts',(-50.0544421389824,-52.5127802989903,
0.));
#76452=CARTESIAN_POINT('Ctrl Pts',(-50.0639980257477,-52.5359130209789,
0.));
#76453=CARTESIAN_POINT('Ctrl Pts',(-50.0735470891996,-52.5590918908691,
0.));
#76454=CARTESIAN_POINT('Ctrl Pts',(-50.0830892368095,-52.5823168304981,
0.));
#76455=CARTESIAN_POINT('Ctrl Pts',(-50.0926243764569,-52.6055877619338,
0.));
#76456=CARTESIAN_POINT('Ctrl Pts',(-50.1021524164261,-52.6289046074743,
0.));
#76457=CARTESIAN_POINT('Ctrl Pts',(-50.1116732654041,-52.6522672896462,
0.));
#76458=CARTESIAN_POINT('Ctrl Pts',(-50.1211868324781,-52.6756757311979,
0.));
#76459=CARTESIAN_POINT('Ctrl Pts',(-50.1306930271343,-52.6991298550928,
0.));
#76460=CARTESIAN_POINT('Ctrl Pts',(-50.1401917592532,-52.7226295845156,
0.));
#76461=CARTESIAN_POINT('Ctrl Pts',(-50.1496829391068,-52.7461748428733,
0.));
#76462=CARTESIAN_POINT('Ctrl Pts',(-50.1591664773561,-52.769765553794,0.));
#76463=CARTESIAN_POINT('Ctrl Pts',(-50.1686422850493,-52.793401641121,0.));
#76464=CARTESIAN_POINT('Ctrl Pts',(-50.1781102736215,-52.8170830289052,
0.));
#76465=CARTESIAN_POINT('Ctrl Pts',(-50.1875703548893,-52.8408096414101,
0.));
#76466=CARTESIAN_POINT('Ctrl Pts',(-50.1970224410476,-52.8645814031137,
0.));
#76467=CARTESIAN_POINT('Ctrl Pts',(-50.2064664446663,-52.8883982387068,
0.));
#76468=CARTESIAN_POINT('Ctrl Pts',(-50.2159022786876,-52.9122600730882,
0.));
#76469=CARTESIAN_POINT('Ctrl Pts',(-50.2253298564237,-52.9361668313539,
0.));
#76470=CARTESIAN_POINT('Ctrl Pts',(-50.2347490915553,-52.9601184388027,
0.));
#76471=CARTESIAN_POINT('Ctrl Pts',(-50.2441598981286,-52.9841148209404,
0.));
#76472=CARTESIAN_POINT('Ctrl Pts',(-50.2535621905553,-53.0081559034802,
0.));
#76473=CARTESIAN_POINT('Ctrl Pts',(-50.262955883611,-53.0322416123404,0.));
#76474=CARTESIAN_POINT('Ctrl Pts',(-50.272340892437,-53.0563718736361,0.));
#76475=CARTESIAN_POINT('Ctrl Pts',(-50.2817171325354,-53.0805466136791,
0.));
#76476=CARTESIAN_POINT('Ctrl Pts',(-50.2910845197615,-53.1047657589806,
0.));
#76477=CARTESIAN_POINT('Ctrl Pts',(-50.3004429703188,-53.1290292362482,
0.));
#76478=CARTESIAN_POINT('Ctrl Pts',(-50.3097924007536,-53.153336972382,0.));
#76479=CARTESIAN_POINT('Ctrl Pts',(-50.3191327279497,-53.1776888944622,
0.));
#76480=CARTESIAN_POINT('Ctrl Pts',(-50.3284638691285,-53.202084929748,0.));
#76481=CARTESIAN_POINT('Ctrl Pts',(-50.3377857418522,-53.2265250056896,
0.));
#76482=CARTESIAN_POINT('Ctrl Pts',(-50.3470982640294,-53.2510090499341,
0.));
#76483=CARTESIAN_POINT('Ctrl Pts',(-50.3564013539198,-53.2755369903291,
0.));
#76484=CARTESIAN_POINT('Ctrl Pts',(-50.3656949301424,-53.3001087549222,
0.));
#76485=CARTESIAN_POINT('Ctrl Pts',(-50.3749789116777,-53.3247242719575,
0.));
#76486=CARTESIAN_POINT('Ctrl Pts',(-50.3842532178451,-53.3493834698685,
0.));
#76487=CARTESIAN_POINT('Ctrl Pts',(-50.393517768283,-53.3740862772673,0.));
#76488=CARTESIAN_POINT('Ctrl Pts',(-50.4027724829296,-53.3988326229308,
0.));
#76489=CARTESIAN_POINT('Ctrl Pts',(-50.4120172820054,-53.4236224357846,
0.));
#76490=CARTESIAN_POINT('Ctrl Pts',(-50.4212520859924,-53.4484556448787,
0.));
#76491=CARTESIAN_POINT('Ctrl Pts',(-50.4304768156677,-53.4733321794199,
0.));
#76492=CARTESIAN_POINT('Ctrl Pts',(-50.4396913921389,-53.4982519688032,
0.));
#76493=CARTESIAN_POINT('Ctrl Pts',(-50.4488957368841,-53.5232149426415,
0.));
#76494=CARTESIAN_POINT('Ctrl Pts',(-50.4580897717835,-53.5482210307864,
0.));
#76495=CARTESIAN_POINT('Ctrl Pts',(-50.467273419175,-53.5732701633603,0.));
#76496=CARTESIAN_POINT('Ctrl Pts',(-50.4764466018064,-53.5983622707231,
0.));
#76497=CARTESIAN_POINT('Ctrl Pts',(-50.485609242731,-53.6234972834055,0.));
#76498=CARTESIAN_POINT('Ctrl Pts',(-50.4947612652147,-53.6486751320434,
0.));
#76499=CARTESIAN_POINT('Ctrl Pts',(-50.5039025926531,-53.6738957473158,
0.));
#76500=CARTESIAN_POINT('Ctrl Pts',(-50.5130331484563,-53.6991590598551,
0.));
#76501=CARTESIAN_POINT('Ctrl Pts',(-50.5221528560427,-53.7244650002382,
0.));
#76502=CARTESIAN_POINT('Ctrl Pts',(-50.5312616390789,-53.7498134991714,
0.));
#76503=CARTESIAN_POINT('Ctrl Pts',(-50.5403594216706,-53.7752044876313,
0.));
#76504=CARTESIAN_POINT('Ctrl Pts',(-50.5494461285762,-53.8006378970198,
0.));
#76505=CARTESIAN_POINT('Ctrl Pts',(-50.5585216854082,-53.8261136593064,
0.));
#76506=CARTESIAN_POINT('Ctrl Pts',(-50.567586018852,-53.8516317071783,0.));
#76507=CARTESIAN_POINT('Ctrl Pts',(-50.5766390561861,-53.8771919737007,
0.));
#76508=CARTESIAN_POINT('Ctrl Pts',(-50.5856807248133,-53.9027943919814,
0.));
#76509=CARTESIAN_POINT('Ctrl Pts',(-50.5947109517476,-53.9284388947996,
0.));
#76510=CARTESIAN_POINT('Ctrl Pts',(-50.603729663215,-53.9541254143131,0.));
#76511=CARTESIAN_POINT('Ctrl Pts',(-50.6127367839738,-53.9798538815561,
0.));
#76512=CARTESIAN_POINT('Ctrl Pts',(-50.6217322378686,-54.0056242268443,
0.));
#76513=CARTESIAN_POINT('Ctrl Pts',(-50.630715949059,-54.0314363806751,0.));
#76514=CARTESIAN_POINT('Ctrl Pts',(-50.6396878430961,-54.0572902745101,
0.));
#76515=CARTESIAN_POINT('Ctrl Pts',(-50.6486478479459,-54.0831858415182,
0.));
#76516=CARTESIAN_POINT('Ctrl Pts',(-50.657595895318,-54.1091230175319,0.));
#76517=CARTESIAN_POINT('Ctrl Pts',(-50.6665319209798,-54.1351017412722,
0.));
#76518=CARTESIAN_POINT('Ctrl Pts',(-50.6741814675382,-54.1574061041881,
0.));
#76519=CARTESIAN_POINT('Ctrl Pts',(-50.6800396668659,-54.1745287898576,
0.));
#76520=CARTESIAN_POINT('Ctrl Pts',(-50.6841118861802,-54.1864514381923,
0.));
#76521=CARTESIAN_POINT('Ctrl Pts',(-50.6864016965602,-54.1931619277294,
0.));
#76522=CARTESIAN_POINT('Ctrl Pts',(-50.6869108458688,-54.1946543499977,
0.));
#76523=CARTESIAN_POINT('',(-48.8900464144686,-50.0975384783634,12.));
#76524=CARTESIAN_POINT('',(-48.8900464144686,-50.0975384783634,0.));
#76525=CARTESIAN_POINT('Ctrl Pts',(-50.6869108458688,-54.1946543499976,
12.));
#76526=CARTESIAN_POINT('Ctrl Pts',(-50.6864016965602,-54.1931619277293,
12.));
#76527=CARTESIAN_POINT('Ctrl Pts',(-50.6841118861802,-54.1864514381923,
12.));
#76528=CARTESIAN_POINT('Ctrl Pts',(-50.6800396668659,-54.1745287898576,
12.));
#76529=CARTESIAN_POINT('Ctrl Pts',(-50.6741814675382,-54.1574061041882,
12.));
#76530=CARTESIAN_POINT('Ctrl Pts',(-50.6665319209798,-54.1351017412722,
12.));
#76531=CARTESIAN_POINT('Ctrl Pts',(-50.657595895318,-54.1091230175319,12.));
#76532=CARTESIAN_POINT('Ctrl Pts',(-50.6486478479459,-54.0831858415182,
12.));
#76533=CARTESIAN_POINT('Ctrl Pts',(-50.6396878430961,-54.0572902745101,
12.));
#76534=CARTESIAN_POINT('Ctrl Pts',(-50.630715949059,-54.0314363806751,12.));
#76535=CARTESIAN_POINT('Ctrl Pts',(-50.6217322378686,-54.0056242268443,
12.));
#76536=CARTESIAN_POINT('Ctrl Pts',(-50.6127367839738,-53.9798538815561,
12.));
#76537=CARTESIAN_POINT('Ctrl Pts',(-50.603729663215,-53.9541254143131,12.));
#76538=CARTESIAN_POINT('Ctrl Pts',(-50.5947109517476,-53.9284388947996,
12.));
#76539=CARTESIAN_POINT('Ctrl Pts',(-50.5856807248133,-53.9027943919814,
12.));
#76540=CARTESIAN_POINT('Ctrl Pts',(-50.5766390561861,-53.8771919737007,
12.));
#76541=CARTESIAN_POINT('Ctrl Pts',(-50.567586018852,-53.8516317071783,12.));
#76542=CARTESIAN_POINT('Ctrl Pts',(-50.5585216854082,-53.8261136593064,
12.));
#76543=CARTESIAN_POINT('Ctrl Pts',(-50.5494461285762,-53.8006378970198,
12.));
#76544=CARTESIAN_POINT('Ctrl Pts',(-50.5403594216706,-53.7752044876313,
12.));
#76545=CARTESIAN_POINT('Ctrl Pts',(-50.5312616390789,-53.7498134991714,
12.));
#76546=CARTESIAN_POINT('Ctrl Pts',(-50.5221528560427,-53.7244650002382,
12.));
#76547=CARTESIAN_POINT('Ctrl Pts',(-50.5130331484563,-53.6991590598551,
12.));
#76548=CARTESIAN_POINT('Ctrl Pts',(-50.5039025926531,-53.6738957473158,
12.));
#76549=CARTESIAN_POINT('Ctrl Pts',(-50.4947612652147,-53.6486751320434,
12.));
#76550=CARTESIAN_POINT('Ctrl Pts',(-50.485609242731,-53.6234972834055,12.));
#76551=CARTESIAN_POINT('Ctrl Pts',(-50.4764466018064,-53.5983622707231,
12.));
#76552=CARTESIAN_POINT('Ctrl Pts',(-50.467273419175,-53.5732701633603,12.));
#76553=CARTESIAN_POINT('Ctrl Pts',(-50.4580897717835,-53.5482210307864,
12.));
#76554=CARTESIAN_POINT('Ctrl Pts',(-50.4488957368841,-53.5232149426415,
12.));
#76555=CARTESIAN_POINT('Ctrl Pts',(-50.4396913921389,-53.4982519688032,
12.));
#76556=CARTESIAN_POINT('Ctrl Pts',(-50.4304768156677,-53.4733321794199,
12.));
#76557=CARTESIAN_POINT('Ctrl Pts',(-50.4212520859924,-53.4484556448787,
12.));
#76558=CARTESIAN_POINT('Ctrl Pts',(-50.4120172820054,-53.4236224357846,
12.));
#76559=CARTESIAN_POINT('Ctrl Pts',(-50.4027724829296,-53.3988326229308,
12.));
#76560=CARTESIAN_POINT('Ctrl Pts',(-50.393517768283,-53.3740862772673,12.));
#76561=CARTESIAN_POINT('Ctrl Pts',(-50.3842532178451,-53.3493834698685,
12.));
#76562=CARTESIAN_POINT('Ctrl Pts',(-50.3749789116777,-53.3247242719575,
12.));
#76563=CARTESIAN_POINT('Ctrl Pts',(-50.3656949301424,-53.3001087549222,
12.));
#76564=CARTESIAN_POINT('Ctrl Pts',(-50.3564013539198,-53.2755369903291,
12.));
#76565=CARTESIAN_POINT('Ctrl Pts',(-50.3470982640294,-53.2510090499341,
12.));
#76566=CARTESIAN_POINT('Ctrl Pts',(-50.3377857418522,-53.2265250056896,
12.));
#76567=CARTESIAN_POINT('Ctrl Pts',(-50.3284638691285,-53.202084929748,12.));
#76568=CARTESIAN_POINT('Ctrl Pts',(-50.3191327279497,-53.1776888944622,
12.));
#76569=CARTESIAN_POINT('Ctrl Pts',(-50.3097924007536,-53.153336972382,12.));
#76570=CARTESIAN_POINT('Ctrl Pts',(-50.3004429703188,-53.1290292362482,
12.));
#76571=CARTESIAN_POINT('Ctrl Pts',(-50.2910845197615,-53.1047657589806,
12.));
#76572=CARTESIAN_POINT('Ctrl Pts',(-50.2817171325354,-53.0805466136791,
12.));
#76573=CARTESIAN_POINT('Ctrl Pts',(-50.272340892437,-53.0563718736361,12.));
#76574=CARTESIAN_POINT('Ctrl Pts',(-50.262955883611,-53.0322416123404,12.));
#76575=CARTESIAN_POINT('Ctrl Pts',(-50.2535621905553,-53.0081559034802,
12.));
#76576=CARTESIAN_POINT('Ctrl Pts',(-50.2441598981286,-52.9841148209404,
12.));
#76577=CARTESIAN_POINT('Ctrl Pts',(-50.2347490915553,-52.9601184388027,
12.));
#76578=CARTESIAN_POINT('Ctrl Pts',(-50.2253298564237,-52.9361668313539,
12.));
#76579=CARTESIAN_POINT('Ctrl Pts',(-50.2159022786876,-52.9122600730882,
12.));
#76580=CARTESIAN_POINT('Ctrl Pts',(-50.2064664446663,-52.8883982387068,
12.));
#76581=CARTESIAN_POINT('Ctrl Pts',(-50.1970224410476,-52.8645814031137,
12.));
#76582=CARTESIAN_POINT('Ctrl Pts',(-50.1875703548893,-52.8408096414101,
12.));
#76583=CARTESIAN_POINT('Ctrl Pts',(-50.1781102736215,-52.8170830289052,
12.));
#76584=CARTESIAN_POINT('Ctrl Pts',(-50.1686422850493,-52.793401641121,12.));
#76585=CARTESIAN_POINT('Ctrl Pts',(-50.1591664773561,-52.769765553794,12.));
#76586=CARTESIAN_POINT('Ctrl Pts',(-50.1496829391068,-52.7461748428733,
12.));
#76587=CARTESIAN_POINT('Ctrl Pts',(-50.1401917592532,-52.7226295845156,
12.));
#76588=CARTESIAN_POINT('Ctrl Pts',(-50.1306930271343,-52.6991298550928,
12.));
#76589=CARTESIAN_POINT('Ctrl Pts',(-50.1211868324781,-52.6756757311979,
12.));
#76590=CARTESIAN_POINT('Ctrl Pts',(-50.1116732654041,-52.6522672896462,
12.));
#76591=CARTESIAN_POINT('Ctrl Pts',(-50.1021524164261,-52.6289046074743,
12.));
#76592=CARTESIAN_POINT('Ctrl Pts',(-50.0926243764569,-52.6055877619338,
12.));
#76593=CARTESIAN_POINT('Ctrl Pts',(-50.0830892368095,-52.5823168304981,
12.));
#76594=CARTESIAN_POINT('Ctrl Pts',(-50.0735470891996,-52.5590918908691,
12.));
#76595=CARTESIAN_POINT('Ctrl Pts',(-50.0639980257477,-52.5359130209789,
12.));
#76596=CARTESIAN_POINT('Ctrl Pts',(-50.0544421389824,-52.5127802989903,
12.));
#76597=CARTESIAN_POINT('Ctrl Pts',(-50.0448795218453,-52.4896938032896,
12.));
#76598=CARTESIAN_POINT('Ctrl Pts',(-50.0353102676933,-52.4666536124926,
12.));
#76599=CARTESIAN_POINT('Ctrl Pts',(-50.0257344703008,-52.4436598054523,
12.));
#76600=CARTESIAN_POINT('Ctrl Pts',(-50.0161522238619,-52.420712461261,12.));
#76601=CARTESIAN_POINT('Ctrl Pts',(-50.0065636229934,-52.3978116592505,
12.));
#76602=CARTESIAN_POINT('Ctrl Pts',(-49.9969687627402,-52.3749574789865,
12.));
#76603=CARTESIAN_POINT('Ctrl Pts',(-49.9873677385769,-52.3521500002711,
12.));
#76604=CARTESIAN_POINT('Ctrl Pts',(-49.9777606464103,-52.3293893031524,
12.));
#76605=CARTESIAN_POINT('Ctrl Pts',(-49.9681475825824,-52.3066754679265,
12.));
#76606=CARTESIAN_POINT('Ctrl Pts',(-49.9585286438734,-52.2840085751385,
12.));
#76607=CARTESIAN_POINT('Ctrl Pts',(-49.9489039275064,-52.2613887055773,
12.));
#76608=CARTESIAN_POINT('Ctrl Pts',(-49.9392735311507,-52.238815940277,12.));
#76609=CARTESIAN_POINT('Ctrl Pts',(-49.9296375529241,-52.2162903605272,
12.));
#76610=CARTESIAN_POINT('Ctrl Pts',(-49.919996091396,-52.1938120478752,12.));
#76611=CARTESIAN_POINT('Ctrl Pts',(-49.9103492455904,-52.1713810841277,
12.));
#76612=CARTESIAN_POINT('Ctrl Pts',(-49.90069711499,-52.1489975513449,12.));
#76613=CARTESIAN_POINT('Ctrl Pts',(-49.8910397995404,-52.1266615318414,
12.));
#76614=CARTESIAN_POINT('Ctrl Pts',(-49.8813773996523,-52.1043731081968,
12.));
#76615=CARTESIAN_POINT('Ctrl Pts',(-49.871710016205,-52.0821323632588,12.));
#76616=CARTESIAN_POINT('Ctrl Pts',(-49.8620377505498,-52.059939380145,12.));
#76617=CARTESIAN_POINT('Ctrl Pts',(-49.8523607045146,-52.0377942422373,
12.));
#76618=CARTESIAN_POINT('Ctrl Pts',(-49.8426789804068,-52.015697033182,12.));
#76619=CARTESIAN_POINT('Ctrl Pts',(-49.8329926810172,-51.9936478369008,
12.));
#76620=CARTESIAN_POINT('Ctrl Pts',(-49.8233019096224,-51.9716467375938,
12.));
#76621=CARTESIAN_POINT('Ctrl Pts',(-49.8136067699896,-51.9496938197418,
12.));
#76622=CARTESIAN_POINT('Ctrl Pts',(-49.8039073663808,-51.9277891681014,
12.));
#76623=CARTESIAN_POINT('Ctrl Pts',(-49.7942038035568,-51.9059328677051,
12.));
#76624=CARTESIAN_POINT('Ctrl Pts',(-49.78449618678,-51.8841250038716,12.));
#76625=CARTESIAN_POINT('Ctrl Pts',(-49.7747846218177,-51.8623656622092,
12.));
#76626=CARTESIAN_POINT('Ctrl Pts',(-49.7650692149464,-51.8406549286177,
12.));
#76627=CARTESIAN_POINT('Ctrl Pts',(-49.7553500729563,-51.8189928892841,
12.));
#76628=CARTESIAN_POINT('Ctrl Pts',(-49.7456273031555,-51.7973796306826,
12.));
#76629=CARTESIAN_POINT('Ctrl Pts',(-49.7359010133741,-51.7758152395857,
12.));
#76630=CARTESIAN_POINT('Ctrl Pts',(-49.7261713119672,-51.754299803068,12.));
#76631=CARTESIAN_POINT('Ctrl Pts',(-49.7164383078206,-51.7328334085084,
12.));
#76632=CARTESIAN_POINT('Ctrl Pts',(-49.7067021103534,-51.7114161435848,
12.));
#76633=CARTESIAN_POINT('Ctrl Pts',(-49.6969628295236,-51.6900480962744,
12.));
#76634=CARTESIAN_POINT('Ctrl Pts',(-49.6872205758314,-51.6687293548656,
12.));
#76635=CARTESIAN_POINT('Ctrl Pts',(-49.6774754603235,-51.6474600079611,
12.));
#76636=CARTESIAN_POINT('Ctrl Pts',(-49.6677275945975,-51.6262401444799,
12.));
#76637=CARTESIAN_POINT('Ctrl Pts',(-49.6579770908063,-51.6050698536525,
12.));
#76638=CARTESIAN_POINT('Ctrl Pts',(-49.6482240616627,-51.5839492250218,
12.));
#76639=CARTESIAN_POINT('Ctrl Pts',(-49.6384686204443,-51.5628783484556,
12.));
#76640=CARTESIAN_POINT('Ctrl Pts',(-49.6287108809975,-51.5418573141494,
12.));
#76641=CARTESIAN_POINT('Ctrl Pts',(-49.6189509577441,-51.5208862126303,
12.));
#76642=CARTESIAN_POINT('Ctrl Pts',(-49.609188965684,-51.4999651347496,12.));
#76643=CARTESIAN_POINT('Ctrl Pts',(-49.5994250204003,-51.4790941716859,
12.));
#76644=CARTESIAN_POINT('Ctrl Pts',(-49.5896592380634,-51.4582734149562,
12.));
#76645=CARTESIAN_POINT('Ctrl Pts',(-49.579891735436,-51.4375029564191,12.));
#76646=CARTESIAN_POINT('Ctrl Pts',(-49.5701226298779,-51.4167828882765,
12.));
#76647=CARTESIAN_POINT('Ctrl Pts',(-49.5603520393514,-51.3961133030688,
12.));
#76648=CARTESIAN_POINT('Ctrl Pts',(-49.5505800824268,-51.3754942936796,
12.));
#76649=CARTESIAN_POINT('Ctrl Pts',(-49.5408068782871,-51.354925953347,12.));
#76650=CARTESIAN_POINT('Ctrl Pts',(-49.5310325467334,-51.3344083756659,
12.));
#76651=CARTESIAN_POINT('Ctrl Pts',(-49.5212572081901,-51.3139416545903,
12.));
#76652=CARTESIAN_POINT('Ctrl Pts',(-49.5114809837111,-51.2935258844278,
12.));
#76653=CARTESIAN_POINT('Ctrl Pts',(-49.5017039949841,-51.2731611598465,
12.));
#76654=CARTESIAN_POINT('Ctrl Pts',(-49.4919263643357,-51.2528475758841,
12.));
#76655=CARTESIAN_POINT('Ctrl Pts',(-49.4821482147357,-51.2325852279507,
12.));
#76656=CARTESIAN_POINT('Ctrl Pts',(-49.4723696698022,-51.2123742118288,
12.));
#76657=CARTESIAN_POINT('Ctrl Pts',(-49.4625908538076,-51.1922146236686,
12.));
#76658=CARTESIAN_POINT('Ctrl Pts',(-49.4528118916833,-51.1721065599972,
12.));
#76659=CARTESIAN_POINT('Ctrl Pts',(-49.4430329090288,-51.1520501177291,
12.));
#76660=CARTESIAN_POINT('Ctrl Pts',(-49.4332540321178,-51.1320453941702,
12.));
#76661=CARTESIAN_POINT('Ctrl Pts',(-49.4234753879071,-51.1120924870196,
12.));
#76662=CARTESIAN_POINT('Ctrl Pts',(-49.4136971040428,-51.0921914943663,
12.));
#76663=CARTESIAN_POINT('Ctrl Pts',(-49.4039193088636,-51.0723425146987,
12.));
#76664=CARTESIAN_POINT('Ctrl Pts',(-49.3941421314014,-51.0525456469072,
12.));
#76665=CARTESIAN_POINT('Ctrl Pts',(-49.3843657013851,-51.0328009902857,
12.));
#76666=CARTESIAN_POINT('Ctrl Pts',(-49.3745901492429,-51.0131086445268,
12.));
#76667=CARTESIAN_POINT('Ctrl Pts',(-49.3648156061049,-50.9934687097179,
12.));
#76668=CARTESIAN_POINT('Ctrl Pts',(-49.3550422038221,-50.9738812863636,
12.));
#76669=CARTESIAN_POINT('Ctrl Pts',(-49.3452700749804,-50.9543464753974,
12.));
#76670=CARTESIAN_POINT('Ctrl Pts',(-49.3354993529163,-50.9348643781928,
12.));
#76671=CARTESIAN_POINT('Ctrl Pts',(-49.325730171735,-50.9154350965681,12.));
#76672=CARTESIAN_POINT('Ctrl Pts',(-49.3159626663129,-50.8960587327869,
12.));
#76673=CARTESIAN_POINT('Ctrl Pts',(-49.3061969722798,-50.8767353895509,
12.));
#76674=CARTESIAN_POINT('Ctrl Pts',(-49.2964332260043,-50.8574651699877,
12.));
#76675=CARTESIAN_POINT('Ctrl Pts',(-49.2866715645828,-50.8382481776392,
12.));
#76676=CARTESIAN_POINT('Ctrl Pts',(-49.2769121258144,-50.8190845164319,
12.));
#76677=CARTESIAN_POINT('Ctrl Pts',(-49.2671550482415,-50.7999742907111,
12.));
#76678=CARTESIAN_POINT('Ctrl Pts',(-49.2574004712122,-50.7809176052954,
12.));
#76679=CARTESIAN_POINT('Ctrl Pts',(-49.2476485349373,-50.7619145655207,
12.));
#76680=CARTESIAN_POINT('Ctrl Pts',(-49.2378993805482,-50.7429652772816,
12.));
#76681=CARTESIAN_POINT('Ctrl Pts',(-49.2281531501569,-50.7240698470698,
12.));
#76682=CARTESIAN_POINT('Ctrl Pts',(-49.218409986748,-50.7052283818941,12.));
#76683=CARTESIAN_POINT('Ctrl Pts',(-49.2086700340625,-50.6864409891905,
12.));
#76684=CARTESIAN_POINT('Ctrl Pts',(-49.1989334364992,-50.6677077767427,
12.));
#76685=CARTESIAN_POINT('Ctrl Pts',(-49.1892003389743,-50.6490288525639,
12.));
#76686=CARTESIAN_POINT('Ctrl Pts',(-49.1794708869074,-50.6304043248796,
12.));
#76687=CARTESIAN_POINT('Ctrl Pts',(-49.1697452265473,-50.6118343023937,
12.));
#76688=CARTESIAN_POINT('Ctrl Pts',(-49.1600235052613,-50.593318894516,12.));
#76689=CARTESIAN_POINT('Ctrl Pts',(-49.1503058717831,-50.5748582115575,
12.));
#76690=CARTESIAN_POINT('Ctrl Pts',(-49.1405924766169,-50.5564523650406,
12.));
#76691=CARTESIAN_POINT('Ctrl Pts',(-49.1308834717645,-50.5381014674822,
12.));
#76692=CARTESIAN_POINT('Ctrl Pts',(-49.1211790099817,-50.5198056318111,
12.));
#76693=CARTESIAN_POINT('Ctrl Pts',(-49.1114792441573,-50.5015649708742,
12.));
#76694=CARTESIAN_POINT('Ctrl Pts',(-49.1017843266782,-50.4833795969296,
12.));
#76695=CARTESIAN_POINT('Ctrl Pts',(-49.0920944086973,-50.465249621057,12.));
#76696=CARTESIAN_POINT('Ctrl Pts',(-49.0824096415339,-50.4471751542717,
12.));
#76697=CARTESIAN_POINT('Ctrl Pts',(-49.0727301783477,-50.4291563088528,
12.));
#76698=CARTESIAN_POINT('Ctrl Pts',(-49.0630561755082,-50.4111931994264,
12.));
#76699=CARTESIAN_POINT('Ctrl Pts',(-49.0533877945771,-50.393285944528,12.));
#76700=CARTESIAN_POINT('Ctrl Pts',(-49.0437252024868,-50.3754346667389,
12.));
#76701=CARTESIAN_POINT('Ctrl Pts',(-49.034068567401,-50.3576394894136,12.));
#76702=CARTESIAN_POINT('Ctrl Pts',(-49.0244180550759,-50.3399005337967,
12.));
#76703=CARTESIAN_POINT('Ctrl Pts',(-49.0147738256925,-50.3222179165102,
12.));
#76704=CARTESIAN_POINT('Ctrl Pts',(-49.0051360288002,-50.3045917455383,
12.));
#76705=CARTESIAN_POINT('Ctrl Pts',(-48.9955048082028,-50.2870221241003,
12.));
#76706=CARTESIAN_POINT('Ctrl Pts',(-48.9858803116649,-50.2695091583473,
12.));
#76707=CARTESIAN_POINT('Ctrl Pts',(-48.9762626987227,-50.252052963548,12.));
#76708=CARTESIAN_POINT('Ctrl Pts',(-48.9666521500969,-50.2346536715465,
12.));
#76709=CARTESIAN_POINT('Ctrl Pts',(-48.9570488741273,-50.2173114358423,
12.));
#76710=CARTESIAN_POINT('Ctrl Pts',(-48.9474530868847,-50.2000264157903,
12.));
#76711=CARTESIAN_POINT('Ctrl Pts',(-48.9378649933116,-50.1827987615659,
12.));
#76712=CARTESIAN_POINT('Ctrl Pts',(-48.9282847698237,-50.1656286003943,
12.));
#76713=CARTESIAN_POINT('Ctrl Pts',(-48.9187125417897,-50.148516018447,12.));
#76714=CARTESIAN_POINT('Ctrl Pts',(-48.9091483817797,-50.1314610602286,
12.));
#76715=CARTESIAN_POINT('Ctrl Pts',(-48.9015035371772,-50.1178632066821,
12.));
#76716=CARTESIAN_POINT('Ctrl Pts',(-48.8957735556681,-50.1076907555303,
12.));
#76717=CARTESIAN_POINT('Ctrl Pts',(-48.8919551910299,-50.1009206494209,
12.));
#76718=CARTESIAN_POINT('Ctrl Pts',(-48.8900464144686,-50.0975384783634,
12.));
#76719=CARTESIAN_POINT('Ctrl Pts',(-49.5707719660638,-55.2174072001495,
0.));
#76720=CARTESIAN_POINT('Ctrl Pts',(-49.5707719660638,-55.2174072001495,
4.));
#76721=CARTESIAN_POINT('Ctrl Pts',(-49.5707719660638,-55.2174072001495,
8.));
#76722=CARTESIAN_POINT('Ctrl Pts',(-49.5707719660638,-55.2174072001495,
12.));
#76723=CARTESIAN_POINT('Ctrl Pts',(-49.6712810246932,-55.2618153697169,
0.));
#76724=CARTESIAN_POINT('Ctrl Pts',(-49.6712810246932,-55.2618153697169,
4.));
#76725=CARTESIAN_POINT('Ctrl Pts',(-49.6712810246932,-55.2618153697169,
8.));
#76726=CARTESIAN_POINT('Ctrl Pts',(-49.6712810246932,-55.2618153697169,
12.));
#76727=CARTESIAN_POINT('Ctrl Pts',(-49.8732090625341,-55.2790667815473,
0.));
#76728=CARTESIAN_POINT('Ctrl Pts',(-49.8732090625341,-55.2790667815473,
4.));
#76729=CARTESIAN_POINT('Ctrl Pts',(-49.8732090625341,-55.2790667815473,
7.99999999999999));
#76730=CARTESIAN_POINT('Ctrl Pts',(-49.8732090625341,-55.2790667815473,
12.));
#76731=CARTESIAN_POINT('Ctrl Pts',(-50.0481613529516,-55.1854902750885,
0.));
#76732=CARTESIAN_POINT('Ctrl Pts',(-50.0481613529516,-55.1854902750885,
4.));
#76733=CARTESIAN_POINT('Ctrl Pts',(-50.0481613529516,-55.1854902750885,
8.00000000000001));
#76734=CARTESIAN_POINT('Ctrl Pts',(-50.0481613529516,-55.1854902750885,
12.));
#76735=CARTESIAN_POINT('Ctrl Pts',(-50.1091461876225,-55.1300595714123,
0.));
#76736=CARTESIAN_POINT('Ctrl Pts',(-50.1091461876225,-55.1300595714123,
4.));
#76737=CARTESIAN_POINT('Ctrl Pts',(-50.1091461876225,-55.1300595714123,
8.));
#76738=CARTESIAN_POINT('Ctrl Pts',(-50.1091461876225,-55.1300595714123,
12.));
#76739=CARTESIAN_POINT('',(-49.5707719660638,-55.2174072001495,0.));
#76740=CARTESIAN_POINT('',(-50.1091461876226,-55.1300595714123,0.));
#76741=CARTESIAN_POINT('Ctrl Pts',(-49.5707719660638,-55.2174072001495,
2.77555756156289E-16));
#76742=CARTESIAN_POINT('Ctrl Pts',(-49.6712810246932,-55.2618153697169,
2.77555756156289E-16));
#76743=CARTESIAN_POINT('Ctrl Pts',(-49.786668474888,-55.2716733193343,2.77555756156289E-16));
#76744=CARTESIAN_POINT('Ctrl Pts',(-49.8932475177609,-55.2453425609388,
2.77555756156289E-16));
#76745=CARTESIAN_POINT('Ctrl Pts',(-49.9731817999155,-55.2255944921423,
2.77555756156289E-16));
#76746=CARTESIAN_POINT('Ctrl Pts',(-50.0481613529516,-55.1854902750885,
2.77555756156289E-16));
#76747=CARTESIAN_POINT('Ctrl Pts',(-50.1091461876225,-55.1300595714123,
2.77555756156289E-16));
#76748=CARTESIAN_POINT('',(-50.1091461876226,-55.1300595714123,12.));
#76749=CARTESIAN_POINT('Ctrl Pts',(-50.1091461876225,-55.1300595714123,
0.));
#76750=CARTESIAN_POINT('Ctrl Pts',(-50.1091461876225,-55.1300595714123,
4.));
#76751=CARTESIAN_POINT('Ctrl Pts',(-50.1091461876225,-55.1300595714123,
8.));
#76752=CARTESIAN_POINT('Ctrl Pts',(-50.1091461876225,-55.1300595714123,
12.));
#76753=CARTESIAN_POINT('',(-49.5707719660638,-55.2174072001495,12.));
#76754=CARTESIAN_POINT('Ctrl Pts',(-50.1091461876225,-55.1300595714123,
12.));
#76755=CARTESIAN_POINT('Ctrl Pts',(-50.0481613529516,-55.1854902750885,
12.));
#76756=CARTESIAN_POINT('Ctrl Pts',(-49.9731817999155,-55.2255944921423,
12.));
#76757=CARTESIAN_POINT('Ctrl Pts',(-49.8932475177609,-55.2453425609389,
12.));
#76758=CARTESIAN_POINT('Ctrl Pts',(-49.786668474888,-55.2716733193343,12.));
#76759=CARTESIAN_POINT('Ctrl Pts',(-49.6712810246932,-55.2618153697169,
12.));
#76760=CARTESIAN_POINT('Ctrl Pts',(-49.5707719660638,-55.2174072001495,
12.));
#76761=CARTESIAN_POINT('Ctrl Pts',(-49.5707719660638,-55.2174072001495,
12.));
#76762=CARTESIAN_POINT('Ctrl Pts',(-49.5707719660638,-55.2174072001495,
8.));
#76763=CARTESIAN_POINT('Ctrl Pts',(-49.5707719660638,-55.2174072001495,
4.));
#76764=CARTESIAN_POINT('Ctrl Pts',(-49.5707719660638,-55.2174072001495,
0.));
#76765=CARTESIAN_POINT('Origin',(-2.53167595884892E-10,-2.7643087079898E-10,
0.));
#76766=CARTESIAN_POINT('Origin',(-2.53167595884892E-10,-2.7643087079898E-10,
12.));
#76767=CARTESIAN_POINT('Origin',(-2.53167595884892E-10,-2.7643087079898E-10,
0.));
#76768=CARTESIAN_POINT('Ctrl Pts',(-55.1300595714105,-50.1091461876246,
0.));
#76769=CARTESIAN_POINT('Ctrl Pts',(-55.1300595714105,-50.1091461876246,
4.));
#76770=CARTESIAN_POINT('Ctrl Pts',(-55.1300595714105,-50.1091461876246,
8.));
#76771=CARTESIAN_POINT('Ctrl Pts',(-55.1300595714105,-50.1091461876246,
12.));
#76772=CARTESIAN_POINT('Ctrl Pts',(-55.2039671763178,-50.0278330747237,
0.));
#76773=CARTESIAN_POINT('Ctrl Pts',(-55.2039671763178,-50.0278330747237,
4.));
#76774=CARTESIAN_POINT('Ctrl Pts',(-55.2039671763178,-50.0278330747237,
8.));
#76775=CARTESIAN_POINT('Ctrl Pts',(-55.2039671763178,-50.0278330747237,
12.));
#76776=CARTESIAN_POINT('Ctrl Pts',(-55.2841761056306,-49.8417173275612,
0.));
#76777=CARTESIAN_POINT('Ctrl Pts',(-55.2841761056306,-49.8417173275612,
4.));
#76778=CARTESIAN_POINT('Ctrl Pts',(-55.2841761056306,-49.8417173275612,
7.99999999999999));
#76779=CARTESIAN_POINT('Ctrl Pts',(-55.2841761056306,-49.8417173275612,
12.));
#76780=CARTESIAN_POINT('Ctrl Pts',(-55.2507133273147,-49.6461537600002,
0.));
#76781=CARTESIAN_POINT('Ctrl Pts',(-55.2507133273147,-49.6461537600002,
4.));
#76782=CARTESIAN_POINT('Ctrl Pts',(-55.2507133273147,-49.6461537600002,
8.00000000000001));
#76783=CARTESIAN_POINT('Ctrl Pts',(-55.2507133273147,-49.6461537600002,
12.));
#76784=CARTESIAN_POINT('Ctrl Pts',(-55.21740720013,-49.5707719660253,0.));
#76785=CARTESIAN_POINT('Ctrl Pts',(-55.21740720013,-49.5707719660253,4.));
#76786=CARTESIAN_POINT('Ctrl Pts',(-55.21740720013,-49.5707719660253,8.));
#76787=CARTESIAN_POINT('Ctrl Pts',(-55.21740720013,-49.5707719660253,12.));
#76788=CARTESIAN_POINT('',(-55.1300595714105,-50.1091461876246,0.));
#76789=CARTESIAN_POINT('',(-55.2174072001297,-49.5707719660254,0.));
#76790=CARTESIAN_POINT('Ctrl Pts',(-55.1300595714105,-50.1091461876246,
1.38777878078145E-16));
#76791=CARTESIAN_POINT('Ctrl Pts',(-55.2039671763178,-50.0278330747237,
1.38777878078145E-16));
#76792=CARTESIAN_POINT('Ctrl Pts',(-55.2498008502108,-49.9214812192023,
1.38777878078145E-16));
#76793=CARTESIAN_POINT('Ctrl Pts',(-55.2585172318169,-49.8120443611017,
1.38777878078145E-16));
#76794=CARTESIAN_POINT('Ctrl Pts',(-55.2650545180215,-49.7299667175263,
1.38777878078145E-16));
#76795=CARTESIAN_POINT('Ctrl Pts',(-55.2507133273147,-49.6461537600002,
1.38777878078144E-16));
#76796=CARTESIAN_POINT('Ctrl Pts',(-55.21740720013,-49.5707719660253,1.38777878078145E-16));
#76797=CARTESIAN_POINT('',(-55.2174072001297,-49.5707719660254,12.));
#76798=CARTESIAN_POINT('Ctrl Pts',(-55.21740720013,-49.5707719660253,0.));
#76799=CARTESIAN_POINT('Ctrl Pts',(-55.21740720013,-49.5707719660253,4.));
#76800=CARTESIAN_POINT('Ctrl Pts',(-55.21740720013,-49.5707719660253,8.));
#76801=CARTESIAN_POINT('Ctrl Pts',(-55.21740720013,-49.5707719660253,12.));
#76802=CARTESIAN_POINT('',(-55.1300595714105,-50.1091461876246,12.));
#76803=CARTESIAN_POINT('Ctrl Pts',(-55.21740720013,-49.5707719660253,12.));
#76804=CARTESIAN_POINT('Ctrl Pts',(-55.2507133273147,-49.6461537600002,
12.));
#76805=CARTESIAN_POINT('Ctrl Pts',(-55.2650545180215,-49.7299667175263,
12.));
#76806=CARTESIAN_POINT('Ctrl Pts',(-55.2585172318169,-49.8120443611017,
12.));
#76807=CARTESIAN_POINT('Ctrl Pts',(-55.2498008502108,-49.9214812192023,
12.));
#76808=CARTESIAN_POINT('Ctrl Pts',(-55.2039671763178,-50.0278330747237,
12.));
#76809=CARTESIAN_POINT('Ctrl Pts',(-55.1300595714105,-50.1091461876246,
12.));
#76810=CARTESIAN_POINT('Ctrl Pts',(-55.1300595714105,-50.1091461876246,
12.));
#76811=CARTESIAN_POINT('Ctrl Pts',(-55.1300595714105,-50.1091461876246,
8.));
#76812=CARTESIAN_POINT('Ctrl Pts',(-55.1300595714105,-50.1091461876246,
4.));
#76813=CARTESIAN_POINT('Ctrl Pts',(-55.1300595714105,-50.1091461876246,
0.));
#76814=CARTESIAN_POINT('Ctrl Pts',(-53.0702932034641,-45.6458539113724,
0.));
#76815=CARTESIAN_POINT('Ctrl Pts',(-53.0702932034641,-45.6458539113724,
12.));
#76816=CARTESIAN_POINT('Ctrl Pts',(-53.0724894921849,-45.6490568514089,
0.));
#76817=CARTESIAN_POINT('Ctrl Pts',(-53.0724894921849,-45.6490568514089,
12.));
#76818=CARTESIAN_POINT('Ctrl Pts',(-53.0768833804193,-45.6554684028145,
0.));
#76819=CARTESIAN_POINT('Ctrl Pts',(-53.0768833804193,-45.6554684028145,
12.));
#76820=CARTESIAN_POINT('Ctrl Pts',(-53.0834781451546,-45.6651027439241,
0.));
#76821=CARTESIAN_POINT('Ctrl Pts',(-53.0834781451546,-45.6651027439241,
12.));
#76822=CARTESIAN_POINT('Ctrl Pts',(-53.0922790298409,-45.6779825614231,
0.));
#76823=CARTESIAN_POINT('Ctrl Pts',(-53.0922790298409,-45.6779825614231,
12.));
#76824=CARTESIAN_POINT('Ctrl Pts',(-53.1032932328857,-45.694139048907,0.));
#76825=CARTESIAN_POINT('Ctrl Pts',(-53.1032932328857,-45.694139048907,12.));
#76826=CARTESIAN_POINT('Ctrl Pts',(-53.114320495492,-45.7103522376696,0.));
#76827=CARTESIAN_POINT('Ctrl Pts',(-53.114320495492,-45.7103522376696,12.));
#76828=CARTESIAN_POINT('Ctrl Pts',(-53.1253607414872,-45.7266220897003,
0.));
#76829=CARTESIAN_POINT('Ctrl Pts',(-53.1253607414872,-45.7266220897003,
12.));
#76830=CARTESIAN_POINT('Ctrl Pts',(-53.1364138384693,-45.7429485300823,
0.));
#76831=CARTESIAN_POINT('Ctrl Pts',(-53.1364138384693,-45.7429485300823,
12.));
#76832=CARTESIAN_POINT('Ctrl Pts',(-53.1474795996053,-45.7593314474501,
0.));
#76833=CARTESIAN_POINT('Ctrl Pts',(-53.1474795996053,-45.7593314474501,
12.));
#76834=CARTESIAN_POINT('Ctrl Pts',(-53.1585578076444,-45.7757707100618,
0.));
#76835=CARTESIAN_POINT('Ctrl Pts',(-53.1585578076444,-45.7757707100618,
12.));
#76836=CARTESIAN_POINT('Ctrl Pts',(-53.1696482334487,-45.7922661780005,
0.));
#76837=CARTESIAN_POINT('Ctrl Pts',(-53.1696482334487,-45.7922661780005,
12.));
#76838=CARTESIAN_POINT('Ctrl Pts',(-53.1807506560933,-45.808817716509,0.));
#76839=CARTESIAN_POINT('Ctrl Pts',(-53.1807506560933,-45.808817716509,12.));
#76840=CARTESIAN_POINT('Ctrl Pts',(-53.1918648840541,-45.8254252099957,
0.));
#76841=CARTESIAN_POINT('Ctrl Pts',(-53.1918648840541,-45.8254252099957,
12.));
#76842=CARTESIAN_POINT('Ctrl Pts',(-53.2029907483557,-45.8420885575349,
0.));
#76843=CARTESIAN_POINT('Ctrl Pts',(-53.2029907483557,-45.8420885575349,
12.));
#76844=CARTESIAN_POINT('Ctrl Pts',(-53.2141280925439,-45.8588076662582,
0.));
#76845=CARTESIAN_POINT('Ctrl Pts',(-53.2141280925439,-45.8588076662582,
12.));
#76846=CARTESIAN_POINT('Ctrl Pts',(-53.2252767643662,-45.8755824458723,
0.));
#76847=CARTESIAN_POINT('Ctrl Pts',(-53.2252767643662,-45.8755824458723,
12.));
#76848=CARTESIAN_POINT('Ctrl Pts',(-53.2364366054306,-45.892412801838,0.));
#76849=CARTESIAN_POINT('Ctrl Pts',(-53.2364366054306,-45.892412801838,12.));
#76850=CARTESIAN_POINT('Ctrl Pts',(-53.2476074460017,-45.9092986319377,
0.));
#76851=CARTESIAN_POINT('Ctrl Pts',(-53.2476074460017,-45.9092986319377,
12.));
#76852=CARTESIAN_POINT('Ctrl Pts',(-53.2587891103866,-45.9262398298349,
0.));
#76853=CARTESIAN_POINT('Ctrl Pts',(-53.2587891103866,-45.9262398298349,
12.));
#76854=CARTESIAN_POINT('Ctrl Pts',(-53.2699814203105,-45.9432362873008,
0.));
#76855=CARTESIAN_POINT('Ctrl Pts',(-53.2699814203105,-45.9432362873008,
12.));
#76856=CARTESIAN_POINT('Ctrl Pts',(-53.2811841987926,-45.9602878967698,
0.));
#76857=CARTESIAN_POINT('Ctrl Pts',(-53.2811841987926,-45.9602878967698,
12.));
#76858=CARTESIAN_POINT('Ctrl Pts',(-53.292397274555,-45.9773945542384,0.));
#76859=CARTESIAN_POINT('Ctrl Pts',(-53.292397274555,-45.9773945542384,12.));
#76860=CARTESIAN_POINT('Ctrl Pts',(-53.3036204818329,-45.9945561591453,
0.));
#76861=CARTESIAN_POINT('Ctrl Pts',(-53.3036204818329,-45.9945561591453,
12.));
#76862=CARTESIAN_POINT('Ctrl Pts',(-53.3148536582635,-46.0117726129873,
0.));
#76863=CARTESIAN_POINT('Ctrl Pts',(-53.3148536582635,-46.0117726129873,
12.));
#76864=CARTESIAN_POINT('Ctrl Pts',(-53.326096643428,-46.02904381836,0.));
#76865=CARTESIAN_POINT('Ctrl Pts',(-53.326096643428,-46.02904381836,12.));
#76866=CARTESIAN_POINT('Ctrl Pts',(-53.3373492770671,-46.0463696777801,
0.));
#76867=CARTESIAN_POINT('Ctrl Pts',(-53.3373492770671,-46.0463696777801,
12.));
#76868=CARTESIAN_POINT('Ctrl Pts',(-53.3486113975901,-46.0637500926982,
0.));
#76869=CARTESIAN_POINT('Ctrl Pts',(-53.3486113975901,-46.0637500926982,
12.));
#76870=CARTESIAN_POINT('Ctrl Pts',(-53.3598828428546,-46.0811849640218,
0.));
#76871=CARTESIAN_POINT('Ctrl Pts',(-53.3598828428546,-46.0811849640218,
12.));
#76872=CARTESIAN_POINT('Ctrl Pts',(-53.3711634508437,-46.0986741925656,
0.));
#76873=CARTESIAN_POINT('Ctrl Pts',(-53.3711634508437,-46.0986741925656,
12.));
#76874=CARTESIAN_POINT('Ctrl Pts',(-53.3824530603276,-46.1162176794884,
0.));
#76875=CARTESIAN_POINT('Ctrl Pts',(-53.3824530603276,-46.1162176794884,
12.));
#76876=CARTESIAN_POINT('Ctrl Pts',(-53.3937515116549,-46.1338153268097,
0.));
#76877=CARTESIAN_POINT('Ctrl Pts',(-53.3937515116549,-46.1338153268097,
12.));
#76878=CARTESIAN_POINT('Ctrl Pts',(-53.4050586470436,-46.1514670376012,
0.));
#76879=CARTESIAN_POINT('Ctrl Pts',(-53.4050586470436,-46.1514670376012,
12.));
#76880=CARTESIAN_POINT('Ctrl Pts',(-53.4163743101517,-46.1691727157134,
0.));
#76881=CARTESIAN_POINT('Ctrl Pts',(-53.4163743101517,-46.1691727157134,
12.));
#76882=CARTESIAN_POINT('Ctrl Pts',(-53.4276983458125,-46.1869322656024,
0.));
#76883=CARTESIAN_POINT('Ctrl Pts',(-53.4276983458125,-46.1869322656024,
12.));
#76884=CARTESIAN_POINT('Ctrl Pts',(-53.4390305997274,-46.2047455921286,
0.));
#76885=CARTESIAN_POINT('Ctrl Pts',(-53.4390305997274,-46.2047455921286,
12.));
#76886=CARTESIAN_POINT('Ctrl Pts',(-53.4503709181178,-46.2226126003202,
0.));
#76887=CARTESIAN_POINT('Ctrl Pts',(-53.4503709181178,-46.2226126003202,
12.));
#76888=CARTESIAN_POINT('Ctrl Pts',(-53.4617191477402,-46.2405331953889,
0.));
#76889=CARTESIAN_POINT('Ctrl Pts',(-53.4617191477402,-46.2405331953889,
12.));
#76890=CARTESIAN_POINT('Ctrl Pts',(-53.4730751360371,-46.2585072828353,
0.));
#76891=CARTESIAN_POINT('Ctrl Pts',(-53.4730751360371,-46.2585072828353,
12.));
#76892=CARTESIAN_POINT('Ctrl Pts',(-53.4844387312414,-46.2765347685198,
0.));
#76893=CARTESIAN_POINT('Ctrl Pts',(-53.4844387312414,-46.2765347685198,
12.));
#76894=CARTESIAN_POINT('Ctrl Pts',(-53.4958097825006,-46.2946155587417,
0.));
#76895=CARTESIAN_POINT('Ctrl Pts',(-53.4958097825006,-46.2946155587417,
12.));
#76896=CARTESIAN_POINT('Ctrl Pts',(-53.5071881399911,-46.3127495603098,
0.));
#76897=CARTESIAN_POINT('Ctrl Pts',(-53.5071881399911,-46.3127495603098,
12.));
#76898=CARTESIAN_POINT('Ctrl Pts',(-53.5185736548548,-46.3309366805093,
0.));
#76899=CARTESIAN_POINT('Ctrl Pts',(-53.5185736548548,-46.3309366805093,
12.));
#76900=CARTESIAN_POINT('Ctrl Pts',(-53.5299661791385,-46.3491768270655,
0.));
#76901=CARTESIAN_POINT('Ctrl Pts',(-53.5299661791385,-46.3491768270655,
12.));
#76902=CARTESIAN_POINT('Ctrl Pts',(-53.5413655657327,-46.3674699081046,
0.));
#76903=CARTESIAN_POINT('Ctrl Pts',(-53.5413655657327,-46.3674699081046,
12.));
#76904=CARTESIAN_POINT('Ctrl Pts',(-53.5527716683048,-46.3858158321059,
0.));
#76905=CARTESIAN_POINT('Ctrl Pts',(-53.5527716683048,-46.3858158321059,
12.));
#76906=CARTESIAN_POINT('Ctrl Pts',(-53.5641843412559,-46.4042145078701,
0.));
#76907=CARTESIAN_POINT('Ctrl Pts',(-53.5641843412559,-46.4042145078701,
12.));
#76908=CARTESIAN_POINT('Ctrl Pts',(-53.5756034397481,-46.4226658445474,
0.));
#76909=CARTESIAN_POINT('Ctrl Pts',(-53.5756034397481,-46.4226658445474,
12.));
#76910=CARTESIAN_POINT('Ctrl Pts',(-53.5870288197166,-46.4411697516478,
0.));
#76911=CARTESIAN_POINT('Ctrl Pts',(-53.5870288197166,-46.4411697516478,
12.));
#76912=CARTESIAN_POINT('Ctrl Pts',(-53.5984603378855,-46.459726139052,0.));
#76913=CARTESIAN_POINT('Ctrl Pts',(-53.5984603378855,-46.459726139052,12.));
#76914=CARTESIAN_POINT('Ctrl Pts',(-53.6098978517859,-46.4783349170173,
0.));
#76915=CARTESIAN_POINT('Ctrl Pts',(-53.6098978517859,-46.4783349170173,
12.));
#76916=CARTESIAN_POINT('Ctrl Pts',(-53.6213412197533,-46.496995996177,0.));
#76917=CARTESIAN_POINT('Ctrl Pts',(-53.6213412197533,-46.496995996177,12.));
#76918=CARTESIAN_POINT('Ctrl Pts',(-53.6327903009094,-46.5157092875373,
0.));
#76919=CARTESIAN_POINT('Ctrl Pts',(-53.6327903009094,-46.5157092875373,
12.));
#76920=CARTESIAN_POINT('Ctrl Pts',(-53.6442449551455,-46.5344747024676,
0.));
#76921=CARTESIAN_POINT('Ctrl Pts',(-53.6442449551455,-46.5344747024676,
12.));
#76922=CARTESIAN_POINT('Ctrl Pts',(-53.6557050431071,-46.5532921526901,
0.));
#76923=CARTESIAN_POINT('Ctrl Pts',(-53.6557050431071,-46.5532921526901,
12.));
#76924=CARTESIAN_POINT('Ctrl Pts',(-53.6671704261737,-46.5721615502591,
0.));
#76925=CARTESIAN_POINT('Ctrl Pts',(-53.6671704261737,-46.5721615502591,
12.));
#76926=CARTESIAN_POINT('Ctrl Pts',(-53.678640966456,-46.5910828075653,0.));
#76927=CARTESIAN_POINT('Ctrl Pts',(-53.678640966456,-46.5910828075653,12.));
#76928=CARTESIAN_POINT('Ctrl Pts',(-53.6901165267941,-46.6100558373402,
0.));
#76929=CARTESIAN_POINT('Ctrl Pts',(-53.6901165267941,-46.6100558373402,
12.));
#76930=CARTESIAN_POINT('Ctrl Pts',(-53.701596970754,-46.6290805526559,0.));
#76931=CARTESIAN_POINT('Ctrl Pts',(-53.701596970754,-46.6290805526559,12.));
#76932=CARTESIAN_POINT('Ctrl Pts',(-53.7130821626263,-46.6481568669216,
0.));
#76933=CARTESIAN_POINT('Ctrl Pts',(-53.7130821626263,-46.6481568669216,
12.));
#76934=CARTESIAN_POINT('Ctrl Pts',(-53.7245719674222,-46.6672846938752,
0.));
#76935=CARTESIAN_POINT('Ctrl Pts',(-53.7245719674222,-46.6672846938752,
12.));
#76936=CARTESIAN_POINT('Ctrl Pts',(-53.7360662508677,-46.6864639475863,
0.));
#76937=CARTESIAN_POINT('Ctrl Pts',(-53.7360662508677,-46.6864639475863,
12.));
#76938=CARTESIAN_POINT('Ctrl Pts',(-53.7475648793948,-46.7056945424559,
0.));
#76939=CARTESIAN_POINT('Ctrl Pts',(-53.7475648793948,-46.7056945424559,
12.));
#76940=CARTESIAN_POINT('Ctrl Pts',(-53.7590677201344,-46.724976393213,0.));
#76941=CARTESIAN_POINT('Ctrl Pts',(-53.7590677201344,-46.724976393213,12.));
#76942=CARTESIAN_POINT('Ctrl Pts',(-53.770574640907,-46.7443094149041,0.));
#76943=CARTESIAN_POINT('Ctrl Pts',(-53.770574640907,-46.7443094149041,12.));
#76944=CARTESIAN_POINT('Ctrl Pts',(-53.782085510217,-46.7636935228851,0.));
#76945=CARTESIAN_POINT('Ctrl Pts',(-53.782085510217,-46.7636935228851,12.));
#76946=CARTESIAN_POINT('Ctrl Pts',(-53.7936001972468,-46.7831286328268,
0.));
#76947=CARTESIAN_POINT('Ctrl Pts',(-53.7936001972468,-46.7831286328268,
12.));
#76948=CARTESIAN_POINT('Ctrl Pts',(-53.8051185718525,-46.8026146607144,
0.));
#76949=CARTESIAN_POINT('Ctrl Pts',(-53.8051185718525,-46.8026146607144,
12.));
#76950=CARTESIAN_POINT('Ctrl Pts',(-53.8166405045582,-46.8221515228459,
0.));
#76951=CARTESIAN_POINT('Ctrl Pts',(-53.8166405045582,-46.8221515228459,
12.));
#76952=CARTESIAN_POINT('Ctrl Pts',(-53.8281658665517,-46.8417391358231,
0.));
#76953=CARTESIAN_POINT('Ctrl Pts',(-53.8281658665517,-46.8417391358231,
12.));
#76954=CARTESIAN_POINT('Ctrl Pts',(-53.8396945296777,-46.8613774165452,
0.));
#76955=CARTESIAN_POINT('Ctrl Pts',(-53.8396945296777,-46.8613774165452,
12.));
#76956=CARTESIAN_POINT('Ctrl Pts',(-53.851226366434,-46.8810662822147,0.));
#76957=CARTESIAN_POINT('Ctrl Pts',(-53.851226366434,-46.8810662822147,12.));
#76958=CARTESIAN_POINT('Ctrl Pts',(-53.8627612499648,-46.900805650336,0.));
#76959=CARTESIAN_POINT('Ctrl Pts',(-53.8627612499648,-46.900805650336,12.));
#76960=CARTESIAN_POINT('Ctrl Pts',(-53.8742990540557,-46.9205954387128,
0.));
#76961=CARTESIAN_POINT('Ctrl Pts',(-53.8742990540557,-46.9205954387128,
12.));
#76962=CARTESIAN_POINT('Ctrl Pts',(-53.8858396531277,-46.9404355654381,
0.));
#76963=CARTESIAN_POINT('Ctrl Pts',(-53.8858396531277,-46.9404355654381,
12.));
#76964=CARTESIAN_POINT('Ctrl Pts',(-53.8973829222317,-46.9603259488894,
0.));
#76965=CARTESIAN_POINT('Ctrl Pts',(-53.8973829222317,-46.9603259488894,
12.));
#76966=CARTESIAN_POINT('Ctrl Pts',(-53.9089287370436,-46.9802665077342,
0.));
#76967=CARTESIAN_POINT('Ctrl Pts',(-53.9089287370436,-46.9802665077342,
12.));
#76968=CARTESIAN_POINT('Ctrl Pts',(-53.9204769738584,-47.0002571609286,
0.));
#76969=CARTESIAN_POINT('Ctrl Pts',(-53.9204769738584,-47.0002571609286,
12.));
#76970=CARTESIAN_POINT('Ctrl Pts',(-53.9320275095864,-47.0202978277148,
0.));
#76971=CARTESIAN_POINT('Ctrl Pts',(-53.9320275095864,-47.0202978277148,
12.));
#76972=CARTESIAN_POINT('Ctrl Pts',(-53.9435802217468,-47.04038842761,0.));
#76973=CARTESIAN_POINT('Ctrl Pts',(-53.9435802217468,-47.04038842761,12.));
#76974=CARTESIAN_POINT('Ctrl Pts',(-53.9551349884637,-47.0605288804042,
0.));
#76975=CARTESIAN_POINT('Ctrl Pts',(-53.9551349884637,-47.0605288804042,
12.));
#76976=CARTESIAN_POINT('Ctrl Pts',(-53.9666916884624,-47.0807191061674,
0.));
#76977=CARTESIAN_POINT('Ctrl Pts',(-53.9666916884624,-47.0807191061674,
12.));
#76978=CARTESIAN_POINT('Ctrl Pts',(-53.9782502010642,-47.1009590252466,
0.));
#76979=CARTESIAN_POINT('Ctrl Pts',(-53.9782502010642,-47.1009590252466,
12.));
#76980=CARTESIAN_POINT('Ctrl Pts',(-53.9898104061809,-47.1212485582632,
0.));
#76981=CARTESIAN_POINT('Ctrl Pts',(-53.9898104061809,-47.1212485582632,
12.));
#76982=CARTESIAN_POINT('Ctrl Pts',(-54.0013721843094,-47.1415876261012,
0.));
#76983=CARTESIAN_POINT('Ctrl Pts',(-54.0013721843094,-47.1415876261012,
12.));
#76984=CARTESIAN_POINT('Ctrl Pts',(-54.0129354165269,-47.161976149906,0.));
#76985=CARTESIAN_POINT('Ctrl Pts',(-54.0129354165269,-47.161976149906,12.));
#76986=CARTESIAN_POINT('Ctrl Pts',(-54.0244999844872,-47.1824140510906,
0.));
#76987=CARTESIAN_POINT('Ctrl Pts',(-54.0244999844872,-47.1824140510906,
12.));
#76988=CARTESIAN_POINT('Ctrl Pts',(-54.0360657704156,-47.2029012513334,
0.));
#76989=CARTESIAN_POINT('Ctrl Pts',(-54.0360657704156,-47.2029012513334,
12.));
#76990=CARTESIAN_POINT('Ctrl Pts',(-54.047632657105,-47.2234376725752,0.));
#76991=CARTESIAN_POINT('Ctrl Pts',(-54.047632657105,-47.2234376725752,12.));
#76992=CARTESIAN_POINT('Ctrl Pts',(-54.0592005279108,-47.2440232370085,
0.));
#76993=CARTESIAN_POINT('Ctrl Pts',(-54.0592005279108,-47.2440232370085,
12.));
#76994=CARTESIAN_POINT('Ctrl Pts',(-54.0707692667461,-47.2646578670767,
0.));
#76995=CARTESIAN_POINT('Ctrl Pts',(-54.0707692667461,-47.2646578670767,
12.));
#76996=CARTESIAN_POINT('Ctrl Pts',(-54.082338758079,-47.2853414854805,0.));
#76997=CARTESIAN_POINT('Ctrl Pts',(-54.082338758079,-47.2853414854805,12.));
#76998=CARTESIAN_POINT('Ctrl Pts',(-54.0939088869271,-47.3060740151754,
0.));
#76999=CARTESIAN_POINT('Ctrl Pts',(-54.0939088869271,-47.3060740151754,
12.));
#77000=CARTESIAN_POINT('Ctrl Pts',(-54.1054795388538,-47.326855379369,0.));
#77001=CARTESIAN_POINT('Ctrl Pts',(-54.1054795388538,-47.326855379369,12.));
#77002=CARTESIAN_POINT('Ctrl Pts',(-54.1170505999637,-47.3476855015095,
0.));
#77003=CARTESIAN_POINT('Ctrl Pts',(-54.1170505999637,-47.3476855015095,
12.));
#77004=CARTESIAN_POINT('Ctrl Pts',(-54.1286219568981,-47.3685643052867,
0.));
#77005=CARTESIAN_POINT('Ctrl Pts',(-54.1286219568981,-47.3685643052867,
12.));
#77006=CARTESIAN_POINT('Ctrl Pts',(-54.1401934968306,-47.3894917146361,
0.));
#77007=CARTESIAN_POINT('Ctrl Pts',(-54.1401934968306,-47.3894917146361,
12.));
#77008=CARTESIAN_POINT('Ctrl Pts',(-54.1517651074638,-47.4104676537381,
0.));
#77009=CARTESIAN_POINT('Ctrl Pts',(-54.1517651074638,-47.4104676537381,
12.));
#77010=CARTESIAN_POINT('Ctrl Pts',(-54.163336677024,-47.4314920470142,0.));
#77011=CARTESIAN_POINT('Ctrl Pts',(-54.163336677024,-47.4314920470142,12.));
#77012=CARTESIAN_POINT('Ctrl Pts',(-54.1749080942593,-47.4525648191173,
0.));
#77013=CARTESIAN_POINT('Ctrl Pts',(-54.1749080942593,-47.4525648191173,
12.));
#77014=CARTESIAN_POINT('Ctrl Pts',(-54.1864792484343,-47.473685894932,0.));
#77015=CARTESIAN_POINT('Ctrl Pts',(-54.1864792484343,-47.473685894932,12.));
#77016=CARTESIAN_POINT('Ctrl Pts',(-54.1980500293267,-47.4948551995799,
0.));
#77017=CARTESIAN_POINT('Ctrl Pts',(-54.1980500293267,-47.4948551995799,
12.));
#77018=CARTESIAN_POINT('Ctrl Pts',(-54.2096203272228,-47.5160726584172,
0.));
#77019=CARTESIAN_POINT('Ctrl Pts',(-54.2096203272228,-47.5160726584172,
12.));
#77020=CARTESIAN_POINT('Ctrl Pts',(-54.2211900329141,-47.5373381970328,
0.));
#77021=CARTESIAN_POINT('Ctrl Pts',(-54.2211900329141,-47.5373381970328,
12.));
#77022=CARTESIAN_POINT('Ctrl Pts',(-54.232759037693,-47.5586517412368,0.));
#77023=CARTESIAN_POINT('Ctrl Pts',(-54.232759037693,-47.5586517412368,12.));
#77024=CARTESIAN_POINT('Ctrl Pts',(-54.2443272333498,-47.5800132170614,
0.));
#77025=CARTESIAN_POINT('Ctrl Pts',(-54.2443272333498,-47.5800132170614,
12.));
#77026=CARTESIAN_POINT('Ctrl Pts',(-54.2558945121684,-47.6014225507664,
0.));
#77027=CARTESIAN_POINT('Ctrl Pts',(-54.2558945121684,-47.6014225507664,
12.));
#77028=CARTESIAN_POINT('Ctrl Pts',(-54.2674607669228,-47.6228796688376,
0.));
#77029=CARTESIAN_POINT('Ctrl Pts',(-54.2674607669228,-47.6228796688376,
12.));
#77030=CARTESIAN_POINT('Ctrl Pts',(-54.2790258908736,-47.6443844979846,
0.));
#77031=CARTESIAN_POINT('Ctrl Pts',(-54.2790258908736,-47.6443844979846,
12.));
#77032=CARTESIAN_POINT('Ctrl Pts',(-54.2905897777647,-47.6659369651299,
0.));
#77033=CARTESIAN_POINT('Ctrl Pts',(-54.2905897777647,-47.6659369651299,
12.));
#77034=CARTESIAN_POINT('Ctrl Pts',(-54.3021523218188,-47.6875369974086,
0.));
#77035=CARTESIAN_POINT('Ctrl Pts',(-54.3021523218188,-47.6875369974086,
12.));
#77036=CARTESIAN_POINT('Ctrl Pts',(-54.3137134177345,-47.7091845221748,
0.));
#77037=CARTESIAN_POINT('Ctrl Pts',(-54.3137134177345,-47.7091845221748,
12.));
#77038=CARTESIAN_POINT('Ctrl Pts',(-54.3252729606824,-47.7308794669994,
0.));
#77039=CARTESIAN_POINT('Ctrl Pts',(-54.3252729606824,-47.7308794669994,
12.));
#77040=CARTESIAN_POINT('Ctrl Pts',(-54.3368308463023,-47.7526217596694,
0.));
#77041=CARTESIAN_POINT('Ctrl Pts',(-54.3368308463023,-47.7526217596694,
12.));
#77042=CARTESIAN_POINT('Ctrl Pts',(-54.3483869706998,-47.7744113281768,
0.));
#77043=CARTESIAN_POINT('Ctrl Pts',(-54.3483869706998,-47.7744113281768,
12.));
#77044=CARTESIAN_POINT('Ctrl Pts',(-54.3599412304431,-47.7962481007179,
0.));
#77045=CARTESIAN_POINT('Ctrl Pts',(-54.3599412304431,-47.7962481007179,
12.));
#77046=CARTESIAN_POINT('Ctrl Pts',(-54.3714935225585,-47.8181320056988,
0.));
#77047=CARTESIAN_POINT('Ctrl Pts',(-54.3714935225585,-47.8181320056988,
12.));
#77048=CARTESIAN_POINT('Ctrl Pts',(-54.3830437445275,-47.8400629717352,
0.));
#77049=CARTESIAN_POINT('Ctrl Pts',(-54.3830437445275,-47.8400629717352,
12.));
#77050=CARTESIAN_POINT('Ctrl Pts',(-54.3945917942835,-47.8620409276495,
0.));
#77051=CARTESIAN_POINT('Ctrl Pts',(-54.3945917942835,-47.8620409276495,
12.));
#77052=CARTESIAN_POINT('Ctrl Pts',(-54.4061375702088,-47.8840658024626,
0.));
#77053=CARTESIAN_POINT('Ctrl Pts',(-54.4061375702088,-47.8840658024626,
12.));
#77054=CARTESIAN_POINT('Ctrl Pts',(-54.4176809711324,-47.9061375253909,
0.));
#77055=CARTESIAN_POINT('Ctrl Pts',(-54.4176809711324,-47.9061375253909,
12.));
#77056=CARTESIAN_POINT('Ctrl Pts',(-54.4292218963253,-47.9282560258528,
0.));
#77057=CARTESIAN_POINT('Ctrl Pts',(-54.4292218963253,-47.9282560258528,
12.));
#77058=CARTESIAN_POINT('Ctrl Pts',(-54.4407602454974,-47.9504212334681,
0.));
#77059=CARTESIAN_POINT('Ctrl Pts',(-54.4407602454974,-47.9504212334681,
12.));
#77060=CARTESIAN_POINT('Ctrl Pts',(-54.4522959187952,-47.972633078057,0.));
#77061=CARTESIAN_POINT('Ctrl Pts',(-54.4522959187952,-47.972633078057,12.));
#77062=CARTESIAN_POINT('Ctrl Pts',(-54.4638288167991,-47.9948914896316,
0.));
#77063=CARTESIAN_POINT('Ctrl Pts',(-54.4638288167991,-47.9948914896316,
12.));
#77064=CARTESIAN_POINT('Ctrl Pts',(-54.4753588405202,-48.0171963983912,
0.));
#77065=CARTESIAN_POINT('Ctrl Pts',(-54.4753588405202,-48.0171963983912,
12.));
#77066=CARTESIAN_POINT('Ctrl Pts',(-54.4868858913961,-48.039547734729,0.));
#77067=CARTESIAN_POINT('Ctrl Pts',(-54.4868858913961,-48.039547734729,12.));
#77068=CARTESIAN_POINT('Ctrl Pts',(-54.4984098712883,-48.0619454292321,
0.));
#77069=CARTESIAN_POINT('Ctrl Pts',(-54.4984098712883,-48.0619454292321,
12.));
#77070=CARTESIAN_POINT('Ctrl Pts',(-54.5099306824788,-48.0843894126807,
0.));
#77071=CARTESIAN_POINT('Ctrl Pts',(-54.5099306824788,-48.0843894126807,
12.));
#77072=CARTESIAN_POINT('Ctrl Pts',(-54.5214482276679,-48.1068796160406,
0.));
#77073=CARTESIAN_POINT('Ctrl Pts',(-54.5214482276679,-48.1068796160406,
12.));
#77074=CARTESIAN_POINT('Ctrl Pts',(-54.5329624099719,-48.1294159704571,
0.));
#77075=CARTESIAN_POINT('Ctrl Pts',(-54.5329624099719,-48.1294159704571,
12.));
#77076=CARTESIAN_POINT('Ctrl Pts',(-54.5444731329196,-48.1519984072617,
0.));
#77077=CARTESIAN_POINT('Ctrl Pts',(-54.5444731329196,-48.1519984072617,
12.));
#77078=CARTESIAN_POINT('Ctrl Pts',(-54.5559803004487,-48.1746268579732,
0.));
#77079=CARTESIAN_POINT('Ctrl Pts',(-54.5559803004487,-48.1746268579732,
12.));
#77080=CARTESIAN_POINT('Ctrl Pts',(-54.5674838169041,-48.1973012542966,
0.));
#77081=CARTESIAN_POINT('Ctrl Pts',(-54.5674838169041,-48.1973012542966,
12.));
#77082=CARTESIAN_POINT('Ctrl Pts',(-54.5789835870348,-48.2200215281178,
0.));
#77083=CARTESIAN_POINT('Ctrl Pts',(-54.5789835870348,-48.2200215281178,
12.));
#77084=CARTESIAN_POINT('Ctrl Pts',(-54.5904795159936,-48.2427876114956,
0.));
#77085=CARTESIAN_POINT('Ctrl Pts',(-54.5904795159936,-48.2427876114956,
12.));
#77086=CARTESIAN_POINT('Ctrl Pts',(-54.6019715093319,-48.2655994366672,
0.));
#77087=CARTESIAN_POINT('Ctrl Pts',(-54.6019715093319,-48.2655994366672,
12.));
#77088=CARTESIAN_POINT('Ctrl Pts',(-54.6134594729964,-48.288456936051,0.));
#77089=CARTESIAN_POINT('Ctrl Pts',(-54.6134594729964,-48.288456936051,12.));
#77090=CARTESIAN_POINT('Ctrl Pts',(-54.6249433133262,-48.3113600422443,
0.));
#77091=CARTESIAN_POINT('Ctrl Pts',(-54.6249433133262,-48.3113600422443,
12.));
#77092=CARTESIAN_POINT('Ctrl Pts',(-54.636422937049,-48.3343086880192,0.));
#77093=CARTESIAN_POINT('Ctrl Pts',(-54.636422937049,-48.3343086880192,12.));
#77094=CARTESIAN_POINT('Ctrl Pts',(-54.647898251279,-48.3573028063122,0.));
#77095=CARTESIAN_POINT('Ctrl Pts',(-54.647898251279,-48.3573028063122,12.));
#77096=CARTESIAN_POINT('Ctrl Pts',(-54.6593691635143,-48.3803423302294,
0.));
#77097=CARTESIAN_POINT('Ctrl Pts',(-54.6593691635143,-48.3803423302294,
12.));
#77098=CARTESIAN_POINT('Ctrl Pts',(-54.6708355816359,-48.4034271930516,
0.));
#77099=CARTESIAN_POINT('Ctrl Pts',(-54.6708355816359,-48.4034271930516,
12.));
#77100=CARTESIAN_POINT('Ctrl Pts',(-54.6822974139065,-48.4265573282342,
0.));
#77101=CARTESIAN_POINT('Ctrl Pts',(-54.6822974139065,-48.4265573282342,
12.));
#77102=CARTESIAN_POINT('Ctrl Pts',(-54.6937545689694,-48.4497326694051,
0.));
#77103=CARTESIAN_POINT('Ctrl Pts',(-54.6937545689694,-48.4497326694051,
12.));
#77104=CARTESIAN_POINT('Ctrl Pts',(-54.7052069558493,-48.4729531503565,
0.));
#77105=CARTESIAN_POINT('Ctrl Pts',(-54.7052069558493,-48.4729531503565,
12.));
#77106=CARTESIAN_POINT('Ctrl Pts',(-54.7166544839475,-48.4962187050452,
0.));
#77107=CARTESIAN_POINT('Ctrl Pts',(-54.7166544839475,-48.4962187050452,
12.));
#77108=CARTESIAN_POINT('Ctrl Pts',(-54.7280970630346,-48.5195292675955,
0.));
#77109=CARTESIAN_POINT('Ctrl Pts',(-54.7280970630346,-48.5195292675955,
12.));
#77110=CARTESIAN_POINT('Ctrl Pts',(-54.7395346032451,-48.5428847722975,
0.));
#77111=CARTESIAN_POINT('Ctrl Pts',(-54.7395346032451,-48.5428847722975,
12.));
#77112=CARTESIAN_POINT('Ctrl Pts',(-54.7509670150716,-48.5662851536027,
0.));
#77113=CARTESIAN_POINT('Ctrl Pts',(-54.7509670150716,-48.5662851536027,
12.));
#77114=CARTESIAN_POINT('Ctrl Pts',(-54.7623942093591,-48.5897303461131,
0.));
#77115=CARTESIAN_POINT('Ctrl Pts',(-54.7623942093591,-48.5897303461131,
12.));
#77116=CARTESIAN_POINT('Ctrl Pts',(-54.773816097304,-48.6132202845792,0.));
#77117=CARTESIAN_POINT('Ctrl Pts',(-54.773816097304,-48.6132202845792,12.));
#77118=CARTESIAN_POINT('Ctrl Pts',(-54.7852325904591,-48.6367549039121,
0.));
#77119=CARTESIAN_POINT('Ctrl Pts',(-54.7852325904591,-48.6367549039121,
12.));
#77120=CARTESIAN_POINT('Ctrl Pts',(-54.7966436007395,-48.6603341391891,
0.));
#77121=CARTESIAN_POINT('Ctrl Pts',(-54.7966436007395,-48.6603341391891,
12.));
#77122=CARTESIAN_POINT('Ctrl Pts',(-54.8080490404274,-48.6839579256565,
0.));
#77123=CARTESIAN_POINT('Ctrl Pts',(-54.8080490404274,-48.6839579256565,
12.));
#77124=CARTESIAN_POINT('Ctrl Pts',(-54.8194488221803,-48.7076261987284,
0.));
#77125=CARTESIAN_POINT('Ctrl Pts',(-54.8194488221803,-48.7076261987284,
12.));
#77126=CARTESIAN_POINT('Ctrl Pts',(-54.8308428590334,-48.7313388939834,
0.));
#77127=CARTESIAN_POINT('Ctrl Pts',(-54.8308428590334,-48.7313388939834,
12.));
#77128=CARTESIAN_POINT('Ctrl Pts',(-54.8422310643752,-48.755095947159,0.));
#77129=CARTESIAN_POINT('Ctrl Pts',(-54.8422310643752,-48.755095947159,12.));
#77130=CARTESIAN_POINT('Ctrl Pts',(-54.8536133519285,-48.7788972941431,
0.));
#77131=CARTESIAN_POINT('Ctrl Pts',(-54.8536133519285,-48.7788972941431,
12.));
#77132=CARTESIAN_POINT('Ctrl Pts',(-54.8649896357284,-48.8027428709613,
0.));
#77133=CARTESIAN_POINT('Ctrl Pts',(-54.8649896357284,-48.8027428709613,
12.));
#77134=CARTESIAN_POINT('Ctrl Pts',(-54.8763598301045,-48.8266326137629,
0.));
#77135=CARTESIAN_POINT('Ctrl Pts',(-54.8763598301045,-48.8266326137629,
12.));
#77136=CARTESIAN_POINT('Ctrl Pts',(-54.8877238496577,-48.8505664587985,
0.));
#77137=CARTESIAN_POINT('Ctrl Pts',(-54.8877238496577,-48.8505664587985,
12.));
#77138=CARTESIAN_POINT('Ctrl Pts',(-54.8990816092964,-48.8745443424488,
0.));
#77139=CARTESIAN_POINT('Ctrl Pts',(-54.8990816092964,-48.8745443424488,
12.));
#77140=CARTESIAN_POINT('Ctrl Pts',(-54.910433024275,-48.8985662012535,0.));
#77141=CARTESIAN_POINT('Ctrl Pts',(-54.910433024275,-48.8985662012535,12.));
#77142=CARTESIAN_POINT('Ctrl Pts',(-54.9217780102357,-48.922631971937,0.));
#77143=CARTESIAN_POINT('Ctrl Pts',(-54.9217780102357,-48.922631971937,12.));
#77144=CARTESIAN_POINT('Ctrl Pts',(-54.933116483242,-48.9467415914266,0.));
#77145=CARTESIAN_POINT('Ctrl Pts',(-54.933116483242,-48.9467415914266,12.));
#77146=CARTESIAN_POINT('Ctrl Pts',(-54.9444483598372,-48.9708949968789,
0.));
#77147=CARTESIAN_POINT('Ctrl Pts',(-54.9444483598372,-48.9708949968789,
12.));
#77148=CARTESIAN_POINT('Ctrl Pts',(-54.9557735569936,-48.995092125652,0.));
#77149=CARTESIAN_POINT('Ctrl Pts',(-54.9557735569936,-48.995092125652,12.));
#77150=CARTESIAN_POINT('Ctrl Pts',(-54.9670919920024,-49.0193329152475,
0.));
#77151=CARTESIAN_POINT('Ctrl Pts',(-54.9670919920024,-49.0193329152475,
12.));
#77152=CARTESIAN_POINT('Ctrl Pts',(-54.9784035823764,-49.0436173032527,
0.));
#77153=CARTESIAN_POINT('Ctrl Pts',(-54.9784035823764,-49.0436173032527,
12.));
#77154=CARTESIAN_POINT('Ctrl Pts',(-54.9897082457606,-49.0679452272871,
0.));
#77155=CARTESIAN_POINT('Ctrl Pts',(-54.9897082457606,-49.0679452272871,
12.));
#77156=CARTESIAN_POINT('Ctrl Pts',(-55.0010058998111,-49.0923166249222,
0.));
#77157=CARTESIAN_POINT('Ctrl Pts',(-55.0010058998111,-49.0923166249222,
12.));
#77158=CARTESIAN_POINT('Ctrl Pts',(-55.0122964621868,-49.1167314336737,
0.));
#77159=CARTESIAN_POINT('Ctrl Pts',(-55.0122964621868,-49.1167314336737,
12.));
#77160=CARTESIAN_POINT('Ctrl Pts',(-55.0235798508056,-49.1411895911646,
0.));
#77161=CARTESIAN_POINT('Ctrl Pts',(-55.0235798508056,-49.1411895911646,
12.));
#77162=CARTESIAN_POINT('Ctrl Pts',(-55.0348559840462,-49.1656910352484,
0.));
#77163=CARTESIAN_POINT('Ctrl Pts',(-55.0348559840462,-49.1656910352484,
12.));
#77164=CARTESIAN_POINT('Ctrl Pts',(-55.0461247809745,-49.1902357041462,
0.));
#77165=CARTESIAN_POINT('Ctrl Pts',(-55.0461247809745,-49.1902357041462,
12.));
#77166=CARTESIAN_POINT('Ctrl Pts',(-55.0573861615569,-49.2148235365694,
0.));
#77167=CARTESIAN_POINT('Ctrl Pts',(-55.0573861615569,-49.2148235365694,
12.));
#77168=CARTESIAN_POINT('Ctrl Pts',(-55.0686400468911,-49.2394544718513,
0.));
#77169=CARTESIAN_POINT('Ctrl Pts',(-55.0686400468911,-49.2394544718513,
12.));
#77170=CARTESIAN_POINT('Ctrl Pts',(-55.0798863586986,-49.2641284496496,
0.));
#77171=CARTESIAN_POINT('Ctrl Pts',(-55.0798863586986,-49.2641284496496,
12.));
#77172=CARTESIAN_POINT('Ctrl Pts',(-55.0911250188282,-49.2888454096544,
0.));
#77173=CARTESIAN_POINT('Ctrl Pts',(-55.0911250188282,-49.2888454096544,
12.));
#77174=CARTESIAN_POINT('Ctrl Pts',(-55.1023559487133,-49.3136052912614,
0.));
#77175=CARTESIAN_POINT('Ctrl Pts',(-55.1023559487133,-49.3136052912614,
12.));
#77176=CARTESIAN_POINT('Ctrl Pts',(-55.1135790689475,-49.3384080333166,
0.));
#77177=CARTESIAN_POINT('Ctrl Pts',(-55.1135790689475,-49.3384080333166,
12.));
#77178=CARTESIAN_POINT('Ctrl Pts',(-55.1247942985649,-49.3632535736744,
0.));
#77179=CARTESIAN_POINT('Ctrl Pts',(-55.1247942985649,-49.3632535736744,
12.));
#77180=CARTESIAN_POINT('Ctrl Pts',(-55.1360015556262,-49.3881418495529,
0.));
#77181=CARTESIAN_POINT('Ctrl Pts',(-55.1360015556262,-49.3881418495529,
12.));
#77182=CARTESIAN_POINT('Ctrl Pts',(-55.1472007585224,-49.413072798324,0.));
#77183=CARTESIAN_POINT('Ctrl Pts',(-55.1472007585224,-49.413072798324,12.));
#77184=CARTESIAN_POINT('Ctrl Pts',(-55.158391827114,-49.4380463581989,0.));
#77185=CARTESIAN_POINT('Ctrl Pts',(-55.158391827114,-49.4380463581989,12.));
#77186=CARTESIAN_POINT('Ctrl Pts',(-55.1695746838168,-49.4630624688787,
0.));
#77187=CARTESIAN_POINT('Ctrl Pts',(-55.1695746838168,-49.4630624688787,
12.));
#77188=CARTESIAN_POINT('Ctrl Pts',(-55.1807492550073,-49.4881210723921,
0.));
#77189=CARTESIAN_POINT('Ctrl Pts',(-55.1807492550073,-49.4881210723921,
12.));
#77190=CARTESIAN_POINT('Ctrl Pts',(-55.1919154713569,-49.5132221132916,
0.));
#77191=CARTESIAN_POINT('Ctrl Pts',(-55.1919154713569,-49.5132221132916,
12.));
#77192=CARTESIAN_POINT('Ctrl Pts',(-55.2030732647222,-49.5383655367987,
0.));
#77193=CARTESIAN_POINT('Ctrl Pts',(-55.2030732647222,-49.5383655367987,
12.));
#77194=CARTESIAN_POINT('Ctrl Pts',(-55.2142225656943,-49.5635512873368,
0.));
#77195=CARTESIAN_POINT('Ctrl Pts',(-55.2142225656943,-49.5635512873368,
12.));
#77196=CARTESIAN_POINT('Ctrl Pts',(-55.225363300765,-49.5887793068337,0.));
#77197=CARTESIAN_POINT('Ctrl Pts',(-55.225363300765,-49.5887793068337,12.));
#77198=CARTESIAN_POINT('Ctrl Pts',(-55.2364953899423,-49.6140495332865,
0.));
#77199=CARTESIAN_POINT('Ctrl Pts',(-55.2364953899423,-49.6140495332865,
12.));
#77200=CARTESIAN_POINT('Ctrl Pts',(-55.2476187434204,-49.6393618987614,
0.));
#77201=CARTESIAN_POINT('Ctrl Pts',(-55.2476187434204,-49.6393618987614,
12.));
#77202=CARTESIAN_POINT('Ctrl Pts',(-55.2587332663982,-49.6647163322457,
0.));
#77203=CARTESIAN_POINT('Ctrl Pts',(-55.2587332663982,-49.6647163322457,
12.));
#77204=CARTESIAN_POINT('Ctrl Pts',(-55.2698388650215,-49.690112763181,0.));
#77205=CARTESIAN_POINT('Ctrl Pts',(-55.2698388650215,-49.690112763181,12.));
#77206=CARTESIAN_POINT('Ctrl Pts',(-55.2809354521616,-49.7155511248629,
0.));
#77207=CARTESIAN_POINT('Ctrl Pts',(-55.2809354521616,-49.7155511248629,
12.));
#77208=CARTESIAN_POINT('Ctrl Pts',(-55.292022952748,-49.7410313576444,0.));
#77209=CARTESIAN_POINT('Ctrl Pts',(-55.292022952748,-49.7410313576444,12.));
#77210=CARTESIAN_POINT('Ctrl Pts',(-55.3031013105578,-49.7665534128269,
0.));
#77211=CARTESIAN_POINT('Ctrl Pts',(-55.3031013105578,-49.7665534128269,
12.));
#77212=CARTESIAN_POINT('Ctrl Pts',(-55.3141704897307,-49.7921172540185,
0.));
#77213=CARTESIAN_POINT('Ctrl Pts',(-55.3141704897307,-49.7921172540185,
12.));
#77214=CARTESIAN_POINT('Ctrl Pts',(-55.3252304694066,-49.817722855186,0.));
#77215=CARTESIAN_POINT('Ctrl Pts',(-55.3252304694066,-49.817722855186,12.));
#77216=CARTESIAN_POINT('Ctrl Pts',(-55.3340710859607,-49.8382407306675,
0.));
#77217=CARTESIAN_POINT('Ctrl Pts',(-55.3340710859607,-49.8382407306675,
12.));
#77218=CARTESIAN_POINT('Ctrl Pts',(-55.340697403233,-49.8536479176573,0.));
#77219=CARTESIAN_POINT('Ctrl Pts',(-55.340697403233,-49.8536479176573,12.));
#77220=CARTESIAN_POINT('Ctrl Pts',(-55.3451131058727,-49.8639277221471,
0.));
#77221=CARTESIAN_POINT('Ctrl Pts',(-55.3451131058727,-49.8639277221471,
12.));
#77222=CARTESIAN_POINT('Ctrl Pts',(-55.3473204966403,-49.8690697110161,
0.));
#77223=CARTESIAN_POINT('Ctrl Pts',(-55.3473204966403,-49.8690697110161,
12.));
#77224=CARTESIAN_POINT('',(-53.0702932034641,-45.6458539113724,0.));
#77225=CARTESIAN_POINT('Ctrl Pts',(-53.0702932034641,-45.6458539113724,
0.));
#77226=CARTESIAN_POINT('Ctrl Pts',(-53.0724894921849,-45.6490568514089,
0.));
#77227=CARTESIAN_POINT('Ctrl Pts',(-53.0768833804193,-45.6554684028145,
0.));
#77228=CARTESIAN_POINT('Ctrl Pts',(-53.0834781451546,-45.6651027439241,
0.));
#77229=CARTESIAN_POINT('Ctrl Pts',(-53.0922790298409,-45.6779825614231,
0.));
#77230=CARTESIAN_POINT('Ctrl Pts',(-53.1032932328857,-45.694139048907,0.));
#77231=CARTESIAN_POINT('Ctrl Pts',(-53.114320495492,-45.7103522376696,0.));
#77232=CARTESIAN_POINT('Ctrl Pts',(-53.1253607414872,-45.7266220897003,
0.));
#77233=CARTESIAN_POINT('Ctrl Pts',(-53.1364138384693,-45.7429485300823,
0.));
#77234=CARTESIAN_POINT('Ctrl Pts',(-53.1474795996053,-45.7593314474501,
0.));
#77235=CARTESIAN_POINT('Ctrl Pts',(-53.1585578076444,-45.7757707100618,
0.));
#77236=CARTESIAN_POINT('Ctrl Pts',(-53.1696482334487,-45.7922661780005,
0.));
#77237=CARTESIAN_POINT('Ctrl Pts',(-53.1807506560933,-45.808817716509,0.));
#77238=CARTESIAN_POINT('Ctrl Pts',(-53.1918648840541,-45.8254252099957,
0.));
#77239=CARTESIAN_POINT('Ctrl Pts',(-53.2029907483557,-45.8420885575349,
0.));
#77240=CARTESIAN_POINT('Ctrl Pts',(-53.2141280925439,-45.8588076662582,
0.));
#77241=CARTESIAN_POINT('Ctrl Pts',(-53.2252767643662,-45.8755824458723,
0.));
#77242=CARTESIAN_POINT('Ctrl Pts',(-53.2364366054306,-45.892412801838,0.));
#77243=CARTESIAN_POINT('Ctrl Pts',(-53.2476074460017,-45.9092986319377,
0.));
#77244=CARTESIAN_POINT('Ctrl Pts',(-53.2587891103866,-45.9262398298349,
0.));
#77245=CARTESIAN_POINT('Ctrl Pts',(-53.2699814203105,-45.9432362873008,
0.));
#77246=CARTESIAN_POINT('Ctrl Pts',(-53.2811841987926,-45.9602878967698,
0.));
#77247=CARTESIAN_POINT('Ctrl Pts',(-53.292397274555,-45.9773945542384,0.));
#77248=CARTESIAN_POINT('Ctrl Pts',(-53.3036204818329,-45.9945561591453,
0.));
#77249=CARTESIAN_POINT('Ctrl Pts',(-53.3148536582635,-46.0117726129873,
0.));
#77250=CARTESIAN_POINT('Ctrl Pts',(-53.326096643428,-46.02904381836,0.));
#77251=CARTESIAN_POINT('Ctrl Pts',(-53.3373492770671,-46.0463696777801,
0.));
#77252=CARTESIAN_POINT('Ctrl Pts',(-53.3486113975901,-46.0637500926982,
0.));
#77253=CARTESIAN_POINT('Ctrl Pts',(-53.3598828428546,-46.0811849640218,
0.));
#77254=CARTESIAN_POINT('Ctrl Pts',(-53.3711634508437,-46.0986741925656,
0.));
#77255=CARTESIAN_POINT('Ctrl Pts',(-53.3824530603276,-46.1162176794884,
0.));
#77256=CARTESIAN_POINT('Ctrl Pts',(-53.3937515116549,-46.1338153268097,
0.));
#77257=CARTESIAN_POINT('Ctrl Pts',(-53.4050586470436,-46.1514670376012,
0.));
#77258=CARTESIAN_POINT('Ctrl Pts',(-53.4163743101517,-46.1691727157134,
0.));
#77259=CARTESIAN_POINT('Ctrl Pts',(-53.4276983458125,-46.1869322656024,
0.));
#77260=CARTESIAN_POINT('Ctrl Pts',(-53.4390305997274,-46.2047455921286,
0.));
#77261=CARTESIAN_POINT('Ctrl Pts',(-53.4503709181178,-46.2226126003202,
0.));
#77262=CARTESIAN_POINT('Ctrl Pts',(-53.4617191477402,-46.2405331953889,
0.));
#77263=CARTESIAN_POINT('Ctrl Pts',(-53.4730751360371,-46.2585072828353,
0.));
#77264=CARTESIAN_POINT('Ctrl Pts',(-53.4844387312414,-46.2765347685198,
0.));
#77265=CARTESIAN_POINT('Ctrl Pts',(-53.4958097825006,-46.2946155587417,
0.));
#77266=CARTESIAN_POINT('Ctrl Pts',(-53.5071881399911,-46.3127495603098,
0.));
#77267=CARTESIAN_POINT('Ctrl Pts',(-53.5185736548548,-46.3309366805093,
0.));
#77268=CARTESIAN_POINT('Ctrl Pts',(-53.5299661791385,-46.3491768270655,
0.));
#77269=CARTESIAN_POINT('Ctrl Pts',(-53.5413655657327,-46.3674699081046,
0.));
#77270=CARTESIAN_POINT('Ctrl Pts',(-53.5527716683048,-46.3858158321059,
0.));
#77271=CARTESIAN_POINT('Ctrl Pts',(-53.5641843412559,-46.4042145078701,
0.));
#77272=CARTESIAN_POINT('Ctrl Pts',(-53.5756034397481,-46.4226658445474,
0.));
#77273=CARTESIAN_POINT('Ctrl Pts',(-53.5870288197166,-46.4411697516478,
0.));
#77274=CARTESIAN_POINT('Ctrl Pts',(-53.5984603378855,-46.459726139052,0.));
#77275=CARTESIAN_POINT('Ctrl Pts',(-53.6098978517859,-46.4783349170173,
0.));
#77276=CARTESIAN_POINT('Ctrl Pts',(-53.6213412197533,-46.496995996177,0.));
#77277=CARTESIAN_POINT('Ctrl Pts',(-53.6327903009094,-46.5157092875373,
0.));
#77278=CARTESIAN_POINT('Ctrl Pts',(-53.6442449551455,-46.5344747024676,
0.));
#77279=CARTESIAN_POINT('Ctrl Pts',(-53.6557050431071,-46.5532921526901,
0.));
#77280=CARTESIAN_POINT('Ctrl Pts',(-53.6671704261737,-46.5721615502591,
0.));
#77281=CARTESIAN_POINT('Ctrl Pts',(-53.678640966456,-46.5910828075653,0.));
#77282=CARTESIAN_POINT('Ctrl Pts',(-53.6901165267941,-46.6100558373402,
0.));
#77283=CARTESIAN_POINT('Ctrl Pts',(-53.701596970754,-46.6290805526559,0.));
#77284=CARTESIAN_POINT('Ctrl Pts',(-53.7130821626263,-46.6481568669216,
0.));
#77285=CARTESIAN_POINT('Ctrl Pts',(-53.7245719674222,-46.6672846938752,
0.));
#77286=CARTESIAN_POINT('Ctrl Pts',(-53.7360662508677,-46.6864639475863,
0.));
#77287=CARTESIAN_POINT('Ctrl Pts',(-53.7475648793948,-46.7056945424559,
0.));
#77288=CARTESIAN_POINT('Ctrl Pts',(-53.7590677201344,-46.724976393213,0.));
#77289=CARTESIAN_POINT('Ctrl Pts',(-53.770574640907,-46.7443094149041,0.));
#77290=CARTESIAN_POINT('Ctrl Pts',(-53.782085510217,-46.7636935228851,0.));
#77291=CARTESIAN_POINT('Ctrl Pts',(-53.7936001972468,-46.7831286328268,
0.));
#77292=CARTESIAN_POINT('Ctrl Pts',(-53.8051185718525,-46.8026146607144,
0.));
#77293=CARTESIAN_POINT('Ctrl Pts',(-53.8166405045582,-46.8221515228459,
0.));
#77294=CARTESIAN_POINT('Ctrl Pts',(-53.8281658665517,-46.8417391358231,
0.));
#77295=CARTESIAN_POINT('Ctrl Pts',(-53.8396945296777,-46.8613774165452,
0.));
#77296=CARTESIAN_POINT('Ctrl Pts',(-53.851226366434,-46.8810662822147,0.));
#77297=CARTESIAN_POINT('Ctrl Pts',(-53.8627612499648,-46.900805650336,0.));
#77298=CARTESIAN_POINT('Ctrl Pts',(-53.8742990540557,-46.9205954387128,
0.));
#77299=CARTESIAN_POINT('Ctrl Pts',(-53.8858396531277,-46.9404355654381,
0.));
#77300=CARTESIAN_POINT('Ctrl Pts',(-53.8973829222317,-46.9603259488894,
0.));
#77301=CARTESIAN_POINT('Ctrl Pts',(-53.9089287370436,-46.9802665077342,
0.));
#77302=CARTESIAN_POINT('Ctrl Pts',(-53.9204769738584,-47.0002571609286,
0.));
#77303=CARTESIAN_POINT('Ctrl Pts',(-53.9320275095864,-47.0202978277148,
0.));
#77304=CARTESIAN_POINT('Ctrl Pts',(-53.9435802217468,-47.04038842761,0.));
#77305=CARTESIAN_POINT('Ctrl Pts',(-53.9551349884637,-47.0605288804042,
0.));
#77306=CARTESIAN_POINT('Ctrl Pts',(-53.9666916884624,-47.0807191061674,
0.));
#77307=CARTESIAN_POINT('Ctrl Pts',(-53.9782502010642,-47.1009590252466,
0.));
#77308=CARTESIAN_POINT('Ctrl Pts',(-53.9898104061809,-47.1212485582632,
0.));
#77309=CARTESIAN_POINT('Ctrl Pts',(-54.0013721843094,-47.1415876261012,
0.));
#77310=CARTESIAN_POINT('Ctrl Pts',(-54.0129354165269,-47.161976149906,0.));
#77311=CARTESIAN_POINT('Ctrl Pts',(-54.0244999844872,-47.1824140510906,
0.));
#77312=CARTESIAN_POINT('Ctrl Pts',(-54.0360657704156,-47.2029012513334,
0.));
#77313=CARTESIAN_POINT('Ctrl Pts',(-54.047632657105,-47.2234376725752,0.));
#77314=CARTESIAN_POINT('Ctrl Pts',(-54.0592005279108,-47.2440232370085,
0.));
#77315=CARTESIAN_POINT('Ctrl Pts',(-54.0707692667461,-47.2646578670767,
0.));
#77316=CARTESIAN_POINT('Ctrl Pts',(-54.082338758079,-47.2853414854805,0.));
#77317=CARTESIAN_POINT('Ctrl Pts',(-54.0939088869271,-47.3060740151754,
0.));
#77318=CARTESIAN_POINT('Ctrl Pts',(-54.1054795388538,-47.326855379369,0.));
#77319=CARTESIAN_POINT('Ctrl Pts',(-54.1170505999637,-47.3476855015095,
0.));
#77320=CARTESIAN_POINT('Ctrl Pts',(-54.1286219568981,-47.3685643052867,
0.));
#77321=CARTESIAN_POINT('Ctrl Pts',(-54.1401934968306,-47.3894917146361,
0.));
#77322=CARTESIAN_POINT('Ctrl Pts',(-54.1517651074638,-47.4104676537381,
0.));
#77323=CARTESIAN_POINT('Ctrl Pts',(-54.163336677024,-47.4314920470142,0.));
#77324=CARTESIAN_POINT('Ctrl Pts',(-54.1749080942593,-47.4525648191173,
0.));
#77325=CARTESIAN_POINT('Ctrl Pts',(-54.1864792484343,-47.473685894932,0.));
#77326=CARTESIAN_POINT('Ctrl Pts',(-54.1980500293267,-47.4948551995799,
0.));
#77327=CARTESIAN_POINT('Ctrl Pts',(-54.2096203272228,-47.5160726584172,
0.));
#77328=CARTESIAN_POINT('Ctrl Pts',(-54.2211900329141,-47.5373381970328,
0.));
#77329=CARTESIAN_POINT('Ctrl Pts',(-54.232759037693,-47.5586517412368,0.));
#77330=CARTESIAN_POINT('Ctrl Pts',(-54.2443272333498,-47.5800132170614,
0.));
#77331=CARTESIAN_POINT('Ctrl Pts',(-54.2558945121684,-47.6014225507664,
0.));
#77332=CARTESIAN_POINT('Ctrl Pts',(-54.2674607669228,-47.6228796688376,
0.));
#77333=CARTESIAN_POINT('Ctrl Pts',(-54.2790258908736,-47.6443844979846,
0.));
#77334=CARTESIAN_POINT('Ctrl Pts',(-54.2905897777647,-47.6659369651299,
0.));
#77335=CARTESIAN_POINT('Ctrl Pts',(-54.3021523218188,-47.6875369974086,
0.));
#77336=CARTESIAN_POINT('Ctrl Pts',(-54.3137134177345,-47.7091845221748,
0.));
#77337=CARTESIAN_POINT('Ctrl Pts',(-54.3252729606824,-47.7308794669994,
0.));
#77338=CARTESIAN_POINT('Ctrl Pts',(-54.3368308463023,-47.7526217596694,
0.));
#77339=CARTESIAN_POINT('Ctrl Pts',(-54.3483869706998,-47.7744113281768,
0.));
#77340=CARTESIAN_POINT('Ctrl Pts',(-54.3599412304431,-47.7962481007179,
0.));
#77341=CARTESIAN_POINT('Ctrl Pts',(-54.3714935225585,-47.8181320056988,
0.));
#77342=CARTESIAN_POINT('Ctrl Pts',(-54.3830437445275,-47.8400629717352,
0.));
#77343=CARTESIAN_POINT('Ctrl Pts',(-54.3945917942835,-47.8620409276495,
0.));
#77344=CARTESIAN_POINT('Ctrl Pts',(-54.4061375702088,-47.8840658024626,
0.));
#77345=CARTESIAN_POINT('Ctrl Pts',(-54.4176809711324,-47.9061375253909,
0.));
#77346=CARTESIAN_POINT('Ctrl Pts',(-54.4292218963253,-47.9282560258528,
0.));
#77347=CARTESIAN_POINT('Ctrl Pts',(-54.4407602454974,-47.9504212334681,
0.));
#77348=CARTESIAN_POINT('Ctrl Pts',(-54.4522959187952,-47.972633078057,0.));
#77349=CARTESIAN_POINT('Ctrl Pts',(-54.4638288167991,-47.9948914896316,
0.));
#77350=CARTESIAN_POINT('Ctrl Pts',(-54.4753588405202,-48.0171963983912,
0.));
#77351=CARTESIAN_POINT('Ctrl Pts',(-54.4868858913961,-48.039547734729,0.));
#77352=CARTESIAN_POINT('Ctrl Pts',(-54.4984098712883,-48.0619454292321,
0.));
#77353=CARTESIAN_POINT('Ctrl Pts',(-54.5099306824788,-48.0843894126807,
0.));
#77354=CARTESIAN_POINT('Ctrl Pts',(-54.5214482276679,-48.1068796160406,
0.));
#77355=CARTESIAN_POINT('Ctrl Pts',(-54.5329624099719,-48.1294159704571,
0.));
#77356=CARTESIAN_POINT('Ctrl Pts',(-54.5444731329196,-48.1519984072617,
0.));
#77357=CARTESIAN_POINT('Ctrl Pts',(-54.5559803004487,-48.1746268579732,
0.));
#77358=CARTESIAN_POINT('Ctrl Pts',(-54.5674838169041,-48.1973012542966,
0.));
#77359=CARTESIAN_POINT('Ctrl Pts',(-54.5789835870348,-48.2200215281178,
0.));
#77360=CARTESIAN_POINT('Ctrl Pts',(-54.5904795159936,-48.2427876114956,
0.));
#77361=CARTESIAN_POINT('Ctrl Pts',(-54.6019715093319,-48.2655994366672,
0.));
#77362=CARTESIAN_POINT('Ctrl Pts',(-54.6134594729964,-48.288456936051,0.));
#77363=CARTESIAN_POINT('Ctrl Pts',(-54.6249433133262,-48.3113600422443,
0.));
#77364=CARTESIAN_POINT('Ctrl Pts',(-54.636422937049,-48.3343086880192,0.));
#77365=CARTESIAN_POINT('Ctrl Pts',(-54.647898251279,-48.3573028063122,0.));
#77366=CARTESIAN_POINT('Ctrl Pts',(-54.6593691635143,-48.3803423302294,
0.));
#77367=CARTESIAN_POINT('Ctrl Pts',(-54.6708355816359,-48.4034271930516,
0.));
#77368=CARTESIAN_POINT('Ctrl Pts',(-54.6822974139065,-48.4265573282342,
0.));
#77369=CARTESIAN_POINT('Ctrl Pts',(-54.6937545689694,-48.4497326694051,
0.));
#77370=CARTESIAN_POINT('Ctrl Pts',(-54.7052069558493,-48.4729531503565,
0.));
#77371=CARTESIAN_POINT('Ctrl Pts',(-54.7166544839475,-48.4962187050452,
0.));
#77372=CARTESIAN_POINT('Ctrl Pts',(-54.7280970630346,-48.5195292675955,
0.));
#77373=CARTESIAN_POINT('Ctrl Pts',(-54.7395346032451,-48.5428847722975,
0.));
#77374=CARTESIAN_POINT('Ctrl Pts',(-54.7509670150716,-48.5662851536027,
0.));
#77375=CARTESIAN_POINT('Ctrl Pts',(-54.7623942093591,-48.5897303461131,
0.));
#77376=CARTESIAN_POINT('Ctrl Pts',(-54.773816097304,-48.6132202845792,0.));
#77377=CARTESIAN_POINT('Ctrl Pts',(-54.7852325904591,-48.6367549039121,
0.));
#77378=CARTESIAN_POINT('Ctrl Pts',(-54.7966436007395,-48.6603341391891,
0.));
#77379=CARTESIAN_POINT('Ctrl Pts',(-54.8080490404274,-48.6839579256565,
0.));
#77380=CARTESIAN_POINT('Ctrl Pts',(-54.8194488221803,-48.7076261987284,
0.));
#77381=CARTESIAN_POINT('Ctrl Pts',(-54.8308428590334,-48.7313388939834,
0.));
#77382=CARTESIAN_POINT('Ctrl Pts',(-54.8422310643752,-48.755095947159,0.));
#77383=CARTESIAN_POINT('Ctrl Pts',(-54.8536133519285,-48.7788972941431,
0.));
#77384=CARTESIAN_POINT('Ctrl Pts',(-54.8649896357284,-48.8027428709613,
0.));
#77385=CARTESIAN_POINT('Ctrl Pts',(-54.8763598301045,-48.8266326137629,
0.));
#77386=CARTESIAN_POINT('Ctrl Pts',(-54.8877238496577,-48.8505664587985,
0.));
#77387=CARTESIAN_POINT('Ctrl Pts',(-54.8990816092964,-48.8745443424488,
0.));
#77388=CARTESIAN_POINT('Ctrl Pts',(-54.910433024275,-48.8985662012535,0.));
#77389=CARTESIAN_POINT('Ctrl Pts',(-54.9217780102357,-48.922631971937,0.));
#77390=CARTESIAN_POINT('Ctrl Pts',(-54.933116483242,-48.9467415914266,0.));
#77391=CARTESIAN_POINT('Ctrl Pts',(-54.9444483598372,-48.9708949968789,
0.));
#77392=CARTESIAN_POINT('Ctrl Pts',(-54.9557735569936,-48.995092125652,0.));
#77393=CARTESIAN_POINT('Ctrl Pts',(-54.9670919920024,-49.0193329152475,
0.));
#77394=CARTESIAN_POINT('Ctrl Pts',(-54.9784035823764,-49.0436173032527,
0.));
#77395=CARTESIAN_POINT('Ctrl Pts',(-54.9897082457606,-49.0679452272871,
0.));
#77396=CARTESIAN_POINT('Ctrl Pts',(-55.0010058998111,-49.0923166249222,
0.));
#77397=CARTESIAN_POINT('Ctrl Pts',(-55.0122964621868,-49.1167314336737,
0.));
#77398=CARTESIAN_POINT('Ctrl Pts',(-55.0235798508056,-49.1411895911646,
0.));
#77399=CARTESIAN_POINT('Ctrl Pts',(-55.0348559840462,-49.1656910352484,
0.));
#77400=CARTESIAN_POINT('Ctrl Pts',(-55.0461247809745,-49.1902357041462,
0.));
#77401=CARTESIAN_POINT('Ctrl Pts',(-55.0573861615569,-49.2148235365694,
0.));
#77402=CARTESIAN_POINT('Ctrl Pts',(-55.0686400468911,-49.2394544718513,
0.));
#77403=CARTESIAN_POINT('Ctrl Pts',(-55.0798863586986,-49.2641284496496,
0.));
#77404=CARTESIAN_POINT('Ctrl Pts',(-55.0911250188282,-49.2888454096544,
0.));
#77405=CARTESIAN_POINT('Ctrl Pts',(-55.1023559487133,-49.3136052912614,
0.));
#77406=CARTESIAN_POINT('Ctrl Pts',(-55.1135790689475,-49.3384080333166,
0.));
#77407=CARTESIAN_POINT('Ctrl Pts',(-55.1247942985649,-49.3632535736744,
0.));
#77408=CARTESIAN_POINT('Ctrl Pts',(-55.1360015556262,-49.3881418495529,
0.));
#77409=CARTESIAN_POINT('Ctrl Pts',(-55.1472007585224,-49.413072798324,0.));
#77410=CARTESIAN_POINT('Ctrl Pts',(-55.158391827114,-49.4380463581989,0.));
#77411=CARTESIAN_POINT('Ctrl Pts',(-55.1695746838168,-49.4630624688787,
0.));
#77412=CARTESIAN_POINT('Ctrl Pts',(-55.1807492550073,-49.4881210723921,
0.));
#77413=CARTESIAN_POINT('Ctrl Pts',(-55.1919154713569,-49.5132221132916,
0.));
#77414=CARTESIAN_POINT('Ctrl Pts',(-55.2014798623975,-49.5347748994607,
0.));
#77415=CARTESIAN_POINT('Ctrl Pts',(-55.2088081098955,-49.5513218524279,
0.));
#77416=CARTESIAN_POINT('Ctrl Pts',(-55.2139039604569,-49.5628442141869,
0.));
#77417=CARTESIAN_POINT('Ctrl Pts',(-55.2167699151168,-49.5693295981608,
0.));
#77418=CARTESIAN_POINT('Ctrl Pts',(-55.2174072001297,-49.5707719660254,
0.));
#77419=CARTESIAN_POINT('',(-53.0702932034641,-45.6458539113724,12.));
#77420=CARTESIAN_POINT('',(-53.0702932034641,-45.6458539113724,0.));
#77421=CARTESIAN_POINT('Ctrl Pts',(-55.2174072001297,-49.5707719660254,
12.));
#77422=CARTESIAN_POINT('Ctrl Pts',(-55.2167699151168,-49.5693295981608,
12.));
#77423=CARTESIAN_POINT('Ctrl Pts',(-55.2139039604569,-49.5628442141869,
12.));
#77424=CARTESIAN_POINT('Ctrl Pts',(-55.2088081098955,-49.5513218524279,
12.));
#77425=CARTESIAN_POINT('Ctrl Pts',(-55.2014798623975,-49.5347748994607,
12.));
#77426=CARTESIAN_POINT('Ctrl Pts',(-55.1919154713569,-49.5132221132916,
12.));
#77427=CARTESIAN_POINT('Ctrl Pts',(-55.1807492550073,-49.4881210723921,
12.));
#77428=CARTESIAN_POINT('Ctrl Pts',(-55.1695746838168,-49.4630624688787,
12.));
#77429=CARTESIAN_POINT('Ctrl Pts',(-55.158391827114,-49.4380463581989,12.));
#77430=CARTESIAN_POINT('Ctrl Pts',(-55.1472007585224,-49.413072798324,12.));
#77431=CARTESIAN_POINT('Ctrl Pts',(-55.1360015556262,-49.3881418495529,
12.));
#77432=CARTESIAN_POINT('Ctrl Pts',(-55.1247942985649,-49.3632535736744,
12.));
#77433=CARTESIAN_POINT('Ctrl Pts',(-55.1135790689475,-49.3384080333166,
12.));
#77434=CARTESIAN_POINT('Ctrl Pts',(-55.1023559487133,-49.3136052912614,
12.));
#77435=CARTESIAN_POINT('Ctrl Pts',(-55.0911250188282,-49.2888454096544,
12.));
#77436=CARTESIAN_POINT('Ctrl Pts',(-55.0798863586986,-49.2641284496496,
12.));
#77437=CARTESIAN_POINT('Ctrl Pts',(-55.0686400468911,-49.2394544718513,
12.));
#77438=CARTESIAN_POINT('Ctrl Pts',(-55.0573861615569,-49.2148235365694,
12.));
#77439=CARTESIAN_POINT('Ctrl Pts',(-55.0461247809745,-49.1902357041462,
12.));
#77440=CARTESIAN_POINT('Ctrl Pts',(-55.0348559840462,-49.1656910352484,
12.));
#77441=CARTESIAN_POINT('Ctrl Pts',(-55.0235798508056,-49.1411895911646,
12.));
#77442=CARTESIAN_POINT('Ctrl Pts',(-55.0122964621868,-49.1167314336737,
12.));
#77443=CARTESIAN_POINT('Ctrl Pts',(-55.0010058998111,-49.0923166249222,
12.));
#77444=CARTESIAN_POINT('Ctrl Pts',(-54.9897082457606,-49.0679452272871,
12.));
#77445=CARTESIAN_POINT('Ctrl Pts',(-54.9784035823764,-49.0436173032527,
12.));
#77446=CARTESIAN_POINT('Ctrl Pts',(-54.9670919920024,-49.0193329152475,
12.));
#77447=CARTESIAN_POINT('Ctrl Pts',(-54.9557735569936,-48.995092125652,12.));
#77448=CARTESIAN_POINT('Ctrl Pts',(-54.9444483598372,-48.9708949968789,
12.));
#77449=CARTESIAN_POINT('Ctrl Pts',(-54.933116483242,-48.9467415914266,12.));
#77450=CARTESIAN_POINT('Ctrl Pts',(-54.9217780102357,-48.922631971937,12.));
#77451=CARTESIAN_POINT('Ctrl Pts',(-54.910433024275,-48.8985662012535,12.));
#77452=CARTESIAN_POINT('Ctrl Pts',(-54.8990816092964,-48.8745443424488,
12.));
#77453=CARTESIAN_POINT('Ctrl Pts',(-54.8877238496577,-48.8505664587985,
12.));
#77454=CARTESIAN_POINT('Ctrl Pts',(-54.8763598301045,-48.8266326137629,
12.));
#77455=CARTESIAN_POINT('Ctrl Pts',(-54.8649896357284,-48.8027428709613,
12.));
#77456=CARTESIAN_POINT('Ctrl Pts',(-54.8536133519285,-48.7788972941431,
12.));
#77457=CARTESIAN_POINT('Ctrl Pts',(-54.8422310643752,-48.755095947159,12.));
#77458=CARTESIAN_POINT('Ctrl Pts',(-54.8308428590334,-48.7313388939834,
12.));
#77459=CARTESIAN_POINT('Ctrl Pts',(-54.8194488221803,-48.7076261987284,
12.));
#77460=CARTESIAN_POINT('Ctrl Pts',(-54.8080490404274,-48.6839579256565,
12.));
#77461=CARTESIAN_POINT('Ctrl Pts',(-54.7966436007395,-48.6603341391891,
12.));
#77462=CARTESIAN_POINT('Ctrl Pts',(-54.7852325904591,-48.6367549039121,
12.));
#77463=CARTESIAN_POINT('Ctrl Pts',(-54.773816097304,-48.6132202845792,12.));
#77464=CARTESIAN_POINT('Ctrl Pts',(-54.7623942093591,-48.5897303461131,
12.));
#77465=CARTESIAN_POINT('Ctrl Pts',(-54.7509670150716,-48.5662851536027,
12.));
#77466=CARTESIAN_POINT('Ctrl Pts',(-54.7395346032451,-48.5428847722975,
12.));
#77467=CARTESIAN_POINT('Ctrl Pts',(-54.7280970630346,-48.5195292675955,
12.));
#77468=CARTESIAN_POINT('Ctrl Pts',(-54.7166544839475,-48.4962187050452,
12.));
#77469=CARTESIAN_POINT('Ctrl Pts',(-54.7052069558493,-48.4729531503565,
12.));
#77470=CARTESIAN_POINT('Ctrl Pts',(-54.6937545689694,-48.4497326694051,
12.));
#77471=CARTESIAN_POINT('Ctrl Pts',(-54.6822974139065,-48.4265573282342,
12.));
#77472=CARTESIAN_POINT('Ctrl Pts',(-54.6708355816359,-48.4034271930516,
12.));
#77473=CARTESIAN_POINT('Ctrl Pts',(-54.6593691635143,-48.3803423302294,
12.));
#77474=CARTESIAN_POINT('Ctrl Pts',(-54.647898251279,-48.3573028063122,12.));
#77475=CARTESIAN_POINT('Ctrl Pts',(-54.636422937049,-48.3343086880192,12.));
#77476=CARTESIAN_POINT('Ctrl Pts',(-54.6249433133262,-48.3113600422443,
12.));
#77477=CARTESIAN_POINT('Ctrl Pts',(-54.6134594729964,-48.288456936051,12.));
#77478=CARTESIAN_POINT('Ctrl Pts',(-54.6019715093319,-48.2655994366672,
12.));
#77479=CARTESIAN_POINT('Ctrl Pts',(-54.5904795159936,-48.2427876114956,
12.));
#77480=CARTESIAN_POINT('Ctrl Pts',(-54.5789835870348,-48.2200215281178,
12.));
#77481=CARTESIAN_POINT('Ctrl Pts',(-54.5674838169041,-48.1973012542966,
12.));
#77482=CARTESIAN_POINT('Ctrl Pts',(-54.5559803004487,-48.1746268579732,
12.));
#77483=CARTESIAN_POINT('Ctrl Pts',(-54.5444731329196,-48.1519984072617,
12.));
#77484=CARTESIAN_POINT('Ctrl Pts',(-54.5329624099719,-48.1294159704571,
12.));
#77485=CARTESIAN_POINT('Ctrl Pts',(-54.5214482276679,-48.1068796160406,
12.));
#77486=CARTESIAN_POINT('Ctrl Pts',(-54.5099306824788,-48.0843894126807,
12.));
#77487=CARTESIAN_POINT('Ctrl Pts',(-54.4984098712883,-48.0619454292321,
12.));
#77488=CARTESIAN_POINT('Ctrl Pts',(-54.4868858913961,-48.039547734729,12.));
#77489=CARTESIAN_POINT('Ctrl Pts',(-54.4753588405202,-48.0171963983912,
12.));
#77490=CARTESIAN_POINT('Ctrl Pts',(-54.4638288167991,-47.9948914896316,
12.));
#77491=CARTESIAN_POINT('Ctrl Pts',(-54.4522959187952,-47.972633078057,12.));
#77492=CARTESIAN_POINT('Ctrl Pts',(-54.4407602454974,-47.9504212334681,
12.));
#77493=CARTESIAN_POINT('Ctrl Pts',(-54.4292218963253,-47.9282560258528,
12.));
#77494=CARTESIAN_POINT('Ctrl Pts',(-54.4176809711324,-47.9061375253909,
12.));
#77495=CARTESIAN_POINT('Ctrl Pts',(-54.4061375702088,-47.8840658024626,
12.));
#77496=CARTESIAN_POINT('Ctrl Pts',(-54.3945917942835,-47.8620409276495,
12.));
#77497=CARTESIAN_POINT('Ctrl Pts',(-54.3830437445275,-47.8400629717352,
12.));
#77498=CARTESIAN_POINT('Ctrl Pts',(-54.3714935225585,-47.8181320056988,
12.));
#77499=CARTESIAN_POINT('Ctrl Pts',(-54.3599412304431,-47.7962481007179,
12.));
#77500=CARTESIAN_POINT('Ctrl Pts',(-54.3483869706998,-47.7744113281768,
12.));
#77501=CARTESIAN_POINT('Ctrl Pts',(-54.3368308463023,-47.7526217596694,
12.));
#77502=CARTESIAN_POINT('Ctrl Pts',(-54.3252729606824,-47.7308794669994,
12.));
#77503=CARTESIAN_POINT('Ctrl Pts',(-54.3137134177345,-47.7091845221748,
12.));
#77504=CARTESIAN_POINT('Ctrl Pts',(-54.3021523218188,-47.6875369974086,
12.));
#77505=CARTESIAN_POINT('Ctrl Pts',(-54.2905897777647,-47.6659369651299,
12.));
#77506=CARTESIAN_POINT('Ctrl Pts',(-54.2790258908736,-47.6443844979846,
12.));
#77507=CARTESIAN_POINT('Ctrl Pts',(-54.2674607669228,-47.6228796688376,
12.));
#77508=CARTESIAN_POINT('Ctrl Pts',(-54.2558945121684,-47.6014225507664,
12.));
#77509=CARTESIAN_POINT('Ctrl Pts',(-54.2443272333498,-47.5800132170614,
12.));
#77510=CARTESIAN_POINT('Ctrl Pts',(-54.232759037693,-47.5586517412368,12.));
#77511=CARTESIAN_POINT('Ctrl Pts',(-54.2211900329141,-47.5373381970328,
12.));
#77512=CARTESIAN_POINT('Ctrl Pts',(-54.2096203272228,-47.5160726584172,
12.));
#77513=CARTESIAN_POINT('Ctrl Pts',(-54.1980500293267,-47.4948551995799,
12.));
#77514=CARTESIAN_POINT('Ctrl Pts',(-54.1864792484343,-47.473685894932,12.));
#77515=CARTESIAN_POINT('Ctrl Pts',(-54.1749080942593,-47.4525648191173,
12.));
#77516=CARTESIAN_POINT('Ctrl Pts',(-54.163336677024,-47.4314920470142,12.));
#77517=CARTESIAN_POINT('Ctrl Pts',(-54.1517651074638,-47.4104676537381,
12.));
#77518=CARTESIAN_POINT('Ctrl Pts',(-54.1401934968306,-47.3894917146361,
12.));
#77519=CARTESIAN_POINT('Ctrl Pts',(-54.1286219568981,-47.3685643052867,
12.));
#77520=CARTESIAN_POINT('Ctrl Pts',(-54.1170505999637,-47.3476855015095,
12.));
#77521=CARTESIAN_POINT('Ctrl Pts',(-54.1054795388538,-47.326855379369,12.));
#77522=CARTESIAN_POINT('Ctrl Pts',(-54.0939088869271,-47.3060740151754,
12.));
#77523=CARTESIAN_POINT('Ctrl Pts',(-54.082338758079,-47.2853414854805,12.));
#77524=CARTESIAN_POINT('Ctrl Pts',(-54.0707692667461,-47.2646578670767,
12.));
#77525=CARTESIAN_POINT('Ctrl Pts',(-54.0592005279108,-47.2440232370085,
12.));
#77526=CARTESIAN_POINT('Ctrl Pts',(-54.047632657105,-47.2234376725752,12.));
#77527=CARTESIAN_POINT('Ctrl Pts',(-54.0360657704156,-47.2029012513334,
12.));
#77528=CARTESIAN_POINT('Ctrl Pts',(-54.0244999844872,-47.1824140510906,
12.));
#77529=CARTESIAN_POINT('Ctrl Pts',(-54.0129354165269,-47.161976149906,12.));
#77530=CARTESIAN_POINT('Ctrl Pts',(-54.0013721843094,-47.1415876261012,
12.));
#77531=CARTESIAN_POINT('Ctrl Pts',(-53.9898104061809,-47.1212485582632,
12.));
#77532=CARTESIAN_POINT('Ctrl Pts',(-53.9782502010642,-47.1009590252466,
12.));
#77533=CARTESIAN_POINT('Ctrl Pts',(-53.9666916884624,-47.0807191061674,
12.));
#77534=CARTESIAN_POINT('Ctrl Pts',(-53.9551349884637,-47.0605288804042,
12.));
#77535=CARTESIAN_POINT('Ctrl Pts',(-53.9435802217468,-47.04038842761,12.));
#77536=CARTESIAN_POINT('Ctrl Pts',(-53.9320275095864,-47.0202978277148,
12.));
#77537=CARTESIAN_POINT('Ctrl Pts',(-53.9204769738584,-47.0002571609286,
12.));
#77538=CARTESIAN_POINT('Ctrl Pts',(-53.9089287370436,-46.9802665077342,
12.));
#77539=CARTESIAN_POINT('Ctrl Pts',(-53.8973829222317,-46.9603259488894,
12.));
#77540=CARTESIAN_POINT('Ctrl Pts',(-53.8858396531277,-46.9404355654381,
12.));
#77541=CARTESIAN_POINT('Ctrl Pts',(-53.8742990540557,-46.9205954387128,
12.));
#77542=CARTESIAN_POINT('Ctrl Pts',(-53.8627612499648,-46.900805650336,12.));
#77543=CARTESIAN_POINT('Ctrl Pts',(-53.851226366434,-46.8810662822147,12.));
#77544=CARTESIAN_POINT('Ctrl Pts',(-53.8396945296777,-46.8613774165452,
12.));
#77545=CARTESIAN_POINT('Ctrl Pts',(-53.8281658665517,-46.8417391358231,
12.));
#77546=CARTESIAN_POINT('Ctrl Pts',(-53.8166405045582,-46.8221515228459,
12.));
#77547=CARTESIAN_POINT('Ctrl Pts',(-53.8051185718525,-46.8026146607144,
12.));
#77548=CARTESIAN_POINT('Ctrl Pts',(-53.7936001972468,-46.7831286328268,
12.));
#77549=CARTESIAN_POINT('Ctrl Pts',(-53.782085510217,-46.7636935228851,12.));
#77550=CARTESIAN_POINT('Ctrl Pts',(-53.770574640907,-46.7443094149041,12.));
#77551=CARTESIAN_POINT('Ctrl Pts',(-53.7590677201344,-46.724976393213,12.));
#77552=CARTESIAN_POINT('Ctrl Pts',(-53.7475648793948,-46.7056945424559,
12.));
#77553=CARTESIAN_POINT('Ctrl Pts',(-53.7360662508677,-46.6864639475863,
12.));
#77554=CARTESIAN_POINT('Ctrl Pts',(-53.7245719674222,-46.6672846938752,
12.));
#77555=CARTESIAN_POINT('Ctrl Pts',(-53.7130821626263,-46.6481568669216,
12.));
#77556=CARTESIAN_POINT('Ctrl Pts',(-53.701596970754,-46.6290805526559,12.));
#77557=CARTESIAN_POINT('Ctrl Pts',(-53.6901165267941,-46.6100558373402,
12.));
#77558=CARTESIAN_POINT('Ctrl Pts',(-53.678640966456,-46.5910828075653,12.));
#77559=CARTESIAN_POINT('Ctrl Pts',(-53.6671704261737,-46.5721615502591,
12.));
#77560=CARTESIAN_POINT('Ctrl Pts',(-53.6557050431071,-46.5532921526901,
12.));
#77561=CARTESIAN_POINT('Ctrl Pts',(-53.6442449551455,-46.5344747024676,
12.));
#77562=CARTESIAN_POINT('Ctrl Pts',(-53.6327903009094,-46.5157092875373,
12.));
#77563=CARTESIAN_POINT('Ctrl Pts',(-53.6213412197533,-46.496995996177,12.));
#77564=CARTESIAN_POINT('Ctrl Pts',(-53.6098978517859,-46.4783349170173,
12.));
#77565=CARTESIAN_POINT('Ctrl Pts',(-53.5984603378855,-46.459726139052,12.));
#77566=CARTESIAN_POINT('Ctrl Pts',(-53.5870288197166,-46.4411697516478,
12.));
#77567=CARTESIAN_POINT('Ctrl Pts',(-53.5756034397481,-46.4226658445474,
12.));
#77568=CARTESIAN_POINT('Ctrl Pts',(-53.5641843412559,-46.4042145078701,
12.));
#77569=CARTESIAN_POINT('Ctrl Pts',(-53.5527716683048,-46.3858158321059,
12.));
#77570=CARTESIAN_POINT('Ctrl Pts',(-53.5413655657327,-46.3674699081046,
12.));
#77571=CARTESIAN_POINT('Ctrl Pts',(-53.5299661791385,-46.3491768270655,
12.));
#77572=CARTESIAN_POINT('Ctrl Pts',(-53.5185736548548,-46.3309366805093,
12.));
#77573=CARTESIAN_POINT('Ctrl Pts',(-53.5071881399911,-46.3127495603098,
12.));
#77574=CARTESIAN_POINT('Ctrl Pts',(-53.4958097825006,-46.2946155587417,
12.));
#77575=CARTESIAN_POINT('Ctrl Pts',(-53.4844387312414,-46.2765347685198,
12.));
#77576=CARTESIAN_POINT('Ctrl Pts',(-53.4730751360371,-46.2585072828353,
12.));
#77577=CARTESIAN_POINT('Ctrl Pts',(-53.4617191477402,-46.2405331953889,
12.));
#77578=CARTESIAN_POINT('Ctrl Pts',(-53.4503709181178,-46.2226126003202,
12.));
#77579=CARTESIAN_POINT('Ctrl Pts',(-53.4390305997274,-46.2047455921286,
12.));
#77580=CARTESIAN_POINT('Ctrl Pts',(-53.4276983458125,-46.1869322656024,
12.));
#77581=CARTESIAN_POINT('Ctrl Pts',(-53.4163743101517,-46.1691727157134,
12.));
#77582=CARTESIAN_POINT('Ctrl Pts',(-53.4050586470436,-46.1514670376012,
12.));
#77583=CARTESIAN_POINT('Ctrl Pts',(-53.3937515116549,-46.1338153268097,
12.));
#77584=CARTESIAN_POINT('Ctrl Pts',(-53.3824530603276,-46.1162176794884,
12.));
#77585=CARTESIAN_POINT('Ctrl Pts',(-53.3711634508437,-46.0986741925656,
12.));
#77586=CARTESIAN_POINT('Ctrl Pts',(-53.3598828428546,-46.0811849640218,
12.));
#77587=CARTESIAN_POINT('Ctrl Pts',(-53.3486113975901,-46.0637500926982,
12.));
#77588=CARTESIAN_POINT('Ctrl Pts',(-53.3373492770671,-46.0463696777801,
12.));
#77589=CARTESIAN_POINT('Ctrl Pts',(-53.326096643428,-46.02904381836,12.));
#77590=CARTESIAN_POINT('Ctrl Pts',(-53.3148536582635,-46.0117726129873,
12.));
#77591=CARTESIAN_POINT('Ctrl Pts',(-53.3036204818329,-45.9945561591453,
12.));
#77592=CARTESIAN_POINT('Ctrl Pts',(-53.292397274555,-45.9773945542384,12.));
#77593=CARTESIAN_POINT('Ctrl Pts',(-53.2811841987926,-45.9602878967698,
12.));
#77594=CARTESIAN_POINT('Ctrl Pts',(-53.2699814203105,-45.9432362873008,
12.));
#77595=CARTESIAN_POINT('Ctrl Pts',(-53.2587891103866,-45.9262398298349,
12.));
#77596=CARTESIAN_POINT('Ctrl Pts',(-53.2476074460017,-45.9092986319377,
12.));
#77597=CARTESIAN_POINT('Ctrl Pts',(-53.2364366054306,-45.892412801838,12.));
#77598=CARTESIAN_POINT('Ctrl Pts',(-53.2252767643662,-45.8755824458723,
12.));
#77599=CARTESIAN_POINT('Ctrl Pts',(-53.2141280925439,-45.8588076662582,
12.));
#77600=CARTESIAN_POINT('Ctrl Pts',(-53.2029907483557,-45.8420885575349,
12.));
#77601=CARTESIAN_POINT('Ctrl Pts',(-53.1918648840541,-45.8254252099957,
12.));
#77602=CARTESIAN_POINT('Ctrl Pts',(-53.1807506560933,-45.808817716509,12.));
#77603=CARTESIAN_POINT('Ctrl Pts',(-53.1696482334487,-45.7922661780005,
12.));
#77604=CARTESIAN_POINT('Ctrl Pts',(-53.1585578076444,-45.7757707100618,
12.));
#77605=CARTESIAN_POINT('Ctrl Pts',(-53.1474795996053,-45.7593314474501,
12.));
#77606=CARTESIAN_POINT('Ctrl Pts',(-53.1364138384693,-45.7429485300823,
12.));
#77607=CARTESIAN_POINT('Ctrl Pts',(-53.1253607414872,-45.7266220897003,
12.));
#77608=CARTESIAN_POINT('Ctrl Pts',(-53.114320495492,-45.7103522376696,12.));
#77609=CARTESIAN_POINT('Ctrl Pts',(-53.1032932328857,-45.694139048907,12.));
#77610=CARTESIAN_POINT('Ctrl Pts',(-53.0922790298409,-45.6779825614231,
12.));
#77611=CARTESIAN_POINT('Ctrl Pts',(-53.0834781451546,-45.6651027439241,
12.));
#77612=CARTESIAN_POINT('Ctrl Pts',(-53.0768833804193,-45.6554684028145,
12.));
#77613=CARTESIAN_POINT('Ctrl Pts',(-53.0724894921849,-45.6490568514089,
12.));
#77614=CARTESIAN_POINT('Ctrl Pts',(-53.0702932034641,-45.6458539113724,
12.));
#77615=CARTESIAN_POINT('Ctrl Pts',(-54.1946543500373,-50.6869108458851,
-1.11022302462516E-15));
#77616=CARTESIAN_POINT('Ctrl Pts',(-54.1946543500373,-50.6869108458851,
4.));
#77617=CARTESIAN_POINT('Ctrl Pts',(-54.1946543500373,-50.6869108458851,
8.));
#77618=CARTESIAN_POINT('Ctrl Pts',(-54.1946543500373,-50.6869108458851,
12.));
#77619=CARTESIAN_POINT('Ctrl Pts',(-54.2986513683568,-50.7223900873023,
-1.11022302462516E-15));
#77620=CARTESIAN_POINT('Ctrl Pts',(-54.2986513683568,-50.7223900873023,
4.));
#77621=CARTESIAN_POINT('Ctrl Pts',(-54.2986513683568,-50.7223900873023,
8.));
#77622=CARTESIAN_POINT('Ctrl Pts',(-54.2986513683568,-50.7223900873023,
12.));
#77623=CARTESIAN_POINT('Ctrl Pts',(-54.5013145669267,-50.7219766588197,
-1.03713937562159E-15));
#77624=CARTESIAN_POINT('Ctrl Pts',(-54.5013145669267,-50.7219766588197,
4.));
#77625=CARTESIAN_POINT('Ctrl Pts',(-54.5013145669267,-50.7219766588197,
7.99999999999999));
#77626=CARTESIAN_POINT('Ctrl Pts',(-54.5013145669267,-50.7219766588197,
12.));
#77627=CARTESIAN_POINT('Ctrl Pts',(-54.6674453828701,-50.6135081477658,
-8.63611844427818E-16));
#77628=CARTESIAN_POINT('Ctrl Pts',(-54.6674453828701,-50.6135081477658,
4.));
#77629=CARTESIAN_POINT('Ctrl Pts',(-54.6674453828701,-50.6135081477658,
8.));
#77630=CARTESIAN_POINT('Ctrl Pts',(-54.6674453828701,-50.6135081477658,
12.));
#77631=CARTESIAN_POINT('Ctrl Pts',(-54.7233670476834,-50.55297319609,-7.79957864200068E-16));
#77632=CARTESIAN_POINT('Ctrl Pts',(-54.7233670476834,-50.55297319609,4.));
#77633=CARTESIAN_POINT('Ctrl Pts',(-54.7233670476834,-50.55297319609,8.));
#77634=CARTESIAN_POINT('Ctrl Pts',(-54.7233670476834,-50.55297319609,12.));
#77635=CARTESIAN_POINT('',(-54.1946543500373,-50.6869108458851,0.));
#77636=CARTESIAN_POINT('',(-54.723367047683,-50.5529731960897,0.));
#77637=CARTESIAN_POINT('Ctrl Pts',(-54.1946543500373,-50.6869108458851,
8.74764948622162E-18));
#77638=CARTESIAN_POINT('Ctrl Pts',(-54.2986513683568,-50.7223900873023,
8.74764948622131E-18));
#77639=CARTESIAN_POINT('Ctrl Pts',(-54.4144589103968,-50.7221538424551,
5.05097346311187E-17));
#77640=CARTESIAN_POINT('Ctrl Pts',(-54.5183375111709,-50.6866343053397,
1.25069822123835E-16));
#77641=CARTESIAN_POINT('Ctrl Pts',(-54.5962464617515,-50.6599946525032,
1.80989887743373E-16));
#77642=CARTESIAN_POINT('Ctrl Pts',(-54.6674453828701,-50.6135081477658,
2.55358829683559E-16));
#77643=CARTESIAN_POINT('Ctrl Pts',(-54.7233670476834,-50.55297319609,3.3901280991131E-16));
#77644=CARTESIAN_POINT('',(-54.723367047683,-50.5529731960897,12.));
#77645=CARTESIAN_POINT('Ctrl Pts',(-54.7233670476834,-50.55297319609,-7.79957864200068E-16));
#77646=CARTESIAN_POINT('Ctrl Pts',(-54.7233670476834,-50.55297319609,4.));
#77647=CARTESIAN_POINT('Ctrl Pts',(-54.7233670476834,-50.55297319609,8.));
#77648=CARTESIAN_POINT('Ctrl Pts',(-54.7233670476834,-50.55297319609,12.));
#77649=CARTESIAN_POINT('',(-54.1946543500373,-50.6869108458851,12.));
#77650=CARTESIAN_POINT('Ctrl Pts',(-54.7233670476834,-50.55297319609,12.));
#77651=CARTESIAN_POINT('Ctrl Pts',(-54.6674453828701,-50.6135081477658,
12.));
#77652=CARTESIAN_POINT('Ctrl Pts',(-54.5962464617515,-50.6599946525032,
12.));
#77653=CARTESIAN_POINT('Ctrl Pts',(-54.5183375111709,-50.6866343053397,
12.));
#77654=CARTESIAN_POINT('Ctrl Pts',(-54.4144589103968,-50.7221538424551,
12.));
#77655=CARTESIAN_POINT('Ctrl Pts',(-54.2986513683568,-50.7223900873023,
12.));
#77656=CARTESIAN_POINT('Ctrl Pts',(-54.1946543500373,-50.6869108458851,
12.));
#77657=CARTESIAN_POINT('Ctrl Pts',(-54.1946543500373,-50.6869108458851,
12.));
#77658=CARTESIAN_POINT('Ctrl Pts',(-54.1946543500373,-50.6869108458851,
8.));
#77659=CARTESIAN_POINT('Ctrl Pts',(-54.1946543500373,-50.6869108458851,
4.));
#77660=CARTESIAN_POINT('Ctrl Pts',(-54.1946543500373,-50.6869108458851,
-1.11022302462516E-15));
#77661=CARTESIAN_POINT('Origin',(-2.7629675461203E-10,-2.53313958019842E-10,
0.));
#77662=CARTESIAN_POINT('Origin',(-2.7629675461203E-10,-2.53313958019842E-10,
12.));
#77663=CARTESIAN_POINT('Origin',(-2.7629675461203E-10,-2.53313958019842E-10,
0.));
#77664=CARTESIAN_POINT('Ctrl Pts',(-59.2875729049545,-45.1135644683471,
-5.55111512312578E-16));
#77665=CARTESIAN_POINT('Ctrl Pts',(-59.2875729049545,-45.1135644683471,
4.));
#77666=CARTESIAN_POINT('Ctrl Pts',(-59.2875729049545,-45.113564468347,8.));
#77667=CARTESIAN_POINT('Ctrl Pts',(-59.2875729049545,-45.113564468347,12.));
#77668=CARTESIAN_POINT('Ctrl Pts',(-59.3541123643618,-45.0261193041895,
-5.55111512312578E-16));
#77669=CARTESIAN_POINT('Ctrl Pts',(-59.3541123643618,-45.0261193041895,
4.));
#77670=CARTESIAN_POINT('Ctrl Pts',(-59.3541123643618,-45.0261193041895,
8.));
#77671=CARTESIAN_POINT('Ctrl Pts',(-59.3541123643618,-45.0261193041895,
12.));
#77672=CARTESIAN_POINT('Ctrl Pts',(-59.4177951463802,-44.8337211159574,
-5.55111512312578E-16));
#77673=CARTESIAN_POINT('Ctrl Pts',(-59.4177951463802,-44.8337211159574,
4.));
#77674=CARTESIAN_POINT('Ctrl Pts',(-59.4177951463802,-44.8337211159573,
8.));
#77675=CARTESIAN_POINT('Ctrl Pts',(-59.4177951463802,-44.8337211159573,
12.));
#77676=CARTESIAN_POINT('Ctrl Pts',(-59.3674150879747,-44.6418181989797,
-5.55111512312578E-16));
#77677=CARTESIAN_POINT('Ctrl Pts',(-59.3674150879747,-44.6418181989797,
4.));
#77678=CARTESIAN_POINT('Ctrl Pts',(-59.3674150879747,-44.6418181989796,
8.00000000000001));
#77679=CARTESIAN_POINT('Ctrl Pts',(-59.3674150879747,-44.6418181989796,
12.));
#77680=CARTESIAN_POINT('Ctrl Pts',(-59.3276657444156,-44.5696260757421,
-5.55111512312578E-16));
#77681=CARTESIAN_POINT('Ctrl Pts',(-59.3276657444156,-44.5696260757421,
4.));
#77682=CARTESIAN_POINT('Ctrl Pts',(-59.3276657444156,-44.5696260757421,
8.));
#77683=CARTESIAN_POINT('Ctrl Pts',(-59.3276657444156,-44.5696260757421,
12.));
#77684=CARTESIAN_POINT('',(-59.2875729049545,-45.1135644683471,0.));
#77685=CARTESIAN_POINT('',(-59.3276657444158,-44.5696260757421,0.));
#77686=CARTESIAN_POINT('Ctrl Pts',(-59.2875729049545,-45.1135644683471,
-5.55111512312578E-16));
#77687=CARTESIAN_POINT('Ctrl Pts',(-59.3541123643618,-45.0261193041895,
-5.55111512312578E-16));
#77688=CARTESIAN_POINT('Ctrl Pts',(-59.3905025255151,-44.9161774823426,
-5.55111512312578E-16));
#77689=CARTESIAN_POINT('Ctrl Pts',(-59.3896476775505,-44.8063973817216,
-5.55111512312578E-16));
#77690=CARTESIAN_POINT('Ctrl Pts',(-59.389006541577,-44.7240623062559,-5.55111512312578E-16));
#77691=CARTESIAN_POINT('Ctrl Pts',(-59.3674150879747,-44.6418181989797,
-5.55111512312578E-16));
#77692=CARTESIAN_POINT('Ctrl Pts',(-59.3276657444156,-44.5696260757421,
-5.55111512312578E-16));
#77693=CARTESIAN_POINT('',(-59.3276657444158,-44.569626075742,12.));
#77694=CARTESIAN_POINT('Ctrl Pts',(-59.3276657444156,-44.5696260757421,
-5.55111512312578E-16));
#77695=CARTESIAN_POINT('Ctrl Pts',(-59.3276657444156,-44.5696260757421,
4.));
#77696=CARTESIAN_POINT('Ctrl Pts',(-59.3276657444156,-44.5696260757421,
8.));
#77697=CARTESIAN_POINT('Ctrl Pts',(-59.3276657444156,-44.5696260757421,
12.));
#77698=CARTESIAN_POINT('',(-59.2875729049545,-45.113564468347,12.));
#77699=CARTESIAN_POINT('Ctrl Pts',(-59.3276657444156,-44.5696260757421,
12.));
#77700=CARTESIAN_POINT('Ctrl Pts',(-59.3674150879747,-44.6418181989796,
12.));
#77701=CARTESIAN_POINT('Ctrl Pts',(-59.3890065415771,-44.7240623062558,
12.));
#77702=CARTESIAN_POINT('Ctrl Pts',(-59.3896476775505,-44.8063973817216,
12.));
#77703=CARTESIAN_POINT('Ctrl Pts',(-59.3905025255152,-44.9161774823425,
12.));
#77704=CARTESIAN_POINT('Ctrl Pts',(-59.3541123643618,-45.0261193041895,
12.));
#77705=CARTESIAN_POINT('Ctrl Pts',(-59.2875729049545,-45.113564468347,12.));
#77706=CARTESIAN_POINT('Ctrl Pts',(-59.2875729049545,-45.113564468347,12.));
#77707=CARTESIAN_POINT('Ctrl Pts',(-59.2875729049545,-45.113564468347,8.));
#77708=CARTESIAN_POINT('Ctrl Pts',(-59.2875729049545,-45.1135644683471,
4.));
#77709=CARTESIAN_POINT('Ctrl Pts',(-59.2875729049545,-45.1135644683471,
-5.55111512312578E-16));
#77710=CARTESIAN_POINT('Ctrl Pts',(-56.8466430164621,-40.8467768343956,
0.));
#77711=CARTESIAN_POINT('Ctrl Pts',(-56.8466430164621,-40.8467768343956,
12.));
#77712=CARTESIAN_POINT('Ctrl Pts',(-56.8491101022591,-40.8497761671036,
0.));
#77713=CARTESIAN_POINT('Ctrl Pts',(-56.8491101022591,-40.8497761671036,
12.));
#77714=CARTESIAN_POINT('Ctrl Pts',(-56.8540460739472,-40.8557803680277,
0.));
#77715=CARTESIAN_POINT('Ctrl Pts',(-56.8540460739472,-40.8557803680277,
12.));
#77716=CARTESIAN_POINT('Ctrl Pts',(-56.8614554317668,-40.864803275942,0.));
#77717=CARTESIAN_POINT('Ctrl Pts',(-56.8614554317668,-40.864803275942,12.));
#77718=CARTESIAN_POINT('Ctrl Pts',(-56.8713453764905,-40.8768670342052,
0.));
#77719=CARTESIAN_POINT('Ctrl Pts',(-56.8713453764905,-40.8768670342052,
12.));
#77720=CARTESIAN_POINT('Ctrl Pts',(-56.8837257978343,-40.8920020903293,
0.));
#77721=CARTESIAN_POINT('Ctrl Pts',(-56.8837257978343,-40.8920020903293,
12.));
#77722=CARTESIAN_POINT('Ctrl Pts',(-56.8961241708861,-40.9071924937508,
0.));
#77723=CARTESIAN_POINT('Ctrl Pts',(-56.8961241708861,-40.9071924937508,
12.));
#77724=CARTESIAN_POINT('Ctrl Pts',(-56.9085404164502,-40.9224382132427,
0.));
#77725=CARTESIAN_POINT('Ctrl Pts',(-56.9085404164502,-40.9224382132427,
12.));
#77726=CARTESIAN_POINT('Ctrl Pts',(-56.9209743960992,-40.9377391857128,
0.));
#77727=CARTESIAN_POINT('Ctrl Pts',(-56.9209743960992,-40.9377391857128,
12.));
#77728=CARTESIAN_POINT('Ctrl Pts',(-56.9334259140049,-40.9530953165031,
0.));
#77729=CARTESIAN_POINT('Ctrl Pts',(-56.9334259140049,-40.9530953165031,
12.));
#77730=CARTESIAN_POINT('Ctrl Pts',(-56.9458947422608,-40.9685064933074,
0.));
#77731=CARTESIAN_POINT('Ctrl Pts',(-56.9458947422608,-40.9685064933074,
12.));
#77732=CARTESIAN_POINT('Ctrl Pts',(-56.9583806404069,-40.9839725967121,
0.));
#77733=CARTESIAN_POINT('Ctrl Pts',(-56.9583806404069,-40.9839725967121,
12.));
#77734=CARTESIAN_POINT('Ctrl Pts',(-56.9708833766137,-40.9994935117276,
0.));
#77735=CARTESIAN_POINT('Ctrl Pts',(-56.9708833766137,-40.9994935117276,
12.));
#77736=CARTESIAN_POINT('Ctrl Pts',(-56.9834027500117,-41.0150691398947,
0.));
#77737=CARTESIAN_POINT('Ctrl Pts',(-56.9834027500117,-41.0150691398947,
12.));
#77738=CARTESIAN_POINT('Ctrl Pts',(-56.995938583472,-41.0306993953988,0.));
#77739=CARTESIAN_POINT('Ctrl Pts',(-56.995938583472,-41.0306993953988,12.));
#77740=CARTESIAN_POINT('Ctrl Pts',(-57.008490713042,-41.0463841993608,0.));
#77741=CARTESIAN_POINT('Ctrl Pts',(-57.008490713042,-41.0463841993608,12.));
#77742=CARTESIAN_POINT('Ctrl Pts',(-57.0210589791788,-41.0621234751007,
0.));
#77743=CARTESIAN_POINT('Ctrl Pts',(-57.0210589791788,-41.0621234751007,
12.));
#77744=CARTESIAN_POINT('Ctrl Pts',(-57.0336432158536,-41.0779171422438,
0.));
#77745=CARTESIAN_POINT('Ctrl Pts',(-57.0336432158536,-41.0779171422438,
12.));
#77746=CARTESIAN_POINT('Ctrl Pts',(-57.046243245068,-41.0937651137549,0.));
#77747=CARTESIAN_POINT('Ctrl Pts',(-57.046243245068,-41.0937651137549,12.));
#77748=CARTESIAN_POINT('Ctrl Pts',(-57.0588588825298,-41.1096672990148,
0.));
#77749=CARTESIAN_POINT('Ctrl Pts',(-57.0588588825298,-41.1096672990148,
12.));
#77750=CARTESIAN_POINT('Ctrl Pts',(-57.0714899412099,-41.1256236057442,
0.));
#77751=CARTESIAN_POINT('Ctrl Pts',(-57.0714899412099,-41.1256236057442,
12.));
#77752=CARTESIAN_POINT('Ctrl Pts',(-57.084136235426,-41.1416339422117,0.));
#77753=CARTESIAN_POINT('Ctrl Pts',(-57.084136235426,-41.1416339422117,12.));
#77754=CARTESIAN_POINT('Ctrl Pts',(-57.0967975854874,-41.1576982197374,
0.));
#77755=CARTESIAN_POINT('Ctrl Pts',(-57.0967975854874,-41.1576982197374,
12.));
#77756=CARTESIAN_POINT('Ctrl Pts',(-57.1094738174957,-41.1738163525901,
0.));
#77757=CARTESIAN_POINT('Ctrl Pts',(-57.1094738174957,-41.1738163525901,
12.));
#77758=CARTESIAN_POINT('Ctrl Pts',(-57.1221647611207,-41.1899882567923,
0.));
#77759=CARTESIAN_POINT('Ctrl Pts',(-57.1221647611207,-41.1899882567923,
12.));
#77760=CARTESIAN_POINT('Ctrl Pts',(-57.1348702480647,-41.2062138492915,
0.));
#77761=CARTESIAN_POINT('Ctrl Pts',(-57.1348702480647,-41.2062138492915,
12.));
#77762=CARTESIAN_POINT('Ctrl Pts',(-57.147590110182,-41.222493046943,0.));
#77763=CARTESIAN_POINT('Ctrl Pts',(-57.147590110182,-41.222493046943,12.));
#77764=CARTESIAN_POINT('Ctrl Pts',(-57.1603241779077,-41.2388257656559,
0.));
#77765=CARTESIAN_POINT('Ctrl Pts',(-57.1603241779077,-41.2388257656559,
12.));
#77766=CARTESIAN_POINT('Ctrl Pts',(-57.17307228108,-41.2552119208465,0.));
#77767=CARTESIAN_POINT('Ctrl Pts',(-57.17307228108,-41.2552119208465,12.));
#77768=CARTESIAN_POINT('Ctrl Pts',(-57.1858342496538,-41.2716514278276,
0.));
#77769=CARTESIAN_POINT('Ctrl Pts',(-57.1858342496538,-41.2716514278276,
12.));
#77770=CARTESIAN_POINT('Ctrl Pts',(-57.1986099143983,-41.2881442021863,
0.));
#77771=CARTESIAN_POINT('Ctrl Pts',(-57.1986099143983,-41.2881442021863,
12.));
#77772=CARTESIAN_POINT('Ctrl Pts',(-57.2113991077302,-41.3046901602293,
0.));
#77773=CARTESIAN_POINT('Ctrl Pts',(-57.2113991077302,-41.3046901602293,
12.));
#77774=CARTESIAN_POINT('Ctrl Pts',(-57.2242016640198,-41.321289219149,0.));
#77775=CARTESIAN_POINT('Ctrl Pts',(-57.2242016640198,-41.321289219149,12.));
#77776=CARTESIAN_POINT('Ctrl Pts',(-57.2370174191401,-41.3379412967875,
0.));
#77777=CARTESIAN_POINT('Ctrl Pts',(-57.2370174191401,-41.3379412967875,
12.));
#77778=CARTESIAN_POINT('Ctrl Pts',(-57.2498462101879,-41.3546463114885,
0.));
#77779=CARTESIAN_POINT('Ctrl Pts',(-57.2498462101879,-41.3546463114885,
12.));
#77780=CARTESIAN_POINT('Ctrl Pts',(-57.2626878751596,-41.3714041819223,
0.));
#77781=CARTESIAN_POINT('Ctrl Pts',(-57.2626878751596,-41.3714041819223,
12.));
#77782=CARTESIAN_POINT('Ctrl Pts',(-57.2755422525844,-41.3882148268813,
0.));
#77783=CARTESIAN_POINT('Ctrl Pts',(-57.2755422525844,-41.3882148268813,
12.));
#77784=CARTESIAN_POINT('Ctrl Pts',(-57.2884091815406,-41.4050781652938,
0.));
#77785=CARTESIAN_POINT('Ctrl Pts',(-57.2884091815406,-41.4050781652938,
12.));
#77786=CARTESIAN_POINT('Ctrl Pts',(-57.3012885018151,-41.4219941163163,
0.));
#77787=CARTESIAN_POINT('Ctrl Pts',(-57.3012885018151,-41.4219941163163,
12.));
#77788=CARTESIAN_POINT('Ctrl Pts',(-57.3141800540137,-41.4389625993948,
0.));
#77789=CARTESIAN_POINT('Ctrl Pts',(-57.3141800540137,-41.4389625993948,
12.));
#77790=CARTESIAN_POINT('Ctrl Pts',(-57.3270836796911,-41.4559835343328,
0.));
#77791=CARTESIAN_POINT('Ctrl Pts',(-57.3270836796911,-41.4559835343328,
12.));
#77792=CARTESIAN_POINT('Ctrl Pts',(-57.3399992214717,-41.4730568413518,
0.));
#77793=CARTESIAN_POINT('Ctrl Pts',(-57.3399992214717,-41.4730568413518,
12.));
#77794=CARTESIAN_POINT('Ctrl Pts',(-57.3529265229835,-41.4901824410636,
0.));
#77795=CARTESIAN_POINT('Ctrl Pts',(-57.3529265229835,-41.4901824410636,
12.));
#77796=CARTESIAN_POINT('Ctrl Pts',(-57.3658654287937,-41.5073602544396,
0.));
#77797=CARTESIAN_POINT('Ctrl Pts',(-57.3658654287937,-41.5073602544396,
12.));
#77798=CARTESIAN_POINT('Ctrl Pts',(-57.3788157843454,-41.524590202777,0.));
#77799=CARTESIAN_POINT('Ctrl Pts',(-57.3788157843454,-41.524590202777,12.));
#77800=CARTESIAN_POINT('Ctrl Pts',(-57.3917774358863,-41.5418722076572,
0.));
#77801=CARTESIAN_POINT('Ctrl Pts',(-57.3917774358863,-41.5418722076572,
12.));
#77802=CARTESIAN_POINT('Ctrl Pts',(-57.4047502304231,-41.5592061909176,
0.));
#77803=CARTESIAN_POINT('Ctrl Pts',(-57.4047502304231,-41.5592061909176,
12.));
#77804=CARTESIAN_POINT('Ctrl Pts',(-57.4177340157508,-41.5765920746777,
0.));
#77805=CARTESIAN_POINT('Ctrl Pts',(-57.4177340157508,-41.5765920746777,
12.));
#77806=CARTESIAN_POINT('Ctrl Pts',(-57.4307286404662,-41.5940297813477,
0.));
#77807=CARTESIAN_POINT('Ctrl Pts',(-57.4307286404662,-41.5940297813477,
12.));
#77808=CARTESIAN_POINT('Ctrl Pts',(-57.4437339539841,-41.6115192336388,
0.));
#77809=CARTESIAN_POINT('Ctrl Pts',(-57.4437339539841,-41.6115192336388,
12.));
#77810=CARTESIAN_POINT('Ctrl Pts',(-57.4567498065562,-41.6290603545666,
0.));
#77811=CARTESIAN_POINT('Ctrl Pts',(-57.4567498065562,-41.6290603545666,
12.));
#77812=CARTESIAN_POINT('Ctrl Pts',(-57.4697760492683,-41.6466530674514,
0.));
#77813=CARTESIAN_POINT('Ctrl Pts',(-57.4697760492683,-41.6466530674514,
12.));
#77814=CARTESIAN_POINT('Ctrl Pts',(-57.4828125340218,-41.6642972959165,
0.));
#77815=CARTESIAN_POINT('Ctrl Pts',(-57.4828125340218,-41.6642972959165,
12.));
#77816=CARTESIAN_POINT('Ctrl Pts',(-57.4958591135165,-41.6819929638797,
0.));
#77817=CARTESIAN_POINT('Ctrl Pts',(-57.4958591135165,-41.6819929638797,
12.));
#77818=CARTESIAN_POINT('Ctrl Pts',(-57.5089156412343,-41.6997399955447,
0.));
#77819=CARTESIAN_POINT('Ctrl Pts',(-57.5089156412343,-41.6997399955447,
12.));
#77820=CARTESIAN_POINT('Ctrl Pts',(-57.5219819714171,-41.7175383153821,
0.));
#77821=CARTESIAN_POINT('Ctrl Pts',(-57.5219819714171,-41.7175383153821,
12.));
#77822=CARTESIAN_POINT('Ctrl Pts',(-57.5350579590649,-41.7353878481336,
0.));
#77823=CARTESIAN_POINT('Ctrl Pts',(-57.5350579590649,-41.7353878481336,
12.));
#77824=CARTESIAN_POINT('Ctrl Pts',(-57.5481434599335,-41.7532885188174,
0.));
#77825=CARTESIAN_POINT('Ctrl Pts',(-57.5481434599335,-41.7532885188174,
12.));
#77826=CARTESIAN_POINT('Ctrl Pts',(-57.561238330532,-41.7712402527273,0.));
#77827=CARTESIAN_POINT('Ctrl Pts',(-57.561238330532,-41.7712402527273,12.));
#77828=CARTESIAN_POINT('Ctrl Pts',(-57.5743424281205,-41.7892429754297,
0.));
#77829=CARTESIAN_POINT('Ctrl Pts',(-57.5743424281205,-41.7892429754297,
12.));
#77830=CARTESIAN_POINT('Ctrl Pts',(-57.5874556107056,-41.8072966127558,
0.));
#77831=CARTESIAN_POINT('Ctrl Pts',(-57.5874556107056,-41.8072966127558,
12.));
#77832=CARTESIAN_POINT('Ctrl Pts',(-57.6005777370349,-41.8254010908051,
0.));
#77833=CARTESIAN_POINT('Ctrl Pts',(-57.6005777370349,-41.8254010908051,
12.));
#77834=CARTESIAN_POINT('Ctrl Pts',(-57.6137086665882,-41.8435563359456,
0.));
#77835=CARTESIAN_POINT('Ctrl Pts',(-57.6137086665882,-41.8435563359456,
12.));
#77836=CARTESIAN_POINT('Ctrl Pts',(-57.6268482595702,-41.8617622748108,
0.));
#77837=CARTESIAN_POINT('Ctrl Pts',(-57.6268482595702,-41.8617622748108,
12.));
#77838=CARTESIAN_POINT('Ctrl Pts',(-57.6399963769003,-41.8800188342908,
0.));
#77839=CARTESIAN_POINT('Ctrl Pts',(-57.6399963769003,-41.8800188342908,
12.));
#77840=CARTESIAN_POINT('Ctrl Pts',(-57.6531528802059,-41.8983259415244,
0.));
#77841=CARTESIAN_POINT('Ctrl Pts',(-57.6531528802059,-41.8983259415244,
12.));
#77842=CARTESIAN_POINT('Ctrl Pts',(-57.6663176318176,-41.9166835239046,
0.));
#77843=CARTESIAN_POINT('Ctrl Pts',(-57.6663176318176,-41.9166835239046,
12.));
#77844=CARTESIAN_POINT('Ctrl Pts',(-57.6794904947641,-41.9350915090791,
0.));
#77845=CARTESIAN_POINT('Ctrl Pts',(-57.6794904947641,-41.9350915090791,
12.));
#77846=CARTESIAN_POINT('Ctrl Pts',(-57.6926713327674,-41.9535498249489,
0.));
#77847=CARTESIAN_POINT('Ctrl Pts',(-57.6926713327674,-41.9535498249489,
12.));
#77848=CARTESIAN_POINT('Ctrl Pts',(-57.7058600102365,-41.9720583996601,
0.));
#77849=CARTESIAN_POINT('Ctrl Pts',(-57.7058600102365,-41.9720583996601,
12.));
#77850=CARTESIAN_POINT('Ctrl Pts',(-57.7190563922614,-41.9906171615974,
0.));
#77851=CARTESIAN_POINT('Ctrl Pts',(-57.7190563922614,-41.9906171615974,
12.));
#77852=CARTESIAN_POINT('Ctrl Pts',(-57.7322603446086,-42.0092260393911,
0.));
#77853=CARTESIAN_POINT('Ctrl Pts',(-57.7322603446086,-42.0092260393911,
12.));
#77854=CARTESIAN_POINT('Ctrl Pts',(-57.7454717337151,-42.0278849619156,
0.));
#77855=CARTESIAN_POINT('Ctrl Pts',(-57.7454717337151,-42.0278849619156,
12.));
#77856=CARTESIAN_POINT('Ctrl Pts',(-57.7586904266828,-42.0465938582877,
0.));
#77857=CARTESIAN_POINT('Ctrl Pts',(-57.7586904266828,-42.0465938582877,
12.));
#77858=CARTESIAN_POINT('Ctrl Pts',(-57.7719162912721,-42.0653526578571,
0.));
#77859=CARTESIAN_POINT('Ctrl Pts',(-57.7719162912721,-42.0653526578571,
12.));
#77860=CARTESIAN_POINT('Ctrl Pts',(-57.7851491958954,-42.0841612902018,
0.));
#77861=CARTESIAN_POINT('Ctrl Pts',(-57.7851491958954,-42.0841612902018,
12.));
#77862=CARTESIAN_POINT('Ctrl Pts',(-57.798389009613,-42.1030196851344,0.));
#77863=CARTESIAN_POINT('Ctrl Pts',(-57.798389009613,-42.1030196851344,12.));
#77864=CARTESIAN_POINT('Ctrl Pts',(-57.8116356021274,-42.121927772701,0.));
#77865=CARTESIAN_POINT('Ctrl Pts',(-57.8116356021274,-42.121927772701,12.));
#77866=CARTESIAN_POINT('Ctrl Pts',(-57.8248888437787,-42.1408854831791,
0.));
#77867=CARTESIAN_POINT('Ctrl Pts',(-57.8248888437787,-42.1408854831791,
12.));
#77868=CARTESIAN_POINT('Ctrl Pts',(-57.8381486055376,-42.1598927470671,
0.));
#77869=CARTESIAN_POINT('Ctrl Pts',(-57.8381486055376,-42.1598927470671,
12.));
#77870=CARTESIAN_POINT('Ctrl Pts',(-57.8514147590012,-42.1789494950824,
0.));
#77871=CARTESIAN_POINT('Ctrl Pts',(-57.8514147590012,-42.1789494950824,
12.));
#77872=CARTESIAN_POINT('Ctrl Pts',(-57.86468717639,-42.1980556581688,0.));
#77873=CARTESIAN_POINT('Ctrl Pts',(-57.86468717639,-42.1980556581688,12.));
#77874=CARTESIAN_POINT('Ctrl Pts',(-57.8779657305423,-42.2172111674945,
0.));
#77875=CARTESIAN_POINT('Ctrl Pts',(-57.8779657305423,-42.2172111674945,
12.));
#77876=CARTESIAN_POINT('Ctrl Pts',(-57.8912502949084,-42.2364159544492,
0.));
#77877=CARTESIAN_POINT('Ctrl Pts',(-57.8912502949084,-42.2364159544492,
12.));
#77878=CARTESIAN_POINT('Ctrl Pts',(-57.9045407435447,-42.2556699506332,
0.));
#77879=CARTESIAN_POINT('Ctrl Pts',(-57.9045407435447,-42.2556699506332,
12.));
#77880=CARTESIAN_POINT('Ctrl Pts',(-57.9178369511084,-42.274973087857,0.));
#77881=CARTESIAN_POINT('Ctrl Pts',(-57.9178369511084,-42.274973087857,12.));
#77882=CARTESIAN_POINT('Ctrl Pts',(-57.9311387928541,-42.2943252981471,
0.));
#77883=CARTESIAN_POINT('Ctrl Pts',(-57.9311387928541,-42.2943252981471,
12.));
#77884=CARTESIAN_POINT('Ctrl Pts',(-57.9444461446292,-42.3137265137446,
0.));
#77885=CARTESIAN_POINT('Ctrl Pts',(-57.9444461446292,-42.3137265137446,
12.));
#77886=CARTESIAN_POINT('Ctrl Pts',(-57.9577588828693,-42.3331766671028,
0.));
#77887=CARTESIAN_POINT('Ctrl Pts',(-57.9577588828693,-42.3331766671028,
12.));
#77888=CARTESIAN_POINT('Ctrl Pts',(-57.9710768845923,-42.3526756908764,
0.));
#77889=CARTESIAN_POINT('Ctrl Pts',(-57.9710768845923,-42.3526756908764,
12.));
#77890=CARTESIAN_POINT('Ctrl Pts',(-57.9844000273936,-42.3722235179216,
0.));
#77891=CARTESIAN_POINT('Ctrl Pts',(-57.9844000273936,-42.3722235179216,
12.));
#77892=CARTESIAN_POINT('Ctrl Pts',(-57.9977281894437,-42.3918200813024,
0.));
#77893=CARTESIAN_POINT('Ctrl Pts',(-57.9977281894437,-42.3918200813024,
12.));
#77894=CARTESIAN_POINT('Ctrl Pts',(-58.011061249483,-42.4114653142891,0.));
#77895=CARTESIAN_POINT('Ctrl Pts',(-58.011061249483,-42.4114653142891,12.));
#77896=CARTESIAN_POINT('Ctrl Pts',(-58.0243990868175,-42.4311591503551,
0.));
#77897=CARTESIAN_POINT('Ctrl Pts',(-58.0243990868175,-42.4311591503551,
12.));
#77898=CARTESIAN_POINT('Ctrl Pts',(-58.0377415813132,-42.4509015231667,
0.));
#77899=CARTESIAN_POINT('Ctrl Pts',(-58.0377415813132,-42.4509015231667,
12.));
#77900=CARTESIAN_POINT('Ctrl Pts',(-58.0510886133917,-42.4706923665838,
0.));
#77901=CARTESIAN_POINT('Ctrl Pts',(-58.0510886133917,-42.4706923665838,
12.));
#77902=CARTESIAN_POINT('Ctrl Pts',(-58.064440064027,-42.4905316146649,0.));
#77903=CARTESIAN_POINT('Ctrl Pts',(-58.064440064027,-42.4905316146649,12.));
#77904=CARTESIAN_POINT('Ctrl Pts',(-58.0777958147404,-42.5104192016664,
0.));
#77905=CARTESIAN_POINT('Ctrl Pts',(-58.0777958147404,-42.5104192016664,
12.));
#77906=CARTESIAN_POINT('Ctrl Pts',(-58.0911557475967,-42.5303550620388,
0.));
#77907=CARTESIAN_POINT('Ctrl Pts',(-58.0911557475967,-42.5303550620388,
12.));
#77908=CARTESIAN_POINT('Ctrl Pts',(-58.1045197452003,-42.5503391304182,
0.));
#77909=CARTESIAN_POINT('Ctrl Pts',(-58.1045197452003,-42.5503391304182,
12.));
#77910=CARTESIAN_POINT('Ctrl Pts',(-58.1178876906905,-42.5703713416263,
0.));
#77911=CARTESIAN_POINT('Ctrl Pts',(-58.1178876906905,-42.5703713416263,
12.));
#77912=CARTESIAN_POINT('Ctrl Pts',(-58.1312594677383,-42.5904516306759,
0.));
#77913=CARTESIAN_POINT('Ctrl Pts',(-58.1312594677383,-42.5904516306759,
12.));
#77914=CARTESIAN_POINT('Ctrl Pts',(-58.1446349605419,-42.6105799327697,
0.));
#77915=CARTESIAN_POINT('Ctrl Pts',(-58.1446349605419,-42.6105799327697,
12.));
#77916=CARTESIAN_POINT('Ctrl Pts',(-58.158014053823,-42.6307561832977,0.));
#77917=CARTESIAN_POINT('Ctrl Pts',(-58.158014053823,-42.6307561832977,12.));
#77918=CARTESIAN_POINT('Ctrl Pts',(-58.1713966328217,-42.6509803178269,
0.));
#77919=CARTESIAN_POINT('Ctrl Pts',(-58.1713966328217,-42.6509803178269,
12.));
#77920=CARTESIAN_POINT('Ctrl Pts',(-58.1847825832932,-42.6712522721021,
0.));
#77921=CARTESIAN_POINT('Ctrl Pts',(-58.1847825832932,-42.6712522721021,
12.));
#77922=CARTESIAN_POINT('Ctrl Pts',(-58.1981717915043,-42.6915719820516,
0.));
#77923=CARTESIAN_POINT('Ctrl Pts',(-58.1981717915043,-42.6915719820516,
12.));
#77924=CARTESIAN_POINT('Ctrl Pts',(-58.2115641442302,-42.7119393837866,
0.));
#77925=CARTESIAN_POINT('Ctrl Pts',(-58.2115641442302,-42.7119393837866,
12.));
#77926=CARTESIAN_POINT('Ctrl Pts',(-58.2249595287497,-42.7323544135983,
0.));
#77927=CARTESIAN_POINT('Ctrl Pts',(-58.2249595287497,-42.7323544135983,
12.));
#77928=CARTESIAN_POINT('Ctrl Pts',(-58.238357832842,-42.7528170079482,0.));
#77929=CARTESIAN_POINT('Ctrl Pts',(-58.238357832842,-42.7528170079482,12.));
#77930=CARTESIAN_POINT('Ctrl Pts',(-58.2517589447818,-42.7733271034678,
0.));
#77931=CARTESIAN_POINT('Ctrl Pts',(-58.2517589447818,-42.7733271034678,
12.));
#77932=CARTESIAN_POINT('Ctrl Pts',(-58.2651627533368,-42.7938846369651,
0.));
#77933=CARTESIAN_POINT('Ctrl Pts',(-58.2651627533368,-42.7938846369651,
12.));
#77934=CARTESIAN_POINT('Ctrl Pts',(-58.278569147764,-42.8144895454234,0.));
#77935=CARTESIAN_POINT('Ctrl Pts',(-58.278569147764,-42.8144895454234,12.));
#77936=CARTESIAN_POINT('Ctrl Pts',(-58.2919780178063,-42.8351417659998,
0.));
#77937=CARTESIAN_POINT('Ctrl Pts',(-58.2919780178063,-42.8351417659998,
12.));
#77938=CARTESIAN_POINT('Ctrl Pts',(-58.305389253689,-42.8558412360154,0.));
#77939=CARTESIAN_POINT('Ctrl Pts',(-58.305389253689,-42.8558412360154,12.));
#77940=CARTESIAN_POINT('Ctrl Pts',(-58.3188027461158,-42.8765878929545,
0.));
#77941=CARTESIAN_POINT('Ctrl Pts',(-58.3188027461158,-42.8765878929545,
12.));
#77942=CARTESIAN_POINT('Ctrl Pts',(-58.3322183862647,-42.8973816744703,
0.));
#77943=CARTESIAN_POINT('Ctrl Pts',(-58.3322183862647,-42.8973816744703,
12.));
#77944=CARTESIAN_POINT('Ctrl Pts',(-58.3456360657861,-42.9182225183851,
0.));
#77945=CARTESIAN_POINT('Ctrl Pts',(-58.3456360657861,-42.9182225183851,
12.));
#77946=CARTESIAN_POINT('Ctrl Pts',(-58.3590556767981,-42.9391103626881,
0.));
#77947=CARTESIAN_POINT('Ctrl Pts',(-58.3590556767981,-42.9391103626881,
12.));
#77948=CARTESIAN_POINT('Ctrl Pts',(-58.3724771118835,-42.9600451455267,
0.));
#77949=CARTESIAN_POINT('Ctrl Pts',(-58.3724771118835,-42.9600451455267,
12.));
#77950=CARTESIAN_POINT('Ctrl Pts',(-58.3859002640871,-42.9810268052043,
0.));
#77951=CARTESIAN_POINT('Ctrl Pts',(-58.3859002640871,-42.9810268052043,
12.));
#77952=CARTESIAN_POINT('Ctrl Pts',(-58.3993250269115,-43.0020552801869,
0.));
#77953=CARTESIAN_POINT('Ctrl Pts',(-58.3993250269115,-43.0020552801869,
12.));
#77954=CARTESIAN_POINT('Ctrl Pts',(-58.4127512943144,-43.0231305091032,
0.));
#77955=CARTESIAN_POINT('Ctrl Pts',(-58.4127512943144,-43.0231305091032,
12.));
#77956=CARTESIAN_POINT('Ctrl Pts',(-58.4261789607055,-43.0442524307432,
0.));
#77957=CARTESIAN_POINT('Ctrl Pts',(-58.4261789607055,-43.0442524307432,
12.));
#77958=CARTESIAN_POINT('Ctrl Pts',(-58.4396079209438,-43.0654209840502,
0.));
#77959=CARTESIAN_POINT('Ctrl Pts',(-58.4396079209438,-43.0654209840502,
12.));
#77960=CARTESIAN_POINT('Ctrl Pts',(-58.4530380703335,-43.0866361081166,
0.));
#77961=CARTESIAN_POINT('Ctrl Pts',(-58.4530380703335,-43.0866361081166,
12.));
#77962=CARTESIAN_POINT('Ctrl Pts',(-58.4664693046206,-43.1078977421908,
0.));
#77963=CARTESIAN_POINT('Ctrl Pts',(-58.4664693046206,-43.1078977421908,
12.));
#77964=CARTESIAN_POINT('Ctrl Pts',(-58.4799015199904,-43.1292058256774,
0.));
#77965=CARTESIAN_POINT('Ctrl Pts',(-58.4799015199904,-43.1292058256774,
12.));
#77966=CARTESIAN_POINT('Ctrl Pts',(-58.4933346130638,-43.1505602981366,
0.));
#77967=CARTESIAN_POINT('Ctrl Pts',(-58.4933346130638,-43.1505602981366,
12.));
#77968=CARTESIAN_POINT('Ctrl Pts',(-58.5067684808946,-43.1719610992771,
0.));
#77969=CARTESIAN_POINT('Ctrl Pts',(-58.5067684808946,-43.1719610992771,
12.));
#77970=CARTESIAN_POINT('Ctrl Pts',(-58.5202030209667,-43.1934081689503,
0.));
#77971=CARTESIAN_POINT('Ctrl Pts',(-58.5202030209667,-43.1934081689503,
12.));
#77972=CARTESIAN_POINT('Ctrl Pts',(-58.5336381311911,-43.214901447157,0.));
#77973=CARTESIAN_POINT('Ctrl Pts',(-58.5336381311911,-43.214901447157,12.));
#77974=CARTESIAN_POINT('Ctrl Pts',(-58.5470737099027,-43.2364408740488,
0.));
#77975=CARTESIAN_POINT('Ctrl Pts',(-58.5470737099027,-43.2364408740488,
12.));
#77976=CARTESIAN_POINT('Ctrl Pts',(-58.5605096558578,-43.2580263899278,
0.));
#77977=CARTESIAN_POINT('Ctrl Pts',(-58.5605096558578,-43.2580263899278,
12.));
#77978=CARTESIAN_POINT('Ctrl Pts',(-58.5739458682317,-43.2796579352405,
0.));
#77979=CARTESIAN_POINT('Ctrl Pts',(-58.5739458682317,-43.2796579352405,
12.));
#77980=CARTESIAN_POINT('Ctrl Pts',(-58.5873822466163,-43.3013354505707,
0.));
#77981=CARTESIAN_POINT('Ctrl Pts',(-58.5873822466163,-43.3013354505707,
12.));
#77982=CARTESIAN_POINT('Ctrl Pts',(-58.6008186910166,-43.3230588766455,
0.));
#77983=CARTESIAN_POINT('Ctrl Pts',(-58.6008186910166,-43.3230588766455,
12.));
#77984=CARTESIAN_POINT('Ctrl Pts',(-58.6142551018473,-43.3448281543374,
0.));
#77985=CARTESIAN_POINT('Ctrl Pts',(-58.6142551018473,-43.3448281543374,
12.));
#77986=CARTESIAN_POINT('Ctrl Pts',(-58.627691379929,-43.3666432246634,0.));
#77987=CARTESIAN_POINT('Ctrl Pts',(-58.627691379929,-43.3666432246634,12.));
#77988=CARTESIAN_POINT('Ctrl Pts',(-58.6411274264854,-43.3885040287808,
0.));
#77989=CARTESIAN_POINT('Ctrl Pts',(-58.6411274264854,-43.3885040287808,
12.));
#77990=CARTESIAN_POINT('Ctrl Pts',(-58.6545631431388,-43.4104105079766,
0.));
#77991=CARTESIAN_POINT('Ctrl Pts',(-58.6545631431388,-43.4104105079766,
12.));
#77992=CARTESIAN_POINT('Ctrl Pts',(-58.6679984319095,-43.4323626036736,
0.));
#77993=CARTESIAN_POINT('Ctrl Pts',(-58.6679984319095,-43.4323626036736,
12.));
#77994=CARTESIAN_POINT('Ctrl Pts',(-58.6814331952138,-43.4543602574352,
0.));
#77995=CARTESIAN_POINT('Ctrl Pts',(-58.6814331952138,-43.4543602574352,
12.));
#77996=CARTESIAN_POINT('Ctrl Pts',(-58.6948673358639,-43.4764034109654,
0.));
#77997=CARTESIAN_POINT('Ctrl Pts',(-58.6948673358639,-43.4764034109654,
12.));
#77998=CARTESIAN_POINT('Ctrl Pts',(-58.708300757066,-43.4984920061071,0.));
#77999=CARTESIAN_POINT('Ctrl Pts',(-58.708300757066,-43.4984920061071,12.));
#78000=CARTESIAN_POINT('Ctrl Pts',(-58.7217333624206,-43.5206259848333,
0.));
#78001=CARTESIAN_POINT('Ctrl Pts',(-58.7217333624206,-43.5206259848333,
12.));
#78002=CARTESIAN_POINT('Ctrl Pts',(-58.7351650559176,-43.5428052892483,
0.));
#78003=CARTESIAN_POINT('Ctrl Pts',(-58.7351650559176,-43.5428052892483,
12.));
#78004=CARTESIAN_POINT('Ctrl Pts',(-58.7485957419296,-43.5650298615911,
0.));
#78005=CARTESIAN_POINT('Ctrl Pts',(-58.7485957419296,-43.5650298615911,
12.));
#78006=CARTESIAN_POINT('Ctrl Pts',(-58.7620253252059,-43.5872996442343,
0.));
#78007=CARTESIAN_POINT('Ctrl Pts',(-58.7620253252059,-43.5872996442343,
12.));
#78008=CARTESIAN_POINT('Ctrl Pts',(-58.7754537108672,-43.6096145796798,
0.));
#78009=CARTESIAN_POINT('Ctrl Pts',(-58.7754537108672,-43.6096145796798,
12.));
#78010=CARTESIAN_POINT('Ctrl Pts',(-58.7888808043976,-43.6319746105487,
0.));
#78011=CARTESIAN_POINT('Ctrl Pts',(-58.7888808043976,-43.6319746105487,
12.));
#78012=CARTESIAN_POINT('Ctrl Pts',(-58.8023065116446,-43.6543796795797,
0.));
#78013=CARTESIAN_POINT('Ctrl Pts',(-58.8023065116446,-43.6543796795797,
12.));
#78014=CARTESIAN_POINT('Ctrl Pts',(-58.8157307388247,-43.6768297296402,
0.));
#78015=CARTESIAN_POINT('Ctrl Pts',(-58.8157307388247,-43.6768297296402,
12.));
#78016=CARTESIAN_POINT('Ctrl Pts',(-58.8291533925299,-43.6993247037318,
0.));
#78017=CARTESIAN_POINT('Ctrl Pts',(-58.8291533925299,-43.6993247037318,
12.));
#78018=CARTESIAN_POINT('Ctrl Pts',(-58.8425743797325,-43.7218645449921,
0.));
#78019=CARTESIAN_POINT('Ctrl Pts',(-58.8425743797325,-43.7218645449921,
12.));
#78020=CARTESIAN_POINT('Ctrl Pts',(-58.8559936077933,-43.7444491966935,
0.));
#78021=CARTESIAN_POINT('Ctrl Pts',(-58.8559936077933,-43.7444491966935,
12.));
#78022=CARTESIAN_POINT('Ctrl Pts',(-58.8694109844636,-43.7670786022392,
0.));
#78023=CARTESIAN_POINT('Ctrl Pts',(-58.8694109844636,-43.7670786022392,
12.));
#78024=CARTESIAN_POINT('Ctrl Pts',(-58.882826417861,-43.7897527051599,0.));
#78025=CARTESIAN_POINT('Ctrl Pts',(-58.882826417861,-43.7897527051599,12.));
#78026=CARTESIAN_POINT('Ctrl Pts',(-58.8962398164486,-43.8124714491069,
0.));
#78027=CARTESIAN_POINT('Ctrl Pts',(-58.8962398164486,-43.8124714491069,
12.));
#78028=CARTESIAN_POINT('Ctrl Pts',(-58.9096510890128,-43.8352347778419,
0.));
#78029=CARTESIAN_POINT('Ctrl Pts',(-58.9096510890128,-43.8352347778419,
12.));
#78030=CARTESIAN_POINT('Ctrl Pts',(-58.9230601446445,-43.8580426352236,
0.));
#78031=CARTESIAN_POINT('Ctrl Pts',(-58.9230601446445,-43.8580426352236,
12.));
#78032=CARTESIAN_POINT('Ctrl Pts',(-58.9364668927132,-43.8808949651882,
0.));
#78033=CARTESIAN_POINT('Ctrl Pts',(-58.9364668927132,-43.8808949651882,
12.));
#78034=CARTESIAN_POINT('Ctrl Pts',(-58.9498712429066,-43.9037917117748,
0.));
#78035=CARTESIAN_POINT('Ctrl Pts',(-58.9498712429066,-43.9037917117748,
12.));
#78036=CARTESIAN_POINT('Ctrl Pts',(-58.9632731052704,-43.9267328191507,
0.));
#78037=CARTESIAN_POINT('Ctrl Pts',(-58.9632731052704,-43.9267328191507,
12.));
#78038=CARTESIAN_POINT('Ctrl Pts',(-58.9766723902531,-43.9497182316333,
0.));
#78039=CARTESIAN_POINT('Ctrl Pts',(-58.9766723902531,-43.9497182316333,
12.));
#78040=CARTESIAN_POINT('Ctrl Pts',(-58.9900690087404,-43.9727478937053,
0.));
#78041=CARTESIAN_POINT('Ctrl Pts',(-58.9900690087404,-43.9727478937053,
12.));
#78042=CARTESIAN_POINT('Ctrl Pts',(-59.0034628721161,-43.9958217500363,
0.));
#78043=CARTESIAN_POINT('Ctrl Pts',(-59.0034628721161,-43.9958217500363,
12.));
#78044=CARTESIAN_POINT('Ctrl Pts',(-59.0168538922087,-44.0189397454593,
0.));
#78045=CARTESIAN_POINT('Ctrl Pts',(-59.0168538922087,-44.0189397454593,
12.));
#78046=CARTESIAN_POINT('Ctrl Pts',(-59.0302419811772,-44.0421018249219,
0.));
#78047=CARTESIAN_POINT('Ctrl Pts',(-59.0302419811772,-44.0421018249219,
12.));
#78048=CARTESIAN_POINT('Ctrl Pts',(-59.0436270514085,-44.0653079334384,
0.));
#78049=CARTESIAN_POINT('Ctrl Pts',(-59.0436270514085,-44.0653079334384,
12.));
#78050=CARTESIAN_POINT('Ctrl Pts',(-59.0570090154243,-44.0885580160433,
0.));
#78051=CARTESIAN_POINT('Ctrl Pts',(-59.0570090154243,-44.0885580160433,
12.));
#78052=CARTESIAN_POINT('Ctrl Pts',(-59.0703877857529,-44.1118520177223,
0.));
#78053=CARTESIAN_POINT('Ctrl Pts',(-59.0703877857529,-44.1118520177223,
12.));
#78054=CARTESIAN_POINT('Ctrl Pts',(-59.0837632749209,-44.1351898834057,
0.));
#78055=CARTESIAN_POINT('Ctrl Pts',(-59.0837632749209,-44.1351898834057,
12.));
#78056=CARTESIAN_POINT('Ctrl Pts',(-59.0971353957218,-44.1585715581073,
0.));
#78057=CARTESIAN_POINT('Ctrl Pts',(-59.0971353957218,-44.1585715581073,
12.));
#78058=CARTESIAN_POINT('Ctrl Pts',(-59.1105040614285,-44.1819969870314,
0.));
#78059=CARTESIAN_POINT('Ctrl Pts',(-59.1105040614285,-44.1819969870314,
12.));
#78060=CARTESIAN_POINT('Ctrl Pts',(-59.1238691860307,-44.2054661156876,
0.));
#78061=CARTESIAN_POINT('Ctrl Pts',(-59.1238691860307,-44.2054661156876,
12.));
#78062=CARTESIAN_POINT('Ctrl Pts',(-59.1372306844575,-44.2289788899962,
0.));
#78063=CARTESIAN_POINT('Ctrl Pts',(-59.1372306844575,-44.2289788899962,
12.));
#78064=CARTESIAN_POINT('Ctrl Pts',(-59.1505884728194,-44.2525352563979,
0.));
#78065=CARTESIAN_POINT('Ctrl Pts',(-59.1505884728194,-44.2525352563979,
12.));
#78066=CARTESIAN_POINT('Ctrl Pts',(-59.1639424678766,-44.2761351616027,
0.));
#78067=CARTESIAN_POINT('Ctrl Pts',(-59.1639424678766,-44.2761351616027,
12.));
#78068=CARTESIAN_POINT('Ctrl Pts',(-59.1772925865191,-44.2997785523413,
0.));
#78069=CARTESIAN_POINT('Ctrl Pts',(-59.1772925865191,-44.2997785523413,
12.));
#78070=CARTESIAN_POINT('Ctrl Pts',(-59.1906387451971,-44.3234653750877,
0.));
#78071=CARTESIAN_POINT('Ctrl Pts',(-59.1906387451971,-44.3234653750877,
12.));
#78072=CARTESIAN_POINT('Ctrl Pts',(-59.2039808594765,-44.3471955758412,
0.));
#78073=CARTESIAN_POINT('Ctrl Pts',(-59.2039808594765,-44.3471955758412,
12.));
#78074=CARTESIAN_POINT('Ctrl Pts',(-59.217318843283,-44.3709690997495,0.));
#78075=CARTESIAN_POINT('Ctrl Pts',(-59.217318843283,-44.3709690997495,12.));
#78076=CARTESIAN_POINT('Ctrl Pts',(-59.2306526095175,-44.394785891411,0.));
#78077=CARTESIAN_POINT('Ctrl Pts',(-59.2306526095175,-44.394785891411,12.));
#78078=CARTESIAN_POINT('Ctrl Pts',(-59.2439820714231,-44.4186458955486,
0.));
#78079=CARTESIAN_POINT('Ctrl Pts',(-59.2439820714231,-44.4186458955486,
12.));
#78080=CARTESIAN_POINT('Ctrl Pts',(-59.2573071437801,-44.4425490575932,
0.));
#78081=CARTESIAN_POINT('Ctrl Pts',(-59.2573071437801,-44.4425490575932,
12.));
#78082=CARTESIAN_POINT('Ctrl Pts',(-59.2706277440438,-44.4664953242373,
0.));
#78083=CARTESIAN_POINT('Ctrl Pts',(-59.2706277440438,-44.4664953242373,
12.));
#78084=CARTESIAN_POINT('Ctrl Pts',(-59.2839437938187,-44.490484644147,0.));
#78085=CARTESIAN_POINT('Ctrl Pts',(-59.2839437938187,-44.490484644147,12.));
#78086=CARTESIAN_POINT('Ctrl Pts',(-59.2972552192072,-44.514516968128,0.));
#78087=CARTESIAN_POINT('Ctrl Pts',(-59.2972552192072,-44.514516968128,12.));
#78088=CARTESIAN_POINT('Ctrl Pts',(-59.3105619475512,-44.5385922475494,
0.));
#78089=CARTESIAN_POINT('Ctrl Pts',(-59.3105619475512,-44.5385922475494,
12.));
#78090=CARTESIAN_POINT('Ctrl Pts',(-59.3238639048618,-44.5627104330956,
0.));
#78091=CARTESIAN_POINT('Ctrl Pts',(-59.3238639048618,-44.5627104330956,
12.));
#78092=CARTESIAN_POINT('Ctrl Pts',(-59.3371610128494,-44.5868714733219,
0.));
#78093=CARTESIAN_POINT('Ctrl Pts',(-59.3371610128494,-44.5868714733219,
12.));
#78094=CARTESIAN_POINT('Ctrl Pts',(-59.3504531864223,-44.6110753134333,
0.));
#78095=CARTESIAN_POINT('Ctrl Pts',(-59.3504531864223,-44.6110753134333,
12.));
#78096=CARTESIAN_POINT('Ctrl Pts',(-59.3637403301959,-44.6353218935813,
0.));
#78097=CARTESIAN_POINT('Ctrl Pts',(-59.3637403301959,-44.6353218935813,
12.));
#78098=CARTESIAN_POINT('Ctrl Pts',(-59.3770223435405,-44.659611151286,0.));
#78099=CARTESIAN_POINT('Ctrl Pts',(-59.3770223435405,-44.659611151286,12.));
#78100=CARTESIAN_POINT('Ctrl Pts',(-59.3902991268094,-44.6839430244375,
0.));
#78101=CARTESIAN_POINT('Ctrl Pts',(-59.3902991268094,-44.6839430244375,
12.));
#78102=CARTESIAN_POINT('Ctrl Pts',(-59.403570587392,-44.708317454179,0.));
#78103=CARTESIAN_POINT('Ctrl Pts',(-59.403570587392,-44.708317454179,12.));
#78104=CARTESIAN_POINT('Ctrl Pts',(-59.4168366453047,-44.7327343876333,
0.));
#78105=CARTESIAN_POINT('Ctrl Pts',(-59.4168366453047,-44.7327343876333,
12.));
#78106=CARTESIAN_POINT('Ctrl Pts',(-59.4300972402943,-44.7571937811872,
0.));
#78107=CARTESIAN_POINT('Ctrl Pts',(-59.4300972402943,-44.7571937811872,
12.));
#78108=CARTESIAN_POINT('Ctrl Pts',(-59.4433523334651,-44.7816956017126,
0.));
#78109=CARTESIAN_POINT('Ctrl Pts',(-59.4433523334651,-44.7816956017126,
12.));
#78110=CARTESIAN_POINT('Ctrl Pts',(-59.4566019017674,-44.8062398250937,
0.));
#78111=CARTESIAN_POINT('Ctrl Pts',(-59.4566019017674,-44.8062398250937,
12.));
#78112=CARTESIAN_POINT('Ctrl Pts',(-59.4671971277837,-44.8259091133624,
0.));
#78113=CARTESIAN_POINT('Ctrl Pts',(-59.4671971277837,-44.8259091133624,
12.));
#78114=CARTESIAN_POINT('Ctrl Pts',(-59.475141054744,-44.8406801497506,0.));
#78115=CARTESIAN_POINT('Ctrl Pts',(-59.475141054744,-44.8406801497506,12.));
#78116=CARTESIAN_POINT('Ctrl Pts',(-59.4804358982977,-44.8505359826374,
0.));
#78117=CARTESIAN_POINT('Ctrl Pts',(-59.4804358982977,-44.8505359826374,
12.));
#78118=CARTESIAN_POINT('Ctrl Pts',(-59.483083043136,-44.8554660179045,0.));
#78119=CARTESIAN_POINT('Ctrl Pts',(-59.483083043136,-44.8554660179045,12.));
#78120=CARTESIAN_POINT('',(-56.8466430164621,-40.8467768343956,0.));
#78121=CARTESIAN_POINT('Ctrl Pts',(-56.8466430164621,-40.8467768343956,
0.));
#78122=CARTESIAN_POINT('Ctrl Pts',(-56.8491101022591,-40.8497761671036,
0.));
#78123=CARTESIAN_POINT('Ctrl Pts',(-56.8540460739472,-40.8557803680277,
0.));
#78124=CARTESIAN_POINT('Ctrl Pts',(-56.8614554317668,-40.864803275942,0.));
#78125=CARTESIAN_POINT('Ctrl Pts',(-56.8713453764905,-40.8768670342052,
0.));
#78126=CARTESIAN_POINT('Ctrl Pts',(-56.8837257978343,-40.8920020903293,
0.));
#78127=CARTESIAN_POINT('Ctrl Pts',(-56.8961241708861,-40.9071924937508,
0.));
#78128=CARTESIAN_POINT('Ctrl Pts',(-56.9085404164502,-40.9224382132427,
0.));
#78129=CARTESIAN_POINT('Ctrl Pts',(-56.9209743960992,-40.9377391857128,
0.));
#78130=CARTESIAN_POINT('Ctrl Pts',(-56.9334259140049,-40.9530953165031,
0.));
#78131=CARTESIAN_POINT('Ctrl Pts',(-56.9458947422608,-40.9685064933074,
0.));
#78132=CARTESIAN_POINT('Ctrl Pts',(-56.9583806404069,-40.9839725967121,
0.));
#78133=CARTESIAN_POINT('Ctrl Pts',(-56.9708833766137,-40.9994935117276,
0.));
#78134=CARTESIAN_POINT('Ctrl Pts',(-56.9834027500117,-41.0150691398947,
0.));
#78135=CARTESIAN_POINT('Ctrl Pts',(-56.995938583472,-41.0306993953988,0.));
#78136=CARTESIAN_POINT('Ctrl Pts',(-57.008490713042,-41.0463841993608,0.));
#78137=CARTESIAN_POINT('Ctrl Pts',(-57.0210589791788,-41.0621234751007,
0.));
#78138=CARTESIAN_POINT('Ctrl Pts',(-57.0336432158536,-41.0779171422438,
0.));
#78139=CARTESIAN_POINT('Ctrl Pts',(-57.046243245068,-41.0937651137549,0.));
#78140=CARTESIAN_POINT('Ctrl Pts',(-57.0588588825298,-41.1096672990148,
0.));
#78141=CARTESIAN_POINT('Ctrl Pts',(-57.0714899412099,-41.1256236057442,
0.));
#78142=CARTESIAN_POINT('Ctrl Pts',(-57.084136235426,-41.1416339422117,0.));
#78143=CARTESIAN_POINT('Ctrl Pts',(-57.0967975854874,-41.1576982197374,
0.));
#78144=CARTESIAN_POINT('Ctrl Pts',(-57.1094738174957,-41.1738163525901,
0.));
#78145=CARTESIAN_POINT('Ctrl Pts',(-57.1221647611207,-41.1899882567923,
0.));
#78146=CARTESIAN_POINT('Ctrl Pts',(-57.1348702480647,-41.2062138492915,
0.));
#78147=CARTESIAN_POINT('Ctrl Pts',(-57.147590110182,-41.222493046943,0.));
#78148=CARTESIAN_POINT('Ctrl Pts',(-57.1603241779077,-41.2388257656559,
0.));
#78149=CARTESIAN_POINT('Ctrl Pts',(-57.17307228108,-41.2552119208465,0.));
#78150=CARTESIAN_POINT('Ctrl Pts',(-57.1858342496538,-41.2716514278276,
0.));
#78151=CARTESIAN_POINT('Ctrl Pts',(-57.1986099143983,-41.2881442021863,
0.));
#78152=CARTESIAN_POINT('Ctrl Pts',(-57.2113991077302,-41.3046901602293,
0.));
#78153=CARTESIAN_POINT('Ctrl Pts',(-57.2242016640198,-41.321289219149,0.));
#78154=CARTESIAN_POINT('Ctrl Pts',(-57.2370174191401,-41.3379412967875,
0.));
#78155=CARTESIAN_POINT('Ctrl Pts',(-57.2498462101879,-41.3546463114885,
0.));
#78156=CARTESIAN_POINT('Ctrl Pts',(-57.2626878751596,-41.3714041819223,
0.));
#78157=CARTESIAN_POINT('Ctrl Pts',(-57.2755422525844,-41.3882148268813,
0.));
#78158=CARTESIAN_POINT('Ctrl Pts',(-57.2884091815406,-41.4050781652938,
0.));
#78159=CARTESIAN_POINT('Ctrl Pts',(-57.3012885018151,-41.4219941163163,
0.));
#78160=CARTESIAN_POINT('Ctrl Pts',(-57.3141800540137,-41.4389625993948,
0.));
#78161=CARTESIAN_POINT('Ctrl Pts',(-57.3270836796911,-41.4559835343328,
0.));
#78162=CARTESIAN_POINT('Ctrl Pts',(-57.3399992214717,-41.4730568413518,
0.));
#78163=CARTESIAN_POINT('Ctrl Pts',(-57.3529265229835,-41.4901824410636,
0.));
#78164=CARTESIAN_POINT('Ctrl Pts',(-57.3658654287937,-41.5073602544396,
0.));
#78165=CARTESIAN_POINT('Ctrl Pts',(-57.3788157843454,-41.524590202777,0.));
#78166=CARTESIAN_POINT('Ctrl Pts',(-57.3917774358863,-41.5418722076572,
0.));
#78167=CARTESIAN_POINT('Ctrl Pts',(-57.4047502304231,-41.5592061909176,
0.));
#78168=CARTESIAN_POINT('Ctrl Pts',(-57.4177340157508,-41.5765920746777,
0.));
#78169=CARTESIAN_POINT('Ctrl Pts',(-57.4307286404662,-41.5940297813477,
0.));
#78170=CARTESIAN_POINT('Ctrl Pts',(-57.4437339539841,-41.6115192336388,
0.));
#78171=CARTESIAN_POINT('Ctrl Pts',(-57.4567498065562,-41.6290603545666,
0.));
#78172=CARTESIAN_POINT('Ctrl Pts',(-57.4697760492683,-41.6466530674514,
0.));
#78173=CARTESIAN_POINT('Ctrl Pts',(-57.4828125340218,-41.6642972959165,
0.));
#78174=CARTESIAN_POINT('Ctrl Pts',(-57.4958591135165,-41.6819929638797,
0.));
#78175=CARTESIAN_POINT('Ctrl Pts',(-57.5089156412343,-41.6997399955447,
0.));
#78176=CARTESIAN_POINT('Ctrl Pts',(-57.5219819714171,-41.7175383153821,
0.));
#78177=CARTESIAN_POINT('Ctrl Pts',(-57.5350579590649,-41.7353878481336,
0.));
#78178=CARTESIAN_POINT('Ctrl Pts',(-57.5481434599335,-41.7532885188174,
0.));
#78179=CARTESIAN_POINT('Ctrl Pts',(-57.561238330532,-41.7712402527273,0.));
#78180=CARTESIAN_POINT('Ctrl Pts',(-57.5743424281205,-41.7892429754297,
0.));
#78181=CARTESIAN_POINT('Ctrl Pts',(-57.5874556107056,-41.8072966127558,
0.));
#78182=CARTESIAN_POINT('Ctrl Pts',(-57.6005777370349,-41.8254010908051,
0.));
#78183=CARTESIAN_POINT('Ctrl Pts',(-57.6137086665882,-41.8435563359456,
0.));
#78184=CARTESIAN_POINT('Ctrl Pts',(-57.6268482595702,-41.8617622748108,
0.));
#78185=CARTESIAN_POINT('Ctrl Pts',(-57.6399963769003,-41.8800188342908,
0.));
#78186=CARTESIAN_POINT('Ctrl Pts',(-57.6531528802059,-41.8983259415244,
0.));
#78187=CARTESIAN_POINT('Ctrl Pts',(-57.6663176318176,-41.9166835239046,
0.));
#78188=CARTESIAN_POINT('Ctrl Pts',(-57.6794904947641,-41.9350915090791,
0.));
#78189=CARTESIAN_POINT('Ctrl Pts',(-57.6926713327674,-41.9535498249489,
0.));
#78190=CARTESIAN_POINT('Ctrl Pts',(-57.7058600102365,-41.9720583996601,
0.));
#78191=CARTESIAN_POINT('Ctrl Pts',(-57.7190563922614,-41.9906171615974,
0.));
#78192=CARTESIAN_POINT('Ctrl Pts',(-57.7322603446086,-42.0092260393911,
0.));
#78193=CARTESIAN_POINT('Ctrl Pts',(-57.7454717337151,-42.0278849619156,
0.));
#78194=CARTESIAN_POINT('Ctrl Pts',(-57.7586904266828,-42.0465938582877,
0.));
#78195=CARTESIAN_POINT('Ctrl Pts',(-57.7719162912721,-42.0653526578571,
0.));
#78196=CARTESIAN_POINT('Ctrl Pts',(-57.7851491958954,-42.0841612902018,
0.));
#78197=CARTESIAN_POINT('Ctrl Pts',(-57.798389009613,-42.1030196851344,0.));
#78198=CARTESIAN_POINT('Ctrl Pts',(-57.8116356021274,-42.121927772701,0.));
#78199=CARTESIAN_POINT('Ctrl Pts',(-57.8248888437787,-42.1408854831791,
0.));
#78200=CARTESIAN_POINT('Ctrl Pts',(-57.8381486055376,-42.1598927470671,
0.));
#78201=CARTESIAN_POINT('Ctrl Pts',(-57.8514147590012,-42.1789494950824,
0.));
#78202=CARTESIAN_POINT('Ctrl Pts',(-57.86468717639,-42.1980556581688,0.));
#78203=CARTESIAN_POINT('Ctrl Pts',(-57.8779657305423,-42.2172111674945,
0.));
#78204=CARTESIAN_POINT('Ctrl Pts',(-57.8912502949084,-42.2364159544492,
0.));
#78205=CARTESIAN_POINT('Ctrl Pts',(-57.9045407435447,-42.2556699506332,
0.));
#78206=CARTESIAN_POINT('Ctrl Pts',(-57.9178369511084,-42.274973087857,0.));
#78207=CARTESIAN_POINT('Ctrl Pts',(-57.9311387928541,-42.2943252981471,
0.));
#78208=CARTESIAN_POINT('Ctrl Pts',(-57.9444461446292,-42.3137265137446,
0.));
#78209=CARTESIAN_POINT('Ctrl Pts',(-57.9577588828693,-42.3331766671028,
0.));
#78210=CARTESIAN_POINT('Ctrl Pts',(-57.9710768845923,-42.3526756908764,
0.));
#78211=CARTESIAN_POINT('Ctrl Pts',(-57.9844000273936,-42.3722235179216,
0.));
#78212=CARTESIAN_POINT('Ctrl Pts',(-57.9977281894437,-42.3918200813024,
0.));
#78213=CARTESIAN_POINT('Ctrl Pts',(-58.011061249483,-42.4114653142891,0.));
#78214=CARTESIAN_POINT('Ctrl Pts',(-58.0243990868175,-42.4311591503551,
0.));
#78215=CARTESIAN_POINT('Ctrl Pts',(-58.0377415813132,-42.4509015231667,
0.));
#78216=CARTESIAN_POINT('Ctrl Pts',(-58.0510886133917,-42.4706923665838,
0.));
#78217=CARTESIAN_POINT('Ctrl Pts',(-58.064440064027,-42.4905316146649,0.));
#78218=CARTESIAN_POINT('Ctrl Pts',(-58.0777958147404,-42.5104192016664,
0.));
#78219=CARTESIAN_POINT('Ctrl Pts',(-58.0911557475967,-42.5303550620388,
0.));
#78220=CARTESIAN_POINT('Ctrl Pts',(-58.1045197452003,-42.5503391304182,
0.));
#78221=CARTESIAN_POINT('Ctrl Pts',(-58.1178876906905,-42.5703713416263,
0.));
#78222=CARTESIAN_POINT('Ctrl Pts',(-58.1312594677383,-42.5904516306759,
0.));
#78223=CARTESIAN_POINT('Ctrl Pts',(-58.1446349605419,-42.6105799327697,
0.));
#78224=CARTESIAN_POINT('Ctrl Pts',(-58.158014053823,-42.6307561832977,0.));
#78225=CARTESIAN_POINT('Ctrl Pts',(-58.1713966328217,-42.6509803178269,
0.));
#78226=CARTESIAN_POINT('Ctrl Pts',(-58.1847825832932,-42.6712522721021,
0.));
#78227=CARTESIAN_POINT('Ctrl Pts',(-58.1981717915043,-42.6915719820516,
0.));
#78228=CARTESIAN_POINT('Ctrl Pts',(-58.2115641442302,-42.7119393837866,
0.));
#78229=CARTESIAN_POINT('Ctrl Pts',(-58.2249595287497,-42.7323544135983,
0.));
#78230=CARTESIAN_POINT('Ctrl Pts',(-58.238357832842,-42.7528170079482,0.));
#78231=CARTESIAN_POINT('Ctrl Pts',(-58.2517589447818,-42.7733271034678,
0.));
#78232=CARTESIAN_POINT('Ctrl Pts',(-58.2651627533368,-42.7938846369651,
0.));
#78233=CARTESIAN_POINT('Ctrl Pts',(-58.278569147764,-42.8144895454234,0.));
#78234=CARTESIAN_POINT('Ctrl Pts',(-58.2919780178063,-42.8351417659998,
0.));
#78235=CARTESIAN_POINT('Ctrl Pts',(-58.305389253689,-42.8558412360154,0.));
#78236=CARTESIAN_POINT('Ctrl Pts',(-58.3188027461158,-42.8765878929545,
0.));
#78237=CARTESIAN_POINT('Ctrl Pts',(-58.3322183862647,-42.8973816744703,
0.));
#78238=CARTESIAN_POINT('Ctrl Pts',(-58.3456360657861,-42.9182225183851,
0.));
#78239=CARTESIAN_POINT('Ctrl Pts',(-58.3590556767981,-42.9391103626881,
0.));
#78240=CARTESIAN_POINT('Ctrl Pts',(-58.3724771118835,-42.9600451455267,
0.));
#78241=CARTESIAN_POINT('Ctrl Pts',(-58.3859002640871,-42.9810268052043,
0.));
#78242=CARTESIAN_POINT('Ctrl Pts',(-58.3993250269115,-43.0020552801869,
0.));
#78243=CARTESIAN_POINT('Ctrl Pts',(-58.4127512943144,-43.0231305091032,
0.));
#78244=CARTESIAN_POINT('Ctrl Pts',(-58.4261789607055,-43.0442524307432,
0.));
#78245=CARTESIAN_POINT('Ctrl Pts',(-58.4396079209438,-43.0654209840502,
0.));
#78246=CARTESIAN_POINT('Ctrl Pts',(-58.4530380703335,-43.0866361081166,
0.));
#78247=CARTESIAN_POINT('Ctrl Pts',(-58.4664693046206,-43.1078977421908,
0.));
#78248=CARTESIAN_POINT('Ctrl Pts',(-58.4799015199904,-43.1292058256774,
0.));
#78249=CARTESIAN_POINT('Ctrl Pts',(-58.4933346130638,-43.1505602981366,
0.));
#78250=CARTESIAN_POINT('Ctrl Pts',(-58.5067684808946,-43.1719610992771,
0.));
#78251=CARTESIAN_POINT('Ctrl Pts',(-58.5202030209667,-43.1934081689503,
0.));
#78252=CARTESIAN_POINT('Ctrl Pts',(-58.5336381311911,-43.214901447157,0.));
#78253=CARTESIAN_POINT('Ctrl Pts',(-58.5470737099027,-43.2364408740488,
0.));
#78254=CARTESIAN_POINT('Ctrl Pts',(-58.5605096558578,-43.2580263899278,
0.));
#78255=CARTESIAN_POINT('Ctrl Pts',(-58.5739458682317,-43.2796579352405,
0.));
#78256=CARTESIAN_POINT('Ctrl Pts',(-58.5873822466163,-43.3013354505707,
0.));
#78257=CARTESIAN_POINT('Ctrl Pts',(-58.6008186910166,-43.3230588766455,
0.));
#78258=CARTESIAN_POINT('Ctrl Pts',(-58.6142551018473,-43.3448281543374,
0.));
#78259=CARTESIAN_POINT('Ctrl Pts',(-58.627691379929,-43.3666432246634,0.));
#78260=CARTESIAN_POINT('Ctrl Pts',(-58.6411274264854,-43.3885040287808,
0.));
#78261=CARTESIAN_POINT('Ctrl Pts',(-58.6545631431388,-43.4104105079766,
0.));
#78262=CARTESIAN_POINT('Ctrl Pts',(-58.6679984319095,-43.4323626036736,
0.));
#78263=CARTESIAN_POINT('Ctrl Pts',(-58.6814331952138,-43.4543602574352,
0.));
#78264=CARTESIAN_POINT('Ctrl Pts',(-58.6948673358639,-43.4764034109654,
0.));
#78265=CARTESIAN_POINT('Ctrl Pts',(-58.708300757066,-43.4984920061071,0.));
#78266=CARTESIAN_POINT('Ctrl Pts',(-58.7217333624206,-43.5206259848333,
0.));
#78267=CARTESIAN_POINT('Ctrl Pts',(-58.7351650559176,-43.5428052892483,
0.));
#78268=CARTESIAN_POINT('Ctrl Pts',(-58.7485957419296,-43.5650298615911,
0.));
#78269=CARTESIAN_POINT('Ctrl Pts',(-58.7620253252059,-43.5872996442343,
0.));
#78270=CARTESIAN_POINT('Ctrl Pts',(-58.7754537108672,-43.6096145796798,
0.));
#78271=CARTESIAN_POINT('Ctrl Pts',(-58.7888808043976,-43.6319746105487,
0.));
#78272=CARTESIAN_POINT('Ctrl Pts',(-58.8023065116446,-43.6543796795797,
0.));
#78273=CARTESIAN_POINT('Ctrl Pts',(-58.8157307388247,-43.6768297296402,
0.));
#78274=CARTESIAN_POINT('Ctrl Pts',(-58.8291533925299,-43.6993247037318,
0.));
#78275=CARTESIAN_POINT('Ctrl Pts',(-58.8425743797325,-43.7218645449921,
0.));
#78276=CARTESIAN_POINT('Ctrl Pts',(-58.8559936077933,-43.7444491966935,
0.));
#78277=CARTESIAN_POINT('Ctrl Pts',(-58.8694109844636,-43.7670786022392,
0.));
#78278=CARTESIAN_POINT('Ctrl Pts',(-58.882826417861,-43.7897527051599,0.));
#78279=CARTESIAN_POINT('Ctrl Pts',(-58.8962398164486,-43.8124714491069,
0.));
#78280=CARTESIAN_POINT('Ctrl Pts',(-58.9096510890128,-43.8352347778419,
0.));
#78281=CARTESIAN_POINT('Ctrl Pts',(-58.9230601446445,-43.8580426352236,
0.));
#78282=CARTESIAN_POINT('Ctrl Pts',(-58.9364668927132,-43.8808949651882,
0.));
#78283=CARTESIAN_POINT('Ctrl Pts',(-58.9498712429066,-43.9037917117748,
0.));
#78284=CARTESIAN_POINT('Ctrl Pts',(-58.9632731052704,-43.9267328191507,
0.));
#78285=CARTESIAN_POINT('Ctrl Pts',(-58.9766723902531,-43.9497182316333,
0.));
#78286=CARTESIAN_POINT('Ctrl Pts',(-58.9900690087404,-43.9727478937053,
0.));
#78287=CARTESIAN_POINT('Ctrl Pts',(-59.0034628721161,-43.9958217500363,
0.));
#78288=CARTESIAN_POINT('Ctrl Pts',(-59.0168538922087,-44.0189397454593,
0.));
#78289=CARTESIAN_POINT('Ctrl Pts',(-59.0302419811772,-44.0421018249219,
0.));
#78290=CARTESIAN_POINT('Ctrl Pts',(-59.0436270514085,-44.0653079334384,
0.));
#78291=CARTESIAN_POINT('Ctrl Pts',(-59.0570090154243,-44.0885580160433,
0.));
#78292=CARTESIAN_POINT('Ctrl Pts',(-59.0703877857529,-44.1118520177223,
0.));
#78293=CARTESIAN_POINT('Ctrl Pts',(-59.0837632749209,-44.1351898834057,
0.));
#78294=CARTESIAN_POINT('Ctrl Pts',(-59.0971353957218,-44.1585715581073,
0.));
#78295=CARTESIAN_POINT('Ctrl Pts',(-59.1105040614285,-44.1819969870314,
0.));
#78296=CARTESIAN_POINT('Ctrl Pts',(-59.1238691860307,-44.2054661156876,
0.));
#78297=CARTESIAN_POINT('Ctrl Pts',(-59.1372306844575,-44.2289788899962,
0.));
#78298=CARTESIAN_POINT('Ctrl Pts',(-59.1505884728194,-44.2525352563979,
0.));
#78299=CARTESIAN_POINT('Ctrl Pts',(-59.1639424678766,-44.2761351616027,
0.));
#78300=CARTESIAN_POINT('Ctrl Pts',(-59.1772925865191,-44.2997785523413,
0.));
#78301=CARTESIAN_POINT('Ctrl Pts',(-59.1906387451971,-44.3234653750877,
0.));
#78302=CARTESIAN_POINT('Ctrl Pts',(-59.2039808594765,-44.3471955758412,
0.));
#78303=CARTESIAN_POINT('Ctrl Pts',(-59.217318843283,-44.3709690997495,0.));
#78304=CARTESIAN_POINT('Ctrl Pts',(-59.2306526095175,-44.394785891411,0.));
#78305=CARTESIAN_POINT('Ctrl Pts',(-59.2439820714231,-44.4186458955486,
0.));
#78306=CARTESIAN_POINT('Ctrl Pts',(-59.2573071437801,-44.4425490575932,
0.));
#78307=CARTESIAN_POINT('Ctrl Pts',(-59.2706277440438,-44.4664953242373,
0.));
#78308=CARTESIAN_POINT('Ctrl Pts',(-59.2839437938187,-44.490484644147,0.));
#78309=CARTESIAN_POINT('Ctrl Pts',(-59.2972552192072,-44.514516968128,0.));
#78310=CARTESIAN_POINT('Ctrl Pts',(-59.3086616639392,-44.5351541478336,
0.));
#78311=CARTESIAN_POINT('Ctrl Pts',(-59.317404187219,-44.5509994357954,0.));
#78312=CARTESIAN_POINT('Ctrl Pts',(-59.3234848865278,-44.5620338188485,
0.));
#78313=CARTESIAN_POINT('Ctrl Pts',(-59.3269051738222,-44.5682447395713,
0.));
#78314=CARTESIAN_POINT('Ctrl Pts',(-59.3276657444158,-44.569626075742,0.));
#78315=CARTESIAN_POINT('',(-56.8466430164621,-40.8467768343956,12.));
#78316=CARTESIAN_POINT('',(-56.8466430164621,-40.8467768343956,0.));
#78317=CARTESIAN_POINT('Ctrl Pts',(-59.3276657444158,-44.569626075742,12.));
#78318=CARTESIAN_POINT('Ctrl Pts',(-59.3269051738222,-44.5682447395712,
12.));
#78319=CARTESIAN_POINT('Ctrl Pts',(-59.3234848865278,-44.5620338188485,
12.));
#78320=CARTESIAN_POINT('Ctrl Pts',(-59.317404187219,-44.5509994357953,12.));
#78321=CARTESIAN_POINT('Ctrl Pts',(-59.3086616639392,-44.5351541478336,
12.));
#78322=CARTESIAN_POINT('Ctrl Pts',(-59.2972552192072,-44.514516968128,12.));
#78323=CARTESIAN_POINT('Ctrl Pts',(-59.2839437938187,-44.490484644147,12.));
#78324=CARTESIAN_POINT('Ctrl Pts',(-59.2706277440438,-44.4664953242373,
12.));
#78325=CARTESIAN_POINT('Ctrl Pts',(-59.2573071437801,-44.4425490575932,
12.));
#78326=CARTESIAN_POINT('Ctrl Pts',(-59.2439820714231,-44.4186458955486,
12.));
#78327=CARTESIAN_POINT('Ctrl Pts',(-59.2306526095175,-44.394785891411,12.));
#78328=CARTESIAN_POINT('Ctrl Pts',(-59.217318843283,-44.3709690997495,12.));
#78329=CARTESIAN_POINT('Ctrl Pts',(-59.2039808594765,-44.3471955758412,
12.));
#78330=CARTESIAN_POINT('Ctrl Pts',(-59.1906387451971,-44.3234653750877,
12.));
#78331=CARTESIAN_POINT('Ctrl Pts',(-59.1772925865191,-44.2997785523413,
12.));
#78332=CARTESIAN_POINT('Ctrl Pts',(-59.1639424678766,-44.2761351616027,
12.));
#78333=CARTESIAN_POINT('Ctrl Pts',(-59.1505884728194,-44.2525352563979,
12.));
#78334=CARTESIAN_POINT('Ctrl Pts',(-59.1372306844575,-44.2289788899962,
12.));
#78335=CARTESIAN_POINT('Ctrl Pts',(-59.1238691860307,-44.2054661156876,
12.));
#78336=CARTESIAN_POINT('Ctrl Pts',(-59.1105040614285,-44.1819969870314,
12.));
#78337=CARTESIAN_POINT('Ctrl Pts',(-59.0971353957218,-44.1585715581073,
12.));
#78338=CARTESIAN_POINT('Ctrl Pts',(-59.0837632749209,-44.1351898834057,
12.));
#78339=CARTESIAN_POINT('Ctrl Pts',(-59.0703877857529,-44.1118520177223,
12.));
#78340=CARTESIAN_POINT('Ctrl Pts',(-59.0570090154243,-44.0885580160433,
12.));
#78341=CARTESIAN_POINT('Ctrl Pts',(-59.0436270514085,-44.0653079334384,
12.));
#78342=CARTESIAN_POINT('Ctrl Pts',(-59.0302419811772,-44.0421018249219,
12.));
#78343=CARTESIAN_POINT('Ctrl Pts',(-59.0168538922087,-44.0189397454593,
12.));
#78344=CARTESIAN_POINT('Ctrl Pts',(-59.0034628721161,-43.9958217500363,
12.));
#78345=CARTESIAN_POINT('Ctrl Pts',(-58.9900690087404,-43.9727478937053,
12.));
#78346=CARTESIAN_POINT('Ctrl Pts',(-58.9766723902531,-43.9497182316333,
12.));
#78347=CARTESIAN_POINT('Ctrl Pts',(-58.9632731052704,-43.9267328191507,
12.));
#78348=CARTESIAN_POINT('Ctrl Pts',(-58.9498712429066,-43.9037917117748,
12.));
#78349=CARTESIAN_POINT('Ctrl Pts',(-58.9364668927132,-43.8808949651882,
12.));
#78350=CARTESIAN_POINT('Ctrl Pts',(-58.9230601446445,-43.8580426352236,
12.));
#78351=CARTESIAN_POINT('Ctrl Pts',(-58.9096510890128,-43.8352347778419,
12.));
#78352=CARTESIAN_POINT('Ctrl Pts',(-58.8962398164486,-43.8124714491069,
12.));
#78353=CARTESIAN_POINT('Ctrl Pts',(-58.882826417861,-43.7897527051599,12.));
#78354=CARTESIAN_POINT('Ctrl Pts',(-58.8694109844636,-43.7670786022392,
12.));
#78355=CARTESIAN_POINT('Ctrl Pts',(-58.8559936077933,-43.7444491966935,
12.));
#78356=CARTESIAN_POINT('Ctrl Pts',(-58.8425743797325,-43.7218645449921,
12.));
#78357=CARTESIAN_POINT('Ctrl Pts',(-58.8291533925299,-43.6993247037318,
12.));
#78358=CARTESIAN_POINT('Ctrl Pts',(-58.8157307388247,-43.6768297296402,
12.));
#78359=CARTESIAN_POINT('Ctrl Pts',(-58.8023065116446,-43.6543796795797,
12.));
#78360=CARTESIAN_POINT('Ctrl Pts',(-58.7888808043976,-43.6319746105487,
12.));
#78361=CARTESIAN_POINT('Ctrl Pts',(-58.7754537108672,-43.6096145796798,
12.));
#78362=CARTESIAN_POINT('Ctrl Pts',(-58.7620253252059,-43.5872996442343,
12.));
#78363=CARTESIAN_POINT('Ctrl Pts',(-58.7485957419296,-43.5650298615911,
12.));
#78364=CARTESIAN_POINT('Ctrl Pts',(-58.7351650559176,-43.5428052892483,
12.));
#78365=CARTESIAN_POINT('Ctrl Pts',(-58.7217333624206,-43.5206259848333,
12.));
#78366=CARTESIAN_POINT('Ctrl Pts',(-58.708300757066,-43.4984920061071,12.));
#78367=CARTESIAN_POINT('Ctrl Pts',(-58.6948673358639,-43.4764034109654,
12.));
#78368=CARTESIAN_POINT('Ctrl Pts',(-58.6814331952138,-43.4543602574352,
12.));
#78369=CARTESIAN_POINT('Ctrl Pts',(-58.6679984319095,-43.4323626036736,
12.));
#78370=CARTESIAN_POINT('Ctrl Pts',(-58.6545631431388,-43.4104105079766,
12.));
#78371=CARTESIAN_POINT('Ctrl Pts',(-58.6411274264854,-43.3885040287808,
12.));
#78372=CARTESIAN_POINT('Ctrl Pts',(-58.627691379929,-43.3666432246634,12.));
#78373=CARTESIAN_POINT('Ctrl Pts',(-58.6142551018473,-43.3448281543374,
12.));
#78374=CARTESIAN_POINT('Ctrl Pts',(-58.6008186910166,-43.3230588766455,
12.));
#78375=CARTESIAN_POINT('Ctrl Pts',(-58.5873822466163,-43.3013354505707,
12.));
#78376=CARTESIAN_POINT('Ctrl Pts',(-58.5739458682317,-43.2796579352405,
12.));
#78377=CARTESIAN_POINT('Ctrl Pts',(-58.5605096558578,-43.2580263899278,
12.));
#78378=CARTESIAN_POINT('Ctrl Pts',(-58.5470737099027,-43.2364408740488,
12.));
#78379=CARTESIAN_POINT('Ctrl Pts',(-58.5336381311911,-43.214901447157,12.));
#78380=CARTESIAN_POINT('Ctrl Pts',(-58.5202030209667,-43.1934081689503,
12.));
#78381=CARTESIAN_POINT('Ctrl Pts',(-58.5067684808946,-43.1719610992771,
12.));
#78382=CARTESIAN_POINT('Ctrl Pts',(-58.4933346130638,-43.1505602981366,
12.));
#78383=CARTESIAN_POINT('Ctrl Pts',(-58.4799015199904,-43.1292058256774,
12.));
#78384=CARTESIAN_POINT('Ctrl Pts',(-58.4664693046206,-43.1078977421908,
12.));
#78385=CARTESIAN_POINT('Ctrl Pts',(-58.4530380703335,-43.0866361081166,
12.));
#78386=CARTESIAN_POINT('Ctrl Pts',(-58.4396079209438,-43.0654209840502,
12.));
#78387=CARTESIAN_POINT('Ctrl Pts',(-58.4261789607055,-43.0442524307432,
12.));
#78388=CARTESIAN_POINT('Ctrl Pts',(-58.4127512943144,-43.0231305091032,
12.));
#78389=CARTESIAN_POINT('Ctrl Pts',(-58.3993250269115,-43.0020552801869,
12.));
#78390=CARTESIAN_POINT('Ctrl Pts',(-58.3859002640871,-42.9810268052043,
12.));
#78391=CARTESIAN_POINT('Ctrl Pts',(-58.3724771118835,-42.9600451455267,
12.));
#78392=CARTESIAN_POINT('Ctrl Pts',(-58.3590556767981,-42.9391103626881,
12.));
#78393=CARTESIAN_POINT('Ctrl Pts',(-58.3456360657861,-42.9182225183851,
12.));
#78394=CARTESIAN_POINT('Ctrl Pts',(-58.3322183862647,-42.8973816744703,
12.));
#78395=CARTESIAN_POINT('Ctrl Pts',(-58.3188027461158,-42.8765878929545,
12.));
#78396=CARTESIAN_POINT('Ctrl Pts',(-58.305389253689,-42.8558412360154,12.));
#78397=CARTESIAN_POINT('Ctrl Pts',(-58.2919780178063,-42.8351417659998,
12.));
#78398=CARTESIAN_POINT('Ctrl Pts',(-58.278569147764,-42.8144895454234,12.));
#78399=CARTESIAN_POINT('Ctrl Pts',(-58.2651627533368,-42.7938846369651,
12.));
#78400=CARTESIAN_POINT('Ctrl Pts',(-58.2517589447818,-42.7733271034678,
12.));
#78401=CARTESIAN_POINT('Ctrl Pts',(-58.238357832842,-42.7528170079482,12.));
#78402=CARTESIAN_POINT('Ctrl Pts',(-58.2249595287497,-42.7323544135983,
12.));
#78403=CARTESIAN_POINT('Ctrl Pts',(-58.2115641442302,-42.7119393837866,
12.));
#78404=CARTESIAN_POINT('Ctrl Pts',(-58.1981717915043,-42.6915719820516,
12.));
#78405=CARTESIAN_POINT('Ctrl Pts',(-58.1847825832932,-42.6712522721021,
12.));
#78406=CARTESIAN_POINT('Ctrl Pts',(-58.1713966328217,-42.6509803178269,
12.));
#78407=CARTESIAN_POINT('Ctrl Pts',(-58.158014053823,-42.6307561832977,12.));
#78408=CARTESIAN_POINT('Ctrl Pts',(-58.1446349605419,-42.6105799327697,
12.));
#78409=CARTESIAN_POINT('Ctrl Pts',(-58.1312594677383,-42.5904516306759,
12.));
#78410=CARTESIAN_POINT('Ctrl Pts',(-58.1178876906905,-42.5703713416263,
12.));
#78411=CARTESIAN_POINT('Ctrl Pts',(-58.1045197452003,-42.5503391304182,
12.));
#78412=CARTESIAN_POINT('Ctrl Pts',(-58.0911557475967,-42.5303550620388,
12.));
#78413=CARTESIAN_POINT('Ctrl Pts',(-58.0777958147404,-42.5104192016664,
12.));
#78414=CARTESIAN_POINT('Ctrl Pts',(-58.064440064027,-42.4905316146649,12.));
#78415=CARTESIAN_POINT('Ctrl Pts',(-58.0510886133917,-42.4706923665838,
12.));
#78416=CARTESIAN_POINT('Ctrl Pts',(-58.0377415813132,-42.4509015231667,
12.));
#78417=CARTESIAN_POINT('Ctrl Pts',(-58.0243990868175,-42.4311591503551,
12.));
#78418=CARTESIAN_POINT('Ctrl Pts',(-58.011061249483,-42.4114653142891,12.));
#78419=CARTESIAN_POINT('Ctrl Pts',(-57.9977281894437,-42.3918200813024,
12.));
#78420=CARTESIAN_POINT('Ctrl Pts',(-57.9844000273936,-42.3722235179216,
12.));
#78421=CARTESIAN_POINT('Ctrl Pts',(-57.9710768845923,-42.3526756908764,
12.));
#78422=CARTESIAN_POINT('Ctrl Pts',(-57.9577588828693,-42.3331766671028,
12.));
#78423=CARTESIAN_POINT('Ctrl Pts',(-57.9444461446292,-42.3137265137446,
12.));
#78424=CARTESIAN_POINT('Ctrl Pts',(-57.9311387928541,-42.2943252981471,
12.));
#78425=CARTESIAN_POINT('Ctrl Pts',(-57.9178369511084,-42.274973087857,12.));
#78426=CARTESIAN_POINT('Ctrl Pts',(-57.9045407435447,-42.2556699506332,
12.));
#78427=CARTESIAN_POINT('Ctrl Pts',(-57.8912502949084,-42.2364159544492,
12.));
#78428=CARTESIAN_POINT('Ctrl Pts',(-57.8779657305423,-42.2172111674945,
12.));
#78429=CARTESIAN_POINT('Ctrl Pts',(-57.86468717639,-42.1980556581688,12.));
#78430=CARTESIAN_POINT('Ctrl Pts',(-57.8514147590012,-42.1789494950824,
12.));
#78431=CARTESIAN_POINT('Ctrl Pts',(-57.8381486055376,-42.1598927470671,
12.));
#78432=CARTESIAN_POINT('Ctrl Pts',(-57.8248888437787,-42.1408854831791,
12.));
#78433=CARTESIAN_POINT('Ctrl Pts',(-57.8116356021274,-42.121927772701,12.));
#78434=CARTESIAN_POINT('Ctrl Pts',(-57.798389009613,-42.1030196851344,12.));
#78435=CARTESIAN_POINT('Ctrl Pts',(-57.7851491958954,-42.0841612902018,
12.));
#78436=CARTESIAN_POINT('Ctrl Pts',(-57.7719162912721,-42.0653526578571,
12.));
#78437=CARTESIAN_POINT('Ctrl Pts',(-57.7586904266828,-42.0465938582877,
12.));
#78438=CARTESIAN_POINT('Ctrl Pts',(-57.7454717337151,-42.0278849619156,
12.));
#78439=CARTESIAN_POINT('Ctrl Pts',(-57.7322603446086,-42.0092260393911,
12.));
#78440=CARTESIAN_POINT('Ctrl Pts',(-57.7190563922614,-41.9906171615974,
12.));
#78441=CARTESIAN_POINT('Ctrl Pts',(-57.7058600102365,-41.9720583996601,
12.));
#78442=CARTESIAN_POINT('Ctrl Pts',(-57.6926713327674,-41.9535498249489,
12.));
#78443=CARTESIAN_POINT('Ctrl Pts',(-57.6794904947641,-41.9350915090791,
12.));
#78444=CARTESIAN_POINT('Ctrl Pts',(-57.6663176318176,-41.9166835239046,
12.));
#78445=CARTESIAN_POINT('Ctrl Pts',(-57.6531528802059,-41.8983259415244,
12.));
#78446=CARTESIAN_POINT('Ctrl Pts',(-57.6399963769003,-41.8800188342908,
12.));
#78447=CARTESIAN_POINT('Ctrl Pts',(-57.6268482595702,-41.8617622748108,
12.));
#78448=CARTESIAN_POINT('Ctrl Pts',(-57.6137086665882,-41.8435563359456,
12.));
#78449=CARTESIAN_POINT('Ctrl Pts',(-57.6005777370349,-41.8254010908051,
12.));
#78450=CARTESIAN_POINT('Ctrl Pts',(-57.5874556107056,-41.8072966127558,
12.));
#78451=CARTESIAN_POINT('Ctrl Pts',(-57.5743424281205,-41.7892429754297,
12.));
#78452=CARTESIAN_POINT('Ctrl Pts',(-57.561238330532,-41.7712402527273,12.));
#78453=CARTESIAN_POINT('Ctrl Pts',(-57.5481434599335,-41.7532885188174,
12.));
#78454=CARTESIAN_POINT('Ctrl Pts',(-57.5350579590649,-41.7353878481336,
12.));
#78455=CARTESIAN_POINT('Ctrl Pts',(-57.5219819714171,-41.7175383153821,
12.));
#78456=CARTESIAN_POINT('Ctrl Pts',(-57.5089156412343,-41.6997399955447,
12.));
#78457=CARTESIAN_POINT('Ctrl Pts',(-57.4958591135165,-41.6819929638797,
12.));
#78458=CARTESIAN_POINT('Ctrl Pts',(-57.4828125340218,-41.6642972959165,
12.));
#78459=CARTESIAN_POINT('Ctrl Pts',(-57.4697760492683,-41.6466530674514,
12.));
#78460=CARTESIAN_POINT('Ctrl Pts',(-57.4567498065562,-41.6290603545666,
12.));
#78461=CARTESIAN_POINT('Ctrl Pts',(-57.4437339539841,-41.6115192336388,
12.));
#78462=CARTESIAN_POINT('Ctrl Pts',(-57.4307286404662,-41.5940297813477,
12.));
#78463=CARTESIAN_POINT('Ctrl Pts',(-57.4177340157508,-41.5765920746777,
12.));
#78464=CARTESIAN_POINT('Ctrl Pts',(-57.4047502304231,-41.5592061909176,
12.));
#78465=CARTESIAN_POINT('Ctrl Pts',(-57.3917774358863,-41.5418722076572,
12.));
#78466=CARTESIAN_POINT('Ctrl Pts',(-57.3788157843454,-41.524590202777,12.));
#78467=CARTESIAN_POINT('Ctrl Pts',(-57.3658654287937,-41.5073602544396,
12.));
#78468=CARTESIAN_POINT('Ctrl Pts',(-57.3529265229835,-41.4901824410636,
12.));
#78469=CARTESIAN_POINT('Ctrl Pts',(-57.3399992214717,-41.4730568413518,
12.));
#78470=CARTESIAN_POINT('Ctrl Pts',(-57.3270836796911,-41.4559835343328,
12.));
#78471=CARTESIAN_POINT('Ctrl Pts',(-57.3141800540137,-41.4389625993948,
12.));
#78472=CARTESIAN_POINT('Ctrl Pts',(-57.3012885018151,-41.4219941163163,
12.));
#78473=CARTESIAN_POINT('Ctrl Pts',(-57.2884091815406,-41.4050781652938,
12.));
#78474=CARTESIAN_POINT('Ctrl Pts',(-57.2755422525844,-41.3882148268813,
12.));
#78475=CARTESIAN_POINT('Ctrl Pts',(-57.2626878751596,-41.3714041819223,
12.));
#78476=CARTESIAN_POINT('Ctrl Pts',(-57.2498462101879,-41.3546463114885,
12.));
#78477=CARTESIAN_POINT('Ctrl Pts',(-57.2370174191401,-41.3379412967875,
12.));
#78478=CARTESIAN_POINT('Ctrl Pts',(-57.2242016640198,-41.321289219149,12.));
#78479=CARTESIAN_POINT('Ctrl Pts',(-57.2113991077302,-41.3046901602293,
12.));
#78480=CARTESIAN_POINT('Ctrl Pts',(-57.1986099143983,-41.2881442021863,
12.));
#78481=CARTESIAN_POINT('Ctrl Pts',(-57.1858342496538,-41.2716514278276,
12.));
#78482=CARTESIAN_POINT('Ctrl Pts',(-57.17307228108,-41.2552119208465,12.));
#78483=CARTESIAN_POINT('Ctrl Pts',(-57.1603241779077,-41.2388257656559,
12.));
#78484=CARTESIAN_POINT('Ctrl Pts',(-57.147590110182,-41.222493046943,12.));
#78485=CARTESIAN_POINT('Ctrl Pts',(-57.1348702480647,-41.2062138492915,
12.));
#78486=CARTESIAN_POINT('Ctrl Pts',(-57.1221647611207,-41.1899882567923,
12.));
#78487=CARTESIAN_POINT('Ctrl Pts',(-57.1094738174957,-41.1738163525901,
12.));
#78488=CARTESIAN_POINT('Ctrl Pts',(-57.0967975854874,-41.1576982197374,
12.));
#78489=CARTESIAN_POINT('Ctrl Pts',(-57.084136235426,-41.1416339422117,12.));
#78490=CARTESIAN_POINT('Ctrl Pts',(-57.0714899412099,-41.1256236057442,
12.));
#78491=CARTESIAN_POINT('Ctrl Pts',(-57.0588588825298,-41.1096672990148,
12.));
#78492=CARTESIAN_POINT('Ctrl Pts',(-57.046243245068,-41.0937651137549,12.));
#78493=CARTESIAN_POINT('Ctrl Pts',(-57.0336432158536,-41.0779171422438,
12.));
#78494=CARTESIAN_POINT('Ctrl Pts',(-57.0210589791788,-41.0621234751007,
12.));
#78495=CARTESIAN_POINT('Ctrl Pts',(-57.008490713042,-41.0463841993608,12.));
#78496=CARTESIAN_POINT('Ctrl Pts',(-56.995938583472,-41.0306993953988,12.));
#78497=CARTESIAN_POINT('Ctrl Pts',(-56.9834027500117,-41.0150691398947,
12.));
#78498=CARTESIAN_POINT('Ctrl Pts',(-56.9708833766137,-40.9994935117276,
12.));
#78499=CARTESIAN_POINT('Ctrl Pts',(-56.9583806404069,-40.9839725967121,
12.));
#78500=CARTESIAN_POINT('Ctrl Pts',(-56.9458947422608,-40.9685064933074,
12.));
#78501=CARTESIAN_POINT('Ctrl Pts',(-56.9334259140049,-40.9530953165031,
12.));
#78502=CARTESIAN_POINT('Ctrl Pts',(-56.9209743960992,-40.9377391857128,
12.));
#78503=CARTESIAN_POINT('Ctrl Pts',(-56.9085404164502,-40.9224382132427,
12.));
#78504=CARTESIAN_POINT('Ctrl Pts',(-56.8961241708861,-40.9071924937508,
12.));
#78505=CARTESIAN_POINT('Ctrl Pts',(-56.8837257978343,-40.8920020903293,
12.));
#78506=CARTESIAN_POINT('Ctrl Pts',(-56.8713453764905,-40.8768670342052,
12.));
#78507=CARTESIAN_POINT('Ctrl Pts',(-56.8614554317668,-40.864803275942,12.));
#78508=CARTESIAN_POINT('Ctrl Pts',(-56.8540460739472,-40.8557803680277,
12.));
#78509=CARTESIAN_POINT('Ctrl Pts',(-56.8491101022591,-40.8497761671036,
12.));
#78510=CARTESIAN_POINT('Ctrl Pts',(-56.8466430164621,-40.8467768343956,
12.));
#78511=CARTESIAN_POINT('Ctrl Pts',(-58.4060826907797,-45.7706564944896,
-5.55111512312578E-16));
#78512=CARTESIAN_POINT('Ctrl Pts',(-58.4060826907797,-45.7706564944896,
4.));
#78513=CARTESIAN_POINT('Ctrl Pts',(-58.4060826907797,-45.7706564944896,
8.));
#78514=CARTESIAN_POINT('Ctrl Pts',(-58.4060826907797,-45.7706564944896,
12.));
#78515=CARTESIAN_POINT('Ctrl Pts',(-58.5127761886847,-45.7969367893064,
-5.55111512312578E-16));
#78516=CARTESIAN_POINT('Ctrl Pts',(-58.5127761886847,-45.7969367893064,
4.));
#78517=CARTESIAN_POINT('Ctrl Pts',(-58.5127761886847,-45.7969367893064,
8.00000000000001));
#78518=CARTESIAN_POINT('Ctrl Pts',(-58.5127761886847,-45.7969367893064,
12.));
#78519=CARTESIAN_POINT('Ctrl Pts',(-58.714632205056,-45.7788617791411,-5.55111512312578E-16));
#78520=CARTESIAN_POINT('Ctrl Pts',(-58.714632205056,-45.7788617791411,4.));
#78521=CARTESIAN_POINT('Ctrl Pts',(-58.714632205056,-45.7788617791411,7.99999999999999));
#78522=CARTESIAN_POINT('Ctrl Pts',(-58.714632205056,-45.7788617791411,12.));
#78523=CARTESIAN_POINT('Ctrl Pts',(-58.870677144318,-45.6563266621663,-5.55111512312578E-16));
#78524=CARTESIAN_POINT('Ctrl Pts',(-58.870677144318,-45.6563266621663,4.));
#78525=CARTESIAN_POINT('Ctrl Pts',(-58.870677144318,-45.6563266621663,8.00000000000001));
#78526=CARTESIAN_POINT('Ctrl Pts',(-58.870677144318,-45.6563266621663,12.));
#78527=CARTESIAN_POINT('Ctrl Pts',(-58.9211100416378,-45.5911481700252,
-5.55111512312578E-16));
#78528=CARTESIAN_POINT('Ctrl Pts',(-58.9211100416378,-45.5911481700252,
4.));
#78529=CARTESIAN_POINT('Ctrl Pts',(-58.9211100416378,-45.5911481700252,
8.));
#78530=CARTESIAN_POINT('Ctrl Pts',(-58.9211100416378,-45.5911481700252,
12.));
#78531=CARTESIAN_POINT('',(-58.4060826907797,-45.7706564944896,2.77555756156289E-16));
#78532=CARTESIAN_POINT('',(-58.9211100416379,-45.5911481700253,0.));
#78533=CARTESIAN_POINT('Ctrl Pts',(-58.4060826907797,-45.7706564944896,
-1.38777878078145E-16));
#78534=CARTESIAN_POINT('Ctrl Pts',(-58.5127761886847,-45.7969367893064,
-1.38777878078145E-16));
#78535=CARTESIAN_POINT('Ctrl Pts',(-58.628122483754,-45.7866082120691,-1.38777878078144E-16));
#78536=CARTESIAN_POINT('Ctrl Pts',(-58.7285100597672,-45.7421702122001,
-1.38777878078145E-16));
#78537=CARTESIAN_POINT('Ctrl Pts',(-58.8038007417772,-45.7088417122983,
-1.38777878078145E-16));
#78538=CARTESIAN_POINT('Ctrl Pts',(-58.870677144318,-45.6563266621663,-1.38777878078145E-16));
#78539=CARTESIAN_POINT('Ctrl Pts',(-58.9211100416378,-45.5911481700252,
-1.38777878078145E-16));
#78540=CARTESIAN_POINT('',(-58.9211100416379,-45.5911481700253,12.));
#78541=CARTESIAN_POINT('Ctrl Pts',(-58.9211100416378,-45.5911481700252,
-5.55111512312578E-16));
#78542=CARTESIAN_POINT('Ctrl Pts',(-58.9211100416378,-45.5911481700252,
4.));
#78543=CARTESIAN_POINT('Ctrl Pts',(-58.9211100416378,-45.5911481700252,
8.));
#78544=CARTESIAN_POINT('Ctrl Pts',(-58.9211100416378,-45.5911481700252,
12.));
#78545=CARTESIAN_POINT('',(-58.4060826907797,-45.7706564944896,12.));
#78546=CARTESIAN_POINT('Ctrl Pts',(-58.9211100416378,-45.5911481700252,
12.));
#78547=CARTESIAN_POINT('Ctrl Pts',(-58.870677144318,-45.6563266621663,12.));
#78548=CARTESIAN_POINT('Ctrl Pts',(-58.8038007417772,-45.7088417122983,
12.));
#78549=CARTESIAN_POINT('Ctrl Pts',(-58.7285100597672,-45.7421702122001,
12.));
#78550=CARTESIAN_POINT('Ctrl Pts',(-58.628122483754,-45.7866082120691,12.));
#78551=CARTESIAN_POINT('Ctrl Pts',(-58.5127761886847,-45.7969367893064,
12.));
#78552=CARTESIAN_POINT('Ctrl Pts',(-58.4060826907797,-45.7706564944896,
12.));
#78553=CARTESIAN_POINT('Ctrl Pts',(-58.4060826907797,-45.7706564944896,
12.));
#78554=CARTESIAN_POINT('Ctrl Pts',(-58.4060826907797,-45.7706564944896,
8.));
#78555=CARTESIAN_POINT('Ctrl Pts',(-58.4060826907797,-45.7706564944896,
4.));
#78556=CARTESIAN_POINT('Ctrl Pts',(-58.4060826907797,-45.7706564944896,
-5.55111512312578E-16));
#78557=CARTESIAN_POINT('Origin',(-2.97323128204029E-10,-2.28269173065022E-10,
0.));
#78558=CARTESIAN_POINT('Origin',(-2.97323128204029E-10,-2.28269173065022E-10,
12.));
#78559=CARTESIAN_POINT('Origin',(-2.97323128204029E-10,-2.28269173065022E-10,
0.));
#78560=CARTESIAN_POINT('Ctrl Pts',(-62.9938720098768,-39.77464128315,0.));
#78561=CARTESIAN_POINT('Ctrl Pts',(-62.9938720098768,-39.77464128315,4.));
#78562=CARTESIAN_POINT('Ctrl Pts',(-62.9938720098768,-39.7746412831501,
8.));
#78563=CARTESIAN_POINT('Ctrl Pts',(-62.9938720098768,-39.7746412831501,
12.));
#78564=CARTESIAN_POINT('Ctrl Pts',(-63.0525369183205,-39.6817295782357,
0.));
#78565=CARTESIAN_POINT('Ctrl Pts',(-63.0525369183205,-39.6817295782357,
4.));
#78566=CARTESIAN_POINT('Ctrl Pts',(-63.0525369183204,-39.6817295782358,
8.00000000000001));
#78567=CARTESIAN_POINT('Ctrl Pts',(-63.0525369183204,-39.6817295782358,
12.));
#78568=CARTESIAN_POINT('Ctrl Pts',(-63.0992090147611,-39.4845131830964,
-7.30833037965888E-17));
#78569=CARTESIAN_POINT('Ctrl Pts',(-63.0992090147611,-39.4845131830964,
4.00000000000001));
#78570=CARTESIAN_POINT('Ctrl Pts',(-63.099209014761,-39.4845131830966,7.99999999999999));
#78571=CARTESIAN_POINT('Ctrl Pts',(-63.099209014761,-39.4845131830966,12.));
#78572=CARTESIAN_POINT('Ctrl Pts',(-63.0322949727907,-39.2977314459977,
-2.46611180232692E-16));
#78573=CARTESIAN_POINT('Ctrl Pts',(-63.0322949727907,-39.2977314459977,
4.));
#78574=CARTESIAN_POINT('Ctrl Pts',(-63.0322949727907,-39.2977314459979,
8.00000000000001));
#78575=CARTESIAN_POINT('Ctrl Pts',(-63.0322949727907,-39.2977314459979,
12.));
#78576=CARTESIAN_POINT('Ctrl Pts',(-62.9864049293633,-39.2292784191459,
-3.30265160470176E-16));
#78577=CARTESIAN_POINT('Ctrl Pts',(-62.9864049293633,-39.2292784191459,
4.));
#78578=CARTESIAN_POINT('Ctrl Pts',(-62.9864049293633,-39.2292784191462,
8.));
#78579=CARTESIAN_POINT('Ctrl Pts',(-62.9864049293633,-39.2292784191462,
12.));
#78580=CARTESIAN_POINT('',(-62.9938720098768,-39.77464128315,0.));
#78581=CARTESIAN_POINT('',(-62.9864049293628,-39.2292784191463,0.));
#78582=CARTESIAN_POINT('Ctrl Pts',(-62.9938720098768,-39.77464128315,2.74425517504379E-17));
#78583=CARTESIAN_POINT('Ctrl Pts',(-63.0525369183205,-39.6817295782357,
2.74425517504379E-17));
#78584=CARTESIAN_POINT('Ctrl Pts',(-63.0792066877151,-39.569034495299,-1.43193361333271E-17));
#78585=CARTESIAN_POINT('Ctrl Pts',(-63.0687871057919,-39.4597466476407,
-8.887945181775E-17));
#78586=CARTESIAN_POINT('Ctrl Pts',(-63.0609724193495,-39.3777807618971,
-1.44799538581067E-16));
#78587=CARTESIAN_POINT('Ctrl Pts',(-63.0322949727907,-39.2977314459977,
-2.19168628482255E-16));
#78588=CARTESIAN_POINT('Ctrl Pts',(-62.9864049293633,-39.2292784191459,
-3.02822608719738E-16));
#78589=CARTESIAN_POINT('',(-62.9864049293629,-39.2292784191464,12.));
#78590=CARTESIAN_POINT('Ctrl Pts',(-62.9864049293633,-39.2292784191459,
-3.30265160470176E-16));
#78591=CARTESIAN_POINT('Ctrl Pts',(-62.9864049293633,-39.2292784191459,
4.));
#78592=CARTESIAN_POINT('Ctrl Pts',(-62.9864049293633,-39.2292784191462,
8.));
#78593=CARTESIAN_POINT('Ctrl Pts',(-62.9864049293633,-39.2292784191462,
12.));
#78594=CARTESIAN_POINT('',(-62.9938720098768,-39.7746412831501,12.));
#78595=CARTESIAN_POINT('Ctrl Pts',(-62.9864049293633,-39.2292784191462,
12.));
#78596=CARTESIAN_POINT('Ctrl Pts',(-63.0322949727907,-39.2977314459979,
12.));
#78597=CARTESIAN_POINT('Ctrl Pts',(-63.0609724193494,-39.3777807618974,
12.));
#78598=CARTESIAN_POINT('Ctrl Pts',(-63.0687871057918,-39.459746647641,12.));
#78599=CARTESIAN_POINT('Ctrl Pts',(-63.079206687715,-39.5690344952991,12.));
#78600=CARTESIAN_POINT('Ctrl Pts',(-63.0525369183204,-39.6817295782358,
12.));
#78601=CARTESIAN_POINT('Ctrl Pts',(-62.9938720098768,-39.7746412831501,
12.));
#78602=CARTESIAN_POINT('Ctrl Pts',(-62.9938720098768,-39.7746412831501,
12.));
#78603=CARTESIAN_POINT('Ctrl Pts',(-62.9938720098768,-39.7746412831501,
8.));
#78604=CARTESIAN_POINT('Ctrl Pts',(-62.9938720098768,-39.77464128315,4.));
#78605=CARTESIAN_POINT('Ctrl Pts',(-62.9938720098768,-39.77464128315,0.));
#78606=CARTESIAN_POINT('Ctrl Pts',(-60.1903555511633,-35.7368311217509,
0.));
#78607=CARTESIAN_POINT('Ctrl Pts',(-60.1903555511633,-35.7368311217509,
12.));
#78608=CARTESIAN_POINT('Ctrl Pts',(-60.1930746580239,-35.7396040203973,
0.));
#78609=CARTESIAN_POINT('Ctrl Pts',(-60.1930746580239,-35.7396040203973,
12.));
#78610=CARTESIAN_POINT('Ctrl Pts',(-60.1985151474406,-35.7451551752456,
0.));
#78611=CARTESIAN_POINT('Ctrl Pts',(-60.1985151474406,-35.7451551752456,
12.));
#78612=CARTESIAN_POINT('Ctrl Pts',(-60.2066827086579,-35.7534979801871,
0.));
#78613=CARTESIAN_POINT('Ctrl Pts',(-60.2066827086579,-35.7534979801871,
12.));
#78614=CARTESIAN_POINT('Ctrl Pts',(-60.2175864449678,-35.7646538667299,
0.));
#78615=CARTESIAN_POINT('Ctrl Pts',(-60.2175864449678,-35.7646538667299,
12.));
#78616=CARTESIAN_POINT('Ctrl Pts',(-60.2312388621286,-35.7786523045782,
0.));
#78617=CARTESIAN_POINT('Ctrl Pts',(-60.2312388621286,-35.7786523045782,
12.));
#78618=CARTESIAN_POINT('Ctrl Pts',(-60.2449139865206,-35.7927043145164,
0.));
#78619=CARTESIAN_POINT('Ctrl Pts',(-60.2449139865206,-35.7927043145164,
12.));
#78620=CARTESIAN_POINT('Ctrl Pts',(-60.2586117365278,-35.8068098723386,
0.));
#78621=CARTESIAN_POINT('Ctrl Pts',(-60.2586117365278,-35.8068098723386,
12.));
#78622=CARTESIAN_POINT('Ctrl Pts',(-60.2723319687507,-35.8209689272574,
0.));
#78623=CARTESIAN_POINT('Ctrl Pts',(-60.2723319687507,-35.8209689272574,
12.));
#78624=CARTESIAN_POINT('Ctrl Pts',(-60.2860744798563,-35.8351814020424,
0.));
#78625=CARTESIAN_POINT('Ctrl Pts',(-60.2860744798563,-35.8351814020424,
12.));
#78626=CARTESIAN_POINT('Ctrl Pts',(-60.2998390330173,-35.8494472046783,
0.));
#78627=CARTESIAN_POINT('Ctrl Pts',(-60.2998390330173,-35.8494472046783,
12.));
#78628=CARTESIAN_POINT('Ctrl Pts',(-60.313625378281,-35.8637662371635,0.));
#78629=CARTESIAN_POINT('Ctrl Pts',(-60.313625378281,-35.8637662371635,12.));
#78630=CARTESIAN_POINT('Ctrl Pts',(-60.3274332746782,-35.878138405151,0.));
#78631=CARTESIAN_POINT('Ctrl Pts',(-60.3274332746782,-35.878138405151,12.));
#78632=CARTESIAN_POINT('Ctrl Pts',(-60.3412625135223,-35.8925636280632,
0.));
#78633=CARTESIAN_POINT('Ctrl Pts',(-60.3412625135223,-35.8925636280632,
12.));
#78634=CARTESIAN_POINT('Ctrl Pts',(-60.3551129108794,-35.9070418358501,
0.));
#78635=CARTESIAN_POINT('Ctrl Pts',(-60.3551129108794,-35.9070418358501,
12.));
#78636=CARTESIAN_POINT('Ctrl Pts',(-60.368984296546,-35.9215729642219,0.));
#78637=CARTESIAN_POINT('Ctrl Pts',(-60.368984296546,-35.9215729642219,12.));
#78638=CARTESIAN_POINT('Ctrl Pts',(-60.3828765049031,-35.9361569506955,
0.));
#78639=CARTESIAN_POINT('Ctrl Pts',(-60.3828765049031,-35.9361569506955,
12.));
#78640=CARTESIAN_POINT('Ctrl Pts',(-60.3967893635487,-35.9507937296726,
0.));
#78641=CARTESIAN_POINT('Ctrl Pts',(-60.3967893635487,-35.9507937296726,
12.));
#78642=CARTESIAN_POINT('Ctrl Pts',(-60.4107226875759,-35.9654832299627,
0.));
#78643=CARTESIAN_POINT('Ctrl Pts',(-60.4107226875759,-35.9654832299627,
12.));
#78644=CARTESIAN_POINT('Ctrl Pts',(-60.4246762854961,-35.9802253773534,
0.));
#78645=CARTESIAN_POINT('Ctrl Pts',(-60.4246762854961,-35.9802253773534,
12.));
#78646=CARTESIAN_POINT('Ctrl Pts',(-60.438649962949,-35.9950200962175,0.));
#78647=CARTESIAN_POINT('Ctrl Pts',(-60.438649962949,-35.9950200962175,12.));
#78648=CARTESIAN_POINT('Ctrl Pts',(-60.452643526964,-36.0098673113556,0.));
#78649=CARTESIAN_POINT('Ctrl Pts',(-60.452643526964,-36.0098673113556,12.));
#78650=CARTESIAN_POINT('Ctrl Pts',(-60.4666567908053,-36.0247669500867,
0.));
#78651=CARTESIAN_POINT('Ctrl Pts',(-60.4666567908053,-36.0247669500867,
12.));
#78652=CARTESIAN_POINT('Ctrl Pts',(-60.4806895737643,-36.0397189421617,
0.));
#78653=CARTESIAN_POINT('Ctrl Pts',(-60.4806895737643,-36.0397189421617,
12.));
#78654=CARTESIAN_POINT('Ctrl Pts',(-60.4947416988396,-36.0547232187681,
0.));
#78655=CARTESIAN_POINT('Ctrl Pts',(-60.4947416988396,-36.0547232187681,
12.));
#78656=CARTESIAN_POINT('Ctrl Pts',(-60.5088129911357,-36.0697797118377,
0.));
#78657=CARTESIAN_POINT('Ctrl Pts',(-60.5088129911357,-36.0697797118377,
12.));
#78658=CARTESIAN_POINT('Ctrl Pts',(-60.5229032759001,-36.0848883531968,
0.));
#78659=CARTESIAN_POINT('Ctrl Pts',(-60.5229032759001,-36.0848883531968,
12.));
#78660=CARTESIAN_POINT('Ctrl Pts',(-60.5370123768841,-36.1000490738532,
0.));
#78661=CARTESIAN_POINT('Ctrl Pts',(-60.5370123768841,-36.1000490738532,
12.));
#78662=CARTESIAN_POINT('Ctrl Pts',(-60.5511401172014,-36.1152618043756,
0.));
#78663=CARTESIAN_POINT('Ctrl Pts',(-60.5511401172014,-36.1152618043756,
12.));
#78664=CARTESIAN_POINT('Ctrl Pts',(-60.5652863200732,-36.1305264752195,
0.));
#78665=CARTESIAN_POINT('Ctrl Pts',(-60.5652863200732,-36.1305264752195,
12.));
#78666=CARTESIAN_POINT('Ctrl Pts',(-60.5794508095555,-36.1458430170425,
0.));
#78667=CARTESIAN_POINT('Ctrl Pts',(-60.5794508095555,-36.1458430170425,
12.));
#78668=CARTESIAN_POINT('Ctrl Pts',(-60.5936334114083,-36.1612113610758,
0.));
#78669=CARTESIAN_POINT('Ctrl Pts',(-60.5936334114083,-36.1612113610758,
12.));
#78670=CARTESIAN_POINT('Ctrl Pts',(-60.6078339534151,-36.1766314392624,
0.));
#78671=CARTESIAN_POINT('Ctrl Pts',(-60.6078339534151,-36.1766314392624,
12.));
#78672=CARTESIAN_POINT('Ctrl Pts',(-60.6220522649129,-36.1921031840617,
0.));
#78673=CARTESIAN_POINT('Ctrl Pts',(-60.6220522649129,-36.1921031840617,
12.));
#78674=CARTESIAN_POINT('Ctrl Pts',(-60.6362881765014,-36.2076265283261,
0.));
#78675=CARTESIAN_POINT('Ctrl Pts',(-60.6362881765014,-36.2076265283261,
12.));
#78676=CARTESIAN_POINT('Ctrl Pts',(-60.6505415197055,-36.2232014051549,
0.));
#78677=CARTESIAN_POINT('Ctrl Pts',(-60.6505415197055,-36.2232014051549,
12.));
#78678=CARTESIAN_POINT('Ctrl Pts',(-60.6648121265908,-36.2388277477225,
0.));
#78679=CARTESIAN_POINT('Ctrl Pts',(-60.6648121265908,-36.2388277477225,
12.));
#78680=CARTESIAN_POINT('Ctrl Pts',(-60.6790998297823,-36.2545054892911,
0.));
#78681=CARTESIAN_POINT('Ctrl Pts',(-60.6790998297823,-36.2545054892911,
12.));
#78682=CARTESIAN_POINT('Ctrl Pts',(-60.6934044626304,-36.2702345632882,
0.));
#78683=CARTESIAN_POINT('Ctrl Pts',(-60.6934044626304,-36.2702345632882,
12.));
#78684=CARTESIAN_POINT('Ctrl Pts',(-60.7077258593268,-36.2860149033586,
0.));
#78685=CARTESIAN_POINT('Ctrl Pts',(-60.7077258593268,-36.2860149033586,
12.));
#78686=CARTESIAN_POINT('Ctrl Pts',(-60.7220638550396,-36.3018464434204,
0.));
#78687=CARTESIAN_POINT('Ctrl Pts',(-60.7220638550396,-36.3018464434204,
12.));
#78688=CARTESIAN_POINT('Ctrl Pts',(-60.7364182860388,-36.3177291177148,
0.));
#78689=CARTESIAN_POINT('Ctrl Pts',(-60.7364182860388,-36.3177291177148,
12.));
#78690=CARTESIAN_POINT('Ctrl Pts',(-60.7507889896284,-36.3336628607844,
0.));
#78691=CARTESIAN_POINT('Ctrl Pts',(-60.7507889896284,-36.3336628607844,
12.));
#78692=CARTESIAN_POINT('Ctrl Pts',(-60.7651758040792,-36.349647607448,0.));
#78693=CARTESIAN_POINT('Ctrl Pts',(-60.7651758040792,-36.349647607448,12.));
#78694=CARTESIAN_POINT('Ctrl Pts',(-60.7795785685631,-36.3656832927733,
0.));
#78695=CARTESIAN_POINT('Ctrl Pts',(-60.7795785685631,-36.3656832927733,
12.));
#78696=CARTESIAN_POINT('Ctrl Pts',(-60.7939971230781,-36.38176985204,0.));
#78697=CARTESIAN_POINT('Ctrl Pts',(-60.7939971230781,-36.38176985204,12.));
#78698=CARTESIAN_POINT('Ctrl Pts',(-60.8084313084009,-36.3979072207174,
0.));
#78699=CARTESIAN_POINT('Ctrl Pts',(-60.8084313084009,-36.3979072207174,
12.));
#78700=CARTESIAN_POINT('Ctrl Pts',(-60.8228809661179,-36.4140953344869,
0.));
#78701=CARTESIAN_POINT('Ctrl Pts',(-60.8228809661179,-36.4140953344869,
12.));
#78702=CARTESIAN_POINT('Ctrl Pts',(-60.8373459386397,-36.4303341292497,
0.));
#78703=CARTESIAN_POINT('Ctrl Pts',(-60.8373459386397,-36.4303341292497,
12.));
#78704=CARTESIAN_POINT('Ctrl Pts',(-60.851826069218,-36.4466235411353,0.));
#78705=CARTESIAN_POINT('Ctrl Pts',(-60.851826069218,-36.4466235411353,12.));
#78706=CARTESIAN_POINT('Ctrl Pts',(-60.8663212019646,-36.4629635065037,
0.));
#78707=CARTESIAN_POINT('Ctrl Pts',(-60.8663212019646,-36.4629635065037,
12.));
#78708=CARTESIAN_POINT('Ctrl Pts',(-60.8808311818489,-36.4793539619459,
0.));
#78709=CARTESIAN_POINT('Ctrl Pts',(-60.8808311818489,-36.4793539619459,
12.));
#78710=CARTESIAN_POINT('Ctrl Pts',(-60.8953558546791,-36.4957948442832,
0.));
#78711=CARTESIAN_POINT('Ctrl Pts',(-60.8953558546791,-36.4957948442832,
12.));
#78712=CARTESIAN_POINT('Ctrl Pts',(-60.9098950670847,-36.5122860905611,
0.));
#78713=CARTESIAN_POINT('Ctrl Pts',(-60.9098950670847,-36.5122860905611,
12.));
#78714=CARTESIAN_POINT('Ctrl Pts',(-60.924448666499,-36.5288276380417,0.));
#78715=CARTESIAN_POINT('Ctrl Pts',(-60.924448666499,-36.5288276380417,12.));
#78716=CARTESIAN_POINT('Ctrl Pts',(-60.9390165011357,-36.5454194241866,
0.));
#78717=CARTESIAN_POINT('Ctrl Pts',(-60.9390165011357,-36.5454194241866,
12.));
#78718=CARTESIAN_POINT('Ctrl Pts',(-60.9535984199874,-36.5620613866615,
0.));
#78719=CARTESIAN_POINT('Ctrl Pts',(-60.9535984199874,-36.5620613866615,
12.));
#78720=CARTESIAN_POINT('Ctrl Pts',(-60.9681942728237,-36.5787534633416,
0.));
#78721=CARTESIAN_POINT('Ctrl Pts',(-60.9681942728237,-36.5787534633416,
12.));
#78722=CARTESIAN_POINT('Ctrl Pts',(-60.9828039101887,-36.5954955923109,
0.));
#78723=CARTESIAN_POINT('Ctrl Pts',(-60.9828039101887,-36.5954955923109,
12.));
#78724=CARTESIAN_POINT('Ctrl Pts',(-60.9974271833982,-36.6122877118599,
0.));
#78725=CARTESIAN_POINT('Ctrl Pts',(-60.9974271833982,-36.6122877118599,
12.));
#78726=CARTESIAN_POINT('Ctrl Pts',(-61.012063944535,-36.6291297604775,0.));
#78727=CARTESIAN_POINT('Ctrl Pts',(-61.012063944535,-36.6291297604775,12.));
#78728=CARTESIAN_POINT('Ctrl Pts',(-61.0267140464434,-36.6460216768553,
0.));
#78729=CARTESIAN_POINT('Ctrl Pts',(-61.0267140464434,-36.6460216768553,
12.));
#78730=CARTESIAN_POINT('Ctrl Pts',(-61.0413773427204,-36.6629633998885,
0.));
#78731=CARTESIAN_POINT('Ctrl Pts',(-61.0413773427204,-36.6629633998885,
12.));
#78732=CARTESIAN_POINT('Ctrl Pts',(-61.0560536877084,-36.6799548686741,
0.));
#78733=CARTESIAN_POINT('Ctrl Pts',(-61.0560536877084,-36.6799548686741,
12.));
#78734=CARTESIAN_POINT('Ctrl Pts',(-61.0707429364841,-36.6969960225019,
0.));
#78735=CARTESIAN_POINT('Ctrl Pts',(-61.0707429364841,-36.6969960225019,
12.));
#78736=CARTESIAN_POINT('Ctrl Pts',(-61.085444944851,-36.7140868008479,0.));
#78737=CARTESIAN_POINT('Ctrl Pts',(-61.085444944851,-36.7140868008479,12.));
#78738=CARTESIAN_POINT('Ctrl Pts',(-61.1001595693357,-36.7312271433799,
0.));
#78739=CARTESIAN_POINT('Ctrl Pts',(-61.1001595693357,-36.7312271433799,
12.));
#78740=CARTESIAN_POINT('Ctrl Pts',(-61.1148866671821,-36.7484169899591,
0.));
#78741=CARTESIAN_POINT('Ctrl Pts',(-61.1148866671821,-36.7484169899591,
12.));
#78742=CARTESIAN_POINT('Ctrl Pts',(-61.1296260963468,-36.7656562806381,
0.));
#78743=CARTESIAN_POINT('Ctrl Pts',(-61.1296260963468,-36.7656562806381,
12.));
#78744=CARTESIAN_POINT('Ctrl Pts',(-61.1443777154926,-36.782944955654,0.));
#78745=CARTESIAN_POINT('Ctrl Pts',(-61.1443777154926,-36.782944955654,12.));
#78746=CARTESIAN_POINT('Ctrl Pts',(-61.1591413839809,-36.8002829554221,
0.));
#78747=CARTESIAN_POINT('Ctrl Pts',(-61.1591413839809,-36.8002829554221,
12.));
#78748=CARTESIAN_POINT('Ctrl Pts',(-61.1739169618688,-36.8176702205436,
0.));
#78749=CARTESIAN_POINT('Ctrl Pts',(-61.1739169618688,-36.8176702205436,
12.));
#78750=CARTESIAN_POINT('Ctrl Pts',(-61.1887043099026,-36.8351066918043,
0.));
#78751=CARTESIAN_POINT('Ctrl Pts',(-61.1887043099026,-36.8351066918043,
12.));
#78752=CARTESIAN_POINT('Ctrl Pts',(-61.2035032895121,-36.8525923101736,
0.));
#78753=CARTESIAN_POINT('Ctrl Pts',(-61.2035032895121,-36.8525923101736,
12.));
#78754=CARTESIAN_POINT('Ctrl Pts',(-61.2183137628031,-36.8701270167954,
0.));
#78755=CARTESIAN_POINT('Ctrl Pts',(-61.2183137628031,-36.8701270167954,
12.));
#78756=CARTESIAN_POINT('Ctrl Pts',(-61.2331355925513,-36.8877107529844,
0.));
#78757=CARTESIAN_POINT('Ctrl Pts',(-61.2331355925513,-36.8877107529844,
12.));
#78758=CARTESIAN_POINT('Ctrl Pts',(-61.2479686421979,-36.9053434602324,
0.));
#78759=CARTESIAN_POINT('Ctrl Pts',(-61.2479686421979,-36.9053434602324,
12.));
#78760=CARTESIAN_POINT('Ctrl Pts',(-61.2628127758443,-36.9230250802078,
0.));
#78761=CARTESIAN_POINT('Ctrl Pts',(-61.2628127758443,-36.9230250802078,
12.));
#78762=CARTESIAN_POINT('Ctrl Pts',(-61.2776678582474,-36.9407555547542,
0.));
#78763=CARTESIAN_POINT('Ctrl Pts',(-61.2776678582474,-36.9407555547542,
12.));
#78764=CARTESIAN_POINT('Ctrl Pts',(-61.2925337548113,-36.9585348258798,
0.));
#78765=CARTESIAN_POINT('Ctrl Pts',(-61.2925337548113,-36.9585348258798,
12.));
#78766=CARTESIAN_POINT('Ctrl Pts',(-61.3074103315834,-36.976362835757,0.));
#78767=CARTESIAN_POINT('Ctrl Pts',(-61.3074103315834,-36.976362835757,12.));
#78768=CARTESIAN_POINT('Ctrl Pts',(-61.3222974552519,-36.994239526729,0.));
#78769=CARTESIAN_POINT('Ctrl Pts',(-61.3222974552519,-36.994239526729,12.));
#78770=CARTESIAN_POINT('Ctrl Pts',(-61.3371949931397,-37.0121648413088,
0.));
#78771=CARTESIAN_POINT('Ctrl Pts',(-61.3371949931397,-37.0121648413088,
12.));
#78772=CARTESIAN_POINT('Ctrl Pts',(-61.352102813199,-37.0301387221766,0.));
#78773=CARTESIAN_POINT('Ctrl Pts',(-61.352102813199,-37.0301387221766,12.));
#78774=CARTESIAN_POINT('Ctrl Pts',(-61.3670207840041,-37.0481611121698,
0.));
#78775=CARTESIAN_POINT('Ctrl Pts',(-61.3670207840041,-37.0481611121698,
12.));
#78776=CARTESIAN_POINT('Ctrl Pts',(-61.3819487747458,-37.0662319542827,
0.));
#78777=CARTESIAN_POINT('Ctrl Pts',(-61.3819487747458,-37.0662319542827,
12.));
#78778=CARTESIAN_POINT('Ctrl Pts',(-61.3968866552294,-37.0843511916728,
0.));
#78779=CARTESIAN_POINT('Ctrl Pts',(-61.3968866552294,-37.0843511916728,
12.));
#78780=CARTESIAN_POINT('Ctrl Pts',(-61.411834295869,-37.1025187676597,0.));
#78781=CARTESIAN_POINT('Ctrl Pts',(-61.411834295869,-37.1025187676597,12.));
#78782=CARTESIAN_POINT('Ctrl Pts',(-61.4267915676834,-37.1207346257228,
0.));
#78783=CARTESIAN_POINT('Ctrl Pts',(-61.4267915676834,-37.1207346257228,
12.));
#78784=CARTESIAN_POINT('Ctrl Pts',(-61.4417583422888,-37.138998709492,0.));
#78785=CARTESIAN_POINT('Ctrl Pts',(-61.4417583422888,-37.138998709492,12.));
#78786=CARTESIAN_POINT('Ctrl Pts',(-61.4567344918946,-37.157310962747,0.));
#78787=CARTESIAN_POINT('Ctrl Pts',(-61.4567344918946,-37.157310962747,12.));
#78788=CARTESIAN_POINT('Ctrl Pts',(-61.471719889301,-37.1756713294249,0.));
#78789=CARTESIAN_POINT('Ctrl Pts',(-61.471719889301,-37.1756713294249,12.));
#78790=CARTESIAN_POINT('Ctrl Pts',(-61.4867144078939,-37.1940797536182,
0.));
#78791=CARTESIAN_POINT('Ctrl Pts',(-61.4867144078939,-37.1940797536182,
12.));
#78792=CARTESIAN_POINT('Ctrl Pts',(-61.5017179216404,-37.2125361795727,
0.));
#78793=CARTESIAN_POINT('Ctrl Pts',(-61.5017179216404,-37.2125361795727,
12.));
#78794=CARTESIAN_POINT('Ctrl Pts',(-61.5167303050823,-37.2310405516775,
0.));
#78795=CARTESIAN_POINT('Ctrl Pts',(-61.5167303050823,-37.2310405516775,
12.));
#78796=CARTESIAN_POINT('Ctrl Pts',(-61.5317514333319,-37.2495928144661,
0.));
#78797=CARTESIAN_POINT('Ctrl Pts',(-61.5317514333319,-37.2495928144661,
12.));
#78798=CARTESIAN_POINT('Ctrl Pts',(-61.5467811820686,-37.2681929126217,
0.));
#78799=CARTESIAN_POINT('Ctrl Pts',(-61.5467811820686,-37.2681929126217,
12.));
#78800=CARTESIAN_POINT('Ctrl Pts',(-61.5618194275349,-37.286840790977,0.));
#78801=CARTESIAN_POINT('Ctrl Pts',(-61.5618194275349,-37.286840790977,12.));
#78802=CARTESIAN_POINT('Ctrl Pts',(-61.5768660465313,-37.3055363945108,
0.));
#78803=CARTESIAN_POINT('Ctrl Pts',(-61.5768660465313,-37.3055363945108,
12.));
#78804=CARTESIAN_POINT('Ctrl Pts',(-61.591920916412,-37.3242796683395,0.));
#78805=CARTESIAN_POINT('Ctrl Pts',(-61.591920916412,-37.3242796683395,12.));
#78806=CARTESIAN_POINT('Ctrl Pts',(-61.6069839150804,-37.3430705577178,
0.));
#78807=CARTESIAN_POINT('Ctrl Pts',(-61.6069839150804,-37.3430705577178,
12.));
#78808=CARTESIAN_POINT('Ctrl Pts',(-61.6220549209862,-37.3619090080447,
0.));
#78809=CARTESIAN_POINT('Ctrl Pts',(-61.6220549209862,-37.3619090080447,
12.));
#78810=CARTESIAN_POINT('Ctrl Pts',(-61.6371338131208,-37.3807949648622,
0.));
#78811=CARTESIAN_POINT('Ctrl Pts',(-61.6371338131208,-37.3807949648622,
12.));
#78812=CARTESIAN_POINT('Ctrl Pts',(-61.6522204710133,-37.3997283738534,
0.));
#78813=CARTESIAN_POINT('Ctrl Pts',(-61.6522204710133,-37.3997283738534,
12.));
#78814=CARTESIAN_POINT('Ctrl Pts',(-61.667314774725,-37.4187091808324,0.));
#78815=CARTESIAN_POINT('Ctrl Pts',(-61.667314774725,-37.4187091808324,12.));
#78816=CARTESIAN_POINT('Ctrl Pts',(-61.6824166048454,-37.4377373317456,
0.));
#78817=CARTESIAN_POINT('Ctrl Pts',(-61.6824166048454,-37.4377373317456,
12.));
#78818=CARTESIAN_POINT('Ctrl Pts',(-61.69752584249,-37.4568127726776,0.));
#78819=CARTESIAN_POINT('Ctrl Pts',(-61.69752584249,-37.4568127726776,12.));
#78820=CARTESIAN_POINT('Ctrl Pts',(-61.7126423692965,-37.4759354498509,
0.));
#78821=CARTESIAN_POINT('Ctrl Pts',(-61.7126423692965,-37.4759354498509,
12.));
#78822=CARTESIAN_POINT('Ctrl Pts',(-61.7277660674203,-37.4951053096235,
0.));
#78823=CARTESIAN_POINT('Ctrl Pts',(-61.7277660674203,-37.4951053096235,
12.));
#78824=CARTESIAN_POINT('Ctrl Pts',(-61.7428968195296,-37.5143222984794,
0.));
#78825=CARTESIAN_POINT('Ctrl Pts',(-61.7428968195296,-37.5143222984794,
12.));
#78826=CARTESIAN_POINT('Ctrl Pts',(-61.7580345088014,-37.5335863630286,
0.));
#78827=CARTESIAN_POINT('Ctrl Pts',(-61.7580345088014,-37.5335863630286,
12.));
#78828=CARTESIAN_POINT('Ctrl Pts',(-61.7731790189191,-37.5528974500142,
0.));
#78829=CARTESIAN_POINT('Ctrl Pts',(-61.7731790189191,-37.5528974500142,
12.));
#78830=CARTESIAN_POINT('Ctrl Pts',(-61.7883302340689,-37.5722555063112,
0.));
#78831=CARTESIAN_POINT('Ctrl Pts',(-61.7883302340689,-37.5722555063112,
12.));
#78832=CARTESIAN_POINT('Ctrl Pts',(-61.8034880389362,-37.5916604789252,
0.));
#78833=CARTESIAN_POINT('Ctrl Pts',(-61.8034880389362,-37.5916604789252,
12.));
#78834=CARTESIAN_POINT('Ctrl Pts',(-61.8186523187011,-37.6111123149835,
0.));
#78835=CARTESIAN_POINT('Ctrl Pts',(-61.8186523187011,-37.6111123149835,
12.));
#78836=CARTESIAN_POINT('Ctrl Pts',(-61.8338229590345,-37.6306109617341,
0.));
#78837=CARTESIAN_POINT('Ctrl Pts',(-61.8338229590345,-37.6306109617341,
12.));
#78838=CARTESIAN_POINT('Ctrl Pts',(-61.848999846095,-37.6501563665518,0.));
#78839=CARTESIAN_POINT('Ctrl Pts',(-61.848999846095,-37.6501563665518,12.));
#78840=CARTESIAN_POINT('Ctrl Pts',(-61.8641828665257,-37.6697484769389,
0.));
#78841=CARTESIAN_POINT('Ctrl Pts',(-61.8641828665257,-37.6697484769389,
12.));
#78842=CARTESIAN_POINT('Ctrl Pts',(-61.879371907451,-37.6893872405229,0.));
#78843=CARTESIAN_POINT('Ctrl Pts',(-61.879371907451,-37.6893872405229,12.));
#78844=CARTESIAN_POINT('Ctrl Pts',(-61.8945668564714,-37.7090726050488,
0.));
#78845=CARTESIAN_POINT('Ctrl Pts',(-61.8945668564714,-37.7090726050488,
12.));
#78846=CARTESIAN_POINT('Ctrl Pts',(-61.9097676016616,-37.7288045183765,
0.));
#78847=CARTESIAN_POINT('Ctrl Pts',(-61.9097676016616,-37.7288045183765,
12.));
#78848=CARTESIAN_POINT('Ctrl Pts',(-61.9249740315664,-37.748582928488,0.));
#78849=CARTESIAN_POINT('Ctrl Pts',(-61.9249740315664,-37.748582928488,12.));
#78850=CARTESIAN_POINT('Ctrl Pts',(-61.940186035198,-37.7684077834877,0.));
#78851=CARTESIAN_POINT('Ctrl Pts',(-61.940186035198,-37.7684077834877,12.));
#78852=CARTESIAN_POINT('Ctrl Pts',(-61.9554035020335,-37.7882790316012,
0.));
#78853=CARTESIAN_POINT('Ctrl Pts',(-61.9554035020335,-37.7882790316012,
12.));
#78854=CARTESIAN_POINT('Ctrl Pts',(-61.9706263220101,-37.808196621168,0.));
#78855=CARTESIAN_POINT('Ctrl Pts',(-61.9706263220101,-37.808196621168,12.));
#78856=CARTESIAN_POINT('Ctrl Pts',(-61.9858543855221,-37.8281605006371,
0.));
#78857=CARTESIAN_POINT('Ctrl Pts',(-61.9858543855221,-37.8281605006371,
12.));
#78858=CARTESIAN_POINT('Ctrl Pts',(-62.0010875834176,-37.8481706185742,
0.));
#78859=CARTESIAN_POINT('Ctrl Pts',(-62.0010875834176,-37.8481706185742,
12.));
#78860=CARTESIAN_POINT('Ctrl Pts',(-62.0163258069954,-37.8682269236628,
0.));
#78861=CARTESIAN_POINT('Ctrl Pts',(-62.0163258069954,-37.8682269236628,
12.));
#78862=CARTESIAN_POINT('Ctrl Pts',(-62.0315689480022,-37.888329364703,0.));
#78863=CARTESIAN_POINT('Ctrl Pts',(-62.0315689480022,-37.888329364703,12.));
#78864=CARTESIAN_POINT('Ctrl Pts',(-62.0468168986289,-37.9084778906053,
0.));
#78865=CARTESIAN_POINT('Ctrl Pts',(-62.0468168986289,-37.9084778906053,
12.));
#78866=CARTESIAN_POINT('Ctrl Pts',(-62.0620695515072,-37.9286724503849,
0.));
#78867=CARTESIAN_POINT('Ctrl Pts',(-62.0620695515072,-37.9286724503849,
12.));
#78868=CARTESIAN_POINT('Ctrl Pts',(-62.0773267997072,-37.9489129931685,
0.));
#78869=CARTESIAN_POINT('Ctrl Pts',(-62.0773267997072,-37.9489129931685,
12.));
#78870=CARTESIAN_POINT('Ctrl Pts',(-62.0925885367346,-37.9691994681962,
0.));
#78871=CARTESIAN_POINT('Ctrl Pts',(-62.0925885367346,-37.9691994681962,
12.));
#78872=CARTESIAN_POINT('Ctrl Pts',(-62.107854656528,-37.9895318248212,0.));
#78873=CARTESIAN_POINT('Ctrl Pts',(-62.107854656528,-37.9895318248212,12.));
#78874=CARTESIAN_POINT('Ctrl Pts',(-62.1231250534558,-38.0099100125041,
0.));
#78875=CARTESIAN_POINT('Ctrl Pts',(-62.1231250534558,-38.0099100125041,
12.));
#78876=CARTESIAN_POINT('Ctrl Pts',(-62.1383996223136,-38.0303339808059,
0.));
#78877=CARTESIAN_POINT('Ctrl Pts',(-62.1383996223136,-38.0303339808059,
12.));
#78878=CARTESIAN_POINT('Ctrl Pts',(-62.153678258321,-38.0508036793944,0.));
#78879=CARTESIAN_POINT('Ctrl Pts',(-62.153678258321,-38.0508036793944,12.));
#78880=CARTESIAN_POINT('Ctrl Pts',(-62.1689608571182,-38.0713190580466,
0.));
#78881=CARTESIAN_POINT('Ctrl Pts',(-62.1689608571182,-38.0713190580466,
12.));
#78882=CARTESIAN_POINT('Ctrl Pts',(-62.1842473147627,-38.0918800666479,
0.));
#78883=CARTESIAN_POINT('Ctrl Pts',(-62.1842473147627,-38.0918800666479,
12.));
#78884=CARTESIAN_POINT('Ctrl Pts',(-62.1995375277253,-38.1124866551883,
0.));
#78885=CARTESIAN_POINT('Ctrl Pts',(-62.1995375277253,-38.1124866551883,
12.));
#78886=CARTESIAN_POINT('Ctrl Pts',(-62.2148313928859,-38.1331387737528,
0.));
#78887=CARTESIAN_POINT('Ctrl Pts',(-62.2148313928859,-38.1331387737528,
12.));
#78888=CARTESIAN_POINT('Ctrl Pts',(-62.2301288075319,-38.1538363725263,
0.));
#78889=CARTESIAN_POINT('Ctrl Pts',(-62.2301288075319,-38.1538363725263,
12.));
#78890=CARTESIAN_POINT('Ctrl Pts',(-62.2454296693581,-38.1745794017997,
0.));
#78891=CARTESIAN_POINT('Ctrl Pts',(-62.2454296693581,-38.1745794017997,
12.));
#78892=CARTESIAN_POINT('Ctrl Pts',(-62.2607338764655,-38.1953678119692,
0.));
#78893=CARTESIAN_POINT('Ctrl Pts',(-62.2607338764655,-38.1953678119692,
12.));
#78894=CARTESIAN_POINT('Ctrl Pts',(-62.2760413273601,-38.2162015535351,
0.));
#78895=CARTESIAN_POINT('Ctrl Pts',(-62.2760413273601,-38.2162015535351,
12.));
#78896=CARTESIAN_POINT('Ctrl Pts',(-62.2913519209517,-38.2370805770931,
0.));
#78897=CARTESIAN_POINT('Ctrl Pts',(-62.2913519209517,-38.2370805770931,
12.));
#78898=CARTESIAN_POINT('Ctrl Pts',(-62.3066655565497,-38.2580048333356,
0.));
#78899=CARTESIAN_POINT('Ctrl Pts',(-62.3066655565497,-38.2580048333356,
12.));
#78900=CARTESIAN_POINT('Ctrl Pts',(-62.3219821338564,-38.2789742730559,
0.));
#78901=CARTESIAN_POINT('Ctrl Pts',(-62.3219821338564,-38.2789742730559,
12.));
#78902=CARTESIAN_POINT('Ctrl Pts',(-62.337301552961,-38.2999888471474,0.));
#78903=CARTESIAN_POINT('Ctrl Pts',(-62.337301552961,-38.2999888471474,12.));
#78904=CARTESIAN_POINT('Ctrl Pts',(-62.3526237143338,-38.3210485066002,
0.));
#78905=CARTESIAN_POINT('Ctrl Pts',(-62.3526237143338,-38.3210485066002,
12.));
#78906=CARTESIAN_POINT('Ctrl Pts',(-62.3679485188178,-38.3421532024915,
0.));
#78907=CARTESIAN_POINT('Ctrl Pts',(-62.3679485188178,-38.3421532024915,
12.));
#78908=CARTESIAN_POINT('Ctrl Pts',(-62.3832758676281,-38.3633028859835,
0.));
#78909=CARTESIAN_POINT('Ctrl Pts',(-62.3832758676281,-38.3633028859835,
12.));
#78910=CARTESIAN_POINT('Ctrl Pts',(-62.3986056623587,-38.384497508335,0.));
#78911=CARTESIAN_POINT('Ctrl Pts',(-62.3986056623587,-38.384497508335,12.));
#78912=CARTESIAN_POINT('Ctrl Pts',(-62.4139378049891,-38.4057370209054,
0.));
#78913=CARTESIAN_POINT('Ctrl Pts',(-62.4139378049891,-38.4057370209054,
12.));
#78914=CARTESIAN_POINT('Ctrl Pts',(-62.42927219789,-38.4270213751567,0.));
#78915=CARTESIAN_POINT('Ctrl Pts',(-62.42927219789,-38.4270213751567,12.));
#78916=CARTESIAN_POINT('Ctrl Pts',(-62.4446087438304,-38.4483505226511,
0.));
#78917=CARTESIAN_POINT('Ctrl Pts',(-62.4446087438304,-38.4483505226511,
12.));
#78918=CARTESIAN_POINT('Ctrl Pts',(-62.4599473459799,-38.4697244150473,
0.));
#78919=CARTESIAN_POINT('Ctrl Pts',(-62.4599473459799,-38.4697244150473,
12.));
#78920=CARTESIAN_POINT('Ctrl Pts',(-62.4752879078842,-38.4911430040988,
0.));
#78921=CARTESIAN_POINT('Ctrl Pts',(-62.4752879078842,-38.4911430040988,
12.));
#78922=CARTESIAN_POINT('Ctrl Pts',(-62.4906303334435,-38.5126062416495,
0.));
#78923=CARTESIAN_POINT('Ctrl Pts',(-62.4906303334435,-38.5126062416495,
12.));
#78924=CARTESIAN_POINT('Ctrl Pts',(-62.50597452689,-38.5341140796247,0.));
#78925=CARTESIAN_POINT('Ctrl Pts',(-62.50597452689,-38.5341140796247,12.));
#78926=CARTESIAN_POINT('Ctrl Pts',(-62.5213203927672,-38.5556664700201,
0.));
#78927=CARTESIAN_POINT('Ctrl Pts',(-62.5213203927672,-38.5556664700201,
12.));
#78928=CARTESIAN_POINT('Ctrl Pts',(-62.5366678359036,-38.5772633648841,
0.));
#78929=CARTESIAN_POINT('Ctrl Pts',(-62.5366678359036,-38.5772633648841,
12.));
#78930=CARTESIAN_POINT('Ctrl Pts',(-62.5520167614529,-38.5989047163401,
0.));
#78931=CARTESIAN_POINT('Ctrl Pts',(-62.5520167614529,-38.5989047163401,
12.));
#78932=CARTESIAN_POINT('Ctrl Pts',(-62.567367074937,-38.6205904766078,0.));
#78933=CARTESIAN_POINT('Ctrl Pts',(-62.567367074937,-38.6205904766078,12.));
#78934=CARTESIAN_POINT('Ctrl Pts',(-62.5827186822923,-38.6423205980214,
0.));
#78935=CARTESIAN_POINT('Ctrl Pts',(-62.5827186822923,-38.6423205980214,
12.));
#78936=CARTESIAN_POINT('Ctrl Pts',(-62.5980714899048,-38.6640950330418,
0.));
#78937=CARTESIAN_POINT('Ctrl Pts',(-62.5980714899048,-38.6640950330418,
12.));
#78938=CARTESIAN_POINT('Ctrl Pts',(-62.6134254046732,-38.6859137342726,
0.));
#78939=CARTESIAN_POINT('Ctrl Pts',(-62.6134254046732,-38.6859137342726,
12.));
#78940=CARTESIAN_POINT('Ctrl Pts',(-62.6287803339534,-38.7077766544411,
0.));
#78941=CARTESIAN_POINT('Ctrl Pts',(-62.6287803339534,-38.7077766544411,
12.));
#78942=CARTESIAN_POINT('Ctrl Pts',(-62.6441361854406,-38.7296837463605,
0.));
#78943=CARTESIAN_POINT('Ctrl Pts',(-62.6441361854406,-38.7296837463605,
12.));
#78944=CARTESIAN_POINT('Ctrl Pts',(-62.6594928670626,-38.7516349628902,
0.));
#78945=CARTESIAN_POINT('Ctrl Pts',(-62.6594928670626,-38.7516349628902,
12.));
#78946=CARTESIAN_POINT('Ctrl Pts',(-62.6748502868836,-38.7736302568982,
0.));
#78947=CARTESIAN_POINT('Ctrl Pts',(-62.6748502868836,-38.7736302568982,
12.));
#78948=CARTESIAN_POINT('Ctrl Pts',(-62.6902083529698,-38.7956695812032,
0.));
#78949=CARTESIAN_POINT('Ctrl Pts',(-62.6902083529698,-38.7956695812032,
12.));
#78950=CARTESIAN_POINT('Ctrl Pts',(-62.7055669733811,-38.8177528885686,
0.));
#78951=CARTESIAN_POINT('Ctrl Pts',(-62.7055669733811,-38.8177528885686,
12.));
#78952=CARTESIAN_POINT('Ctrl Pts',(-62.7209260564506,-38.8398801318184,
0.));
#78953=CARTESIAN_POINT('Ctrl Pts',(-62.7209260564506,-38.8398801318184,
12.));
#78954=CARTESIAN_POINT('Ctrl Pts',(-62.7362855110052,-38.8620512639239,
0.));
#78955=CARTESIAN_POINT('Ctrl Pts',(-62.7362855110052,-38.8620512639239,
12.));
#78956=CARTESIAN_POINT('Ctrl Pts',(-62.7516452466129,-38.8842662380984,
0.));
#78957=CARTESIAN_POINT('Ctrl Pts',(-62.7516452466129,-38.8842662380984,
12.));
#78958=CARTESIAN_POINT('Ctrl Pts',(-62.7670051738132,-38.9065250078824,
0.));
#78959=CARTESIAN_POINT('Ctrl Pts',(-62.7670051738132,-38.9065250078824,
12.));
#78960=CARTESIAN_POINT('Ctrl Pts',(-62.7823652043677,-38.9288275272319,
0.));
#78961=CARTESIAN_POINT('Ctrl Pts',(-62.7823652043677,-38.9288275272319,
12.));
#78962=CARTESIAN_POINT('Ctrl Pts',(-62.797725250709,-38.9511737503146,0.));
#78963=CARTESIAN_POINT('Ctrl Pts',(-62.797725250709,-38.9511737503146,12.));
#78964=CARTESIAN_POINT('Ctrl Pts',(-62.8130852254004,-38.9735636313073,
0.));
#78965=CARTESIAN_POINT('Ctrl Pts',(-62.8130852254004,-38.9735636313073,
12.));
#78966=CARTESIAN_POINT('Ctrl Pts',(-62.8284450405451,-38.9959971241695,
0.));
#78967=CARTESIAN_POINT('Ctrl Pts',(-62.8284450405451,-38.9959971241695,
12.));
#78968=CARTESIAN_POINT('Ctrl Pts',(-62.8438046073237,-39.0184741824649,
0.));
#78969=CARTESIAN_POINT('Ctrl Pts',(-62.8438046073237,-39.0184741824649,
12.));
#78970=CARTESIAN_POINT('Ctrl Pts',(-62.859163835209,-39.0409947590519,0.));
#78971=CARTESIAN_POINT('Ctrl Pts',(-62.859163835209,-39.0409947590519,12.));
#78972=CARTESIAN_POINT('Ctrl Pts',(-62.8745226326046,-39.0635588063308,
0.));
#78973=CARTESIAN_POINT('Ctrl Pts',(-62.8745226326046,-39.0635588063308,
12.));
#78974=CARTESIAN_POINT('Ctrl Pts',(-62.8898809082659,-39.0861662767964,
0.));
#78975=CARTESIAN_POINT('Ctrl Pts',(-62.8898809082659,-39.0861662767964,
12.));
#78976=CARTESIAN_POINT('Ctrl Pts',(-62.9052385725416,-39.1088171235144,
0.));
#78977=CARTESIAN_POINT('Ctrl Pts',(-62.9052385725416,-39.1088171235144,
12.));
#78978=CARTESIAN_POINT('Ctrl Pts',(-62.9205955385551,-39.1315113005745,
0.));
#78979=CARTESIAN_POINT('Ctrl Pts',(-62.9205955385551,-39.1315113005745,
12.));
#78980=CARTESIAN_POINT('Ctrl Pts',(-62.9359517237352,-39.1542487636708,
0.));
#78981=CARTESIAN_POINT('Ctrl Pts',(-62.9359517237352,-39.1542487636708,
12.));
#78982=CARTESIAN_POINT('Ctrl Pts',(-62.9513070501777,-39.1770294702367,
0.));
#78983=CARTESIAN_POINT('Ctrl Pts',(-62.9513070501777,-39.1770294702367,
12.));
#78984=CARTESIAN_POINT('Ctrl Pts',(-62.9666614412628,-39.199853378159,0.));
#78985=CARTESIAN_POINT('Ctrl Pts',(-62.9666614412628,-39.199853378159,12.));
#78986=CARTESIAN_POINT('Ctrl Pts',(-62.9820148189849,-39.2227204447583,
0.));
#78987=CARTESIAN_POINT('Ctrl Pts',(-62.9820148189849,-39.2227204447583,
12.));
#78988=CARTESIAN_POINT('Ctrl Pts',(-62.9973671008685,-39.2456306256092,
0.));
#78989=CARTESIAN_POINT('Ctrl Pts',(-62.9973671008685,-39.2456306256092,
12.));
#78990=CARTESIAN_POINT('Ctrl Pts',(-63.0127181973703,-39.268583873541,0.));
#78991=CARTESIAN_POINT('Ctrl Pts',(-63.0127181973703,-39.268583873541,12.));
#78992=CARTESIAN_POINT('Ctrl Pts',(-63.0280680082522,-39.2915801372467,
0.));
#78993=CARTESIAN_POINT('Ctrl Pts',(-63.0280680082522,-39.2915801372467,
12.));
#78994=CARTESIAN_POINT('Ctrl Pts',(-63.0434164278221,-39.3146193632546,
0.));
#78995=CARTESIAN_POINT('Ctrl Pts',(-63.0434164278221,-39.3146193632546,
12.));
#78996=CARTESIAN_POINT('Ctrl Pts',(-63.0587633513993,-39.3377014983756,
0.));
#78997=CARTESIAN_POINT('Ctrl Pts',(-63.0587633513993,-39.3377014983756,
12.));
#78998=CARTESIAN_POINT('Ctrl Pts',(-63.0741086815958,-39.3608264920487,
0.));
#78999=CARTESIAN_POINT('Ctrl Pts',(-63.0741086815958,-39.3608264920487,
12.));
#79000=CARTESIAN_POINT('Ctrl Pts',(-63.0894523341238,-39.3839942985688,
0.));
#79001=CARTESIAN_POINT('Ctrl Pts',(-63.0894523341238,-39.3839942985688,
12.));
#79002=CARTESIAN_POINT('Ctrl Pts',(-63.1047942451583,-39.4072048797401,
0.));
#79003=CARTESIAN_POINT('Ctrl Pts',(-63.1047942451583,-39.4072048797401,
12.));
#79004=CARTESIAN_POINT('Ctrl Pts',(-63.1201343730643,-39.4304582059507,
0.));
#79005=CARTESIAN_POINT('Ctrl Pts',(-63.1201343730643,-39.4304582059507,
12.));
#79006=CARTESIAN_POINT('Ctrl Pts',(-63.1354726927781,-39.4537542551852,
0.));
#79007=CARTESIAN_POINT('Ctrl Pts',(-63.1354726927781,-39.4537542551852,
12.));
#79008=CARTESIAN_POINT('Ctrl Pts',(-63.147741892189,-39.4724252610807,0.));
#79009=CARTESIAN_POINT('Ctrl Pts',(-63.147741892189,-39.4724252610807,12.));
#79010=CARTESIAN_POINT('Ctrl Pts',(-63.1569429707564,-39.4864477303613,
0.));
#79011=CARTESIAN_POINT('Ctrl Pts',(-63.1569429707564,-39.4864477303613,
12.));
#79012=CARTESIAN_POINT('Ctrl Pts',(-63.1630766582674,-39.4958045828059,
0.));
#79013=CARTESIAN_POINT('Ctrl Pts',(-63.1630766582674,-39.4958045828059,
12.));
#79014=CARTESIAN_POINT('Ctrl Pts',(-63.1661434108059,-39.5004851439257,
0.));
#79015=CARTESIAN_POINT('Ctrl Pts',(-63.1661434108059,-39.5004851439257,
12.));
#79016=CARTESIAN_POINT('',(-60.1903555511633,-35.7368311217509,0.));
#79017=CARTESIAN_POINT('Ctrl Pts',(-60.1903555511633,-35.7368311217509,
0.));
#79018=CARTESIAN_POINT('Ctrl Pts',(-60.1930746580239,-35.7396040203973,
0.));
#79019=CARTESIAN_POINT('Ctrl Pts',(-60.1985151474406,-35.7451551752456,
0.));
#79020=CARTESIAN_POINT('Ctrl Pts',(-60.2066827086579,-35.7534979801871,
0.));
#79021=CARTESIAN_POINT('Ctrl Pts',(-60.2175864449678,-35.7646538667299,
0.));
#79022=CARTESIAN_POINT('Ctrl Pts',(-60.2312388621286,-35.7786523045782,
0.));
#79023=CARTESIAN_POINT('Ctrl Pts',(-60.2449139865206,-35.7927043145164,
0.));
#79024=CARTESIAN_POINT('Ctrl Pts',(-60.2586117365278,-35.8068098723386,
0.));
#79025=CARTESIAN_POINT('Ctrl Pts',(-60.2723319687507,-35.8209689272574,
0.));
#79026=CARTESIAN_POINT('Ctrl Pts',(-60.2860744798563,-35.8351814020424,
0.));
#79027=CARTESIAN_POINT('Ctrl Pts',(-60.2998390330173,-35.8494472046783,
0.));
#79028=CARTESIAN_POINT('Ctrl Pts',(-60.313625378281,-35.8637662371635,0.));
#79029=CARTESIAN_POINT('Ctrl Pts',(-60.3274332746782,-35.878138405151,0.));
#79030=CARTESIAN_POINT('Ctrl Pts',(-60.3412625135223,-35.8925636280632,
0.));
#79031=CARTESIAN_POINT('Ctrl Pts',(-60.3551129108794,-35.9070418358501,
0.));
#79032=CARTESIAN_POINT('Ctrl Pts',(-60.368984296546,-35.9215729642219,0.));
#79033=CARTESIAN_POINT('Ctrl Pts',(-60.3828765049031,-35.9361569506955,
0.));
#79034=CARTESIAN_POINT('Ctrl Pts',(-60.3967893635487,-35.9507937296726,
0.));
#79035=CARTESIAN_POINT('Ctrl Pts',(-60.4107226875759,-35.9654832299627,
0.));
#79036=CARTESIAN_POINT('Ctrl Pts',(-60.4246762854961,-35.9802253773534,
0.));
#79037=CARTESIAN_POINT('Ctrl Pts',(-60.438649962949,-35.9950200962175,0.));
#79038=CARTESIAN_POINT('Ctrl Pts',(-60.452643526964,-36.0098673113556,0.));
#79039=CARTESIAN_POINT('Ctrl Pts',(-60.4666567908053,-36.0247669500867,
0.));
#79040=CARTESIAN_POINT('Ctrl Pts',(-60.4806895737643,-36.0397189421617,
0.));
#79041=CARTESIAN_POINT('Ctrl Pts',(-60.4947416988396,-36.0547232187681,
0.));
#79042=CARTESIAN_POINT('Ctrl Pts',(-60.5088129911357,-36.0697797118377,
0.));
#79043=CARTESIAN_POINT('Ctrl Pts',(-60.5229032759001,-36.0848883531968,
0.));
#79044=CARTESIAN_POINT('Ctrl Pts',(-60.5370123768841,-36.1000490738532,
0.));
#79045=CARTESIAN_POINT('Ctrl Pts',(-60.5511401172014,-36.1152618043756,
0.));
#79046=CARTESIAN_POINT('Ctrl Pts',(-60.5652863200732,-36.1305264752195,
0.));
#79047=CARTESIAN_POINT('Ctrl Pts',(-60.5794508095555,-36.1458430170425,
0.));
#79048=CARTESIAN_POINT('Ctrl Pts',(-60.5936334114083,-36.1612113610758,
0.));
#79049=CARTESIAN_POINT('Ctrl Pts',(-60.6078339534151,-36.1766314392624,
0.));
#79050=CARTESIAN_POINT('Ctrl Pts',(-60.6220522649129,-36.1921031840617,
0.));
#79051=CARTESIAN_POINT('Ctrl Pts',(-60.6362881765014,-36.2076265283261,
0.));
#79052=CARTESIAN_POINT('Ctrl Pts',(-60.6505415197055,-36.2232014051549,
0.));
#79053=CARTESIAN_POINT('Ctrl Pts',(-60.6648121265908,-36.2388277477225,
0.));
#79054=CARTESIAN_POINT('Ctrl Pts',(-60.6790998297823,-36.2545054892911,
0.));
#79055=CARTESIAN_POINT('Ctrl Pts',(-60.6934044626304,-36.2702345632882,
0.));
#79056=CARTESIAN_POINT('Ctrl Pts',(-60.7077258593268,-36.2860149033586,
0.));
#79057=CARTESIAN_POINT('Ctrl Pts',(-60.7220638550396,-36.3018464434204,
0.));
#79058=CARTESIAN_POINT('Ctrl Pts',(-60.7364182860388,-36.3177291177148,
0.));
#79059=CARTESIAN_POINT('Ctrl Pts',(-60.7507889896284,-36.3336628607844,
0.));
#79060=CARTESIAN_POINT('Ctrl Pts',(-60.7651758040792,-36.349647607448,0.));
#79061=CARTESIAN_POINT('Ctrl Pts',(-60.7795785685631,-36.3656832927733,
0.));
#79062=CARTESIAN_POINT('Ctrl Pts',(-60.7939971230781,-36.38176985204,0.));
#79063=CARTESIAN_POINT('Ctrl Pts',(-60.8084313084009,-36.3979072207174,
0.));
#79064=CARTESIAN_POINT('Ctrl Pts',(-60.8228809661179,-36.4140953344869,
0.));
#79065=CARTESIAN_POINT('Ctrl Pts',(-60.8373459386397,-36.4303341292497,
0.));
#79066=CARTESIAN_POINT('Ctrl Pts',(-60.851826069218,-36.4466235411353,0.));
#79067=CARTESIAN_POINT('Ctrl Pts',(-60.8663212019646,-36.4629635065037,
0.));
#79068=CARTESIAN_POINT('Ctrl Pts',(-60.8808311818489,-36.4793539619459,
0.));
#79069=CARTESIAN_POINT('Ctrl Pts',(-60.8953558546791,-36.4957948442832,
0.));
#79070=CARTESIAN_POINT('Ctrl Pts',(-60.9098950670847,-36.5122860905611,
0.));
#79071=CARTESIAN_POINT('Ctrl Pts',(-60.924448666499,-36.5288276380417,0.));
#79072=CARTESIAN_POINT('Ctrl Pts',(-60.9390165011357,-36.5454194241866,
0.));
#79073=CARTESIAN_POINT('Ctrl Pts',(-60.9535984199874,-36.5620613866615,
0.));
#79074=CARTESIAN_POINT('Ctrl Pts',(-60.9681942728237,-36.5787534633416,
0.));
#79075=CARTESIAN_POINT('Ctrl Pts',(-60.9828039101887,-36.5954955923109,
0.));
#79076=CARTESIAN_POINT('Ctrl Pts',(-60.9974271833982,-36.6122877118599,
0.));
#79077=CARTESIAN_POINT('Ctrl Pts',(-61.012063944535,-36.6291297604775,0.));
#79078=CARTESIAN_POINT('Ctrl Pts',(-61.0267140464434,-36.6460216768553,
0.));
#79079=CARTESIAN_POINT('Ctrl Pts',(-61.0413773427204,-36.6629633998885,
0.));
#79080=CARTESIAN_POINT('Ctrl Pts',(-61.0560536877084,-36.6799548686741,
0.));
#79081=CARTESIAN_POINT('Ctrl Pts',(-61.0707429364841,-36.6969960225019,
0.));
#79082=CARTESIAN_POINT('Ctrl Pts',(-61.085444944851,-36.7140868008479,0.));
#79083=CARTESIAN_POINT('Ctrl Pts',(-61.1001595693357,-36.7312271433799,
0.));
#79084=CARTESIAN_POINT('Ctrl Pts',(-61.1148866671821,-36.7484169899591,
0.));
#79085=CARTESIAN_POINT('Ctrl Pts',(-61.1296260963468,-36.7656562806381,
0.));
#79086=CARTESIAN_POINT('Ctrl Pts',(-61.1443777154926,-36.782944955654,0.));
#79087=CARTESIAN_POINT('Ctrl Pts',(-61.1591413839809,-36.8002829554221,
0.));
#79088=CARTESIAN_POINT('Ctrl Pts',(-61.1739169618688,-36.8176702205436,
0.));
#79089=CARTESIAN_POINT('Ctrl Pts',(-61.1887043099026,-36.8351066918043,
0.));
#79090=CARTESIAN_POINT('Ctrl Pts',(-61.2035032895121,-36.8525923101736,
0.));
#79091=CARTESIAN_POINT('Ctrl Pts',(-61.2183137628031,-36.8701270167954,
0.));
#79092=CARTESIAN_POINT('Ctrl Pts',(-61.2331355925513,-36.8877107529844,
0.));
#79093=CARTESIAN_POINT('Ctrl Pts',(-61.2479686421979,-36.9053434602324,
0.));
#79094=CARTESIAN_POINT('Ctrl Pts',(-61.2628127758443,-36.9230250802078,
0.));
#79095=CARTESIAN_POINT('Ctrl Pts',(-61.2776678582474,-36.9407555547542,
0.));
#79096=CARTESIAN_POINT('Ctrl Pts',(-61.2925337548113,-36.9585348258798,
0.));
#79097=CARTESIAN_POINT('Ctrl Pts',(-61.3074103315834,-36.976362835757,0.));
#79098=CARTESIAN_POINT('Ctrl Pts',(-61.3222974552519,-36.994239526729,0.));
#79099=CARTESIAN_POINT('Ctrl Pts',(-61.3371949931397,-37.0121648413088,
0.));
#79100=CARTESIAN_POINT('Ctrl Pts',(-61.352102813199,-37.0301387221766,0.));
#79101=CARTESIAN_POINT('Ctrl Pts',(-61.3670207840041,-37.0481611121698,
0.));
#79102=CARTESIAN_POINT('Ctrl Pts',(-61.3819487747458,-37.0662319542827,
0.));
#79103=CARTESIAN_POINT('Ctrl Pts',(-61.3968866552294,-37.0843511916728,
0.));
#79104=CARTESIAN_POINT('Ctrl Pts',(-61.411834295869,-37.1025187676597,0.));
#79105=CARTESIAN_POINT('Ctrl Pts',(-61.4267915676834,-37.1207346257228,
0.));
#79106=CARTESIAN_POINT('Ctrl Pts',(-61.4417583422888,-37.138998709492,0.));
#79107=CARTESIAN_POINT('Ctrl Pts',(-61.4567344918946,-37.157310962747,0.));
#79108=CARTESIAN_POINT('Ctrl Pts',(-61.471719889301,-37.1756713294249,0.));
#79109=CARTESIAN_POINT('Ctrl Pts',(-61.4867144078939,-37.1940797536182,
0.));
#79110=CARTESIAN_POINT('Ctrl Pts',(-61.5017179216404,-37.2125361795727,
0.));
#79111=CARTESIAN_POINT('Ctrl Pts',(-61.5167303050823,-37.2310405516775,
0.));
#79112=CARTESIAN_POINT('Ctrl Pts',(-61.5317514333319,-37.2495928144661,
0.));
#79113=CARTESIAN_POINT('Ctrl Pts',(-61.5467811820686,-37.2681929126217,
0.));
#79114=CARTESIAN_POINT('Ctrl Pts',(-61.5618194275349,-37.286840790977,0.));
#79115=CARTESIAN_POINT('Ctrl Pts',(-61.5768660465313,-37.3055363945108,
0.));
#79116=CARTESIAN_POINT('Ctrl Pts',(-61.591920916412,-37.3242796683395,0.));
#79117=CARTESIAN_POINT('Ctrl Pts',(-61.6069839150804,-37.3430705577178,
0.));
#79118=CARTESIAN_POINT('Ctrl Pts',(-61.6220549209862,-37.3619090080447,
0.));
#79119=CARTESIAN_POINT('Ctrl Pts',(-61.6371338131208,-37.3807949648622,
0.));
#79120=CARTESIAN_POINT('Ctrl Pts',(-61.6522204710133,-37.3997283738534,
0.));
#79121=CARTESIAN_POINT('Ctrl Pts',(-61.667314774725,-37.4187091808324,0.));
#79122=CARTESIAN_POINT('Ctrl Pts',(-61.6824166048454,-37.4377373317456,
0.));
#79123=CARTESIAN_POINT('Ctrl Pts',(-61.69752584249,-37.4568127726776,0.));
#79124=CARTESIAN_POINT('Ctrl Pts',(-61.7126423692965,-37.4759354498509,
0.));
#79125=CARTESIAN_POINT('Ctrl Pts',(-61.7277660674203,-37.4951053096235,
0.));
#79126=CARTESIAN_POINT('Ctrl Pts',(-61.7428968195296,-37.5143222984794,
0.));
#79127=CARTESIAN_POINT('Ctrl Pts',(-61.7580345088014,-37.5335863630286,
0.));
#79128=CARTESIAN_POINT('Ctrl Pts',(-61.7731790189191,-37.5528974500142,
0.));
#79129=CARTESIAN_POINT('Ctrl Pts',(-61.7883302340689,-37.5722555063112,
0.));
#79130=CARTESIAN_POINT('Ctrl Pts',(-61.8034880389362,-37.5916604789252,
0.));
#79131=CARTESIAN_POINT('Ctrl Pts',(-61.8186523187011,-37.6111123149835,
0.));
#79132=CARTESIAN_POINT('Ctrl Pts',(-61.8338229590345,-37.6306109617341,
0.));
#79133=CARTESIAN_POINT('Ctrl Pts',(-61.848999846095,-37.6501563665518,0.));
#79134=CARTESIAN_POINT('Ctrl Pts',(-61.8641828665257,-37.6697484769389,
0.));
#79135=CARTESIAN_POINT('Ctrl Pts',(-61.879371907451,-37.6893872405229,0.));
#79136=CARTESIAN_POINT('Ctrl Pts',(-61.8945668564714,-37.7090726050488,
0.));
#79137=CARTESIAN_POINT('Ctrl Pts',(-61.9097676016616,-37.7288045183765,
0.));
#79138=CARTESIAN_POINT('Ctrl Pts',(-61.9249740315664,-37.748582928488,0.));
#79139=CARTESIAN_POINT('Ctrl Pts',(-61.940186035198,-37.7684077834877,0.));
#79140=CARTESIAN_POINT('Ctrl Pts',(-61.9554035020335,-37.7882790316012,
0.));
#79141=CARTESIAN_POINT('Ctrl Pts',(-61.9706263220101,-37.808196621168,0.));
#79142=CARTESIAN_POINT('Ctrl Pts',(-61.9858543855221,-37.8281605006371,
0.));
#79143=CARTESIAN_POINT('Ctrl Pts',(-62.0010875834176,-37.8481706185742,
0.));
#79144=CARTESIAN_POINT('Ctrl Pts',(-62.0163258069954,-37.8682269236628,
0.));
#79145=CARTESIAN_POINT('Ctrl Pts',(-62.0315689480022,-37.888329364703,0.));
#79146=CARTESIAN_POINT('Ctrl Pts',(-62.0468168986289,-37.9084778906053,
0.));
#79147=CARTESIAN_POINT('Ctrl Pts',(-62.0620695515072,-37.9286724503849,
0.));
#79148=CARTESIAN_POINT('Ctrl Pts',(-62.0773267997072,-37.9489129931685,
0.));
#79149=CARTESIAN_POINT('Ctrl Pts',(-62.0925885367346,-37.9691994681962,
0.));
#79150=CARTESIAN_POINT('Ctrl Pts',(-62.107854656528,-37.9895318248212,0.));
#79151=CARTESIAN_POINT('Ctrl Pts',(-62.1231250534558,-38.0099100125041,
0.));
#79152=CARTESIAN_POINT('Ctrl Pts',(-62.1383996223136,-38.0303339808059,
0.));
#79153=CARTESIAN_POINT('Ctrl Pts',(-62.153678258321,-38.0508036793944,0.));
#79154=CARTESIAN_POINT('Ctrl Pts',(-62.1689608571182,-38.0713190580466,
0.));
#79155=CARTESIAN_POINT('Ctrl Pts',(-62.1842473147627,-38.0918800666479,
0.));
#79156=CARTESIAN_POINT('Ctrl Pts',(-62.1995375277253,-38.1124866551883,
0.));
#79157=CARTESIAN_POINT('Ctrl Pts',(-62.2148313928859,-38.1331387737528,
0.));
#79158=CARTESIAN_POINT('Ctrl Pts',(-62.2301288075319,-38.1538363725263,
0.));
#79159=CARTESIAN_POINT('Ctrl Pts',(-62.2454296693581,-38.1745794017997,
0.));
#79160=CARTESIAN_POINT('Ctrl Pts',(-62.2607338764655,-38.1953678119692,
0.));
#79161=CARTESIAN_POINT('Ctrl Pts',(-62.2760413273601,-38.2162015535351,
0.));
#79162=CARTESIAN_POINT('Ctrl Pts',(-62.2913519209517,-38.2370805770931,
0.));
#79163=CARTESIAN_POINT('Ctrl Pts',(-62.3066655565497,-38.2580048333356,
0.));
#79164=CARTESIAN_POINT('Ctrl Pts',(-62.3219821338564,-38.2789742730559,
0.));
#79165=CARTESIAN_POINT('Ctrl Pts',(-62.337301552961,-38.2999888471474,0.));
#79166=CARTESIAN_POINT('Ctrl Pts',(-62.3526237143338,-38.3210485066002,
0.));
#79167=CARTESIAN_POINT('Ctrl Pts',(-62.3679485188178,-38.3421532024915,
0.));
#79168=CARTESIAN_POINT('Ctrl Pts',(-62.3832758676281,-38.3633028859835,
0.));
#79169=CARTESIAN_POINT('Ctrl Pts',(-62.3986056623587,-38.384497508335,0.));
#79170=CARTESIAN_POINT('Ctrl Pts',(-62.4139378049891,-38.4057370209054,
0.));
#79171=CARTESIAN_POINT('Ctrl Pts',(-62.42927219789,-38.4270213751567,0.));
#79172=CARTESIAN_POINT('Ctrl Pts',(-62.4446087438304,-38.4483505226511,
0.));
#79173=CARTESIAN_POINT('Ctrl Pts',(-62.4599473459799,-38.4697244150473,
0.));
#79174=CARTESIAN_POINT('Ctrl Pts',(-62.4752879078842,-38.4911430040988,
0.));
#79175=CARTESIAN_POINT('Ctrl Pts',(-62.4906303334435,-38.5126062416495,
0.));
#79176=CARTESIAN_POINT('Ctrl Pts',(-62.50597452689,-38.5341140796247,0.));
#79177=CARTESIAN_POINT('Ctrl Pts',(-62.5213203927672,-38.5556664700201,
0.));
#79178=CARTESIAN_POINT('Ctrl Pts',(-62.5366678359036,-38.5772633648841,
0.));
#79179=CARTESIAN_POINT('Ctrl Pts',(-62.5520167614529,-38.5989047163401,
0.));
#79180=CARTESIAN_POINT('Ctrl Pts',(-62.567367074937,-38.6205904766078,0.));
#79181=CARTESIAN_POINT('Ctrl Pts',(-62.5827186822923,-38.6423205980214,
0.));
#79182=CARTESIAN_POINT('Ctrl Pts',(-62.5980714899048,-38.6640950330418,
0.));
#79183=CARTESIAN_POINT('Ctrl Pts',(-62.6134254046732,-38.6859137342726,
0.));
#79184=CARTESIAN_POINT('Ctrl Pts',(-62.6287803339534,-38.7077766544411,
0.));
#79185=CARTESIAN_POINT('Ctrl Pts',(-62.6441361854406,-38.7296837463605,
0.));
#79186=CARTESIAN_POINT('Ctrl Pts',(-62.6594928670626,-38.7516349628902,
0.));
#79187=CARTESIAN_POINT('Ctrl Pts',(-62.6748502868836,-38.7736302568982,
0.));
#79188=CARTESIAN_POINT('Ctrl Pts',(-62.6902083529698,-38.7956695812032,
0.));
#79189=CARTESIAN_POINT('Ctrl Pts',(-62.7055669733811,-38.8177528885686,
0.));
#79190=CARTESIAN_POINT('Ctrl Pts',(-62.7209260564506,-38.8398801318184,
0.));
#79191=CARTESIAN_POINT('Ctrl Pts',(-62.7362855110052,-38.8620512639239,
0.));
#79192=CARTESIAN_POINT('Ctrl Pts',(-62.7516452466129,-38.8842662380984,
0.));
#79193=CARTESIAN_POINT('Ctrl Pts',(-62.7670051738132,-38.9065250078824,
0.));
#79194=CARTESIAN_POINT('Ctrl Pts',(-62.7823652043677,-38.9288275272319,
0.));
#79195=CARTESIAN_POINT('Ctrl Pts',(-62.797725250709,-38.9511737503146,0.));
#79196=CARTESIAN_POINT('Ctrl Pts',(-62.8130852254004,-38.9735636313073,
0.));
#79197=CARTESIAN_POINT('Ctrl Pts',(-62.8284450405451,-38.9959971241695,
0.));
#79198=CARTESIAN_POINT('Ctrl Pts',(-62.8438046073237,-39.0184741824649,
0.));
#79199=CARTESIAN_POINT('Ctrl Pts',(-62.859163835209,-39.0409947590519,0.));
#79200=CARTESIAN_POINT('Ctrl Pts',(-62.8745226326046,-39.0635588063308,
0.));
#79201=CARTESIAN_POINT('Ctrl Pts',(-62.8898809082659,-39.0861662767964,
0.));
#79202=CARTESIAN_POINT('Ctrl Pts',(-62.9052385725416,-39.1088171235144,
0.));
#79203=CARTESIAN_POINT('Ctrl Pts',(-62.9205955385551,-39.1315113005745,
0.));
#79204=CARTESIAN_POINT('Ctrl Pts',(-62.9359517237352,-39.1542487636708,
0.));
#79205=CARTESIAN_POINT('Ctrl Pts',(-62.9513070501777,-39.1770294702367,
0.));
#79206=CARTESIAN_POINT('Ctrl Pts',(-62.9644687386693,-39.1965939820802,
0.));
#79207=CARTESIAN_POINT('Ctrl Pts',(-62.9745590018499,-39.2116170128275,
0.));
#79208=CARTESIAN_POINT('Ctrl Pts',(-62.9815782721128,-39.2220794388571,
0.));
#79209=CARTESIAN_POINT('Ctrl Pts',(-62.9855268615901,-39.2279686274717,
0.));
#79210=CARTESIAN_POINT('Ctrl Pts',(-62.9864049293628,-39.2292784191463,
0.));
#79211=CARTESIAN_POINT('',(-60.1903555511633,-35.7368311217509,12.));
#79212=CARTESIAN_POINT('',(-60.1903555511633,-35.7368311217509,0.));
#79213=CARTESIAN_POINT('Ctrl Pts',(-62.9864049293629,-39.2292784191464,
12.));
#79214=CARTESIAN_POINT('Ctrl Pts',(-62.9855268615902,-39.2279686274718,
12.));
#79215=CARTESIAN_POINT('Ctrl Pts',(-62.9815782721128,-39.2220794388572,
12.));
#79216=CARTESIAN_POINT('Ctrl Pts',(-62.9745590018499,-39.2116170128276,
12.));
#79217=CARTESIAN_POINT('Ctrl Pts',(-62.9644687386693,-39.1965939820803,
12.));
#79218=CARTESIAN_POINT('Ctrl Pts',(-62.9513070501777,-39.1770294702367,
12.));
#79219=CARTESIAN_POINT('Ctrl Pts',(-62.9359517237352,-39.1542487636708,
12.));
#79220=CARTESIAN_POINT('Ctrl Pts',(-62.9205955385551,-39.1315113005745,
12.));
#79221=CARTESIAN_POINT('Ctrl Pts',(-62.9052385725416,-39.1088171235144,
12.));
#79222=CARTESIAN_POINT('Ctrl Pts',(-62.8898809082659,-39.0861662767964,
12.));
#79223=CARTESIAN_POINT('Ctrl Pts',(-62.8745226326046,-39.0635588063308,
12.));
#79224=CARTESIAN_POINT('Ctrl Pts',(-62.859163835209,-39.0409947590519,12.));
#79225=CARTESIAN_POINT('Ctrl Pts',(-62.8438046073237,-39.0184741824649,
12.));
#79226=CARTESIAN_POINT('Ctrl Pts',(-62.8284450405451,-38.9959971241695,
12.));
#79227=CARTESIAN_POINT('Ctrl Pts',(-62.8130852254004,-38.9735636313073,
12.));
#79228=CARTESIAN_POINT('Ctrl Pts',(-62.797725250709,-38.9511737503146,12.));
#79229=CARTESIAN_POINT('Ctrl Pts',(-62.7823652043677,-38.9288275272319,
12.));
#79230=CARTESIAN_POINT('Ctrl Pts',(-62.7670051738132,-38.9065250078824,
12.));
#79231=CARTESIAN_POINT('Ctrl Pts',(-62.7516452466129,-38.8842662380984,
12.));
#79232=CARTESIAN_POINT('Ctrl Pts',(-62.7362855110052,-38.8620512639239,
12.));
#79233=CARTESIAN_POINT('Ctrl Pts',(-62.7209260564506,-38.8398801318184,
12.));
#79234=CARTESIAN_POINT('Ctrl Pts',(-62.7055669733811,-38.8177528885686,
12.));
#79235=CARTESIAN_POINT('Ctrl Pts',(-62.6902083529698,-38.7956695812032,
12.));
#79236=CARTESIAN_POINT('Ctrl Pts',(-62.6748502868836,-38.7736302568982,
12.));
#79237=CARTESIAN_POINT('Ctrl Pts',(-62.6594928670626,-38.7516349628902,
12.));
#79238=CARTESIAN_POINT('Ctrl Pts',(-62.6441361854406,-38.7296837463605,
12.));
#79239=CARTESIAN_POINT('Ctrl Pts',(-62.6287803339534,-38.7077766544411,
12.));
#79240=CARTESIAN_POINT('Ctrl Pts',(-62.6134254046732,-38.6859137342726,
12.));
#79241=CARTESIAN_POINT('Ctrl Pts',(-62.5980714899048,-38.6640950330418,
12.));
#79242=CARTESIAN_POINT('Ctrl Pts',(-62.5827186822923,-38.6423205980214,
12.));
#79243=CARTESIAN_POINT('Ctrl Pts',(-62.567367074937,-38.6205904766078,12.));
#79244=CARTESIAN_POINT('Ctrl Pts',(-62.5520167614529,-38.5989047163401,
12.));
#79245=CARTESIAN_POINT('Ctrl Pts',(-62.5366678359036,-38.5772633648841,
12.));
#79246=CARTESIAN_POINT('Ctrl Pts',(-62.5213203927672,-38.5556664700201,
12.));
#79247=CARTESIAN_POINT('Ctrl Pts',(-62.50597452689,-38.5341140796247,12.));
#79248=CARTESIAN_POINT('Ctrl Pts',(-62.4906303334435,-38.5126062416495,
12.));
#79249=CARTESIAN_POINT('Ctrl Pts',(-62.4752879078842,-38.4911430040988,
12.));
#79250=CARTESIAN_POINT('Ctrl Pts',(-62.4599473459799,-38.4697244150473,
12.));
#79251=CARTESIAN_POINT('Ctrl Pts',(-62.4446087438304,-38.4483505226511,
12.));
#79252=CARTESIAN_POINT('Ctrl Pts',(-62.42927219789,-38.4270213751567,12.));
#79253=CARTESIAN_POINT('Ctrl Pts',(-62.4139378049891,-38.4057370209054,
12.));
#79254=CARTESIAN_POINT('Ctrl Pts',(-62.3986056623587,-38.384497508335,12.));
#79255=CARTESIAN_POINT('Ctrl Pts',(-62.3832758676281,-38.3633028859835,
12.));
#79256=CARTESIAN_POINT('Ctrl Pts',(-62.3679485188178,-38.3421532024915,
12.));
#79257=CARTESIAN_POINT('Ctrl Pts',(-62.3526237143338,-38.3210485066002,
12.));
#79258=CARTESIAN_POINT('Ctrl Pts',(-62.337301552961,-38.2999888471474,12.));
#79259=CARTESIAN_POINT('Ctrl Pts',(-62.3219821338564,-38.2789742730559,
12.));
#79260=CARTESIAN_POINT('Ctrl Pts',(-62.3066655565497,-38.2580048333356,
12.));
#79261=CARTESIAN_POINT('Ctrl Pts',(-62.2913519209517,-38.2370805770931,
12.));
#79262=CARTESIAN_POINT('Ctrl Pts',(-62.2760413273601,-38.2162015535351,
12.));
#79263=CARTESIAN_POINT('Ctrl Pts',(-62.2607338764655,-38.1953678119692,
12.));
#79264=CARTESIAN_POINT('Ctrl Pts',(-62.2454296693581,-38.1745794017997,
12.));
#79265=CARTESIAN_POINT('Ctrl Pts',(-62.2301288075319,-38.1538363725263,
12.));
#79266=CARTESIAN_POINT('Ctrl Pts',(-62.2148313928859,-38.1331387737528,
12.));
#79267=CARTESIAN_POINT('Ctrl Pts',(-62.1995375277253,-38.1124866551883,
12.));
#79268=CARTESIAN_POINT('Ctrl Pts',(-62.1842473147627,-38.0918800666479,
12.));
#79269=CARTESIAN_POINT('Ctrl Pts',(-62.1689608571182,-38.0713190580466,
12.));
#79270=CARTESIAN_POINT('Ctrl Pts',(-62.153678258321,-38.0508036793944,12.));
#79271=CARTESIAN_POINT('Ctrl Pts',(-62.1383996223136,-38.0303339808059,
12.));
#79272=CARTESIAN_POINT('Ctrl Pts',(-62.1231250534558,-38.0099100125041,
12.));
#79273=CARTESIAN_POINT('Ctrl Pts',(-62.107854656528,-37.9895318248212,12.));
#79274=CARTESIAN_POINT('Ctrl Pts',(-62.0925885367346,-37.9691994681962,
12.));
#79275=CARTESIAN_POINT('Ctrl Pts',(-62.0773267997072,-37.9489129931685,
12.));
#79276=CARTESIAN_POINT('Ctrl Pts',(-62.0620695515072,-37.9286724503849,
12.));
#79277=CARTESIAN_POINT('Ctrl Pts',(-62.0468168986289,-37.9084778906053,
12.));
#79278=CARTESIAN_POINT('Ctrl Pts',(-62.0315689480022,-37.888329364703,12.));
#79279=CARTESIAN_POINT('Ctrl Pts',(-62.0163258069954,-37.8682269236628,
12.));
#79280=CARTESIAN_POINT('Ctrl Pts',(-62.0010875834176,-37.8481706185742,
12.));
#79281=CARTESIAN_POINT('Ctrl Pts',(-61.9858543855221,-37.8281605006371,
12.));
#79282=CARTESIAN_POINT('Ctrl Pts',(-61.9706263220101,-37.808196621168,12.));
#79283=CARTESIAN_POINT('Ctrl Pts',(-61.9554035020335,-37.7882790316012,
12.));
#79284=CARTESIAN_POINT('Ctrl Pts',(-61.940186035198,-37.7684077834877,12.));
#79285=CARTESIAN_POINT('Ctrl Pts',(-61.9249740315664,-37.748582928488,12.));
#79286=CARTESIAN_POINT('Ctrl Pts',(-61.9097676016616,-37.7288045183765,
12.));
#79287=CARTESIAN_POINT('Ctrl Pts',(-61.8945668564714,-37.7090726050488,
12.));
#79288=CARTESIAN_POINT('Ctrl Pts',(-61.879371907451,-37.6893872405229,12.));
#79289=CARTESIAN_POINT('Ctrl Pts',(-61.8641828665257,-37.6697484769389,
12.));
#79290=CARTESIAN_POINT('Ctrl Pts',(-61.848999846095,-37.6501563665518,12.));
#79291=CARTESIAN_POINT('Ctrl Pts',(-61.8338229590345,-37.6306109617341,
12.));
#79292=CARTESIAN_POINT('Ctrl Pts',(-61.8186523187011,-37.6111123149835,
12.));
#79293=CARTESIAN_POINT('Ctrl Pts',(-61.8034880389362,-37.5916604789252,
12.));
#79294=CARTESIAN_POINT('Ctrl Pts',(-61.7883302340689,-37.5722555063112,
12.));
#79295=CARTESIAN_POINT('Ctrl Pts',(-61.7731790189191,-37.5528974500142,
12.));
#79296=CARTESIAN_POINT('Ctrl Pts',(-61.7580345088014,-37.5335863630286,
12.));
#79297=CARTESIAN_POINT('Ctrl Pts',(-61.7428968195296,-37.5143222984794,
12.));
#79298=CARTESIAN_POINT('Ctrl Pts',(-61.7277660674203,-37.4951053096235,
12.));
#79299=CARTESIAN_POINT('Ctrl Pts',(-61.7126423692965,-37.4759354498509,
12.));
#79300=CARTESIAN_POINT('Ctrl Pts',(-61.69752584249,-37.4568127726776,12.));
#79301=CARTESIAN_POINT('Ctrl Pts',(-61.6824166048454,-37.4377373317456,
12.));
#79302=CARTESIAN_POINT('Ctrl Pts',(-61.667314774725,-37.4187091808324,12.));
#79303=CARTESIAN_POINT('Ctrl Pts',(-61.6522204710133,-37.3997283738534,
12.));
#79304=CARTESIAN_POINT('Ctrl Pts',(-61.6371338131208,-37.3807949648622,
12.));
#79305=CARTESIAN_POINT('Ctrl Pts',(-61.6220549209862,-37.3619090080447,
12.));
#79306=CARTESIAN_POINT('Ctrl Pts',(-61.6069839150804,-37.3430705577178,
12.));
#79307=CARTESIAN_POINT('Ctrl Pts',(-61.591920916412,-37.3242796683395,12.));
#79308=CARTESIAN_POINT('Ctrl Pts',(-61.5768660465313,-37.3055363945108,
12.));
#79309=CARTESIAN_POINT('Ctrl Pts',(-61.5618194275349,-37.286840790977,12.));
#79310=CARTESIAN_POINT('Ctrl Pts',(-61.5467811820686,-37.2681929126217,
12.));
#79311=CARTESIAN_POINT('Ctrl Pts',(-61.5317514333319,-37.2495928144661,
12.));
#79312=CARTESIAN_POINT('Ctrl Pts',(-61.5167303050823,-37.2310405516775,
12.));
#79313=CARTESIAN_POINT('Ctrl Pts',(-61.5017179216404,-37.2125361795727,
12.));
#79314=CARTESIAN_POINT('Ctrl Pts',(-61.4867144078939,-37.1940797536182,
12.));
#79315=CARTESIAN_POINT('Ctrl Pts',(-61.471719889301,-37.1756713294249,12.));
#79316=CARTESIAN_POINT('Ctrl Pts',(-61.4567344918946,-37.157310962747,12.));
#79317=CARTESIAN_POINT('Ctrl Pts',(-61.4417583422888,-37.138998709492,12.));
#79318=CARTESIAN_POINT('Ctrl Pts',(-61.4267915676834,-37.1207346257228,
12.));
#79319=CARTESIAN_POINT('Ctrl Pts',(-61.411834295869,-37.1025187676597,12.));
#79320=CARTESIAN_POINT('Ctrl Pts',(-61.3968866552294,-37.0843511916728,
12.));
#79321=CARTESIAN_POINT('Ctrl Pts',(-61.3819487747458,-37.0662319542827,
12.));
#79322=CARTESIAN_POINT('Ctrl Pts',(-61.3670207840041,-37.0481611121698,
12.));
#79323=CARTESIAN_POINT('Ctrl Pts',(-61.352102813199,-37.0301387221766,12.));
#79324=CARTESIAN_POINT('Ctrl Pts',(-61.3371949931397,-37.0121648413088,
12.));
#79325=CARTESIAN_POINT('Ctrl Pts',(-61.3222974552519,-36.994239526729,12.));
#79326=CARTESIAN_POINT('Ctrl Pts',(-61.3074103315834,-36.976362835757,12.));
#79327=CARTESIAN_POINT('Ctrl Pts',(-61.2925337548113,-36.9585348258798,
12.));
#79328=CARTESIAN_POINT('Ctrl Pts',(-61.2776678582474,-36.9407555547542,
12.));
#79329=CARTESIAN_POINT('Ctrl Pts',(-61.2628127758443,-36.9230250802078,
12.));
#79330=CARTESIAN_POINT('Ctrl Pts',(-61.2479686421979,-36.9053434602324,
12.));
#79331=CARTESIAN_POINT('Ctrl Pts',(-61.2331355925513,-36.8877107529844,
12.));
#79332=CARTESIAN_POINT('Ctrl Pts',(-61.2183137628031,-36.8701270167954,
12.));
#79333=CARTESIAN_POINT('Ctrl Pts',(-61.2035032895121,-36.8525923101736,
12.));
#79334=CARTESIAN_POINT('Ctrl Pts',(-61.1887043099026,-36.8351066918043,
12.));
#79335=CARTESIAN_POINT('Ctrl Pts',(-61.1739169618688,-36.8176702205436,
12.));
#79336=CARTESIAN_POINT('Ctrl Pts',(-61.1591413839809,-36.8002829554221,
12.));
#79337=CARTESIAN_POINT('Ctrl Pts',(-61.1443777154926,-36.782944955654,12.));
#79338=CARTESIAN_POINT('Ctrl Pts',(-61.1296260963468,-36.7656562806381,
12.));
#79339=CARTESIAN_POINT('Ctrl Pts',(-61.1148866671821,-36.7484169899591,
12.));
#79340=CARTESIAN_POINT('Ctrl Pts',(-61.1001595693357,-36.7312271433799,
12.));
#79341=CARTESIAN_POINT('Ctrl Pts',(-61.085444944851,-36.7140868008479,12.));
#79342=CARTESIAN_POINT('Ctrl Pts',(-61.0707429364841,-36.6969960225019,
12.));
#79343=CARTESIAN_POINT('Ctrl Pts',(-61.0560536877084,-36.6799548686741,
12.));
#79344=CARTESIAN_POINT('Ctrl Pts',(-61.0413773427204,-36.6629633998885,
12.));
#79345=CARTESIAN_POINT('Ctrl Pts',(-61.0267140464434,-36.6460216768553,
12.));
#79346=CARTESIAN_POINT('Ctrl Pts',(-61.012063944535,-36.6291297604775,12.));
#79347=CARTESIAN_POINT('Ctrl Pts',(-60.9974271833982,-36.6122877118599,
12.));
#79348=CARTESIAN_POINT('Ctrl Pts',(-60.9828039101887,-36.5954955923109,
12.));
#79349=CARTESIAN_POINT('Ctrl Pts',(-60.9681942728237,-36.5787534633416,
12.));
#79350=CARTESIAN_POINT('Ctrl Pts',(-60.9535984199874,-36.5620613866615,
12.));
#79351=CARTESIAN_POINT('Ctrl Pts',(-60.9390165011357,-36.5454194241866,
12.));
#79352=CARTESIAN_POINT('Ctrl Pts',(-60.924448666499,-36.5288276380417,12.));
#79353=CARTESIAN_POINT('Ctrl Pts',(-60.9098950670847,-36.5122860905611,
12.));
#79354=CARTESIAN_POINT('Ctrl Pts',(-60.8953558546791,-36.4957948442832,
12.));
#79355=CARTESIAN_POINT('Ctrl Pts',(-60.8808311818489,-36.4793539619459,
12.));
#79356=CARTESIAN_POINT('Ctrl Pts',(-60.8663212019646,-36.4629635065037,
12.));
#79357=CARTESIAN_POINT('Ctrl Pts',(-60.851826069218,-36.4466235411353,12.));
#79358=CARTESIAN_POINT('Ctrl Pts',(-60.8373459386397,-36.4303341292497,
12.));
#79359=CARTESIAN_POINT('Ctrl Pts',(-60.8228809661179,-36.4140953344869,
12.));
#79360=CARTESIAN_POINT('Ctrl Pts',(-60.8084313084009,-36.3979072207174,
12.));
#79361=CARTESIAN_POINT('Ctrl Pts',(-60.7939971230781,-36.38176985204,12.));
#79362=CARTESIAN_POINT('Ctrl Pts',(-60.7795785685631,-36.3656832927733,
12.));
#79363=CARTESIAN_POINT('Ctrl Pts',(-60.7651758040792,-36.349647607448,12.));
#79364=CARTESIAN_POINT('Ctrl Pts',(-60.7507889896284,-36.3336628607844,
12.));
#79365=CARTESIAN_POINT('Ctrl Pts',(-60.7364182860388,-36.3177291177148,
12.));
#79366=CARTESIAN_POINT('Ctrl Pts',(-60.7220638550396,-36.3018464434204,
12.));
#79367=CARTESIAN_POINT('Ctrl Pts',(-60.7077258593268,-36.2860149033586,
12.));
#79368=CARTESIAN_POINT('Ctrl Pts',(-60.6934044626304,-36.2702345632882,
12.));
#79369=CARTESIAN_POINT('Ctrl Pts',(-60.6790998297823,-36.2545054892911,
12.));
#79370=CARTESIAN_POINT('Ctrl Pts',(-60.6648121265908,-36.2388277477225,
12.));
#79371=CARTESIAN_POINT('Ctrl Pts',(-60.6505415197055,-36.2232014051549,
12.));
#79372=CARTESIAN_POINT('Ctrl Pts',(-60.6362881765014,-36.2076265283261,
12.));
#79373=CARTESIAN_POINT('Ctrl Pts',(-60.6220522649129,-36.1921031840617,
12.));
#79374=CARTESIAN_POINT('Ctrl Pts',(-60.6078339534151,-36.1766314392624,
12.));
#79375=CARTESIAN_POINT('Ctrl Pts',(-60.5936334114083,-36.1612113610758,
12.));
#79376=CARTESIAN_POINT('Ctrl Pts',(-60.5794508095555,-36.1458430170425,
12.));
#79377=CARTESIAN_POINT('Ctrl Pts',(-60.5652863200732,-36.1305264752195,
12.));
#79378=CARTESIAN_POINT('Ctrl Pts',(-60.5511401172014,-36.1152618043756,
12.));
#79379=CARTESIAN_POINT('Ctrl Pts',(-60.5370123768841,-36.1000490738532,
12.));
#79380=CARTESIAN_POINT('Ctrl Pts',(-60.5229032759001,-36.0848883531968,
12.));
#79381=CARTESIAN_POINT('Ctrl Pts',(-60.5088129911357,-36.0697797118377,
12.));
#79382=CARTESIAN_POINT('Ctrl Pts',(-60.4947416988396,-36.0547232187681,
12.));
#79383=CARTESIAN_POINT('Ctrl Pts',(-60.4806895737643,-36.0397189421617,
12.));
#79384=CARTESIAN_POINT('Ctrl Pts',(-60.4666567908053,-36.0247669500867,
12.));
#79385=CARTESIAN_POINT('Ctrl Pts',(-60.452643526964,-36.0098673113556,12.));
#79386=CARTESIAN_POINT('Ctrl Pts',(-60.438649962949,-35.9950200962175,12.));
#79387=CARTESIAN_POINT('Ctrl Pts',(-60.4246762854961,-35.9802253773534,
12.));
#79388=CARTESIAN_POINT('Ctrl Pts',(-60.4107226875759,-35.9654832299627,
12.));
#79389=CARTESIAN_POINT('Ctrl Pts',(-60.3967893635487,-35.9507937296726,
12.));
#79390=CARTESIAN_POINT('Ctrl Pts',(-60.3828765049031,-35.9361569506955,
12.));
#79391=CARTESIAN_POINT('Ctrl Pts',(-60.368984296546,-35.9215729642219,12.));
#79392=CARTESIAN_POINT('Ctrl Pts',(-60.3551129108794,-35.9070418358501,
12.));
#79393=CARTESIAN_POINT('Ctrl Pts',(-60.3412625135223,-35.8925636280632,
12.));
#79394=CARTESIAN_POINT('Ctrl Pts',(-60.3274332746782,-35.878138405151,12.));
#79395=CARTESIAN_POINT('Ctrl Pts',(-60.313625378281,-35.8637662371635,12.));
#79396=CARTESIAN_POINT('Ctrl Pts',(-60.2998390330173,-35.8494472046783,
12.));
#79397=CARTESIAN_POINT('Ctrl Pts',(-60.2860744798563,-35.8351814020424,
12.));
#79398=CARTESIAN_POINT('Ctrl Pts',(-60.2723319687507,-35.8209689272574,
12.));
#79399=CARTESIAN_POINT('Ctrl Pts',(-60.2586117365278,-35.8068098723386,
12.));
#79400=CARTESIAN_POINT('Ctrl Pts',(-60.2449139865206,-35.7927043145164,
12.));
#79401=CARTESIAN_POINT('Ctrl Pts',(-60.2312388621286,-35.7786523045782,
12.));
#79402=CARTESIAN_POINT('Ctrl Pts',(-60.2175864449678,-35.7646538667299,
12.));
#79403=CARTESIAN_POINT('Ctrl Pts',(-60.2066827086579,-35.7534979801871,
12.));
#79404=CARTESIAN_POINT('Ctrl Pts',(-60.1985151474406,-35.7451551752456,
12.));
#79405=CARTESIAN_POINT('Ctrl Pts',(-60.1930746580239,-35.7396040203973,
12.));
#79406=CARTESIAN_POINT('Ctrl Pts',(-60.1903555511633,-35.7368311217509,
12.));
#79407=CARTESIAN_POINT('Ctrl Pts',(-62.1730054756879,-40.506059810093,0.));
#79408=CARTESIAN_POINT('Ctrl Pts',(-62.1730054756879,-40.506059810093,4.));
#79409=CARTESIAN_POINT('Ctrl Pts',(-62.1730054756879,-40.506059810093,8.));
#79410=CARTESIAN_POINT('Ctrl Pts',(-62.1730054756879,-40.506059810093,12.));
#79411=CARTESIAN_POINT('Ctrl Pts',(-62.2815834512361,-40.5229411493977,
0.));
#79412=CARTESIAN_POINT('Ctrl Pts',(-62.2815834512361,-40.5229411493977,
4.));
#79413=CARTESIAN_POINT('Ctrl Pts',(-62.2815834512362,-40.5229411493977,
8.));
#79414=CARTESIAN_POINT('Ctrl Pts',(-62.2815834512362,-40.5229411493977,
12.));
#79415=CARTESIAN_POINT('Ctrl Pts',(-62.4810961163748,-40.4873422218646,
0.));
#79416=CARTESIAN_POINT('Ctrl Pts',(-62.4810961163748,-40.4873422218646,
4.00000000000001));
#79417=CARTESIAN_POINT('Ctrl Pts',(-62.4810961163749,-40.4873422218646,
7.99999999999999));
#79418=CARTESIAN_POINT('Ctrl Pts',(-62.4810961163749,-40.4873422218646,
12.));
#79419=CARTESIAN_POINT('Ctrl Pts',(-62.6258675056117,-40.3516729626243,
0.));
#79420=CARTESIAN_POINT('Ctrl Pts',(-62.6258675056117,-40.3516729626243,
4.));
#79421=CARTESIAN_POINT('Ctrl Pts',(-62.6258675056118,-40.3516729626244,
8.00000000000001));
#79422=CARTESIAN_POINT('Ctrl Pts',(-62.6258675056118,-40.3516729626244,
12.));
#79423=CARTESIAN_POINT('Ctrl Pts',(-62.6704278106374,-40.2823469776989,
0.));
#79424=CARTESIAN_POINT('Ctrl Pts',(-62.6704278106374,-40.2823469776989,
4.));
#79425=CARTESIAN_POINT('Ctrl Pts',(-62.6704278106375,-40.282346977699,8.));
#79426=CARTESIAN_POINT('Ctrl Pts',(-62.6704278106375,-40.282346977699,12.));
#79427=CARTESIAN_POINT('',(-62.1730054756878,-40.506059810093,0.));
#79428=CARTESIAN_POINT('',(-62.6704278106372,-40.2823469776988,0.));
#79429=CARTESIAN_POINT('Ctrl Pts',(-62.1730054756879,-40.506059810093,2.77555756156289E-16));
#79430=CARTESIAN_POINT('Ctrl Pts',(-62.2815834512361,-40.5229411493977,
2.77555756156289E-16));
#79431=CARTESIAN_POINT('Ctrl Pts',(-62.3955906884582,-40.5025989050931,
2.77555756156289E-16));
#79432=CARTESIAN_POINT('Ctrl Pts',(-62.4917232233451,-40.4495806341085,
2.77555756156289E-16));
#79433=CARTESIAN_POINT('Ctrl Pts',(-62.5638226245102,-40.4098169308702,
2.77555756156289E-16));
#79434=CARTESIAN_POINT('Ctrl Pts',(-62.6258675056117,-40.3516729626243,
2.77555756156289E-16));
#79435=CARTESIAN_POINT('Ctrl Pts',(-62.6704278106374,-40.2823469776989,
2.77555756156289E-16));
#79436=CARTESIAN_POINT('',(-62.6704278106372,-40.2823469776988,12.));
#79437=CARTESIAN_POINT('Ctrl Pts',(-62.6704278106374,-40.2823469776989,
0.));
#79438=CARTESIAN_POINT('Ctrl Pts',(-62.6704278106374,-40.2823469776989,
4.));
#79439=CARTESIAN_POINT('Ctrl Pts',(-62.6704278106375,-40.282346977699,8.));
#79440=CARTESIAN_POINT('Ctrl Pts',(-62.6704278106375,-40.282346977699,12.));
#79441=CARTESIAN_POINT('',(-62.1730054756879,-40.506059810093,12.));
#79442=CARTESIAN_POINT('Ctrl Pts',(-62.6704278106375,-40.282346977699,12.));
#79443=CARTESIAN_POINT('Ctrl Pts',(-62.6258675056118,-40.3516729626244,
12.));
#79444=CARTESIAN_POINT('Ctrl Pts',(-62.5638226245103,-40.4098169308702,
12.));
#79445=CARTESIAN_POINT('Ctrl Pts',(-62.4917232233451,-40.4495806341086,
12.));
#79446=CARTESIAN_POINT('Ctrl Pts',(-62.3955906884583,-40.5025989050931,
12.));
#79447=CARTESIAN_POINT('Ctrl Pts',(-62.2815834512362,-40.5229411493977,
12.));
#79448=CARTESIAN_POINT('Ctrl Pts',(-62.1730054756879,-40.506059810093,12.));
#79449=CARTESIAN_POINT('Ctrl Pts',(-62.1730054756879,-40.506059810093,12.));
#79450=CARTESIAN_POINT('Ctrl Pts',(-62.1730054756879,-40.506059810093,8.));
#79451=CARTESIAN_POINT('Ctrl Pts',(-62.1730054756879,-40.506059810093,4.));
#79452=CARTESIAN_POINT('Ctrl Pts',(-62.1730054756879,-40.506059810093,0.));
#79453=CARTESIAN_POINT('Origin',(-3.16086693261782E-10,-2.01487121870483E-10,
0.));
#79454=CARTESIAN_POINT('Origin',(-3.16086693261782E-10,-2.01487121870483E-10,
12.));
#79455=CARTESIAN_POINT('Origin',(-3.16086693261782E-10,-2.01487121870483E-10,
0.));
#79456=CARTESIAN_POINT('Ctrl Pts',(-66.2207497120638,-34.1330090612036,
0.));
#79457=CARTESIAN_POINT('Ctrl Pts',(-66.2207497120638,-34.1330090612036,
4.));
#79458=CARTESIAN_POINT('Ctrl Pts',(-66.2207497120638,-34.1330090612036,
8.));
#79459=CARTESIAN_POINT('Ctrl Pts',(-66.2207497120638,-34.1330090612036,
12.));
#79460=CARTESIAN_POINT('Ctrl Pts',(-66.2710935941675,-34.0353379297089,
0.));
#79461=CARTESIAN_POINT('Ctrl Pts',(-66.2710935941675,-34.0353379297089,
4.));
#79462=CARTESIAN_POINT('Ctrl Pts',(-66.2710935941675,-34.0353379297089,
8.00000000000001));
#79463=CARTESIAN_POINT('Ctrl Pts',(-66.2710935941675,-34.0353379297089,
12.));
#79464=CARTESIAN_POINT('Ctrl Pts',(-66.3003999311009,-33.8348041971634,
0.));
#79465=CARTESIAN_POINT('Ctrl Pts',(-66.3003999311009,-33.8348041971634,
4.));
#79466=CARTESIAN_POINT('Ctrl Pts',(-66.3003999311009,-33.8348041971634,
7.99999999999999));
#79467=CARTESIAN_POINT('Ctrl Pts',(-66.3003999311009,-33.8348041971634,
12.));
#79468=CARTESIAN_POINT('Ctrl Pts',(-66.2174610329231,-33.6545652280942,
0.));
#79469=CARTESIAN_POINT('Ctrl Pts',(-66.2174610329231,-33.6545652280942,
4.));
#79470=CARTESIAN_POINT('Ctrl Pts',(-66.2174610329231,-33.6545652280942,
8.00000000000001));
#79471=CARTESIAN_POINT('Ctrl Pts',(-66.2174610329231,-33.6545652280942,
12.));
#79472=CARTESIAN_POINT('Ctrl Pts',(-66.165779540567,-33.5903722664959,0.));
#79473=CARTESIAN_POINT('Ctrl Pts',(-66.165779540567,-33.5903722664959,4.));
#79474=CARTESIAN_POINT('Ctrl Pts',(-66.165779540567,-33.5903722664959,8.));
#79475=CARTESIAN_POINT('Ctrl Pts',(-66.165779540567,-33.5903722664959,12.));
#79476=CARTESIAN_POINT('',(-66.2207497120638,-34.1330090612036,0.));
#79477=CARTESIAN_POINT('',(-66.165779540567,-33.5903722664959,0.));
#79478=CARTESIAN_POINT('Ctrl Pts',(-66.2207497120638,-34.1330090612036,
1.38777878078145E-16));
#79479=CARTESIAN_POINT('Ctrl Pts',(-66.2710935941675,-34.0353379297089,
1.38777878078145E-16));
#79480=CARTESIAN_POINT('Ctrl Pts',(-66.2878400724152,-33.9207472253972,
1.38777878078145E-16));
#79481=CARTESIAN_POINT('Ctrl Pts',(-66.2679350453204,-33.8127833826287,
1.38777878078145E-16));
#79482=CARTESIAN_POINT('Ctrl Pts',(-66.2530062749993,-33.7318105005524,
1.38777878078145E-16));
#79483=CARTESIAN_POINT('Ctrl Pts',(-66.2174610329231,-33.6545652280942,
1.38777878078144E-16));
#79484=CARTESIAN_POINT('Ctrl Pts',(-66.165779540567,-33.5903722664959,1.38777878078145E-16));
#79485=CARTESIAN_POINT('',(-66.1657795405671,-33.5903722664959,12.));
#79486=CARTESIAN_POINT('Ctrl Pts',(-66.165779540567,-33.5903722664959,0.));
#79487=CARTESIAN_POINT('Ctrl Pts',(-66.165779540567,-33.5903722664959,4.));
#79488=CARTESIAN_POINT('Ctrl Pts',(-66.165779540567,-33.5903722664959,8.));
#79489=CARTESIAN_POINT('Ctrl Pts',(-66.165779540567,-33.5903722664959,12.));
#79490=CARTESIAN_POINT('',(-66.2207497120638,-34.1330090612036,12.));
#79491=CARTESIAN_POINT('Ctrl Pts',(-66.165779540567,-33.5903722664959,12.));
#79492=CARTESIAN_POINT('Ctrl Pts',(-66.2174610329231,-33.6545652280942,
12.));
#79493=CARTESIAN_POINT('Ctrl Pts',(-66.2530062749993,-33.7318105005524,
12.));
#79494=CARTESIAN_POINT('Ctrl Pts',(-66.2679350453204,-33.8127833826288,
12.));
#79495=CARTESIAN_POINT('Ctrl Pts',(-66.2878400724152,-33.9207472253972,
12.));
#79496=CARTESIAN_POINT('Ctrl Pts',(-66.2710935941675,-34.0353379297089,
12.));
#79497=CARTESIAN_POINT('Ctrl Pts',(-66.2207497120638,-34.1330090612036,
12.));
#79498=CARTESIAN_POINT('Ctrl Pts',(-66.2207497120638,-34.1330090612036,
12.));
#79499=CARTESIAN_POINT('Ctrl Pts',(-66.2207497120638,-34.1330090612036,
8.));
#79500=CARTESIAN_POINT('Ctrl Pts',(-66.2207497120638,-34.1330090612036,
4.));
#79501=CARTESIAN_POINT('Ctrl Pts',(-66.2207497120638,-34.1330090612036,
0.));
#79502=CARTESIAN_POINT('Ctrl Pts',(-63.0759831361898,-30.3549065457811,
0.));
#79503=CARTESIAN_POINT('Ctrl Pts',(-63.0759831361898,-30.3549065457811,
12.));
#79504=CARTESIAN_POINT('Ctrl Pts',(-63.078933570069,-30.3574319069329,0.));
#79505=CARTESIAN_POINT('Ctrl Pts',(-63.078933570069,-30.3574319069329,12.));
#79506=CARTESIAN_POINT('Ctrl Pts',(-63.0848371718048,-30.3624877680651,
0.));
#79507=CARTESIAN_POINT('Ctrl Pts',(-63.0848371718048,-30.3624877680651,
12.));
#79508=CARTESIAN_POINT('Ctrl Pts',(-63.0937007763471,-30.3700869762507,
0.));
#79509=CARTESIAN_POINT('Ctrl Pts',(-63.0937007763471,-30.3700869762507,
12.));
#79510=CARTESIAN_POINT('Ctrl Pts',(-63.105535320226,-30.3802500880403,0.));
#79511=CARTESIAN_POINT('Ctrl Pts',(-63.105535320226,-30.3802500880403,12.));
#79512=CARTESIAN_POINT('Ctrl Pts',(-63.1203558300657,-30.3930053710484,
0.));
#79513=CARTESIAN_POINT('Ctrl Pts',(-63.1203558300657,-30.3930053710484,
12.));
#79514=CARTESIAN_POINT('Ctrl Pts',(-63.135203629844,-30.4058120432228,0.));
#79515=CARTESIAN_POINT('Ctrl Pts',(-63.135203629844,-30.4058120432228,12.));
#79516=CARTESIAN_POINT('Ctrl Pts',(-63.1500786361459,-30.418670087563,0.));
#79517=CARTESIAN_POINT('Ctrl Pts',(-63.1500786361459,-30.418670087563,12.));
#79518=CARTESIAN_POINT('Ctrl Pts',(-63.164980701691,-30.4315794659731,0.));
#79519=CARTESIAN_POINT('Ctrl Pts',(-63.164980701691,-30.4315794659731,12.));
#79520=CARTESIAN_POINT('Ctrl Pts',(-63.179909617189,-30.444540119238,0.));
#79521=CARTESIAN_POINT('Ctrl Pts',(-63.179909617189,-30.444540119238,12.));
#79522=CARTESIAN_POINT('Ctrl Pts',(-63.1948651386942,-30.4575519763337,
0.));
#79523=CARTESIAN_POINT('Ctrl Pts',(-63.1948651386942,-30.4575519763337,
12.));
#79524=CARTESIAN_POINT('Ctrl Pts',(-63.2098470086636,-30.470614961416,0.));
#79525=CARTESIAN_POINT('Ctrl Pts',(-63.2098470086636,-30.470614961416,12.));
#79526=CARTESIAN_POINT('Ctrl Pts',(-63.2248549788221,-30.4837290014989,
0.));
#79527=CARTESIAN_POINT('Ctrl Pts',(-63.2248549788221,-30.4837290014989,
12.));
#79528=CARTESIAN_POINT('Ctrl Pts',(-63.2398888342545,-30.4968940344998,
0.));
#79529=CARTESIAN_POINT('Ctrl Pts',(-63.2398888342545,-30.4968940344998,
12.));
#79530=CARTESIAN_POINT('Ctrl Pts',(-63.2549483856215,-30.5101100066659,
0.));
#79531=CARTESIAN_POINT('Ctrl Pts',(-63.2549483856215,-30.5101100066659,
12.));
#79532=CARTESIAN_POINT('Ctrl Pts',(-63.2700334577639,-30.5233768687865,
0.));
#79533=CARTESIAN_POINT('Ctrl Pts',(-63.2700334577639,-30.5233768687865,
12.));
#79534=CARTESIAN_POINT('Ctrl Pts',(-63.2851438802473,-30.5366945730508,
0.));
#79535=CARTESIAN_POINT('Ctrl Pts',(-63.2851438802473,-30.5366945730508,
12.));
#79536=CARTESIAN_POINT('Ctrl Pts',(-63.3002794756086,-30.5500630691359,
0.));
#79537=CARTESIAN_POINT('Ctrl Pts',(-63.3002794756086,-30.5500630691359,
12.));
#79538=CARTESIAN_POINT('Ctrl Pts',(-63.3154400534397,-30.563482302238,0.));
#79539=CARTESIAN_POINT('Ctrl Pts',(-63.3154400534397,-30.563482302238,12.));
#79540=CARTESIAN_POINT('Ctrl Pts',(-63.3306254165126,-30.5769522151164,
0.));
#79541=CARTESIAN_POINT('Ctrl Pts',(-63.3306254165126,-30.5769522151164,
12.));
#79542=CARTESIAN_POINT('Ctrl Pts',(-63.3458353646154,-30.5904727493711,
0.));
#79543=CARTESIAN_POINT('Ctrl Pts',(-63.3458353646154,-30.5904727493711,
12.));
#79544=CARTESIAN_POINT('Ctrl Pts',(-63.3610696989577,-30.6040438469078,
0.));
#79545=CARTESIAN_POINT('Ctrl Pts',(-63.3610696989577,-30.6040438469078,
12.));
#79546=CARTESIAN_POINT('Ctrl Pts',(-63.3763282271796,-30.6176654515967,
0.));
#79547=CARTESIAN_POINT('Ctrl Pts',(-63.3763282271796,-30.6176654515967,
12.));
#79548=CARTESIAN_POINT('Ctrl Pts',(-63.3916107631376,-30.6313375092062,
0.));
#79549=CARTESIAN_POINT('Ctrl Pts',(-63.3916107631376,-30.6313375092062,
12.));
#79550=CARTESIAN_POINT('Ctrl Pts',(-63.4069171245066,-30.6450599666121,
0.));
#79551=CARTESIAN_POINT('Ctrl Pts',(-63.4069171245066,-30.6450599666121,
12.));
#79552=CARTESIAN_POINT('Ctrl Pts',(-63.4222471311239,-30.6588327712483,
0.));
#79553=CARTESIAN_POINT('Ctrl Pts',(-63.4222471311239,-30.6588327712483,
12.));
#79554=CARTESIAN_POINT('Ctrl Pts',(-63.4376006029604,-30.6726558704315,
0.));
#79555=CARTESIAN_POINT('Ctrl Pts',(-63.4376006029604,-30.6726558704315,
12.));
#79556=CARTESIAN_POINT('Ctrl Pts',(-63.4529773584249,-30.6865292107929,
0.));
#79557=CARTESIAN_POINT('Ctrl Pts',(-63.4529773584249,-30.6865292107929,
12.));
#79558=CARTESIAN_POINT('Ctrl Pts',(-63.4683772152529,-30.7004527385821,
0.));
#79559=CARTESIAN_POINT('Ctrl Pts',(-63.4683772152529,-30.7004527385821,
12.));
#79560=CARTESIAN_POINT('Ctrl Pts',(-63.4837999912771,-30.7144263999265,
0.));
#79561=CARTESIAN_POINT('Ctrl Pts',(-63.4837999912771,-30.7144263999265,
12.));
#79562=CARTESIAN_POINT('Ctrl Pts',(-63.4992455051795,-30.7284501410822,
0.));
#79563=CARTESIAN_POINT('Ctrl Pts',(-63.4992455051795,-30.7284501410822,
12.));
#79564=CARTESIAN_POINT('Ctrl Pts',(-63.5147135773894,-30.7425239087281,
0.));
#79565=CARTESIAN_POINT('Ctrl Pts',(-63.5147135773894,-30.7425239087281,
12.));
#79566=CARTESIAN_POINT('Ctrl Pts',(-63.5302040304142,-30.7566476500757,
0.));
#79567=CARTESIAN_POINT('Ctrl Pts',(-63.5302040304142,-30.7566476500757,
12.));
#79568=CARTESIAN_POINT('Ctrl Pts',(-63.5457166883537,-30.7708213127159,
0.));
#79569=CARTESIAN_POINT('Ctrl Pts',(-63.5457166883537,-30.7708213127159,
12.));
#79570=CARTESIAN_POINT('Ctrl Pts',(-63.5612513766,-30.7850448445205,0.));
#79571=CARTESIAN_POINT('Ctrl Pts',(-63.5612513766,-30.7850448445205,12.));
#79572=CARTESIAN_POINT('Ctrl Pts',(-63.5768079214881,-30.7993181935271,
0.));
#79573=CARTESIAN_POINT('Ctrl Pts',(-63.5768079214881,-30.7993181935271,
12.));
#79574=CARTESIAN_POINT('Ctrl Pts',(-63.5923861498987,-30.813641307801,0.));
#79575=CARTESIAN_POINT('Ctrl Pts',(-63.5923861498987,-30.813641307801,12.));
#79576=CARTESIAN_POINT('Ctrl Pts',(-63.6079858892771,-30.8280141354459,
0.));
#79577=CARTESIAN_POINT('Ctrl Pts',(-63.6079858892771,-30.8280141354459,
12.));
#79578=CARTESIAN_POINT('Ctrl Pts',(-63.6236069678055,-30.8424366246671,
0.));
#79579=CARTESIAN_POINT('Ctrl Pts',(-63.6236069678055,-30.8424366246671,
12.));
#79580=CARTESIAN_POINT('Ctrl Pts',(-63.6392492145233,-30.8569087238131,
0.));
#79581=CARTESIAN_POINT('Ctrl Pts',(-63.6392492145233,-30.8569087238131,
12.));
#79582=CARTESIAN_POINT('Ctrl Pts',(-63.6549124594666,-30.8714303814194,
0.));
#79583=CARTESIAN_POINT('Ctrl Pts',(-63.6549124594666,-30.8714303814194,
12.));
#79584=CARTESIAN_POINT('Ctrl Pts',(-63.6705965337971,-30.8860015462475,
0.));
#79585=CARTESIAN_POINT('Ctrl Pts',(-63.6705965337971,-30.8860015462475,
12.));
#79586=CARTESIAN_POINT('Ctrl Pts',(-63.6863012697328,-30.900622167269,0.));
#79587=CARTESIAN_POINT('Ctrl Pts',(-63.6863012697328,-30.900622167269,12.));
#79588=CARTESIAN_POINT('Ctrl Pts',(-63.7020265004792,-30.9152921936465,
0.));
#79589=CARTESIAN_POINT('Ctrl Pts',(-63.7020265004792,-30.9152921936465,
12.));
#79590=CARTESIAN_POINT('Ctrl Pts',(-63.7177720601609,-30.9300115747115,
0.));
#79591=CARTESIAN_POINT('Ctrl Pts',(-63.7177720601609,-30.9300115747115,
12.));
#79592=CARTESIAN_POINT('Ctrl Pts',(-63.7335377837441,-30.9447802599355,
0.));
#79593=CARTESIAN_POINT('Ctrl Pts',(-63.7335377837441,-30.9447802599355,
12.));
#79594=CARTESIAN_POINT('Ctrl Pts',(-63.749323506987,-30.9595981989103,0.));
#79595=CARTESIAN_POINT('Ctrl Pts',(-63.749323506987,-30.9595981989103,12.));
#79596=CARTESIAN_POINT('Ctrl Pts',(-63.7651290664733,-30.9744653413689,
0.));
#79597=CARTESIAN_POINT('Ctrl Pts',(-63.7651290664733,-30.9744653413689,
12.));
#79598=CARTESIAN_POINT('Ctrl Pts',(-63.7809542996264,-30.989381637191,0.));
#79599=CARTESIAN_POINT('Ctrl Pts',(-63.7809542996264,-30.989381637191,12.));
#79600=CARTESIAN_POINT('Ctrl Pts',(-63.796799044728,-31.0043470364108,0.));
#79601=CARTESIAN_POINT('Ctrl Pts',(-63.796799044728,-31.0043470364108,12.));
#79602=CARTESIAN_POINT('Ctrl Pts',(-63.8126631409364,-31.0193614892171,
0.));
#79603=CARTESIAN_POINT('Ctrl Pts',(-63.8126631409364,-31.0193614892171,
12.));
#79604=CARTESIAN_POINT('Ctrl Pts',(-63.8285464282846,-31.0344249459538,
0.));
#79605=CARTESIAN_POINT('Ctrl Pts',(-63.8285464282846,-31.0344249459538,
12.));
#79606=CARTESIAN_POINT('Ctrl Pts',(-63.8444487476611,-31.0495373571215,
0.));
#79607=CARTESIAN_POINT('Ctrl Pts',(-63.8444487476611,-31.0495373571215,
12.));
#79608=CARTESIAN_POINT('Ctrl Pts',(-63.8603699407922,-31.0646986733723,
0.));
#79609=CARTESIAN_POINT('Ctrl Pts',(-63.8603699407922,-31.0646986733723,
12.));
#79610=CARTESIAN_POINT('Ctrl Pts',(-63.8763098502237,-31.0799088455041,
0.));
#79611=CARTESIAN_POINT('Ctrl Pts',(-63.8763098502237,-31.0799088455041,
12.));
#79612=CARTESIAN_POINT('Ctrl Pts',(-63.8922683192964,-31.0951678244455,
0.));
#79613=CARTESIAN_POINT('Ctrl Pts',(-63.8922683192964,-31.0951678244455,
12.));
#79614=CARTESIAN_POINT('Ctrl Pts',(-63.9082451921448,-31.1104755612607,
0.));
#79615=CARTESIAN_POINT('Ctrl Pts',(-63.9082451921448,-31.1104755612607,
12.));
#79616=CARTESIAN_POINT('Ctrl Pts',(-63.9242403136955,-31.1258320071545,
0.));
#79617=CARTESIAN_POINT('Ctrl Pts',(-63.9242403136955,-31.1258320071545,
12.));
#79618=CARTESIAN_POINT('Ctrl Pts',(-63.940253529665,-31.1412371134727,0.));
#79619=CARTESIAN_POINT('Ctrl Pts',(-63.940253529665,-31.1412371134727,12.));
#79620=CARTESIAN_POINT('Ctrl Pts',(-63.9562846865567,-31.1566908316992,
0.));
#79621=CARTESIAN_POINT('Ctrl Pts',(-63.9562846865567,-31.1566908316992,
12.));
#79622=CARTESIAN_POINT('Ctrl Pts',(-63.9723336316551,-31.1721931134487,
0.));
#79623=CARTESIAN_POINT('Ctrl Pts',(-63.9723336316551,-31.1721931134487,
12.));
#79624=CARTESIAN_POINT('Ctrl Pts',(-63.9884002130211,-31.1877439104717,
0.));
#79625=CARTESIAN_POINT('Ctrl Pts',(-63.9884002130211,-31.1877439104717,
12.));
#79626=CARTESIAN_POINT('Ctrl Pts',(-64.0044842794831,-31.2033431746558,
0.));
#79627=CARTESIAN_POINT('Ctrl Pts',(-64.0044842794831,-31.2033431746558,
12.));
#79628=CARTESIAN_POINT('Ctrl Pts',(-64.02058568063,-31.2189908580245,0.));
#79629=CARTESIAN_POINT('Ctrl Pts',(-64.02058568063,-31.2189908580245,12.));
#79630=CARTESIAN_POINT('Ctrl Pts',(-64.0367042667984,-31.2346869127297,
0.));
#79631=CARTESIAN_POINT('Ctrl Pts',(-64.0367042667984,-31.2346869127297,
12.));
#79632=CARTESIAN_POINT('Ctrl Pts',(-64.0528398890657,-31.2504312910451,
0.));
#79633=CARTESIAN_POINT('Ctrl Pts',(-64.0528398890657,-31.2504312910451,
12.));
#79634=CARTESIAN_POINT('Ctrl Pts',(-64.0689923992461,-31.2662239453728,
0.));
#79635=CARTESIAN_POINT('Ctrl Pts',(-64.0689923992461,-31.2662239453728,
12.));
#79636=CARTESIAN_POINT('Ctrl Pts',(-64.0851616498852,-31.2820648282447,
0.));
#79637=CARTESIAN_POINT('Ctrl Pts',(-64.0851616498852,-31.2820648282447,
12.));
#79638=CARTESIAN_POINT('Ctrl Pts',(-64.1013474942556,-31.2979538923214,
0.));
#79639=CARTESIAN_POINT('Ctrl Pts',(-64.1013474942556,-31.2979538923214,
12.));
#79640=CARTESIAN_POINT('Ctrl Pts',(-64.117549786349,-31.3138910903859,0.));
#79641=CARTESIAN_POINT('Ctrl Pts',(-64.117549786349,-31.3138910903859,12.));
#79642=CARTESIAN_POINT('Ctrl Pts',(-64.133768380869,-31.3298763753377,0.));
#79643=CARTESIAN_POINT('Ctrl Pts',(-64.133768380869,-31.3298763753377,12.));
#79644=CARTESIAN_POINT('Ctrl Pts',(-64.1500031332282,-31.3459097002006,
0.));
#79645=CARTESIAN_POINT('Ctrl Pts',(-64.1500031332282,-31.3459097002006,
12.));
#79646=CARTESIAN_POINT('Ctrl Pts',(-64.166253899542,-31.3619910181228,0.));
#79647=CARTESIAN_POINT('Ctrl Pts',(-64.166253899542,-31.3619910181228,12.));
#79648=CARTESIAN_POINT('Ctrl Pts',(-64.1825205366224,-31.3781202823754,
0.));
#79649=CARTESIAN_POINT('Ctrl Pts',(-64.1825205366224,-31.3781202823754,
12.));
#79650=CARTESIAN_POINT('Ctrl Pts',(-64.1988029019707,-31.3942974463445,
0.));
#79651=CARTESIAN_POINT('Ctrl Pts',(-64.1988029019707,-31.3942974463445,
12.));
#79652=CARTESIAN_POINT('Ctrl Pts',(-64.2151008537697,-31.410522463528,0.));
#79653=CARTESIAN_POINT('Ctrl Pts',(-64.2151008537697,-31.410522463528,12.));
#79654=CARTESIAN_POINT('Ctrl Pts',(-64.231414250881,-31.4267952875423,0.));
#79655=CARTESIAN_POINT('Ctrl Pts',(-64.231414250881,-31.4267952875423,12.));
#79656=CARTESIAN_POINT('Ctrl Pts',(-64.2477429528393,-31.4431158721222,
0.));
#79657=CARTESIAN_POINT('Ctrl Pts',(-64.2477429528393,-31.4431158721222,
12.));
#79658=CARTESIAN_POINT('Ctrl Pts',(-64.2640868198473,-31.4594841711194,
0.));
#79659=CARTESIAN_POINT('Ctrl Pts',(-64.2640868198473,-31.4594841711194,
12.));
#79660=CARTESIAN_POINT('Ctrl Pts',(-64.2804457127671,-31.4759001384941,
0.));
#79661=CARTESIAN_POINT('Ctrl Pts',(-64.2804457127671,-31.4759001384941,
12.));
#79662=CARTESIAN_POINT('Ctrl Pts',(-64.2968194931158,-31.4923637283132,
0.));
#79663=CARTESIAN_POINT('Ctrl Pts',(-64.2968194931158,-31.4923637283132,
12.));
#79664=CARTESIAN_POINT('Ctrl Pts',(-64.3132080230637,-31.5088748947582,
0.));
#79665=CARTESIAN_POINT('Ctrl Pts',(-64.3132080230637,-31.5088748947582,
12.));
#79666=CARTESIAN_POINT('Ctrl Pts',(-64.3296111654283,-31.5254335921245,
0.));
#79667=CARTESIAN_POINT('Ctrl Pts',(-64.3296111654283,-31.5254335921245,
12.));
#79668=CARTESIAN_POINT('Ctrl Pts',(-64.3460287836687,-31.5420397748191,
0.));
#79669=CARTESIAN_POINT('Ctrl Pts',(-64.3460287836687,-31.5420397748191,
12.));
#79670=CARTESIAN_POINT('Ctrl Pts',(-64.3624607418768,-31.5586933973515,
0.));
#79671=CARTESIAN_POINT('Ctrl Pts',(-64.3624607418768,-31.5586933973515,
12.));
#79672=CARTESIAN_POINT('Ctrl Pts',(-64.3789069047733,-31.5753944143336,
0.));
#79673=CARTESIAN_POINT('Ctrl Pts',(-64.3789069047733,-31.5753944143336,
12.));
#79674=CARTESIAN_POINT('Ctrl Pts',(-64.3953671377046,-31.5921427804865,
0.));
#79675=CARTESIAN_POINT('Ctrl Pts',(-64.3953671377046,-31.5921427804865,
12.));
#79676=CARTESIAN_POINT('Ctrl Pts',(-64.4118413066378,-31.6089384506395,
0.));
#79677=CARTESIAN_POINT('Ctrl Pts',(-64.4118413066378,-31.6089384506395,
12.));
#79678=CARTESIAN_POINT('Ctrl Pts',(-64.4283292781565,-31.6257813797287,
0.));
#79679=CARTESIAN_POINT('Ctrl Pts',(-64.4283292781565,-31.6257813797287,
12.));
#79680=CARTESIAN_POINT('Ctrl Pts',(-64.4448309194525,-31.6426715227878,
0.));
#79681=CARTESIAN_POINT('Ctrl Pts',(-64.4448309194525,-31.6426715227878,
12.));
#79682=CARTESIAN_POINT('Ctrl Pts',(-64.4613460983214,-31.6596088349482,
0.));
#79683=CARTESIAN_POINT('Ctrl Pts',(-64.4613460983214,-31.6596088349482,
12.));
#79684=CARTESIAN_POINT('Ctrl Pts',(-64.4778746831614,-31.6765932714464,
0.));
#79685=CARTESIAN_POINT('Ctrl Pts',(-64.4778746831614,-31.6765932714464,
12.));
#79686=CARTESIAN_POINT('Ctrl Pts',(-64.4944165429675,-31.6936247876229,
0.));
#79687=CARTESIAN_POINT('Ctrl Pts',(-64.4944165429675,-31.6936247876229,
12.));
#79688=CARTESIAN_POINT('Ctrl Pts',(-64.510971547327,-31.7107033389201,0.));
#79689=CARTESIAN_POINT('Ctrl Pts',(-64.510971547327,-31.7107033389201,12.));
#79690=CARTESIAN_POINT('Ctrl Pts',(-64.5275395664124,-31.7278288808731,
0.));
#79691=CARTESIAN_POINT('Ctrl Pts',(-64.5275395664124,-31.7278288808731,
12.));
#79692=CARTESIAN_POINT('Ctrl Pts',(-64.544120470977,-31.7450013691112,0.));
#79693=CARTESIAN_POINT('Ctrl Pts',(-64.544120470977,-31.7450013691112,12.));
#79694=CARTESIAN_POINT('Ctrl Pts',(-64.5607141323521,-31.7622207593634,
0.));
#79695=CARTESIAN_POINT('Ctrl Pts',(-64.5607141323521,-31.7622207593634,
12.));
#79696=CARTESIAN_POINT('Ctrl Pts',(-64.5773204224429,-31.7794870074583,
0.));
#79697=CARTESIAN_POINT('Ctrl Pts',(-64.5773204224429,-31.7794870074583,
12.));
#79698=CARTESIAN_POINT('Ctrl Pts',(-64.5939392137235,-31.7968000693218,
0.));
#79699=CARTESIAN_POINT('Ctrl Pts',(-64.5939392137235,-31.7968000693218,
12.));
#79700=CARTESIAN_POINT('Ctrl Pts',(-64.6105703792312,-31.8141599009684,
0.));
#79701=CARTESIAN_POINT('Ctrl Pts',(-64.6105703792312,-31.8141599009684,
12.));
#79702=CARTESIAN_POINT('Ctrl Pts',(-64.6272137925627,-31.8315664585026,
0.));
#79703=CARTESIAN_POINT('Ctrl Pts',(-64.6272137925627,-31.8315664585026,
12.));
#79704=CARTESIAN_POINT('Ctrl Pts',(-64.6438693278714,-31.8490196981248,
0.));
#79705=CARTESIAN_POINT('Ctrl Pts',(-64.6438693278714,-31.8490196981248,
12.));
#79706=CARTESIAN_POINT('Ctrl Pts',(-64.6605368598629,-31.866519576131,0.));
#79707=CARTESIAN_POINT('Ctrl Pts',(-64.6605368598629,-31.866519576131,12.));
#79708=CARTESIAN_POINT('Ctrl Pts',(-64.6772162637907,-31.8840660489107,
0.));
#79709=CARTESIAN_POINT('Ctrl Pts',(-64.6772162637907,-31.8840660489107,
12.));
#79710=CARTESIAN_POINT('Ctrl Pts',(-64.6939074154498,-31.9016590729374,
0.));
#79711=CARTESIAN_POINT('Ctrl Pts',(-64.6939074154498,-31.9016590729374,
12.));
#79712=CARTESIAN_POINT('Ctrl Pts',(-64.7106101911732,-31.9192986047706,
0.));
#79713=CARTESIAN_POINT('Ctrl Pts',(-64.7106101911732,-31.9192986047706,
12.));
#79714=CARTESIAN_POINT('Ctrl Pts',(-64.7273244678297,-31.9369846010615,
0.));
#79715=CARTESIAN_POINT('Ctrl Pts',(-64.7273244678297,-31.9369846010615,
12.));
#79716=CARTESIAN_POINT('Ctrl Pts',(-64.7440501228202,-31.9547170185534,
0.));
#79717=CARTESIAN_POINT('Ctrl Pts',(-64.7440501228202,-31.9547170185534,
12.));
#79718=CARTESIAN_POINT('Ctrl Pts',(-64.7607870340735,-31.9724958140789,
0.));
#79719=CARTESIAN_POINT('Ctrl Pts',(-64.7607870340735,-31.9724958140789,
12.));
#79720=CARTESIAN_POINT('Ctrl Pts',(-64.77753508004,-31.990320944552,0.));
#79721=CARTESIAN_POINT('Ctrl Pts',(-64.77753508004,-31.990320944552,12.));
#79722=CARTESIAN_POINT('Ctrl Pts',(-64.7942941396881,-32.0081923669677,
0.));
#79723=CARTESIAN_POINT('Ctrl Pts',(-64.7942941396881,-32.0081923669677,
12.));
#79724=CARTESIAN_POINT('Ctrl Pts',(-64.8110640925021,-32.0261100384092,
0.));
#79725=CARTESIAN_POINT('Ctrl Pts',(-64.8110640925021,-32.0261100384092,
12.));
#79726=CARTESIAN_POINT('Ctrl Pts',(-64.8278448184786,-32.0440739160477,
0.));
#79727=CARTESIAN_POINT('Ctrl Pts',(-64.8278448184786,-32.0440739160477,
12.));
#79728=CARTESIAN_POINT('Ctrl Pts',(-64.8446361981234,-32.0620839571408,
0.));
#79729=CARTESIAN_POINT('Ctrl Pts',(-64.8446361981234,-32.0620839571408,
12.));
#79730=CARTESIAN_POINT('Ctrl Pts',(-64.861438112445,-32.0801401190241,0.));
#79731=CARTESIAN_POINT('Ctrl Pts',(-64.861438112445,-32.0801401190241,12.));
#79732=CARTESIAN_POINT('Ctrl Pts',(-64.878250442952,-32.0982423591108,0.));
#79733=CARTESIAN_POINT('Ctrl Pts',(-64.878250442952,-32.0982423591108,12.));
#79734=CARTESIAN_POINT('Ctrl Pts',(-64.8950730716493,-32.1163906348979,
0.));
#79735=CARTESIAN_POINT('Ctrl Pts',(-64.8950730716493,-32.1163906348979,
12.));
#79736=CARTESIAN_POINT('Ctrl Pts',(-64.9119058810362,-32.1345849039671,
0.));
#79737=CARTESIAN_POINT('Ctrl Pts',(-64.9119058810362,-32.1345849039671,
12.));
#79738=CARTESIAN_POINT('Ctrl Pts',(-64.9287487541018,-32.1528251239832,
0.));
#79739=CARTESIAN_POINT('Ctrl Pts',(-64.9287487541018,-32.1528251239832,
12.));
#79740=CARTESIAN_POINT('Ctrl Pts',(-64.9456015743203,-32.171111252686,0.));
#79741=CARTESIAN_POINT('Ctrl Pts',(-64.9456015743203,-32.171111252686,12.));
#79742=CARTESIAN_POINT('Ctrl Pts',(-64.9624642256477,-32.1894432478889,
0.));
#79743=CARTESIAN_POINT('Ctrl Pts',(-64.9624642256477,-32.1894432478889,
12.));
#79744=CARTESIAN_POINT('Ctrl Pts',(-64.9793365925194,-32.2078210674857,
0.));
#79745=CARTESIAN_POINT('Ctrl Pts',(-64.9793365925194,-32.2078210674857,
12.));
#79746=CARTESIAN_POINT('Ctrl Pts',(-64.996218559847,-32.2262446694516,0.));
#79747=CARTESIAN_POINT('Ctrl Pts',(-64.996218559847,-32.2262446694516,12.));
#79748=CARTESIAN_POINT('Ctrl Pts',(-65.0131100130155,-32.244714011842,0.));
#79749=CARTESIAN_POINT('Ctrl Pts',(-65.0131100130155,-32.244714011842,12.));
#79750=CARTESIAN_POINT('Ctrl Pts',(-65.0300108378786,-32.2632290527855,
0.));
#79751=CARTESIAN_POINT('Ctrl Pts',(-65.0300108378786,-32.2632290527855,
12.));
#79752=CARTESIAN_POINT('Ctrl Pts',(-65.0469209207548,-32.2817897504799,
0.));
#79753=CARTESIAN_POINT('Ctrl Pts',(-65.0469209207548,-32.2817897504799,
12.));
#79754=CARTESIAN_POINT('Ctrl Pts',(-65.0638401484245,-32.3003960632,0.));
#79755=CARTESIAN_POINT('Ctrl Pts',(-65.0638401484245,-32.3003960632,12.));
#79756=CARTESIAN_POINT('Ctrl Pts',(-65.0807684081278,-32.3190479492985,
0.));
#79757=CARTESIAN_POINT('Ctrl Pts',(-65.0807684081278,-32.3190479492985,
12.));
#79758=CARTESIAN_POINT('Ctrl Pts',(-65.097705587561,-32.3377453672052,0.));
#79759=CARTESIAN_POINT('Ctrl Pts',(-65.097705587561,-32.3377453672052,12.));
#79760=CARTESIAN_POINT('Ctrl Pts',(-65.1146515748723,-32.3564882754212,
0.));
#79761=CARTESIAN_POINT('Ctrl Pts',(-65.1146515748723,-32.3564882754212,
12.));
#79762=CARTESIAN_POINT('Ctrl Pts',(-65.1316062586586,-32.3752766325135,
0.));
#79763=CARTESIAN_POINT('Ctrl Pts',(-65.1316062586586,-32.3752766325135,
12.));
#79764=CARTESIAN_POINT('Ctrl Pts',(-65.1485695279628,-32.3941103971218,
0.));
#79765=CARTESIAN_POINT('Ctrl Pts',(-65.1485695279628,-32.3941103971218,
12.));
#79766=CARTESIAN_POINT('Ctrl Pts',(-65.165541272272,-32.4129895279612,0.));
#79767=CARTESIAN_POINT('Ctrl Pts',(-65.165541272272,-32.4129895279612,12.));
#79768=CARTESIAN_POINT('Ctrl Pts',(-65.182521381514,-32.4319139838212,0.));
#79769=CARTESIAN_POINT('Ctrl Pts',(-65.182521381514,-32.4319139838212,12.));
#79770=CARTESIAN_POINT('Ctrl Pts',(-65.1995097460546,-32.4508837235613,
0.));
#79771=CARTESIAN_POINT('Ctrl Pts',(-65.1995097460546,-32.4508837235613,
12.));
#79772=CARTESIAN_POINT('Ctrl Pts',(-65.2165062566936,-32.4698987061037,
0.));
#79773=CARTESIAN_POINT('Ctrl Pts',(-65.2165062566936,-32.4698987061037,
12.));
#79774=CARTESIAN_POINT('Ctrl Pts',(-65.2335108046625,-32.4889588904397,
0.));
#79775=CARTESIAN_POINT('Ctrl Pts',(-65.2335108046625,-32.4889588904397,
12.));
#79776=CARTESIAN_POINT('Ctrl Pts',(-65.2505232816215,-32.508064235633,0.));
#79777=CARTESIAN_POINT('Ctrl Pts',(-65.2505232816215,-32.508064235633,12.));
#79778=CARTESIAN_POINT('Ctrl Pts',(-65.2675435796558,-32.5272147008191,
0.));
#79779=CARTESIAN_POINT('Ctrl Pts',(-65.2675435796558,-32.5272147008191,
12.));
#79780=CARTESIAN_POINT('Ctrl Pts',(-65.2845715912717,-32.5464102452013,
0.));
#79781=CARTESIAN_POINT('Ctrl Pts',(-65.2845715912717,-32.5464102452013,
12.));
#79782=CARTESIAN_POINT('Ctrl Pts',(-65.3016072093907,-32.565650828042,0.));
#79783=CARTESIAN_POINT('Ctrl Pts',(-65.3016072093907,-32.565650828042,12.));
#79784=CARTESIAN_POINT('Ctrl Pts',(-65.3186503273498,-32.5849364086679,
0.));
#79785=CARTESIAN_POINT('Ctrl Pts',(-65.3186503273498,-32.5849364086679,
12.));
#79786=CARTESIAN_POINT('Ctrl Pts',(-65.3357008389004,-32.6042669464752,
0.));
#79787=CARTESIAN_POINT('Ctrl Pts',(-65.3357008389004,-32.6042669464752,
12.));
#79788=CARTESIAN_POINT('Ctrl Pts',(-65.3527586382082,-32.6236424009302,
0.));
#79789=CARTESIAN_POINT('Ctrl Pts',(-65.3527586382082,-32.6236424009302,
12.));
#79790=CARTESIAN_POINT('Ctrl Pts',(-65.3698236198511,-32.6430627315673,
0.));
#79791=CARTESIAN_POINT('Ctrl Pts',(-65.3698236198511,-32.6430627315673,
12.));
#79792=CARTESIAN_POINT('Ctrl Pts',(-65.3868956788178,-32.6625278979807,
0.));
#79793=CARTESIAN_POINT('Ctrl Pts',(-65.3868956788178,-32.6625278979807,
12.));
#79794=CARTESIAN_POINT('Ctrl Pts',(-65.4039747105033,-32.6820378598262,
0.));
#79795=CARTESIAN_POINT('Ctrl Pts',(-65.4039747105033,-32.6820378598262,
12.));
#79796=CARTESIAN_POINT('Ctrl Pts',(-65.4210606107029,-32.7015925768261,
0.));
#79797=CARTESIAN_POINT('Ctrl Pts',(-65.4210606107029,-32.7015925768261,
12.));
#79798=CARTESIAN_POINT('Ctrl Pts',(-65.4381532756062,-32.7211920087682,
0.));
#79799=CARTESIAN_POINT('Ctrl Pts',(-65.4381532756062,-32.7211920087682,
12.));
#79800=CARTESIAN_POINT('Ctrl Pts',(-65.4552526017907,-32.7408361155038,
0.));
#79801=CARTESIAN_POINT('Ctrl Pts',(-65.4552526017907,-32.7408361155038,
12.));
#79802=CARTESIAN_POINT('Ctrl Pts',(-65.4723584862129,-32.7605248569382,
0.));
#79803=CARTESIAN_POINT('Ctrl Pts',(-65.4723584862129,-32.7605248569382,
12.));
#79804=CARTESIAN_POINT('Ctrl Pts',(-65.4894708262071,-32.7802581930293,
0.));
#79805=CARTESIAN_POINT('Ctrl Pts',(-65.4894708262071,-32.7802581930293,
12.));
#79806=CARTESIAN_POINT('Ctrl Pts',(-65.5065895194938,-32.8000360837981,
0.));
#79807=CARTESIAN_POINT('Ctrl Pts',(-65.5065895194938,-32.8000360837981,
12.));
#79808=CARTESIAN_POINT('Ctrl Pts',(-65.5237144641864,-32.8198584893319,
0.));
#79809=CARTESIAN_POINT('Ctrl Pts',(-65.5237144641864,-32.8198584893319,
12.));
#79810=CARTESIAN_POINT('Ctrl Pts',(-65.5408455587963,-32.8397253697864,
0.));
#79811=CARTESIAN_POINT('Ctrl Pts',(-65.5408455587963,-32.8397253697864,
12.));
#79812=CARTESIAN_POINT('Ctrl Pts',(-65.5579827022412,-32.8596366853826,
0.));
#79813=CARTESIAN_POINT('Ctrl Pts',(-65.5579827022412,-32.8596366853826,
12.));
#79814=CARTESIAN_POINT('Ctrl Pts',(-65.575125793846,-32.8795923964022,0.));
#79815=CARTESIAN_POINT('Ctrl Pts',(-65.575125793846,-32.8795923964022,12.));
#79816=CARTESIAN_POINT('Ctrl Pts',(-65.5922747333181,-32.899592463189,0.));
#79817=CARTESIAN_POINT('Ctrl Pts',(-65.5922747333181,-32.899592463189,12.));
#79818=CARTESIAN_POINT('Ctrl Pts',(-65.6094294207267,-32.9196368461457,
0.));
#79819=CARTESIAN_POINT('Ctrl Pts',(-65.6094294207267,-32.9196368461457,
12.));
#79820=CARTESIAN_POINT('Ctrl Pts',(-65.6265897564782,-32.9397255057273,
0.));
#79821=CARTESIAN_POINT('Ctrl Pts',(-65.6265897564782,-32.9397255057273,
12.));
#79822=CARTESIAN_POINT('Ctrl Pts',(-65.6437556412956,-32.9598584024318,
0.));
#79823=CARTESIAN_POINT('Ctrl Pts',(-65.6437556412956,-32.9598584024318,
12.));
#79824=CARTESIAN_POINT('Ctrl Pts',(-65.6609269761902,-32.9800354967847,
0.));
#79825=CARTESIAN_POINT('Ctrl Pts',(-65.6609269761902,-32.9800354967847,
12.));
#79826=CARTESIAN_POINT('Ctrl Pts',(-65.6781036625041,-33.0002567493581,
0.));
#79827=CARTESIAN_POINT('Ctrl Pts',(-65.6781036625041,-33.0002567493581,
12.));
#79828=CARTESIAN_POINT('Ctrl Pts',(-65.6952856019542,-33.0205221207877,
0.));
#79829=CARTESIAN_POINT('Ctrl Pts',(-65.6952856019542,-33.0205221207877,
12.));
#79830=CARTESIAN_POINT('Ctrl Pts',(-65.7124726966805,-33.0408315717874,
0.));
#79831=CARTESIAN_POINT('Ctrl Pts',(-65.7124726966805,-33.0408315717874,
12.));
#79832=CARTESIAN_POINT('Ctrl Pts',(-65.729664849282,-33.061185063158,0.));
#79833=CARTESIAN_POINT('Ctrl Pts',(-65.729664849282,-33.061185063158,12.));
#79834=CARTESIAN_POINT('Ctrl Pts',(-65.7468619628808,-33.0815825557976,
0.));
#79835=CARTESIAN_POINT('Ctrl Pts',(-65.7468619628808,-33.0815825557976,
12.));
#79836=CARTESIAN_POINT('Ctrl Pts',(-65.7640639410653,-33.102024010688,0.));
#79837=CARTESIAN_POINT('Ctrl Pts',(-65.7640639410653,-33.102024010688,12.));
#79838=CARTESIAN_POINT('Ctrl Pts',(-65.7812706877691,-33.1225093888668,
0.));
#79839=CARTESIAN_POINT('Ctrl Pts',(-65.7812706877691,-33.1225093888668,
12.));
#79840=CARTESIAN_POINT('Ctrl Pts',(-65.7984821071621,-33.1430386513975,
0.));
#79841=CARTESIAN_POINT('Ctrl Pts',(-65.7984821071621,-33.1430386513975,
12.));
#79842=CARTESIAN_POINT('Ctrl Pts',(-65.8156981035504,-33.16361175934,0.));
#79843=CARTESIAN_POINT('Ctrl Pts',(-65.8156981035504,-33.16361175934,12.));
#79844=CARTESIAN_POINT('Ctrl Pts',(-65.8329185812379,-33.1842286737053,
0.));
#79845=CARTESIAN_POINT('Ctrl Pts',(-65.8329185812379,-33.1842286737053,
12.));
#79846=CARTESIAN_POINT('Ctrl Pts',(-65.8501434445174,-33.2048893554496,
0.));
#79847=CARTESIAN_POINT('Ctrl Pts',(-65.8501434445174,-33.2048893554496,
12.));
#79848=CARTESIAN_POINT('Ctrl Pts',(-65.8673725979591,-33.2255937655656,
0.));
#79849=CARTESIAN_POINT('Ctrl Pts',(-65.8673725979591,-33.2255937655656,
12.));
#79850=CARTESIAN_POINT('Ctrl Pts',(-65.8846059466382,-33.2463418651498,
0.));
#79851=CARTESIAN_POINT('Ctrl Pts',(-65.8846059466382,-33.2463418651498,
12.));
#79852=CARTESIAN_POINT('Ctrl Pts',(-65.901843396389,-33.2671336154754,0.));
#79853=CARTESIAN_POINT('Ctrl Pts',(-65.901843396389,-33.2671336154754,12.));
#79854=CARTESIAN_POINT('Ctrl Pts',(-65.9190848540422,-33.2879689780566,
0.));
#79855=CARTESIAN_POINT('Ctrl Pts',(-65.9190848540422,-33.2879689780566,
12.));
#79856=CARTESIAN_POINT('Ctrl Pts',(-65.9363302276822,-33.3088479147151,
0.));
#79857=CARTESIAN_POINT('Ctrl Pts',(-65.9363302276822,-33.3088479147151,
12.));
#79858=CARTESIAN_POINT('Ctrl Pts',(-65.9535794260802,-33.3297703874249,
0.));
#79859=CARTESIAN_POINT('Ctrl Pts',(-65.9535794260802,-33.3297703874249,
12.));
#79860=CARTESIAN_POINT('Ctrl Pts',(-65.9708323581385,-33.3507363581579,
0.));
#79861=CARTESIAN_POINT('Ctrl Pts',(-65.9708323581385,-33.3507363581579,
12.));
#79862=CARTESIAN_POINT('Ctrl Pts',(-65.9880889322822,-33.3717457887095,
0.));
#79863=CARTESIAN_POINT('Ctrl Pts',(-65.9880889322822,-33.3717457887095,
12.));
#79864=CARTESIAN_POINT('Ctrl Pts',(-66.0053490559826,-33.3927986405612,
0.));
#79865=CARTESIAN_POINT('Ctrl Pts',(-66.0053490559826,-33.3927986405612,
12.));
#79866=CARTESIAN_POINT('Ctrl Pts',(-66.0226126349482,-33.4138948746408,
0.));
#79867=CARTESIAN_POINT('Ctrl Pts',(-66.0226126349482,-33.4138948746408,
12.));
#79868=CARTESIAN_POINT('Ctrl Pts',(-66.0398795737827,-33.4350344515128,
0.));
#79869=CARTESIAN_POINT('Ctrl Pts',(-66.0398795737827,-33.4350344515128,
12.));
#79870=CARTESIAN_POINT('Ctrl Pts',(-66.0571497774484,-33.4562173318052,
0.));
#79871=CARTESIAN_POINT('Ctrl Pts',(-66.0571497774484,-33.4562173318052,
12.));
#79872=CARTESIAN_POINT('Ctrl Pts',(-66.0744231525445,-33.4774434765762,
0.));
#79873=CARTESIAN_POINT('Ctrl Pts',(-66.0744231525445,-33.4774434765762,
12.));
#79874=CARTESIAN_POINT('Ctrl Pts',(-66.0916996085237,-33.4987128476618,
0.));
#79875=CARTESIAN_POINT('Ctrl Pts',(-66.0916996085237,-33.4987128476618,
12.));
#79876=CARTESIAN_POINT('Ctrl Pts',(-66.1089790592673,-33.5200254081212,
0.));
#79877=CARTESIAN_POINT('Ctrl Pts',(-66.1089790592673,-33.5200254081212,
12.));
#79878=CARTESIAN_POINT('Ctrl Pts',(-66.1262614234579,-33.5413811223398,
0.));
#79879=CARTESIAN_POINT('Ctrl Pts',(-66.1262614234579,-33.5413811223398,
12.));
#79880=CARTESIAN_POINT('Ctrl Pts',(-66.1435466210966,-33.5627799550422,
0.));
#79881=CARTESIAN_POINT('Ctrl Pts',(-66.1435466210966,-33.5627799550422,
12.));
#79882=CARTESIAN_POINT('Ctrl Pts',(-66.1608345707552,-33.5842218705103,
0.));
#79883=CARTESIAN_POINT('Ctrl Pts',(-66.1608345707552,-33.5842218705103,
12.));
#79884=CARTESIAN_POINT('Ctrl Pts',(-66.1781251863998,-33.6057068316758,
0.));
#79885=CARTESIAN_POINT('Ctrl Pts',(-66.1781251863998,-33.6057068316758,
12.));
#79886=CARTESIAN_POINT('Ctrl Pts',(-66.1954183747167,-33.6272347993519,
0.));
#79887=CARTESIAN_POINT('Ctrl Pts',(-66.1954183747167,-33.6272347993519,
12.));
#79888=CARTESIAN_POINT('Ctrl Pts',(-66.2127140313777,-33.648805731163,0.));
#79889=CARTESIAN_POINT('Ctrl Pts',(-66.2127140313777,-33.648805731163,12.));
#79890=CARTESIAN_POINT('Ctrl Pts',(-66.2300120464323,-33.6704195830526,
0.));
#79891=CARTESIAN_POINT('Ctrl Pts',(-66.2300120464323,-33.6704195830526,
12.));
#79892=CARTESIAN_POINT('Ctrl Pts',(-66.2473123109626,-33.6920763111575,
0.));
#79893=CARTESIAN_POINT('Ctrl Pts',(-66.2473123109626,-33.6920763111575,
12.));
#79894=CARTESIAN_POINT('Ctrl Pts',(-66.2646147235444,-33.713775873597,0.));
#79895=CARTESIAN_POINT('Ctrl Pts',(-66.2646147235444,-33.713775873597,12.));
#79896=CARTESIAN_POINT('Ctrl Pts',(-66.2819191962273,-33.7355182321862,
0.));
#79897=CARTESIAN_POINT('Ctrl Pts',(-66.2819191962273,-33.7355182321862,
12.));
#79898=CARTESIAN_POINT('Ctrl Pts',(-66.2992256621001,-33.7573033544374,
0.));
#79899=CARTESIAN_POINT('Ctrl Pts',(-66.2992256621001,-33.7573033544374,
12.));
#79900=CARTESIAN_POINT('Ctrl Pts',(-66.3165340771053,-33.7791312144798,
0.));
#79901=CARTESIAN_POINT('Ctrl Pts',(-66.3165340771053,-33.7791312144798,
12.));
#79902=CARTESIAN_POINT('Ctrl Pts',(-66.3338444143559,-33.8010017925666,
0.));
#79903=CARTESIAN_POINT('Ctrl Pts',(-66.3338444143559,-33.8010017925666,
12.));
#79904=CARTESIAN_POINT('Ctrl Pts',(-66.3476942111456,-33.8185324184602,
0.));
#79905=CARTESIAN_POINT('Ctrl Pts',(-66.3476942111456,-33.8185324184602,
12.));
#79906=CARTESIAN_POINT('Ctrl Pts',(-66.3580824155565,-33.831699601175,0.));
#79907=CARTESIAN_POINT('Ctrl Pts',(-66.3580824155565,-33.831699601175,12.));
#79908=CARTESIAN_POINT('Ctrl Pts',(-66.3650082659593,-33.8404862618803,
0.));
#79909=CARTESIAN_POINT('Ctrl Pts',(-66.3650082659593,-33.8404862618803,
12.));
#79910=CARTESIAN_POINT('Ctrl Pts',(-66.3684712863594,-33.8448817269567,
0.));
#79911=CARTESIAN_POINT('Ctrl Pts',(-66.3684712863594,-33.8448817269567,
12.));
#79912=CARTESIAN_POINT('',(-63.0759831361898,-30.3549065457811,0.));
#79913=CARTESIAN_POINT('Ctrl Pts',(-63.0759831361898,-30.3549065457811,
0.));
#79914=CARTESIAN_POINT('Ctrl Pts',(-63.078933570069,-30.3574319069329,0.));
#79915=CARTESIAN_POINT('Ctrl Pts',(-63.0848371718048,-30.3624877680651,
0.));
#79916=CARTESIAN_POINT('Ctrl Pts',(-63.0937007763471,-30.3700869762507,
0.));
#79917=CARTESIAN_POINT('Ctrl Pts',(-63.105535320226,-30.3802500880403,0.));
#79918=CARTESIAN_POINT('Ctrl Pts',(-63.1203558300657,-30.3930053710484,
0.));
#79919=CARTESIAN_POINT('Ctrl Pts',(-63.135203629844,-30.4058120432228,0.));
#79920=CARTESIAN_POINT('Ctrl Pts',(-63.1500786361459,-30.418670087563,0.));
#79921=CARTESIAN_POINT('Ctrl Pts',(-63.164980701691,-30.4315794659731,0.));
#79922=CARTESIAN_POINT('Ctrl Pts',(-63.179909617189,-30.444540119238,0.));
#79923=CARTESIAN_POINT('Ctrl Pts',(-63.1948651386942,-30.4575519763337,
0.));
#79924=CARTESIAN_POINT('Ctrl Pts',(-63.2098470086636,-30.470614961416,0.));
#79925=CARTESIAN_POINT('Ctrl Pts',(-63.2248549788221,-30.4837290014989,
0.));
#79926=CARTESIAN_POINT('Ctrl Pts',(-63.2398888342545,-30.4968940344998,
0.));
#79927=CARTESIAN_POINT('Ctrl Pts',(-63.2549483856215,-30.5101100066659,
0.));
#79928=CARTESIAN_POINT('Ctrl Pts',(-63.2700334577639,-30.5233768687865,
0.));
#79929=CARTESIAN_POINT('Ctrl Pts',(-63.2851438802473,-30.5366945730508,
0.));
#79930=CARTESIAN_POINT('Ctrl Pts',(-63.3002794756086,-30.5500630691359,
0.));
#79931=CARTESIAN_POINT('Ctrl Pts',(-63.3154400534397,-30.563482302238,0.));
#79932=CARTESIAN_POINT('Ctrl Pts',(-63.3306254165126,-30.5769522151164,
0.));
#79933=CARTESIAN_POINT('Ctrl Pts',(-63.3458353646154,-30.5904727493711,
0.));
#79934=CARTESIAN_POINT('Ctrl Pts',(-63.3610696989577,-30.6040438469078,
0.));
#79935=CARTESIAN_POINT('Ctrl Pts',(-63.3763282271796,-30.6176654515967,
0.));
#79936=CARTESIAN_POINT('Ctrl Pts',(-63.3916107631376,-30.6313375092062,
0.));
#79937=CARTESIAN_POINT('Ctrl Pts',(-63.4069171245066,-30.6450599666121,
0.));
#79938=CARTESIAN_POINT('Ctrl Pts',(-63.4222471311239,-30.6588327712483,
0.));
#79939=CARTESIAN_POINT('Ctrl Pts',(-63.4376006029604,-30.6726558704315,
0.));
#79940=CARTESIAN_POINT('Ctrl Pts',(-63.4529773584249,-30.6865292107929,
0.));
#79941=CARTESIAN_POINT('Ctrl Pts',(-63.4683772152529,-30.7004527385821,
0.));
#79942=CARTESIAN_POINT('Ctrl Pts',(-63.4837999912771,-30.7144263999265,
0.));
#79943=CARTESIAN_POINT('Ctrl Pts',(-63.4992455051795,-30.7284501410822,
0.));
#79944=CARTESIAN_POINT('Ctrl Pts',(-63.5147135773894,-30.7425239087281,
0.));
#79945=CARTESIAN_POINT('Ctrl Pts',(-63.5302040304142,-30.7566476500757,
0.));
#79946=CARTESIAN_POINT('Ctrl Pts',(-63.5457166883537,-30.7708213127159,
0.));
#79947=CARTESIAN_POINT('Ctrl Pts',(-63.5612513766,-30.7850448445205,0.));
#79948=CARTESIAN_POINT('Ctrl Pts',(-63.5768079214881,-30.7993181935271,
0.));
#79949=CARTESIAN_POINT('Ctrl Pts',(-63.5923861498987,-30.813641307801,0.));
#79950=CARTESIAN_POINT('Ctrl Pts',(-63.6079858892771,-30.8280141354459,
0.));
#79951=CARTESIAN_POINT('Ctrl Pts',(-63.6236069678055,-30.8424366246671,
0.));
#79952=CARTESIAN_POINT('Ctrl Pts',(-63.6392492145233,-30.8569087238131,
0.));
#79953=CARTESIAN_POINT('Ctrl Pts',(-63.6549124594666,-30.8714303814194,
0.));
#79954=CARTESIAN_POINT('Ctrl Pts',(-63.6705965337971,-30.8860015462475,
0.));
#79955=CARTESIAN_POINT('Ctrl Pts',(-63.6863012697328,-30.900622167269,0.));
#79956=CARTESIAN_POINT('Ctrl Pts',(-63.7020265004792,-30.9152921936465,
0.));
#79957=CARTESIAN_POINT('Ctrl Pts',(-63.7177720601609,-30.9300115747115,
0.));
#79958=CARTESIAN_POINT('Ctrl Pts',(-63.7335377837441,-30.9447802599355,
0.));
#79959=CARTESIAN_POINT('Ctrl Pts',(-63.749323506987,-30.9595981989103,0.));
#79960=CARTESIAN_POINT('Ctrl Pts',(-63.7651290664733,-30.9744653413689,
0.));
#79961=CARTESIAN_POINT('Ctrl Pts',(-63.7809542996264,-30.989381637191,0.));
#79962=CARTESIAN_POINT('Ctrl Pts',(-63.796799044728,-31.0043470364108,0.));
#79963=CARTESIAN_POINT('Ctrl Pts',(-63.8126631409364,-31.0193614892171,
0.));
#79964=CARTESIAN_POINT('Ctrl Pts',(-63.8285464282846,-31.0344249459538,
0.));
#79965=CARTESIAN_POINT('Ctrl Pts',(-63.8444487476611,-31.0495373571215,
0.));
#79966=CARTESIAN_POINT('Ctrl Pts',(-63.8603699407922,-31.0646986733723,
0.));
#79967=CARTESIAN_POINT('Ctrl Pts',(-63.8763098502237,-31.0799088455041,
0.));
#79968=CARTESIAN_POINT('Ctrl Pts',(-63.8922683192964,-31.0951678244455,
0.));
#79969=CARTESIAN_POINT('Ctrl Pts',(-63.9082451921448,-31.1104755612607,
0.));
#79970=CARTESIAN_POINT('Ctrl Pts',(-63.9242403136955,-31.1258320071545,
0.));
#79971=CARTESIAN_POINT('Ctrl Pts',(-63.940253529665,-31.1412371134727,0.));
#79972=CARTESIAN_POINT('Ctrl Pts',(-63.9562846865567,-31.1566908316992,
0.));
#79973=CARTESIAN_POINT('Ctrl Pts',(-63.9723336316551,-31.1721931134487,
0.));
#79974=CARTESIAN_POINT('Ctrl Pts',(-63.9884002130211,-31.1877439104717,
0.));
#79975=CARTESIAN_POINT('Ctrl Pts',(-64.0044842794831,-31.2033431746558,
0.));
#79976=CARTESIAN_POINT('Ctrl Pts',(-64.02058568063,-31.2189908580245,0.));
#79977=CARTESIAN_POINT('Ctrl Pts',(-64.0367042667984,-31.2346869127297,
0.));
#79978=CARTESIAN_POINT('Ctrl Pts',(-64.0528398890657,-31.2504312910451,
0.));
#79979=CARTESIAN_POINT('Ctrl Pts',(-64.0689923992461,-31.2662239453728,
0.));
#79980=CARTESIAN_POINT('Ctrl Pts',(-64.0851616498852,-31.2820648282447,
0.));
#79981=CARTESIAN_POINT('Ctrl Pts',(-64.1013474942556,-31.2979538923214,
0.));
#79982=CARTESIAN_POINT('Ctrl Pts',(-64.117549786349,-31.3138910903859,0.));
#79983=CARTESIAN_POINT('Ctrl Pts',(-64.133768380869,-31.3298763753377,0.));
#79984=CARTESIAN_POINT('Ctrl Pts',(-64.1500031332282,-31.3459097002006,
0.));
#79985=CARTESIAN_POINT('Ctrl Pts',(-64.166253899542,-31.3619910181228,0.));
#79986=CARTESIAN_POINT('Ctrl Pts',(-64.1825205366224,-31.3781202823754,
0.));
#79987=CARTESIAN_POINT('Ctrl Pts',(-64.1988029019707,-31.3942974463445,
0.));
#79988=CARTESIAN_POINT('Ctrl Pts',(-64.2151008537697,-31.410522463528,0.));
#79989=CARTESIAN_POINT('Ctrl Pts',(-64.231414250881,-31.4267952875423,0.));
#79990=CARTESIAN_POINT('Ctrl Pts',(-64.2477429528393,-31.4431158721222,
0.));
#79991=CARTESIAN_POINT('Ctrl Pts',(-64.2640868198473,-31.4594841711194,
0.));
#79992=CARTESIAN_POINT('Ctrl Pts',(-64.2804457127671,-31.4759001384941,
0.));
#79993=CARTESIAN_POINT('Ctrl Pts',(-64.2968194931158,-31.4923637283132,
0.));
#79994=CARTESIAN_POINT('Ctrl Pts',(-64.3132080230637,-31.5088748947582,
0.));
#79995=CARTESIAN_POINT('Ctrl Pts',(-64.3296111654283,-31.5254335921245,
0.));
#79996=CARTESIAN_POINT('Ctrl Pts',(-64.3460287836687,-31.5420397748191,
0.));
#79997=CARTESIAN_POINT('Ctrl Pts',(-64.3624607418768,-31.5586933973515,
0.));
#79998=CARTESIAN_POINT('Ctrl Pts',(-64.3789069047733,-31.5753944143336,
0.));
#79999=CARTESIAN_POINT('Ctrl Pts',(-64.3953671377046,-31.5921427804865,
0.));
#80000=CARTESIAN_POINT('Ctrl Pts',(-64.4118413066378,-31.6089384506395,
0.));
#80001=CARTESIAN_POINT('Ctrl Pts',(-64.4283292781565,-31.6257813797287,
0.));
#80002=CARTESIAN_POINT('Ctrl Pts',(-64.4448309194525,-31.6426715227878,
0.));
#80003=CARTESIAN_POINT('Ctrl Pts',(-64.4613460983214,-31.6596088349482,
0.));
#80004=CARTESIAN_POINT('Ctrl Pts',(-64.4778746831614,-31.6765932714464,
0.));
#80005=CARTESIAN_POINT('Ctrl Pts',(-64.4944165429675,-31.6936247876229,
0.));
#80006=CARTESIAN_POINT('Ctrl Pts',(-64.510971547327,-31.7107033389201,0.));
#80007=CARTESIAN_POINT('Ctrl Pts',(-64.5275395664124,-31.7278288808731,
0.));
#80008=CARTESIAN_POINT('Ctrl Pts',(-64.544120470977,-31.7450013691112,0.));
#80009=CARTESIAN_POINT('Ctrl Pts',(-64.5607141323521,-31.7622207593634,
0.));
#80010=CARTESIAN_POINT('Ctrl Pts',(-64.5773204224429,-31.7794870074583,
0.));
#80011=CARTESIAN_POINT('Ctrl Pts',(-64.5939392137235,-31.7968000693218,
0.));
#80012=CARTESIAN_POINT('Ctrl Pts',(-64.6105703792312,-31.8141599009684,
0.));
#80013=CARTESIAN_POINT('Ctrl Pts',(-64.6272137925627,-31.8315664585026,
0.));
#80014=CARTESIAN_POINT('Ctrl Pts',(-64.6438693278714,-31.8490196981248,
0.));
#80015=CARTESIAN_POINT('Ctrl Pts',(-64.6605368598629,-31.866519576131,0.));
#80016=CARTESIAN_POINT('Ctrl Pts',(-64.6772162637907,-31.8840660489107,
0.));
#80017=CARTESIAN_POINT('Ctrl Pts',(-64.6939074154498,-31.9016590729374,
0.));
#80018=CARTESIAN_POINT('Ctrl Pts',(-64.7106101911732,-31.9192986047706,
0.));
#80019=CARTESIAN_POINT('Ctrl Pts',(-64.7273244678297,-31.9369846010615,
0.));
#80020=CARTESIAN_POINT('Ctrl Pts',(-64.7440501228202,-31.9547170185534,
0.));
#80021=CARTESIAN_POINT('Ctrl Pts',(-64.7607870340735,-31.9724958140789,
0.));
#80022=CARTESIAN_POINT('Ctrl Pts',(-64.77753508004,-31.990320944552,0.));
#80023=CARTESIAN_POINT('Ctrl Pts',(-64.7942941396881,-32.0081923669677,
0.));
#80024=CARTESIAN_POINT('Ctrl Pts',(-64.8110640925021,-32.0261100384092,
0.));
#80025=CARTESIAN_POINT('Ctrl Pts',(-64.8278448184786,-32.0440739160477,
0.));
#80026=CARTESIAN_POINT('Ctrl Pts',(-64.8446361981234,-32.0620839571408,
0.));
#80027=CARTESIAN_POINT('Ctrl Pts',(-64.861438112445,-32.0801401190241,0.));
#80028=CARTESIAN_POINT('Ctrl Pts',(-64.878250442952,-32.0982423591108,0.));
#80029=CARTESIAN_POINT('Ctrl Pts',(-64.8950730716493,-32.1163906348979,
0.));
#80030=CARTESIAN_POINT('Ctrl Pts',(-64.9119058810362,-32.1345849039671,
0.));
#80031=CARTESIAN_POINT('Ctrl Pts',(-64.9287487541018,-32.1528251239832,
0.));
#80032=CARTESIAN_POINT('Ctrl Pts',(-64.9456015743203,-32.171111252686,0.));
#80033=CARTESIAN_POINT('Ctrl Pts',(-64.9624642256477,-32.1894432478889,
0.));
#80034=CARTESIAN_POINT('Ctrl Pts',(-64.9793365925194,-32.2078210674857,
0.));
#80035=CARTESIAN_POINT('Ctrl Pts',(-64.996218559847,-32.2262446694516,0.));
#80036=CARTESIAN_POINT('Ctrl Pts',(-65.0131100130155,-32.244714011842,0.));
#80037=CARTESIAN_POINT('Ctrl Pts',(-65.0300108378786,-32.2632290527855,
0.));
#80038=CARTESIAN_POINT('Ctrl Pts',(-65.0469209207548,-32.2817897504799,
0.));
#80039=CARTESIAN_POINT('Ctrl Pts',(-65.0638401484245,-32.3003960632,0.));
#80040=CARTESIAN_POINT('Ctrl Pts',(-65.0807684081278,-32.3190479492985,
0.));
#80041=CARTESIAN_POINT('Ctrl Pts',(-65.097705587561,-32.3377453672052,0.));
#80042=CARTESIAN_POINT('Ctrl Pts',(-65.1146515748723,-32.3564882754212,
0.));
#80043=CARTESIAN_POINT('Ctrl Pts',(-65.1316062586586,-32.3752766325135,
0.));
#80044=CARTESIAN_POINT('Ctrl Pts',(-65.1485695279628,-32.3941103971218,
0.));
#80045=CARTESIAN_POINT('Ctrl Pts',(-65.165541272272,-32.4129895279612,0.));
#80046=CARTESIAN_POINT('Ctrl Pts',(-65.182521381514,-32.4319139838212,0.));
#80047=CARTESIAN_POINT('Ctrl Pts',(-65.1995097460546,-32.4508837235613,
0.));
#80048=CARTESIAN_POINT('Ctrl Pts',(-65.2165062566936,-32.4698987061037,
0.));
#80049=CARTESIAN_POINT('Ctrl Pts',(-65.2335108046625,-32.4889588904397,
0.));
#80050=CARTESIAN_POINT('Ctrl Pts',(-65.2505232816215,-32.508064235633,0.));
#80051=CARTESIAN_POINT('Ctrl Pts',(-65.2675435796558,-32.5272147008191,
0.));
#80052=CARTESIAN_POINT('Ctrl Pts',(-65.2845715912717,-32.5464102452013,
0.));
#80053=CARTESIAN_POINT('Ctrl Pts',(-65.3016072093907,-32.565650828042,0.));
#80054=CARTESIAN_POINT('Ctrl Pts',(-65.3186503273498,-32.5849364086679,
0.));
#80055=CARTESIAN_POINT('Ctrl Pts',(-65.3357008389004,-32.6042669464752,
0.));
#80056=CARTESIAN_POINT('Ctrl Pts',(-65.3527586382082,-32.6236424009302,
0.));
#80057=CARTESIAN_POINT('Ctrl Pts',(-65.3698236198511,-32.6430627315673,
0.));
#80058=CARTESIAN_POINT('Ctrl Pts',(-65.3868956788178,-32.6625278979807,
0.));
#80059=CARTESIAN_POINT('Ctrl Pts',(-65.4039747105033,-32.6820378598262,
0.));
#80060=CARTESIAN_POINT('Ctrl Pts',(-65.4210606107029,-32.7015925768261,
0.));
#80061=CARTESIAN_POINT('Ctrl Pts',(-65.4381532756062,-32.7211920087682,
0.));
#80062=CARTESIAN_POINT('Ctrl Pts',(-65.4552526017907,-32.7408361155038,
0.));
#80063=CARTESIAN_POINT('Ctrl Pts',(-65.4723584862129,-32.7605248569382,
0.));
#80064=CARTESIAN_POINT('Ctrl Pts',(-65.4894708262071,-32.7802581930293,
0.));
#80065=CARTESIAN_POINT('Ctrl Pts',(-65.5065895194938,-32.8000360837981,
0.));
#80066=CARTESIAN_POINT('Ctrl Pts',(-65.5237144641864,-32.8198584893319,
0.));
#80067=CARTESIAN_POINT('Ctrl Pts',(-65.5408455587963,-32.8397253697864,
0.));
#80068=CARTESIAN_POINT('Ctrl Pts',(-65.5579827022412,-32.8596366853826,
0.));
#80069=CARTESIAN_POINT('Ctrl Pts',(-65.575125793846,-32.8795923964022,0.));
#80070=CARTESIAN_POINT('Ctrl Pts',(-65.5922747333181,-32.899592463189,0.));
#80071=CARTESIAN_POINT('Ctrl Pts',(-65.6094294207267,-32.9196368461457,
0.));
#80072=CARTESIAN_POINT('Ctrl Pts',(-65.6265897564782,-32.9397255057273,
0.));
#80073=CARTESIAN_POINT('Ctrl Pts',(-65.6437556412956,-32.9598584024318,
0.));
#80074=CARTESIAN_POINT('Ctrl Pts',(-65.6609269761902,-32.9800354967847,
0.));
#80075=CARTESIAN_POINT('Ctrl Pts',(-65.6781036625041,-33.0002567493581,
0.));
#80076=CARTESIAN_POINT('Ctrl Pts',(-65.6952856019542,-33.0205221207877,
0.));
#80077=CARTESIAN_POINT('Ctrl Pts',(-65.7124726966805,-33.0408315717874,
0.));
#80078=CARTESIAN_POINT('Ctrl Pts',(-65.729664849282,-33.061185063158,0.));
#80079=CARTESIAN_POINT('Ctrl Pts',(-65.7468619628808,-33.0815825557976,
0.));
#80080=CARTESIAN_POINT('Ctrl Pts',(-65.7640639410653,-33.102024010688,0.));
#80081=CARTESIAN_POINT('Ctrl Pts',(-65.7812706877691,-33.1225093888668,
0.));
#80082=CARTESIAN_POINT('Ctrl Pts',(-65.7984821071621,-33.1430386513975,
0.));
#80083=CARTESIAN_POINT('Ctrl Pts',(-65.8156981035504,-33.16361175934,0.));
#80084=CARTESIAN_POINT('Ctrl Pts',(-65.8329185812379,-33.1842286737053,
0.));
#80085=CARTESIAN_POINT('Ctrl Pts',(-65.8501434445174,-33.2048893554496,
0.));
#80086=CARTESIAN_POINT('Ctrl Pts',(-65.8673725979591,-33.2255937655656,
0.));
#80087=CARTESIAN_POINT('Ctrl Pts',(-65.8846059466382,-33.2463418651498,
0.));
#80088=CARTESIAN_POINT('Ctrl Pts',(-65.901843396389,-33.2671336154754,0.));
#80089=CARTESIAN_POINT('Ctrl Pts',(-65.9190848540422,-33.2879689780566,
0.));
#80090=CARTESIAN_POINT('Ctrl Pts',(-65.9363302276822,-33.3088479147151,
0.));
#80091=CARTESIAN_POINT('Ctrl Pts',(-65.9535794260802,-33.3297703874249,
0.));
#80092=CARTESIAN_POINT('Ctrl Pts',(-65.9708323581385,-33.3507363581579,
0.));
#80093=CARTESIAN_POINT('Ctrl Pts',(-65.9880889322822,-33.3717457887095,
0.));
#80094=CARTESIAN_POINT('Ctrl Pts',(-66.0053490559826,-33.3927986405612,
0.));
#80095=CARTESIAN_POINT('Ctrl Pts',(-66.0226126349482,-33.4138948746408,
0.));
#80096=CARTESIAN_POINT('Ctrl Pts',(-66.0398795737827,-33.4350344515128,
0.));
#80097=CARTESIAN_POINT('Ctrl Pts',(-66.0571497774484,-33.4562173318052,
0.));
#80098=CARTESIAN_POINT('Ctrl Pts',(-66.0744231525445,-33.4774434765762,
0.));
#80099=CARTESIAN_POINT('Ctrl Pts',(-66.0916996085237,-33.4987128476618,
0.));
#80100=CARTESIAN_POINT('Ctrl Pts',(-66.1089790592673,-33.5200254081212,
0.));
#80101=CARTESIAN_POINT('Ctrl Pts',(-66.1262614234579,-33.5413811223398,
0.));
#80102=CARTESIAN_POINT('Ctrl Pts',(-66.1410781873125,-33.5597240685729,
0.));
#80103=CARTESIAN_POINT('Ctrl Pts',(-66.1524393973986,-33.5738105077707,
0.));
#80104=CARTESIAN_POINT('Ctrl Pts',(-66.1603438177306,-33.5836213513974,
0.));
#80105=CARTESIAN_POINT('Ctrl Pts',(-66.1647906582409,-33.5891439876228,
0.));
#80106=CARTESIAN_POINT('Ctrl Pts',(-66.165779540567,-33.5903722664958,0.));
#80107=CARTESIAN_POINT('',(-63.0759831361898,-30.3549065457811,12.));
#80108=CARTESIAN_POINT('',(-63.0759831361898,-30.3549065457811,0.));
#80109=CARTESIAN_POINT('Ctrl Pts',(-66.165779540567,-33.5903722664958,12.));
#80110=CARTESIAN_POINT('Ctrl Pts',(-66.1647906582409,-33.5891439876228,
12.));
#80111=CARTESIAN_POINT('Ctrl Pts',(-66.1603438177306,-33.5836213513974,
12.));
#80112=CARTESIAN_POINT('Ctrl Pts',(-66.1524393973986,-33.5738105077707,
12.));
#80113=CARTESIAN_POINT('Ctrl Pts',(-66.1410781873125,-33.5597240685729,
12.));
#80114=CARTESIAN_POINT('Ctrl Pts',(-66.1262614234579,-33.5413811223398,
12.));
#80115=CARTESIAN_POINT('Ctrl Pts',(-66.1089790592673,-33.5200254081212,
12.));
#80116=CARTESIAN_POINT('Ctrl Pts',(-66.0916996085237,-33.4987128476618,
12.));
#80117=CARTESIAN_POINT('Ctrl Pts',(-66.0744231525445,-33.4774434765762,
12.));
#80118=CARTESIAN_POINT('Ctrl Pts',(-66.0571497774484,-33.4562173318052,
12.));
#80119=CARTESIAN_POINT('Ctrl Pts',(-66.0398795737827,-33.4350344515128,
12.));
#80120=CARTESIAN_POINT('Ctrl Pts',(-66.0226126349482,-33.4138948746408,
12.));
#80121=CARTESIAN_POINT('Ctrl Pts',(-66.0053490559826,-33.3927986405612,
12.));
#80122=CARTESIAN_POINT('Ctrl Pts',(-65.9880889322822,-33.3717457887095,
12.));
#80123=CARTESIAN_POINT('Ctrl Pts',(-65.9708323581385,-33.3507363581579,
12.));
#80124=CARTESIAN_POINT('Ctrl Pts',(-65.9535794260802,-33.3297703874249,
12.));
#80125=CARTESIAN_POINT('Ctrl Pts',(-65.9363302276822,-33.3088479147151,
12.));
#80126=CARTESIAN_POINT('Ctrl Pts',(-65.9190848540422,-33.2879689780566,
12.));
#80127=CARTESIAN_POINT('Ctrl Pts',(-65.901843396389,-33.2671336154754,12.));
#80128=CARTESIAN_POINT('Ctrl Pts',(-65.8846059466382,-33.2463418651498,
12.));
#80129=CARTESIAN_POINT('Ctrl Pts',(-65.8673725979591,-33.2255937655656,
12.));
#80130=CARTESIAN_POINT('Ctrl Pts',(-65.8501434445174,-33.2048893554496,
12.));
#80131=CARTESIAN_POINT('Ctrl Pts',(-65.8329185812379,-33.1842286737053,
12.));
#80132=CARTESIAN_POINT('Ctrl Pts',(-65.8156981035504,-33.16361175934,12.));
#80133=CARTESIAN_POINT('Ctrl Pts',(-65.7984821071621,-33.1430386513975,
12.));
#80134=CARTESIAN_POINT('Ctrl Pts',(-65.7812706877691,-33.1225093888668,
12.));
#80135=CARTESIAN_POINT('Ctrl Pts',(-65.7640639410653,-33.102024010688,12.));
#80136=CARTESIAN_POINT('Ctrl Pts',(-65.7468619628808,-33.0815825557976,
12.));
#80137=CARTESIAN_POINT('Ctrl Pts',(-65.729664849282,-33.061185063158,12.));
#80138=CARTESIAN_POINT('Ctrl Pts',(-65.7124726966805,-33.0408315717874,
12.));
#80139=CARTESIAN_POINT('Ctrl Pts',(-65.6952856019542,-33.0205221207877,
12.));
#80140=CARTESIAN_POINT('Ctrl Pts',(-65.6781036625041,-33.0002567493581,
12.));
#80141=CARTESIAN_POINT('Ctrl Pts',(-65.6609269761902,-32.9800354967847,
12.));
#80142=CARTESIAN_POINT('Ctrl Pts',(-65.6437556412956,-32.9598584024318,
12.));
#80143=CARTESIAN_POINT('Ctrl Pts',(-65.6265897564782,-32.9397255057273,
12.));
#80144=CARTESIAN_POINT('Ctrl Pts',(-65.6094294207267,-32.9196368461457,
12.));
#80145=CARTESIAN_POINT('Ctrl Pts',(-65.5922747333181,-32.899592463189,12.));
#80146=CARTESIAN_POINT('Ctrl Pts',(-65.575125793846,-32.8795923964022,12.));
#80147=CARTESIAN_POINT('Ctrl Pts',(-65.5579827022412,-32.8596366853826,
12.));
#80148=CARTESIAN_POINT('Ctrl Pts',(-65.5408455587963,-32.8397253697864,
12.));
#80149=CARTESIAN_POINT('Ctrl Pts',(-65.5237144641864,-32.8198584893319,
12.));
#80150=CARTESIAN_POINT('Ctrl Pts',(-65.5065895194938,-32.8000360837981,
12.));
#80151=CARTESIAN_POINT('Ctrl Pts',(-65.4894708262071,-32.7802581930293,
12.));
#80152=CARTESIAN_POINT('Ctrl Pts',(-65.4723584862129,-32.7605248569382,
12.));
#80153=CARTESIAN_POINT('Ctrl Pts',(-65.4552526017907,-32.7408361155038,
12.));
#80154=CARTESIAN_POINT('Ctrl Pts',(-65.4381532756062,-32.7211920087682,
12.));
#80155=CARTESIAN_POINT('Ctrl Pts',(-65.4210606107029,-32.7015925768261,
12.));
#80156=CARTESIAN_POINT('Ctrl Pts',(-65.4039747105033,-32.6820378598262,
12.));
#80157=CARTESIAN_POINT('Ctrl Pts',(-65.3868956788178,-32.6625278979807,
12.));
#80158=CARTESIAN_POINT('Ctrl Pts',(-65.3698236198511,-32.6430627315673,
12.));
#80159=CARTESIAN_POINT('Ctrl Pts',(-65.3527586382082,-32.6236424009302,
12.));
#80160=CARTESIAN_POINT('Ctrl Pts',(-65.3357008389004,-32.6042669464752,
12.));
#80161=CARTESIAN_POINT('Ctrl Pts',(-65.3186503273498,-32.5849364086679,
12.));
#80162=CARTESIAN_POINT('Ctrl Pts',(-65.3016072093907,-32.565650828042,12.));
#80163=CARTESIAN_POINT('Ctrl Pts',(-65.2845715912717,-32.5464102452013,
12.));
#80164=CARTESIAN_POINT('Ctrl Pts',(-65.2675435796558,-32.5272147008191,
12.));
#80165=CARTESIAN_POINT('Ctrl Pts',(-65.2505232816215,-32.508064235633,12.));
#80166=CARTESIAN_POINT('Ctrl Pts',(-65.2335108046625,-32.4889588904397,
12.));
#80167=CARTESIAN_POINT('Ctrl Pts',(-65.2165062566936,-32.4698987061037,
12.));
#80168=CARTESIAN_POINT('Ctrl Pts',(-65.1995097460546,-32.4508837235613,
12.));
#80169=CARTESIAN_POINT('Ctrl Pts',(-65.182521381514,-32.4319139838212,12.));
#80170=CARTESIAN_POINT('Ctrl Pts',(-65.165541272272,-32.4129895279612,12.));
#80171=CARTESIAN_POINT('Ctrl Pts',(-65.1485695279628,-32.3941103971218,
12.));
#80172=CARTESIAN_POINT('Ctrl Pts',(-65.1316062586586,-32.3752766325135,
12.));
#80173=CARTESIAN_POINT('Ctrl Pts',(-65.1146515748723,-32.3564882754212,
12.));
#80174=CARTESIAN_POINT('Ctrl Pts',(-65.097705587561,-32.3377453672052,12.));
#80175=CARTESIAN_POINT('Ctrl Pts',(-65.0807684081278,-32.3190479492985,
12.));
#80176=CARTESIAN_POINT('Ctrl Pts',(-65.0638401484245,-32.3003960632,12.));
#80177=CARTESIAN_POINT('Ctrl Pts',(-65.0469209207548,-32.2817897504799,
12.));
#80178=CARTESIAN_POINT('Ctrl Pts',(-65.0300108378786,-32.2632290527855,
12.));
#80179=CARTESIAN_POINT('Ctrl Pts',(-65.0131100130155,-32.244714011842,12.));
#80180=CARTESIAN_POINT('Ctrl Pts',(-64.996218559847,-32.2262446694516,12.));
#80181=CARTESIAN_POINT('Ctrl Pts',(-64.9793365925194,-32.2078210674857,
12.));
#80182=CARTESIAN_POINT('Ctrl Pts',(-64.9624642256477,-32.1894432478889,
12.));
#80183=CARTESIAN_POINT('Ctrl Pts',(-64.9456015743203,-32.171111252686,12.));
#80184=CARTESIAN_POINT('Ctrl Pts',(-64.9287487541018,-32.1528251239832,
12.));
#80185=CARTESIAN_POINT('Ctrl Pts',(-64.9119058810362,-32.1345849039671,
12.));
#80186=CARTESIAN_POINT('Ctrl Pts',(-64.8950730716493,-32.1163906348979,
12.));
#80187=CARTESIAN_POINT('Ctrl Pts',(-64.878250442952,-32.0982423591108,12.));
#80188=CARTESIAN_POINT('Ctrl Pts',(-64.861438112445,-32.0801401190241,12.));
#80189=CARTESIAN_POINT('Ctrl Pts',(-64.8446361981234,-32.0620839571408,
12.));
#80190=CARTESIAN_POINT('Ctrl Pts',(-64.8278448184786,-32.0440739160477,
12.));
#80191=CARTESIAN_POINT('Ctrl Pts',(-64.8110640925021,-32.0261100384092,
12.));
#80192=CARTESIAN_POINT('Ctrl Pts',(-64.7942941396881,-32.0081923669677,
12.));
#80193=CARTESIAN_POINT('Ctrl Pts',(-64.77753508004,-31.990320944552,12.));
#80194=CARTESIAN_POINT('Ctrl Pts',(-64.7607870340735,-31.9724958140789,
12.));
#80195=CARTESIAN_POINT('Ctrl Pts',(-64.7440501228202,-31.9547170185534,
12.));
#80196=CARTESIAN_POINT('Ctrl Pts',(-64.7273244678297,-31.9369846010615,
12.));
#80197=CARTESIAN_POINT('Ctrl Pts',(-64.7106101911732,-31.9192986047706,
12.));
#80198=CARTESIAN_POINT('Ctrl Pts',(-64.6939074154498,-31.9016590729374,
12.));
#80199=CARTESIAN_POINT('Ctrl Pts',(-64.6772162637907,-31.8840660489107,
12.));
#80200=CARTESIAN_POINT('Ctrl Pts',(-64.6605368598629,-31.866519576131,12.));
#80201=CARTESIAN_POINT('Ctrl Pts',(-64.6438693278714,-31.8490196981248,
12.));
#80202=CARTESIAN_POINT('Ctrl Pts',(-64.6272137925627,-31.8315664585026,
12.));
#80203=CARTESIAN_POINT('Ctrl Pts',(-64.6105703792312,-31.8141599009684,
12.));
#80204=CARTESIAN_POINT('Ctrl Pts',(-64.5939392137235,-31.7968000693218,
12.));
#80205=CARTESIAN_POINT('Ctrl Pts',(-64.5773204224429,-31.7794870074583,
12.));
#80206=CARTESIAN_POINT('Ctrl Pts',(-64.5607141323521,-31.7622207593634,
12.));
#80207=CARTESIAN_POINT('Ctrl Pts',(-64.544120470977,-31.7450013691112,12.));
#80208=CARTESIAN_POINT('Ctrl Pts',(-64.5275395664124,-31.7278288808731,
12.));
#80209=CARTESIAN_POINT('Ctrl Pts',(-64.510971547327,-31.7107033389201,12.));
#80210=CARTESIAN_POINT('Ctrl Pts',(-64.4944165429675,-31.6936247876229,
12.));
#80211=CARTESIAN_POINT('Ctrl Pts',(-64.4778746831614,-31.6765932714464,
12.));
#80212=CARTESIAN_POINT('Ctrl Pts',(-64.4613460983214,-31.6596088349482,
12.));
#80213=CARTESIAN_POINT('Ctrl Pts',(-64.4448309194525,-31.6426715227878,
12.));
#80214=CARTESIAN_POINT('Ctrl Pts',(-64.4283292781565,-31.6257813797287,
12.));
#80215=CARTESIAN_POINT('Ctrl Pts',(-64.4118413066378,-31.6089384506395,
12.));
#80216=CARTESIAN_POINT('Ctrl Pts',(-64.3953671377046,-31.5921427804865,
12.));
#80217=CARTESIAN_POINT('Ctrl Pts',(-64.3789069047733,-31.5753944143336,
12.));
#80218=CARTESIAN_POINT('Ctrl Pts',(-64.3624607418768,-31.5586933973515,
12.));
#80219=CARTESIAN_POINT('Ctrl Pts',(-64.3460287836687,-31.5420397748191,
12.));
#80220=CARTESIAN_POINT('Ctrl Pts',(-64.3296111654283,-31.5254335921245,
12.));
#80221=CARTESIAN_POINT('Ctrl Pts',(-64.3132080230637,-31.5088748947582,
12.));
#80222=CARTESIAN_POINT('Ctrl Pts',(-64.2968194931158,-31.4923637283132,
12.));
#80223=CARTESIAN_POINT('Ctrl Pts',(-64.2804457127671,-31.4759001384941,
12.));
#80224=CARTESIAN_POINT('Ctrl Pts',(-64.2640868198473,-31.4594841711194,
12.));
#80225=CARTESIAN_POINT('Ctrl Pts',(-64.2477429528393,-31.4431158721222,
12.));
#80226=CARTESIAN_POINT('Ctrl Pts',(-64.231414250881,-31.4267952875423,12.));
#80227=CARTESIAN_POINT('Ctrl Pts',(-64.2151008537697,-31.410522463528,12.));
#80228=CARTESIAN_POINT('Ctrl Pts',(-64.1988029019707,-31.3942974463445,
12.));
#80229=CARTESIAN_POINT('Ctrl Pts',(-64.1825205366224,-31.3781202823754,
12.));
#80230=CARTESIAN_POINT('Ctrl Pts',(-64.166253899542,-31.3619910181228,12.));
#80231=CARTESIAN_POINT('Ctrl Pts',(-64.1500031332282,-31.3459097002006,
12.));
#80232=CARTESIAN_POINT('Ctrl Pts',(-64.133768380869,-31.3298763753377,12.));
#80233=CARTESIAN_POINT('Ctrl Pts',(-64.117549786349,-31.3138910903859,12.));
#80234=CARTESIAN_POINT('Ctrl Pts',(-64.1013474942556,-31.2979538923214,
12.));
#80235=CARTESIAN_POINT('Ctrl Pts',(-64.0851616498852,-31.2820648282447,
12.));
#80236=CARTESIAN_POINT('Ctrl Pts',(-64.0689923992461,-31.2662239453728,
12.));
#80237=CARTESIAN_POINT('Ctrl Pts',(-64.0528398890657,-31.2504312910451,
12.));
#80238=CARTESIAN_POINT('Ctrl Pts',(-64.0367042667984,-31.2346869127297,
12.));
#80239=CARTESIAN_POINT('Ctrl Pts',(-64.02058568063,-31.2189908580245,12.));
#80240=CARTESIAN_POINT('Ctrl Pts',(-64.0044842794831,-31.2033431746558,
12.));
#80241=CARTESIAN_POINT('Ctrl Pts',(-63.9884002130211,-31.1877439104717,
12.));
#80242=CARTESIAN_POINT('Ctrl Pts',(-63.9723336316551,-31.1721931134487,
12.));
#80243=CARTESIAN_POINT('Ctrl Pts',(-63.9562846865567,-31.1566908316992,
12.));
#80244=CARTESIAN_POINT('Ctrl Pts',(-63.940253529665,-31.1412371134727,12.));
#80245=CARTESIAN_POINT('Ctrl Pts',(-63.9242403136955,-31.1258320071545,
12.));
#80246=CARTESIAN_POINT('Ctrl Pts',(-63.9082451921448,-31.1104755612607,
12.));
#80247=CARTESIAN_POINT('Ctrl Pts',(-63.8922683192964,-31.0951678244455,
12.));
#80248=CARTESIAN_POINT('Ctrl Pts',(-63.8763098502237,-31.0799088455041,
12.));
#80249=CARTESIAN_POINT('Ctrl Pts',(-63.8603699407922,-31.0646986733723,
12.));
#80250=CARTESIAN_POINT('Ctrl Pts',(-63.8444487476611,-31.0495373571215,
12.));
#80251=CARTESIAN_POINT('Ctrl Pts',(-63.8285464282846,-31.0344249459538,
12.));
#80252=CARTESIAN_POINT('Ctrl Pts',(-63.8126631409364,-31.0193614892171,
12.));
#80253=CARTESIAN_POINT('Ctrl Pts',(-63.796799044728,-31.0043470364108,12.));
#80254=CARTESIAN_POINT('Ctrl Pts',(-63.7809542996264,-30.989381637191,12.));
#80255=CARTESIAN_POINT('Ctrl Pts',(-63.7651290664733,-30.9744653413689,
12.));
#80256=CARTESIAN_POINT('Ctrl Pts',(-63.749323506987,-30.9595981989103,12.));
#80257=CARTESIAN_POINT('Ctrl Pts',(-63.7335377837441,-30.9447802599355,
12.));
#80258=CARTESIAN_POINT('Ctrl Pts',(-63.7177720601609,-30.9300115747115,
12.));
#80259=CARTESIAN_POINT('Ctrl Pts',(-63.7020265004792,-30.9152921936465,
12.));
#80260=CARTESIAN_POINT('Ctrl Pts',(-63.6863012697328,-30.900622167269,12.));
#80261=CARTESIAN_POINT('Ctrl Pts',(-63.6705965337971,-30.8860015462475,
12.));
#80262=CARTESIAN_POINT('Ctrl Pts',(-63.6549124594666,-30.8714303814194,
12.));
#80263=CARTESIAN_POINT('Ctrl Pts',(-63.6392492145233,-30.8569087238131,
12.));
#80264=CARTESIAN_POINT('Ctrl Pts',(-63.6236069678055,-30.8424366246671,
12.));
#80265=CARTESIAN_POINT('Ctrl Pts',(-63.6079858892771,-30.8280141354459,
12.));
#80266=CARTESIAN_POINT('Ctrl Pts',(-63.5923861498987,-30.813641307801,12.));
#80267=CARTESIAN_POINT('Ctrl Pts',(-63.5768079214881,-30.7993181935271,
12.));
#80268=CARTESIAN_POINT('Ctrl Pts',(-63.5612513766,-30.7850448445205,12.));
#80269=CARTESIAN_POINT('Ctrl Pts',(-63.5457166883537,-30.7708213127159,
12.));
#80270=CARTESIAN_POINT('Ctrl Pts',(-63.5302040304142,-30.7566476500757,
12.));
#80271=CARTESIAN_POINT('Ctrl Pts',(-63.5147135773894,-30.7425239087281,
12.));
#80272=CARTESIAN_POINT('Ctrl Pts',(-63.4992455051795,-30.7284501410822,
12.));
#80273=CARTESIAN_POINT('Ctrl Pts',(-63.4837999912771,-30.7144263999265,
12.));
#80274=CARTESIAN_POINT('Ctrl Pts',(-63.4683772152529,-30.7004527385821,
12.));
#80275=CARTESIAN_POINT('Ctrl Pts',(-63.4529773584249,-30.6865292107929,
12.));
#80276=CARTESIAN_POINT('Ctrl Pts',(-63.4376006029604,-30.6726558704315,
12.));
#80277=CARTESIAN_POINT('Ctrl Pts',(-63.4222471311239,-30.6588327712483,
12.));
#80278=CARTESIAN_POINT('Ctrl Pts',(-63.4069171245066,-30.6450599666121,
12.));
#80279=CARTESIAN_POINT('Ctrl Pts',(-63.3916107631376,-30.6313375092062,
12.));
#80280=CARTESIAN_POINT('Ctrl Pts',(-63.3763282271796,-30.6176654515967,
12.));
#80281=CARTESIAN_POINT('Ctrl Pts',(-63.3610696989577,-30.6040438469078,
12.));
#80282=CARTESIAN_POINT('Ctrl Pts',(-63.3458353646154,-30.5904727493711,
12.));
#80283=CARTESIAN_POINT('Ctrl Pts',(-63.3306254165126,-30.5769522151164,
12.));
#80284=CARTESIAN_POINT('Ctrl Pts',(-63.3154400534397,-30.563482302238,12.));
#80285=CARTESIAN_POINT('Ctrl Pts',(-63.3002794756086,-30.5500630691359,
12.));
#80286=CARTESIAN_POINT('Ctrl Pts',(-63.2851438802473,-30.5366945730508,
12.));
#80287=CARTESIAN_POINT('Ctrl Pts',(-63.2700334577639,-30.5233768687865,
12.));
#80288=CARTESIAN_POINT('Ctrl Pts',(-63.2549483856215,-30.5101100066659,
12.));
#80289=CARTESIAN_POINT('Ctrl Pts',(-63.2398888342545,-30.4968940344998,
12.));
#80290=CARTESIAN_POINT('Ctrl Pts',(-63.2248549788221,-30.4837290014989,
12.));
#80291=CARTESIAN_POINT('Ctrl Pts',(-63.2098470086636,-30.470614961416,12.));
#80292=CARTESIAN_POINT('Ctrl Pts',(-63.1948651386942,-30.4575519763337,
12.));
#80293=CARTESIAN_POINT('Ctrl Pts',(-63.179909617189,-30.444540119238,12.));
#80294=CARTESIAN_POINT('Ctrl Pts',(-63.164980701691,-30.4315794659731,12.));
#80295=CARTESIAN_POINT('Ctrl Pts',(-63.1500786361459,-30.418670087563,12.));
#80296=CARTESIAN_POINT('Ctrl Pts',(-63.135203629844,-30.4058120432228,12.));
#80297=CARTESIAN_POINT('Ctrl Pts',(-63.1203558300657,-30.3930053710484,
12.));
#80298=CARTESIAN_POINT('Ctrl Pts',(-63.105535320226,-30.3802500880403,12.));
#80299=CARTESIAN_POINT('Ctrl Pts',(-63.0937007763471,-30.3700869762507,
12.));
#80300=CARTESIAN_POINT('Ctrl Pts',(-63.0848371718048,-30.3624877680651,
12.));
#80301=CARTESIAN_POINT('Ctrl Pts',(-63.078933570069,-30.3574319069329,12.));
#80302=CARTESIAN_POINT('Ctrl Pts',(-63.0759831361898,-30.3549065457811,
12.));
#80303=CARTESIAN_POINT('Ctrl Pts',(-65.4667541478385,-34.933187552314,-5.55111512312578E-16));
#80304=CARTESIAN_POINT('Ctrl Pts',(-65.4667541478385,-34.933187552314,4.));
#80305=CARTESIAN_POINT('Ctrl Pts',(-65.4667541478385,-34.933187552314,8.));
#80306=CARTESIAN_POINT('Ctrl Pts',(-65.4667541478385,-34.933187552314,12.));
#80307=CARTESIAN_POINT('Ctrl Pts',(-65.5763902570748,-34.940541458921,-5.55111512312578E-16));
#80308=CARTESIAN_POINT('Ctrl Pts',(-65.5763902570748,-34.940541458921,4.));
#80309=CARTESIAN_POINT('Ctrl Pts',(-65.5763902570748,-34.940541458921,8.));
#80310=CARTESIAN_POINT('Ctrl Pts',(-65.5763902570748,-34.940541458921,12.));
#80311=CARTESIAN_POINT('Ctrl Pts',(-65.7720412680588,-34.8876896346299,
-5.55111512312578E-16));
#80312=CARTESIAN_POINT('Ctrl Pts',(-65.7720412680588,-34.8876896346299,
4.00000000000001));
#80313=CARTESIAN_POINT('Ctrl Pts',(-65.7720412680588,-34.8876896346299,
7.99999999999999));
#80314=CARTESIAN_POINT('Ctrl Pts',(-65.7720412680588,-34.8876896346299,
12.));
#80315=CARTESIAN_POINT('Ctrl Pts',(-65.9044372006542,-34.7399186668304,
-5.55111512312578E-16));
#80316=CARTESIAN_POINT('Ctrl Pts',(-65.9044372006542,-34.7399186668304,
3.99999999999999));
#80317=CARTESIAN_POINT('Ctrl Pts',(-65.9044372006542,-34.7399186668304,
8.00000000000001));
#80318=CARTESIAN_POINT('Ctrl Pts',(-65.9044372006542,-34.7399186668304,
12.));
#80319=CARTESIAN_POINT('Ctrl Pts',(-65.9427857825584,-34.6669728017261,
-5.55111512312578E-16));
#80320=CARTESIAN_POINT('Ctrl Pts',(-65.9427857825584,-34.6669728017261,
4.));
#80321=CARTESIAN_POINT('Ctrl Pts',(-65.9427857825584,-34.6669728017261,
8.));
#80322=CARTESIAN_POINT('Ctrl Pts',(-65.9427857825584,-34.6669728017261,
12.));
#80323=CARTESIAN_POINT('',(-65.4667541478385,-34.933187552314,0.));
#80324=CARTESIAN_POINT('',(-65.9427857825584,-34.6669728017261,2.77555756156289E-16));
#80325=CARTESIAN_POINT('Ctrl Pts',(-65.4667541478385,-34.933187552314,8.50995567916391E-16));
#80326=CARTESIAN_POINT('Ctrl Pts',(-65.5763902570748,-34.940541458921,8.50995567916389E-16));
#80327=CARTESIAN_POINT('Ctrl Pts',(-65.6881908347799,-34.910340416469,8.50995567916392E-16));
#80328=CARTESIAN_POINT('Ctrl Pts',(-65.7793366930113,-34.8491453679733,
8.50995567916391E-16));
#80329=CARTESIAN_POINT('Ctrl Pts',(-65.8476960866847,-34.8032490816016,
8.50995567916391E-16));
#80330=CARTESIAN_POINT('Ctrl Pts',(-65.9044372006542,-34.7399186668304,
8.50995567916389E-16));
#80331=CARTESIAN_POINT('Ctrl Pts',(-65.9427857825584,-34.6669728017261,
8.50995567916391E-16));
#80332=CARTESIAN_POINT('',(-65.9427857825584,-34.6669728017261,12.));
#80333=CARTESIAN_POINT('Ctrl Pts',(-65.9427857825584,-34.6669728017261,
-5.55111512312578E-16));
#80334=CARTESIAN_POINT('Ctrl Pts',(-65.9427857825584,-34.6669728017261,
4.));
#80335=CARTESIAN_POINT('Ctrl Pts',(-65.9427857825584,-34.6669728017261,
8.));
#80336=CARTESIAN_POINT('Ctrl Pts',(-65.9427857825584,-34.6669728017261,
12.));
#80337=CARTESIAN_POINT('',(-65.4667541478385,-34.933187552314,12.));
#80338=CARTESIAN_POINT('Ctrl Pts',(-65.9427857825584,-34.6669728017261,
12.));
#80339=CARTESIAN_POINT('Ctrl Pts',(-65.9044372006542,-34.7399186668304,
12.));
#80340=CARTESIAN_POINT('Ctrl Pts',(-65.8476960866847,-34.8032490816016,
12.));
#80341=CARTESIAN_POINT('Ctrl Pts',(-65.7793366930113,-34.8491453679733,
12.));
#80342=CARTESIAN_POINT('Ctrl Pts',(-65.68819083478,-34.910340416469,12.));
#80343=CARTESIAN_POINT('Ctrl Pts',(-65.5763902570748,-34.940541458921,12.));
#80344=CARTESIAN_POINT('Ctrl Pts',(-65.4667541478385,-34.933187552314,12.));
#80345=CARTESIAN_POINT('Ctrl Pts',(-65.4667541478385,-34.933187552314,12.));
#80346=CARTESIAN_POINT('Ctrl Pts',(-65.4667541478385,-34.933187552314,8.));
#80347=CARTESIAN_POINT('Ctrl Pts',(-65.4667541478385,-34.933187552314,4.));
#80348=CARTESIAN_POINT('Ctrl Pts',(-65.4667541478385,-34.933187552314,-5.55111512312578E-16));
#80349=CARTESIAN_POINT('Origin',(-3.32444647725448E-10,-1.73171632017259E-10,
0.));
#80350=CARTESIAN_POINT('Origin',(-3.32444647725448E-10,-1.73171632017259E-10,
12.));
#80351=CARTESIAN_POINT('Origin',(-3.32444647725448E-10,-1.73171632017259E-10,
0.));
#80352=CARTESIAN_POINT('Ctrl Pts',(-68.9436475237602,-28.2316040302268,
0.));
#80353=CARTESIAN_POINT('Ctrl Pts',(-68.9436475237602,-28.2316040302268,
4.));
#80354=CARTESIAN_POINT('Ctrl Pts',(-68.9436475237602,-28.2316040302268,
8.));
#80355=CARTESIAN_POINT('Ctrl Pts',(-68.9436475237602,-28.2316040302268,
12.));
#80356=CARTESIAN_POINT('Ctrl Pts',(-68.9852872321829,-28.1299168084375,
0.));
#80357=CARTESIAN_POINT('Ctrl Pts',(-68.9852872321829,-28.1299168084375,
4.));
#80358=CARTESIAN_POINT('Ctrl Pts',(-68.9852872321829,-28.1299168084375,
8.));
#80359=CARTESIAN_POINT('Ctrl Pts',(-68.9852872321829,-28.1299168084375,
12.));
#80360=CARTESIAN_POINT('Ctrl Pts',(-68.9970049015576,-27.9275918177424,
0.));
#80361=CARTESIAN_POINT('Ctrl Pts',(-68.9970049015576,-27.9275918177424,
4.));
#80362=CARTESIAN_POINT('Ctrl Pts',(-68.9970049015576,-27.9275918177424,
8.));
#80363=CARTESIAN_POINT('Ctrl Pts',(-68.9970049015576,-27.9275918177424,
12.));
#80364=CARTESIAN_POINT('Ctrl Pts',(-68.8986722313985,-27.7552674476211,
0.));
#80365=CARTESIAN_POINT('Ctrl Pts',(-68.8986722313985,-27.7552674476211,
4.));
#80366=CARTESIAN_POINT('Ctrl Pts',(-68.8986722313985,-27.7552674476211,
8.));
#80367=CARTESIAN_POINT('Ctrl Pts',(-68.8986722313985,-27.7552674476211,
12.));
#80368=CARTESIAN_POINT('Ctrl Pts',(-68.8415926174766,-27.6958230984747,
0.));
#80369=CARTESIAN_POINT('Ctrl Pts',(-68.8415926174766,-27.6958230984747,
4.));
#80370=CARTESIAN_POINT('Ctrl Pts',(-68.8415926174766,-27.6958230984747,
8.));
#80371=CARTESIAN_POINT('Ctrl Pts',(-68.8415926174766,-27.6958230984747,
12.));
#80372=CARTESIAN_POINT('',(-68.9436475237602,-28.2316040302268,0.));
#80373=CARTESIAN_POINT('',(-68.8415926174765,-27.6958230984748,0.));
#80374=CARTESIAN_POINT('Ctrl Pts',(-68.9436475237602,-28.2316040302268,
1.8809784878858E-35));
#80375=CARTESIAN_POINT('Ctrl Pts',(-68.9852872321829,-28.1299168084375,
1.88097848788579E-35));
#80376=CARTESIAN_POINT('Ctrl Pts',(-68.9919830432542,-28.0143025280403,
1.8809784878858E-35));
#80377=CARTESIAN_POINT('Ctrl Pts',(-68.9627440495797,-27.9084843686468,
1.8809784878858E-35));
#80378=CARTESIAN_POINT('Ctrl Pts',(-68.9408148043239,-27.8291207491017,
1.8809784878858E-35));
#80379=CARTESIAN_POINT('Ctrl Pts',(-68.8986722313985,-27.7552674476211,
1.88097848788579E-35));
#80380=CARTESIAN_POINT('Ctrl Pts',(-68.8415926174766,-27.6958230984747,
1.8809784878858E-35));
#80381=CARTESIAN_POINT('',(-68.8415926174765,-27.6958230984748,12.));
#80382=CARTESIAN_POINT('Ctrl Pts',(-68.8415926174766,-27.6958230984747,
0.));
#80383=CARTESIAN_POINT('Ctrl Pts',(-68.8415926174766,-27.6958230984747,
4.));
#80384=CARTESIAN_POINT('Ctrl Pts',(-68.8415926174766,-27.6958230984747,
8.));
#80385=CARTESIAN_POINT('Ctrl Pts',(-68.8415926174766,-27.6958230984747,
12.));
#80386=CARTESIAN_POINT('',(-68.9436475237602,-28.2316040302268,12.));
#80387=CARTESIAN_POINT('Ctrl Pts',(-68.8415926174766,-27.6958230984747,
12.));
#80388=CARTESIAN_POINT('Ctrl Pts',(-68.8986722313985,-27.7552674476211,
12.));
#80389=CARTESIAN_POINT('Ctrl Pts',(-68.9408148043239,-27.8291207491017,
12.));
#80390=CARTESIAN_POINT('Ctrl Pts',(-68.9627440495797,-27.9084843686468,
12.));
#80391=CARTESIAN_POINT('Ctrl Pts',(-68.9919830432542,-28.0143025280403,
12.));
#80392=CARTESIAN_POINT('Ctrl Pts',(-68.9852872321829,-28.1299168084375,
12.));
#80393=CARTESIAN_POINT('Ctrl Pts',(-68.9436475237602,-28.2316040302268,
12.));
#80394=CARTESIAN_POINT('Ctrl Pts',(-68.9436475237602,-28.2316040302268,
12.));
#80395=CARTESIAN_POINT('Ctrl Pts',(-68.9436475237602,-28.2316040302268,
8.));
#80396=CARTESIAN_POINT('Ctrl Pts',(-68.9436475237602,-28.2316040302268,
4.));
#80397=CARTESIAN_POINT('Ctrl Pts',(-68.9436475237602,-28.2316040302268,
0.));
#80398=CARTESIAN_POINT('Ctrl Pts',(-65.4815644032299,-24.7419628022042,
0.));
#80399=CARTESIAN_POINT('Ctrl Pts',(-65.4815644032299,-24.7419628022042,
12.));
#80400=CARTESIAN_POINT('Ctrl Pts',(-65.4847237095443,-24.7442214063382,
0.));
#80401=CARTESIAN_POINT('Ctrl Pts',(-65.4847237095443,-24.7442214063382,
12.));
#80402=CARTESIAN_POINT('Ctrl Pts',(-65.4910454936254,-24.7487434955982,
0.));
#80403=CARTESIAN_POINT('Ctrl Pts',(-65.4910454936254,-24.7487434955982,
12.));
#80404=CARTESIAN_POINT('Ctrl Pts',(-65.5005376841101,-24.7555412724651,
0.));
#80405=CARTESIAN_POINT('Ctrl Pts',(-65.5005376841101,-24.7555412724651,
12.));
#80406=CARTESIAN_POINT('Ctrl Pts',(-65.5132129675333,-24.7646342620841,
0.));
#80407=CARTESIAN_POINT('Ctrl Pts',(-65.5132129675333,-24.7646342620841,
12.));
#80408=CARTESIAN_POINT('Ctrl Pts',(-65.5290887770232,-24.7760493148465,
0.));
#80409=CARTESIAN_POINT('Ctrl Pts',(-65.5290887770232,-24.7760493148465,
12.));
#80410=CARTESIAN_POINT('Ctrl Pts',(-65.5449962514661,-24.787513182749,0.));
#80411=CARTESIAN_POINT('Ctrl Pts',(-65.5449962514661,-24.787513182749,12.));
#80412=CARTESIAN_POINT('Ctrl Pts',(-65.5609353062829,-24.799025856126,0.));
#80413=CARTESIAN_POINT('Ctrl Pts',(-65.5609353062829,-24.799025856126,12.));
#80414=CARTESIAN_POINT('Ctrl Pts',(-65.5769057914333,-24.8105873098626,
0.));
#80415=CARTESIAN_POINT('Ctrl Pts',(-65.5769057914333,-24.8105873098626,
12.));
#80416=CARTESIAN_POINT('Ctrl Pts',(-65.5929074932624,-24.8221975032104,
0.));
#80417=CARTESIAN_POINT('Ctrl Pts',(-65.5929074932624,-24.8221975032104,
12.));
#80418=CARTESIAN_POINT('Ctrl Pts',(-65.6089401625628,-24.8338563866764,
0.));
#80419=CARTESIAN_POINT('Ctrl Pts',(-65.6089401625628,-24.8338563866764,
12.));
#80420=CARTESIAN_POINT('Ctrl Pts',(-65.6250035361612,-24.8455639071517,
0.));
#80421=CARTESIAN_POINT('Ctrl Pts',(-65.6250035361612,-24.8455639071517,
12.));
#80422=CARTESIAN_POINT('Ctrl Pts',(-65.6410973603661,-24.8573200135666,
0.));
#80423=CARTESIAN_POINT('Ctrl Pts',(-65.6410973603661,-24.8573200135666,
12.));
#80424=CARTESIAN_POINT('Ctrl Pts',(-65.6572214156692,-24.8691246628057,
0.));
#80425=CARTESIAN_POINT('Ctrl Pts',(-65.6572214156692,-24.8691246628057,
12.));
#80426=CARTESIAN_POINT('Ctrl Pts',(-65.6733755087669,-24.8809778178229,
0.));
#80427=CARTESIAN_POINT('Ctrl Pts',(-65.6733755087669,-24.8809778178229,
12.));
#80428=CARTESIAN_POINT('Ctrl Pts',(-65.6895594608775,-24.8928794448607,
0.));
#80429=CARTESIAN_POINT('Ctrl Pts',(-65.6895594608775,-24.8928794448607,
12.));
#80430=CARTESIAN_POINT('Ctrl Pts',(-65.7057730980483,-24.9048295111448,
0.));
#80431=CARTESIAN_POINT('Ctrl Pts',(-65.7057730980483,-24.9048295111448,
12.));
#80432=CARTESIAN_POINT('Ctrl Pts',(-65.7220162391054,-24.9168279820106,
0.));
#80433=CARTESIAN_POINT('Ctrl Pts',(-65.7220162391054,-24.9168279820106,
12.));
#80434=CARTESIAN_POINT('Ctrl Pts',(-65.7382886895888,-24.928874819458,0.));
#80435=CARTESIAN_POINT('Ctrl Pts',(-65.7382886895888,-24.928874819458,12.));
#80436=CARTESIAN_POINT('Ctrl Pts',(-65.7545902480323,-24.9409699836537,
0.));
#80437=CARTESIAN_POINT('Ctrl Pts',(-65.7545902480323,-24.9409699836537,
12.));
#80438=CARTESIAN_POINT('Ctrl Pts',(-65.7709207098959,-24.9531134338696,
0.));
#80439=CARTESIAN_POINT('Ctrl Pts',(-65.7709207098959,-24.9531134338696,
12.));
#80440=CARTESIAN_POINT('Ctrl Pts',(-65.7872798720823,-24.9653051295581,
0.));
#80441=CARTESIAN_POINT('Ctrl Pts',(-65.7872798720823,-24.9653051295581,
12.));
#80442=CARTESIAN_POINT('Ctrl Pts',(-65.8036675380718,-24.9775450315682,
0.));
#80443=CARTESIAN_POINT('Ctrl Pts',(-65.8036675380718,-24.9775450315682,
12.));
#80444=CARTESIAN_POINT('Ctrl Pts',(-65.8200835177024,-24.9898331020983,
0.));
#80445=CARTESIAN_POINT('Ctrl Pts',(-65.8200835177024,-24.9898331020983,
12.));
#80446=CARTESIAN_POINT('Ctrl Pts',(-65.8365276247128,-25.002169304117,0.));
#80447=CARTESIAN_POINT('Ctrl Pts',(-65.8365276247128,-25.002169304117,12.));
#80448=CARTESIAN_POINT('Ctrl Pts',(-65.8529996750445,-25.0145536009604,
0.));
#80449=CARTESIAN_POINT('Ctrl Pts',(-65.8529996750445,-25.0145536009604,
12.));
#80450=CARTESIAN_POINT('Ctrl Pts',(-65.8694994847616,-25.0269859558362,
0.));
#80451=CARTESIAN_POINT('Ctrl Pts',(-65.8694994847616,-25.0269859558362,
12.));
#80452=CARTESIAN_POINT('Ctrl Pts',(-65.8860268683128,-25.0394663314055,
0.));
#80453=CARTESIAN_POINT('Ctrl Pts',(-65.8860268683128,-25.0394663314055,
12.));
#80454=CARTESIAN_POINT('Ctrl Pts',(-65.9025816394424,-25.0519946900078,
0.));
#80455=CARTESIAN_POINT('Ctrl Pts',(-65.9025816394424,-25.0519946900078,
12.));
#80456=CARTESIAN_POINT('Ctrl Pts',(-65.919163611981,-25.0645709938524,0.));
#80457=CARTESIAN_POINT('Ctrl Pts',(-65.919163611981,-25.0645709938524,12.));
#80458=CARTESIAN_POINT('Ctrl Pts',(-65.9357726006163,-25.0771952052028,
0.));
#80459=CARTESIAN_POINT('Ctrl Pts',(-65.9357726006163,-25.0771952052028,
12.));
#80460=CARTESIAN_POINT('Ctrl Pts',(-65.9524084218139,-25.0898672865915,
0.));
#80461=CARTESIAN_POINT('Ctrl Pts',(-65.9524084218139,-25.0898672865915,
12.));
#80462=CARTESIAN_POINT('Ctrl Pts',(-65.9690708941558,-25.1025872009004,
0.));
#80463=CARTESIAN_POINT('Ctrl Pts',(-65.9690708941558,-25.1025872009004,
12.));
#80464=CARTESIAN_POINT('Ctrl Pts',(-65.9857598378433,-25.1153549112503,
0.));
#80465=CARTESIAN_POINT('Ctrl Pts',(-65.9857598378433,-25.1153549112503,
12.));
#80466=CARTESIAN_POINT('Ctrl Pts',(-66.0024750743897,-25.1281703809297,
0.));
#80467=CARTESIAN_POINT('Ctrl Pts',(-66.0024750743897,-25.1281703809297,
12.));
#80468=CARTESIAN_POINT('Ctrl Pts',(-66.0192164262621,-25.1410335733099,
0.));
#80469=CARTESIAN_POINT('Ctrl Pts',(-66.0192164262621,-25.1410335733099,
12.));
#80470=CARTESIAN_POINT('Ctrl Pts',(-66.0359837164734,-25.1539444517419,
0.));
#80471=CARTESIAN_POINT('Ctrl Pts',(-66.0359837164734,-25.1539444517419,
12.));
#80472=CARTESIAN_POINT('Ctrl Pts',(-66.0527767686025,-25.1669029795661,
0.));
#80473=CARTESIAN_POINT('Ctrl Pts',(-66.0527767686025,-25.1669029795661,
12.));
#80474=CARTESIAN_POINT('Ctrl Pts',(-66.0695954069713,-25.1799091201599,
0.));
#80475=CARTESIAN_POINT('Ctrl Pts',(-66.0695954069713,-25.1799091201599,
12.));
#80476=CARTESIAN_POINT('Ctrl Pts',(-66.086439456768,-25.1929628369685,0.));
#80477=CARTESIAN_POINT('Ctrl Pts',(-66.086439456768,-25.1929628369685,12.));
#80478=CARTESIAN_POINT('Ctrl Pts',(-66.10330874419,-25.2060640935365,0.));
#80479=CARTESIAN_POINT('Ctrl Pts',(-66.10330874419,-25.2060640935365,12.));
#80480=CARTESIAN_POINT('Ctrl Pts',(-66.1202030965758,-25.2192128535357,
0.));
#80481=CARTESIAN_POINT('Ctrl Pts',(-66.1202030965758,-25.2192128535357,
12.));
#80482=CARTESIAN_POINT('Ctrl Pts',(-66.1371223423345,-25.232409080755,0.));
#80483=CARTESIAN_POINT('Ctrl Pts',(-66.1371223423345,-25.232409080755,12.));
#80484=CARTESIAN_POINT('Ctrl Pts',(-66.1540663108754,-25.2456527390875,
0.));
#80485=CARTESIAN_POINT('Ctrl Pts',(-66.1540663108754,-25.2456527390875,
12.));
#80486=CARTESIAN_POINT('Ctrl Pts',(-66.1710348325384,-25.2589437925147,
0.));
#80487=CARTESIAN_POINT('Ctrl Pts',(-66.1710348325384,-25.2589437925147,
12.));
#80488=CARTESIAN_POINT('Ctrl Pts',(-66.1880277385136,-25.2722822050837,
0.));
#80489=CARTESIAN_POINT('Ctrl Pts',(-66.1880277385136,-25.2722822050837,
12.));
#80490=CARTESIAN_POINT('Ctrl Pts',(-66.2050448607911,-25.285667940893,0.));
#80491=CARTESIAN_POINT('Ctrl Pts',(-66.2050448607911,-25.285667940893,12.));
#80492=CARTESIAN_POINT('Ctrl Pts',(-66.2220860321952,-25.2991009641094,
0.));
#80493=CARTESIAN_POINT('Ctrl Pts',(-66.2220860321952,-25.2991009641094,
12.));
#80494=CARTESIAN_POINT('Ctrl Pts',(-66.2391510863998,-25.312581238973,0.));
#80495=CARTESIAN_POINT('Ctrl Pts',(-66.2391510863998,-25.312581238973,12.));
#80496=CARTESIAN_POINT('Ctrl Pts',(-66.2562398579471,-25.3261087298026,
0.));
#80497=CARTESIAN_POINT('Ctrl Pts',(-66.2562398579471,-25.3261087298026,
12.));
#80498=CARTESIAN_POINT('Ctrl Pts',(-66.2733521822662,-25.3396834009949,
0.));
#80499=CARTESIAN_POINT('Ctrl Pts',(-66.2733521822662,-25.3396834009949,
12.));
#80500=CARTESIAN_POINT('Ctrl Pts',(-66.290487895671,-25.3533052170249,0.));
#80501=CARTESIAN_POINT('Ctrl Pts',(-66.290487895671,-25.3533052170249,12.));
#80502=CARTESIAN_POINT('Ctrl Pts',(-66.3076468353412,-25.3669741424488,
0.));
#80503=CARTESIAN_POINT('Ctrl Pts',(-66.3076468353412,-25.3669741424488,
12.));
#80504=CARTESIAN_POINT('Ctrl Pts',(-66.3248288393046,-25.3806901419012,
0.));
#80505=CARTESIAN_POINT('Ctrl Pts',(-66.3248288393046,-25.3806901419012,
12.));
#80506=CARTESIAN_POINT('Ctrl Pts',(-66.3420337464178,-25.3944531800901,
0.));
#80507=CARTESIAN_POINT('Ctrl Pts',(-66.3420337464178,-25.3944531800901,
12.));
#80508=CARTESIAN_POINT('Ctrl Pts',(-66.359261396341,-25.4082632217847,0.));
#80509=CARTESIAN_POINT('Ctrl Pts',(-66.359261396341,-25.4082632217847,12.));
#80510=CARTESIAN_POINT('Ctrl Pts',(-66.3765116295364,-25.4221202318199,
0.));
#80511=CARTESIAN_POINT('Ctrl Pts',(-66.3765116295364,-25.4221202318199,
12.));
#80512=CARTESIAN_POINT('Ctrl Pts',(-66.3937842872685,-25.4360241751018,
0.));
#80513=CARTESIAN_POINT('Ctrl Pts',(-66.3937842872685,-25.4360241751018,
12.));
#80514=CARTESIAN_POINT('Ctrl Pts',(-66.4110792116,-25.4499750166079,0.));
#80515=CARTESIAN_POINT('Ctrl Pts',(-66.4110792116,-25.4499750166079,12.));
#80516=CARTESIAN_POINT('Ctrl Pts',(-66.4283962453899,-25.4639727213849,
0.));
#80517=CARTESIAN_POINT('Ctrl Pts',(-66.4283962453899,-25.4639727213849,
12.));
#80518=CARTESIAN_POINT('Ctrl Pts',(-66.4457352322871,-25.4780172545417,
0.));
#80519=CARTESIAN_POINT('Ctrl Pts',(-66.4457352322871,-25.4780172545417,
12.));
#80520=CARTESIAN_POINT('Ctrl Pts',(-66.4630960167252,-25.4921085812547,
0.));
#80521=CARTESIAN_POINT('Ctrl Pts',(-66.4630960167252,-25.4921085812547,
12.));
#80522=CARTESIAN_POINT('Ctrl Pts',(-66.4804784439148,-25.5062466667702,
0.));
#80523=CARTESIAN_POINT('Ctrl Pts',(-66.4804784439148,-25.5062466667702,
12.));
#80524=CARTESIAN_POINT('Ctrl Pts',(-66.4978823598354,-25.5204314764033,
0.));
#80525=CARTESIAN_POINT('Ctrl Pts',(-66.4978823598354,-25.5204314764033,
12.));
#80526=CARTESIAN_POINT('Ctrl Pts',(-66.5153076112231,-25.534662975532,0.));
#80527=CARTESIAN_POINT('Ctrl Pts',(-66.5153076112231,-25.534662975532,12.));
#80528=CARTESIAN_POINT('Ctrl Pts',(-66.5327540455624,-25.5489411295912,
0.));
#80529=CARTESIAN_POINT('Ctrl Pts',(-66.5327540455624,-25.5489411295912,
12.));
#80530=CARTESIAN_POINT('Ctrl Pts',(-66.5502215110829,-25.5632659040792,
0.));
#80531=CARTESIAN_POINT('Ctrl Pts',(-66.5502215110829,-25.5632659040792,
12.));
#80532=CARTESIAN_POINT('Ctrl Pts',(-66.5677098567542,-25.5776372645601,
0.));
#80533=CARTESIAN_POINT('Ctrl Pts',(-66.5677098567542,-25.5776372645601,
12.));
#80534=CARTESIAN_POINT('Ctrl Pts',(-66.5852189322813,-25.5920551766629,
0.));
#80535=CARTESIAN_POINT('Ctrl Pts',(-66.5852189322813,-25.5920551766629,
12.));
#80536=CARTESIAN_POINT('Ctrl Pts',(-66.6027485880963,-25.6065196060756,
0.));
#80537=CARTESIAN_POINT('Ctrl Pts',(-66.6027485880963,-25.6065196060756,
12.));
#80538=CARTESIAN_POINT('Ctrl Pts',(-66.6202986753506,-25.6210305185403,
0.));
#80539=CARTESIAN_POINT('Ctrl Pts',(-66.6202986753506,-25.6210305185403,
12.));
#80540=CARTESIAN_POINT('Ctrl Pts',(-66.6378690459129,-25.6355878798614,
0.));
#80541=CARTESIAN_POINT('Ctrl Pts',(-66.6378690459129,-25.6355878798614,
12.));
#80542=CARTESIAN_POINT('Ctrl Pts',(-66.6554595523624,-25.6501916559055,
0.));
#80543=CARTESIAN_POINT('Ctrl Pts',(-66.6554595523624,-25.6501916559055,
12.));
#80544=CARTESIAN_POINT('Ctrl Pts',(-66.6730700479837,-25.6648418126013,
0.));
#80545=CARTESIAN_POINT('Ctrl Pts',(-66.6730700479837,-25.6648418126013,
12.));
#80546=CARTESIAN_POINT('Ctrl Pts',(-66.6907003867572,-25.6795383159319,
0.));
#80547=CARTESIAN_POINT('Ctrl Pts',(-66.6907003867572,-25.6795383159319,
12.));
#80548=CARTESIAN_POINT('Ctrl Pts',(-66.7083504233529,-25.6942811319322,
0.));
#80549=CARTESIAN_POINT('Ctrl Pts',(-66.7083504233529,-25.6942811319322,
12.));
#80550=CARTESIAN_POINT('Ctrl Pts',(-66.7260200131266,-25.7090702266963,
0.));
#80551=CARTESIAN_POINT('Ctrl Pts',(-66.7260200131266,-25.7090702266963,
12.));
#80552=CARTESIAN_POINT('Ctrl Pts',(-66.7437090121153,-25.7239055663772,
0.));
#80553=CARTESIAN_POINT('Ctrl Pts',(-66.7437090121153,-25.7239055663772,
12.));
#80554=CARTESIAN_POINT('Ctrl Pts',(-66.7614172770316,-25.7387871171866,
0.));
#80555=CARTESIAN_POINT('Ctrl Pts',(-66.7614172770316,-25.7387871171866,
12.));
#80556=CARTESIAN_POINT('Ctrl Pts',(-66.7791446652545,-25.7537148453864,
0.));
#80557=CARTESIAN_POINT('Ctrl Pts',(-66.7791446652545,-25.7537148453864,
12.));
#80558=CARTESIAN_POINT('Ctrl Pts',(-66.7968910348245,-25.7686887172878,
0.));
#80559=CARTESIAN_POINT('Ctrl Pts',(-66.7968910348245,-25.7686887172878,
12.));
#80560=CARTESIAN_POINT('Ctrl Pts',(-66.8146562444433,-25.7837086992595,
0.));
#80561=CARTESIAN_POINT('Ctrl Pts',(-66.8146562444433,-25.7837086992595,
12.));
#80562=CARTESIAN_POINT('Ctrl Pts',(-66.8324401534668,-25.7987747577269,
0.));
#80563=CARTESIAN_POINT('Ctrl Pts',(-66.8324401534668,-25.7987747577269,
12.));
#80564=CARTESIAN_POINT('Ctrl Pts',(-66.8502426219001,-25.8138868591709,
0.));
#80565=CARTESIAN_POINT('Ctrl Pts',(-66.8502426219001,-25.8138868591709,
12.));
#80566=CARTESIAN_POINT('Ctrl Pts',(-66.8680635103876,-25.8290449701193,
0.));
#80567=CARTESIAN_POINT('Ctrl Pts',(-66.8680635103876,-25.8290449701193,
12.));
#80568=CARTESIAN_POINT('Ctrl Pts',(-66.8859026802088,-25.844249057147,0.));
#80569=CARTESIAN_POINT('Ctrl Pts',(-66.8859026802088,-25.844249057147,12.));
#80570=CARTESIAN_POINT('Ctrl Pts',(-66.9037599932761,-25.8594990868833,
0.));
#80571=CARTESIAN_POINT('Ctrl Pts',(-66.9037599932761,-25.8594990868833,
12.));
#80572=CARTESIAN_POINT('Ctrl Pts',(-66.92163531213,-25.8747950260111,0.));
#80573=CARTESIAN_POINT('Ctrl Pts',(-66.92163531213,-25.8747950260111,12.));
#80574=CARTESIAN_POINT('Ctrl Pts',(-66.939528499934,-25.890136841266,0.));
#80575=CARTESIAN_POINT('Ctrl Pts',(-66.939528499934,-25.890136841266,12.));
#80576=CARTESIAN_POINT('Ctrl Pts',(-66.9574394204663,-25.9055244994277,
0.));
#80577=CARTESIAN_POINT('Ctrl Pts',(-66.9574394204663,-25.9055244994277,
12.));
#80578=CARTESIAN_POINT('Ctrl Pts',(-66.975367938115,-25.9209579673209,0.));
#80579=CARTESIAN_POINT('Ctrl Pts',(-66.975367938115,-25.9209579673209,12.));
#80580=CARTESIAN_POINT('Ctrl Pts',(-66.9933139178778,-25.9364372118222,
0.));
#80581=CARTESIAN_POINT('Ctrl Pts',(-66.9933139178778,-25.9364372118222,
12.));
#80582=CARTESIAN_POINT('Ctrl Pts',(-67.0112772253556,-25.9519621998598,
0.));
#80583=CARTESIAN_POINT('Ctrl Pts',(-67.0112772253556,-25.9519621998598,
12.));
#80584=CARTESIAN_POINT('Ctrl Pts',(-67.0292577267489,-25.967532898412,0.));
#80585=CARTESIAN_POINT('Ctrl Pts',(-67.0292577267489,-25.967532898412,12.));
#80586=CARTESIAN_POINT('Ctrl Pts',(-67.0472552888485,-25.9831492744984,
0.));
#80587=CARTESIAN_POINT('Ctrl Pts',(-67.0472552888485,-25.9831492744984,
12.));
#80588=CARTESIAN_POINT('Ctrl Pts',(-67.0652697790325,-25.9988112951814,
0.));
#80589=CARTESIAN_POINT('Ctrl Pts',(-67.0652697790325,-25.9988112951814,
12.));
#80590=CARTESIAN_POINT('Ctrl Pts',(-67.0833010652634,-26.014518927573,0.));
#80591=CARTESIAN_POINT('Ctrl Pts',(-67.0833010652634,-26.014518927573,12.));
#80592=CARTESIAN_POINT('Ctrl Pts',(-67.101349016084,-26.030272138834,0.));
#80593=CARTESIAN_POINT('Ctrl Pts',(-67.101349016084,-26.030272138834,12.));
#80594=CARTESIAN_POINT('Ctrl Pts',(-67.1194135006124,-26.0460708961725,
0.));
#80595=CARTESIAN_POINT('Ctrl Pts',(-67.1194135006124,-26.0460708961725,
12.));
#80596=CARTESIAN_POINT('Ctrl Pts',(-67.1374943885354,-26.061915166836,0.));
#80597=CARTESIAN_POINT('Ctrl Pts',(-67.1374943885354,-26.061915166836,12.));
#80598=CARTESIAN_POINT('Ctrl Pts',(-67.1555915501049,-26.0778049181128,
0.));
#80599=CARTESIAN_POINT('Ctrl Pts',(-67.1555915501049,-26.0778049181128,
12.));
#80600=CARTESIAN_POINT('Ctrl Pts',(-67.173704856136,-26.0937401173383,0.));
#80601=CARTESIAN_POINT('Ctrl Pts',(-67.173704856136,-26.0937401173383,12.));
#80602=CARTESIAN_POINT('Ctrl Pts',(-67.1918341780018,-26.1097207318949,
0.));
#80603=CARTESIAN_POINT('Ctrl Pts',(-67.1918341780018,-26.1097207318949,
12.));
#80604=CARTESIAN_POINT('Ctrl Pts',(-67.2099793876297,-26.1257467292102,
0.));
#80605=CARTESIAN_POINT('Ctrl Pts',(-67.2099793876297,-26.1257467292102,
12.));
#80606=CARTESIAN_POINT('Ctrl Pts',(-67.2281403574938,-26.1418180767489,
0.));
#80607=CARTESIAN_POINT('Ctrl Pts',(-67.2281403574938,-26.1418180767489,
12.));
#80608=CARTESIAN_POINT('Ctrl Pts',(-67.2463169606115,-26.1579347420138,
0.));
#80609=CARTESIAN_POINT('Ctrl Pts',(-67.2463169606115,-26.1579347420138,
12.));
#80610=CARTESIAN_POINT('Ctrl Pts',(-67.2645090705421,-26.1740966925529,
0.));
#80611=CARTESIAN_POINT('Ctrl Pts',(-67.2645090705421,-26.1740966925529,
12.));
#80612=CARTESIAN_POINT('Ctrl Pts',(-67.282716561383,-26.1903038959589,0.));
#80613=CARTESIAN_POINT('Ctrl Pts',(-67.282716561383,-26.1903038959589,12.));
#80614=CARTESIAN_POINT('Ctrl Pts',(-67.3009393077651,-26.2065563198683,
0.));
#80615=CARTESIAN_POINT('Ctrl Pts',(-67.3009393077651,-26.2065563198683,
12.));
#80616=CARTESIAN_POINT('Ctrl Pts',(-67.3191771848463,-26.2228539319526,
0.));
#80617=CARTESIAN_POINT('Ctrl Pts',(-67.3191771848463,-26.2228539319526,
12.));
#80618=CARTESIAN_POINT('Ctrl Pts',(-67.3374300683073,-26.2391966999191,
0.));
#80619=CARTESIAN_POINT('Ctrl Pts',(-67.3374300683073,-26.2391966999191,
12.));
#80620=CARTESIAN_POINT('Ctrl Pts',(-67.3556978343507,-26.255584591518,0.));
#80621=CARTESIAN_POINT('Ctrl Pts',(-67.3556978343507,-26.255584591518,12.));
#80622=CARTESIAN_POINT('Ctrl Pts',(-67.3739803596969,-26.2720175745423,
0.));
#80623=CARTESIAN_POINT('Ctrl Pts',(-67.3739803596969,-26.2720175745423,
12.));
#80624=CARTESIAN_POINT('Ctrl Pts',(-67.392277521581,-26.288495616827,0.));
#80625=CARTESIAN_POINT('Ctrl Pts',(-67.392277521581,-26.288495616827,12.));
#80626=CARTESIAN_POINT('Ctrl Pts',(-67.4105891977461,-26.3050186862407,
0.));
#80627=CARTESIAN_POINT('Ctrl Pts',(-67.4105891977461,-26.3050186862407,
12.));
#80628=CARTESIAN_POINT('Ctrl Pts',(-67.4289152664398,-26.321586750686,0.));
#80629=CARTESIAN_POINT('Ctrl Pts',(-67.4289152664398,-26.321586750686,12.));
#80630=CARTESIAN_POINT('Ctrl Pts',(-67.4472556064119,-26.3381997781055,
0.));
#80631=CARTESIAN_POINT('Ctrl Pts',(-67.4472556064119,-26.3381997781055,
12.));
#80632=CARTESIAN_POINT('Ctrl Pts',(-67.4656100969116,-26.3548577364833,
0.));
#80633=CARTESIAN_POINT('Ctrl Pts',(-67.4656100969116,-26.3548577364833,
12.));
#80634=CARTESIAN_POINT('Ctrl Pts',(-67.4839786176836,-26.3715605938433,
0.));
#80635=CARTESIAN_POINT('Ctrl Pts',(-67.4839786176836,-26.3715605938433,
12.));
#80636=CARTESIAN_POINT('Ctrl Pts',(-67.5023610489622,-26.3883083182421,
0.));
#80637=CARTESIAN_POINT('Ctrl Pts',(-67.5023610489622,-26.3883083182421,
12.));
#80638=CARTESIAN_POINT('Ctrl Pts',(-67.5207572714683,-26.4051008777675,
0.));
#80639=CARTESIAN_POINT('Ctrl Pts',(-67.5207572714683,-26.4051008777675,
12.));
#80640=CARTESIAN_POINT('Ctrl Pts',(-67.5391671664072,-26.4219382405458,
0.));
#80641=CARTESIAN_POINT('Ctrl Pts',(-67.5391671664072,-26.4219382405458,
12.));
#80642=CARTESIAN_POINT('Ctrl Pts',(-67.5575906154657,-26.4388203747425,
0.));
#80643=CARTESIAN_POINT('Ctrl Pts',(-67.5575906154657,-26.4388203747425,
12.));
#80644=CARTESIAN_POINT('Ctrl Pts',(-67.5760275008093,-26.4557472485621,
0.));
#80645=CARTESIAN_POINT('Ctrl Pts',(-67.5760275008093,-26.4557472485621,
12.));
#80646=CARTESIAN_POINT('Ctrl Pts',(-67.5944777050768,-26.4727188302409,
0.));
#80647=CARTESIAN_POINT('Ctrl Pts',(-67.5944777050768,-26.4727188302409,
12.));
#80648=CARTESIAN_POINT('Ctrl Pts',(-67.6129411113757,-26.489735088044,0.));
#80649=CARTESIAN_POINT('Ctrl Pts',(-67.6129411113757,-26.489735088044,12.));
#80650=CARTESIAN_POINT('Ctrl Pts',(-67.6314176032811,-26.5067959902725,
0.));
#80651=CARTESIAN_POINT('Ctrl Pts',(-67.6314176032811,-26.5067959902725,
12.));
#80652=CARTESIAN_POINT('Ctrl Pts',(-67.649907064832,-26.5239015052654,0.));
#80653=CARTESIAN_POINT('Ctrl Pts',(-67.649907064832,-26.5239015052654,12.));
#80654=CARTESIAN_POINT('Ctrl Pts',(-67.6684093805291,-26.5410516013985,
0.));
#80655=CARTESIAN_POINT('Ctrl Pts',(-67.6684093805291,-26.5410516013985,
12.));
#80656=CARTESIAN_POINT('Ctrl Pts',(-67.6869244353294,-26.5582462470794,
0.));
#80657=CARTESIAN_POINT('Ctrl Pts',(-67.6869244353294,-26.5582462470794,
12.));
#80658=CARTESIAN_POINT('Ctrl Pts',(-67.7054521146424,-26.5754854107421,
0.));
#80659=CARTESIAN_POINT('Ctrl Pts',(-67.7054521146424,-26.5754854107421,
12.));
#80660=CARTESIAN_POINT('Ctrl Pts',(-67.7239923043288,-26.5927690608544,
0.));
#80661=CARTESIAN_POINT('Ctrl Pts',(-67.7239923043288,-26.5927690608544,
12.));
#80662=CARTESIAN_POINT('Ctrl Pts',(-67.7425448906977,-26.6100971659202,
0.));
#80663=CARTESIAN_POINT('Ctrl Pts',(-67.7425448906977,-26.6100971659202,
12.));
#80664=CARTESIAN_POINT('Ctrl Pts',(-67.7611097605042,-26.6274696944793,
0.));
#80665=CARTESIAN_POINT('Ctrl Pts',(-67.7611097605042,-26.6274696944793,
12.));
#80666=CARTESIAN_POINT('Ctrl Pts',(-67.7796868009455,-26.6448866151029,
0.));
#80667=CARTESIAN_POINT('Ctrl Pts',(-67.7796868009455,-26.6448866151029,
12.));
#80668=CARTESIAN_POINT('Ctrl Pts',(-67.798275899657,-26.6623478963871,0.));
#80669=CARTESIAN_POINT('Ctrl Pts',(-67.798275899657,-26.6623478963871,12.));
#80670=CARTESIAN_POINT('Ctrl Pts',(-67.8168769447098,-26.6798535069589,
0.));
#80671=CARTESIAN_POINT('Ctrl Pts',(-67.8168769447098,-26.6798535069589,
12.));
#80672=CARTESIAN_POINT('Ctrl Pts',(-67.8354898246086,-26.6974034154804,
0.));
#80673=CARTESIAN_POINT('Ctrl Pts',(-67.8354898246086,-26.6974034154804,
12.));
#80674=CARTESIAN_POINT('Ctrl Pts',(-67.8541144282875,-26.7149975906478,
0.));
#80675=CARTESIAN_POINT('Ctrl Pts',(-67.8541144282875,-26.7149975906478,
12.));
#80676=CARTESIAN_POINT('Ctrl Pts',(-67.8727506451063,-26.7326360011885,
0.));
#80677=CARTESIAN_POINT('Ctrl Pts',(-67.8727506451063,-26.7326360011885,
12.));
#80678=CARTESIAN_POINT('Ctrl Pts',(-67.8913983648436,-26.7503186158522,
0.));
#80679=CARTESIAN_POINT('Ctrl Pts',(-67.8913983648436,-26.7503186158522,
12.));
#80680=CARTESIAN_POINT('Ctrl Pts',(-67.9100574776972,-26.7680454034169,
0.));
#80681=CARTESIAN_POINT('Ctrl Pts',(-67.9100574776972,-26.7680454034169,
12.));
#80682=CARTESIAN_POINT('Ctrl Pts',(-67.928727874284,-26.7858163326934,0.));
#80683=CARTESIAN_POINT('Ctrl Pts',(-67.928727874284,-26.7858163326934,12.));
#80684=CARTESIAN_POINT('Ctrl Pts',(-67.9474094456396,-26.8036313725262,
0.));
#80685=CARTESIAN_POINT('Ctrl Pts',(-67.9474094456396,-26.8036313725262,
12.));
#80686=CARTESIAN_POINT('Ctrl Pts',(-67.9661020832164,-26.821490491792,0.));
#80687=CARTESIAN_POINT('Ctrl Pts',(-67.9661020832164,-26.821490491792,12.));
#80688=CARTESIAN_POINT('Ctrl Pts',(-67.9848056788809,-26.8393936593911,
0.));
#80689=CARTESIAN_POINT('Ctrl Pts',(-67.9848056788809,-26.8393936593911,
12.));
#80690=CARTESIAN_POINT('Ctrl Pts',(-68.0035201249102,-26.8573408442496,
0.));
#80691=CARTESIAN_POINT('Ctrl Pts',(-68.0035201249102,-26.8573408442496,
12.));
#80692=CARTESIAN_POINT('Ctrl Pts',(-68.0222453139856,-26.8753320153252,
0.));
#80693=CARTESIAN_POINT('Ctrl Pts',(-68.0222453139856,-26.8753320153252,
12.));
#80694=CARTESIAN_POINT('Ctrl Pts',(-68.0409811391869,-26.8933671416063,
0.));
#80695=CARTESIAN_POINT('Ctrl Pts',(-68.0409811391869,-26.8933671416063,
12.));
#80696=CARTESIAN_POINT('Ctrl Pts',(-68.0597274939859,-26.911446192111,0.));
#80697=CARTESIAN_POINT('Ctrl Pts',(-68.0597274939859,-26.911446192111,12.));
#80698=CARTESIAN_POINT('Ctrl Pts',(-68.0784842722369,-26.9295691358779,
0.));
#80699=CARTESIAN_POINT('Ctrl Pts',(-68.0784842722369,-26.9295691358779,
12.));
#80700=CARTESIAN_POINT('Ctrl Pts',(-68.0972513681751,-26.9477359419652,
0.));
#80701=CARTESIAN_POINT('Ctrl Pts',(-68.0972513681751,-26.9477359419652,
12.));
#80702=CARTESIAN_POINT('Ctrl Pts',(-68.1160286764255,-26.9659465794601,
0.));
#80703=CARTESIAN_POINT('Ctrl Pts',(-68.1160286764255,-26.9659465794601,
12.));
#80704=CARTESIAN_POINT('Ctrl Pts',(-68.1348160920106,-26.9842010174822,
0.));
#80705=CARTESIAN_POINT('Ctrl Pts',(-68.1348160920106,-26.9842010174822,
12.));
#80706=CARTESIAN_POINT('Ctrl Pts',(-68.1536135103557,-27.0024992251838,
0.));
#80707=CARTESIAN_POINT('Ctrl Pts',(-68.1536135103557,-27.0024992251838,
12.));
#80708=CARTESIAN_POINT('Ctrl Pts',(-68.1724208272958,-27.0208411717472,
0.));
#80709=CARTESIAN_POINT('Ctrl Pts',(-68.1724208272958,-27.0208411717472,
12.));
#80710=CARTESIAN_POINT('Ctrl Pts',(-68.1912379390773,-27.0392268263798,
0.));
#80711=CARTESIAN_POINT('Ctrl Pts',(-68.1912379390773,-27.0392268263798,
12.));
#80712=CARTESIAN_POINT('Ctrl Pts',(-68.2100647423332,-27.0576561583172,
0.));
#80713=CARTESIAN_POINT('Ctrl Pts',(-68.2100647423332,-27.0576561583172,
12.));
#80714=CARTESIAN_POINT('Ctrl Pts',(-68.2289011340615,-27.0761291368226,
0.));
#80715=CARTESIAN_POINT('Ctrl Pts',(-68.2289011340615,-27.0761291368226,
12.));
#80716=CARTESIAN_POINT('Ctrl Pts',(-68.2477470116012,-27.0946457311813,
0.));
#80717=CARTESIAN_POINT('Ctrl Pts',(-68.2477470116012,-27.0946457311813,
12.));
#80718=CARTESIAN_POINT('Ctrl Pts',(-68.2666022726104,-27.1132059106943,
0.));
#80719=CARTESIAN_POINT('Ctrl Pts',(-68.2666022726104,-27.1132059106943,
12.));
#80720=CARTESIAN_POINT('Ctrl Pts',(-68.2854668150364,-27.1318096446649,
0.));
#80721=CARTESIAN_POINT('Ctrl Pts',(-68.2854668150364,-27.1318096446649,
12.));
#80722=CARTESIAN_POINT('Ctrl Pts',(-68.3043405371603,-27.1504569024136,
0.));
#80723=CARTESIAN_POINT('Ctrl Pts',(-68.3043405371603,-27.1504569024136,
12.));
#80724=CARTESIAN_POINT('Ctrl Pts',(-68.3232233376425,-27.1691476532921,
0.));
#80725=CARTESIAN_POINT('Ctrl Pts',(-68.3232233376425,-27.1691476532921,
12.));
#80726=CARTESIAN_POINT('Ctrl Pts',(-68.3421151155711,-27.1878818666926,
0.));
#80727=CARTESIAN_POINT('Ctrl Pts',(-68.3421151155711,-27.1878818666926,
12.));
#80728=CARTESIAN_POINT('Ctrl Pts',(-68.3610157704994,-27.2066595120542,
0.));
#80729=CARTESIAN_POINT('Ctrl Pts',(-68.3610157704994,-27.2066595120542,
12.));
#80730=CARTESIAN_POINT('Ctrl Pts',(-68.3799252025102,-27.2254805588673,
0.));
#80731=CARTESIAN_POINT('Ctrl Pts',(-68.3799252025102,-27.2254805588673,
12.));
#80732=CARTESIAN_POINT('Ctrl Pts',(-68.3988433121581,-27.244344976665,0.));
#80733=CARTESIAN_POINT('Ctrl Pts',(-68.3988433121581,-27.244344976665,12.));
#80734=CARTESIAN_POINT('Ctrl Pts',(-68.4177700003465,-27.263252735006,0.));
#80735=CARTESIAN_POINT('Ctrl Pts',(-68.4177700003465,-27.263252735006,12.));
#80736=CARTESIAN_POINT('Ctrl Pts',(-68.4367051682164,-27.2822038034538,
0.));
#80737=CARTESIAN_POINT('Ctrl Pts',(-68.4367051682164,-27.2822038034538,
12.));
#80738=CARTESIAN_POINT('Ctrl Pts',(-68.4556487170441,-27.301198151557,0.));
#80739=CARTESIAN_POINT('Ctrl Pts',(-68.4556487170441,-27.301198151557,12.));
#80740=CARTESIAN_POINT('Ctrl Pts',(-68.4746005480997,-27.3202357488154,
0.));
#80741=CARTESIAN_POINT('Ctrl Pts',(-68.4746005480997,-27.3202357488154,
12.));
#80742=CARTESIAN_POINT('Ctrl Pts',(-68.4935605626372,-27.3393165646752,
0.));
#80743=CARTESIAN_POINT('Ctrl Pts',(-68.4935605626372,-27.3393165646752,
12.));
#80744=CARTESIAN_POINT('Ctrl Pts',(-68.5125286621902,-27.3584405685947,
0.));
#80745=CARTESIAN_POINT('Ctrl Pts',(-68.5125286621902,-27.3584405685947,
12.));
#80746=CARTESIAN_POINT('Ctrl Pts',(-68.5315047488046,-27.3776077300918,
0.));
#80747=CARTESIAN_POINT('Ctrl Pts',(-68.5315047488046,-27.3776077300918,
12.));
#80748=CARTESIAN_POINT('Ctrl Pts',(-68.5504887252976,-27.3968180187941,
0.));
#80749=CARTESIAN_POINT('Ctrl Pts',(-68.5504887252976,-27.3968180187941,
12.));
#80750=CARTESIAN_POINT('Ctrl Pts',(-68.5694804955002,-27.4160714044825,
0.));
#80751=CARTESIAN_POINT('Ctrl Pts',(-68.5694804955002,-27.4160714044825,
12.));
#80752=CARTESIAN_POINT('Ctrl Pts',(-68.5884799645193,-27.4353678571349,
0.));
#80753=CARTESIAN_POINT('Ctrl Pts',(-68.5884799645193,-27.4353678571349,
12.));
#80754=CARTESIAN_POINT('Ctrl Pts',(-68.6074870381588,-27.4547073468213,
0.));
#80755=CARTESIAN_POINT('Ctrl Pts',(-68.6074870381588,-27.4547073468213,
12.));
#80756=CARTESIAN_POINT('Ctrl Pts',(-68.6265016223536,-27.4740898435977,
0.));
#80757=CARTESIAN_POINT('Ctrl Pts',(-68.6265016223536,-27.4740898435977,
12.));
#80758=CARTESIAN_POINT('Ctrl Pts',(-68.6455236225471,-27.4935153173863,
0.));
#80759=CARTESIAN_POINT('Ctrl Pts',(-68.6455236225471,-27.4935153173863,
12.));
#80760=CARTESIAN_POINT('Ctrl Pts',(-68.6645529432059,-27.5129837378797,
0.));
#80761=CARTESIAN_POINT('Ctrl Pts',(-68.6645529432059,-27.5129837378797,
12.));
#80762=CARTESIAN_POINT('Ctrl Pts',(-68.683589486992,-27.5324950743723,0.));
#80763=CARTESIAN_POINT('Ctrl Pts',(-68.683589486992,-27.5324950743723,12.));
#80764=CARTESIAN_POINT('Ctrl Pts',(-68.7026331554348,-27.552049295893,0.));
#80765=CARTESIAN_POINT('Ctrl Pts',(-68.7026331554348,-27.552049295893,12.));
#80766=CARTESIAN_POINT('Ctrl Pts',(-68.721683850427,-27.5716463715027,0.));
#80767=CARTESIAN_POINT('Ctrl Pts',(-68.721683850427,-27.5716463715027,12.));
#80768=CARTESIAN_POINT('Ctrl Pts',(-68.7407414755291,-27.5912862705482,
0.));
#80769=CARTESIAN_POINT('Ctrl Pts',(-68.7407414755291,-27.5912862705482,
12.));
#80770=CARTESIAN_POINT('Ctrl Pts',(-68.7598059372121,-27.6109689629025,
0.));
#80771=CARTESIAN_POINT('Ctrl Pts',(-68.7598059372121,-27.6109689629025,
12.));
#80772=CARTESIAN_POINT('Ctrl Pts',(-68.7788771464655,-27.6306944192711,
0.));
#80773=CARTESIAN_POINT('Ctrl Pts',(-68.7788771464655,-27.6306944192711,
12.));
#80774=CARTESIAN_POINT('Ctrl Pts',(-68.7979550191773,-27.6504626112621,
0.));
#80775=CARTESIAN_POINT('Ctrl Pts',(-68.7979550191773,-27.6504626112621,
12.));
#80776=CARTESIAN_POINT('Ctrl Pts',(-68.8170394725786,-27.670273510707,0.));
#80777=CARTESIAN_POINT('Ctrl Pts',(-68.8170394725786,-27.670273510707,12.));
#80778=CARTESIAN_POINT('Ctrl Pts',(-68.8361304224378,-27.6901270891201,
0.));
#80779=CARTESIAN_POINT('Ctrl Pts',(-68.8361304224378,-27.6901270891201,
12.));
#80780=CARTESIAN_POINT('Ctrl Pts',(-68.855227779818,-27.7100233170728,0.));
#80781=CARTESIAN_POINT('Ctrl Pts',(-68.855227779818,-27.7100233170728,12.));
#80782=CARTESIAN_POINT('Ctrl Pts',(-68.8743314483451,-27.7299621636602,
0.));
#80783=CARTESIAN_POINT('Ctrl Pts',(-68.8743314483451,-27.7299621636602,
12.));
#80784=CARTESIAN_POINT('Ctrl Pts',(-68.8934413203945,-27.7499435957608,
0.));
#80785=CARTESIAN_POINT('Ctrl Pts',(-68.8934413203945,-27.7499435957608,
12.));
#80786=CARTESIAN_POINT('Ctrl Pts',(-68.9125572825946,-27.7699675790683,
0.));
#80787=CARTESIAN_POINT('Ctrl Pts',(-68.9125572825946,-27.7699675790683,
12.));
#80788=CARTESIAN_POINT('Ctrl Pts',(-68.9316792226187,-27.7900340793796,
0.));
#80789=CARTESIAN_POINT('Ctrl Pts',(-68.9316792226187,-27.7900340793796,
12.));
#80790=CARTESIAN_POINT('Ctrl Pts',(-68.9508070357786,-27.8101430638128,
0.));
#80791=CARTESIAN_POINT('Ctrl Pts',(-68.9508070357786,-27.8101430638128,
12.));
#80792=CARTESIAN_POINT('Ctrl Pts',(-68.9699406311305,-27.8302945019939,
0.));
#80793=CARTESIAN_POINT('Ctrl Pts',(-68.9699406311305,-27.8302945019939,
12.));
#80794=CARTESIAN_POINT('Ctrl Pts',(-68.9890799391863,-27.8504883673903,
0.));
#80795=CARTESIAN_POINT('Ctrl Pts',(-68.9890799391863,-27.8504883673903,
12.));
#80796=CARTESIAN_POINT('Ctrl Pts',(-69.0082249138015,-27.8707246380697,
0.));
#80797=CARTESIAN_POINT('Ctrl Pts',(-69.0082249138015,-27.8707246380697,
12.));
#80798=CARTESIAN_POINT('Ctrl Pts',(-69.0273755264702,-27.8910032967037,
0.));
#80799=CARTESIAN_POINT('Ctrl Pts',(-69.0273755264702,-27.8910032967037,
12.));
#80800=CARTESIAN_POINT('Ctrl Pts',(-69.0427005153223,-27.9072601239469,
0.));
#80801=CARTESIAN_POINT('Ctrl Pts',(-69.0427005153223,-27.9072601239469,
12.));
#80802=CARTESIAN_POINT('Ctrl Pts',(-69.0541967850685,-27.9194718098851,
0.));
#80803=CARTESIAN_POINT('Ctrl Pts',(-69.0541967850685,-27.9194718098851,
12.));
#80804=CARTESIAN_POINT('Ctrl Pts',(-69.0618620884596,-27.9276214070576,
0.));
#80805=CARTESIAN_POINT('Ctrl Pts',(-69.0618620884596,-27.9276214070576,
12.));
#80806=CARTESIAN_POINT('Ctrl Pts',(-69.065695021045,-27.9316983239472,0.));
#80807=CARTESIAN_POINT('Ctrl Pts',(-69.065695021045,-27.9316983239472,12.));
#80808=CARTESIAN_POINT('',(-65.4815644032299,-24.7419628022042,0.));
#80809=CARTESIAN_POINT('Ctrl Pts',(-65.4815644032299,-24.7419628022042,
0.));
#80810=CARTESIAN_POINT('Ctrl Pts',(-65.4847237095443,-24.7442214063382,
0.));
#80811=CARTESIAN_POINT('Ctrl Pts',(-65.4910454936254,-24.7487434955982,
0.));
#80812=CARTESIAN_POINT('Ctrl Pts',(-65.5005376841101,-24.7555412724651,
0.));
#80813=CARTESIAN_POINT('Ctrl Pts',(-65.5132129675333,-24.7646342620841,
0.));
#80814=CARTESIAN_POINT('Ctrl Pts',(-65.5290887770232,-24.7760493148465,
0.));
#80815=CARTESIAN_POINT('Ctrl Pts',(-65.5449962514661,-24.787513182749,0.));
#80816=CARTESIAN_POINT('Ctrl Pts',(-65.5609353062829,-24.799025856126,0.));
#80817=CARTESIAN_POINT('Ctrl Pts',(-65.5769057914333,-24.8105873098626,
0.));
#80818=CARTESIAN_POINT('Ctrl Pts',(-65.5929074932624,-24.8221975032104,
0.));
#80819=CARTESIAN_POINT('Ctrl Pts',(-65.6089401625628,-24.8338563866764,
0.));
#80820=CARTESIAN_POINT('Ctrl Pts',(-65.6250035361612,-24.8455639071517,
0.));
#80821=CARTESIAN_POINT('Ctrl Pts',(-65.6410973603661,-24.8573200135666,
0.));
#80822=CARTESIAN_POINT('Ctrl Pts',(-65.6572214156692,-24.8691246628057,
0.));
#80823=CARTESIAN_POINT('Ctrl Pts',(-65.6733755087669,-24.8809778178229,
0.));
#80824=CARTESIAN_POINT('Ctrl Pts',(-65.6895594608775,-24.8928794448607,
0.));
#80825=CARTESIAN_POINT('Ctrl Pts',(-65.7057730980483,-24.9048295111448,
0.));
#80826=CARTESIAN_POINT('Ctrl Pts',(-65.7220162391054,-24.9168279820106,
0.));
#80827=CARTESIAN_POINT('Ctrl Pts',(-65.7382886895888,-24.928874819458,0.));
#80828=CARTESIAN_POINT('Ctrl Pts',(-65.7545902480323,-24.9409699836537,
0.));
#80829=CARTESIAN_POINT('Ctrl Pts',(-65.7709207098959,-24.9531134338696,
0.));
#80830=CARTESIAN_POINT('Ctrl Pts',(-65.7872798720823,-24.9653051295581,
0.));
#80831=CARTESIAN_POINT('Ctrl Pts',(-65.8036675380718,-24.9775450315682,
0.));
#80832=CARTESIAN_POINT('Ctrl Pts',(-65.8200835177024,-24.9898331020983,
0.));
#80833=CARTESIAN_POINT('Ctrl Pts',(-65.8365276247128,-25.002169304117,0.));
#80834=CARTESIAN_POINT('Ctrl Pts',(-65.8529996750445,-25.0145536009604,
0.));
#80835=CARTESIAN_POINT('Ctrl Pts',(-65.8694994847616,-25.0269859558362,
0.));
#80836=CARTESIAN_POINT('Ctrl Pts',(-65.8860268683128,-25.0394663314055,
0.));
#80837=CARTESIAN_POINT('Ctrl Pts',(-65.9025816394424,-25.0519946900078,
0.));
#80838=CARTESIAN_POINT('Ctrl Pts',(-65.919163611981,-25.0645709938524,0.));
#80839=CARTESIAN_POINT('Ctrl Pts',(-65.9357726006163,-25.0771952052028,
0.));
#80840=CARTESIAN_POINT('Ctrl Pts',(-65.9524084218139,-25.0898672865915,
0.));
#80841=CARTESIAN_POINT('Ctrl Pts',(-65.9690708941558,-25.1025872009004,
0.));
#80842=CARTESIAN_POINT('Ctrl Pts',(-65.9857598378433,-25.1153549112503,
0.));
#80843=CARTESIAN_POINT('Ctrl Pts',(-66.0024750743897,-25.1281703809297,
0.));
#80844=CARTESIAN_POINT('Ctrl Pts',(-66.0192164262621,-25.1410335733099,
0.));
#80845=CARTESIAN_POINT('Ctrl Pts',(-66.0359837164734,-25.1539444517419,
0.));
#80846=CARTESIAN_POINT('Ctrl Pts',(-66.0527767686025,-25.1669029795661,
0.));
#80847=CARTESIAN_POINT('Ctrl Pts',(-66.0695954069713,-25.1799091201599,
0.));
#80848=CARTESIAN_POINT('Ctrl Pts',(-66.086439456768,-25.1929628369685,0.));
#80849=CARTESIAN_POINT('Ctrl Pts',(-66.10330874419,-25.2060640935365,0.));
#80850=CARTESIAN_POINT('Ctrl Pts',(-66.1202030965758,-25.2192128535357,
0.));
#80851=CARTESIAN_POINT('Ctrl Pts',(-66.1371223423345,-25.232409080755,0.));
#80852=CARTESIAN_POINT('Ctrl Pts',(-66.1540663108754,-25.2456527390875,
0.));
#80853=CARTESIAN_POINT('Ctrl Pts',(-66.1710348325384,-25.2589437925147,
0.));
#80854=CARTESIAN_POINT('Ctrl Pts',(-66.1880277385136,-25.2722822050837,
0.));
#80855=CARTESIAN_POINT('Ctrl Pts',(-66.2050448607911,-25.285667940893,0.));
#80856=CARTESIAN_POINT('Ctrl Pts',(-66.2220860321952,-25.2991009641094,
0.));
#80857=CARTESIAN_POINT('Ctrl Pts',(-66.2391510863998,-25.312581238973,0.));
#80858=CARTESIAN_POINT('Ctrl Pts',(-66.2562398579471,-25.3261087298026,
0.));
#80859=CARTESIAN_POINT('Ctrl Pts',(-66.2733521822662,-25.3396834009949,
0.));
#80860=CARTESIAN_POINT('Ctrl Pts',(-66.290487895671,-25.3533052170249,0.));
#80861=CARTESIAN_POINT('Ctrl Pts',(-66.3076468353412,-25.3669741424488,
0.));
#80862=CARTESIAN_POINT('Ctrl Pts',(-66.3248288393046,-25.3806901419012,
0.));
#80863=CARTESIAN_POINT('Ctrl Pts',(-66.3420337464178,-25.3944531800901,
0.));
#80864=CARTESIAN_POINT('Ctrl Pts',(-66.359261396341,-25.4082632217847,0.));
#80865=CARTESIAN_POINT('Ctrl Pts',(-66.3765116295364,-25.4221202318199,
0.));
#80866=CARTESIAN_POINT('Ctrl Pts',(-66.3937842872685,-25.4360241751018,
0.));
#80867=CARTESIAN_POINT('Ctrl Pts',(-66.4110792116,-25.4499750166079,0.));
#80868=CARTESIAN_POINT('Ctrl Pts',(-66.4283962453899,-25.4639727213849,
0.));
#80869=CARTESIAN_POINT('Ctrl Pts',(-66.4457352322871,-25.4780172545417,
0.));
#80870=CARTESIAN_POINT('Ctrl Pts',(-66.4630960167252,-25.4921085812547,
0.));
#80871=CARTESIAN_POINT('Ctrl Pts',(-66.4804784439148,-25.5062466667702,
0.));
#80872=CARTESIAN_POINT('Ctrl Pts',(-66.4978823598354,-25.5204314764033,
0.));
#80873=CARTESIAN_POINT('Ctrl Pts',(-66.5153076112231,-25.534662975532,0.));
#80874=CARTESIAN_POINT('Ctrl Pts',(-66.5327540455624,-25.5489411295912,
0.));
#80875=CARTESIAN_POINT('Ctrl Pts',(-66.5502215110829,-25.5632659040792,
0.));
#80876=CARTESIAN_POINT('Ctrl Pts',(-66.5677098567542,-25.5776372645601,
0.));
#80877=CARTESIAN_POINT('Ctrl Pts',(-66.5852189322813,-25.5920551766629,
0.));
#80878=CARTESIAN_POINT('Ctrl Pts',(-66.6027485880963,-25.6065196060756,
0.));
#80879=CARTESIAN_POINT('Ctrl Pts',(-66.6202986753506,-25.6210305185403,
0.));
#80880=CARTESIAN_POINT('Ctrl Pts',(-66.6378690459129,-25.6355878798614,
0.));
#80881=CARTESIAN_POINT('Ctrl Pts',(-66.6554595523624,-25.6501916559055,
0.));
#80882=CARTESIAN_POINT('Ctrl Pts',(-66.6730700479837,-25.6648418126013,
0.));
#80883=CARTESIAN_POINT('Ctrl Pts',(-66.6907003867572,-25.6795383159319,
0.));
#80884=CARTESIAN_POINT('Ctrl Pts',(-66.7083504233529,-25.6942811319322,
0.));
#80885=CARTESIAN_POINT('Ctrl Pts',(-66.7260200131266,-25.7090702266963,
0.));
#80886=CARTESIAN_POINT('Ctrl Pts',(-66.7437090121153,-25.7239055663772,
0.));
#80887=CARTESIAN_POINT('Ctrl Pts',(-66.7614172770316,-25.7387871171866,
0.));
#80888=CARTESIAN_POINT('Ctrl Pts',(-66.7791446652545,-25.7537148453864,
0.));
#80889=CARTESIAN_POINT('Ctrl Pts',(-66.7968910348245,-25.7686887172878,
0.));
#80890=CARTESIAN_POINT('Ctrl Pts',(-66.8146562444433,-25.7837086992595,
0.));
#80891=CARTESIAN_POINT('Ctrl Pts',(-66.8324401534668,-25.7987747577269,
0.));
#80892=CARTESIAN_POINT('Ctrl Pts',(-66.8502426219001,-25.8138868591709,
0.));
#80893=CARTESIAN_POINT('Ctrl Pts',(-66.8680635103876,-25.8290449701193,
0.));
#80894=CARTESIAN_POINT('Ctrl Pts',(-66.8859026802088,-25.844249057147,0.));
#80895=CARTESIAN_POINT('Ctrl Pts',(-66.9037599932761,-25.8594990868833,
0.));
#80896=CARTESIAN_POINT('Ctrl Pts',(-66.92163531213,-25.8747950260111,0.));
#80897=CARTESIAN_POINT('Ctrl Pts',(-66.939528499934,-25.890136841266,0.));
#80898=CARTESIAN_POINT('Ctrl Pts',(-66.9574394204663,-25.9055244994277,
0.));
#80899=CARTESIAN_POINT('Ctrl Pts',(-66.975367938115,-25.9209579673209,0.));
#80900=CARTESIAN_POINT('Ctrl Pts',(-66.9933139178778,-25.9364372118222,
0.));
#80901=CARTESIAN_POINT('Ctrl Pts',(-67.0112772253556,-25.9519621998598,
0.));
#80902=CARTESIAN_POINT('Ctrl Pts',(-67.0292577267489,-25.967532898412,0.));
#80903=CARTESIAN_POINT('Ctrl Pts',(-67.0472552888485,-25.9831492744984,
0.));
#80904=CARTESIAN_POINT('Ctrl Pts',(-67.0652697790325,-25.9988112951814,
0.));
#80905=CARTESIAN_POINT('Ctrl Pts',(-67.0833010652634,-26.014518927573,0.));
#80906=CARTESIAN_POINT('Ctrl Pts',(-67.101349016084,-26.030272138834,0.));
#80907=CARTESIAN_POINT('Ctrl Pts',(-67.1194135006124,-26.0460708961725,
0.));
#80908=CARTESIAN_POINT('Ctrl Pts',(-67.1374943885354,-26.061915166836,0.));
#80909=CARTESIAN_POINT('Ctrl Pts',(-67.1555915501049,-26.0778049181128,
0.));
#80910=CARTESIAN_POINT('Ctrl Pts',(-67.173704856136,-26.0937401173383,0.));
#80911=CARTESIAN_POINT('Ctrl Pts',(-67.1918341780018,-26.1097207318949,
0.));
#80912=CARTESIAN_POINT('Ctrl Pts',(-67.2099793876297,-26.1257467292102,
0.));
#80913=CARTESIAN_POINT('Ctrl Pts',(-67.2281403574938,-26.1418180767489,
0.));
#80914=CARTESIAN_POINT('Ctrl Pts',(-67.2463169606115,-26.1579347420138,
0.));
#80915=CARTESIAN_POINT('Ctrl Pts',(-67.2645090705421,-26.1740966925529,
0.));
#80916=CARTESIAN_POINT('Ctrl Pts',(-67.282716561383,-26.1903038959589,0.));
#80917=CARTESIAN_POINT('Ctrl Pts',(-67.3009393077651,-26.2065563198683,
0.));
#80918=CARTESIAN_POINT('Ctrl Pts',(-67.3191771848463,-26.2228539319526,
0.));
#80919=CARTESIAN_POINT('Ctrl Pts',(-67.3374300683073,-26.2391966999191,
0.));
#80920=CARTESIAN_POINT('Ctrl Pts',(-67.3556978343507,-26.255584591518,0.));
#80921=CARTESIAN_POINT('Ctrl Pts',(-67.3739803596969,-26.2720175745423,
0.));
#80922=CARTESIAN_POINT('Ctrl Pts',(-67.392277521581,-26.288495616827,0.));
#80923=CARTESIAN_POINT('Ctrl Pts',(-67.4105891977461,-26.3050186862407,
0.));
#80924=CARTESIAN_POINT('Ctrl Pts',(-67.4289152664398,-26.321586750686,0.));
#80925=CARTESIAN_POINT('Ctrl Pts',(-67.4472556064119,-26.3381997781055,
0.));
#80926=CARTESIAN_POINT('Ctrl Pts',(-67.4656100969116,-26.3548577364833,
0.));
#80927=CARTESIAN_POINT('Ctrl Pts',(-67.4839786176836,-26.3715605938433,
0.));
#80928=CARTESIAN_POINT('Ctrl Pts',(-67.5023610489622,-26.3883083182421,
0.));
#80929=CARTESIAN_POINT('Ctrl Pts',(-67.5207572714683,-26.4051008777675,
0.));
#80930=CARTESIAN_POINT('Ctrl Pts',(-67.5391671664072,-26.4219382405458,
0.));
#80931=CARTESIAN_POINT('Ctrl Pts',(-67.5575906154657,-26.4388203747425,
0.));
#80932=CARTESIAN_POINT('Ctrl Pts',(-67.5760275008093,-26.4557472485621,
0.));
#80933=CARTESIAN_POINT('Ctrl Pts',(-67.5944777050768,-26.4727188302409,
0.));
#80934=CARTESIAN_POINT('Ctrl Pts',(-67.6129411113757,-26.489735088044,0.));
#80935=CARTESIAN_POINT('Ctrl Pts',(-67.6314176032811,-26.5067959902725,
0.));
#80936=CARTESIAN_POINT('Ctrl Pts',(-67.649907064832,-26.5239015052654,0.));
#80937=CARTESIAN_POINT('Ctrl Pts',(-67.6684093805291,-26.5410516013985,
0.));
#80938=CARTESIAN_POINT('Ctrl Pts',(-67.6869244353294,-26.5582462470794,
0.));
#80939=CARTESIAN_POINT('Ctrl Pts',(-67.7054521146424,-26.5754854107421,
0.));
#80940=CARTESIAN_POINT('Ctrl Pts',(-67.7239923043288,-26.5927690608544,
0.));
#80941=CARTESIAN_POINT('Ctrl Pts',(-67.7425448906977,-26.6100971659202,
0.));
#80942=CARTESIAN_POINT('Ctrl Pts',(-67.7611097605042,-26.6274696944793,
0.));
#80943=CARTESIAN_POINT('Ctrl Pts',(-67.7796868009455,-26.6448866151029,
0.));
#80944=CARTESIAN_POINT('Ctrl Pts',(-67.798275899657,-26.6623478963871,0.));
#80945=CARTESIAN_POINT('Ctrl Pts',(-67.8168769447098,-26.6798535069589,
0.));
#80946=CARTESIAN_POINT('Ctrl Pts',(-67.8354898246086,-26.6974034154804,
0.));
#80947=CARTESIAN_POINT('Ctrl Pts',(-67.8541144282875,-26.7149975906478,
0.));
#80948=CARTESIAN_POINT('Ctrl Pts',(-67.8727506451063,-26.7326360011885,
0.));
#80949=CARTESIAN_POINT('Ctrl Pts',(-67.8913983648436,-26.7503186158522,
0.));
#80950=CARTESIAN_POINT('Ctrl Pts',(-67.9100574776972,-26.7680454034169,
0.));
#80951=CARTESIAN_POINT('Ctrl Pts',(-67.928727874284,-26.7858163326934,0.));
#80952=CARTESIAN_POINT('Ctrl Pts',(-67.9474094456396,-26.8036313725262,
0.));
#80953=CARTESIAN_POINT('Ctrl Pts',(-67.9661020832164,-26.821490491792,0.));
#80954=CARTESIAN_POINT('Ctrl Pts',(-67.9848056788809,-26.8393936593911,
0.));
#80955=CARTESIAN_POINT('Ctrl Pts',(-68.0035201249102,-26.8573408442496,
0.));
#80956=CARTESIAN_POINT('Ctrl Pts',(-68.0222453139856,-26.8753320153252,
0.));
#80957=CARTESIAN_POINT('Ctrl Pts',(-68.0409811391869,-26.8933671416063,
0.));
#80958=CARTESIAN_POINT('Ctrl Pts',(-68.0597274939859,-26.911446192111,0.));
#80959=CARTESIAN_POINT('Ctrl Pts',(-68.0784842722369,-26.9295691358779,
0.));
#80960=CARTESIAN_POINT('Ctrl Pts',(-68.0972513681751,-26.9477359419652,
0.));
#80961=CARTESIAN_POINT('Ctrl Pts',(-68.1160286764255,-26.9659465794601,
0.));
#80962=CARTESIAN_POINT('Ctrl Pts',(-68.1348160920106,-26.9842010174822,
0.));
#80963=CARTESIAN_POINT('Ctrl Pts',(-68.1536135103557,-27.0024992251838,
0.));
#80964=CARTESIAN_POINT('Ctrl Pts',(-68.1724208272958,-27.0208411717472,
0.));
#80965=CARTESIAN_POINT('Ctrl Pts',(-68.1912379390773,-27.0392268263798,
0.));
#80966=CARTESIAN_POINT('Ctrl Pts',(-68.2100647423332,-27.0576561583172,
0.));
#80967=CARTESIAN_POINT('Ctrl Pts',(-68.2289011340615,-27.0761291368226,
0.));
#80968=CARTESIAN_POINT('Ctrl Pts',(-68.2477470116012,-27.0946457311813,
0.));
#80969=CARTESIAN_POINT('Ctrl Pts',(-68.2666022726104,-27.1132059106943,
0.));
#80970=CARTESIAN_POINT('Ctrl Pts',(-68.2854668150364,-27.1318096446649,
0.));
#80971=CARTESIAN_POINT('Ctrl Pts',(-68.3043405371603,-27.1504569024136,
0.));
#80972=CARTESIAN_POINT('Ctrl Pts',(-68.3232233376425,-27.1691476532921,
0.));
#80973=CARTESIAN_POINT('Ctrl Pts',(-68.3421151155711,-27.1878818666926,
0.));
#80974=CARTESIAN_POINT('Ctrl Pts',(-68.3610157704994,-27.2066595120542,
0.));
#80975=CARTESIAN_POINT('Ctrl Pts',(-68.3799252025102,-27.2254805588673,
0.));
#80976=CARTESIAN_POINT('Ctrl Pts',(-68.3988433121581,-27.244344976665,0.));
#80977=CARTESIAN_POINT('Ctrl Pts',(-68.4177700003465,-27.263252735006,0.));
#80978=CARTESIAN_POINT('Ctrl Pts',(-68.4367051682164,-27.2822038034538,
0.));
#80979=CARTESIAN_POINT('Ctrl Pts',(-68.4556487170441,-27.301198151557,0.));
#80980=CARTESIAN_POINT('Ctrl Pts',(-68.4746005480997,-27.3202357488154,
0.));
#80981=CARTESIAN_POINT('Ctrl Pts',(-68.4935605626372,-27.3393165646752,
0.));
#80982=CARTESIAN_POINT('Ctrl Pts',(-68.5125286621902,-27.3584405685947,
0.));
#80983=CARTESIAN_POINT('Ctrl Pts',(-68.5315047488046,-27.3776077300918,
0.));
#80984=CARTESIAN_POINT('Ctrl Pts',(-68.5504887252976,-27.3968180187941,
0.));
#80985=CARTESIAN_POINT('Ctrl Pts',(-68.5694804955002,-27.4160714044825,
0.));
#80986=CARTESIAN_POINT('Ctrl Pts',(-68.5884799645193,-27.4353678571349,
0.));
#80987=CARTESIAN_POINT('Ctrl Pts',(-68.6074870381588,-27.4547073468213,
0.));
#80988=CARTESIAN_POINT('Ctrl Pts',(-68.6265016223536,-27.4740898435977,
0.));
#80989=CARTESIAN_POINT('Ctrl Pts',(-68.6455236225471,-27.4935153173863,
0.));
#80990=CARTESIAN_POINT('Ctrl Pts',(-68.6645529432059,-27.5129837378797,
0.));
#80991=CARTESIAN_POINT('Ctrl Pts',(-68.683589486992,-27.5324950743723,0.));
#80992=CARTESIAN_POINT('Ctrl Pts',(-68.7026331554348,-27.552049295893,0.));
#80993=CARTESIAN_POINT('Ctrl Pts',(-68.721683850427,-27.5716463715027,0.));
#80994=CARTESIAN_POINT('Ctrl Pts',(-68.7407414755291,-27.5912862705482,
0.));
#80995=CARTESIAN_POINT('Ctrl Pts',(-68.7598059372121,-27.6109689629025,
0.));
#80996=CARTESIAN_POINT('Ctrl Pts',(-68.7788771464655,-27.6306944192711,
0.));
#80997=CARTESIAN_POINT('Ctrl Pts',(-68.7979550191773,-27.6504626112621,
0.));
#80998=CARTESIAN_POINT('Ctrl Pts',(-68.8143140938751,-27.667444390988,0.));
#80999=CARTESIAN_POINT('Ctrl Pts',(-68.8268597851977,-27.6804870323282,
0.));
#81000=CARTESIAN_POINT('Ctrl Pts',(-68.8355891981871,-27.6895716271078,
0.));
#81001=CARTESIAN_POINT('Ctrl Pts',(-68.8405004465887,-27.6946856803474,
0.));
#81002=CARTESIAN_POINT('Ctrl Pts',(-68.8415926174765,-27.6958230984748,
0.));
#81003=CARTESIAN_POINT('',(-65.4815644032299,-24.7419628022042,12.));
#81004=CARTESIAN_POINT('',(-65.4815644032299,-24.7419628022042,0.));
#81005=CARTESIAN_POINT('Ctrl Pts',(-68.8415926174765,-27.6958230984748,
12.));
#81006=CARTESIAN_POINT('Ctrl Pts',(-68.8405004465887,-27.6946856803474,
12.));
#81007=CARTESIAN_POINT('Ctrl Pts',(-68.8355891981871,-27.6895716271078,
12.));
#81008=CARTESIAN_POINT('Ctrl Pts',(-68.8268597851977,-27.6804870323282,
12.));
#81009=CARTESIAN_POINT('Ctrl Pts',(-68.8143140938751,-27.667444390988,12.));
#81010=CARTESIAN_POINT('Ctrl Pts',(-68.7979550191773,-27.6504626112621,
12.));
#81011=CARTESIAN_POINT('Ctrl Pts',(-68.7788771464655,-27.6306944192711,
12.));
#81012=CARTESIAN_POINT('Ctrl Pts',(-68.7598059372121,-27.6109689629025,
12.));
#81013=CARTESIAN_POINT('Ctrl Pts',(-68.7407414755291,-27.5912862705482,
12.));
#81014=CARTESIAN_POINT('Ctrl Pts',(-68.721683850427,-27.5716463715027,12.));
#81015=CARTESIAN_POINT('Ctrl Pts',(-68.7026331554348,-27.552049295893,12.));
#81016=CARTESIAN_POINT('Ctrl Pts',(-68.683589486992,-27.5324950743723,12.));
#81017=CARTESIAN_POINT('Ctrl Pts',(-68.6645529432059,-27.5129837378797,
12.));
#81018=CARTESIAN_POINT('Ctrl Pts',(-68.6455236225471,-27.4935153173863,
12.));
#81019=CARTESIAN_POINT('Ctrl Pts',(-68.6265016223536,-27.4740898435977,
12.));
#81020=CARTESIAN_POINT('Ctrl Pts',(-68.6074870381588,-27.4547073468213,
12.));
#81021=CARTESIAN_POINT('Ctrl Pts',(-68.5884799645193,-27.4353678571349,
12.));
#81022=CARTESIAN_POINT('Ctrl Pts',(-68.5694804955002,-27.4160714044825,
12.));
#81023=CARTESIAN_POINT('Ctrl Pts',(-68.5504887252976,-27.3968180187941,
12.));
#81024=CARTESIAN_POINT('Ctrl Pts',(-68.5315047488046,-27.3776077300918,
12.));
#81025=CARTESIAN_POINT('Ctrl Pts',(-68.5125286621902,-27.3584405685947,
12.));
#81026=CARTESIAN_POINT('Ctrl Pts',(-68.4935605626372,-27.3393165646752,
12.));
#81027=CARTESIAN_POINT('Ctrl Pts',(-68.4746005480997,-27.3202357488154,
12.));
#81028=CARTESIAN_POINT('Ctrl Pts',(-68.4556487170441,-27.301198151557,12.));
#81029=CARTESIAN_POINT('Ctrl Pts',(-68.4367051682164,-27.2822038034538,
12.));
#81030=CARTESIAN_POINT('Ctrl Pts',(-68.4177700003465,-27.263252735006,12.));
#81031=CARTESIAN_POINT('Ctrl Pts',(-68.3988433121581,-27.244344976665,12.));
#81032=CARTESIAN_POINT('Ctrl Pts',(-68.3799252025102,-27.2254805588673,
12.));
#81033=CARTESIAN_POINT('Ctrl Pts',(-68.3610157704994,-27.2066595120542,
12.));
#81034=CARTESIAN_POINT('Ctrl Pts',(-68.3421151155711,-27.1878818666926,
12.));
#81035=CARTESIAN_POINT('Ctrl Pts',(-68.3232233376425,-27.1691476532921,
12.));
#81036=CARTESIAN_POINT('Ctrl Pts',(-68.3043405371603,-27.1504569024136,
12.));
#81037=CARTESIAN_POINT('Ctrl Pts',(-68.2854668150364,-27.1318096446649,
12.));
#81038=CARTESIAN_POINT('Ctrl Pts',(-68.2666022726104,-27.1132059106943,
12.));
#81039=CARTESIAN_POINT('Ctrl Pts',(-68.2477470116012,-27.0946457311813,
12.));
#81040=CARTESIAN_POINT('Ctrl Pts',(-68.2289011340615,-27.0761291368226,
12.));
#81041=CARTESIAN_POINT('Ctrl Pts',(-68.2100647423332,-27.0576561583172,
12.));
#81042=CARTESIAN_POINT('Ctrl Pts',(-68.1912379390773,-27.0392268263798,
12.));
#81043=CARTESIAN_POINT('Ctrl Pts',(-68.1724208272958,-27.0208411717472,
12.));
#81044=CARTESIAN_POINT('Ctrl Pts',(-68.1536135103557,-27.0024992251838,
12.));
#81045=CARTESIAN_POINT('Ctrl Pts',(-68.1348160920106,-26.9842010174822,
12.));
#81046=CARTESIAN_POINT('Ctrl Pts',(-68.1160286764255,-26.9659465794601,
12.));
#81047=CARTESIAN_POINT('Ctrl Pts',(-68.0972513681751,-26.9477359419652,
12.));
#81048=CARTESIAN_POINT('Ctrl Pts',(-68.0784842722369,-26.9295691358779,
12.));
#81049=CARTESIAN_POINT('Ctrl Pts',(-68.0597274939859,-26.911446192111,12.));
#81050=CARTESIAN_POINT('Ctrl Pts',(-68.0409811391869,-26.8933671416063,
12.));
#81051=CARTESIAN_POINT('Ctrl Pts',(-68.0222453139856,-26.8753320153252,
12.));
#81052=CARTESIAN_POINT('Ctrl Pts',(-68.0035201249102,-26.8573408442496,
12.));
#81053=CARTESIAN_POINT('Ctrl Pts',(-67.9848056788809,-26.8393936593911,
12.));
#81054=CARTESIAN_POINT('Ctrl Pts',(-67.9661020832164,-26.821490491792,12.));
#81055=CARTESIAN_POINT('Ctrl Pts',(-67.9474094456396,-26.8036313725262,
12.));
#81056=CARTESIAN_POINT('Ctrl Pts',(-67.928727874284,-26.7858163326934,12.));
#81057=CARTESIAN_POINT('Ctrl Pts',(-67.9100574776972,-26.7680454034169,
12.));
#81058=CARTESIAN_POINT('Ctrl Pts',(-67.8913983648436,-26.7503186158522,
12.));
#81059=CARTESIAN_POINT('Ctrl Pts',(-67.8727506451063,-26.7326360011885,
12.));
#81060=CARTESIAN_POINT('Ctrl Pts',(-67.8541144282875,-26.7149975906478,
12.));
#81061=CARTESIAN_POINT('Ctrl Pts',(-67.8354898246086,-26.6974034154804,
12.));
#81062=CARTESIAN_POINT('Ctrl Pts',(-67.8168769447098,-26.6798535069589,
12.));
#81063=CARTESIAN_POINT('Ctrl Pts',(-67.798275899657,-26.6623478963871,12.));
#81064=CARTESIAN_POINT('Ctrl Pts',(-67.7796868009455,-26.6448866151029,
12.));
#81065=CARTESIAN_POINT('Ctrl Pts',(-67.7611097605042,-26.6274696944793,
12.));
#81066=CARTESIAN_POINT('Ctrl Pts',(-67.7425448906977,-26.6100971659202,
12.));
#81067=CARTESIAN_POINT('Ctrl Pts',(-67.7239923043288,-26.5927690608544,
12.));
#81068=CARTESIAN_POINT('Ctrl Pts',(-67.7054521146424,-26.5754854107421,
12.));
#81069=CARTESIAN_POINT('Ctrl Pts',(-67.6869244353294,-26.5582462470794,
12.));
#81070=CARTESIAN_POINT('Ctrl Pts',(-67.6684093805291,-26.5410516013985,
12.));
#81071=CARTESIAN_POINT('Ctrl Pts',(-67.649907064832,-26.5239015052654,12.));
#81072=CARTESIAN_POINT('Ctrl Pts',(-67.6314176032811,-26.5067959902725,
12.));
#81073=CARTESIAN_POINT('Ctrl Pts',(-67.6129411113757,-26.489735088044,12.));
#81074=CARTESIAN_POINT('Ctrl Pts',(-67.5944777050768,-26.4727188302409,
12.));
#81075=CARTESIAN_POINT('Ctrl Pts',(-67.5760275008093,-26.4557472485621,
12.));
#81076=CARTESIAN_POINT('Ctrl Pts',(-67.5575906154657,-26.4388203747425,
12.));
#81077=CARTESIAN_POINT('Ctrl Pts',(-67.5391671664072,-26.4219382405458,
12.));
#81078=CARTESIAN_POINT('Ctrl Pts',(-67.5207572714683,-26.4051008777675,
12.));
#81079=CARTESIAN_POINT('Ctrl Pts',(-67.5023610489622,-26.3883083182421,
12.));
#81080=CARTESIAN_POINT('Ctrl Pts',(-67.4839786176836,-26.3715605938433,
12.));
#81081=CARTESIAN_POINT('Ctrl Pts',(-67.4656100969116,-26.3548577364833,
12.));
#81082=CARTESIAN_POINT('Ctrl Pts',(-67.4472556064119,-26.3381997781055,
12.));
#81083=CARTESIAN_POINT('Ctrl Pts',(-67.4289152664398,-26.321586750686,12.));
#81084=CARTESIAN_POINT('Ctrl Pts',(-67.4105891977461,-26.3050186862407,
12.));
#81085=CARTESIAN_POINT('Ctrl Pts',(-67.392277521581,-26.288495616827,12.));
#81086=CARTESIAN_POINT('Ctrl Pts',(-67.3739803596969,-26.2720175745423,
12.));
#81087=CARTESIAN_POINT('Ctrl Pts',(-67.3556978343507,-26.255584591518,12.));
#81088=CARTESIAN_POINT('Ctrl Pts',(-67.3374300683073,-26.2391966999191,
12.));
#81089=CARTESIAN_POINT('Ctrl Pts',(-67.3191771848463,-26.2228539319526,
12.));
#81090=CARTESIAN_POINT('Ctrl Pts',(-67.3009393077651,-26.2065563198683,
12.));
#81091=CARTESIAN_POINT('Ctrl Pts',(-67.282716561383,-26.1903038959589,12.));
#81092=CARTESIAN_POINT('Ctrl Pts',(-67.2645090705421,-26.1740966925529,
12.));
#81093=CARTESIAN_POINT('Ctrl Pts',(-67.2463169606115,-26.1579347420138,
12.));
#81094=CARTESIAN_POINT('Ctrl Pts',(-67.2281403574938,-26.1418180767489,
12.));
#81095=CARTESIAN_POINT('Ctrl Pts',(-67.2099793876297,-26.1257467292102,
12.));
#81096=CARTESIAN_POINT('Ctrl Pts',(-67.1918341780018,-26.1097207318949,
12.));
#81097=CARTESIAN_POINT('Ctrl Pts',(-67.173704856136,-26.0937401173383,12.));
#81098=CARTESIAN_POINT('Ctrl Pts',(-67.1555915501049,-26.0778049181128,
12.));
#81099=CARTESIAN_POINT('Ctrl Pts',(-67.1374943885354,-26.061915166836,12.));
#81100=CARTESIAN_POINT('Ctrl Pts',(-67.1194135006124,-26.0460708961725,
12.));
#81101=CARTESIAN_POINT('Ctrl Pts',(-67.101349016084,-26.030272138834,12.));
#81102=CARTESIAN_POINT('Ctrl Pts',(-67.0833010652634,-26.014518927573,12.));
#81103=CARTESIAN_POINT('Ctrl Pts',(-67.0652697790325,-25.9988112951814,
12.));
#81104=CARTESIAN_POINT('Ctrl Pts',(-67.0472552888485,-25.9831492744984,
12.));
#81105=CARTESIAN_POINT('Ctrl Pts',(-67.0292577267489,-25.967532898412,12.));
#81106=CARTESIAN_POINT('Ctrl Pts',(-67.0112772253556,-25.9519621998598,
12.));
#81107=CARTESIAN_POINT('Ctrl Pts',(-66.9933139178778,-25.9364372118222,
12.));
#81108=CARTESIAN_POINT('Ctrl Pts',(-66.975367938115,-25.9209579673209,12.));
#81109=CARTESIAN_POINT('Ctrl Pts',(-66.9574394204663,-25.9055244994277,
12.));
#81110=CARTESIAN_POINT('Ctrl Pts',(-66.939528499934,-25.890136841266,12.));
#81111=CARTESIAN_POINT('Ctrl Pts',(-66.92163531213,-25.8747950260111,12.));
#81112=CARTESIAN_POINT('Ctrl Pts',(-66.9037599932761,-25.8594990868833,
12.));
#81113=CARTESIAN_POINT('Ctrl Pts',(-66.8859026802088,-25.844249057147,12.));
#81114=CARTESIAN_POINT('Ctrl Pts',(-66.8680635103876,-25.8290449701193,
12.));
#81115=CARTESIAN_POINT('Ctrl Pts',(-66.8502426219001,-25.8138868591709,
12.));
#81116=CARTESIAN_POINT('Ctrl Pts',(-66.8324401534668,-25.7987747577269,
12.));
#81117=CARTESIAN_POINT('Ctrl Pts',(-66.8146562444433,-25.7837086992595,
12.));
#81118=CARTESIAN_POINT('Ctrl Pts',(-66.7968910348245,-25.7686887172878,
12.));
#81119=CARTESIAN_POINT('Ctrl Pts',(-66.7791446652545,-25.7537148453864,
12.));
#81120=CARTESIAN_POINT('Ctrl Pts',(-66.7614172770316,-25.7387871171866,
12.));
#81121=CARTESIAN_POINT('Ctrl Pts',(-66.7437090121153,-25.7239055663772,
12.));
#81122=CARTESIAN_POINT('Ctrl Pts',(-66.7260200131266,-25.7090702266963,
12.));
#81123=CARTESIAN_POINT('Ctrl Pts',(-66.7083504233529,-25.6942811319322,
12.));
#81124=CARTESIAN_POINT('Ctrl Pts',(-66.6907003867572,-25.6795383159319,
12.));
#81125=CARTESIAN_POINT('Ctrl Pts',(-66.6730700479837,-25.6648418126013,
12.));
#81126=CARTESIAN_POINT('Ctrl Pts',(-66.6554595523624,-25.6501916559055,
12.));
#81127=CARTESIAN_POINT('Ctrl Pts',(-66.6378690459129,-25.6355878798614,
12.));
#81128=CARTESIAN_POINT('Ctrl Pts',(-66.6202986753506,-25.6210305185403,
12.));
#81129=CARTESIAN_POINT('Ctrl Pts',(-66.6027485880963,-25.6065196060756,
12.));
#81130=CARTESIAN_POINT('Ctrl Pts',(-66.5852189322813,-25.5920551766629,
12.));
#81131=CARTESIAN_POINT('Ctrl Pts',(-66.5677098567542,-25.5776372645601,
12.));
#81132=CARTESIAN_POINT('Ctrl Pts',(-66.5502215110829,-25.5632659040792,
12.));
#81133=CARTESIAN_POINT('Ctrl Pts',(-66.5327540455624,-25.5489411295912,
12.));
#81134=CARTESIAN_POINT('Ctrl Pts',(-66.5153076112231,-25.534662975532,12.));
#81135=CARTESIAN_POINT('Ctrl Pts',(-66.4978823598354,-25.5204314764033,
12.));
#81136=CARTESIAN_POINT('Ctrl Pts',(-66.4804784439148,-25.5062466667702,
12.));
#81137=CARTESIAN_POINT('Ctrl Pts',(-66.4630960167252,-25.4921085812547,
12.));
#81138=CARTESIAN_POINT('Ctrl Pts',(-66.4457352322871,-25.4780172545417,
12.));
#81139=CARTESIAN_POINT('Ctrl Pts',(-66.4283962453899,-25.4639727213849,
12.));
#81140=CARTESIAN_POINT('Ctrl Pts',(-66.4110792116,-25.4499750166079,12.));
#81141=CARTESIAN_POINT('Ctrl Pts',(-66.3937842872685,-25.4360241751018,
12.));
#81142=CARTESIAN_POINT('Ctrl Pts',(-66.3765116295364,-25.4221202318199,
12.));
#81143=CARTESIAN_POINT('Ctrl Pts',(-66.359261396341,-25.4082632217847,12.));
#81144=CARTESIAN_POINT('Ctrl Pts',(-66.3420337464178,-25.3944531800901,
12.));
#81145=CARTESIAN_POINT('Ctrl Pts',(-66.3248288393046,-25.3806901419012,
12.));
#81146=CARTESIAN_POINT('Ctrl Pts',(-66.3076468353412,-25.3669741424488,
12.));
#81147=CARTESIAN_POINT('Ctrl Pts',(-66.290487895671,-25.3533052170249,12.));
#81148=CARTESIAN_POINT('Ctrl Pts',(-66.2733521822662,-25.3396834009949,
12.));
#81149=CARTESIAN_POINT('Ctrl Pts',(-66.2562398579471,-25.3261087298026,
12.));
#81150=CARTESIAN_POINT('Ctrl Pts',(-66.2391510863998,-25.312581238973,12.));
#81151=CARTESIAN_POINT('Ctrl Pts',(-66.2220860321952,-25.2991009641094,
12.));
#81152=CARTESIAN_POINT('Ctrl Pts',(-66.2050448607911,-25.285667940893,12.));
#81153=CARTESIAN_POINT('Ctrl Pts',(-66.1880277385136,-25.2722822050837,
12.));
#81154=CARTESIAN_POINT('Ctrl Pts',(-66.1710348325384,-25.2589437925147,
12.));
#81155=CARTESIAN_POINT('Ctrl Pts',(-66.1540663108754,-25.2456527390875,
12.));
#81156=CARTESIAN_POINT('Ctrl Pts',(-66.1371223423345,-25.232409080755,12.));
#81157=CARTESIAN_POINT('Ctrl Pts',(-66.1202030965758,-25.2192128535357,
12.));
#81158=CARTESIAN_POINT('Ctrl Pts',(-66.10330874419,-25.2060640935365,12.));
#81159=CARTESIAN_POINT('Ctrl Pts',(-66.086439456768,-25.1929628369685,12.));
#81160=CARTESIAN_POINT('Ctrl Pts',(-66.0695954069713,-25.1799091201599,
12.));
#81161=CARTESIAN_POINT('Ctrl Pts',(-66.0527767686025,-25.1669029795661,
12.));
#81162=CARTESIAN_POINT('Ctrl Pts',(-66.0359837164734,-25.1539444517419,
12.));
#81163=CARTESIAN_POINT('Ctrl Pts',(-66.0192164262621,-25.1410335733099,
12.));
#81164=CARTESIAN_POINT('Ctrl Pts',(-66.0024750743897,-25.1281703809297,
12.));
#81165=CARTESIAN_POINT('Ctrl Pts',(-65.9857598378433,-25.1153549112503,
12.));
#81166=CARTESIAN_POINT('Ctrl Pts',(-65.9690708941558,-25.1025872009004,
12.));
#81167=CARTESIAN_POINT('Ctrl Pts',(-65.9524084218139,-25.0898672865915,
12.));
#81168=CARTESIAN_POINT('Ctrl Pts',(-65.9357726006163,-25.0771952052028,
12.));
#81169=CARTESIAN_POINT('Ctrl Pts',(-65.919163611981,-25.0645709938524,12.));
#81170=CARTESIAN_POINT('Ctrl Pts',(-65.9025816394424,-25.0519946900078,
12.));
#81171=CARTESIAN_POINT('Ctrl Pts',(-65.8860268683128,-25.0394663314055,
12.));
#81172=CARTESIAN_POINT('Ctrl Pts',(-65.8694994847616,-25.0269859558362,
12.));
#81173=CARTESIAN_POINT('Ctrl Pts',(-65.8529996750445,-25.0145536009604,
12.));
#81174=CARTESIAN_POINT('Ctrl Pts',(-65.8365276247128,-25.002169304117,12.));
#81175=CARTESIAN_POINT('Ctrl Pts',(-65.8200835177024,-24.9898331020983,
12.));
#81176=CARTESIAN_POINT('Ctrl Pts',(-65.8036675380718,-24.9775450315682,
12.));
#81177=CARTESIAN_POINT('Ctrl Pts',(-65.7872798720823,-24.9653051295581,
12.));
#81178=CARTESIAN_POINT('Ctrl Pts',(-65.7709207098959,-24.9531134338696,
12.));
#81179=CARTESIAN_POINT('Ctrl Pts',(-65.7545902480323,-24.9409699836537,
12.));
#81180=CARTESIAN_POINT('Ctrl Pts',(-65.7382886895888,-24.928874819458,12.));
#81181=CARTESIAN_POINT('Ctrl Pts',(-65.7220162391054,-24.9168279820106,
12.));
#81182=CARTESIAN_POINT('Ctrl Pts',(-65.7057730980483,-24.9048295111448,
12.));
#81183=CARTESIAN_POINT('Ctrl Pts',(-65.6895594608775,-24.8928794448607,
12.));
#81184=CARTESIAN_POINT('Ctrl Pts',(-65.6733755087669,-24.8809778178229,
12.));
#81185=CARTESIAN_POINT('Ctrl Pts',(-65.6572214156692,-24.8691246628057,
12.));
#81186=CARTESIAN_POINT('Ctrl Pts',(-65.6410973603661,-24.8573200135666,
12.));
#81187=CARTESIAN_POINT('Ctrl Pts',(-65.6250035361612,-24.8455639071517,
12.));
#81188=CARTESIAN_POINT('Ctrl Pts',(-65.6089401625628,-24.8338563866764,
12.));
#81189=CARTESIAN_POINT('Ctrl Pts',(-65.5929074932624,-24.8221975032104,
12.));
#81190=CARTESIAN_POINT('Ctrl Pts',(-65.5769057914333,-24.8105873098626,
12.));
#81191=CARTESIAN_POINT('Ctrl Pts',(-65.5609353062829,-24.799025856126,12.));
#81192=CARTESIAN_POINT('Ctrl Pts',(-65.5449962514661,-24.787513182749,12.));
#81193=CARTESIAN_POINT('Ctrl Pts',(-65.5290887770232,-24.7760493148465,
12.));
#81194=CARTESIAN_POINT('Ctrl Pts',(-65.5132129675333,-24.7646342620841,
12.));
#81195=CARTESIAN_POINT('Ctrl Pts',(-65.5005376841101,-24.7555412724651,
12.));
#81196=CARTESIAN_POINT('Ctrl Pts',(-65.4910454936254,-24.7487434955982,
12.));
#81197=CARTESIAN_POINT('Ctrl Pts',(-65.4847237095443,-24.7442214063382,
12.));
#81198=CARTESIAN_POINT('Ctrl Pts',(-65.4815644032299,-24.7419628022042,
12.));
#81199=CARTESIAN_POINT('Ctrl Pts',(-68.2622612910177,-29.0944526440266,
-5.55111512312578E-16));
#81200=CARTESIAN_POINT('Ctrl Pts',(-68.2622612910177,-29.0944526440266,
4.));
#81201=CARTESIAN_POINT('Ctrl Pts',(-68.2622612910177,-29.0944526440266,
8.));
#81202=CARTESIAN_POINT('Ctrl Pts',(-68.2622612910177,-29.0944526440266,
12.));
#81203=CARTESIAN_POINT('Ctrl Pts',(-68.3721211369509,-29.0922231502664,
-5.55111512312578E-16));
#81204=CARTESIAN_POINT('Ctrl Pts',(-68.3721211369509,-29.0922231502664,
3.99999999999999));
#81205=CARTESIAN_POINT('Ctrl Pts',(-68.3721211369508,-29.0922231502664,
8.));
#81206=CARTESIAN_POINT('Ctrl Pts',(-68.3721211369508,-29.0922231502664,
12.));
#81207=CARTESIAN_POINT('Ctrl Pts',(-68.5624216146675,-29.0225207419381,
-5.55111512312578E-16));
#81208=CARTESIAN_POINT('Ctrl Pts',(-68.5624216146675,-29.0225207419381,
4.00000000000001));
#81209=CARTESIAN_POINT('Ctrl Pts',(-68.5624216146675,-29.0225207419382,
7.99999999999999));
#81210=CARTESIAN_POINT('Ctrl Pts',(-68.5624216146675,-29.0225207419382,
12.));
#81211=CARTESIAN_POINT('Ctrl Pts',(-68.6814343344132,-28.8637726134455,
-5.55111512312578E-16));
#81212=CARTESIAN_POINT('Ctrl Pts',(-68.6814343344132,-28.8637726134455,
3.99999999999999));
#81213=CARTESIAN_POINT('Ctrl Pts',(-68.6814343344132,-28.8637726134455,
8.00000000000001));
#81214=CARTESIAN_POINT('Ctrl Pts',(-68.6814343344132,-28.8637726134455,
12.));
#81215=CARTESIAN_POINT('Ctrl Pts',(-68.7132793373319,-28.7877620302417,
-5.55111512312578E-16));
#81216=CARTESIAN_POINT('Ctrl Pts',(-68.7132793373319,-28.7877620302417,
4.));
#81217=CARTESIAN_POINT('Ctrl Pts',(-68.7132793373319,-28.7877620302417,
8.));
#81218=CARTESIAN_POINT('Ctrl Pts',(-68.7132793373319,-28.7877620302417,
12.));
#81219=CARTESIAN_POINT('',(-68.2622612910177,-29.0944526440266,0.));
#81220=CARTESIAN_POINT('',(-68.7132793373317,-28.7877620302417,0.));
#81221=CARTESIAN_POINT('Ctrl Pts',(-68.2622612910177,-29.0944526440266,
2.77555756156289E-16));
#81222=CARTESIAN_POINT('Ctrl Pts',(-68.3721211369509,-29.0922231502664,
2.77555756156288E-16));
#81223=CARTESIAN_POINT('Ctrl Pts',(-68.4808642670747,-29.0523932026502,
2.7755575615629E-16));
#81224=CARTESIAN_POINT('Ctrl Pts',(-68.5663297619426,-28.983487101511,2.77555756156289E-16));
#81225=CARTESIAN_POINT('Ctrl Pts',(-68.6304288830936,-28.9318075256566,
2.77555756156289E-16));
#81226=CARTESIAN_POINT('Ctrl Pts',(-68.6814343344132,-28.8637726134455,
2.77555756156288E-16));
#81227=CARTESIAN_POINT('Ctrl Pts',(-68.7132793373319,-28.7877620302417,
2.77555756156289E-16));
#81228=CARTESIAN_POINT('',(-68.7132793373317,-28.7877620302417,12.));
#81229=CARTESIAN_POINT('Ctrl Pts',(-68.7132793373319,-28.7877620302417,
-5.55111512312578E-16));
#81230=CARTESIAN_POINT('Ctrl Pts',(-68.7132793373319,-28.7877620302417,
4.));
#81231=CARTESIAN_POINT('Ctrl Pts',(-68.7132793373319,-28.7877620302417,
8.));
#81232=CARTESIAN_POINT('Ctrl Pts',(-68.7132793373319,-28.7877620302417,
12.));
#81233=CARTESIAN_POINT('',(-68.2622612910177,-29.0944526440266,12.));
#81234=CARTESIAN_POINT('Ctrl Pts',(-68.7132793373319,-28.7877620302417,
12.));
#81235=CARTESIAN_POINT('Ctrl Pts',(-68.6814343344132,-28.8637726134455,
12.));
#81236=CARTESIAN_POINT('Ctrl Pts',(-68.6304288830936,-28.9318075256567,
12.));
#81237=CARTESIAN_POINT('Ctrl Pts',(-68.5663297619426,-28.983487101511,12.));
#81238=CARTESIAN_POINT('Ctrl Pts',(-68.4808642670747,-29.0523932026502,
12.));
#81239=CARTESIAN_POINT('Ctrl Pts',(-68.3721211369508,-29.0922231502664,
12.));
#81240=CARTESIAN_POINT('Ctrl Pts',(-68.2622612910177,-29.0944526440266,
12.));
#81241=CARTESIAN_POINT('Ctrl Pts',(-68.2622612910177,-29.0944526440266,
12.));
#81242=CARTESIAN_POINT('Ctrl Pts',(-68.2622612910177,-29.0944526440266,
8.));
#81243=CARTESIAN_POINT('Ctrl Pts',(-68.2622612910177,-29.0944526440266,
4.));
#81244=CARTESIAN_POINT('Ctrl Pts',(-68.2622612910177,-29.0944526440266,
-5.55111512312578E-16));
#81245=CARTESIAN_POINT('Origin',(-3.46272497684358E-10,-1.43538201480493E-10,
0.));
#81246=CARTESIAN_POINT('Origin',(-3.46272497684358E-10,-1.43538201480493E-10,
12.));
#81247=CARTESIAN_POINT('Origin',(-3.46272497684358E-10,-1.43538201480493E-10,
0.));
#81248=CARTESIAN_POINT('Ctrl Pts',(-71.1418425484881,-22.1153394458716,
0.));
#81249=CARTESIAN_POINT('Ctrl Pts',(-71.1418425484881,-22.1153394458716,
4.));
#81250=CARTESIAN_POINT('Ctrl Pts',(-71.1418425484881,-22.1153394458716,
8.));
#81251=CARTESIAN_POINT('Ctrl Pts',(-71.1418425484881,-22.1153394458716,
12.));
#81252=CARTESIAN_POINT('Ctrl Pts',(-71.1744611799059,-22.0104100349462,
0.));
#81253=CARTESIAN_POINT('Ctrl Pts',(-71.1744611799059,-22.0104100349462,
4.));
#81254=CARTESIAN_POINT('Ctrl Pts',(-71.1744611799059,-22.0104100349463,
8.));
#81255=CARTESIAN_POINT('Ctrl Pts',(-71.1744611799059,-22.0104100349463,
12.));
#81256=CARTESIAN_POINT('Ctrl Pts',(-71.168501135194,-21.8078334561032,0.));
#81257=CARTESIAN_POINT('Ctrl Pts',(-71.168501135194,-21.8078334561032,4.));
#81258=CARTESIAN_POINT('Ctrl Pts',(-71.168501135194,-21.8078334561032,7.99999999999999));
#81259=CARTESIAN_POINT('Ctrl Pts',(-71.168501135194,-21.8078334561032,12.));
#81260=CARTESIAN_POINT('Ctrl Pts',(-71.0555229320378,-21.6447353227845,
0.));
#81261=CARTESIAN_POINT('Ctrl Pts',(-71.0555229320378,-21.6447353227845,
4.));
#81262=CARTESIAN_POINT('Ctrl Pts',(-71.0555229320377,-21.6447353227846,
8.00000000000001));
#81263=CARTESIAN_POINT('Ctrl Pts',(-71.0555229320377,-21.6447353227846,
12.));
#81264=CARTESIAN_POINT('Ctrl Pts',(-70.9934796068778,-21.5904919934805,
0.));
#81265=CARTESIAN_POINT('Ctrl Pts',(-70.9934796068778,-21.5904919934805,
4.));
#81266=CARTESIAN_POINT('Ctrl Pts',(-70.9934796068777,-21.5904919934805,
8.));
#81267=CARTESIAN_POINT('Ctrl Pts',(-70.9934796068777,-21.5904919934805,
12.));
#81268=CARTESIAN_POINT('',(-71.1418425484881,-22.1153394458716,0.));
#81269=CARTESIAN_POINT('',(-70.993479606878,-21.5904919934802,0.));
#81270=CARTESIAN_POINT('Ctrl Pts',(-71.1418425484881,-22.1153394458716,
0.));
#81271=CARTESIAN_POINT('Ctrl Pts',(-71.1744611799059,-22.0104100349462,
0.));
#81272=CARTESIAN_POINT('Ctrl Pts',(-71.1710554400705,-21.894651989893,0.));
#81273=CARTESIAN_POINT('Ctrl Pts',(-71.132704995437,-21.7917848658274,0.));
#81274=CARTESIAN_POINT('Ctrl Pts',(-71.1039421619619,-21.7146345227782,
0.));
#81275=CARTESIAN_POINT('Ctrl Pts',(-71.0555229320378,-21.6447353227845,
0.));
#81276=CARTESIAN_POINT('Ctrl Pts',(-70.9934796068778,-21.5904919934805,
0.));
#81277=CARTESIAN_POINT('',(-70.993479606878,-21.5904919934802,12.));
#81278=CARTESIAN_POINT('Ctrl Pts',(-70.9934796068778,-21.5904919934805,
0.));
#81279=CARTESIAN_POINT('Ctrl Pts',(-70.9934796068778,-21.5904919934805,
4.));
#81280=CARTESIAN_POINT('Ctrl Pts',(-70.9934796068777,-21.5904919934805,
8.));
#81281=CARTESIAN_POINT('Ctrl Pts',(-70.9934796068777,-21.5904919934805,
12.));
#81282=CARTESIAN_POINT('',(-71.1418425484881,-22.1153394458716,12.));
#81283=CARTESIAN_POINT('Ctrl Pts',(-70.9934796068777,-21.5904919934805,
12.));
#81284=CARTESIAN_POINT('Ctrl Pts',(-71.0555229320377,-21.6447353227846,
12.));
#81285=CARTESIAN_POINT('Ctrl Pts',(-71.1039421619619,-21.7146345227783,
12.));
#81286=CARTESIAN_POINT('Ctrl Pts',(-71.132704995437,-21.7917848658275,12.));
#81287=CARTESIAN_POINT('Ctrl Pts',(-71.1710554400705,-21.8946519898931,
12.));
#81288=CARTESIAN_POINT('Ctrl Pts',(-71.1744611799059,-22.0104100349463,
12.));
#81289=CARTESIAN_POINT('Ctrl Pts',(-71.1418425484881,-22.1153394458716,
12.));
#81290=CARTESIAN_POINT('Ctrl Pts',(-71.1418425484881,-22.1153394458716,
12.));
#81291=CARTESIAN_POINT('Ctrl Pts',(-71.1418425484881,-22.1153394458716,
8.));
#81292=CARTESIAN_POINT('Ctrl Pts',(-71.1418425484881,-22.1153394458716,
4.));
#81293=CARTESIAN_POINT('Ctrl Pts',(-71.1418425484881,-22.1153394458716,
0.));
#81294=CARTESIAN_POINT('Ctrl Pts',(-67.3887914263118,-18.9407177820969,
0.));
#81295=CARTESIAN_POINT('Ctrl Pts',(-67.3887914263118,-18.9407177820969,
12.));
#81296=CARTESIAN_POINT('Ctrl Pts',(-67.3921355608328,-18.9426924398719,
0.));
#81297=CARTESIAN_POINT('Ctrl Pts',(-67.3921355608328,-18.9426924398719,
12.));
#81298=CARTESIAN_POINT('Ctrl Pts',(-67.3988274146651,-18.9466463414299,
0.));
#81299=CARTESIAN_POINT('Ctrl Pts',(-67.3988274146651,-18.9466463414299,
12.));
#81300=CARTESIAN_POINT('Ctrl Pts',(-67.4088759497911,-18.9525909517915,
0.));
#81301=CARTESIAN_POINT('Ctrl Pts',(-67.4088759497911,-18.9525909517915,
12.));
#81302=CARTESIAN_POINT('Ctrl Pts',(-67.4222955061981,-18.9605446160985,
0.));
#81303=CARTESIAN_POINT('Ctrl Pts',(-67.4222955061981,-18.9605446160985,
12.));
#81304=CARTESIAN_POINT('Ctrl Pts',(-67.4391057908418,-18.9705325631711,
0.));
#81305=CARTESIAN_POINT('Ctrl Pts',(-67.4391057908418,-18.9705325631711,
12.));
#81306=CARTESIAN_POINT('Ctrl Pts',(-67.4559518744638,-18.9805663798449,
0.));
#81307=CARTESIAN_POINT('Ctrl Pts',(-67.4559518744638,-18.9805663798449,
12.));
#81308=CARTESIAN_POINT('Ctrl Pts',(-67.472833671964,-18.9906460638625,0.));
#81309=CARTESIAN_POINT('Ctrl Pts',(-67.472833671964,-18.9906460638625,12.));
#81310=CARTESIAN_POINT('Ctrl Pts',(-67.4897510316844,-19.0007716032819,
0.));
#81311=CARTESIAN_POINT('Ctrl Pts',(-67.4897510316844,-19.0007716032819,
12.));
#81312=CARTESIAN_POINT('Ctrl Pts',(-67.5067037372317,-19.0109429761306,
0.));
#81313=CARTESIAN_POINT('Ctrl Pts',(-67.5067037372317,-19.0109429761306,
12.));
#81314=CARTESIAN_POINT('Ctrl Pts',(-67.5236915360331,-19.021160154824,0.));
#81315=CARTESIAN_POINT('Ctrl Pts',(-67.5236915360331,-19.021160154824,12.));
#81316=CARTESIAN_POINT('Ctrl Pts',(-67.540714161288,-19.0314231093923,0.));
#81317=CARTESIAN_POINT('Ctrl Pts',(-67.540714161288,-19.0314231093923,12.));
#81318=CARTESIAN_POINT('Ctrl Pts',(-67.5577713558194,-19.0417318110708,
0.));
#81319=CARTESIAN_POINT('Ctrl Pts',(-67.5577713558194,-19.0417318110708,
12.));
#81320=CARTESIAN_POINT('Ctrl Pts',(-67.5748628971964,-19.0520862360396,
0.));
#81321=CARTESIAN_POINT('Ctrl Pts',(-67.5748628971964,-19.0520862360396,
12.));
#81322=CARTESIAN_POINT('Ctrl Pts',(-67.5919885896222,-19.062486364241,0.));
#81323=CARTESIAN_POINT('Ctrl Pts',(-67.5919885896222,-19.062486364241,12.));
#81324=CARTESIAN_POINT('Ctrl Pts',(-67.6091482520534,-19.072932177628,0.));
#81325=CARTESIAN_POINT('Ctrl Pts',(-67.6091482520534,-19.072932177628,12.));
#81326=CARTESIAN_POINT('Ctrl Pts',(-67.6263417083426,-19.0834236587118,
0.));
#81327=CARTESIAN_POINT('Ctrl Pts',(-67.6263417083426,-19.0834236587118,
12.));
#81328=CARTESIAN_POINT('Ctrl Pts',(-67.6435687749841,-19.0939607887502,
0.));
#81329=CARTESIAN_POINT('Ctrl Pts',(-67.6435687749841,-19.0939607887502,
12.));
#81330=CARTESIAN_POINT('Ctrl Pts',(-67.6608292549462,-19.1045435468358,
0.));
#81331=CARTESIAN_POINT('Ctrl Pts',(-67.6608292549462,-19.1045435468358,
12.));
#81332=CARTESIAN_POINT('Ctrl Pts',(-67.6781229440573,-19.115171910846,0.));
#81333=CARTESIAN_POINT('Ctrl Pts',(-67.6781229440573,-19.115171910846,12.));
#81334=CARTESIAN_POINT('Ctrl Pts',(-67.6954496350063,-19.1258458580345,
0.));
#81335=CARTESIAN_POINT('Ctrl Pts',(-67.6954496350063,-19.1258458580345,
12.));
#81336=CARTESIAN_POINT('Ctrl Pts',(-67.7128091219348,-19.136565365709,0.));
#81337=CARTESIAN_POINT('Ctrl Pts',(-67.7128091219348,-19.136565365709,12.));
#81338=CARTESIAN_POINT('Ctrl Pts',(-67.7302012056584,-19.1473304119955,
0.));
#81339=CARTESIAN_POINT('Ctrl Pts',(-67.7302012056584,-19.1473304119955,
12.));
#81340=CARTESIAN_POINT('Ctrl Pts',(-67.7476256934444,-19.1581409758097,
0.));
#81341=CARTESIAN_POINT('Ctrl Pts',(-67.7476256934444,-19.1581409758097,
12.));
#81342=CARTESIAN_POINT('Ctrl Pts',(-67.7650823965127,-19.168997036495,0.));
#81343=CARTESIAN_POINT('Ctrl Pts',(-67.7650823965127,-19.168997036495,12.));
#81344=CARTESIAN_POINT('Ctrl Pts',(-67.7825711283096,-19.1798985735688,
0.));
#81345=CARTESIAN_POINT('Ctrl Pts',(-67.7825711283096,-19.1798985735688,
12.));
#81346=CARTESIAN_POINT('Ctrl Pts',(-67.8000917023926,-19.1908455664098,
0.));
#81347=CARTESIAN_POINT('Ctrl Pts',(-67.8000917023926,-19.1908455664098,
12.));
#81348=CARTESIAN_POINT('Ctrl Pts',(-67.8176439306621,-19.201837993993,0.));
#81349=CARTESIAN_POINT('Ctrl Pts',(-67.8176439306621,-19.201837993993,12.));
#81350=CARTESIAN_POINT('Ctrl Pts',(-67.835227624289,-19.2128758350346,0.));
#81351=CARTESIAN_POINT('Ctrl Pts',(-67.835227624289,-19.2128758350346,12.));
#81352=CARTESIAN_POINT('Ctrl Pts',(-67.8528425945184,-19.2239590681133,
0.));
#81353=CARTESIAN_POINT('Ctrl Pts',(-67.8528425945184,-19.2239590681133,
12.));
#81354=CARTESIAN_POINT('Ctrl Pts',(-67.8704886534544,-19.2350876717874,
0.));
#81355=CARTESIAN_POINT('Ctrl Pts',(-67.8704886534544,-19.2350876717874,
12.));
#81356=CARTESIAN_POINT('Ctrl Pts',(-67.8881656149955,-19.2462616247279,
0.));
#81357=CARTESIAN_POINT('Ctrl Pts',(-67.8881656149955,-19.2462616247279,
12.));
#81358=CARTESIAN_POINT('Ctrl Pts',(-67.9058732951788,-19.2574809057696,
0.));
#81359=CARTESIAN_POINT('Ctrl Pts',(-67.9058732951788,-19.2574809057696,
12.));
#81360=CARTESIAN_POINT('Ctrl Pts',(-67.9236115116758,-19.2687454938442,
0.));
#81361=CARTESIAN_POINT('Ctrl Pts',(-67.9236115116758,-19.2687454938442,
12.));
#81362=CARTESIAN_POINT('Ctrl Pts',(-67.9413800834793,-19.280055367936,0.));
#81363=CARTESIAN_POINT('Ctrl Pts',(-67.9413800834793,-19.280055367936,12.));
#81364=CARTESIAN_POINT('Ctrl Pts',(-67.9591788305394,-19.2914105070286,
0.));
#81365=CARTESIAN_POINT('Ctrl Pts',(-67.9591788305394,-19.2914105070286,
12.));
#81366=CARTESIAN_POINT('Ctrl Pts',(-67.9770075733485,-19.302810890038,0.));
#81367=CARTESIAN_POINT('Ctrl Pts',(-67.9770075733485,-19.302810890038,12.));
#81368=CARTESIAN_POINT('Ctrl Pts',(-67.9948661329617,-19.3142564958203,
0.));
#81369=CARTESIAN_POINT('Ctrl Pts',(-67.9948661329617,-19.3142564958203,
12.));
#81370=CARTESIAN_POINT('Ctrl Pts',(-68.0127543311776,-19.3257473032035,
0.));
#81371=CARTESIAN_POINT('Ctrl Pts',(-68.0127543311776,-19.3257473032035,
12.));
#81372=CARTESIAN_POINT('Ctrl Pts',(-68.0306719906636,-19.3372832910076,
0.));
#81373=CARTESIAN_POINT('Ctrl Pts',(-68.0306719906636,-19.3372832910076,
12.));
#81374=CARTESIAN_POINT('Ctrl Pts',(-68.0486189351011,-19.3488644380641,
0.));
#81375=CARTESIAN_POINT('Ctrl Pts',(-68.0486189351011,-19.3488644380641,
12.));
#81376=CARTESIAN_POINT('Ctrl Pts',(-68.0665949893195,-19.3604907232314,
0.));
#81377=CARTESIAN_POINT('Ctrl Pts',(-68.0665949893195,-19.3604907232314,
12.));
#81378=CARTESIAN_POINT('Ctrl Pts',(-68.0845999792247,-19.3721621253912,
0.));
#81379=CARTESIAN_POINT('Ctrl Pts',(-68.0845999792247,-19.3721621253912,
12.));
#81380=CARTESIAN_POINT('Ctrl Pts',(-68.1026337317285,-19.3838786234421,
0.));
#81381=CARTESIAN_POINT('Ctrl Pts',(-68.1026337317285,-19.3838786234421,
12.));
#81382=CARTESIAN_POINT('Ctrl Pts',(-68.1206960746769,-19.3956401962895,
0.));
#81383=CARTESIAN_POINT('Ctrl Pts',(-68.1206960746769,-19.3956401962895,
12.));
#81384=CARTESIAN_POINT('Ctrl Pts',(-68.1387868367691,-19.40744682283,0.));
#81385=CARTESIAN_POINT('Ctrl Pts',(-68.1387868367691,-19.40744682283,12.));
#81386=CARTESIAN_POINT('Ctrl Pts',(-68.1569058475054,-19.4192984819418,
0.));
#81387=CARTESIAN_POINT('Ctrl Pts',(-68.1569058475054,-19.4192984819418,
12.));
#81388=CARTESIAN_POINT('Ctrl Pts',(-68.1750529372232,-19.4311951524983,
0.));
#81389=CARTESIAN_POINT('Ctrl Pts',(-68.1750529372232,-19.4311951524983,
12.));
#81390=CARTESIAN_POINT('Ctrl Pts',(-68.1932279371127,-19.4431368133719,
0.));
#81391=CARTESIAN_POINT('Ctrl Pts',(-68.1932279371127,-19.4431368133719,
12.));
#81392=CARTESIAN_POINT('Ctrl Pts',(-68.2114306792358,-19.4551234434381,
0.));
#81393=CARTESIAN_POINT('Ctrl Pts',(-68.2114306792358,-19.4551234434381,
12.));
#81394=CARTESIAN_POINT('Ctrl Pts',(-68.2296609965448,-19.467155021572,0.));
#81395=CARTESIAN_POINT('Ctrl Pts',(-68.2296609965448,-19.467155021572,12.));
#81396=CARTESIAN_POINT('Ctrl Pts',(-68.2479187228803,-19.4792315266501,
0.));
#81397=CARTESIAN_POINT('Ctrl Pts',(-68.2479187228803,-19.4792315266501,
12.));
#81398=CARTESIAN_POINT('Ctrl Pts',(-68.2662036929526,-19.4913529375543,
0.));
#81399=CARTESIAN_POINT('Ctrl Pts',(-68.2662036929526,-19.4913529375543,
12.));
#81400=CARTESIAN_POINT('Ctrl Pts',(-68.2845157423233,-19.5035192331705,
0.));
#81401=CARTESIAN_POINT('Ctrl Pts',(-68.2845157423233,-19.5035192331705,
12.));
#81402=CARTESIAN_POINT('Ctrl Pts',(-68.3028547073864,-19.5157303923856,
0.));
#81403=CARTESIAN_POINT('Ctrl Pts',(-68.3028547073864,-19.5157303923856,
12.));
#81404=CARTESIAN_POINT('Ctrl Pts',(-68.3212204253417,-19.5279863940773,
0.));
#81405=CARTESIAN_POINT('Ctrl Pts',(-68.3212204253417,-19.5279863940773,
12.));
#81406=CARTESIAN_POINT('Ctrl Pts',(-68.3396127341938,-19.5402872171191,
0.));
#81407=CARTESIAN_POINT('Ctrl Pts',(-68.3396127341938,-19.5402872171191,
12.));
#81408=CARTESIAN_POINT('Ctrl Pts',(-68.3580314727523,-19.5526328403852,
0.));
#81409=CARTESIAN_POINT('Ctrl Pts',(-68.3580314727523,-19.5526328403852,
12.));
#81410=CARTESIAN_POINT('Ctrl Pts',(-68.3764764806287,-19.5650232427516,
0.));
#81411=CARTESIAN_POINT('Ctrl Pts',(-68.3764764806287,-19.5650232427516,
12.));
#81412=CARTESIAN_POINT('Ctrl Pts',(-68.3949475982335,-19.5774584030938,
0.));
#81413=CARTESIAN_POINT('Ctrl Pts',(-68.3949475982335,-19.5774584030938,
12.));
#81414=CARTESIAN_POINT('Ctrl Pts',(-68.4134446667696,-19.5899383002803,
0.));
#81415=CARTESIAN_POINT('Ctrl Pts',(-68.4134446667696,-19.5899383002803,
12.));
#81416=CARTESIAN_POINT('Ctrl Pts',(-68.4319675282275,-19.6024629131785,
0.));
#81417=CARTESIAN_POINT('Ctrl Pts',(-68.4319675282275,-19.6024629131785,
12.));
#81418=CARTESIAN_POINT('Ctrl Pts',(-68.4505160253778,-19.6150322206577,
0.));
#81419=CARTESIAN_POINT('Ctrl Pts',(-68.4505160253778,-19.6150322206577,
12.));
#81420=CARTESIAN_POINT('Ctrl Pts',(-68.4690900017632,-19.6276462015888,
0.));
#81421=CARTESIAN_POINT('Ctrl Pts',(-68.4690900017632,-19.6276462015888,
12.));
#81422=CARTESIAN_POINT('Ctrl Pts',(-68.4876893016856,-19.6403048348395,
0.));
#81423=CARTESIAN_POINT('Ctrl Pts',(-68.4876893016856,-19.6403048348395,
12.));
#81424=CARTESIAN_POINT('Ctrl Pts',(-68.5063137701971,-19.6530080992686,
0.));
#81425=CARTESIAN_POINT('Ctrl Pts',(-68.5063137701971,-19.6530080992686,
12.));
#81426=CARTESIAN_POINT('Ctrl Pts',(-68.5249632530979,-19.6657559737336,
0.));
#81427=CARTESIAN_POINT('Ctrl Pts',(-68.5249632530979,-19.6657559737336,
12.));
#81428=CARTESIAN_POINT('Ctrl Pts',(-68.5436375969311,-19.6785484370927,
0.));
#81429=CARTESIAN_POINT('Ctrl Pts',(-68.5436375969311,-19.6785484370927,
12.));
#81430=CARTESIAN_POINT('Ctrl Pts',(-68.5623366489779,-19.6913854682046,
0.));
#81431=CARTESIAN_POINT('Ctrl Pts',(-68.5623366489779,-19.6913854682046,
12.));
#81432=CARTESIAN_POINT('Ctrl Pts',(-68.581060257249,-19.7042670459237,0.));
#81433=CARTESIAN_POINT('Ctrl Pts',(-68.581060257249,-19.7042670459237,12.));
#81434=CARTESIAN_POINT('Ctrl Pts',(-68.5998082704766,-19.7171931490956,
0.));
#81435=CARTESIAN_POINT('Ctrl Pts',(-68.5998082704766,-19.7171931490956,
12.));
#81436=CARTESIAN_POINT('Ctrl Pts',(-68.6185805381126,-19.7301637565652,
0.));
#81437=CARTESIAN_POINT('Ctrl Pts',(-68.6185805381126,-19.7301637565652,
12.));
#81438=CARTESIAN_POINT('Ctrl Pts',(-68.6373769103224,-19.7431788471776,
0.));
#81439=CARTESIAN_POINT('Ctrl Pts',(-68.6373769103224,-19.7431788471776,
12.));
#81440=CARTESIAN_POINT('Ctrl Pts',(-68.6561972379793,-19.7562383997781,
0.));
#81441=CARTESIAN_POINT('Ctrl Pts',(-68.6561972379793,-19.7562383997781,
12.));
#81442=CARTESIAN_POINT('Ctrl Pts',(-68.6750413726547,-19.7693423932058,
0.));
#81443=CARTESIAN_POINT('Ctrl Pts',(-68.6750413726547,-19.7693423932058,
12.));
#81444=CARTESIAN_POINT('Ctrl Pts',(-68.6939091666111,-19.7824908062913,
0.));
#81445=CARTESIAN_POINT('Ctrl Pts',(-68.6939091666111,-19.7824908062913,
12.));
#81446=CARTESIAN_POINT('Ctrl Pts',(-68.7128004727998,-19.795683617864,0.));
#81447=CARTESIAN_POINT('Ctrl Pts',(-68.7128004727998,-19.795683617864,12.));
#81448=CARTESIAN_POINT('Ctrl Pts',(-68.7317151448557,-19.8089208067532,
0.));
#81449=CARTESIAN_POINT('Ctrl Pts',(-68.7317151448557,-19.8089208067532,
12.));
#81450=CARTESIAN_POINT('Ctrl Pts',(-68.7506530370918,-19.8222023517874,
0.));
#81451=CARTESIAN_POINT('Ctrl Pts',(-68.7506530370918,-19.8222023517874,
12.));
#81452=CARTESIAN_POINT('Ctrl Pts',(-68.7696140044892,-19.835528231787,0.));
#81453=CARTESIAN_POINT('Ctrl Pts',(-68.7696140044892,-19.835528231787,12.));
#81454=CARTESIAN_POINT('Ctrl Pts',(-68.7885979026927,-19.8488984255642,
0.));
#81455=CARTESIAN_POINT('Ctrl Pts',(-68.7885979026927,-19.8488984255642,
12.));
#81456=CARTESIAN_POINT('Ctrl Pts',(-68.8076045880102,-19.8623129119304,
0.));
#81457=CARTESIAN_POINT('Ctrl Pts',(-68.8076045880102,-19.8623129119304,
12.));
#81458=CARTESIAN_POINT('Ctrl Pts',(-68.8266339174068,-19.8757716696969,
0.));
#81459=CARTESIAN_POINT('Ctrl Pts',(-68.8266339174068,-19.8757716696969,
12.));
#81460=CARTESIAN_POINT('Ctrl Pts',(-68.8456857484988,-19.8892746776734,
0.));
#81461=CARTESIAN_POINT('Ctrl Pts',(-68.8456857484988,-19.8892746776734,
12.));
#81462=CARTESIAN_POINT('Ctrl Pts',(-68.8647599395437,-19.9028219146607,
0.));
#81463=CARTESIAN_POINT('Ctrl Pts',(-68.8647599395437,-19.9028219146607,
12.));
#81464=CARTESIAN_POINT('Ctrl Pts',(-68.8838563494356,-19.9164133594513,
0.));
#81465=CARTESIAN_POINT('Ctrl Pts',(-68.8838563494356,-19.9164133594513,
12.));
#81466=CARTESIAN_POINT('Ctrl Pts',(-68.902974837704,-19.9300489908364,0.));
#81467=CARTESIAN_POINT('Ctrl Pts',(-68.902974837704,-19.9300489908364,12.));
#81468=CARTESIAN_POINT('Ctrl Pts',(-68.9221152645086,-19.9437287876063,
0.));
#81469=CARTESIAN_POINT('Ctrl Pts',(-68.9221152645086,-19.9437287876063,
12.));
#81470=CARTESIAN_POINT('Ctrl Pts',(-68.9412774906346,-19.9574527285492,
0.));
#81471=CARTESIAN_POINT('Ctrl Pts',(-68.9412774906346,-19.9574527285492,
12.));
#81472=CARTESIAN_POINT('Ctrl Pts',(-68.960461377483,-19.9712207924437,0.));
#81473=CARTESIAN_POINT('Ctrl Pts',(-68.960461377483,-19.9712207924437,12.));
#81474=CARTESIAN_POINT('Ctrl Pts',(-68.9796667870667,-19.98503295806,0.));
#81475=CARTESIAN_POINT('Ctrl Pts',(-68.9796667870667,-19.98503295806,12.));
#81476=CARTESIAN_POINT('Ctrl Pts',(-68.9988935820101,-19.9988892041671,
0.));
#81477=CARTESIAN_POINT('Ctrl Pts',(-68.9988935820101,-19.9988892041671,
12.));
#81478=CARTESIAN_POINT('Ctrl Pts',(-69.0181416255433,-20.0127895095327,
0.));
#81479=CARTESIAN_POINT('Ctrl Pts',(-69.0181416255433,-20.0127895095327,
12.));
#81480=CARTESIAN_POINT('Ctrl Pts',(-69.0374107814977,-20.0267338529221,
0.));
#81481=CARTESIAN_POINT('Ctrl Pts',(-69.0374107814977,-20.0267338529221,
12.));
#81482=CARTESIAN_POINT('Ctrl Pts',(-69.0567009142968,-20.0407222130902,
0.));
#81483=CARTESIAN_POINT('Ctrl Pts',(-69.0567009142968,-20.0407222130902,
12.));
#81484=CARTESIAN_POINT('Ctrl Pts',(-69.0760118889525,-20.0547545687839,
0.));
#81485=CARTESIAN_POINT('Ctrl Pts',(-69.0760118889525,-20.0547545687839,
12.));
#81486=CARTESIAN_POINT('Ctrl Pts',(-69.0953435710634,-20.0688308987478,
0.));
#81487=CARTESIAN_POINT('Ctrl Pts',(-69.0953435710634,-20.0688308987478,
12.));
#81488=CARTESIAN_POINT('Ctrl Pts',(-69.1146958268104,-20.0829511817251,
0.));
#81489=CARTESIAN_POINT('Ctrl Pts',(-69.1146958268104,-20.0829511817251,
12.));
#81490=CARTESIAN_POINT('Ctrl Pts',(-69.1340685229516,-20.0971153964557,
0.));
#81491=CARTESIAN_POINT('Ctrl Pts',(-69.1340685229516,-20.0971153964557,
12.));
#81492=CARTESIAN_POINT('Ctrl Pts',(-69.1534615268153,-20.1113235216694,
0.));
#81493=CARTESIAN_POINT('Ctrl Pts',(-69.1534615268153,-20.1113235216694,
12.));
#81494=CARTESIAN_POINT('Ctrl Pts',(-69.172874706296,-20.1255755360871,0.));
#81495=CARTESIAN_POINT('Ctrl Pts',(-69.172874706296,-20.1255755360871,12.));
#81496=CARTESIAN_POINT('Ctrl Pts',(-69.1923079298534,-20.1398714184278,
0.));
#81497=CARTESIAN_POINT('Ctrl Pts',(-69.1923079298534,-20.1398714184278,
12.));
#81498=CARTESIAN_POINT('Ctrl Pts',(-69.2117610665073,-20.1542111474086,
0.));
#81499=CARTESIAN_POINT('Ctrl Pts',(-69.2117610665073,-20.1542111474086,
12.));
#81500=CARTESIAN_POINT('Ctrl Pts',(-69.2312339858337,-20.1685947017433,
0.));
#81501=CARTESIAN_POINT('Ctrl Pts',(-69.2312339858337,-20.1685947017433,
12.));
#81502=CARTESIAN_POINT('Ctrl Pts',(-69.2507265579562,-20.183022060135,0.));
#81503=CARTESIAN_POINT('Ctrl Pts',(-69.2507265579562,-20.183022060135,12.));
#81504=CARTESIAN_POINT('Ctrl Pts',(-69.2702386535432,-20.1974932012775,
0.));
#81505=CARTESIAN_POINT('Ctrl Pts',(-69.2702386535432,-20.1974932012775,
12.));
#81506=CARTESIAN_POINT('Ctrl Pts',(-69.2897701438066,-20.2120081038622,
0.));
#81507=CARTESIAN_POINT('Ctrl Pts',(-69.2897701438066,-20.2120081038622,
12.));
#81508=CARTESIAN_POINT('Ctrl Pts',(-69.3093209004986,-20.2265667465784,
0.));
#81509=CARTESIAN_POINT('Ctrl Pts',(-69.3093209004986,-20.2265667465784,
12.));
#81510=CARTESIAN_POINT('Ctrl Pts',(-69.3288907959065,-20.2411691081122,
0.));
#81511=CARTESIAN_POINT('Ctrl Pts',(-69.3288907959065,-20.2411691081122,
12.));
#81512=CARTESIAN_POINT('Ctrl Pts',(-69.3484797028454,-20.255815167139,0.));
#81513=CARTESIAN_POINT('Ctrl Pts',(-69.3484797028454,-20.255815167139,12.));
#81514=CARTESIAN_POINT('Ctrl Pts',(-69.3680874946548,-20.2705049023241,
0.));
#81515=CARTESIAN_POINT('Ctrl Pts',(-69.3680874946548,-20.2705049023241,
12.));
#81516=CARTESIAN_POINT('Ctrl Pts',(-69.3877140451975,-20.2852382923299,
0.));
#81517=CARTESIAN_POINT('Ctrl Pts',(-69.3877140451975,-20.2852382923299,
12.));
#81518=CARTESIAN_POINT('Ctrl Pts',(-69.4073592288562,-20.3000153158167,
0.));
#81519=CARTESIAN_POINT('Ctrl Pts',(-69.4073592288562,-20.3000153158167,
12.));
#81520=CARTESIAN_POINT('Ctrl Pts',(-69.4270229205296,-20.3148359514414,
0.));
#81521=CARTESIAN_POINT('Ctrl Pts',(-69.4270229205296,-20.3148359514414,
12.));
#81522=CARTESIAN_POINT('Ctrl Pts',(-69.4467049956257,-20.3297001778505,
0.));
#81523=CARTESIAN_POINT('Ctrl Pts',(-69.4467049956257,-20.3297001778505,
12.));
#81524=CARTESIAN_POINT('Ctrl Pts',(-69.4664053300579,-20.3446079736799,
0.));
#81525=CARTESIAN_POINT('Ctrl Pts',(-69.4664053300579,-20.3446079736799,
12.));
#81526=CARTESIAN_POINT('Ctrl Pts',(-69.4861238002433,-20.359559317562,0.));
#81527=CARTESIAN_POINT('Ctrl Pts',(-69.4861238002433,-20.359559317562,12.));
#81528=CARTESIAN_POINT('Ctrl Pts',(-69.5058602831004,-20.3745541881267,
0.));
#81529=CARTESIAN_POINT('Ctrl Pts',(-69.5058602831004,-20.3745541881267,
12.));
#81530=CARTESIAN_POINT('Ctrl Pts',(-69.5256146560444,-20.3895925640006,
0.));
#81531=CARTESIAN_POINT('Ctrl Pts',(-69.5256146560444,-20.3895925640006,
12.));
#81532=CARTESIAN_POINT('Ctrl Pts',(-69.5453867969815,-20.4046744238002,
0.));
#81533=CARTESIAN_POINT('Ctrl Pts',(-69.5453867969815,-20.4046744238002,
12.));
#81534=CARTESIAN_POINT('Ctrl Pts',(-69.565176584305,-20.4197997461306,0.));
#81535=CARTESIAN_POINT('Ctrl Pts',(-69.565176584305,-20.4197997461306,12.));
#81536=CARTESIAN_POINT('Ctrl Pts',(-69.5849838968944,-20.4349685095928,
0.));
#81537=CARTESIAN_POINT('Ctrl Pts',(-69.5849838968944,-20.4349685095928,
12.));
#81538=CARTESIAN_POINT('Ctrl Pts',(-69.6048086141122,-20.4501806927854,
0.));
#81539=CARTESIAN_POINT('Ctrl Pts',(-69.6048086141122,-20.4501806927854,
12.));
#81540=CARTESIAN_POINT('Ctrl Pts',(-69.6246506158009,-20.4654362743036,
0.));
#81541=CARTESIAN_POINT('Ctrl Pts',(-69.6246506158009,-20.4654362743036,
12.));
#81542=CARTESIAN_POINT('Ctrl Pts',(-69.6445097822778,-20.4807352327335,
0.));
#81543=CARTESIAN_POINT('Ctrl Pts',(-69.6445097822778,-20.4807352327335,
12.));
#81544=CARTESIAN_POINT('Ctrl Pts',(-69.6643859943291,-20.4960775466487,
0.));
#81545=CARTESIAN_POINT('Ctrl Pts',(-69.6643859943291,-20.4960775466487,
12.));
#81546=CARTESIAN_POINT('Ctrl Pts',(-69.6842791332102,-20.511463194618,0.));
#81547=CARTESIAN_POINT('Ctrl Pts',(-69.6842791332102,-20.511463194618,12.));
#81548=CARTESIAN_POINT('Ctrl Pts',(-69.7041890806421,-20.5268921552076,
0.));
#81549=CARTESIAN_POINT('Ctrl Pts',(-69.7041890806421,-20.5268921552076,
12.));
#81550=CARTESIAN_POINT('Ctrl Pts',(-69.7241157188086,-20.54236440698,0.));
#81551=CARTESIAN_POINT('Ctrl Pts',(-69.7241157188086,-20.54236440698,12.));
#81552=CARTESIAN_POINT('Ctrl Pts',(-69.7440589303511,-20.5578799284898,
0.));
#81553=CARTESIAN_POINT('Ctrl Pts',(-69.7440589303511,-20.5578799284898,
12.));
#81554=CARTESIAN_POINT('Ctrl Pts',(-69.7640185983641,-20.5734386982782,
0.));
#81555=CARTESIAN_POINT('Ctrl Pts',(-69.7640185983641,-20.5734386982782,
12.));
#81556=CARTESIAN_POINT('Ctrl Pts',(-69.7839946063942,-20.5890406948809,
0.));
#81557=CARTESIAN_POINT('Ctrl Pts',(-69.7839946063942,-20.5890406948809,
12.));
#81558=CARTESIAN_POINT('Ctrl Pts',(-69.8039868384382,-20.6046858968305,
0.));
#81559=CARTESIAN_POINT('Ctrl Pts',(-69.8039868384382,-20.6046858968305,
12.));
#81560=CARTESIAN_POINT('Ctrl Pts',(-69.8239951789402,-20.6203742826566,
0.));
#81561=CARTESIAN_POINT('Ctrl Pts',(-69.8239951789402,-20.6203742826566,
12.));
#81562=CARTESIAN_POINT('Ctrl Pts',(-69.8440195127874,-20.6361058308812,
0.));
#81563=CARTESIAN_POINT('Ctrl Pts',(-69.8440195127874,-20.6361058308812,
12.));
#81564=CARTESIAN_POINT('Ctrl Pts',(-69.8640597253058,-20.6518805200132,
0.));
#81565=CARTESIAN_POINT('Ctrl Pts',(-69.8640597253058,-20.6518805200132,
12.));
#81566=CARTESIAN_POINT('Ctrl Pts',(-69.884115702258,-20.6676983285542,0.));
#81567=CARTESIAN_POINT('Ctrl Pts',(-69.884115702258,-20.6676983285542,12.));
#81568=CARTESIAN_POINT('Ctrl Pts',(-69.9041873298416,-20.6835592350031,
0.));
#81569=CARTESIAN_POINT('Ctrl Pts',(-69.9041873298416,-20.6835592350031,
12.));
#81570=CARTESIAN_POINT('Ctrl Pts',(-69.9242744946854,-20.6994632178551,
0.));
#81571=CARTESIAN_POINT('Ctrl Pts',(-69.9242744946854,-20.6994632178551,
12.));
#81572=CARTESIAN_POINT('Ctrl Pts',(-69.9443770838444,-20.7154102555996,
0.));
#81573=CARTESIAN_POINT('Ctrl Pts',(-69.9443770838444,-20.7154102555996,
12.));
#81574=CARTESIAN_POINT('Ctrl Pts',(-69.9644949847929,-20.7314003267118,
0.));
#81575=CARTESIAN_POINT('Ctrl Pts',(-69.9644949847929,-20.7314003267118,
12.));
#81576=CARTESIAN_POINT('Ctrl Pts',(-69.9846280854254,-20.7474334096582,
0.));
#81577=CARTESIAN_POINT('Ctrl Pts',(-69.9846280854254,-20.7474334096582,
12.));
#81578=CARTESIAN_POINT('Ctrl Pts',(-70.0047762740569,-20.7635094829017,
0.));
#81579=CARTESIAN_POINT('Ctrl Pts',(-70.0047762740569,-20.7635094829017,
12.));
#81580=CARTESIAN_POINT('Ctrl Pts',(-70.0249394394221,-20.7796285249023,
0.));
#81581=CARTESIAN_POINT('Ctrl Pts',(-70.0249394394221,-20.7796285249023,
12.));
#81582=CARTESIAN_POINT('Ctrl Pts',(-70.0451174706739,-20.7957905141155,
0.));
#81583=CARTESIAN_POINT('Ctrl Pts',(-70.0451174706739,-20.7957905141155,
12.));
#81584=CARTESIAN_POINT('Ctrl Pts',(-70.0653102573798,-20.8119954289846,
0.));
#81585=CARTESIAN_POINT('Ctrl Pts',(-70.0653102573798,-20.8119954289846,
12.));
#81586=CARTESIAN_POINT('Ctrl Pts',(-70.0855176895185,-20.8282432479425,
0.));
#81587=CARTESIAN_POINT('Ctrl Pts',(-70.0855176895185,-20.8282432479425,
12.));
#81588=CARTESIAN_POINT('Ctrl Pts',(-70.1057396574741,-20.8445339494185,
0.));
#81589=CARTESIAN_POINT('Ctrl Pts',(-70.1057396574741,-20.8445339494185,
12.));
#81590=CARTESIAN_POINT('Ctrl Pts',(-70.1259760520306,-20.8608675118377,
0.));
#81591=CARTESIAN_POINT('Ctrl Pts',(-70.1259760520306,-20.8608675118377,
12.));
#81592=CARTESIAN_POINT('Ctrl Pts',(-70.1462267643649,-20.8772439136207,
0.));
#81593=CARTESIAN_POINT('Ctrl Pts',(-70.1462267643649,-20.8772439136207,
12.));
#81594=CARTESIAN_POINT('Ctrl Pts',(-70.1664916860366,-20.8936631331751,
0.));
#81595=CARTESIAN_POINT('Ctrl Pts',(-70.1664916860366,-20.8936631331751,
12.));
#81596=CARTESIAN_POINT('Ctrl Pts',(-70.1867707089866,-20.9101251488948,
0.));
#81597=CARTESIAN_POINT('Ctrl Pts',(-70.1867707089866,-20.9101251488948,
12.));
#81598=CARTESIAN_POINT('Ctrl Pts',(-70.2070637255469,-20.9266299391688,
0.));
#81599=CARTESIAN_POINT('Ctrl Pts',(-70.2070637255469,-20.9266299391688,
12.));
#81600=CARTESIAN_POINT('Ctrl Pts',(-70.2273706284479,-20.9431774823833,
0.));
#81601=CARTESIAN_POINT('Ctrl Pts',(-70.2273706284479,-20.9431774823833,
12.));
#81602=CARTESIAN_POINT('Ctrl Pts',(-70.2476913108242,-20.9597677569227,
0.));
#81603=CARTESIAN_POINT('Ctrl Pts',(-70.2476913108242,-20.9597677569227,
12.));
#81604=CARTESIAN_POINT('Ctrl Pts',(-70.2680256662215,-20.9764007411649,
0.));
#81605=CARTESIAN_POINT('Ctrl Pts',(-70.2680256662215,-20.9764007411649,
12.));
#81606=CARTESIAN_POINT('Ctrl Pts',(-70.288373588597,-20.9930764134771,0.));
#81607=CARTESIAN_POINT('Ctrl Pts',(-70.288373588597,-20.9930764134771,12.));
#81608=CARTESIAN_POINT('Ctrl Pts',(-70.3087349722959,-21.0097947522212,
0.));
#81609=CARTESIAN_POINT('Ctrl Pts',(-70.3087349722959,-21.0097947522212,
12.));
#81610=CARTESIAN_POINT('Ctrl Pts',(-70.3291097120293,-21.0265557357544,
0.));
#81611=CARTESIAN_POINT('Ctrl Pts',(-70.3291097120293,-21.0265557357544,
12.));
#81612=CARTESIAN_POINT('Ctrl Pts',(-70.3494977028497,-21.0433593424266,
0.));
#81613=CARTESIAN_POINT('Ctrl Pts',(-70.3494977028497,-21.0433593424266,
12.));
#81614=CARTESIAN_POINT('Ctrl Pts',(-70.3698988401291,-21.0602055505751,
0.));
#81615=CARTESIAN_POINT('Ctrl Pts',(-70.3698988401291,-21.0602055505751,
12.));
#81616=CARTESIAN_POINT('Ctrl Pts',(-70.3903130195279,-21.0770943385146,
0.));
#81617=CARTESIAN_POINT('Ctrl Pts',(-70.3903130195279,-21.0770943385146,
12.));
#81618=CARTESIAN_POINT('Ctrl Pts',(-70.4107401370403,-21.0940256845477,
0.));
#81619=CARTESIAN_POINT('Ctrl Pts',(-70.4107401370403,-21.0940256845477,
12.));
#81620=CARTESIAN_POINT('Ctrl Pts',(-70.4311800890411,-21.110999566975,0.));
#81621=CARTESIAN_POINT('Ctrl Pts',(-70.4311800890411,-21.110999566975,12.));
#81622=CARTESIAN_POINT('Ctrl Pts',(-70.4516327723349,-21.1280159641003,
0.));
#81623=CARTESIAN_POINT('Ctrl Pts',(-70.4516327723349,-21.1280159641003,
12.));
#81624=CARTESIAN_POINT('Ctrl Pts',(-70.4720980841934,-21.1450748542335,
0.));
#81625=CARTESIAN_POINT('Ctrl Pts',(-70.4720980841934,-21.1450748542335,
12.));
#81626=CARTESIAN_POINT('Ctrl Pts',(-70.4925759224208,-21.1621762156894,
0.));
#81627=CARTESIAN_POINT('Ctrl Pts',(-70.4925759224208,-21.1621762156894,
12.));
#81628=CARTESIAN_POINT('Ctrl Pts',(-70.5130661852946,-21.1793200267844,
0.));
#81629=CARTESIAN_POINT('Ctrl Pts',(-70.5130661852946,-21.1793200267844,
12.));
#81630=CARTESIAN_POINT('Ctrl Pts',(-70.5335687714422,-21.1965062658296,
0.));
#81631=CARTESIAN_POINT('Ctrl Pts',(-70.5335687714422,-21.1965062658296,
12.));
#81632=CARTESIAN_POINT('Ctrl Pts',(-70.5540835797281,-21.2137349111207,
0.));
#81633=CARTESIAN_POINT('Ctrl Pts',(-70.5540835797281,-21.2137349111207,
12.));
#81634=CARTESIAN_POINT('Ctrl Pts',(-70.5746105091503,-21.2310059409265,
0.));
#81635=CARTESIAN_POINT('Ctrl Pts',(-70.5746105091503,-21.2310059409265,
12.));
#81636=CARTESIAN_POINT('Ctrl Pts',(-70.5951494586961,-21.2483193334677,
0.));
#81637=CARTESIAN_POINT('Ctrl Pts',(-70.5951494586961,-21.2483193334677,
12.));
#81638=CARTESIAN_POINT('Ctrl Pts',(-70.6157003273326,-21.2656750669129,
0.));
#81639=CARTESIAN_POINT('Ctrl Pts',(-70.6157003273326,-21.2656750669129,
12.));
#81640=CARTESIAN_POINT('Ctrl Pts',(-70.6362630143062,-21.2830731194188,
0.));
#81641=CARTESIAN_POINT('Ctrl Pts',(-70.6362630143062,-21.2830731194188,
12.));
#81642=CARTESIAN_POINT('Ctrl Pts',(-70.6568374193786,-21.3005134691563,
0.));
#81643=CARTESIAN_POINT('Ctrl Pts',(-70.6568374193786,-21.3005134691563,
12.));
#81644=CARTESIAN_POINT('Ctrl Pts',(-70.6774234430899,-21.3179960943389,
0.));
#81645=CARTESIAN_POINT('Ctrl Pts',(-70.6774234430899,-21.3179960943389,
12.));
#81646=CARTESIAN_POINT('Ctrl Pts',(-70.6980209870032,-21.3355209732438,
0.));
#81647=CARTESIAN_POINT('Ctrl Pts',(-70.6980209870032,-21.3355209732438,
12.));
#81648=CARTESIAN_POINT('Ctrl Pts',(-70.7186299539698,-21.353088084234,0.));
#81649=CARTESIAN_POINT('Ctrl Pts',(-70.7186299539698,-21.353088084234,12.));
#81650=CARTESIAN_POINT('Ctrl Pts',(-70.7392502475437,-21.3706974057028,
0.));
#81651=CARTESIAN_POINT('Ctrl Pts',(-70.7392502475437,-21.3706974057028,
12.));
#81652=CARTESIAN_POINT('Ctrl Pts',(-70.7598817714078,-21.3883489160187,
0.));
#81653=CARTESIAN_POINT('Ctrl Pts',(-70.7598817714078,-21.3883489160187,
12.));
#81654=CARTESIAN_POINT('Ctrl Pts',(-70.780524428744,-21.4060425934595,0.));
#81655=CARTESIAN_POINT('Ctrl Pts',(-70.780524428744,-21.4060425934595,12.));
#81656=CARTESIAN_POINT('Ctrl Pts',(-70.8011781217409,-21.4237784161592,
0.));
#81657=CARTESIAN_POINT('Ctrl Pts',(-70.8011781217409,-21.4237784161592,
12.));
#81658=CARTESIAN_POINT('Ctrl Pts',(-70.8218427507545,-21.4415563620127,
0.));
#81659=CARTESIAN_POINT('Ctrl Pts',(-70.8218427507545,-21.4415563620127,
12.));
#81660=CARTESIAN_POINT('Ctrl Pts',(-70.84251821499,-21.4593764087492,0.));
#81661=CARTESIAN_POINT('Ctrl Pts',(-70.84251821499,-21.4593764087492,12.));
#81662=CARTESIAN_POINT('Ctrl Pts',(-70.8632044140166,-21.4772385340978,
0.));
#81663=CARTESIAN_POINT('Ctrl Pts',(-70.8632044140166,-21.4772385340978,
12.));
#81664=CARTESIAN_POINT('Ctrl Pts',(-70.8839012490903,-21.4951427159272,
0.));
#81665=CARTESIAN_POINT('Ctrl Pts',(-70.8839012490903,-21.4951427159272,
12.));
#81666=CARTESIAN_POINT('Ctrl Pts',(-70.9046086244123,-21.5130889323767,
0.));
#81667=CARTESIAN_POINT('Ctrl Pts',(-70.9046086244123,-21.5130889323767,
12.));
#81668=CARTESIAN_POINT('Ctrl Pts',(-70.9253264487576,-21.5310771620209,
0.));
#81669=CARTESIAN_POINT('Ctrl Pts',(-70.9253264487576,-21.5310771620209,
12.));
#81670=CARTESIAN_POINT('Ctrl Pts',(-70.9460546358597,-21.549107383907,0.));
#81671=CARTESIAN_POINT('Ctrl Pts',(-70.9460546358597,-21.549107383907,12.));
#81672=CARTESIAN_POINT('Ctrl Pts',(-70.9667931008097,-21.5671795771873,
0.));
#81673=CARTESIAN_POINT('Ctrl Pts',(-70.9667931008097,-21.5671795771873,
12.));
#81674=CARTESIAN_POINT('Ctrl Pts',(-70.9875417572138,-21.5852937208258,
0.));
#81675=CARTESIAN_POINT('Ctrl Pts',(-70.9875417572138,-21.5852937208258,
12.));
#81676=CARTESIAN_POINT('Ctrl Pts',(-71.0083005139086,-21.6034497932574,
0.));
#81677=CARTESIAN_POINT('Ctrl Pts',(-71.0083005139086,-21.6034497932574,
12.));
#81678=CARTESIAN_POINT('Ctrl Pts',(-71.0290692721932,-21.6216477720941,
0.));
#81679=CARTESIAN_POINT('Ctrl Pts',(-71.0290692721932,-21.6216477720941,
12.));
#81680=CARTESIAN_POINT('Ctrl Pts',(-71.0498479219659,-21.6398876337207,
0.));
#81681=CARTESIAN_POINT('Ctrl Pts',(-71.0498479219659,-21.6398876337207,
12.));
#81682=CARTESIAN_POINT('Ctrl Pts',(-71.0706363472965,-21.6581693538424,
0.));
#81683=CARTESIAN_POINT('Ctrl Pts',(-71.0706363472965,-21.6581693538424,
12.));
#81684=CARTESIAN_POINT('Ctrl Pts',(-71.0914344333048,-21.6764929081763,
0.));
#81685=CARTESIAN_POINT('Ctrl Pts',(-71.0914344333048,-21.6764929081763,
12.));
#81686=CARTESIAN_POINT('Ctrl Pts',(-71.1122420728349,-21.6948582730895,
0.));
#81687=CARTESIAN_POINT('Ctrl Pts',(-71.1122420728349,-21.6948582730895,
12.));
#81688=CARTESIAN_POINT('Ctrl Pts',(-71.133059172642,-21.7132654262501,0.));
#81689=CARTESIAN_POINT('Ctrl Pts',(-71.133059172642,-21.7132654262501,12.));
#81690=CARTESIAN_POINT('Ctrl Pts',(-71.1538856611899,-21.7317143472827,
0.));
#81691=CARTESIAN_POINT('Ctrl Pts',(-71.1538856611899,-21.7317143472827,
12.));
#81692=CARTESIAN_POINT('Ctrl Pts',(-71.1747214905981,-21.7502050183602,
0.));
#81693=CARTESIAN_POINT('Ctrl Pts',(-71.1747214905981,-21.7502050183602,
12.));
#81694=CARTESIAN_POINT('Ctrl Pts',(-71.1955666309591,-21.7687374247046,
0.));
#81695=CARTESIAN_POINT('Ctrl Pts',(-71.1955666309591,-21.7687374247046,
12.));
#81696=CARTESIAN_POINT('Ctrl Pts',(-71.212250179455,-21.7835967290261,0.));
#81697=CARTESIAN_POINT('Ctrl Pts',(-71.212250179455,-21.7835967290261,12.));
#81698=CARTESIAN_POINT('Ctrl Pts',(-71.2247670209821,-21.7947599798839,
0.));
#81699=CARTESIAN_POINT('Ctrl Pts',(-71.2247670209821,-21.7947599798839,
12.));
#81700=CARTESIAN_POINT('Ctrl Pts',(-71.2331134397743,-21.8022104901682,
0.));
#81701=CARTESIAN_POINT('Ctrl Pts',(-71.2331134397743,-21.8022104901682,
12.));
#81702=CARTESIAN_POINT('Ctrl Pts',(-71.2372871136137,-21.8059378310719,
0.));
#81703=CARTESIAN_POINT('Ctrl Pts',(-71.2372871136137,-21.8059378310719,
12.));
#81704=CARTESIAN_POINT('',(-67.3887914263118,-18.9407177820969,0.));
#81705=CARTESIAN_POINT('Ctrl Pts',(-67.3887914263118,-18.9407177820969,
0.));
#81706=CARTESIAN_POINT('Ctrl Pts',(-67.3921355608328,-18.9426924398719,
0.));
#81707=CARTESIAN_POINT('Ctrl Pts',(-67.3988274146651,-18.9466463414299,
0.));
#81708=CARTESIAN_POINT('Ctrl Pts',(-67.4088759497911,-18.9525909517915,
0.));
#81709=CARTESIAN_POINT('Ctrl Pts',(-67.4222955061981,-18.9605446160985,
0.));
#81710=CARTESIAN_POINT('Ctrl Pts',(-67.4391057908418,-18.9705325631711,
0.));
#81711=CARTESIAN_POINT('Ctrl Pts',(-67.4559518744638,-18.9805663798449,
0.));
#81712=CARTESIAN_POINT('Ctrl Pts',(-67.472833671964,-18.9906460638625,0.));
#81713=CARTESIAN_POINT('Ctrl Pts',(-67.4897510316844,-19.0007716032819,
0.));
#81714=CARTESIAN_POINT('Ctrl Pts',(-67.5067037372317,-19.0109429761306,
0.));
#81715=CARTESIAN_POINT('Ctrl Pts',(-67.5236915360331,-19.021160154824,0.));
#81716=CARTESIAN_POINT('Ctrl Pts',(-67.540714161288,-19.0314231093923,0.));
#81717=CARTESIAN_POINT('Ctrl Pts',(-67.5577713558194,-19.0417318110708,
0.));
#81718=CARTESIAN_POINT('Ctrl Pts',(-67.5748628971964,-19.0520862360396,
0.));
#81719=CARTESIAN_POINT('Ctrl Pts',(-67.5919885896222,-19.062486364241,0.));
#81720=CARTESIAN_POINT('Ctrl Pts',(-67.6091482520534,-19.072932177628,0.));
#81721=CARTESIAN_POINT('Ctrl Pts',(-67.6263417083426,-19.0834236587118,
0.));
#81722=CARTESIAN_POINT('Ctrl Pts',(-67.6435687749841,-19.0939607887502,
0.));
#81723=CARTESIAN_POINT('Ctrl Pts',(-67.6608292549462,-19.1045435468358,
0.));
#81724=CARTESIAN_POINT('Ctrl Pts',(-67.6781229440573,-19.115171910846,0.));
#81725=CARTESIAN_POINT('Ctrl Pts',(-67.6954496350063,-19.1258458580345,
0.));
#81726=CARTESIAN_POINT('Ctrl Pts',(-67.7128091219348,-19.136565365709,0.));
#81727=CARTESIAN_POINT('Ctrl Pts',(-67.7302012056584,-19.1473304119955,
0.));
#81728=CARTESIAN_POINT('Ctrl Pts',(-67.7476256934444,-19.1581409758097,
0.));
#81729=CARTESIAN_POINT('Ctrl Pts',(-67.7650823965127,-19.168997036495,0.));
#81730=CARTESIAN_POINT('Ctrl Pts',(-67.7825711283096,-19.1798985735688,
0.));
#81731=CARTESIAN_POINT('Ctrl Pts',(-67.8000917023926,-19.1908455664098,
0.));
#81732=CARTESIAN_POINT('Ctrl Pts',(-67.8176439306621,-19.201837993993,0.));
#81733=CARTESIAN_POINT('Ctrl Pts',(-67.835227624289,-19.2128758350346,0.));
#81734=CARTESIAN_POINT('Ctrl Pts',(-67.8528425945184,-19.2239590681133,
0.));
#81735=CARTESIAN_POINT('Ctrl Pts',(-67.8704886534544,-19.2350876717874,
0.));
#81736=CARTESIAN_POINT('Ctrl Pts',(-67.8881656149955,-19.2462616247279,
0.));
#81737=CARTESIAN_POINT('Ctrl Pts',(-67.9058732951788,-19.2574809057696,
0.));
#81738=CARTESIAN_POINT('Ctrl Pts',(-67.9236115116758,-19.2687454938442,
0.));
#81739=CARTESIAN_POINT('Ctrl Pts',(-67.9413800834793,-19.280055367936,0.));
#81740=CARTESIAN_POINT('Ctrl Pts',(-67.9591788305394,-19.2914105070286,
0.));
#81741=CARTESIAN_POINT('Ctrl Pts',(-67.9770075733485,-19.302810890038,0.));
#81742=CARTESIAN_POINT('Ctrl Pts',(-67.9948661329617,-19.3142564958203,
0.));
#81743=CARTESIAN_POINT('Ctrl Pts',(-68.0127543311776,-19.3257473032035,
0.));
#81744=CARTESIAN_POINT('Ctrl Pts',(-68.0306719906636,-19.3372832910076,
0.));
#81745=CARTESIAN_POINT('Ctrl Pts',(-68.0486189351011,-19.3488644380641,
0.));
#81746=CARTESIAN_POINT('Ctrl Pts',(-68.0665949893195,-19.3604907232314,
0.));
#81747=CARTESIAN_POINT('Ctrl Pts',(-68.0845999792247,-19.3721621253912,
0.));
#81748=CARTESIAN_POINT('Ctrl Pts',(-68.1026337317285,-19.3838786234421,
0.));
#81749=CARTESIAN_POINT('Ctrl Pts',(-68.1206960746769,-19.3956401962895,
0.));
#81750=CARTESIAN_POINT('Ctrl Pts',(-68.1387868367691,-19.40744682283,0.));
#81751=CARTESIAN_POINT('Ctrl Pts',(-68.1569058475054,-19.4192984819418,
0.));
#81752=CARTESIAN_POINT('Ctrl Pts',(-68.1750529372232,-19.4311951524983,
0.));
#81753=CARTESIAN_POINT('Ctrl Pts',(-68.1932279371127,-19.4431368133719,
0.));
#81754=CARTESIAN_POINT('Ctrl Pts',(-68.2114306792358,-19.4551234434381,
0.));
#81755=CARTESIAN_POINT('Ctrl Pts',(-68.2296609965448,-19.467155021572,0.));
#81756=CARTESIAN_POINT('Ctrl Pts',(-68.2479187228803,-19.4792315266501,
0.));
#81757=CARTESIAN_POINT('Ctrl Pts',(-68.2662036929526,-19.4913529375543,
0.));
#81758=CARTESIAN_POINT('Ctrl Pts',(-68.2845157423233,-19.5035192331705,
0.));
#81759=CARTESIAN_POINT('Ctrl Pts',(-68.3028547073864,-19.5157303923856,
0.));
#81760=CARTESIAN_POINT('Ctrl Pts',(-68.3212204253417,-19.5279863940773,
0.));
#81761=CARTESIAN_POINT('Ctrl Pts',(-68.3396127341938,-19.5402872171191,
0.));
#81762=CARTESIAN_POINT('Ctrl Pts',(-68.3580314727523,-19.5526328403852,
0.));
#81763=CARTESIAN_POINT('Ctrl Pts',(-68.3764764806287,-19.5650232427516,
0.));
#81764=CARTESIAN_POINT('Ctrl Pts',(-68.3949475982335,-19.5774584030938,
0.));
#81765=CARTESIAN_POINT('Ctrl Pts',(-68.4134446667696,-19.5899383002803,
0.));
#81766=CARTESIAN_POINT('Ctrl Pts',(-68.4319675282275,-19.6024629131785,
0.));
#81767=CARTESIAN_POINT('Ctrl Pts',(-68.4505160253778,-19.6150322206577,
0.));
#81768=CARTESIAN_POINT('Ctrl Pts',(-68.4690900017632,-19.6276462015888,
0.));
#81769=CARTESIAN_POINT('Ctrl Pts',(-68.4876893016856,-19.6403048348395,
0.));
#81770=CARTESIAN_POINT('Ctrl Pts',(-68.5063137701971,-19.6530080992686,
0.));
#81771=CARTESIAN_POINT('Ctrl Pts',(-68.5249632530979,-19.6657559737336,
0.));
#81772=CARTESIAN_POINT('Ctrl Pts',(-68.5436375969311,-19.6785484370927,
0.));
#81773=CARTESIAN_POINT('Ctrl Pts',(-68.5623366489779,-19.6913854682046,
0.));
#81774=CARTESIAN_POINT('Ctrl Pts',(-68.581060257249,-19.7042670459237,0.));
#81775=CARTESIAN_POINT('Ctrl Pts',(-68.5998082704766,-19.7171931490956,
0.));
#81776=CARTESIAN_POINT('Ctrl Pts',(-68.6185805381126,-19.7301637565652,
0.));
#81777=CARTESIAN_POINT('Ctrl Pts',(-68.6373769103224,-19.7431788471776,
0.));
#81778=CARTESIAN_POINT('Ctrl Pts',(-68.6561972379793,-19.7562383997781,
0.));
#81779=CARTESIAN_POINT('Ctrl Pts',(-68.6750413726547,-19.7693423932058,
0.));
#81780=CARTESIAN_POINT('Ctrl Pts',(-68.6939091666111,-19.7824908062913,
0.));
#81781=CARTESIAN_POINT('Ctrl Pts',(-68.7128004727998,-19.795683617864,0.));
#81782=CARTESIAN_POINT('Ctrl Pts',(-68.7317151448557,-19.8089208067532,
0.));
#81783=CARTESIAN_POINT('Ctrl Pts',(-68.7506530370918,-19.8222023517874,
0.));
#81784=CARTESIAN_POINT('Ctrl Pts',(-68.7696140044892,-19.835528231787,0.));
#81785=CARTESIAN_POINT('Ctrl Pts',(-68.7885979026927,-19.8488984255642,
0.));
#81786=CARTESIAN_POINT('Ctrl Pts',(-68.8076045880102,-19.8623129119304,
0.));
#81787=CARTESIAN_POINT('Ctrl Pts',(-68.8266339174068,-19.8757716696969,
0.));
#81788=CARTESIAN_POINT('Ctrl Pts',(-68.8456857484988,-19.8892746776734,
0.));
#81789=CARTESIAN_POINT('Ctrl Pts',(-68.8647599395437,-19.9028219146607,
0.));
#81790=CARTESIAN_POINT('Ctrl Pts',(-68.8838563494356,-19.9164133594513,
0.));
#81791=CARTESIAN_POINT('Ctrl Pts',(-68.902974837704,-19.9300489908364,0.));
#81792=CARTESIAN_POINT('Ctrl Pts',(-68.9221152645086,-19.9437287876063,
0.));
#81793=CARTESIAN_POINT('Ctrl Pts',(-68.9412774906346,-19.9574527285492,
0.));
#81794=CARTESIAN_POINT('Ctrl Pts',(-68.960461377483,-19.9712207924437,0.));
#81795=CARTESIAN_POINT('Ctrl Pts',(-68.9796667870667,-19.98503295806,0.));
#81796=CARTESIAN_POINT('Ctrl Pts',(-68.9988935820101,-19.9988892041671,
0.));
#81797=CARTESIAN_POINT('Ctrl Pts',(-69.0181416255433,-20.0127895095327,
0.));
#81798=CARTESIAN_POINT('Ctrl Pts',(-69.0374107814977,-20.0267338529221,
0.));
#81799=CARTESIAN_POINT('Ctrl Pts',(-69.0567009142968,-20.0407222130902,
0.));
#81800=CARTESIAN_POINT('Ctrl Pts',(-69.0760118889525,-20.0547545687839,
0.));
#81801=CARTESIAN_POINT('Ctrl Pts',(-69.0953435710634,-20.0688308987478,
0.));
#81802=CARTESIAN_POINT('Ctrl Pts',(-69.1146958268104,-20.0829511817251,
0.));
#81803=CARTESIAN_POINT('Ctrl Pts',(-69.1340685229516,-20.0971153964557,
0.));
#81804=CARTESIAN_POINT('Ctrl Pts',(-69.1534615268153,-20.1113235216694,
0.));
#81805=CARTESIAN_POINT('Ctrl Pts',(-69.172874706296,-20.1255755360871,0.));
#81806=CARTESIAN_POINT('Ctrl Pts',(-69.1923079298534,-20.1398714184278,
0.));
#81807=CARTESIAN_POINT('Ctrl Pts',(-69.2117610665073,-20.1542111474086,
0.));
#81808=CARTESIAN_POINT('Ctrl Pts',(-69.2312339858337,-20.1685947017433,
0.));
#81809=CARTESIAN_POINT('Ctrl Pts',(-69.2507265579562,-20.183022060135,0.));
#81810=CARTESIAN_POINT('Ctrl Pts',(-69.2702386535432,-20.1974932012775,
0.));
#81811=CARTESIAN_POINT('Ctrl Pts',(-69.2897701438066,-20.2120081038622,
0.));
#81812=CARTESIAN_POINT('Ctrl Pts',(-69.3093209004986,-20.2265667465784,
0.));
#81813=CARTESIAN_POINT('Ctrl Pts',(-69.3288907959065,-20.2411691081122,
0.));
#81814=CARTESIAN_POINT('Ctrl Pts',(-69.3484797028454,-20.255815167139,0.));
#81815=CARTESIAN_POINT('Ctrl Pts',(-69.3680874946548,-20.2705049023241,
0.));
#81816=CARTESIAN_POINT('Ctrl Pts',(-69.3877140451975,-20.2852382923299,
0.));
#81817=CARTESIAN_POINT('Ctrl Pts',(-69.4073592288562,-20.3000153158167,
0.));
#81818=CARTESIAN_POINT('Ctrl Pts',(-69.4270229205296,-20.3148359514414,
0.));
#81819=CARTESIAN_POINT('Ctrl Pts',(-69.4467049956257,-20.3297001778505,
0.));
#81820=CARTESIAN_POINT('Ctrl Pts',(-69.4664053300579,-20.3446079736799,
0.));
#81821=CARTESIAN_POINT('Ctrl Pts',(-69.4861238002433,-20.359559317562,0.));
#81822=CARTESIAN_POINT('Ctrl Pts',(-69.5058602831004,-20.3745541881267,
0.));
#81823=CARTESIAN_POINT('Ctrl Pts',(-69.5256146560444,-20.3895925640006,
0.));
#81824=CARTESIAN_POINT('Ctrl Pts',(-69.5453867969815,-20.4046744238002,
0.));
#81825=CARTESIAN_POINT('Ctrl Pts',(-69.565176584305,-20.4197997461306,0.));
#81826=CARTESIAN_POINT('Ctrl Pts',(-69.5849838968944,-20.4349685095928,
0.));
#81827=CARTESIAN_POINT('Ctrl Pts',(-69.6048086141122,-20.4501806927854,
0.));
#81828=CARTESIAN_POINT('Ctrl Pts',(-69.6246506158009,-20.4654362743036,
0.));
#81829=CARTESIAN_POINT('Ctrl Pts',(-69.6445097822778,-20.4807352327335,
0.));
#81830=CARTESIAN_POINT('Ctrl Pts',(-69.6643859943291,-20.4960775466487,
0.));
#81831=CARTESIAN_POINT('Ctrl Pts',(-69.6842791332102,-20.511463194618,0.));
#81832=CARTESIAN_POINT('Ctrl Pts',(-69.7041890806421,-20.5268921552076,
0.));
#81833=CARTESIAN_POINT('Ctrl Pts',(-69.7241157188086,-20.54236440698,0.));
#81834=CARTESIAN_POINT('Ctrl Pts',(-69.7440589303511,-20.5578799284898,
0.));
#81835=CARTESIAN_POINT('Ctrl Pts',(-69.7640185983641,-20.5734386982782,
0.));
#81836=CARTESIAN_POINT('Ctrl Pts',(-69.7839946063942,-20.5890406948809,
0.));
#81837=CARTESIAN_POINT('Ctrl Pts',(-69.8039868384382,-20.6046858968305,
0.));
#81838=CARTESIAN_POINT('Ctrl Pts',(-69.8239951789402,-20.6203742826566,
0.));
#81839=CARTESIAN_POINT('Ctrl Pts',(-69.8440195127874,-20.6361058308812,
0.));
#81840=CARTESIAN_POINT('Ctrl Pts',(-69.8640597253058,-20.6518805200132,
0.));
#81841=CARTESIAN_POINT('Ctrl Pts',(-69.884115702258,-20.6676983285542,0.));
#81842=CARTESIAN_POINT('Ctrl Pts',(-69.9041873298416,-20.6835592350031,
0.));
#81843=CARTESIAN_POINT('Ctrl Pts',(-69.9242744946854,-20.6994632178551,
0.));
#81844=CARTESIAN_POINT('Ctrl Pts',(-69.9443770838444,-20.7154102555996,
0.));
#81845=CARTESIAN_POINT('Ctrl Pts',(-69.9644949847929,-20.7314003267118,
0.));
#81846=CARTESIAN_POINT('Ctrl Pts',(-69.9846280854254,-20.7474334096582,
0.));
#81847=CARTESIAN_POINT('Ctrl Pts',(-70.0047762740569,-20.7635094829017,
0.));
#81848=CARTESIAN_POINT('Ctrl Pts',(-70.0249394394221,-20.7796285249023,
0.));
#81849=CARTESIAN_POINT('Ctrl Pts',(-70.0451174706739,-20.7957905141155,
0.));
#81850=CARTESIAN_POINT('Ctrl Pts',(-70.0653102573798,-20.8119954289846,
0.));
#81851=CARTESIAN_POINT('Ctrl Pts',(-70.0855176895185,-20.8282432479425,
0.));
#81852=CARTESIAN_POINT('Ctrl Pts',(-70.1057396574741,-20.8445339494185,
0.));
#81853=CARTESIAN_POINT('Ctrl Pts',(-70.1259760520306,-20.8608675118377,
0.));
#81854=CARTESIAN_POINT('Ctrl Pts',(-70.1462267643649,-20.8772439136207,
0.));
#81855=CARTESIAN_POINT('Ctrl Pts',(-70.1664916860366,-20.8936631331751,
0.));
#81856=CARTESIAN_POINT('Ctrl Pts',(-70.1867707089866,-20.9101251488948,
0.));
#81857=CARTESIAN_POINT('Ctrl Pts',(-70.2070637255469,-20.9266299391688,
0.));
#81858=CARTESIAN_POINT('Ctrl Pts',(-70.2273706284479,-20.9431774823833,
0.));
#81859=CARTESIAN_POINT('Ctrl Pts',(-70.2476913108242,-20.9597677569227,
0.));
#81860=CARTESIAN_POINT('Ctrl Pts',(-70.2680256662215,-20.9764007411649,
0.));
#81861=CARTESIAN_POINT('Ctrl Pts',(-70.288373588597,-20.9930764134771,0.));
#81862=CARTESIAN_POINT('Ctrl Pts',(-70.3087349722959,-21.0097947522212,
0.));
#81863=CARTESIAN_POINT('Ctrl Pts',(-70.3291097120293,-21.0265557357544,
0.));
#81864=CARTESIAN_POINT('Ctrl Pts',(-70.3494977028497,-21.0433593424266,
0.));
#81865=CARTESIAN_POINT('Ctrl Pts',(-70.3698988401291,-21.0602055505751,
0.));
#81866=CARTESIAN_POINT('Ctrl Pts',(-70.3903130195279,-21.0770943385146,
0.));
#81867=CARTESIAN_POINT('Ctrl Pts',(-70.4107401370403,-21.0940256845477,
0.));
#81868=CARTESIAN_POINT('Ctrl Pts',(-70.4311800890411,-21.110999566975,0.));
#81869=CARTESIAN_POINT('Ctrl Pts',(-70.4516327723349,-21.1280159641003,
0.));
#81870=CARTESIAN_POINT('Ctrl Pts',(-70.4720980841934,-21.1450748542335,
0.));
#81871=CARTESIAN_POINT('Ctrl Pts',(-70.4925759224208,-21.1621762156894,
0.));
#81872=CARTESIAN_POINT('Ctrl Pts',(-70.5130661852946,-21.1793200267844,
0.));
#81873=CARTESIAN_POINT('Ctrl Pts',(-70.5335687714422,-21.1965062658296,
0.));
#81874=CARTESIAN_POINT('Ctrl Pts',(-70.5540835797281,-21.2137349111207,
0.));
#81875=CARTESIAN_POINT('Ctrl Pts',(-70.5746105091503,-21.2310059409265,
0.));
#81876=CARTESIAN_POINT('Ctrl Pts',(-70.5951494586961,-21.2483193334677,
0.));
#81877=CARTESIAN_POINT('Ctrl Pts',(-70.6157003273326,-21.2656750669129,
0.));
#81878=CARTESIAN_POINT('Ctrl Pts',(-70.6362630143062,-21.2830731194188,
0.));
#81879=CARTESIAN_POINT('Ctrl Pts',(-70.6568374193786,-21.3005134691563,
0.));
#81880=CARTESIAN_POINT('Ctrl Pts',(-70.6774234430899,-21.3179960943389,
0.));
#81881=CARTESIAN_POINT('Ctrl Pts',(-70.6980209870032,-21.3355209732438,
0.));
#81882=CARTESIAN_POINT('Ctrl Pts',(-70.7186299539698,-21.353088084234,0.));
#81883=CARTESIAN_POINT('Ctrl Pts',(-70.7392502475437,-21.3706974057028,
0.));
#81884=CARTESIAN_POINT('Ctrl Pts',(-70.7598817714078,-21.3883489160187,
0.));
#81885=CARTESIAN_POINT('Ctrl Pts',(-70.780524428744,-21.4060425934595,0.));
#81886=CARTESIAN_POINT('Ctrl Pts',(-70.8011781217409,-21.4237784161592,
0.));
#81887=CARTESIAN_POINT('Ctrl Pts',(-70.8218427507545,-21.4415563620127,
0.));
#81888=CARTESIAN_POINT('Ctrl Pts',(-70.84251821499,-21.4593764087492,0.));
#81889=CARTESIAN_POINT('Ctrl Pts',(-70.8632044140166,-21.4772385340978,
0.));
#81890=CARTESIAN_POINT('Ctrl Pts',(-70.8839012490903,-21.4951427159272,
0.));
#81891=CARTESIAN_POINT('Ctrl Pts',(-70.9046086244123,-21.5130889323767,
0.));
#81892=CARTESIAN_POINT('Ctrl Pts',(-70.9253264487576,-21.5310771620209,
0.));
#81893=CARTESIAN_POINT('Ctrl Pts',(-70.9460546358597,-21.549107383907,0.));
#81894=CARTESIAN_POINT('Ctrl Pts',(-70.9638315189647,-21.5645987555282,
0.));
#81895=CARTESIAN_POINT('Ctrl Pts',(-70.9774662112376,-21.5764983366351,
0.));
#81896=CARTESIAN_POINT('Ctrl Pts',(-70.9869541807809,-21.5847875433161,
0.));
#81897=CARTESIAN_POINT('Ctrl Pts',(-70.9922924595083,-21.589454092537,0.));
#81898=CARTESIAN_POINT('Ctrl Pts',(-70.993479606878,-21.5904919934802,0.));
#81899=CARTESIAN_POINT('',(-67.3887914263118,-18.9407177820969,12.));
#81900=CARTESIAN_POINT('',(-67.3887914263118,-18.9407177820969,0.));
#81901=CARTESIAN_POINT('Ctrl Pts',(-70.993479606878,-21.5904919934802,12.));
#81902=CARTESIAN_POINT('Ctrl Pts',(-70.9922924595083,-21.589454092537,12.));
#81903=CARTESIAN_POINT('Ctrl Pts',(-70.9869541807809,-21.5847875433161,
12.));
#81904=CARTESIAN_POINT('Ctrl Pts',(-70.9774662112376,-21.5764983366351,
12.));
#81905=CARTESIAN_POINT('Ctrl Pts',(-70.9638315189647,-21.5645987555282,
12.));
#81906=CARTESIAN_POINT('Ctrl Pts',(-70.9460546358597,-21.549107383907,12.));
#81907=CARTESIAN_POINT('Ctrl Pts',(-70.9253264487576,-21.5310771620209,
12.));
#81908=CARTESIAN_POINT('Ctrl Pts',(-70.9046086244123,-21.5130889323767,
12.));
#81909=CARTESIAN_POINT('Ctrl Pts',(-70.8839012490903,-21.4951427159272,
12.));
#81910=CARTESIAN_POINT('Ctrl Pts',(-70.8632044140166,-21.4772385340978,
12.));
#81911=CARTESIAN_POINT('Ctrl Pts',(-70.84251821499,-21.4593764087492,12.));
#81912=CARTESIAN_POINT('Ctrl Pts',(-70.8218427507545,-21.4415563620127,
12.));
#81913=CARTESIAN_POINT('Ctrl Pts',(-70.8011781217409,-21.4237784161592,
12.));
#81914=CARTESIAN_POINT('Ctrl Pts',(-70.780524428744,-21.4060425934595,12.));
#81915=CARTESIAN_POINT('Ctrl Pts',(-70.7598817714078,-21.3883489160187,
12.));
#81916=CARTESIAN_POINT('Ctrl Pts',(-70.7392502475437,-21.3706974057028,
12.));
#81917=CARTESIAN_POINT('Ctrl Pts',(-70.7186299539698,-21.353088084234,12.));
#81918=CARTESIAN_POINT('Ctrl Pts',(-70.6980209870032,-21.3355209732438,
12.));
#81919=CARTESIAN_POINT('Ctrl Pts',(-70.6774234430899,-21.3179960943389,
12.));
#81920=CARTESIAN_POINT('Ctrl Pts',(-70.6568374193786,-21.3005134691563,
12.));
#81921=CARTESIAN_POINT('Ctrl Pts',(-70.6362630143062,-21.2830731194188,
12.));
#81922=CARTESIAN_POINT('Ctrl Pts',(-70.6157003273326,-21.2656750669129,
12.));
#81923=CARTESIAN_POINT('Ctrl Pts',(-70.5951494586961,-21.2483193334677,
12.));
#81924=CARTESIAN_POINT('Ctrl Pts',(-70.5746105091503,-21.2310059409265,
12.));
#81925=CARTESIAN_POINT('Ctrl Pts',(-70.5540835797281,-21.2137349111207,
12.));
#81926=CARTESIAN_POINT('Ctrl Pts',(-70.5335687714422,-21.1965062658296,
12.));
#81927=CARTESIAN_POINT('Ctrl Pts',(-70.5130661852946,-21.1793200267844,
12.));
#81928=CARTESIAN_POINT('Ctrl Pts',(-70.4925759224208,-21.1621762156894,
12.));
#81929=CARTESIAN_POINT('Ctrl Pts',(-70.4720980841934,-21.1450748542335,
12.));
#81930=CARTESIAN_POINT('Ctrl Pts',(-70.4516327723349,-21.1280159641003,
12.));
#81931=CARTESIAN_POINT('Ctrl Pts',(-70.4311800890411,-21.110999566975,12.));
#81932=CARTESIAN_POINT('Ctrl Pts',(-70.4107401370403,-21.0940256845477,
12.));
#81933=CARTESIAN_POINT('Ctrl Pts',(-70.3903130195279,-21.0770943385146,
12.));
#81934=CARTESIAN_POINT('Ctrl Pts',(-70.3698988401291,-21.0602055505751,
12.));
#81935=CARTESIAN_POINT('Ctrl Pts',(-70.3494977028497,-21.0433593424266,
12.));
#81936=CARTESIAN_POINT('Ctrl Pts',(-70.3291097120293,-21.0265557357544,
12.));
#81937=CARTESIAN_POINT('Ctrl Pts',(-70.3087349722959,-21.0097947522212,
12.));
#81938=CARTESIAN_POINT('Ctrl Pts',(-70.288373588597,-20.9930764134771,12.));
#81939=CARTESIAN_POINT('Ctrl Pts',(-70.2680256662215,-20.9764007411649,
12.));
#81940=CARTESIAN_POINT('Ctrl Pts',(-70.2476913108242,-20.9597677569227,
12.));
#81941=CARTESIAN_POINT('Ctrl Pts',(-70.2273706284479,-20.9431774823833,
12.));
#81942=CARTESIAN_POINT('Ctrl Pts',(-70.2070637255469,-20.9266299391688,
12.));
#81943=CARTESIAN_POINT('Ctrl Pts',(-70.1867707089866,-20.9101251488948,
12.));
#81944=CARTESIAN_POINT('Ctrl Pts',(-70.1664916860366,-20.8936631331751,
12.));
#81945=CARTESIAN_POINT('Ctrl Pts',(-70.1462267643649,-20.8772439136207,
12.));
#81946=CARTESIAN_POINT('Ctrl Pts',(-70.1259760520306,-20.8608675118377,
12.));
#81947=CARTESIAN_POINT('Ctrl Pts',(-70.1057396574741,-20.8445339494185,
12.));
#81948=CARTESIAN_POINT('Ctrl Pts',(-70.0855176895185,-20.8282432479425,
12.));
#81949=CARTESIAN_POINT('Ctrl Pts',(-70.0653102573798,-20.8119954289846,
12.));
#81950=CARTESIAN_POINT('Ctrl Pts',(-70.0451174706739,-20.7957905141155,
12.));
#81951=CARTESIAN_POINT('Ctrl Pts',(-70.0249394394221,-20.7796285249023,
12.));
#81952=CARTESIAN_POINT('Ctrl Pts',(-70.0047762740569,-20.7635094829017,
12.));
#81953=CARTESIAN_POINT('Ctrl Pts',(-69.9846280854254,-20.7474334096582,
12.));
#81954=CARTESIAN_POINT('Ctrl Pts',(-69.9644949847929,-20.7314003267118,
12.));
#81955=CARTESIAN_POINT('Ctrl Pts',(-69.9443770838444,-20.7154102555996,
12.));
#81956=CARTESIAN_POINT('Ctrl Pts',(-69.9242744946854,-20.6994632178551,
12.));
#81957=CARTESIAN_POINT('Ctrl Pts',(-69.9041873298416,-20.6835592350031,
12.));
#81958=CARTESIAN_POINT('Ctrl Pts',(-69.884115702258,-20.6676983285542,12.));
#81959=CARTESIAN_POINT('Ctrl Pts',(-69.8640597253058,-20.6518805200132,
12.));
#81960=CARTESIAN_POINT('Ctrl Pts',(-69.8440195127874,-20.6361058308812,
12.));
#81961=CARTESIAN_POINT('Ctrl Pts',(-69.8239951789402,-20.6203742826566,
12.));
#81962=CARTESIAN_POINT('Ctrl Pts',(-69.8039868384382,-20.6046858968305,
12.));
#81963=CARTESIAN_POINT('Ctrl Pts',(-69.7839946063942,-20.5890406948809,
12.));
#81964=CARTESIAN_POINT('Ctrl Pts',(-69.7640185983641,-20.5734386982782,
12.));
#81965=CARTESIAN_POINT('Ctrl Pts',(-69.7440589303511,-20.5578799284898,
12.));
#81966=CARTESIAN_POINT('Ctrl Pts',(-69.7241157188086,-20.54236440698,12.));
#81967=CARTESIAN_POINT('Ctrl Pts',(-69.7041890806421,-20.5268921552076,
12.));
#81968=CARTESIAN_POINT('Ctrl Pts',(-69.6842791332102,-20.511463194618,12.));
#81969=CARTESIAN_POINT('Ctrl Pts',(-69.6643859943291,-20.4960775466487,
12.));
#81970=CARTESIAN_POINT('Ctrl Pts',(-69.6445097822778,-20.4807352327335,
12.));
#81971=CARTESIAN_POINT('Ctrl Pts',(-69.6246506158009,-20.4654362743036,
12.));
#81972=CARTESIAN_POINT('Ctrl Pts',(-69.6048086141122,-20.4501806927854,
12.));
#81973=CARTESIAN_POINT('Ctrl Pts',(-69.5849838968944,-20.4349685095928,
12.));
#81974=CARTESIAN_POINT('Ctrl Pts',(-69.565176584305,-20.4197997461306,12.));
#81975=CARTESIAN_POINT('Ctrl Pts',(-69.5453867969815,-20.4046744238002,
12.));
#81976=CARTESIAN_POINT('Ctrl Pts',(-69.5256146560444,-20.3895925640006,
12.));
#81977=CARTESIAN_POINT('Ctrl Pts',(-69.5058602831004,-20.3745541881267,
12.));
#81978=CARTESIAN_POINT('Ctrl Pts',(-69.4861238002433,-20.359559317562,12.));
#81979=CARTESIAN_POINT('Ctrl Pts',(-69.4664053300579,-20.3446079736799,
12.));
#81980=CARTESIAN_POINT('Ctrl Pts',(-69.4467049956257,-20.3297001778505,
12.));
#81981=CARTESIAN_POINT('Ctrl Pts',(-69.4270229205296,-20.3148359514414,
12.));
#81982=CARTESIAN_POINT('Ctrl Pts',(-69.4073592288562,-20.3000153158167,
12.));
#81983=CARTESIAN_POINT('Ctrl Pts',(-69.3877140451975,-20.2852382923299,
12.));
#81984=CARTESIAN_POINT('Ctrl Pts',(-69.3680874946548,-20.2705049023241,
12.));
#81985=CARTESIAN_POINT('Ctrl Pts',(-69.3484797028454,-20.255815167139,12.));
#81986=CARTESIAN_POINT('Ctrl Pts',(-69.3288907959065,-20.2411691081122,
12.));
#81987=CARTESIAN_POINT('Ctrl Pts',(-69.3093209004986,-20.2265667465784,
12.));
#81988=CARTESIAN_POINT('Ctrl Pts',(-69.2897701438066,-20.2120081038622,
12.));
#81989=CARTESIAN_POINT('Ctrl Pts',(-69.2702386535432,-20.1974932012775,
12.));
#81990=CARTESIAN_POINT('Ctrl Pts',(-69.2507265579562,-20.183022060135,12.));
#81991=CARTESIAN_POINT('Ctrl Pts',(-69.2312339858337,-20.1685947017433,
12.));
#81992=CARTESIAN_POINT('Ctrl Pts',(-69.2117610665073,-20.1542111474086,
12.));
#81993=CARTESIAN_POINT('Ctrl Pts',(-69.1923079298534,-20.1398714184278,
12.));
#81994=CARTESIAN_POINT('Ctrl Pts',(-69.172874706296,-20.1255755360871,12.));
#81995=CARTESIAN_POINT('Ctrl Pts',(-69.1534615268153,-20.1113235216694,
12.));
#81996=CARTESIAN_POINT('Ctrl Pts',(-69.1340685229516,-20.0971153964557,
12.));
#81997=CARTESIAN_POINT('Ctrl Pts',(-69.1146958268104,-20.0829511817251,
12.));
#81998=CARTESIAN_POINT('Ctrl Pts',(-69.0953435710634,-20.0688308987478,
12.));
#81999=CARTESIAN_POINT('Ctrl Pts',(-69.0760118889525,-20.0547545687839,
12.));
#82000=CARTESIAN_POINT('Ctrl Pts',(-69.0567009142968,-20.0407222130902,
12.));
#82001=CARTESIAN_POINT('Ctrl Pts',(-69.0374107814977,-20.0267338529221,
12.));
#82002=CARTESIAN_POINT('Ctrl Pts',(-69.0181416255433,-20.0127895095327,
12.));
#82003=CARTESIAN_POINT('Ctrl Pts',(-68.9988935820101,-19.9988892041671,
12.));
#82004=CARTESIAN_POINT('Ctrl Pts',(-68.9796667870667,-19.98503295806,12.));
#82005=CARTESIAN_POINT('Ctrl Pts',(-68.960461377483,-19.9712207924437,12.));
#82006=CARTESIAN_POINT('Ctrl Pts',(-68.9412774906346,-19.9574527285492,
12.));
#82007=CARTESIAN_POINT('Ctrl Pts',(-68.9221152645086,-19.9437287876063,
12.));
#82008=CARTESIAN_POINT('Ctrl Pts',(-68.902974837704,-19.9300489908364,12.));
#82009=CARTESIAN_POINT('Ctrl Pts',(-68.8838563494356,-19.9164133594513,
12.));
#82010=CARTESIAN_POINT('Ctrl Pts',(-68.8647599395437,-19.9028219146607,
12.));
#82011=CARTESIAN_POINT('Ctrl Pts',(-68.8456857484988,-19.8892746776734,
12.));
#82012=CARTESIAN_POINT('Ctrl Pts',(-68.8266339174068,-19.8757716696969,
12.));
#82013=CARTESIAN_POINT('Ctrl Pts',(-68.8076045880102,-19.8623129119304,
12.));
#82014=CARTESIAN_POINT('Ctrl Pts',(-68.7885979026927,-19.8488984255642,
12.));
#82015=CARTESIAN_POINT('Ctrl Pts',(-68.7696140044892,-19.835528231787,12.));
#82016=CARTESIAN_POINT('Ctrl Pts',(-68.7506530370918,-19.8222023517874,
12.));
#82017=CARTESIAN_POINT('Ctrl Pts',(-68.7317151448557,-19.8089208067532,
12.));
#82018=CARTESIAN_POINT('Ctrl Pts',(-68.7128004727998,-19.795683617864,12.));
#82019=CARTESIAN_POINT('Ctrl Pts',(-68.6939091666111,-19.7824908062913,
12.));
#82020=CARTESIAN_POINT('Ctrl Pts',(-68.6750413726547,-19.7693423932058,
12.));
#82021=CARTESIAN_POINT('Ctrl Pts',(-68.6561972379793,-19.7562383997781,
12.));
#82022=CARTESIAN_POINT('Ctrl Pts',(-68.6373769103224,-19.7431788471776,
12.));
#82023=CARTESIAN_POINT('Ctrl Pts',(-68.6185805381126,-19.7301637565652,
12.));
#82024=CARTESIAN_POINT('Ctrl Pts',(-68.5998082704766,-19.7171931490956,
12.));
#82025=CARTESIAN_POINT('Ctrl Pts',(-68.581060257249,-19.7042670459237,12.));
#82026=CARTESIAN_POINT('Ctrl Pts',(-68.5623366489779,-19.6913854682046,
12.));
#82027=CARTESIAN_POINT('Ctrl Pts',(-68.5436375969311,-19.6785484370927,
12.));
#82028=CARTESIAN_POINT('Ctrl Pts',(-68.5249632530979,-19.6657559737336,
12.));
#82029=CARTESIAN_POINT('Ctrl Pts',(-68.5063137701971,-19.6530080992686,
12.));
#82030=CARTESIAN_POINT('Ctrl Pts',(-68.4876893016856,-19.6403048348395,
12.));
#82031=CARTESIAN_POINT('Ctrl Pts',(-68.4690900017632,-19.6276462015888,
12.));
#82032=CARTESIAN_POINT('Ctrl Pts',(-68.4505160253778,-19.6150322206577,
12.));
#82033=CARTESIAN_POINT('Ctrl Pts',(-68.4319675282275,-19.6024629131785,
12.));
#82034=CARTESIAN_POINT('Ctrl Pts',(-68.4134446667696,-19.5899383002803,
12.));
#82035=CARTESIAN_POINT('Ctrl Pts',(-68.3949475982335,-19.5774584030938,
12.));
#82036=CARTESIAN_POINT('Ctrl Pts',(-68.3764764806287,-19.5650232427516,
12.));
#82037=CARTESIAN_POINT('Ctrl Pts',(-68.3580314727523,-19.5526328403852,
12.));
#82038=CARTESIAN_POINT('Ctrl Pts',(-68.3396127341938,-19.5402872171191,
12.));
#82039=CARTESIAN_POINT('Ctrl Pts',(-68.3212204253417,-19.5279863940773,
12.));
#82040=CARTESIAN_POINT('Ctrl Pts',(-68.3028547073864,-19.5157303923856,
12.));
#82041=CARTESIAN_POINT('Ctrl Pts',(-68.2845157423233,-19.5035192331705,
12.));
#82042=CARTESIAN_POINT('Ctrl Pts',(-68.2662036929526,-19.4913529375543,
12.));
#82043=CARTESIAN_POINT('Ctrl Pts',(-68.2479187228803,-19.4792315266501,
12.));
#82044=CARTESIAN_POINT('Ctrl Pts',(-68.2296609965448,-19.467155021572,12.));
#82045=CARTESIAN_POINT('Ctrl Pts',(-68.2114306792358,-19.4551234434381,
12.));
#82046=CARTESIAN_POINT('Ctrl Pts',(-68.1932279371127,-19.4431368133719,
12.));
#82047=CARTESIAN_POINT('Ctrl Pts',(-68.1750529372232,-19.4311951524983,
12.));
#82048=CARTESIAN_POINT('Ctrl Pts',(-68.1569058475054,-19.4192984819418,
12.));
#82049=CARTESIAN_POINT('Ctrl Pts',(-68.1387868367691,-19.40744682283,12.));
#82050=CARTESIAN_POINT('Ctrl Pts',(-68.1206960746769,-19.3956401962895,
12.));
#82051=CARTESIAN_POINT('Ctrl Pts',(-68.1026337317285,-19.3838786234421,
12.));
#82052=CARTESIAN_POINT('Ctrl Pts',(-68.0845999792247,-19.3721621253912,
12.));
#82053=CARTESIAN_POINT('Ctrl Pts',(-68.0665949893195,-19.3604907232314,
12.));
#82054=CARTESIAN_POINT('Ctrl Pts',(-68.0486189351011,-19.3488644380641,
12.));
#82055=CARTESIAN_POINT('Ctrl Pts',(-68.0306719906636,-19.3372832910076,
12.));
#82056=CARTESIAN_POINT('Ctrl Pts',(-68.0127543311776,-19.3257473032035,
12.));
#82057=CARTESIAN_POINT('Ctrl Pts',(-67.9948661329617,-19.3142564958203,
12.));
#82058=CARTESIAN_POINT('Ctrl Pts',(-67.9770075733485,-19.302810890038,12.));
#82059=CARTESIAN_POINT('Ctrl Pts',(-67.9591788305394,-19.2914105070286,
12.));
#82060=CARTESIAN_POINT('Ctrl Pts',(-67.9413800834793,-19.280055367936,12.));
#82061=CARTESIAN_POINT('Ctrl Pts',(-67.9236115116758,-19.2687454938442,
12.));
#82062=CARTESIAN_POINT('Ctrl Pts',(-67.9058732951788,-19.2574809057696,
12.));
#82063=CARTESIAN_POINT('Ctrl Pts',(-67.8881656149955,-19.2462616247279,
12.));
#82064=CARTESIAN_POINT('Ctrl Pts',(-67.8704886534544,-19.2350876717874,
12.));
#82065=CARTESIAN_POINT('Ctrl Pts',(-67.8528425945184,-19.2239590681133,
12.));
#82066=CARTESIAN_POINT('Ctrl Pts',(-67.835227624289,-19.2128758350346,12.));
#82067=CARTESIAN_POINT('Ctrl Pts',(-67.8176439306621,-19.201837993993,12.));
#82068=CARTESIAN_POINT('Ctrl Pts',(-67.8000917023926,-19.1908455664098,
12.));
#82069=CARTESIAN_POINT('Ctrl Pts',(-67.7825711283096,-19.1798985735688,
12.));
#82070=CARTESIAN_POINT('Ctrl Pts',(-67.7650823965127,-19.168997036495,12.));
#82071=CARTESIAN_POINT('Ctrl Pts',(-67.7476256934444,-19.1581409758097,
12.));
#82072=CARTESIAN_POINT('Ctrl Pts',(-67.7302012056584,-19.1473304119955,
12.));
#82073=CARTESIAN_POINT('Ctrl Pts',(-67.7128091219348,-19.136565365709,12.));
#82074=CARTESIAN_POINT('Ctrl Pts',(-67.6954496350063,-19.1258458580345,
12.));
#82075=CARTESIAN_POINT('Ctrl Pts',(-67.6781229440573,-19.115171910846,12.));
#82076=CARTESIAN_POINT('Ctrl Pts',(-67.6608292549462,-19.1045435468358,
12.));
#82077=CARTESIAN_POINT('Ctrl Pts',(-67.6435687749841,-19.0939607887502,
12.));
#82078=CARTESIAN_POINT('Ctrl Pts',(-67.6263417083426,-19.0834236587118,
12.));
#82079=CARTESIAN_POINT('Ctrl Pts',(-67.6091482520534,-19.072932177628,12.));
#82080=CARTESIAN_POINT('Ctrl Pts',(-67.5919885896222,-19.062486364241,12.));
#82081=CARTESIAN_POINT('Ctrl Pts',(-67.5748628971964,-19.0520862360396,
12.));
#82082=CARTESIAN_POINT('Ctrl Pts',(-67.5577713558194,-19.0417318110708,
12.));
#82083=CARTESIAN_POINT('Ctrl Pts',(-67.540714161288,-19.0314231093923,12.));
#82084=CARTESIAN_POINT('Ctrl Pts',(-67.5236915360331,-19.021160154824,12.));
#82085=CARTESIAN_POINT('Ctrl Pts',(-67.5067037372317,-19.0109429761306,
12.));
#82086=CARTESIAN_POINT('Ctrl Pts',(-67.4897510316844,-19.0007716032819,
12.));
#82087=CARTESIAN_POINT('Ctrl Pts',(-67.472833671964,-18.9906460638625,12.));
#82088=CARTESIAN_POINT('Ctrl Pts',(-67.4559518744638,-18.9805663798449,
12.));
#82089=CARTESIAN_POINT('Ctrl Pts',(-67.4391057908418,-18.9705325631711,
12.));
#82090=CARTESIAN_POINT('Ctrl Pts',(-67.4222955061981,-18.9605446160985,
12.));
#82091=CARTESIAN_POINT('Ctrl Pts',(-67.4088759497911,-18.9525909517915,
12.));
#82092=CARTESIAN_POINT('Ctrl Pts',(-67.3988274146651,-18.9466463414299,
12.));
#82093=CARTESIAN_POINT('Ctrl Pts',(-67.3921355608328,-18.9426924398719,
12.));
#82094=CARTESIAN_POINT('Ctrl Pts',(-67.3887914263118,-18.9407177820969,
12.));
#82095=CARTESIAN_POINT('Ctrl Pts',(-70.538251407892,-23.0342913834073,-1.11022302462516E-15));
#82096=CARTESIAN_POINT('Ctrl Pts',(-70.538251407892,-23.0342913834073,4.));
#82097=CARTESIAN_POINT('Ctrl Pts',(-70.538251407892,-23.0342913834073,8.));
#82098=CARTESIAN_POINT('Ctrl Pts',(-70.538251407892,-23.0342913834073,12.));
#82099=CARTESIAN_POINT('Ctrl Pts',(-70.6474988907591,-23.0224954570734,
-1.11022302462516E-15));
#82100=CARTESIAN_POINT('Ctrl Pts',(-70.6474988907591,-23.0224954570734,
4.));
#82101=CARTESIAN_POINT('Ctrl Pts',(-70.6474988907591,-23.0224954570734,
8.00000000000001));
#82102=CARTESIAN_POINT('Ctrl Pts',(-70.6474988907591,-23.0224954570734,
12.));
#82103=CARTESIAN_POINT('Ctrl Pts',(-70.83100071469,-22.9364730048789,-1.11022302462516E-15));
#82104=CARTESIAN_POINT('Ctrl Pts',(-70.83100071469,-22.9364730048789,4.));
#82105=CARTESIAN_POINT('Ctrl Pts',(-70.83100071469,-22.936473004879,7.99999999999999));
#82106=CARTESIAN_POINT('Ctrl Pts',(-70.83100071469,-22.936473004879,12.));
#82107=CARTESIAN_POINT('Ctrl Pts',(-70.9357242819029,-22.7679558220498,
-1.11022302462516E-15));
#82108=CARTESIAN_POINT('Ctrl Pts',(-70.9357242819029,-22.7679558220498,
4.));
#82109=CARTESIAN_POINT('Ctrl Pts',(-70.935724281903,-22.7679558220499,8.00000000000001));
#82110=CARTESIAN_POINT('Ctrl Pts',(-70.935724281903,-22.7679558220499,12.));
#82111=CARTESIAN_POINT('Ctrl Pts',(-70.9608233461354,-22.6894590071812,
-1.11022302462516E-15));
#82112=CARTESIAN_POINT('Ctrl Pts',(-70.9608233461354,-22.6894590071812,
4.));
#82113=CARTESIAN_POINT('Ctrl Pts',(-70.9608233461355,-22.6894590071812,
8.));
#82114=CARTESIAN_POINT('Ctrl Pts',(-70.9608233461355,-22.6894590071812,
12.));
#82115=CARTESIAN_POINT('',(-70.538251407892,-23.0342913834073,0.));
#82116=CARTESIAN_POINT('',(-70.9608233461355,-22.6894590071813,2.77555756156289E-16));
#82117=CARTESIAN_POINT('Ctrl Pts',(-70.538251407892,-23.0342913834073,0.));
#82118=CARTESIAN_POINT('Ctrl Pts',(-70.6474988907591,-23.0224954570734,
-3.08148791101957E-31));
#82119=CARTESIAN_POINT('Ctrl Pts',(-70.7523570758625,-22.9733397701051,
4.3140830754274E-31));
#82120=CARTESIAN_POINT('Ctrl Pts',(-70.8314917485681,-22.8972470282358,
0.));
#82121=CARTESIAN_POINT('Ctrl Pts',(-70.8908427530974,-22.8401774718337,
-1.54074395550979E-31));
#82122=CARTESIAN_POINT('Ctrl Pts',(-70.9357242819029,-22.7679558220498,
-9.24446373305873E-31));
#82123=CARTESIAN_POINT('Ctrl Pts',(-70.9608233461354,-22.6894590071812,
3.28429327576129E-46));
#82124=CARTESIAN_POINT('',(-70.9608233461355,-22.6894590071812,12.));
#82125=CARTESIAN_POINT('Ctrl Pts',(-70.9608233461354,-22.6894590071812,
-1.11022302462516E-15));
#82126=CARTESIAN_POINT('Ctrl Pts',(-70.9608233461354,-22.6894590071812,
4.));
#82127=CARTESIAN_POINT('Ctrl Pts',(-70.9608233461355,-22.6894590071812,
8.));
#82128=CARTESIAN_POINT('Ctrl Pts',(-70.9608233461355,-22.6894590071812,
12.));
#82129=CARTESIAN_POINT('',(-70.538251407892,-23.0342913834073,12.));
#82130=CARTESIAN_POINT('Ctrl Pts',(-70.9608233461355,-22.6894590071812,
12.));
#82131=CARTESIAN_POINT('Ctrl Pts',(-70.935724281903,-22.7679558220499,12.));
#82132=CARTESIAN_POINT('Ctrl Pts',(-70.8908427530974,-22.8401774718338,
12.));
#82133=CARTESIAN_POINT('Ctrl Pts',(-70.8314917485682,-22.8972470282358,
12.));
#82134=CARTESIAN_POINT('Ctrl Pts',(-70.7523570758625,-22.9733397701052,
12.));
#82135=CARTESIAN_POINT('Ctrl Pts',(-70.6474988907591,-23.0224954570734,
12.));
#82136=CARTESIAN_POINT('Ctrl Pts',(-70.538251407892,-23.0342913834073,12.));
#82137=CARTESIAN_POINT('Ctrl Pts',(-70.538251407892,-23.0342913834073,12.));
#82138=CARTESIAN_POINT('Ctrl Pts',(-70.538251407892,-23.0342913834073,8.));
#82139=CARTESIAN_POINT('Ctrl Pts',(-70.538251407892,-23.0342913834073,4.));
#82140=CARTESIAN_POINT('Ctrl Pts',(-70.538251407892,-23.0342913834073,-1.11022302462516E-15));
#82141=CARTESIAN_POINT('Origin',(-3.57465004850839E-10,-1.12812358559725E-10,
0.));
#82142=CARTESIAN_POINT('Origin',(-3.57465004850839E-10,-1.12812358559725E-10,
12.));
#82143=CARTESIAN_POINT('Origin',(-3.57465004850839E-10,-1.12812358559725E-10,
0.));
#82144=CARTESIAN_POINT('Ctrl Pts',(-72.7986051948032,-15.8307637747259,
-1.11022302462516E-15));
#82145=CARTESIAN_POINT('Ctrl Pts',(-72.7986051948032,-15.8307637747259,
4.));
#82146=CARTESIAN_POINT('Ctrl Pts',(-72.7986051948032,-15.8307637747259,
8.));
#82147=CARTESIAN_POINT('Ctrl Pts',(-72.7986051948032,-15.8307637747259,
12.));
#82148=CARTESIAN_POINT('Ctrl Pts',(-72.8219545017353,-15.7233907508395,
-1.11022302462516E-15));
#82149=CARTESIAN_POINT('Ctrl Pts',(-72.8219545017353,-15.7233907508395,
3.99999999999999));
#82150=CARTESIAN_POINT('Ctrl Pts',(-72.8219545017353,-15.7233907508395,
8.));
#82151=CARTESIAN_POINT('Ctrl Pts',(-72.8219545017353,-15.7233907508395,
12.));
#82152=CARTESIAN_POINT('Ctrl Pts',(-72.7983622347338,-15.5221041200722,
-1.0371419571966E-15));
#82153=CARTESIAN_POINT('Ctrl Pts',(-72.7983622347338,-15.5221041200722,
4.00000000000001));
#82154=CARTESIAN_POINT('Ctrl Pts',(-72.7983622347338,-15.5221041200722,
8.));
#82155=CARTESIAN_POINT('Ctrl Pts',(-72.7983622347338,-15.5221041200722,
12.));
#82156=CARTESIAN_POINT('Ctrl Pts',(-72.6715981986666,-15.3694736926919,
-8.63611844393267E-16));
#82157=CARTESIAN_POINT('Ctrl Pts',(-72.6715981986666,-15.3694736926919,
3.99999999999999));
#82158=CARTESIAN_POINT('Ctrl Pts',(-72.6715981986666,-15.3694736926919,
8.));
#82159=CARTESIAN_POINT('Ctrl Pts',(-72.6715981986666,-15.3694736926919,
12.));
#82160=CARTESIAN_POINT('Ctrl Pts',(-72.6050633494357,-15.3208442077191,
-7.79957864156004E-16));
#82161=CARTESIAN_POINT('Ctrl Pts',(-72.6050633494357,-15.3208442077191,
4.));
#82162=CARTESIAN_POINT('Ctrl Pts',(-72.6050633494357,-15.3208442077191,
8.));
#82163=CARTESIAN_POINT('Ctrl Pts',(-72.6050633494357,-15.3208442077191,
12.));
#82164=CARTESIAN_POINT('',(-72.7986051948032,-15.8307637747259,0.));
#82165=CARTESIAN_POINT('',(-72.6050633494356,-15.3208442077192,0.));
#82166=CARTESIAN_POINT('Ctrl Pts',(-72.7986051948032,-15.8307637747259,
-1.38777878078144E-16));
#82167=CARTESIAN_POINT('Ctrl Pts',(-72.8219545017353,-15.7233907508395,
-1.38777878078146E-16));
#82168=CARTESIAN_POINT('Ctrl Pts',(-72.8084732063058,-15.6083698189725,
-9.70172681189663E-17));
#82169=CARTESIAN_POINT('Ctrl Pts',(-72.761303169957,-15.5092366269869,-2.24569698741506E-17));
#82170=CARTESIAN_POINT('Ctrl Pts',(-72.7259256426954,-15.4348867329977,
3.34632538094614E-17));
#82171=CARTESIAN_POINT('Ctrl Pts',(-72.6715981986666,-15.3694736926919,
1.07833302153744E-16));
#82172=CARTESIAN_POINT('Ctrl Pts',(-72.6050633494357,-15.3208442077191,
1.91487282391008E-16));
#82173=CARTESIAN_POINT('',(-72.6050633494356,-15.3208442077192,12.));
#82174=CARTESIAN_POINT('Ctrl Pts',(-72.6050633494357,-15.3208442077191,
-7.79957864156004E-16));
#82175=CARTESIAN_POINT('Ctrl Pts',(-72.6050633494357,-15.3208442077191,
4.));
#82176=CARTESIAN_POINT('Ctrl Pts',(-72.6050633494357,-15.3208442077191,
8.));
#82177=CARTESIAN_POINT('Ctrl Pts',(-72.6050633494357,-15.3208442077191,
12.));
#82178=CARTESIAN_POINT('',(-72.7986051948032,-15.8307637747259,12.));
#82179=CARTESIAN_POINT('Ctrl Pts',(-72.6050633494357,-15.3208442077191,
12.));
#82180=CARTESIAN_POINT('Ctrl Pts',(-72.6715981986666,-15.3694736926919,
12.));
#82181=CARTESIAN_POINT('Ctrl Pts',(-72.7259256426954,-15.4348867329977,
12.));
#82182=CARTESIAN_POINT('Ctrl Pts',(-72.761303169957,-15.5092366269869,12.));
#82183=CARTESIAN_POINT('Ctrl Pts',(-72.8084732063058,-15.6083698189725,
12.));
#82184=CARTESIAN_POINT('Ctrl Pts',(-72.8219545017353,-15.7233907508395,
12.));
#82185=CARTESIAN_POINT('Ctrl Pts',(-72.7986051948032,-15.8307637747259,
12.));
#82186=CARTESIAN_POINT('Ctrl Pts',(-72.7986051948032,-15.8307637747259,
12.));
#82187=CARTESIAN_POINT('Ctrl Pts',(-72.7986051948032,-15.8307637747259,
8.));
#82188=CARTESIAN_POINT('Ctrl Pts',(-72.7986051948032,-15.8307637747259,
4.));
#82189=CARTESIAN_POINT('Ctrl Pts',(-72.7986051948032,-15.8307637747259,
-1.11022302462516E-15));
#82190=CARTESIAN_POINT('Ctrl Pts',(-68.7831490561748,-12.9953224629497,
0.));
#82191=CARTESIAN_POINT('Ctrl Pts',(-68.7831490561748,-12.9953224629497,
12.));
#82192=CARTESIAN_POINT('Ctrl Pts',(-68.7866525680193,-12.9969981460277,
0.));
#82193=CARTESIAN_POINT('Ctrl Pts',(-68.7866525680193,-12.9969981460277,
12.));
#82194=CARTESIAN_POINT('Ctrl Pts',(-68.7936635625545,-13.0003537683054,
0.));
#82195=CARTESIAN_POINT('Ctrl Pts',(-68.7936635625545,-13.0003537683054,
12.));
#82196=CARTESIAN_POINT('Ctrl Pts',(-68.804191966902,-13.0053999700875,0.));
#82197=CARTESIAN_POINT('Ctrl Pts',(-68.804191966902,-13.0053999700875,12.));
#82198=CARTESIAN_POINT('Ctrl Pts',(-68.8182536653656,-13.0121537768945,
0.));
#82199=CARTESIAN_POINT('Ctrl Pts',(-68.8182536653656,-13.0121537768945,
12.));
#82200=CARTESIAN_POINT('Ctrl Pts',(-68.8358704887468,-13.0206386039691,
0.));
#82201=CARTESIAN_POINT('Ctrl Pts',(-68.8358704887468,-13.0206386039691,
12.));
#82202=CARTESIAN_POINT('Ctrl Pts',(-68.8535269726793,-13.0291660060107,
0.));
#82203=CARTESIAN_POINT('Ctrl Pts',(-68.8535269726793,-13.0291660060107,
12.));
#82204=CARTESIAN_POINT('Ctrl Pts',(-68.8712230321906,-13.0377359881875,
0.));
#82205=CARTESIAN_POINT('Ctrl Pts',(-68.8712230321906,-13.0377359881875,
12.));
#82206=CARTESIAN_POINT('Ctrl Pts',(-68.8889585151585,-13.0463485518206,
0.));
#82207=CARTESIAN_POINT('Ctrl Pts',(-68.8889585151585,-13.0463485518206,
12.));
#82208=CARTESIAN_POINT('Ctrl Pts',(-68.9067332040985,-13.0550036938813,
0.));
#82209=CARTESIAN_POINT('Ctrl Pts',(-68.9067332040985,-13.0550036938813,
12.));
#82210=CARTESIAN_POINT('Ctrl Pts',(-68.9245468449945,-13.0637014089029,
0.));
#82211=CARTESIAN_POINT('Ctrl Pts',(-68.9245468449945,-13.0637014089029,
12.));
#82212=CARTESIAN_POINT('Ctrl Pts',(-68.9423991694492,-13.072441690283,0.));
#82213=CARTESIAN_POINT('Ctrl Pts',(-68.9423991694492,-13.072441690283,12.));
#82214=CARTESIAN_POINT('Ctrl Pts',(-68.9602899187573,-13.0812245317807,
0.));
#82215=CARTESIAN_POINT('Ctrl Pts',(-68.9602899187573,-13.0812245317807,
12.));
#82216=CARTESIAN_POINT('Ctrl Pts',(-68.9782188692581,-13.090049929053,0.));
#82217=CARTESIAN_POINT('Ctrl Pts',(-68.9782188692581,-13.090049929053,12.));
#82218=CARTESIAN_POINT('Ctrl Pts',(-68.9961858241519,-13.0989178791833,
0.));
#82219=CARTESIAN_POINT('Ctrl Pts',(-68.9961858241519,-13.0989178791833,
12.));
#82220=CARTESIAN_POINT('Ctrl Pts',(-69.0141906015113,-13.1078283799722,
0.));
#82221=CARTESIAN_POINT('Ctrl Pts',(-69.0141906015113,-13.1078283799722,
12.));
#82222=CARTESIAN_POINT('Ctrl Pts',(-69.0322330243348,-13.1167814293497,
0.));
#82223=CARTESIAN_POINT('Ctrl Pts',(-69.0322330243348,-13.1167814293497,
12.));
#82224=CARTESIAN_POINT('Ctrl Pts',(-69.0503129081817,-13.1257770246385,
0.));
#82225=CARTESIAN_POINT('Ctrl Pts',(-69.0503129081817,-13.1257770246385,
12.));
#82226=CARTESIAN_POINT('Ctrl Pts',(-69.0684300549477,-13.1348151621834,
0.));
#82227=CARTESIAN_POINT('Ctrl Pts',(-69.0684300549477,-13.1348151621834,
12.));
#82228=CARTESIAN_POINT('Ctrl Pts',(-69.0865842593102,-13.1438958377404,
0.));
#82229=CARTESIAN_POINT('Ctrl Pts',(-69.0865842593102,-13.1438958377404,
12.));
#82230=CARTESIAN_POINT('Ctrl Pts',(-69.1047753127643,-13.1530190467183,
0.));
#82231=CARTESIAN_POINT('Ctrl Pts',(-69.1047753127643,-13.1530190467183,
12.));
#82232=CARTESIAN_POINT('Ctrl Pts',(-69.1230030082573,-13.1621847844528,
0.));
#82233=CARTESIAN_POINT('Ctrl Pts',(-69.1230030082573,-13.1621847844528,
12.));
#82234=CARTESIAN_POINT('Ctrl Pts',(-69.1412671454564,-13.1713930465132,
0.));
#82235=CARTESIAN_POINT('Ctrl Pts',(-69.1412671454564,-13.1713930465132,
12.));
#82236=CARTESIAN_POINT('Ctrl Pts',(-69.1595675305245,-13.1806438286934,
0.));
#82237=CARTESIAN_POINT('Ctrl Pts',(-69.1595675305245,-13.1806438286934,
12.));
#82238=CARTESIAN_POINT('Ctrl Pts',(-69.1779039735996,-13.1899371268683,
0.));
#82239=CARTESIAN_POINT('Ctrl Pts',(-69.1779039735996,-13.1899371268683,
12.));
#82240=CARTESIAN_POINT('Ctrl Pts',(-69.1962762870527,-13.1992729368928,
0.));
#82241=CARTESIAN_POINT('Ctrl Pts',(-69.1962762870527,-13.1992729368928,
12.));
#82242=CARTESIAN_POINT('Ctrl Pts',(-69.2146842833537,-13.2086512544735,
0.));
#82243=CARTESIAN_POINT('Ctrl Pts',(-69.2146842833537,-13.2086512544735,
12.));
#82244=CARTESIAN_POINT('Ctrl Pts',(-69.2331277732861,-13.2180720750594,
0.));
#82245=CARTESIAN_POINT('Ctrl Pts',(-69.2331277732861,-13.2180720750594,
12.));
#82246=CARTESIAN_POINT('Ctrl Pts',(-69.2516065668844,-13.2275353939051,
0.));
#82247=CARTESIAN_POINT('Ctrl Pts',(-69.2516065668844,-13.2275353939051,
12.));
#82248=CARTESIAN_POINT('Ctrl Pts',(-69.2701204742449,-13.237041206122,0.));
#82249=CARTESIAN_POINT('Ctrl Pts',(-69.2701204742449,-13.237041206122,12.));
#82250=CARTESIAN_POINT('Ctrl Pts',(-69.2886693063182,-13.2465895067262,
0.));
#82251=CARTESIAN_POINT('Ctrl Pts',(-69.2886693063182,-13.2465895067262,
12.));
#82252=CARTESIAN_POINT('Ctrl Pts',(-69.3072528758518,-13.2561802906896,
0.));
#82253=CARTESIAN_POINT('Ctrl Pts',(-69.3072528758518,-13.2561802906896,
12.));
#82254=CARTESIAN_POINT('Ctrl Pts',(-69.3258709977382,-13.265813552961,0.));
#82255=CARTESIAN_POINT('Ctrl Pts',(-69.3258709977382,-13.265813552961,12.));
#82256=CARTESIAN_POINT('Ctrl Pts',(-69.3445234885065,-13.2754892884433,
0.));
#82257=CARTESIAN_POINT('Ctrl Pts',(-69.3445234885065,-13.2754892884433,
12.));
#82258=CARTESIAN_POINT('Ctrl Pts',(-69.3632101660066,-13.2852074919765,
0.));
#82259=CARTESIAN_POINT('Ctrl Pts',(-69.3632101660066,-13.2852074919765,
12.));
#82260=CARTESIAN_POINT('Ctrl Pts',(-69.3819308490422,-13.2949681583167,
0.));
#82261=CARTESIAN_POINT('Ctrl Pts',(-69.3819308490422,-13.2949681583167,
12.));
#82262=CARTESIAN_POINT('Ctrl Pts',(-69.4006853569511,-13.3047712821051,
0.));
#82263=CARTESIAN_POINT('Ctrl Pts',(-69.4006853569511,-13.3047712821051,
12.));
#82264=CARTESIAN_POINT('Ctrl Pts',(-69.4194735096265,-13.3146168578743,
0.));
#82265=CARTESIAN_POINT('Ctrl Pts',(-69.4194735096265,-13.3146168578743,
12.));
#82266=CARTESIAN_POINT('Ctrl Pts',(-69.4382951276998,-13.3245048800643,
0.));
#82267=CARTESIAN_POINT('Ctrl Pts',(-69.4382951276998,-13.3245048800643,
12.));
#82268=CARTESIAN_POINT('Ctrl Pts',(-69.4571500326673,-13.3344353430313,
0.));
#82269=CARTESIAN_POINT('Ctrl Pts',(-69.4571500326673,-13.3344353430313,
12.));
#82270=CARTESIAN_POINT('Ctrl Pts',(-69.4760380470365,-13.3444082410543,
0.));
#82271=CARTESIAN_POINT('Ctrl Pts',(-69.4760380470365,-13.3444082410543,
12.));
#82272=CARTESIAN_POINT('Ctrl Pts',(-69.4949589944606,-13.3544235683393,
0.));
#82273=CARTESIAN_POINT('Ctrl Pts',(-69.4949589944606,-13.3544235683393,
12.));
#82274=CARTESIAN_POINT('Ctrl Pts',(-69.5139126996675,-13.3644813190219,
0.));
#82275=CARTESIAN_POINT('Ctrl Pts',(-69.5139126996675,-13.3644813190219,
12.));
#82276=CARTESIAN_POINT('Ctrl Pts',(-69.5328989883885,-13.3745814871664,
0.));
#82277=CARTESIAN_POINT('Ctrl Pts',(-69.5328989883885,-13.3745814871664,
12.));
#82278=CARTESIAN_POINT('Ctrl Pts',(-69.5519176872862,-13.3847240667627,
0.));
#82279=CARTESIAN_POINT('Ctrl Pts',(-69.5519176872862,-13.3847240667627,
12.));
#82280=CARTESIAN_POINT('Ctrl Pts',(-69.5709686238724,-13.3949090517177,
0.));
#82281=CARTESIAN_POINT('Ctrl Pts',(-69.5709686238724,-13.3949090517177,
12.));
#82282=CARTESIAN_POINT('Ctrl Pts',(-69.5900516264553,-13.40513643585,0.));
#82283=CARTESIAN_POINT('Ctrl Pts',(-69.5900516264553,-13.40513643585,12.));
#82284=CARTESIAN_POINT('Ctrl Pts',(-69.6091665241765,-13.4154062129002,
0.));
#82285=CARTESIAN_POINT('Ctrl Pts',(-69.6091665241765,-13.4154062129002,
12.));
#82286=CARTESIAN_POINT('Ctrl Pts',(-69.6283131470273,-13.4257183765341,
0.));
#82287=CARTESIAN_POINT('Ctrl Pts',(-69.6283131470273,-13.4257183765341,
12.));
#82288=CARTESIAN_POINT('Ctrl Pts',(-69.6474913258675,-13.4360729203442,
0.));
#82289=CARTESIAN_POINT('Ctrl Pts',(-69.6474913258675,-13.4360729203442,
12.));
#82290=CARTESIAN_POINT('Ctrl Pts',(-69.666700892444,-13.4464698378453,0.));
#82291=CARTESIAN_POINT('Ctrl Pts',(-69.666700892444,-13.4464698378453,12.));
#82292=CARTESIAN_POINT('Ctrl Pts',(-69.6859416793886,-13.456909122476,0.));
#82293=CARTESIAN_POINT('Ctrl Pts',(-69.6859416793886,-13.456909122476,12.));
#82294=CARTESIAN_POINT('Ctrl Pts',(-69.7052135201998,-13.4673907676044,
0.));
#82295=CARTESIAN_POINT('Ctrl Pts',(-69.7052135201998,-13.4673907676044,
12.));
#82296=CARTESIAN_POINT('Ctrl Pts',(-69.724516249225,-13.4779147665285,0.));
#82297=CARTESIAN_POINT('Ctrl Pts',(-69.724516249225,-13.4779147665285,12.));
#82298=CARTESIAN_POINT('Ctrl Pts',(-69.7438497016406,-13.4884811124748,
0.));
#82299=CARTESIAN_POINT('Ctrl Pts',(-69.7438497016406,-13.4884811124748,
12.));
#82300=CARTESIAN_POINT('Ctrl Pts',(-69.7632137134249,-13.4990897985904,
0.));
#82301=CARTESIAN_POINT('Ctrl Pts',(-69.7632137134249,-13.4990897985904,
12.));
#82302=CARTESIAN_POINT('Ctrl Pts',(-69.7826081213576,-13.5097408179479,
0.));
#82303=CARTESIAN_POINT('Ctrl Pts',(-69.7826081213576,-13.5097408179479,
12.));
#82304=CARTESIAN_POINT('Ctrl Pts',(-69.8020327630205,-13.5204341635507,
0.));
#82305=CARTESIAN_POINT('Ctrl Pts',(-69.8020327630205,-13.5204341635507,
12.));
#82306=CARTESIAN_POINT('Ctrl Pts',(-69.8214874767944,-13.5311698283339,
0.));
#82307=CARTESIAN_POINT('Ctrl Pts',(-69.8214874767944,-13.5311698283339,
12.));
#82308=CARTESIAN_POINT('Ctrl Pts',(-69.840972101856,-13.5419478051625,0.));
#82309=CARTESIAN_POINT('Ctrl Pts',(-69.840972101856,-13.5419478051625,12.));
#82310=CARTESIAN_POINT('Ctrl Pts',(-69.8604864781706,-13.5527680868255,
0.));
#82311=CARTESIAN_POINT('Ctrl Pts',(-69.8604864781706,-13.5527680868255,
12.));
#82312=CARTESIAN_POINT('Ctrl Pts',(-69.8800304464882,-13.5636306660421,
0.));
#82313=CARTESIAN_POINT('Ctrl Pts',(-69.8800304464882,-13.5636306660421,
12.));
#82314=CARTESIAN_POINT('Ctrl Pts',(-69.8996038483361,-13.5745355354656,
0.));
#82315=CARTESIAN_POINT('Ctrl Pts',(-69.8996038483361,-13.5745355354656,
12.));
#82316=CARTESIAN_POINT('Ctrl Pts',(-69.9192065260108,-13.5854826876834,
0.));
#82317=CARTESIAN_POINT('Ctrl Pts',(-69.9192065260108,-13.5854826876834,
12.));
#82318=CARTESIAN_POINT('Ctrl Pts',(-69.9388383225648,-13.5964721152135,
0.));
#82319=CARTESIAN_POINT('Ctrl Pts',(-69.9388383225648,-13.5964721152135,
12.));
#82320=CARTESIAN_POINT('Ctrl Pts',(-69.9584990817974,-13.6075038104998,
0.));
#82321=CARTESIAN_POINT('Ctrl Pts',(-69.9584990817974,-13.6075038104998,
12.));
#82322=CARTESIAN_POINT('Ctrl Pts',(-69.9781886482527,-13.6185777659198,
0.));
#82323=CARTESIAN_POINT('Ctrl Pts',(-69.9781886482527,-13.6185777659198,
12.));
#82324=CARTESIAN_POINT('Ctrl Pts',(-69.9979068672153,-13.6296939737865,
0.));
#82325=CARTESIAN_POINT('Ctrl Pts',(-69.9979068672153,-13.6296939737865,
12.));
#82326=CARTESIAN_POINT('Ctrl Pts',(-70.0176535847049,-13.6408524263496,
0.));
#82327=CARTESIAN_POINT('Ctrl Pts',(-70.0176535847049,-13.6408524263496,
12.));
#82328=CARTESIAN_POINT('Ctrl Pts',(-70.0374286474677,-13.6520531157907,
0.));
#82329=CARTESIAN_POINT('Ctrl Pts',(-70.0374286474677,-13.6520531157907,
12.));
#82330=CARTESIAN_POINT('Ctrl Pts',(-70.0572319029676,-13.6632960342196,
0.));
#82331=CARTESIAN_POINT('Ctrl Pts',(-70.0572319029676,-13.6632960342196,
12.));
#82332=CARTESIAN_POINT('Ctrl Pts',(-70.0770631993856,-13.6745811736829,
0.));
#82333=CARTESIAN_POINT('Ctrl Pts',(-70.0770631993856,-13.6745811736829,
12.));
#82334=CARTESIAN_POINT('Ctrl Pts',(-70.0969223856136,-13.6859085261653,
0.));
#82335=CARTESIAN_POINT('Ctrl Pts',(-70.0969223856136,-13.6859085261653,
12.));
#82336=CARTESIAN_POINT('Ctrl Pts',(-70.1168093112486,-13.6972780835897,
0.));
#82337=CARTESIAN_POINT('Ctrl Pts',(-70.1168093112486,-13.6972780835897,
12.));
#82338=CARTESIAN_POINT('Ctrl Pts',(-70.1367238265825,-13.7086898378121,
0.));
#82339=CARTESIAN_POINT('Ctrl Pts',(-70.1367238265825,-13.7086898378121,
12.));
#82340=CARTESIAN_POINT('Ctrl Pts',(-70.156665782595,-13.7201437806199,0.));
#82341=CARTESIAN_POINT('Ctrl Pts',(-70.156665782595,-13.7201437806199,12.));
#82342=CARTESIAN_POINT('Ctrl Pts',(-70.1766350309518,-13.7316399037392,
0.));
#82343=CARTESIAN_POINT('Ctrl Pts',(-70.1766350309518,-13.7316399037392,
12.));
#82344=CARTESIAN_POINT('Ctrl Pts',(-70.1966314239995,-13.7431781988364,
0.));
#82345=CARTESIAN_POINT('Ctrl Pts',(-70.1966314239995,-13.7431781988364,
12.));
#82346=CARTESIAN_POINT('Ctrl Pts',(-70.2166548147604,-13.754758657518,0.));
#82347=CARTESIAN_POINT('Ctrl Pts',(-70.2166548147604,-13.754758657518,12.));
#82348=CARTESIAN_POINT('Ctrl Pts',(-70.2367050569215,-13.7663812713243,
0.));
#82349=CARTESIAN_POINT('Ctrl Pts',(-70.2367050569215,-13.7663812713243,
12.));
#82350=CARTESIAN_POINT('Ctrl Pts',(-70.2567820048303,-13.7780460317294,
0.));
#82351=CARTESIAN_POINT('Ctrl Pts',(-70.2567820048303,-13.7780460317294,
12.));
#82352=CARTESIAN_POINT('Ctrl Pts',(-70.2768855134947,-13.7897529301491,
0.));
#82353=CARTESIAN_POINT('Ctrl Pts',(-70.2768855134947,-13.7897529301491,
12.));
#82354=CARTESIAN_POINT('Ctrl Pts',(-70.2970154385774,-13.8015019579414,
0.));
#82355=CARTESIAN_POINT('Ctrl Pts',(-70.2970154385774,-13.8015019579414,
12.));
#82356=CARTESIAN_POINT('Ctrl Pts',(-70.3171716363897,-13.8132931064063,
0.));
#82357=CARTESIAN_POINT('Ctrl Pts',(-70.3171716363897,-13.8132931064063,
12.));
#82358=CARTESIAN_POINT('Ctrl Pts',(-70.3373539638809,-13.825126366779,0.));
#82359=CARTESIAN_POINT('Ctrl Pts',(-70.3373539638809,-13.825126366779,12.));
#82360=CARTESIAN_POINT('Ctrl Pts',(-70.3575622786335,-13.8370017302309,
0.));
#82361=CARTESIAN_POINT('Ctrl Pts',(-70.3575622786335,-13.8370017302309,
12.));
#82362=CARTESIAN_POINT('Ctrl Pts',(-70.3777964388632,-13.8489191878767,
0.));
#82363=CARTESIAN_POINT('Ctrl Pts',(-70.3777964388632,-13.8489191878767,
12.));
#82364=CARTESIAN_POINT('Ctrl Pts',(-70.3980563034133,-13.8608787307751,
0.));
#82365=CARTESIAN_POINT('Ctrl Pts',(-70.3980563034133,-13.8608787307751,
12.));
#82366=CARTESIAN_POINT('Ctrl Pts',(-70.4183417317499,-13.8728803499287,
0.));
#82367=CARTESIAN_POINT('Ctrl Pts',(-70.4183417317499,-13.8728803499287,
12.));
#82368=CARTESIAN_POINT('Ctrl Pts',(-70.4386525839521,-13.8849240362763,
0.));
#82369=CARTESIAN_POINT('Ctrl Pts',(-70.4386525839521,-13.8849240362763,
12.));
#82370=CARTESIAN_POINT('Ctrl Pts',(-70.4589887207073,-13.8970097806953,
0.));
#82371=CARTESIAN_POINT('Ctrl Pts',(-70.4589887207073,-13.8970097806953,
12.));
#82372=CARTESIAN_POINT('Ctrl Pts',(-70.4793500033124,-13.9091375740088,
0.));
#82373=CARTESIAN_POINT('Ctrl Pts',(-70.4793500033124,-13.9091375740088,
12.));
#82374=CARTESIAN_POINT('Ctrl Pts',(-70.4997362936673,-13.9213074069852,
0.));
#82375=CARTESIAN_POINT('Ctrl Pts',(-70.4997362936673,-13.9213074069852,
12.));
#82376=CARTESIAN_POINT('Ctrl Pts',(-70.520147454271,-13.9335192703388,0.));
#82377=CARTESIAN_POINT('Ctrl Pts',(-70.520147454271,-13.9335192703388,12.));
#82378=CARTESIAN_POINT('Ctrl Pts',(-70.5405833482112,-13.9457731547215,
0.));
#82379=CARTESIAN_POINT('Ctrl Pts',(-70.5405833482112,-13.9457731547215,
12.));
#82380=CARTESIAN_POINT('Ctrl Pts',(-70.5610438391612,-13.958069050726,0.));
#82381=CARTESIAN_POINT('Ctrl Pts',(-70.5610438391612,-13.958069050726,12.));
#82382=CARTESIAN_POINT('Ctrl Pts',(-70.5815287913784,-13.9704069488917,
0.));
#82383=CARTESIAN_POINT('Ctrl Pts',(-70.5815287913784,-13.9704069488917,
12.));
#82384=CARTESIAN_POINT('Ctrl Pts',(-70.6020380697004,-13.9827868397057,
0.));
#82385=CARTESIAN_POINT('Ctrl Pts',(-70.6020380697004,-13.9827868397057,
12.));
#82386=CARTESIAN_POINT('Ctrl Pts',(-70.6225715395394,-13.9952087136018,
0.));
#82387=CARTESIAN_POINT('Ctrl Pts',(-70.6225715395394,-13.9952087136018,
12.));
#82388=CARTESIAN_POINT('Ctrl Pts',(-70.6431290668745,-14.0076725609536,
0.));
#82389=CARTESIAN_POINT('Ctrl Pts',(-70.6431290668745,-14.0076725609536,
12.));
#82390=CARTESIAN_POINT('Ctrl Pts',(-70.6637105182484,-14.0201783720769,
0.));
#82391=CARTESIAN_POINT('Ctrl Pts',(-70.6637105182484,-14.0201783720769,
12.));
#82392=CARTESIAN_POINT('Ctrl Pts',(-70.6843157607668,-14.0327261372362,
0.));
#82393=CARTESIAN_POINT('Ctrl Pts',(-70.6843157607668,-14.0327261372362,
12.));
#82394=CARTESIAN_POINT('Ctrl Pts',(-70.7049446620928,-14.0453158466451,
0.));
#82395=CARTESIAN_POINT('Ctrl Pts',(-70.7049446620928,-14.0453158466451,
12.));
#82396=CARTESIAN_POINT('Ctrl Pts',(-70.7255970904436,-14.0579474904657,
0.));
#82397=CARTESIAN_POINT('Ctrl Pts',(-70.7255970904436,-14.0579474904657,
12.));
#82398=CARTESIAN_POINT('Ctrl Pts',(-70.7462729145807,-14.0706210588016,
0.));
#82399=CARTESIAN_POINT('Ctrl Pts',(-70.7462729145807,-14.0706210588016,
12.));
#82400=CARTESIAN_POINT('Ctrl Pts',(-70.7669720038077,-14.0833365416996,
0.));
#82401=CARTESIAN_POINT('Ctrl Pts',(-70.7669720038077,-14.0833365416996,
12.));
#82402=CARTESIAN_POINT('Ctrl Pts',(-70.7876942279697,-14.0960939291569,
0.));
#82403=CARTESIAN_POINT('Ctrl Pts',(-70.7876942279697,-14.0960939291569,
12.));
#82404=CARTESIAN_POINT('Ctrl Pts',(-70.8084394574493,-14.1088932111214,
0.));
#82405=CARTESIAN_POINT('Ctrl Pts',(-70.8084394574493,-14.1088932111214,
12.));
#82406=CARTESIAN_POINT('Ctrl Pts',(-70.8292075631621,-14.1217343774913,
0.));
#82407=CARTESIAN_POINT('Ctrl Pts',(-70.8292075631621,-14.1217343774913,
12.));
#82408=CARTESIAN_POINT('Ctrl Pts',(-70.8499984165489,-14.1346174181078,
0.));
#82409=CARTESIAN_POINT('Ctrl Pts',(-70.8499984165489,-14.1346174181078,
12.));
#82410=CARTESIAN_POINT('Ctrl Pts',(-70.8708118895715,-14.1475423227568,
0.));
#82411=CARTESIAN_POINT('Ctrl Pts',(-70.8708118895715,-14.1475423227568,
12.));
#82412=CARTESIAN_POINT('Ctrl Pts',(-70.8916478547132,-14.1605090811754,
0.));
#82413=CARTESIAN_POINT('Ctrl Pts',(-70.8916478547132,-14.1605090811754,
12.));
#82414=CARTESIAN_POINT('Ctrl Pts',(-70.9125061849745,-14.1735176830533,
0.));
#82415=CARTESIAN_POINT('Ctrl Pts',(-70.9125061849745,-14.1735176830533,
12.));
#82416=CARTESIAN_POINT('Ctrl Pts',(-70.9333867538704,-14.186568118032,0.));
#82417=CARTESIAN_POINT('Ctrl Pts',(-70.9333867538704,-14.186568118032,12.));
#82418=CARTESIAN_POINT('Ctrl Pts',(-70.9542894354216,-14.1996603756982,
0.));
#82419=CARTESIAN_POINT('Ctrl Pts',(-70.9542894354216,-14.1996603756982,
12.));
#82420=CARTESIAN_POINT('Ctrl Pts',(-70.9752141041518,-14.2127944455838,
0.));
#82421=CARTESIAN_POINT('Ctrl Pts',(-70.9752141041518,-14.2127944455838,
12.));
#82422=CARTESIAN_POINT('Ctrl Pts',(-70.9961606350861,-14.2259703171737,
0.));
#82423=CARTESIAN_POINT('Ctrl Pts',(-70.9961606350861,-14.2259703171737,
12.));
#82424=CARTESIAN_POINT('Ctrl Pts',(-71.0171289037488,-14.2391879799061,
0.));
#82425=CARTESIAN_POINT('Ctrl Pts',(-71.0171289037488,-14.2391879799061,
12.));
#82426=CARTESIAN_POINT('Ctrl Pts',(-71.0381187861588,-14.2524474231732,
0.));
#82427=CARTESIAN_POINT('Ctrl Pts',(-71.0381187861588,-14.2524474231732,
12.));
#82428=CARTESIAN_POINT('Ctrl Pts',(-71.0591301588231,-14.2657486363139,
0.));
#82429=CARTESIAN_POINT('Ctrl Pts',(-71.0591301588231,-14.2657486363139,
12.));
#82430=CARTESIAN_POINT('Ctrl Pts',(-71.0801628987332,-14.2790916086133,
0.));
#82431=CARTESIAN_POINT('Ctrl Pts',(-71.0801628987332,-14.2790916086133,
12.));
#82432=CARTESIAN_POINT('Ctrl Pts',(-71.1012168833643,-14.2924763293105,
0.));
#82433=CARTESIAN_POINT('Ctrl Pts',(-71.1012168833643,-14.2924763293105,
12.));
#82434=CARTESIAN_POINT('Ctrl Pts',(-71.1222919906727,-14.3059027875994,
0.));
#82435=CARTESIAN_POINT('Ctrl Pts',(-71.1222919906727,-14.3059027875994,
12.));
#82436=CARTESIAN_POINT('Ctrl Pts',(-71.1433880990929,-14.3193709726294,
0.));
#82437=CARTESIAN_POINT('Ctrl Pts',(-71.1433880990929,-14.3193709726294,
12.));
#82438=CARTESIAN_POINT('Ctrl Pts',(-71.1645050875308,-14.3328808734989,
0.));
#82439=CARTESIAN_POINT('Ctrl Pts',(-71.1645050875308,-14.3328808734989,
12.));
#82440=CARTESIAN_POINT('Ctrl Pts',(-71.1856428353593,-14.3464324792533,
0.));
#82441=CARTESIAN_POINT('Ctrl Pts',(-71.1856428353593,-14.3464324792533,
12.));
#82442=CARTESIAN_POINT('Ctrl Pts',(-71.2068012224174,-14.3600257788924,
0.));
#82443=CARTESIAN_POINT('Ctrl Pts',(-71.2068012224174,-14.3600257788924,
12.));
#82444=CARTESIAN_POINT('Ctrl Pts',(-71.2279801290084,-14.3736607613722,
0.));
#82445=CARTESIAN_POINT('Ctrl Pts',(-71.2279801290084,-14.3736607613722,
12.));
#82446=CARTESIAN_POINT('Ctrl Pts',(-71.2491794358958,-14.3873374156056,
0.));
#82447=CARTESIAN_POINT('Ctrl Pts',(-71.2491794358958,-14.3873374156056,
12.));
#82448=CARTESIAN_POINT('Ctrl Pts',(-71.2703990242988,-14.401055730457,0.));
#82449=CARTESIAN_POINT('Ctrl Pts',(-71.2703990242988,-14.401055730457,12.));
#82450=CARTESIAN_POINT('Ctrl Pts',(-71.2916387758861,-14.4148156947384,
0.));
#82451=CARTESIAN_POINT('Ctrl Pts',(-71.2916387758861,-14.4148156947384,
12.));
#82452=CARTESIAN_POINT('Ctrl Pts',(-71.312898572777,-14.4286172972166,0.));
#82453=CARTESIAN_POINT('Ctrl Pts',(-71.312898572777,-14.4286172972166,12.));
#82454=CARTESIAN_POINT('Ctrl Pts',(-71.3341782975386,-14.4424605266165,
0.));
#82455=CARTESIAN_POINT('Ctrl Pts',(-71.3341782975386,-14.4424605266165,
12.));
#82456=CARTESIAN_POINT('Ctrl Pts',(-71.3554778331835,-14.4563453716204,
0.));
#82457=CARTESIAN_POINT('Ctrl Pts',(-71.3554778331835,-14.4563453716204,
12.));
#82458=CARTESIAN_POINT('Ctrl Pts',(-71.376797063165,-14.4702718208651,0.));
#82459=CARTESIAN_POINT('Ctrl Pts',(-71.376797063165,-14.4702718208651,12.));
#82460=CARTESIAN_POINT('Ctrl Pts',(-71.3981358713723,-14.4842398629355,
0.));
#82461=CARTESIAN_POINT('Ctrl Pts',(-71.3981358713723,-14.4842398629355,
12.));
#82462=CARTESIAN_POINT('Ctrl Pts',(-71.4194941421292,-14.4982494863718,
0.));
#82463=CARTESIAN_POINT('Ctrl Pts',(-71.4194941421292,-14.4982494863718,
12.));
#82464=CARTESIAN_POINT('Ctrl Pts',(-71.4408717601923,-14.5123006796728,
0.));
#82465=CARTESIAN_POINT('Ctrl Pts',(-71.4408717601923,-14.5123006796728,
12.));
#82466=CARTESIAN_POINT('Ctrl Pts',(-71.4622686107475,-14.5263934312969,
0.));
#82467=CARTESIAN_POINT('Ctrl Pts',(-71.4622686107475,-14.5263934312969,
12.));
#82468=CARTESIAN_POINT('Ctrl Pts',(-71.4836845794048,-14.540527729659,0.));
#82469=CARTESIAN_POINT('Ctrl Pts',(-71.4836845794048,-14.540527729659,12.));
#82470=CARTESIAN_POINT('Ctrl Pts',(-71.5051195521909,-14.5547035631233,
0.));
#82471=CARTESIAN_POINT('Ctrl Pts',(-71.5051195521909,-14.5547035631233,
12.));
#82472=CARTESIAN_POINT('Ctrl Pts',(-71.5265734155498,-14.5689209200091,
0.));
#82473=CARTESIAN_POINT('Ctrl Pts',(-71.5265734155498,-14.5689209200091,
12.));
#82474=CARTESIAN_POINT('Ctrl Pts',(-71.5480460563447,-14.5831797885952,
0.));
#82475=CARTESIAN_POINT('Ctrl Pts',(-71.5480460563447,-14.5831797885952,
12.));
#82476=CARTESIAN_POINT('Ctrl Pts',(-71.5695373618562,-14.597480157121,0.));
#82477=CARTESIAN_POINT('Ctrl Pts',(-71.5695373618562,-14.597480157121,12.));
#82478=CARTESIAN_POINT('Ctrl Pts',(-71.5910472197813,-14.6118220137849,
0.));
#82479=CARTESIAN_POINT('Ctrl Pts',(-71.5910472197813,-14.6118220137849,
12.));
#82480=CARTESIAN_POINT('Ctrl Pts',(-71.612575518229,-14.626205346737,0.));
#82481=CARTESIAN_POINT('Ctrl Pts',(-71.612575518229,-14.626205346737,12.));
#82482=CARTESIAN_POINT('Ctrl Pts',(-71.6341221457168,-14.6406301440814,
0.));
#82483=CARTESIAN_POINT('Ctrl Pts',(-71.6341221457168,-14.6406301440814,
12.));
#82484=CARTESIAN_POINT('Ctrl Pts',(-71.6556869911662,-14.6550963938829,
0.));
#82485=CARTESIAN_POINT('Ctrl Pts',(-71.6556869911662,-14.6550963938829,
12.));
#82486=CARTESIAN_POINT('Ctrl Pts',(-71.6772699438963,-14.6696040841678,
0.));
#82487=CARTESIAN_POINT('Ctrl Pts',(-71.6772699438963,-14.6696040841678,
12.));
#82488=CARTESIAN_POINT('Ctrl Pts',(-71.6988708936172,-14.6841532029232,
0.));
#82489=CARTESIAN_POINT('Ctrl Pts',(-71.6988708936172,-14.6841532029232,
12.));
#82490=CARTESIAN_POINT('Ctrl Pts',(-71.7204897304194,-14.69874373809,0.));
#82491=CARTESIAN_POINT('Ctrl Pts',(-71.7204897304194,-14.69874373809,12.));
#82492=CARTESIAN_POINT('Ctrl Pts',(-71.7421263447719,-14.7133756775625,
0.));
#82493=CARTESIAN_POINT('Ctrl Pts',(-71.7421263447719,-14.7133756775625,
12.));
#82494=CARTESIAN_POINT('Ctrl Pts',(-71.7637806275328,-14.7280490091957,
0.));
#82495=CARTESIAN_POINT('Ctrl Pts',(-71.7637806275328,-14.7280490091957,
12.));
#82496=CARTESIAN_POINT('Ctrl Pts',(-71.7854524699569,-14.7427637208072,
0.));
#82497=CARTESIAN_POINT('Ctrl Pts',(-71.7854524699569,-14.7427637208072,
12.));
#82498=CARTESIAN_POINT('Ctrl Pts',(-71.8071417637017,-14.7575198001776,
0.));
#82499=CARTESIAN_POINT('Ctrl Pts',(-71.8071417637017,-14.7575198001776,
12.));
#82500=CARTESIAN_POINT('Ctrl Pts',(-71.8288484008333,-14.7723172350451,
0.));
#82501=CARTESIAN_POINT('Ctrl Pts',(-71.8288484008333,-14.7723172350451,
12.));
#82502=CARTESIAN_POINT('Ctrl Pts',(-71.8505722738272,-14.7871560131016,
0.));
#82503=CARTESIAN_POINT('Ctrl Pts',(-71.8505722738272,-14.7871560131016,
12.));
#82504=CARTESIAN_POINT('Ctrl Pts',(-71.8723132755446,-14.8020361219998,
0.));
#82505=CARTESIAN_POINT('Ctrl Pts',(-71.8723132755446,-14.8020361219998,
12.));
#82506=CARTESIAN_POINT('Ctrl Pts',(-71.8940712992109,-14.8169575493557,
0.));
#82507=CARTESIAN_POINT('Ctrl Pts',(-71.8940712992109,-14.8169575493557,
12.));
#82508=CARTESIAN_POINT('Ctrl Pts',(-71.9158462383914,-14.8319202827482,
0.));
#82509=CARTESIAN_POINT('Ctrl Pts',(-71.9158462383914,-14.8319202827482,
12.));
#82510=CARTESIAN_POINT('Ctrl Pts',(-71.9376379869678,-14.8469243097162,
0.));
#82511=CARTESIAN_POINT('Ctrl Pts',(-71.9376379869678,-14.8469243097162,
12.));
#82512=CARTESIAN_POINT('Ctrl Pts',(-71.9594464391078,-14.8619696177506,
0.));
#82513=CARTESIAN_POINT('Ctrl Pts',(-71.9594464391078,-14.8619696177506,
12.));
#82514=CARTESIAN_POINT('Ctrl Pts',(-71.9812714893102,-14.8770561943014,
0.));
#82515=CARTESIAN_POINT('Ctrl Pts',(-71.9812714893102,-14.8770561943014,
12.));
#82516=CARTESIAN_POINT('Ctrl Pts',(-72.0031130324529,-14.8921840267832,
0.));
#82517=CARTESIAN_POINT('Ctrl Pts',(-72.0031130324529,-14.8921840267832,
12.));
#82518=CARTESIAN_POINT('Ctrl Pts',(-72.0249709638422,-14.9073531025764,
0.));
#82519=CARTESIAN_POINT('Ctrl Pts',(-72.0249709638422,-14.9073531025764,
12.));
#82520=CARTESIAN_POINT('Ctrl Pts',(-72.0468451792505,-14.9225634090268,
0.));
#82521=CARTESIAN_POINT('Ctrl Pts',(-72.0468451792505,-14.9225634090268,
12.));
#82522=CARTESIAN_POINT('Ctrl Pts',(-72.0687355749806,-14.9378149334388,
0.));
#82523=CARTESIAN_POINT('Ctrl Pts',(-72.0687355749806,-14.9378149334388,
12.));
#82524=CARTESIAN_POINT('Ctrl Pts',(-72.0906420478076,-14.9531076630767,
0.));
#82525=CARTESIAN_POINT('Ctrl Pts',(-72.0906420478076,-14.9531076630767,
12.));
#82526=CARTESIAN_POINT('Ctrl Pts',(-72.112564494854,-14.9684415851698,0.));
#82527=CARTESIAN_POINT('Ctrl Pts',(-72.112564494854,-14.9684415851698,12.));
#82528=CARTESIAN_POINT('Ctrl Pts',(-72.1345028134777,-14.9838166869107,
0.));
#82529=CARTESIAN_POINT('Ctrl Pts',(-72.1345028134777,-14.9838166869107,
12.));
#82530=CARTESIAN_POINT('Ctrl Pts',(-72.1564569011669,-14.9992329554537,
0.));
#82531=CARTESIAN_POINT('Ctrl Pts',(-72.1564569011669,-14.9992329554537,
12.));
#82532=CARTESIAN_POINT('Ctrl Pts',(-72.1784266553953,-15.0146903779062,
0.));
#82533=CARTESIAN_POINT('Ctrl Pts',(-72.1784266553953,-15.0146903779062,
12.));
#82534=CARTESIAN_POINT('Ctrl Pts',(-72.2004119736115,-15.0301889413257,
0.));
#82535=CARTESIAN_POINT('Ctrl Pts',(-72.2004119736115,-15.0301889413257,
12.));
#82536=CARTESIAN_POINT('Ctrl Pts',(-72.2224127535415,-15.0457286327331,
0.));
#82537=CARTESIAN_POINT('Ctrl Pts',(-72.2224127535415,-15.0457286327331,
12.));
#82538=CARTESIAN_POINT('Ctrl Pts',(-72.2444288934262,-15.0613094391189,
0.));
#82539=CARTESIAN_POINT('Ctrl Pts',(-72.2444288934262,-15.0613094391189,
12.));
#82540=CARTESIAN_POINT('Ctrl Pts',(-72.2664602922852,-15.0769313474476,
0.));
#82541=CARTESIAN_POINT('Ctrl Pts',(-72.2664602922852,-15.0769313474476,
12.));
#82542=CARTESIAN_POINT('Ctrl Pts',(-72.2885068501628,-15.0925943446589,
0.));
#82543=CARTESIAN_POINT('Ctrl Pts',(-72.2885068501628,-15.0925943446589,
12.));
#82544=CARTESIAN_POINT('Ctrl Pts',(-72.3105684683944,-15.1082984176649,
0.));
#82545=CARTESIAN_POINT('Ctrl Pts',(-72.3105684683944,-15.1082984176649,
12.));
#82546=CARTESIAN_POINT('Ctrl Pts',(-72.3326450490177,-15.124043553347,0.));
#82547=CARTESIAN_POINT('Ctrl Pts',(-72.3326450490177,-15.124043553347,12.));
#82548=CARTESIAN_POINT('Ctrl Pts',(-72.3547364941969,-15.1398297385506,
0.));
#82549=CARTESIAN_POINT('Ctrl Pts',(-72.3547364941969,-15.1398297385506,
12.));
#82550=CARTESIAN_POINT('Ctrl Pts',(-72.376842705589,-15.1556569600744,0.));
#82551=CARTESIAN_POINT('Ctrl Pts',(-72.376842705589,-15.1556569600744,12.));
#82552=CARTESIAN_POINT('Ctrl Pts',(-72.3989635838492,-15.1715252046606,
0.));
#82553=CARTESIAN_POINT('Ctrl Pts',(-72.3989635838492,-15.1715252046606,
12.));
#82554=CARTESIAN_POINT('Ctrl Pts',(-72.421099027786,-15.1874344589725,0.));
#82555=CARTESIAN_POINT('Ctrl Pts',(-72.421099027786,-15.1874344589725,12.));
#82556=CARTESIAN_POINT('Ctrl Pts',(-72.4432489350471,-15.2033847096091,
0.));
#82557=CARTESIAN_POINT('Ctrl Pts',(-72.4432489350471,-15.2033847096091,
12.));
#82558=CARTESIAN_POINT('Ctrl Pts',(-72.4654132036428,-15.2193759431372,
0.));
#82559=CARTESIAN_POINT('Ctrl Pts',(-72.4654132036428,-15.2193759431372,
12.));
#82560=CARTESIAN_POINT('Ctrl Pts',(-72.4875917332761,-15.235408146116,0.));
#82561=CARTESIAN_POINT('Ctrl Pts',(-72.4875917332761,-15.235408146116,12.));
#82562=CARTESIAN_POINT('Ctrl Pts',(-72.5097844266075,-15.2514813051172,
0.));
#82563=CARTESIAN_POINT('Ctrl Pts',(-72.5097844266075,-15.2514813051172,
12.));
#82564=CARTESIAN_POINT('Ctrl Pts',(-72.5319911908917,-15.2675954067479,
0.));
#82565=CARTESIAN_POINT('Ctrl Pts',(-72.5319911908917,-15.2675954067479,
12.));
#82566=CARTESIAN_POINT('Ctrl Pts',(-72.5542119383642,-15.2837504376535,
0.));
#82567=CARTESIAN_POINT('Ctrl Pts',(-72.5542119383642,-15.2837504376535,
12.));
#82568=CARTESIAN_POINT('Ctrl Pts',(-72.5764465826224,-15.299946384466,0.));
#82569=CARTESIAN_POINT('Ctrl Pts',(-72.5764465826224,-15.299946384466,12.));
#82570=CARTESIAN_POINT('Ctrl Pts',(-72.5986950357677,-15.3161832337594,
0.));
#82571=CARTESIAN_POINT('Ctrl Pts',(-72.5986950357677,-15.3161832337594,
12.));
#82572=CARTESIAN_POINT('Ctrl Pts',(-72.6209572051042,-15.3324609719955,
0.));
#82573=CARTESIAN_POINT('Ctrl Pts',(-72.6209572051042,-15.3324609719955,
12.));
#82574=CARTESIAN_POINT('Ctrl Pts',(-72.6432329903553,-15.3487795854745,
0.));
#82575=CARTESIAN_POINT('Ctrl Pts',(-72.6432329903553,-15.3487795854745,
12.));
#82576=CARTESIAN_POINT('Ctrl Pts',(-72.6655222797801,-15.3651390602665,
0.));
#82577=CARTESIAN_POINT('Ctrl Pts',(-72.6655222797801,-15.3651390602665,
12.));
#82578=CARTESIAN_POINT('Ctrl Pts',(-72.687824955772,-15.3815393822736,0.));
#82579=CARTESIAN_POINT('Ctrl Pts',(-72.687824955772,-15.3815393822736,12.));
#82580=CARTESIAN_POINT('Ctrl Pts',(-72.7101409017716,-15.3979805373174,
0.));
#82581=CARTESIAN_POINT('Ctrl Pts',(-72.7101409017716,-15.3979805373174,
12.));
#82582=CARTESIAN_POINT('Ctrl Pts',(-72.7324700089712,-15.4144625111944,
0.));
#82583=CARTESIAN_POINT('Ctrl Pts',(-72.7324700089712,-15.4144625111944,
12.));
#82584=CARTESIAN_POINT('Ctrl Pts',(-72.7548121825342,-15.4309852897844,
0.));
#82585=CARTESIAN_POINT('Ctrl Pts',(-72.7548121825342,-15.4309852897844,
12.));
#82586=CARTESIAN_POINT('Ctrl Pts',(-72.777167349421,-15.4475488590243,0.));
#82587=CARTESIAN_POINT('Ctrl Pts',(-72.777167349421,-15.4475488590243,12.));
#82588=CARTESIAN_POINT('Ctrl Pts',(-72.7995354603795,-15.4641532053281,
0.));
#82589=CARTESIAN_POINT('Ctrl Pts',(-72.7995354603795,-15.4641532053281,
12.));
#82590=CARTESIAN_POINT('Ctrl Pts',(-72.8219164843279,-15.4807983165804,
0.));
#82591=CARTESIAN_POINT('Ctrl Pts',(-72.8219164843279,-15.4807983165804,
12.));
#82592=CARTESIAN_POINT('Ctrl Pts',(-72.8398316205897,-15.494147009702,0.));
#82593=CARTESIAN_POINT('Ctrl Pts',(-72.8398316205897,-15.494147009702,12.));
#82594=CARTESIAN_POINT('Ctrl Pts',(-72.8532737731759,-15.5041768663998,
0.));
#82595=CARTESIAN_POINT('Ctrl Pts',(-72.8532737731759,-15.5041768663998,
12.));
#82596=CARTESIAN_POINT('Ctrl Pts',(-72.8622377860824,-15.5108715869141,
0.));
#82597=CARTESIAN_POINT('Ctrl Pts',(-72.8622377860824,-15.5108715869141,
12.));
#82598=CARTESIAN_POINT('Ctrl Pts',(-72.8667204369977,-15.5142209845168,
0.));
#82599=CARTESIAN_POINT('Ctrl Pts',(-72.8667204369977,-15.5142209845168,
12.));
#82600=CARTESIAN_POINT('',(-68.7831490561748,-12.9953224629497,0.));
#82601=CARTESIAN_POINT('Ctrl Pts',(-68.7831490561748,-12.9953224629497,
0.));
#82602=CARTESIAN_POINT('Ctrl Pts',(-68.7866525680193,-12.9969981460277,
0.));
#82603=CARTESIAN_POINT('Ctrl Pts',(-68.7936635625545,-13.0003537683054,
0.));
#82604=CARTESIAN_POINT('Ctrl Pts',(-68.804191966902,-13.0053999700875,0.));
#82605=CARTESIAN_POINT('Ctrl Pts',(-68.8182536653656,-13.0121537768945,
0.));
#82606=CARTESIAN_POINT('Ctrl Pts',(-68.8358704887468,-13.0206386039691,
0.));
#82607=CARTESIAN_POINT('Ctrl Pts',(-68.8535269726793,-13.0291660060107,
0.));
#82608=CARTESIAN_POINT('Ctrl Pts',(-68.8712230321906,-13.0377359881875,
0.));
#82609=CARTESIAN_POINT('Ctrl Pts',(-68.8889585151585,-13.0463485518206,
0.));
#82610=CARTESIAN_POINT('Ctrl Pts',(-68.9067332040985,-13.0550036938813,
0.));
#82611=CARTESIAN_POINT('Ctrl Pts',(-68.9245468449945,-13.0637014089029,
0.));
#82612=CARTESIAN_POINT('Ctrl Pts',(-68.9423991694492,-13.072441690283,0.));
#82613=CARTESIAN_POINT('Ctrl Pts',(-68.9602899187573,-13.0812245317807,
0.));
#82614=CARTESIAN_POINT('Ctrl Pts',(-68.9782188692581,-13.090049929053,0.));
#82615=CARTESIAN_POINT('Ctrl Pts',(-68.9961858241519,-13.0989178791833,
0.));
#82616=CARTESIAN_POINT('Ctrl Pts',(-69.0141906015113,-13.1078283799722,
0.));
#82617=CARTESIAN_POINT('Ctrl Pts',(-69.0322330243348,-13.1167814293497,
0.));
#82618=CARTESIAN_POINT('Ctrl Pts',(-69.0503129081817,-13.1257770246385,
0.));
#82619=CARTESIAN_POINT('Ctrl Pts',(-69.0684300549477,-13.1348151621834,
0.));
#82620=CARTESIAN_POINT('Ctrl Pts',(-69.0865842593102,-13.1438958377404,
0.));
#82621=CARTESIAN_POINT('Ctrl Pts',(-69.1047753127643,-13.1530190467183,
0.));
#82622=CARTESIAN_POINT('Ctrl Pts',(-69.1230030082573,-13.1621847844528,
0.));
#82623=CARTESIAN_POINT('Ctrl Pts',(-69.1412671454564,-13.1713930465132,
0.));
#82624=CARTESIAN_POINT('Ctrl Pts',(-69.1595675305245,-13.1806438286934,
0.));
#82625=CARTESIAN_POINT('Ctrl Pts',(-69.1779039735996,-13.1899371268683,
0.));
#82626=CARTESIAN_POINT('Ctrl Pts',(-69.1962762870527,-13.1992729368928,
0.));
#82627=CARTESIAN_POINT('Ctrl Pts',(-69.2146842833537,-13.2086512544735,
0.));
#82628=CARTESIAN_POINT('Ctrl Pts',(-69.2331277732861,-13.2180720750594,
0.));
#82629=CARTESIAN_POINT('Ctrl Pts',(-69.2516065668844,-13.2275353939051,
0.));
#82630=CARTESIAN_POINT('Ctrl Pts',(-69.2701204742449,-13.237041206122,0.));
#82631=CARTESIAN_POINT('Ctrl Pts',(-69.2886693063182,-13.2465895067262,
0.));
#82632=CARTESIAN_POINT('Ctrl Pts',(-69.3072528758518,-13.2561802906896,
0.));
#82633=CARTESIAN_POINT('Ctrl Pts',(-69.3258709977382,-13.265813552961,0.));
#82634=CARTESIAN_POINT('Ctrl Pts',(-69.3445234885065,-13.2754892884433,
0.));
#82635=CARTESIAN_POINT('Ctrl Pts',(-69.3632101660066,-13.2852074919765,
0.));
#82636=CARTESIAN_POINT('Ctrl Pts',(-69.3819308490422,-13.2949681583167,
0.));
#82637=CARTESIAN_POINT('Ctrl Pts',(-69.4006853569511,-13.3047712821051,
0.));
#82638=CARTESIAN_POINT('Ctrl Pts',(-69.4194735096265,-13.3146168578743,
0.));
#82639=CARTESIAN_POINT('Ctrl Pts',(-69.4382951276998,-13.3245048800643,
0.));
#82640=CARTESIAN_POINT('Ctrl Pts',(-69.4571500326673,-13.3344353430313,
0.));
#82641=CARTESIAN_POINT('Ctrl Pts',(-69.4760380470365,-13.3444082410543,
0.));
#82642=CARTESIAN_POINT('Ctrl Pts',(-69.4949589944606,-13.3544235683393,
0.));
#82643=CARTESIAN_POINT('Ctrl Pts',(-69.5139126996675,-13.3644813190219,
0.));
#82644=CARTESIAN_POINT('Ctrl Pts',(-69.5328989883885,-13.3745814871664,
0.));
#82645=CARTESIAN_POINT('Ctrl Pts',(-69.5519176872862,-13.3847240667627,
0.));
#82646=CARTESIAN_POINT('Ctrl Pts',(-69.5709686238724,-13.3949090517177,
0.));
#82647=CARTESIAN_POINT('Ctrl Pts',(-69.5900516264553,-13.40513643585,0.));
#82648=CARTESIAN_POINT('Ctrl Pts',(-69.6091665241765,-13.4154062129002,
0.));
#82649=CARTESIAN_POINT('Ctrl Pts',(-69.6283131470273,-13.4257183765341,
0.));
#82650=CARTESIAN_POINT('Ctrl Pts',(-69.6474913258675,-13.4360729203442,
0.));
#82651=CARTESIAN_POINT('Ctrl Pts',(-69.666700892444,-13.4464698378453,0.));
#82652=CARTESIAN_POINT('Ctrl Pts',(-69.6859416793886,-13.456909122476,0.));
#82653=CARTESIAN_POINT('Ctrl Pts',(-69.7052135201998,-13.4673907676044,
0.));
#82654=CARTESIAN_POINT('Ctrl Pts',(-69.724516249225,-13.4779147665285,0.));
#82655=CARTESIAN_POINT('Ctrl Pts',(-69.7438497016406,-13.4884811124748,
0.));
#82656=CARTESIAN_POINT('Ctrl Pts',(-69.7632137134249,-13.4990897985904,
0.));
#82657=CARTESIAN_POINT('Ctrl Pts',(-69.7826081213576,-13.5097408179479,
0.));
#82658=CARTESIAN_POINT('Ctrl Pts',(-69.8020327630205,-13.5204341635507,
0.));
#82659=CARTESIAN_POINT('Ctrl Pts',(-69.8214874767944,-13.5311698283339,
0.));
#82660=CARTESIAN_POINT('Ctrl Pts',(-69.840972101856,-13.5419478051625,0.));
#82661=CARTESIAN_POINT('Ctrl Pts',(-69.8604864781706,-13.5527680868255,
0.));
#82662=CARTESIAN_POINT('Ctrl Pts',(-69.8800304464882,-13.5636306660421,
0.));
#82663=CARTESIAN_POINT('Ctrl Pts',(-69.8996038483361,-13.5745355354656,
0.));
#82664=CARTESIAN_POINT('Ctrl Pts',(-69.9192065260108,-13.5854826876834,
0.));
#82665=CARTESIAN_POINT('Ctrl Pts',(-69.9388383225648,-13.5964721152135,
0.));
#82666=CARTESIAN_POINT('Ctrl Pts',(-69.9584990817974,-13.6075038104998,
0.));
#82667=CARTESIAN_POINT('Ctrl Pts',(-69.9781886482527,-13.6185777659198,
0.));
#82668=CARTESIAN_POINT('Ctrl Pts',(-69.9979068672153,-13.6296939737865,
0.));
#82669=CARTESIAN_POINT('Ctrl Pts',(-70.0176535847049,-13.6408524263496,
0.));
#82670=CARTESIAN_POINT('Ctrl Pts',(-70.0374286474677,-13.6520531157907,
0.));
#82671=CARTESIAN_POINT('Ctrl Pts',(-70.0572319029676,-13.6632960342196,
0.));
#82672=CARTESIAN_POINT('Ctrl Pts',(-70.0770631993856,-13.6745811736829,
0.));
#82673=CARTESIAN_POINT('Ctrl Pts',(-70.0969223856136,-13.6859085261653,
0.));
#82674=CARTESIAN_POINT('Ctrl Pts',(-70.1168093112486,-13.6972780835897,
0.));
#82675=CARTESIAN_POINT('Ctrl Pts',(-70.1367238265825,-13.7086898378121,
0.));
#82676=CARTESIAN_POINT('Ctrl Pts',(-70.156665782595,-13.7201437806199,0.));
#82677=CARTESIAN_POINT('Ctrl Pts',(-70.1766350309518,-13.7316399037392,
0.));
#82678=CARTESIAN_POINT('Ctrl Pts',(-70.1966314239995,-13.7431781988364,
0.));
#82679=CARTESIAN_POINT('Ctrl Pts',(-70.2166548147604,-13.754758657518,0.));
#82680=CARTESIAN_POINT('Ctrl Pts',(-70.2367050569215,-13.7663812713243,
0.));
#82681=CARTESIAN_POINT('Ctrl Pts',(-70.2567820048303,-13.7780460317294,
0.));
#82682=CARTESIAN_POINT('Ctrl Pts',(-70.2768855134947,-13.7897529301491,
0.));
#82683=CARTESIAN_POINT('Ctrl Pts',(-70.2970154385774,-13.8015019579414,
0.));
#82684=CARTESIAN_POINT('Ctrl Pts',(-70.3171716363897,-13.8132931064063,
0.));
#82685=CARTESIAN_POINT('Ctrl Pts',(-70.3373539638809,-13.825126366779,0.));
#82686=CARTESIAN_POINT('Ctrl Pts',(-70.3575622786335,-13.8370017302309,
0.));
#82687=CARTESIAN_POINT('Ctrl Pts',(-70.3777964388632,-13.8489191878767,
0.));
#82688=CARTESIAN_POINT('Ctrl Pts',(-70.3980563034133,-13.8608787307751,
0.));
#82689=CARTESIAN_POINT('Ctrl Pts',(-70.4183417317499,-13.8728803499287,
0.));
#82690=CARTESIAN_POINT('Ctrl Pts',(-70.4386525839521,-13.8849240362763,
0.));
#82691=CARTESIAN_POINT('Ctrl Pts',(-70.4589887207073,-13.8970097806953,
0.));
#82692=CARTESIAN_POINT('Ctrl Pts',(-70.4793500033124,-13.9091375740088,
0.));
#82693=CARTESIAN_POINT('Ctrl Pts',(-70.4997362936673,-13.9213074069852,
0.));
#82694=CARTESIAN_POINT('Ctrl Pts',(-70.520147454271,-13.9335192703388,0.));
#82695=CARTESIAN_POINT('Ctrl Pts',(-70.5405833482112,-13.9457731547215,
0.));
#82696=CARTESIAN_POINT('Ctrl Pts',(-70.5610438391612,-13.958069050726,0.));
#82697=CARTESIAN_POINT('Ctrl Pts',(-70.5815287913784,-13.9704069488917,
0.));
#82698=CARTESIAN_POINT('Ctrl Pts',(-70.6020380697004,-13.9827868397057,
0.));
#82699=CARTESIAN_POINT('Ctrl Pts',(-70.6225715395394,-13.9952087136018,
0.));
#82700=CARTESIAN_POINT('Ctrl Pts',(-70.6431290668745,-14.0076725609536,
0.));
#82701=CARTESIAN_POINT('Ctrl Pts',(-70.6637105182484,-14.0201783720769,
0.));
#82702=CARTESIAN_POINT('Ctrl Pts',(-70.6843157607668,-14.0327261372362,
0.));
#82703=CARTESIAN_POINT('Ctrl Pts',(-70.7049446620928,-14.0453158466451,
0.));
#82704=CARTESIAN_POINT('Ctrl Pts',(-70.7255970904436,-14.0579474904657,
0.));
#82705=CARTESIAN_POINT('Ctrl Pts',(-70.7462729145807,-14.0706210588016,
0.));
#82706=CARTESIAN_POINT('Ctrl Pts',(-70.7669720038077,-14.0833365416996,
0.));
#82707=CARTESIAN_POINT('Ctrl Pts',(-70.7876942279697,-14.0960939291569,
0.));
#82708=CARTESIAN_POINT('Ctrl Pts',(-70.8084394574493,-14.1088932111214,
0.));
#82709=CARTESIAN_POINT('Ctrl Pts',(-70.8292075631621,-14.1217343774913,
0.));
#82710=CARTESIAN_POINT('Ctrl Pts',(-70.8499984165489,-14.1346174181078,
0.));
#82711=CARTESIAN_POINT('Ctrl Pts',(-70.8708118895715,-14.1475423227568,
0.));
#82712=CARTESIAN_POINT('Ctrl Pts',(-70.8916478547132,-14.1605090811754,
0.));
#82713=CARTESIAN_POINT('Ctrl Pts',(-70.9125061849745,-14.1735176830533,
0.));
#82714=CARTESIAN_POINT('Ctrl Pts',(-70.9333867538704,-14.186568118032,0.));
#82715=CARTESIAN_POINT('Ctrl Pts',(-70.9542894354216,-14.1996603756982,
0.));
#82716=CARTESIAN_POINT('Ctrl Pts',(-70.9752141041518,-14.2127944455838,
0.));
#82717=CARTESIAN_POINT('Ctrl Pts',(-70.9961606350861,-14.2259703171737,
0.));
#82718=CARTESIAN_POINT('Ctrl Pts',(-71.0171289037488,-14.2391879799061,
0.));
#82719=CARTESIAN_POINT('Ctrl Pts',(-71.0381187861588,-14.2524474231732,
0.));
#82720=CARTESIAN_POINT('Ctrl Pts',(-71.0591301588231,-14.2657486363139,
0.));
#82721=CARTESIAN_POINT('Ctrl Pts',(-71.0801628987332,-14.2790916086133,
0.));
#82722=CARTESIAN_POINT('Ctrl Pts',(-71.1012168833643,-14.2924763293105,
0.));
#82723=CARTESIAN_POINT('Ctrl Pts',(-71.1222919906727,-14.3059027875994,
0.));
#82724=CARTESIAN_POINT('Ctrl Pts',(-71.1433880990929,-14.3193709726294,
0.));
#82725=CARTESIAN_POINT('Ctrl Pts',(-71.1645050875308,-14.3328808734989,
0.));
#82726=CARTESIAN_POINT('Ctrl Pts',(-71.1856428353593,-14.3464324792533,
0.));
#82727=CARTESIAN_POINT('Ctrl Pts',(-71.2068012224174,-14.3600257788924,
0.));
#82728=CARTESIAN_POINT('Ctrl Pts',(-71.2279801290084,-14.3736607613722,
0.));
#82729=CARTESIAN_POINT('Ctrl Pts',(-71.2491794358958,-14.3873374156056,
0.));
#82730=CARTESIAN_POINT('Ctrl Pts',(-71.2703990242988,-14.401055730457,0.));
#82731=CARTESIAN_POINT('Ctrl Pts',(-71.2916387758861,-14.4148156947384,
0.));
#82732=CARTESIAN_POINT('Ctrl Pts',(-71.312898572777,-14.4286172972166,0.));
#82733=CARTESIAN_POINT('Ctrl Pts',(-71.3341782975386,-14.4424605266165,
0.));
#82734=CARTESIAN_POINT('Ctrl Pts',(-71.3554778331835,-14.4563453716204,
0.));
#82735=CARTESIAN_POINT('Ctrl Pts',(-71.376797063165,-14.4702718208651,0.));
#82736=CARTESIAN_POINT('Ctrl Pts',(-71.3981358713723,-14.4842398629355,
0.));
#82737=CARTESIAN_POINT('Ctrl Pts',(-71.4194941421292,-14.4982494863718,
0.));
#82738=CARTESIAN_POINT('Ctrl Pts',(-71.4408717601923,-14.5123006796728,
0.));
#82739=CARTESIAN_POINT('Ctrl Pts',(-71.4622686107475,-14.5263934312969,
0.));
#82740=CARTESIAN_POINT('Ctrl Pts',(-71.4836845794048,-14.540527729659,0.));
#82741=CARTESIAN_POINT('Ctrl Pts',(-71.5051195521909,-14.5547035631233,
0.));
#82742=CARTESIAN_POINT('Ctrl Pts',(-71.5265734155498,-14.5689209200091,
0.));
#82743=CARTESIAN_POINT('Ctrl Pts',(-71.5480460563447,-14.5831797885952,
0.));
#82744=CARTESIAN_POINT('Ctrl Pts',(-71.5695373618562,-14.597480157121,0.));
#82745=CARTESIAN_POINT('Ctrl Pts',(-71.5910472197813,-14.6118220137849,
0.));
#82746=CARTESIAN_POINT('Ctrl Pts',(-71.612575518229,-14.626205346737,0.));
#82747=CARTESIAN_POINT('Ctrl Pts',(-71.6341221457168,-14.6406301440814,
0.));
#82748=CARTESIAN_POINT('Ctrl Pts',(-71.6556869911662,-14.6550963938829,
0.));
#82749=CARTESIAN_POINT('Ctrl Pts',(-71.6772699438963,-14.6696040841678,
0.));
#82750=CARTESIAN_POINT('Ctrl Pts',(-71.6988708936172,-14.6841532029232,
0.));
#82751=CARTESIAN_POINT('Ctrl Pts',(-71.7204897304194,-14.69874373809,0.));
#82752=CARTESIAN_POINT('Ctrl Pts',(-71.7421263447719,-14.7133756775625,
0.));
#82753=CARTESIAN_POINT('Ctrl Pts',(-71.7637806275328,-14.7280490091957,
0.));
#82754=CARTESIAN_POINT('Ctrl Pts',(-71.7854524699569,-14.7427637208072,
0.));
#82755=CARTESIAN_POINT('Ctrl Pts',(-71.8071417637017,-14.7575198001776,
0.));
#82756=CARTESIAN_POINT('Ctrl Pts',(-71.8288484008333,-14.7723172350451,
0.));
#82757=CARTESIAN_POINT('Ctrl Pts',(-71.8505722738272,-14.7871560131016,
0.));
#82758=CARTESIAN_POINT('Ctrl Pts',(-71.8723132755446,-14.8020361219998,
0.));
#82759=CARTESIAN_POINT('Ctrl Pts',(-71.8940712992109,-14.8169575493557,
0.));
#82760=CARTESIAN_POINT('Ctrl Pts',(-71.9158462383914,-14.8319202827482,
0.));
#82761=CARTESIAN_POINT('Ctrl Pts',(-71.9376379869678,-14.8469243097162,
0.));
#82762=CARTESIAN_POINT('Ctrl Pts',(-71.9594464391078,-14.8619696177506,
0.));
#82763=CARTESIAN_POINT('Ctrl Pts',(-71.9812714893102,-14.8770561943014,
0.));
#82764=CARTESIAN_POINT('Ctrl Pts',(-72.0031130324529,-14.8921840267832,
0.));
#82765=CARTESIAN_POINT('Ctrl Pts',(-72.0249709638422,-14.9073531025764,
0.));
#82766=CARTESIAN_POINT('Ctrl Pts',(-72.0468451792505,-14.9225634090268,
0.));
#82767=CARTESIAN_POINT('Ctrl Pts',(-72.0687355749806,-14.9378149334388,
0.));
#82768=CARTESIAN_POINT('Ctrl Pts',(-72.0906420478076,-14.9531076630767,
0.));
#82769=CARTESIAN_POINT('Ctrl Pts',(-72.112564494854,-14.9684415851698,0.));
#82770=CARTESIAN_POINT('Ctrl Pts',(-72.1345028134777,-14.9838166869107,
0.));
#82771=CARTESIAN_POINT('Ctrl Pts',(-72.1564569011669,-14.9992329554537,
0.));
#82772=CARTESIAN_POINT('Ctrl Pts',(-72.1784266553953,-15.0146903779062,
0.));
#82773=CARTESIAN_POINT('Ctrl Pts',(-72.2004119736115,-15.0301889413257,
0.));
#82774=CARTESIAN_POINT('Ctrl Pts',(-72.2224127535415,-15.0457286327331,
0.));
#82775=CARTESIAN_POINT('Ctrl Pts',(-72.2444288934262,-15.0613094391189,
0.));
#82776=CARTESIAN_POINT('Ctrl Pts',(-72.2664602922852,-15.0769313474476,
0.));
#82777=CARTESIAN_POINT('Ctrl Pts',(-72.2885068501628,-15.0925943446589,
0.));
#82778=CARTESIAN_POINT('Ctrl Pts',(-72.3105684683944,-15.1082984176649,
0.));
#82779=CARTESIAN_POINT('Ctrl Pts',(-72.3326450490177,-15.124043553347,0.));
#82780=CARTESIAN_POINT('Ctrl Pts',(-72.3547364941969,-15.1398297385506,
0.));
#82781=CARTESIAN_POINT('Ctrl Pts',(-72.376842705589,-15.1556569600744,0.));
#82782=CARTESIAN_POINT('Ctrl Pts',(-72.3989635838492,-15.1715252046606,
0.));
#82783=CARTESIAN_POINT('Ctrl Pts',(-72.421099027786,-15.1874344589725,0.));
#82784=CARTESIAN_POINT('Ctrl Pts',(-72.4432489350471,-15.2033847096091,
0.));
#82785=CARTESIAN_POINT('Ctrl Pts',(-72.4654132036428,-15.2193759431372,
0.));
#82786=CARTESIAN_POINT('Ctrl Pts',(-72.4875917332761,-15.235408146116,0.));
#82787=CARTESIAN_POINT('Ctrl Pts',(-72.5097844266075,-15.2514813051172,
0.));
#82788=CARTESIAN_POINT('Ctrl Pts',(-72.5319911908917,-15.2675954067479,
0.));
#82789=CARTESIAN_POINT('Ctrl Pts',(-72.5542119383642,-15.2837504376535,
0.));
#82790=CARTESIAN_POINT('Ctrl Pts',(-72.5732713370619,-15.297633502478,0.));
#82791=CARTESIAN_POINT('Ctrl Pts',(-72.5878912620441,-15.308299460354,0.));
#82792=CARTESIAN_POINT('Ctrl Pts',(-72.5980655789638,-15.3157301930684,
0.));
#82793=CARTESIAN_POINT('Ctrl Pts',(-72.6037902604925,-15.3199137230132,
0.));
#82794=CARTESIAN_POINT('Ctrl Pts',(-72.6050633494356,-15.3208442077192,
0.));
#82795=CARTESIAN_POINT('',(-68.7831490561748,-12.9953224629497,12.));
#82796=CARTESIAN_POINT('',(-68.7831490561748,-12.9953224629497,0.));
#82797=CARTESIAN_POINT('Ctrl Pts',(-72.6050633494356,-15.3208442077192,
12.));
#82798=CARTESIAN_POINT('Ctrl Pts',(-72.6037902604925,-15.3199137230132,
12.));
#82799=CARTESIAN_POINT('Ctrl Pts',(-72.5980655789638,-15.3157301930684,
12.));
#82800=CARTESIAN_POINT('Ctrl Pts',(-72.5878912620441,-15.308299460354,12.));
#82801=CARTESIAN_POINT('Ctrl Pts',(-72.5732713370619,-15.297633502478,12.));
#82802=CARTESIAN_POINT('Ctrl Pts',(-72.5542119383642,-15.2837504376535,
12.));
#82803=CARTESIAN_POINT('Ctrl Pts',(-72.5319911908917,-15.2675954067479,
12.));
#82804=CARTESIAN_POINT('Ctrl Pts',(-72.5097844266075,-15.2514813051172,
12.));
#82805=CARTESIAN_POINT('Ctrl Pts',(-72.4875917332761,-15.235408146116,12.));
#82806=CARTESIAN_POINT('Ctrl Pts',(-72.4654132036428,-15.2193759431372,
12.));
#82807=CARTESIAN_POINT('Ctrl Pts',(-72.4432489350471,-15.2033847096091,
12.));
#82808=CARTESIAN_POINT('Ctrl Pts',(-72.421099027786,-15.1874344589725,12.));
#82809=CARTESIAN_POINT('Ctrl Pts',(-72.3989635838492,-15.1715252046606,
12.));
#82810=CARTESIAN_POINT('Ctrl Pts',(-72.376842705589,-15.1556569600744,12.));
#82811=CARTESIAN_POINT('Ctrl Pts',(-72.3547364941969,-15.1398297385506,
12.));
#82812=CARTESIAN_POINT('Ctrl Pts',(-72.3326450490177,-15.124043553347,12.));
#82813=CARTESIAN_POINT('Ctrl Pts',(-72.3105684683944,-15.1082984176649,
12.));
#82814=CARTESIAN_POINT('Ctrl Pts',(-72.2885068501628,-15.0925943446589,
12.));
#82815=CARTESIAN_POINT('Ctrl Pts',(-72.2664602922852,-15.0769313474476,
12.));
#82816=CARTESIAN_POINT('Ctrl Pts',(-72.2444288934262,-15.0613094391189,
12.));
#82817=CARTESIAN_POINT('Ctrl Pts',(-72.2224127535415,-15.0457286327331,
12.));
#82818=CARTESIAN_POINT('Ctrl Pts',(-72.2004119736115,-15.0301889413257,
12.));
#82819=CARTESIAN_POINT('Ctrl Pts',(-72.1784266553953,-15.0146903779062,
12.));
#82820=CARTESIAN_POINT('Ctrl Pts',(-72.1564569011669,-14.9992329554537,
12.));
#82821=CARTESIAN_POINT('Ctrl Pts',(-72.1345028134777,-14.9838166869107,
12.));
#82822=CARTESIAN_POINT('Ctrl Pts',(-72.112564494854,-14.9684415851698,12.));
#82823=CARTESIAN_POINT('Ctrl Pts',(-72.0906420478076,-14.9531076630767,
12.));
#82824=CARTESIAN_POINT('Ctrl Pts',(-72.0687355749806,-14.9378149334388,
12.));
#82825=CARTESIAN_POINT('Ctrl Pts',(-72.0468451792505,-14.9225634090268,
12.));
#82826=CARTESIAN_POINT('Ctrl Pts',(-72.0249709638422,-14.9073531025764,
12.));
#82827=CARTESIAN_POINT('Ctrl Pts',(-72.0031130324529,-14.8921840267832,
12.));
#82828=CARTESIAN_POINT('Ctrl Pts',(-71.9812714893102,-14.8770561943014,
12.));
#82829=CARTESIAN_POINT('Ctrl Pts',(-71.9594464391078,-14.8619696177506,
12.));
#82830=CARTESIAN_POINT('Ctrl Pts',(-71.9376379869678,-14.8469243097162,
12.));
#82831=CARTESIAN_POINT('Ctrl Pts',(-71.9158462383914,-14.8319202827482,
12.));
#82832=CARTESIAN_POINT('Ctrl Pts',(-71.8940712992109,-14.8169575493557,
12.));
#82833=CARTESIAN_POINT('Ctrl Pts',(-71.8723132755446,-14.8020361219998,
12.));
#82834=CARTESIAN_POINT('Ctrl Pts',(-71.8505722738272,-14.7871560131016,
12.));
#82835=CARTESIAN_POINT('Ctrl Pts',(-71.8288484008333,-14.7723172350451,
12.));
#82836=CARTESIAN_POINT('Ctrl Pts',(-71.8071417637017,-14.7575198001776,
12.));
#82837=CARTESIAN_POINT('Ctrl Pts',(-71.7854524699569,-14.7427637208072,
12.));
#82838=CARTESIAN_POINT('Ctrl Pts',(-71.7637806275328,-14.7280490091957,
12.));
#82839=CARTESIAN_POINT('Ctrl Pts',(-71.7421263447719,-14.7133756775625,
12.));
#82840=CARTESIAN_POINT('Ctrl Pts',(-71.7204897304194,-14.69874373809,12.));
#82841=CARTESIAN_POINT('Ctrl Pts',(-71.6988708936172,-14.6841532029232,
12.));
#82842=CARTESIAN_POINT('Ctrl Pts',(-71.6772699438963,-14.6696040841678,
12.));
#82843=CARTESIAN_POINT('Ctrl Pts',(-71.6556869911662,-14.6550963938829,
12.));
#82844=CARTESIAN_POINT('Ctrl Pts',(-71.6341221457168,-14.6406301440814,
12.));
#82845=CARTESIAN_POINT('Ctrl Pts',(-71.612575518229,-14.626205346737,12.));
#82846=CARTESIAN_POINT('Ctrl Pts',(-71.5910472197813,-14.6118220137849,
12.));
#82847=CARTESIAN_POINT('Ctrl Pts',(-71.5695373618562,-14.597480157121,12.));
#82848=CARTESIAN_POINT('Ctrl Pts',(-71.5480460563447,-14.5831797885952,
12.));
#82849=CARTESIAN_POINT('Ctrl Pts',(-71.5265734155498,-14.5689209200091,
12.));
#82850=CARTESIAN_POINT('Ctrl Pts',(-71.5051195521909,-14.5547035631233,
12.));
#82851=CARTESIAN_POINT('Ctrl Pts',(-71.4836845794048,-14.540527729659,12.));
#82852=CARTESIAN_POINT('Ctrl Pts',(-71.4622686107475,-14.5263934312969,
12.));
#82853=CARTESIAN_POINT('Ctrl Pts',(-71.4408717601923,-14.5123006796728,
12.));
#82854=CARTESIAN_POINT('Ctrl Pts',(-71.4194941421292,-14.4982494863718,
12.));
#82855=CARTESIAN_POINT('Ctrl Pts',(-71.3981358713723,-14.4842398629355,
12.));
#82856=CARTESIAN_POINT('Ctrl Pts',(-71.376797063165,-14.4702718208651,12.));
#82857=CARTESIAN_POINT('Ctrl Pts',(-71.3554778331835,-14.4563453716204,
12.));
#82858=CARTESIAN_POINT('Ctrl Pts',(-71.3341782975386,-14.4424605266165,
12.));
#82859=CARTESIAN_POINT('Ctrl Pts',(-71.312898572777,-14.4286172972166,12.));
#82860=CARTESIAN_POINT('Ctrl Pts',(-71.2916387758861,-14.4148156947384,
12.));
#82861=CARTESIAN_POINT('Ctrl Pts',(-71.2703990242988,-14.401055730457,12.));
#82862=CARTESIAN_POINT('Ctrl Pts',(-71.2491794358958,-14.3873374156056,
12.));
#82863=CARTESIAN_POINT('Ctrl Pts',(-71.2279801290084,-14.3736607613722,
12.));
#82864=CARTESIAN_POINT('Ctrl Pts',(-71.2068012224174,-14.3600257788924,
12.));
#82865=CARTESIAN_POINT('Ctrl Pts',(-71.1856428353593,-14.3464324792533,
12.));
#82866=CARTESIAN_POINT('Ctrl Pts',(-71.1645050875308,-14.3328808734989,
12.));
#82867=CARTESIAN_POINT('Ctrl Pts',(-71.1433880990929,-14.3193709726294,
12.));
#82868=CARTESIAN_POINT('Ctrl Pts',(-71.1222919906727,-14.3059027875994,
12.));
#82869=CARTESIAN_POINT('Ctrl Pts',(-71.1012168833643,-14.2924763293105,
12.));
#82870=CARTESIAN_POINT('Ctrl Pts',(-71.0801628987332,-14.2790916086133,
12.));
#82871=CARTESIAN_POINT('Ctrl Pts',(-71.0591301588231,-14.2657486363139,
12.));
#82872=CARTESIAN_POINT('Ctrl Pts',(-71.0381187861588,-14.2524474231732,
12.));
#82873=CARTESIAN_POINT('Ctrl Pts',(-71.0171289037488,-14.2391879799061,
12.));
#82874=CARTESIAN_POINT('Ctrl Pts',(-70.9961606350861,-14.2259703171737,
12.));
#82875=CARTESIAN_POINT('Ctrl Pts',(-70.9752141041518,-14.2127944455838,
12.));
#82876=CARTESIAN_POINT('Ctrl Pts',(-70.9542894354216,-14.1996603756982,
12.));
#82877=CARTESIAN_POINT('Ctrl Pts',(-70.9333867538704,-14.186568118032,12.));
#82878=CARTESIAN_POINT('Ctrl Pts',(-70.9125061849745,-14.1735176830533,
12.));
#82879=CARTESIAN_POINT('Ctrl Pts',(-70.8916478547132,-14.1605090811754,
12.));
#82880=CARTESIAN_POINT('Ctrl Pts',(-70.8708118895715,-14.1475423227568,
12.));
#82881=CARTESIAN_POINT('Ctrl Pts',(-70.8499984165489,-14.1346174181078,
12.));
#82882=CARTESIAN_POINT('Ctrl Pts',(-70.8292075631621,-14.1217343774913,
12.));
#82883=CARTESIAN_POINT('Ctrl Pts',(-70.8084394574493,-14.1088932111214,
12.));
#82884=CARTESIAN_POINT('Ctrl Pts',(-70.7876942279697,-14.0960939291569,
12.));
#82885=CARTESIAN_POINT('Ctrl Pts',(-70.7669720038077,-14.0833365416996,
12.));
#82886=CARTESIAN_POINT('Ctrl Pts',(-70.7462729145807,-14.0706210588016,
12.));
#82887=CARTESIAN_POINT('Ctrl Pts',(-70.7255970904436,-14.0579474904657,
12.));
#82888=CARTESIAN_POINT('Ctrl Pts',(-70.7049446620928,-14.0453158466451,
12.));
#82889=CARTESIAN_POINT('Ctrl Pts',(-70.6843157607668,-14.0327261372362,
12.));
#82890=CARTESIAN_POINT('Ctrl Pts',(-70.6637105182484,-14.0201783720769,
12.));
#82891=CARTESIAN_POINT('Ctrl Pts',(-70.6431290668745,-14.0076725609536,
12.));
#82892=CARTESIAN_POINT('Ctrl Pts',(-70.6225715395394,-13.9952087136018,
12.));
#82893=CARTESIAN_POINT('Ctrl Pts',(-70.6020380697004,-13.9827868397057,
12.));
#82894=CARTESIAN_POINT('Ctrl Pts',(-70.5815287913784,-13.9704069488917,
12.));
#82895=CARTESIAN_POINT('Ctrl Pts',(-70.5610438391612,-13.958069050726,12.));
#82896=CARTESIAN_POINT('Ctrl Pts',(-70.5405833482112,-13.9457731547215,
12.));
#82897=CARTESIAN_POINT('Ctrl Pts',(-70.520147454271,-13.9335192703388,12.));
#82898=CARTESIAN_POINT('Ctrl Pts',(-70.4997362936673,-13.9213074069852,
12.));
#82899=CARTESIAN_POINT('Ctrl Pts',(-70.4793500033124,-13.9091375740088,
12.));
#82900=CARTESIAN_POINT('Ctrl Pts',(-70.4589887207073,-13.8970097806953,
12.));
#82901=CARTESIAN_POINT('Ctrl Pts',(-70.4386525839521,-13.8849240362763,
12.));
#82902=CARTESIAN_POINT('Ctrl Pts',(-70.4183417317499,-13.8728803499287,
12.));
#82903=CARTESIAN_POINT('Ctrl Pts',(-70.3980563034133,-13.8608787307751,
12.));
#82904=CARTESIAN_POINT('Ctrl Pts',(-70.3777964388632,-13.8489191878767,
12.));
#82905=CARTESIAN_POINT('Ctrl Pts',(-70.3575622786335,-13.8370017302309,
12.));
#82906=CARTESIAN_POINT('Ctrl Pts',(-70.3373539638809,-13.825126366779,12.));
#82907=CARTESIAN_POINT('Ctrl Pts',(-70.3171716363897,-13.8132931064063,
12.));
#82908=CARTESIAN_POINT('Ctrl Pts',(-70.2970154385774,-13.8015019579414,
12.));
#82909=CARTESIAN_POINT('Ctrl Pts',(-70.2768855134947,-13.7897529301491,
12.));
#82910=CARTESIAN_POINT('Ctrl Pts',(-70.2567820048303,-13.7780460317294,
12.));
#82911=CARTESIAN_POINT('Ctrl Pts',(-70.2367050569215,-13.7663812713243,
12.));
#82912=CARTESIAN_POINT('Ctrl Pts',(-70.2166548147604,-13.754758657518,12.));
#82913=CARTESIAN_POINT('Ctrl Pts',(-70.1966314239995,-13.7431781988364,
12.));
#82914=CARTESIAN_POINT('Ctrl Pts',(-70.1766350309518,-13.7316399037392,
12.));
#82915=CARTESIAN_POINT('Ctrl Pts',(-70.156665782595,-13.7201437806199,12.));
#82916=CARTESIAN_POINT('Ctrl Pts',(-70.1367238265825,-13.7086898378121,
12.));
#82917=CARTESIAN_POINT('Ctrl Pts',(-70.1168093112486,-13.6972780835897,
12.));
#82918=CARTESIAN_POINT('Ctrl Pts',(-70.0969223856136,-13.6859085261653,
12.));
#82919=CARTESIAN_POINT('Ctrl Pts',(-70.0770631993856,-13.6745811736829,
12.));
#82920=CARTESIAN_POINT('Ctrl Pts',(-70.0572319029676,-13.6632960342196,
12.));
#82921=CARTESIAN_POINT('Ctrl Pts',(-70.0374286474677,-13.6520531157907,
12.));
#82922=CARTESIAN_POINT('Ctrl Pts',(-70.0176535847049,-13.6408524263496,
12.));
#82923=CARTESIAN_POINT('Ctrl Pts',(-69.9979068672153,-13.6296939737865,
12.));
#82924=CARTESIAN_POINT('Ctrl Pts',(-69.9781886482527,-13.6185777659198,
12.));
#82925=CARTESIAN_POINT('Ctrl Pts',(-69.9584990817974,-13.6075038104998,
12.));
#82926=CARTESIAN_POINT('Ctrl Pts',(-69.9388383225648,-13.5964721152135,
12.));
#82927=CARTESIAN_POINT('Ctrl Pts',(-69.9192065260108,-13.5854826876834,
12.));
#82928=CARTESIAN_POINT('Ctrl Pts',(-69.8996038483361,-13.5745355354656,
12.));
#82929=CARTESIAN_POINT('Ctrl Pts',(-69.8800304464882,-13.5636306660421,
12.));
#82930=CARTESIAN_POINT('Ctrl Pts',(-69.8604864781706,-13.5527680868255,
12.));
#82931=CARTESIAN_POINT('Ctrl Pts',(-69.840972101856,-13.5419478051625,12.));
#82932=CARTESIAN_POINT('Ctrl Pts',(-69.8214874767944,-13.5311698283339,
12.));
#82933=CARTESIAN_POINT('Ctrl Pts',(-69.8020327630205,-13.5204341635507,
12.));
#82934=CARTESIAN_POINT('Ctrl Pts',(-69.7826081213576,-13.5097408179479,
12.));
#82935=CARTESIAN_POINT('Ctrl Pts',(-69.7632137134249,-13.4990897985904,
12.));
#82936=CARTESIAN_POINT('Ctrl Pts',(-69.7438497016406,-13.4884811124748,
12.));
#82937=CARTESIAN_POINT('Ctrl Pts',(-69.724516249225,-13.4779147665285,12.));
#82938=CARTESIAN_POINT('Ctrl Pts',(-69.7052135201998,-13.4673907676044,
12.));
#82939=CARTESIAN_POINT('Ctrl Pts',(-69.6859416793886,-13.456909122476,12.));
#82940=CARTESIAN_POINT('Ctrl Pts',(-69.666700892444,-13.4464698378453,12.));
#82941=CARTESIAN_POINT('Ctrl Pts',(-69.6474913258675,-13.4360729203442,
12.));
#82942=CARTESIAN_POINT('Ctrl Pts',(-69.6283131470273,-13.4257183765341,
12.));
#82943=CARTESIAN_POINT('Ctrl Pts',(-69.6091665241765,-13.4154062129002,
12.));
#82944=CARTESIAN_POINT('Ctrl Pts',(-69.5900516264553,-13.40513643585,12.));
#82945=CARTESIAN_POINT('Ctrl Pts',(-69.5709686238724,-13.3949090517177,
12.));
#82946=CARTESIAN_POINT('Ctrl Pts',(-69.5519176872862,-13.3847240667627,
12.));
#82947=CARTESIAN_POINT('Ctrl Pts',(-69.5328989883885,-13.3745814871664,
12.));
#82948=CARTESIAN_POINT('Ctrl Pts',(-69.5139126996675,-13.3644813190219,
12.));
#82949=CARTESIAN_POINT('Ctrl Pts',(-69.4949589944606,-13.3544235683393,
12.));
#82950=CARTESIAN_POINT('Ctrl Pts',(-69.4760380470365,-13.3444082410543,
12.));
#82951=CARTESIAN_POINT('Ctrl Pts',(-69.4571500326673,-13.3344353430313,
12.));
#82952=CARTESIAN_POINT('Ctrl Pts',(-69.4382951276998,-13.3245048800643,
12.));
#82953=CARTESIAN_POINT('Ctrl Pts',(-69.4194735096265,-13.3146168578743,
12.));
#82954=CARTESIAN_POINT('Ctrl Pts',(-69.4006853569511,-13.3047712821051,
12.));
#82955=CARTESIAN_POINT('Ctrl Pts',(-69.3819308490422,-13.2949681583167,
12.));
#82956=CARTESIAN_POINT('Ctrl Pts',(-69.3632101660066,-13.2852074919765,
12.));
#82957=CARTESIAN_POINT('Ctrl Pts',(-69.3445234885065,-13.2754892884433,
12.));
#82958=CARTESIAN_POINT('Ctrl Pts',(-69.3258709977382,-13.265813552961,12.));
#82959=CARTESIAN_POINT('Ctrl Pts',(-69.3072528758518,-13.2561802906896,
12.));
#82960=CARTESIAN_POINT('Ctrl Pts',(-69.2886693063182,-13.2465895067262,
12.));
#82961=CARTESIAN_POINT('Ctrl Pts',(-69.2701204742449,-13.237041206122,12.));
#82962=CARTESIAN_POINT('Ctrl Pts',(-69.2516065668844,-13.2275353939051,
12.));
#82963=CARTESIAN_POINT('Ctrl Pts',(-69.2331277732861,-13.2180720750594,
12.));
#82964=CARTESIAN_POINT('Ctrl Pts',(-69.2146842833537,-13.2086512544735,
12.));
#82965=CARTESIAN_POINT('Ctrl Pts',(-69.1962762870527,-13.1992729368928,
12.));
#82966=CARTESIAN_POINT('Ctrl Pts',(-69.1779039735996,-13.1899371268683,
12.));
#82967=CARTESIAN_POINT('Ctrl Pts',(-69.1595675305245,-13.1806438286934,
12.));
#82968=CARTESIAN_POINT('Ctrl Pts',(-69.1412671454564,-13.1713930465132,
12.));
#82969=CARTESIAN_POINT('Ctrl Pts',(-69.1230030082573,-13.1621847844528,
12.));
#82970=CARTESIAN_POINT('Ctrl Pts',(-69.1047753127643,-13.1530190467183,
12.));
#82971=CARTESIAN_POINT('Ctrl Pts',(-69.0865842593102,-13.1438958377404,
12.));
#82972=CARTESIAN_POINT('Ctrl Pts',(-69.0684300549477,-13.1348151621834,
12.));
#82973=CARTESIAN_POINT('Ctrl Pts',(-69.0503129081817,-13.1257770246385,
12.));
#82974=CARTESIAN_POINT('Ctrl Pts',(-69.0322330243348,-13.1167814293497,
12.));
#82975=CARTESIAN_POINT('Ctrl Pts',(-69.0141906015113,-13.1078283799722,
12.));
#82976=CARTESIAN_POINT('Ctrl Pts',(-68.9961858241519,-13.0989178791833,
12.));
#82977=CARTESIAN_POINT('Ctrl Pts',(-68.9782188692581,-13.090049929053,12.));
#82978=CARTESIAN_POINT('Ctrl Pts',(-68.9602899187573,-13.0812245317807,
12.));
#82979=CARTESIAN_POINT('Ctrl Pts',(-68.9423991694492,-13.072441690283,12.));
#82980=CARTESIAN_POINT('Ctrl Pts',(-68.9245468449945,-13.0637014089029,
12.));
#82981=CARTESIAN_POINT('Ctrl Pts',(-68.9067332040985,-13.0550036938813,
12.));
#82982=CARTESIAN_POINT('Ctrl Pts',(-68.8889585151585,-13.0463485518206,
12.));
#82983=CARTESIAN_POINT('Ctrl Pts',(-68.8712230321906,-13.0377359881875,
12.));
#82984=CARTESIAN_POINT('Ctrl Pts',(-68.8535269726793,-13.0291660060107,
12.));
#82985=CARTESIAN_POINT('Ctrl Pts',(-68.8358704887468,-13.0206386039691,
12.));
#82986=CARTESIAN_POINT('Ctrl Pts',(-68.8182536653656,-13.0121537768945,
12.));
#82987=CARTESIAN_POINT('Ctrl Pts',(-68.804191966902,-13.0053999700875,12.));
#82988=CARTESIAN_POINT('Ctrl Pts',(-68.7936635625545,-13.0003537683054,
12.));
#82989=CARTESIAN_POINT('Ctrl Pts',(-68.7866525680193,-12.9969981460277,
12.));
#82990=CARTESIAN_POINT('Ctrl Pts',(-68.7831490561748,-12.9953224629497,
12.));
#82991=CARTESIAN_POINT('Ctrl Pts',(-72.277402839391,-16.7988252568749,0.));
#82992=CARTESIAN_POINT('Ctrl Pts',(-72.277402839391,-16.7988252568749,4.));
#82993=CARTESIAN_POINT('Ctrl Pts',(-72.2774028393911,-16.7988252568749,
8.));
#82994=CARTESIAN_POINT('Ctrl Pts',(-72.2774028393911,-16.7988252568749,
12.));
#82995=CARTESIAN_POINT('Ctrl Pts',(-72.3852065198821,-16.7775526720895,
0.));
#82996=CARTESIAN_POINT('Ctrl Pts',(-72.3852065198821,-16.7775526720895,
4.));
#82997=CARTESIAN_POINT('Ctrl Pts',(-72.3852065198822,-16.7775526720895,
8.00000000000001));
#82998=CARTESIAN_POINT('Ctrl Pts',(-72.3852065198822,-16.7775526720895,
12.));
#82999=CARTESIAN_POINT('Ctrl Pts',(-72.5605133546287,-16.675864902556,0.));
#83000=CARTESIAN_POINT('Ctrl Pts',(-72.5605133546287,-16.675864902556,4.));
#83001=CARTESIAN_POINT('Ctrl Pts',(-72.5605133546287,-16.675864902556,7.99999999999999));
#83002=CARTESIAN_POINT('Ctrl Pts',(-72.5605133546287,-16.675864902556,12.));
#83003=CARTESIAN_POINT('Ctrl Pts',(-72.650150535446,-16.4988611391809,0.));
#83004=CARTESIAN_POINT('Ctrl Pts',(-72.650150535446,-16.4988611391809,4.));
#83005=CARTESIAN_POINT('Ctrl Pts',(-72.6501505354461,-16.4988611391808,
8.00000000000001));
#83006=CARTESIAN_POINT('Ctrl Pts',(-72.6501505354461,-16.4988611391808,
12.));
#83007=CARTESIAN_POINT('Ctrl Pts',(-72.6683126419583,-16.4184755008062,
0.));
#83008=CARTESIAN_POINT('Ctrl Pts',(-72.6683126419583,-16.4184755008062,
4.));
#83009=CARTESIAN_POINT('Ctrl Pts',(-72.6683126419584,-16.4184755008061,
8.));
#83010=CARTESIAN_POINT('Ctrl Pts',(-72.6683126419584,-16.4184755008061,
12.));
#83011=CARTESIAN_POINT('',(-72.277402839391,-16.7988252568749,0.));
#83012=CARTESIAN_POINT('',(-72.6683126419585,-16.4184755008062,0.));
#83013=CARTESIAN_POINT('Ctrl Pts',(-72.277402839391,-16.7988252568749,2.77555756156289E-16));
#83014=CARTESIAN_POINT('Ctrl Pts',(-72.3852065198821,-16.7775526720895,
2.77555756156289E-16));
#83015=CARTESIAN_POINT('Ctrl Pts',(-72.485381854023,-16.7194453752132,2.77555756156289E-16));
#83016=CARTESIAN_POINT('Ctrl Pts',(-72.5575834236156,-16.636745100756,2.77555756156289E-16));
#83017=CARTESIAN_POINT('Ctrl Pts',(-72.61173460081,-16.574719894913,2.77555756156289E-16));
#83018=CARTESIAN_POINT('Ctrl Pts',(-72.650150535446,-16.4988611391809,2.77555756156289E-16));
#83019=CARTESIAN_POINT('Ctrl Pts',(-72.6683126419583,-16.4184755008062,
2.77555756156289E-16));
#83020=CARTESIAN_POINT('',(-72.6683126419585,-16.4184755008062,12.));
#83021=CARTESIAN_POINT('Ctrl Pts',(-72.6683126419583,-16.4184755008062,
0.));
#83022=CARTESIAN_POINT('Ctrl Pts',(-72.6683126419583,-16.4184755008062,
4.));
#83023=CARTESIAN_POINT('Ctrl Pts',(-72.6683126419584,-16.4184755008061,
8.));
#83024=CARTESIAN_POINT('Ctrl Pts',(-72.6683126419584,-16.4184755008061,
12.));
#83025=CARTESIAN_POINT('',(-72.2774028393911,-16.7988252568749,12.));
#83026=CARTESIAN_POINT('Ctrl Pts',(-72.6683126419584,-16.4184755008061,
12.));
#83027=CARTESIAN_POINT('Ctrl Pts',(-72.6501505354461,-16.4988611391808,
12.));
#83028=CARTESIAN_POINT('Ctrl Pts',(-72.6117346008101,-16.574719894913,12.));
#83029=CARTESIAN_POINT('Ctrl Pts',(-72.5575834236157,-16.6367451007559,
12.));
#83030=CARTESIAN_POINT('Ctrl Pts',(-72.4853818540231,-16.7194453752132,
12.));
#83031=CARTESIAN_POINT('Ctrl Pts',(-72.3852065198822,-16.7775526720895,
12.));
#83032=CARTESIAN_POINT('Ctrl Pts',(-72.2774028393911,-16.7988252568749,
12.));
#83033=CARTESIAN_POINT('Ctrl Pts',(-72.2774028393911,-16.7988252568749,
12.));
#83034=CARTESIAN_POINT('Ctrl Pts',(-72.2774028393911,-16.7988252568749,
8.));
#83035=CARTESIAN_POINT('Ctrl Pts',(-72.277402839391,-16.7988252568749,4.));
#83036=CARTESIAN_POINT('Ctrl Pts',(-72.277402839391,-16.7988252568749,0.));
#83037=CARTESIAN_POINT('Origin',(-3.65936987487134E-10,-8.12279454723525E-11,
0.));
#83038=CARTESIAN_POINT('Origin',(-3.65936987487134E-10,-8.12279454723525E-11,
12.));
#83039=CARTESIAN_POINT('Origin',(-3.65936987487134E-10,-8.12279454723525E-11,
0.));
#83040=CARTESIAN_POINT('Ctrl Pts',(-73.9013264985861,-9.42570643237816,
0.));
#83041=CARTESIAN_POINT('Ctrl Pts',(-73.9013264985861,-9.42570643237816,
4.));
#83042=CARTESIAN_POINT('Ctrl Pts',(-73.9013264985861,-9.42570643237813,
8.));
#83043=CARTESIAN_POINT('Ctrl Pts',(-73.9013264985861,-9.42570643237813,
12.));
#83044=CARTESIAN_POINT('Ctrl Pts',(-73.9152287787081,-9.31670696907602,
0.));
#83045=CARTESIAN_POINT('Ctrl Pts',(-73.9152287787081,-9.31670696907602,
4.));
#83046=CARTESIAN_POINT('Ctrl Pts',(-73.9152287787081,-9.31670696907599,
8.00000000000001));
#83047=CARTESIAN_POINT('Ctrl Pts',(-73.9152287787081,-9.31670696907599,
12.));
#83048=CARTESIAN_POINT('Ctrl Pts',(-73.8741839722667,-9.11824194722532,
0.));
#83049=CARTESIAN_POINT('Ctrl Pts',(-73.8741839722667,-9.11824194722532,
4.));
#83050=CARTESIAN_POINT('Ctrl Pts',(-73.8741839722668,-9.1182419472253,7.99999999999999));
#83051=CARTESIAN_POINT('Ctrl Pts',(-73.8741839722668,-9.1182419472253,12.));
#83052=CARTESIAN_POINT('Ctrl Pts',(-73.7345987226919,-8.97724108745549,
0.));
#83053=CARTESIAN_POINT('Ctrl Pts',(-73.7345987226919,-8.97724108745549,
4.));
#83054=CARTESIAN_POINT('Ctrl Pts',(-73.7345987226919,-8.97724108745545,
8.00000000000001));
#83055=CARTESIAN_POINT('Ctrl Pts',(-73.7345987226919,-8.97724108745545,
12.));
#83056=CARTESIAN_POINT('Ctrl Pts',(-73.6640787197673,-8.93459554655806,
0.));
#83057=CARTESIAN_POINT('Ctrl Pts',(-73.6640787197673,-8.93459554655806,
4.));
#83058=CARTESIAN_POINT('Ctrl Pts',(-73.6640787197673,-8.93459554655801,
8.));
#83059=CARTESIAN_POINT('Ctrl Pts',(-73.6640787197673,-8.93459554655801,
12.));
#83060=CARTESIAN_POINT('',(-73.9013264985861,-9.42570643237816,0.));
#83061=CARTESIAN_POINT('',(-73.6640787197672,-8.93459554655821,0.));
#83062=CARTESIAN_POINT('Ctrl Pts',(-73.9013264985861,-9.42570643237816,
0.));
#83063=CARTESIAN_POINT('Ctrl Pts',(-73.9152287787081,-9.31670696907602,
0.));
#83064=CARTESIAN_POINT('Ctrl Pts',(-73.8917746035988,-9.20329838516133,
0.));
#83065=CARTESIAN_POINT('Ctrl Pts',(-73.8361439572621,-9.10865360927305,
0.));
#83066=CARTESIAN_POINT('Ctrl Pts',(-73.7944209725097,-9.03767002735684,
0.));
#83067=CARTESIAN_POINT('Ctrl Pts',(-73.7345987226919,-8.97724108745549,
0.));
#83068=CARTESIAN_POINT('Ctrl Pts',(-73.6640787197673,-8.93459554655806,
0.));
#83069=CARTESIAN_POINT('',(-73.6640787197672,-8.93459554655823,12.));
#83070=CARTESIAN_POINT('Ctrl Pts',(-73.6640787197673,-8.93459554655806,
0.));
#83071=CARTESIAN_POINT('Ctrl Pts',(-73.6640787197673,-8.93459554655806,
4.));
#83072=CARTESIAN_POINT('Ctrl Pts',(-73.6640787197673,-8.93459554655801,
8.));
#83073=CARTESIAN_POINT('Ctrl Pts',(-73.6640787197673,-8.93459554655801,
12.));
#83074=CARTESIAN_POINT('',(-73.9013264985861,-9.42570643237813,12.));
#83075=CARTESIAN_POINT('Ctrl Pts',(-73.6640787197673,-8.93459554655801,
12.));
#83076=CARTESIAN_POINT('Ctrl Pts',(-73.7345987226919,-8.97724108745545,
12.));
#83077=CARTESIAN_POINT('Ctrl Pts',(-73.7944209725097,-9.03767002735682,
12.));
#83078=CARTESIAN_POINT('Ctrl Pts',(-73.8361439572622,-9.10865360927303,
12.));
#83079=CARTESIAN_POINT('Ctrl Pts',(-73.8917746035988,-9.20329838516131,
12.));
#83080=CARTESIAN_POINT('Ctrl Pts',(-73.9152287787081,-9.31670696907599,
12.));
#83081=CARTESIAN_POINT('Ctrl Pts',(-73.9013264985861,-9.42570643237813,
12.));
#83082=CARTESIAN_POINT('Ctrl Pts',(-73.9013264985861,-9.42570643237813,
12.));
#83083=CARTESIAN_POINT('Ctrl Pts',(-73.9013264985861,-9.42570643237813,
8.));
#83084=CARTESIAN_POINT('Ctrl Pts',(-73.9013264985861,-9.42570643237816,
4.));
#83085=CARTESIAN_POINT('Ctrl Pts',(-73.9013264985861,-9.42570643237816,
0.));
#83086=CARTESIAN_POINT('Ctrl Pts',(-69.6540253893192,-6.95102489306925,
0.));
#83087=CARTESIAN_POINT('Ctrl Pts',(-69.6540253893192,-6.95102489306925,
12.));
#83088=CARTESIAN_POINT('Ctrl Pts',(-69.6576616146467,-6.95238884849025,
0.));
#83089=CARTESIAN_POINT('Ctrl Pts',(-69.6576616146467,-6.95238884849025,
12.));
#83090=CARTESIAN_POINT('Ctrl Pts',(-69.664938391983,-6.95512065317599,0.));
#83091=CARTESIAN_POINT('Ctrl Pts',(-69.664938391983,-6.95512065317599,12.));
#83092=CARTESIAN_POINT('Ctrl Pts',(-69.6758665380378,-6.95923004173591,
0.));
#83093=CARTESIAN_POINT('Ctrl Pts',(-69.6758665380378,-6.95923004173591,
12.));
#83094=CARTESIAN_POINT('Ctrl Pts',(-69.6904633605421,-6.96473259049513,
0.));
#83095=CARTESIAN_POINT('Ctrl Pts',(-69.6904633605421,-6.96473259049513,
12.));
#83096=CARTESIAN_POINT('Ctrl Pts',(-69.7087526479973,-6.97164972291439,
0.));
#83097=CARTESIAN_POINT('Ctrl Pts',(-69.7087526479973,-6.97164972291439,
12.));
#83098=CARTESIAN_POINT('Ctrl Pts',(-69.7270851557366,-6.97860581164527,
0.));
#83099=CARTESIAN_POINT('Ctrl Pts',(-69.7270851557366,-6.97860581164527,
12.));
#83100=CARTESIAN_POINT('Ctrl Pts',(-69.7454607995607,-6.98560086924214,
0.));
#83101=CARTESIAN_POINT('Ctrl Pts',(-69.7454607995607,-6.98560086924214,
12.));
#83102=CARTESIAN_POINT('Ctrl Pts',(-69.7638794280419,-6.9926349102794,0.));
#83103=CARTESIAN_POINT('Ctrl Pts',(-69.7638794280419,-6.9926349102794,12.));
#83104=CARTESIAN_POINT('Ctrl Pts',(-69.782340824259,-6.99970795069476,0.));
#83105=CARTESIAN_POINT('Ctrl Pts',(-69.782340824259,-6.99970795069476,12.));
#83106=CARTESIAN_POINT('Ctrl Pts',(-69.8008447346863,-7.0068200071815,0.));
#83107=CARTESIAN_POINT('Ctrl Pts',(-69.8008447346863,-7.0068200071815,12.));
#83108=CARTESIAN_POINT('Ctrl Pts',(-69.8193908913722,-7.01397109655454,
0.));
#83109=CARTESIAN_POINT('Ctrl Pts',(-69.8193908913722,-7.01397109655454,
12.));
#83110=CARTESIAN_POINT('Ctrl Pts',(-69.8379790360518,-7.02116123514451,
0.));
#83111=CARTESIAN_POINT('Ctrl Pts',(-69.8379790360518,-7.02116123514451,
12.));
#83112=CARTESIAN_POINT('Ctrl Pts',(-69.8566089455375,-7.02839043811812,
0.));
#83113=CARTESIAN_POINT('Ctrl Pts',(-69.8566089455375,-7.02839043811812,
12.));
#83114=CARTESIAN_POINT('Ctrl Pts',(-69.8752804235238,-7.03565871972221,
0.));
#83115=CARTESIAN_POINT('Ctrl Pts',(-69.8752804235238,-7.03565871972221,
12.));
#83116=CARTESIAN_POINT('Ctrl Pts',(-69.8939932885841,-7.04296609362165,
0.));
#83117=CARTESIAN_POINT('Ctrl Pts',(-69.8939932885841,-7.04296609362165,
12.));
#83118=CARTESIAN_POINT('Ctrl Pts',(-69.9127473642099,-7.05031257318115,
0.));
#83119=CARTESIAN_POINT('Ctrl Pts',(-69.9127473642099,-7.05031257318115,
12.));
#83120=CARTESIAN_POINT('Ctrl Pts',(-69.9315424664291,-7.05769817180857,
0.));
#83121=CARTESIAN_POINT('Ctrl Pts',(-69.9315424664291,-7.05769817180857,
12.));
#83122=CARTESIAN_POINT('Ctrl Pts',(-69.9503783975727,-7.06512290312849,
0.));
#83123=CARTESIAN_POINT('Ctrl Pts',(-69.9503783975727,-7.06512290312849,
12.));
#83124=CARTESIAN_POINT('Ctrl Pts',(-69.9692549527296,-7.07258678080831,
0.));
#83125=CARTESIAN_POINT('Ctrl Pts',(-69.9692549527296,-7.07258678080831,
12.));
#83126=CARTESIAN_POINT('Ctrl Pts',(-69.988171923788,-7.08008981844652,0.));
#83127=CARTESIAN_POINT('Ctrl Pts',(-69.988171923788,-7.08008981844652,12.));
#83128=CARTESIAN_POINT('Ctrl Pts',(-70.0071291040766,-7.08763202944246,
0.));
#83129=CARTESIAN_POINT('Ctrl Pts',(-70.0071291040766,-7.08763202944246,
12.));
#83130=CARTESIAN_POINT('Ctrl Pts',(-70.0261262936388,-7.09521342684248,
0.));
#83131=CARTESIAN_POINT('Ctrl Pts',(-70.0261262936388,-7.09521342684248,
12.));
#83132=CARTESIAN_POINT('Ctrl Pts',(-70.0451632990086,-7.10283402335034,
0.));
#83133=CARTESIAN_POINT('Ctrl Pts',(-70.0451632990086,-7.10283402335034,
12.));
#83134=CARTESIAN_POINT('Ctrl Pts',(-70.0642399306869,-7.11049383140445,
0.));
#83135=CARTESIAN_POINT('Ctrl Pts',(-70.0642399306869,-7.11049383140445,
12.));
#83136=CARTESIAN_POINT('Ctrl Pts',(-70.0833560013975,-7.11819286322826,
0.));
#83137=CARTESIAN_POINT('Ctrl Pts',(-70.0833560013975,-7.11819286322826,
12.));
#83138=CARTESIAN_POINT('Ctrl Pts',(-70.1025113239495,-7.12593113088903,
0.));
#83139=CARTESIAN_POINT('Ctrl Pts',(-70.1025113239495,-7.12593113088903,
12.));
#83140=CARTESIAN_POINT('Ctrl Pts',(-70.1217057094499,-7.13370864634442,
0.));
#83141=CARTESIAN_POINT('Ctrl Pts',(-70.1217057094499,-7.13370864634442,
12.));
#83142=CARTESIAN_POINT('Ctrl Pts',(-70.1409389682424,-7.14152542142373,
0.));
#83143=CARTESIAN_POINT('Ctrl Pts',(-70.1409389682424,-7.14152542142373,
12.));
#83144=CARTESIAN_POINT('Ctrl Pts',(-70.1602109107202,-7.14938146780813,
0.));
#83145=CARTESIAN_POINT('Ctrl Pts',(-70.1602109107202,-7.14938146780813,
12.));
#83146=CARTESIAN_POINT('Ctrl Pts',(-70.1795213481185,-7.15727679700933,
0.));
#83147=CARTESIAN_POINT('Ctrl Pts',(-70.1795213481185,-7.15727679700933,
12.));
#83148=CARTESIAN_POINT('Ctrl Pts',(-70.1988700934593,-7.16521142033863,
0.));
#83149=CARTESIAN_POINT('Ctrl Pts',(-70.1988700934593,-7.16521142033863,
12.));
#83150=CARTESIAN_POINT('Ctrl Pts',(-70.2182569618994,-7.17318534889715,
0.));
#83151=CARTESIAN_POINT('Ctrl Pts',(-70.2182569618994,-7.17318534889715,
12.));
#83152=CARTESIAN_POINT('Ctrl Pts',(-70.2376817702215,-7.18119859359777,
0.));
#83153=CARTESIAN_POINT('Ctrl Pts',(-70.2376817702215,-7.18119859359777,
12.));
#83154=CARTESIAN_POINT('Ctrl Pts',(-70.2571443365192,-7.18925116517555,
0.));
#83155=CARTESIAN_POINT('Ctrl Pts',(-70.2571443365192,-7.18925116517555,
12.));
#83156=CARTESIAN_POINT('Ctrl Pts',(-70.2766444798285,-7.19734307419873,
0.));
#83157=CARTESIAN_POINT('Ctrl Pts',(-70.2766444798285,-7.19734307419873,
12.));
#83158=CARTESIAN_POINT('Ctrl Pts',(-70.2961820197077,-7.20547433107482,
0.));
#83159=CARTESIAN_POINT('Ctrl Pts',(-70.2961820197077,-7.20547433107482,
12.));
#83160=CARTESIAN_POINT('Ctrl Pts',(-70.3157567762588,-7.21364494605449,
0.));
#83161=CARTESIAN_POINT('Ctrl Pts',(-70.3157567762588,-7.21364494605449,
12.));
#83162=CARTESIAN_POINT('Ctrl Pts',(-70.3353685703112,-7.22185492923191,
0.));
#83163=CARTESIAN_POINT('Ctrl Pts',(-70.3353685703112,-7.22185492923191,
12.));
#83164=CARTESIAN_POINT('Ctrl Pts',(-70.3550172235486,-7.23010429054229,
0.));
#83165=CARTESIAN_POINT('Ctrl Pts',(-70.3550172235486,-7.23010429054229,
12.));
#83166=CARTESIAN_POINT('Ctrl Pts',(-70.3747025586552,-7.23839303975606,
0.));
#83167=CARTESIAN_POINT('Ctrl Pts',(-70.3747025586552,-7.23839303975606,
12.));
#83168=CARTESIAN_POINT('Ctrl Pts',(-70.3944243994504,-7.24672118647084,
0.));
#83169=CARTESIAN_POINT('Ctrl Pts',(-70.3944243994504,-7.24672118647084,
12.));
#83170=CARTESIAN_POINT('Ctrl Pts',(-70.4141825708178,-7.25508874012043,
0.));
#83171=CARTESIAN_POINT('Ctrl Pts',(-70.4141825708178,-7.25508874012043,
12.));
#83172=CARTESIAN_POINT('Ctrl Pts',(-70.4339768986346,-7.26349570998032,
0.));
#83173=CARTESIAN_POINT('Ctrl Pts',(-70.4339768986346,-7.26349570998032,
12.));
#83174=CARTESIAN_POINT('Ctrl Pts',(-70.4538072096992,-7.27194210517062,
0.));
#83175=CARTESIAN_POINT('Ctrl Pts',(-70.4538072096992,-7.27194210517062,
12.));
#83176=CARTESIAN_POINT('Ctrl Pts',(-70.4736733316487,-7.2804279346547,0.));
#83177=CARTESIAN_POINT('Ctrl Pts',(-70.4736733316487,-7.2804279346547,12.));
#83178=CARTESIAN_POINT('Ctrl Pts',(-70.4935750929058,-7.28895320723862,
0.));
#83179=CARTESIAN_POINT('Ctrl Pts',(-70.4935750929058,-7.28895320723862,
12.));
#83180=CARTESIAN_POINT('Ctrl Pts',(-70.5135123227169,-7.29751793157822,
0.));
#83181=CARTESIAN_POINT('Ctrl Pts',(-70.5135123227169,-7.29751793157822,
12.));
#83182=CARTESIAN_POINT('Ctrl Pts',(-70.5334848511681,-7.30612211618053,
0.));
#83183=CARTESIAN_POINT('Ctrl Pts',(-70.5334848511681,-7.30612211618053,
12.));
#83184=CARTESIAN_POINT('Ctrl Pts',(-70.5534925092043,-7.31476576940391,
0.));
#83185=CARTESIAN_POINT('Ctrl Pts',(-70.5534925092043,-7.31476576940391,
12.));
#83186=CARTESIAN_POINT('Ctrl Pts',(-70.5735351286476,-7.32344889945219,
0.));
#83187=CARTESIAN_POINT('Ctrl Pts',(-70.5735351286476,-7.32344889945219,
12.));
#83188=CARTESIAN_POINT('Ctrl Pts',(-70.5936125421946,-7.3321715143759,0.));
#83189=CARTESIAN_POINT('Ctrl Pts',(-70.5936125421946,-7.3321715143759,12.));
#83190=CARTESIAN_POINT('Ctrl Pts',(-70.6137245833996,-7.34093362208007,
0.));
#83191=CARTESIAN_POINT('Ctrl Pts',(-70.6137245833996,-7.34093362208007,
12.));
#83192=CARTESIAN_POINT('Ctrl Pts',(-70.6338710866562,-7.34973523032577,
0.));
#83193=CARTESIAN_POINT('Ctrl Pts',(-70.6338710866562,-7.34973523032577,
12.));
#83194=CARTESIAN_POINT('Ctrl Pts',(-70.6540518871775,-7.35857634673054,
0.));
#83195=CARTESIAN_POINT('Ctrl Pts',(-70.6540518871775,-7.35857634673054,
12.));
#83196=CARTESIAN_POINT('Ctrl Pts',(-70.6742668209687,-7.367456978763,0.));
#83197=CARTESIAN_POINT('Ctrl Pts',(-70.6742668209687,-7.367456978763,12.));
#83198=CARTESIAN_POINT('Ctrl Pts',(-70.694515724827,-7.37637713374767,0.));
#83199=CARTESIAN_POINT('Ctrl Pts',(-70.694515724827,-7.37637713374767,12.));
#83200=CARTESIAN_POINT('Ctrl Pts',(-70.7147984363424,-7.38533681887032,
0.));
#83201=CARTESIAN_POINT('Ctrl Pts',(-70.7147984363424,-7.38533681887032,
12.));
#83202=CARTESIAN_POINT('Ctrl Pts',(-70.735114793895,-7.3943360411789,0.));
#83203=CARTESIAN_POINT('Ctrl Pts',(-70.735114793895,-7.3943360411789,12.));
#83204=CARTESIAN_POINT('Ctrl Pts',(-70.7554646366514,-7.4033748075823,0.));
#83205=CARTESIAN_POINT('Ctrl Pts',(-70.7554646366514,-7.4033748075823,12.));
#83206=CARTESIAN_POINT('Ctrl Pts',(-70.7758478045576,-7.41245312484487,
0.));
#83207=CARTESIAN_POINT('Ctrl Pts',(-70.7758478045576,-7.41245312484487,
12.));
#83208=CARTESIAN_POINT('Ctrl Pts',(-70.7962641383351,-7.42157099959316,
0.));
#83209=CARTESIAN_POINT('Ctrl Pts',(-70.7962641383351,-7.42157099959316,
12.));
#83210=CARTESIAN_POINT('Ctrl Pts',(-70.8167134794738,-7.43072843832008,
0.));
#83211=CARTESIAN_POINT('Ctrl Pts',(-70.8167134794738,-7.43072843832008,
12.));
#83212=CARTESIAN_POINT('Ctrl Pts',(-70.8371956702242,-7.43992544738606,
0.));
#83213=CARTESIAN_POINT('Ctrl Pts',(-70.8371956702242,-7.43992544738606,
12.));
#83214=CARTESIAN_POINT('Ctrl Pts',(-70.8577105535841,-7.44916203301645,
0.));
#83215=CARTESIAN_POINT('Ctrl Pts',(-70.8577105535841,-7.44916203301645,
12.));
#83216=CARTESIAN_POINT('Ctrl Pts',(-70.8782579732885,-7.45843820129776,
0.));
#83217=CARTESIAN_POINT('Ctrl Pts',(-70.8782579732885,-7.45843820129776,
12.));
#83218=CARTESIAN_POINT('Ctrl Pts',(-70.8988377738088,-7.46775395818518,
0.));
#83219=CARTESIAN_POINT('Ctrl Pts',(-70.8988377738088,-7.46775395818518,
12.));
#83220=CARTESIAN_POINT('Ctrl Pts',(-70.9194498003483,-7.47710930950554,
0.));
#83221=CARTESIAN_POINT('Ctrl Pts',(-70.9194498003483,-7.47710930950554,
12.));
#83222=CARTESIAN_POINT('Ctrl Pts',(-70.9400938988373,-7.48650426095823,
0.));
#83223=CARTESIAN_POINT('Ctrl Pts',(-70.9400938988373,-7.48650426095823,
12.));
#83224=CARTESIAN_POINT('Ctrl Pts',(-70.9607699159234,-7.49593881811141,
0.));
#83225=CARTESIAN_POINT('Ctrl Pts',(-70.9607699159234,-7.49593881811141,
12.));
#83226=CARTESIAN_POINT('Ctrl Pts',(-70.9814776989637,-7.50541298639948,
0.));
#83227=CARTESIAN_POINT('Ctrl Pts',(-70.9814776989637,-7.50541298639948,
12.));
#83228=CARTESIAN_POINT('Ctrl Pts',(-71.0022170960235,-7.51492677113111,
0.));
#83229=CARTESIAN_POINT('Ctrl Pts',(-71.0022170960235,-7.51492677113111,
12.));
#83230=CARTESIAN_POINT('Ctrl Pts',(-71.0229879558713,-7.52448017749136,
0.));
#83231=CARTESIAN_POINT('Ctrl Pts',(-71.0229879558713,-7.52448017749136,
12.));
#83232=CARTESIAN_POINT('Ctrl Pts',(-71.0437901279722,-7.53407321054253,
0.));
#83233=CARTESIAN_POINT('Ctrl Pts',(-71.0437901279722,-7.53407321054253,
12.));
#83234=CARTESIAN_POINT('Ctrl Pts',(-71.0646234624783,-7.54370587521948,
0.));
#83235=CARTESIAN_POINT('Ctrl Pts',(-71.0646234624783,-7.54370587521948,
12.));
#83236=CARTESIAN_POINT('Ctrl Pts',(-71.0854878102203,-7.55337817632872,
0.));
#83237=CARTESIAN_POINT('Ctrl Pts',(-71.0854878102203,-7.55337817632872,
12.));
#83238=CARTESIAN_POINT('Ctrl Pts',(-71.1063830227074,-7.56309011855616,
0.));
#83239=CARTESIAN_POINT('Ctrl Pts',(-71.1063830227074,-7.56309011855616,
12.));
#83240=CARTESIAN_POINT('Ctrl Pts',(-71.1273089521218,-7.57284170646866,
0.));
#83241=CARTESIAN_POINT('Ctrl Pts',(-71.1273089521218,-7.57284170646866,
12.));
#83242=CARTESIAN_POINT('Ctrl Pts',(-71.1482654513133,-7.58263294451465,
0.));
#83243=CARTESIAN_POINT('Ctrl Pts',(-71.1482654513133,-7.58263294451465,
12.));
#83244=CARTESIAN_POINT('Ctrl Pts',(-71.1692523737887,-7.5924638370186,0.));
#83245=CARTESIAN_POINT('Ctrl Pts',(-71.1692523737887,-7.5924638370186,12.));
#83246=CARTESIAN_POINT('Ctrl Pts',(-71.1902695737063,-7.60233438818156,
0.));
#83247=CARTESIAN_POINT('Ctrl Pts',(-71.1902695737063,-7.60233438818156,
12.));
#83248=CARTESIAN_POINT('Ctrl Pts',(-71.2113169058778,-7.61224460208886,
0.));
#83249=CARTESIAN_POINT('Ctrl Pts',(-71.2113169058778,-7.61224460208886,
12.));
#83250=CARTESIAN_POINT('Ctrl Pts',(-71.232394225762,-7.62219448271124,0.));
#83251=CARTESIAN_POINT('Ctrl Pts',(-71.232394225762,-7.62219448271124,12.));
#83252=CARTESIAN_POINT('Ctrl Pts',(-71.2535013894587,-7.63218403390514,
0.));
#83253=CARTESIAN_POINT('Ctrl Pts',(-71.2535013894587,-7.63218403390514,
12.));
#83254=CARTESIAN_POINT('Ctrl Pts',(-71.2746382536974,-7.64221325940671,
0.));
#83255=CARTESIAN_POINT('Ctrl Pts',(-71.2746382536974,-7.64221325940671,
12.));
#83256=CARTESIAN_POINT('Ctrl Pts',(-71.2958046758334,-7.65228216283342,
0.));
#83257=CARTESIAN_POINT('Ctrl Pts',(-71.2958046758334,-7.65228216283342,
12.));
#83258=CARTESIAN_POINT('Ctrl Pts',(-71.3170005138474,-7.66239074769119,
0.));
#83259=CARTESIAN_POINT('Ctrl Pts',(-71.3170005138474,-7.66239074769119,
12.));
#83260=CARTESIAN_POINT('Ctrl Pts',(-71.3382256263405,-7.67253901737539,
0.));
#83261=CARTESIAN_POINT('Ctrl Pts',(-71.3382256263405,-7.67253901737539,
12.));
#83262=CARTESIAN_POINT('Ctrl Pts',(-71.3594798725294,-7.68272697517103,
0.));
#83263=CARTESIAN_POINT('Ctrl Pts',(-71.3594798725294,-7.68272697517103,
12.));
#83264=CARTESIAN_POINT('Ctrl Pts',(-71.380763112236,-7.69295462424647,0.));
#83265=CARTESIAN_POINT('Ctrl Pts',(-71.380763112236,-7.69295462424647,12.));
#83266=CARTESIAN_POINT('Ctrl Pts',(-71.4020752058827,-7.70322196765572,
0.));
#83267=CARTESIAN_POINT('Ctrl Pts',(-71.4020752058827,-7.70322196765572,
12.));
#83268=CARTESIAN_POINT('Ctrl Pts',(-71.4234160144943,-7.71352900834537,
0.));
#83269=CARTESIAN_POINT('Ctrl Pts',(-71.4234160144943,-7.71352900834537,
12.));
#83270=CARTESIAN_POINT('Ctrl Pts',(-71.4447853996919,-7.72387574915544,
0.));
#83271=CARTESIAN_POINT('Ctrl Pts',(-71.4447853996919,-7.72387574915544,
12.));
#83272=CARTESIAN_POINT('Ctrl Pts',(-71.4661832236881,-7.73426219281931,
0.));
#83273=CARTESIAN_POINT('Ctrl Pts',(-71.4661832236881,-7.73426219281931,
12.));
#83274=CARTESIAN_POINT('Ctrl Pts',(-71.487609349277,-7.74468834195734,0.));
#83275=CARTESIAN_POINT('Ctrl Pts',(-71.487609349277,-7.74468834195734,12.));
#83276=CARTESIAN_POINT('Ctrl Pts',(-71.5090636398307,-7.75515419907955,
0.));
#83277=CARTESIAN_POINT('Ctrl Pts',(-71.5090636398307,-7.75515419907955,
12.));
#83278=CARTESIAN_POINT('Ctrl Pts',(-71.5305459592987,-7.76565976659218,
0.));
#83279=CARTESIAN_POINT('Ctrl Pts',(-71.5305459592987,-7.76565976659218,
12.));
#83280=CARTESIAN_POINT('Ctrl Pts',(-71.5520561722039,-7.77620504679868,
0.));
#83281=CARTESIAN_POINT('Ctrl Pts',(-71.5520561722039,-7.77620504679868,
12.));
#83282=CARTESIAN_POINT('Ctrl Pts',(-71.5735941436366,-7.78679004189935,
0.));
#83283=CARTESIAN_POINT('Ctrl Pts',(-71.5735941436366,-7.78679004189935,
12.));
#83284=CARTESIAN_POINT('Ctrl Pts',(-71.5951597392471,-7.79741475398511,
0.));
#83285=CARTESIAN_POINT('Ctrl Pts',(-71.5951597392471,-7.79741475398511,
12.));
#83286=CARTESIAN_POINT('Ctrl Pts',(-71.616752825242,-7.80807918504017,0.));
#83287=CARTESIAN_POINT('Ctrl Pts',(-71.616752825242,-7.80807918504017,12.));
#83288=CARTESIAN_POINT('Ctrl Pts',(-71.638373268384,-7.81878333694856,0.));
#83289=CARTESIAN_POINT('Ctrl Pts',(-71.638373268384,-7.81878333694856,12.));
#83290=CARTESIAN_POINT('Ctrl Pts',(-71.6600209359869,-7.82952721149504,
0.));
#83291=CARTESIAN_POINT('Ctrl Pts',(-71.6600209359869,-7.82952721149504,
12.));
#83292=CARTESIAN_POINT('Ctrl Pts',(-71.681695695912,-7.84031081036488,0.));
#83293=CARTESIAN_POINT('Ctrl Pts',(-71.681695695912,-7.84031081036488,12.));
#83294=CARTESIAN_POINT('Ctrl Pts',(-71.7033974165576,-7.85113413513739,
0.));
#83295=CARTESIAN_POINT('Ctrl Pts',(-71.7033974165576,-7.85113413513739,
12.));
#83296=CARTESIAN_POINT('Ctrl Pts',(-71.7251259668573,-7.86199718728829,
0.));
#83297=CARTESIAN_POINT('Ctrl Pts',(-71.7251259668573,-7.86199718728829,
12.));
#83298=CARTESIAN_POINT('Ctrl Pts',(-71.7468812162795,-7.87289996819654,
0.));
#83299=CARTESIAN_POINT('Ctrl Pts',(-71.7468812162795,-7.87289996819654,
12.));
#83300=CARTESIAN_POINT('Ctrl Pts',(-71.768663034824,-7.88384247914521,0.));
#83301=CARTESIAN_POINT('Ctrl Pts',(-71.768663034824,-7.88384247914521,12.));
#83302=CARTESIAN_POINT('Ctrl Pts',(-71.7904712930172,-7.89482472132135,
0.));
#83303=CARTESIAN_POINT('Ctrl Pts',(-71.7904712930172,-7.89482472132135,
12.));
#83304=CARTESIAN_POINT('Ctrl Pts',(-71.8123058619038,-7.90584669580955,
0.));
#83305=CARTESIAN_POINT('Ctrl Pts',(-71.8123058619038,-7.90584669580955,
12.));
#83306=CARTESIAN_POINT('Ctrl Pts',(-71.8341666130424,-7.9169084035937,0.));
#83307=CARTESIAN_POINT('Ctrl Pts',(-71.8341666130424,-7.9169084035937,12.));
#83308=CARTESIAN_POINT('Ctrl Pts',(-71.8560534185071,-7.928009845564,0.));
#83309=CARTESIAN_POINT('Ctrl Pts',(-71.8560534185071,-7.928009845564,12.));
#83310=CARTESIAN_POINT('Ctrl Pts',(-71.8779661508833,-7.93915102251796,
0.));
#83311=CARTESIAN_POINT('Ctrl Pts',(-71.8779661508833,-7.93915102251796,
12.));
#83312=CARTESIAN_POINT('Ctrl Pts',(-71.8999046832642,-7.95033193516046,
0.));
#83313=CARTESIAN_POINT('Ctrl Pts',(-71.8999046832642,-7.95033193516046,
12.));
#83314=CARTESIAN_POINT('Ctrl Pts',(-71.9218688892426,-7.96155258409751,
0.));
#83315=CARTESIAN_POINT('Ctrl Pts',(-71.9218688892426,-7.96155258409751,
12.));
#83316=CARTESIAN_POINT('Ctrl Pts',(-71.9438586429072,-7.97281296983702,
0.));
#83317=CARTESIAN_POINT('Ctrl Pts',(-71.9438586429072,-7.97281296983702,
12.));
#83318=CARTESIAN_POINT('Ctrl Pts',(-71.9658738188421,-7.98411309279597,
0.));
#83319=CARTESIAN_POINT('Ctrl Pts',(-71.9658738188421,-7.98411309279597,
12.));
#83320=CARTESIAN_POINT('Ctrl Pts',(-71.9879142921248,-7.99545295330182,
0.));
#83321=CARTESIAN_POINT('Ctrl Pts',(-71.9879142921248,-7.99545295330182,
12.));
#83322=CARTESIAN_POINT('Ctrl Pts',(-72.0099799383216,-8.0068325515925,0.));
#83323=CARTESIAN_POINT('Ctrl Pts',(-72.0099799383216,-8.0068325515925,12.));
#83324=CARTESIAN_POINT('Ctrl Pts',(-72.0320706334802,-8.0182518878107,0.));
#83325=CARTESIAN_POINT('Ctrl Pts',(-72.0320706334802,-8.0182518878107,12.));
#83326=CARTESIAN_POINT('Ctrl Pts',(-72.0541862541262,-8.02971096200328,
0.));
#83327=CARTESIAN_POINT('Ctrl Pts',(-72.0541862541262,-8.02971096200328,
12.));
#83328=CARTESIAN_POINT('Ctrl Pts',(-72.0763266772632,-8.04120977412891,
0.));
#83329=CARTESIAN_POINT('Ctrl Pts',(-72.0763266772632,-8.04120977412891,
12.));
#83330=CARTESIAN_POINT('Ctrl Pts',(-72.0984917803702,-8.05274832405957,
0.));
#83331=CARTESIAN_POINT('Ctrl Pts',(-72.0984917803702,-8.05274832405957,
12.));
#83332=CARTESIAN_POINT('Ctrl Pts',(-72.1206814413985,-8.06432661158089,
0.));
#83333=CARTESIAN_POINT('Ctrl Pts',(-72.1206814413985,-8.06432661158089,
12.));
#83334=CARTESIAN_POINT('Ctrl Pts',(-72.1428955387648,-8.07594463638699,
0.));
#83335=CARTESIAN_POINT('Ctrl Pts',(-72.1428955387648,-8.07594463638699,
12.));
#83336=CARTESIAN_POINT('Ctrl Pts',(-72.165133951346,-8.08760239807815,0.));
#83337=CARTESIAN_POINT('Ctrl Pts',(-72.165133951346,-8.08760239807815,12.));
#83338=CARTESIAN_POINT('Ctrl Pts',(-72.18739655848,-8.09929989616873,0.));
#83339=CARTESIAN_POINT('Ctrl Pts',(-72.18739655848,-8.09929989616873,12.));
#83340=CARTESIAN_POINT('Ctrl Pts',(-72.2096832399626,-8.11103713008922,
0.));
#83341=CARTESIAN_POINT('Ctrl Pts',(-72.2096832399626,-8.11103713008922,
12.));
#83342=CARTESIAN_POINT('Ctrl Pts',(-72.2319938760451,-8.12281409918661,
0.));
#83343=CARTESIAN_POINT('Ctrl Pts',(-72.2319938760451,-8.12281409918661,
12.));
#83344=CARTESIAN_POINT('Ctrl Pts',(-72.2543283474279,-8.13463080272029,
0.));
#83345=CARTESIAN_POINT('Ctrl Pts',(-72.2543283474279,-8.13463080272029,
12.));
#83346=CARTESIAN_POINT('Ctrl Pts',(-72.2766865352552,-8.14648723985793,
0.));
#83347=CARTESIAN_POINT('Ctrl Pts',(-72.2766865352552,-8.14648723985793,
12.));
#83348=CARTESIAN_POINT('Ctrl Pts',(-72.2990683211155,-8.15838340968327,
0.));
#83349=CARTESIAN_POINT('Ctrl Pts',(-72.2990683211155,-8.15838340968327,
12.));
#83350=CARTESIAN_POINT('Ctrl Pts',(-72.3214735870402,-8.17031931119882,
0.));
#83351=CARTESIAN_POINT('Ctrl Pts',(-72.3214735870402,-8.17031931119882,
12.));
#83352=CARTESIAN_POINT('Ctrl Pts',(-72.3439022155007,-8.18229494332622,
0.));
#83353=CARTESIAN_POINT('Ctrl Pts',(-72.3439022155007,-8.18229494332622,
12.));
#83354=CARTESIAN_POINT('Ctrl Pts',(-72.3663540894034,-8.19431030490319,
0.));
#83355=CARTESIAN_POINT('Ctrl Pts',(-72.3663540894034,-8.19431030490319,
12.));
#83356=CARTESIAN_POINT('Ctrl Pts',(-72.3888290920845,-8.20636539467781,
0.));
#83357=CARTESIAN_POINT('Ctrl Pts',(-72.3888290920845,-8.20636539467781,
12.));
#83358=CARTESIAN_POINT('Ctrl Pts',(-72.4113271073091,-8.21846021131563,
0.));
#83359=CARTESIAN_POINT('Ctrl Pts',(-72.4113271073091,-8.21846021131563,
12.));
#83360=CARTESIAN_POINT('Ctrl Pts',(-72.4338480192701,-8.23059475340354,
0.));
#83361=CARTESIAN_POINT('Ctrl Pts',(-72.4338480192701,-8.23059475340354,
12.));
#83362=CARTESIAN_POINT('Ctrl Pts',(-72.4563917125842,-8.24276901945036,
0.));
#83363=CARTESIAN_POINT('Ctrl Pts',(-72.4563917125842,-8.24276901945036,
12.));
#83364=CARTESIAN_POINT('Ctrl Pts',(-72.4789580722871,-8.25498300788493,
0.));
#83365=CARTESIAN_POINT('Ctrl Pts',(-72.4789580722871,-8.25498300788493,
12.));
#83366=CARTESIAN_POINT('Ctrl Pts',(-72.501546983825,-8.26723671704923,0.));
#83367=CARTESIAN_POINT('Ctrl Pts',(-72.501546983825,-8.26723671704923,12.));
#83368=CARTESIAN_POINT('Ctrl Pts',(-72.524158333056,-8.27953014520385,0.));
#83369=CARTESIAN_POINT('Ctrl Pts',(-72.524158333056,-8.27953014520385,12.));
#83370=CARTESIAN_POINT('Ctrl Pts',(-72.5467920062522,-8.29186329053288,
0.));
#83371=CARTESIAN_POINT('Ctrl Pts',(-72.5467920062522,-8.29186329053288,
12.));
#83372=CARTESIAN_POINT('Ctrl Pts',(-72.5694478900983,-8.30423615114455,
0.));
#83373=CARTESIAN_POINT('Ctrl Pts',(-72.5694478900983,-8.30423615114455,
12.));
#83374=CARTESIAN_POINT('Ctrl Pts',(-72.5921258716899,-8.31664872507008,
0.));
#83375=CARTESIAN_POINT('Ctrl Pts',(-72.5921258716899,-8.31664872507008,
12.));
#83376=CARTESIAN_POINT('Ctrl Pts',(-72.614825838529,-8.32910101025652,0.));
#83377=CARTESIAN_POINT('Ctrl Pts',(-72.614825838529,-8.32910101025652,12.));
#83378=CARTESIAN_POINT('Ctrl Pts',(-72.6375476785208,-8.34159300456965,
0.));
#83379=CARTESIAN_POINT('Ctrl Pts',(-72.6375476785208,-8.34159300456965,
12.));
#83380=CARTESIAN_POINT('Ctrl Pts',(-72.6602912799689,-8.35412470580083,
0.));
#83381=CARTESIAN_POINT('Ctrl Pts',(-72.6602912799689,-8.35412470580083,
12.));
#83382=CARTESIAN_POINT('Ctrl Pts',(-72.68305653157,-8.36669611166833,0.));
#83383=CARTESIAN_POINT('Ctrl Pts',(-72.68305653157,-8.36669611166833,12.));
#83384=CARTESIAN_POINT('Ctrl Pts',(-72.7058433224072,-8.37930721981734,
0.));
#83385=CARTESIAN_POINT('Ctrl Pts',(-72.7058433224072,-8.37930721981734,
12.));
#83386=CARTESIAN_POINT('Ctrl Pts',(-72.728651541938,-8.39195802781406,0.));
#83387=CARTESIAN_POINT('Ctrl Pts',(-72.728651541938,-8.39195802781406,12.));
#83388=CARTESIAN_POINT('Ctrl Pts',(-72.7514810799932,-8.40464853314493,
0.));
#83389=CARTESIAN_POINT('Ctrl Pts',(-72.7514810799932,-8.40464853314493,
12.));
#83390=CARTESIAN_POINT('Ctrl Pts',(-72.7743318267876,-8.41737873322352,
0.));
#83391=CARTESIAN_POINT('Ctrl Pts',(-72.7743318267876,-8.41737873322352,
12.));
#83392=CARTESIAN_POINT('Ctrl Pts',(-72.7972036729283,-8.4301486253917,0.));
#83393=CARTESIAN_POINT('Ctrl Pts',(-72.7972036729283,-8.4301486253917,12.));
#83394=CARTESIAN_POINT('Ctrl Pts',(-72.8200965094197,-8.44295820691906,
0.));
#83395=CARTESIAN_POINT('Ctrl Pts',(-72.8200965094197,-8.44295820691906,
12.));
#83396=CARTESIAN_POINT('Ctrl Pts',(-72.8430102276703,-8.4558074749977,0.));
#83397=CARTESIAN_POINT('Ctrl Pts',(-72.8430102276703,-8.4558074749977,12.));
#83398=CARTESIAN_POINT('Ctrl Pts',(-72.8659447194918,-8.46869642673763,
0.));
#83399=CARTESIAN_POINT('Ctrl Pts',(-72.8659447194918,-8.46869642673763,
12.));
#83400=CARTESIAN_POINT('Ctrl Pts',(-72.888899877077,-8.48162505917627,0.));
#83401=CARTESIAN_POINT('Ctrl Pts',(-72.888899877077,-8.48162505917627,12.));
#83402=CARTESIAN_POINT('Ctrl Pts',(-72.9118755929785,-8.49459336928275,
0.));
#83403=CARTESIAN_POINT('Ctrl Pts',(-72.9118755929785,-8.49459336928275,
12.));
#83404=CARTESIAN_POINT('Ctrl Pts',(-72.9348717600837,-8.50760135395979,
0.));
#83405=CARTESIAN_POINT('Ctrl Pts',(-72.9348717600837,-8.50760135395979,
12.));
#83406=CARTESIAN_POINT('Ctrl Pts',(-72.9578882715923,-8.52064901004243,
0.));
#83407=CARTESIAN_POINT('Ctrl Pts',(-72.9578882715923,-8.52064901004243,
12.));
#83408=CARTESIAN_POINT('Ctrl Pts',(-72.9809250209843,-8.53373633429303,
0.));
#83409=CARTESIAN_POINT('Ctrl Pts',(-72.9809250209843,-8.53373633429303,
12.));
#83410=CARTESIAN_POINT('Ctrl Pts',(-73.0039819020663,-8.54686332340438,
0.));
#83411=CARTESIAN_POINT('Ctrl Pts',(-73.0039819020663,-8.54686332340438,
12.));
#83412=CARTESIAN_POINT('Ctrl Pts',(-73.0270588090193,-8.56002997400096,
0.));
#83413=CARTESIAN_POINT('Ctrl Pts',(-73.0270588090193,-8.56002997400096,
12.));
#83414=CARTESIAN_POINT('Ctrl Pts',(-73.0501556364482,-8.57323628263595,
0.));
#83415=CARTESIAN_POINT('Ctrl Pts',(-73.0501556364482,-8.57323628263595,
12.));
#83416=CARTESIAN_POINT('Ctrl Pts',(-73.073272279419,-8.58648224578723,0.));
#83417=CARTESIAN_POINT('Ctrl Pts',(-73.073272279419,-8.58648224578723,12.));
#83418=CARTESIAN_POINT('Ctrl Pts',(-73.0964086335226,-8.59976785984538,
0.));
#83419=CARTESIAN_POINT('Ctrl Pts',(-73.0964086335226,-8.59976785984538,
12.));
#83420=CARTESIAN_POINT('Ctrl Pts',(-73.1195645948169,-8.61309312111988,
0.));
#83421=CARTESIAN_POINT('Ctrl Pts',(-73.1195645948169,-8.61309312111988,
12.));
#83422=CARTESIAN_POINT('Ctrl Pts',(-73.142740059703,-8.62645802585474,0.));
#83423=CARTESIAN_POINT('Ctrl Pts',(-73.142740059703,-8.62645802585474,12.));
#83424=CARTESIAN_POINT('Ctrl Pts',(-73.165934924813,-8.63986257023735,0.));
#83425=CARTESIAN_POINT('Ctrl Pts',(-73.165934924813,-8.63986257023735,12.));
#83426=CARTESIAN_POINT('Ctrl Pts',(-73.1891490869057,-8.65330675040535,
0.));
#83427=CARTESIAN_POINT('Ctrl Pts',(-73.1891490869057,-8.65330675040535,
12.));
#83428=CARTESIAN_POINT('Ctrl Pts',(-73.2123824427212,-8.66679056245095,
0.));
#83429=CARTESIAN_POINT('Ctrl Pts',(-73.2123824427212,-8.66679056245095,
12.));
#83430=CARTESIAN_POINT('Ctrl Pts',(-73.2356348889704,-8.68031400241883,
0.));
#83431=CARTESIAN_POINT('Ctrl Pts',(-73.2356348889704,-8.68031400241883,
12.));
#83432=CARTESIAN_POINT('Ctrl Pts',(-73.2589063226373,-8.69387706629304,
0.));
#83433=CARTESIAN_POINT('Ctrl Pts',(-73.2589063226373,-8.69387706629304,
12.));
#83434=CARTESIAN_POINT('Ctrl Pts',(-73.282196641216,-8.70747974998244,0.));
#83435=CARTESIAN_POINT('Ctrl Pts',(-73.282196641216,-8.70747974998244,12.));
#83436=CARTESIAN_POINT('Ctrl Pts',(-73.3055057429744,-8.72112204930232,
0.));
#83437=CARTESIAN_POINT('Ctrl Pts',(-73.3055057429744,-8.72112204930232,
12.));
#83438=CARTESIAN_POINT('Ctrl Pts',(-73.3288335271989,-8.73480395995359,
0.));
#83439=CARTESIAN_POINT('Ctrl Pts',(-73.3288335271989,-8.73480395995359,
12.));
#83440=CARTESIAN_POINT('Ctrl Pts',(-73.3521798944595,-8.74852547749736,
0.));
#83441=CARTESIAN_POINT('Ctrl Pts',(-73.3521798944595,-8.74852547749736,
12.));
#83442=CARTESIAN_POINT('Ctrl Pts',(-73.3755447460235,-8.76228659740304,
0.));
#83443=CARTESIAN_POINT('Ctrl Pts',(-73.3755447460235,-8.76228659740304,
12.));
#83444=CARTESIAN_POINT('Ctrl Pts',(-73.3989279832808,-8.77608731509303,
0.));
#83445=CARTESIAN_POINT('Ctrl Pts',(-73.3989279832808,-8.77608731509303,
12.));
#83446=CARTESIAN_POINT('Ctrl Pts',(-73.422329507112,-8.78992762598738,0.));
#83447=CARTESIAN_POINT('Ctrl Pts',(-73.422329507112,-8.78992762598738,12.));
#83448=CARTESIAN_POINT('Ctrl Pts',(-73.4457492173949,-8.80380752553714,
0.));
#83449=CARTESIAN_POINT('Ctrl Pts',(-73.4457492173949,-8.80380752553714,
12.));
#83450=CARTESIAN_POINT('Ctrl Pts',(-73.4691870121608,-8.81772700927593,
0.));
#83451=CARTESIAN_POINT('Ctrl Pts',(-73.4691870121608,-8.81772700927593,
12.));
#83452=CARTESIAN_POINT('Ctrl Pts',(-73.4926427882787,-8.83168607277414,
0.));
#83453=CARTESIAN_POINT('Ctrl Pts',(-73.4926427882787,-8.83168607277414,
12.));
#83454=CARTESIAN_POINT('Ctrl Pts',(-73.5161164429765,-8.84568471153893,
0.));
#83455=CARTESIAN_POINT('Ctrl Pts',(-73.5161164429765,-8.84568471153893,
12.));
#83456=CARTESIAN_POINT('Ctrl Pts',(-73.5396078751672,-8.85972292092182,
0.));
#83457=CARTESIAN_POINT('Ctrl Pts',(-73.5396078751672,-8.85972292092182,
12.));
#83458=CARTESIAN_POINT('Ctrl Pts',(-73.5631169867113,-8.87380069602954,
0.));
#83459=CARTESIAN_POINT('Ctrl Pts',(-73.5631169867113,-8.87380069602954,
12.));
#83460=CARTESIAN_POINT('Ctrl Pts',(-73.5866436840493,-8.8879180316034,0.));
#83461=CARTESIAN_POINT('Ctrl Pts',(-73.5866436840493,-8.8879180316034,12.));
#83462=CARTESIAN_POINT('Ctrl Pts',(-73.6101878785868,-8.90207492198871,
0.));
#83463=CARTESIAN_POINT('Ctrl Pts',(-73.6101878785868,-8.90207492198871,
12.));
#83464=CARTESIAN_POINT('Ctrl Pts',(-73.6337494830846,-8.91627136139886,
0.));
#83465=CARTESIAN_POINT('Ctrl Pts',(-73.6337494830846,-8.91627136139886,
12.));
#83466=CARTESIAN_POINT('Ctrl Pts',(-73.6573284088088,-8.9305073441197,0.));
#83467=CARTESIAN_POINT('Ctrl Pts',(-73.6573284088088,-8.9305073441197,12.));
#83468=CARTESIAN_POINT('Ctrl Pts',(-73.6809245622361,-8.94478286474383,
0.));
#83469=CARTESIAN_POINT('Ctrl Pts',(-73.6809245622361,-8.94478286474383,
12.));
#83470=CARTESIAN_POINT('Ctrl Pts',(-73.7045378422775,-8.9590979183629,0.));
#83471=CARTESIAN_POINT('Ctrl Pts',(-73.7045378422775,-8.9590979183629,12.));
#83472=CARTESIAN_POINT('Ctrl Pts',(-73.7281681364031,-8.97345250083917,
0.));
#83473=CARTESIAN_POINT('Ctrl Pts',(-73.7281681364031,-8.97345250083917,
12.));
#83474=CARTESIAN_POINT('Ctrl Pts',(-73.7518153262253,-8.98784660837827,
0.));
#83475=CARTESIAN_POINT('Ctrl Pts',(-73.7518153262253,-8.98784660837827,
12.));
#83476=CARTESIAN_POINT('Ctrl Pts',(-73.7754792943925,-9.00228023701466,
0.));
#83477=CARTESIAN_POINT('Ctrl Pts',(-73.7754792943925,-9.00228023701466,
12.));
#83478=CARTESIAN_POINT('Ctrl Pts',(-73.7991599312731,-9.01675338208221,
0.));
#83479=CARTESIAN_POINT('Ctrl Pts',(-73.7991599312731,-9.01675338208221,
12.));
#83480=CARTESIAN_POINT('Ctrl Pts',(-73.8228571411607,-9.0312660377798,0.));
#83481=CARTESIAN_POINT('Ctrl Pts',(-73.8228571411607,-9.0312660377798,12.));
#83482=CARTESIAN_POINT('Ctrl Pts',(-73.8465708500679,-9.04581819646384,
0.));
#83483=CARTESIAN_POINT('Ctrl Pts',(-73.8465708500679,-9.04581819646384,
12.));
#83484=CARTESIAN_POINT('Ctrl Pts',(-73.870301007746,-9.06040984889249,0.));
#83485=CARTESIAN_POINT('Ctrl Pts',(-73.870301007746,-9.06040984889249,12.));
#83486=CARTESIAN_POINT('Ctrl Pts',(-73.8940475821756,-9.07504098570547,
0.));
#83487=CARTESIAN_POINT('Ctrl Pts',(-73.8940475821756,-9.07504098570547,
12.));
#83488=CARTESIAN_POINT('Ctrl Pts',(-73.9130579611989,-9.08677747601237,
0.));
#83489=CARTESIAN_POINT('Ctrl Pts',(-73.9130579611989,-9.08677747601237,
12.));
#83490=CARTESIAN_POINT('Ctrl Pts',(-73.9273231219464,-9.09559760528458,
0.));
#83491=CARTESIAN_POINT('Ctrl Pts',(-73.9273231219464,-9.09559760528458,
12.));
#83492=CARTESIAN_POINT('Ctrl Pts',(-73.9368365074164,-9.10148558516323,
0.));
#83493=CARTESIAN_POINT('Ctrl Pts',(-73.9368365074164,-9.10148558516323,
12.));
#83494=CARTESIAN_POINT('Ctrl Pts',(-73.9415940197274,-9.10443154852686,
0.));
#83495=CARTESIAN_POINT('Ctrl Pts',(-73.9415940197274,-9.10443154852686,
12.));
#83496=CARTESIAN_POINT('',(-69.6540253893192,-6.95102489306925,0.));
#83497=CARTESIAN_POINT('Ctrl Pts',(-69.6540253893192,-6.95102489306925,
0.));
#83498=CARTESIAN_POINT('Ctrl Pts',(-69.6576616146467,-6.95238884849025,
0.));
#83499=CARTESIAN_POINT('Ctrl Pts',(-69.664938391983,-6.95512065317599,0.));
#83500=CARTESIAN_POINT('Ctrl Pts',(-69.6758665380378,-6.95923004173591,
0.));
#83501=CARTESIAN_POINT('Ctrl Pts',(-69.6904633605421,-6.96473259049513,
0.));
#83502=CARTESIAN_POINT('Ctrl Pts',(-69.7087526479973,-6.97164972291439,
0.));
#83503=CARTESIAN_POINT('Ctrl Pts',(-69.7270851557366,-6.97860581164527,
0.));
#83504=CARTESIAN_POINT('Ctrl Pts',(-69.7454607995607,-6.98560086924214,
0.));
#83505=CARTESIAN_POINT('Ctrl Pts',(-69.7638794280419,-6.9926349102794,0.));
#83506=CARTESIAN_POINT('Ctrl Pts',(-69.782340824259,-6.99970795069476,0.));
#83507=CARTESIAN_POINT('Ctrl Pts',(-69.8008447346863,-7.0068200071815,0.));
#83508=CARTESIAN_POINT('Ctrl Pts',(-69.8193908913722,-7.01397109655454,
0.));
#83509=CARTESIAN_POINT('Ctrl Pts',(-69.8379790360518,-7.02116123514451,
0.));
#83510=CARTESIAN_POINT('Ctrl Pts',(-69.8566089455375,-7.02839043811812,
0.));
#83511=CARTESIAN_POINT('Ctrl Pts',(-69.8752804235238,-7.03565871972221,
0.));
#83512=CARTESIAN_POINT('Ctrl Pts',(-69.8939932885841,-7.04296609362165,
0.));
#83513=CARTESIAN_POINT('Ctrl Pts',(-69.9127473642099,-7.05031257318115,
0.));
#83514=CARTESIAN_POINT('Ctrl Pts',(-69.9315424664291,-7.05769817180857,
0.));
#83515=CARTESIAN_POINT('Ctrl Pts',(-69.9503783975727,-7.06512290312849,
0.));
#83516=CARTESIAN_POINT('Ctrl Pts',(-69.9692549527296,-7.07258678080831,
0.));
#83517=CARTESIAN_POINT('Ctrl Pts',(-69.988171923788,-7.08008981844652,0.));
#83518=CARTESIAN_POINT('Ctrl Pts',(-70.0071291040766,-7.08763202944246,
0.));
#83519=CARTESIAN_POINT('Ctrl Pts',(-70.0261262936388,-7.09521342684248,
0.));
#83520=CARTESIAN_POINT('Ctrl Pts',(-70.0451632990086,-7.10283402335034,
0.));
#83521=CARTESIAN_POINT('Ctrl Pts',(-70.0642399306869,-7.11049383140445,
0.));
#83522=CARTESIAN_POINT('Ctrl Pts',(-70.0833560013975,-7.11819286322826,
0.));
#83523=CARTESIAN_POINT('Ctrl Pts',(-70.1025113239495,-7.12593113088903,
0.));
#83524=CARTESIAN_POINT('Ctrl Pts',(-70.1217057094499,-7.13370864634442,
0.));
#83525=CARTESIAN_POINT('Ctrl Pts',(-70.1409389682424,-7.14152542142373,
0.));
#83526=CARTESIAN_POINT('Ctrl Pts',(-70.1602109107202,-7.14938146780813,
0.));
#83527=CARTESIAN_POINT('Ctrl Pts',(-70.1795213481185,-7.15727679700933,
0.));
#83528=CARTESIAN_POINT('Ctrl Pts',(-70.1988700934593,-7.16521142033863,
0.));
#83529=CARTESIAN_POINT('Ctrl Pts',(-70.2182569618994,-7.17318534889715,
0.));
#83530=CARTESIAN_POINT('Ctrl Pts',(-70.2376817702215,-7.18119859359777,
0.));
#83531=CARTESIAN_POINT('Ctrl Pts',(-70.2571443365192,-7.18925116517555,
0.));
#83532=CARTESIAN_POINT('Ctrl Pts',(-70.2766444798285,-7.19734307419873,
0.));
#83533=CARTESIAN_POINT('Ctrl Pts',(-70.2961820197077,-7.20547433107482,
0.));
#83534=CARTESIAN_POINT('Ctrl Pts',(-70.3157567762588,-7.21364494605449,
0.));
#83535=CARTESIAN_POINT('Ctrl Pts',(-70.3353685703112,-7.22185492923191,
0.));
#83536=CARTESIAN_POINT('Ctrl Pts',(-70.3550172235486,-7.23010429054229,
0.));
#83537=CARTESIAN_POINT('Ctrl Pts',(-70.3747025586552,-7.23839303975606,
0.));
#83538=CARTESIAN_POINT('Ctrl Pts',(-70.3944243994504,-7.24672118647084,
0.));
#83539=CARTESIAN_POINT('Ctrl Pts',(-70.4141825708178,-7.25508874012043,
0.));
#83540=CARTESIAN_POINT('Ctrl Pts',(-70.4339768986346,-7.26349570998032,
0.));
#83541=CARTESIAN_POINT('Ctrl Pts',(-70.4538072096992,-7.27194210517062,
0.));
#83542=CARTESIAN_POINT('Ctrl Pts',(-70.4736733316487,-7.2804279346547,0.));
#83543=CARTESIAN_POINT('Ctrl Pts',(-70.4935750929058,-7.28895320723862,
0.));
#83544=CARTESIAN_POINT('Ctrl Pts',(-70.5135123227169,-7.29751793157822,
0.));
#83545=CARTESIAN_POINT('Ctrl Pts',(-70.5334848511681,-7.30612211618053,
0.));
#83546=CARTESIAN_POINT('Ctrl Pts',(-70.5534925092043,-7.31476576940391,
0.));
#83547=CARTESIAN_POINT('Ctrl Pts',(-70.5735351286476,-7.32344889945219,
0.));
#83548=CARTESIAN_POINT('Ctrl Pts',(-70.5936125421946,-7.3321715143759,0.));
#83549=CARTESIAN_POINT('Ctrl Pts',(-70.6137245833996,-7.34093362208007,
0.));
#83550=CARTESIAN_POINT('Ctrl Pts',(-70.6338710866562,-7.34973523032577,
0.));
#83551=CARTESIAN_POINT('Ctrl Pts',(-70.6540518871775,-7.35857634673054,
0.));
#83552=CARTESIAN_POINT('Ctrl Pts',(-70.6742668209687,-7.367456978763,0.));
#83553=CARTESIAN_POINT('Ctrl Pts',(-70.694515724827,-7.37637713374767,0.));
#83554=CARTESIAN_POINT('Ctrl Pts',(-70.7147984363424,-7.38533681887032,
0.));
#83555=CARTESIAN_POINT('Ctrl Pts',(-70.735114793895,-7.3943360411789,0.));
#83556=CARTESIAN_POINT('Ctrl Pts',(-70.7554646366514,-7.4033748075823,0.));
#83557=CARTESIAN_POINT('Ctrl Pts',(-70.7758478045576,-7.41245312484487,
0.));
#83558=CARTESIAN_POINT('Ctrl Pts',(-70.7962641383351,-7.42157099959316,
0.));
#83559=CARTESIAN_POINT('Ctrl Pts',(-70.8167134794738,-7.43072843832008,
0.));
#83560=CARTESIAN_POINT('Ctrl Pts',(-70.8371956702242,-7.43992544738606,
0.));
#83561=CARTESIAN_POINT('Ctrl Pts',(-70.8577105535841,-7.44916203301645,
0.));
#83562=CARTESIAN_POINT('Ctrl Pts',(-70.8782579732885,-7.45843820129776,
0.));
#83563=CARTESIAN_POINT('Ctrl Pts',(-70.8988377738088,-7.46775395818518,
0.));
#83564=CARTESIAN_POINT('Ctrl Pts',(-70.9194498003483,-7.47710930950554,
0.));
#83565=CARTESIAN_POINT('Ctrl Pts',(-70.9400938988373,-7.48650426095823,
0.));
#83566=CARTESIAN_POINT('Ctrl Pts',(-70.9607699159234,-7.49593881811141,
0.));
#83567=CARTESIAN_POINT('Ctrl Pts',(-70.9814776989637,-7.50541298639948,
0.));
#83568=CARTESIAN_POINT('Ctrl Pts',(-71.0022170960235,-7.51492677113111,
0.));
#83569=CARTESIAN_POINT('Ctrl Pts',(-71.0229879558713,-7.52448017749136,
0.));
#83570=CARTESIAN_POINT('Ctrl Pts',(-71.0437901279722,-7.53407321054253,
0.));
#83571=CARTESIAN_POINT('Ctrl Pts',(-71.0646234624783,-7.54370587521948,
0.));
#83572=CARTESIAN_POINT('Ctrl Pts',(-71.0854878102203,-7.55337817632872,
0.));
#83573=CARTESIAN_POINT('Ctrl Pts',(-71.1063830227074,-7.56309011855616,
0.));
#83574=CARTESIAN_POINT('Ctrl Pts',(-71.1273089521218,-7.57284170646866,
0.));
#83575=CARTESIAN_POINT('Ctrl Pts',(-71.1482654513133,-7.58263294451465,
0.));
#83576=CARTESIAN_POINT('Ctrl Pts',(-71.1692523737887,-7.5924638370186,0.));
#83577=CARTESIAN_POINT('Ctrl Pts',(-71.1902695737063,-7.60233438818156,
0.));
#83578=CARTESIAN_POINT('Ctrl Pts',(-71.2113169058778,-7.61224460208886,
0.));
#83579=CARTESIAN_POINT('Ctrl Pts',(-71.232394225762,-7.62219448271124,0.));
#83580=CARTESIAN_POINT('Ctrl Pts',(-71.2535013894587,-7.63218403390514,
0.));
#83581=CARTESIAN_POINT('Ctrl Pts',(-71.2746382536974,-7.64221325940671,
0.));
#83582=CARTESIAN_POINT('Ctrl Pts',(-71.2958046758334,-7.65228216283342,
0.));
#83583=CARTESIAN_POINT('Ctrl Pts',(-71.3170005138474,-7.66239074769119,
0.));
#83584=CARTESIAN_POINT('Ctrl Pts',(-71.3382256263405,-7.67253901737539,
0.));
#83585=CARTESIAN_POINT('Ctrl Pts',(-71.3594798725294,-7.68272697517103,
0.));
#83586=CARTESIAN_POINT('Ctrl Pts',(-71.380763112236,-7.69295462424647,0.));
#83587=CARTESIAN_POINT('Ctrl Pts',(-71.4020752058827,-7.70322196765572,
0.));
#83588=CARTESIAN_POINT('Ctrl Pts',(-71.4234160144943,-7.71352900834537,
0.));
#83589=CARTESIAN_POINT('Ctrl Pts',(-71.4447853996919,-7.72387574915544,
0.));
#83590=CARTESIAN_POINT('Ctrl Pts',(-71.4661832236881,-7.73426219281931,
0.));
#83591=CARTESIAN_POINT('Ctrl Pts',(-71.487609349277,-7.74468834195734,0.));
#83592=CARTESIAN_POINT('Ctrl Pts',(-71.5090636398307,-7.75515419907955,
0.));
#83593=CARTESIAN_POINT('Ctrl Pts',(-71.5305459592987,-7.76565976659218,
0.));
#83594=CARTESIAN_POINT('Ctrl Pts',(-71.5520561722039,-7.77620504679868,
0.));
#83595=CARTESIAN_POINT('Ctrl Pts',(-71.5735941436366,-7.78679004189935,
0.));
#83596=CARTESIAN_POINT('Ctrl Pts',(-71.5951597392471,-7.79741475398511,
0.));
#83597=CARTESIAN_POINT('Ctrl Pts',(-71.616752825242,-7.80807918504017,0.));
#83598=CARTESIAN_POINT('Ctrl Pts',(-71.638373268384,-7.81878333694856,0.));
#83599=CARTESIAN_POINT('Ctrl Pts',(-71.6600209359869,-7.82952721149504,
0.));
#83600=CARTESIAN_POINT('Ctrl Pts',(-71.681695695912,-7.84031081036488,0.));
#83601=CARTESIAN_POINT('Ctrl Pts',(-71.7033974165576,-7.85113413513739,
0.));
#83602=CARTESIAN_POINT('Ctrl Pts',(-71.7251259668573,-7.86199718728829,
0.));
#83603=CARTESIAN_POINT('Ctrl Pts',(-71.7468812162795,-7.87289996819654,
0.));
#83604=CARTESIAN_POINT('Ctrl Pts',(-71.768663034824,-7.88384247914521,0.));
#83605=CARTESIAN_POINT('Ctrl Pts',(-71.7904712930172,-7.89482472132135,
0.));
#83606=CARTESIAN_POINT('Ctrl Pts',(-71.8123058619038,-7.90584669580955,
0.));
#83607=CARTESIAN_POINT('Ctrl Pts',(-71.8341666130424,-7.9169084035937,0.));
#83608=CARTESIAN_POINT('Ctrl Pts',(-71.8560534185071,-7.928009845564,0.));
#83609=CARTESIAN_POINT('Ctrl Pts',(-71.8779661508833,-7.93915102251796,
0.));
#83610=CARTESIAN_POINT('Ctrl Pts',(-71.8999046832642,-7.95033193516046,
0.));
#83611=CARTESIAN_POINT('Ctrl Pts',(-71.9218688892426,-7.96155258409751,
0.));
#83612=CARTESIAN_POINT('Ctrl Pts',(-71.9438586429072,-7.97281296983702,
0.));
#83613=CARTESIAN_POINT('Ctrl Pts',(-71.9658738188421,-7.98411309279597,
0.));
#83614=CARTESIAN_POINT('Ctrl Pts',(-71.9879142921248,-7.99545295330182,
0.));
#83615=CARTESIAN_POINT('Ctrl Pts',(-72.0099799383216,-8.0068325515925,0.));
#83616=CARTESIAN_POINT('Ctrl Pts',(-72.0320706334802,-8.0182518878107,0.));
#83617=CARTESIAN_POINT('Ctrl Pts',(-72.0541862541262,-8.02971096200328,
0.));
#83618=CARTESIAN_POINT('Ctrl Pts',(-72.0763266772632,-8.04120977412891,
0.));
#83619=CARTESIAN_POINT('Ctrl Pts',(-72.0984917803702,-8.05274832405957,
0.));
#83620=CARTESIAN_POINT('Ctrl Pts',(-72.1206814413985,-8.06432661158089,
0.));
#83621=CARTESIAN_POINT('Ctrl Pts',(-72.1428955387648,-8.07594463638699,
0.));
#83622=CARTESIAN_POINT('Ctrl Pts',(-72.165133951346,-8.08760239807815,0.));
#83623=CARTESIAN_POINT('Ctrl Pts',(-72.18739655848,-8.09929989616873,0.));
#83624=CARTESIAN_POINT('Ctrl Pts',(-72.2096832399626,-8.11103713008922,
0.));
#83625=CARTESIAN_POINT('Ctrl Pts',(-72.2319938760451,-8.12281409918661,
0.));
#83626=CARTESIAN_POINT('Ctrl Pts',(-72.2543283474279,-8.13463080272029,
0.));
#83627=CARTESIAN_POINT('Ctrl Pts',(-72.2766865352552,-8.14648723985793,
0.));
#83628=CARTESIAN_POINT('Ctrl Pts',(-72.2990683211155,-8.15838340968327,
0.));
#83629=CARTESIAN_POINT('Ctrl Pts',(-72.3214735870402,-8.17031931119882,
0.));
#83630=CARTESIAN_POINT('Ctrl Pts',(-72.3439022155007,-8.18229494332622,
0.));
#83631=CARTESIAN_POINT('Ctrl Pts',(-72.3663540894034,-8.19431030490319,
0.));
#83632=CARTESIAN_POINT('Ctrl Pts',(-72.3888290920845,-8.20636539467781,
0.));
#83633=CARTESIAN_POINT('Ctrl Pts',(-72.4113271073091,-8.21846021131563,
0.));
#83634=CARTESIAN_POINT('Ctrl Pts',(-72.4338480192701,-8.23059475340354,
0.));
#83635=CARTESIAN_POINT('Ctrl Pts',(-72.4563917125842,-8.24276901945036,
0.));
#83636=CARTESIAN_POINT('Ctrl Pts',(-72.4789580722871,-8.25498300788493,
0.));
#83637=CARTESIAN_POINT('Ctrl Pts',(-72.501546983825,-8.26723671704923,0.));
#83638=CARTESIAN_POINT('Ctrl Pts',(-72.524158333056,-8.27953014520385,0.));
#83639=CARTESIAN_POINT('Ctrl Pts',(-72.5467920062522,-8.29186329053288,
0.));
#83640=CARTESIAN_POINT('Ctrl Pts',(-72.5694478900983,-8.30423615114455,
0.));
#83641=CARTESIAN_POINT('Ctrl Pts',(-72.5921258716899,-8.31664872507008,
0.));
#83642=CARTESIAN_POINT('Ctrl Pts',(-72.614825838529,-8.32910101025652,0.));
#83643=CARTESIAN_POINT('Ctrl Pts',(-72.6375476785208,-8.34159300456965,
0.));
#83644=CARTESIAN_POINT('Ctrl Pts',(-72.6602912799689,-8.35412470580083,
0.));
#83645=CARTESIAN_POINT('Ctrl Pts',(-72.68305653157,-8.36669611166833,0.));
#83646=CARTESIAN_POINT('Ctrl Pts',(-72.7058433224072,-8.37930721981734,
0.));
#83647=CARTESIAN_POINT('Ctrl Pts',(-72.728651541938,-8.39195802781406,0.));
#83648=CARTESIAN_POINT('Ctrl Pts',(-72.7514810799932,-8.40464853314493,
0.));
#83649=CARTESIAN_POINT('Ctrl Pts',(-72.7743318267876,-8.41737873322352,
0.));
#83650=CARTESIAN_POINT('Ctrl Pts',(-72.7972036729283,-8.4301486253917,0.));
#83651=CARTESIAN_POINT('Ctrl Pts',(-72.8200965094197,-8.44295820691906,
0.));
#83652=CARTESIAN_POINT('Ctrl Pts',(-72.8430102276703,-8.4558074749977,0.));
#83653=CARTESIAN_POINT('Ctrl Pts',(-72.8659447194918,-8.46869642673763,
0.));
#83654=CARTESIAN_POINT('Ctrl Pts',(-72.888899877077,-8.48162505917627,0.));
#83655=CARTESIAN_POINT('Ctrl Pts',(-72.9118755929785,-8.49459336928275,
0.));
#83656=CARTESIAN_POINT('Ctrl Pts',(-72.9348717600837,-8.50760135395979,
0.));
#83657=CARTESIAN_POINT('Ctrl Pts',(-72.9578882715923,-8.52064901004243,
0.));
#83658=CARTESIAN_POINT('Ctrl Pts',(-72.9809250209843,-8.53373633429303,
0.));
#83659=CARTESIAN_POINT('Ctrl Pts',(-73.0039819020663,-8.54686332340438,
0.));
#83660=CARTESIAN_POINT('Ctrl Pts',(-73.0270588090193,-8.56002997400096,
0.));
#83661=CARTESIAN_POINT('Ctrl Pts',(-73.0501556364482,-8.57323628263595,
0.));
#83662=CARTESIAN_POINT('Ctrl Pts',(-73.073272279419,-8.58648224578723,0.));
#83663=CARTESIAN_POINT('Ctrl Pts',(-73.0964086335226,-8.59976785984538,
0.));
#83664=CARTESIAN_POINT('Ctrl Pts',(-73.1195645948169,-8.61309312111988,
0.));
#83665=CARTESIAN_POINT('Ctrl Pts',(-73.142740059703,-8.62645802585474,0.));
#83666=CARTESIAN_POINT('Ctrl Pts',(-73.165934924813,-8.63986257023735,0.));
#83667=CARTESIAN_POINT('Ctrl Pts',(-73.1891490869057,-8.65330675040535,
0.));
#83668=CARTESIAN_POINT('Ctrl Pts',(-73.2123824427212,-8.66679056245095,
0.));
#83669=CARTESIAN_POINT('Ctrl Pts',(-73.2356348889704,-8.68031400241883,
0.));
#83670=CARTESIAN_POINT('Ctrl Pts',(-73.2589063226373,-8.69387706629304,
0.));
#83671=CARTESIAN_POINT('Ctrl Pts',(-73.282196641216,-8.70747974998244,0.));
#83672=CARTESIAN_POINT('Ctrl Pts',(-73.3055057429744,-8.72112204930232,
0.));
#83673=CARTESIAN_POINT('Ctrl Pts',(-73.3288335271989,-8.73480395995359,
0.));
#83674=CARTESIAN_POINT('Ctrl Pts',(-73.3521798944595,-8.74852547749736,
0.));
#83675=CARTESIAN_POINT('Ctrl Pts',(-73.3755447460235,-8.76228659740304,
0.));
#83676=CARTESIAN_POINT('Ctrl Pts',(-73.3989279832808,-8.77608731509303,
0.));
#83677=CARTESIAN_POINT('Ctrl Pts',(-73.422329507112,-8.78992762598738,0.));
#83678=CARTESIAN_POINT('Ctrl Pts',(-73.4457492173949,-8.80380752553714,
0.));
#83679=CARTESIAN_POINT('Ctrl Pts',(-73.4691870121608,-8.81772700927593,
0.));
#83680=CARTESIAN_POINT('Ctrl Pts',(-73.4926427882787,-8.83168607277414,
0.));
#83681=CARTESIAN_POINT('Ctrl Pts',(-73.5161164429765,-8.84568471153893,
0.));
#83682=CARTESIAN_POINT('Ctrl Pts',(-73.5396078751672,-8.85972292092182,
0.));
#83683=CARTESIAN_POINT('Ctrl Pts',(-73.5631169867113,-8.87380069602954,
0.));
#83684=CARTESIAN_POINT('Ctrl Pts',(-73.5866436840493,-8.8879180316034,0.));
#83685=CARTESIAN_POINT('Ctrl Pts',(-73.6101878785868,-8.90207492198871,
0.));
#83686=CARTESIAN_POINT('Ctrl Pts',(-73.6303847393444,-8.91424402151024,
0.));
#83687=CARTESIAN_POINT('Ctrl Pts',(-73.6458786305788,-8.92359518177555,
0.));
#83688=CARTESIAN_POINT('Ctrl Pts',(-73.6566618621797,-8.9301108881603,0.));
#83689=CARTESIAN_POINT('Ctrl Pts',(-73.6627293782263,-8.9337795596399,0.));
#83690=CARTESIAN_POINT('Ctrl Pts',(-73.6640787197672,-8.9345955465582,0.));
#83691=CARTESIAN_POINT('',(-69.6540253893192,-6.95102489306925,12.));
#83692=CARTESIAN_POINT('',(-69.6540253893192,-6.95102489306925,0.));
#83693=CARTESIAN_POINT('Ctrl Pts',(-73.6640787197672,-8.93459554655823,
12.));
#83694=CARTESIAN_POINT('Ctrl Pts',(-73.6627293782263,-8.93377955963992,
12.));
#83695=CARTESIAN_POINT('Ctrl Pts',(-73.6566618621798,-8.93011088816032,
12.));
#83696=CARTESIAN_POINT('Ctrl Pts',(-73.6458786305789,-8.92359518177556,
12.));
#83697=CARTESIAN_POINT('Ctrl Pts',(-73.6303847393445,-8.91424402151025,
12.));
#83698=CARTESIAN_POINT('Ctrl Pts',(-73.6101878785868,-8.90207492198871,
12.));
#83699=CARTESIAN_POINT('Ctrl Pts',(-73.5866436840493,-8.8879180316034,12.));
#83700=CARTESIAN_POINT('Ctrl Pts',(-73.5631169867113,-8.87380069602954,
12.));
#83701=CARTESIAN_POINT('Ctrl Pts',(-73.5396078751672,-8.85972292092182,
12.));
#83702=CARTESIAN_POINT('Ctrl Pts',(-73.5161164429765,-8.84568471153893,
12.));
#83703=CARTESIAN_POINT('Ctrl Pts',(-73.4926427882787,-8.83168607277414,
12.));
#83704=CARTESIAN_POINT('Ctrl Pts',(-73.4691870121608,-8.81772700927593,
12.));
#83705=CARTESIAN_POINT('Ctrl Pts',(-73.4457492173949,-8.80380752553714,
12.));
#83706=CARTESIAN_POINT('Ctrl Pts',(-73.422329507112,-8.78992762598738,12.));
#83707=CARTESIAN_POINT('Ctrl Pts',(-73.3989279832808,-8.77608731509303,
12.));
#83708=CARTESIAN_POINT('Ctrl Pts',(-73.3755447460235,-8.76228659740304,
12.));
#83709=CARTESIAN_POINT('Ctrl Pts',(-73.3521798944595,-8.74852547749736,
12.));
#83710=CARTESIAN_POINT('Ctrl Pts',(-73.3288335271989,-8.73480395995359,
12.));
#83711=CARTESIAN_POINT('Ctrl Pts',(-73.3055057429744,-8.72112204930232,
12.));
#83712=CARTESIAN_POINT('Ctrl Pts',(-73.282196641216,-8.70747974998244,12.));
#83713=CARTESIAN_POINT('Ctrl Pts',(-73.2589063226373,-8.69387706629304,
12.));
#83714=CARTESIAN_POINT('Ctrl Pts',(-73.2356348889704,-8.68031400241883,
12.));
#83715=CARTESIAN_POINT('Ctrl Pts',(-73.2123824427212,-8.66679056245095,
12.));
#83716=CARTESIAN_POINT('Ctrl Pts',(-73.1891490869057,-8.65330675040535,
12.));
#83717=CARTESIAN_POINT('Ctrl Pts',(-73.165934924813,-8.63986257023735,12.));
#83718=CARTESIAN_POINT('Ctrl Pts',(-73.142740059703,-8.62645802585474,12.));
#83719=CARTESIAN_POINT('Ctrl Pts',(-73.1195645948169,-8.61309312111988,
12.));
#83720=CARTESIAN_POINT('Ctrl Pts',(-73.0964086335226,-8.59976785984538,
12.));
#83721=CARTESIAN_POINT('Ctrl Pts',(-73.073272279419,-8.58648224578723,12.));
#83722=CARTESIAN_POINT('Ctrl Pts',(-73.0501556364482,-8.57323628263595,
12.));
#83723=CARTESIAN_POINT('Ctrl Pts',(-73.0270588090193,-8.56002997400096,
12.));
#83724=CARTESIAN_POINT('Ctrl Pts',(-73.0039819020663,-8.54686332340438,
12.));
#83725=CARTESIAN_POINT('Ctrl Pts',(-72.9809250209843,-8.53373633429303,
12.));
#83726=CARTESIAN_POINT('Ctrl Pts',(-72.9578882715923,-8.52064901004243,
12.));
#83727=CARTESIAN_POINT('Ctrl Pts',(-72.9348717600837,-8.50760135395979,
12.));
#83728=CARTESIAN_POINT('Ctrl Pts',(-72.9118755929785,-8.49459336928275,
12.));
#83729=CARTESIAN_POINT('Ctrl Pts',(-72.888899877077,-8.48162505917627,12.));
#83730=CARTESIAN_POINT('Ctrl Pts',(-72.8659447194918,-8.46869642673763,
12.));
#83731=CARTESIAN_POINT('Ctrl Pts',(-72.8430102276703,-8.4558074749977,12.));
#83732=CARTESIAN_POINT('Ctrl Pts',(-72.8200965094197,-8.44295820691906,
12.));
#83733=CARTESIAN_POINT('Ctrl Pts',(-72.7972036729283,-8.4301486253917,12.));
#83734=CARTESIAN_POINT('Ctrl Pts',(-72.7743318267876,-8.41737873322352,
12.));
#83735=CARTESIAN_POINT('Ctrl Pts',(-72.7514810799932,-8.40464853314493,
12.));
#83736=CARTESIAN_POINT('Ctrl Pts',(-72.728651541938,-8.39195802781406,12.));
#83737=CARTESIAN_POINT('Ctrl Pts',(-72.7058433224072,-8.37930721981734,
12.));
#83738=CARTESIAN_POINT('Ctrl Pts',(-72.68305653157,-8.36669611166833,12.));
#83739=CARTESIAN_POINT('Ctrl Pts',(-72.6602912799689,-8.35412470580083,
12.));
#83740=CARTESIAN_POINT('Ctrl Pts',(-72.6375476785208,-8.34159300456965,
12.));
#83741=CARTESIAN_POINT('Ctrl Pts',(-72.614825838529,-8.32910101025652,12.));
#83742=CARTESIAN_POINT('Ctrl Pts',(-72.5921258716899,-8.31664872507008,
12.));
#83743=CARTESIAN_POINT('Ctrl Pts',(-72.5694478900983,-8.30423615114455,
12.));
#83744=CARTESIAN_POINT('Ctrl Pts',(-72.5467920062522,-8.29186329053288,
12.));
#83745=CARTESIAN_POINT('Ctrl Pts',(-72.524158333056,-8.27953014520385,12.));
#83746=CARTESIAN_POINT('Ctrl Pts',(-72.501546983825,-8.26723671704923,12.));
#83747=CARTESIAN_POINT('Ctrl Pts',(-72.4789580722871,-8.25498300788493,
12.));
#83748=CARTESIAN_POINT('Ctrl Pts',(-72.4563917125842,-8.24276901945036,
12.));
#83749=CARTESIAN_POINT('Ctrl Pts',(-72.4338480192701,-8.23059475340354,
12.));
#83750=CARTESIAN_POINT('Ctrl Pts',(-72.4113271073091,-8.21846021131563,
12.));
#83751=CARTESIAN_POINT('Ctrl Pts',(-72.3888290920845,-8.20636539467781,
12.));
#83752=CARTESIAN_POINT('Ctrl Pts',(-72.3663540894034,-8.19431030490319,
12.));
#83753=CARTESIAN_POINT('Ctrl Pts',(-72.3439022155007,-8.18229494332622,
12.));
#83754=CARTESIAN_POINT('Ctrl Pts',(-72.3214735870402,-8.17031931119882,
12.));
#83755=CARTESIAN_POINT('Ctrl Pts',(-72.2990683211155,-8.15838340968327,
12.));
#83756=CARTESIAN_POINT('Ctrl Pts',(-72.2766865352552,-8.14648723985793,
12.));
#83757=CARTESIAN_POINT('Ctrl Pts',(-72.2543283474279,-8.13463080272029,
12.));
#83758=CARTESIAN_POINT('Ctrl Pts',(-72.2319938760451,-8.12281409918661,
12.));
#83759=CARTESIAN_POINT('Ctrl Pts',(-72.2096832399626,-8.11103713008922,
12.));
#83760=CARTESIAN_POINT('Ctrl Pts',(-72.18739655848,-8.09929989616873,12.));
#83761=CARTESIAN_POINT('Ctrl Pts',(-72.165133951346,-8.08760239807815,12.));
#83762=CARTESIAN_POINT('Ctrl Pts',(-72.1428955387648,-8.07594463638699,
12.));
#83763=CARTESIAN_POINT('Ctrl Pts',(-72.1206814413985,-8.06432661158089,
12.));
#83764=CARTESIAN_POINT('Ctrl Pts',(-72.0984917803702,-8.05274832405957,
12.));
#83765=CARTESIAN_POINT('Ctrl Pts',(-72.0763266772632,-8.04120977412891,
12.));
#83766=CARTESIAN_POINT('Ctrl Pts',(-72.0541862541262,-8.02971096200328,
12.));
#83767=CARTESIAN_POINT('Ctrl Pts',(-72.0320706334802,-8.0182518878107,12.));
#83768=CARTESIAN_POINT('Ctrl Pts',(-72.0099799383216,-8.0068325515925,12.));
#83769=CARTESIAN_POINT('Ctrl Pts',(-71.9879142921248,-7.99545295330182,
12.));
#83770=CARTESIAN_POINT('Ctrl Pts',(-71.9658738188421,-7.98411309279597,
12.));
#83771=CARTESIAN_POINT('Ctrl Pts',(-71.9438586429072,-7.97281296983702,
12.));
#83772=CARTESIAN_POINT('Ctrl Pts',(-71.9218688892426,-7.96155258409751,
12.));
#83773=CARTESIAN_POINT('Ctrl Pts',(-71.8999046832642,-7.95033193516046,
12.));
#83774=CARTESIAN_POINT('Ctrl Pts',(-71.8779661508833,-7.93915102251796,
12.));
#83775=CARTESIAN_POINT('Ctrl Pts',(-71.8560534185071,-7.928009845564,12.));
#83776=CARTESIAN_POINT('Ctrl Pts',(-71.8341666130424,-7.9169084035937,12.));
#83777=CARTESIAN_POINT('Ctrl Pts',(-71.8123058619038,-7.90584669580955,
12.));
#83778=CARTESIAN_POINT('Ctrl Pts',(-71.7904712930172,-7.89482472132135,
12.));
#83779=CARTESIAN_POINT('Ctrl Pts',(-71.768663034824,-7.88384247914521,12.));
#83780=CARTESIAN_POINT('Ctrl Pts',(-71.7468812162795,-7.87289996819654,
12.));
#83781=CARTESIAN_POINT('Ctrl Pts',(-71.7251259668573,-7.86199718728829,
12.));
#83782=CARTESIAN_POINT('Ctrl Pts',(-71.7033974165576,-7.85113413513739,
12.));
#83783=CARTESIAN_POINT('Ctrl Pts',(-71.681695695912,-7.84031081036488,12.));
#83784=CARTESIAN_POINT('Ctrl Pts',(-71.6600209359869,-7.82952721149504,
12.));
#83785=CARTESIAN_POINT('Ctrl Pts',(-71.638373268384,-7.81878333694856,12.));
#83786=CARTESIAN_POINT('Ctrl Pts',(-71.616752825242,-7.80807918504017,12.));
#83787=CARTESIAN_POINT('Ctrl Pts',(-71.5951597392471,-7.79741475398511,
12.));
#83788=CARTESIAN_POINT('Ctrl Pts',(-71.5735941436366,-7.78679004189935,
12.));
#83789=CARTESIAN_POINT('Ctrl Pts',(-71.5520561722039,-7.77620504679868,
12.));
#83790=CARTESIAN_POINT('Ctrl Pts',(-71.5305459592987,-7.76565976659218,
12.));
#83791=CARTESIAN_POINT('Ctrl Pts',(-71.5090636398307,-7.75515419907955,
12.));
#83792=CARTESIAN_POINT('Ctrl Pts',(-71.487609349277,-7.74468834195734,12.));
#83793=CARTESIAN_POINT('Ctrl Pts',(-71.4661832236881,-7.73426219281931,
12.));
#83794=CARTESIAN_POINT('Ctrl Pts',(-71.4447853996919,-7.72387574915544,
12.));
#83795=CARTESIAN_POINT('Ctrl Pts',(-71.4234160144943,-7.71352900834537,
12.));
#83796=CARTESIAN_POINT('Ctrl Pts',(-71.4020752058827,-7.70322196765572,
12.));
#83797=CARTESIAN_POINT('Ctrl Pts',(-71.380763112236,-7.69295462424647,12.));
#83798=CARTESIAN_POINT('Ctrl Pts',(-71.3594798725294,-7.68272697517103,
12.));
#83799=CARTESIAN_POINT('Ctrl Pts',(-71.3382256263405,-7.67253901737539,
12.));
#83800=CARTESIAN_POINT('Ctrl Pts',(-71.3170005138474,-7.66239074769119,
12.));
#83801=CARTESIAN_POINT('Ctrl Pts',(-71.2958046758334,-7.65228216283342,
12.));
#83802=CARTESIAN_POINT('Ctrl Pts',(-71.2746382536974,-7.64221325940671,
12.));
#83803=CARTESIAN_POINT('Ctrl Pts',(-71.2535013894587,-7.63218403390514,
12.));
#83804=CARTESIAN_POINT('Ctrl Pts',(-71.232394225762,-7.62219448271124,12.));
#83805=CARTESIAN_POINT('Ctrl Pts',(-71.2113169058778,-7.61224460208886,
12.));
#83806=CARTESIAN_POINT('Ctrl Pts',(-71.1902695737063,-7.60233438818156,
12.));
#83807=CARTESIAN_POINT('Ctrl Pts',(-71.1692523737887,-7.5924638370186,12.));
#83808=CARTESIAN_POINT('Ctrl Pts',(-71.1482654513133,-7.58263294451465,
12.));
#83809=CARTESIAN_POINT('Ctrl Pts',(-71.1273089521218,-7.57284170646866,
12.));
#83810=CARTESIAN_POINT('Ctrl Pts',(-71.1063830227074,-7.56309011855616,
12.));
#83811=CARTESIAN_POINT('Ctrl Pts',(-71.0854878102203,-7.55337817632872,
12.));
#83812=CARTESIAN_POINT('Ctrl Pts',(-71.0646234624783,-7.54370587521948,
12.));
#83813=CARTESIAN_POINT('Ctrl Pts',(-71.0437901279722,-7.53407321054253,
12.));
#83814=CARTESIAN_POINT('Ctrl Pts',(-71.0229879558713,-7.52448017749136,
12.));
#83815=CARTESIAN_POINT('Ctrl Pts',(-71.0022170960235,-7.51492677113111,
12.));
#83816=CARTESIAN_POINT('Ctrl Pts',(-70.9814776989637,-7.50541298639948,
12.));
#83817=CARTESIAN_POINT('Ctrl Pts',(-70.9607699159234,-7.49593881811141,
12.));
#83818=CARTESIAN_POINT('Ctrl Pts',(-70.9400938988373,-7.48650426095823,
12.));
#83819=CARTESIAN_POINT('Ctrl Pts',(-70.9194498003483,-7.47710930950554,
12.));
#83820=CARTESIAN_POINT('Ctrl Pts',(-70.8988377738088,-7.46775395818518,
12.));
#83821=CARTESIAN_POINT('Ctrl Pts',(-70.8782579732885,-7.45843820129776,
12.));
#83822=CARTESIAN_POINT('Ctrl Pts',(-70.8577105535841,-7.44916203301645,
12.));
#83823=CARTESIAN_POINT('Ctrl Pts',(-70.8371956702242,-7.43992544738606,
12.));
#83824=CARTESIAN_POINT('Ctrl Pts',(-70.8167134794738,-7.43072843832008,
12.));
#83825=CARTESIAN_POINT('Ctrl Pts',(-70.7962641383351,-7.42157099959316,
12.));
#83826=CARTESIAN_POINT('Ctrl Pts',(-70.7758478045576,-7.41245312484487,
12.));
#83827=CARTESIAN_POINT('Ctrl Pts',(-70.7554646366514,-7.4033748075823,12.));
#83828=CARTESIAN_POINT('Ctrl Pts',(-70.735114793895,-7.3943360411789,12.));
#83829=CARTESIAN_POINT('Ctrl Pts',(-70.7147984363424,-7.38533681887032,
12.));
#83830=CARTESIAN_POINT('Ctrl Pts',(-70.694515724827,-7.37637713374767,12.));
#83831=CARTESIAN_POINT('Ctrl Pts',(-70.6742668209687,-7.367456978763,12.));
#83832=CARTESIAN_POINT('Ctrl Pts',(-70.6540518871775,-7.35857634673054,
12.));
#83833=CARTESIAN_POINT('Ctrl Pts',(-70.6338710866562,-7.34973523032577,
12.));
#83834=CARTESIAN_POINT('Ctrl Pts',(-70.6137245833996,-7.34093362208007,
12.));
#83835=CARTESIAN_POINT('Ctrl Pts',(-70.5936125421946,-7.3321715143759,12.));
#83836=CARTESIAN_POINT('Ctrl Pts',(-70.5735351286476,-7.32344889945219,
12.));
#83837=CARTESIAN_POINT('Ctrl Pts',(-70.5534925092043,-7.31476576940391,
12.));
#83838=CARTESIAN_POINT('Ctrl Pts',(-70.5334848511681,-7.30612211618053,
12.));
#83839=CARTESIAN_POINT('Ctrl Pts',(-70.5135123227169,-7.29751793157822,
12.));
#83840=CARTESIAN_POINT('Ctrl Pts',(-70.4935750929058,-7.28895320723862,
12.));
#83841=CARTESIAN_POINT('Ctrl Pts',(-70.4736733316487,-7.2804279346547,12.));
#83842=CARTESIAN_POINT('Ctrl Pts',(-70.4538072096992,-7.27194210517062,
12.));
#83843=CARTESIAN_POINT('Ctrl Pts',(-70.4339768986346,-7.26349570998032,
12.));
#83844=CARTESIAN_POINT('Ctrl Pts',(-70.4141825708178,-7.25508874012043,
12.));
#83845=CARTESIAN_POINT('Ctrl Pts',(-70.3944243994504,-7.24672118647084,
12.));
#83846=CARTESIAN_POINT('Ctrl Pts',(-70.3747025586552,-7.23839303975606,
12.));
#83847=CARTESIAN_POINT('Ctrl Pts',(-70.3550172235486,-7.23010429054229,
12.));
#83848=CARTESIAN_POINT('Ctrl Pts',(-70.3353685703112,-7.22185492923191,
12.));
#83849=CARTESIAN_POINT('Ctrl Pts',(-70.3157567762588,-7.21364494605449,
12.));
#83850=CARTESIAN_POINT('Ctrl Pts',(-70.2961820197077,-7.20547433107482,
12.));
#83851=CARTESIAN_POINT('Ctrl Pts',(-70.2766444798285,-7.19734307419873,
12.));
#83852=CARTESIAN_POINT('Ctrl Pts',(-70.2571443365192,-7.18925116517555,
12.));
#83853=CARTESIAN_POINT('Ctrl Pts',(-70.2376817702215,-7.18119859359777,
12.));
#83854=CARTESIAN_POINT('Ctrl Pts',(-70.2182569618994,-7.17318534889715,
12.));
#83855=CARTESIAN_POINT('Ctrl Pts',(-70.1988700934593,-7.16521142033863,
12.));
#83856=CARTESIAN_POINT('Ctrl Pts',(-70.1795213481185,-7.15727679700933,
12.));
#83857=CARTESIAN_POINT('Ctrl Pts',(-70.1602109107202,-7.14938146780813,
12.));
#83858=CARTESIAN_POINT('Ctrl Pts',(-70.1409389682424,-7.14152542142373,
12.));
#83859=CARTESIAN_POINT('Ctrl Pts',(-70.1217057094499,-7.13370864634442,
12.));
#83860=CARTESIAN_POINT('Ctrl Pts',(-70.1025113239495,-7.12593113088903,
12.));
#83861=CARTESIAN_POINT('Ctrl Pts',(-70.0833560013975,-7.11819286322826,
12.));
#83862=CARTESIAN_POINT('Ctrl Pts',(-70.0642399306869,-7.11049383140445,
12.));
#83863=CARTESIAN_POINT('Ctrl Pts',(-70.0451632990086,-7.10283402335034,
12.));
#83864=CARTESIAN_POINT('Ctrl Pts',(-70.0261262936388,-7.09521342684248,
12.));
#83865=CARTESIAN_POINT('Ctrl Pts',(-70.0071291040766,-7.08763202944246,
12.));
#83866=CARTESIAN_POINT('Ctrl Pts',(-69.988171923788,-7.08008981844652,12.));
#83867=CARTESIAN_POINT('Ctrl Pts',(-69.9692549527296,-7.07258678080831,
12.));
#83868=CARTESIAN_POINT('Ctrl Pts',(-69.9503783975727,-7.06512290312849,
12.));
#83869=CARTESIAN_POINT('Ctrl Pts',(-69.9315424664291,-7.05769817180857,
12.));
#83870=CARTESIAN_POINT('Ctrl Pts',(-69.9127473642099,-7.05031257318115,
12.));
#83871=CARTESIAN_POINT('Ctrl Pts',(-69.8939932885841,-7.04296609362165,
12.));
#83872=CARTESIAN_POINT('Ctrl Pts',(-69.8752804235238,-7.03565871972221,
12.));
#83873=CARTESIAN_POINT('Ctrl Pts',(-69.8566089455375,-7.02839043811812,
12.));
#83874=CARTESIAN_POINT('Ctrl Pts',(-69.8379790360518,-7.02116123514451,
12.));
#83875=CARTESIAN_POINT('Ctrl Pts',(-69.8193908913722,-7.01397109655454,
12.));
#83876=CARTESIAN_POINT('Ctrl Pts',(-69.8008447346863,-7.0068200071815,12.));
#83877=CARTESIAN_POINT('Ctrl Pts',(-69.782340824259,-6.99970795069476,12.));
#83878=CARTESIAN_POINT('Ctrl Pts',(-69.7638794280419,-6.9926349102794,12.));
#83879=CARTESIAN_POINT('Ctrl Pts',(-69.7454607995607,-6.98560086924214,
12.));
#83880=CARTESIAN_POINT('Ctrl Pts',(-69.7270851557366,-6.97860581164527,
12.));
#83881=CARTESIAN_POINT('Ctrl Pts',(-69.7087526479973,-6.97164972291439,
12.));
#83882=CARTESIAN_POINT('Ctrl Pts',(-69.6904633605421,-6.96473259049513,
12.));
#83883=CARTESIAN_POINT('Ctrl Pts',(-69.6758665380378,-6.95923004173591,
12.));
#83884=CARTESIAN_POINT('Ctrl Pts',(-69.664938391983,-6.95512065317599,12.));
#83885=CARTESIAN_POINT('Ctrl Pts',(-69.6576616146467,-6.95238884849025,
12.));
#83886=CARTESIAN_POINT('Ctrl Pts',(-69.6540253893192,-6.95102489306925,
12.));
#83887=CARTESIAN_POINT('Ctrl Pts',(-73.4664795929942,-10.4355099267295,
-5.55111512312578E-16));
#83888=CARTESIAN_POINT('Ctrl Pts',(-73.4664795929942,-10.4355099267295,
4.));
#83889=CARTESIAN_POINT('Ctrl Pts',(-73.4664795929942,-10.4355099267295,
8.));
#83890=CARTESIAN_POINT('Ctrl Pts',(-73.4664795929942,-10.4355099267295,
12.));
#83891=CARTESIAN_POINT('Ctrl Pts',(-73.572019020007,-10.4049225807074,-5.55111512312578E-16));
#83892=CARTESIAN_POINT('Ctrl Pts',(-73.572019020007,-10.4049225807074,4.));
#83893=CARTESIAN_POINT('Ctrl Pts',(-73.572019020007,-10.4049225807074,8.00000000000001));
#83894=CARTESIAN_POINT('Ctrl Pts',(-73.572019020007,-10.4049225807074,12.));
#83895=CARTESIAN_POINT('Ctrl Pts',(-73.7377969500798,-10.2883434191781,
-5.55111512312578E-16));
#83896=CARTESIAN_POINT('Ctrl Pts',(-73.7377969500798,-10.2883434191781,
4.));
#83897=CARTESIAN_POINT('Ctrl Pts',(-73.7377969500798,-10.2883434191781,
7.99999999999999));
#83898=CARTESIAN_POINT('Ctrl Pts',(-73.7377969500798,-10.2883434191781,
12.));
#83899=CARTESIAN_POINT('Ctrl Pts',(-73.8116652760545,-10.1042001607578,
-5.55111512312578E-16));
#83900=CARTESIAN_POINT('Ctrl Pts',(-73.8116652760545,-10.1042001607578,
4.));
#83901=CARTESIAN_POINT('Ctrl Pts',(-73.8116652760545,-10.1042001607578,
8.00000000000001));
#83902=CARTESIAN_POINT('Ctrl Pts',(-73.8116652760545,-10.1042001607578,
12.));
#83903=CARTESIAN_POINT('Ctrl Pts',(-73.8227522002494,-10.0225374821233,
-5.55111512312578E-16));
#83904=CARTESIAN_POINT('Ctrl Pts',(-73.8227522002494,-10.0225374821233,
4.));
#83905=CARTESIAN_POINT('Ctrl Pts',(-73.8227522002494,-10.0225374821233,
8.));
#83906=CARTESIAN_POINT('Ctrl Pts',(-73.8227522002494,-10.0225374821233,
12.));
#83907=CARTESIAN_POINT('',(-73.4664795929942,-10.4355099267295,2.77555756156289E-16));
#83908=CARTESIAN_POINT('',(-73.8227522002494,-10.0225374821234,0.));
#83909=CARTESIAN_POINT('Ctrl Pts',(-73.4664795929942,-10.4355099267295,
4.16333634234434E-16));
#83910=CARTESIAN_POINT('Ctrl Pts',(-73.572019020007,-10.4049225807074,4.16333634234433E-16));
#83911=CARTESIAN_POINT('Ctrl Pts',(-73.6667492657629,-10.3383059169764,
4.16333634234434E-16));
#83912=CARTESIAN_POINT('Ctrl Pts',(-73.7314682122214,-10.2496275073218,
4.16333634234434E-16));
#83913=CARTESIAN_POINT('Ctrl Pts',(-73.7800074220654,-10.1831187000808,
4.16333634234434E-16));
#83914=CARTESIAN_POINT('Ctrl Pts',(-73.8116652760545,-10.1042001607578,
4.16333634234433E-16));
#83915=CARTESIAN_POINT('Ctrl Pts',(-73.8227522002494,-10.0225374821233,
4.16333634234434E-16));
#83916=CARTESIAN_POINT('',(-73.8227522002494,-10.0225374821234,12.));
#83917=CARTESIAN_POINT('Ctrl Pts',(-73.8227522002494,-10.0225374821233,
-5.55111512312578E-16));
#83918=CARTESIAN_POINT('Ctrl Pts',(-73.8227522002494,-10.0225374821233,
4.));
#83919=CARTESIAN_POINT('Ctrl Pts',(-73.8227522002494,-10.0225374821233,
8.));
#83920=CARTESIAN_POINT('Ctrl Pts',(-73.8227522002494,-10.0225374821233,
12.));
#83921=CARTESIAN_POINT('',(-73.4664795929942,-10.4355099267295,12.));
#83922=CARTESIAN_POINT('Ctrl Pts',(-73.8227522002494,-10.0225374821233,
12.));
#83923=CARTESIAN_POINT('Ctrl Pts',(-73.8116652760545,-10.1042001607578,
12.));
#83924=CARTESIAN_POINT('Ctrl Pts',(-73.7800074220654,-10.1831187000808,
12.));
#83925=CARTESIAN_POINT('Ctrl Pts',(-73.7314682122214,-10.2496275073218,
12.));
#83926=CARTESIAN_POINT('Ctrl Pts',(-73.6667492657629,-10.3383059169764,
12.));
#83927=CARTESIAN_POINT('Ctrl Pts',(-73.572019020007,-10.4049225807074,12.));
#83928=CARTESIAN_POINT('Ctrl Pts',(-73.4664795929942,-10.4355099267295,
12.));
#83929=CARTESIAN_POINT('Ctrl Pts',(-73.4664795929942,-10.4355099267295,
12.));
#83930=CARTESIAN_POINT('Ctrl Pts',(-73.4664795929942,-10.4355099267295,
8.));
#83931=CARTESIAN_POINT('Ctrl Pts',(-73.4664795929942,-10.4355099267295,
4.));
#83932=CARTESIAN_POINT('Ctrl Pts',(-73.4664795929942,-10.4355099267295,
-5.55111512312578E-16));
#83933=CARTESIAN_POINT('Origin',(-3.71623968689858E-10,-4.90253386731613E-11,
0.));
#83934=CARTESIAN_POINT('Origin',(-3.71623968689858E-10,-4.90253386731613E-11,
12.));
#83935=CARTESIAN_POINT('Origin',(-3.71623968689858E-10,-4.90253386731613E-11,
0.));
#83936=CARTESIAN_POINT('Ctrl Pts',(-74.4416140848738,-2.94891377268286,
0.));
#83937=CARTESIAN_POINT('Ctrl Pts',(-74.4416140848738,-2.94891377268286,
4.));
#83938=CARTESIAN_POINT('Ctrl Pts',(-74.4416140848738,-2.94891377268283,
8.));
#83939=CARTESIAN_POINT('Ctrl Pts',(-74.4416140848738,-2.94891377268283,
12.));
#83940=CARTESIAN_POINT('Ctrl Pts',(-74.4459635334396,-2.83911742169655,
0.));
#83941=CARTESIAN_POINT('Ctrl Pts',(-74.4459635334396,-2.83911742169655,
4.));
#83942=CARTESIAN_POINT('Ctrl Pts',(-74.4459635334396,-2.83911742169652,
8.00000000000001));
#83943=CARTESIAN_POINT('Ctrl Pts',(-74.4459635334396,-2.83911742169652,
12.));
#83944=CARTESIAN_POINT('Ctrl Pts',(-74.3877786926473,-2.64498412359339,
0.));
#83945=CARTESIAN_POINT('Ctrl Pts',(-74.3877786926473,-2.64498412359339,
4.));
#83946=CARTESIAN_POINT('Ctrl Pts',(-74.3877786926473,-2.64498412359335,
7.99999999999999));
#83947=CARTESIAN_POINT('Ctrl Pts',(-74.3877786926473,-2.64498412359335,
12.));
#83948=CARTESIAN_POINT('Ctrl Pts',(-74.2364344282703,-2.51668625693784,
0.));
#83949=CARTESIAN_POINT('Ctrl Pts',(-74.2364344282703,-2.51668625693784,
4.));
#83950=CARTESIAN_POINT('Ctrl Pts',(-74.2364344282703,-2.51668625693778,
8.00000000000001));
#83951=CARTESIAN_POINT('Ctrl Pts',(-74.2364344282703,-2.51668625693778,
12.));
#83952=CARTESIAN_POINT('Ctrl Pts',(-74.1624659714557,-2.48034921843197,
0.));
#83953=CARTESIAN_POINT('Ctrl Pts',(-74.1624659714557,-2.48034921843197,
4.));
#83954=CARTESIAN_POINT('Ctrl Pts',(-74.1624659714557,-2.48034921843191,
8.));
#83955=CARTESIAN_POINT('Ctrl Pts',(-74.1624659714557,-2.48034921843191,
12.));
#83956=CARTESIAN_POINT('',(-74.4416140848738,-2.94891377268286,0.));
#83957=CARTESIAN_POINT('',(-74.1624659714555,-2.48034921843229,0.));
#83958=CARTESIAN_POINT('Ctrl Pts',(-74.4416140848738,-2.94891377268286,
0.));
#83959=CARTESIAN_POINT('Ctrl Pts',(-74.4459635334396,-2.83911742169655,
0.));
#83960=CARTESIAN_POINT('Ctrl Pts',(-74.4127150529868,-2.72818410849474,
0.));
#83961=CARTESIAN_POINT('Ctrl Pts',(-74.3490471689146,-2.63874807903093,
0.));
#83962=CARTESIAN_POINT('Ctrl Pts',(-74.3012962558604,-2.57167105693308,
0.));
#83963=CARTESIAN_POINT('Ctrl Pts',(-74.2364344282703,-2.51668625693784,
0.));
#83964=CARTESIAN_POINT('Ctrl Pts',(-74.1624659714557,-2.48034921843197,
0.));
#83965=CARTESIAN_POINT('',(-74.1624659714555,-2.48034921843228,12.));
#83966=CARTESIAN_POINT('Ctrl Pts',(-74.1624659714557,-2.48034921843197,
0.));
#83967=CARTESIAN_POINT('Ctrl Pts',(-74.1624659714557,-2.48034921843197,
4.));
#83968=CARTESIAN_POINT('Ctrl Pts',(-74.1624659714557,-2.48034921843191,
8.));
#83969=CARTESIAN_POINT('Ctrl Pts',(-74.1624659714557,-2.48034921843191,
12.));
#83970=CARTESIAN_POINT('',(-74.4416140848738,-2.94891377268283,12.));
#83971=CARTESIAN_POINT('Ctrl Pts',(-74.1624659714557,-2.48034921843191,
12.));
#83972=CARTESIAN_POINT('Ctrl Pts',(-74.2364344282703,-2.51668625693778,
12.));
#83973=CARTESIAN_POINT('Ctrl Pts',(-74.3012962558604,-2.57167105693303,
12.));
#83974=CARTESIAN_POINT('Ctrl Pts',(-74.3490471689146,-2.63874807903089,
12.));
#83975=CARTESIAN_POINT('Ctrl Pts',(-74.4127150529868,-2.72818410849471,
12.));
#83976=CARTESIAN_POINT('Ctrl Pts',(-74.4459635334396,-2.83911742169652,
12.));
#83977=CARTESIAN_POINT('Ctrl Pts',(-74.4416140848738,-2.94891377268283,
12.));
#83978=CARTESIAN_POINT('Ctrl Pts',(-74.4416140848738,-2.94891377268283,
12.));
#83979=CARTESIAN_POINT('Ctrl Pts',(-74.4416140848738,-2.94891377268283,
8.));
#83980=CARTESIAN_POINT('Ctrl Pts',(-74.4416140848738,-2.94891377268286,
4.));
#83981=CARTESIAN_POINT('Ctrl Pts',(-74.4416140848738,-2.94891377268286,
0.));
#83982=CARTESIAN_POINT('Ctrl Pts',(-69.9947925310006,-0.85382582660898,
0.));
#83983=CARTESIAN_POINT('Ctrl Pts',(-69.9947925310006,-0.85382582660898,
12.));
#83984=CARTESIAN_POINT('Ctrl Pts',(-69.9985337959407,-0.854867673848592,
0.));
#83985=CARTESIAN_POINT('Ctrl Pts',(-69.9985337959407,-0.854867673848592,
12.));
#83986=CARTESIAN_POINT('Ctrl Pts',(-70.0060209754087,-0.856954870259201,
0.));
#83987=CARTESIAN_POINT('Ctrl Pts',(-70.0060209754087,-0.856954870259201,
12.));
#83988=CARTESIAN_POINT('Ctrl Pts',(-70.0172656933806,-0.860096170668732,
0.));
#83989=CARTESIAN_POINT('Ctrl Pts',(-70.0172656933806,-0.860096170668732,
12.));
#83990=CARTESIAN_POINT('Ctrl Pts',(-70.0322865492925,-0.864305583661541,
0.));
#83991=CARTESIAN_POINT('Ctrl Pts',(-70.0322865492925,-0.864305583661541,
12.));
#83992=CARTESIAN_POINT('Ctrl Pts',(-70.051109108301,-0.86960237787112,0.));
#83993=CARTESIAN_POINT('Ctrl Pts',(-70.051109108301,-0.86960237787112,12.));
#83994=CARTESIAN_POINT('Ctrl Pts',(-70.0699781183935,-0.874934213255836,
0.));
#83995=CARTESIAN_POINT('Ctrl Pts',(-70.0699781183935,-0.874934213255836,
12.));
#83996=CARTESIAN_POINT('Ctrl Pts',(-70.0888934967855,-0.880301109660725,
0.));
#83997=CARTESIAN_POINT('Ctrl Pts',(-70.0888934967855,-0.880301109660725,
12.));
#83998=CARTESIAN_POINT('Ctrl Pts',(-70.1078550938958,-0.885703094802532,
0.));
#83999=CARTESIAN_POINT('Ctrl Pts',(-70.1078550938958,-0.885703094802532,
12.));
#84000=CARTESIAN_POINT('Ctrl Pts',(-70.1268626950175,-0.891140203464239,
0.));
#84001=CARTESIAN_POINT('Ctrl Pts',(-70.1268626950175,-0.891140203464239,
12.));
#84002=CARTESIAN_POINT('Ctrl Pts',(-70.1459160490446,-0.89661247437184,
0.));
#84003=CARTESIAN_POINT('Ctrl Pts',(-70.1459160490446,-0.89661247437184,
12.));
#84004=CARTESIAN_POINT('Ctrl Pts',(-70.1650148905109,-0.902119947629767,
0.));
#84005=CARTESIAN_POINT('Ctrl Pts',(-70.1650148905109,-0.902119947629767,
12.));
#84006=CARTESIAN_POINT('Ctrl Pts',(-70.1841589635574,-0.907662662015781,
0.));
#84007=CARTESIAN_POINT('Ctrl Pts',(-70.1841589635574,-0.907662662015781,
12.));
#84008=CARTESIAN_POINT('Ctrl Pts',(-70.2033480471676,-0.913240652090975,
0.));
#84009=CARTESIAN_POINT('Ctrl Pts',(-70.2033480471676,-0.913240652090975,
12.));
#84010=CARTESIAN_POINT('Ctrl Pts',(-70.2225819470248,-0.918853949157115,
0.));
#84011=CARTESIAN_POINT('Ctrl Pts',(-70.2225819470248,-0.918853949157115,
12.));
#84012=CARTESIAN_POINT('Ctrl Pts',(-70.2418604835837,-0.924502582639452,
0.));
#84013=CARTESIAN_POINT('Ctrl Pts',(-70.2418604835837,-0.924502582639452,
12.));
#84014=CARTESIAN_POINT('Ctrl Pts',(-70.2611834821724,-0.930186581235545,
0.));
#84015=CARTESIAN_POINT('Ctrl Pts',(-70.2611834821724,-0.930186581235545,
12.));
#84016=CARTESIAN_POINT('Ctrl Pts',(-70.2805507606872,-0.935905974336476,
0.));
#84017=CARTESIAN_POINT('Ctrl Pts',(-70.2805507606872,-0.935905974336476,
12.));
#84018=CARTESIAN_POINT('Ctrl Pts',(-70.299962123399,-0.941660792742975,
0.));
#84019=CARTESIAN_POINT('Ctrl Pts',(-70.299962123399,-0.941660792742975,
12.));
#84020=CARTESIAN_POINT('Ctrl Pts',(-70.3194173673674,-0.9474510679296,0.));
#84021=CARTESIAN_POINT('Ctrl Pts',(-70.3194173673674,-0.9474510679296,12.));
#84022=CARTESIAN_POINT('Ctrl Pts',(-70.338916286458,-0.953276831581238,
0.));
#84023=CARTESIAN_POINT('Ctrl Pts',(-70.338916286458,-0.953276831581238,
12.));
#84024=CARTESIAN_POINT('Ctrl Pts',(-70.3584586759536,-0.959138115058827,
0.));
#84025=CARTESIAN_POINT('Ctrl Pts',(-70.3584586759536,-0.959138115058827,
12.));
#84026=CARTESIAN_POINT('Ctrl Pts',(-70.3780443377956,-0.965034948786444,
0.));
#84027=CARTESIAN_POINT('Ctrl Pts',(-70.3780443377956,-0.965034948786444,
12.));
#84028=CARTESIAN_POINT('Ctrl Pts',(-70.3976730803614,-0.970967362281171,
0.));
#84029=CARTESIAN_POINT('Ctrl Pts',(-70.3976730803614,-0.970967362281171,
12.));
#84030=CARTESIAN_POINT('Ctrl Pts',(-70.417344715957,-0.976935384450037,
0.));
#84031=CARTESIAN_POINT('Ctrl Pts',(-70.417344715957,-0.976935384450037,
12.));
#84032=CARTESIAN_POINT('Ctrl Pts',(-70.4370590590842,-0.982939043792151,
0.));
#84033=CARTESIAN_POINT('Ctrl Pts',(-70.4370590590842,-0.982939043792151,
12.));
#84034=CARTESIAN_POINT('Ctrl Pts',(-70.4568159243163,-0.988978368643646,
0.));
#84035=CARTESIAN_POINT('Ctrl Pts',(-70.4568159243163,-0.988978368643646,
12.));
#84036=CARTESIAN_POINT('Ctrl Pts',(-70.4766151245212,-0.995053387379752,
0.));
#84037=CARTESIAN_POINT('Ctrl Pts',(-70.4766151245212,-0.995053387379752,
12.));
#84038=CARTESIAN_POINT('Ctrl Pts',(-70.4964564717953,-1.00116412831442,
0.));
#84039=CARTESIAN_POINT('Ctrl Pts',(-70.4964564717953,-1.00116412831442,
12.));
#84040=CARTESIAN_POINT('Ctrl Pts',(-70.5163397782713,-1.00731061960968,
0.));
#84041=CARTESIAN_POINT('Ctrl Pts',(-70.5163397782713,-1.00731061960968,
12.));
#84042=CARTESIAN_POINT('Ctrl Pts',(-70.5362648569061,-1.01349288918537,
0.));
#84043=CARTESIAN_POINT('Ctrl Pts',(-70.5362648569061,-1.01349288918537,
12.));
#84044=CARTESIAN_POINT('Ctrl Pts',(-70.556231522419,-1.01971096460597,0.));
#84045=CARTESIAN_POINT('Ctrl Pts',(-70.556231522419,-1.01971096460597,12.));
#84046=CARTESIAN_POINT('Ctrl Pts',(-70.5762395916377,-1.02596487304048,
0.));
#84047=CARTESIAN_POINT('Ctrl Pts',(-70.5762395916377,-1.02596487304048,
12.));
#84048=CARTESIAN_POINT('Ctrl Pts',(-70.5962888829934,-1.0322546413287,0.));
#84049=CARTESIAN_POINT('Ctrl Pts',(-70.5962888829934,-1.0322546413287,12.));
#84050=CARTESIAN_POINT('Ctrl Pts',(-70.6163792162073,-1.03858029601903,
0.));
#84051=CARTESIAN_POINT('Ctrl Pts',(-70.6163792162073,-1.03858029601903,
12.));
#84052=CARTESIAN_POINT('Ctrl Pts',(-70.6365104119252,-1.04494186341156,
0.));
#84053=CARTESIAN_POINT('Ctrl Pts',(-70.6365104119252,-1.04494186341156,
12.));
#84054=CARTESIAN_POINT('Ctrl Pts',(-70.6566822912991,-1.05133936960071,
0.));
#84055=CARTESIAN_POINT('Ctrl Pts',(-70.6566822912991,-1.05133936960071,
12.));
#84056=CARTESIAN_POINT('Ctrl Pts',(-70.676894676009,-1.0577728404773,0.));
#84057=CARTESIAN_POINT('Ctrl Pts',(-70.676894676009,-1.0577728404773,12.));
#84058=CARTESIAN_POINT('Ctrl Pts',(-70.6971473884459,-1.0642423017128,0.));
#84059=CARTESIAN_POINT('Ctrl Pts',(-70.6971473884459,-1.0642423017128,12.));
#84060=CARTESIAN_POINT('Ctrl Pts',(-70.7174402518378,-1.07074777874595,
0.));
#84061=CARTESIAN_POINT('Ctrl Pts',(-70.7174402518378,-1.07074777874595,
12.));
#84062=CARTESIAN_POINT('Ctrl Pts',(-70.7377730903953,-1.07728929676408,
0.));
#84063=CARTESIAN_POINT('Ctrl Pts',(-70.7377730903953,-1.07728929676408,
12.));
#84064=CARTESIAN_POINT('Ctrl Pts',(-70.7581457294447,-1.08386688068342,
0.));
#84065=CARTESIAN_POINT('Ctrl Pts',(-70.7581457294447,-1.08386688068342,
12.));
#84066=CARTESIAN_POINT('Ctrl Pts',(-70.7785579953583,-1.09048055516426,
0.));
#84067=CARTESIAN_POINT('Ctrl Pts',(-70.7785579953583,-1.09048055516426,
12.));
#84068=CARTESIAN_POINT('Ctrl Pts',(-70.799009715484,-1.09713034462265,0.));
#84069=CARTESIAN_POINT('Ctrl Pts',(-70.799009715484,-1.09713034462265,12.));
#84070=CARTESIAN_POINT('Ctrl Pts',(-70.8195007180745,-1.10381627323946,
0.));
#84071=CARTESIAN_POINT('Ctrl Pts',(-70.8195007180745,-1.10381627323946,
12.));
#84072=CARTESIAN_POINT('Ctrl Pts',(-70.8400308322037,-1.11053836496639,
0.));
#84073=CARTESIAN_POINT('Ctrl Pts',(-70.8400308322037,-1.11053836496639,
12.));
#84074=CARTESIAN_POINT('Ctrl Pts',(-70.8605998877149,-1.11729664352992,
0.));
#84075=CARTESIAN_POINT('Ctrl Pts',(-70.8605998877149,-1.11729664352992,
12.));
#84076=CARTESIAN_POINT('Ctrl Pts',(-70.8812077152586,-1.12409113243513,
0.));
#84077=CARTESIAN_POINT('Ctrl Pts',(-70.8812077152586,-1.12409113243513,
12.));
#84078=CARTESIAN_POINT('Ctrl Pts',(-70.9018541463089,-1.13092185496564,
0.));
#84079=CARTESIAN_POINT('Ctrl Pts',(-70.9018541463089,-1.13092185496564,
12.));
#84080=CARTESIAN_POINT('Ctrl Pts',(-70.9225390131826,-1.13778883418213,
0.));
#84081=CARTESIAN_POINT('Ctrl Pts',(-70.9225390131826,-1.13778883418213,
12.));
#84082=CARTESIAN_POINT('Ctrl Pts',(-70.9432621490566,-1.14469209291488,
0.));
#84083=CARTESIAN_POINT('Ctrl Pts',(-70.9432621490566,-1.14469209291488,
12.));
#84084=CARTESIAN_POINT('Ctrl Pts',(-70.9640233879659,-1.15163165376524,
0.));
#84085=CARTESIAN_POINT('Ctrl Pts',(-70.9640233879659,-1.15163165376524,
12.));
#84086=CARTESIAN_POINT('Ctrl Pts',(-70.9848225647871,-1.15860753911485,
0.));
#84087=CARTESIAN_POINT('Ctrl Pts',(-70.9848225647871,-1.15860753911485,
12.));
#84088=CARTESIAN_POINT('Ctrl Pts',(-71.0056595152204,-1.1656197711288,0.));
#84089=CARTESIAN_POINT('Ctrl Pts',(-71.0056595152204,-1.1656197711288,12.));
#84090=CARTESIAN_POINT('Ctrl Pts',(-71.0265340757699,-1.17266837175777,
0.));
#84091=CARTESIAN_POINT('Ctrl Pts',(-71.0265340757699,-1.17266837175777,
12.));
#84092=CARTESIAN_POINT('Ctrl Pts',(-71.0474460837159,-1.17975336273504,
0.));
#84093=CARTESIAN_POINT('Ctrl Pts',(-71.0474460837159,-1.17975336273504,
12.));
#84094=CARTESIAN_POINT('Ctrl Pts',(-71.0683953771149,-1.18687476558133,
0.));
#84095=CARTESIAN_POINT('Ctrl Pts',(-71.0683953771149,-1.18687476558133,
12.));
#84096=CARTESIAN_POINT('Ctrl Pts',(-71.089381794801,-1.19403260161002,0.));
#84097=CARTESIAN_POINT('Ctrl Pts',(-71.089381794801,-1.19403260161002,12.));
#84098=CARTESIAN_POINT('Ctrl Pts',(-71.1104051763839,-1.20122689192836,
0.));
#84099=CARTESIAN_POINT('Ctrl Pts',(-71.1104051763839,-1.20122689192836,
12.));
#84100=CARTESIAN_POINT('Ctrl Pts',(-71.1314653622442,-1.20845765743647,
0.));
#84101=CARTESIAN_POINT('Ctrl Pts',(-71.1314653622442,-1.20845765743647,
12.));
#84102=CARTESIAN_POINT('Ctrl Pts',(-71.1525621935267,-1.21572491882262,
0.));
#84103=CARTESIAN_POINT('Ctrl Pts',(-71.1525621935267,-1.21572491882262,
12.));
#84104=CARTESIAN_POINT('Ctrl Pts',(-71.1736955121362,-1.22302869657017,
0.));
#84105=CARTESIAN_POINT('Ctrl Pts',(-71.1736955121362,-1.22302869657017,
12.));
#84106=CARTESIAN_POINT('Ctrl Pts',(-71.194865160732,-1.23036901096239,0.));
#84107=CARTESIAN_POINT('Ctrl Pts',(-71.194865160732,-1.23036901096239,12.));
#84108=CARTESIAN_POINT('Ctrl Pts',(-71.2160709827191,-1.23774588208427,
0.));
#84109=CARTESIAN_POINT('Ctrl Pts',(-71.2160709827191,-1.23774588208427,
12.));
#84110=CARTESIAN_POINT('Ctrl Pts',(-71.2373128222352,-1.24515932982112,
0.));
#84111=CARTESIAN_POINT('Ctrl Pts',(-71.2373128222352,-1.24515932982112,
12.));
#84112=CARTESIAN_POINT('Ctrl Pts',(-71.2585905241406,-1.25260937385568,
0.));
#84113=CARTESIAN_POINT('Ctrl Pts',(-71.2585905241406,-1.25260937385568,
12.));
#84114=CARTESIAN_POINT('Ctrl Pts',(-71.2799039340175,-1.2600960336757,0.));
#84115=CARTESIAN_POINT('Ctrl Pts',(-71.2799039340175,-1.2600960336757,12.));
#84116=CARTESIAN_POINT('Ctrl Pts',(-71.3012528981661,-1.26761932857724,
0.));
#84117=CARTESIAN_POINT('Ctrl Pts',(-71.3012528981661,-1.26761932857724,
12.));
#84118=CARTESIAN_POINT('Ctrl Pts',(-71.3226372635996,-1.27517927766608,
0.));
#84119=CARTESIAN_POINT('Ctrl Pts',(-71.3226372635996,-1.27517927766608,
12.));
#84120=CARTESIAN_POINT('Ctrl Pts',(-71.3440568780347,-1.28277589985471,
0.));
#84121=CARTESIAN_POINT('Ctrl Pts',(-71.3440568780347,-1.28277589985471,
12.));
#84122=CARTESIAN_POINT('Ctrl Pts',(-71.3655115898827,-1.29040921386059,
0.));
#84123=CARTESIAN_POINT('Ctrl Pts',(-71.3655115898827,-1.29040921386059,
12.));
#84124=CARTESIAN_POINT('Ctrl Pts',(-71.3870012482499,-1.29807923821413,
0.));
#84125=CARTESIAN_POINT('Ctrl Pts',(-71.3870012482499,-1.29807923821413,
12.));
#84126=CARTESIAN_POINT('Ctrl Pts',(-71.4085257029322,-1.30578599126139,
0.));
#84127=CARTESIAN_POINT('Ctrl Pts',(-71.4085257029322,-1.30578599126139,
12.));
#84128=CARTESIAN_POINT('Ctrl Pts',(-71.4300848044087,-1.31352949116537,
0.));
#84129=CARTESIAN_POINT('Ctrl Pts',(-71.4300848044087,-1.31352949116537,
12.));
#84130=CARTESIAN_POINT('Ctrl Pts',(-71.4516784038317,-1.32130975590226,
0.));
#84131=CARTESIAN_POINT('Ctrl Pts',(-71.4516784038317,-1.32130975590226,
12.));
#84132=CARTESIAN_POINT('Ctrl Pts',(-71.4733063530187,-1.32912680326123,
0.));
#84133=CARTESIAN_POINT('Ctrl Pts',(-71.4733063530187,-1.32912680326123,
12.));
#84134=CARTESIAN_POINT('Ctrl Pts',(-71.4949685044522,-1.33698065085219,
0.));
#84135=CARTESIAN_POINT('Ctrl Pts',(-71.4949685044522,-1.33698065085219,
12.));
#84136=CARTESIAN_POINT('Ctrl Pts',(-71.516664711275,-1.3448713161078,0.));
#84137=CARTESIAN_POINT('Ctrl Pts',(-71.516664711275,-1.3448713161078,12.));
#84138=CARTESIAN_POINT('Ctrl Pts',(-71.5383948272845,-1.35279881628455,
0.));
#84139=CARTESIAN_POINT('Ctrl Pts',(-71.5383948272845,-1.35279881628455,
12.));
#84140=CARTESIAN_POINT('Ctrl Pts',(-71.5601587069217,-1.36076316845816,
0.));
#84141=CARTESIAN_POINT('Ctrl Pts',(-71.5601587069217,-1.36076316845816,
12.));
#84142=CARTESIAN_POINT('Ctrl Pts',(-71.5819562052663,-1.36876438952465,
0.));
#84143=CARTESIAN_POINT('Ctrl Pts',(-71.5819562052663,-1.36876438952465,
12.));
#84144=CARTESIAN_POINT('Ctrl Pts',(-71.6037871780385,-1.37680249620779,
0.));
#84145=CARTESIAN_POINT('Ctrl Pts',(-71.6037871780385,-1.37680249620779,
12.));
#84146=CARTESIAN_POINT('Ctrl Pts',(-71.625651481593,-1.38487750506082,0.));
#84147=CARTESIAN_POINT('Ctrl Pts',(-71.625651481593,-1.38487750506082,12.));
#84148=CARTESIAN_POINT('Ctrl Pts',(-71.6475489729134,-1.39298943246722,
0.));
#84149=CARTESIAN_POINT('Ctrl Pts',(-71.6475489729134,-1.39298943246722,
12.));
#84150=CARTESIAN_POINT('Ctrl Pts',(-71.6694795096001,-1.40113829463576,
0.));
#84151=CARTESIAN_POINT('Ctrl Pts',(-71.6694795096001,-1.40113829463576,
12.));
#84152=CARTESIAN_POINT('Ctrl Pts',(-71.6914429498663,-1.40932410760248,
0.));
#84153=CARTESIAN_POINT('Ctrl Pts',(-71.6914429498663,-1.40932410760248,
12.));
#84154=CARTESIAN_POINT('Ctrl Pts',(-71.7134391525389,-1.41754688723773,
0.));
#84155=CARTESIAN_POINT('Ctrl Pts',(-71.7134391525389,-1.41754688723773,
12.));
#84156=CARTESIAN_POINT('Ctrl Pts',(-71.7354679770528,-1.42580664924769,
0.));
#84157=CARTESIAN_POINT('Ctrl Pts',(-71.7354679770528,-1.42580664924769,
12.));
#84158=CARTESIAN_POINT('Ctrl Pts',(-71.7575292834469,-1.43410340917495,
0.));
#84159=CARTESIAN_POINT('Ctrl Pts',(-71.7575292834469,-1.43410340917495,
12.));
#84160=CARTESIAN_POINT('Ctrl Pts',(-71.7796229323526,-1.44243718239315,
0.));
#84161=CARTESIAN_POINT('Ctrl Pts',(-71.7796229323526,-1.44243718239315,
12.));
#84162=CARTESIAN_POINT('Ctrl Pts',(-71.8017487849895,-1.45080798410965,
0.));
#84163=CARTESIAN_POINT('Ctrl Pts',(-71.8017487849895,-1.45080798410965,
12.));
#84164=CARTESIAN_POINT('Ctrl Pts',(-71.8239067031683,-1.45921582937231,
0.));
#84165=CARTESIAN_POINT('Ctrl Pts',(-71.8239067031683,-1.45921582937231,
12.));
#84166=CARTESIAN_POINT('Ctrl Pts',(-71.8460965492839,-1.46766073307088,
0.));
#84167=CARTESIAN_POINT('Ctrl Pts',(-71.8460965492839,-1.46766073307088,
12.));
#84168=CARTESIAN_POINT('Ctrl Pts',(-71.8683181863116,-1.47614270993728,
0.));
#84169=CARTESIAN_POINT('Ctrl Pts',(-71.8683181863116,-1.47614270993728,
12.));
#84170=CARTESIAN_POINT('Ctrl Pts',(-71.8905714777961,-1.48466177454019,
0.));
#84171=CARTESIAN_POINT('Ctrl Pts',(-71.8905714777961,-1.48466177454019,
12.));
#84172=CARTESIAN_POINT('Ctrl Pts',(-71.912856287848,-1.49321794128798,0.));
#84173=CARTESIAN_POINT('Ctrl Pts',(-71.912856287848,-1.49321794128798,12.));
#84174=CARTESIAN_POINT('Ctrl Pts',(-71.9351724811443,-1.50181122443534,
0.));
#84175=CARTESIAN_POINT('Ctrl Pts',(-71.9351724811443,-1.50181122443534,
12.));
#84176=CARTESIAN_POINT('Ctrl Pts',(-71.9575199229241,-1.51044163808453,
0.));
#84177=CARTESIAN_POINT('Ctrl Pts',(-71.9575199229241,-1.51044163808453,
12.));
#84178=CARTESIAN_POINT('Ctrl Pts',(-71.979898478983,-1.51910919618566,0.));
#84179=CARTESIAN_POINT('Ctrl Pts',(-71.979898478983,-1.51910919618566,12.));
#84180=CARTESIAN_POINT('Ctrl Pts',(-72.0023080156647,-1.52781391253102,
0.));
#84181=CARTESIAN_POINT('Ctrl Pts',(-72.0023080156647,-1.52781391253102,
12.));
#84182=CARTESIAN_POINT('Ctrl Pts',(-72.0247483998579,-1.53655580075812,
0.));
#84183=CARTESIAN_POINT('Ctrl Pts',(-72.0247483998579,-1.53655580075812,
12.));
#84184=CARTESIAN_POINT('Ctrl Pts',(-72.0472194989963,-1.54533487435626,
0.));
#84185=CARTESIAN_POINT('Ctrl Pts',(-72.0472194989963,-1.54533487435626,
12.));
#84186=CARTESIAN_POINT('Ctrl Pts',(-72.0697211810545,-1.55415114666773,
0.));
#84187=CARTESIAN_POINT('Ctrl Pts',(-72.0697211810545,-1.55415114666773,
12.));
#84188=CARTESIAN_POINT('Ctrl Pts',(-72.0922533145433,-1.56300463088808,
0.));
#84189=CARTESIAN_POINT('Ctrl Pts',(-72.0922533145433,-1.56300463088808,
12.));
#84190=CARTESIAN_POINT('Ctrl Pts',(-72.1148157684995,-1.5718953400604,0.));
#84191=CARTESIAN_POINT('Ctrl Pts',(-72.1148157684995,-1.5718953400604,12.));
#84192=CARTESIAN_POINT('Ctrl Pts',(-72.1374084124839,-1.58082328707803,
0.));
#84193=CARTESIAN_POINT('Ctrl Pts',(-72.1374084124839,-1.58082328707803,
12.));
#84194=CARTESIAN_POINT('Ctrl Pts',(-72.1600311165821,-1.58978848469123,
0.));
#84195=CARTESIAN_POINT('Ctrl Pts',(-72.1600311165821,-1.58978848469123,
12.));
#84196=CARTESIAN_POINT('Ctrl Pts',(-72.1826837514001,-1.59879094550847,
0.));
#84197=CARTESIAN_POINT('Ctrl Pts',(-72.1826837514001,-1.59879094550847,
12.));
#84198=CARTESIAN_POINT('Ctrl Pts',(-72.2053661880608,-1.60783068199663,
0.));
#84199=CARTESIAN_POINT('Ctrl Pts',(-72.2053661880608,-1.60783068199663,
12.));
#84200=CARTESIAN_POINT('Ctrl Pts',(-72.2280782981937,-1.6169077064754,0.));
#84201=CARTESIAN_POINT('Ctrl Pts',(-72.2280782981937,-1.6169077064754,12.));
#84202=CARTESIAN_POINT('Ctrl Pts',(-72.2508199539323,-1.6260220311193,0.));
#84203=CARTESIAN_POINT('Ctrl Pts',(-72.2508199539323,-1.6260220311193,12.));
#84204=CARTESIAN_POINT('Ctrl Pts',(-72.2735910279149,-1.63517366796463,
0.));
#84205=CARTESIAN_POINT('Ctrl Pts',(-72.2735910279149,-1.63517366796463,
12.));
#84206=CARTESIAN_POINT('Ctrl Pts',(-72.2963913932813,-1.64436262891079,
0.));
#84207=CARTESIAN_POINT('Ctrl Pts',(-72.2963913932813,-1.64436262891079,
12.));
#84208=CARTESIAN_POINT('Ctrl Pts',(-72.319220923669,-1.65358892572062,0.));
#84209=CARTESIAN_POINT('Ctrl Pts',(-72.319220923669,-1.65358892572062,12.));
#84210=CARTESIAN_POINT('Ctrl Pts',(-72.3420794932047,-1.66285257001496,
0.));
#84211=CARTESIAN_POINT('Ctrl Pts',(-72.3420794932047,-1.66285257001496,
12.));
#84212=CARTESIAN_POINT('Ctrl Pts',(-72.3649669765004,-1.67215357327365,
0.));
#84213=CARTESIAN_POINT('Ctrl Pts',(-72.3649669765004,-1.67215357327365,
12.));
#84214=CARTESIAN_POINT('Ctrl Pts',(-72.387883248654,-1.68149194684281,0.));
#84215=CARTESIAN_POINT('Ctrl Pts',(-72.387883248654,-1.68149194684281,12.));
#84216=CARTESIAN_POINT('Ctrl Pts',(-72.4108281852467,-1.69086770193637,
0.));
#84217=CARTESIAN_POINT('Ctrl Pts',(-72.4108281852467,-1.69086770193637,
12.));
#84218=CARTESIAN_POINT('Ctrl Pts',(-72.4338016623391,-1.70028084963647,
0.));
#84219=CARTESIAN_POINT('Ctrl Pts',(-72.4338016623391,-1.70028084963647,
12.));
#84220=CARTESIAN_POINT('Ctrl Pts',(-72.456803556463,-1.70973140088841,0.));
#84221=CARTESIAN_POINT('Ctrl Pts',(-72.456803556463,-1.70973140088841,12.));
#84222=CARTESIAN_POINT('Ctrl Pts',(-72.479833744618,-1.71921936650038,0.));
#84223=CARTESIAN_POINT('Ctrl Pts',(-72.479833744618,-1.71921936650038,12.));
#84224=CARTESIAN_POINT('Ctrl Pts',(-72.5028921042721,-1.72874475715103,
0.));
#84225=CARTESIAN_POINT('Ctrl Pts',(-72.5028921042721,-1.72874475715103,
12.));
#84226=CARTESIAN_POINT('Ctrl Pts',(-72.5259785133595,-1.73830758339125,
0.));
#84227=CARTESIAN_POINT('Ctrl Pts',(-72.5259785133595,-1.73830758339125,
12.));
#84228=CARTESIAN_POINT('Ctrl Pts',(-72.5490928502769,-1.74790785564473,
0.));
#84229=CARTESIAN_POINT('Ctrl Pts',(-72.5490928502769,-1.74790785564473,
12.));
#84230=CARTESIAN_POINT('Ctrl Pts',(-72.5722349938774,-1.75754558420344,
0.));
#84231=CARTESIAN_POINT('Ctrl Pts',(-72.5722349938774,-1.75754558420344,
12.));
#84232=CARTESIAN_POINT('Ctrl Pts',(-72.5954048234638,-1.76722077922574,
0.));
#84233=CARTESIAN_POINT('Ctrl Pts',(-72.5954048234638,-1.76722077922574,
12.));
#84234=CARTESIAN_POINT('Ctrl Pts',(-72.6186022187907,-1.77693345074426,
0.));
#84235=CARTESIAN_POINT('Ctrl Pts',(-72.6186022187907,-1.77693345074426,
12.));
#84236=CARTESIAN_POINT('Ctrl Pts',(-72.6418270600619,-1.78668360866811,
0.));
#84237=CARTESIAN_POINT('Ctrl Pts',(-72.6418270600619,-1.78668360866811,
12.));
#84238=CARTESIAN_POINT('Ctrl Pts',(-72.6650792279274,-1.79647126278358,
0.));
#84239=CARTESIAN_POINT('Ctrl Pts',(-72.6650792279274,-1.79647126278358,
12.));
#84240=CARTESIAN_POINT('Ctrl Pts',(-72.6883586034769,-1.8062964227505,0.));
#84241=CARTESIAN_POINT('Ctrl Pts',(-72.6883586034769,-1.8062964227505,12.));
#84242=CARTESIAN_POINT('Ctrl Pts',(-72.7116650682344,-1.81615909809871,
0.));
#84243=CARTESIAN_POINT('Ctrl Pts',(-72.7116650682344,-1.81615909809871,
12.));
#84244=CARTESIAN_POINT('Ctrl Pts',(-72.7349985041592,-1.82605929823564,
0.));
#84245=CARTESIAN_POINT('Ctrl Pts',(-72.7349985041592,-1.82605929823564,
12.));
#84246=CARTESIAN_POINT('Ctrl Pts',(-72.7583587936447,-1.83599703244924,
0.));
#84247=CARTESIAN_POINT('Ctrl Pts',(-72.7583587936447,-1.83599703244924,
12.));
#84248=CARTESIAN_POINT('Ctrl Pts',(-72.7817458195155,-1.84597230990857,
0.));
#84249=CARTESIAN_POINT('Ctrl Pts',(-72.7817458195155,-1.84597230990857,
12.));
#84250=CARTESIAN_POINT('Ctrl Pts',(-72.8051594650222,-1.85598513966113,
0.));
#84251=CARTESIAN_POINT('Ctrl Pts',(-72.8051594650222,-1.85598513966113,
12.));
#84252=CARTESIAN_POINT('Ctrl Pts',(-72.8285996138359,-1.86603553062771,
0.));
#84253=CARTESIAN_POINT('Ctrl Pts',(-72.8285996138359,-1.86603553062771,
12.));
#84254=CARTESIAN_POINT('Ctrl Pts',(-72.8520661500477,-1.87612349160944,
0.));
#84255=CARTESIAN_POINT('Ctrl Pts',(-72.8520661500477,-1.87612349160944,
12.));
#84256=CARTESIAN_POINT('Ctrl Pts',(-72.875558958168,-1.88624903129188,0.));
#84257=CARTESIAN_POINT('Ctrl Pts',(-72.875558958168,-1.88624903129188,12.));
#84258=CARTESIAN_POINT('Ctrl Pts',(-72.8990779231226,-1.89641215824582,
0.));
#84259=CARTESIAN_POINT('Ctrl Pts',(-72.8990779231226,-1.89641215824582,
12.));
#84260=CARTESIAN_POINT('Ctrl Pts',(-72.9226229302478,-1.90661288092587,
0.));
#84261=CARTESIAN_POINT('Ctrl Pts',(-72.9226229302478,-1.90661288092587,
12.));
#84262=CARTESIAN_POINT('Ctrl Pts',(-72.9461938652811,-1.91685120766436,
0.));
#84263=CARTESIAN_POINT('Ctrl Pts',(-72.9461938652811,-1.91685120766436,
12.));
#84264=CARTESIAN_POINT('Ctrl Pts',(-72.9697906143636,-1.9271271466766,0.));
#84265=CARTESIAN_POINT('Ctrl Pts',(-72.9697906143636,-1.9271271466766,12.));
#84266=CARTESIAN_POINT('Ctrl Pts',(-72.9934130640415,-1.93744070606566,
0.));
#84267=CARTESIAN_POINT('Ctrl Pts',(-72.9934130640415,-1.93744070606566,
12.));
#84268=CARTESIAN_POINT('Ctrl Pts',(-73.0170611012661,-1.94779189382302,
0.));
#84269=CARTESIAN_POINT('Ctrl Pts',(-73.0170611012661,-1.94779189382302,
12.));
#84270=CARTESIAN_POINT('Ctrl Pts',(-73.040734613391,-1.95818071782767,0.));
#84271=CARTESIAN_POINT('Ctrl Pts',(-73.040734613391,-1.95818071782767,12.));
#84272=CARTESIAN_POINT('Ctrl Pts',(-73.0644334881673,-1.96860718583932,
0.));
#84273=CARTESIAN_POINT('Ctrl Pts',(-73.0644334881673,-1.96860718583932,
12.));
#84274=CARTESIAN_POINT('Ctrl Pts',(-73.0881576137407,-1.97907130550157,
0.));
#84275=CARTESIAN_POINT('Ctrl Pts',(-73.0881576137407,-1.97907130550157,
12.));
#84276=CARTESIAN_POINT('Ctrl Pts',(-73.1119068786475,-1.98957308434918,
0.));
#84277=CARTESIAN_POINT('Ctrl Pts',(-73.1119068786475,-1.98957308434918,
12.));
#84278=CARTESIAN_POINT('Ctrl Pts',(-73.1356811718091,-2.00011252980981,
0.));
#84279=CARTESIAN_POINT('Ctrl Pts',(-73.1356811718091,-2.00011252980981,
12.));
#84280=CARTESIAN_POINT('Ctrl Pts',(-73.1594803825252,-2.01068964920467,
0.));
#84281=CARTESIAN_POINT('Ctrl Pts',(-73.1594803825252,-2.01068964920467,
12.));
#84282=CARTESIAN_POINT('Ctrl Pts',(-73.183304400462,-2.02130444974362,0.));
#84283=CARTESIAN_POINT('Ctrl Pts',(-73.183304400462,-2.02130444974362,12.));
#84284=CARTESIAN_POINT('Ctrl Pts',(-73.2071531156504,-2.03195693852454,
0.));
#84285=CARTESIAN_POINT('Ctrl Pts',(-73.2071531156504,-2.03195693852454,
12.));
#84286=CARTESIAN_POINT('Ctrl Pts',(-73.2310264184976,-2.04264712253928,
0.));
#84287=CARTESIAN_POINT('Ctrl Pts',(-73.2310264184976,-2.04264712253928,
12.));
#84288=CARTESIAN_POINT('Ctrl Pts',(-73.2549241997953,-2.05337500867403,
0.));
#84289=CARTESIAN_POINT('Ctrl Pts',(-73.2549241997953,-2.05337500867403,
12.));
#84290=CARTESIAN_POINT('Ctrl Pts',(-73.2788463507246,-2.06414060370834,
0.));
#84291=CARTESIAN_POINT('Ctrl Pts',(-73.2788463507246,-2.06414060370834,
12.));
#84292=CARTESIAN_POINT('Ctrl Pts',(-73.3027927628626,-2.07494391430941,
0.));
#84293=CARTESIAN_POINT('Ctrl Pts',(-73.3027927628626,-2.07494391430941,
12.));
#84294=CARTESIAN_POINT('Ctrl Pts',(-73.3267633281807,-2.08578494702743,
0.));
#84295=CARTESIAN_POINT('Ctrl Pts',(-73.3267633281807,-2.08578494702743,
12.));
#84296=CARTESIAN_POINT('Ctrl Pts',(-73.3507579390239,-2.09666370830716,
0.));
#84297=CARTESIAN_POINT('Ctrl Pts',(-73.3507579390239,-2.09666370830716,
12.));
#84298=CARTESIAN_POINT('Ctrl Pts',(-73.3747764880893,-2.1075802044939,0.));
#84299=CARTESIAN_POINT('Ctrl Pts',(-73.3747764880893,-2.1075802044939,12.));
#84300=CARTESIAN_POINT('Ctrl Pts',(-73.3988188684021,-2.11853444183761,
0.));
#84301=CARTESIAN_POINT('Ctrl Pts',(-73.3988188684021,-2.11853444183761,
12.));
#84302=CARTESIAN_POINT('Ctrl Pts',(-73.4228849732925,-2.12952642649367,
0.));
#84303=CARTESIAN_POINT('Ctrl Pts',(-73.4228849732925,-2.12952642649367,
12.));
#84304=CARTESIAN_POINT('Ctrl Pts',(-73.4469746963637,-2.14055616452057,
0.));
#84305=CARTESIAN_POINT('Ctrl Pts',(-73.4469746963637,-2.14055616452057,
12.));
#84306=CARTESIAN_POINT('Ctrl Pts',(-73.4710879315382,-2.15162366187906,
0.));
#84307=CARTESIAN_POINT('Ctrl Pts',(-73.4710879315382,-2.15162366187906,
12.));
#84308=CARTESIAN_POINT('Ctrl Pts',(-73.4952245731054,-2.16272892442919,
0.));
#84309=CARTESIAN_POINT('Ctrl Pts',(-73.4952245731054,-2.16272892442919,
12.));
#84310=CARTESIAN_POINT('Ctrl Pts',(-73.5193845157708,-2.17387195792306,
0.));
#84311=CARTESIAN_POINT('Ctrl Pts',(-73.5193845157708,-2.17387195792306,
12.));
#84312=CARTESIAN_POINT('Ctrl Pts',(-73.5435676546929,-2.18505276799753,
0.));
#84313=CARTESIAN_POINT('Ctrl Pts',(-73.5435676546929,-2.18505276799753,
12.));
#84314=CARTESIAN_POINT('Ctrl Pts',(-73.5677738855452,-2.19627136015678,
0.));
#84315=CARTESIAN_POINT('Ctrl Pts',(-73.5677738855452,-2.19627136015678,
12.));
#84316=CARTESIAN_POINT('Ctrl Pts',(-73.5920031044595,-2.20752773978348,
0.));
#84317=CARTESIAN_POINT('Ctrl Pts',(-73.5920031044595,-2.20752773978348,
12.));
#84318=CARTESIAN_POINT('Ctrl Pts',(-73.6162552079038,-2.21882191216518,
0.));
#84319=CARTESIAN_POINT('Ctrl Pts',(-73.6162552079038,-2.21882191216518,
12.));
#84320=CARTESIAN_POINT('Ctrl Pts',(-73.6405300925712,-2.23015388251287,
0.));
#84321=CARTESIAN_POINT('Ctrl Pts',(-73.6405300925712,-2.23015388251287,
12.));
#84322=CARTESIAN_POINT('Ctrl Pts',(-73.6648276552767,-2.24152365597697,
0.));
#84323=CARTESIAN_POINT('Ctrl Pts',(-73.6648276552767,-2.24152365597697,
12.));
#84324=CARTESIAN_POINT('Ctrl Pts',(-73.6891477928129,-2.25293123766425,
0.));
#84325=CARTESIAN_POINT('Ctrl Pts',(-73.6891477928129,-2.25293123766425,
12.));
#84326=CARTESIAN_POINT('Ctrl Pts',(-73.7134904019389,-2.26437663263667,
0.));
#84327=CARTESIAN_POINT('Ctrl Pts',(-73.7134904019389,-2.26437663263667,
12.));
#84328=CARTESIAN_POINT('Ctrl Pts',(-73.7378553796807,-2.27585984587198,
0.));
#84329=CARTESIAN_POINT('Ctrl Pts',(-73.7378553796807,-2.27585984587198,
12.));
#84330=CARTESIAN_POINT('Ctrl Pts',(-73.762242623566,-2.28738088222863,0.));
#84331=CARTESIAN_POINT('Ctrl Pts',(-73.762242623566,-2.28738088222863,12.));
#84332=CARTESIAN_POINT('Ctrl Pts',(-73.786652031885,-2.29893974640434,0.));
#84333=CARTESIAN_POINT('Ctrl Pts',(-73.786652031885,-2.29893974640434,12.));
#84334=CARTESIAN_POINT('Ctrl Pts',(-73.8110835039327,-2.31053644289416,
0.));
#84335=CARTESIAN_POINT('Ctrl Pts',(-73.8110835039327,-2.31053644289416,
12.));
#84336=CARTESIAN_POINT('Ctrl Pts',(-73.8355369402706,-2.32217097594197,
0.));
#84337=CARTESIAN_POINT('Ctrl Pts',(-73.8355369402706,-2.32217097594197,
12.));
#84338=CARTESIAN_POINT('Ctrl Pts',(-73.8600122421468,-2.33384334963957,
0.));
#84339=CARTESIAN_POINT('Ctrl Pts',(-73.8600122421468,-2.33384334963957,
12.));
#84340=CARTESIAN_POINT('Ctrl Pts',(-73.8845093109274,-2.3455535680212,0.));
#84341=CARTESIAN_POINT('Ctrl Pts',(-73.8845093109274,-2.3455535680212,12.));
#84342=CARTESIAN_POINT('Ctrl Pts',(-73.9090280474712,-2.35730163516315,
0.));
#84343=CARTESIAN_POINT('Ctrl Pts',(-73.9090280474712,-2.35730163516315,
12.));
#84344=CARTESIAN_POINT('Ctrl Pts',(-73.9335683516404,-2.36908755526003,
0.));
#84345=CARTESIAN_POINT('Ctrl Pts',(-73.9335683516404,-2.36908755526003,
12.));
#84346=CARTESIAN_POINT('Ctrl Pts',(-73.958130121465,-2.3809113327496,0.));
#84347=CARTESIAN_POINT('Ctrl Pts',(-73.958130121465,-2.3809113327496,12.));
#84348=CARTESIAN_POINT('Ctrl Pts',(-73.9827132538206,-2.39277297220756,
0.));
#84349=CARTESIAN_POINT('Ctrl Pts',(-73.9827132538206,-2.39277297220756,
12.));
#84350=CARTESIAN_POINT('Ctrl Pts',(-74.0073176459344,-2.40467247811536,
0.));
#84351=CARTESIAN_POINT('Ctrl Pts',(-74.0073176459344,-2.40467247811536,
12.));
#84352=CARTESIAN_POINT('Ctrl Pts',(-74.0319431966989,-2.41660985465251,
0.));
#84353=CARTESIAN_POINT('Ctrl Pts',(-74.0319431966989,-2.41660985465251,
12.));
#84354=CARTESIAN_POINT('Ctrl Pts',(-74.0565898079218,-2.42858510549778,
0.));
#84355=CARTESIAN_POINT('Ctrl Pts',(-74.0565898079218,-2.42858510549778,
12.));
#84356=CARTESIAN_POINT('Ctrl Pts',(-74.0812573859411,-2.44059823356675,
0.));
#84357=CARTESIAN_POINT('Ctrl Pts',(-74.0812573859411,-2.44059823356675,
12.));
#84358=CARTESIAN_POINT('Ctrl Pts',(-74.1059458420067,-2.45264924094775,
0.));
#84359=CARTESIAN_POINT('Ctrl Pts',(-74.1059458420067,-2.45264924094775,
12.));
#84360=CARTESIAN_POINT('Ctrl Pts',(-74.1306550887071,-2.46473812947959,
0.));
#84361=CARTESIAN_POINT('Ctrl Pts',(-74.1306550887071,-2.46473812947959,
12.));
#84362=CARTESIAN_POINT('Ctrl Pts',(-74.155385037148,-2.47686490120354,0.));
#84363=CARTESIAN_POINT('Ctrl Pts',(-74.155385037148,-2.47686490120354,12.));
#84364=CARTESIAN_POINT('Ctrl Pts',(-74.1801355936907,-2.48902955888384,
0.));
#84365=CARTESIAN_POINT('Ctrl Pts',(-74.1801355936907,-2.48902955888384,
12.));
#84366=CARTESIAN_POINT('Ctrl Pts',(-74.2049066572031,-2.50123210644135,
0.));
#84367=CARTESIAN_POINT('Ctrl Pts',(-74.2049066572031,-2.50123210644135,
12.));
#84368=CARTESIAN_POINT('Ctrl Pts',(-74.229698115223,-2.51347254956167,0.));
#84369=CARTESIAN_POINT('Ctrl Pts',(-74.229698115223,-2.51347254956167,12.));
#84370=CARTESIAN_POINT('Ctrl Pts',(-74.2545098494824,-2.52575089478303,
0.));
#84371=CARTESIAN_POINT('Ctrl Pts',(-74.2545098494824,-2.52575089478303,
12.));
#84372=CARTESIAN_POINT('Ctrl Pts',(-74.2793417427308,-2.53806714838286,
0.));
#84373=CARTESIAN_POINT('Ctrl Pts',(-74.2793417427308,-2.53806714838286,
12.));
#84374=CARTESIAN_POINT('Ctrl Pts',(-74.3041936853468,-2.5504213152678,0.));
#84375=CARTESIAN_POINT('Ctrl Pts',(-74.3041936853468,-2.5504213152678,12.));
#84376=CARTESIAN_POINT('Ctrl Pts',(-74.3290655814831,-2.56281339800017,
0.));
#84377=CARTESIAN_POINT('Ctrl Pts',(-74.3290655814831,-2.56281339800017,
12.));
#84378=CARTESIAN_POINT('Ctrl Pts',(-74.3539573567672,-2.57524339541389,
0.));
#84379=CARTESIAN_POINT('Ctrl Pts',(-74.3539573567672,-2.57524339541389,
12.));
#84380=CARTESIAN_POINT('Ctrl Pts',(-74.3788689603363,-2.58771130268175,
0.));
#84381=CARTESIAN_POINT('Ctrl Pts',(-74.3788689603363,-2.58771130268175,
12.));
#84382=CARTESIAN_POINT('Ctrl Pts',(-74.4038003594771,-2.60021711326977,
0.));
#84383=CARTESIAN_POINT('Ctrl Pts',(-74.4038003594771,-2.60021711326977,
12.));
#84384=CARTESIAN_POINT('Ctrl Pts',(-74.4237613007988,-2.61025207898403,
0.));
#84385=CARTESIAN_POINT('Ctrl Pts',(-74.4237613007988,-2.61025207898403,
12.));
#84386=CARTESIAN_POINT('Ctrl Pts',(-74.4387409032207,-2.61779535432112,
0.));
#84387=CARTESIAN_POINT('Ctrl Pts',(-74.4387409032207,-2.61779535432112,
12.));
#84388=CARTESIAN_POINT('Ctrl Pts',(-74.4487312586464,-2.62283178248202,
0.));
#84389=CARTESIAN_POINT('Ctrl Pts',(-74.4487312586464,-2.62283178248202,
12.));
#84390=CARTESIAN_POINT('Ctrl Pts',(-74.4537274248118,-2.62535189104655,
0.));
#84391=CARTESIAN_POINT('Ctrl Pts',(-74.4537274248118,-2.62535189104655,
12.));
#84392=CARTESIAN_POINT('',(-69.9947925310006,-0.85382582660898,0.));
#84393=CARTESIAN_POINT('Ctrl Pts',(-69.9947925310006,-0.85382582660898,
0.));
#84394=CARTESIAN_POINT('Ctrl Pts',(-69.9985337959407,-0.854867673848592,
0.));
#84395=CARTESIAN_POINT('Ctrl Pts',(-70.0060209754087,-0.856954870259201,
0.));
#84396=CARTESIAN_POINT('Ctrl Pts',(-70.0172656933806,-0.860096170668732,
0.));
#84397=CARTESIAN_POINT('Ctrl Pts',(-70.0322865492925,-0.864305583661541,
0.));
#84398=CARTESIAN_POINT('Ctrl Pts',(-70.051109108301,-0.86960237787112,0.));
#84399=CARTESIAN_POINT('Ctrl Pts',(-70.0699781183935,-0.874934213255836,
0.));
#84400=CARTESIAN_POINT('Ctrl Pts',(-70.0888934967855,-0.880301109660725,
0.));
#84401=CARTESIAN_POINT('Ctrl Pts',(-70.1078550938958,-0.885703094802532,
0.));
#84402=CARTESIAN_POINT('Ctrl Pts',(-70.1268626950175,-0.891140203464239,
0.));
#84403=CARTESIAN_POINT('Ctrl Pts',(-70.1459160490446,-0.89661247437184,
0.));
#84404=CARTESIAN_POINT('Ctrl Pts',(-70.1650148905109,-0.902119947629767,
0.));
#84405=CARTESIAN_POINT('Ctrl Pts',(-70.1841589635574,-0.907662662015781,
0.));
#84406=CARTESIAN_POINT('Ctrl Pts',(-70.2033480471676,-0.913240652090975,
0.));
#84407=CARTESIAN_POINT('Ctrl Pts',(-70.2225819470248,-0.918853949157115,
0.));
#84408=CARTESIAN_POINT('Ctrl Pts',(-70.2418604835837,-0.924502582639452,
0.));
#84409=CARTESIAN_POINT('Ctrl Pts',(-70.2611834821724,-0.930186581235545,
0.));
#84410=CARTESIAN_POINT('Ctrl Pts',(-70.2805507606872,-0.935905974336476,
0.));
#84411=CARTESIAN_POINT('Ctrl Pts',(-70.299962123399,-0.941660792742975,
0.));
#84412=CARTESIAN_POINT('Ctrl Pts',(-70.3194173673674,-0.9474510679296,0.));
#84413=CARTESIAN_POINT('Ctrl Pts',(-70.338916286458,-0.953276831581238,
0.));
#84414=CARTESIAN_POINT('Ctrl Pts',(-70.3584586759536,-0.959138115058827,
0.));
#84415=CARTESIAN_POINT('Ctrl Pts',(-70.3780443377956,-0.965034948786444,
0.));
#84416=CARTESIAN_POINT('Ctrl Pts',(-70.3976730803614,-0.970967362281171,
0.));
#84417=CARTESIAN_POINT('Ctrl Pts',(-70.417344715957,-0.976935384450037,
0.));
#84418=CARTESIAN_POINT('Ctrl Pts',(-70.4370590590842,-0.982939043792151,
0.));
#84419=CARTESIAN_POINT('Ctrl Pts',(-70.4568159243163,-0.988978368643646,
0.));
#84420=CARTESIAN_POINT('Ctrl Pts',(-70.4766151245212,-0.995053387379752,
0.));
#84421=CARTESIAN_POINT('Ctrl Pts',(-70.4964564717953,-1.00116412831442,
0.));
#84422=CARTESIAN_POINT('Ctrl Pts',(-70.5163397782713,-1.00731061960968,
0.));
#84423=CARTESIAN_POINT('Ctrl Pts',(-70.5362648569061,-1.01349288918537,
0.));
#84424=CARTESIAN_POINT('Ctrl Pts',(-70.556231522419,-1.01971096460597,0.));
#84425=CARTESIAN_POINT('Ctrl Pts',(-70.5762395916377,-1.02596487304048,
0.));
#84426=CARTESIAN_POINT('Ctrl Pts',(-70.5962888829934,-1.0322546413287,0.));
#84427=CARTESIAN_POINT('Ctrl Pts',(-70.6163792162073,-1.03858029601903,
0.));
#84428=CARTESIAN_POINT('Ctrl Pts',(-70.6365104119252,-1.04494186341156,
0.));
#84429=CARTESIAN_POINT('Ctrl Pts',(-70.6566822912991,-1.05133936960071,
0.));
#84430=CARTESIAN_POINT('Ctrl Pts',(-70.676894676009,-1.0577728404773,0.));
#84431=CARTESIAN_POINT('Ctrl Pts',(-70.6971473884459,-1.0642423017128,0.));
#84432=CARTESIAN_POINT('Ctrl Pts',(-70.7174402518378,-1.07074777874595,
0.));
#84433=CARTESIAN_POINT('Ctrl Pts',(-70.7377730903953,-1.07728929676408,
0.));
#84434=CARTESIAN_POINT('Ctrl Pts',(-70.7581457294447,-1.08386688068342,
0.));
#84435=CARTESIAN_POINT('Ctrl Pts',(-70.7785579953583,-1.09048055516426,
0.));
#84436=CARTESIAN_POINT('Ctrl Pts',(-70.799009715484,-1.09713034462265,0.));
#84437=CARTESIAN_POINT('Ctrl Pts',(-70.8195007180745,-1.10381627323946,
0.));
#84438=CARTESIAN_POINT('Ctrl Pts',(-70.8400308322037,-1.11053836496639,
0.));
#84439=CARTESIAN_POINT('Ctrl Pts',(-70.8605998877149,-1.11729664352992,
0.));
#84440=CARTESIAN_POINT('Ctrl Pts',(-70.8812077152586,-1.12409113243513,
0.));
#84441=CARTESIAN_POINT('Ctrl Pts',(-70.9018541463089,-1.13092185496564,
0.));
#84442=CARTESIAN_POINT('Ctrl Pts',(-70.9225390131826,-1.13778883418213,
0.));
#84443=CARTESIAN_POINT('Ctrl Pts',(-70.9432621490566,-1.14469209291488,
0.));
#84444=CARTESIAN_POINT('Ctrl Pts',(-70.9640233879659,-1.15163165376524,
0.));
#84445=CARTESIAN_POINT('Ctrl Pts',(-70.9848225647871,-1.15860753911485,
0.));
#84446=CARTESIAN_POINT('Ctrl Pts',(-71.0056595152204,-1.1656197711288,0.));
#84447=CARTESIAN_POINT('Ctrl Pts',(-71.0265340757699,-1.17266837175777,
0.));
#84448=CARTESIAN_POINT('Ctrl Pts',(-71.0474460837159,-1.17975336273504,
0.));
#84449=CARTESIAN_POINT('Ctrl Pts',(-71.0683953771149,-1.18687476558133,
0.));
#84450=CARTESIAN_POINT('Ctrl Pts',(-71.089381794801,-1.19403260161002,0.));
#84451=CARTESIAN_POINT('Ctrl Pts',(-71.1104051763839,-1.20122689192836,
0.));
#84452=CARTESIAN_POINT('Ctrl Pts',(-71.1314653622442,-1.20845765743647,
0.));
#84453=CARTESIAN_POINT('Ctrl Pts',(-71.1525621935267,-1.21572491882262,
0.));
#84454=CARTESIAN_POINT('Ctrl Pts',(-71.1736955121362,-1.22302869657017,
0.));
#84455=CARTESIAN_POINT('Ctrl Pts',(-71.194865160732,-1.23036901096239,0.));
#84456=CARTESIAN_POINT('Ctrl Pts',(-71.2160709827191,-1.23774588208427,
0.));
#84457=CARTESIAN_POINT('Ctrl Pts',(-71.2373128222352,-1.24515932982112,
0.));
#84458=CARTESIAN_POINT('Ctrl Pts',(-71.2585905241406,-1.25260937385568,
0.));
#84459=CARTESIAN_POINT('Ctrl Pts',(-71.2799039340175,-1.2600960336757,0.));
#84460=CARTESIAN_POINT('Ctrl Pts',(-71.3012528981661,-1.26761932857724,
0.));
#84461=CARTESIAN_POINT('Ctrl Pts',(-71.3226372635996,-1.27517927766608,
0.));
#84462=CARTESIAN_POINT('Ctrl Pts',(-71.3440568780347,-1.28277589985471,
0.));
#84463=CARTESIAN_POINT('Ctrl Pts',(-71.3655115898827,-1.29040921386059,
0.));
#84464=CARTESIAN_POINT('Ctrl Pts',(-71.3870012482499,-1.29807923821413,
0.));
#84465=CARTESIAN_POINT('Ctrl Pts',(-71.4085257029322,-1.30578599126139,
0.));
#84466=CARTESIAN_POINT('Ctrl Pts',(-71.4300848044087,-1.31352949116537,
0.));
#84467=CARTESIAN_POINT('Ctrl Pts',(-71.4516784038317,-1.32130975590226,
0.));
#84468=CARTESIAN_POINT('Ctrl Pts',(-71.4733063530187,-1.32912680326123,
0.));
#84469=CARTESIAN_POINT('Ctrl Pts',(-71.4949685044522,-1.33698065085219,
0.));
#84470=CARTESIAN_POINT('Ctrl Pts',(-71.516664711275,-1.3448713161078,0.));
#84471=CARTESIAN_POINT('Ctrl Pts',(-71.5383948272845,-1.35279881628455,
0.));
#84472=CARTESIAN_POINT('Ctrl Pts',(-71.5601587069217,-1.36076316845816,
0.));
#84473=CARTESIAN_POINT('Ctrl Pts',(-71.5819562052663,-1.36876438952465,
0.));
#84474=CARTESIAN_POINT('Ctrl Pts',(-71.6037871780385,-1.37680249620779,
0.));
#84475=CARTESIAN_POINT('Ctrl Pts',(-71.625651481593,-1.38487750506082,0.));
#84476=CARTESIAN_POINT('Ctrl Pts',(-71.6475489729134,-1.39298943246722,
0.));
#84477=CARTESIAN_POINT('Ctrl Pts',(-71.6694795096001,-1.40113829463576,
0.));
#84478=CARTESIAN_POINT('Ctrl Pts',(-71.6914429498663,-1.40932410760248,
0.));
#84479=CARTESIAN_POINT('Ctrl Pts',(-71.7134391525389,-1.41754688723773,
0.));
#84480=CARTESIAN_POINT('Ctrl Pts',(-71.7354679770528,-1.42580664924769,
0.));
#84481=CARTESIAN_POINT('Ctrl Pts',(-71.7575292834469,-1.43410340917495,
0.));
#84482=CARTESIAN_POINT('Ctrl Pts',(-71.7796229323526,-1.44243718239315,
0.));
#84483=CARTESIAN_POINT('Ctrl Pts',(-71.8017487849895,-1.45080798410965,
0.));
#84484=CARTESIAN_POINT('Ctrl Pts',(-71.8239067031683,-1.45921582937231,
0.));
#84485=CARTESIAN_POINT('Ctrl Pts',(-71.8460965492839,-1.46766073307088,
0.));
#84486=CARTESIAN_POINT('Ctrl Pts',(-71.8683181863116,-1.47614270993728,
0.));
#84487=CARTESIAN_POINT('Ctrl Pts',(-71.8905714777961,-1.48466177454019,
0.));
#84488=CARTESIAN_POINT('Ctrl Pts',(-71.912856287848,-1.49321794128798,0.));
#84489=CARTESIAN_POINT('Ctrl Pts',(-71.9351724811443,-1.50181122443534,
0.));
#84490=CARTESIAN_POINT('Ctrl Pts',(-71.9575199229241,-1.51044163808453,
0.));
#84491=CARTESIAN_POINT('Ctrl Pts',(-71.979898478983,-1.51910919618566,0.));
#84492=CARTESIAN_POINT('Ctrl Pts',(-72.0023080156647,-1.52781391253102,
0.));
#84493=CARTESIAN_POINT('Ctrl Pts',(-72.0247483998579,-1.53655580075812,
0.));
#84494=CARTESIAN_POINT('Ctrl Pts',(-72.0472194989963,-1.54533487435626,
0.));
#84495=CARTESIAN_POINT('Ctrl Pts',(-72.0697211810545,-1.55415114666773,
0.));
#84496=CARTESIAN_POINT('Ctrl Pts',(-72.0922533145433,-1.56300463088808,
0.));
#84497=CARTESIAN_POINT('Ctrl Pts',(-72.1148157684995,-1.5718953400604,0.));
#84498=CARTESIAN_POINT('Ctrl Pts',(-72.1374084124839,-1.58082328707803,
0.));
#84499=CARTESIAN_POINT('Ctrl Pts',(-72.1600311165821,-1.58978848469123,
0.));
#84500=CARTESIAN_POINT('Ctrl Pts',(-72.1826837514001,-1.59879094550847,
0.));
#84501=CARTESIAN_POINT('Ctrl Pts',(-72.2053661880608,-1.60783068199663,
0.));
#84502=CARTESIAN_POINT('Ctrl Pts',(-72.2280782981937,-1.6169077064754,0.));
#84503=CARTESIAN_POINT('Ctrl Pts',(-72.2508199539323,-1.6260220311193,0.));
#84504=CARTESIAN_POINT('Ctrl Pts',(-72.2735910279149,-1.63517366796463,
0.));
#84505=CARTESIAN_POINT('Ctrl Pts',(-72.2963913932813,-1.64436262891079,
0.));
#84506=CARTESIAN_POINT('Ctrl Pts',(-72.319220923669,-1.65358892572062,0.));
#84507=CARTESIAN_POINT('Ctrl Pts',(-72.3420794932047,-1.66285257001496,
0.));
#84508=CARTESIAN_POINT('Ctrl Pts',(-72.3649669765004,-1.67215357327365,
0.));
#84509=CARTESIAN_POINT('Ctrl Pts',(-72.387883248654,-1.68149194684281,0.));
#84510=CARTESIAN_POINT('Ctrl Pts',(-72.4108281852467,-1.69086770193637,
0.));
#84511=CARTESIAN_POINT('Ctrl Pts',(-72.4338016623391,-1.70028084963647,
0.));
#84512=CARTESIAN_POINT('Ctrl Pts',(-72.456803556463,-1.70973140088841,0.));
#84513=CARTESIAN_POINT('Ctrl Pts',(-72.479833744618,-1.71921936650038,0.));
#84514=CARTESIAN_POINT('Ctrl Pts',(-72.5028921042721,-1.72874475715103,
0.));
#84515=CARTESIAN_POINT('Ctrl Pts',(-72.5259785133595,-1.73830758339125,
0.));
#84516=CARTESIAN_POINT('Ctrl Pts',(-72.5490928502769,-1.74790785564473,
0.));
#84517=CARTESIAN_POINT('Ctrl Pts',(-72.5722349938774,-1.75754558420344,
0.));
#84518=CARTESIAN_POINT('Ctrl Pts',(-72.5954048234638,-1.76722077922574,
0.));
#84519=CARTESIAN_POINT('Ctrl Pts',(-72.6186022187907,-1.77693345074426,
0.));
#84520=CARTESIAN_POINT('Ctrl Pts',(-72.6418270600619,-1.78668360866811,
0.));
#84521=CARTESIAN_POINT('Ctrl Pts',(-72.6650792279274,-1.79647126278358,
0.));
#84522=CARTESIAN_POINT('Ctrl Pts',(-72.6883586034769,-1.8062964227505,0.));
#84523=CARTESIAN_POINT('Ctrl Pts',(-72.7116650682344,-1.81615909809871,
0.));
#84524=CARTESIAN_POINT('Ctrl Pts',(-72.7349985041592,-1.82605929823564,
0.));
#84525=CARTESIAN_POINT('Ctrl Pts',(-72.7583587936447,-1.83599703244924,
0.));
#84526=CARTESIAN_POINT('Ctrl Pts',(-72.7817458195155,-1.84597230990857,
0.));
#84527=CARTESIAN_POINT('Ctrl Pts',(-72.8051594650222,-1.85598513966113,
0.));
#84528=CARTESIAN_POINT('Ctrl Pts',(-72.8285996138359,-1.86603553062771,
0.));
#84529=CARTESIAN_POINT('Ctrl Pts',(-72.8520661500477,-1.87612349160944,
0.));
#84530=CARTESIAN_POINT('Ctrl Pts',(-72.875558958168,-1.88624903129188,0.));
#84531=CARTESIAN_POINT('Ctrl Pts',(-72.8990779231226,-1.89641215824582,
0.));
#84532=CARTESIAN_POINT('Ctrl Pts',(-72.9226229302478,-1.90661288092587,
0.));
#84533=CARTESIAN_POINT('Ctrl Pts',(-72.9461938652811,-1.91685120766436,
0.));
#84534=CARTESIAN_POINT('Ctrl Pts',(-72.9697906143636,-1.9271271466766,0.));
#84535=CARTESIAN_POINT('Ctrl Pts',(-72.9934130640415,-1.93744070606566,
0.));
#84536=CARTESIAN_POINT('Ctrl Pts',(-73.0170611012661,-1.94779189382302,
0.));
#84537=CARTESIAN_POINT('Ctrl Pts',(-73.040734613391,-1.95818071782767,0.));
#84538=CARTESIAN_POINT('Ctrl Pts',(-73.0644334881673,-1.96860718583932,
0.));
#84539=CARTESIAN_POINT('Ctrl Pts',(-73.0881576137407,-1.97907130550157,
0.));
#84540=CARTESIAN_POINT('Ctrl Pts',(-73.1119068786475,-1.98957308434918,
0.));
#84541=CARTESIAN_POINT('Ctrl Pts',(-73.1356811718091,-2.00011252980981,
0.));
#84542=CARTESIAN_POINT('Ctrl Pts',(-73.1594803825252,-2.01068964920467,
0.));
#84543=CARTESIAN_POINT('Ctrl Pts',(-73.183304400462,-2.02130444974362,0.));
#84544=CARTESIAN_POINT('Ctrl Pts',(-73.2071531156504,-2.03195693852454,
0.));
#84545=CARTESIAN_POINT('Ctrl Pts',(-73.2310264184976,-2.04264712253928,
0.));
#84546=CARTESIAN_POINT('Ctrl Pts',(-73.2549241997953,-2.05337500867403,
0.));
#84547=CARTESIAN_POINT('Ctrl Pts',(-73.2788463507246,-2.06414060370834,
0.));
#84548=CARTESIAN_POINT('Ctrl Pts',(-73.3027927628626,-2.07494391430941,
0.));
#84549=CARTESIAN_POINT('Ctrl Pts',(-73.3267633281807,-2.08578494702743,
0.));
#84550=CARTESIAN_POINT('Ctrl Pts',(-73.3507579390239,-2.09666370830716,
0.));
#84551=CARTESIAN_POINT('Ctrl Pts',(-73.3747764880893,-2.1075802044939,0.));
#84552=CARTESIAN_POINT('Ctrl Pts',(-73.3988188684021,-2.11853444183761,
0.));
#84553=CARTESIAN_POINT('Ctrl Pts',(-73.4228849732925,-2.12952642649367,
0.));
#84554=CARTESIAN_POINT('Ctrl Pts',(-73.4469746963637,-2.14055616452057,
0.));
#84555=CARTESIAN_POINT('Ctrl Pts',(-73.4710879315382,-2.15162366187906,
0.));
#84556=CARTESIAN_POINT('Ctrl Pts',(-73.4952245731054,-2.16272892442919,
0.));
#84557=CARTESIAN_POINT('Ctrl Pts',(-73.5193845157708,-2.17387195792306,
0.));
#84558=CARTESIAN_POINT('Ctrl Pts',(-73.5435676546929,-2.18505276799753,
0.));
#84559=CARTESIAN_POINT('Ctrl Pts',(-73.5677738855452,-2.19627136015678,
0.));
#84560=CARTESIAN_POINT('Ctrl Pts',(-73.5920031044595,-2.20752773978348,
0.));
#84561=CARTESIAN_POINT('Ctrl Pts',(-73.6162552079038,-2.21882191216518,
0.));
#84562=CARTESIAN_POINT('Ctrl Pts',(-73.6405300925712,-2.23015388251287,
0.));
#84563=CARTESIAN_POINT('Ctrl Pts',(-73.6648276552767,-2.24152365597697,
0.));
#84564=CARTESIAN_POINT('Ctrl Pts',(-73.6891477928129,-2.25293123766425,
0.));
#84565=CARTESIAN_POINT('Ctrl Pts',(-73.7134904019389,-2.26437663263667,
0.));
#84566=CARTESIAN_POINT('Ctrl Pts',(-73.7378553796807,-2.27585984587198,
0.));
#84567=CARTESIAN_POINT('Ctrl Pts',(-73.762242623566,-2.28738088222863,0.));
#84568=CARTESIAN_POINT('Ctrl Pts',(-73.786652031885,-2.29893974640434,0.));
#84569=CARTESIAN_POINT('Ctrl Pts',(-73.8110835039327,-2.31053644289416,
0.));
#84570=CARTESIAN_POINT('Ctrl Pts',(-73.8355369402706,-2.32217097594197,
0.));
#84571=CARTESIAN_POINT('Ctrl Pts',(-73.8600122421468,-2.33384334963957,
0.));
#84572=CARTESIAN_POINT('Ctrl Pts',(-73.8845093109274,-2.3455535680212,0.));
#84573=CARTESIAN_POINT('Ctrl Pts',(-73.9090280474712,-2.35730163516315,
0.));
#84574=CARTESIAN_POINT('Ctrl Pts',(-73.9335683516404,-2.36908755526003,
0.));
#84575=CARTESIAN_POINT('Ctrl Pts',(-73.958130121465,-2.3809113327496,0.));
#84576=CARTESIAN_POINT('Ctrl Pts',(-73.9827132538206,-2.39277297220756,
0.));
#84577=CARTESIAN_POINT('Ctrl Pts',(-74.0073176459344,-2.40467247811536,
0.));
#84578=CARTESIAN_POINT('Ctrl Pts',(-74.0319431966989,-2.41660985465251,
0.));
#84579=CARTESIAN_POINT('Ctrl Pts',(-74.0565898079218,-2.42858510549778,
0.));
#84580=CARTESIAN_POINT('Ctrl Pts',(-74.0812573859411,-2.44059823356675,
0.));
#84581=CARTESIAN_POINT('Ctrl Pts',(-74.1059458420067,-2.45264924094775,
0.));
#84582=CARTESIAN_POINT('Ctrl Pts',(-74.127126454519,-2.46301176097118,0.));
#84583=CARTESIAN_POINT('Ctrl Pts',(-74.143376394138,-2.47097695564993,0.));
#84584=CARTESIAN_POINT('Ctrl Pts',(-74.1546864735166,-2.47652804724537,
0.));
#84585=CARTESIAN_POINT('Ctrl Pts',(-74.1610506466206,-2.47965393945475,
0.));
#84586=CARTESIAN_POINT('Ctrl Pts',(-74.1624659714555,-2.48034921843229,
0.));
#84587=CARTESIAN_POINT('',(-69.9947925310006,-0.85382582660898,12.));
#84588=CARTESIAN_POINT('',(-69.9947925310006,-0.85382582660898,0.));
#84589=CARTESIAN_POINT('Ctrl Pts',(-74.1624659714555,-2.48034921843227,
12.));
#84590=CARTESIAN_POINT('Ctrl Pts',(-74.1610506466206,-2.47965393945474,
12.));
#84591=CARTESIAN_POINT('Ctrl Pts',(-74.1546864735166,-2.47652804724537,
12.));
#84592=CARTESIAN_POINT('Ctrl Pts',(-74.143376394138,-2.47097695564992,12.));
#84593=CARTESIAN_POINT('Ctrl Pts',(-74.127126454519,-2.46301176097117,12.));
#84594=CARTESIAN_POINT('Ctrl Pts',(-74.1059458420067,-2.45264924094775,
12.));
#84595=CARTESIAN_POINT('Ctrl Pts',(-74.0812573859411,-2.44059823356675,
12.));
#84596=CARTESIAN_POINT('Ctrl Pts',(-74.0565898079218,-2.42858510549778,
12.));
#84597=CARTESIAN_POINT('Ctrl Pts',(-74.0319431966989,-2.41660985465251,
12.));
#84598=CARTESIAN_POINT('Ctrl Pts',(-74.0073176459344,-2.40467247811536,
12.));
#84599=CARTESIAN_POINT('Ctrl Pts',(-73.9827132538206,-2.39277297220756,
12.));
#84600=CARTESIAN_POINT('Ctrl Pts',(-73.958130121465,-2.3809113327496,12.));
#84601=CARTESIAN_POINT('Ctrl Pts',(-73.9335683516404,-2.36908755526003,
12.));
#84602=CARTESIAN_POINT('Ctrl Pts',(-73.9090280474712,-2.35730163516315,
12.));
#84603=CARTESIAN_POINT('Ctrl Pts',(-73.8845093109274,-2.3455535680212,12.));
#84604=CARTESIAN_POINT('Ctrl Pts',(-73.8600122421468,-2.33384334963957,
12.));
#84605=CARTESIAN_POINT('Ctrl Pts',(-73.8355369402706,-2.32217097594197,
12.));
#84606=CARTESIAN_POINT('Ctrl Pts',(-73.8110835039327,-2.31053644289416,
12.));
#84607=CARTESIAN_POINT('Ctrl Pts',(-73.786652031885,-2.29893974640434,12.));
#84608=CARTESIAN_POINT('Ctrl Pts',(-73.762242623566,-2.28738088222863,12.));
#84609=CARTESIAN_POINT('Ctrl Pts',(-73.7378553796807,-2.27585984587198,
12.));
#84610=CARTESIAN_POINT('Ctrl Pts',(-73.7134904019389,-2.26437663263667,
12.));
#84611=CARTESIAN_POINT('Ctrl Pts',(-73.6891477928129,-2.25293123766425,
12.));
#84612=CARTESIAN_POINT('Ctrl Pts',(-73.6648276552767,-2.24152365597697,
12.));
#84613=CARTESIAN_POINT('Ctrl Pts',(-73.6405300925712,-2.23015388251287,
12.));
#84614=CARTESIAN_POINT('Ctrl Pts',(-73.6162552079038,-2.21882191216518,
12.));
#84615=CARTESIAN_POINT('Ctrl Pts',(-73.5920031044595,-2.20752773978348,
12.));
#84616=CARTESIAN_POINT('Ctrl Pts',(-73.5677738855452,-2.19627136015678,
12.));
#84617=CARTESIAN_POINT('Ctrl Pts',(-73.5435676546929,-2.18505276799753,
12.));
#84618=CARTESIAN_POINT('Ctrl Pts',(-73.5193845157708,-2.17387195792306,
12.));
#84619=CARTESIAN_POINT('Ctrl Pts',(-73.4952245731054,-2.16272892442919,
12.));
#84620=CARTESIAN_POINT('Ctrl Pts',(-73.4710879315382,-2.15162366187906,
12.));
#84621=CARTESIAN_POINT('Ctrl Pts',(-73.4469746963637,-2.14055616452057,
12.));
#84622=CARTESIAN_POINT('Ctrl Pts',(-73.4228849732925,-2.12952642649367,
12.));
#84623=CARTESIAN_POINT('Ctrl Pts',(-73.3988188684021,-2.11853444183761,
12.));
#84624=CARTESIAN_POINT('Ctrl Pts',(-73.3747764880893,-2.1075802044939,12.));
#84625=CARTESIAN_POINT('Ctrl Pts',(-73.3507579390239,-2.09666370830716,
12.));
#84626=CARTESIAN_POINT('Ctrl Pts',(-73.3267633281807,-2.08578494702743,
12.));
#84627=CARTESIAN_POINT('Ctrl Pts',(-73.3027927628626,-2.07494391430941,
12.));
#84628=CARTESIAN_POINT('Ctrl Pts',(-73.2788463507246,-2.06414060370834,
12.));
#84629=CARTESIAN_POINT('Ctrl Pts',(-73.2549241997953,-2.05337500867403,
12.));
#84630=CARTESIAN_POINT('Ctrl Pts',(-73.2310264184976,-2.04264712253928,
12.));
#84631=CARTESIAN_POINT('Ctrl Pts',(-73.2071531156504,-2.03195693852454,
12.));
#84632=CARTESIAN_POINT('Ctrl Pts',(-73.183304400462,-2.02130444974362,12.));
#84633=CARTESIAN_POINT('Ctrl Pts',(-73.1594803825252,-2.01068964920467,
12.));
#84634=CARTESIAN_POINT('Ctrl Pts',(-73.1356811718091,-2.00011252980981,
12.));
#84635=CARTESIAN_POINT('Ctrl Pts',(-73.1119068786475,-1.98957308434918,
12.));
#84636=CARTESIAN_POINT('Ctrl Pts',(-73.0881576137407,-1.97907130550157,
12.));
#84637=CARTESIAN_POINT('Ctrl Pts',(-73.0644334881673,-1.96860718583932,
12.));
#84638=CARTESIAN_POINT('Ctrl Pts',(-73.040734613391,-1.95818071782767,12.));
#84639=CARTESIAN_POINT('Ctrl Pts',(-73.0170611012661,-1.94779189382302,
12.));
#84640=CARTESIAN_POINT('Ctrl Pts',(-72.9934130640415,-1.93744070606566,
12.));
#84641=CARTESIAN_POINT('Ctrl Pts',(-72.9697906143636,-1.9271271466766,12.));
#84642=CARTESIAN_POINT('Ctrl Pts',(-72.9461938652811,-1.91685120766436,
12.));
#84643=CARTESIAN_POINT('Ctrl Pts',(-72.9226229302478,-1.90661288092587,
12.));
#84644=CARTESIAN_POINT('Ctrl Pts',(-72.8990779231226,-1.89641215824582,
12.));
#84645=CARTESIAN_POINT('Ctrl Pts',(-72.875558958168,-1.88624903129188,12.));
#84646=CARTESIAN_POINT('Ctrl Pts',(-72.8520661500477,-1.87612349160944,
12.));
#84647=CARTESIAN_POINT('Ctrl Pts',(-72.8285996138359,-1.86603553062771,
12.));
#84648=CARTESIAN_POINT('Ctrl Pts',(-72.8051594650222,-1.85598513966113,
12.));
#84649=CARTESIAN_POINT('Ctrl Pts',(-72.7817458195155,-1.84597230990857,
12.));
#84650=CARTESIAN_POINT('Ctrl Pts',(-72.7583587936447,-1.83599703244924,
12.));
#84651=CARTESIAN_POINT('Ctrl Pts',(-72.7349985041592,-1.82605929823564,
12.));
#84652=CARTESIAN_POINT('Ctrl Pts',(-72.7116650682344,-1.81615909809871,
12.));
#84653=CARTESIAN_POINT('Ctrl Pts',(-72.6883586034769,-1.8062964227505,12.));
#84654=CARTESIAN_POINT('Ctrl Pts',(-72.6650792279274,-1.79647126278358,
12.));
#84655=CARTESIAN_POINT('Ctrl Pts',(-72.6418270600619,-1.78668360866811,
12.));
#84656=CARTESIAN_POINT('Ctrl Pts',(-72.6186022187907,-1.77693345074426,
12.));
#84657=CARTESIAN_POINT('Ctrl Pts',(-72.5954048234638,-1.76722077922574,
12.));
#84658=CARTESIAN_POINT('Ctrl Pts',(-72.5722349938774,-1.75754558420344,
12.));
#84659=CARTESIAN_POINT('Ctrl Pts',(-72.5490928502769,-1.74790785564473,
12.));
#84660=CARTESIAN_POINT('Ctrl Pts',(-72.5259785133595,-1.73830758339125,
12.));
#84661=CARTESIAN_POINT('Ctrl Pts',(-72.5028921042721,-1.72874475715103,
12.));
#84662=CARTESIAN_POINT('Ctrl Pts',(-72.479833744618,-1.71921936650038,12.));
#84663=CARTESIAN_POINT('Ctrl Pts',(-72.456803556463,-1.70973140088841,12.));
#84664=CARTESIAN_POINT('Ctrl Pts',(-72.4338016623391,-1.70028084963647,
12.));
#84665=CARTESIAN_POINT('Ctrl Pts',(-72.4108281852467,-1.69086770193637,
12.));
#84666=CARTESIAN_POINT('Ctrl Pts',(-72.387883248654,-1.68149194684281,12.));
#84667=CARTESIAN_POINT('Ctrl Pts',(-72.3649669765004,-1.67215357327365,
12.));
#84668=CARTESIAN_POINT('Ctrl Pts',(-72.3420794932047,-1.66285257001496,
12.));
#84669=CARTESIAN_POINT('Ctrl Pts',(-72.319220923669,-1.65358892572062,12.));
#84670=CARTESIAN_POINT('Ctrl Pts',(-72.2963913932813,-1.64436262891079,
12.));
#84671=CARTESIAN_POINT('Ctrl Pts',(-72.2735910279149,-1.63517366796463,
12.));
#84672=CARTESIAN_POINT('Ctrl Pts',(-72.2508199539323,-1.6260220311193,12.));
#84673=CARTESIAN_POINT('Ctrl Pts',(-72.2280782981937,-1.6169077064754,12.));
#84674=CARTESIAN_POINT('Ctrl Pts',(-72.2053661880608,-1.60783068199663,
12.));
#84675=CARTESIAN_POINT('Ctrl Pts',(-72.1826837514001,-1.59879094550847,
12.));
#84676=CARTESIAN_POINT('Ctrl Pts',(-72.1600311165821,-1.58978848469123,
12.));
#84677=CARTESIAN_POINT('Ctrl Pts',(-72.1374084124839,-1.58082328707803,
12.));
#84678=CARTESIAN_POINT('Ctrl Pts',(-72.1148157684995,-1.5718953400604,12.));
#84679=CARTESIAN_POINT('Ctrl Pts',(-72.0922533145433,-1.56300463088808,
12.));
#84680=CARTESIAN_POINT('Ctrl Pts',(-72.0697211810545,-1.55415114666773,
12.));
#84681=CARTESIAN_POINT('Ctrl Pts',(-72.0472194989963,-1.54533487435626,
12.));
#84682=CARTESIAN_POINT('Ctrl Pts',(-72.0247483998579,-1.53655580075812,
12.));
#84683=CARTESIAN_POINT('Ctrl Pts',(-72.0023080156647,-1.52781391253102,
12.));
#84684=CARTESIAN_POINT('Ctrl Pts',(-71.979898478983,-1.51910919618566,12.));
#84685=CARTESIAN_POINT('Ctrl Pts',(-71.9575199229241,-1.51044163808453,
12.));
#84686=CARTESIAN_POINT('Ctrl Pts',(-71.9351724811443,-1.50181122443534,
12.));
#84687=CARTESIAN_POINT('Ctrl Pts',(-71.912856287848,-1.49321794128798,12.));
#84688=CARTESIAN_POINT('Ctrl Pts',(-71.8905714777961,-1.48466177454019,
12.));
#84689=CARTESIAN_POINT('Ctrl Pts',(-71.8683181863116,-1.47614270993728,
12.));
#84690=CARTESIAN_POINT('Ctrl Pts',(-71.8460965492839,-1.46766073307088,
12.));
#84691=CARTESIAN_POINT('Ctrl Pts',(-71.8239067031683,-1.45921582937231,
12.));
#84692=CARTESIAN_POINT('Ctrl Pts',(-71.8017487849895,-1.45080798410965,
12.));
#84693=CARTESIAN_POINT('Ctrl Pts',(-71.7796229323526,-1.44243718239315,
12.));
#84694=CARTESIAN_POINT('Ctrl Pts',(-71.7575292834469,-1.43410340917495,
12.));
#84695=CARTESIAN_POINT('Ctrl Pts',(-71.7354679770528,-1.42580664924769,
12.));
#84696=CARTESIAN_POINT('Ctrl Pts',(-71.7134391525389,-1.41754688723773,
12.));
#84697=CARTESIAN_POINT('Ctrl Pts',(-71.6914429498663,-1.40932410760248,
12.));
#84698=CARTESIAN_POINT('Ctrl Pts',(-71.6694795096001,-1.40113829463576,
12.));
#84699=CARTESIAN_POINT('Ctrl Pts',(-71.6475489729134,-1.39298943246722,
12.));
#84700=CARTESIAN_POINT('Ctrl Pts',(-71.625651481593,-1.38487750506082,12.));
#84701=CARTESIAN_POINT('Ctrl Pts',(-71.6037871780385,-1.37680249620779,
12.));
#84702=CARTESIAN_POINT('Ctrl Pts',(-71.5819562052663,-1.36876438952465,
12.));
#84703=CARTESIAN_POINT('Ctrl Pts',(-71.5601587069217,-1.36076316845816,
12.));
#84704=CARTESIAN_POINT('Ctrl Pts',(-71.5383948272845,-1.35279881628455,
12.));
#84705=CARTESIAN_POINT('Ctrl Pts',(-71.516664711275,-1.3448713161078,12.));
#84706=CARTESIAN_POINT('Ctrl Pts',(-71.4949685044522,-1.33698065085219,
12.));
#84707=CARTESIAN_POINT('Ctrl Pts',(-71.4733063530187,-1.32912680326123,
12.));
#84708=CARTESIAN_POINT('Ctrl Pts',(-71.4516784038317,-1.32130975590226,
12.));
#84709=CARTESIAN_POINT('Ctrl Pts',(-71.4300848044087,-1.31352949116537,
12.));
#84710=CARTESIAN_POINT('Ctrl Pts',(-71.4085257029322,-1.30578599126139,
12.));
#84711=CARTESIAN_POINT('Ctrl Pts',(-71.3870012482499,-1.29807923821413,
12.));
#84712=CARTESIAN_POINT('Ctrl Pts',(-71.3655115898827,-1.29040921386059,
12.));
#84713=CARTESIAN_POINT('Ctrl Pts',(-71.3440568780347,-1.28277589985471,
12.));
#84714=CARTESIAN_POINT('Ctrl Pts',(-71.3226372635996,-1.27517927766608,
12.));
#84715=CARTESIAN_POINT('Ctrl Pts',(-71.3012528981661,-1.26761932857724,
12.));
#84716=CARTESIAN_POINT('Ctrl Pts',(-71.2799039340175,-1.2600960336757,12.));
#84717=CARTESIAN_POINT('Ctrl Pts',(-71.2585905241406,-1.25260937385568,
12.));
#84718=CARTESIAN_POINT('Ctrl Pts',(-71.2373128222352,-1.24515932982112,
12.));
#84719=CARTESIAN_POINT('Ctrl Pts',(-71.2160709827191,-1.23774588208427,
12.));
#84720=CARTESIAN_POINT('Ctrl Pts',(-71.194865160732,-1.23036901096239,12.));
#84721=CARTESIAN_POINT('Ctrl Pts',(-71.1736955121362,-1.22302869657017,
12.));
#84722=CARTESIAN_POINT('Ctrl Pts',(-71.1525621935267,-1.21572491882262,
12.));
#84723=CARTESIAN_POINT('Ctrl Pts',(-71.1314653622442,-1.20845765743647,
12.));
#84724=CARTESIAN_POINT('Ctrl Pts',(-71.1104051763839,-1.20122689192836,
12.));
#84725=CARTESIAN_POINT('Ctrl Pts',(-71.089381794801,-1.19403260161002,12.));
#84726=CARTESIAN_POINT('Ctrl Pts',(-71.0683953771149,-1.18687476558133,
12.));
#84727=CARTESIAN_POINT('Ctrl Pts',(-71.0474460837159,-1.17975336273504,
12.));
#84728=CARTESIAN_POINT('Ctrl Pts',(-71.0265340757699,-1.17266837175777,
12.));
#84729=CARTESIAN_POINT('Ctrl Pts',(-71.0056595152204,-1.1656197711288,12.));
#84730=CARTESIAN_POINT('Ctrl Pts',(-70.9848225647871,-1.15860753911485,
12.));
#84731=CARTESIAN_POINT('Ctrl Pts',(-70.9640233879659,-1.15163165376524,
12.));
#84732=CARTESIAN_POINT('Ctrl Pts',(-70.9432621490566,-1.14469209291488,
12.));
#84733=CARTESIAN_POINT('Ctrl Pts',(-70.9225390131826,-1.13778883418213,
12.));
#84734=CARTESIAN_POINT('Ctrl Pts',(-70.9018541463089,-1.13092185496564,
12.));
#84735=CARTESIAN_POINT('Ctrl Pts',(-70.8812077152586,-1.12409113243513,
12.));
#84736=CARTESIAN_POINT('Ctrl Pts',(-70.8605998877149,-1.11729664352992,
12.));
#84737=CARTESIAN_POINT('Ctrl Pts',(-70.8400308322037,-1.11053836496639,
12.));
#84738=CARTESIAN_POINT('Ctrl Pts',(-70.8195007180745,-1.10381627323946,
12.));
#84739=CARTESIAN_POINT('Ctrl Pts',(-70.799009715484,-1.09713034462265,12.));
#84740=CARTESIAN_POINT('Ctrl Pts',(-70.7785579953583,-1.09048055516426,
12.));
#84741=CARTESIAN_POINT('Ctrl Pts',(-70.7581457294447,-1.08386688068342,
12.));
#84742=CARTESIAN_POINT('Ctrl Pts',(-70.7377730903953,-1.07728929676408,
12.));
#84743=CARTESIAN_POINT('Ctrl Pts',(-70.7174402518378,-1.07074777874595,
12.));
#84744=CARTESIAN_POINT('Ctrl Pts',(-70.6971473884459,-1.0642423017128,12.));
#84745=CARTESIAN_POINT('Ctrl Pts',(-70.676894676009,-1.0577728404773,12.));
#84746=CARTESIAN_POINT('Ctrl Pts',(-70.6566822912991,-1.05133936960071,
12.));
#84747=CARTESIAN_POINT('Ctrl Pts',(-70.6365104119252,-1.04494186341156,
12.));
#84748=CARTESIAN_POINT('Ctrl Pts',(-70.6163792162073,-1.03858029601903,
12.));
#84749=CARTESIAN_POINT('Ctrl Pts',(-70.5962888829934,-1.0322546413287,12.));
#84750=CARTESIAN_POINT('Ctrl Pts',(-70.5762395916377,-1.02596487304048,
12.));
#84751=CARTESIAN_POINT('Ctrl Pts',(-70.556231522419,-1.01971096460597,12.));
#84752=CARTESIAN_POINT('Ctrl Pts',(-70.5362648569061,-1.01349288918537,
12.));
#84753=CARTESIAN_POINT('Ctrl Pts',(-70.5163397782713,-1.00731061960968,
12.));
#84754=CARTESIAN_POINT('Ctrl Pts',(-70.4964564717953,-1.00116412831442,
12.));
#84755=CARTESIAN_POINT('Ctrl Pts',(-70.4766151245212,-0.995053387379752,
12.));
#84756=CARTESIAN_POINT('Ctrl Pts',(-70.4568159243163,-0.988978368643646,
12.));
#84757=CARTESIAN_POINT('Ctrl Pts',(-70.4370590590842,-0.982939043792151,
12.));
#84758=CARTESIAN_POINT('Ctrl Pts',(-70.417344715957,-0.976935384450037,
12.));
#84759=CARTESIAN_POINT('Ctrl Pts',(-70.3976730803614,-0.970967362281171,
12.));
#84760=CARTESIAN_POINT('Ctrl Pts',(-70.3780443377956,-0.965034948786444,
12.));
#84761=CARTESIAN_POINT('Ctrl Pts',(-70.3584586759536,-0.959138115058827,
12.));
#84762=CARTESIAN_POINT('Ctrl Pts',(-70.338916286458,-0.953276831581238,
12.));
#84763=CARTESIAN_POINT('Ctrl Pts',(-70.3194173673674,-0.9474510679296,12.));
#84764=CARTESIAN_POINT('Ctrl Pts',(-70.299962123399,-0.941660792742975,
12.));
#84765=CARTESIAN_POINT('Ctrl Pts',(-70.2805507606872,-0.935905974336476,
12.));
#84766=CARTESIAN_POINT('Ctrl Pts',(-70.2611834821724,-0.930186581235545,
12.));
#84767=CARTESIAN_POINT('Ctrl Pts',(-70.2418604835837,-0.924502582639452,
12.));
#84768=CARTESIAN_POINT('Ctrl Pts',(-70.2225819470248,-0.918853949157115,
12.));
#84769=CARTESIAN_POINT('Ctrl Pts',(-70.2033480471676,-0.913240652090975,
12.));
#84770=CARTESIAN_POINT('Ctrl Pts',(-70.1841589635574,-0.907662662015781,
12.));
#84771=CARTESIAN_POINT('Ctrl Pts',(-70.1650148905109,-0.902119947629767,
12.));
#84772=CARTESIAN_POINT('Ctrl Pts',(-70.1459160490446,-0.89661247437184,
12.));
#84773=CARTESIAN_POINT('Ctrl Pts',(-70.1268626950175,-0.891140203464239,
12.));
#84774=CARTESIAN_POINT('Ctrl Pts',(-70.1078550938958,-0.885703094802532,
12.));
#84775=CARTESIAN_POINT('Ctrl Pts',(-70.0888934967855,-0.880301109660725,
12.));
#84776=CARTESIAN_POINT('Ctrl Pts',(-70.0699781183935,-0.874934213255836,
12.));
#84777=CARTESIAN_POINT('Ctrl Pts',(-70.051109108301,-0.86960237787112,12.));
#84778=CARTESIAN_POINT('Ctrl Pts',(-70.0322865492925,-0.864305583661541,
12.));
#84779=CARTESIAN_POINT('Ctrl Pts',(-70.0172656933806,-0.860096170668732,
12.));
#84780=CARTESIAN_POINT('Ctrl Pts',(-70.0060209754087,-0.856954870259201,
12.));
#84781=CARTESIAN_POINT('Ctrl Pts',(-69.9985337959407,-0.854867673848592,
12.));
#84782=CARTESIAN_POINT('Ctrl Pts',(-69.9947925310006,-0.85382582660898,
12.));
#84783=CARTESIAN_POINT('Ctrl Pts',(-74.0964320766209,-3.99277406490865,
-5.55111512312578E-16));
#84784=CARTESIAN_POINT('Ctrl Pts',(-74.0964320766209,-3.99277406490865,
4.));
#84785=CARTESIAN_POINT('Ctrl Pts',(-74.0964320766209,-3.99277406490865,
8.));
#84786=CARTESIAN_POINT('Ctrl Pts',(-74.0964320766209,-3.99277406490865,
12.));
#84787=CARTESIAN_POINT('Ctrl Pts',(-74.1989040313894,-3.95310474582224,
-5.55111512312578E-16));
#84788=CARTESIAN_POINT('Ctrl Pts',(-74.1989040313894,-3.95310474582224,
3.99999999999999));
#84789=CARTESIAN_POINT('Ctrl Pts',(-74.1989040313895,-3.95310474582224,
8.));
#84790=CARTESIAN_POINT('Ctrl Pts',(-74.1989040313895,-3.95310474582224,
12.));
#84791=CARTESIAN_POINT('Ctrl Pts',(-74.3538917248567,-3.82252142018526,
-5.55111512312578E-16));
#84792=CARTESIAN_POINT('Ctrl Pts',(-74.3538917248567,-3.82252142018526,
4.00000000000001));
#84793=CARTESIAN_POINT('Ctrl Pts',(-74.3538917248567,-3.82252142018526,
7.99999999999998));
#84794=CARTESIAN_POINT('Ctrl Pts',(-74.3538917248567,-3.82252142018526,
12.));
#84795=CARTESIAN_POINT('Ctrl Pts',(-74.41142867521,-3.63264011802866,-5.55111512312578E-16));
#84796=CARTESIAN_POINT('Ctrl Pts',(-74.41142867521,-3.63264011802866,3.99999999999999));
#84797=CARTESIAN_POINT('Ctrl Pts',(-74.41142867521,-3.63264011802866,8.00000000000001));
#84798=CARTESIAN_POINT('Ctrl Pts',(-74.41142867521,-3.63264011802866,12.));
#84799=CARTESIAN_POINT('Ctrl Pts',(-74.4153560388999,-3.55032190142802,
-5.55111512312578E-16));
#84800=CARTESIAN_POINT('Ctrl Pts',(-74.4153560388999,-3.55032190142802,
4.));
#84801=CARTESIAN_POINT('Ctrl Pts',(-74.4153560388999,-3.55032190142802,
8.));
#84802=CARTESIAN_POINT('Ctrl Pts',(-74.4153560388999,-3.55032190142802,
12.));
#84803=CARTESIAN_POINT('',(-74.0964320766209,-3.99277406490865,0.));
#84804=CARTESIAN_POINT('',(-74.4153560388999,-3.55032190142802,-2.77555756156289E-16));
#84805=CARTESIAN_POINT('Ctrl Pts',(-74.0964320766209,-3.99277406490865,
-1.23259516440783E-31));
#84806=CARTESIAN_POINT('Ctrl Pts',(-74.1989040313894,-3.95310474582224,
-8.16594296420187E-31));
#84807=CARTESIAN_POINT('Ctrl Pts',(-74.2874684276565,-3.87848570260111,
3.85185988877447E-31));
#84808=CARTESIAN_POINT('Ctrl Pts',(-74.3442121731107,-3.78450405480215,
1.54074395550979E-31));
#84809=CARTESIAN_POINT('Ctrl Pts',(-74.3867699822014,-3.71401781895292,
-3.08148791101957E-32));
#84810=CARTESIAN_POINT('Ctrl Pts',(-74.41142867521,-3.63264011802866,-1.07852076885685E-30));
#84811=CARTESIAN_POINT('Ctrl Pts',(-74.4153560388999,-3.55032190142802,
-7.70371977754892E-32));
#84812=CARTESIAN_POINT('',(-74.4153560388999,-3.55032190142802,12.));
#84813=CARTESIAN_POINT('Ctrl Pts',(-74.4153560388999,-3.55032190142802,
-5.55111512312578E-16));
#84814=CARTESIAN_POINT('Ctrl Pts',(-74.4153560388999,-3.55032190142802,
4.));
#84815=CARTESIAN_POINT('Ctrl Pts',(-74.4153560388999,-3.55032190142802,
8.));
#84816=CARTESIAN_POINT('Ctrl Pts',(-74.4153560388999,-3.55032190142802,
12.));
#84817=CARTESIAN_POINT('',(-74.0964320766209,-3.99277406490864,12.));
#84818=CARTESIAN_POINT('Ctrl Pts',(-74.4153560388999,-3.55032190142802,
12.));
#84819=CARTESIAN_POINT('Ctrl Pts',(-74.41142867521,-3.63264011802866,12.));
#84820=CARTESIAN_POINT('Ctrl Pts',(-74.3867699822014,-3.71401781895292,
12.));
#84821=CARTESIAN_POINT('Ctrl Pts',(-74.3442121731107,-3.78450405480214,
12.));
#84822=CARTESIAN_POINT('Ctrl Pts',(-74.2874684276565,-3.87848570260111,
12.));
#84823=CARTESIAN_POINT('Ctrl Pts',(-74.1989040313895,-3.95310474582224,
12.));
#84824=CARTESIAN_POINT('Ctrl Pts',(-74.0964320766209,-3.99277406490865,
12.));
#84825=CARTESIAN_POINT('Ctrl Pts',(-74.0964320766209,-3.99277406490865,
12.));
#84826=CARTESIAN_POINT('Ctrl Pts',(-74.0964320766209,-3.99277406490865,
8.));
#84827=CARTESIAN_POINT('Ctrl Pts',(-74.0964320766209,-3.99277406490865,
4.));
#84828=CARTESIAN_POINT('Ctrl Pts',(-74.0964320766209,-3.99277406490865,
-5.55111512312578E-16));
#84829=CARTESIAN_POINT('Origin',(-3.74482667098164E-10,-1.64496194443586E-11,
0.));
#84830=CARTESIAN_POINT('Origin',(-3.74482667098164E-10,-1.64496194443586E-11,
12.));
#84831=CARTESIAN_POINT('Origin',(-3.74482667098164E-10,-1.64496194443586E-11,
0.));
#84832=CARTESIAN_POINT('Ctrl Pts',(-74.4153560389001,3.55032190142523,0.));
#84833=CARTESIAN_POINT('Ctrl Pts',(-74.4153560389001,3.55032190142523,4.));
#84834=CARTESIAN_POINT('Ctrl Pts',(-74.4153560389001,3.55032190142524,8.));
#84835=CARTESIAN_POINT('Ctrl Pts',(-74.4153560389001,3.55032190142524,12.));
#84836=CARTESIAN_POINT('Ctrl Pts',(-74.4101195539797,3.66007952356786,0.));
#84837=CARTESIAN_POINT('Ctrl Pts',(-74.4101195539797,3.66007952356786,4.));
#84838=CARTESIAN_POINT('Ctrl Pts',(-74.4101195539797,3.66007952356787,8.00000000000001));
#84839=CARTESIAN_POINT('Ctrl Pts',(-74.4101195539797,3.66007952356787,12.));
#84840=CARTESIAN_POINT('Ctrl Pts',(-74.3352361483148,3.84840282419241,-7.30790067565468E-17));
#84841=CARTESIAN_POINT('Ctrl Pts',(-74.3352361483148,3.84840282419241,4.));
#84842=CARTESIAN_POINT('Ctrl Pts',(-74.3352361483148,3.84840282419244,7.99999999999999));
#84843=CARTESIAN_POINT('Ctrl Pts',(-74.3352361483148,3.84840282419244,12.));
#84844=CARTESIAN_POINT('Ctrl Pts',(-74.1732860426647,3.96302207561163,-2.46611180232189E-16));
#84845=CARTESIAN_POINT('Ctrl Pts',(-74.1732860426647,3.96302207561163,4.));
#84846=CARTESIAN_POINT('Ctrl Pts',(-74.1732860426647,3.96302207561166,8.00000000000001));
#84847=CARTESIAN_POINT('Ctrl Pts',(-74.1732860426647,3.96302207561166,12.));
#84848=CARTESIAN_POINT('Ctrl Pts',(-74.0964320765798,3.99277406492194,-3.30265160469534E-16));
#84849=CARTESIAN_POINT('Ctrl Pts',(-74.0964320765798,3.99277406492194,4.));
#84850=CARTESIAN_POINT('Ctrl Pts',(-74.0964320765798,3.99277406492197,8.));
#84851=CARTESIAN_POINT('Ctrl Pts',(-74.0964320765798,3.99277406492197,12.));
#84852=CARTESIAN_POINT('',(-74.4153560389001,3.55032190142523,0.));
#84853=CARTESIAN_POINT('',(-74.0964320765797,3.9927740649218,0.));
#84854=CARTESIAN_POINT('Ctrl Pts',(-74.4153560389001,3.55032190142523,2.74425517504379E-17));
#84855=CARTESIAN_POINT('Ctrl Pts',(-74.4101195539797,3.66007952356786,2.74425517504379E-17));
#84856=CARTESIAN_POINT('Ctrl Pts',(-74.3673290364569,3.76769283821046,-1.43168806818745E-17));
#84857=CARTESIAN_POINT('Ctrl Pts',(-74.2961085760818,3.85123952454111,-8.88773471449119E-17));
#84858=CARTESIAN_POINT('Ctrl Pts',(-74.2426932308005,3.91389953928911,-1.4479769699219E-16));
#84859=CARTESIAN_POINT('Ctrl Pts',(-74.1732860426647,3.96302207561163,-2.19168628481751E-16));
#84860=CARTESIAN_POINT('Ctrl Pts',(-74.0964320765798,3.99277406492194,-3.02822608719096E-16));
#84861=CARTESIAN_POINT('',(-74.0964320765797,3.99277406492181,12.));
#84862=CARTESIAN_POINT('Ctrl Pts',(-74.0964320765798,3.99277406492194,-3.30265160469534E-16));
#84863=CARTESIAN_POINT('Ctrl Pts',(-74.0964320765798,3.99277406492194,4.));
#84864=CARTESIAN_POINT('Ctrl Pts',(-74.0964320765798,3.99277406492197,8.));
#84865=CARTESIAN_POINT('Ctrl Pts',(-74.0964320765798,3.99277406492197,12.));
#84866=CARTESIAN_POINT('',(-74.4153560389001,3.55032190142524,12.));
#84867=CARTESIAN_POINT('Ctrl Pts',(-74.0964320765798,3.99277406492197,12.));
#84868=CARTESIAN_POINT('Ctrl Pts',(-74.1732860426647,3.96302207561166,12.));
#84869=CARTESIAN_POINT('Ctrl Pts',(-74.2426932308005,3.91389953928914,12.));
#84870=CARTESIAN_POINT('Ctrl Pts',(-74.2961085760818,3.85123952454114,12.));
#84871=CARTESIAN_POINT('Ctrl Pts',(-74.3673290364569,3.76769283821048,12.));
#84872=CARTESIAN_POINT('Ctrl Pts',(-74.4101195539797,3.66007952356787,12.));
#84873=CARTESIAN_POINT('Ctrl Pts',(-74.4153560389001,3.55032190142524,12.));
#84874=CARTESIAN_POINT('Ctrl Pts',(-74.4153560389001,3.55032190142524,12.));
#84875=CARTESIAN_POINT('Ctrl Pts',(-74.4153560389001,3.55032190142524,8.));
#84876=CARTESIAN_POINT('Ctrl Pts',(-74.4153560389001,3.55032190142523,4.));
#84877=CARTESIAN_POINT('Ctrl Pts',(-74.4153560389001,3.55032190142523,0.));
#84878=CARTESIAN_POINT('Ctrl Pts',(-69.8028570375097,5.24987136994592,0.));
#84879=CARTESIAN_POINT('Ctrl Pts',(-69.8028570375097,5.24987136994592,12.));
#84880=CARTESIAN_POINT('Ctrl Pts',(-69.8066748687772,5.24915955997427,0.));
#84881=CARTESIAN_POINT('Ctrl Pts',(-69.8066748687772,5.24915955997427,12.));
#84882=CARTESIAN_POINT('Ctrl Pts',(-69.8143154684204,5.24773285666376,0.));
#84883=CARTESIAN_POINT('Ctrl Pts',(-69.8143154684204,5.24773285666376,12.));
#84884=CARTESIAN_POINT('Ctrl Pts',(-69.8257911792159,5.2455835515975,0.));
#84885=CARTESIAN_POINT('Ctrl Pts',(-69.8257911792159,5.2455835515975,12.));
#84886=CARTESIAN_POINT('Ctrl Pts',(-69.841121750752,5.24269931054569,0.));
#84887=CARTESIAN_POINT('Ctrl Pts',(-69.841121750752,5.24269931054569,12.));
#84888=CARTESIAN_POINT('Ctrl Pts',(-69.8603343302743,5.23906316634802,0.));
#84889=CARTESIAN_POINT('Ctrl Pts',(-69.8603343302743,5.23906316634802,12.));
#84890=CARTESIAN_POINT('Ctrl Pts',(-69.8795962381599,5.2353961627962,0.));
#84891=CARTESIAN_POINT('Ctrl Pts',(-69.8795962381599,5.2353961627962,12.));
#84892=CARTESIAN_POINT('Ctrl Pts',(-69.8989073936688,5.23169827290555,0.));
#84893=CARTESIAN_POINT('Ctrl Pts',(-69.8989073936688,5.23169827290555,12.));
#84894=CARTESIAN_POINT('Ctrl Pts',(-69.9182676502048,5.22796945602793,0.));
#84895=CARTESIAN_POINT('Ctrl Pts',(-69.9182676502048,5.22796945602793,12.));
#84896=CARTESIAN_POINT('Ctrl Pts',(-69.9376767969095,5.22420965879981,0.));
#84897=CARTESIAN_POINT('Ctrl Pts',(-69.9376767969095,5.22420965879981,12.));
#84898=CARTESIAN_POINT('Ctrl Pts',(-69.9571345870076,5.2204188207572,0.));
#84899=CARTESIAN_POINT('Ctrl Pts',(-69.9571345870076,5.2204188207572,12.));
#84900=CARTESIAN_POINT('Ctrl Pts',(-69.9766407595385,5.21659687881139,0.));
#84901=CARTESIAN_POINT('Ctrl Pts',(-69.9766407595385,5.21659687881139,12.));
#84902=CARTESIAN_POINT('Ctrl Pts',(-69.9961950629965,5.21274377203259,0.));
#84903=CARTESIAN_POINT('Ctrl Pts',(-69.9961950629965,5.21274377203259,12.));
#84904=CARTESIAN_POINT('Ctrl Pts',(-70.0157972802182,5.20885944672836,0.));
#84905=CARTESIAN_POINT('Ctrl Pts',(-70.0157972802182,5.20885944672836,12.));
#84906=CARTESIAN_POINT('Ctrl Pts',(-70.0354472203546,5.20494385478025,0.));
#84907=CARTESIAN_POINT('Ctrl Pts',(-70.0354472203546,5.20494385478025,12.));
#84908=CARTESIAN_POINT('Ctrl Pts',(-70.0551447071082,5.20099695122656,0.));
#84909=CARTESIAN_POINT('Ctrl Pts',(-70.0551447071082,5.20099695122656,12.));
#84910=CARTESIAN_POINT('Ctrl Pts',(-70.0748895689729,5.19701869225528,0.));
#84911=CARTESIAN_POINT('Ctrl Pts',(-70.0748895689729,5.19701869225528,12.));
#84912=CARTESIAN_POINT('Ctrl Pts',(-70.0946816270997,5.19300903271579,0.));
#84913=CARTESIAN_POINT('Ctrl Pts',(-70.0946816270997,5.19300903271579,12.));
#84914=CARTESIAN_POINT('Ctrl Pts',(-70.1145206891885,5.18896792486565,0.));
#84915=CARTESIAN_POINT('Ctrl Pts',(-70.1145206891885,5.18896792486565,12.));
#84916=CARTESIAN_POINT('Ctrl Pts',(-70.1344065558145,5.18489531966264,0.));
#84917=CARTESIAN_POINT('Ctrl Pts',(-70.1344065558145,5.18489531966264,12.));
#84918=CARTESIAN_POINT('Ctrl Pts',(-70.1543390243892,5.18079116757666,0.));
#84919=CARTESIAN_POINT('Ctrl Pts',(-70.1543390243892,5.18079116757666,12.));
#84920=CARTESIAN_POINT('Ctrl Pts',(-70.1743178937077,5.17665541952382,0.));
#84921=CARTESIAN_POINT('Ctrl Pts',(-70.1743178937077,5.17665541952382,12.));
#84922=CARTESIAN_POINT('Ctrl Pts',(-70.1943429691167,5.17248802793389,0.));
#84923=CARTESIAN_POINT('Ctrl Pts',(-70.1943429691167,5.17248802793389,12.));
#84924=CARTESIAN_POINT('Ctrl Pts',(-70.2144140622953,5.16828894670108,0.));
#84925=CARTESIAN_POINT('Ctrl Pts',(-70.2144140622953,5.16828894670108,12.));
#84926=CARTESIAN_POINT('Ctrl Pts',(-70.2345309887833,5.16405813066976,0.));
#84927=CARTESIAN_POINT('Ctrl Pts',(-70.2345309887833,5.16405813066976,12.));
#84928=CARTESIAN_POINT('Ctrl Pts',(-70.2546935662722,5.15979553528203,0.));
#84929=CARTESIAN_POINT('Ctrl Pts',(-70.2546935662722,5.15979553528203,12.));
#84930=CARTESIAN_POINT('Ctrl Pts',(-70.2749016125105,5.15550111614859,0.));
#84931=CARTESIAN_POINT('Ctrl Pts',(-70.2749016125105,5.15550111614859,12.));
#84932=CARTESIAN_POINT('Ctrl Pts',(-70.2951549435512,5.15117482869254,0.));
#84933=CARTESIAN_POINT('Ctrl Pts',(-70.2951549435512,5.15117482869254,12.));
#84934=CARTESIAN_POINT('Ctrl Pts',(-70.3154533746736,5.1468166283308,0.));
#84935=CARTESIAN_POINT('Ctrl Pts',(-70.3154533746736,5.1468166283308,12.));
#84936=CARTESIAN_POINT('Ctrl Pts',(-70.3357967211796,5.14242647063479,0.));
#84937=CARTESIAN_POINT('Ctrl Pts',(-70.3357967211796,5.14242647063479,12.));
#84938=CARTESIAN_POINT('Ctrl Pts',(-70.3561847991714,5.13800431148903,0.));
#84939=CARTESIAN_POINT('Ctrl Pts',(-70.3561847991714,5.13800431148903,12.));
#84940=CARTESIAN_POINT('Ctrl Pts',(-70.3766174264757,5.13355010728567,0.));
#84941=CARTESIAN_POINT('Ctrl Pts',(-70.3766174264757,5.13355010728567,12.));
#84942=CARTESIAN_POINT('Ctrl Pts',(-70.3970944229851,5.12906381499456,0.));
#84943=CARTESIAN_POINT('Ctrl Pts',(-70.3970944229851,5.12906381499456,12.));
#84944=CARTESIAN_POINT('Ctrl Pts',(-70.417615610161,5.12454539205328,0.));
#84945=CARTESIAN_POINT('Ctrl Pts',(-70.417615610161,5.12454539205328,12.));
#84946=CARTESIAN_POINT('Ctrl Pts',(-70.4381808107245,5.11999479630211,0.));
#84947=CARTESIAN_POINT('Ctrl Pts',(-70.4381808107245,5.11999479630211,12.));
#84948=CARTESIAN_POINT('Ctrl Pts',(-70.458789848296,5.11541198590932,0.));
#84949=CARTESIAN_POINT('Ctrl Pts',(-70.458789848296,5.11541198590932,12.));
#84950=CARTESIAN_POINT('Ctrl Pts',(-70.4794425469825,5.11079691929213,0.));
#84951=CARTESIAN_POINT('Ctrl Pts',(-70.4794425469825,5.11079691929213,12.));
#84952=CARTESIAN_POINT('Ctrl Pts',(-70.500138731399,5.10614955511663,0.));
#84953=CARTESIAN_POINT('Ctrl Pts',(-70.500138731399,5.10614955511663,12.));
#84954=CARTESIAN_POINT('Ctrl Pts',(-70.5208782268497,5.1014698523294,0.));
#84955=CARTESIAN_POINT('Ctrl Pts',(-70.5208782268497,5.1014698523294,12.));
#84956=CARTESIAN_POINT('Ctrl Pts',(-70.5416608594526,5.09675777018182,0.));
#84957=CARTESIAN_POINT('Ctrl Pts',(-70.5416608594526,5.09675777018182,12.));
#84958=CARTESIAN_POINT('Ctrl Pts',(-70.5624864562824,5.09201326826134,0.));
#84959=CARTESIAN_POINT('Ctrl Pts',(-70.5624864562824,5.09201326826134,12.));
#84960=CARTESIAN_POINT('Ctrl Pts',(-70.5833548455014,5.08723630652272,0.));
#84961=CARTESIAN_POINT('Ctrl Pts',(-70.5833548455014,5.08723630652272,12.));
#84962=CARTESIAN_POINT('Ctrl Pts',(-70.6042658562923,5.08242684526686,0.));
#84963=CARTESIAN_POINT('Ctrl Pts',(-70.6042658562923,5.08242684526686,12.));
#84964=CARTESIAN_POINT('Ctrl Pts',(-70.6252193187878,5.07758484512302,0.));
#84965=CARTESIAN_POINT('Ctrl Pts',(-70.6252193187878,5.07758484512302,12.));
#84966=CARTESIAN_POINT('Ctrl Pts',(-70.6462150640015,5.07271026703354,0.));
#84967=CARTESIAN_POINT('Ctrl Pts',(-70.6462150640015,5.07271026703354,12.));
#84968=CARTESIAN_POINT('Ctrl Pts',(-70.6672529237455,5.06780307224071,0.));
#84969=CARTESIAN_POINT('Ctrl Pts',(-70.6672529237455,5.06780307224071,12.));
#84970=CARTESIAN_POINT('Ctrl Pts',(-70.6883327305784,5.06286322227819,0.));
#84971=CARTESIAN_POINT('Ctrl Pts',(-70.6883327305784,5.06286322227819,12.));
#84972=CARTESIAN_POINT('Ctrl Pts',(-70.7094543178438,5.05789067897057,0.));
#84973=CARTESIAN_POINT('Ctrl Pts',(-70.7094543178438,5.05789067897057,12.));
#84974=CARTESIAN_POINT('Ctrl Pts',(-70.7306175196863,5.05288540443482,0.));
#84975=CARTESIAN_POINT('Ctrl Pts',(-70.7306175196863,5.05288540443482,12.));
#84976=CARTESIAN_POINT('Ctrl Pts',(-70.7518221710706,5.04784736108346,0.));
#84977=CARTESIAN_POINT('Ctrl Pts',(-70.7518221710706,5.04784736108346,12.));
#84978=CARTESIAN_POINT('Ctrl Pts',(-70.7730681077983,5.04277651163349,0.));
#84979=CARTESIAN_POINT('Ctrl Pts',(-70.7730681077983,5.04277651163349,12.));
#84980=CARTESIAN_POINT('Ctrl Pts',(-70.7943551665059,5.03767281910479,0.));
#84981=CARTESIAN_POINT('Ctrl Pts',(-70.7943551665059,5.03767281910479,12.));
#84982=CARTESIAN_POINT('Ctrl Pts',(-70.8156831846488,5.0325362468094,0.));
#84983=CARTESIAN_POINT('Ctrl Pts',(-70.8156831846488,5.0325362468094,12.));
#84984=CARTESIAN_POINT('Ctrl Pts',(-70.8370520004843,5.02736675834692,0.));
#84985=CARTESIAN_POINT('Ctrl Pts',(-70.8370520004843,5.02736675834692,12.));
#84986=CARTESIAN_POINT('Ctrl Pts',(-70.8584614530519,5.0221643176006,0.));
#84987=CARTESIAN_POINT('Ctrl Pts',(-70.8584614530519,5.0221643176006,12.));
#84988=CARTESIAN_POINT('Ctrl Pts',(-70.8799113821452,5.0169288887379,0.));
#84989=CARTESIAN_POINT('Ctrl Pts',(-70.8799113821452,5.0169288887379,12.));
#84990=CARTESIAN_POINT('Ctrl Pts',(-70.9014016283124,5.01166043620567,0.));
#84991=CARTESIAN_POINT('Ctrl Pts',(-70.9014016283124,5.01166043620567,12.));
#84992=CARTESIAN_POINT('Ctrl Pts',(-70.9229320328589,5.00635892472513,0.));
#84993=CARTESIAN_POINT('Ctrl Pts',(-70.9229320328589,5.00635892472513,12.));
#84994=CARTESIAN_POINT('Ctrl Pts',(-70.9445024378439,5.00102431929039,0.));
#84995=CARTESIAN_POINT('Ctrl Pts',(-70.9445024378439,5.00102431929039,12.));
#84996=CARTESIAN_POINT('Ctrl Pts',(-70.9661126860773,4.99565658516913,0.));
#84997=CARTESIAN_POINT('Ctrl Pts',(-70.9661126860773,4.99565658516913,12.));
#84998=CARTESIAN_POINT('Ctrl Pts',(-70.9877626211113,4.99025568790664,0.));
#84999=CARTESIAN_POINT('Ctrl Pts',(-70.9877626211113,4.99025568790664,12.));
#85000=CARTESIAN_POINT('Ctrl Pts',(-71.0094520872377,4.98482159331863,0.));
#85001=CARTESIAN_POINT('Ctrl Pts',(-71.0094520872377,4.98482159331863,12.));
#85002=CARTESIAN_POINT('Ctrl Pts',(-71.0311809294821,4.97935426748584,0.));
#85003=CARTESIAN_POINT('Ctrl Pts',(-71.0311809294821,4.97935426748584,12.));
#85004=CARTESIAN_POINT('Ctrl Pts',(-71.0529489935961,4.97385367675158,0.));
#85005=CARTESIAN_POINT('Ctrl Pts',(-71.0529489935961,4.97385367675158,12.));
#85006=CARTESIAN_POINT('Ctrl Pts',(-71.0747561260436,4.9683197877219,0.));
#85007=CARTESIAN_POINT('Ctrl Pts',(-71.0747561260436,4.9683197877219,12.));
#85008=CARTESIAN_POINT('Ctrl Pts',(-71.0966021739907,4.96275256726765,0.));
#85009=CARTESIAN_POINT('Ctrl Pts',(-71.0966021739907,4.96275256726765,12.));
#85010=CARTESIAN_POINT('Ctrl Pts',(-71.1184869853056,4.95715198251684,0.));
#85011=CARTESIAN_POINT('Ctrl Pts',(-71.1184869853056,4.95715198251684,12.));
#85012=CARTESIAN_POINT('Ctrl Pts',(-71.1404104085552,4.95151800085101,0.));
#85013=CARTESIAN_POINT('Ctrl Pts',(-71.1404104085552,4.95151800085101,12.));
#85014=CARTESIAN_POINT('Ctrl Pts',(-71.1623722930001,4.94585058990341,0.));
#85015=CARTESIAN_POINT('Ctrl Pts',(-71.1623722930001,4.94585058990341,12.));
#85016=CARTESIAN_POINT('Ctrl Pts',(-71.1843724885847,4.94014971756114,0.));
#85017=CARTESIAN_POINT('Ctrl Pts',(-71.1843724885847,4.94014971756114,12.));
#85018=CARTESIAN_POINT('Ctrl Pts',(-71.2064108459286,4.93441535196617,0.));
#85019=CARTESIAN_POINT('Ctrl Pts',(-71.2064108459286,4.93441535196617,12.));
#85020=CARTESIAN_POINT('Ctrl Pts',(-71.2284872163273,4.92864746150732,0.));
#85021=CARTESIAN_POINT('Ctrl Pts',(-71.2284872163273,4.92864746150732,12.));
#85022=CARTESIAN_POINT('Ctrl Pts',(-71.250601451747,4.92284601481721,0.));
#85023=CARTESIAN_POINT('Ctrl Pts',(-71.250601451747,4.92284601481721,12.));
#85024=CARTESIAN_POINT('Ctrl Pts',(-71.2727534048192,4.91701098077036,0.));
#85025=CARTESIAN_POINT('Ctrl Pts',(-71.2727534048192,4.91701098077036,12.));
#85026=CARTESIAN_POINT('Ctrl Pts',(-71.294942928829,4.91114232848603,0.));
#85027=CARTESIAN_POINT('Ctrl Pts',(-71.294942928829,4.91114232848603,12.));
#85028=CARTESIAN_POINT('Ctrl Pts',(-71.3171698777084,4.90524002732778,0.));
#85029=CARTESIAN_POINT('Ctrl Pts',(-71.3171698777084,4.90524002732778,12.));
#85030=CARTESIAN_POINT('Ctrl Pts',(-71.3394341060359,4.89930404689574,0.));
#85031=CARTESIAN_POINT('Ctrl Pts',(-71.3394341060359,4.89930404689574,12.));
#85032=CARTESIAN_POINT('Ctrl Pts',(-71.3617354690325,4.89333435702413,0.));
#85033=CARTESIAN_POINT('Ctrl Pts',(-71.3617354690325,4.89333435702413,12.));
#85034=CARTESIAN_POINT('Ctrl Pts',(-71.3840738225562,4.88733092777974,0.));
#85035=CARTESIAN_POINT('Ctrl Pts',(-71.3840738225562,4.88733092777974,12.));
#85036=CARTESIAN_POINT('Ctrl Pts',(-71.4064490230899,4.88129372946551,0.));
#85037=CARTESIAN_POINT('Ctrl Pts',(-71.4064490230899,4.88129372946551,12.));
#85038=CARTESIAN_POINT('Ctrl Pts',(-71.4288609277374,4.87522273261907,0.));
#85039=CARTESIAN_POINT('Ctrl Pts',(-71.4288609277374,4.87522273261907,12.));
#85040=CARTESIAN_POINT('Ctrl Pts',(-71.4513093942255,4.86911790800549,0.));
#85041=CARTESIAN_POINT('Ctrl Pts',(-71.4513093942255,4.86911790800549,12.));
#85042=CARTESIAN_POINT('Ctrl Pts',(-71.4737942808982,4.86297922661502,0.));
#85043=CARTESIAN_POINT('Ctrl Pts',(-71.4737942808982,4.86297922661502,12.));
#85044=CARTESIAN_POINT('Ctrl Pts',(-71.4963154467113,4.8568066596618,0.));
#85045=CARTESIAN_POINT('Ctrl Pts',(-71.4963154467113,4.8568066596618,12.));
#85046=CARTESIAN_POINT('Ctrl Pts',(-71.5188727512197,4.8506001785878,0.));
#85047=CARTESIAN_POINT('Ctrl Pts',(-71.5188727512197,4.8506001785878,12.));
#85048=CARTESIAN_POINT('Ctrl Pts',(-71.5414660545739,4.84435975506048,0.));
#85049=CARTESIAN_POINT('Ctrl Pts',(-71.5414660545739,4.84435975506048,12.));
#85050=CARTESIAN_POINT('Ctrl Pts',(-71.564095217521,4.83808536096583,0.));
#85051=CARTESIAN_POINT('Ctrl Pts',(-71.564095217521,4.83808536096583,12.));
#85052=CARTESIAN_POINT('Ctrl Pts',(-71.5867601014,4.83177696840637,0.));
#85053=CARTESIAN_POINT('Ctrl Pts',(-71.5867601014,4.83177696840637,12.));
#85054=CARTESIAN_POINT('Ctrl Pts',(-71.6094605681366,4.82543454970026,0.));
#85055=CARTESIAN_POINT('Ctrl Pts',(-71.6094605681366,4.82543454970026,12.));
#85056=CARTESIAN_POINT('Ctrl Pts',(-71.6321964802326,4.81905807738557,0.));
#85057=CARTESIAN_POINT('Ctrl Pts',(-71.6321964802326,4.81905807738557,12.));
#85058=CARTESIAN_POINT('Ctrl Pts',(-71.6549677007613,4.81264752421732,0.));
#85059=CARTESIAN_POINT('Ctrl Pts',(-71.6549677007613,4.81264752421732,12.));
#85060=CARTESIAN_POINT('Ctrl Pts',(-71.6777740933705,4.80620286316088,0.));
#85061=CARTESIAN_POINT('Ctrl Pts',(-71.6777740933705,4.80620286316088,12.));
#85062=CARTESIAN_POINT('Ctrl Pts',(-71.7006155222766,4.79972406739013,0.));
#85063=CARTESIAN_POINT('Ctrl Pts',(-71.7006155222766,4.79972406739013,12.));
#85064=CARTESIAN_POINT('Ctrl Pts',(-71.7234918522604,4.79321111028671,0.));
#85065=CARTESIAN_POINT('Ctrl Pts',(-71.7234918522604,4.79321111028671,12.));
#85066=CARTESIAN_POINT('Ctrl Pts',(-71.7464029486552,4.7866639654445,0.));
#85067=CARTESIAN_POINT('Ctrl Pts',(-71.7464029486552,4.7866639654445,12.));
#85068=CARTESIAN_POINT('Ctrl Pts',(-71.7693486773449,4.78008260666642,0.));
#85069=CARTESIAN_POINT('Ctrl Pts',(-71.7693486773449,4.78008260666642,12.));
#85070=CARTESIAN_POINT('Ctrl Pts',(-71.7923289047636,4.77346700795787,0.));
#85071=CARTESIAN_POINT('Ctrl Pts',(-71.7923289047636,4.77346700795787,12.));
#85072=CARTESIAN_POINT('Ctrl Pts',(-71.8153434978924,4.76681714352503,0.));
#85073=CARTESIAN_POINT('Ctrl Pts',(-71.8153434978924,4.76681714352503,12.));
#85074=CARTESIAN_POINT('Ctrl Pts',(-71.8383923242533,4.76013298777422,0.));
#85075=CARTESIAN_POINT('Ctrl Pts',(-71.8383923242533,4.76013298777422,12.));
#85076=CARTESIAN_POINT('Ctrl Pts',(-71.8614752519008,4.7534145153167,0.));
#85077=CARTESIAN_POINT('Ctrl Pts',(-71.8614752519008,4.7534145153167,12.));
#85078=CARTESIAN_POINT('Ctrl Pts',(-71.8845921494186,4.74666170096545,0.));
#85079=CARTESIAN_POINT('Ctrl Pts',(-71.8845921494186,4.74666170096545,12.));
#85080=CARTESIAN_POINT('Ctrl Pts',(-71.9077428859207,4.7398745197286,0.));
#85081=CARTESIAN_POINT('Ctrl Pts',(-71.9077428859207,4.7398745197286,12.));
#85082=CARTESIAN_POINT('Ctrl Pts',(-71.9309273310469,4.73305294680783,0.));
#85083=CARTESIAN_POINT('Ctrl Pts',(-71.9309273310469,4.73305294680783,12.));
#85084=CARTESIAN_POINT('Ctrl Pts',(-71.9541453549582,4.72619695759778,0.));
#85085=CARTESIAN_POINT('Ctrl Pts',(-71.9541453549582,4.72619695759778,12.));
#85086=CARTESIAN_POINT('Ctrl Pts',(-71.9773968283267,4.7193065276908,0.));
#85087=CARTESIAN_POINT('Ctrl Pts',(-71.9773968283267,4.7193065276908,12.));
#85088=CARTESIAN_POINT('Ctrl Pts',(-72.0006816223335,4.7123816328741,0.));
#85089=CARTESIAN_POINT('Ctrl Pts',(-72.0006816223335,4.7123816328741,12.));
#85090=CARTESIAN_POINT('Ctrl Pts',(-72.0239996086694,4.70542224912312,0.));
#85091=CARTESIAN_POINT('Ctrl Pts',(-72.0239996086694,4.70542224912312,12.));
#85092=CARTESIAN_POINT('Ctrl Pts',(-72.047350659532,4.69842835259997,0.));
#85093=CARTESIAN_POINT('Ctrl Pts',(-72.047350659532,4.69842835259997,12.));
#85094=CARTESIAN_POINT('Ctrl Pts',(-72.070734647621,4.69139991965279,0.));
#85095=CARTESIAN_POINT('Ctrl Pts',(-72.070734647621,4.69139991965279,12.));
#85096=CARTESIAN_POINT('Ctrl Pts',(-72.0941514461283,4.6843369268206,0.));
#85097=CARTESIAN_POINT('Ctrl Pts',(-72.0941514461283,4.6843369268206,12.));
#85098=CARTESIAN_POINT('Ctrl Pts',(-72.1176009287349,4.67723935083087,0.));
#85099=CARTESIAN_POINT('Ctrl Pts',(-72.1176009287349,4.67723935083087,12.));
#85100=CARTESIAN_POINT('Ctrl Pts',(-72.1410829696129,4.6701071685928,0.));
#85101=CARTESIAN_POINT('Ctrl Pts',(-72.1410829696129,4.6701071685928,12.));
#85102=CARTESIAN_POINT('Ctrl Pts',(-72.1645974434218,4.6629403571957,0.));
#85103=CARTESIAN_POINT('Ctrl Pts',(-72.1645974434218,4.6629403571957,12.));
#85104=CARTESIAN_POINT('Ctrl Pts',(-72.1881442253052,4.65573889390824,0.));
#85105=CARTESIAN_POINT('Ctrl Pts',(-72.1881442253052,4.65573889390824,12.));
#85106=CARTESIAN_POINT('Ctrl Pts',(-72.2117231908816,4.64850275618324,0.));
#85107=CARTESIAN_POINT('Ctrl Pts',(-72.2117231908816,4.64850275618324,12.));
#85108=CARTESIAN_POINT('Ctrl Pts',(-72.2353342162408,4.64123192165627,0.));
#85109=CARTESIAN_POINT('Ctrl Pts',(-72.2353342162408,4.64123192165627,12.));
#85110=CARTESIAN_POINT('Ctrl Pts',(-72.2589771779447,4.63392636813842,0.));
#85111=CARTESIAN_POINT('Ctrl Pts',(-72.2589771779447,4.63392636813842,12.));
#85112=CARTESIAN_POINT('Ctrl Pts',(-72.2826519530254,4.62658607361465,0.));
#85113=CARTESIAN_POINT('Ctrl Pts',(-72.2826519530254,4.62658607361465,12.));
#85114=CARTESIAN_POINT('Ctrl Pts',(-72.306358418981,4.61921101624294,0.));
#85115=CARTESIAN_POINT('Ctrl Pts',(-72.306358418981,4.61921101624294,12.));
#85116=CARTESIAN_POINT('Ctrl Pts',(-72.330096453767,4.61180117435868,0.));
#85117=CARTESIAN_POINT('Ctrl Pts',(-72.330096453767,4.61180117435868,12.));
#85118=CARTESIAN_POINT('Ctrl Pts',(-72.3538659357932,4.60435652647463,0.));
#85119=CARTESIAN_POINT('Ctrl Pts',(-72.3538659357932,4.60435652647463,12.));
#85120=CARTESIAN_POINT('Ctrl Pts',(-72.3776667439244,4.5968770512734,0.));
#85121=CARTESIAN_POINT('Ctrl Pts',(-72.3776667439244,4.5968770512734,12.));
#85122=CARTESIAN_POINT('Ctrl Pts',(-72.4014987574789,4.5893627276055,0.));
#85123=CARTESIAN_POINT('Ctrl Pts',(-72.4014987574789,4.5893627276055,12.));
#85124=CARTESIAN_POINT('Ctrl Pts',(-72.4253618562249,4.5818135344885,0.));
#85125=CARTESIAN_POINT('Ctrl Pts',(-72.4253618562249,4.5818135344885,12.));
#85126=CARTESIAN_POINT('Ctrl Pts',(-72.449255920373,4.57422945111094,0.));
#85127=CARTESIAN_POINT('Ctrl Pts',(-72.449255920373,4.57422945111094,12.));
#85128=CARTESIAN_POINT('Ctrl Pts',(-72.473180830571,4.56661045683366,0.));
#85129=CARTESIAN_POINT('Ctrl Pts',(-72.473180830571,4.56661045683366,12.));
#85130=CARTESIAN_POINT('Ctrl Pts',(-72.4971364679055,4.55895653118213,0.));
#85131=CARTESIAN_POINT('Ctrl Pts',(-72.4971364679055,4.55895653118213,12.));
#85132=CARTESIAN_POINT('Ctrl Pts',(-72.5211227138997,4.55126765384402,0.));
#85133=CARTESIAN_POINT('Ctrl Pts',(-72.5211227138997,4.55126765384402,12.));
#85134=CARTESIAN_POINT('Ctrl Pts',(-72.5451394505106,4.54354380466824,0.));
#85135=CARTESIAN_POINT('Ctrl Pts',(-72.5451394505106,4.54354380466824,12.));
#85136=CARTESIAN_POINT('Ctrl Pts',(-72.5691865601225,4.53578496366801,0.));
#85137=CARTESIAN_POINT('Ctrl Pts',(-72.5691865601225,4.53578496366801,12.));
#85138=CARTESIAN_POINT('Ctrl Pts',(-72.5932639255406,4.5279911110239,0.));
#85139=CARTESIAN_POINT('Ctrl Pts',(-72.5932639255406,4.5279911110239,12.));
#85140=CARTESIAN_POINT('Ctrl Pts',(-72.6173714299935,4.52016222707632,0.));
#85141=CARTESIAN_POINT('Ctrl Pts',(-72.6173714299935,4.52016222707632,12.));
#85142=CARTESIAN_POINT('Ctrl Pts',(-72.6415089571314,4.51229829232259,0.));
#85143=CARTESIAN_POINT('Ctrl Pts',(-72.6415089571314,4.51229829232259,12.));
#85144=CARTESIAN_POINT('Ctrl Pts',(-72.6656763910241,4.50439928741604,0.));
#85145=CARTESIAN_POINT('Ctrl Pts',(-72.6656763910241,4.50439928741604,12.));
#85146=CARTESIAN_POINT('Ctrl Pts',(-72.689873616155,4.49646519316821,0.));
#85147=CARTESIAN_POINT('Ctrl Pts',(-72.689873616155,4.49646519316821,12.));
#85148=CARTESIAN_POINT('Ctrl Pts',(-72.7141005174153,4.48849599055353,0.));
#85149=CARTESIAN_POINT('Ctrl Pts',(-72.7141005174153,4.48849599055353,12.));
#85150=CARTESIAN_POINT('Ctrl Pts',(-72.7383569801042,4.48049166070223,0.));
#85151=CARTESIAN_POINT('Ctrl Pts',(-72.7383569801042,4.48049166070223,12.));
#85152=CARTESIAN_POINT('Ctrl Pts',(-72.7626428899287,4.47245218489622,0.));
#85153=CARTESIAN_POINT('Ctrl Pts',(-72.7626428899287,4.47245218489622,12.));
#85154=CARTESIAN_POINT('Ctrl Pts',(-72.7869581329994,4.46437754456795,0.));
#85155=CARTESIAN_POINT('Ctrl Pts',(-72.7869581329994,4.46437754456795,12.));
#85156=CARTESIAN_POINT('Ctrl Pts',(-72.8113025958258,4.45626772130138,0.));
#85157=CARTESIAN_POINT('Ctrl Pts',(-72.8113025958258,4.45626772130138,12.));
#85158=CARTESIAN_POINT('Ctrl Pts',(-72.8356761653064,4.44812269683724,0.));
#85159=CARTESIAN_POINT('Ctrl Pts',(-72.8356761653064,4.44812269683724,12.));
#85160=CARTESIAN_POINT('Ctrl Pts',(-72.8600787287316,4.43994245306804,0.));
#85161=CARTESIAN_POINT('Ctrl Pts',(-72.8600787287316,4.43994245306804,12.));
#85162=CARTESIAN_POINT('Ctrl Pts',(-72.8845101737856,4.43172697203341,0.));
#85163=CARTESIAN_POINT('Ctrl Pts',(-72.8845101737856,4.43172697203341,12.));
#85164=CARTESIAN_POINT('Ctrl Pts',(-72.9089703885463,4.42347623591941,0.));
#85165=CARTESIAN_POINT('Ctrl Pts',(-72.9089703885463,4.42347623591941,12.));
#85166=CARTESIAN_POINT('Ctrl Pts',(-72.9334592614828,4.41519022705926,0.));
#85167=CARTESIAN_POINT('Ctrl Pts',(-72.9334592614828,4.41519022705926,12.));
#85168=CARTESIAN_POINT('Ctrl Pts',(-72.9579766814495,4.40686892793964,0.));
#85169=CARTESIAN_POINT('Ctrl Pts',(-72.9579766814495,4.40686892793964,12.));
#85170=CARTESIAN_POINT('Ctrl Pts',(-72.9825225376839,4.3985123211973,0.));
#85171=CARTESIAN_POINT('Ctrl Pts',(-72.9825225376839,4.3985123211973,12.));
#85172=CARTESIAN_POINT('Ctrl Pts',(-73.0070967198033,4.39012038961144,0.));
#85173=CARTESIAN_POINT('Ctrl Pts',(-73.0070967198033,4.39012038961144,12.));
#85174=CARTESIAN_POINT('Ctrl Pts',(-73.031699117799,4.38169311610153,0.));
#85175=CARTESIAN_POINT('Ctrl Pts',(-73.031699117799,4.38169311610153,12.));
#85176=CARTESIAN_POINT('Ctrl Pts',(-73.0563296220301,4.37323048372606,0.));
#85177=CARTESIAN_POINT('Ctrl Pts',(-73.0563296220301,4.37323048372606,12.));
#85178=CARTESIAN_POINT('Ctrl Pts',(-73.0809881232111,4.36473247568638,0.));
#85179=CARTESIAN_POINT('Ctrl Pts',(-73.0809881232111,4.36473247568638,12.));
#85180=CARTESIAN_POINT('Ctrl Pts',(-73.1056745124099,4.35619907532715,0.));
#85181=CARTESIAN_POINT('Ctrl Pts',(-73.1056745124099,4.35619907532715,12.));
#85182=CARTESIAN_POINT('Ctrl Pts',(-73.1303886810602,4.34763026613154,0.));
#85183=CARTESIAN_POINT('Ctrl Pts',(-73.1303886810602,4.34763026613154,12.));
#85184=CARTESIAN_POINT('Ctrl Pts',(-73.1551305209692,4.33902603172139,0.));
#85185=CARTESIAN_POINT('Ctrl Pts',(-73.1551305209692,4.33902603172139,12.));
#85186=CARTESIAN_POINT('Ctrl Pts',(-73.1798999243234,4.33038635585878,0.));
#85187=CARTESIAN_POINT('Ctrl Pts',(-73.1798999243234,4.33038635585878,12.));
#85188=CARTESIAN_POINT('Ctrl Pts',(-73.204696783693,4.32171122245218,0.));
#85189=CARTESIAN_POINT('Ctrl Pts',(-73.204696783693,4.32171122245218,12.));
#85190=CARTESIAN_POINT('Ctrl Pts',(-73.2295209920319,4.31300061556102,0.));
#85191=CARTESIAN_POINT('Ctrl Pts',(-73.2295209920319,4.31300061556102,12.));
#85192=CARTESIAN_POINT('Ctrl Pts',(-73.2543724426562,4.30425451938233,0.));
#85193=CARTESIAN_POINT('Ctrl Pts',(-73.2543724426562,4.30425451938233,12.));
#85194=CARTESIAN_POINT('Ctrl Pts',(-73.2792510292243,4.29547291824288,0.));
#85195=CARTESIAN_POINT('Ctrl Pts',(-73.2792510292243,4.29547291824288,12.));
#85196=CARTESIAN_POINT('Ctrl Pts',(-73.3041566457134,4.28665579659301,0.));
#85197=CARTESIAN_POINT('Ctrl Pts',(-73.3041566457134,4.28665579659301,12.));
#85198=CARTESIAN_POINT('Ctrl Pts',(-73.3290891863959,4.27780313900391,0.));
#85199=CARTESIAN_POINT('Ctrl Pts',(-73.3290891863959,4.27780313900391,12.));
#85200=CARTESIAN_POINT('Ctrl Pts',(-73.354048545808,4.26891493016703,0.));
#85201=CARTESIAN_POINT('Ctrl Pts',(-73.354048545808,4.26891493016703,12.));
#85202=CARTESIAN_POINT('Ctrl Pts',(-73.3790346187953,4.25999115489904,0.));
#85203=CARTESIAN_POINT('Ctrl Pts',(-73.3790346187953,4.25999115489904,12.));
#85204=CARTESIAN_POINT('Ctrl Pts',(-73.4040473005603,4.25103179814891,0.));
#85205=CARTESIAN_POINT('Ctrl Pts',(-73.4040473005603,4.25103179814891,12.));
#85206=CARTESIAN_POINT('Ctrl Pts',(-73.4290864867103,4.24203684500941,0.));
#85207=CARTESIAN_POINT('Ctrl Pts',(-73.4290864867103,4.24203684500941,12.));
#85208=CARTESIAN_POINT('Ctrl Pts',(-73.4541520732943,4.23300628072757,0.));
#85209=CARTESIAN_POINT('Ctrl Pts',(-73.4541520732943,4.23300628072757,12.));
#85210=CARTESIAN_POINT('Ctrl Pts',(-73.4792439568624,4.22394009072752,0.));
#85211=CARTESIAN_POINT('Ctrl Pts',(-73.4792439568624,4.22394009072752,12.));
#85212=CARTESIAN_POINT('Ctrl Pts',(-73.5043620344107,4.21483826059436,0.));
#85213=CARTESIAN_POINT('Ctrl Pts',(-73.5043620344107,4.21483826059436,12.));
#85214=CARTESIAN_POINT('Ctrl Pts',(-73.5295062032621,4.20570077603727,0.));
#85215=CARTESIAN_POINT('Ctrl Pts',(-73.5295062032621,4.20570077603727,12.));
#85216=CARTESIAN_POINT('Ctrl Pts',(-73.554676360957,4.19652762286126,0.));
#85217=CARTESIAN_POINT('Ctrl Pts',(-73.554676360957,4.19652762286126,12.));
#85218=CARTESIAN_POINT('Ctrl Pts',(-73.5798724051519,4.18731878694237,0.));
#85219=CARTESIAN_POINT('Ctrl Pts',(-73.5798724051519,4.18731878694237,12.));
#85220=CARTESIAN_POINT('Ctrl Pts',(-73.6050942334773,4.17807425419816,0.));
#85221=CARTESIAN_POINT('Ctrl Pts',(-73.6050942334773,4.17807425419816,12.));
#85222=CARTESIAN_POINT('Ctrl Pts',(-73.6303417435262,4.16879401058786,0.));
#85223=CARTESIAN_POINT('Ctrl Pts',(-73.6303417435262,4.16879401058786,12.));
#85224=CARTESIAN_POINT('Ctrl Pts',(-73.6556148331504,4.1594780421779,0.));
#85225=CARTESIAN_POINT('Ctrl Pts',(-73.6556148331504,4.1594780421779,12.));
#85226=CARTESIAN_POINT('Ctrl Pts',(-73.6809134006909,4.15012633519727,0.));
#85227=CARTESIAN_POINT('Ctrl Pts',(-73.6809134006909,4.15012633519727,12.));
#85228=CARTESIAN_POINT('Ctrl Pts',(-73.7062373452344,4.14073887610154,0.));
#85229=CARTESIAN_POINT('Ctrl Pts',(-73.7062373452344,4.14073887610154,12.));
#85230=CARTESIAN_POINT('Ctrl Pts',(-73.7315865668508,4.13131565163574,0.));
#85231=CARTESIAN_POINT('Ctrl Pts',(-73.7315865668508,4.13131565163574,12.));
#85232=CARTESIAN_POINT('Ctrl Pts',(-73.7569609668501,4.1218566489055,0.));
#85233=CARTESIAN_POINT('Ctrl Pts',(-73.7569609668501,4.1218566489055,12.));
#85234=CARTESIAN_POINT('Ctrl Pts',(-73.7823604472126,4.1123618552278,0.));
#85235=CARTESIAN_POINT('Ctrl Pts',(-73.7823604472126,4.1123618552278,12.));
#85236=CARTESIAN_POINT('Ctrl Pts',(-73.8077849100314,4.10283125798724,0.));
#85237=CARTESIAN_POINT('Ctrl Pts',(-73.8077849100314,4.10283125798724,12.));
#85238=CARTESIAN_POINT('Ctrl Pts',(-73.8332342568978,4.09326484448231,0.));
#85239=CARTESIAN_POINT('Ctrl Pts',(-73.8332342568978,4.09326484448231,12.));
#85240=CARTESIAN_POINT('Ctrl Pts',(-73.8587083884208,4.08366260180679,0.));
#85241=CARTESIAN_POINT('Ctrl Pts',(-73.8587083884208,4.08366260180679,12.));
#85242=CARTESIAN_POINT('Ctrl Pts',(-73.884207203405,4.07402451665252,0.));
#85243=CARTESIAN_POINT('Ctrl Pts',(-73.884207203405,4.07402451665252,12.));
#85244=CARTESIAN_POINT('Ctrl Pts',(-73.9097305995173,4.06435057547334,0.));
#85245=CARTESIAN_POINT('Ctrl Pts',(-73.9097305995173,4.06435057547334,12.));
#85246=CARTESIAN_POINT('Ctrl Pts',(-73.9352784747665,4.05464076484761,0.));
#85247=CARTESIAN_POINT('Ctrl Pts',(-73.9352784747665,4.05464076484761,12.));
#85248=CARTESIAN_POINT('Ctrl Pts',(-73.9608507287943,4.04489507179963,0.));
#85249=CARTESIAN_POINT('Ctrl Pts',(-73.9608507287943,4.04489507179963,12.));
#85250=CARTESIAN_POINT('Ctrl Pts',(-73.9864472641025,4.03511348410659,0.));
#85251=CARTESIAN_POINT('Ctrl Pts',(-73.9864472641025,4.03511348410659,12.));
#85252=CARTESIAN_POINT('Ctrl Pts',(-74.0120679876396,4.02529599070084,0.));
#85253=CARTESIAN_POINT('Ctrl Pts',(-74.0120679876396,4.02529599070084,12.));
#85254=CARTESIAN_POINT('Ctrl Pts',(-74.0377128111754,4.01544258176692,0.));
#85255=CARTESIAN_POINT('Ctrl Pts',(-74.0377128111754,4.01544258176692,12.));
#85256=CARTESIAN_POINT('Ctrl Pts',(-74.0633816477912,4.00555324785459,0.));
#85257=CARTESIAN_POINT('Ctrl Pts',(-74.0633816477912,4.00555324785459,12.));
#85258=CARTESIAN_POINT('Ctrl Pts',(-74.0890744091088,3.99562797918271,0.));
#85259=CARTESIAN_POINT('Ctrl Pts',(-74.0890744091088,3.99562797918271,12.));
#85260=CARTESIAN_POINT('Ctrl Pts',(-74.1147910020869,3.98566676483638,0.));
#85261=CARTESIAN_POINT('Ctrl Pts',(-74.1147910020869,3.98566676483638,12.));
#85262=CARTESIAN_POINT('Ctrl Pts',(-74.1405313263198,3.97566959209546,0.));
#85263=CARTESIAN_POINT('Ctrl Pts',(-74.1405313263198,3.97566959209546,12.));
#85264=CARTESIAN_POINT('Ctrl Pts',(-74.1662952702689,3.96563644549422,0.));
#85265=CARTESIAN_POINT('Ctrl Pts',(-74.1662952702689,3.96563644549422,12.));
#85266=CARTESIAN_POINT('Ctrl Pts',(-74.1920827166861,3.95556730821159,0.));
#85267=CARTESIAN_POINT('Ctrl Pts',(-74.1920827166861,3.95556730821159,12.));
#85268=CARTESIAN_POINT('Ctrl Pts',(-74.217893549314,3.94546216377498,0.));
#85269=CARTESIAN_POINT('Ctrl Pts',(-74.217893549314,3.94546216377498,12.));
#85270=CARTESIAN_POINT('Ctrl Pts',(-74.2437276593763,3.93532099774229,0.));
#85271=CARTESIAN_POINT('Ctrl Pts',(-74.2437276593763,3.93532099774229,12.));
#85272=CARTESIAN_POINT('Ctrl Pts',(-74.2695849516134,3.92514379920728,0.));
#85273=CARTESIAN_POINT('Ctrl Pts',(-74.2695849516134,3.92514379920728,12.));
#85274=CARTESIAN_POINT('Ctrl Pts',(-74.2954653518345,3.91493056284964,0.));
#85275=CARTESIAN_POINT('Ctrl Pts',(-74.2954653518345,3.91493056284964,12.));
#85276=CARTESIAN_POINT('Ctrl Pts',(-74.3213688089495,3.9046812890452,0.));
#85277=CARTESIAN_POINT('Ctrl Pts',(-74.3213688089495,3.9046812890452,12.));
#85278=CARTESIAN_POINT('Ctrl Pts',(-74.3472952898,3.89439598145193,0.));
#85279=CARTESIAN_POINT('Ctrl Pts',(-74.3472952898,3.89439598145193,12.));
#85280=CARTESIAN_POINT('Ctrl Pts',(-74.3680548786039,3.88613891247869,0.));
#85281=CARTESIAN_POINT('Ctrl Pts',(-74.3680548786039,3.88613891247869,12.));
#85282=CARTESIAN_POINT('Ctrl Pts',(-74.3836349188809,3.87992989995677,0.));
#85283=CARTESIAN_POINT('Ctrl Pts',(-74.3836349188809,3.87992989995677,12.));
#85284=CARTESIAN_POINT('Ctrl Pts',(-74.3940262116251,3.875783353773,0.));
#85285=CARTESIAN_POINT('Ctrl Pts',(-74.3940262116251,3.875783353773,12.));
#85286=CARTESIAN_POINT('Ctrl Pts',(-74.3992230078037,3.87370827955544,0.));
#85287=CARTESIAN_POINT('Ctrl Pts',(-74.3992230078037,3.87370827955544,12.));
#85288=CARTESIAN_POINT('',(-69.8028570375097,5.24987136994592,0.));
#85289=CARTESIAN_POINT('Ctrl Pts',(-69.8028570375097,5.24987136994592,0.));
#85290=CARTESIAN_POINT('Ctrl Pts',(-69.8066748687772,5.24915955997427,0.));
#85291=CARTESIAN_POINT('Ctrl Pts',(-69.8143154684204,5.24773285666376,0.));
#85292=CARTESIAN_POINT('Ctrl Pts',(-69.8257911792159,5.2455835515975,0.));
#85293=CARTESIAN_POINT('Ctrl Pts',(-69.841121750752,5.24269931054569,0.));
#85294=CARTESIAN_POINT('Ctrl Pts',(-69.8603343302743,5.23906316634802,0.));
#85295=CARTESIAN_POINT('Ctrl Pts',(-69.8795962381599,5.2353961627962,0.));
#85296=CARTESIAN_POINT('Ctrl Pts',(-69.8989073936688,5.23169827290555,0.));
#85297=CARTESIAN_POINT('Ctrl Pts',(-69.9182676502048,5.22796945602793,0.));
#85298=CARTESIAN_POINT('Ctrl Pts',(-69.9376767969095,5.22420965879981,0.));
#85299=CARTESIAN_POINT('Ctrl Pts',(-69.9571345870076,5.2204188207572,0.));
#85300=CARTESIAN_POINT('Ctrl Pts',(-69.9766407595385,5.21659687881139,0.));
#85301=CARTESIAN_POINT('Ctrl Pts',(-69.9961950629965,5.21274377203259,0.));
#85302=CARTESIAN_POINT('Ctrl Pts',(-70.0157972802182,5.20885944672836,0.));
#85303=CARTESIAN_POINT('Ctrl Pts',(-70.0354472203546,5.20494385478025,0.));
#85304=CARTESIAN_POINT('Ctrl Pts',(-70.0551447071082,5.20099695122656,0.));
#85305=CARTESIAN_POINT('Ctrl Pts',(-70.0748895689729,5.19701869225528,0.));
#85306=CARTESIAN_POINT('Ctrl Pts',(-70.0946816270997,5.19300903271579,0.));
#85307=CARTESIAN_POINT('Ctrl Pts',(-70.1145206891885,5.18896792486565,0.));
#85308=CARTESIAN_POINT('Ctrl Pts',(-70.1344065558145,5.18489531966264,0.));
#85309=CARTESIAN_POINT('Ctrl Pts',(-70.1543390243892,5.18079116757666,0.));
#85310=CARTESIAN_POINT('Ctrl Pts',(-70.1743178937077,5.17665541952382,0.));
#85311=CARTESIAN_POINT('Ctrl Pts',(-70.1943429691167,5.17248802793389,0.));
#85312=CARTESIAN_POINT('Ctrl Pts',(-70.2144140622953,5.16828894670108,0.));
#85313=CARTESIAN_POINT('Ctrl Pts',(-70.2345309887833,5.16405813066976,0.));
#85314=CARTESIAN_POINT('Ctrl Pts',(-70.2546935662722,5.15979553528203,0.));
#85315=CARTESIAN_POINT('Ctrl Pts',(-70.2749016125105,5.15550111614859,0.));
#85316=CARTESIAN_POINT('Ctrl Pts',(-70.2951549435512,5.15117482869254,0.));
#85317=CARTESIAN_POINT('Ctrl Pts',(-70.3154533746736,5.1468166283308,0.));
#85318=CARTESIAN_POINT('Ctrl Pts',(-70.3357967211796,5.14242647063479,0.));
#85319=CARTESIAN_POINT('Ctrl Pts',(-70.3561847991714,5.13800431148903,0.));
#85320=CARTESIAN_POINT('Ctrl Pts',(-70.3766174264757,5.13355010728567,0.));
#85321=CARTESIAN_POINT('Ctrl Pts',(-70.3970944229851,5.12906381499456,0.));
#85322=CARTESIAN_POINT('Ctrl Pts',(-70.417615610161,5.12454539205328,0.));
#85323=CARTESIAN_POINT('Ctrl Pts',(-70.4381808107245,5.11999479630211,0.));
#85324=CARTESIAN_POINT('Ctrl Pts',(-70.458789848296,5.11541198590932,0.));
#85325=CARTESIAN_POINT('Ctrl Pts',(-70.4794425469825,5.11079691929213,0.));
#85326=CARTESIAN_POINT('Ctrl Pts',(-70.500138731399,5.10614955511663,0.));
#85327=CARTESIAN_POINT('Ctrl Pts',(-70.5208782268497,5.1014698523294,0.));
#85328=CARTESIAN_POINT('Ctrl Pts',(-70.5416608594526,5.09675777018182,0.));
#85329=CARTESIAN_POINT('Ctrl Pts',(-70.5624864562824,5.09201326826134,0.));
#85330=CARTESIAN_POINT('Ctrl Pts',(-70.5833548455014,5.08723630652272,0.));
#85331=CARTESIAN_POINT('Ctrl Pts',(-70.6042658562923,5.08242684526686,0.));
#85332=CARTESIAN_POINT('Ctrl Pts',(-70.6252193187878,5.07758484512302,0.));
#85333=CARTESIAN_POINT('Ctrl Pts',(-70.6462150640015,5.07271026703354,0.));
#85334=CARTESIAN_POINT('Ctrl Pts',(-70.6672529237455,5.06780307224071,0.));
#85335=CARTESIAN_POINT('Ctrl Pts',(-70.6883327305784,5.06286322227819,0.));
#85336=CARTESIAN_POINT('Ctrl Pts',(-70.7094543178438,5.05789067897057,0.));
#85337=CARTESIAN_POINT('Ctrl Pts',(-70.7306175196863,5.05288540443482,0.));
#85338=CARTESIAN_POINT('Ctrl Pts',(-70.7518221710706,5.04784736108346,0.));
#85339=CARTESIAN_POINT('Ctrl Pts',(-70.7730681077983,5.04277651163349,0.));
#85340=CARTESIAN_POINT('Ctrl Pts',(-70.7943551665059,5.03767281910479,0.));
#85341=CARTESIAN_POINT('Ctrl Pts',(-70.8156831846488,5.0325362468094,0.));
#85342=CARTESIAN_POINT('Ctrl Pts',(-70.8370520004843,5.02736675834692,0.));
#85343=CARTESIAN_POINT('Ctrl Pts',(-70.8584614530519,5.0221643176006,0.));
#85344=CARTESIAN_POINT('Ctrl Pts',(-70.8799113821452,5.0169288887379,0.));
#85345=CARTESIAN_POINT('Ctrl Pts',(-70.9014016283124,5.01166043620567,0.));
#85346=CARTESIAN_POINT('Ctrl Pts',(-70.9229320328589,5.00635892472513,0.));
#85347=CARTESIAN_POINT('Ctrl Pts',(-70.9445024378439,5.00102431929039,0.));
#85348=CARTESIAN_POINT('Ctrl Pts',(-70.9661126860773,4.99565658516913,0.));
#85349=CARTESIAN_POINT('Ctrl Pts',(-70.9877626211113,4.99025568790664,0.));
#85350=CARTESIAN_POINT('Ctrl Pts',(-71.0094520872377,4.98482159331863,0.));
#85351=CARTESIAN_POINT('Ctrl Pts',(-71.0311809294821,4.97935426748584,0.));
#85352=CARTESIAN_POINT('Ctrl Pts',(-71.0529489935961,4.97385367675158,0.));
#85353=CARTESIAN_POINT('Ctrl Pts',(-71.0747561260436,4.9683197877219,0.));
#85354=CARTESIAN_POINT('Ctrl Pts',(-71.0966021739907,4.96275256726765,0.));
#85355=CARTESIAN_POINT('Ctrl Pts',(-71.1184869853056,4.95715198251684,0.));
#85356=CARTESIAN_POINT('Ctrl Pts',(-71.1404104085552,4.95151800085101,0.));
#85357=CARTESIAN_POINT('Ctrl Pts',(-71.1623722930001,4.94585058990341,0.));
#85358=CARTESIAN_POINT('Ctrl Pts',(-71.1843724885847,4.94014971756114,0.));
#85359=CARTESIAN_POINT('Ctrl Pts',(-71.2064108459286,4.93441535196617,0.));
#85360=CARTESIAN_POINT('Ctrl Pts',(-71.2284872163273,4.92864746150732,0.));
#85361=CARTESIAN_POINT('Ctrl Pts',(-71.250601451747,4.92284601481721,0.));
#85362=CARTESIAN_POINT('Ctrl Pts',(-71.2727534048192,4.91701098077036,0.));
#85363=CARTESIAN_POINT('Ctrl Pts',(-71.294942928829,4.91114232848603,0.));
#85364=CARTESIAN_POINT('Ctrl Pts',(-71.3171698777084,4.90524002732778,0.));
#85365=CARTESIAN_POINT('Ctrl Pts',(-71.3394341060359,4.89930404689574,0.));
#85366=CARTESIAN_POINT('Ctrl Pts',(-71.3617354690325,4.89333435702413,0.));
#85367=CARTESIAN_POINT('Ctrl Pts',(-71.3840738225562,4.88733092777974,0.));
#85368=CARTESIAN_POINT('Ctrl Pts',(-71.4064490230899,4.88129372946551,0.));
#85369=CARTESIAN_POINT('Ctrl Pts',(-71.4288609277374,4.87522273261907,0.));
#85370=CARTESIAN_POINT('Ctrl Pts',(-71.4513093942255,4.86911790800549,0.));
#85371=CARTESIAN_POINT('Ctrl Pts',(-71.4737942808982,4.86297922661502,0.));
#85372=CARTESIAN_POINT('Ctrl Pts',(-71.4963154467113,4.8568066596618,0.));
#85373=CARTESIAN_POINT('Ctrl Pts',(-71.5188727512197,4.8506001785878,0.));
#85374=CARTESIAN_POINT('Ctrl Pts',(-71.5414660545739,4.84435975506048,0.));
#85375=CARTESIAN_POINT('Ctrl Pts',(-71.564095217521,4.83808536096583,0.));
#85376=CARTESIAN_POINT('Ctrl Pts',(-71.5867601014,4.83177696840637,0.));
#85377=CARTESIAN_POINT('Ctrl Pts',(-71.6094605681366,4.82543454970026,0.));
#85378=CARTESIAN_POINT('Ctrl Pts',(-71.6321964802326,4.81905807738557,0.));
#85379=CARTESIAN_POINT('Ctrl Pts',(-71.6549677007613,4.81264752421732,0.));
#85380=CARTESIAN_POINT('Ctrl Pts',(-71.6777740933705,4.80620286316088,0.));
#85381=CARTESIAN_POINT('Ctrl Pts',(-71.7006155222766,4.79972406739013,0.));
#85382=CARTESIAN_POINT('Ctrl Pts',(-71.7234918522604,4.79321111028671,0.));
#85383=CARTESIAN_POINT('Ctrl Pts',(-71.7464029486552,4.7866639654445,0.));
#85384=CARTESIAN_POINT('Ctrl Pts',(-71.7693486773449,4.78008260666642,0.));
#85385=CARTESIAN_POINT('Ctrl Pts',(-71.7923289047636,4.77346700795787,0.));
#85386=CARTESIAN_POINT('Ctrl Pts',(-71.8153434978924,4.76681714352503,0.));
#85387=CARTESIAN_POINT('Ctrl Pts',(-71.8383923242533,4.76013298777422,0.));
#85388=CARTESIAN_POINT('Ctrl Pts',(-71.8614752519008,4.7534145153167,0.));
#85389=CARTESIAN_POINT('Ctrl Pts',(-71.8845921494186,4.74666170096545,0.));
#85390=CARTESIAN_POINT('Ctrl Pts',(-71.9077428859207,4.7398745197286,0.));
#85391=CARTESIAN_POINT('Ctrl Pts',(-71.9309273310469,4.73305294680783,0.));
#85392=CARTESIAN_POINT('Ctrl Pts',(-71.9541453549582,4.72619695759778,0.));
#85393=CARTESIAN_POINT('Ctrl Pts',(-71.9773968283267,4.7193065276908,0.));
#85394=CARTESIAN_POINT('Ctrl Pts',(-72.0006816223335,4.7123816328741,0.));
#85395=CARTESIAN_POINT('Ctrl Pts',(-72.0239996086694,4.70542224912312,0.));
#85396=CARTESIAN_POINT('Ctrl Pts',(-72.047350659532,4.69842835259997,0.));
#85397=CARTESIAN_POINT('Ctrl Pts',(-72.070734647621,4.69139991965279,0.));
#85398=CARTESIAN_POINT('Ctrl Pts',(-72.0941514461283,4.6843369268206,0.));
#85399=CARTESIAN_POINT('Ctrl Pts',(-72.1176009287349,4.67723935083087,0.));
#85400=CARTESIAN_POINT('Ctrl Pts',(-72.1410829696129,4.6701071685928,0.));
#85401=CARTESIAN_POINT('Ctrl Pts',(-72.1645974434218,4.6629403571957,0.));
#85402=CARTESIAN_POINT('Ctrl Pts',(-72.1881442253052,4.65573889390824,0.));
#85403=CARTESIAN_POINT('Ctrl Pts',(-72.2117231908816,4.64850275618324,0.));
#85404=CARTESIAN_POINT('Ctrl Pts',(-72.2353342162408,4.64123192165627,0.));
#85405=CARTESIAN_POINT('Ctrl Pts',(-72.2589771779447,4.63392636813842,0.));
#85406=CARTESIAN_POINT('Ctrl Pts',(-72.2826519530254,4.62658607361465,0.));
#85407=CARTESIAN_POINT('Ctrl Pts',(-72.306358418981,4.61921101624294,0.));
#85408=CARTESIAN_POINT('Ctrl Pts',(-72.330096453767,4.61180117435868,0.));
#85409=CARTESIAN_POINT('Ctrl Pts',(-72.3538659357932,4.60435652647463,0.));
#85410=CARTESIAN_POINT('Ctrl Pts',(-72.3776667439244,4.5968770512734,0.));
#85411=CARTESIAN_POINT('Ctrl Pts',(-72.4014987574789,4.5893627276055,0.));
#85412=CARTESIAN_POINT('Ctrl Pts',(-72.4253618562249,4.5818135344885,0.));
#85413=CARTESIAN_POINT('Ctrl Pts',(-72.449255920373,4.57422945111094,0.));
#85414=CARTESIAN_POINT('Ctrl Pts',(-72.473180830571,4.56661045683366,0.));
#85415=CARTESIAN_POINT('Ctrl Pts',(-72.4971364679055,4.55895653118213,0.));
#85416=CARTESIAN_POINT('Ctrl Pts',(-72.5211227138997,4.55126765384402,0.));
#85417=CARTESIAN_POINT('Ctrl Pts',(-72.5451394505106,4.54354380466824,0.));
#85418=CARTESIAN_POINT('Ctrl Pts',(-72.5691865601225,4.53578496366801,0.));
#85419=CARTESIAN_POINT('Ctrl Pts',(-72.5932639255406,4.5279911110239,0.));
#85420=CARTESIAN_POINT('Ctrl Pts',(-72.6173714299935,4.52016222707632,0.));
#85421=CARTESIAN_POINT('Ctrl Pts',(-72.6415089571314,4.51229829232259,0.));
#85422=CARTESIAN_POINT('Ctrl Pts',(-72.6656763910241,4.50439928741604,0.));
#85423=CARTESIAN_POINT('Ctrl Pts',(-72.689873616155,4.49646519316821,0.));
#85424=CARTESIAN_POINT('Ctrl Pts',(-72.7141005174153,4.48849599055353,0.));
#85425=CARTESIAN_POINT('Ctrl Pts',(-72.7383569801042,4.48049166070223,0.));
#85426=CARTESIAN_POINT('Ctrl Pts',(-72.7626428899287,4.47245218489622,0.));
#85427=CARTESIAN_POINT('Ctrl Pts',(-72.7869581329994,4.46437754456795,0.));
#85428=CARTESIAN_POINT('Ctrl Pts',(-72.8113025958258,4.45626772130138,0.));
#85429=CARTESIAN_POINT('Ctrl Pts',(-72.8356761653064,4.44812269683724,0.));
#85430=CARTESIAN_POINT('Ctrl Pts',(-72.8600787287316,4.43994245306804,0.));
#85431=CARTESIAN_POINT('Ctrl Pts',(-72.8845101737856,4.43172697203341,0.));
#85432=CARTESIAN_POINT('Ctrl Pts',(-72.9089703885463,4.42347623591941,0.));
#85433=CARTESIAN_POINT('Ctrl Pts',(-72.9334592614828,4.41519022705926,0.));
#85434=CARTESIAN_POINT('Ctrl Pts',(-72.9579766814495,4.40686892793964,0.));
#85435=CARTESIAN_POINT('Ctrl Pts',(-72.9825225376839,4.3985123211973,0.));
#85436=CARTESIAN_POINT('Ctrl Pts',(-73.0070967198033,4.39012038961144,0.));
#85437=CARTESIAN_POINT('Ctrl Pts',(-73.031699117799,4.38169311610153,0.));
#85438=CARTESIAN_POINT('Ctrl Pts',(-73.0563296220301,4.37323048372606,0.));
#85439=CARTESIAN_POINT('Ctrl Pts',(-73.0809881232111,4.36473247568638,0.));
#85440=CARTESIAN_POINT('Ctrl Pts',(-73.1056745124099,4.35619907532715,0.));
#85441=CARTESIAN_POINT('Ctrl Pts',(-73.1303886810602,4.34763026613154,0.));
#85442=CARTESIAN_POINT('Ctrl Pts',(-73.1551305209692,4.33902603172139,0.));
#85443=CARTESIAN_POINT('Ctrl Pts',(-73.1798999243234,4.33038635585878,0.));
#85444=CARTESIAN_POINT('Ctrl Pts',(-73.204696783693,4.32171122245218,0.));
#85445=CARTESIAN_POINT('Ctrl Pts',(-73.2295209920319,4.31300061556102,0.));
#85446=CARTESIAN_POINT('Ctrl Pts',(-73.2543724426562,4.30425451938233,0.));
#85447=CARTESIAN_POINT('Ctrl Pts',(-73.2792510292243,4.29547291824288,0.));
#85448=CARTESIAN_POINT('Ctrl Pts',(-73.3041566457134,4.28665579659301,0.));
#85449=CARTESIAN_POINT('Ctrl Pts',(-73.3290891863959,4.27780313900391,0.));
#85450=CARTESIAN_POINT('Ctrl Pts',(-73.354048545808,4.26891493016703,0.));
#85451=CARTESIAN_POINT('Ctrl Pts',(-73.3790346187953,4.25999115489904,0.));
#85452=CARTESIAN_POINT('Ctrl Pts',(-73.4040473005603,4.25103179814891,0.));
#85453=CARTESIAN_POINT('Ctrl Pts',(-73.4290864867103,4.24203684500941,0.));
#85454=CARTESIAN_POINT('Ctrl Pts',(-73.4541520732943,4.23300628072757,0.));
#85455=CARTESIAN_POINT('Ctrl Pts',(-73.4792439568624,4.22394009072752,0.));
#85456=CARTESIAN_POINT('Ctrl Pts',(-73.5043620344107,4.21483826059436,0.));
#85457=CARTESIAN_POINT('Ctrl Pts',(-73.5295062032621,4.20570077603727,0.));
#85458=CARTESIAN_POINT('Ctrl Pts',(-73.554676360957,4.19652762286126,0.));
#85459=CARTESIAN_POINT('Ctrl Pts',(-73.5798724051519,4.18731878694237,0.));
#85460=CARTESIAN_POINT('Ctrl Pts',(-73.6050942334773,4.17807425419816,0.));
#85461=CARTESIAN_POINT('Ctrl Pts',(-73.6303417435262,4.16879401058786,0.));
#85462=CARTESIAN_POINT('Ctrl Pts',(-73.6556148331504,4.1594780421779,0.));
#85463=CARTESIAN_POINT('Ctrl Pts',(-73.6809134006909,4.15012633519727,0.));
#85464=CARTESIAN_POINT('Ctrl Pts',(-73.7062373452344,4.14073887610154,0.));
#85465=CARTESIAN_POINT('Ctrl Pts',(-73.7315865668508,4.13131565163574,0.));
#85466=CARTESIAN_POINT('Ctrl Pts',(-73.7569609668501,4.1218566489055,0.));
#85467=CARTESIAN_POINT('Ctrl Pts',(-73.7823604472126,4.1123618552278,0.));
#85468=CARTESIAN_POINT('Ctrl Pts',(-73.8077849100314,4.10283125798724,0.));
#85469=CARTESIAN_POINT('Ctrl Pts',(-73.8332342568978,4.09326484448231,0.));
#85470=CARTESIAN_POINT('Ctrl Pts',(-73.8587083884208,4.08366260180679,0.));
#85471=CARTESIAN_POINT('Ctrl Pts',(-73.884207203405,4.07402451665252,0.));
#85472=CARTESIAN_POINT('Ctrl Pts',(-73.9097305995173,4.06435057547334,0.));
#85473=CARTESIAN_POINT('Ctrl Pts',(-73.9352784747665,4.05464076484761,0.));
#85474=CARTESIAN_POINT('Ctrl Pts',(-73.9608507287943,4.04489507179963,0.));
#85475=CARTESIAN_POINT('Ctrl Pts',(-73.9864472641025,4.03511348410659,0.));
#85476=CARTESIAN_POINT('Ctrl Pts',(-74.0120679876396,4.02529599070084,0.));
#85477=CARTESIAN_POINT('Ctrl Pts',(-74.0377128111754,4.01544258176692,0.));
#85478=CARTESIAN_POINT('Ctrl Pts',(-74.0597159781919,4.00696550627606,0.));
#85479=CARTESIAN_POINT('Ctrl Pts',(-74.0765982943431,4.0004468971249,0.));
#85480=CARTESIAN_POINT('Ctrl Pts',(-74.0883491449662,3.99590266747766,0.));
#85481=CARTESIAN_POINT('Ctrl Pts',(-74.0949615399274,3.99334334446571,0.));
#85482=CARTESIAN_POINT('Ctrl Pts',(-74.0964320765797,3.99277406492179,0.));
#85483=CARTESIAN_POINT('',(-69.8028570375097,5.24987136994592,12.));
#85484=CARTESIAN_POINT('',(-69.8028570375097,5.24987136994592,0.));
#85485=CARTESIAN_POINT('Ctrl Pts',(-74.0964320765797,3.99277406492181,12.));
#85486=CARTESIAN_POINT('Ctrl Pts',(-74.0949615399273,3.99334334446573,12.));
#85487=CARTESIAN_POINT('Ctrl Pts',(-74.0883491449662,3.99590266747768,12.));
#85488=CARTESIAN_POINT('Ctrl Pts',(-74.0765982943431,4.00044689712491,12.));
#85489=CARTESIAN_POINT('Ctrl Pts',(-74.0597159781919,4.00696550627606,12.));
#85490=CARTESIAN_POINT('Ctrl Pts',(-74.0377128111754,4.01544258176692,12.));
#85491=CARTESIAN_POINT('Ctrl Pts',(-74.0120679876396,4.02529599070084,12.));
#85492=CARTESIAN_POINT('Ctrl Pts',(-73.9864472641025,4.03511348410659,12.));
#85493=CARTESIAN_POINT('Ctrl Pts',(-73.9608507287943,4.04489507179963,12.));
#85494=CARTESIAN_POINT('Ctrl Pts',(-73.9352784747665,4.05464076484761,12.));
#85495=CARTESIAN_POINT('Ctrl Pts',(-73.9097305995173,4.06435057547334,12.));
#85496=CARTESIAN_POINT('Ctrl Pts',(-73.884207203405,4.07402451665252,12.));
#85497=CARTESIAN_POINT('Ctrl Pts',(-73.8587083884208,4.08366260180679,12.));
#85498=CARTESIAN_POINT('Ctrl Pts',(-73.8332342568978,4.09326484448231,12.));
#85499=CARTESIAN_POINT('Ctrl Pts',(-73.8077849100314,4.10283125798724,12.));
#85500=CARTESIAN_POINT('Ctrl Pts',(-73.7823604472126,4.1123618552278,12.));
#85501=CARTESIAN_POINT('Ctrl Pts',(-73.7569609668501,4.1218566489055,12.));
#85502=CARTESIAN_POINT('Ctrl Pts',(-73.7315865668508,4.13131565163574,12.));
#85503=CARTESIAN_POINT('Ctrl Pts',(-73.7062373452344,4.14073887610154,12.));
#85504=CARTESIAN_POINT('Ctrl Pts',(-73.6809134006909,4.15012633519727,12.));
#85505=CARTESIAN_POINT('Ctrl Pts',(-73.6556148331504,4.1594780421779,12.));
#85506=CARTESIAN_POINT('Ctrl Pts',(-73.6303417435262,4.16879401058786,12.));
#85507=CARTESIAN_POINT('Ctrl Pts',(-73.6050942334773,4.17807425419816,12.));
#85508=CARTESIAN_POINT('Ctrl Pts',(-73.5798724051519,4.18731878694237,12.));
#85509=CARTESIAN_POINT('Ctrl Pts',(-73.554676360957,4.19652762286126,12.));
#85510=CARTESIAN_POINT('Ctrl Pts',(-73.5295062032621,4.20570077603727,12.));
#85511=CARTESIAN_POINT('Ctrl Pts',(-73.5043620344107,4.21483826059436,12.));
#85512=CARTESIAN_POINT('Ctrl Pts',(-73.4792439568624,4.22394009072752,12.));
#85513=CARTESIAN_POINT('Ctrl Pts',(-73.4541520732943,4.23300628072757,12.));
#85514=CARTESIAN_POINT('Ctrl Pts',(-73.4290864867103,4.24203684500941,12.));
#85515=CARTESIAN_POINT('Ctrl Pts',(-73.4040473005603,4.25103179814891,12.));
#85516=CARTESIAN_POINT('Ctrl Pts',(-73.3790346187953,4.25999115489904,12.));
#85517=CARTESIAN_POINT('Ctrl Pts',(-73.354048545808,4.26891493016703,12.));
#85518=CARTESIAN_POINT('Ctrl Pts',(-73.3290891863959,4.27780313900391,12.));
#85519=CARTESIAN_POINT('Ctrl Pts',(-73.3041566457134,4.28665579659301,12.));
#85520=CARTESIAN_POINT('Ctrl Pts',(-73.2792510292243,4.29547291824288,12.));
#85521=CARTESIAN_POINT('Ctrl Pts',(-73.2543724426562,4.30425451938233,12.));
#85522=CARTESIAN_POINT('Ctrl Pts',(-73.2295209920319,4.31300061556102,12.));
#85523=CARTESIAN_POINT('Ctrl Pts',(-73.204696783693,4.32171122245218,12.));
#85524=CARTESIAN_POINT('Ctrl Pts',(-73.1798999243234,4.33038635585878,12.));
#85525=CARTESIAN_POINT('Ctrl Pts',(-73.1551305209692,4.33902603172139,12.));
#85526=CARTESIAN_POINT('Ctrl Pts',(-73.1303886810602,4.34763026613154,12.));
#85527=CARTESIAN_POINT('Ctrl Pts',(-73.1056745124099,4.35619907532715,12.));
#85528=CARTESIAN_POINT('Ctrl Pts',(-73.0809881232111,4.36473247568638,12.));
#85529=CARTESIAN_POINT('Ctrl Pts',(-73.0563296220301,4.37323048372606,12.));
#85530=CARTESIAN_POINT('Ctrl Pts',(-73.031699117799,4.38169311610153,12.));
#85531=CARTESIAN_POINT('Ctrl Pts',(-73.0070967198033,4.39012038961144,12.));
#85532=CARTESIAN_POINT('Ctrl Pts',(-72.9825225376839,4.3985123211973,12.));
#85533=CARTESIAN_POINT('Ctrl Pts',(-72.9579766814495,4.40686892793964,12.));
#85534=CARTESIAN_POINT('Ctrl Pts',(-72.9334592614828,4.41519022705926,12.));
#85535=CARTESIAN_POINT('Ctrl Pts',(-72.9089703885463,4.42347623591941,12.));
#85536=CARTESIAN_POINT('Ctrl Pts',(-72.8845101737856,4.43172697203341,12.));
#85537=CARTESIAN_POINT('Ctrl Pts',(-72.8600787287316,4.43994245306804,12.));
#85538=CARTESIAN_POINT('Ctrl Pts',(-72.8356761653064,4.44812269683724,12.));
#85539=CARTESIAN_POINT('Ctrl Pts',(-72.8113025958258,4.45626772130138,12.));
#85540=CARTESIAN_POINT('Ctrl Pts',(-72.7869581329994,4.46437754456795,12.));
#85541=CARTESIAN_POINT('Ctrl Pts',(-72.7626428899287,4.47245218489622,12.));
#85542=CARTESIAN_POINT('Ctrl Pts',(-72.7383569801042,4.48049166070223,12.));
#85543=CARTESIAN_POINT('Ctrl Pts',(-72.7141005174153,4.48849599055353,12.));
#85544=CARTESIAN_POINT('Ctrl Pts',(-72.689873616155,4.49646519316821,12.));
#85545=CARTESIAN_POINT('Ctrl Pts',(-72.6656763910241,4.50439928741604,12.));
#85546=CARTESIAN_POINT('Ctrl Pts',(-72.6415089571314,4.51229829232259,12.));
#85547=CARTESIAN_POINT('Ctrl Pts',(-72.6173714299935,4.52016222707632,12.));
#85548=CARTESIAN_POINT('Ctrl Pts',(-72.5932639255406,4.5279911110239,12.));
#85549=CARTESIAN_POINT('Ctrl Pts',(-72.5691865601225,4.53578496366801,12.));
#85550=CARTESIAN_POINT('Ctrl Pts',(-72.5451394505106,4.54354380466824,12.));
#85551=CARTESIAN_POINT('Ctrl Pts',(-72.5211227138997,4.55126765384402,12.));
#85552=CARTESIAN_POINT('Ctrl Pts',(-72.4971364679055,4.55895653118213,12.));
#85553=CARTESIAN_POINT('Ctrl Pts',(-72.473180830571,4.56661045683366,12.));
#85554=CARTESIAN_POINT('Ctrl Pts',(-72.449255920373,4.57422945111094,12.));
#85555=CARTESIAN_POINT('Ctrl Pts',(-72.4253618562249,4.5818135344885,12.));
#85556=CARTESIAN_POINT('Ctrl Pts',(-72.4014987574789,4.5893627276055,12.));
#85557=CARTESIAN_POINT('Ctrl Pts',(-72.3776667439244,4.5968770512734,12.));
#85558=CARTESIAN_POINT('Ctrl Pts',(-72.3538659357932,4.60435652647463,12.));
#85559=CARTESIAN_POINT('Ctrl Pts',(-72.330096453767,4.61180117435868,12.));
#85560=CARTESIAN_POINT('Ctrl Pts',(-72.306358418981,4.61921101624294,12.));
#85561=CARTESIAN_POINT('Ctrl Pts',(-72.2826519530254,4.62658607361465,12.));
#85562=CARTESIAN_POINT('Ctrl Pts',(-72.2589771779447,4.63392636813842,12.));
#85563=CARTESIAN_POINT('Ctrl Pts',(-72.2353342162408,4.64123192165627,12.));
#85564=CARTESIAN_POINT('Ctrl Pts',(-72.2117231908816,4.64850275618324,12.));
#85565=CARTESIAN_POINT('Ctrl Pts',(-72.1881442253052,4.65573889390824,12.));
#85566=CARTESIAN_POINT('Ctrl Pts',(-72.1645974434218,4.6629403571957,12.));
#85567=CARTESIAN_POINT('Ctrl Pts',(-72.1410829696129,4.6701071685928,12.));
#85568=CARTESIAN_POINT('Ctrl Pts',(-72.1176009287349,4.67723935083087,12.));
#85569=CARTESIAN_POINT('Ctrl Pts',(-72.0941514461283,4.6843369268206,12.));
#85570=CARTESIAN_POINT('Ctrl Pts',(-72.070734647621,4.69139991965279,12.));
#85571=CARTESIAN_POINT('Ctrl Pts',(-72.047350659532,4.69842835259997,12.));
#85572=CARTESIAN_POINT('Ctrl Pts',(-72.0239996086694,4.70542224912312,12.));
#85573=CARTESIAN_POINT('Ctrl Pts',(-72.0006816223335,4.7123816328741,12.));
#85574=CARTESIAN_POINT('Ctrl Pts',(-71.9773968283267,4.7193065276908,12.));
#85575=CARTESIAN_POINT('Ctrl Pts',(-71.9541453549582,4.72619695759778,12.));
#85576=CARTESIAN_POINT('Ctrl Pts',(-71.9309273310469,4.73305294680783,12.));
#85577=CARTESIAN_POINT('Ctrl Pts',(-71.9077428859207,4.7398745197286,12.));
#85578=CARTESIAN_POINT('Ctrl Pts',(-71.8845921494186,4.74666170096545,12.));
#85579=CARTESIAN_POINT('Ctrl Pts',(-71.8614752519008,4.7534145153167,12.));
#85580=CARTESIAN_POINT('Ctrl Pts',(-71.8383923242533,4.76013298777422,12.));
#85581=CARTESIAN_POINT('Ctrl Pts',(-71.8153434978924,4.76681714352503,12.));
#85582=CARTESIAN_POINT('Ctrl Pts',(-71.7923289047636,4.77346700795787,12.));
#85583=CARTESIAN_POINT('Ctrl Pts',(-71.7693486773449,4.78008260666642,12.));
#85584=CARTESIAN_POINT('Ctrl Pts',(-71.7464029486552,4.7866639654445,12.));
#85585=CARTESIAN_POINT('Ctrl Pts',(-71.7234918522604,4.79321111028671,12.));
#85586=CARTESIAN_POINT('Ctrl Pts',(-71.7006155222766,4.79972406739013,12.));
#85587=CARTESIAN_POINT('Ctrl Pts',(-71.6777740933705,4.80620286316088,12.));
#85588=CARTESIAN_POINT('Ctrl Pts',(-71.6549677007613,4.81264752421732,12.));
#85589=CARTESIAN_POINT('Ctrl Pts',(-71.6321964802326,4.81905807738557,12.));
#85590=CARTESIAN_POINT('Ctrl Pts',(-71.6094605681366,4.82543454970026,12.));
#85591=CARTESIAN_POINT('Ctrl Pts',(-71.5867601014,4.83177696840637,12.));
#85592=CARTESIAN_POINT('Ctrl Pts',(-71.564095217521,4.83808536096583,12.));
#85593=CARTESIAN_POINT('Ctrl Pts',(-71.5414660545739,4.84435975506048,12.));
#85594=CARTESIAN_POINT('Ctrl Pts',(-71.5188727512197,4.8506001785878,12.));
#85595=CARTESIAN_POINT('Ctrl Pts',(-71.4963154467113,4.8568066596618,12.));
#85596=CARTESIAN_POINT('Ctrl Pts',(-71.4737942808982,4.86297922661502,12.));
#85597=CARTESIAN_POINT('Ctrl Pts',(-71.4513093942255,4.86911790800549,12.));
#85598=CARTESIAN_POINT('Ctrl Pts',(-71.4288609277374,4.87522273261907,12.));
#85599=CARTESIAN_POINT('Ctrl Pts',(-71.4064490230899,4.88129372946551,12.));
#85600=CARTESIAN_POINT('Ctrl Pts',(-71.3840738225562,4.88733092777974,12.));
#85601=CARTESIAN_POINT('Ctrl Pts',(-71.3617354690325,4.89333435702413,12.));
#85602=CARTESIAN_POINT('Ctrl Pts',(-71.3394341060359,4.89930404689574,12.));
#85603=CARTESIAN_POINT('Ctrl Pts',(-71.3171698777084,4.90524002732778,12.));
#85604=CARTESIAN_POINT('Ctrl Pts',(-71.294942928829,4.91114232848603,12.));
#85605=CARTESIAN_POINT('Ctrl Pts',(-71.2727534048192,4.91701098077036,12.));
#85606=CARTESIAN_POINT('Ctrl Pts',(-71.250601451747,4.92284601481721,12.));
#85607=CARTESIAN_POINT('Ctrl Pts',(-71.2284872163273,4.92864746150732,12.));
#85608=CARTESIAN_POINT('Ctrl Pts',(-71.2064108459286,4.93441535196617,12.));
#85609=CARTESIAN_POINT('Ctrl Pts',(-71.1843724885847,4.94014971756114,12.));
#85610=CARTESIAN_POINT('Ctrl Pts',(-71.1623722930001,4.94585058990341,12.));
#85611=CARTESIAN_POINT('Ctrl Pts',(-71.1404104085552,4.95151800085101,12.));
#85612=CARTESIAN_POINT('Ctrl Pts',(-71.1184869853056,4.95715198251684,12.));
#85613=CARTESIAN_POINT('Ctrl Pts',(-71.0966021739907,4.96275256726765,12.));
#85614=CARTESIAN_POINT('Ctrl Pts',(-71.0747561260436,4.9683197877219,12.));
#85615=CARTESIAN_POINT('Ctrl Pts',(-71.0529489935961,4.97385367675158,12.));
#85616=CARTESIAN_POINT('Ctrl Pts',(-71.0311809294821,4.97935426748584,12.));
#85617=CARTESIAN_POINT('Ctrl Pts',(-71.0094520872377,4.98482159331863,12.));
#85618=CARTESIAN_POINT('Ctrl Pts',(-70.9877626211113,4.99025568790664,12.));
#85619=CARTESIAN_POINT('Ctrl Pts',(-70.9661126860773,4.99565658516913,12.));
#85620=CARTESIAN_POINT('Ctrl Pts',(-70.9445024378439,5.00102431929039,12.));
#85621=CARTESIAN_POINT('Ctrl Pts',(-70.9229320328589,5.00635892472513,12.));
#85622=CARTESIAN_POINT('Ctrl Pts',(-70.9014016283124,5.01166043620567,12.));
#85623=CARTESIAN_POINT('Ctrl Pts',(-70.8799113821452,5.0169288887379,12.));
#85624=CARTESIAN_POINT('Ctrl Pts',(-70.8584614530519,5.0221643176006,12.));
#85625=CARTESIAN_POINT('Ctrl Pts',(-70.8370520004843,5.02736675834692,12.));
#85626=CARTESIAN_POINT('Ctrl Pts',(-70.8156831846488,5.0325362468094,12.));
#85627=CARTESIAN_POINT('Ctrl Pts',(-70.7943551665059,5.03767281910479,12.));
#85628=CARTESIAN_POINT('Ctrl Pts',(-70.7730681077983,5.04277651163349,12.));
#85629=CARTESIAN_POINT('Ctrl Pts',(-70.7518221710706,5.04784736108346,12.));
#85630=CARTESIAN_POINT('Ctrl Pts',(-70.7306175196863,5.05288540443482,12.));
#85631=CARTESIAN_POINT('Ctrl Pts',(-70.7094543178438,5.05789067897057,12.));
#85632=CARTESIAN_POINT('Ctrl Pts',(-70.6883327305784,5.06286322227819,12.));
#85633=CARTESIAN_POINT('Ctrl Pts',(-70.6672529237455,5.06780307224071,12.));
#85634=CARTESIAN_POINT('Ctrl Pts',(-70.6462150640015,5.07271026703354,12.));
#85635=CARTESIAN_POINT('Ctrl Pts',(-70.6252193187878,5.07758484512302,12.));
#85636=CARTESIAN_POINT('Ctrl Pts',(-70.6042658562923,5.08242684526686,12.));
#85637=CARTESIAN_POINT('Ctrl Pts',(-70.5833548455014,5.08723630652272,12.));
#85638=CARTESIAN_POINT('Ctrl Pts',(-70.5624864562824,5.09201326826134,12.));
#85639=CARTESIAN_POINT('Ctrl Pts',(-70.5416608594526,5.09675777018182,12.));
#85640=CARTESIAN_POINT('Ctrl Pts',(-70.5208782268497,5.1014698523294,12.));
#85641=CARTESIAN_POINT('Ctrl Pts',(-70.500138731399,5.10614955511663,12.));
#85642=CARTESIAN_POINT('Ctrl Pts',(-70.4794425469825,5.11079691929213,12.));
#85643=CARTESIAN_POINT('Ctrl Pts',(-70.458789848296,5.11541198590932,12.));
#85644=CARTESIAN_POINT('Ctrl Pts',(-70.4381808107245,5.11999479630211,12.));
#85645=CARTESIAN_POINT('Ctrl Pts',(-70.417615610161,5.12454539205328,12.));
#85646=CARTESIAN_POINT('Ctrl Pts',(-70.3970944229851,5.12906381499456,12.));
#85647=CARTESIAN_POINT('Ctrl Pts',(-70.3766174264757,5.13355010728567,12.));
#85648=CARTESIAN_POINT('Ctrl Pts',(-70.3561847991714,5.13800431148903,12.));
#85649=CARTESIAN_POINT('Ctrl Pts',(-70.3357967211796,5.14242647063479,12.));
#85650=CARTESIAN_POINT('Ctrl Pts',(-70.3154533746736,5.1468166283308,12.));
#85651=CARTESIAN_POINT('Ctrl Pts',(-70.2951549435512,5.15117482869254,12.));
#85652=CARTESIAN_POINT('Ctrl Pts',(-70.2749016125105,5.15550111614859,12.));
#85653=CARTESIAN_POINT('Ctrl Pts',(-70.2546935662722,5.15979553528203,12.));
#85654=CARTESIAN_POINT('Ctrl Pts',(-70.2345309887833,5.16405813066976,12.));
#85655=CARTESIAN_POINT('Ctrl Pts',(-70.2144140622953,5.16828894670108,12.));
#85656=CARTESIAN_POINT('Ctrl Pts',(-70.1943429691167,5.17248802793389,12.));
#85657=CARTESIAN_POINT('Ctrl Pts',(-70.1743178937077,5.17665541952382,12.));
#85658=CARTESIAN_POINT('Ctrl Pts',(-70.1543390243892,5.18079116757666,12.));
#85659=CARTESIAN_POINT('Ctrl Pts',(-70.1344065558145,5.18489531966264,12.));
#85660=CARTESIAN_POINT('Ctrl Pts',(-70.1145206891885,5.18896792486565,12.));
#85661=CARTESIAN_POINT('Ctrl Pts',(-70.0946816270997,5.19300903271579,12.));
#85662=CARTESIAN_POINT('Ctrl Pts',(-70.0748895689729,5.19701869225528,12.));
#85663=CARTESIAN_POINT('Ctrl Pts',(-70.0551447071082,5.20099695122656,12.));
#85664=CARTESIAN_POINT('Ctrl Pts',(-70.0354472203546,5.20494385478025,12.));
#85665=CARTESIAN_POINT('Ctrl Pts',(-70.0157972802182,5.20885944672836,12.));
#85666=CARTESIAN_POINT('Ctrl Pts',(-69.9961950629965,5.21274377203259,12.));
#85667=CARTESIAN_POINT('Ctrl Pts',(-69.9766407595385,5.21659687881139,12.));
#85668=CARTESIAN_POINT('Ctrl Pts',(-69.9571345870076,5.2204188207572,12.));
#85669=CARTESIAN_POINT('Ctrl Pts',(-69.9376767969095,5.22420965879981,12.));
#85670=CARTESIAN_POINT('Ctrl Pts',(-69.9182676502048,5.22796945602793,12.));
#85671=CARTESIAN_POINT('Ctrl Pts',(-69.8989073936688,5.23169827290555,12.));
#85672=CARTESIAN_POINT('Ctrl Pts',(-69.8795962381599,5.2353961627962,12.));
#85673=CARTESIAN_POINT('Ctrl Pts',(-69.8603343302743,5.23906316634802,12.));
#85674=CARTESIAN_POINT('Ctrl Pts',(-69.841121750752,5.24269931054569,12.));
#85675=CARTESIAN_POINT('Ctrl Pts',(-69.8257911792159,5.2455835515975,12.));
#85676=CARTESIAN_POINT('Ctrl Pts',(-69.8143154684204,5.24773285666376,12.));
#85677=CARTESIAN_POINT('Ctrl Pts',(-69.8066748687772,5.24915955997427,12.));
#85678=CARTESIAN_POINT('Ctrl Pts',(-69.8028570375097,5.24987136994592,12.));
#85679=CARTESIAN_POINT('Ctrl Pts',(-74.1624659714955,2.48034921844904,-2.77555756156289E-15));
#85680=CARTESIAN_POINT('Ctrl Pts',(-74.1624659714955,2.48034921844904,4.));
#85681=CARTESIAN_POINT('Ctrl Pts',(-74.1624659714955,2.48034921844904,8.));
#85682=CARTESIAN_POINT('Ctrl Pts',(-74.1624659714955,2.48034921844904,12.));
#85683=CARTESIAN_POINT('Ctrl Pts',(-74.2610905805698,2.52879860312848,-2.77555756156289E-15));
#85684=CARTESIAN_POINT('Ctrl Pts',(-74.2610905805698,2.52879860312848,4.));
#85685=CARTESIAN_POINT('Ctrl Pts',(-74.2610905805698,2.52879860312849,8.));
#85686=CARTESIAN_POINT('Ctrl Pts',(-74.2610905805698,2.52879860312849,12.));
#85687=CARTESIAN_POINT('Ctrl Pts',(-74.4041075779819,2.67239300265259,-2.55632103913301E-15));
#85688=CARTESIAN_POINT('Ctrl Pts',(-74.4041075779819,2.67239300265259,4.));
#85689=CARTESIAN_POINT('Ctrl Pts',(-74.4041075779819,2.67239300265259,7.99999999999999));
#85690=CARTESIAN_POINT('Ctrl Pts',(-74.4041075779819,2.67239300265259,12.));
#85691=CARTESIAN_POINT('Ctrl Pts',(-74.444876171298,2.86656650944678,-2.03572402097153E-15));
#85692=CARTESIAN_POINT('Ctrl Pts',(-74.444876171298,2.86656650944678,4.));
#85693=CARTESIAN_POINT('Ctrl Pts',(-74.444876171298,2.86656650944676,8.00000000000001));
#85694=CARTESIAN_POINT('Ctrl Pts',(-74.444876171298,2.86656650944676,12.));
#85695=CARTESIAN_POINT('Ctrl Pts',(-74.4416140848739,2.94891377268016,-1.78476208028845E-15));
#85696=CARTESIAN_POINT('Ctrl Pts',(-74.4416140848739,2.94891377268016,4.));
#85697=CARTESIAN_POINT('Ctrl Pts',(-74.4416140848739,2.94891377268014,8.));
#85698=CARTESIAN_POINT('Ctrl Pts',(-74.4416140848739,2.94891377268014,12.));
#85699=CARTESIAN_POINT('',(-74.1624659714955,2.48034921844904,0.));
#85700=CARTESIAN_POINT('',(-74.4416140848739,2.94891377268016,0.));
#85701=CARTESIAN_POINT('Ctrl Pts',(-74.1624659714955,2.48034921844904,-9.71445146547012E-16));
#85702=CARTESIAN_POINT('Ctrl Pts',(-74.2610905805698,2.52879860312848,-9.71445146547012E-16));
#85703=CARTESIAN_POINT('Ctrl Pts',(-74.342814579091,2.61085254571368,-8.46167133729938E-16));
#85704=CARTESIAN_POINT('Ctrl Pts',(-74.3911513436217,2.70942211516259,-6.22485693735197E-16));
#85705=CARTESIAN_POINT('Ctrl Pts',(-74.4274039170197,2.78334929224927,-4.54724613739141E-16));
#85706=CARTESIAN_POINT('Ctrl Pts',(-74.444876171298,2.86656650944678,-2.31611605955647E-16));
#85707=CARTESIAN_POINT('Ctrl Pts',(-74.4416140848739,2.94891377268016,1.93503347274265E-17));
#85708=CARTESIAN_POINT('',(-74.4416140848739,2.94891377268014,12.));
#85709=CARTESIAN_POINT('Ctrl Pts',(-74.4416140848739,2.94891377268016,-1.78476208028845E-15));
#85710=CARTESIAN_POINT('Ctrl Pts',(-74.4416140848739,2.94891377268016,4.));
#85711=CARTESIAN_POINT('Ctrl Pts',(-74.4416140848739,2.94891377268014,8.));
#85712=CARTESIAN_POINT('Ctrl Pts',(-74.4416140848739,2.94891377268014,12.));
#85713=CARTESIAN_POINT('',(-74.1624659714955,2.48034921844905,12.));
#85714=CARTESIAN_POINT('Ctrl Pts',(-74.4416140848739,2.94891377268014,12.));
#85715=CARTESIAN_POINT('Ctrl Pts',(-74.444876171298,2.86656650944676,12.));
#85716=CARTESIAN_POINT('Ctrl Pts',(-74.4274039170196,2.78334929224926,12.));
#85717=CARTESIAN_POINT('Ctrl Pts',(-74.3911513436217,2.70942211516259,12.));
#85718=CARTESIAN_POINT('Ctrl Pts',(-74.342814579091,2.61085254571369,12.));
#85719=CARTESIAN_POINT('Ctrl Pts',(-74.2610905805698,2.52879860312849,12.));
#85720=CARTESIAN_POINT('Ctrl Pts',(-74.1624659714955,2.48034921844904,12.));
#85721=CARTESIAN_POINT('Ctrl Pts',(-74.1624659714955,2.48034921844904,12.));
#85722=CARTESIAN_POINT('Ctrl Pts',(-74.1624659714955,2.48034921844904,8.));
#85723=CARTESIAN_POINT('Ctrl Pts',(-74.1624659714955,2.48034921844904,4.));
#85724=CARTESIAN_POINT('Ctrl Pts',(-74.1624659714955,2.48034921844904,-2.77555756156289E-15));
#85725=CARTESIAN_POINT('Origin',(-3.74491326291036E-10,1.62512913209675E-11,
0.));
#85726=CARTESIAN_POINT('Origin',(-3.74491326291036E-10,1.62512913209675E-11,
12.));
#85727=CARTESIAN_POINT('Origin',(-3.74491326291036E-10,1.62512913209675E-11,
0.));
#85728=CARTESIAN_POINT('Ctrl Pts',(-73.8227522002498,10.0225374821206,0.));
#85729=CARTESIAN_POINT('Ctrl Pts',(-73.8227522002498,10.0225374821206,4.));
#85730=CARTESIAN_POINT('Ctrl Pts',(-73.8227522002498,10.0225374821206,8.));
#85731=CARTESIAN_POINT('Ctrl Pts',(-73.8227522002498,10.0225374821206,12.));
#85732=CARTESIAN_POINT('Ctrl Pts',(-73.8079696346554,10.1314210536418,0.));
#85733=CARTESIAN_POINT('Ctrl Pts',(-73.8079696346554,10.1314210536418,4.));
#85734=CARTESIAN_POINT('Ctrl Pts',(-73.8079696346554,10.1314210536418,8.00000000000001));
#85735=CARTESIAN_POINT('Ctrl Pts',(-73.8079696346554,10.1314210536418,12.));
#85736=CARTESIAN_POINT('Ctrl Pts',(-73.716956764919,10.3125002643521,-7.30802048705264E-17));
#85737=CARTESIAN_POINT('Ctrl Pts',(-73.716956764919,10.3125002643521,4.00000000000001));
#85738=CARTESIAN_POINT('Ctrl Pts',(-73.716956764919,10.3125002643521,7.99999999999999));
#85739=CARTESIAN_POINT('Ctrl Pts',(-73.716956764919,10.3125002643521,12.));
#85740=CARTESIAN_POINT('Ctrl Pts',(-73.5456341632194,10.4125694172281,-2.46611180232542E-16));
#85741=CARTESIAN_POINT('Ctrl Pts',(-73.5456341632194,10.4125694172281,3.99999999999999));
#85742=CARTESIAN_POINT('Ctrl Pts',(-73.5456341632194,10.4125694172281,8.00000000000001));
#85743=CARTESIAN_POINT('Ctrl Pts',(-73.5456341632194,10.4125694172281,12.));
#85744=CARTESIAN_POINT('Ctrl Pts',(-73.4664795929516,10.4355099267394,-3.30265160469984E-16));
#85745=CARTESIAN_POINT('Ctrl Pts',(-73.4664795929516,10.4355099267394,4.));
#85746=CARTESIAN_POINT('Ctrl Pts',(-73.4664795929516,10.4355099267394,8.));
#85747=CARTESIAN_POINT('Ctrl Pts',(-73.4664795929516,10.4355099267394,12.));
#85748=CARTESIAN_POINT('',(-73.8227522002498,10.0225374821206,0.));
#85749=CARTESIAN_POINT('',(-73.4664795929515,10.4355099267392,0.));
#85750=CARTESIAN_POINT('Ctrl Pts',(-73.8227522002498,10.0225374821206,2.7442551750438E-17));
#85751=CARTESIAN_POINT('Ctrl Pts',(-73.8079696346554,10.1314210536418,2.74425517504379E-17));
#85752=CARTESIAN_POINT('Ctrl Pts',(-73.7559622805204,10.2348948883334,-1.43175653184342E-17));
#85753=CARTESIAN_POINT('Ctrl Pts',(-73.6777313404381,10.3119164592424,-8.88779339763642E-17));
#85754=CARTESIAN_POINT('Ctrl Pts',(-73.6190581353764,10.3696826374241,-1.44798210469812E-16));
#85755=CARTESIAN_POINT('Ctrl Pts',(-73.5456341632194,10.4125694172281,-2.19168628482104E-16));
#85756=CARTESIAN_POINT('Ctrl Pts',(-73.4664795929516,10.4355099267394,-3.02822608719546E-16));
#85757=CARTESIAN_POINT('',(-73.4664795929515,10.4355099267392,12.));
#85758=CARTESIAN_POINT('Ctrl Pts',(-73.4664795929516,10.4355099267394,-3.30265160469984E-16));
#85759=CARTESIAN_POINT('Ctrl Pts',(-73.4664795929516,10.4355099267394,4.));
#85760=CARTESIAN_POINT('Ctrl Pts',(-73.4664795929516,10.4355099267394,8.));
#85761=CARTESIAN_POINT('Ctrl Pts',(-73.4664795929516,10.4355099267394,12.));
#85762=CARTESIAN_POINT('',(-73.8227522002498,10.0225374821206,12.));
#85763=CARTESIAN_POINT('Ctrl Pts',(-73.4664795929516,10.4355099267394,12.));
#85764=CARTESIAN_POINT('Ctrl Pts',(-73.5456341632194,10.4125694172281,12.));
#85765=CARTESIAN_POINT('Ctrl Pts',(-73.6190581353764,10.3696826374241,12.));
#85766=CARTESIAN_POINT('Ctrl Pts',(-73.6777313404381,10.3119164592424,12.));
#85767=CARTESIAN_POINT('Ctrl Pts',(-73.7559622805204,10.2348948883334,12.));
#85768=CARTESIAN_POINT('Ctrl Pts',(-73.8079696346554,10.1314210536418,12.));
#85769=CARTESIAN_POINT('Ctrl Pts',(-73.8227522002498,10.0225374821206,12.));
#85770=CARTESIAN_POINT('Ctrl Pts',(-73.8227522002498,10.0225374821206,12.));
#85771=CARTESIAN_POINT('Ctrl Pts',(-73.8227522002498,10.0225374821206,8.));
#85772=CARTESIAN_POINT('Ctrl Pts',(-73.8227522002498,10.0225374821206,4.));
#85773=CARTESIAN_POINT('Ctrl Pts',(-73.8227522002498,10.0225374821206,0.));
#85774=CARTESIAN_POINT('Ctrl Pts',(-69.079679653846,11.3136138754166,0.));
#85775=CARTESIAN_POINT('Ctrl Pts',(-69.079679653846,11.3136138754166,12.));
#85776=CARTESIAN_POINT('Ctrl Pts',(-69.0835449954396,11.3132375200165,0.));
#85777=CARTESIAN_POINT('Ctrl Pts',(-69.0835449954396,11.3132375200165,12.));
#85778=CARTESIAN_POINT('Ctrl Pts',(-69.0912808656811,11.3124821678798,0.));
#85779=CARTESIAN_POINT('Ctrl Pts',(-69.0912808656811,11.3124821678798,12.));
#85780=CARTESIAN_POINT('Ctrl Pts',(-69.1029002322118,11.3113412156662,0.));
#85781=CARTESIAN_POINT('Ctrl Pts',(-69.1029002322118,11.3113412156662,12.));
#85782=CARTESIAN_POINT('Ctrl Pts',(-69.118423844466,11.3098040973713,0.));
#85783=CARTESIAN_POINT('Ctrl Pts',(-69.118423844466,11.3098040973713,12.));
#85784=CARTESIAN_POINT('Ctrl Pts',(-69.1378802251711,11.3078562764385,0.));
#85785=CARTESIAN_POINT('Ctrl Pts',(-69.1378802251711,11.3078562764385,12.));
#85786=CARTESIAN_POINT('Ctrl Pts',(-69.1573884361,11.3058820128308,0.));
#85787=CARTESIAN_POINT('Ctrl Pts',(-69.1573884361,11.3058820128308,12.));
#85788=CARTESIAN_POINT('Ctrl Pts',(-69.1769483991721,11.3038812726293,0.));
#85789=CARTESIAN_POINT('Ctrl Pts',(-69.1769483991721,11.3038812726293,12.));
#85790=CARTESIAN_POINT('Ctrl Pts',(-69.1965599718914,11.3018540025638,0.));
#85791=CARTESIAN_POINT('Ctrl Pts',(-69.1965599718914,11.3018540025638,12.));
#85792=CARTESIAN_POINT('Ctrl Pts',(-69.2162229488531,11.2998001310964,0.));
#85793=CARTESIAN_POINT('Ctrl Pts',(-69.2162229488531,11.2998001310964,12.));
#85794=CARTESIAN_POINT('Ctrl Pts',(-69.2359370894907,11.2977195764853,0.));
#85795=CARTESIAN_POINT('Ctrl Pts',(-69.2359370894907,11.2977195764853,12.));
#85796=CARTESIAN_POINT('Ctrl Pts',(-69.255702139335,11.2956122531375,0.));
#85797=CARTESIAN_POINT('Ctrl Pts',(-69.255702139335,11.2956122531375,12.));
#85798=CARTESIAN_POINT('Ctrl Pts',(-69.2755178531479,11.2934780784351,0.));
#85799=CARTESIAN_POINT('Ctrl Pts',(-69.2755178531479,11.2934780784351,12.));
#85800=CARTESIAN_POINT('Ctrl Pts',(-69.295384019272,11.2913169799628,0.));
#85801=CARTESIAN_POINT('Ctrl Pts',(-69.295384019272,11.2913169799628,12.));
#85802=CARTESIAN_POINT('Ctrl Pts',(-69.3153004517783,11.2891288931517,0.));
#85803=CARTESIAN_POINT('Ctrl Pts',(-69.3153004517783,11.2891288931517,12.));
#85804=CARTESIAN_POINT('Ctrl Pts',(-69.3352669789587,11.2869137578459,0.));
#85805=CARTESIAN_POINT('Ctrl Pts',(-69.3352669789587,11.2869137578459,12.));
#85806=CARTESIAN_POINT('Ctrl Pts',(-69.3552834337784,11.2846715154524,0.));
#85807=CARTESIAN_POINT('Ctrl Pts',(-69.3552834337784,11.2846715154524,12.));
#85808=CARTESIAN_POINT('Ctrl Pts',(-69.3753496420039,11.2824021054045,0.));
#85809=CARTESIAN_POINT('Ctrl Pts',(-69.3753496420039,11.2824021054045,12.));
#85810=CARTESIAN_POINT('Ctrl Pts',(-69.3954654162281,11.2801054633816,0.));
#85811=CARTESIAN_POINT('Ctrl Pts',(-69.3954654162281,11.2801054633816,12.));
#85812=CARTESIAN_POINT('Ctrl Pts',(-69.4156305620593,11.2777815231469,0.));
#85813=CARTESIAN_POINT('Ctrl Pts',(-69.4156305620593,11.2777815231469,12.));
#85814=CARTESIAN_POINT('Ctrl Pts',(-69.4358448819967,11.2754302177021,0.));
#85815=CARTESIAN_POINT('Ctrl Pts',(-69.4358448819967,11.2754302177021,12.));
#85816=CARTESIAN_POINT('Ctrl Pts',(-69.456108179879,11.2730514806139,0.));
#85817=CARTESIAN_POINT('Ctrl Pts',(-69.456108179879,11.2730514806139,12.));
#85818=CARTESIAN_POINT('Ctrl Pts',(-69.4764202659397,11.270645247528,0.));
#85819=CARTESIAN_POINT('Ctrl Pts',(-69.4764202659397,11.270645247528,12.));
#85820=CARTESIAN_POINT('Ctrl Pts',(-69.4967809565929,11.2682114561008,0.));
#85821=CARTESIAN_POINT('Ctrl Pts',(-69.4967809565929,11.2682114561008,12.));
#85822=CARTESIAN_POINT('Ctrl Pts',(-69.5171900720158,11.2657500452716,0.));
#85823=CARTESIAN_POINT('Ctrl Pts',(-69.5171900720158,11.2657500452716,12.));
#85824=CARTESIAN_POINT('Ctrl Pts',(-69.5376474344771,11.263260954763,0.));
#85825=CARTESIAN_POINT('Ctrl Pts',(-69.5376474344771,11.263260954763,12.));
#85826=CARTESIAN_POINT('Ctrl Pts',(-69.5581528662877,11.2607441244703,0.));
#85827=CARTESIAN_POINT('Ctrl Pts',(-69.5581528662877,11.2607441244703,12.));
#85828=CARTESIAN_POINT('Ctrl Pts',(-69.5787061880857,11.2581994939541,0.));
#85829=CARTESIAN_POINT('Ctrl Pts',(-69.5787061880857,11.2581994939541,12.));
#85830=CARTESIAN_POINT('Ctrl Pts',(-69.599307219739,11.2556270027016,0.));
#85831=CARTESIAN_POINT('Ctrl Pts',(-69.599307219739,11.2556270027016,12.));
#85832=CARTESIAN_POINT('Ctrl Pts',(-69.6199557811245,11.2530265903558,0.));
#85833=CARTESIAN_POINT('Ctrl Pts',(-69.6199557811245,11.2530265903558,12.));
#85834=CARTESIAN_POINT('Ctrl Pts',(-69.6406516928891,11.2503981969412,0.));
#85835=CARTESIAN_POINT('Ctrl Pts',(-69.6406516928891,11.2503981969412,12.));
#85836=CARTESIAN_POINT('Ctrl Pts',(-69.6613947773534,11.2477417631386,0.));
#85837=CARTESIAN_POINT('Ctrl Pts',(-69.6613947773534,11.2477417631386,12.));
#85838=CARTESIAN_POINT('Ctrl Pts',(-69.6821848588457,11.2450572303841,0.));
#85839=CARTESIAN_POINT('Ctrl Pts',(-69.6821848588457,11.2450572303841,12.));
#85840=CARTESIAN_POINT('Ctrl Pts',(-69.7030217632164,11.2423445407167,0.));
#85841=CARTESIAN_POINT('Ctrl Pts',(-69.7030217632164,11.2423445407167,12.));
#85842=CARTESIAN_POINT('Ctrl Pts',(-69.7239053175356,11.239603636686,0.));
#85843=CARTESIAN_POINT('Ctrl Pts',(-69.7239053175356,11.239603636686,12.));
#85844=CARTESIAN_POINT('Ctrl Pts',(-69.7448353497408,11.2368344612473,0.));
#85845=CARTESIAN_POINT('Ctrl Pts',(-69.7448353497408,11.2368344612473,12.));
#85846=CARTESIAN_POINT('Ctrl Pts',(-69.7658116882324,11.2340369576456,0.));
#85847=CARTESIAN_POINT('Ctrl Pts',(-69.7658116882324,11.2340369576456,12.));
#85848=CARTESIAN_POINT('Ctrl Pts',(-69.7868341618954,11.2312110694188,0.));
#85849=CARTESIAN_POINT('Ctrl Pts',(-69.7868341618954,11.2312110694188,12.));
#85850=CARTESIAN_POINT('Ctrl Pts',(-69.8079026002768,11.2283567404437,0.));
#85851=CARTESIAN_POINT('Ctrl Pts',(-69.8079026002768,11.2283567404437,12.));
#85852=CARTESIAN_POINT('Ctrl Pts',(-69.8290168337076,11.2254739149721,0.));
#85853=CARTESIAN_POINT('Ctrl Pts',(-69.8290168337076,11.2254739149721,12.));
#85854=CARTESIAN_POINT('Ctrl Pts',(-69.8501766934428,11.2225625376737,0.));
#85855=CARTESIAN_POINT('Ctrl Pts',(-69.8501766934428,11.2225625376737,12.));
#85856=CARTESIAN_POINT('Ctrl Pts',(-69.871382011789,11.219622553679,0.));
#85857=CARTESIAN_POINT('Ctrl Pts',(-69.871382011789,11.219622553679,12.));
#85858=CARTESIAN_POINT('Ctrl Pts',(-69.8926326220385,11.2166539085523,0.));
#85859=CARTESIAN_POINT('Ctrl Pts',(-69.8926326220385,11.2166539085523,12.));
#85860=CARTESIAN_POINT('Ctrl Pts',(-69.9139283584021,11.2136565482678,0.));
#85861=CARTESIAN_POINT('Ctrl Pts',(-69.9139283584021,11.2136565482678,12.));
#85862=CARTESIAN_POINT('Ctrl Pts',(-69.9352690559405,11.2106304191883,0.));
#85863=CARTESIAN_POINT('Ctrl Pts',(-69.9352690559405,11.2106304191883,12.));
#85864=CARTESIAN_POINT('Ctrl Pts',(-69.9566545504837,11.2075754680449,0.));
#85865=CARTESIAN_POINT('Ctrl Pts',(-69.9566545504837,11.2075754680449,12.));
#85866=CARTESIAN_POINT('Ctrl Pts',(-69.97808467858,11.2044916419244,0.));
#85867=CARTESIAN_POINT('Ctrl Pts',(-69.97808467858,11.2044916419244,12.));
#85868=CARTESIAN_POINT('Ctrl Pts',(-69.9995592775343,11.2013788882714,0.));
#85869=CARTESIAN_POINT('Ctrl Pts',(-69.9995592775343,11.2013788882714,12.));
#85870=CARTESIAN_POINT('Ctrl Pts',(-70.0210781854243,11.1982371548919,0.));
#85871=CARTESIAN_POINT('Ctrl Pts',(-70.0210781854243,11.1982371548919,12.));
#85872=CARTESIAN_POINT('Ctrl Pts',(-70.0426412411185,11.1950663899577,0.));
#85873=CARTESIAN_POINT('Ctrl Pts',(-70.0426412411185,11.1950663899577,12.));
#85874=CARTESIAN_POINT('Ctrl Pts',(-70.0642482842928,11.1918665420167,0.));
#85875=CARTESIAN_POINT('Ctrl Pts',(-70.0642482842928,11.1918665420167,12.));
#85876=CARTESIAN_POINT('Ctrl Pts',(-70.0858991554283,11.1886375599914,0.));
#85877=CARTESIAN_POINT('Ctrl Pts',(-70.0858991554283,11.1886375599914,12.));
#85878=CARTESIAN_POINT('Ctrl Pts',(-70.1075936957968,11.185379393167,0.));
#85879=CARTESIAN_POINT('Ctrl Pts',(-70.1075936957968,11.185379393167,12.));
#85880=CARTESIAN_POINT('Ctrl Pts',(-70.1293317474432,11.1820919911846,0.));
#85881=CARTESIAN_POINT('Ctrl Pts',(-70.1293317474432,11.1820919911846,12.));
#85882=CARTESIAN_POINT('Ctrl Pts',(-70.1511131531674,11.1787753040363,0.));
#85883=CARTESIAN_POINT('Ctrl Pts',(-70.1511131531674,11.1787753040363,12.));
#85884=CARTESIAN_POINT('Ctrl Pts',(-70.1729377564956,11.1754292820631,0.));
#85885=CARTESIAN_POINT('Ctrl Pts',(-70.1729377564956,11.1754292820631,12.));
#85886=CARTESIAN_POINT('Ctrl Pts',(-70.1948054016817,11.1720538759499,0.));
#85887=CARTESIAN_POINT('Ctrl Pts',(-70.1948054016817,11.1720538759499,12.));
#85888=CARTESIAN_POINT('Ctrl Pts',(-70.2167159337095,11.168649036721,0.));
#85889=CARTESIAN_POINT('Ctrl Pts',(-70.2167159337095,11.168649036721,12.));
#85890=CARTESIAN_POINT('Ctrl Pts',(-70.2386691982902,11.1652147157383,0.));
#85891=CARTESIAN_POINT('Ctrl Pts',(-70.2386691982902,11.1652147157383,12.));
#85892=CARTESIAN_POINT('Ctrl Pts',(-70.2606650418589,11.1617508647017,0.));
#85893=CARTESIAN_POINT('Ctrl Pts',(-70.2606650418589,11.1617508647017,12.));
#85894=CARTESIAN_POINT('Ctrl Pts',(-70.2827033115662,11.1582574356522,0.));
#85895=CARTESIAN_POINT('Ctrl Pts',(-70.2827033115662,11.1582574356522,12.));
#85896=CARTESIAN_POINT('Ctrl Pts',(-70.3047838552757,11.1547343809647,0.));
#85897=CARTESIAN_POINT('Ctrl Pts',(-70.3047838552757,11.1547343809647,12.));
#85898=CARTESIAN_POINT('Ctrl Pts',(-70.3269065215591,11.1511816533422,0.));
#85899=CARTESIAN_POINT('Ctrl Pts',(-70.3269065215591,11.1511816533422,12.));
#85900=CARTESIAN_POINT('Ctrl Pts',(-70.3490711596882,11.1475992058124,0.));
#85901=CARTESIAN_POINT('Ctrl Pts',(-70.3490711596882,11.1475992058124,12.));
#85902=CARTESIAN_POINT('Ctrl Pts',(-70.3712776196216,11.1439869917269,0.));
#85903=CARTESIAN_POINT('Ctrl Pts',(-70.3712776196216,11.1439869917269,12.));
#85904=CARTESIAN_POINT('Ctrl Pts',(-70.3935257519945,11.1403449647622,0.));
#85905=CARTESIAN_POINT('Ctrl Pts',(-70.3935257519945,11.1403449647622,12.));
#85906=CARTESIAN_POINT('Ctrl Pts',(-70.415815408119,11.1366730789123,0.));
#85907=CARTESIAN_POINT('Ctrl Pts',(-70.415815408119,11.1366730789123,12.));
#85908=CARTESIAN_POINT('Ctrl Pts',(-70.438146439981,11.1329712884845,0.));
#85909=CARTESIAN_POINT('Ctrl Pts',(-70.438146439981,11.1329712884845,12.));
#85910=CARTESIAN_POINT('Ctrl Pts',(-70.4605187002356,11.1292395480975,0.));
#85911=CARTESIAN_POINT('Ctrl Pts',(-70.4605187002356,11.1292395480975,12.));
#85912=CARTESIAN_POINT('Ctrl Pts',(-70.4829320421973,11.1254778126824,0.));
#85913=CARTESIAN_POINT('Ctrl Pts',(-70.4829320421973,11.1254778126824,12.));
#85914=CARTESIAN_POINT('Ctrl Pts',(-70.5053863198306,11.121686037483,0.));
#85915=CARTESIAN_POINT('Ctrl Pts',(-70.5053863198306,11.121686037483,12.));
#85916=CARTESIAN_POINT('Ctrl Pts',(-70.5278813877519,11.117864178048,0.));
#85917=CARTESIAN_POINT('Ctrl Pts',(-70.5278813877519,11.117864178048,12.));
#85918=CARTESIAN_POINT('Ctrl Pts',(-70.5504171012247,11.1140121902274,0.));
#85919=CARTESIAN_POINT('Ctrl Pts',(-70.5504171012247,11.1140121902274,12.));
#85920=CARTESIAN_POINT('Ctrl Pts',(-70.5729933161538,11.1101300301701,0.));
#85921=CARTESIAN_POINT('Ctrl Pts',(-70.5729933161538,11.1101300301701,12.));
#85922=CARTESIAN_POINT('Ctrl Pts',(-70.5956098890744,11.1062176543258,0.));
#85923=CARTESIAN_POINT('Ctrl Pts',(-70.5956098890744,11.1062176543258,12.));
#85924=CARTESIAN_POINT('Ctrl Pts',(-70.6182666771441,11.102275019444,0.));
#85925=CARTESIAN_POINT('Ctrl Pts',(-70.6182666771441,11.102275019444,12.));
#85926=CARTESIAN_POINT('Ctrl Pts',(-70.6409635381446,11.0983020825662,0.));
#85927=CARTESIAN_POINT('Ctrl Pts',(-70.6409635381446,11.0983020825662,12.));
#85928=CARTESIAN_POINT('Ctrl Pts',(-70.6637003304768,11.0942988010231,0.));
#85929=CARTESIAN_POINT('Ctrl Pts',(-70.6637003304768,11.0942988010231,12.));
#85930=CARTESIAN_POINT('Ctrl Pts',(-70.686476913156,11.0902651324326,0.));
#85931=CARTESIAN_POINT('Ctrl Pts',(-70.686476913156,11.0902651324326,12.));
#85932=CARTESIAN_POINT('Ctrl Pts',(-70.7092931457996,11.0862010347022,0.));
#85933=CARTESIAN_POINT('Ctrl Pts',(-70.7092931457996,11.0862010347022,12.));
#85934=CARTESIAN_POINT('Ctrl Pts',(-70.7321488886229,11.0821064660276,0.));
#85935=CARTESIAN_POINT('Ctrl Pts',(-70.7321488886229,11.0821064660276,12.));
#85936=CARTESIAN_POINT('Ctrl Pts',(-70.7550440024422,11.0779813848851,0.));
#85937=CARTESIAN_POINT('Ctrl Pts',(-70.7550440024422,11.0779813848851,12.));
#85938=CARTESIAN_POINT('Ctrl Pts',(-70.7779783486689,11.0738257500292,0.));
#85939=CARTESIAN_POINT('Ctrl Pts',(-70.7779783486689,11.0738257500292,12.));
#85940=CARTESIAN_POINT('Ctrl Pts',(-70.8009517893042,11.0696395204908,0.));
#85941=CARTESIAN_POINT('Ctrl Pts',(-70.8009517893042,11.0696395204908,12.));
#85942=CARTESIAN_POINT('Ctrl Pts',(-70.8239641869266,11.0654226555799,0.));
#85943=CARTESIAN_POINT('Ctrl Pts',(-70.8239641869266,11.0654226555799,12.));
#85944=CARTESIAN_POINT('Ctrl Pts',(-70.847015404688,11.0611751148831,0.));
#85945=CARTESIAN_POINT('Ctrl Pts',(-70.847015404688,11.0611751148831,12.));
#85946=CARTESIAN_POINT('Ctrl Pts',(-70.8701053063158,11.0568968582566,0.));
#85947=CARTESIAN_POINT('Ctrl Pts',(-70.8701053063158,11.0568968582566,12.));
#85948=CARTESIAN_POINT('Ctrl Pts',(-70.8932337561079,11.0525878458242,0.));
#85949=CARTESIAN_POINT('Ctrl Pts',(-70.8932337561079,11.0525878458242,12.));
#85950=CARTESIAN_POINT('Ctrl Pts',(-70.9164006189283,11.0482480379752,0.));
#85951=CARTESIAN_POINT('Ctrl Pts',(-70.9164006189283,11.0482480379752,12.));
#85952=CARTESIAN_POINT('Ctrl Pts',(-70.9396057601953,11.0438773953686,0.));
#85953=CARTESIAN_POINT('Ctrl Pts',(-70.9396057601953,11.0438773953686,12.));
#85954=CARTESIAN_POINT('Ctrl Pts',(-70.9628490458779,11.039475878929,0.));
#85955=CARTESIAN_POINT('Ctrl Pts',(-70.9628490458779,11.039475878929,12.));
#85956=CARTESIAN_POINT('Ctrl Pts',(-70.9861303424989,11.0350434498408,0.));
#85957=CARTESIAN_POINT('Ctrl Pts',(-70.9861303424989,11.0350434498408,12.));
#85958=CARTESIAN_POINT('Ctrl Pts',(-71.0094495171295,11.0305800695457,0.));
#85959=CARTESIAN_POINT('Ctrl Pts',(-71.0094495171295,11.0305800695457,12.));
#85960=CARTESIAN_POINT('Ctrl Pts',(-71.0328064373849,11.0260856997415,0.));
#85961=CARTESIAN_POINT('Ctrl Pts',(-71.0328064373849,11.0260856997415,12.));
#85962=CARTESIAN_POINT('Ctrl Pts',(-71.0562009714125,11.0215603023855,0.));
#85963=CARTESIAN_POINT('Ctrl Pts',(-71.0562009714125,11.0215603023855,12.));
#85964=CARTESIAN_POINT('Ctrl Pts',(-71.0796329878896,11.0170038396913,0.));
#85965=CARTESIAN_POINT('Ctrl Pts',(-71.0796329878896,11.0170038396913,12.));
#85966=CARTESIAN_POINT('Ctrl Pts',(-71.1031023560243,11.0124162741224,0.));
#85967=CARTESIAN_POINT('Ctrl Pts',(-71.1031023560243,11.0124162741224,12.));
#85968=CARTESIAN_POINT('Ctrl Pts',(-71.1266089455517,11.0077975683895,0.));
#85969=CARTESIAN_POINT('Ctrl Pts',(-71.1266089455517,11.0077975683895,12.));
#85970=CARTESIAN_POINT('Ctrl Pts',(-71.1501526267288,11.0031476854503,0.));
#85971=CARTESIAN_POINT('Ctrl Pts',(-71.1501526267288,11.0031476854503,12.));
#85972=CARTESIAN_POINT('Ctrl Pts',(-71.1737332703248,10.9984665885127,0.));
#85973=CARTESIAN_POINT('Ctrl Pts',(-71.1737332703248,10.9984665885127,12.));
#85974=CARTESIAN_POINT('Ctrl Pts',(-71.1973507476188,10.993754241032,0.));
#85975=CARTESIAN_POINT('Ctrl Pts',(-71.1973507476188,10.993754241032,12.));
#85976=CARTESIAN_POINT('Ctrl Pts',(-71.221004930401,10.9890106067039,0.));
#85977=CARTESIAN_POINT('Ctrl Pts',(-71.221004930401,10.9890106067039,12.));
#85978=CARTESIAN_POINT('Ctrl Pts',(-71.2446956909685,10.9842356494627,0.));
#85979=CARTESIAN_POINT('Ctrl Pts',(-71.2446956909685,10.9842356494627,12.));
#85980=CARTESIAN_POINT('Ctrl Pts',(-71.2684229021209,10.9794293334806,0.));
#85981=CARTESIAN_POINT('Ctrl Pts',(-71.2684229021209,10.9794293334806,12.));
#85982=CARTESIAN_POINT('Ctrl Pts',(-71.2921864371499,10.9745916231711,0.));
#85983=CARTESIAN_POINT('Ctrl Pts',(-71.2921864371499,10.9745916231711,12.));
#85984=CARTESIAN_POINT('Ctrl Pts',(-71.3159861698368,10.9697224831863,0.));
#85985=CARTESIAN_POINT('Ctrl Pts',(-71.3159861698368,10.9697224831863,12.));
#85986=CARTESIAN_POINT('Ctrl Pts',(-71.3398219744547,10.96482187841,0.));
#85987=CARTESIAN_POINT('Ctrl Pts',(-71.3398219744547,10.96482187841,12.));
#85988=CARTESIAN_POINT('Ctrl Pts',(-71.3636937257651,10.9598897739565,0.));
#85989=CARTESIAN_POINT('Ctrl Pts',(-71.3636937257651,10.9598897739565,12.));
#85990=CARTESIAN_POINT('Ctrl Pts',(-71.3876012990135,10.954926135169,0.));
#85991=CARTESIAN_POINT('Ctrl Pts',(-71.3876012990135,10.954926135169,12.));
#85992=CARTESIAN_POINT('Ctrl Pts',(-71.411544569919,10.9499309276236,0.));
#85993=CARTESIAN_POINT('Ctrl Pts',(-71.411544569919,10.9499309276236,12.));
#85994=CARTESIAN_POINT('Ctrl Pts',(-71.4355234146718,10.9449041171269,0.));
#85995=CARTESIAN_POINT('Ctrl Pts',(-71.4355234146718,10.9449041171269,12.));
#85996=CARTESIAN_POINT('Ctrl Pts',(-71.4595377099352,10.9398456697095,0.));
#85997=CARTESIAN_POINT('Ctrl Pts',(-71.4595377099352,10.9398456697095,12.));
#85998=CARTESIAN_POINT('Ctrl Pts',(-71.4835873328425,10.9347555516236,0.));
#85999=CARTESIAN_POINT('Ctrl Pts',(-71.4835873328425,10.9347555516236,12.));
#86000=CARTESIAN_POINT('Ctrl Pts',(-71.5076721609936,10.9296337293425,0.));
#86001=CARTESIAN_POINT('Ctrl Pts',(-71.5076721609936,10.9296337293425,12.));
#86002=CARTESIAN_POINT('Ctrl Pts',(-71.5317920724453,10.9244801695642,0.));
#86003=CARTESIAN_POINT('Ctrl Pts',(-71.5317920724453,10.9244801695642,12.));
#86004=CARTESIAN_POINT('Ctrl Pts',(-71.5559469457082,10.91929483921,0.));
#86005=CARTESIAN_POINT('Ctrl Pts',(-71.5559469457082,10.91929483921,12.));
#86006=CARTESIAN_POINT('Ctrl Pts',(-71.5801366597479,10.9140777054169,0.));
#86007=CARTESIAN_POINT('Ctrl Pts',(-71.5801366597479,10.9140777054169,12.));
#86008=CARTESIAN_POINT('Ctrl Pts',(-71.604361093983,10.9088287355364,0.));
#86009=CARTESIAN_POINT('Ctrl Pts',(-71.604361093983,10.9088287355364,12.));
#86010=CARTESIAN_POINT('Ctrl Pts',(-71.6286201282815,10.9035478971329,0.));
#86011=CARTESIAN_POINT('Ctrl Pts',(-71.6286201282815,10.9035478971329,12.));
#86012=CARTESIAN_POINT('Ctrl Pts',(-71.6529136429515,10.8982351579873,0.));
#86013=CARTESIAN_POINT('Ctrl Pts',(-71.6529136429515,10.8982351579873,12.));
#86014=CARTESIAN_POINT('Ctrl Pts',(-71.6772415187382,10.8928904860967,0.));
#86015=CARTESIAN_POINT('Ctrl Pts',(-71.6772415187382,10.8928904860967,12.));
#86016=CARTESIAN_POINT('Ctrl Pts',(-71.7016036368254,10.8875138496674,0.));
#86017=CARTESIAN_POINT('Ctrl Pts',(-71.7016036368254,10.8875138496674,12.));
#86018=CARTESIAN_POINT('Ctrl Pts',(-71.7259998788337,10.8821052171122,0.));
#86019=CARTESIAN_POINT('Ctrl Pts',(-71.7259998788337,10.8821052171122,12.));
#86020=CARTESIAN_POINT('Ctrl Pts',(-71.7504301268177,10.8766645570497,0.));
#86021=CARTESIAN_POINT('Ctrl Pts',(-71.7504301268177,10.8766645570497,12.));
#86022=CARTESIAN_POINT('Ctrl Pts',(-71.7748942632578,10.8711918383071,0.));
#86023=CARTESIAN_POINT('Ctrl Pts',(-71.7748942632578,10.8711918383071,12.));
#86024=CARTESIAN_POINT('Ctrl Pts',(-71.7993921710546,10.8656870299218,0.));
#86025=CARTESIAN_POINT('Ctrl Pts',(-71.7993921710546,10.8656870299218,12.));
#86026=CARTESIAN_POINT('Ctrl Pts',(-71.8239237335317,10.860150101133,0.));
#86027=CARTESIAN_POINT('Ctrl Pts',(-71.8239237335317,10.860150101133,12.));
#86028=CARTESIAN_POINT('Ctrl Pts',(-71.8484888344335,10.8545810213799,0.));
#86029=CARTESIAN_POINT('Ctrl Pts',(-71.8484888344335,10.8545810213799,12.));
#86030=CARTESIAN_POINT('Ctrl Pts',(-71.8730873579226,10.8489797602998,0.));
#86031=CARTESIAN_POINT('Ctrl Pts',(-71.8730873579226,10.8489797602998,12.));
#86032=CARTESIAN_POINT('Ctrl Pts',(-71.8977191885726,10.8433462877312,0.));
#86033=CARTESIAN_POINT('Ctrl Pts',(-71.8977191885726,10.8433462877312,12.));
#86034=CARTESIAN_POINT('Ctrl Pts',(-71.9223842113622,10.8376805737159,0.));
#86035=CARTESIAN_POINT('Ctrl Pts',(-71.9223842113622,10.8376805737159,12.));
#86036=CARTESIAN_POINT('Ctrl Pts',(-71.9470823116777,10.8319825884917,0.));
#86037=CARTESIAN_POINT('Ctrl Pts',(-71.9470823116777,10.8319825884917,12.));
#86038=CARTESIAN_POINT('Ctrl Pts',(-71.971813375312,10.8262523024897,0.));
#86039=CARTESIAN_POINT('Ctrl Pts',(-71.971813375312,10.8262523024897,12.));
#86040=CARTESIAN_POINT('Ctrl Pts',(-71.9965772884619,10.8204896863328,0.));
#86041=CARTESIAN_POINT('Ctrl Pts',(-71.9965772884619,10.8204896863328,12.));
#86042=CARTESIAN_POINT('Ctrl Pts',(-72.0213739377231,10.8146947108377,0.));
#86043=CARTESIAN_POINT('Ctrl Pts',(-72.0213739377231,10.8146947108377,12.));
#86044=CARTESIAN_POINT('Ctrl Pts',(-72.0462032100828,10.8088673470187,0.));
#86045=CARTESIAN_POINT('Ctrl Pts',(-72.0462032100828,10.8088673470187,12.));
#86046=CARTESIAN_POINT('Ctrl Pts',(-72.0710649929214,10.8030075660812,0.));
#86047=CARTESIAN_POINT('Ctrl Pts',(-72.0710649929214,10.8030075660812,12.));
#86048=CARTESIAN_POINT('Ctrl Pts',(-72.095959174012,10.7971153394168,0.));
#86049=CARTESIAN_POINT('Ctrl Pts',(-72.095959174012,10.7971153394168,12.));
#86050=CARTESIAN_POINT('Ctrl Pts',(-72.1208856415171,10.7911906386027,0.));
#86051=CARTESIAN_POINT('Ctrl Pts',(-72.1208856415171,10.7911906386027,12.));
#86052=CARTESIAN_POINT('Ctrl Pts',(-72.145844283983,10.7852334354015,0.));
#86053=CARTESIAN_POINT('Ctrl Pts',(-72.145844283983,10.7852334354015,12.));
#86054=CARTESIAN_POINT('Ctrl Pts',(-72.17083499033,10.779243701766,0.));
#86055=CARTESIAN_POINT('Ctrl Pts',(-72.17083499033,10.779243701766,12.));
#86056=CARTESIAN_POINT('Ctrl Pts',(-72.1958576498556,10.7732214098343,0.));
#86057=CARTESIAN_POINT('Ctrl Pts',(-72.1958576498556,10.7732214098343,12.));
#86058=CARTESIAN_POINT('Ctrl Pts',(-72.2209121522367,10.7671665319254,0.));
#86059=CARTESIAN_POINT('Ctrl Pts',(-72.2209121522367,10.7671665319254,12.));
#86060=CARTESIAN_POINT('Ctrl Pts',(-72.2459983875297,10.7610790405385,0.));
#86061=CARTESIAN_POINT('Ctrl Pts',(-72.2459983875297,10.7610790405385,12.));
#86062=CARTESIAN_POINT('Ctrl Pts',(-72.2711162461679,10.7549589083536,0.));
#86063=CARTESIAN_POINT('Ctrl Pts',(-72.2711162461679,10.7549589083536,12.));
#86064=CARTESIAN_POINT('Ctrl Pts',(-72.296265618955,10.7488061082368,0.));
#86065=CARTESIAN_POINT('Ctrl Pts',(-72.296265618955,10.7488061082368,12.));
#86066=CARTESIAN_POINT('Ctrl Pts',(-72.3214463970634,10.7426206132375,0.));
#86067=CARTESIAN_POINT('Ctrl Pts',(-72.3214463970634,10.7426206132375,12.));
#86068=CARTESIAN_POINT('Ctrl Pts',(-72.3466584720311,10.73640239658,0.));
#86069=CARTESIAN_POINT('Ctrl Pts',(-72.3466584720311,10.73640239658,12.));
#86070=CARTESIAN_POINT('Ctrl Pts',(-72.3719017357568,10.7301514316607,0.));
#86071=CARTESIAN_POINT('Ctrl Pts',(-72.3719017357568,10.7301514316607,12.));
#86072=CARTESIAN_POINT('Ctrl Pts',(-72.3971760804935,10.7238676920469,0.));
#86073=CARTESIAN_POINT('Ctrl Pts',(-72.3971760804935,10.7238676920469,12.));
#86074=CARTESIAN_POINT('Ctrl Pts',(-72.4224813988355,10.7175511514789,0.));
#86075=CARTESIAN_POINT('Ctrl Pts',(-72.4224813988355,10.7175511514789,12.));
#86076=CARTESIAN_POINT('Ctrl Pts',(-72.4478175837168,10.7112017838707,0.));
#86077=CARTESIAN_POINT('Ctrl Pts',(-72.4478175837168,10.7112017838707,12.));
#86078=CARTESIAN_POINT('Ctrl Pts',(-72.4731845284238,10.7048195633062,0.));
#86079=CARTESIAN_POINT('Ctrl Pts',(-72.4731845284238,10.7048195633062,12.));
#86080=CARTESIAN_POINT('Ctrl Pts',(-72.4985821266031,10.6984044640399,0.));
#86081=CARTESIAN_POINT('Ctrl Pts',(-72.4985821266031,10.6984044640399,12.));
#86082=CARTESIAN_POINT('Ctrl Pts',(-72.5240102722662,10.6919564604991,0.));
#86083=CARTESIAN_POINT('Ctrl Pts',(-72.5240102722662,10.6919564604991,12.));
#86084=CARTESIAN_POINT('Ctrl Pts',(-72.5494688597951,10.6854755272904,0.));
#86085=CARTESIAN_POINT('Ctrl Pts',(-72.5494688597951,10.6854755272904,12.));
#86086=CARTESIAN_POINT('Ctrl Pts',(-72.57495778394,10.6789616392041,0.));
#86087=CARTESIAN_POINT('Ctrl Pts',(-72.57495778394,10.6789616392041,12.));
#86088=CARTESIAN_POINT('Ctrl Pts',(-72.6004769398004,10.6724147711994,0.));
#86089=CARTESIAN_POINT('Ctrl Pts',(-72.6004769398004,10.6724147711994,12.));
#86090=CARTESIAN_POINT('Ctrl Pts',(-72.6260262228055,10.6658348983944,0.));
#86091=CARTESIAN_POINT('Ctrl Pts',(-72.6260262228055,10.6658348983944,12.));
#86092=CARTESIAN_POINT('Ctrl Pts',(-72.6516055286908,10.6592219960581,0.));
#86093=CARTESIAN_POINT('Ctrl Pts',(-72.6516055286908,10.6592219960581,12.));
#86094=CARTESIAN_POINT('Ctrl Pts',(-72.6772147534762,10.6525760396056,0.));
#86095=CARTESIAN_POINT('Ctrl Pts',(-72.6772147534762,10.6525760396056,12.));
#86096=CARTESIAN_POINT('Ctrl Pts',(-72.7028537934332,10.6458970045948,0.));
#86097=CARTESIAN_POINT('Ctrl Pts',(-72.7028537934332,10.6458970045948,12.));
#86098=CARTESIAN_POINT('Ctrl Pts',(-72.7285225451309,10.6391848667354,0.));
#86099=CARTESIAN_POINT('Ctrl Pts',(-72.7285225451309,10.6391848667354,12.));
#86100=CARTESIAN_POINT('Ctrl Pts',(-72.7542209054823,10.6324396019,0.));
#86101=CARTESIAN_POINT('Ctrl Pts',(-72.7542209054823,10.6324396019,12.));
#86102=CARTESIAN_POINT('Ctrl Pts',(-72.7799487717914,10.6256611861395,0.));
#86103=CARTESIAN_POINT('Ctrl Pts',(-72.7799487717914,10.6256611861395,12.));
#86104=CARTESIAN_POINT('Ctrl Pts',(-72.8057060417882,10.6188495956973,0.));
#86105=CARTESIAN_POINT('Ctrl Pts',(-72.8057060417882,10.6188495956973,12.));
#86106=CARTESIAN_POINT('Ctrl Pts',(-72.8314926136872,10.6120048070367,0.));
#86107=CARTESIAN_POINT('Ctrl Pts',(-72.8314926136872,10.6120048070367,12.));
#86108=CARTESIAN_POINT('Ctrl Pts',(-72.8573083861328,10.6051267968202,0.));
#86109=CARTESIAN_POINT('Ctrl Pts',(-72.8573083861328,10.6051267968202,12.));
#86110=CARTESIAN_POINT('Ctrl Pts',(-72.8831532580839,10.5982155418625,0.));
#86111=CARTESIAN_POINT('Ctrl Pts',(-72.8831532580839,10.5982155418625,12.));
#86112=CARTESIAN_POINT('Ctrl Pts',(-72.9090271287081,10.5912710190928,0.));
#86113=CARTESIAN_POINT('Ctrl Pts',(-72.9090271287081,10.5912710190928,12.));
#86114=CARTESIAN_POINT('Ctrl Pts',(-72.9349298972823,10.5842932055209,0.));
#86115=CARTESIAN_POINT('Ctrl Pts',(-72.9349298972823,10.5842932055209,12.));
#86116=CARTESIAN_POINT('Ctrl Pts',(-72.9608614630538,10.5772820781959,0.));
#86117=CARTESIAN_POINT('Ctrl Pts',(-72.9608614630538,10.5772820781959,12.));
#86118=CARTESIAN_POINT('Ctrl Pts',(-72.9868217252293,10.5702376142052,0.));
#86119=CARTESIAN_POINT('Ctrl Pts',(-72.9868217252293,10.5702376142052,12.));
#86120=CARTESIAN_POINT('Ctrl Pts',(-73.0128105832635,10.5631597907653,0.));
#86121=CARTESIAN_POINT('Ctrl Pts',(-73.0128105832635,10.5631597907653,12.));
#86122=CARTESIAN_POINT('Ctrl Pts',(-73.0388279370845,10.5560485852976,0.));
#86123=CARTESIAN_POINT('Ctrl Pts',(-73.0388279370845,10.5560485852976,12.));
#86124=CARTESIAN_POINT('Ctrl Pts',(-73.0648736873435,10.5489039755138,0.));
#86125=CARTESIAN_POINT('Ctrl Pts',(-73.0648736873435,10.5489039755138,12.));
#86126=CARTESIAN_POINT('Ctrl Pts',(-73.090947735646,10.5417259395001,0.));
#86127=CARTESIAN_POINT('Ctrl Pts',(-73.090947735646,10.5417259395001,12.));
#86128=CARTESIAN_POINT('Ctrl Pts',(-73.1170499848012,10.5345144558097,0.));
#86129=CARTESIAN_POINT('Ctrl Pts',(-73.1170499848012,10.5345144558097,12.));
#86130=CARTESIAN_POINT('Ctrl Pts',(-73.1431803382677,10.5272695032649,0.));
#86131=CARTESIAN_POINT('Ctrl Pts',(-73.1431803382677,10.5272695032649,12.));
#86132=CARTESIAN_POINT('Ctrl Pts',(-73.169338699611,10.5199910607652,0.));
#86133=CARTESIAN_POINT('Ctrl Pts',(-73.169338699611,10.5199910607652,12.));
#86134=CARTESIAN_POINT('Ctrl Pts',(-73.1955249719037,10.5126791070804,0.));
#86135=CARTESIAN_POINT('Ctrl Pts',(-73.1955249719037,10.5126791070804,12.));
#86136=CARTESIAN_POINT('Ctrl Pts',(-73.2217390572578,10.505333620691,0.));
#86137=CARTESIAN_POINT('Ctrl Pts',(-73.2217390572578,10.505333620691,12.));
#86138=CARTESIAN_POINT('Ctrl Pts',(-73.247980856023,10.4979545795197,0.));
#86139=CARTESIAN_POINT('Ctrl Pts',(-73.247980856023,10.4979545795197,12.));
#86140=CARTESIAN_POINT('Ctrl Pts',(-73.2742502674361,10.4905419611529,0.));
#86141=CARTESIAN_POINT('Ctrl Pts',(-73.2742502674361,10.4905419611529,12.));
#86142=CARTESIAN_POINT('Ctrl Pts',(-73.3005471910639,10.4830957433311,0.));
#86143=CARTESIAN_POINT('Ctrl Pts',(-73.3005471910639,10.4830957433311,12.));
#86144=CARTESIAN_POINT('Ctrl Pts',(-73.3268715280609,10.475615904381,0.));
#86145=CARTESIAN_POINT('Ctrl Pts',(-73.3268715280609,10.475615904381,12.));
#86146=CARTESIAN_POINT('Ctrl Pts',(-73.353223182365,10.4681024236288,0.));
#86147=CARTESIAN_POINT('Ctrl Pts',(-73.353223182365,10.4681024236288,12.));
#86148=CARTESIAN_POINT('Ctrl Pts',(-73.3796020622436,10.4605552819391,0.));
#86149=CARTESIAN_POINT('Ctrl Pts',(-73.3796020622436,10.4605552819391,12.));
#86150=CARTESIAN_POINT('Ctrl Pts',(-73.4060080806577,10.4529744618439,0.));
#86151=CARTESIAN_POINT('Ctrl Pts',(-73.4060080806577,10.4529744618439,12.));
#86152=CARTESIAN_POINT('Ctrl Pts',(-73.432441151843,10.4453599463535,0.));
#86153=CARTESIAN_POINT('Ctrl Pts',(-73.432441151843,10.4453599463535,12.));
#86154=CARTESIAN_POINT('Ctrl Pts',(-73.45890118861,10.4377117180213,0.));
#86155=CARTESIAN_POINT('Ctrl Pts',(-73.45890118861,10.4377117180213,12.));
#86156=CARTESIAN_POINT('Ctrl Pts',(-73.4853880992228,10.4300297578648,0.));
#86157=CARTESIAN_POINT('Ctrl Pts',(-73.4853880992228,10.4300297578648,12.));
#86158=CARTESIAN_POINT('Ctrl Pts',(-73.5119017847664,10.4223140444615,0.));
#86159=CARTESIAN_POINT('Ctrl Pts',(-73.5119017847664,10.4223140444615,12.));
#86160=CARTESIAN_POINT('Ctrl Pts',(-73.5384421354746,10.4145645526832,0.));
#86161=CARTESIAN_POINT('Ctrl Pts',(-73.5384421354746,10.4145645526832,12.));
#86162=CARTESIAN_POINT('Ctrl Pts',(-73.5650090360113,10.4067812555539,0.));
#86163=CARTESIAN_POINT('Ctrl Pts',(-73.5650090360113,10.4067812555539,12.));
#86164=CARTESIAN_POINT('Ctrl Pts',(-73.5916023719976,10.3989641265313,0.));
#86165=CARTESIAN_POINT('Ctrl Pts',(-73.5916023719976,10.3989641265313,12.));
#86166=CARTESIAN_POINT('Ctrl Pts',(-73.6182220363295,10.3911131417478,0.));
#86167=CARTESIAN_POINT('Ctrl Pts',(-73.6182220363295,10.3911131417478,12.));
#86168=CARTESIAN_POINT('Ctrl Pts',(-73.6448679350605,10.3832282820362,0.));
#86169=CARTESIAN_POINT('Ctrl Pts',(-73.6448679350605,10.3832282820362,12.));
#86170=CARTESIAN_POINT('Ctrl Pts',(-73.6715399947459,10.3753095356302,0.));
#86171=CARTESIAN_POINT('Ctrl Pts',(-73.6715399947459,10.3753095356302,12.));
#86172=CARTESIAN_POINT('Ctrl Pts',(-73.6982381644571,10.3673568984515,0.));
#86173=CARTESIAN_POINT('Ctrl Pts',(-73.6982381644571,10.3673568984515,12.));
#86174=CARTESIAN_POINT('Ctrl Pts',(-73.7249624108432,10.3593703712542,0.));
#86175=CARTESIAN_POINT('Ctrl Pts',(-73.7249624108432,10.3593703712542,12.));
#86176=CARTESIAN_POINT('Ctrl Pts',(-73.7463626541235,10.3529540403026,0.));
#86177=CARTESIAN_POINT('Ctrl Pts',(-73.7463626541235,10.3529540403026,12.));
#86178=CARTESIAN_POINT('Ctrl Pts',(-73.7624245587416,10.3481265449303,0.));
#86179=CARTESIAN_POINT('Ctrl Pts',(-73.7624245587416,10.3481265449303,12.));
#86180=CARTESIAN_POINT('Ctrl Pts',(-73.7731377047922,10.3449014384439,0.));
#86181=CARTESIAN_POINT('Ctrl Pts',(-73.7731377047922,10.3449014384439,12.));
#86182=CARTESIAN_POINT('Ctrl Pts',(-73.778495580227,10.343287191141,0.));
#86183=CARTESIAN_POINT('Ctrl Pts',(-73.778495580227,10.343287191141,12.));
#86184=CARTESIAN_POINT('',(-69.079679653846,11.3136138754166,0.));
#86185=CARTESIAN_POINT('Ctrl Pts',(-69.079679653846,11.3136138754166,0.));
#86186=CARTESIAN_POINT('Ctrl Pts',(-69.0835449954396,11.3132375200165,0.));
#86187=CARTESIAN_POINT('Ctrl Pts',(-69.0912808656811,11.3124821678798,0.));
#86188=CARTESIAN_POINT('Ctrl Pts',(-69.1029002322118,11.3113412156662,0.));
#86189=CARTESIAN_POINT('Ctrl Pts',(-69.118423844466,11.3098040973713,0.));
#86190=CARTESIAN_POINT('Ctrl Pts',(-69.1378802251711,11.3078562764385,0.));
#86191=CARTESIAN_POINT('Ctrl Pts',(-69.1573884361,11.3058820128308,0.));
#86192=CARTESIAN_POINT('Ctrl Pts',(-69.1769483991721,11.3038812726293,0.));
#86193=CARTESIAN_POINT('Ctrl Pts',(-69.1965599718914,11.3018540025638,0.));
#86194=CARTESIAN_POINT('Ctrl Pts',(-69.2162229488531,11.2998001310964,0.));
#86195=CARTESIAN_POINT('Ctrl Pts',(-69.2359370894907,11.2977195764853,0.));
#86196=CARTESIAN_POINT('Ctrl Pts',(-69.255702139335,11.2956122531375,0.));
#86197=CARTESIAN_POINT('Ctrl Pts',(-69.2755178531479,11.2934780784351,0.));
#86198=CARTESIAN_POINT('Ctrl Pts',(-69.295384019272,11.2913169799628,0.));
#86199=CARTESIAN_POINT('Ctrl Pts',(-69.3153004517783,11.2891288931517,0.));
#86200=CARTESIAN_POINT('Ctrl Pts',(-69.3352669789587,11.2869137578459,0.));
#86201=CARTESIAN_POINT('Ctrl Pts',(-69.3552834337784,11.2846715154524,0.));
#86202=CARTESIAN_POINT('Ctrl Pts',(-69.3753496420039,11.2824021054045,0.));
#86203=CARTESIAN_POINT('Ctrl Pts',(-69.3954654162281,11.2801054633816,0.));
#86204=CARTESIAN_POINT('Ctrl Pts',(-69.4156305620593,11.2777815231469,0.));
#86205=CARTESIAN_POINT('Ctrl Pts',(-69.4358448819967,11.2754302177021,0.));
#86206=CARTESIAN_POINT('Ctrl Pts',(-69.456108179879,11.2730514806139,0.));
#86207=CARTESIAN_POINT('Ctrl Pts',(-69.4764202659397,11.270645247528,0.));
#86208=CARTESIAN_POINT('Ctrl Pts',(-69.4967809565929,11.2682114561008,0.));
#86209=CARTESIAN_POINT('Ctrl Pts',(-69.5171900720158,11.2657500452716,0.));
#86210=CARTESIAN_POINT('Ctrl Pts',(-69.5376474344771,11.263260954763,0.));
#86211=CARTESIAN_POINT('Ctrl Pts',(-69.5581528662877,11.2607441244703,0.));
#86212=CARTESIAN_POINT('Ctrl Pts',(-69.5787061880857,11.2581994939541,0.));
#86213=CARTESIAN_POINT('Ctrl Pts',(-69.599307219739,11.2556270027016,0.));
#86214=CARTESIAN_POINT('Ctrl Pts',(-69.6199557811245,11.2530265903558,0.));
#86215=CARTESIAN_POINT('Ctrl Pts',(-69.6406516928891,11.2503981969412,0.));
#86216=CARTESIAN_POINT('Ctrl Pts',(-69.6613947773534,11.2477417631386,0.));
#86217=CARTESIAN_POINT('Ctrl Pts',(-69.6821848588457,11.2450572303841,0.));
#86218=CARTESIAN_POINT('Ctrl Pts',(-69.7030217632164,11.2423445407167,0.));
#86219=CARTESIAN_POINT('Ctrl Pts',(-69.7239053175356,11.239603636686,0.));
#86220=CARTESIAN_POINT('Ctrl Pts',(-69.7448353497408,11.2368344612473,0.));
#86221=CARTESIAN_POINT('Ctrl Pts',(-69.7658116882324,11.2340369576456,0.));
#86222=CARTESIAN_POINT('Ctrl Pts',(-69.7868341618954,11.2312110694188,0.));
#86223=CARTESIAN_POINT('Ctrl Pts',(-69.8079026002768,11.2283567404437,0.));
#86224=CARTESIAN_POINT('Ctrl Pts',(-69.8290168337076,11.2254739149721,0.));
#86225=CARTESIAN_POINT('Ctrl Pts',(-69.8501766934428,11.2225625376737,0.));
#86226=CARTESIAN_POINT('Ctrl Pts',(-69.871382011789,11.219622553679,0.));
#86227=CARTESIAN_POINT('Ctrl Pts',(-69.8926326220385,11.2166539085523,0.));
#86228=CARTESIAN_POINT('Ctrl Pts',(-69.9139283584021,11.2136565482678,0.));
#86229=CARTESIAN_POINT('Ctrl Pts',(-69.9352690559405,11.2106304191883,0.));
#86230=CARTESIAN_POINT('Ctrl Pts',(-69.9566545504837,11.2075754680449,0.));
#86231=CARTESIAN_POINT('Ctrl Pts',(-69.97808467858,11.2044916419244,0.));
#86232=CARTESIAN_POINT('Ctrl Pts',(-69.9995592775343,11.2013788882714,0.));
#86233=CARTESIAN_POINT('Ctrl Pts',(-70.0210781854243,11.1982371548919,0.));
#86234=CARTESIAN_POINT('Ctrl Pts',(-70.0426412411185,11.1950663899577,0.));
#86235=CARTESIAN_POINT('Ctrl Pts',(-70.0642482842928,11.1918665420167,0.));
#86236=CARTESIAN_POINT('Ctrl Pts',(-70.0858991554283,11.1886375599914,0.));
#86237=CARTESIAN_POINT('Ctrl Pts',(-70.1075936957968,11.185379393167,0.));
#86238=CARTESIAN_POINT('Ctrl Pts',(-70.1293317474432,11.1820919911846,0.));
#86239=CARTESIAN_POINT('Ctrl Pts',(-70.1511131531674,11.1787753040363,0.));
#86240=CARTESIAN_POINT('Ctrl Pts',(-70.1729377564956,11.1754292820631,0.));
#86241=CARTESIAN_POINT('Ctrl Pts',(-70.1948054016817,11.1720538759499,0.));
#86242=CARTESIAN_POINT('Ctrl Pts',(-70.2167159337095,11.168649036721,0.));
#86243=CARTESIAN_POINT('Ctrl Pts',(-70.2386691982902,11.1652147157383,0.));
#86244=CARTESIAN_POINT('Ctrl Pts',(-70.2606650418589,11.1617508647017,0.));
#86245=CARTESIAN_POINT('Ctrl Pts',(-70.2827033115662,11.1582574356522,0.));
#86246=CARTESIAN_POINT('Ctrl Pts',(-70.3047838552757,11.1547343809647,0.));
#86247=CARTESIAN_POINT('Ctrl Pts',(-70.3269065215591,11.1511816533422,0.));
#86248=CARTESIAN_POINT('Ctrl Pts',(-70.3490711596882,11.1475992058124,0.));
#86249=CARTESIAN_POINT('Ctrl Pts',(-70.3712776196216,11.1439869917269,0.));
#86250=CARTESIAN_POINT('Ctrl Pts',(-70.3935257519945,11.1403449647622,0.));
#86251=CARTESIAN_POINT('Ctrl Pts',(-70.415815408119,11.1366730789123,0.));
#86252=CARTESIAN_POINT('Ctrl Pts',(-70.438146439981,11.1329712884845,0.));
#86253=CARTESIAN_POINT('Ctrl Pts',(-70.4605187002356,11.1292395480975,0.));
#86254=CARTESIAN_POINT('Ctrl Pts',(-70.4829320421973,11.1254778126824,0.));
#86255=CARTESIAN_POINT('Ctrl Pts',(-70.5053863198306,11.121686037483,0.));
#86256=CARTESIAN_POINT('Ctrl Pts',(-70.5278813877519,11.117864178048,0.));
#86257=CARTESIAN_POINT('Ctrl Pts',(-70.5504171012247,11.1140121902274,0.));
#86258=CARTESIAN_POINT('Ctrl Pts',(-70.5729933161538,11.1101300301701,0.));
#86259=CARTESIAN_POINT('Ctrl Pts',(-70.5956098890744,11.1062176543258,0.));
#86260=CARTESIAN_POINT('Ctrl Pts',(-70.6182666771441,11.102275019444,0.));
#86261=CARTESIAN_POINT('Ctrl Pts',(-70.6409635381446,11.0983020825662,0.));
#86262=CARTESIAN_POINT('Ctrl Pts',(-70.6637003304768,11.0942988010231,0.));
#86263=CARTESIAN_POINT('Ctrl Pts',(-70.686476913156,11.0902651324326,0.));
#86264=CARTESIAN_POINT('Ctrl Pts',(-70.7092931457996,11.0862010347022,0.));
#86265=CARTESIAN_POINT('Ctrl Pts',(-70.7321488886229,11.0821064660276,0.));
#86266=CARTESIAN_POINT('Ctrl Pts',(-70.7550440024422,11.0779813848851,0.));
#86267=CARTESIAN_POINT('Ctrl Pts',(-70.7779783486689,11.0738257500292,0.));
#86268=CARTESIAN_POINT('Ctrl Pts',(-70.8009517893042,11.0696395204908,0.));
#86269=CARTESIAN_POINT('Ctrl Pts',(-70.8239641869266,11.0654226555799,0.));
#86270=CARTESIAN_POINT('Ctrl Pts',(-70.847015404688,11.0611751148831,0.));
#86271=CARTESIAN_POINT('Ctrl Pts',(-70.8701053063158,11.0568968582566,0.));
#86272=CARTESIAN_POINT('Ctrl Pts',(-70.8932337561079,11.0525878458242,0.));
#86273=CARTESIAN_POINT('Ctrl Pts',(-70.9164006189283,11.0482480379752,0.));
#86274=CARTESIAN_POINT('Ctrl Pts',(-70.9396057601953,11.0438773953686,0.));
#86275=CARTESIAN_POINT('Ctrl Pts',(-70.9628490458779,11.039475878929,0.));
#86276=CARTESIAN_POINT('Ctrl Pts',(-70.9861303424989,11.0350434498408,0.));
#86277=CARTESIAN_POINT('Ctrl Pts',(-71.0094495171295,11.0305800695457,0.));
#86278=CARTESIAN_POINT('Ctrl Pts',(-71.0328064373849,11.0260856997415,0.));
#86279=CARTESIAN_POINT('Ctrl Pts',(-71.0562009714125,11.0215603023855,0.));
#86280=CARTESIAN_POINT('Ctrl Pts',(-71.0796329878896,11.0170038396913,0.));
#86281=CARTESIAN_POINT('Ctrl Pts',(-71.1031023560243,11.0124162741224,0.));
#86282=CARTESIAN_POINT('Ctrl Pts',(-71.1266089455517,11.0077975683895,0.));
#86283=CARTESIAN_POINT('Ctrl Pts',(-71.1501526267288,11.0031476854503,0.));
#86284=CARTESIAN_POINT('Ctrl Pts',(-71.1737332703248,10.9984665885127,0.));
#86285=CARTESIAN_POINT('Ctrl Pts',(-71.1973507476188,10.993754241032,0.));
#86286=CARTESIAN_POINT('Ctrl Pts',(-71.221004930401,10.9890106067039,0.));
#86287=CARTESIAN_POINT('Ctrl Pts',(-71.2446956909685,10.9842356494627,0.));
#86288=CARTESIAN_POINT('Ctrl Pts',(-71.2684229021209,10.9794293334806,0.));
#86289=CARTESIAN_POINT('Ctrl Pts',(-71.2921864371499,10.9745916231711,0.));
#86290=CARTESIAN_POINT('Ctrl Pts',(-71.3159861698368,10.9697224831863,0.));
#86291=CARTESIAN_POINT('Ctrl Pts',(-71.3398219744547,10.96482187841,0.));
#86292=CARTESIAN_POINT('Ctrl Pts',(-71.3636937257651,10.9598897739565,0.));
#86293=CARTESIAN_POINT('Ctrl Pts',(-71.3876012990135,10.954926135169,0.));
#86294=CARTESIAN_POINT('Ctrl Pts',(-71.411544569919,10.9499309276236,0.));
#86295=CARTESIAN_POINT('Ctrl Pts',(-71.4355234146718,10.9449041171269,0.));
#86296=CARTESIAN_POINT('Ctrl Pts',(-71.4595377099352,10.9398456697095,0.));
#86297=CARTESIAN_POINT('Ctrl Pts',(-71.4835873328425,10.9347555516236,0.));
#86298=CARTESIAN_POINT('Ctrl Pts',(-71.5076721609936,10.9296337293425,0.));
#86299=CARTESIAN_POINT('Ctrl Pts',(-71.5317920724453,10.9244801695642,0.));
#86300=CARTESIAN_POINT('Ctrl Pts',(-71.5559469457082,10.91929483921,0.));
#86301=CARTESIAN_POINT('Ctrl Pts',(-71.5801366597479,10.9140777054169,0.));
#86302=CARTESIAN_POINT('Ctrl Pts',(-71.604361093983,10.9088287355364,0.));
#86303=CARTESIAN_POINT('Ctrl Pts',(-71.6286201282815,10.9035478971329,0.));
#86304=CARTESIAN_POINT('Ctrl Pts',(-71.6529136429515,10.8982351579873,0.));
#86305=CARTESIAN_POINT('Ctrl Pts',(-71.6772415187382,10.8928904860967,0.));
#86306=CARTESIAN_POINT('Ctrl Pts',(-71.7016036368254,10.8875138496674,0.));
#86307=CARTESIAN_POINT('Ctrl Pts',(-71.7259998788337,10.8821052171122,0.));
#86308=CARTESIAN_POINT('Ctrl Pts',(-71.7504301268177,10.8766645570497,0.));
#86309=CARTESIAN_POINT('Ctrl Pts',(-71.7748942632578,10.8711918383071,0.));
#86310=CARTESIAN_POINT('Ctrl Pts',(-71.7993921710546,10.8656870299218,0.));
#86311=CARTESIAN_POINT('Ctrl Pts',(-71.8239237335317,10.860150101133,0.));
#86312=CARTESIAN_POINT('Ctrl Pts',(-71.8484888344335,10.8545810213799,0.));
#86313=CARTESIAN_POINT('Ctrl Pts',(-71.8730873579226,10.8489797602998,0.));
#86314=CARTESIAN_POINT('Ctrl Pts',(-71.8977191885726,10.8433462877312,0.));
#86315=CARTESIAN_POINT('Ctrl Pts',(-71.9223842113622,10.8376805737159,0.));
#86316=CARTESIAN_POINT('Ctrl Pts',(-71.9470823116777,10.8319825884917,0.));
#86317=CARTESIAN_POINT('Ctrl Pts',(-71.971813375312,10.8262523024897,0.));
#86318=CARTESIAN_POINT('Ctrl Pts',(-71.9965772884619,10.8204896863328,0.));
#86319=CARTESIAN_POINT('Ctrl Pts',(-72.0213739377231,10.8146947108377,0.));
#86320=CARTESIAN_POINT('Ctrl Pts',(-72.0462032100828,10.8088673470187,0.));
#86321=CARTESIAN_POINT('Ctrl Pts',(-72.0710649929214,10.8030075660812,0.));
#86322=CARTESIAN_POINT('Ctrl Pts',(-72.095959174012,10.7971153394168,0.));
#86323=CARTESIAN_POINT('Ctrl Pts',(-72.1208856415171,10.7911906386027,0.));
#86324=CARTESIAN_POINT('Ctrl Pts',(-72.145844283983,10.7852334354015,0.));
#86325=CARTESIAN_POINT('Ctrl Pts',(-72.17083499033,10.779243701766,0.));
#86326=CARTESIAN_POINT('Ctrl Pts',(-72.1958576498556,10.7732214098343,0.));
#86327=CARTESIAN_POINT('Ctrl Pts',(-72.2209121522367,10.7671665319254,0.));
#86328=CARTESIAN_POINT('Ctrl Pts',(-72.2459983875297,10.7610790405385,0.));
#86329=CARTESIAN_POINT('Ctrl Pts',(-72.2711162461679,10.7549589083536,0.));
#86330=CARTESIAN_POINT('Ctrl Pts',(-72.296265618955,10.7488061082368,0.));
#86331=CARTESIAN_POINT('Ctrl Pts',(-72.3214463970634,10.7426206132375,0.));
#86332=CARTESIAN_POINT('Ctrl Pts',(-72.3466584720311,10.73640239658,0.));
#86333=CARTESIAN_POINT('Ctrl Pts',(-72.3719017357568,10.7301514316607,0.));
#86334=CARTESIAN_POINT('Ctrl Pts',(-72.3971760804935,10.7238676920469,0.));
#86335=CARTESIAN_POINT('Ctrl Pts',(-72.4224813988355,10.7175511514789,0.));
#86336=CARTESIAN_POINT('Ctrl Pts',(-72.4478175837168,10.7112017838707,0.));
#86337=CARTESIAN_POINT('Ctrl Pts',(-72.4731845284238,10.7048195633062,0.));
#86338=CARTESIAN_POINT('Ctrl Pts',(-72.4985821266031,10.6984044640399,0.));
#86339=CARTESIAN_POINT('Ctrl Pts',(-72.5240102722662,10.6919564604991,0.));
#86340=CARTESIAN_POINT('Ctrl Pts',(-72.5494688597951,10.6854755272904,0.));
#86341=CARTESIAN_POINT('Ctrl Pts',(-72.57495778394,10.6789616392041,0.));
#86342=CARTESIAN_POINT('Ctrl Pts',(-72.6004769398004,10.6724147711994,0.));
#86343=CARTESIAN_POINT('Ctrl Pts',(-72.6260262228055,10.6658348983944,0.));
#86344=CARTESIAN_POINT('Ctrl Pts',(-72.6516055286908,10.6592219960581,0.));
#86345=CARTESIAN_POINT('Ctrl Pts',(-72.6772147534762,10.6525760396056,0.));
#86346=CARTESIAN_POINT('Ctrl Pts',(-72.7028537934332,10.6458970045948,0.));
#86347=CARTESIAN_POINT('Ctrl Pts',(-72.7285225451309,10.6391848667354,0.));
#86348=CARTESIAN_POINT('Ctrl Pts',(-72.7542209054823,10.6324396019,0.));
#86349=CARTESIAN_POINT('Ctrl Pts',(-72.7799487717914,10.6256611861395,0.));
#86350=CARTESIAN_POINT('Ctrl Pts',(-72.8057060417882,10.6188495956973,0.));
#86351=CARTESIAN_POINT('Ctrl Pts',(-72.8314926136872,10.6120048070367,0.));
#86352=CARTESIAN_POINT('Ctrl Pts',(-72.8573083861328,10.6051267968202,0.));
#86353=CARTESIAN_POINT('Ctrl Pts',(-72.8831532580839,10.5982155418625,0.));
#86354=CARTESIAN_POINT('Ctrl Pts',(-72.9090271287081,10.5912710190928,0.));
#86355=CARTESIAN_POINT('Ctrl Pts',(-72.9349298972823,10.5842932055209,0.));
#86356=CARTESIAN_POINT('Ctrl Pts',(-72.9608614630538,10.5772820781959,0.));
#86357=CARTESIAN_POINT('Ctrl Pts',(-72.9868217252293,10.5702376142052,0.));
#86358=CARTESIAN_POINT('Ctrl Pts',(-73.0128105832635,10.5631597907653,0.));
#86359=CARTESIAN_POINT('Ctrl Pts',(-73.0388279370845,10.5560485852976,0.));
#86360=CARTESIAN_POINT('Ctrl Pts',(-73.0648736873435,10.5489039755138,0.));
#86361=CARTESIAN_POINT('Ctrl Pts',(-73.090947735646,10.5417259395001,0.));
#86362=CARTESIAN_POINT('Ctrl Pts',(-73.1170499848012,10.5345144558097,0.));
#86363=CARTESIAN_POINT('Ctrl Pts',(-73.1431803382677,10.5272695032649,0.));
#86364=CARTESIAN_POINT('Ctrl Pts',(-73.169338699611,10.5199910607652,0.));
#86365=CARTESIAN_POINT('Ctrl Pts',(-73.1955249719037,10.5126791070804,0.));
#86366=CARTESIAN_POINT('Ctrl Pts',(-73.2217390572578,10.505333620691,0.));
#86367=CARTESIAN_POINT('Ctrl Pts',(-73.247980856023,10.4979545795197,0.));
#86368=CARTESIAN_POINT('Ctrl Pts',(-73.2742502674361,10.4905419611529,0.));
#86369=CARTESIAN_POINT('Ctrl Pts',(-73.3005471910639,10.4830957433311,0.));
#86370=CARTESIAN_POINT('Ctrl Pts',(-73.3268715280609,10.475615904381,0.));
#86371=CARTESIAN_POINT('Ctrl Pts',(-73.353223182365,10.4681024236288,0.));
#86372=CARTESIAN_POINT('Ctrl Pts',(-73.3796020622436,10.4605552819391,0.));
#86373=CARTESIAN_POINT('Ctrl Pts',(-73.4060080806577,10.4529744618439,0.));
#86374=CARTESIAN_POINT('Ctrl Pts',(-73.4286663447914,10.4464473465487,0.));
#86375=CARTESIAN_POINT('Ctrl Pts',(-73.4460525528549,10.4414249334769,0.));
#86376=CARTESIAN_POINT('Ctrl Pts',(-73.4581547436537,10.4379221501094,0.));
#86377=CARTESIAN_POINT('Ctrl Pts',(-73.4649650361537,10.4359488742884,0.));
#86378=CARTESIAN_POINT('Ctrl Pts',(-73.4664795929515,10.4355099267392,0.));
#86379=CARTESIAN_POINT('',(-69.079679653846,11.3136138754166,12.));
#86380=CARTESIAN_POINT('',(-69.079679653846,11.3136138754166,0.));
#86381=CARTESIAN_POINT('Ctrl Pts',(-73.4664795929515,10.4355099267392,12.));
#86382=CARTESIAN_POINT('Ctrl Pts',(-73.4649650361537,10.4359488742884,12.));
#86383=CARTESIAN_POINT('Ctrl Pts',(-73.4581547436537,10.4379221501094,12.));
#86384=CARTESIAN_POINT('Ctrl Pts',(-73.4460525528549,10.4414249334769,12.));
#86385=CARTESIAN_POINT('Ctrl Pts',(-73.4286663447914,10.4464473465487,12.));
#86386=CARTESIAN_POINT('Ctrl Pts',(-73.4060080806577,10.4529744618439,12.));
#86387=CARTESIAN_POINT('Ctrl Pts',(-73.3796020622436,10.4605552819391,12.));
#86388=CARTESIAN_POINT('Ctrl Pts',(-73.353223182365,10.4681024236288,12.));
#86389=CARTESIAN_POINT('Ctrl Pts',(-73.3268715280609,10.475615904381,12.));
#86390=CARTESIAN_POINT('Ctrl Pts',(-73.3005471910639,10.4830957433311,12.));
#86391=CARTESIAN_POINT('Ctrl Pts',(-73.2742502674361,10.4905419611529,12.));
#86392=CARTESIAN_POINT('Ctrl Pts',(-73.247980856023,10.4979545795197,12.));
#86393=CARTESIAN_POINT('Ctrl Pts',(-73.2217390572578,10.505333620691,12.));
#86394=CARTESIAN_POINT('Ctrl Pts',(-73.1955249719037,10.5126791070804,12.));
#86395=CARTESIAN_POINT('Ctrl Pts',(-73.169338699611,10.5199910607652,12.));
#86396=CARTESIAN_POINT('Ctrl Pts',(-73.1431803382677,10.5272695032649,12.));
#86397=CARTESIAN_POINT('Ctrl Pts',(-73.1170499848012,10.5345144558097,12.));
#86398=CARTESIAN_POINT('Ctrl Pts',(-73.090947735646,10.5417259395001,12.));
#86399=CARTESIAN_POINT('Ctrl Pts',(-73.0648736873435,10.5489039755138,12.));
#86400=CARTESIAN_POINT('Ctrl Pts',(-73.0388279370845,10.5560485852976,12.));
#86401=CARTESIAN_POINT('Ctrl Pts',(-73.0128105832635,10.5631597907653,12.));
#86402=CARTESIAN_POINT('Ctrl Pts',(-72.9868217252293,10.5702376142052,12.));
#86403=CARTESIAN_POINT('Ctrl Pts',(-72.9608614630538,10.5772820781959,12.));
#86404=CARTESIAN_POINT('Ctrl Pts',(-72.9349298972823,10.5842932055209,12.));
#86405=CARTESIAN_POINT('Ctrl Pts',(-72.9090271287081,10.5912710190928,12.));
#86406=CARTESIAN_POINT('Ctrl Pts',(-72.8831532580839,10.5982155418625,12.));
#86407=CARTESIAN_POINT('Ctrl Pts',(-72.8573083861328,10.6051267968202,12.));
#86408=CARTESIAN_POINT('Ctrl Pts',(-72.8314926136872,10.6120048070367,12.));
#86409=CARTESIAN_POINT('Ctrl Pts',(-72.8057060417882,10.6188495956973,12.));
#86410=CARTESIAN_POINT('Ctrl Pts',(-72.7799487717914,10.6256611861395,12.));
#86411=CARTESIAN_POINT('Ctrl Pts',(-72.7542209054823,10.6324396019,12.));
#86412=CARTESIAN_POINT('Ctrl Pts',(-72.7285225451309,10.6391848667354,12.));
#86413=CARTESIAN_POINT('Ctrl Pts',(-72.7028537934332,10.6458970045948,12.));
#86414=CARTESIAN_POINT('Ctrl Pts',(-72.6772147534762,10.6525760396056,12.));
#86415=CARTESIAN_POINT('Ctrl Pts',(-72.6516055286908,10.6592219960581,12.));
#86416=CARTESIAN_POINT('Ctrl Pts',(-72.6260262228055,10.6658348983944,12.));
#86417=CARTESIAN_POINT('Ctrl Pts',(-72.6004769398004,10.6724147711994,12.));
#86418=CARTESIAN_POINT('Ctrl Pts',(-72.57495778394,10.6789616392041,12.));
#86419=CARTESIAN_POINT('Ctrl Pts',(-72.5494688597951,10.6854755272904,12.));
#86420=CARTESIAN_POINT('Ctrl Pts',(-72.5240102722662,10.6919564604991,12.));
#86421=CARTESIAN_POINT('Ctrl Pts',(-72.4985821266031,10.6984044640399,12.));
#86422=CARTESIAN_POINT('Ctrl Pts',(-72.4731845284238,10.7048195633062,12.));
#86423=CARTESIAN_POINT('Ctrl Pts',(-72.4478175837168,10.7112017838707,12.));
#86424=CARTESIAN_POINT('Ctrl Pts',(-72.4224813988355,10.7175511514789,12.));
#86425=CARTESIAN_POINT('Ctrl Pts',(-72.3971760804935,10.7238676920469,12.));
#86426=CARTESIAN_POINT('Ctrl Pts',(-72.3719017357568,10.7301514316607,12.));
#86427=CARTESIAN_POINT('Ctrl Pts',(-72.3466584720311,10.73640239658,12.));
#86428=CARTESIAN_POINT('Ctrl Pts',(-72.3214463970634,10.7426206132375,12.));
#86429=CARTESIAN_POINT('Ctrl Pts',(-72.296265618955,10.7488061082368,12.));
#86430=CARTESIAN_POINT('Ctrl Pts',(-72.2711162461679,10.7549589083536,12.));
#86431=CARTESIAN_POINT('Ctrl Pts',(-72.2459983875297,10.7610790405385,12.));
#86432=CARTESIAN_POINT('Ctrl Pts',(-72.2209121522367,10.7671665319254,12.));
#86433=CARTESIAN_POINT('Ctrl Pts',(-72.1958576498556,10.7732214098343,12.));
#86434=CARTESIAN_POINT('Ctrl Pts',(-72.17083499033,10.779243701766,12.));
#86435=CARTESIAN_POINT('Ctrl Pts',(-72.145844283983,10.7852334354015,12.));
#86436=CARTESIAN_POINT('Ctrl Pts',(-72.1208856415171,10.7911906386027,12.));
#86437=CARTESIAN_POINT('Ctrl Pts',(-72.095959174012,10.7971153394168,12.));
#86438=CARTESIAN_POINT('Ctrl Pts',(-72.0710649929214,10.8030075660812,12.));
#86439=CARTESIAN_POINT('Ctrl Pts',(-72.0462032100828,10.8088673470187,12.));
#86440=CARTESIAN_POINT('Ctrl Pts',(-72.0213739377231,10.8146947108377,12.));
#86441=CARTESIAN_POINT('Ctrl Pts',(-71.9965772884619,10.8204896863328,12.));
#86442=CARTESIAN_POINT('Ctrl Pts',(-71.971813375312,10.8262523024897,12.));
#86443=CARTESIAN_POINT('Ctrl Pts',(-71.9470823116777,10.8319825884917,12.));
#86444=CARTESIAN_POINT('Ctrl Pts',(-71.9223842113622,10.8376805737159,12.));
#86445=CARTESIAN_POINT('Ctrl Pts',(-71.8977191885726,10.8433462877312,12.));
#86446=CARTESIAN_POINT('Ctrl Pts',(-71.8730873579226,10.8489797602998,12.));
#86447=CARTESIAN_POINT('Ctrl Pts',(-71.8484888344335,10.8545810213799,12.));
#86448=CARTESIAN_POINT('Ctrl Pts',(-71.8239237335317,10.860150101133,12.));
#86449=CARTESIAN_POINT('Ctrl Pts',(-71.7993921710546,10.8656870299218,12.));
#86450=CARTESIAN_POINT('Ctrl Pts',(-71.7748942632578,10.8711918383071,12.));
#86451=CARTESIAN_POINT('Ctrl Pts',(-71.7504301268177,10.8766645570497,12.));
#86452=CARTESIAN_POINT('Ctrl Pts',(-71.7259998788337,10.8821052171122,12.));
#86453=CARTESIAN_POINT('Ctrl Pts',(-71.7016036368254,10.8875138496674,12.));
#86454=CARTESIAN_POINT('Ctrl Pts',(-71.6772415187382,10.8928904860967,12.));
#86455=CARTESIAN_POINT('Ctrl Pts',(-71.6529136429515,10.8982351579873,12.));
#86456=CARTESIAN_POINT('Ctrl Pts',(-71.6286201282815,10.9035478971329,12.));
#86457=CARTESIAN_POINT('Ctrl Pts',(-71.604361093983,10.9088287355364,12.));
#86458=CARTESIAN_POINT('Ctrl Pts',(-71.5801366597479,10.9140777054169,12.));
#86459=CARTESIAN_POINT('Ctrl Pts',(-71.5559469457082,10.91929483921,12.));
#86460=CARTESIAN_POINT('Ctrl Pts',(-71.5317920724453,10.9244801695642,12.));
#86461=CARTESIAN_POINT('Ctrl Pts',(-71.5076721609936,10.9296337293425,12.));
#86462=CARTESIAN_POINT('Ctrl Pts',(-71.4835873328425,10.9347555516236,12.));
#86463=CARTESIAN_POINT('Ctrl Pts',(-71.4595377099352,10.9398456697095,12.));
#86464=CARTESIAN_POINT('Ctrl Pts',(-71.4355234146718,10.9449041171269,12.));
#86465=CARTESIAN_POINT('Ctrl Pts',(-71.411544569919,10.9499309276236,12.));
#86466=CARTESIAN_POINT('Ctrl Pts',(-71.3876012990135,10.954926135169,12.));
#86467=CARTESIAN_POINT('Ctrl Pts',(-71.3636937257651,10.9598897739565,12.));
#86468=CARTESIAN_POINT('Ctrl Pts',(-71.3398219744547,10.96482187841,12.));
#86469=CARTESIAN_POINT('Ctrl Pts',(-71.3159861698368,10.9697224831863,12.));
#86470=CARTESIAN_POINT('Ctrl Pts',(-71.2921864371499,10.9745916231711,12.));
#86471=CARTESIAN_POINT('Ctrl Pts',(-71.2684229021209,10.9794293334806,12.));
#86472=CARTESIAN_POINT('Ctrl Pts',(-71.2446956909685,10.9842356494627,12.));
#86473=CARTESIAN_POINT('Ctrl Pts',(-71.221004930401,10.9890106067039,12.));
#86474=CARTESIAN_POINT('Ctrl Pts',(-71.1973507476188,10.993754241032,12.));
#86475=CARTESIAN_POINT('Ctrl Pts',(-71.1737332703248,10.9984665885127,12.));
#86476=CARTESIAN_POINT('Ctrl Pts',(-71.1501526267288,11.0031476854503,12.));
#86477=CARTESIAN_POINT('Ctrl Pts',(-71.1266089455517,11.0077975683895,12.));
#86478=CARTESIAN_POINT('Ctrl Pts',(-71.1031023560243,11.0124162741224,12.));
#86479=CARTESIAN_POINT('Ctrl Pts',(-71.0796329878896,11.0170038396913,12.));
#86480=CARTESIAN_POINT('Ctrl Pts',(-71.0562009714125,11.0215603023855,12.));
#86481=CARTESIAN_POINT('Ctrl Pts',(-71.0328064373849,11.0260856997415,12.));
#86482=CARTESIAN_POINT('Ctrl Pts',(-71.0094495171295,11.0305800695457,12.));
#86483=CARTESIAN_POINT('Ctrl Pts',(-70.9861303424989,11.0350434498408,12.));
#86484=CARTESIAN_POINT('Ctrl Pts',(-70.9628490458779,11.039475878929,12.));
#86485=CARTESIAN_POINT('Ctrl Pts',(-70.9396057601953,11.0438773953686,12.));
#86486=CARTESIAN_POINT('Ctrl Pts',(-70.9164006189283,11.0482480379752,12.));
#86487=CARTESIAN_POINT('Ctrl Pts',(-70.8932337561079,11.0525878458242,12.));
#86488=CARTESIAN_POINT('Ctrl Pts',(-70.8701053063158,11.0568968582566,12.));
#86489=CARTESIAN_POINT('Ctrl Pts',(-70.847015404688,11.0611751148831,12.));
#86490=CARTESIAN_POINT('Ctrl Pts',(-70.8239641869266,11.0654226555799,12.));
#86491=CARTESIAN_POINT('Ctrl Pts',(-70.8009517893042,11.0696395204908,12.));
#86492=CARTESIAN_POINT('Ctrl Pts',(-70.7779783486689,11.0738257500292,12.));
#86493=CARTESIAN_POINT('Ctrl Pts',(-70.7550440024422,11.0779813848851,12.));
#86494=CARTESIAN_POINT('Ctrl Pts',(-70.7321488886229,11.0821064660276,12.));
#86495=CARTESIAN_POINT('Ctrl Pts',(-70.7092931457996,11.0862010347022,12.));
#86496=CARTESIAN_POINT('Ctrl Pts',(-70.686476913156,11.0902651324326,12.));
#86497=CARTESIAN_POINT('Ctrl Pts',(-70.6637003304768,11.0942988010231,12.));
#86498=CARTESIAN_POINT('Ctrl Pts',(-70.6409635381446,11.0983020825662,12.));
#86499=CARTESIAN_POINT('Ctrl Pts',(-70.6182666771441,11.102275019444,12.));
#86500=CARTESIAN_POINT('Ctrl Pts',(-70.5956098890744,11.1062176543258,12.));
#86501=CARTESIAN_POINT('Ctrl Pts',(-70.5729933161538,11.1101300301701,12.));
#86502=CARTESIAN_POINT('Ctrl Pts',(-70.5504171012247,11.1140121902274,12.));
#86503=CARTESIAN_POINT('Ctrl Pts',(-70.5278813877519,11.117864178048,12.));
#86504=CARTESIAN_POINT('Ctrl Pts',(-70.5053863198306,11.121686037483,12.));
#86505=CARTESIAN_POINT('Ctrl Pts',(-70.4829320421973,11.1254778126824,12.));
#86506=CARTESIAN_POINT('Ctrl Pts',(-70.4605187002356,11.1292395480975,12.));
#86507=CARTESIAN_POINT('Ctrl Pts',(-70.438146439981,11.1329712884845,12.));
#86508=CARTESIAN_POINT('Ctrl Pts',(-70.415815408119,11.1366730789123,12.));
#86509=CARTESIAN_POINT('Ctrl Pts',(-70.3935257519945,11.1403449647622,12.));
#86510=CARTESIAN_POINT('Ctrl Pts',(-70.3712776196216,11.1439869917269,12.));
#86511=CARTESIAN_POINT('Ctrl Pts',(-70.3490711596882,11.1475992058124,12.));
#86512=CARTESIAN_POINT('Ctrl Pts',(-70.3269065215591,11.1511816533422,12.));
#86513=CARTESIAN_POINT('Ctrl Pts',(-70.3047838552757,11.1547343809647,12.));
#86514=CARTESIAN_POINT('Ctrl Pts',(-70.2827033115662,11.1582574356522,12.));
#86515=CARTESIAN_POINT('Ctrl Pts',(-70.2606650418589,11.1617508647017,12.));
#86516=CARTESIAN_POINT('Ctrl Pts',(-70.2386691982902,11.1652147157383,12.));
#86517=CARTESIAN_POINT('Ctrl Pts',(-70.2167159337095,11.168649036721,12.));
#86518=CARTESIAN_POINT('Ctrl Pts',(-70.1948054016817,11.1720538759499,12.));
#86519=CARTESIAN_POINT('Ctrl Pts',(-70.1729377564956,11.1754292820631,12.));
#86520=CARTESIAN_POINT('Ctrl Pts',(-70.1511131531674,11.1787753040363,12.));
#86521=CARTESIAN_POINT('Ctrl Pts',(-70.1293317474432,11.1820919911846,12.));
#86522=CARTESIAN_POINT('Ctrl Pts',(-70.1075936957968,11.185379393167,12.));
#86523=CARTESIAN_POINT('Ctrl Pts',(-70.0858991554283,11.1886375599914,12.));
#86524=CARTESIAN_POINT('Ctrl Pts',(-70.0642482842928,11.1918665420167,12.));
#86525=CARTESIAN_POINT('Ctrl Pts',(-70.0426412411185,11.1950663899577,12.));
#86526=CARTESIAN_POINT('Ctrl Pts',(-70.0210781854243,11.1982371548919,12.));
#86527=CARTESIAN_POINT('Ctrl Pts',(-69.9995592775343,11.2013788882714,12.));
#86528=CARTESIAN_POINT('Ctrl Pts',(-69.97808467858,11.2044916419244,12.));
#86529=CARTESIAN_POINT('Ctrl Pts',(-69.9566545504837,11.2075754680449,12.));
#86530=CARTESIAN_POINT('Ctrl Pts',(-69.9352690559405,11.2106304191883,12.));
#86531=CARTESIAN_POINT('Ctrl Pts',(-69.9139283584021,11.2136565482678,12.));
#86532=CARTESIAN_POINT('Ctrl Pts',(-69.8926326220385,11.2166539085523,12.));
#86533=CARTESIAN_POINT('Ctrl Pts',(-69.871382011789,11.219622553679,12.));
#86534=CARTESIAN_POINT('Ctrl Pts',(-69.8501766934428,11.2225625376737,12.));
#86535=CARTESIAN_POINT('Ctrl Pts',(-69.8290168337076,11.2254739149721,12.));
#86536=CARTESIAN_POINT('Ctrl Pts',(-69.8079026002768,11.2283567404437,12.));
#86537=CARTESIAN_POINT('Ctrl Pts',(-69.7868341618954,11.2312110694188,12.));
#86538=CARTESIAN_POINT('Ctrl Pts',(-69.7658116882324,11.2340369576456,12.));
#86539=CARTESIAN_POINT('Ctrl Pts',(-69.7448353497408,11.2368344612473,12.));
#86540=CARTESIAN_POINT('Ctrl Pts',(-69.7239053175356,11.239603636686,12.));
#86541=CARTESIAN_POINT('Ctrl Pts',(-69.7030217632164,11.2423445407167,12.));
#86542=CARTESIAN_POINT('Ctrl Pts',(-69.6821848588457,11.2450572303841,12.));
#86543=CARTESIAN_POINT('Ctrl Pts',(-69.6613947773534,11.2477417631386,12.));
#86544=CARTESIAN_POINT('Ctrl Pts',(-69.6406516928891,11.2503981969412,12.));
#86545=CARTESIAN_POINT('Ctrl Pts',(-69.6199557811245,11.2530265903558,12.));
#86546=CARTESIAN_POINT('Ctrl Pts',(-69.599307219739,11.2556270027016,12.));
#86547=CARTESIAN_POINT('Ctrl Pts',(-69.5787061880857,11.2581994939541,12.));
#86548=CARTESIAN_POINT('Ctrl Pts',(-69.5581528662877,11.2607441244703,12.));
#86549=CARTESIAN_POINT('Ctrl Pts',(-69.5376474344771,11.263260954763,12.));
#86550=CARTESIAN_POINT('Ctrl Pts',(-69.5171900720158,11.2657500452716,12.));
#86551=CARTESIAN_POINT('Ctrl Pts',(-69.4967809565929,11.2682114561008,12.));
#86552=CARTESIAN_POINT('Ctrl Pts',(-69.4764202659397,11.270645247528,12.));
#86553=CARTESIAN_POINT('Ctrl Pts',(-69.456108179879,11.2730514806139,12.));
#86554=CARTESIAN_POINT('Ctrl Pts',(-69.4358448819967,11.2754302177021,12.));
#86555=CARTESIAN_POINT('Ctrl Pts',(-69.4156305620593,11.2777815231469,12.));
#86556=CARTESIAN_POINT('Ctrl Pts',(-69.3954654162281,11.2801054633816,12.));
#86557=CARTESIAN_POINT('Ctrl Pts',(-69.3753496420039,11.2824021054045,12.));
#86558=CARTESIAN_POINT('Ctrl Pts',(-69.3552834337784,11.2846715154524,12.));
#86559=CARTESIAN_POINT('Ctrl Pts',(-69.3352669789587,11.2869137578459,12.));
#86560=CARTESIAN_POINT('Ctrl Pts',(-69.3153004517783,11.2891288931517,12.));
#86561=CARTESIAN_POINT('Ctrl Pts',(-69.295384019272,11.2913169799628,12.));
#86562=CARTESIAN_POINT('Ctrl Pts',(-69.2755178531479,11.2934780784351,12.));
#86563=CARTESIAN_POINT('Ctrl Pts',(-69.255702139335,11.2956122531375,12.));
#86564=CARTESIAN_POINT('Ctrl Pts',(-69.2359370894907,11.2977195764853,12.));
#86565=CARTESIAN_POINT('Ctrl Pts',(-69.2162229488531,11.2998001310964,12.));
#86566=CARTESIAN_POINT('Ctrl Pts',(-69.1965599718914,11.3018540025638,12.));
#86567=CARTESIAN_POINT('Ctrl Pts',(-69.1769483991721,11.3038812726293,12.));
#86568=CARTESIAN_POINT('Ctrl Pts',(-69.1573884361,11.3058820128308,12.));
#86569=CARTESIAN_POINT('Ctrl Pts',(-69.1378802251711,11.3078562764385,12.));
#86570=CARTESIAN_POINT('Ctrl Pts',(-69.118423844466,11.3098040973713,12.));
#86571=CARTESIAN_POINT('Ctrl Pts',(-69.1029002322118,11.3113412156662,12.));
#86572=CARTESIAN_POINT('Ctrl Pts',(-69.0912808656811,11.3124821678798,12.));
#86573=CARTESIAN_POINT('Ctrl Pts',(-69.0835449954396,11.3132375200165,12.));
#86574=CARTESIAN_POINT('Ctrl Pts',(-69.079679653846,11.3136138754166,12.));
#86575=CARTESIAN_POINT('Ctrl Pts',(-73.6640787198055,8.93459554657839,0.));
#86576=CARTESIAN_POINT('Ctrl Pts',(-73.6640787198055,8.93459554657839,4.));
#86577=CARTESIAN_POINT('Ctrl Pts',(-73.6640787198055,8.93459554657838,8.));
#86578=CARTESIAN_POINT('Ctrl Pts',(-73.6640787198055,8.93459554657838,12.));
#86579=CARTESIAN_POINT('Ctrl Pts',(-73.7581053903594,8.99145626777888,0.));
#86580=CARTESIAN_POINT('Ctrl Pts',(-73.7581053903594,8.99145626777888,4.));
#86581=CARTESIAN_POINT('Ctrl Pts',(-73.7581053903594,8.99145626777887,8.));
#86582=CARTESIAN_POINT('Ctrl Pts',(-73.7581053903594,8.99145626777887,12.));
#86583=CARTESIAN_POINT('Ctrl Pts',(-73.8880618019209,9.14696952162286,0.));
#86584=CARTESIAN_POINT('Ctrl Pts',(-73.8880618019209,9.14696952162286,4.));
#86585=CARTESIAN_POINT('Ctrl Pts',(-73.8880618019209,9.14696952162285,8.));
#86586=CARTESIAN_POINT('Ctrl Pts',(-73.8880618019209,9.14696952162285,12.));
#86587=CARTESIAN_POINT('Ctrl Pts',(-73.9117532086773,9.34395683490519,0.));
#86588=CARTESIAN_POINT('Ctrl Pts',(-73.9117532086773,9.34395683490519,4.));
#86589=CARTESIAN_POINT('Ctrl Pts',(-73.9117532086773,9.34395683490518,8.00000000000001));
#86590=CARTESIAN_POINT('Ctrl Pts',(-73.9117532086773,9.34395683490518,12.));
#86591=CARTESIAN_POINT('Ctrl Pts',(-73.9013264985866,9.42570643237552,0.));
#86592=CARTESIAN_POINT('Ctrl Pts',(-73.9013264985866,9.42570643237552,4.));
#86593=CARTESIAN_POINT('Ctrl Pts',(-73.9013264985866,9.42570643237552,8.));
#86594=CARTESIAN_POINT('Ctrl Pts',(-73.9013264985866,9.42570643237552,12.));
#86595=CARTESIAN_POINT('',(-73.6640787198055,8.9345955465784,0.));
#86596=CARTESIAN_POINT('',(-73.9013264985865,9.42570643237551,0.));
#86597=CARTESIAN_POINT('Ctrl Pts',(-73.6640787198055,8.93459554657839,1.8809784878848E-35));
#86598=CARTESIAN_POINT('Ctrl Pts',(-73.7581053903594,8.99145626777888,1.8809784878848E-35));
#86599=CARTESIAN_POINT('Ctrl Pts',(-73.832366196966,9.08032098426116,1.8809784878848E-35));
#86600=CARTESIAN_POINT('Ctrl Pts',(-73.8719282264933,9.18272825076412,1.8809784878848E-35));
#86601=CARTESIAN_POINT('Ctrl Pts',(-73.9015997486389,9.25953370064133,1.8809784878848E-35));
#86602=CARTESIAN_POINT('Ctrl Pts',(-73.9117532086773,9.34395683490519,1.88097848788479E-35));
#86603=CARTESIAN_POINT('Ctrl Pts',(-73.9013264985866,9.42570643237552,1.8809784878848E-35));
#86604=CARTESIAN_POINT('',(-73.9013264985865,9.4257064323755,12.));
#86605=CARTESIAN_POINT('Ctrl Pts',(-73.9013264985866,9.42570643237552,0.));
#86606=CARTESIAN_POINT('Ctrl Pts',(-73.9013264985866,9.42570643237552,4.));
#86607=CARTESIAN_POINT('Ctrl Pts',(-73.9013264985866,9.42570643237552,8.));
#86608=CARTESIAN_POINT('Ctrl Pts',(-73.9013264985866,9.42570643237552,12.));
#86609=CARTESIAN_POINT('',(-73.6640787198055,8.93459554657838,12.));
#86610=CARTESIAN_POINT('Ctrl Pts',(-73.9013264985866,9.42570643237552,12.));
#86611=CARTESIAN_POINT('Ctrl Pts',(-73.9117532086773,9.34395683490518,12.));
#86612=CARTESIAN_POINT('Ctrl Pts',(-73.9015997486388,9.25953370064132,12.));
#86613=CARTESIAN_POINT('Ctrl Pts',(-73.8719282264933,9.1827282507641,12.));
#86614=CARTESIAN_POINT('Ctrl Pts',(-73.832366196966,9.08032098426114,12.));
#86615=CARTESIAN_POINT('Ctrl Pts',(-73.7581053903594,8.99145626777887,12.));
#86616=CARTESIAN_POINT('Ctrl Pts',(-73.6640787198055,8.93459554657838,12.));
#86617=CARTESIAN_POINT('Ctrl Pts',(-73.6640787198055,8.93459554657838,12.));
#86618=CARTESIAN_POINT('Ctrl Pts',(-73.6640787198055,8.93459554657838,8.));
#86619=CARTESIAN_POINT('Ctrl Pts',(-73.6640787198055,8.93459554657839,4.));
#86620=CARTESIAN_POINT('Ctrl Pts',(-73.6640787198055,8.93459554657839,0.));
#86621=CARTESIAN_POINT('Origin',(-3.71649880366789E-10,4.88285199465433E-11,
0.));
#86622=CARTESIAN_POINT('Origin',(-3.71649880366789E-10,4.88285199465433E-11,
12.));
#86623=CARTESIAN_POINT('Origin',(-3.71649880366789E-10,4.88285199465433E-11,
0.));
#86624=CARTESIAN_POINT('Ctrl Pts',(-72.6683126419591,16.4184755008035,0.));
#86625=CARTESIAN_POINT('Ctrl Pts',(-72.6683126419591,16.4184755008035,4.));
#86626=CARTESIAN_POINT('Ctrl Pts',(-72.6683126419591,16.4184755008035,8.));
#86627=CARTESIAN_POINT('Ctrl Pts',(-72.6683126419591,16.4184755008035,12.));
#86628=CARTESIAN_POINT('Ctrl Pts',(-72.6440964999409,16.525656351978,0.));
#86629=CARTESIAN_POINT('Ctrl Pts',(-72.6440964999409,16.525656351978,4.));
#86630=CARTESIAN_POINT('Ctrl Pts',(-72.6440964999409,16.525656351978,8.));
#86631=CARTESIAN_POINT('Ctrl Pts',(-72.6440964999409,16.525656351978,12.));
#86632=CARTESIAN_POINT('Ctrl Pts',(-72.5376471652843,16.698113384133,0.));
#86633=CARTESIAN_POINT('Ctrl Pts',(-72.5376471652843,16.698113384133,4.));
#86634=CARTESIAN_POINT('Ctrl Pts',(-72.5376471652843,16.698113384133,8.));
#86635=CARTESIAN_POINT('Ctrl Pts',(-72.5376471652843,16.698113384133,12.));
#86636=CARTESIAN_POINT('Ctrl Pts',(-72.3582555997242,16.7828708182978,0.));
#86637=CARTESIAN_POINT('Ctrl Pts',(-72.3582555997242,16.7828708182978,4.));
#86638=CARTESIAN_POINT('Ctrl Pts',(-72.3582555997242,16.7828708182978,7.99999999999999));
#86639=CARTESIAN_POINT('Ctrl Pts',(-72.3582555997242,16.7828708182978,12.));
#86640=CARTESIAN_POINT('Ctrl Pts',(-72.2774028393482,16.798825256881,0.));
#86641=CARTESIAN_POINT('Ctrl Pts',(-72.2774028393482,16.798825256881,4.));
#86642=CARTESIAN_POINT('Ctrl Pts',(-72.2774028393482,16.798825256881,8.));
#86643=CARTESIAN_POINT('Ctrl Pts',(-72.2774028393482,16.798825256881,12.));
#86644=CARTESIAN_POINT('',(-72.6683126419591,16.4184755008035,0.));
#86645=CARTESIAN_POINT('',(-72.2774028393482,16.7988252568807,0.));
#86646=CARTESIAN_POINT('Ctrl Pts',(-72.6683126419591,16.4184755008035,2.77555756156289E-16));
#86647=CARTESIAN_POINT('Ctrl Pts',(-72.6440964999409,16.525656351978,2.77555756156289E-16));
#86648=CARTESIAN_POINT('Ctrl Pts',(-72.5832683087086,16.6242032274951,2.77555756156289E-16));
#86649=CARTESIAN_POINT('Ctrl Pts',(-72.4986222461608,16.6941134995869,2.77555756156289E-16));
#86650=CARTESIAN_POINT('Ctrl Pts',(-72.4351376992499,16.7465462036557,2.77555756156289E-16));
#86651=CARTESIAN_POINT('Ctrl Pts',(-72.3582555997242,16.7828708182978,2.77555756156289E-16));
#86652=CARTESIAN_POINT('Ctrl Pts',(-72.2774028393482,16.798825256881,2.77555756156289E-16));
#86653=CARTESIAN_POINT('',(-72.2774028393482,16.7988252568807,12.));
#86654=CARTESIAN_POINT('Ctrl Pts',(-72.2774028393482,16.798825256881,0.));
#86655=CARTESIAN_POINT('Ctrl Pts',(-72.2774028393482,16.798825256881,4.));
#86656=CARTESIAN_POINT('Ctrl Pts',(-72.2774028393482,16.798825256881,8.));
#86657=CARTESIAN_POINT('Ctrl Pts',(-72.2774028393482,16.798825256881,12.));
#86658=CARTESIAN_POINT('',(-72.6683126419591,16.4184755008035,12.));
#86659=CARTESIAN_POINT('Ctrl Pts',(-72.2774028393482,16.798825256881,12.));
#86660=CARTESIAN_POINT('Ctrl Pts',(-72.3582555997242,16.7828708182978,12.));
#86661=CARTESIAN_POINT('Ctrl Pts',(-72.4351376992499,16.7465462036557,12.));
#86662=CARTESIAN_POINT('Ctrl Pts',(-72.4986222461608,16.6941134995869,12.));
#86663=CARTESIAN_POINT('Ctrl Pts',(-72.5832683087086,16.6242032274951,12.));
#86664=CARTESIAN_POINT('Ctrl Pts',(-72.6440964999409,16.525656351978,12.));
#86665=CARTESIAN_POINT('Ctrl Pts',(-72.6683126419591,16.4184755008035,12.));
#86666=CARTESIAN_POINT('Ctrl Pts',(-72.6683126419591,16.4184755008035,12.));
#86667=CARTESIAN_POINT('Ctrl Pts',(-72.6683126419591,16.4184755008035,8.));
#86668=CARTESIAN_POINT('Ctrl Pts',(-72.6683126419591,16.4184755008035,4.));
#86669=CARTESIAN_POINT('Ctrl Pts',(-72.6683126419591,16.4184755008035,0.));
#86670=CARTESIAN_POINT('Ctrl Pts',(-67.8307641965654,17.2912529479484,0.));
#86671=CARTESIAN_POINT('Ctrl Pts',(-67.8307641965654,17.2912529479484,12.));
#86672=CARTESIAN_POINT('Ctrl Pts',(-67.8346476309018,17.2912149114119,0.));
#86673=CARTESIAN_POINT('Ctrl Pts',(-67.8346476309018,17.2912149114119,12.));
#86674=CARTESIAN_POINT('Ctrl Pts',(-67.842419897098,17.2911366591348,0.));
#86675=CARTESIAN_POINT('Ctrl Pts',(-67.842419897098,17.2911366591348,12.));
#86676=CARTESIAN_POINT('Ctrl Pts',(-67.8540944889687,17.291012743109,0.));
#86677=CARTESIAN_POINT('Ctrl Pts',(-67.8540944889687,17.291012743109,12.));
#86678=CARTESIAN_POINT('Ctrl Pts',(-67.8696929978782,17.2908344459695,0.));
#86679=CARTESIAN_POINT('Ctrl Pts',(-67.8696929978782,17.2908344459695,12.));
#86680=CARTESIAN_POINT('Ctrl Pts',(-67.8892451049608,17.2905897723949,0.));
#86681=CARTESIAN_POINT('Ctrl Pts',(-67.8892451049608,17.2905897723949,12.));
#86682=CARTESIAN_POINT('Ctrl Pts',(-67.9088511496685,17.2903232740694,0.));
#86683=CARTESIAN_POINT('Ctrl Pts',(-67.9088511496685,17.2903232740694,12.));
#86684=CARTESIAN_POINT('Ctrl Pts',(-67.9285110571741,17.2900349103981,0.));
#86685=CARTESIAN_POINT('Ctrl Pts',(-67.9285110571741,17.2900349103981,12.));
#86686=CARTESIAN_POINT('Ctrl Pts',(-67.9482246901667,17.2897246158941,0.));
#86687=CARTESIAN_POINT('Ctrl Pts',(-67.9482246901667,17.2897246158941,12.));
#86688=CARTESIAN_POINT('Ctrl Pts',(-67.9679918502579,17.2893923013894,0.));
#86689=CARTESIAN_POINT('Ctrl Pts',(-67.9679918502579,17.2893923013894,12.));
#86690=CARTESIAN_POINT('Ctrl Pts',(-67.987812304921,17.2890378644866,0.));
#86691=CARTESIAN_POINT('Ctrl Pts',(-67.987812304921,17.2890378644866,12.));
#86692=CARTESIAN_POINT('Ctrl Pts',(-68.007685808115,17.2886611977401,0.));
#86693=CARTESIAN_POINT('Ctrl Pts',(-68.007685808115,17.2886611977401,12.));
#86694=CARTESIAN_POINT('Ctrl Pts',(-68.0276121227356,17.2882621974721,0.));
#86695=CARTESIAN_POINT('Ctrl Pts',(-68.0276121227356,17.2882621974721,12.));
#86696=CARTESIAN_POINT('Ctrl Pts',(-68.0475910442424,17.2878407730961,0.));
#86697=CARTESIAN_POINT('Ctrl Pts',(-68.0475910442424,17.2878407730961,12.));
#86698=CARTESIAN_POINT('Ctrl Pts',(-68.0676223930412,17.2873968440839,0.));
#86699=CARTESIAN_POINT('Ctrl Pts',(-68.0676223930412,17.2873968440839,12.));
#86700=CARTESIAN_POINT('Ctrl Pts',(-68.0877060033205,17.2869303355432,0.));
#86701=CARTESIAN_POINT('Ctrl Pts',(-68.0877060033205,17.2869303355432,12.));
#86702=CARTESIAN_POINT('Ctrl Pts',(-68.1078417137877,17.2864411745459,0.));
#86703=CARTESIAN_POINT('Ctrl Pts',(-68.1078417137877,17.2864411745459,12.));
#86704=CARTESIAN_POINT('Ctrl Pts',(-68.1280293561511,17.2859292855705,0.));
#86705=CARTESIAN_POINT('Ctrl Pts',(-68.1280293561511,17.2859292855705,12.));
#86706=CARTESIAN_POINT('Ctrl Pts',(-68.1482687493226,17.2853945882072,0.));
#86707=CARTESIAN_POINT('Ctrl Pts',(-68.1482687493226,17.2853945882072,12.));
#86708=CARTESIAN_POINT('Ctrl Pts',(-68.1685597054231,17.2848369995293,0.));
#86709=CARTESIAN_POINT('Ctrl Pts',(-68.1685597054231,17.2848369995293,12.));
#86710=CARTESIAN_POINT('Ctrl Pts',(-68.1889020335427,17.2842564355799,0.));
#86711=CARTESIAN_POINT('Ctrl Pts',(-68.1889020335427,17.2842564355799,12.));
#86712=CARTESIAN_POINT('Ctrl Pts',(-68.2092955440567,17.2836528130819,0.));
#86713=CARTESIAN_POINT('Ctrl Pts',(-68.2092955440567,17.2836528130819,12.));
#86714=CARTESIAN_POINT('Ctrl Pts',(-68.2297400535294,17.2830260513868,0.));
#86715=CARTESIAN_POINT('Ctrl Pts',(-68.2297400535294,17.2830260513868,12.));
#86716=CARTESIAN_POINT('Ctrl Pts',(-68.2502353845071,17.2823760723874,0.));
#86717=CARTESIAN_POINT('Ctrl Pts',(-68.2502353845071,17.2823760723874,12.));
#86718=CARTESIAN_POINT('Ctrl Pts',(-68.2707813631731,17.2817027995831,0.));
#86719=CARTESIAN_POINT('Ctrl Pts',(-68.2707813631731,17.2817027995831,12.));
#86720=CARTESIAN_POINT('Ctrl Pts',(-68.2913778177261,17.2810061574353,0.));
#86721=CARTESIAN_POINT('Ctrl Pts',(-68.2913778177261,17.2810061574353,12.));
#86722=CARTESIAN_POINT('Ctrl Pts',(-68.3120245763914,17.2802860705815,0.));
#86723=CARTESIAN_POINT('Ctrl Pts',(-68.3120245763914,17.2802860705815,12.));
#86724=CARTESIAN_POINT('Ctrl Pts',(-68.3327214657575,17.2795424631799,0.));
#86725=CARTESIAN_POINT('Ctrl Pts',(-68.3327214657575,17.2795424631799,12.));
#86726=CARTESIAN_POINT('Ctrl Pts',(-68.3534683116514,17.2787752592484,0.));
#86727=CARTESIAN_POINT('Ctrl Pts',(-68.3534683116514,17.2787752592484,12.));
#86728=CARTESIAN_POINT('Ctrl Pts',(-68.3742649398964,17.2779843829608,0.));
#86729=CARTESIAN_POINT('Ctrl Pts',(-68.3742649398964,17.2779843829608,12.));
#86730=CARTESIAN_POINT('Ctrl Pts',(-68.3951111770487,17.2771697589385,0.));
#86731=CARTESIAN_POINT('Ctrl Pts',(-68.3951111770487,17.2771697589385,12.));
#86732=CARTESIAN_POINT('Ctrl Pts',(-68.4160068512753,17.2763313126018,0.));
#86733=CARTESIAN_POINT('Ctrl Pts',(-68.4160068512753,17.2763313126018,12.));
#86734=CARTESIAN_POINT('Ctrl Pts',(-68.436951792677,17.2754689702992,0.));
#86735=CARTESIAN_POINT('Ctrl Pts',(-68.436951792677,17.2754689702992,12.));
#86736=CARTESIAN_POINT('Ctrl Pts',(-68.4579458328185,17.2745826591119,0.));
#86737=CARTESIAN_POINT('Ctrl Pts',(-68.4579458328185,17.2745826591119,12.));
#86738=CARTESIAN_POINT('Ctrl Pts',(-68.4789888044351,17.2736723067365,0.));
#86739=CARTESIAN_POINT('Ctrl Pts',(-68.4789888044351,17.2736723067365,12.));
#86740=CARTESIAN_POINT('Ctrl Pts',(-68.5000805410911,17.2727378413489,0.));
#86741=CARTESIAN_POINT('Ctrl Pts',(-68.5000805410911,17.2727378413489,12.));
#86742=CARTESIAN_POINT('Ctrl Pts',(-68.521220876786,17.2717791914544,0.));
#86743=CARTESIAN_POINT('Ctrl Pts',(-68.521220876786,17.2717791914544,12.));
#86744=CARTESIAN_POINT('Ctrl Pts',(-68.5424096459772,17.2707962858919,0.));
#86745=CARTESIAN_POINT('Ctrl Pts',(-68.5424096459772,17.2707962858919,12.));
#86746=CARTESIAN_POINT('Ctrl Pts',(-68.5636466837517,17.269789053896,0.));
#86747=CARTESIAN_POINT('Ctrl Pts',(-68.5636466837517,17.269789053896,12.));
#86748=CARTESIAN_POINT('Ctrl Pts',(-68.5849318259449,17.2687574251429,0.));
#86749=CARTESIAN_POINT('Ctrl Pts',(-68.5849318259449,17.2687574251429,12.));
#86750=CARTESIAN_POINT('Ctrl Pts',(-68.6062649092764,17.2677013298057,0.));
#86751=CARTESIAN_POINT('Ctrl Pts',(-68.6062649092764,17.2677013298057,12.));
#86752=CARTESIAN_POINT('Ctrl Pts',(-68.6276457714729,17.2666206986084,0.));
#86753=CARTESIAN_POINT('Ctrl Pts',(-68.6276457714729,17.2666206986084,12.));
#86754=CARTESIAN_POINT('Ctrl Pts',(-68.6490742512057,17.2655154627928,0.));
#86755=CARTESIAN_POINT('Ctrl Pts',(-68.6490742512057,17.2655154627928,12.));
#86756=CARTESIAN_POINT('Ctrl Pts',(-68.6705501880249,17.2643855540892,0.));
#86757=CARTESIAN_POINT('Ctrl Pts',(-68.6705501880249,17.2643855540892,12.));
#86758=CARTESIAN_POINT('Ctrl Pts',(-68.6920734222938,17.2632309046892,0.));
#86759=CARTESIAN_POINT('Ctrl Pts',(-68.6920734222938,17.2632309046892,12.));
#86760=CARTESIAN_POINT('Ctrl Pts',(-68.7136437951097,17.2620514472182,0.));
#86761=CARTESIAN_POINT('Ctrl Pts',(-68.7136437951097,17.2620514472182,12.));
#86762=CARTESIAN_POINT('Ctrl Pts',(-68.7352611482547,17.2608471147185,0.));
#86763=CARTESIAN_POINT('Ctrl Pts',(-68.7352611482547,17.2608471147185,12.));
#86764=CARTESIAN_POINT('Ctrl Pts',(-68.7569253242333,17.2596178406551,0.));
#86765=CARTESIAN_POINT('Ctrl Pts',(-68.7569253242333,17.2596178406551,12.));
#86766=CARTESIAN_POINT('Ctrl Pts',(-68.7786361662882,17.2583635589198,0.));
#86767=CARTESIAN_POINT('Ctrl Pts',(-68.7786361662882,17.2583635589198,12.));
#86768=CARTESIAN_POINT('Ctrl Pts',(-68.8003935184184,17.2570842038384,0.));
#86769=CARTESIAN_POINT('Ctrl Pts',(-68.8003935184184,17.2570842038384,12.));
#86770=CARTESIAN_POINT('Ctrl Pts',(-68.8221972253941,17.2557797101813,0.));
#86771=CARTESIAN_POINT('Ctrl Pts',(-68.8221972253941,17.2557797101813,12.));
#86772=CARTESIAN_POINT('Ctrl Pts',(-68.844047132755,17.2544500131625,0.));
#86773=CARTESIAN_POINT('Ctrl Pts',(-68.844047132755,17.2544500131625,12.));
#86774=CARTESIAN_POINT('Ctrl Pts',(-68.8659430867972,17.2530950484258,0.));
#86775=CARTESIAN_POINT('Ctrl Pts',(-68.8659430867972,17.2530950484258,12.));
#86776=CARTESIAN_POINT('Ctrl Pts',(-68.8878849345557,17.2517147520376,0.));
#86777=CARTESIAN_POINT('Ctrl Pts',(-68.8878849345557,17.2517147520376,12.));
#86778=CARTESIAN_POINT('Ctrl Pts',(-68.909872523787,17.2503090604792,0.));
#86779=CARTESIAN_POINT('Ctrl Pts',(-68.909872523787,17.2503090604792,12.));
#86780=CARTESIAN_POINT('Ctrl Pts',(-68.9319057029409,17.248877910643,0.));
#86781=CARTESIAN_POINT('Ctrl Pts',(-68.9319057029409,17.248877910643,12.));
#86782=CARTESIAN_POINT('Ctrl Pts',(-68.9539843211619,17.2474212398275,0.));
#86783=CARTESIAN_POINT('Ctrl Pts',(-68.9539843211619,17.2474212398275,12.));
#86784=CARTESIAN_POINT('Ctrl Pts',(-68.9761082282922,17.2459389857327,0.));
#86785=CARTESIAN_POINT('Ctrl Pts',(-68.9761082282922,17.2459389857327,12.));
#86786=CARTESIAN_POINT('Ctrl Pts',(-68.9982772748694,17.2444310864585,0.));
#86787=CARTESIAN_POINT('Ctrl Pts',(-68.9982772748694,17.2444310864585,12.));
#86788=CARTESIAN_POINT('Ctrl Pts',(-69.0204913121225,17.2428974805044,0.));
#86789=CARTESIAN_POINT('Ctrl Pts',(-69.0204913121225,17.2428974805044,12.));
#86790=CARTESIAN_POINT('Ctrl Pts',(-69.0427501919636,17.2413381067724,0.));
#86791=CARTESIAN_POINT('Ctrl Pts',(-69.0427501919636,17.2413381067724,12.));
#86792=CARTESIAN_POINT('Ctrl Pts',(-69.065053766986,17.2397529045589,0.));
#86793=CARTESIAN_POINT('Ctrl Pts',(-69.065053766986,17.2397529045589,12.));
#86794=CARTESIAN_POINT('Ctrl Pts',(-69.0874018904598,17.2381418135491,0.));
#86795=CARTESIAN_POINT('Ctrl Pts',(-69.0874018904598,17.2381418135491,12.));
#86796=CARTESIAN_POINT('Ctrl Pts',(-69.1097944163245,17.2365047738126,0.));
#86797=CARTESIAN_POINT('Ctrl Pts',(-69.1097944163245,17.2365047738126,12.));
#86798=CARTESIAN_POINT('Ctrl Pts',(-69.1322311991752,17.2348417258015,0.));
#86799=CARTESIAN_POINT('Ctrl Pts',(-69.1322311991752,17.2348417258015,12.));
#86800=CARTESIAN_POINT('Ctrl Pts',(-69.1547120942527,17.2331526103506,0.));
#86801=CARTESIAN_POINT('Ctrl Pts',(-69.1547120942527,17.2331526103506,12.));
#86802=CARTESIAN_POINT('Ctrl Pts',(-69.1772369574447,17.2314373686701,0.));
#86803=CARTESIAN_POINT('Ctrl Pts',(-69.1772369574447,17.2314373686701,12.));
#86804=CARTESIAN_POINT('Ctrl Pts',(-69.1998056452828,17.2296959423407,0.));
#86805=CARTESIAN_POINT('Ctrl Pts',(-69.1998056452828,17.2296959423407,12.));
#86806=CARTESIAN_POINT('Ctrl Pts',(-69.222418014938,17.227928273312,0.));
#86807=CARTESIAN_POINT('Ctrl Pts',(-69.222418014938,17.227928273312,12.));
#86808=CARTESIAN_POINT('Ctrl Pts',(-69.2450739242109,17.226134303902,0.));
#86809=CARTESIAN_POINT('Ctrl Pts',(-69.2450739242109,17.226134303902,12.));
#86810=CARTESIAN_POINT('Ctrl Pts',(-69.2677732315224,17.224313976797,0.));
#86811=CARTESIAN_POINT('Ctrl Pts',(-69.2677732315224,17.224313976797,12.));
#86812=CARTESIAN_POINT('Ctrl Pts',(-69.2905157959166,17.2224672350439,0.));
#86813=CARTESIAN_POINT('Ctrl Pts',(-69.2905157959166,17.2224672350439,12.));
#86814=CARTESIAN_POINT('Ctrl Pts',(-69.3133014770554,17.2205940220459,0.));
#86815=CARTESIAN_POINT('Ctrl Pts',(-69.3133014770554,17.2205940220459,12.));
#86816=CARTESIAN_POINT('Ctrl Pts',(-69.3361301352141,17.2186942815602,0.));
#86817=CARTESIAN_POINT('Ctrl Pts',(-69.3361301352141,17.2186942815602,12.));
#86818=CARTESIAN_POINT('Ctrl Pts',(-69.3590016312692,17.2167679576984,0.));
#86819=CARTESIAN_POINT('Ctrl Pts',(-69.3590016312692,17.2167679576984,12.));
#86820=CARTESIAN_POINT('Ctrl Pts',(-69.3819158266915,17.2148149949252,0.));
#86821=CARTESIAN_POINT('Ctrl Pts',(-69.3819158266915,17.2148149949252,12.));
#86822=CARTESIAN_POINT('Ctrl Pts',(-69.404872583548,17.2128353380502,0.));
#86823=CARTESIAN_POINT('Ctrl Pts',(-69.404872583548,17.2128353380502,12.));
#86824=CARTESIAN_POINT('Ctrl Pts',(-69.4278717644973,17.2108289322254,0.));
#86825=CARTESIAN_POINT('Ctrl Pts',(-69.4278717644973,17.2108289322254,12.));
#86826=CARTESIAN_POINT('Ctrl Pts',(-69.4509132327849,17.2087957229424,0.));
#86827=CARTESIAN_POINT('Ctrl Pts',(-69.4509132327849,17.2087957229424,12.));
#86828=CARTESIAN_POINT('Ctrl Pts',(-69.4739968522313,17.2067356560337,0.));
#86829=CARTESIAN_POINT('Ctrl Pts',(-69.4739968522313,17.2067356560337,12.));
#86830=CARTESIAN_POINT('Ctrl Pts',(-69.4971224872269,17.2046486776708,0.));
#86831=CARTESIAN_POINT('Ctrl Pts',(-69.4971224872269,17.2046486776708,12.));
#86832=CARTESIAN_POINT('Ctrl Pts',(-69.5202900027367,17.2025347343577,0.));
#86833=CARTESIAN_POINT('Ctrl Pts',(-69.5202900027367,17.2025347343577,12.));
#86834=CARTESIAN_POINT('Ctrl Pts',(-69.5434992642944,17.2003937729268,0.));
#86835=CARTESIAN_POINT('Ctrl Pts',(-69.5434992642944,17.2003937729268,12.));
#86836=CARTESIAN_POINT('Ctrl Pts',(-69.5667501379969,17.1982257405377,0.));
#86837=CARTESIAN_POINT('Ctrl Pts',(-69.5667501379969,17.1982257405377,12.));
#86838=CARTESIAN_POINT('Ctrl Pts',(-69.5900424904921,17.1960305846781,0.));
#86839=CARTESIAN_POINT('Ctrl Pts',(-69.5900424904921,17.1960305846781,12.));
#86840=CARTESIAN_POINT('Ctrl Pts',(-69.6133761889749,17.1938082531612,0.));
#86841=CARTESIAN_POINT('Ctrl Pts',(-69.6133761889749,17.1938082531612,12.));
#86842=CARTESIAN_POINT('Ctrl Pts',(-69.6367511011898,17.1915586941192,0.));
#86843=CARTESIAN_POINT('Ctrl Pts',(-69.6367511011898,17.1915586941192,12.));
#86844=CARTESIAN_POINT('Ctrl Pts',(-69.6601670954269,17.1892818560003,0.));
#86845=CARTESIAN_POINT('Ctrl Pts',(-69.6601670954269,17.1892818560003,12.));
#86846=CARTESIAN_POINT('Ctrl Pts',(-69.6836240405164,17.1869776875666,0.));
#86847=CARTESIAN_POINT('Ctrl Pts',(-69.6836240405164,17.1869776875666,12.));
#86848=CARTESIAN_POINT('Ctrl Pts',(-69.7071218058178,17.1846461378973,0.));
#86849=CARTESIAN_POINT('Ctrl Pts',(-69.7071218058178,17.1846461378973,12.));
#86850=CARTESIAN_POINT('Ctrl Pts',(-69.7306602612155,17.1822871563842,0.));
#86851=CARTESIAN_POINT('Ctrl Pts',(-69.7306602612155,17.1822871563842,12.));
#86852=CARTESIAN_POINT('Ctrl Pts',(-69.7542392771234,17.179900692726,0.));
#86853=CARTESIAN_POINT('Ctrl Pts',(-69.7542392771234,17.179900692726,12.));
#86854=CARTESIAN_POINT('Ctrl Pts',(-69.777858724479,17.1774866969257,0.));
#86855=CARTESIAN_POINT('Ctrl Pts',(-69.777858724479,17.1774866969257,12.));
#86856=CARTESIAN_POINT('Ctrl Pts',(-69.8015184747398,17.1750451192886,0.));
#86857=CARTESIAN_POINT('Ctrl Pts',(-69.8015184747398,17.1750451192886,12.));
#86858=CARTESIAN_POINT('Ctrl Pts',(-69.8252183998702,17.1725759104252,0.));
#86859=CARTESIAN_POINT('Ctrl Pts',(-69.8252183998702,17.1725759104252,12.));
#86860=CARTESIAN_POINT('Ctrl Pts',(-69.8489583723407,17.1700790212474,0.));
#86861=CARTESIAN_POINT('Ctrl Pts',(-69.8489583723407,17.1700790212474,12.));
#86862=CARTESIAN_POINT('Ctrl Pts',(-69.8727382651285,17.167554402962,0.));
#86863=CARTESIAN_POINT('Ctrl Pts',(-69.8727382651285,17.167554402962,12.));
#86864=CARTESIAN_POINT('Ctrl Pts',(-69.8965579517147,17.1650020070686,0.));
#86865=CARTESIAN_POINT('Ctrl Pts',(-69.8965579517147,17.1650020070686,12.));
#86866=CARTESIAN_POINT('Ctrl Pts',(-69.9204173060781,17.1624217853578,0.));
#86867=CARTESIAN_POINT('Ctrl Pts',(-69.9204173060781,17.1624217853578,12.));
#86868=CARTESIAN_POINT('Ctrl Pts',(-69.9443162026865,17.1598136899145,0.));
#86869=CARTESIAN_POINT('Ctrl Pts',(-69.9443162026865,17.1598136899145,12.));
#86870=CARTESIAN_POINT('Ctrl Pts',(-69.9682545164939,17.157177673114,0.));
#86871=CARTESIAN_POINT('Ctrl Pts',(-69.9682545164939,17.157177673114,12.));
#86872=CARTESIAN_POINT('Ctrl Pts',(-69.9922321229424,17.1545136876161,0.));
#86873=CARTESIAN_POINT('Ctrl Pts',(-69.9922321229424,17.1545136876161,12.));
#86874=CARTESIAN_POINT('Ctrl Pts',(-70.0162488979584,17.1518216863623,0.));
#86875=CARTESIAN_POINT('Ctrl Pts',(-70.0162488979584,17.1518216863623,12.));
#86876=CARTESIAN_POINT('Ctrl Pts',(-70.0403047179483,17.1491016225749,0.));
#86877=CARTESIAN_POINT('Ctrl Pts',(-70.0403047179483,17.1491016225749,12.));
#86878=CARTESIAN_POINT('Ctrl Pts',(-70.0643994597873,17.1463534497595,0.));
#86879=CARTESIAN_POINT('Ctrl Pts',(-70.0643994597873,17.1463534497595,12.));
#86880=CARTESIAN_POINT('Ctrl Pts',(-70.0885330008179,17.1435771217018,0.));
#86881=CARTESIAN_POINT('Ctrl Pts',(-70.0885330008179,17.1435771217018,12.));
#86882=CARTESIAN_POINT('Ctrl Pts',(-70.1127052188522,17.1407725924617,0.));
#86883=CARTESIAN_POINT('Ctrl Pts',(-70.1127052188522,17.1407725924617,12.));
#86884=CARTESIAN_POINT('Ctrl Pts',(-70.1369159921687,17.1379398163709,0.));
#86885=CARTESIAN_POINT('Ctrl Pts',(-70.1369159921687,17.1379398163709,12.));
#86886=CARTESIAN_POINT('Ctrl Pts',(-70.1611651995082,17.1350787480312,0.));
#86887=CARTESIAN_POINT('Ctrl Pts',(-70.1611651995082,17.1350787480312,12.));
#86888=CARTESIAN_POINT('Ctrl Pts',(-70.1854527200631,17.1321893423182,0.));
#86889=CARTESIAN_POINT('Ctrl Pts',(-70.1854527200631,17.1321893423182,12.));
#86890=CARTESIAN_POINT('Ctrl Pts',(-70.2097784334747,17.1292715543778,0.));
#86891=CARTESIAN_POINT('Ctrl Pts',(-70.2097784334747,17.1292715543778,12.));
#86892=CARTESIAN_POINT('Ctrl Pts',(-70.2341422198363,17.1263253396202,0.));
#86893=CARTESIAN_POINT('Ctrl Pts',(-70.2341422198363,17.1263253396202,12.));
#86894=CARTESIAN_POINT('Ctrl Pts',(-70.2585439596901,17.1233506537177,0.));
#86895=CARTESIAN_POINT('Ctrl Pts',(-70.2585439596901,17.1233506537177,12.));
#86896=CARTESIAN_POINT('Ctrl Pts',(-70.2829835340238,17.1203474526031,0.));
#86897=CARTESIAN_POINT('Ctrl Pts',(-70.2829835340238,17.1203474526031,12.));
#86898=CARTESIAN_POINT('Ctrl Pts',(-70.3074608242608,17.1173156924733,0.));
#86899=CARTESIAN_POINT('Ctrl Pts',(-70.3074608242608,17.1173156924733,12.));
#86900=CARTESIAN_POINT('Ctrl Pts',(-70.3319757122568,17.1142553297867,0.));
#86901=CARTESIAN_POINT('Ctrl Pts',(-70.3319757122568,17.1142553297867,12.));
#86902=CARTESIAN_POINT('Ctrl Pts',(-70.3565280803022,17.1111663212568,0.));
#86903=CARTESIAN_POINT('Ctrl Pts',(-70.3565280803022,17.1111663212568,12.));
#86904=CARTESIAN_POINT('Ctrl Pts',(-70.3811178111201,17.1080486238499,0.));
#86905=CARTESIAN_POINT('Ctrl Pts',(-70.3811178111201,17.1080486238499,12.));
#86906=CARTESIAN_POINT('Ctrl Pts',(-70.4057447878624,17.1049021947834,0.));
#86907=CARTESIAN_POINT('Ctrl Pts',(-70.4057447878624,17.1049021947834,12.));
#86908=CARTESIAN_POINT('Ctrl Pts',(-70.430408894101,17.1017269915292,0.));
#86909=CARTESIAN_POINT('Ctrl Pts',(-70.430408894101,17.1017269915292,12.));
#86910=CARTESIAN_POINT('Ctrl Pts',(-70.4551100138238,17.0985229718125,0.));
#86911=CARTESIAN_POINT('Ctrl Pts',(-70.4551100138238,17.0985229718125,12.));
#86912=CARTESIAN_POINT('Ctrl Pts',(-70.4798480314381,17.0952900936048,0.));
#86913=CARTESIAN_POINT('Ctrl Pts',(-70.4798480314381,17.0952900936048,12.));
#86914=CARTESIAN_POINT('Ctrl Pts',(-70.5046228317677,17.0920283151219,0.));
#86915=CARTESIAN_POINT('Ctrl Pts',(-70.5046228317677,17.0920283151219,12.));
#86916=CARTESIAN_POINT('Ctrl Pts',(-70.5294343000513,17.088737594822,0.));
#86917=CARTESIAN_POINT('Ctrl Pts',(-70.5294343000513,17.088737594822,12.));
#86918=CARTESIAN_POINT('Ctrl Pts',(-70.5542823219331,17.0854178914087,0.));
#86919=CARTESIAN_POINT('Ctrl Pts',(-70.5542823219331,17.0854178914087,12.));
#86920=CARTESIAN_POINT('Ctrl Pts',(-70.5791667834582,17.082069163831,0.));
#86921=CARTESIAN_POINT('Ctrl Pts',(-70.5791667834582,17.082069163831,12.));
#86922=CARTESIAN_POINT('Ctrl Pts',(-70.6040875710749,17.0786913712764,0.));
#86923=CARTESIAN_POINT('Ctrl Pts',(-70.6040875710749,17.0786913712764,12.));
#86924=CARTESIAN_POINT('Ctrl Pts',(-70.6290445716337,17.0752844731678,0.));
#86925=CARTESIAN_POINT('Ctrl Pts',(-70.6290445716337,17.0752844731678,12.));
#86926=CARTESIAN_POINT('Ctrl Pts',(-70.6540376723841,17.0718484291624,0.));
#86927=CARTESIAN_POINT('Ctrl Pts',(-70.6540376723841,17.0718484291624,12.));
#86928=CARTESIAN_POINT('Ctrl Pts',(-70.6790667609679,17.0683831991532,0.));
#86929=CARTESIAN_POINT('Ctrl Pts',(-70.6790667609679,17.0683831991532,12.));
#86930=CARTESIAN_POINT('Ctrl Pts',(-70.7041317254125,17.0648887432714,0.));
#86931=CARTESIAN_POINT('Ctrl Pts',(-70.7041317254125,17.0648887432714,12.));
#86932=CARTESIAN_POINT('Ctrl Pts',(-70.7292324541341,17.0613650218787,0.));
#86933=CARTESIAN_POINT('Ctrl Pts',(-70.7292324541341,17.0613650218787,12.));
#86934=CARTESIAN_POINT('Ctrl Pts',(-70.7543688359374,17.0578119955649,0.));
#86935=CARTESIAN_POINT('Ctrl Pts',(-70.7543688359374,17.0578119955649,12.));
#86936=CARTESIAN_POINT('Ctrl Pts',(-70.7795407600127,17.0542296251462,0.));
#86937=CARTESIAN_POINT('Ctrl Pts',(-70.7795407600127,17.0542296251462,12.));
#86938=CARTESIAN_POINT('Ctrl Pts',(-70.8047481159306,17.0506178716664,0.));
#86939=CARTESIAN_POINT('Ctrl Pts',(-70.8047481159306,17.0506178716664,12.));
#86940=CARTESIAN_POINT('Ctrl Pts',(-70.8299907936346,17.0469766964005,0.));
#86941=CARTESIAN_POINT('Ctrl Pts',(-70.8299907936346,17.0469766964005,12.));
#86942=CARTESIAN_POINT('Ctrl Pts',(-70.8552686834435,17.0433060608479,0.));
#86943=CARTESIAN_POINT('Ctrl Pts',(-70.8552686834435,17.0433060608479,12.));
#86944=CARTESIAN_POINT('Ctrl Pts',(-70.8805816760507,17.039605926728,0.));
#86945=CARTESIAN_POINT('Ctrl Pts',(-70.8805816760507,17.039605926728,12.));
#86946=CARTESIAN_POINT('Ctrl Pts',(-70.9059296625214,17.0358762559786,0.));
#86947=CARTESIAN_POINT('Ctrl Pts',(-70.9059296625214,17.0358762559786,12.));
#86948=CARTESIAN_POINT('Ctrl Pts',(-70.9313125342872,17.0321170107562,0.));
#86949=CARTESIAN_POINT('Ctrl Pts',(-70.9313125342872,17.0321170107562,12.));
#86950=CARTESIAN_POINT('Ctrl Pts',(-70.9567301831355,17.028328153439,0.));
#86951=CARTESIAN_POINT('Ctrl Pts',(-70.9567301831355,17.028328153439,12.));
#86952=CARTESIAN_POINT('Ctrl Pts',(-70.9821825012134,17.0245096466228,0.));
#86953=CARTESIAN_POINT('Ctrl Pts',(-70.9821825012134,17.0245096466228,12.));
#86954=CARTESIAN_POINT('Ctrl Pts',(-71.0076693810302,17.0206614531166,0.));
#86955=CARTESIAN_POINT('Ctrl Pts',(-71.0076693810302,17.0206614531166,12.));
#86956=CARTESIAN_POINT('Ctrl Pts',(-71.0331907154575,17.016783535942,0.));
#86957=CARTESIAN_POINT('Ctrl Pts',(-71.0331907154575,17.016783535942,12.));
#86958=CARTESIAN_POINT('Ctrl Pts',(-71.0587463977266,17.0128758583335,0.));
#86959=CARTESIAN_POINT('Ctrl Pts',(-71.0587463977266,17.0128758583335,12.));
#86960=CARTESIAN_POINT('Ctrl Pts',(-71.0843363214216,17.0089383837437,0.));
#86961=CARTESIAN_POINT('Ctrl Pts',(-71.0843363214216,17.0089383837437,12.));
#86962=CARTESIAN_POINT('Ctrl Pts',(-71.1099603804779,17.0049710758393,0.));
#86963=CARTESIAN_POINT('Ctrl Pts',(-71.1099603804779,17.0049710758393,12.));
#86964=CARTESIAN_POINT('Ctrl Pts',(-71.1356184691799,17.0009738984935,0.));
#86965=CARTESIAN_POINT('Ctrl Pts',(-71.1356184691799,17.0009738984935,12.));
#86966=CARTESIAN_POINT('Ctrl Pts',(-71.1613104821565,16.9969468157824,0.));
#86967=CARTESIAN_POINT('Ctrl Pts',(-71.1613104821565,16.9969468157824,12.));
#86968=CARTESIAN_POINT('Ctrl Pts',(-71.1870363143742,16.9928897919829,0.));
#86969=CARTESIAN_POINT('Ctrl Pts',(-71.1870363143742,16.9928897919829,12.));
#86970=CARTESIAN_POINT('Ctrl Pts',(-71.2127958611248,16.9888027915743,0.));
#86971=CARTESIAN_POINT('Ctrl Pts',(-71.2127958611248,16.9888027915743,12.));
#86972=CARTESIAN_POINT('Ctrl Pts',(-71.2385890180233,16.9846857792385,0.));
#86973=CARTESIAN_POINT('Ctrl Pts',(-71.2385890180233,16.9846857792385,12.));
#86974=CARTESIAN_POINT('Ctrl Pts',(-71.2644156810209,16.9805387198573,0.));
#86975=CARTESIAN_POINT('Ctrl Pts',(-71.2644156810209,16.9805387198573,12.));
#86976=CARTESIAN_POINT('Ctrl Pts',(-71.2902757464127,16.9763615785138,0.));
#86977=CARTESIAN_POINT('Ctrl Pts',(-71.2902757464127,16.9763615785138,12.));
#86978=CARTESIAN_POINT('Ctrl Pts',(-71.3161691108425,16.9721543204951,0.));
#86979=CARTESIAN_POINT('Ctrl Pts',(-71.3161691108425,16.9721543204951,12.));
#86980=CARTESIAN_POINT('Ctrl Pts',(-71.3420956713072,16.9679169112993,0.));
#86981=CARTESIAN_POINT('Ctrl Pts',(-71.3420956713072,16.9679169112993,12.));
#86982=CARTESIAN_POINT('Ctrl Pts',(-71.3680553251547,16.9636493166395,0.));
#86983=CARTESIAN_POINT('Ctrl Pts',(-71.3680553251547,16.9636493166395,12.));
#86984=CARTESIAN_POINT('Ctrl Pts',(-71.3940479700662,16.9593515024274,0.));
#86985=CARTESIAN_POINT('Ctrl Pts',(-71.3940479700662,16.9593515024274,12.));
#86986=CARTESIAN_POINT('Ctrl Pts',(-71.4200735040374,16.9550234347619,0.));
#86987=CARTESIAN_POINT('Ctrl Pts',(-71.4200735040374,16.9550234347619,12.));
#86988=CARTESIAN_POINT('Ctrl Pts',(-71.4461318253561,16.9506650799189,0.));
#86989=CARTESIAN_POINT('Ctrl Pts',(-71.4461318253561,16.9506650799189,12.));
#86990=CARTESIAN_POINT('Ctrl Pts',(-71.4722228325805,16.9462764043445,0.));
#86991=CARTESIAN_POINT('Ctrl Pts',(-71.4722228325805,16.9462764043445,12.));
#86992=CARTESIAN_POINT('Ctrl Pts',(-71.4983464245069,16.9418573746492,0.));
#86993=CARTESIAN_POINT('Ctrl Pts',(-71.4983464245069,16.9418573746492,12.));
#86994=CARTESIAN_POINT('Ctrl Pts',(-71.5245025002154,16.9374079576204,0.));
#86995=CARTESIAN_POINT('Ctrl Pts',(-71.5245025002154,16.9374079576204,12.));
#86996=CARTESIAN_POINT('Ctrl Pts',(-71.5506909591139,16.9329281202379,0.));
#86997=CARTESIAN_POINT('Ctrl Pts',(-71.5506909591139,16.9329281202379,12.));
#86998=CARTESIAN_POINT('Ctrl Pts',(-71.5769117009845,16.9284178296934,0.));
#86999=CARTESIAN_POINT('Ctrl Pts',(-71.5769117009845,16.9284178296934,12.));
#87000=CARTESIAN_POINT('Ctrl Pts',(-71.6031646260169,16.923877053407,0.));
#87001=CARTESIAN_POINT('Ctrl Pts',(-71.6031646260169,16.923877053407,12.));
#87002=CARTESIAN_POINT('Ctrl Pts',(-71.6294496348644,16.9193057590605,0.));
#87003=CARTESIAN_POINT('Ctrl Pts',(-71.6294496348644,16.9193057590605,12.));
#87004=CARTESIAN_POINT('Ctrl Pts',(-71.6557666285908,16.9147039145716,0.));
#87005=CARTESIAN_POINT('Ctrl Pts',(-71.6557666285908,16.9147039145716,12.));
#87006=CARTESIAN_POINT('Ctrl Pts',(-71.6821155085605,16.9100714880367,0.));
#87007=CARTESIAN_POINT('Ctrl Pts',(-71.6821155085605,16.9100714880367,12.));
#87008=CARTESIAN_POINT('Ctrl Pts',(-71.7084961763355,16.9054084476847,0.));
#87009=CARTESIAN_POINT('Ctrl Pts',(-71.7084961763355,16.9054084476847,12.));
#87010=CARTESIAN_POINT('Ctrl Pts',(-71.7349085335796,16.9007147618344,0.));
#87011=CARTESIAN_POINT('Ctrl Pts',(-71.7349085335796,16.9007147618344,12.));
#87012=CARTESIAN_POINT('Ctrl Pts',(-71.7613524819239,16.8959903988411,0.));
#87013=CARTESIAN_POINT('Ctrl Pts',(-71.7613524819239,16.8959903988411,12.));
#87014=CARTESIAN_POINT('Ctrl Pts',(-71.7878279229556,16.8912353270944,0.));
#87015=CARTESIAN_POINT('Ctrl Pts',(-71.7878279229556,16.8912353270944,12.));
#87016=CARTESIAN_POINT('Ctrl Pts',(-71.8143347584977,16.8864495151347,0.));
#87017=CARTESIAN_POINT('Ctrl Pts',(-71.8143347584977,16.8864495151347,12.));
#87018=CARTESIAN_POINT('Ctrl Pts',(-71.8408728908269,16.8816329317473,0.));
#87019=CARTESIAN_POINT('Ctrl Pts',(-71.8408728908269,16.8816329317473,12.));
#87020=CARTESIAN_POINT('Ctrl Pts',(-71.8674422229151,16.8767855460701,0.));
#87021=CARTESIAN_POINT('Ctrl Pts',(-71.8674422229151,16.8767855460701,12.));
#87022=CARTESIAN_POINT('Ctrl Pts',(-71.8940426586521,16.8719073276967,0.));
#87023=CARTESIAN_POINT('Ctrl Pts',(-71.8940426586521,16.8719073276967,12.));
#87024=CARTESIAN_POINT('Ctrl Pts',(-71.920674103086,16.8669982467915,0.));
#87025=CARTESIAN_POINT('Ctrl Pts',(-71.920674103086,16.8669982467915,12.));
#87026=CARTESIAN_POINT('Ctrl Pts',(-71.9473364618889,16.8620582738431,0.));
#87027=CARTESIAN_POINT('Ctrl Pts',(-71.9473364618889,16.8620582738431,12.));
#87028=CARTESIAN_POINT('Ctrl Pts',(-71.9740296408319,16.8570873794264,0.));
#87029=CARTESIAN_POINT('Ctrl Pts',(-71.9740296408319,16.8570873794264,12.));
#87030=CARTESIAN_POINT('Ctrl Pts',(-72.0007535452071,16.8520855339444,0.));
#87031=CARTESIAN_POINT('Ctrl Pts',(-72.0007535452071,16.8520855339444,12.));
#87032=CARTESIAN_POINT('Ctrl Pts',(-72.0275080793742,16.8470527074278,0.));
#87033=CARTESIAN_POINT('Ctrl Pts',(-72.0275080793742,16.8470527074278,12.));
#87034=CARTESIAN_POINT('Ctrl Pts',(-72.0542931459865,16.8419888691984,0.));
#87035=CARTESIAN_POINT('Ctrl Pts',(-72.0542931459865,16.8419888691984,12.));
#87036=CARTESIAN_POINT('Ctrl Pts',(-72.0811086466178,16.8368939881457,0.));
#87037=CARTESIAN_POINT('Ctrl Pts',(-72.0811086466178,16.8368939881457,12.));
#87038=CARTESIAN_POINT('Ctrl Pts',(-72.1079544831568,16.8317680333415,0.));
#87039=CARTESIAN_POINT('Ctrl Pts',(-72.1079544831568,16.8317680333415,12.));
#87040=CARTESIAN_POINT('Ctrl Pts',(-72.1348305590233,16.8266109745802,0.));
#87041=CARTESIAN_POINT('Ctrl Pts',(-72.1348305590233,16.8266109745802,12.));
#87042=CARTESIAN_POINT('Ctrl Pts',(-72.1617367803226,16.8214227828941,0.));
#87043=CARTESIAN_POINT('Ctrl Pts',(-72.1617367803226,16.8214227828941,12.));
#87044=CARTESIAN_POINT('Ctrl Pts',(-72.1886730573389,16.8162034312257,0.));
#87045=CARTESIAN_POINT('Ctrl Pts',(-72.1886730573389,16.8162034312257,12.));
#87046=CARTESIAN_POINT('Ctrl Pts',(-72.2156393048868,16.8109528945876,0.));
#87047=CARTESIAN_POINT('Ctrl Pts',(-72.2156393048868,16.8109528945876,12.));
#87048=CARTESIAN_POINT('Ctrl Pts',(-72.242635439009,16.8056711485798,0.));
#87049=CARTESIAN_POINT('Ctrl Pts',(-72.242635439009,16.8056711485798,12.));
#87050=CARTESIAN_POINT('Ctrl Pts',(-72.2696613743687,16.800358168223,0.));
#87051=CARTESIAN_POINT('Ctrl Pts',(-72.2696613743687,16.800358168223,12.));
#87052=CARTESIAN_POINT('Ctrl Pts',(-72.2967170212331,16.7950139266118,0.));
#87053=CARTESIAN_POINT('Ctrl Pts',(-72.2967170212331,16.7950139266118,12.));
#87054=CARTESIAN_POINT('Ctrl Pts',(-72.323802282931,16.7896383937839,0.));
#87055=CARTESIAN_POINT('Ctrl Pts',(-72.323802282931,16.7896383937839,12.));
#87056=CARTESIAN_POINT('Ctrl Pts',(-72.3509170523038,16.7842315351402,0.));
#87057=CARTESIAN_POINT('Ctrl Pts',(-72.3509170523038,16.7842315351402,12.));
#87058=CARTESIAN_POINT('Ctrl Pts',(-72.3780612168056,16.7787933137551,0.));
#87059=CARTESIAN_POINT('Ctrl Pts',(-72.3780612168056,16.7787933137551,12.));
#87060=CARTESIAN_POINT('Ctrl Pts',(-72.4052346648058,16.7733236932185,0.));
#87061=CARTESIAN_POINT('Ctrl Pts',(-72.4052346648058,16.7733236932185,12.));
#87062=CARTESIAN_POINT('Ctrl Pts',(-72.4324372916884,16.7678226404189,0.));
#87063=CARTESIAN_POINT('Ctrl Pts',(-72.4324372916884,16.7678226404189,12.));
#87064=CARTESIAN_POINT('Ctrl Pts',(-72.4596690055347,16.7622901280741,0.));
#87065=CARTESIAN_POINT('Ctrl Pts',(-72.4596690055347,16.7622901280741,12.));
#87066=CARTESIAN_POINT('Ctrl Pts',(-72.4869297342051,16.7567261380614,0.));
#87067=CARTESIAN_POINT('Ctrl Pts',(-72.4869297342051,16.7567261380614,12.));
#87068=CARTESIAN_POINT('Ctrl Pts',(-72.5142194273203,16.7511306618794,0.));
#87069=CARTESIAN_POINT('Ctrl Pts',(-72.5142194273203,16.7511306618794,12.));
#87070=CARTESIAN_POINT('Ctrl Pts',(-72.5415380515905,16.7455036973724,0.));
#87071=CARTESIAN_POINT('Ctrl Pts',(-72.5415380515905,16.7455036973724,12.));
#87072=CARTESIAN_POINT('Ctrl Pts',(-72.563416080574,16.7409769365953,0.));
#87073=CARTESIAN_POINT('Ctrl Pts',(-72.563416080574,16.7409769365953,12.));
#87074=CARTESIAN_POINT('Ctrl Pts',(-72.5798376087405,16.7375676985272,0.));
#87075=CARTESIAN_POINT('Ctrl Pts',(-72.5798376087405,16.7375676985272,12.));
#87076=CARTESIAN_POINT('Ctrl Pts',(-72.5907910745874,16.7352885767459,0.));
#87077=CARTESIAN_POINT('Ctrl Pts',(-72.5907910745874,16.7352885767459,12.));
#87078=CARTESIAN_POINT('Ctrl Pts',(-72.5962692526112,16.7341474417545,0.));
#87079=CARTESIAN_POINT('Ctrl Pts',(-72.5962692526112,16.7341474417545,12.));
#87080=CARTESIAN_POINT('',(-67.8307641965654,17.2912529479484,0.));
#87081=CARTESIAN_POINT('Ctrl Pts',(-67.8307641965654,17.2912529479484,0.));
#87082=CARTESIAN_POINT('Ctrl Pts',(-67.8346476309018,17.2912149114119,0.));
#87083=CARTESIAN_POINT('Ctrl Pts',(-67.842419897098,17.2911366591348,0.));
#87084=CARTESIAN_POINT('Ctrl Pts',(-67.8540944889687,17.291012743109,0.));
#87085=CARTESIAN_POINT('Ctrl Pts',(-67.8696929978782,17.2908344459695,0.));
#87086=CARTESIAN_POINT('Ctrl Pts',(-67.8892451049608,17.2905897723949,0.));
#87087=CARTESIAN_POINT('Ctrl Pts',(-67.9088511496685,17.2903232740694,0.));
#87088=CARTESIAN_POINT('Ctrl Pts',(-67.9285110571741,17.2900349103981,0.));
#87089=CARTESIAN_POINT('Ctrl Pts',(-67.9482246901667,17.2897246158941,0.));
#87090=CARTESIAN_POINT('Ctrl Pts',(-67.9679918502579,17.2893923013894,0.));
#87091=CARTESIAN_POINT('Ctrl Pts',(-67.987812304921,17.2890378644866,0.));
#87092=CARTESIAN_POINT('Ctrl Pts',(-68.007685808115,17.2886611977401,0.));
#87093=CARTESIAN_POINT('Ctrl Pts',(-68.0276121227356,17.2882621974721,0.));
#87094=CARTESIAN_POINT('Ctrl Pts',(-68.0475910442424,17.2878407730961,0.));
#87095=CARTESIAN_POINT('Ctrl Pts',(-68.0676223930412,17.2873968440839,0.));
#87096=CARTESIAN_POINT('Ctrl Pts',(-68.0877060033205,17.2869303355432,0.));
#87097=CARTESIAN_POINT('Ctrl Pts',(-68.1078417137877,17.2864411745459,0.));
#87098=CARTESIAN_POINT('Ctrl Pts',(-68.1280293561511,17.2859292855705,0.));
#87099=CARTESIAN_POINT('Ctrl Pts',(-68.1482687493226,17.2853945882072,0.));
#87100=CARTESIAN_POINT('Ctrl Pts',(-68.1685597054231,17.2848369995293,0.));
#87101=CARTESIAN_POINT('Ctrl Pts',(-68.1889020335427,17.2842564355799,0.));
#87102=CARTESIAN_POINT('Ctrl Pts',(-68.2092955440567,17.2836528130819,0.));
#87103=CARTESIAN_POINT('Ctrl Pts',(-68.2297400535294,17.2830260513868,0.));
#87104=CARTESIAN_POINT('Ctrl Pts',(-68.2502353845071,17.2823760723874,0.));
#87105=CARTESIAN_POINT('Ctrl Pts',(-68.2707813631731,17.2817027995831,0.));
#87106=CARTESIAN_POINT('Ctrl Pts',(-68.2913778177261,17.2810061574353,0.));
#87107=CARTESIAN_POINT('Ctrl Pts',(-68.3120245763914,17.2802860705815,0.));
#87108=CARTESIAN_POINT('Ctrl Pts',(-68.3327214657575,17.2795424631799,0.));
#87109=CARTESIAN_POINT('Ctrl Pts',(-68.3534683116514,17.2787752592484,0.));
#87110=CARTESIAN_POINT('Ctrl Pts',(-68.3742649398964,17.2779843829608,0.));
#87111=CARTESIAN_POINT('Ctrl Pts',(-68.3951111770487,17.2771697589385,0.));
#87112=CARTESIAN_POINT('Ctrl Pts',(-68.4160068512753,17.2763313126018,0.));
#87113=CARTESIAN_POINT('Ctrl Pts',(-68.436951792677,17.2754689702992,0.));
#87114=CARTESIAN_POINT('Ctrl Pts',(-68.4579458328185,17.2745826591119,0.));
#87115=CARTESIAN_POINT('Ctrl Pts',(-68.4789888044351,17.2736723067365,0.));
#87116=CARTESIAN_POINT('Ctrl Pts',(-68.5000805410911,17.2727378413489,0.));
#87117=CARTESIAN_POINT('Ctrl Pts',(-68.521220876786,17.2717791914544,0.));
#87118=CARTESIAN_POINT('Ctrl Pts',(-68.5424096459772,17.2707962858919,0.));
#87119=CARTESIAN_POINT('Ctrl Pts',(-68.5636466837517,17.269789053896,0.));
#87120=CARTESIAN_POINT('Ctrl Pts',(-68.5849318259449,17.2687574251429,0.));
#87121=CARTESIAN_POINT('Ctrl Pts',(-68.6062649092764,17.2677013298057,0.));
#87122=CARTESIAN_POINT('Ctrl Pts',(-68.6276457714729,17.2666206986084,0.));
#87123=CARTESIAN_POINT('Ctrl Pts',(-68.6490742512057,17.2655154627928,0.));
#87124=CARTESIAN_POINT('Ctrl Pts',(-68.6705501880249,17.2643855540892,0.));
#87125=CARTESIAN_POINT('Ctrl Pts',(-68.6920734222938,17.2632309046892,0.));
#87126=CARTESIAN_POINT('Ctrl Pts',(-68.7136437951097,17.2620514472182,0.));
#87127=CARTESIAN_POINT('Ctrl Pts',(-68.7352611482547,17.2608471147185,0.));
#87128=CARTESIAN_POINT('Ctrl Pts',(-68.7569253242333,17.2596178406551,0.));
#87129=CARTESIAN_POINT('Ctrl Pts',(-68.7786361662882,17.2583635589198,0.));
#87130=CARTESIAN_POINT('Ctrl Pts',(-68.8003935184184,17.2570842038384,0.));
#87131=CARTESIAN_POINT('Ctrl Pts',(-68.8221972253941,17.2557797101813,0.));
#87132=CARTESIAN_POINT('Ctrl Pts',(-68.844047132755,17.2544500131625,0.));
#87133=CARTESIAN_POINT('Ctrl Pts',(-68.8659430867972,17.2530950484258,0.));
#87134=CARTESIAN_POINT('Ctrl Pts',(-68.8878849345557,17.2517147520376,0.));
#87135=CARTESIAN_POINT('Ctrl Pts',(-68.909872523787,17.2503090604792,0.));
#87136=CARTESIAN_POINT('Ctrl Pts',(-68.9319057029409,17.248877910643,0.));
#87137=CARTESIAN_POINT('Ctrl Pts',(-68.9539843211619,17.2474212398275,0.));
#87138=CARTESIAN_POINT('Ctrl Pts',(-68.9761082282922,17.2459389857327,0.));
#87139=CARTESIAN_POINT('Ctrl Pts',(-68.9982772748694,17.2444310864585,0.));
#87140=CARTESIAN_POINT('Ctrl Pts',(-69.0204913121225,17.2428974805044,0.));
#87141=CARTESIAN_POINT('Ctrl Pts',(-69.0427501919636,17.2413381067724,0.));
#87142=CARTESIAN_POINT('Ctrl Pts',(-69.065053766986,17.2397529045589,0.));
#87143=CARTESIAN_POINT('Ctrl Pts',(-69.0874018904598,17.2381418135491,0.));
#87144=CARTESIAN_POINT('Ctrl Pts',(-69.1097944163245,17.2365047738126,0.));
#87145=CARTESIAN_POINT('Ctrl Pts',(-69.1322311991752,17.2348417258015,0.));
#87146=CARTESIAN_POINT('Ctrl Pts',(-69.1547120942527,17.2331526103506,0.));
#87147=CARTESIAN_POINT('Ctrl Pts',(-69.1772369574447,17.2314373686701,0.));
#87148=CARTESIAN_POINT('Ctrl Pts',(-69.1998056452828,17.2296959423407,0.));
#87149=CARTESIAN_POINT('Ctrl Pts',(-69.222418014938,17.227928273312,0.));
#87150=CARTESIAN_POINT('Ctrl Pts',(-69.2450739242109,17.226134303902,0.));
#87151=CARTESIAN_POINT('Ctrl Pts',(-69.2677732315224,17.224313976797,0.));
#87152=CARTESIAN_POINT('Ctrl Pts',(-69.2905157959166,17.2224672350439,0.));
#87153=CARTESIAN_POINT('Ctrl Pts',(-69.3133014770554,17.2205940220459,0.));
#87154=CARTESIAN_POINT('Ctrl Pts',(-69.3361301352141,17.2186942815602,0.));
#87155=CARTESIAN_POINT('Ctrl Pts',(-69.3590016312692,17.2167679576984,0.));
#87156=CARTESIAN_POINT('Ctrl Pts',(-69.3819158266915,17.2148149949252,0.));
#87157=CARTESIAN_POINT('Ctrl Pts',(-69.404872583548,17.2128353380502,0.));
#87158=CARTESIAN_POINT('Ctrl Pts',(-69.4278717644973,17.2108289322254,0.));
#87159=CARTESIAN_POINT('Ctrl Pts',(-69.4509132327849,17.2087957229424,0.));
#87160=CARTESIAN_POINT('Ctrl Pts',(-69.4739968522313,17.2067356560337,0.));
#87161=CARTESIAN_POINT('Ctrl Pts',(-69.4971224872269,17.2046486776708,0.));
#87162=CARTESIAN_POINT('Ctrl Pts',(-69.5202900027367,17.2025347343577,0.));
#87163=CARTESIAN_POINT('Ctrl Pts',(-69.5434992642944,17.2003937729268,0.));
#87164=CARTESIAN_POINT('Ctrl Pts',(-69.5667501379969,17.1982257405377,0.));
#87165=CARTESIAN_POINT('Ctrl Pts',(-69.5900424904921,17.1960305846781,0.));
#87166=CARTESIAN_POINT('Ctrl Pts',(-69.6133761889749,17.1938082531612,0.));
#87167=CARTESIAN_POINT('Ctrl Pts',(-69.6367511011898,17.1915586941192,0.));
#87168=CARTESIAN_POINT('Ctrl Pts',(-69.6601670954269,17.1892818560003,0.));
#87169=CARTESIAN_POINT('Ctrl Pts',(-69.6836240405164,17.1869776875666,0.));
#87170=CARTESIAN_POINT('Ctrl Pts',(-69.7071218058178,17.1846461378973,0.));
#87171=CARTESIAN_POINT('Ctrl Pts',(-69.7306602612155,17.1822871563842,0.));
#87172=CARTESIAN_POINT('Ctrl Pts',(-69.7542392771234,17.179900692726,0.));
#87173=CARTESIAN_POINT('Ctrl Pts',(-69.777858724479,17.1774866969257,0.));
#87174=CARTESIAN_POINT('Ctrl Pts',(-69.8015184747398,17.1750451192886,0.));
#87175=CARTESIAN_POINT('Ctrl Pts',(-69.8252183998702,17.1725759104252,0.));
#87176=CARTESIAN_POINT('Ctrl Pts',(-69.8489583723407,17.1700790212474,0.));
#87177=CARTESIAN_POINT('Ctrl Pts',(-69.8727382651285,17.167554402962,0.));
#87178=CARTESIAN_POINT('Ctrl Pts',(-69.8965579517147,17.1650020070686,0.));
#87179=CARTESIAN_POINT('Ctrl Pts',(-69.9204173060781,17.1624217853578,0.));
#87180=CARTESIAN_POINT('Ctrl Pts',(-69.9443162026865,17.1598136899145,0.));
#87181=CARTESIAN_POINT('Ctrl Pts',(-69.9682545164939,17.157177673114,0.));
#87182=CARTESIAN_POINT('Ctrl Pts',(-69.9922321229424,17.1545136876161,0.));
#87183=CARTESIAN_POINT('Ctrl Pts',(-70.0162488979584,17.1518216863623,0.));
#87184=CARTESIAN_POINT('Ctrl Pts',(-70.0403047179483,17.1491016225749,0.));
#87185=CARTESIAN_POINT('Ctrl Pts',(-70.0643994597873,17.1463534497595,0.));
#87186=CARTESIAN_POINT('Ctrl Pts',(-70.0885330008179,17.1435771217018,0.));
#87187=CARTESIAN_POINT('Ctrl Pts',(-70.1127052188522,17.1407725924617,0.));
#87188=CARTESIAN_POINT('Ctrl Pts',(-70.1369159921687,17.1379398163709,0.));
#87189=CARTESIAN_POINT('Ctrl Pts',(-70.1611651995082,17.1350787480312,0.));
#87190=CARTESIAN_POINT('Ctrl Pts',(-70.1854527200631,17.1321893423182,0.));
#87191=CARTESIAN_POINT('Ctrl Pts',(-70.2097784334747,17.1292715543778,0.));
#87192=CARTESIAN_POINT('Ctrl Pts',(-70.2341422198363,17.1263253396202,0.));
#87193=CARTESIAN_POINT('Ctrl Pts',(-70.2585439596901,17.1233506537177,0.));
#87194=CARTESIAN_POINT('Ctrl Pts',(-70.2829835340238,17.1203474526031,0.));
#87195=CARTESIAN_POINT('Ctrl Pts',(-70.3074608242608,17.1173156924733,0.));
#87196=CARTESIAN_POINT('Ctrl Pts',(-70.3319757122568,17.1142553297867,0.));
#87197=CARTESIAN_POINT('Ctrl Pts',(-70.3565280803022,17.1111663212568,0.));
#87198=CARTESIAN_POINT('Ctrl Pts',(-70.3811178111201,17.1080486238499,0.));
#87199=CARTESIAN_POINT('Ctrl Pts',(-70.4057447878624,17.1049021947834,0.));
#87200=CARTESIAN_POINT('Ctrl Pts',(-70.430408894101,17.1017269915292,0.));
#87201=CARTESIAN_POINT('Ctrl Pts',(-70.4551100138238,17.0985229718125,0.));
#87202=CARTESIAN_POINT('Ctrl Pts',(-70.4798480314381,17.0952900936048,0.));
#87203=CARTESIAN_POINT('Ctrl Pts',(-70.5046228317677,17.0920283151219,0.));
#87204=CARTESIAN_POINT('Ctrl Pts',(-70.5294343000513,17.088737594822,0.));
#87205=CARTESIAN_POINT('Ctrl Pts',(-70.5542823219331,17.0854178914087,0.));
#87206=CARTESIAN_POINT('Ctrl Pts',(-70.5791667834582,17.082069163831,0.));
#87207=CARTESIAN_POINT('Ctrl Pts',(-70.6040875710749,17.0786913712764,0.));
#87208=CARTESIAN_POINT('Ctrl Pts',(-70.6290445716337,17.0752844731678,0.));
#87209=CARTESIAN_POINT('Ctrl Pts',(-70.6540376723841,17.0718484291624,0.));
#87210=CARTESIAN_POINT('Ctrl Pts',(-70.6790667609679,17.0683831991532,0.));
#87211=CARTESIAN_POINT('Ctrl Pts',(-70.7041317254125,17.0648887432714,0.));
#87212=CARTESIAN_POINT('Ctrl Pts',(-70.7292324541341,17.0613650218787,0.));
#87213=CARTESIAN_POINT('Ctrl Pts',(-70.7543688359374,17.0578119955649,0.));
#87214=CARTESIAN_POINT('Ctrl Pts',(-70.7795407600127,17.0542296251462,0.));
#87215=CARTESIAN_POINT('Ctrl Pts',(-70.8047481159306,17.0506178716664,0.));
#87216=CARTESIAN_POINT('Ctrl Pts',(-70.8299907936346,17.0469766964005,0.));
#87217=CARTESIAN_POINT('Ctrl Pts',(-70.8552686834435,17.0433060608479,0.));
#87218=CARTESIAN_POINT('Ctrl Pts',(-70.8805816760507,17.039605926728,0.));
#87219=CARTESIAN_POINT('Ctrl Pts',(-70.9059296625214,17.0358762559786,0.));
#87220=CARTESIAN_POINT('Ctrl Pts',(-70.9313125342872,17.0321170107562,0.));
#87221=CARTESIAN_POINT('Ctrl Pts',(-70.9567301831355,17.028328153439,0.));
#87222=CARTESIAN_POINT('Ctrl Pts',(-70.9821825012134,17.0245096466228,0.));
#87223=CARTESIAN_POINT('Ctrl Pts',(-71.0076693810302,17.0206614531166,0.));
#87224=CARTESIAN_POINT('Ctrl Pts',(-71.0331907154575,17.016783535942,0.));
#87225=CARTESIAN_POINT('Ctrl Pts',(-71.0587463977266,17.0128758583335,0.));
#87226=CARTESIAN_POINT('Ctrl Pts',(-71.0843363214216,17.0089383837437,0.));
#87227=CARTESIAN_POINT('Ctrl Pts',(-71.1099603804779,17.0049710758393,0.));
#87228=CARTESIAN_POINT('Ctrl Pts',(-71.1356184691799,17.0009738984935,0.));
#87229=CARTESIAN_POINT('Ctrl Pts',(-71.1613104821565,16.9969468157824,0.));
#87230=CARTESIAN_POINT('Ctrl Pts',(-71.1870363143742,16.9928897919829,0.));
#87231=CARTESIAN_POINT('Ctrl Pts',(-71.2127958611248,16.9888027915743,0.));
#87232=CARTESIAN_POINT('Ctrl Pts',(-71.2385890180233,16.9846857792385,0.));
#87233=CARTESIAN_POINT('Ctrl Pts',(-71.2644156810209,16.9805387198573,0.));
#87234=CARTESIAN_POINT('Ctrl Pts',(-71.2902757464127,16.9763615785138,0.));
#87235=CARTESIAN_POINT('Ctrl Pts',(-71.3161691108425,16.9721543204951,0.));
#87236=CARTESIAN_POINT('Ctrl Pts',(-71.3420956713072,16.9679169112993,0.));
#87237=CARTESIAN_POINT('Ctrl Pts',(-71.3680553251547,16.9636493166395,0.));
#87238=CARTESIAN_POINT('Ctrl Pts',(-71.3940479700662,16.9593515024274,0.));
#87239=CARTESIAN_POINT('Ctrl Pts',(-71.4200735040374,16.9550234347619,0.));
#87240=CARTESIAN_POINT('Ctrl Pts',(-71.4461318253561,16.9506650799189,0.));
#87241=CARTESIAN_POINT('Ctrl Pts',(-71.4722228325805,16.9462764043445,0.));
#87242=CARTESIAN_POINT('Ctrl Pts',(-71.4983464245069,16.9418573746492,0.));
#87243=CARTESIAN_POINT('Ctrl Pts',(-71.5245025002154,16.9374079576204,0.));
#87244=CARTESIAN_POINT('Ctrl Pts',(-71.5506909591139,16.9329281202379,0.));
#87245=CARTESIAN_POINT('Ctrl Pts',(-71.5769117009845,16.9284178296934,0.));
#87246=CARTESIAN_POINT('Ctrl Pts',(-71.6031646260169,16.923877053407,0.));
#87247=CARTESIAN_POINT('Ctrl Pts',(-71.6294496348644,16.9193057590605,0.));
#87248=CARTESIAN_POINT('Ctrl Pts',(-71.6557666285908,16.9147039145716,0.));
#87249=CARTESIAN_POINT('Ctrl Pts',(-71.6821155085605,16.9100714880367,0.));
#87250=CARTESIAN_POINT('Ctrl Pts',(-71.7084961763355,16.9054084476847,0.));
#87251=CARTESIAN_POINT('Ctrl Pts',(-71.7349085335796,16.9007147618344,0.));
#87252=CARTESIAN_POINT('Ctrl Pts',(-71.7613524819239,16.8959903988411,0.));
#87253=CARTESIAN_POINT('Ctrl Pts',(-71.7878279229556,16.8912353270944,0.));
#87254=CARTESIAN_POINT('Ctrl Pts',(-71.8143347584977,16.8864495151347,0.));
#87255=CARTESIAN_POINT('Ctrl Pts',(-71.8408728908269,16.8816329317473,0.));
#87256=CARTESIAN_POINT('Ctrl Pts',(-71.8674422229151,16.8767855460701,0.));
#87257=CARTESIAN_POINT('Ctrl Pts',(-71.8940426586521,16.8719073276967,0.));
#87258=CARTESIAN_POINT('Ctrl Pts',(-71.920674103086,16.8669982467915,0.));
#87259=CARTESIAN_POINT('Ctrl Pts',(-71.9473364618889,16.8620582738431,0.));
#87260=CARTESIAN_POINT('Ctrl Pts',(-71.9740296408319,16.8570873794264,0.));
#87261=CARTESIAN_POINT('Ctrl Pts',(-72.0007535452071,16.8520855339444,0.));
#87262=CARTESIAN_POINT('Ctrl Pts',(-72.0275080793742,16.8470527074278,0.));
#87263=CARTESIAN_POINT('Ctrl Pts',(-72.0542931459865,16.8419888691984,0.));
#87264=CARTESIAN_POINT('Ctrl Pts',(-72.0811086466178,16.8368939881457,0.));
#87265=CARTESIAN_POINT('Ctrl Pts',(-72.1079544831568,16.8317680333415,0.));
#87266=CARTESIAN_POINT('Ctrl Pts',(-72.1348305590233,16.8266109745802,0.));
#87267=CARTESIAN_POINT('Ctrl Pts',(-72.1617367803226,16.8214227828941,0.));
#87268=CARTESIAN_POINT('Ctrl Pts',(-72.1886730573389,16.8162034312257,0.));
#87269=CARTESIAN_POINT('Ctrl Pts',(-72.2156393048868,16.8109528945876,0.));
#87270=CARTESIAN_POINT('Ctrl Pts',(-72.2387802230662,16.8064254147767,0.));
#87271=CARTESIAN_POINT('Ctrl Pts',(-72.2565380035007,16.8029374213802,0.));
#87272=CARTESIAN_POINT('Ctrl Pts',(-72.2688994294958,16.8005027425889,0.));
#87273=CARTESIAN_POINT('Ctrl Pts',(-72.2758557890966,16.7991305317793,0.));
#87274=CARTESIAN_POINT('Ctrl Pts',(-72.2774028393482,16.7988252568807,0.));
#87275=CARTESIAN_POINT('',(-67.8307641965654,17.2912529479484,12.));
#87276=CARTESIAN_POINT('',(-67.8307641965654,17.2912529479484,0.));
#87277=CARTESIAN_POINT('Ctrl Pts',(-72.2774028393482,16.7988252568807,12.));
#87278=CARTESIAN_POINT('Ctrl Pts',(-72.2758557890966,16.7991305317793,12.));
#87279=CARTESIAN_POINT('Ctrl Pts',(-72.2688994294958,16.8005027425889,12.));
#87280=CARTESIAN_POINT('Ctrl Pts',(-72.2565380035007,16.8029374213802,12.));
#87281=CARTESIAN_POINT('Ctrl Pts',(-72.2387802230662,16.8064254147767,12.));
#87282=CARTESIAN_POINT('Ctrl Pts',(-72.2156393048868,16.8109528945876,12.));
#87283=CARTESIAN_POINT('Ctrl Pts',(-72.1886730573389,16.8162034312257,12.));
#87284=CARTESIAN_POINT('Ctrl Pts',(-72.1617367803226,16.8214227828941,12.));
#87285=CARTESIAN_POINT('Ctrl Pts',(-72.1348305590233,16.8266109745802,12.));
#87286=CARTESIAN_POINT('Ctrl Pts',(-72.1079544831568,16.8317680333415,12.));
#87287=CARTESIAN_POINT('Ctrl Pts',(-72.0811086466178,16.8368939881457,12.));
#87288=CARTESIAN_POINT('Ctrl Pts',(-72.0542931459865,16.8419888691984,12.));
#87289=CARTESIAN_POINT('Ctrl Pts',(-72.0275080793742,16.8470527074278,12.));
#87290=CARTESIAN_POINT('Ctrl Pts',(-72.0007535452071,16.8520855339444,12.));
#87291=CARTESIAN_POINT('Ctrl Pts',(-71.9740296408319,16.8570873794264,12.));
#87292=CARTESIAN_POINT('Ctrl Pts',(-71.9473364618889,16.8620582738431,12.));
#87293=CARTESIAN_POINT('Ctrl Pts',(-71.920674103086,16.8669982467915,12.));
#87294=CARTESIAN_POINT('Ctrl Pts',(-71.8940426586521,16.8719073276967,12.));
#87295=CARTESIAN_POINT('Ctrl Pts',(-71.8674422229151,16.8767855460701,12.));
#87296=CARTESIAN_POINT('Ctrl Pts',(-71.8408728908269,16.8816329317473,12.));
#87297=CARTESIAN_POINT('Ctrl Pts',(-71.8143347584977,16.8864495151347,12.));
#87298=CARTESIAN_POINT('Ctrl Pts',(-71.7878279229556,16.8912353270944,12.));
#87299=CARTESIAN_POINT('Ctrl Pts',(-71.7613524819239,16.8959903988411,12.));
#87300=CARTESIAN_POINT('Ctrl Pts',(-71.7349085335796,16.9007147618344,12.));
#87301=CARTESIAN_POINT('Ctrl Pts',(-71.7084961763355,16.9054084476847,12.));
#87302=CARTESIAN_POINT('Ctrl Pts',(-71.6821155085605,16.9100714880367,12.));
#87303=CARTESIAN_POINT('Ctrl Pts',(-71.6557666285908,16.9147039145716,12.));
#87304=CARTESIAN_POINT('Ctrl Pts',(-71.6294496348644,16.9193057590605,12.));
#87305=CARTESIAN_POINT('Ctrl Pts',(-71.6031646260169,16.923877053407,12.));
#87306=CARTESIAN_POINT('Ctrl Pts',(-71.5769117009845,16.9284178296934,12.));
#87307=CARTESIAN_POINT('Ctrl Pts',(-71.5506909591139,16.9329281202379,12.));
#87308=CARTESIAN_POINT('Ctrl Pts',(-71.5245025002154,16.9374079576204,12.));
#87309=CARTESIAN_POINT('Ctrl Pts',(-71.4983464245069,16.9418573746492,12.));
#87310=CARTESIAN_POINT('Ctrl Pts',(-71.4722228325805,16.9462764043445,12.));
#87311=CARTESIAN_POINT('Ctrl Pts',(-71.4461318253561,16.9506650799189,12.));
#87312=CARTESIAN_POINT('Ctrl Pts',(-71.4200735040374,16.9550234347619,12.));
#87313=CARTESIAN_POINT('Ctrl Pts',(-71.3940479700662,16.9593515024274,12.));
#87314=CARTESIAN_POINT('Ctrl Pts',(-71.3680553251547,16.9636493166395,12.));
#87315=CARTESIAN_POINT('Ctrl Pts',(-71.3420956713072,16.9679169112993,12.));
#87316=CARTESIAN_POINT('Ctrl Pts',(-71.3161691108425,16.9721543204951,12.));
#87317=CARTESIAN_POINT('Ctrl Pts',(-71.2902757464127,16.9763615785138,12.));
#87318=CARTESIAN_POINT('Ctrl Pts',(-71.2644156810209,16.9805387198573,12.));
#87319=CARTESIAN_POINT('Ctrl Pts',(-71.2385890180233,16.9846857792385,12.));
#87320=CARTESIAN_POINT('Ctrl Pts',(-71.2127958611248,16.9888027915743,12.));
#87321=CARTESIAN_POINT('Ctrl Pts',(-71.1870363143742,16.9928897919829,12.));
#87322=CARTESIAN_POINT('Ctrl Pts',(-71.1613104821565,16.9969468157824,12.));
#87323=CARTESIAN_POINT('Ctrl Pts',(-71.1356184691799,17.0009738984935,12.));
#87324=CARTESIAN_POINT('Ctrl Pts',(-71.1099603804779,17.0049710758393,12.));
#87325=CARTESIAN_POINT('Ctrl Pts',(-71.0843363214216,17.0089383837437,12.));
#87326=CARTESIAN_POINT('Ctrl Pts',(-71.0587463977266,17.0128758583335,12.));
#87327=CARTESIAN_POINT('Ctrl Pts',(-71.0331907154575,17.016783535942,12.));
#87328=CARTESIAN_POINT('Ctrl Pts',(-71.0076693810302,17.0206614531166,12.));
#87329=CARTESIAN_POINT('Ctrl Pts',(-70.9821825012134,17.0245096466228,12.));
#87330=CARTESIAN_POINT('Ctrl Pts',(-70.9567301831355,17.028328153439,12.));
#87331=CARTESIAN_POINT('Ctrl Pts',(-70.9313125342872,17.0321170107562,12.));
#87332=CARTESIAN_POINT('Ctrl Pts',(-70.9059296625214,17.0358762559786,12.));
#87333=CARTESIAN_POINT('Ctrl Pts',(-70.8805816760507,17.039605926728,12.));
#87334=CARTESIAN_POINT('Ctrl Pts',(-70.8552686834435,17.0433060608479,12.));
#87335=CARTESIAN_POINT('Ctrl Pts',(-70.8299907936346,17.0469766964005,12.));
#87336=CARTESIAN_POINT('Ctrl Pts',(-70.8047481159306,17.0506178716664,12.));
#87337=CARTESIAN_POINT('Ctrl Pts',(-70.7795407600127,17.0542296251462,12.));
#87338=CARTESIAN_POINT('Ctrl Pts',(-70.7543688359374,17.0578119955649,12.));
#87339=CARTESIAN_POINT('Ctrl Pts',(-70.7292324541341,17.0613650218787,12.));
#87340=CARTESIAN_POINT('Ctrl Pts',(-70.7041317254125,17.0648887432714,12.));
#87341=CARTESIAN_POINT('Ctrl Pts',(-70.6790667609679,17.0683831991532,12.));
#87342=CARTESIAN_POINT('Ctrl Pts',(-70.6540376723841,17.0718484291624,12.));
#87343=CARTESIAN_POINT('Ctrl Pts',(-70.6290445716337,17.0752844731678,12.));
#87344=CARTESIAN_POINT('Ctrl Pts',(-70.6040875710749,17.0786913712764,12.));
#87345=CARTESIAN_POINT('Ctrl Pts',(-70.5791667834582,17.082069163831,12.));
#87346=CARTESIAN_POINT('Ctrl Pts',(-70.5542823219331,17.0854178914087,12.));
#87347=CARTESIAN_POINT('Ctrl Pts',(-70.5294343000513,17.088737594822,12.));
#87348=CARTESIAN_POINT('Ctrl Pts',(-70.5046228317677,17.0920283151219,12.));
#87349=CARTESIAN_POINT('Ctrl Pts',(-70.4798480314381,17.0952900936048,12.));
#87350=CARTESIAN_POINT('Ctrl Pts',(-70.4551100138238,17.0985229718125,12.));
#87351=CARTESIAN_POINT('Ctrl Pts',(-70.430408894101,17.1017269915292,12.));
#87352=CARTESIAN_POINT('Ctrl Pts',(-70.4057447878624,17.1049021947834,12.));
#87353=CARTESIAN_POINT('Ctrl Pts',(-70.3811178111201,17.1080486238499,12.));
#87354=CARTESIAN_POINT('Ctrl Pts',(-70.3565280803022,17.1111663212568,12.));
#87355=CARTESIAN_POINT('Ctrl Pts',(-70.3319757122568,17.1142553297867,12.));
#87356=CARTESIAN_POINT('Ctrl Pts',(-70.3074608242608,17.1173156924733,12.));
#87357=CARTESIAN_POINT('Ctrl Pts',(-70.2829835340238,17.1203474526031,12.));
#87358=CARTESIAN_POINT('Ctrl Pts',(-70.2585439596901,17.1233506537177,12.));
#87359=CARTESIAN_POINT('Ctrl Pts',(-70.2341422198363,17.1263253396202,12.));
#87360=CARTESIAN_POINT('Ctrl Pts',(-70.2097784334747,17.1292715543778,12.));
#87361=CARTESIAN_POINT('Ctrl Pts',(-70.1854527200631,17.1321893423182,12.));
#87362=CARTESIAN_POINT('Ctrl Pts',(-70.1611651995082,17.1350787480312,12.));
#87363=CARTESIAN_POINT('Ctrl Pts',(-70.1369159921687,17.1379398163709,12.));
#87364=CARTESIAN_POINT('Ctrl Pts',(-70.1127052188522,17.1407725924617,12.));
#87365=CARTESIAN_POINT('Ctrl Pts',(-70.0885330008179,17.1435771217018,12.));
#87366=CARTESIAN_POINT('Ctrl Pts',(-70.0643994597873,17.1463534497595,12.));
#87367=CARTESIAN_POINT('Ctrl Pts',(-70.0403047179483,17.1491016225749,12.));
#87368=CARTESIAN_POINT('Ctrl Pts',(-70.0162488979584,17.1518216863623,12.));
#87369=CARTESIAN_POINT('Ctrl Pts',(-69.9922321229424,17.1545136876161,12.));
#87370=CARTESIAN_POINT('Ctrl Pts',(-69.9682545164939,17.157177673114,12.));
#87371=CARTESIAN_POINT('Ctrl Pts',(-69.9443162026865,17.1598136899145,12.));
#87372=CARTESIAN_POINT('Ctrl Pts',(-69.9204173060781,17.1624217853578,12.));
#87373=CARTESIAN_POINT('Ctrl Pts',(-69.8965579517147,17.1650020070686,12.));
#87374=CARTESIAN_POINT('Ctrl Pts',(-69.8727382651285,17.167554402962,12.));
#87375=CARTESIAN_POINT('Ctrl Pts',(-69.8489583723407,17.1700790212474,12.));
#87376=CARTESIAN_POINT('Ctrl Pts',(-69.8252183998702,17.1725759104252,12.));
#87377=CARTESIAN_POINT('Ctrl Pts',(-69.8015184747398,17.1750451192886,12.));
#87378=CARTESIAN_POINT('Ctrl Pts',(-69.777858724479,17.1774866969257,12.));
#87379=CARTESIAN_POINT('Ctrl Pts',(-69.7542392771234,17.179900692726,12.));
#87380=CARTESIAN_POINT('Ctrl Pts',(-69.7306602612155,17.1822871563842,12.));
#87381=CARTESIAN_POINT('Ctrl Pts',(-69.7071218058178,17.1846461378973,12.));
#87382=CARTESIAN_POINT('Ctrl Pts',(-69.6836240405164,17.1869776875666,12.));
#87383=CARTESIAN_POINT('Ctrl Pts',(-69.6601670954269,17.1892818560003,12.));
#87384=CARTESIAN_POINT('Ctrl Pts',(-69.6367511011898,17.1915586941192,12.));
#87385=CARTESIAN_POINT('Ctrl Pts',(-69.6133761889749,17.1938082531612,12.));
#87386=CARTESIAN_POINT('Ctrl Pts',(-69.5900424904921,17.1960305846781,12.));
#87387=CARTESIAN_POINT('Ctrl Pts',(-69.5667501379969,17.1982257405377,12.));
#87388=CARTESIAN_POINT('Ctrl Pts',(-69.5434992642944,17.2003937729268,12.));
#87389=CARTESIAN_POINT('Ctrl Pts',(-69.5202900027367,17.2025347343577,12.));
#87390=CARTESIAN_POINT('Ctrl Pts',(-69.4971224872269,17.2046486776708,12.));
#87391=CARTESIAN_POINT('Ctrl Pts',(-69.4739968522313,17.2067356560337,12.));
#87392=CARTESIAN_POINT('Ctrl Pts',(-69.4509132327849,17.2087957229424,12.));
#87393=CARTESIAN_POINT('Ctrl Pts',(-69.4278717644973,17.2108289322254,12.));
#87394=CARTESIAN_POINT('Ctrl Pts',(-69.404872583548,17.2128353380502,12.));
#87395=CARTESIAN_POINT('Ctrl Pts',(-69.3819158266915,17.2148149949252,12.));
#87396=CARTESIAN_POINT('Ctrl Pts',(-69.3590016312692,17.2167679576984,12.));
#87397=CARTESIAN_POINT('Ctrl Pts',(-69.3361301352141,17.2186942815602,12.));
#87398=CARTESIAN_POINT('Ctrl Pts',(-69.3133014770554,17.2205940220459,12.));
#87399=CARTESIAN_POINT('Ctrl Pts',(-69.2905157959166,17.2224672350439,12.));
#87400=CARTESIAN_POINT('Ctrl Pts',(-69.2677732315224,17.224313976797,12.));
#87401=CARTESIAN_POINT('Ctrl Pts',(-69.2450739242109,17.226134303902,12.));
#87402=CARTESIAN_POINT('Ctrl Pts',(-69.222418014938,17.227928273312,12.));
#87403=CARTESIAN_POINT('Ctrl Pts',(-69.1998056452828,17.2296959423407,12.));
#87404=CARTESIAN_POINT('Ctrl Pts',(-69.1772369574447,17.2314373686701,12.));
#87405=CARTESIAN_POINT('Ctrl Pts',(-69.1547120942527,17.2331526103506,12.));
#87406=CARTESIAN_POINT('Ctrl Pts',(-69.1322311991752,17.2348417258015,12.));
#87407=CARTESIAN_POINT('Ctrl Pts',(-69.1097944163245,17.2365047738126,12.));
#87408=CARTESIAN_POINT('Ctrl Pts',(-69.0874018904598,17.2381418135491,12.));
#87409=CARTESIAN_POINT('Ctrl Pts',(-69.065053766986,17.2397529045589,12.));
#87410=CARTESIAN_POINT('Ctrl Pts',(-69.0427501919636,17.2413381067724,12.));
#87411=CARTESIAN_POINT('Ctrl Pts',(-69.0204913121225,17.2428974805044,12.));
#87412=CARTESIAN_POINT('Ctrl Pts',(-68.9982772748694,17.2444310864585,12.));
#87413=CARTESIAN_POINT('Ctrl Pts',(-68.9761082282922,17.2459389857327,12.));
#87414=CARTESIAN_POINT('Ctrl Pts',(-68.9539843211619,17.2474212398275,12.));
#87415=CARTESIAN_POINT('Ctrl Pts',(-68.9319057029409,17.248877910643,12.));
#87416=CARTESIAN_POINT('Ctrl Pts',(-68.909872523787,17.2503090604792,12.));
#87417=CARTESIAN_POINT('Ctrl Pts',(-68.8878849345557,17.2517147520376,12.));
#87418=CARTESIAN_POINT('Ctrl Pts',(-68.8659430867972,17.2530950484258,12.));
#87419=CARTESIAN_POINT('Ctrl Pts',(-68.844047132755,17.2544500131625,12.));
#87420=CARTESIAN_POINT('Ctrl Pts',(-68.8221972253941,17.2557797101813,12.));
#87421=CARTESIAN_POINT('Ctrl Pts',(-68.8003935184184,17.2570842038384,12.));
#87422=CARTESIAN_POINT('Ctrl Pts',(-68.7786361662882,17.2583635589198,12.));
#87423=CARTESIAN_POINT('Ctrl Pts',(-68.7569253242333,17.2596178406551,12.));
#87424=CARTESIAN_POINT('Ctrl Pts',(-68.7352611482547,17.2608471147185,12.));
#87425=CARTESIAN_POINT('Ctrl Pts',(-68.7136437951097,17.2620514472182,12.));
#87426=CARTESIAN_POINT('Ctrl Pts',(-68.6920734222938,17.2632309046892,12.));
#87427=CARTESIAN_POINT('Ctrl Pts',(-68.6705501880249,17.2643855540892,12.));
#87428=CARTESIAN_POINT('Ctrl Pts',(-68.6490742512057,17.2655154627928,12.));
#87429=CARTESIAN_POINT('Ctrl Pts',(-68.6276457714729,17.2666206986084,12.));
#87430=CARTESIAN_POINT('Ctrl Pts',(-68.6062649092764,17.2677013298057,12.));
#87431=CARTESIAN_POINT('Ctrl Pts',(-68.5849318259449,17.2687574251429,12.));
#87432=CARTESIAN_POINT('Ctrl Pts',(-68.5636466837517,17.269789053896,12.));
#87433=CARTESIAN_POINT('Ctrl Pts',(-68.5424096459772,17.2707962858919,12.));
#87434=CARTESIAN_POINT('Ctrl Pts',(-68.521220876786,17.2717791914544,12.));
#87435=CARTESIAN_POINT('Ctrl Pts',(-68.5000805410911,17.2727378413489,12.));
#87436=CARTESIAN_POINT('Ctrl Pts',(-68.4789888044351,17.2736723067365,12.));
#87437=CARTESIAN_POINT('Ctrl Pts',(-68.4579458328185,17.2745826591119,12.));
#87438=CARTESIAN_POINT('Ctrl Pts',(-68.436951792677,17.2754689702992,12.));
#87439=CARTESIAN_POINT('Ctrl Pts',(-68.4160068512753,17.2763313126018,12.));
#87440=CARTESIAN_POINT('Ctrl Pts',(-68.3951111770487,17.2771697589385,12.));
#87441=CARTESIAN_POINT('Ctrl Pts',(-68.3742649398964,17.2779843829608,12.));
#87442=CARTESIAN_POINT('Ctrl Pts',(-68.3534683116514,17.2787752592484,12.));
#87443=CARTESIAN_POINT('Ctrl Pts',(-68.3327214657575,17.2795424631799,12.));
#87444=CARTESIAN_POINT('Ctrl Pts',(-68.3120245763914,17.2802860705815,12.));
#87445=CARTESIAN_POINT('Ctrl Pts',(-68.2913778177261,17.2810061574353,12.));
#87446=CARTESIAN_POINT('Ctrl Pts',(-68.2707813631731,17.2817027995831,12.));
#87447=CARTESIAN_POINT('Ctrl Pts',(-68.2502353845071,17.2823760723874,12.));
#87448=CARTESIAN_POINT('Ctrl Pts',(-68.2297400535294,17.2830260513868,12.));
#87449=CARTESIAN_POINT('Ctrl Pts',(-68.2092955440567,17.2836528130819,12.));
#87450=CARTESIAN_POINT('Ctrl Pts',(-68.1889020335427,17.2842564355799,12.));
#87451=CARTESIAN_POINT('Ctrl Pts',(-68.1685597054231,17.2848369995293,12.));
#87452=CARTESIAN_POINT('Ctrl Pts',(-68.1482687493226,17.2853945882072,12.));
#87453=CARTESIAN_POINT('Ctrl Pts',(-68.1280293561511,17.2859292855705,12.));
#87454=CARTESIAN_POINT('Ctrl Pts',(-68.1078417137877,17.2864411745459,12.));
#87455=CARTESIAN_POINT('Ctrl Pts',(-68.0877060033205,17.2869303355432,12.));
#87456=CARTESIAN_POINT('Ctrl Pts',(-68.0676223930412,17.2873968440839,12.));
#87457=CARTESIAN_POINT('Ctrl Pts',(-68.0475910442424,17.2878407730961,12.));
#87458=CARTESIAN_POINT('Ctrl Pts',(-68.0276121227356,17.2882621974721,12.));
#87459=CARTESIAN_POINT('Ctrl Pts',(-68.007685808115,17.2886611977401,12.));
#87460=CARTESIAN_POINT('Ctrl Pts',(-67.987812304921,17.2890378644866,12.));
#87461=CARTESIAN_POINT('Ctrl Pts',(-67.9679918502579,17.2893923013894,12.));
#87462=CARTESIAN_POINT('Ctrl Pts',(-67.9482246901667,17.2897246158941,12.));
#87463=CARTESIAN_POINT('Ctrl Pts',(-67.9285110571741,17.2900349103981,12.));
#87464=CARTESIAN_POINT('Ctrl Pts',(-67.9088511496685,17.2903232740694,12.));
#87465=CARTESIAN_POINT('Ctrl Pts',(-67.8892451049608,17.2905897723949,12.));
#87466=CARTESIAN_POINT('Ctrl Pts',(-67.8696929978782,17.2908344459695,12.));
#87467=CARTESIAN_POINT('Ctrl Pts',(-67.8540944889687,17.291012743109,12.));
#87468=CARTESIAN_POINT('Ctrl Pts',(-67.842419897098,17.2911366591348,12.));
#87469=CARTESIAN_POINT('Ctrl Pts',(-67.8346476309018,17.2912149114119,12.));
#87470=CARTESIAN_POINT('Ctrl Pts',(-67.8307641965654,17.2912529479484,12.));
#87471=CARTESIAN_POINT('Ctrl Pts',(-72.6050633494711,15.320844207742,-1.11022302462516E-15));
#87472=CARTESIAN_POINT('Ctrl Pts',(-72.6050633494711,15.320844207742,4.));
#87473=CARTESIAN_POINT('Ctrl Pts',(-72.6050633494711,15.320844207742,8.));
#87474=CARTESIAN_POINT('Ctrl Pts',(-72.6050633494711,15.320844207742,12.));
#87475=CARTESIAN_POINT('Ctrl Pts',(-72.6937764817667,15.3856835210418,-1.11022302462516E-15));
#87476=CARTESIAN_POINT('Ctrl Pts',(-72.6937764817667,15.3856835210418,4.));
#87477=CARTESIAN_POINT('Ctrl Pts',(-72.6937764817667,15.3856835210418,8.00000000000001));
#87478=CARTESIAN_POINT('Ctrl Pts',(-72.6937764817667,15.3856835210418,12.));
#87479=CARTESIAN_POINT('Ctrl Pts',(-72.8096834307708,15.5519317750286,-1.11022302462516E-15));
#87480=CARTESIAN_POINT('Ctrl Pts',(-72.8096834307708,15.5519317750286,4.));
#87481=CARTESIAN_POINT('Ctrl Pts',(-72.8096834307708,15.5519317750286,7.99999999999999));
#87482=CARTESIAN_POINT('Ctrl Pts',(-72.8096834307708,15.5519317750286,12.));
#87483=CARTESIAN_POINT('Ctrl Pts',(-72.8161171750014,15.7502340068143,-1.11022302462516E-15));
#87484=CARTESIAN_POINT('Ctrl Pts',(-72.8161171750014,15.7502340068143,4.));
#87485=CARTESIAN_POINT('Ctrl Pts',(-72.8161171750014,15.7502340068143,8.00000000000001));
#87486=CARTESIAN_POINT('Ctrl Pts',(-72.8161171750014,15.7502340068143,12.));
#87487=CARTESIAN_POINT('Ctrl Pts',(-72.7986051948036,15.830763774723,-1.11022302462516E-15));
#87488=CARTESIAN_POINT('Ctrl Pts',(-72.7986051948036,15.830763774723,4.));
#87489=CARTESIAN_POINT('Ctrl Pts',(-72.7986051948036,15.830763774723,8.));
#87490=CARTESIAN_POINT('Ctrl Pts',(-72.7986051948036,15.830763774723,12.));
#87491=CARTESIAN_POINT('',(-72.6050633494711,15.320844207742,0.));
#87492=CARTESIAN_POINT('',(-72.7986051948038,15.8307637747231,-2.77555756156289E-16));
#87493=CARTESIAN_POINT('Ctrl Pts',(-72.6050633494711,15.320844207742,0.));
#87494=CARTESIAN_POINT('Ctrl Pts',(-72.6937764817667,15.3856835210418,-3.08148791101957E-31));
#87495=CARTESIAN_POINT('Ctrl Pts',(-72.7600090240548,15.48068252332,3.08148791101958E-31));
#87496=CARTESIAN_POINT('Ctrl Pts',(-72.7904952137637,15.5861481305937,2.18952885050753E-46));
#87497=CARTESIAN_POINT('Ctrl Pts',(-72.8133598560454,15.665247336049,-1.54074395550979E-31));
#87498=CARTESIAN_POINT('Ctrl Pts',(-72.8161171750014,15.7502340068143,-9.24446373305873E-31));
#87499=CARTESIAN_POINT('Ctrl Pts',(-72.7986051948036,15.830763774723,-1.09476442525376E-46));
#87500=CARTESIAN_POINT('',(-72.7986051948038,15.8307637747231,12.));
#87501=CARTESIAN_POINT('Ctrl Pts',(-72.7986051948036,15.830763774723,-1.11022302462516E-15));
#87502=CARTESIAN_POINT('Ctrl Pts',(-72.7986051948036,15.830763774723,4.));
#87503=CARTESIAN_POINT('Ctrl Pts',(-72.7986051948036,15.830763774723,8.));
#87504=CARTESIAN_POINT('Ctrl Pts',(-72.7986051948036,15.830763774723,12.));
#87505=CARTESIAN_POINT('',(-72.6050633494711,15.320844207742,12.));
#87506=CARTESIAN_POINT('Ctrl Pts',(-72.7986051948036,15.830763774723,12.));
#87507=CARTESIAN_POINT('Ctrl Pts',(-72.8161171750014,15.7502340068143,12.));
#87508=CARTESIAN_POINT('Ctrl Pts',(-72.8133598560454,15.665247336049,12.));
#87509=CARTESIAN_POINT('Ctrl Pts',(-72.7904952137637,15.5861481305937,12.));
#87510=CARTESIAN_POINT('Ctrl Pts',(-72.7600090240548,15.48068252332,12.));
#87511=CARTESIAN_POINT('Ctrl Pts',(-72.6937764817667,15.3856835210418,12.));
#87512=CARTESIAN_POINT('Ctrl Pts',(-72.6050633494711,15.320844207742,12.));
#87513=CARTESIAN_POINT('Ctrl Pts',(-72.6050633494711,15.320844207742,12.));
#87514=CARTESIAN_POINT('Ctrl Pts',(-72.6050633494711,15.320844207742,8.));
#87515=CARTESIAN_POINT('Ctrl Pts',(-72.6050633494711,15.320844207742,4.));
#87516=CARTESIAN_POINT('Ctrl Pts',(-72.6050633494711,15.320844207742,-1.11022302462516E-15));
#87517=CARTESIAN_POINT('Origin',(-3.65979954444617E-10,8.10341340518592E-11,
0.));
#87518=CARTESIAN_POINT('Origin',(-3.65979954444617E-10,8.10341340518592E-11,
12.));
#87519=CARTESIAN_POINT('Origin',(-3.65979954444617E-10,8.10341340518592E-11,
0.));
#87520=CARTESIAN_POINT('Ctrl Pts',(-70.9608233461363,22.6894590071785,0.));
#87521=CARTESIAN_POINT('Ctrl Pts',(-70.9608233461363,22.6894590071785,4.));
#87522=CARTESIAN_POINT('Ctrl Pts',(-70.9608233461364,22.6894590071785,8.));
#87523=CARTESIAN_POINT('Ctrl Pts',(-70.9608233461364,22.6894590071785,12.));
#87524=CARTESIAN_POINT('Ctrl Pts',(-70.9273579271571,22.7941214270114,0.));
#87525=CARTESIAN_POINT('Ctrl Pts',(-70.9273579271571,22.7941214270114,4.));
#87526=CARTESIAN_POINT('Ctrl Pts',(-70.9273579271571,22.7941214270114,8.00000000000001));
#87527=CARTESIAN_POINT('Ctrl Pts',(-70.9273579271571,22.7941214270114,12.));
#87528=CARTESIAN_POINT('Ctrl Pts',(-70.8062825417802,22.9566438338675,0.));
#87529=CARTESIAN_POINT('Ctrl Pts',(-70.8062825417802,22.9566438338675,4.));
#87530=CARTESIAN_POINT('Ctrl Pts',(-70.8062825417802,22.9566438338675,7.99999999999999));
#87531=CARTESIAN_POINT('Ctrl Pts',(-70.8062825417802,22.9566438338675,12.));
#87532=CARTESIAN_POINT('Ctrl Pts',(-70.6201870200062,23.0254444386656,0.));
#87533=CARTESIAN_POINT('Ctrl Pts',(-70.6201870200062,23.0254444386656,4.));
#87534=CARTESIAN_POINT('Ctrl Pts',(-70.6201870200063,23.0254444386655,8.00000000000001));
#87535=CARTESIAN_POINT('Ctrl Pts',(-70.6201870200063,23.0254444386655,12.));
#87536=CARTESIAN_POINT('Ctrl Pts',(-70.5382514078488,23.0342913834094,0.));
#87537=CARTESIAN_POINT('Ctrl Pts',(-70.5382514078488,23.0342913834094,4.));
#87538=CARTESIAN_POINT('Ctrl Pts',(-70.5382514078489,23.0342913834093,8.));
#87539=CARTESIAN_POINT('Ctrl Pts',(-70.5382514078489,23.0342913834093,12.));
#87540=CARTESIAN_POINT('',(-70.9608233461363,22.6894590071785,0.));
#87541=CARTESIAN_POINT('',(-70.5382514078488,23.0342913834093,0.));
#87542=CARTESIAN_POINT('Ctrl Pts',(-70.9608233461363,22.6894590071785,0.));
#87543=CARTESIAN_POINT('Ctrl Pts',(-70.9273579271571,22.7941214270114,0.));
#87544=CARTESIAN_POINT('Ctrl Pts',(-70.858171992656,22.8869913737863,0.));
#87545=CARTESIAN_POINT('Ctrl Pts',(-70.767754993209,22.9492582831545,0.));
#87546=CARTESIAN_POINT('Ctrl Pts',(-70.6999422436237,22.9959584651807,0.));
#87547=CARTESIAN_POINT('Ctrl Pts',(-70.6201870200062,23.0254444386656,0.));
#87548=CARTESIAN_POINT('Ctrl Pts',(-70.5382514078488,23.0342913834094,0.));
#87549=CARTESIAN_POINT('',(-70.5382514078489,23.0342913834093,12.));
#87550=CARTESIAN_POINT('Ctrl Pts',(-70.5382514078488,23.0342913834094,0.));
#87551=CARTESIAN_POINT('Ctrl Pts',(-70.5382514078488,23.0342913834094,4.));
#87552=CARTESIAN_POINT('Ctrl Pts',(-70.5382514078489,23.0342913834093,8.));
#87553=CARTESIAN_POINT('Ctrl Pts',(-70.5382514078489,23.0342913834093,12.));
#87554=CARTESIAN_POINT('',(-70.9608233461364,22.6894590071785,12.));
#87555=CARTESIAN_POINT('Ctrl Pts',(-70.5382514078489,23.0342913834093,12.));
#87556=CARTESIAN_POINT('Ctrl Pts',(-70.6201870200063,23.0254444386655,12.));
#87557=CARTESIAN_POINT('Ctrl Pts',(-70.6999422436237,22.9959584651806,12.));
#87558=CARTESIAN_POINT('Ctrl Pts',(-70.767754993209,22.9492582831545,12.));
#87559=CARTESIAN_POINT('Ctrl Pts',(-70.858171992656,22.8869913737863,12.));
#87560=CARTESIAN_POINT('Ctrl Pts',(-70.9273579271571,22.7941214270114,12.));
#87561=CARTESIAN_POINT('Ctrl Pts',(-70.9608233461364,22.6894590071785,12.));
#87562=CARTESIAN_POINT('Ctrl Pts',(-70.9608233461364,22.6894590071785,12.));
#87563=CARTESIAN_POINT('Ctrl Pts',(-70.9608233461364,22.6894590071785,8.));
#87564=CARTESIAN_POINT('Ctrl Pts',(-70.9608233461363,22.6894590071785,4.));
#87565=CARTESIAN_POINT('Ctrl Pts',(-70.9608233461363,22.6894590071785,0.));
#87566=CARTESIAN_POINT('Ctrl Pts',(-66.0656156664138,23.1372951448024,0.));
#87567=CARTESIAN_POINT('Ctrl Pts',(-66.0656156664138,23.1372951448024,12.));
#87568=CARTESIAN_POINT('Ctrl Pts',(-66.0694876382127,23.1375957166104,0.));
#87569=CARTESIAN_POINT('Ctrl Pts',(-66.0694876382127,23.1375957166104,12.));
#87570=CARTESIAN_POINT('Ctrl Pts',(-66.0772371487248,23.13819515974,0.));
#87571=CARTESIAN_POINT('Ctrl Pts',(-66.0772371487248,23.13819515974,12.));
#87572=CARTESIAN_POINT('Ctrl Pts',(-66.0888781152421,23.1390892229778,0.));
#87573=CARTESIAN_POINT('Ctrl Pts',(-66.0888781152421,23.1390892229778,12.));
#87574=CARTESIAN_POINT('Ctrl Pts',(-66.1044328067355,23.1402711039425,0.));
#87575=CARTESIAN_POINT('Ctrl Pts',(-66.1044328067355,23.1402711039425,12.));
#87576=CARTESIAN_POINT('Ctrl Pts',(-66.1239318368548,23.1417314398398,0.));
#87577=CARTESIAN_POINT('Ctrl Pts',(-66.1239318368548,23.1417314398398,12.));
#87578=CARTESIAN_POINT('Ctrl Pts',(-66.1434865015027,23.1431747350098,0.));
#87579=CARTESIAN_POINT('Ctrl Pts',(-66.1434865015027,23.1431747350098,12.));
#87580=CARTESIAN_POINT('Ctrl Pts',(-66.1630967296747,23.1446009424903,0.));
#87581=CARTESIAN_POINT('Ctrl Pts',(-66.1630967296747,23.1446009424903,12.));
#87582=CARTESIAN_POINT('Ctrl Pts',(-66.18276239029,23.1460099850763,0.));
#87583=CARTESIAN_POINT('Ctrl Pts',(-66.18276239029,23.1460099850763,12.));
#87584=CARTESIAN_POINT('Ctrl Pts',(-66.2024832934866,23.1474017566484,0.));
#87585=CARTESIAN_POINT('Ctrl Pts',(-66.2024832934866,23.1474017566484,12.));
#87586=CARTESIAN_POINT('Ctrl Pts',(-66.2222592165473,23.1487761349328,0.));
#87587=CARTESIAN_POINT('Ctrl Pts',(-66.2222592165473,23.1487761349328,12.));
#87588=CARTESIAN_POINT('Ctrl Pts',(-66.2420899237317,23.1501329914488,0.));
#87589=CARTESIAN_POINT('Ctrl Pts',(-66.2420899237317,23.1501329914488,12.));
#87590=CARTESIAN_POINT('Ctrl Pts',(-66.2619751878741,23.1514722022483,0.));
#87591=CARTESIAN_POINT('Ctrl Pts',(-66.2619751878741,23.1514722022483,12.));
#87592=CARTESIAN_POINT('Ctrl Pts',(-66.2819148131072,23.1527936592625,0.));
#87593=CARTESIAN_POINT('Ctrl Pts',(-66.2819148131072,23.1527936592625,12.));
#87594=CARTESIAN_POINT('Ctrl Pts',(-66.301908627539,23.154097266617,0.));
#87595=CARTESIAN_POINT('Ctrl Pts',(-66.301908627539,23.154097266617,12.));
#87596=CARTESIAN_POINT('Ctrl Pts',(-66.3219564725161,23.1553829352531,0.));
#87597=CARTESIAN_POINT('Ctrl Pts',(-66.3219564725161,23.1553829352531,12.));
#87598=CARTESIAN_POINT('Ctrl Pts',(-66.3420581937159,23.1566505784626,0.));
#87599=CARTESIAN_POINT('Ctrl Pts',(-66.3420581937159,23.1566505784626,12.));
#87600=CARTESIAN_POINT('Ctrl Pts',(-66.3622136300692,23.1579001063438,0.));
#87601=CARTESIAN_POINT('Ctrl Pts',(-66.3622136300692,23.1579001063438,12.));
#87602=CARTESIAN_POINT('Ctrl Pts',(-66.382422608185,23.15913142301,0.));
#87603=CARTESIAN_POINT('Ctrl Pts',(-66.382422608185,23.15913142301,12.));
#87604=CARTESIAN_POINT('Ctrl Pts',(-66.402684948127,23.1603444294754,0.));
#87605=CARTESIAN_POINT('Ctrl Pts',(-66.402684948127,23.1603444294754,12.));
#87606=CARTESIAN_POINT('Ctrl Pts',(-66.4230004670288,23.1615390254635,0.));
#87607=CARTESIAN_POINT('Ctrl Pts',(-66.4230004670288,23.1615390254635,12.));
#87608=CARTESIAN_POINT('Ctrl Pts',(-66.4433689832454,23.1627151114875,0.));
#87609=CARTESIAN_POINT('Ctrl Pts',(-66.4433689832454,23.1627151114875,12.));
#87610=CARTESIAN_POINT('Ctrl Pts',(-66.4637903210682,23.163872591218,0.));
#87611=CARTESIAN_POINT('Ctrl Pts',(-66.4637903210682,23.163872591218,12.));
#87612=CARTESIAN_POINT('Ctrl Pts',(-66.4842643105263,23.1650113713792,0.));
#87613=CARTESIAN_POINT('Ctrl Pts',(-66.4842643105263,23.1650113713792,12.));
#87614=CARTESIAN_POINT('Ctrl Pts',(-66.5047907851319,23.1661313606123,0.));
#87615=CARTESIAN_POINT('Ctrl Pts',(-66.5047907851319,23.1661313606123,12.));
#87616=CARTESIAN_POINT('Ctrl Pts',(-66.5253695803209,23.1672324686927,0.));
#87617=CARTESIAN_POINT('Ctrl Pts',(-66.5253695803209,23.1672324686927,12.));
#87618=CARTESIAN_POINT('Ctrl Pts',(-66.5460005315406,23.1683146055736,0.));
#87619=CARTESIAN_POINT('Ctrl Pts',(-66.5460005315406,23.1683146055736,12.));
#87620=CARTESIAN_POINT('Ctrl Pts',(-66.5666834726495,23.169377680588,0.));
#87621=CARTESIAN_POINT('Ctrl Pts',(-66.5666834726495,23.169377680588,12.));
#87622=CARTESIAN_POINT('Ctrl Pts',(-66.5874182367597,23.1704216028626,0.));
#87623=CARTESIAN_POINT('Ctrl Pts',(-66.5874182367597,23.1704216028626,12.));
#87624=CARTESIAN_POINT('Ctrl Pts',(-66.6082046569657,23.1714462816794,0.));
#87625=CARTESIAN_POINT('Ctrl Pts',(-66.6082046569657,23.1714462816794,12.));
#87626=CARTESIAN_POINT('Ctrl Pts',(-66.6290425670538,23.1724516268299,0.));
#87627=CARTESIAN_POINT('Ctrl Pts',(-66.6290425670538,23.1724516268299,12.));
#87628=CARTESIAN_POINT('Ctrl Pts',(-66.6499318023445,23.1734375490421,0.));
#87629=CARTESIAN_POINT('Ctrl Pts',(-66.6499318023445,23.1734375490421,12.));
#87630=CARTESIAN_POINT('Ctrl Pts',(-66.6708722000047,23.174403960137,0.));
#87631=CARTESIAN_POINT('Ctrl Pts',(-66.6708722000047,23.174403960137,12.));
#87632=CARTESIAN_POINT('Ctrl Pts',(-66.691863598595,23.1753507727931,0.));
#87633=CARTESIAN_POINT('Ctrl Pts',(-66.691863598595,23.1753507727931,12.));
#87634=CARTESIAN_POINT('Ctrl Pts',(-66.712905837789,23.1762779004043,0.));
#87635=CARTESIAN_POINT('Ctrl Pts',(-66.712905837789,23.1762779004043,12.));
#87636=CARTESIAN_POINT('Ctrl Pts',(-66.7339987580441,23.1771852569136,0.));
#87637=CARTESIAN_POINT('Ctrl Pts',(-66.7339987580441,23.1771852569136,12.));
#87638=CARTESIAN_POINT('Ctrl Pts',(-66.7551422002229,23.1780727566309,0.));
#87639=CARTESIAN_POINT('Ctrl Pts',(-66.7551422002229,23.1780727566309,12.));
#87640=CARTESIAN_POINT('Ctrl Pts',(-66.7763360056146,23.1789403142375,0.));
#87641=CARTESIAN_POINT('Ctrl Pts',(-66.7763360056146,23.1789403142375,12.));
#87642=CARTESIAN_POINT('Ctrl Pts',(-66.7975800161014,23.1797878448645,0.));
#87643=CARTESIAN_POINT('Ctrl Pts',(-66.7975800161014,23.1797878448645,12.));
#87644=CARTESIAN_POINT('Ctrl Pts',(-66.8188740742727,23.1806152641475,0.));
#87645=CARTESIAN_POINT('Ctrl Pts',(-66.8188740742727,23.1806152641475,12.));
#87646=CARTESIAN_POINT('Ctrl Pts',(-66.840218023555,23.1814224882948,0.));
#87647=CARTESIAN_POINT('Ctrl Pts',(-66.840218023555,23.1814224882948,12.));
#87648=CARTESIAN_POINT('Ctrl Pts',(-66.8616117083304,23.1822094341508,0.));
#87649=CARTESIAN_POINT('Ctrl Pts',(-66.8616117083304,23.1822094341508,12.));
#87650=CARTESIAN_POINT('Ctrl Pts',(-66.8830549738768,23.1829760191582,0.));
#87651=CARTESIAN_POINT('Ctrl Pts',(-66.8830549738768,23.1829760191582,12.));
#87652=CARTESIAN_POINT('Ctrl Pts',(-66.904547666305,23.1837221613231,0.));
#87653=CARTESIAN_POINT('Ctrl Pts',(-66.904547666305,23.1837221613231,12.));
#87654=CARTESIAN_POINT('Ctrl Pts',(-66.9260896324955,23.1844477791816,0.));
#87655=CARTESIAN_POINT('Ctrl Pts',(-66.9260896324955,23.1844477791816,12.));
#87656=CARTESIAN_POINT('Ctrl Pts',(-66.9476807200225,23.1851527917665,0.));
#87657=CARTESIAN_POINT('Ctrl Pts',(-66.9476807200225,23.1851527917665,12.));
#87658=CARTESIAN_POINT('Ctrl Pts',(-66.9693207771059,23.1858371185852,0.));
#87659=CARTESIAN_POINT('Ctrl Pts',(-66.9693207771059,23.1858371185852,12.));
#87660=CARTESIAN_POINT('Ctrl Pts',(-66.9910096526483,23.1865006796291,0.));
#87661=CARTESIAN_POINT('Ctrl Pts',(-66.9910096526483,23.1865006796291,12.));
#87662=CARTESIAN_POINT('Ctrl Pts',(-67.0127471962507,23.1871433953795,0.));
#87663=CARTESIAN_POINT('Ctrl Pts',(-67.0127471962507,23.1871433953795,12.));
#87664=CARTESIAN_POINT('Ctrl Pts',(-67.0345332582297,23.1877651868155,0.));
#87665=CARTESIAN_POINT('Ctrl Pts',(-67.0345332582297,23.1877651868155,12.));
#87666=CARTESIAN_POINT('Ctrl Pts',(-67.0563676896312,23.1883659754267,0.));
#87667=CARTESIAN_POINT('Ctrl Pts',(-67.0563676896312,23.1883659754267,12.));
#87668=CARTESIAN_POINT('Ctrl Pts',(-67.0782503422293,23.1889456832115,0.));
#87669=CARTESIAN_POINT('Ctrl Pts',(-67.0782503422293,23.1889456832115,12.));
#87670=CARTESIAN_POINT('Ctrl Pts',(-67.1001810685138,23.1895042326625,0.));
#87671=CARTESIAN_POINT('Ctrl Pts',(-67.1001810685138,23.1895042326625,12.));
#87672=CARTESIAN_POINT('Ctrl Pts',(-67.122159721674,23.1900415467574,0.));
#87673=CARTESIAN_POINT('Ctrl Pts',(-67.122159721674,23.1900415467574,12.));
#87674=CARTESIAN_POINT('Ctrl Pts',(-67.1441861555819,23.1905575489505,0.));
#87675=CARTESIAN_POINT('Ctrl Pts',(-67.1441861555819,23.1905575489505,12.));
#87676=CARTESIAN_POINT('Ctrl Pts',(-67.1662602247641,23.1910521631658,0.));
#87677=CARTESIAN_POINT('Ctrl Pts',(-67.1662602247641,23.1910521631658,12.));
#87678=CARTESIAN_POINT('Ctrl Pts',(-67.1883817844039,23.1915253137923,0.));
#87679=CARTESIAN_POINT('Ctrl Pts',(-67.1883817844039,23.1915253137923,12.));
#87680=CARTESIAN_POINT('Ctrl Pts',(-67.2105506903448,23.1919769256803,0.));
#87681=CARTESIAN_POINT('Ctrl Pts',(-67.2105506903448,23.1919769256803,12.));
#87682=CARTESIAN_POINT('Ctrl Pts',(-67.232766799088,23.1924069241385,0.));
#87683=CARTESIAN_POINT('Ctrl Pts',(-67.232766799088,23.1924069241385,12.));
#87684=CARTESIAN_POINT('Ctrl Pts',(-67.2550299677888,23.1928152349343,0.));
#87685=CARTESIAN_POINT('Ctrl Pts',(-67.2550299677888,23.1928152349343,12.));
#87686=CARTESIAN_POINT('Ctrl Pts',(-67.2773400542477,23.1932017842954,0.));
#87687=CARTESIAN_POINT('Ctrl Pts',(-67.2773400542477,23.1932017842954,12.));
#87688=CARTESIAN_POINT('Ctrl Pts',(-67.2996969169099,23.193566498902,0.));
#87689=CARTESIAN_POINT('Ctrl Pts',(-67.2996969169099,23.193566498902,12.));
#87690=CARTESIAN_POINT('Ctrl Pts',(-67.3221004148604,23.1939093058802,0.));
#87691=CARTESIAN_POINT('Ctrl Pts',(-67.3221004148604,23.1939093058802,12.));
#87692=CARTESIAN_POINT('Ctrl Pts',(-67.3445504078178,23.1942301327979,0.));
#87693=CARTESIAN_POINT('Ctrl Pts',(-67.3445504078178,23.1942301327979,12.));
#87694=CARTESIAN_POINT('Ctrl Pts',(-67.3670467561205,23.1945289076608,0.));
#87695=CARTESIAN_POINT('Ctrl Pts',(-67.3670467561205,23.1945289076608,12.));
#87696=CARTESIAN_POINT('Ctrl Pts',(-67.3895893207168,23.1948055589123,0.));
#87697=CARTESIAN_POINT('Ctrl Pts',(-67.3895893207168,23.1948055589123,12.));
#87698=CARTESIAN_POINT('Ctrl Pts',(-67.4121779631666,23.1950600154259,0.));
#87699=CARTESIAN_POINT('Ctrl Pts',(-67.4121779631666,23.1950600154259,12.));
#87700=CARTESIAN_POINT('Ctrl Pts',(-67.4348125456389,23.1952922065009,0.));
#87701=CARTESIAN_POINT('Ctrl Pts',(-67.4348125456389,23.1952922065009,12.));
#87702=CARTESIAN_POINT('Ctrl Pts',(-67.4574929309079,23.1955020618591,0.));
#87703=CARTESIAN_POINT('Ctrl Pts',(-67.4574929309079,23.1955020618591,12.));
#87704=CARTESIAN_POINT('Ctrl Pts',(-67.4802189823424,23.1956895116446,0.));
#87705=CARTESIAN_POINT('Ctrl Pts',(-67.4802189823424,23.1956895116446,12.));
#87706=CARTESIAN_POINT('Ctrl Pts',(-67.5029905638974,23.1958544864224,0.));
#87707=CARTESIAN_POINT('Ctrl Pts',(-67.5029905638974,23.1958544864224,12.));
#87708=CARTESIAN_POINT('Ctrl Pts',(-67.525807540117,23.1959969171709,0.));
#87709=CARTESIAN_POINT('Ctrl Pts',(-67.525807540117,23.1959969171709,12.));
#87710=CARTESIAN_POINT('Ctrl Pts',(-67.5486697761301,23.1961167352776,0.));
#87711=CARTESIAN_POINT('Ctrl Pts',(-67.5486697761301,23.1961167352776,12.));
#87712=CARTESIAN_POINT('Ctrl Pts',(-67.5715771376454,23.1962138725358,0.));
#87713=CARTESIAN_POINT('Ctrl Pts',(-67.5715771376454,23.1962138725358,12.));
#87714=CARTESIAN_POINT('Ctrl Pts',(-67.5945294909398,23.1962882611443,0.));
#87715=CARTESIAN_POINT('Ctrl Pts',(-67.5945294909398,23.1962882611443,12.));
#87716=CARTESIAN_POINT('Ctrl Pts',(-67.6175267028517,23.1963398337056,0.));
#87717=CARTESIAN_POINT('Ctrl Pts',(-67.6175267028517,23.1963398337056,12.));
#87718=CARTESIAN_POINT('Ctrl Pts',(-67.6405686407828,23.1963685232176,0.));
#87719=CARTESIAN_POINT('Ctrl Pts',(-67.6405686407828,23.1963685232176,12.));
#87720=CARTESIAN_POINT('Ctrl Pts',(-67.6636551726948,23.1963742630709,0.));
#87721=CARTESIAN_POINT('Ctrl Pts',(-67.6636551726948,23.1963742630709,12.));
#87722=CARTESIAN_POINT('Ctrl Pts',(-67.6867861671045,23.1963569870456,0.));
#87723=CARTESIAN_POINT('Ctrl Pts',(-67.6867861671045,23.1963569870456,12.));
#87724=CARTESIAN_POINT('Ctrl Pts',(-67.7099614930712,23.1963166293116,0.));
#87725=CARTESIAN_POINT('Ctrl Pts',(-67.7099614930712,23.1963166293116,12.));
#87726=CARTESIAN_POINT('Ctrl Pts',(-67.7331810201931,23.1962531244261,0.));
#87727=CARTESIAN_POINT('Ctrl Pts',(-67.7331810201931,23.1962531244261,12.));
#87728=CARTESIAN_POINT('Ctrl Pts',(-67.7564446186115,23.1961664073273,0.));
#87729=CARTESIAN_POINT('Ctrl Pts',(-67.7564446186115,23.1961664073273,12.));
#87730=CARTESIAN_POINT('Ctrl Pts',(-67.7797521590056,23.1960564133308,0.));
#87731=CARTESIAN_POINT('Ctrl Pts',(-67.7797521590056,23.1960564133308,12.));
#87732=CARTESIAN_POINT('Ctrl Pts',(-67.8031035125873,23.1959230781265,0.));
#87733=CARTESIAN_POINT('Ctrl Pts',(-67.8031035125873,23.1959230781265,12.));
#87734=CARTESIAN_POINT('Ctrl Pts',(-67.8264985510885,23.1957663377797,0.));
#87735=CARTESIAN_POINT('Ctrl Pts',(-67.8264985510885,23.1957663377797,12.));
#87736=CARTESIAN_POINT('Ctrl Pts',(-67.8499371467578,23.1955861287275,0.));
#87737=CARTESIAN_POINT('Ctrl Pts',(-67.8499371467578,23.1955861287275,12.));
#87738=CARTESIAN_POINT('Ctrl Pts',(-67.8734191723639,23.1953823877726,0.));
#87739=CARTESIAN_POINT('Ctrl Pts',(-67.8734191723639,23.1953823877726,12.));
#87740=CARTESIAN_POINT('Ctrl Pts',(-67.8969445011908,23.19515505208,0.));
#87741=CARTESIAN_POINT('Ctrl Pts',(-67.8969445011908,23.19515505208,12.));
#87742=CARTESIAN_POINT('Ctrl Pts',(-67.9205130070337,23.1949040591748,0.));
#87743=CARTESIAN_POINT('Ctrl Pts',(-67.9205130070337,23.1949040591748,12.));
#87744=CARTESIAN_POINT('Ctrl Pts',(-67.9441245641871,23.1946293469436,0.));
#87745=CARTESIAN_POINT('Ctrl Pts',(-67.9441245641871,23.1946293469436,12.));
#87746=CARTESIAN_POINT('Ctrl Pts',(-67.9677790474414,23.1943308536307,0.));
#87747=CARTESIAN_POINT('Ctrl Pts',(-67.9677790474414,23.1943308536307,12.));
#87748=CARTESIAN_POINT('Ctrl Pts',(-67.9914763320878,23.1940085178319,0.));
#87749=CARTESIAN_POINT('Ctrl Pts',(-67.9914763320878,23.1940085178319,12.));
#87750=CARTESIAN_POINT('Ctrl Pts',(-68.0152162939123,23.193662278492,0.));
#87751=CARTESIAN_POINT('Ctrl Pts',(-68.0152162939123,23.193662278492,12.));
#87752=CARTESIAN_POINT('Ctrl Pts',(-68.0389988091926,23.1932920749021,0.));
#87753=CARTESIAN_POINT('Ctrl Pts',(-68.0389988091926,23.1932920749021,12.));
#87754=CARTESIAN_POINT('Ctrl Pts',(-68.0628237546853,23.1928978467017,0.));
#87755=CARTESIAN_POINT('Ctrl Pts',(-68.0628237546853,23.1928978467017,12.));
#87756=CARTESIAN_POINT('Ctrl Pts',(-68.0866910076241,23.1924795338745,0.));
#87757=CARTESIAN_POINT('Ctrl Pts',(-68.0866910076241,23.1924795338745,12.));
#87758=CARTESIAN_POINT('Ctrl Pts',(-68.1106004457223,23.1920370767423,0.));
#87759=CARTESIAN_POINT('Ctrl Pts',(-68.1106004457223,23.1920370767423,12.));
#87760=CARTESIAN_POINT('Ctrl Pts',(-68.1345519471695,23.1915704159623,0.));
#87761=CARTESIAN_POINT('Ctrl Pts',(-68.1345519471695,23.1915704159623,12.));
#87762=CARTESIAN_POINT('Ctrl Pts',(-68.1585453906259,23.1910794925252,0.));
#87763=CARTESIAN_POINT('Ctrl Pts',(-68.1585453906259,23.1910794925252,12.));
#87764=CARTESIAN_POINT('Ctrl Pts',(-68.182580655213,23.1905642477571,0.));
#87765=CARTESIAN_POINT('Ctrl Pts',(-68.182580655213,23.1905642477571,12.));
#87766=CARTESIAN_POINT('Ctrl Pts',(-68.2066576205113,23.1900246233164,0.));
#87767=CARTESIAN_POINT('Ctrl Pts',(-68.2066576205113,23.1900246233164,12.));
#87768=CARTESIAN_POINT('Ctrl Pts',(-68.2307761665629,23.1894605611869,0.));
#87769=CARTESIAN_POINT('Ctrl Pts',(-68.2307761665629,23.1894605611869,12.));
#87770=CARTESIAN_POINT('Ctrl Pts',(-68.2549361738679,23.1888720036756,0.));
#87771=CARTESIAN_POINT('Ctrl Pts',(-68.2549361738679,23.1888720036756,12.));
#87772=CARTESIAN_POINT('Ctrl Pts',(-68.2791375233798,23.1882588934108,0.));
#87773=CARTESIAN_POINT('Ctrl Pts',(-68.2791375233798,23.1882588934108,12.));
#87774=CARTESIAN_POINT('Ctrl Pts',(-68.3033800964946,23.1876211733439,0.));
#87775=CARTESIAN_POINT('Ctrl Pts',(-68.3033800964946,23.1876211733439,12.));
#87776=CARTESIAN_POINT('Ctrl Pts',(-68.3276637750494,23.1869587867463,0.));
#87777=CARTESIAN_POINT('Ctrl Pts',(-68.3276637750494,23.1869587867463,12.));
#87778=CARTESIAN_POINT('Ctrl Pts',(-68.3519884413253,23.1862716772034,0.));
#87779=CARTESIAN_POINT('Ctrl Pts',(-68.3519884413253,23.1862716772034,12.));
#87780=CARTESIAN_POINT('Ctrl Pts',(-68.3763539780442,23.1855597886117,0.));
#87781=CARTESIAN_POINT('Ctrl Pts',(-68.3763539780442,23.1855597886117,12.));
#87782=CARTESIAN_POINT('Ctrl Pts',(-68.4007602683649,23.1848230651775,0.));
#87783=CARTESIAN_POINT('Ctrl Pts',(-68.4007602683649,23.1848230651775,12.));
#87784=CARTESIAN_POINT('Ctrl Pts',(-68.4252071958725,23.184061451419,0.));
#87785=CARTESIAN_POINT('Ctrl Pts',(-68.4252071958725,23.184061451419,12.));
#87786=CARTESIAN_POINT('Ctrl Pts',(-68.4496946445756,23.1832748921629,0.));
#87787=CARTESIAN_POINT('Ctrl Pts',(-68.4496946445756,23.1832748921629,12.));
#87788=CARTESIAN_POINT('Ctrl Pts',(-68.4742224989099,23.1824633325384,0.));
#87789=CARTESIAN_POINT('Ctrl Pts',(-68.4742224989099,23.1824633325384,12.));
#87790=CARTESIAN_POINT('Ctrl Pts',(-68.4987906437357,23.1816267179751,0.));
#87791=CARTESIAN_POINT('Ctrl Pts',(-68.4987906437357,23.1816267179751,12.));
#87792=CARTESIAN_POINT('Ctrl Pts',(-68.5233989643344,23.180764994201,0.));
#87793=CARTESIAN_POINT('Ctrl Pts',(-68.5233989643344,23.180764994201,12.));
#87794=CARTESIAN_POINT('Ctrl Pts',(-68.548047346398,23.1798781072449,0.));
#87795=CARTESIAN_POINT('Ctrl Pts',(-68.548047346398,23.1798781072449,12.));
#87796=CARTESIAN_POINT('Ctrl Pts',(-68.572735676027,23.1789660034339,0.));
#87797=CARTESIAN_POINT('Ctrl Pts',(-68.572735676027,23.1789660034339,12.));
#87798=CARTESIAN_POINT('Ctrl Pts',(-68.5974638397322,23.1780286293873,0.));
#87799=CARTESIAN_POINT('Ctrl Pts',(-68.5974638397322,23.1780286293873,12.));
#87800=CARTESIAN_POINT('Ctrl Pts',(-68.6222317244337,23.1770659320136,0.));
#87801=CARTESIAN_POINT('Ctrl Pts',(-68.6222317244337,23.1770659320136,12.));
#87802=CARTESIAN_POINT('Ctrl Pts',(-68.6470392174567,23.1760778585093,0.));
#87803=CARTESIAN_POINT('Ctrl Pts',(-68.6470392174567,23.1760778585093,12.));
#87804=CARTESIAN_POINT('Ctrl Pts',(-68.6718862065227,23.1750643563605,0.));
#87805=CARTESIAN_POINT('Ctrl Pts',(-68.6718862065227,23.1750643563605,12.));
#87806=CARTESIAN_POINT('Ctrl Pts',(-68.6967725797458,23.1740253733423,0.));
#87807=CARTESIAN_POINT('Ctrl Pts',(-68.6967725797458,23.1740253733423,12.));
#87808=CARTESIAN_POINT('Ctrl Pts',(-68.7216982256357,23.1729608575115,0.));
#87809=CARTESIAN_POINT('Ctrl Pts',(-68.7216982256357,23.1729608575115,12.));
#87810=CARTESIAN_POINT('Ctrl Pts',(-68.7466630330968,23.1718707572046,0.));
#87811=CARTESIAN_POINT('Ctrl Pts',(-68.7466630330968,23.1718707572046,12.));
#87812=CARTESIAN_POINT('Ctrl Pts',(-68.7716668914246,23.1707550210359,0.));
#87813=CARTESIAN_POINT('Ctrl Pts',(-68.7716668914246,23.1707550210359,12.));
#87814=CARTESIAN_POINT('Ctrl Pts',(-68.7967096902981,23.1696135978992,0.));
#87815=CARTESIAN_POINT('Ctrl Pts',(-68.7967096902981,23.1696135978992,12.));
#87816=CARTESIAN_POINT('Ctrl Pts',(-68.8217913197735,23.1684464369681,0.));
#87817=CARTESIAN_POINT('Ctrl Pts',(-68.8217913197735,23.1684464369681,12.));
#87818=CARTESIAN_POINT('Ctrl Pts',(-68.8469116702885,23.1672534876885,0.));
#87819=CARTESIAN_POINT('Ctrl Pts',(-68.8469116702885,23.1672534876885,12.));
#87820=CARTESIAN_POINT('Ctrl Pts',(-68.8720706326606,23.1660346997762,0.));
#87821=CARTESIAN_POINT('Ctrl Pts',(-68.8720706326606,23.1660346997762,12.));
#87822=CARTESIAN_POINT('Ctrl Pts',(-68.8972680980844,23.1647900232151,0.));
#87823=CARTESIAN_POINT('Ctrl Pts',(-68.8972680980844,23.1647900232151,12.));
#87824=CARTESIAN_POINT('Ctrl Pts',(-68.9225039581249,23.1635194082581,0.));
#87825=CARTESIAN_POINT('Ctrl Pts',(-68.9225039581249,23.1635194082581,12.));
#87826=CARTESIAN_POINT('Ctrl Pts',(-68.9477781047103,23.162222805429,0.));
#87827=CARTESIAN_POINT('Ctrl Pts',(-68.9477781047103,23.162222805429,12.));
#87828=CARTESIAN_POINT('Ctrl Pts',(-68.9730904301363,23.1609001655153,0.));
#87829=CARTESIAN_POINT('Ctrl Pts',(-68.9730904301363,23.1609001655153,12.));
#87830=CARTESIAN_POINT('Ctrl Pts',(-68.9984408270653,23.1595514395654,0.));
#87831=CARTESIAN_POINT('Ctrl Pts',(-68.9984408270653,23.1595514395654,12.));
#87832=CARTESIAN_POINT('Ctrl Pts',(-69.0238291885245,23.1581765788869,0.));
#87833=CARTESIAN_POINT('Ctrl Pts',(-69.0238291885245,23.1581765788869,12.));
#87834=CARTESIAN_POINT('Ctrl Pts',(-69.0492554078999,23.1567755350472,0.));
#87835=CARTESIAN_POINT('Ctrl Pts',(-69.0492554078999,23.1567755350472,12.));
#87836=CARTESIAN_POINT('Ctrl Pts',(-69.0747193789292,23.1553482598767,0.));
#87837=CARTESIAN_POINT('Ctrl Pts',(-69.0747193789292,23.1553482598767,12.));
#87838=CARTESIAN_POINT('Ctrl Pts',(-69.1002209957037,23.1538947054619,0.));
#87839=CARTESIAN_POINT('Ctrl Pts',(-69.1002209957037,23.1538947054619,12.));
#87840=CARTESIAN_POINT('Ctrl Pts',(-69.1257601526693,23.1524148241413,0.));
#87841=CARTESIAN_POINT('Ctrl Pts',(-69.1257601526693,23.1524148241413,12.));
#87842=CARTESIAN_POINT('Ctrl Pts',(-69.1513367446231,23.1509085685032,0.));
#87843=CARTESIAN_POINT('Ctrl Pts',(-69.1513367446231,23.1509085685032,12.));
#87844=CARTESIAN_POINT('Ctrl Pts',(-69.176950666708,23.1493758913857,0.));
#87845=CARTESIAN_POINT('Ctrl Pts',(-69.176950666708,23.1493758913857,12.));
#87846=CARTESIAN_POINT('Ctrl Pts',(-69.2026018144023,23.1478167458787,0.));
#87847=CARTESIAN_POINT('Ctrl Pts',(-69.2026018144023,23.1478167458787,12.));
#87848=CARTESIAN_POINT('Ctrl Pts',(-69.2282900835234,23.1462310853205,0.));
#87849=CARTESIAN_POINT('Ctrl Pts',(-69.2282900835234,23.1462310853205,12.));
#87850=CARTESIAN_POINT('Ctrl Pts',(-69.2540153702311,23.1446188632931,0.));
#87851=CARTESIAN_POINT('Ctrl Pts',(-69.2540153702311,23.1446188632931,12.));
#87852=CARTESIAN_POINT('Ctrl Pts',(-69.2797775710275,23.142980033622,0.));
#87853=CARTESIAN_POINT('Ctrl Pts',(-69.2797775710275,23.142980033622,12.));
#87854=CARTESIAN_POINT('Ctrl Pts',(-69.3055765827544,23.1413145503762,0.));
#87855=CARTESIAN_POINT('Ctrl Pts',(-69.3055765827544,23.1413145503762,12.));
#87856=CARTESIAN_POINT('Ctrl Pts',(-69.3314123025863,23.1396223678725,0.));
#87857=CARTESIAN_POINT('Ctrl Pts',(-69.3314123025863,23.1396223678725,12.));
#87858=CARTESIAN_POINT('Ctrl Pts',(-69.3572846280289,23.1379034406717,0.));
#87859=CARTESIAN_POINT('Ctrl Pts',(-69.3572846280289,23.1379034406717,12.));
#87860=CARTESIAN_POINT('Ctrl Pts',(-69.3831934569176,23.1361577235708,0.));
#87861=CARTESIAN_POINT('Ctrl Pts',(-69.3831934569176,23.1361577235708,12.));
#87862=CARTESIAN_POINT('Ctrl Pts',(-69.4091386874129,23.1343851715988,0.));
#87863=CARTESIAN_POINT('Ctrl Pts',(-69.4091386874129,23.1343851715988,12.));
#87864=CARTESIAN_POINT('Ctrl Pts',(-69.4351202179948,23.1325857400145,0.));
#87865=CARTESIAN_POINT('Ctrl Pts',(-69.4351202179948,23.1325857400145,12.));
#87866=CARTESIAN_POINT('Ctrl Pts',(-69.4611379474492,23.1307593843063,0.));
#87867=CARTESIAN_POINT('Ctrl Pts',(-69.4611379474492,23.1307593843063,12.));
#87868=CARTESIAN_POINT('Ctrl Pts',(-69.4871917748665,23.1289060601927,0.));
#87869=CARTESIAN_POINT('Ctrl Pts',(-69.4871917748665,23.1289060601927,12.));
#87870=CARTESIAN_POINT('Ctrl Pts',(-69.5132815996548,23.1270257236207,0.));
#87871=CARTESIAN_POINT('Ctrl Pts',(-69.5132815996548,23.1270257236207,12.));
#87872=CARTESIAN_POINT('Ctrl Pts',(-69.5394073215467,23.1251183307678,0.));
#87873=CARTESIAN_POINT('Ctrl Pts',(-69.5394073215467,23.1251183307678,12.));
#87874=CARTESIAN_POINT('Ctrl Pts',(-69.565568840605,23.1231838380452,0.));
#87875=CARTESIAN_POINT('Ctrl Pts',(-69.565568840605,23.1231838380452,12.));
#87876=CARTESIAN_POINT('Ctrl Pts',(-69.5917660572255,23.1212222021049,0.));
#87877=CARTESIAN_POINT('Ctrl Pts',(-69.5917660572255,23.1212222021049,12.));
#87878=CARTESIAN_POINT('Ctrl Pts',(-69.617998872135,23.1192333798437,0.));
#87879=CARTESIAN_POINT('Ctrl Pts',(-69.617998872135,23.1192333798437,12.));
#87880=CARTESIAN_POINT('Ctrl Pts',(-69.6442671863751,23.1172173283855,0.));
#87881=CARTESIAN_POINT('Ctrl Pts',(-69.6442671863751,23.1172173283855,12.));
#87882=CARTESIAN_POINT('Ctrl Pts',(-69.6705709012842,23.1151740050678,0.));
#87883=CARTESIAN_POINT('Ctrl Pts',(-69.6705709012842,23.1151740050678,12.));
#87884=CARTESIAN_POINT('Ctrl Pts',(-69.6969099184766,23.1131033674301,0.));
#87885=CARTESIAN_POINT('Ctrl Pts',(-69.6969099184766,23.1131033674301,12.));
#87886=CARTESIAN_POINT('Ctrl Pts',(-69.7232841398207,23.1110053732049,0.));
#87887=CARTESIAN_POINT('Ctrl Pts',(-69.7232841398207,23.1110053732049,12.));
#87888=CARTESIAN_POINT('Ctrl Pts',(-69.7496934674083,23.1088799803093,0.));
#87889=CARTESIAN_POINT('Ctrl Pts',(-69.7496934674083,23.1088799803093,12.));
#87890=CARTESIAN_POINT('Ctrl Pts',(-69.7761378035979,23.1067271468614,0.));
#87891=CARTESIAN_POINT('Ctrl Pts',(-69.7761378035979,23.1067271468614,12.));
#87892=CARTESIAN_POINT('Ctrl Pts',(-69.8026170510582,23.1045468311994,0.));
#87893=CARTESIAN_POINT('Ctrl Pts',(-69.8026170510582,23.1045468311994,12.));
#87894=CARTESIAN_POINT('Ctrl Pts',(-69.8291311128121,23.1023389919052,0.));
#87895=CARTESIAN_POINT('Ctrl Pts',(-69.8291311128121,23.1023389919052,12.));
#87896=CARTESIAN_POINT('Ctrl Pts',(-69.8556798922688,23.100103587824,0.));
#87897=CARTESIAN_POINT('Ctrl Pts',(-69.8556798922688,23.100103587824,12.));
#87898=CARTESIAN_POINT('Ctrl Pts',(-69.882263293276,23.0978405781018,0.));
#87899=CARTESIAN_POINT('Ctrl Pts',(-69.882263293276,23.0978405781018,12.));
#87900=CARTESIAN_POINT('Ctrl Pts',(-69.9088812200704,23.0955499221556,0.));
#87901=CARTESIAN_POINT('Ctrl Pts',(-69.9088812200704,23.0955499221556,12.));
#87902=CARTESIAN_POINT('Ctrl Pts',(-69.9355335771722,23.0932315796066,0.));
#87903=CARTESIAN_POINT('Ctrl Pts',(-69.9355335771722,23.0932315796066,12.));
#87904=CARTESIAN_POINT('Ctrl Pts',(-69.9622202692871,23.090885510225,0.));
#87905=CARTESIAN_POINT('Ctrl Pts',(-69.9622202692871,23.090885510225,12.));
#87906=CARTESIAN_POINT('Ctrl Pts',(-69.9889412012143,23.0885116738798,0.));
#87907=CARTESIAN_POINT('Ctrl Pts',(-69.9889412012143,23.0885116738798,12.));
#87908=CARTESIAN_POINT('Ctrl Pts',(-70.0156962777173,23.0861100304731,0.));
#87909=CARTESIAN_POINT('Ctrl Pts',(-70.0156962777173,23.0861100304731,12.));
#87910=CARTESIAN_POINT('Ctrl Pts',(-70.0424854035125,23.0836805399377,0.));
#87911=CARTESIAN_POINT('Ctrl Pts',(-70.0424854035125,23.0836805399377,12.));
#87912=CARTESIAN_POINT('Ctrl Pts',(-70.0693084835388,23.081223162377,0.));
#87913=CARTESIAN_POINT('Ctrl Pts',(-70.0693084835388,23.081223162377,12.));
#87914=CARTESIAN_POINT('Ctrl Pts',(-70.096165423165,23.0787378581778,0.));
#87915=CARTESIAN_POINT('Ctrl Pts',(-70.096165423165,23.0787378581778,12.));
#87916=CARTESIAN_POINT('Ctrl Pts',(-70.1230561284222,23.076224588139,0.));
#87917=CARTESIAN_POINT('Ctrl Pts',(-70.1230561284222,23.076224588139,12.));
#87918=CARTESIAN_POINT('Ctrl Pts',(-70.1499805062159,23.0736833135934,0.));
#87919=CARTESIAN_POINT('Ctrl Pts',(-70.1499805062159,23.0736833135934,12.));
#87920=CARTESIAN_POINT('Ctrl Pts',(-70.176938464556,23.0711139965432,0.));
#87921=CARTESIAN_POINT('Ctrl Pts',(-70.176938464556,23.0711139965432,12.));
#87922=CARTESIAN_POINT('Ctrl Pts',(-70.2039299120456,23.0685165993681,0.));
#87923=CARTESIAN_POINT('Ctrl Pts',(-70.2039299120456,23.0685165993681,12.));
#87924=CARTESIAN_POINT('Ctrl Pts',(-70.2309547573789,23.0658910845425,0.));
#87925=CARTESIAN_POINT('Ctrl Pts',(-70.2309547573789,23.0658910845425,12.));
#87926=CARTESIAN_POINT('Ctrl Pts',(-70.2580129087878,23.0632374143276,0.));
#87927=CARTESIAN_POINT('Ctrl Pts',(-70.2580129087878,23.0632374143276,12.));
#87928=CARTESIAN_POINT('Ctrl Pts',(-70.2851042736081,23.0605555505326,0.));
#87929=CARTESIAN_POINT('Ctrl Pts',(-70.2851042736081,23.0605555505326,12.));
#87930=CARTESIAN_POINT('Ctrl Pts',(-70.3122287575374,23.0578454541116,0.));
#87931=CARTESIAN_POINT('Ctrl Pts',(-70.3122287575374,23.0578454541116,12.));
#87932=CARTESIAN_POINT('Ctrl Pts',(-70.3393862652353,23.0551070854942,0.));
#87933=CARTESIAN_POINT('Ctrl Pts',(-70.3393862652353,23.0551070854942,12.));
#87934=CARTESIAN_POINT('Ctrl Pts',(-70.3665767016596,23.0523404053188,0.));
#87935=CARTESIAN_POINT('Ctrl Pts',(-70.3665767016596,23.0523404053188,12.));
#87936=CARTESIAN_POINT('Ctrl Pts',(-70.39379997323,23.0495453750773,0.));
#87937=CARTESIAN_POINT('Ctrl Pts',(-70.39379997323,23.0495453750773,12.));
#87938=CARTESIAN_POINT('Ctrl Pts',(-70.421055988934,23.0467219577288,0.));
#87939=CARTESIAN_POINT('Ctrl Pts',(-70.421055988934,23.0467219577288,12.));
#87940=CARTESIAN_POINT('Ctrl Pts',(-70.4483446617553,23.0438701184995,0.));
#87941=CARTESIAN_POINT('Ctrl Pts',(-70.4483446617553,23.0438701184995,12.));
#87942=CARTESIAN_POINT('Ctrl Pts',(-70.4756659090104,23.0409898250726,0.));
#87943=CARTESIAN_POINT('Ctrl Pts',(-70.4756659090104,23.0409898250726,12.));
#87944=CARTESIAN_POINT('Ctrl Pts',(-70.5030196491883,23.0380810458237,0.));
#87945=CARTESIAN_POINT('Ctrl Pts',(-70.5030196491883,23.0380810458237,12.));
#87946=CARTESIAN_POINT('Ctrl Pts',(-70.5304057994537,23.0351437484309,0.));
#87947=CARTESIAN_POINT('Ctrl Pts',(-70.5304057994537,23.0351437484309,12.));
#87948=CARTESIAN_POINT('Ctrl Pts',(-70.5578242727606,23.0321778982705,0.));
#87949=CARTESIAN_POINT('Ctrl Pts',(-70.5578242727606,23.0321778982705,12.));
#87950=CARTESIAN_POINT('Ctrl Pts',(-70.5852749754168,23.0291834570688,0.));
#87951=CARTESIAN_POINT('Ctrl Pts',(-70.5852749754168,23.0291834570688,12.));
#87952=CARTESIAN_POINT('Ctrl Pts',(-70.6127578036869,23.0261603810187,0.));
#87953=CARTESIAN_POINT('Ctrl Pts',(-70.6127578036869,23.0261603810187,12.));
#87954=CARTESIAN_POINT('Ctrl Pts',(-70.6402726486718,23.0231086235262,0.));
#87955=CARTESIAN_POINT('Ctrl Pts',(-70.6402726486718,23.0231086235262,12.));
#87956=CARTESIAN_POINT('Ctrl Pts',(-70.6678194023389,23.0200281385906,0.));
#87957=CARTESIAN_POINT('Ctrl Pts',(-70.6678194023389,23.0200281385906,12.));
#87958=CARTESIAN_POINT('Ctrl Pts',(-70.6953979633561,23.0169188841083,0.));
#87959=CARTESIAN_POINT('Ctrl Pts',(-70.6953979633561,23.0169188841083,12.));
#87960=CARTESIAN_POINT('Ctrl Pts',(-70.7230082425324,23.0137808248898,0.));
#87961=CARTESIAN_POINT('Ctrl Pts',(-70.7230082425324,23.0137808248898,12.));
#87962=CARTESIAN_POINT('Ctrl Pts',(-70.7506501695822,23.0106139365941,0.));
#87963=CARTESIAN_POINT('Ctrl Pts',(-70.7506501695822,23.0106139365941,12.));
#87964=CARTESIAN_POINT('Ctrl Pts',(-70.7783236950588,23.007418206361,0.));
#87965=CARTESIAN_POINT('Ctrl Pts',(-70.7783236950588,23.007418206361,12.));
#87966=CARTESIAN_POINT('Ctrl Pts',(-70.806028785987,23.004193629142,0.));
#87967=CARTESIAN_POINT('Ctrl Pts',(-70.806028785987,23.004193629142,12.));
#87968=CARTESIAN_POINT('Ctrl Pts',(-70.8282180956627,23.0015908899222,0.));
#87969=CARTESIAN_POINT('Ctrl Pts',(-70.8282180956627,23.0015908899222,12.));
#87970=CARTESIAN_POINT('Ctrl Pts',(-70.8448742696329,22.9996258555187,0.));
#87971=CARTESIAN_POINT('Ctrl Pts',(-70.8448742696329,22.9996258555187,12.));
#87972=CARTESIAN_POINT('Ctrl Pts',(-70.8559846927868,22.9983100639353,0.));
#87973=CARTESIAN_POINT('Ctrl Pts',(-70.8559846927868,22.9983100639353,12.));
#87974=CARTESIAN_POINT('Ctrl Pts',(-70.8615414811572,22.9976507259816,0.));
#87975=CARTESIAN_POINT('Ctrl Pts',(-70.8615414811572,22.9976507259816,12.));
#87976=CARTESIAN_POINT('',(-66.0656156664138,23.1372951448024,0.));
#87977=CARTESIAN_POINT('Ctrl Pts',(-66.0656156664138,23.1372951448024,0.));
#87978=CARTESIAN_POINT('Ctrl Pts',(-66.0694876382127,23.1375957166104,0.));
#87979=CARTESIAN_POINT('Ctrl Pts',(-66.0772371487248,23.13819515974,0.));
#87980=CARTESIAN_POINT('Ctrl Pts',(-66.0888781152421,23.1390892229778,0.));
#87981=CARTESIAN_POINT('Ctrl Pts',(-66.1044328067355,23.1402711039425,0.));
#87982=CARTESIAN_POINT('Ctrl Pts',(-66.1239318368548,23.1417314398398,0.));
#87983=CARTESIAN_POINT('Ctrl Pts',(-66.1434865015027,23.1431747350098,0.));
#87984=CARTESIAN_POINT('Ctrl Pts',(-66.1630967296747,23.1446009424903,0.));
#87985=CARTESIAN_POINT('Ctrl Pts',(-66.18276239029,23.1460099850763,0.));
#87986=CARTESIAN_POINT('Ctrl Pts',(-66.2024832934866,23.1474017566484,0.));
#87987=CARTESIAN_POINT('Ctrl Pts',(-66.2222592165473,23.1487761349328,0.));
#87988=CARTESIAN_POINT('Ctrl Pts',(-66.2420899237317,23.1501329914488,0.));
#87989=CARTESIAN_POINT('Ctrl Pts',(-66.2619751878741,23.1514722022483,0.));
#87990=CARTESIAN_POINT('Ctrl Pts',(-66.2819148131072,23.1527936592625,0.));
#87991=CARTESIAN_POINT('Ctrl Pts',(-66.301908627539,23.154097266617,0.));
#87992=CARTESIAN_POINT('Ctrl Pts',(-66.3219564725161,23.1553829352531,0.));
#87993=CARTESIAN_POINT('Ctrl Pts',(-66.3420581937159,23.1566505784626,0.));
#87994=CARTESIAN_POINT('Ctrl Pts',(-66.3622136300692,23.1579001063438,0.));
#87995=CARTESIAN_POINT('Ctrl Pts',(-66.382422608185,23.15913142301,0.));
#87996=CARTESIAN_POINT('Ctrl Pts',(-66.402684948127,23.1603444294754,0.));
#87997=CARTESIAN_POINT('Ctrl Pts',(-66.4230004670288,23.1615390254635,0.));
#87998=CARTESIAN_POINT('Ctrl Pts',(-66.4433689832454,23.1627151114875,0.));
#87999=CARTESIAN_POINT('Ctrl Pts',(-66.4637903210682,23.163872591218,0.));
#88000=CARTESIAN_POINT('Ctrl Pts',(-66.4842643105263,23.1650113713792,0.));
#88001=CARTESIAN_POINT('Ctrl Pts',(-66.5047907851319,23.1661313606123,0.));
#88002=CARTESIAN_POINT('Ctrl Pts',(-66.5253695803209,23.1672324686927,0.));
#88003=CARTESIAN_POINT('Ctrl Pts',(-66.5460005315406,23.1683146055736,0.));
#88004=CARTESIAN_POINT('Ctrl Pts',(-66.5666834726495,23.169377680588,0.));
#88005=CARTESIAN_POINT('Ctrl Pts',(-66.5874182367597,23.1704216028626,0.));
#88006=CARTESIAN_POINT('Ctrl Pts',(-66.6082046569657,23.1714462816794,0.));
#88007=CARTESIAN_POINT('Ctrl Pts',(-66.6290425670538,23.1724516268299,0.));
#88008=CARTESIAN_POINT('Ctrl Pts',(-66.6499318023445,23.1734375490421,0.));
#88009=CARTESIAN_POINT('Ctrl Pts',(-66.6708722000047,23.174403960137,0.));
#88010=CARTESIAN_POINT('Ctrl Pts',(-66.691863598595,23.1753507727931,0.));
#88011=CARTESIAN_POINT('Ctrl Pts',(-66.712905837789,23.1762779004043,0.));
#88012=CARTESIAN_POINT('Ctrl Pts',(-66.7339987580441,23.1771852569136,0.));
#88013=CARTESIAN_POINT('Ctrl Pts',(-66.7551422002229,23.1780727566309,0.));
#88014=CARTESIAN_POINT('Ctrl Pts',(-66.7763360056146,23.1789403142375,0.));
#88015=CARTESIAN_POINT('Ctrl Pts',(-66.7975800161014,23.1797878448645,0.));
#88016=CARTESIAN_POINT('Ctrl Pts',(-66.8188740742727,23.1806152641475,0.));
#88017=CARTESIAN_POINT('Ctrl Pts',(-66.840218023555,23.1814224882948,0.));
#88018=CARTESIAN_POINT('Ctrl Pts',(-66.8616117083304,23.1822094341508,0.));
#88019=CARTESIAN_POINT('Ctrl Pts',(-66.8830549738768,23.1829760191582,0.));
#88020=CARTESIAN_POINT('Ctrl Pts',(-66.904547666305,23.1837221613231,0.));
#88021=CARTESIAN_POINT('Ctrl Pts',(-66.9260896324955,23.1844477791816,0.));
#88022=CARTESIAN_POINT('Ctrl Pts',(-66.9476807200225,23.1851527917665,0.));
#88023=CARTESIAN_POINT('Ctrl Pts',(-66.9693207771059,23.1858371185852,0.));
#88024=CARTESIAN_POINT('Ctrl Pts',(-66.9910096526483,23.1865006796291,0.));
#88025=CARTESIAN_POINT('Ctrl Pts',(-67.0127471962507,23.1871433953795,0.));
#88026=CARTESIAN_POINT('Ctrl Pts',(-67.0345332582297,23.1877651868155,0.));
#88027=CARTESIAN_POINT('Ctrl Pts',(-67.0563676896312,23.1883659754267,0.));
#88028=CARTESIAN_POINT('Ctrl Pts',(-67.0782503422293,23.1889456832115,0.));
#88029=CARTESIAN_POINT('Ctrl Pts',(-67.1001810685138,23.1895042326625,0.));
#88030=CARTESIAN_POINT('Ctrl Pts',(-67.122159721674,23.1900415467574,0.));
#88031=CARTESIAN_POINT('Ctrl Pts',(-67.1441861555819,23.1905575489505,0.));
#88032=CARTESIAN_POINT('Ctrl Pts',(-67.1662602247641,23.1910521631658,0.));
#88033=CARTESIAN_POINT('Ctrl Pts',(-67.1883817844039,23.1915253137923,0.));
#88034=CARTESIAN_POINT('Ctrl Pts',(-67.2105506903448,23.1919769256803,0.));
#88035=CARTESIAN_POINT('Ctrl Pts',(-67.232766799088,23.1924069241385,0.));
#88036=CARTESIAN_POINT('Ctrl Pts',(-67.2550299677888,23.1928152349343,0.));
#88037=CARTESIAN_POINT('Ctrl Pts',(-67.2773400542477,23.1932017842954,0.));
#88038=CARTESIAN_POINT('Ctrl Pts',(-67.2996969169099,23.193566498902,0.));
#88039=CARTESIAN_POINT('Ctrl Pts',(-67.3221004148604,23.1939093058802,0.));
#88040=CARTESIAN_POINT('Ctrl Pts',(-67.3445504078178,23.1942301327979,0.));
#88041=CARTESIAN_POINT('Ctrl Pts',(-67.3670467561205,23.1945289076608,0.));
#88042=CARTESIAN_POINT('Ctrl Pts',(-67.3895893207168,23.1948055589123,0.));
#88043=CARTESIAN_POINT('Ctrl Pts',(-67.4121779631666,23.1950600154259,0.));
#88044=CARTESIAN_POINT('Ctrl Pts',(-67.4348125456389,23.1952922065009,0.));
#88045=CARTESIAN_POINT('Ctrl Pts',(-67.4574929309079,23.1955020618591,0.));
#88046=CARTESIAN_POINT('Ctrl Pts',(-67.4802189823424,23.1956895116446,0.));
#88047=CARTESIAN_POINT('Ctrl Pts',(-67.5029905638974,23.1958544864224,0.));
#88048=CARTESIAN_POINT('Ctrl Pts',(-67.525807540117,23.1959969171709,0.));
#88049=CARTESIAN_POINT('Ctrl Pts',(-67.5486697761301,23.1961167352776,0.));
#88050=CARTESIAN_POINT('Ctrl Pts',(-67.5715771376454,23.1962138725358,0.));
#88051=CARTESIAN_POINT('Ctrl Pts',(-67.5945294909398,23.1962882611443,0.));
#88052=CARTESIAN_POINT('Ctrl Pts',(-67.6175267028517,23.1963398337056,0.));
#88053=CARTESIAN_POINT('Ctrl Pts',(-67.6405686407828,23.1963685232176,0.));
#88054=CARTESIAN_POINT('Ctrl Pts',(-67.6636551726948,23.1963742630709,0.));
#88055=CARTESIAN_POINT('Ctrl Pts',(-67.6867861671045,23.1963569870456,0.));
#88056=CARTESIAN_POINT('Ctrl Pts',(-67.7099614930712,23.1963166293116,0.));
#88057=CARTESIAN_POINT('Ctrl Pts',(-67.7331810201931,23.1962531244261,0.));
#88058=CARTESIAN_POINT('Ctrl Pts',(-67.7564446186115,23.1961664073273,0.));
#88059=CARTESIAN_POINT('Ctrl Pts',(-67.7797521590056,23.1960564133308,0.));
#88060=CARTESIAN_POINT('Ctrl Pts',(-67.8031035125873,23.1959230781265,0.));
#88061=CARTESIAN_POINT('Ctrl Pts',(-67.8264985510885,23.1957663377797,0.));
#88062=CARTESIAN_POINT('Ctrl Pts',(-67.8499371467578,23.1955861287275,0.));
#88063=CARTESIAN_POINT('Ctrl Pts',(-67.8734191723639,23.1953823877726,0.));
#88064=CARTESIAN_POINT('Ctrl Pts',(-67.8969445011908,23.19515505208,0.));
#88065=CARTESIAN_POINT('Ctrl Pts',(-67.9205130070337,23.1949040591748,0.));
#88066=CARTESIAN_POINT('Ctrl Pts',(-67.9441245641871,23.1946293469436,0.));
#88067=CARTESIAN_POINT('Ctrl Pts',(-67.9677790474414,23.1943308536307,0.));
#88068=CARTESIAN_POINT('Ctrl Pts',(-67.9914763320878,23.1940085178319,0.));
#88069=CARTESIAN_POINT('Ctrl Pts',(-68.0152162939123,23.193662278492,0.));
#88070=CARTESIAN_POINT('Ctrl Pts',(-68.0389988091926,23.1932920749021,0.));
#88071=CARTESIAN_POINT('Ctrl Pts',(-68.0628237546853,23.1928978467017,0.));
#88072=CARTESIAN_POINT('Ctrl Pts',(-68.0866910076241,23.1924795338745,0.));
#88073=CARTESIAN_POINT('Ctrl Pts',(-68.1106004457223,23.1920370767423,0.));
#88074=CARTESIAN_POINT('Ctrl Pts',(-68.1345519471695,23.1915704159623,0.));
#88075=CARTESIAN_POINT('Ctrl Pts',(-68.1585453906259,23.1910794925252,0.));
#88076=CARTESIAN_POINT('Ctrl Pts',(-68.182580655213,23.1905642477571,0.));
#88077=CARTESIAN_POINT('Ctrl Pts',(-68.2066576205113,23.1900246233164,0.));
#88078=CARTESIAN_POINT('Ctrl Pts',(-68.2307761665629,23.1894605611869,0.));
#88079=CARTESIAN_POINT('Ctrl Pts',(-68.2549361738679,23.1888720036756,0.));
#88080=CARTESIAN_POINT('Ctrl Pts',(-68.2791375233798,23.1882588934108,0.));
#88081=CARTESIAN_POINT('Ctrl Pts',(-68.3033800964946,23.1876211733439,0.));
#88082=CARTESIAN_POINT('Ctrl Pts',(-68.3276637750494,23.1869587867463,0.));
#88083=CARTESIAN_POINT('Ctrl Pts',(-68.3519884413253,23.1862716772034,0.));
#88084=CARTESIAN_POINT('Ctrl Pts',(-68.3763539780442,23.1855597886117,0.));
#88085=CARTESIAN_POINT('Ctrl Pts',(-68.4007602683649,23.1848230651775,0.));
#88086=CARTESIAN_POINT('Ctrl Pts',(-68.4252071958725,23.184061451419,0.));
#88087=CARTESIAN_POINT('Ctrl Pts',(-68.4496946445756,23.1832748921629,0.));
#88088=CARTESIAN_POINT('Ctrl Pts',(-68.4742224989099,23.1824633325384,0.));
#88089=CARTESIAN_POINT('Ctrl Pts',(-68.4987906437357,23.1816267179751,0.));
#88090=CARTESIAN_POINT('Ctrl Pts',(-68.5233989643344,23.180764994201,0.));
#88091=CARTESIAN_POINT('Ctrl Pts',(-68.548047346398,23.1798781072449,0.));
#88092=CARTESIAN_POINT('Ctrl Pts',(-68.572735676027,23.1789660034339,0.));
#88093=CARTESIAN_POINT('Ctrl Pts',(-68.5974638397322,23.1780286293873,0.));
#88094=CARTESIAN_POINT('Ctrl Pts',(-68.6222317244337,23.1770659320136,0.));
#88095=CARTESIAN_POINT('Ctrl Pts',(-68.6470392174567,23.1760778585093,0.));
#88096=CARTESIAN_POINT('Ctrl Pts',(-68.6718862065227,23.1750643563605,0.));
#88097=CARTESIAN_POINT('Ctrl Pts',(-68.6967725797458,23.1740253733423,0.));
#88098=CARTESIAN_POINT('Ctrl Pts',(-68.7216982256357,23.1729608575115,0.));
#88099=CARTESIAN_POINT('Ctrl Pts',(-68.7466630330968,23.1718707572046,0.));
#88100=CARTESIAN_POINT('Ctrl Pts',(-68.7716668914246,23.1707550210359,0.));
#88101=CARTESIAN_POINT('Ctrl Pts',(-68.7967096902981,23.1696135978992,0.));
#88102=CARTESIAN_POINT('Ctrl Pts',(-68.8217913197735,23.1684464369681,0.));
#88103=CARTESIAN_POINT('Ctrl Pts',(-68.8469116702885,23.1672534876885,0.));
#88104=CARTESIAN_POINT('Ctrl Pts',(-68.8720706326606,23.1660346997762,0.));
#88105=CARTESIAN_POINT('Ctrl Pts',(-68.8972680980844,23.1647900232151,0.));
#88106=CARTESIAN_POINT('Ctrl Pts',(-68.9225039581249,23.1635194082581,0.));
#88107=CARTESIAN_POINT('Ctrl Pts',(-68.9477781047103,23.162222805429,0.));
#88108=CARTESIAN_POINT('Ctrl Pts',(-68.9730904301363,23.1609001655153,0.));
#88109=CARTESIAN_POINT('Ctrl Pts',(-68.9984408270653,23.1595514395654,0.));
#88110=CARTESIAN_POINT('Ctrl Pts',(-69.0238291885245,23.1581765788869,0.));
#88111=CARTESIAN_POINT('Ctrl Pts',(-69.0492554078999,23.1567755350472,0.));
#88112=CARTESIAN_POINT('Ctrl Pts',(-69.0747193789292,23.1553482598767,0.));
#88113=CARTESIAN_POINT('Ctrl Pts',(-69.1002209957037,23.1538947054619,0.));
#88114=CARTESIAN_POINT('Ctrl Pts',(-69.1257601526693,23.1524148241413,0.));
#88115=CARTESIAN_POINT('Ctrl Pts',(-69.1513367446231,23.1509085685032,0.));
#88116=CARTESIAN_POINT('Ctrl Pts',(-69.176950666708,23.1493758913857,0.));
#88117=CARTESIAN_POINT('Ctrl Pts',(-69.2026018144023,23.1478167458787,0.));
#88118=CARTESIAN_POINT('Ctrl Pts',(-69.2282900835234,23.1462310853205,0.));
#88119=CARTESIAN_POINT('Ctrl Pts',(-69.2540153702311,23.1446188632931,0.));
#88120=CARTESIAN_POINT('Ctrl Pts',(-69.2797775710275,23.142980033622,0.));
#88121=CARTESIAN_POINT('Ctrl Pts',(-69.3055765827544,23.1413145503762,0.));
#88122=CARTESIAN_POINT('Ctrl Pts',(-69.3314123025863,23.1396223678725,0.));
#88123=CARTESIAN_POINT('Ctrl Pts',(-69.3572846280289,23.1379034406717,0.));
#88124=CARTESIAN_POINT('Ctrl Pts',(-69.3831934569176,23.1361577235708,0.));
#88125=CARTESIAN_POINT('Ctrl Pts',(-69.4091386874129,23.1343851715988,0.));
#88126=CARTESIAN_POINT('Ctrl Pts',(-69.4351202179948,23.1325857400145,0.));
#88127=CARTESIAN_POINT('Ctrl Pts',(-69.4611379474492,23.1307593843063,0.));
#88128=CARTESIAN_POINT('Ctrl Pts',(-69.4871917748665,23.1289060601927,0.));
#88129=CARTESIAN_POINT('Ctrl Pts',(-69.5132815996548,23.1270257236207,0.));
#88130=CARTESIAN_POINT('Ctrl Pts',(-69.5394073215467,23.1251183307678,0.));
#88131=CARTESIAN_POINT('Ctrl Pts',(-69.565568840605,23.1231838380452,0.));
#88132=CARTESIAN_POINT('Ctrl Pts',(-69.5917660572255,23.1212222021049,0.));
#88133=CARTESIAN_POINT('Ctrl Pts',(-69.617998872135,23.1192333798437,0.));
#88134=CARTESIAN_POINT('Ctrl Pts',(-69.6442671863751,23.1172173283855,0.));
#88135=CARTESIAN_POINT('Ctrl Pts',(-69.6705709012842,23.1151740050678,0.));
#88136=CARTESIAN_POINT('Ctrl Pts',(-69.6969099184766,23.1131033674301,0.));
#88137=CARTESIAN_POINT('Ctrl Pts',(-69.7232841398207,23.1110053732049,0.));
#88138=CARTESIAN_POINT('Ctrl Pts',(-69.7496934674083,23.1088799803093,0.));
#88139=CARTESIAN_POINT('Ctrl Pts',(-69.7761378035979,23.1067271468614,0.));
#88140=CARTESIAN_POINT('Ctrl Pts',(-69.8026170510582,23.1045468311994,0.));
#88141=CARTESIAN_POINT('Ctrl Pts',(-69.8291311128121,23.1023389919052,0.));
#88142=CARTESIAN_POINT('Ctrl Pts',(-69.8556798922688,23.100103587824,0.));
#88143=CARTESIAN_POINT('Ctrl Pts',(-69.882263293276,23.0978405781018,0.));
#88144=CARTESIAN_POINT('Ctrl Pts',(-69.9088812200704,23.0955499221556,0.));
#88145=CARTESIAN_POINT('Ctrl Pts',(-69.9355335771722,23.0932315796066,0.));
#88146=CARTESIAN_POINT('Ctrl Pts',(-69.9622202692871,23.090885510225,0.));
#88147=CARTESIAN_POINT('Ctrl Pts',(-69.9889412012143,23.0885116738798,0.));
#88148=CARTESIAN_POINT('Ctrl Pts',(-70.0156962777173,23.0861100304731,0.));
#88149=CARTESIAN_POINT('Ctrl Pts',(-70.0424854035125,23.0836805399377,0.));
#88150=CARTESIAN_POINT('Ctrl Pts',(-70.0693084835388,23.081223162377,0.));
#88151=CARTESIAN_POINT('Ctrl Pts',(-70.096165423165,23.0787378581778,0.));
#88152=CARTESIAN_POINT('Ctrl Pts',(-70.1230561284222,23.076224588139,0.));
#88153=CARTESIAN_POINT('Ctrl Pts',(-70.1499805062159,23.0736833135934,0.));
#88154=CARTESIAN_POINT('Ctrl Pts',(-70.176938464556,23.0711139965432,0.));
#88155=CARTESIAN_POINT('Ctrl Pts',(-70.2039299120456,23.0685165993681,0.));
#88156=CARTESIAN_POINT('Ctrl Pts',(-70.2309547573789,23.0658910845425,0.));
#88157=CARTESIAN_POINT('Ctrl Pts',(-70.2580129087878,23.0632374143276,0.));
#88158=CARTESIAN_POINT('Ctrl Pts',(-70.2851042736081,23.0605555505326,0.));
#88159=CARTESIAN_POINT('Ctrl Pts',(-70.3122287575374,23.0578454541116,0.));
#88160=CARTESIAN_POINT('Ctrl Pts',(-70.3393862652353,23.0551070854942,0.));
#88161=CARTESIAN_POINT('Ctrl Pts',(-70.3665767016596,23.0523404053188,0.));
#88162=CARTESIAN_POINT('Ctrl Pts',(-70.39379997323,23.0495453750773,0.));
#88163=CARTESIAN_POINT('Ctrl Pts',(-70.421055988934,23.0467219577288,0.));
#88164=CARTESIAN_POINT('Ctrl Pts',(-70.4483446617553,23.0438701184995,0.));
#88165=CARTESIAN_POINT('Ctrl Pts',(-70.4756659090104,23.0409898250726,0.));
#88166=CARTESIAN_POINT('Ctrl Pts',(-70.4991133648756,23.038496437601,0.));
#88167=CARTESIAN_POINT('Ctrl Pts',(-70.5171075702495,23.0365694096158,0.));
#88168=CARTESIAN_POINT('Ctrl Pts',(-70.5296341535252,23.0352213647764,0.));
#88169=CARTESIAN_POINT('Ctrl Pts',(-70.5366836381299,23.034460662331,0.));
#88170=CARTESIAN_POINT('Ctrl Pts',(-70.5382514078488,23.0342913834093,0.));
#88171=CARTESIAN_POINT('',(-66.0656156664138,23.1372951448024,12.));
#88172=CARTESIAN_POINT('',(-66.0656156664138,23.1372951448024,0.));
#88173=CARTESIAN_POINT('Ctrl Pts',(-70.5382514078489,23.0342913834093,12.));
#88174=CARTESIAN_POINT('Ctrl Pts',(-70.5366836381299,23.034460662331,12.));
#88175=CARTESIAN_POINT('Ctrl Pts',(-70.5296341535252,23.0352213647764,12.));
#88176=CARTESIAN_POINT('Ctrl Pts',(-70.5171075702495,23.0365694096158,12.));
#88177=CARTESIAN_POINT('Ctrl Pts',(-70.4991133648756,23.038496437601,12.));
#88178=CARTESIAN_POINT('Ctrl Pts',(-70.4756659090104,23.0409898250726,12.));
#88179=CARTESIAN_POINT('Ctrl Pts',(-70.4483446617553,23.0438701184995,12.));
#88180=CARTESIAN_POINT('Ctrl Pts',(-70.421055988934,23.0467219577288,12.));
#88181=CARTESIAN_POINT('Ctrl Pts',(-70.39379997323,23.0495453750773,12.));
#88182=CARTESIAN_POINT('Ctrl Pts',(-70.3665767016596,23.0523404053188,12.));
#88183=CARTESIAN_POINT('Ctrl Pts',(-70.3393862652353,23.0551070854942,12.));
#88184=CARTESIAN_POINT('Ctrl Pts',(-70.3122287575374,23.0578454541116,12.));
#88185=CARTESIAN_POINT('Ctrl Pts',(-70.2851042736081,23.0605555505326,12.));
#88186=CARTESIAN_POINT('Ctrl Pts',(-70.2580129087878,23.0632374143276,12.));
#88187=CARTESIAN_POINT('Ctrl Pts',(-70.2309547573789,23.0658910845425,12.));
#88188=CARTESIAN_POINT('Ctrl Pts',(-70.2039299120456,23.0685165993681,12.));
#88189=CARTESIAN_POINT('Ctrl Pts',(-70.176938464556,23.0711139965432,12.));
#88190=CARTESIAN_POINT('Ctrl Pts',(-70.1499805062159,23.0736833135934,12.));
#88191=CARTESIAN_POINT('Ctrl Pts',(-70.1230561284222,23.076224588139,12.));
#88192=CARTESIAN_POINT('Ctrl Pts',(-70.096165423165,23.0787378581778,12.));
#88193=CARTESIAN_POINT('Ctrl Pts',(-70.0693084835388,23.081223162377,12.));
#88194=CARTESIAN_POINT('Ctrl Pts',(-70.0424854035125,23.0836805399377,12.));
#88195=CARTESIAN_POINT('Ctrl Pts',(-70.0156962777173,23.0861100304731,12.));
#88196=CARTESIAN_POINT('Ctrl Pts',(-69.9889412012143,23.0885116738798,12.));
#88197=CARTESIAN_POINT('Ctrl Pts',(-69.9622202692871,23.090885510225,12.));
#88198=CARTESIAN_POINT('Ctrl Pts',(-69.9355335771722,23.0932315796066,12.));
#88199=CARTESIAN_POINT('Ctrl Pts',(-69.9088812200704,23.0955499221556,12.));
#88200=CARTESIAN_POINT('Ctrl Pts',(-69.882263293276,23.0978405781018,12.));
#88201=CARTESIAN_POINT('Ctrl Pts',(-69.8556798922688,23.100103587824,12.));
#88202=CARTESIAN_POINT('Ctrl Pts',(-69.8291311128121,23.1023389919052,12.));
#88203=CARTESIAN_POINT('Ctrl Pts',(-69.8026170510582,23.1045468311994,12.));
#88204=CARTESIAN_POINT('Ctrl Pts',(-69.7761378035979,23.1067271468614,12.));
#88205=CARTESIAN_POINT('Ctrl Pts',(-69.7496934674083,23.1088799803093,12.));
#88206=CARTESIAN_POINT('Ctrl Pts',(-69.7232841398207,23.1110053732049,12.));
#88207=CARTESIAN_POINT('Ctrl Pts',(-69.6969099184766,23.1131033674301,12.));
#88208=CARTESIAN_POINT('Ctrl Pts',(-69.6705709012842,23.1151740050678,12.));
#88209=CARTESIAN_POINT('Ctrl Pts',(-69.6442671863751,23.1172173283855,12.));
#88210=CARTESIAN_POINT('Ctrl Pts',(-69.617998872135,23.1192333798437,12.));
#88211=CARTESIAN_POINT('Ctrl Pts',(-69.5917660572255,23.1212222021049,12.));
#88212=CARTESIAN_POINT('Ctrl Pts',(-69.565568840605,23.1231838380452,12.));
#88213=CARTESIAN_POINT('Ctrl Pts',(-69.5394073215467,23.1251183307678,12.));
#88214=CARTESIAN_POINT('Ctrl Pts',(-69.5132815996548,23.1270257236207,12.));
#88215=CARTESIAN_POINT('Ctrl Pts',(-69.4871917748665,23.1289060601927,12.));
#88216=CARTESIAN_POINT('Ctrl Pts',(-69.4611379474492,23.1307593843063,12.));
#88217=CARTESIAN_POINT('Ctrl Pts',(-69.4351202179948,23.1325857400145,12.));
#88218=CARTESIAN_POINT('Ctrl Pts',(-69.4091386874129,23.1343851715988,12.));
#88219=CARTESIAN_POINT('Ctrl Pts',(-69.3831934569176,23.1361577235708,12.));
#88220=CARTESIAN_POINT('Ctrl Pts',(-69.3572846280289,23.1379034406717,12.));
#88221=CARTESIAN_POINT('Ctrl Pts',(-69.3314123025863,23.1396223678725,12.));
#88222=CARTESIAN_POINT('Ctrl Pts',(-69.3055765827544,23.1413145503762,12.));
#88223=CARTESIAN_POINT('Ctrl Pts',(-69.2797775710275,23.142980033622,12.));
#88224=CARTESIAN_POINT('Ctrl Pts',(-69.2540153702311,23.1446188632931,12.));
#88225=CARTESIAN_POINT('Ctrl Pts',(-69.2282900835234,23.1462310853205,12.));
#88226=CARTESIAN_POINT('Ctrl Pts',(-69.2026018144023,23.1478167458787,12.));
#88227=CARTESIAN_POINT('Ctrl Pts',(-69.176950666708,23.1493758913857,12.));
#88228=CARTESIAN_POINT('Ctrl Pts',(-69.1513367446231,23.1509085685032,12.));
#88229=CARTESIAN_POINT('Ctrl Pts',(-69.1257601526693,23.1524148241413,12.));
#88230=CARTESIAN_POINT('Ctrl Pts',(-69.1002209957037,23.1538947054619,12.));
#88231=CARTESIAN_POINT('Ctrl Pts',(-69.0747193789292,23.1553482598767,12.));
#88232=CARTESIAN_POINT('Ctrl Pts',(-69.0492554078999,23.1567755350472,12.));
#88233=CARTESIAN_POINT('Ctrl Pts',(-69.0238291885245,23.1581765788869,12.));
#88234=CARTESIAN_POINT('Ctrl Pts',(-68.9984408270653,23.1595514395654,12.));
#88235=CARTESIAN_POINT('Ctrl Pts',(-68.9730904301363,23.1609001655153,12.));
#88236=CARTESIAN_POINT('Ctrl Pts',(-68.9477781047103,23.162222805429,12.));
#88237=CARTESIAN_POINT('Ctrl Pts',(-68.9225039581249,23.1635194082581,12.));
#88238=CARTESIAN_POINT('Ctrl Pts',(-68.8972680980844,23.1647900232151,12.));
#88239=CARTESIAN_POINT('Ctrl Pts',(-68.8720706326606,23.1660346997762,12.));
#88240=CARTESIAN_POINT('Ctrl Pts',(-68.8469116702885,23.1672534876885,12.));
#88241=CARTESIAN_POINT('Ctrl Pts',(-68.8217913197735,23.1684464369681,12.));
#88242=CARTESIAN_POINT('Ctrl Pts',(-68.7967096902981,23.1696135978992,12.));
#88243=CARTESIAN_POINT('Ctrl Pts',(-68.7716668914246,23.1707550210359,12.));
#88244=CARTESIAN_POINT('Ctrl Pts',(-68.7466630330968,23.1718707572046,12.));
#88245=CARTESIAN_POINT('Ctrl Pts',(-68.7216982256357,23.1729608575115,12.));
#88246=CARTESIAN_POINT('Ctrl Pts',(-68.6967725797458,23.1740253733423,12.));
#88247=CARTESIAN_POINT('Ctrl Pts',(-68.6718862065227,23.1750643563605,12.));
#88248=CARTESIAN_POINT('Ctrl Pts',(-68.6470392174567,23.1760778585093,12.));
#88249=CARTESIAN_POINT('Ctrl Pts',(-68.6222317244337,23.1770659320136,12.));
#88250=CARTESIAN_POINT('Ctrl Pts',(-68.5974638397322,23.1780286293873,12.));
#88251=CARTESIAN_POINT('Ctrl Pts',(-68.572735676027,23.1789660034339,12.));
#88252=CARTESIAN_POINT('Ctrl Pts',(-68.548047346398,23.1798781072449,12.));
#88253=CARTESIAN_POINT('Ctrl Pts',(-68.5233989643344,23.180764994201,12.));
#88254=CARTESIAN_POINT('Ctrl Pts',(-68.4987906437357,23.1816267179751,12.));
#88255=CARTESIAN_POINT('Ctrl Pts',(-68.4742224989099,23.1824633325384,12.));
#88256=CARTESIAN_POINT('Ctrl Pts',(-68.4496946445756,23.1832748921629,12.));
#88257=CARTESIAN_POINT('Ctrl Pts',(-68.4252071958725,23.184061451419,12.));
#88258=CARTESIAN_POINT('Ctrl Pts',(-68.4007602683649,23.1848230651775,12.));
#88259=CARTESIAN_POINT('Ctrl Pts',(-68.3763539780442,23.1855597886117,12.));
#88260=CARTESIAN_POINT('Ctrl Pts',(-68.3519884413253,23.1862716772034,12.));
#88261=CARTESIAN_POINT('Ctrl Pts',(-68.3276637750494,23.1869587867463,12.));
#88262=CARTESIAN_POINT('Ctrl Pts',(-68.3033800964946,23.1876211733439,12.));
#88263=CARTESIAN_POINT('Ctrl Pts',(-68.2791375233798,23.1882588934108,12.));
#88264=CARTESIAN_POINT('Ctrl Pts',(-68.2549361738679,23.1888720036756,12.));
#88265=CARTESIAN_POINT('Ctrl Pts',(-68.2307761665629,23.1894605611869,12.));
#88266=CARTESIAN_POINT('Ctrl Pts',(-68.2066576205113,23.1900246233164,12.));
#88267=CARTESIAN_POINT('Ctrl Pts',(-68.182580655213,23.1905642477571,12.));
#88268=CARTESIAN_POINT('Ctrl Pts',(-68.1585453906259,23.1910794925252,12.));
#88269=CARTESIAN_POINT('Ctrl Pts',(-68.1345519471695,23.1915704159623,12.));
#88270=CARTESIAN_POINT('Ctrl Pts',(-68.1106004457223,23.1920370767423,12.));
#88271=CARTESIAN_POINT('Ctrl Pts',(-68.0866910076241,23.1924795338745,12.));
#88272=CARTESIAN_POINT('Ctrl Pts',(-68.0628237546853,23.1928978467017,12.));
#88273=CARTESIAN_POINT('Ctrl Pts',(-68.0389988091926,23.1932920749021,12.));
#88274=CARTESIAN_POINT('Ctrl Pts',(-68.0152162939123,23.193662278492,12.));
#88275=CARTESIAN_POINT('Ctrl Pts',(-67.9914763320878,23.1940085178319,12.));
#88276=CARTESIAN_POINT('Ctrl Pts',(-67.9677790474414,23.1943308536307,12.));
#88277=CARTESIAN_POINT('Ctrl Pts',(-67.9441245641871,23.1946293469436,12.));
#88278=CARTESIAN_POINT('Ctrl Pts',(-67.9205130070337,23.1949040591748,12.));
#88279=CARTESIAN_POINT('Ctrl Pts',(-67.8969445011908,23.19515505208,12.));
#88280=CARTESIAN_POINT('Ctrl Pts',(-67.8734191723639,23.1953823877726,12.));
#88281=CARTESIAN_POINT('Ctrl Pts',(-67.8499371467578,23.1955861287275,12.));
#88282=CARTESIAN_POINT('Ctrl Pts',(-67.8264985510885,23.1957663377797,12.));
#88283=CARTESIAN_POINT('Ctrl Pts',(-67.8031035125873,23.1959230781265,12.));
#88284=CARTESIAN_POINT('Ctrl Pts',(-67.7797521590056,23.1960564133308,12.));
#88285=CARTESIAN_POINT('Ctrl Pts',(-67.7564446186115,23.1961664073273,12.));
#88286=CARTESIAN_POINT('Ctrl Pts',(-67.7331810201931,23.1962531244261,12.));
#88287=CARTESIAN_POINT('Ctrl Pts',(-67.7099614930712,23.1963166293116,12.));
#88288=CARTESIAN_POINT('Ctrl Pts',(-67.6867861671045,23.1963569870456,12.));
#88289=CARTESIAN_POINT('Ctrl Pts',(-67.6636551726948,23.1963742630709,12.));
#88290=CARTESIAN_POINT('Ctrl Pts',(-67.6405686407828,23.1963685232176,12.));
#88291=CARTESIAN_POINT('Ctrl Pts',(-67.6175267028517,23.1963398337056,12.));
#88292=CARTESIAN_POINT('Ctrl Pts',(-67.5945294909398,23.1962882611443,12.));
#88293=CARTESIAN_POINT('Ctrl Pts',(-67.5715771376454,23.1962138725358,12.));
#88294=CARTESIAN_POINT('Ctrl Pts',(-67.5486697761301,23.1961167352776,12.));
#88295=CARTESIAN_POINT('Ctrl Pts',(-67.525807540117,23.1959969171709,12.));
#88296=CARTESIAN_POINT('Ctrl Pts',(-67.5029905638974,23.1958544864224,12.));
#88297=CARTESIAN_POINT('Ctrl Pts',(-67.4802189823424,23.1956895116446,12.));
#88298=CARTESIAN_POINT('Ctrl Pts',(-67.4574929309079,23.1955020618591,12.));
#88299=CARTESIAN_POINT('Ctrl Pts',(-67.4348125456389,23.1952922065009,12.));
#88300=CARTESIAN_POINT('Ctrl Pts',(-67.4121779631666,23.1950600154259,12.));
#88301=CARTESIAN_POINT('Ctrl Pts',(-67.3895893207168,23.1948055589123,12.));
#88302=CARTESIAN_POINT('Ctrl Pts',(-67.3670467561205,23.1945289076608,12.));
#88303=CARTESIAN_POINT('Ctrl Pts',(-67.3445504078178,23.1942301327979,12.));
#88304=CARTESIAN_POINT('Ctrl Pts',(-67.3221004148604,23.1939093058802,12.));
#88305=CARTESIAN_POINT('Ctrl Pts',(-67.2996969169099,23.193566498902,12.));
#88306=CARTESIAN_POINT('Ctrl Pts',(-67.2773400542477,23.1932017842954,12.));
#88307=CARTESIAN_POINT('Ctrl Pts',(-67.2550299677888,23.1928152349343,12.));
#88308=CARTESIAN_POINT('Ctrl Pts',(-67.232766799088,23.1924069241385,12.));
#88309=CARTESIAN_POINT('Ctrl Pts',(-67.2105506903448,23.1919769256803,12.));
#88310=CARTESIAN_POINT('Ctrl Pts',(-67.1883817844039,23.1915253137923,12.));
#88311=CARTESIAN_POINT('Ctrl Pts',(-67.1662602247641,23.1910521631658,12.));
#88312=CARTESIAN_POINT('Ctrl Pts',(-67.1441861555819,23.1905575489505,12.));
#88313=CARTESIAN_POINT('Ctrl Pts',(-67.122159721674,23.1900415467574,12.));
#88314=CARTESIAN_POINT('Ctrl Pts',(-67.1001810685138,23.1895042326625,12.));
#88315=CARTESIAN_POINT('Ctrl Pts',(-67.0782503422293,23.1889456832115,12.));
#88316=CARTESIAN_POINT('Ctrl Pts',(-67.0563676896312,23.1883659754267,12.));
#88317=CARTESIAN_POINT('Ctrl Pts',(-67.0345332582297,23.1877651868155,12.));
#88318=CARTESIAN_POINT('Ctrl Pts',(-67.0127471962507,23.1871433953795,12.));
#88319=CARTESIAN_POINT('Ctrl Pts',(-66.9910096526483,23.1865006796291,12.));
#88320=CARTESIAN_POINT('Ctrl Pts',(-66.9693207771059,23.1858371185852,12.));
#88321=CARTESIAN_POINT('Ctrl Pts',(-66.9476807200225,23.1851527917665,12.));
#88322=CARTESIAN_POINT('Ctrl Pts',(-66.9260896324955,23.1844477791816,12.));
#88323=CARTESIAN_POINT('Ctrl Pts',(-66.904547666305,23.1837221613231,12.));
#88324=CARTESIAN_POINT('Ctrl Pts',(-66.8830549738768,23.1829760191582,12.));
#88325=CARTESIAN_POINT('Ctrl Pts',(-66.8616117083304,23.1822094341508,12.));
#88326=CARTESIAN_POINT('Ctrl Pts',(-66.840218023555,23.1814224882948,12.));
#88327=CARTESIAN_POINT('Ctrl Pts',(-66.8188740742727,23.1806152641475,12.));
#88328=CARTESIAN_POINT('Ctrl Pts',(-66.7975800161014,23.1797878448645,12.));
#88329=CARTESIAN_POINT('Ctrl Pts',(-66.7763360056146,23.1789403142375,12.));
#88330=CARTESIAN_POINT('Ctrl Pts',(-66.7551422002229,23.1780727566309,12.));
#88331=CARTESIAN_POINT('Ctrl Pts',(-66.7339987580441,23.1771852569136,12.));
#88332=CARTESIAN_POINT('Ctrl Pts',(-66.712905837789,23.1762779004043,12.));
#88333=CARTESIAN_POINT('Ctrl Pts',(-66.691863598595,23.1753507727931,12.));
#88334=CARTESIAN_POINT('Ctrl Pts',(-66.6708722000047,23.174403960137,12.));
#88335=CARTESIAN_POINT('Ctrl Pts',(-66.6499318023445,23.1734375490421,12.));
#88336=CARTESIAN_POINT('Ctrl Pts',(-66.6290425670538,23.1724516268299,12.));
#88337=CARTESIAN_POINT('Ctrl Pts',(-66.6082046569657,23.1714462816794,12.));
#88338=CARTESIAN_POINT('Ctrl Pts',(-66.5874182367597,23.1704216028626,12.));
#88339=CARTESIAN_POINT('Ctrl Pts',(-66.5666834726495,23.169377680588,12.));
#88340=CARTESIAN_POINT('Ctrl Pts',(-66.5460005315406,23.1683146055736,12.));
#88341=CARTESIAN_POINT('Ctrl Pts',(-66.5253695803209,23.1672324686927,12.));
#88342=CARTESIAN_POINT('Ctrl Pts',(-66.5047907851319,23.1661313606123,12.));
#88343=CARTESIAN_POINT('Ctrl Pts',(-66.4842643105263,23.1650113713792,12.));
#88344=CARTESIAN_POINT('Ctrl Pts',(-66.4637903210682,23.163872591218,12.));
#88345=CARTESIAN_POINT('Ctrl Pts',(-66.4433689832454,23.1627151114875,12.));
#88346=CARTESIAN_POINT('Ctrl Pts',(-66.4230004670288,23.1615390254635,12.));
#88347=CARTESIAN_POINT('Ctrl Pts',(-66.402684948127,23.1603444294754,12.));
#88348=CARTESIAN_POINT('Ctrl Pts',(-66.382422608185,23.15913142301,12.));
#88349=CARTESIAN_POINT('Ctrl Pts',(-66.3622136300692,23.1579001063438,12.));
#88350=CARTESIAN_POINT('Ctrl Pts',(-66.3420581937159,23.1566505784626,12.));
#88351=CARTESIAN_POINT('Ctrl Pts',(-66.3219564725161,23.1553829352531,12.));
#88352=CARTESIAN_POINT('Ctrl Pts',(-66.301908627539,23.154097266617,12.));
#88353=CARTESIAN_POINT('Ctrl Pts',(-66.2819148131072,23.1527936592625,12.));
#88354=CARTESIAN_POINT('Ctrl Pts',(-66.2619751878741,23.1514722022483,12.));
#88355=CARTESIAN_POINT('Ctrl Pts',(-66.2420899237317,23.1501329914488,12.));
#88356=CARTESIAN_POINT('Ctrl Pts',(-66.2222592165473,23.1487761349328,12.));
#88357=CARTESIAN_POINT('Ctrl Pts',(-66.2024832934866,23.1474017566484,12.));
#88358=CARTESIAN_POINT('Ctrl Pts',(-66.18276239029,23.1460099850763,12.));
#88359=CARTESIAN_POINT('Ctrl Pts',(-66.1630967296747,23.1446009424903,12.));
#88360=CARTESIAN_POINT('Ctrl Pts',(-66.1434865015027,23.1431747350098,12.));
#88361=CARTESIAN_POINT('Ctrl Pts',(-66.1239318368548,23.1417314398398,12.));
#88362=CARTESIAN_POINT('Ctrl Pts',(-66.1044328067355,23.1402711039425,12.));
#88363=CARTESIAN_POINT('Ctrl Pts',(-66.0888781152421,23.1390892229778,12.));
#88364=CARTESIAN_POINT('Ctrl Pts',(-66.0772371487248,23.13819515974,12.));
#88365=CARTESIAN_POINT('Ctrl Pts',(-66.0694876382127,23.1375957166104,12.));
#88366=CARTESIAN_POINT('Ctrl Pts',(-66.0656156664138,23.1372951448024,12.));
#88367=CARTESIAN_POINT('Ctrl Pts',(-70.9934796069113,21.5904919935059,-5.55111512312578E-16));
#88368=CARTESIAN_POINT('Ctrl Pts',(-70.9934796069113,21.5904919935059,4.));
#88369=CARTESIAN_POINT('Ctrl Pts',(-70.9934796069113,21.5904919935059,8.));
#88370=CARTESIAN_POINT('Ctrl Pts',(-70.9934796069113,21.5904919935059,12.));
#88371=CARTESIAN_POINT('Ctrl Pts',(-71.0762040404458,21.6628164325797,-5.55111512312578E-16));
#88372=CARTESIAN_POINT('Ctrl Pts',(-71.0762040404458,21.6628164325797,4.));
#88373=CARTESIAN_POINT('Ctrl Pts',(-71.0762040404458,21.6628164325797,8.00000000000001));
#88374=CARTESIAN_POINT('Ctrl Pts',(-71.0762040404458,21.6628164325797,12.));
#88375=CARTESIAN_POINT('Ctrl Pts',(-71.1771795679088,21.8385342042356,-5.55111512312578E-16));
#88376=CARTESIAN_POINT('Ctrl Pts',(-71.1771795679088,21.8385342042356,4.));
#88377=CARTESIAN_POINT('Ctrl Pts',(-71.1771795679088,21.8385342042356,7.99999999999999));
#88378=CARTESIAN_POINT('Ctrl Pts',(-71.1771795679088,21.8385342042356,12.));
#88379=CARTESIAN_POINT('Ctrl Pts',(-71.1663065220513,22.0366423876811,-5.55111512312578E-16));
#88380=CARTESIAN_POINT('Ctrl Pts',(-71.1663065220513,22.0366423876811,4.));
#88381=CARTESIAN_POINT('Ctrl Pts',(-71.1663065220513,22.0366423876811,8.00000000000001));
#88382=CARTESIAN_POINT('Ctrl Pts',(-71.1663065220513,22.0366423876811,12.));
#88383=CARTESIAN_POINT('Ctrl Pts',(-71.1418425484898,22.1153394458694,-5.55111512312578E-16));
#88384=CARTESIAN_POINT('Ctrl Pts',(-71.1418425484898,22.1153394458694,4.));
#88385=CARTESIAN_POINT('Ctrl Pts',(-71.1418425484898,22.1153394458694,8.));
#88386=CARTESIAN_POINT('Ctrl Pts',(-71.1418425484898,22.1153394458694,12.));
#88387=CARTESIAN_POINT('',(-70.9934796069113,21.5904919935059,2.77555756156289E-16));
#88388=CARTESIAN_POINT('',(-71.1418425484889,22.1153394458691,0.));
#88389=CARTESIAN_POINT('Ctrl Pts',(-70.9934796069113,21.5904919935059,-1.38777878078145E-16));
#88390=CARTESIAN_POINT('Ctrl Pts',(-71.0762040404458,21.6628164325797,-1.38777878078145E-16));
#88391=CARTESIAN_POINT('Ctrl Pts',(-71.1339043418532,21.7632265878116,-1.38777878078144E-16));
#88392=CARTESIAN_POINT('Ctrl Pts',(-71.1550826601356,21.8709478979137,-1.38777878078145E-16));
#88393=CARTESIAN_POINT('Ctrl Pts',(-71.1709663988474,21.9517388804902,-1.38777878078145E-16));
#88394=CARTESIAN_POINT('Ctrl Pts',(-71.1663065220513,22.0366423876811,-1.38777878078145E-16));
#88395=CARTESIAN_POINT('Ctrl Pts',(-71.1418425484898,22.1153394458694,-1.38777878078145E-16));
#88396=CARTESIAN_POINT('',(-71.1418425484889,22.1153394458691,12.));
#88397=CARTESIAN_POINT('Ctrl Pts',(-71.1418425484898,22.1153394458694,-5.55111512312578E-16));
#88398=CARTESIAN_POINT('Ctrl Pts',(-71.1418425484898,22.1153394458694,4.));
#88399=CARTESIAN_POINT('Ctrl Pts',(-71.1418425484898,22.1153394458694,8.));
#88400=CARTESIAN_POINT('Ctrl Pts',(-71.1418425484898,22.1153394458694,12.));
#88401=CARTESIAN_POINT('',(-70.9934796069113,21.5904919935059,12.));
#88402=CARTESIAN_POINT('Ctrl Pts',(-71.1418425484898,22.1153394458694,12.));
#88403=CARTESIAN_POINT('Ctrl Pts',(-71.1663065220513,22.0366423876811,12.));
#88404=CARTESIAN_POINT('Ctrl Pts',(-71.1709663988474,21.9517388804902,12.));
#88405=CARTESIAN_POINT('Ctrl Pts',(-71.1550826601356,21.8709478979137,12.));
#88406=CARTESIAN_POINT('Ctrl Pts',(-71.1339043418532,21.7632265878116,12.));
#88407=CARTESIAN_POINT('Ctrl Pts',(-71.0762040404458,21.6628164325797,12.));
#88408=CARTESIAN_POINT('Ctrl Pts',(-70.9934796069113,21.5904919935059,12.));
#88409=CARTESIAN_POINT('Ctrl Pts',(-70.9934796069113,21.5904919935059,12.));
#88410=CARTESIAN_POINT('Ctrl Pts',(-70.9934796069113,21.5904919935059,8.));
#88411=CARTESIAN_POINT('Ctrl Pts',(-70.9934796069113,21.5904919935059,4.));
#88412=CARTESIAN_POINT('Ctrl Pts',(-70.9934796069113,21.5904919935059,-5.55111512312578E-16));
#88413=CARTESIAN_POINT('Origin',(-3.57524700084383E-10,1.12623029467293E-10,
0.));
#88414=CARTESIAN_POINT('Origin',(-3.57524700084383E-10,1.12623029467293E-10,
12.));
#88415=CARTESIAN_POINT('Origin',(-3.57524700084383E-10,1.12623029467293E-10,
0.));
#88416=CARTESIAN_POINT('Ctrl Pts',(-68.7132793373328,28.7877620302391,-5.55111512312578E-16));
#88417=CARTESIAN_POINT('Ctrl Pts',(-68.7132793373328,28.7877620302391,4.));
#88418=CARTESIAN_POINT('Ctrl Pts',(-68.7132793373328,28.7877620302391,8.));
#88419=CARTESIAN_POINT('Ctrl Pts',(-68.7132793373328,28.7877620302391,12.));
#88420=CARTESIAN_POINT('Ctrl Pts',(-68.6708193334379,28.8891094745186,-5.55111512312578E-16));
#88421=CARTESIAN_POINT('Ctrl Pts',(-68.6708193334379,28.8891094745186,4.));
#88422=CARTESIAN_POINT('Ctrl Pts',(-68.6708193334379,28.8891094745186,8.));
#88423=CARTESIAN_POINT('Ctrl Pts',(-68.6708193334379,28.8891094745186,12.));
#88424=CARTESIAN_POINT('Ctrl Pts',(-68.5360395709812,29.0404604348957,-5.55111512312578E-16));
#88425=CARTESIAN_POINT('Ctrl Pts',(-68.5360395709812,29.0404604348957,4.));
#88426=CARTESIAN_POINT('Ctrl Pts',(-68.5360395709812,29.0404604348957,7.99999999999999));
#88427=CARTESIAN_POINT('Ctrl Pts',(-68.5360395709812,29.0404604348957,12.));
#88428=CARTESIAN_POINT('Ctrl Pts',(-68.3446561754307,29.0927805237118,-5.55111512312578E-16));
#88429=CARTESIAN_POINT('Ctrl Pts',(-68.3446561754307,29.0927805237118,4.));
#88430=CARTESIAN_POINT('Ctrl Pts',(-68.3446561754307,29.0927805237118,8.00000000000001));
#88431=CARTESIAN_POINT('Ctrl Pts',(-68.3446561754307,29.0927805237118,12.));
#88432=CARTESIAN_POINT('Ctrl Pts',(-68.2622612909744,29.0944526440248,-5.55111512312578E-16));
#88433=CARTESIAN_POINT('Ctrl Pts',(-68.2622612909744,29.0944526440248,4.));
#88434=CARTESIAN_POINT('Ctrl Pts',(-68.2622612909744,29.0944526440248,8.));
#88435=CARTESIAN_POINT('Ctrl Pts',(-68.2622612909744,29.0944526440248,12.));
#88436=CARTESIAN_POINT('',(-68.7132793373328,28.7877620302391,0.));
#88437=CARTESIAN_POINT('',(-68.2622612909744,29.0944526440249,0.));
#88438=CARTESIAN_POINT('Ctrl Pts',(-68.7132793373328,28.7877620302391,0.));
#88439=CARTESIAN_POINT('Ctrl Pts',(-68.6708193334379,28.8891094745186,-1.54074395550979E-31));
#88440=CARTESIAN_POINT('Ctrl Pts',(-68.5938023263198,28.9755957375912,1.54074395550979E-31));
#88441=CARTESIAN_POINT('Ctrl Pts',(-68.4983025002323,29.0297453895419,7.70371977754892E-32));
#88442=CARTESIAN_POINT('Ctrl Pts',(-68.4266776306666,29.0703576285049,-7.70371977754894E-32));
#88443=CARTESIAN_POINT('Ctrl Pts',(-68.3446561754307,29.0927805237118,-5.39260384428426E-31));
#88444=CARTESIAN_POINT('Ctrl Pts',(-68.2622612909744,29.0944526440248,-7.70371977754895E-32));
#88445=CARTESIAN_POINT('',(-68.2622612909744,29.0944526440249,12.));
#88446=CARTESIAN_POINT('Ctrl Pts',(-68.2622612909744,29.0944526440248,-5.55111512312578E-16));
#88447=CARTESIAN_POINT('Ctrl Pts',(-68.2622612909744,29.0944526440248,4.));
#88448=CARTESIAN_POINT('Ctrl Pts',(-68.2622612909744,29.0944526440248,8.));
#88449=CARTESIAN_POINT('Ctrl Pts',(-68.2622612909744,29.0944526440248,12.));
#88450=CARTESIAN_POINT('',(-68.7132793373328,28.7877620302391,12.));
#88451=CARTESIAN_POINT('Ctrl Pts',(-68.2622612909744,29.0944526440248,12.));
#88452=CARTESIAN_POINT('Ctrl Pts',(-68.3446561754307,29.0927805237118,12.));
#88453=CARTESIAN_POINT('Ctrl Pts',(-68.4266776306666,29.0703576285049,12.));
#88454=CARTESIAN_POINT('Ctrl Pts',(-68.4983025002323,29.0297453895419,12.));
#88455=CARTESIAN_POINT('Ctrl Pts',(-68.5938023263198,28.9755957375912,12.));
#88456=CARTESIAN_POINT('Ctrl Pts',(-68.6708193334379,28.8891094745186,12.));
#88457=CARTESIAN_POINT('Ctrl Pts',(-68.7132793373328,28.7877620302391,12.));
#88458=CARTESIAN_POINT('Ctrl Pts',(-68.7132793373328,28.7877620302391,12.));
#88459=CARTESIAN_POINT('Ctrl Pts',(-68.7132793373328,28.7877620302391,8.));
#88460=CARTESIAN_POINT('Ctrl Pts',(-68.7132793373328,28.7877620302391,4.));
#88461=CARTESIAN_POINT('Ctrl Pts',(-68.7132793373328,28.7877620302391,-5.55111512312578E-16));
#88462=CARTESIAN_POINT('Ctrl Pts',(-63.7976679095314,28.8072485549236,0.));
#88463=CARTESIAN_POINT('Ctrl Pts',(-63.7976679095314,28.8072485549236,12.));
#88464=CARTESIAN_POINT('Ctrl Pts',(-63.8014989507494,28.8078854475432,0.));
#88465=CARTESIAN_POINT('Ctrl Pts',(-63.8014989507494,28.8078854475432,12.));
#88466=CARTESIAN_POINT('Ctrl Pts',(-63.8091667271232,28.8091580239553,0.));
#88467=CARTESIAN_POINT('Ctrl Pts',(-63.8091667271232,28.8091580239553,12.));
#88468=CARTESIAN_POINT('Ctrl Pts',(-63.8206854735028,28.8110632620957,0.));
#88469=CARTESIAN_POINT('Ctrl Pts',(-63.8206854735028,28.8110632620957,12.));
#88470=CARTESIAN_POINT('Ctrl Pts',(-63.8360779669856,28.8135963263368,0.));
#88471=CARTESIAN_POINT('Ctrl Pts',(-63.8360779669856,28.8135963263368,12.));
#88472=CARTESIAN_POINT('Ctrl Pts',(-63.8553755207487,28.8167505576681,0.));
#88473=CARTESIAN_POINT('Ctrl Pts',(-63.8553755207487,28.8167505576681,12.));
#88474=CARTESIAN_POINT('Ctrl Pts',(-63.8747299825313,28.8198926619858,0.));
#88475=CARTESIAN_POINT('Ctrl Pts',(-63.8747299825313,28.8198926619858,12.));
#88476=CARTESIAN_POINT('Ctrl Pts',(-63.8941412856924,28.823022586318,0.));
#88477=CARTESIAN_POINT('Ctrl Pts',(-63.8941412856924,28.823022586318,12.));
#88478=CARTESIAN_POINT('Ctrl Pts',(-63.9136093063786,28.8261402423291,0.));
#88479=CARTESIAN_POINT('Ctrl Pts',(-63.9136093063786,28.8261402423291,12.));
#88480=CARTESIAN_POINT('Ctrl Pts',(-63.9331338646996,28.8292455077559,0.));
#88481=CARTESIAN_POINT('Ctrl Pts',(-63.9331338646996,28.8292455077559,12.));
#88482=CARTESIAN_POINT('Ctrl Pts',(-63.9527147494423,28.8323382413789,0.));
#88483=CARTESIAN_POINT('Ctrl Pts',(-63.9527147494423,28.8323382413789,12.));
#88484=CARTESIAN_POINT('Ctrl Pts',(-63.9723517369614,28.8354182946601,0.));
#88485=CARTESIAN_POINT('Ctrl Pts',(-63.9723517369614,28.8354182946601,12.));
#88486=CARTESIAN_POINT('Ctrl Pts',(-63.9920446117582,28.8384855243243,0.));
#88487=CARTESIAN_POINT('Ctrl Pts',(-63.9920446117582,28.8384855243243,12.));
#88488=CARTESIAN_POINT('Ctrl Pts',(-64.0117931881298,28.8415398056428,0.));
#88489=CARTESIAN_POINT('Ctrl Pts',(-64.0117931881298,28.8415398056428,12.));
#88490=CARTESIAN_POINT('Ctrl Pts',(-64.0315973031942,28.844581028125,0.));
#88491=CARTESIAN_POINT('Ctrl Pts',(-64.0315973031942,28.844581028125,12.));
#88492=CARTESIAN_POINT('Ctrl Pts',(-64.0514568066637,28.8476090892232,0.));
#88493=CARTESIAN_POINT('Ctrl Pts',(-64.0514568066637,28.8476090892232,12.));
#88494=CARTESIAN_POINT('Ctrl Pts',(-64.0713715523599,28.8506238891093,0.));
#88495=CARTESIAN_POINT('Ctrl Pts',(-64.0713715523599,28.8506238891093,12.));
#88496=CARTESIAN_POINT('Ctrl Pts',(-64.0913413876622,28.8536253241854,0.));
#88497=CARTESIAN_POINT('Ctrl Pts',(-64.0913413876622,28.8536253241854,12.));
#88498=CARTESIAN_POINT('Ctrl Pts',(-64.1113661481965,28.8566132838178,0.));
#88499=CARTESIAN_POINT('Ctrl Pts',(-64.1113661481965,28.8566132838178,12.));
#88500=CARTESIAN_POINT('Ctrl Pts',(-64.1314456633381,28.8595876537148,0.));
#88501=CARTESIAN_POINT('Ctrl Pts',(-64.1314456633381,28.8595876537148,12.));
#88502=CARTESIAN_POINT('Ctrl Pts',(-64.1515797596564,28.8625483180437,0.));
#88503=CARTESIAN_POINT('Ctrl Pts',(-64.1515797596564,28.8625483180437,12.));
#88504=CARTESIAN_POINT('Ctrl Pts',(-64.1717682648685,28.8654951618649,0.));
#88505=CARTESIAN_POINT('Ctrl Pts',(-64.1717682648685,28.8654951618649,12.));
#88506=CARTESIAN_POINT('Ctrl Pts',(-64.1920110123299,28.8684280739014,0.));
#88507=CARTESIAN_POINT('Ctrl Pts',(-64.1920110123299,28.8684280739014,12.));
#88508=CARTESIAN_POINT('Ctrl Pts',(-64.2123078408461,28.8713469464185,0.));
#88509=CARTESIAN_POINT('Ctrl Pts',(-64.2123078408461,28.8713469464185,12.));
#88510=CARTESIAN_POINT('Ctrl Pts',(-64.2326585925252,28.8742516738947,0.));
#88511=CARTESIAN_POINT('Ctrl Pts',(-64.2326585925252,28.8742516738947,12.));
#88512=CARTESIAN_POINT('Ctrl Pts',(-64.2530631112929,28.877142152106,0.));
#88513=CARTESIAN_POINT('Ctrl Pts',(-64.2530631112929,28.877142152106,12.));
#88514=CARTESIAN_POINT('Ctrl Pts',(-64.2735212410711,28.8800182770065,0.));
#88515=CARTESIAN_POINT('Ctrl Pts',(-64.2735212410711,28.8800182770065,12.));
#88516=CARTESIAN_POINT('Ctrl Pts',(-64.2940328242521,28.882879943794,0.));
#88517=CARTESIAN_POINT('Ctrl Pts',(-64.2940328242521,28.882879943794,12.));
#88518=CARTESIAN_POINT('Ctrl Pts',(-64.3145977025037,28.8857270473959,0.));
#88519=CARTESIAN_POINT('Ctrl Pts',(-64.3145977025037,28.8857270473959,12.));
#88520=CARTESIAN_POINT('Ctrl Pts',(-64.3352157174619,28.8885594828926,0.));
#88521=CARTESIAN_POINT('Ctrl Pts',(-64.3352157174619,28.8885594828926,12.));
#88522=CARTESIAN_POINT('Ctrl Pts',(-64.3558867114076,28.8913771459323,0.));
#88523=CARTESIAN_POINT('Ctrl Pts',(-64.3558867114076,28.8913771459323,12.));
#88524=CARTESIAN_POINT('Ctrl Pts',(-64.3766105280688,28.89417993323,0.));
#88525=CARTESIAN_POINT('Ctrl Pts',(-64.3766105280688,28.89417993323,12.));
#88526=CARTESIAN_POINT('Ctrl Pts',(-64.397387012917,28.8969677427504,0.));
#88527=CARTESIAN_POINT('Ctrl Pts',(-64.397387012917,28.8969677427504,12.));
#88528=CARTESIAN_POINT('Ctrl Pts',(-64.4182160127379,28.899740473434,0.));
#88529=CARTESIAN_POINT('Ctrl Pts',(-64.4182160127379,28.899740473434,12.));
#88530=CARTESIAN_POINT('Ctrl Pts',(-64.4390973753634,28.9024980250307,0.));
#88531=CARTESIAN_POINT('Ctrl Pts',(-64.4390973753634,28.9024980250307,12.));
#88532=CARTESIAN_POINT('Ctrl Pts',(-64.4600309493583,28.9052402979062,0.));
#88533=CARTESIAN_POINT('Ctrl Pts',(-64.4600309493583,28.9052402979062,12.));
#88534=CARTESIAN_POINT('Ctrl Pts',(-64.4810165836592,28.9079671928264,0.));
#88535=CARTESIAN_POINT('Ctrl Pts',(-64.4810165836592,28.9079671928264,12.));
#88536=CARTESIAN_POINT('Ctrl Pts',(-64.5020541275951,28.910678610965,0.));
#88537=CARTESIAN_POINT('Ctrl Pts',(-64.5020541275951,28.910678610965,12.));
#88538=CARTESIAN_POINT('Ctrl Pts',(-64.523143431047,28.9133744539949,0.));
#88539=CARTESIAN_POINT('Ctrl Pts',(-64.523143431047,28.9133744539949,12.));
#88540=CARTESIAN_POINT('Ctrl Pts',(-64.5442843445559,28.9160546241538,0.));
#88541=CARTESIAN_POINT('Ctrl Pts',(-64.5442843445559,28.9160546241538,12.));
#88542=CARTESIAN_POINT('Ctrl Pts',(-64.5654767194472,28.9187190243224,0.));
#88543=CARTESIAN_POINT('Ctrl Pts',(-64.5654767194472,28.9187190243224,12.));
#88544=CARTESIAN_POINT('Ctrl Pts',(-64.5867204079426,28.9213675580985,0.));
#88545=CARTESIAN_POINT('Ctrl Pts',(-64.5867204079426,28.9213675580985,12.));
#88546=CARTESIAN_POINT('Ctrl Pts',(-64.6080152631039,28.9240001297542,0.));
#88547=CARTESIAN_POINT('Ctrl Pts',(-64.6080152631039,28.9240001297542,12.));
#88548=CARTESIAN_POINT('Ctrl Pts',(-64.629361138774,28.926616644195,0.));
#88549=CARTESIAN_POINT('Ctrl Pts',(-64.629361138774,28.926616644195,12.));
#88550=CARTESIAN_POINT('Ctrl Pts',(-64.6507578895161,28.9292170069221,0.));
#88551=CARTESIAN_POINT('Ctrl Pts',(-64.6507578895161,28.9292170069221,12.));
#88552=CARTESIAN_POINT('Ctrl Pts',(-64.672205370541,28.9318011239915,0.));
#88553=CARTESIAN_POINT('Ctrl Pts',(-64.672205370541,28.9318011239915,12.));
#88554=CARTESIAN_POINT('Ctrl Pts',(-64.6937034376617,28.9343689019882,0.));
#88555=CARTESIAN_POINT('Ctrl Pts',(-64.6937034376617,28.9343689019882,12.));
#88556=CARTESIAN_POINT('Ctrl Pts',(-64.715251947329,28.9369202480393,0.));
#88557=CARTESIAN_POINT('Ctrl Pts',(-64.715251947329,28.9369202480393,12.));
#88558=CARTESIAN_POINT('Ctrl Pts',(-64.7368507566467,28.9394550698204,0.));
#88559=CARTESIAN_POINT('Ctrl Pts',(-64.7368507566467,28.9394550698204,12.));
#88560=CARTESIAN_POINT('Ctrl Pts',(-64.758499723388,28.9419732755656,0.));
#88561=CARTESIAN_POINT('Ctrl Pts',(-64.758499723388,28.9419732755656,12.));
#88562=CARTESIAN_POINT('Ctrl Pts',(-64.7801987060084,28.944474774081,0.));
#88563=CARTESIAN_POINT('Ctrl Pts',(-64.7801987060084,28.944474774081,12.));
#88564=CARTESIAN_POINT('Ctrl Pts',(-64.8019475636442,28.9469594747431,0.));
#88565=CARTESIAN_POINT('Ctrl Pts',(-64.8019475636442,28.9469594747431,12.));
#88566=CARTESIAN_POINT('Ctrl Pts',(-64.8237461561019,28.9494272874832,0.));
#88567=CARTESIAN_POINT('Ctrl Pts',(-64.8237461561019,28.9494272874832,12.));
#88568=CARTESIAN_POINT('Ctrl Pts',(-64.8455943438423,28.9518781227765,0.));
#88569=CARTESIAN_POINT('Ctrl Pts',(-64.8455943438423,28.9518781227765,12.));
#88570=CARTESIAN_POINT('Ctrl Pts',(-64.8674919879648,28.9543118916328,0.));
#88571=CARTESIAN_POINT('Ctrl Pts',(-64.8674919879648,28.9543118916328,12.));
#88572=CARTESIAN_POINT('Ctrl Pts',(-64.8894389501801,28.9567285055866,0.));
#88573=CARTESIAN_POINT('Ctrl Pts',(-64.8894389501801,28.9567285055866,12.));
#88574=CARTESIAN_POINT('Ctrl Pts',(-64.9114350928125,28.9591278766934,0.));
#88575=CARTESIAN_POINT('Ctrl Pts',(-64.9114350928125,28.9591278766934,12.));
#88576=CARTESIAN_POINT('Ctrl Pts',(-64.9334802788038,28.9615099175249,0.));
#88577=CARTESIAN_POINT('Ctrl Pts',(-64.9334802788038,28.9615099175249,12.));
#88578=CARTESIAN_POINT('Ctrl Pts',(-64.955574371711,28.9638745411677,0.));
#88579=CARTESIAN_POINT('Ctrl Pts',(-64.955574371711,28.9638745411677,12.));
#88580=CARTESIAN_POINT('Ctrl Pts',(-64.9777172357027,28.9662216612217,0.));
#88581=CARTESIAN_POINT('Ctrl Pts',(-64.9777172357027,28.9662216612217,12.));
#88582=CARTESIAN_POINT('Ctrl Pts',(-64.9999087355504,28.9685511918018,0.));
#88583=CARTESIAN_POINT('Ctrl Pts',(-64.9999087355504,28.9685511918018,12.));
#88584=CARTESIAN_POINT('Ctrl Pts',(-65.022148736628,28.97086304753,0.));
#88585=CARTESIAN_POINT('Ctrl Pts',(-65.022148736628,28.97086304753,12.));
#88586=CARTESIAN_POINT('Ctrl Pts',(-65.0444371049082,28.9731571435282,0.));
#88587=CARTESIAN_POINT('Ctrl Pts',(-65.0444371049082,28.9731571435282,12.));
#88588=CARTESIAN_POINT('Ctrl Pts',(-65.0667737069563,28.9754333954135,0.));
#88589=CARTESIAN_POINT('Ctrl Pts',(-65.0667737069563,28.9754333954135,12.));
#88590=CARTESIAN_POINT('Ctrl Pts',(-65.0891584099168,28.9776917192933,0.));
#88591=CARTESIAN_POINT('Ctrl Pts',(-65.0891584099168,28.9776917192933,12.));
#88592=CARTESIAN_POINT('Ctrl Pts',(-65.1115910815037,28.9799320317641,0.));
#88593=CARTESIAN_POINT('Ctrl Pts',(-65.1115910815037,28.9799320317641,12.));
#88594=CARTESIAN_POINT('Ctrl Pts',(-65.1340715900028,28.9821542499042,0.));
#88595=CARTESIAN_POINT('Ctrl Pts',(-65.1340715900028,28.9821542499042,12.));
#88596=CARTESIAN_POINT('Ctrl Pts',(-65.1565998042697,28.9843582912692,0.));
#88597=CARTESIAN_POINT('Ctrl Pts',(-65.1565998042697,28.9843582912692,12.));
#88598=CARTESIAN_POINT('Ctrl Pts',(-65.1791755937256,28.9865440738884,0.));
#88599=CARTESIAN_POINT('Ctrl Pts',(-65.1791755937256,28.9865440738884,12.));
#88600=CARTESIAN_POINT('Ctrl Pts',(-65.2017988283479,28.9887115162633,0.));
#88601=CARTESIAN_POINT('Ctrl Pts',(-65.2017988283479,28.9887115162633,12.));
#88602=CARTESIAN_POINT('Ctrl Pts',(-65.2244693786609,28.9908605373663,0.));
#88603=CARTESIAN_POINT('Ctrl Pts',(-65.2244693786609,28.9908605373663,12.));
#88604=CARTESIAN_POINT('Ctrl Pts',(-65.2471871157397,28.9929910566325,0.));
#88605=CARTESIAN_POINT('Ctrl Pts',(-65.2471871157397,28.9929910566325,12.));
#88606=CARTESIAN_POINT('Ctrl Pts',(-65.2699519112064,28.9951029939557,0.));
#88607=CARTESIAN_POINT('Ctrl Pts',(-65.2699519112064,28.9951029939557,12.));
#88608=CARTESIAN_POINT('Ctrl Pts',(-65.2927636372254,28.9971962696845,0.));
#88609=CARTESIAN_POINT('Ctrl Pts',(-65.2927636372254,28.9971962696845,12.));
#88610=CARTESIAN_POINT('Ctrl Pts',(-65.3156221664916,28.9992708046211,0.));
#88611=CARTESIAN_POINT('Ctrl Pts',(-65.3156221664916,28.9992708046211,12.));
#88612=CARTESIAN_POINT('Ctrl Pts',(-65.3385273722242,29.0013265200185,0.));
#88613=CARTESIAN_POINT('Ctrl Pts',(-65.3385273722242,29.0013265200185,12.));
#88614=CARTESIAN_POINT('Ctrl Pts',(-65.3614791281692,29.003363337573,0.));
#88615=CARTESIAN_POINT('Ctrl Pts',(-65.3614791281692,29.003363337573,12.));
#88616=CARTESIAN_POINT('Ctrl Pts',(-65.3844773085961,29.0053811794207,0.));
#88617=CARTESIAN_POINT('Ctrl Pts',(-65.3844773085961,29.0053811794207,12.));
#88618=CARTESIAN_POINT('Ctrl Pts',(-65.4075217882934,29.0073799681342,0.));
#88619=CARTESIAN_POINT('Ctrl Pts',(-65.4075217882934,29.0073799681342,12.));
#88620=CARTESIAN_POINT('Ctrl Pts',(-65.4306124425562,29.0093596267215,0.));
#88621=CARTESIAN_POINT('Ctrl Pts',(-65.4306124425562,29.0093596267215,12.));
#88622=CARTESIAN_POINT('Ctrl Pts',(-65.4537491471828,29.0113200786239,0.));
#88623=CARTESIAN_POINT('Ctrl Pts',(-65.4537491471828,29.0113200786239,12.));
#88624=CARTESIAN_POINT('Ctrl Pts',(-65.4769317784789,29.013261247709,0.));
#88625=CARTESIAN_POINT('Ctrl Pts',(-65.4769317784789,29.013261247709,12.));
#88626=CARTESIAN_POINT('Ctrl Pts',(-65.5001602132535,29.0151830582675,0.));
#88627=CARTESIAN_POINT('Ctrl Pts',(-65.5001602132535,29.0151830582675,12.));
#88628=CARTESIAN_POINT('Ctrl Pts',(-65.5234343288136,29.0170854350095,0.));
#88629=CARTESIAN_POINT('Ctrl Pts',(-65.5234343288136,29.0170854350095,12.));
#88630=CARTESIAN_POINT('Ctrl Pts',(-65.5467540029514,29.0189683030642,0.));
#88631=CARTESIAN_POINT('Ctrl Pts',(-65.5467540029514,29.0189683030642,12.));
#88632=CARTESIAN_POINT('Ctrl Pts',(-65.5701191139418,29.0208315879764,0.));
#88633=CARTESIAN_POINT('Ctrl Pts',(-65.5701191139418,29.0208315879764,12.));
#88634=CARTESIAN_POINT('Ctrl Pts',(-65.5935295405453,29.0226752157003,0.));
#88635=CARTESIAN_POINT('Ctrl Pts',(-65.5935295405453,29.0226752157003,12.));
#88636=CARTESIAN_POINT('Ctrl Pts',(-65.6169851620046,29.0244991125959,0.));
#88637=CARTESIAN_POINT('Ctrl Pts',(-65.6169851620046,29.0244991125959,12.));
#88638=CARTESIAN_POINT('Ctrl Pts',(-65.6404858580403,29.0263032054266,0.));
#88639=CARTESIAN_POINT('Ctrl Pts',(-65.6404858580403,29.0263032054266,12.));
#88640=CARTESIAN_POINT('Ctrl Pts',(-65.6640315088388,29.0280874213596,0.));
#88641=CARTESIAN_POINT('Ctrl Pts',(-65.6640315088388,29.0280874213596,12.));
#88642=CARTESIAN_POINT('Ctrl Pts',(-65.6876219950493,29.0298516879611,0.));
#88643=CARTESIAN_POINT('Ctrl Pts',(-65.6876219950493,29.0298516879611,12.));
#88644=CARTESIAN_POINT('Ctrl Pts',(-65.7112571977891,29.0315959331919,0.));
#88645=CARTESIAN_POINT('Ctrl Pts',(-65.7112571977891,29.0315959331919,12.));
#88646=CARTESIAN_POINT('Ctrl Pts',(-65.7349369986384,29.0333200854027,0.));
#88647=CARTESIAN_POINT('Ctrl Pts',(-65.7349369986384,29.0333200854027,12.));
#88648=CARTESIAN_POINT('Ctrl Pts',(-65.7586612796368,29.035024073333,0.));
#88649=CARTESIAN_POINT('Ctrl Pts',(-65.7586612796368,29.035024073333,12.));
#88650=CARTESIAN_POINT('Ctrl Pts',(-65.7824299232705,29.0367078261103,0.));
#88651=CARTESIAN_POINT('Ctrl Pts',(-65.7824299232705,29.0367078261103,12.));
#88652=CARTESIAN_POINT('Ctrl Pts',(-65.8062428124713,29.0383712732469,0.));
#88653=CARTESIAN_POINT('Ctrl Pts',(-65.8062428124713,29.0383712732469,12.));
#88654=CARTESIAN_POINT('Ctrl Pts',(-65.8300998306191,29.0400143446338,0.));
#88655=CARTESIAN_POINT('Ctrl Pts',(-65.8300998306191,29.0400143446338,12.));
#88656=CARTESIAN_POINT('Ctrl Pts',(-65.854000861539,29.0416369705375,0.));
#88657=CARTESIAN_POINT('Ctrl Pts',(-65.854000861539,29.0416369705375,12.));
#88658=CARTESIAN_POINT('Ctrl Pts',(-65.8779457894961,29.0432390815978,0.));
#88659=CARTESIAN_POINT('Ctrl Pts',(-65.8779457894961,29.0432390815978,12.));
#88660=CARTESIAN_POINT('Ctrl Pts',(-65.9019344991854,29.0448206088288,0.));
#88661=CARTESIAN_POINT('Ctrl Pts',(-65.9019344991854,29.0448206088288,12.));
#88662=CARTESIAN_POINT('Ctrl Pts',(-65.9259668757307,29.0463814836157,0.));
#88663=CARTESIAN_POINT('Ctrl Pts',(-65.9259668757307,29.0463814836157,12.));
#88664=CARTESIAN_POINT('Ctrl Pts',(-65.9500428046868,29.0479216377081,0.));
#88665=CARTESIAN_POINT('Ctrl Pts',(-65.9500428046868,29.0479216377081,12.));
#88666=CARTESIAN_POINT('Ctrl Pts',(-65.974162172037,29.0494410032172,0.));
#88667=CARTESIAN_POINT('Ctrl Pts',(-65.974162172037,29.0494410032172,12.));
#88668=CARTESIAN_POINT('Ctrl Pts',(-65.9983248641879,29.0509395126142,0.));
#88669=CARTESIAN_POINT('Ctrl Pts',(-65.9983248641879,29.0509395126142,12.));
#88670=CARTESIAN_POINT('Ctrl Pts',(-66.0225307679591,29.0524170987307,0.));
#88671=CARTESIAN_POINT('Ctrl Pts',(-66.0225307679591,29.0524170987307,12.));
#88672=CARTESIAN_POINT('Ctrl Pts',(-66.0467797705815,29.0538736947552,0.));
#88673=CARTESIAN_POINT('Ctrl Pts',(-66.0467797705815,29.0538736947552,12.));
#88674=CARTESIAN_POINT('Ctrl Pts',(-66.0710717597009,29.0553092342278,0.));
#88675=CARTESIAN_POINT('Ctrl Pts',(-66.0710717597009,29.0553092342278,12.));
#88676=CARTESIAN_POINT('Ctrl Pts',(-66.0954066233754,29.0567236510373,0.));
#88677=CARTESIAN_POINT('Ctrl Pts',(-66.0954066233754,29.0567236510373,12.));
#88678=CARTESIAN_POINT('Ctrl Pts',(-66.1197842500711,29.0581168794189,0.));
#88679=CARTESIAN_POINT('Ctrl Pts',(-66.1197842500711,29.0581168794189,12.));
#88680=CARTESIAN_POINT('Ctrl Pts',(-66.1442045286516,29.0594888539555,0.));
#88681=CARTESIAN_POINT('Ctrl Pts',(-66.1442045286516,29.0594888539555,12.));
#88682=CARTESIAN_POINT('Ctrl Pts',(-66.1686673483755,29.0608395095745,0.));
#88683=CARTESIAN_POINT('Ctrl Pts',(-66.1686673483755,29.0608395095745,12.));
#88684=CARTESIAN_POINT('Ctrl Pts',(-66.1931725989008,29.062168781542,0.));
#88685=CARTESIAN_POINT('Ctrl Pts',(-66.1931725989008,29.062168781542,12.));
#88686=CARTESIAN_POINT('Ctrl Pts',(-66.2177201702819,29.0634766054599,0.));
#88687=CARTESIAN_POINT('Ctrl Pts',(-66.2177201702819,29.0634766054599,12.));
#88688=CARTESIAN_POINT('Ctrl Pts',(-66.2423099529668,29.0647629172645,0.));
#88689=CARTESIAN_POINT('Ctrl Pts',(-66.2423099529668,29.0647629172645,12.));
#88690=CARTESIAN_POINT('Ctrl Pts',(-66.2669418377866,29.0660276532272,0.));
#88691=CARTESIAN_POINT('Ctrl Pts',(-66.2669418377866,29.0660276532272,12.));
#88692=CARTESIAN_POINT('Ctrl Pts',(-66.2916157159528,29.0672707499527,0.));
#88693=CARTESIAN_POINT('Ctrl Pts',(-66.2916157159528,29.0672707499527,12.));
#88694=CARTESIAN_POINT('Ctrl Pts',(-66.3163314790607,29.0684921443718,0.));
#88695=CARTESIAN_POINT('Ctrl Pts',(-66.3163314790607,29.0684921443718,12.));
#88696=CARTESIAN_POINT('Ctrl Pts',(-66.3410890190879,29.0696917737397,0.));
#88697=CARTESIAN_POINT('Ctrl Pts',(-66.3410890190879,29.0696917737397,12.));
#88698=CARTESIAN_POINT('Ctrl Pts',(-66.3658882283906,29.0708695756335,0.));
#88699=CARTESIAN_POINT('Ctrl Pts',(-66.3658882283906,29.0708695756335,12.));
#88700=CARTESIAN_POINT('Ctrl Pts',(-66.3907289996942,29.0720254879535,0.));
#88701=CARTESIAN_POINT('Ctrl Pts',(-66.3907289996942,29.0720254879535,12.));
#88702=CARTESIAN_POINT('Ctrl Pts',(-66.4156112260904,29.0731594489218,0.));
#88703=CARTESIAN_POINT('Ctrl Pts',(-66.4156112260904,29.0731594489218,12.));
#88704=CARTESIAN_POINT('Ctrl Pts',(-66.4405348010404,29.0742713970762,0.));
#88705=CARTESIAN_POINT('Ctrl Pts',(-66.4405348010404,29.0742713970762,12.));
#88706=CARTESIAN_POINT('Ctrl Pts',(-66.4654996183739,29.0753612712669,0.));
#88707=CARTESIAN_POINT('Ctrl Pts',(-66.4654996183739,29.0753612712669,12.));
#88708=CARTESIAN_POINT('Ctrl Pts',(-66.4905055722864,29.0764290106553,0.));
#88709=CARTESIAN_POINT('Ctrl Pts',(-66.4905055722864,29.0764290106553,12.));
#88710=CARTESIAN_POINT('Ctrl Pts',(-66.5155525573308,29.0774745547146,0.));
#88711=CARTESIAN_POINT('Ctrl Pts',(-66.5155525573308,29.0774745547146,12.));
#88712=CARTESIAN_POINT('Ctrl Pts',(-66.5406404684116,29.0784978432294,0.));
#88713=CARTESIAN_POINT('Ctrl Pts',(-66.5406404684116,29.0784978432294,12.));
#88714=CARTESIAN_POINT('Ctrl Pts',(-66.5657692007894,29.0794988162892,0.));
#88715=CARTESIAN_POINT('Ctrl Pts',(-66.5657692007894,29.0794988162892,12.));
#88716=CARTESIAN_POINT('Ctrl Pts',(-66.5909386500796,29.0804774142852,0.));
#88717=CARTESIAN_POINT('Ctrl Pts',(-66.5909386500796,29.0804774142852,12.));
#88718=CARTESIAN_POINT('Ctrl Pts',(-66.6161487122504,29.0814335779085,0.));
#88719=CARTESIAN_POINT('Ctrl Pts',(-66.6161487122504,29.0814335779085,12.));
#88720=CARTESIAN_POINT('Ctrl Pts',(-66.6413992836148,29.0823672481508,0.));
#88721=CARTESIAN_POINT('Ctrl Pts',(-66.6413992836148,29.0823672481508,12.));
#88722=CARTESIAN_POINT('Ctrl Pts',(-66.6666902608246,29.0832783663048,0.));
#88723=CARTESIAN_POINT('Ctrl Pts',(-66.6666902608246,29.0832783663048,12.));
#88724=CARTESIAN_POINT('Ctrl Pts',(-66.6920215408744,29.0841668739585,0.));
#88725=CARTESIAN_POINT('Ctrl Pts',(-66.6920215408744,29.0841668739585,12.));
#88726=CARTESIAN_POINT('Ctrl Pts',(-66.7173930211015,29.0850327129913,0.));
#88727=CARTESIAN_POINT('Ctrl Pts',(-66.7173930211015,29.0850327129913,12.));
#88728=CARTESIAN_POINT('Ctrl Pts',(-66.7428045991841,29.0858758255729,0.));
#88729=CARTESIAN_POINT('Ctrl Pts',(-66.7428045991841,29.0858758255729,12.));
#88730=CARTESIAN_POINT('Ctrl Pts',(-66.7682561731349,29.0866961541629,0.));
#88731=CARTESIAN_POINT('Ctrl Pts',(-66.7682561731349,29.0866961541629,12.));
#88732=CARTESIAN_POINT('Ctrl Pts',(-66.7937476412941,29.0874936415138,0.));
#88733=CARTESIAN_POINT('Ctrl Pts',(-66.7937476412941,29.0874936415138,12.));
#88734=CARTESIAN_POINT('Ctrl Pts',(-66.8192789023323,29.0882682306636,0.));
#88735=CARTESIAN_POINT('Ctrl Pts',(-66.8192789023323,29.0882682306636,12.));
#88736=CARTESIAN_POINT('Ctrl Pts',(-66.8448498552508,29.0890198649327,0.));
#88737=CARTESIAN_POINT('Ctrl Pts',(-66.8448498552508,29.0890198649327,12.));
#88738=CARTESIAN_POINT('Ctrl Pts',(-66.8704603993794,29.0897484879207,0.));
#88739=CARTESIAN_POINT('Ctrl Pts',(-66.8704603993794,29.0897484879207,12.));
#88740=CARTESIAN_POINT('Ctrl Pts',(-66.8961104343703,29.0904540435063,0.));
#88741=CARTESIAN_POINT('Ctrl Pts',(-66.8961104343703,29.0904540435063,12.));
#88742=CARTESIAN_POINT('Ctrl Pts',(-66.9217998601881,29.0911364758484,0.));
#88743=CARTESIAN_POINT('Ctrl Pts',(-66.9217998601881,29.0911364758484,12.));
#88744=CARTESIAN_POINT('Ctrl Pts',(-66.9475285771133,29.0917957293824,0.));
#88745=CARTESIAN_POINT('Ctrl Pts',(-66.9475285771133,29.0917957293824,12.));
#88746=CARTESIAN_POINT('Ctrl Pts',(-66.9732964857467,29.092431748817,0.));
#88747=CARTESIAN_POINT('Ctrl Pts',(-66.9732964857467,29.092431748817,12.));
#88748=CARTESIAN_POINT('Ctrl Pts',(-66.9991034870084,29.0930444791329,0.));
#88749=CARTESIAN_POINT('Ctrl Pts',(-66.9991034870084,29.0930444791329,12.));
#88750=CARTESIAN_POINT('Ctrl Pts',(-67.0249494821361,29.0936338655828,0.));
#88751=CARTESIAN_POINT('Ctrl Pts',(-67.0249494821361,29.0936338655828,12.));
#88752=CARTESIAN_POINT('Ctrl Pts',(-67.0508343726771,29.0941998536957,0.));
#88753=CARTESIAN_POINT('Ctrl Pts',(-67.0508343726771,29.0941998536957,12.));
#88754=CARTESIAN_POINT('Ctrl Pts',(-67.0767580604872,29.0947423892725,0.));
#88755=CARTESIAN_POINT('Ctrl Pts',(-67.0767580604872,29.0947423892725,12.));
#88756=CARTESIAN_POINT('Ctrl Pts',(-67.1027204477304,29.0952614183777,0.));
#88757=CARTESIAN_POINT('Ctrl Pts',(-67.1027204477304,29.0952614183777,12.));
#88758=CARTESIAN_POINT('Ctrl Pts',(-67.1287214368743,29.0957568873357,0.));
#88759=CARTESIAN_POINT('Ctrl Pts',(-67.1287214368743,29.0957568873357,12.));
#88760=CARTESIAN_POINT('Ctrl Pts',(-67.1547609306845,29.0962287427274,0.));
#88761=CARTESIAN_POINT('Ctrl Pts',(-67.1547609306845,29.0962287427274,12.));
#88762=CARTESIAN_POINT('Ctrl Pts',(-67.1808388322116,29.0966769313893,0.));
#88763=CARTESIAN_POINT('Ctrl Pts',(-67.1808388322116,29.0966769313893,12.));
#88764=CARTESIAN_POINT('Ctrl Pts',(-67.2069550447895,29.0971014004134,0.));
#88765=CARTESIAN_POINT('Ctrl Pts',(-67.2069550447895,29.0971014004134,12.));
#88766=CARTESIAN_POINT('Ctrl Pts',(-67.2331094720482,29.0975020971473,0.));
#88767=CARTESIAN_POINT('Ctrl Pts',(-67.2331094720482,29.0975020971473,12.));
#88768=CARTESIAN_POINT('Ctrl Pts',(-67.2593020179216,29.0978789691965,0.));
#88769=CARTESIAN_POINT('Ctrl Pts',(-67.2593020179216,29.0978789691965,12.));
#88770=CARTESIAN_POINT('Ctrl Pts',(-67.2855325866516,29.0982319644276,0.));
#88771=CARTESIAN_POINT('Ctrl Pts',(-67.2855325866516,29.0982319644276,12.));
#88772=CARTESIAN_POINT('Ctrl Pts',(-67.311801082791,29.0985610309768,0.));
#88773=CARTESIAN_POINT('Ctrl Pts',(-67.311801082791,29.0985610309768,12.));
#88774=CARTESIAN_POINT('Ctrl Pts',(-67.3381074112013,29.0988661172526,0.));
#88775=CARTESIAN_POINT('Ctrl Pts',(-67.3381074112013,29.0988661172526,12.));
#88776=CARTESIAN_POINT('Ctrl Pts',(-67.3644514770373,29.0991471719172,0.));
#88777=CARTESIAN_POINT('Ctrl Pts',(-67.3644514770373,29.0991471719172,12.));
#88778=CARTESIAN_POINT('Ctrl Pts',(-67.3908331857313,29.0994041438715,0.));
#88779=CARTESIAN_POINT('Ctrl Pts',(-67.3908331857313,29.0994041438715,12.));
#88780=CARTESIAN_POINT('Ctrl Pts',(-67.4172524429726,29.0996369822418,0.));
#88781=CARTESIAN_POINT('Ctrl Pts',(-67.4172524429726,29.0996369822418,12.));
#88782=CARTESIAN_POINT('Ctrl Pts',(-67.4437091546869,29.0998456363687,0.));
#88783=CARTESIAN_POINT('Ctrl Pts',(-67.4437091546869,29.0998456363687,12.));
#88784=CARTESIAN_POINT('Ctrl Pts',(-67.4702032270063,29.1000300557961,0.));
#88785=CARTESIAN_POINT('Ctrl Pts',(-67.4702032270063,29.1000300557961,12.));
#88786=CARTESIAN_POINT('Ctrl Pts',(-67.496734566311,29.1001901902915,0.));
#88787=CARTESIAN_POINT('Ctrl Pts',(-67.496734566311,29.1001901902915,12.));
#88788=CARTESIAN_POINT('Ctrl Pts',(-67.5233030792714,29.1003259898686,0.));
#88789=CARTESIAN_POINT('Ctrl Pts',(-67.5233030792714,29.1003259898686,12.));
#88790=CARTESIAN_POINT('Ctrl Pts',(-67.5499086728891,29.1004374048149,0.));
#88791=CARTESIAN_POINT('Ctrl Pts',(-67.5499086728891,29.1004374048149,12.));
#88792=CARTESIAN_POINT('Ctrl Pts',(-67.5765512545277,29.1005243857137,0.));
#88793=CARTESIAN_POINT('Ctrl Pts',(-67.5765512545277,29.1005243857137,12.));
#88794=CARTESIAN_POINT('Ctrl Pts',(-67.6032307319614,29.1005868834863,0.));
#88795=CARTESIAN_POINT('Ctrl Pts',(-67.6032307319614,29.1005868834863,12.));
#88796=CARTESIAN_POINT('Ctrl Pts',(-67.6299470133286,29.1006248493576,0.));
#88797=CARTESIAN_POINT('Ctrl Pts',(-67.6299470133286,29.1006248493576,12.));
#88798=CARTESIAN_POINT('Ctrl Pts',(-67.6567000070319,29.1006382347812,0.));
#88799=CARTESIAN_POINT('Ctrl Pts',(-67.6567000070319,29.1006382347812,12.));
#88800=CARTESIAN_POINT('Ctrl Pts',(-67.6834896216458,29.1006269913747,0.));
#88801=CARTESIAN_POINT('Ctrl Pts',(-67.6834896216458,29.1006269913747,12.));
#88802=CARTESIAN_POINT('Ctrl Pts',(-67.7103157658297,29.1005910708624,0.));
#88803=CARTESIAN_POINT('Ctrl Pts',(-67.7103157658297,29.1005910708624,12.));
#88804=CARTESIAN_POINT('Ctrl Pts',(-67.7371783482039,29.1005304249989,0.));
#88805=CARTESIAN_POINT('Ctrl Pts',(-67.7371783482039,29.1005304249989,12.));
#88806=CARTESIAN_POINT('Ctrl Pts',(-67.7640772773397,29.1004450055647,0.));
#88807=CARTESIAN_POINT('Ctrl Pts',(-67.7640772773397,29.1004450055647,12.));
#88808=CARTESIAN_POINT('Ctrl Pts',(-67.7910124620149,29.1003347645299,0.));
#88809=CARTESIAN_POINT('Ctrl Pts',(-67.7910124620149,29.1003347645299,12.));
#88810=CARTESIAN_POINT('Ctrl Pts',(-67.8179838114109,29.1001996541846,0.));
#88811=CARTESIAN_POINT('Ctrl Pts',(-67.8179838114109,29.1001996541846,12.));
#88812=CARTESIAN_POINT('Ctrl Pts',(-67.844991235333,29.1000396272868,0.));
#88813=CARTESIAN_POINT('Ctrl Pts',(-67.844991235333,29.1000396272868,12.));
#88814=CARTESIAN_POINT('Ctrl Pts',(-67.8720346444111,29.0998546372027,0.));
#88815=CARTESIAN_POINT('Ctrl Pts',(-67.8720346444111,29.0998546372027,12.));
#88816=CARTESIAN_POINT('Ctrl Pts',(-67.8991139503168,29.0996446380617,0.));
#88817=CARTESIAN_POINT('Ctrl Pts',(-67.8991139503168,29.0996446380617,12.));
#88818=CARTESIAN_POINT('Ctrl Pts',(-67.9262290652797,29.0994095844208,0.));
#88819=CARTESIAN_POINT('Ctrl Pts',(-67.9262290652797,29.0994095844208,12.));
#88820=CARTESIAN_POINT('Ctrl Pts',(-67.9533799016122,29.0991494309394,0.));
#88821=CARTESIAN_POINT('Ctrl Pts',(-67.9533799016122,29.0991494309394,12.));
#88822=CARTESIAN_POINT('Ctrl Pts',(-67.9805663711845,29.0988641320243,0.));
#88823=CARTESIAN_POINT('Ctrl Pts',(-67.9805663711845,29.0988641320243,12.));
#88824=CARTESIAN_POINT('Ctrl Pts',(-68.0077883850136,29.0985536415537,0.));
#88825=CARTESIAN_POINT('Ctrl Pts',(-68.0077883850136,29.0985536415537,12.));
#88826=CARTESIAN_POINT('Ctrl Pts',(-68.0350458525589,29.0982179124112,0.));
#88827=CARTESIAN_POINT('Ctrl Pts',(-68.0350458525589,29.0982179124112,12.));
#88828=CARTESIAN_POINT('Ctrl Pts',(-68.0623386822917,29.0978568968677,0.));
#88829=CARTESIAN_POINT('Ctrl Pts',(-68.0623386822917,29.0978568968677,12.));
#88830=CARTESIAN_POINT('Ctrl Pts',(-68.089666782962,29.0974705474279,0.));
#88831=CARTESIAN_POINT('Ctrl Pts',(-68.089666782962,29.0974705474279,12.));
#88832=CARTESIAN_POINT('Ctrl Pts',(-68.1170300647019,29.097058817574,0.));
#88833=CARTESIAN_POINT('Ctrl Pts',(-68.1170300647019,29.097058817574,12.));
#88834=CARTESIAN_POINT('Ctrl Pts',(-68.1444284400734,29.096621662474,0.));
#88835=CARTESIAN_POINT('Ctrl Pts',(-68.1444284400734,29.096621662474,12.));
#88836=CARTESIAN_POINT('Ctrl Pts',(-68.1718618254221,29.0961590399023,0.));
#88837=CARTESIAN_POINT('Ctrl Pts',(-68.1718618254221,29.0961590399023,12.));
#88838=CARTESIAN_POINT('Ctrl Pts',(-68.1993301411959,29.0956709104588,0.));
#88839=CARTESIAN_POINT('Ctrl Pts',(-68.1993301411959,29.0956709104588,12.));
#88840=CARTESIAN_POINT('Ctrl Pts',(-68.22683330895,29.0951572355352,0.));
#88841=CARTESIAN_POINT('Ctrl Pts',(-68.22683330895,29.0951572355352,12.));
#88842=CARTESIAN_POINT('Ctrl Pts',(-68.2543712489815,29.0946179757132,0.));
#88843=CARTESIAN_POINT('Ctrl Pts',(-68.2543712489815,29.0946179757132,12.));
#88844=CARTESIAN_POINT('Ctrl Pts',(-68.2819438775932,29.0940530889141,0.));
#88845=CARTESIAN_POINT('Ctrl Pts',(-68.2819438775932,29.0940530889141,12.));
#88846=CARTESIAN_POINT('Ctrl Pts',(-68.3095511047852,29.0934625288442,0.));
#88847=CARTESIAN_POINT('Ctrl Pts',(-68.3095511047852,29.0934625288442,12.));
#88848=CARTESIAN_POINT('Ctrl Pts',(-68.3371928310351,29.0928462428218,0.));
#88849=CARTESIAN_POINT('Ctrl Pts',(-68.3371928310351,29.0928462428218,12.));
#88850=CARTESIAN_POINT('Ctrl Pts',(-68.3648689519188,29.0922041749393,0.));
#88851=CARTESIAN_POINT('Ctrl Pts',(-68.3648689519188,29.0922041749393,12.));
#88852=CARTESIAN_POINT('Ctrl Pts',(-68.3925793638241,29.091536269955,0.));
#88853=CARTESIAN_POINT('Ctrl Pts',(-68.3925793638241,29.091536269955,12.));
#88854=CARTESIAN_POINT('Ctrl Pts',(-68.4203239694742,29.0908424770941,0.));
#88855=CARTESIAN_POINT('Ctrl Pts',(-68.4203239694742,29.0908424770941,12.));
#88856=CARTESIAN_POINT('Ctrl Pts',(-68.4481026830845,29.0901227535274,0.));
#88857=CARTESIAN_POINT('Ctrl Pts',(-68.4481026830845,29.0901227535274,12.));
#88858=CARTESIAN_POINT('Ctrl Pts',(-68.4759154367582,29.0893770688807,0.));
#88859=CARTESIAN_POINT('Ctrl Pts',(-68.4759154367582,29.0893770688807,12.));
#88860=CARTESIAN_POINT('Ctrl Pts',(-68.5037621823575,29.0886054060334,0.));
#88861=CARTESIAN_POINT('Ctrl Pts',(-68.5037621823575,29.0886054060334,12.));
#88862=CARTESIAN_POINT('Ctrl Pts',(-68.5316428874729,29.0878077570819,0.));
#88863=CARTESIAN_POINT('Ctrl Pts',(-68.5316428874729,29.0878077570819,12.));
#88864=CARTESIAN_POINT('Ctrl Pts',(-68.5539746037961,29.0871488478365,0.));
#88865=CARTESIAN_POINT('Ctrl Pts',(-68.5539746037961,29.0871488478365,12.));
#88866=CARTESIAN_POINT('Ctrl Pts',(-68.5707386600286,29.0866429721959,0.));
#88867=CARTESIAN_POINT('Ctrl Pts',(-68.5707386600286,29.0866429721959,12.));
#88868=CARTESIAN_POINT('Ctrl Pts',(-68.5819214834609,29.0863005247789,0.));
#88869=CARTESIAN_POINT('Ctrl Pts',(-68.5819214834609,29.0863005247789,12.));
#88870=CARTESIAN_POINT('Ctrl Pts',(-68.5875145916629,29.0861280018229,0.));
#88871=CARTESIAN_POINT('Ctrl Pts',(-68.5875145916629,29.0861280018229,12.));
#88872=CARTESIAN_POINT('',(-63.7976679095314,28.8072485549236,0.));
#88873=CARTESIAN_POINT('Ctrl Pts',(-63.7976679095314,28.8072485549236,0.));
#88874=CARTESIAN_POINT('Ctrl Pts',(-63.8014989507494,28.8078854475432,0.));
#88875=CARTESIAN_POINT('Ctrl Pts',(-63.8091667271232,28.8091580239553,0.));
#88876=CARTESIAN_POINT('Ctrl Pts',(-63.8206854735028,28.8110632620957,0.));
#88877=CARTESIAN_POINT('Ctrl Pts',(-63.8360779669856,28.8135963263368,0.));
#88878=CARTESIAN_POINT('Ctrl Pts',(-63.8553755207487,28.8167505576681,0.));
#88879=CARTESIAN_POINT('Ctrl Pts',(-63.8747299825313,28.8198926619858,0.));
#88880=CARTESIAN_POINT('Ctrl Pts',(-63.8941412856924,28.823022586318,0.));
#88881=CARTESIAN_POINT('Ctrl Pts',(-63.9136093063786,28.8261402423291,0.));
#88882=CARTESIAN_POINT('Ctrl Pts',(-63.9331338646996,28.8292455077559,0.));
#88883=CARTESIAN_POINT('Ctrl Pts',(-63.9527147494423,28.8323382413789,0.));
#88884=CARTESIAN_POINT('Ctrl Pts',(-63.9723517369614,28.8354182946601,0.));
#88885=CARTESIAN_POINT('Ctrl Pts',(-63.9920446117582,28.8384855243243,0.));
#88886=CARTESIAN_POINT('Ctrl Pts',(-64.0117931881298,28.8415398056428,0.));
#88887=CARTESIAN_POINT('Ctrl Pts',(-64.0315973031942,28.844581028125,0.));
#88888=CARTESIAN_POINT('Ctrl Pts',(-64.0514568066637,28.8476090892232,0.));
#88889=CARTESIAN_POINT('Ctrl Pts',(-64.0713715523599,28.8506238891093,0.));
#88890=CARTESIAN_POINT('Ctrl Pts',(-64.0913413876622,28.8536253241854,0.));
#88891=CARTESIAN_POINT('Ctrl Pts',(-64.1113661481965,28.8566132838178,0.));
#88892=CARTESIAN_POINT('Ctrl Pts',(-64.1314456633381,28.8595876537148,0.));
#88893=CARTESIAN_POINT('Ctrl Pts',(-64.1515797596564,28.8625483180437,0.));
#88894=CARTESIAN_POINT('Ctrl Pts',(-64.1717682648685,28.8654951618649,0.));
#88895=CARTESIAN_POINT('Ctrl Pts',(-64.1920110123299,28.8684280739014,0.));
#88896=CARTESIAN_POINT('Ctrl Pts',(-64.2123078408461,28.8713469464185,0.));
#88897=CARTESIAN_POINT('Ctrl Pts',(-64.2326585925252,28.8742516738947,0.));
#88898=CARTESIAN_POINT('Ctrl Pts',(-64.2530631112929,28.877142152106,0.));
#88899=CARTESIAN_POINT('Ctrl Pts',(-64.2735212410711,28.8800182770065,0.));
#88900=CARTESIAN_POINT('Ctrl Pts',(-64.2940328242521,28.882879943794,0.));
#88901=CARTESIAN_POINT('Ctrl Pts',(-64.3145977025037,28.8857270473959,0.));
#88902=CARTESIAN_POINT('Ctrl Pts',(-64.3352157174619,28.8885594828926,0.));
#88903=CARTESIAN_POINT('Ctrl Pts',(-64.3558867114076,28.8913771459323,0.));
#88904=CARTESIAN_POINT('Ctrl Pts',(-64.3766105280688,28.89417993323,0.));
#88905=CARTESIAN_POINT('Ctrl Pts',(-64.397387012917,28.8969677427504,0.));
#88906=CARTESIAN_POINT('Ctrl Pts',(-64.4182160127379,28.899740473434,0.));
#88907=CARTESIAN_POINT('Ctrl Pts',(-64.4390973753634,28.9024980250307,0.));
#88908=CARTESIAN_POINT('Ctrl Pts',(-64.4600309493583,28.9052402979062,0.));
#88909=CARTESIAN_POINT('Ctrl Pts',(-64.4810165836592,28.9079671928264,0.));
#88910=CARTESIAN_POINT('Ctrl Pts',(-64.5020541275951,28.910678610965,0.));
#88911=CARTESIAN_POINT('Ctrl Pts',(-64.523143431047,28.9133744539949,0.));
#88912=CARTESIAN_POINT('Ctrl Pts',(-64.5442843445559,28.9160546241538,0.));
#88913=CARTESIAN_POINT('Ctrl Pts',(-64.5654767194472,28.9187190243224,0.));
#88914=CARTESIAN_POINT('Ctrl Pts',(-64.5867204079426,28.9213675580985,0.));
#88915=CARTESIAN_POINT('Ctrl Pts',(-64.6080152631039,28.9240001297542,0.));
#88916=CARTESIAN_POINT('Ctrl Pts',(-64.629361138774,28.926616644195,0.));
#88917=CARTESIAN_POINT('Ctrl Pts',(-64.6507578895161,28.9292170069221,0.));
#88918=CARTESIAN_POINT('Ctrl Pts',(-64.672205370541,28.9318011239915,0.));
#88919=CARTESIAN_POINT('Ctrl Pts',(-64.6937034376617,28.9343689019882,0.));
#88920=CARTESIAN_POINT('Ctrl Pts',(-64.715251947329,28.9369202480393,0.));
#88921=CARTESIAN_POINT('Ctrl Pts',(-64.7368507566467,28.9394550698204,0.));
#88922=CARTESIAN_POINT('Ctrl Pts',(-64.758499723388,28.9419732755656,0.));
#88923=CARTESIAN_POINT('Ctrl Pts',(-64.7801987060084,28.944474774081,0.));
#88924=CARTESIAN_POINT('Ctrl Pts',(-64.8019475636442,28.9469594747431,0.));
#88925=CARTESIAN_POINT('Ctrl Pts',(-64.8237461561019,28.9494272874832,0.));
#88926=CARTESIAN_POINT('Ctrl Pts',(-64.8455943438423,28.9518781227765,0.));
#88927=CARTESIAN_POINT('Ctrl Pts',(-64.8674919879648,28.9543118916328,0.));
#88928=CARTESIAN_POINT('Ctrl Pts',(-64.8894389501801,28.9567285055866,0.));
#88929=CARTESIAN_POINT('Ctrl Pts',(-64.9114350928125,28.9591278766934,0.));
#88930=CARTESIAN_POINT('Ctrl Pts',(-64.9334802788038,28.9615099175249,0.));
#88931=CARTESIAN_POINT('Ctrl Pts',(-64.955574371711,28.9638745411677,0.));
#88932=CARTESIAN_POINT('Ctrl Pts',(-64.9777172357027,28.9662216612217,0.));
#88933=CARTESIAN_POINT('Ctrl Pts',(-64.9999087355504,28.9685511918018,0.));
#88934=CARTESIAN_POINT('Ctrl Pts',(-65.022148736628,28.97086304753,0.));
#88935=CARTESIAN_POINT('Ctrl Pts',(-65.0444371049082,28.9731571435282,0.));
#88936=CARTESIAN_POINT('Ctrl Pts',(-65.0667737069563,28.9754333954135,0.));
#88937=CARTESIAN_POINT('Ctrl Pts',(-65.0891584099168,28.9776917192933,0.));
#88938=CARTESIAN_POINT('Ctrl Pts',(-65.1115910815037,28.9799320317641,0.));
#88939=CARTESIAN_POINT('Ctrl Pts',(-65.1340715900028,28.9821542499042,0.));
#88940=CARTESIAN_POINT('Ctrl Pts',(-65.1565998042697,28.9843582912692,0.));
#88941=CARTESIAN_POINT('Ctrl Pts',(-65.1791755937256,28.9865440738884,0.));
#88942=CARTESIAN_POINT('Ctrl Pts',(-65.2017988283479,28.9887115162633,0.));
#88943=CARTESIAN_POINT('Ctrl Pts',(-65.2244693786609,28.9908605373663,0.));
#88944=CARTESIAN_POINT('Ctrl Pts',(-65.2471871157397,28.9929910566325,0.));
#88945=CARTESIAN_POINT('Ctrl Pts',(-65.2699519112064,28.9951029939557,0.));
#88946=CARTESIAN_POINT('Ctrl Pts',(-65.2927636372254,28.9971962696845,0.));
#88947=CARTESIAN_POINT('Ctrl Pts',(-65.3156221664916,28.9992708046211,0.));
#88948=CARTESIAN_POINT('Ctrl Pts',(-65.3385273722242,29.0013265200185,0.));
#88949=CARTESIAN_POINT('Ctrl Pts',(-65.3614791281692,29.003363337573,0.));
#88950=CARTESIAN_POINT('Ctrl Pts',(-65.3844773085961,29.0053811794207,0.));
#88951=CARTESIAN_POINT('Ctrl Pts',(-65.4075217882934,29.0073799681342,0.));
#88952=CARTESIAN_POINT('Ctrl Pts',(-65.4306124425562,29.0093596267215,0.));
#88953=CARTESIAN_POINT('Ctrl Pts',(-65.4537491471828,29.0113200786239,0.));
#88954=CARTESIAN_POINT('Ctrl Pts',(-65.4769317784789,29.013261247709,0.));
#88955=CARTESIAN_POINT('Ctrl Pts',(-65.5001602132535,29.0151830582675,0.));
#88956=CARTESIAN_POINT('Ctrl Pts',(-65.5234343288136,29.0170854350095,0.));
#88957=CARTESIAN_POINT('Ctrl Pts',(-65.5467540029514,29.0189683030642,0.));
#88958=CARTESIAN_POINT('Ctrl Pts',(-65.5701191139418,29.0208315879764,0.));
#88959=CARTESIAN_POINT('Ctrl Pts',(-65.5935295405453,29.0226752157003,0.));
#88960=CARTESIAN_POINT('Ctrl Pts',(-65.6169851620046,29.0244991125959,0.));
#88961=CARTESIAN_POINT('Ctrl Pts',(-65.6404858580403,29.0263032054266,0.));
#88962=CARTESIAN_POINT('Ctrl Pts',(-65.6640315088388,29.0280874213596,0.));
#88963=CARTESIAN_POINT('Ctrl Pts',(-65.6876219950493,29.0298516879611,0.));
#88964=CARTESIAN_POINT('Ctrl Pts',(-65.7112571977891,29.0315959331919,0.));
#88965=CARTESIAN_POINT('Ctrl Pts',(-65.7349369986384,29.0333200854027,0.));
#88966=CARTESIAN_POINT('Ctrl Pts',(-65.7586612796368,29.035024073333,0.));
#88967=CARTESIAN_POINT('Ctrl Pts',(-65.7824299232705,29.0367078261103,0.));
#88968=CARTESIAN_POINT('Ctrl Pts',(-65.8062428124713,29.0383712732469,0.));
#88969=CARTESIAN_POINT('Ctrl Pts',(-65.8300998306191,29.0400143446338,0.));
#88970=CARTESIAN_POINT('Ctrl Pts',(-65.854000861539,29.0416369705375,0.));
#88971=CARTESIAN_POINT('Ctrl Pts',(-65.8779457894961,29.0432390815978,0.));
#88972=CARTESIAN_POINT('Ctrl Pts',(-65.9019344991854,29.0448206088288,0.));
#88973=CARTESIAN_POINT('Ctrl Pts',(-65.9259668757307,29.0463814836157,0.));
#88974=CARTESIAN_POINT('Ctrl Pts',(-65.9500428046868,29.0479216377081,0.));
#88975=CARTESIAN_POINT('Ctrl Pts',(-65.974162172037,29.0494410032172,0.));
#88976=CARTESIAN_POINT('Ctrl Pts',(-65.9983248641879,29.0509395126142,0.));
#88977=CARTESIAN_POINT('Ctrl Pts',(-66.0225307679591,29.0524170987307,0.));
#88978=CARTESIAN_POINT('Ctrl Pts',(-66.0467797705815,29.0538736947552,0.));
#88979=CARTESIAN_POINT('Ctrl Pts',(-66.0710717597009,29.0553092342278,0.));
#88980=CARTESIAN_POINT('Ctrl Pts',(-66.0954066233754,29.0567236510373,0.));
#88981=CARTESIAN_POINT('Ctrl Pts',(-66.1197842500711,29.0581168794189,0.));
#88982=CARTESIAN_POINT('Ctrl Pts',(-66.1442045286516,29.0594888539555,0.));
#88983=CARTESIAN_POINT('Ctrl Pts',(-66.1686673483755,29.0608395095745,0.));
#88984=CARTESIAN_POINT('Ctrl Pts',(-66.1931725989008,29.062168781542,0.));
#88985=CARTESIAN_POINT('Ctrl Pts',(-66.2177201702819,29.0634766054599,0.));
#88986=CARTESIAN_POINT('Ctrl Pts',(-66.2423099529668,29.0647629172645,0.));
#88987=CARTESIAN_POINT('Ctrl Pts',(-66.2669418377866,29.0660276532272,0.));
#88988=CARTESIAN_POINT('Ctrl Pts',(-66.2916157159528,29.0672707499527,0.));
#88989=CARTESIAN_POINT('Ctrl Pts',(-66.3163314790607,29.0684921443718,0.));
#88990=CARTESIAN_POINT('Ctrl Pts',(-66.3410890190879,29.0696917737397,0.));
#88991=CARTESIAN_POINT('Ctrl Pts',(-66.3658882283906,29.0708695756335,0.));
#88992=CARTESIAN_POINT('Ctrl Pts',(-66.3907289996942,29.0720254879535,0.));
#88993=CARTESIAN_POINT('Ctrl Pts',(-66.4156112260904,29.0731594489218,0.));
#88994=CARTESIAN_POINT('Ctrl Pts',(-66.4405348010404,29.0742713970762,0.));
#88995=CARTESIAN_POINT('Ctrl Pts',(-66.4654996183739,29.0753612712669,0.));
#88996=CARTESIAN_POINT('Ctrl Pts',(-66.4905055722864,29.0764290106553,0.));
#88997=CARTESIAN_POINT('Ctrl Pts',(-66.5155525573308,29.0774745547146,0.));
#88998=CARTESIAN_POINT('Ctrl Pts',(-66.5406404684116,29.0784978432294,0.));
#88999=CARTESIAN_POINT('Ctrl Pts',(-66.5657692007894,29.0794988162892,0.));
#89000=CARTESIAN_POINT('Ctrl Pts',(-66.5909386500796,29.0804774142852,0.));
#89001=CARTESIAN_POINT('Ctrl Pts',(-66.6161487122504,29.0814335779085,0.));
#89002=CARTESIAN_POINT('Ctrl Pts',(-66.6413992836148,29.0823672481508,0.));
#89003=CARTESIAN_POINT('Ctrl Pts',(-66.6666902608246,29.0832783663048,0.));
#89004=CARTESIAN_POINT('Ctrl Pts',(-66.6920215408744,29.0841668739585,0.));
#89005=CARTESIAN_POINT('Ctrl Pts',(-66.7173930211015,29.0850327129913,0.));
#89006=CARTESIAN_POINT('Ctrl Pts',(-66.7428045991841,29.0858758255729,0.));
#89007=CARTESIAN_POINT('Ctrl Pts',(-66.7682561731349,29.0866961541629,0.));
#89008=CARTESIAN_POINT('Ctrl Pts',(-66.7937476412941,29.0874936415138,0.));
#89009=CARTESIAN_POINT('Ctrl Pts',(-66.8192789023323,29.0882682306636,0.));
#89010=CARTESIAN_POINT('Ctrl Pts',(-66.8448498552508,29.0890198649327,0.));
#89011=CARTESIAN_POINT('Ctrl Pts',(-66.8704603993794,29.0897484879207,0.));
#89012=CARTESIAN_POINT('Ctrl Pts',(-66.8961104343703,29.0904540435063,0.));
#89013=CARTESIAN_POINT('Ctrl Pts',(-66.9217998601881,29.0911364758484,0.));
#89014=CARTESIAN_POINT('Ctrl Pts',(-66.9475285771133,29.0917957293824,0.));
#89015=CARTESIAN_POINT('Ctrl Pts',(-66.9732964857467,29.092431748817,0.));
#89016=CARTESIAN_POINT('Ctrl Pts',(-66.9991034870084,29.0930444791329,0.));
#89017=CARTESIAN_POINT('Ctrl Pts',(-67.0249494821361,29.0936338655828,0.));
#89018=CARTESIAN_POINT('Ctrl Pts',(-67.0508343726771,29.0941998536957,0.));
#89019=CARTESIAN_POINT('Ctrl Pts',(-67.0767580604872,29.0947423892725,0.));
#89020=CARTESIAN_POINT('Ctrl Pts',(-67.1027204477304,29.0952614183777,0.));
#89021=CARTESIAN_POINT('Ctrl Pts',(-67.1287214368743,29.0957568873357,0.));
#89022=CARTESIAN_POINT('Ctrl Pts',(-67.1547609306845,29.0962287427274,0.));
#89023=CARTESIAN_POINT('Ctrl Pts',(-67.1808388322116,29.0966769313893,0.));
#89024=CARTESIAN_POINT('Ctrl Pts',(-67.2069550447895,29.0971014004134,0.));
#89025=CARTESIAN_POINT('Ctrl Pts',(-67.2331094720482,29.0975020971473,0.));
#89026=CARTESIAN_POINT('Ctrl Pts',(-67.2593020179216,29.0978789691965,0.));
#89027=CARTESIAN_POINT('Ctrl Pts',(-67.2855325866516,29.0982319644276,0.));
#89028=CARTESIAN_POINT('Ctrl Pts',(-67.311801082791,29.0985610309768,0.));
#89029=CARTESIAN_POINT('Ctrl Pts',(-67.3381074112013,29.0988661172526,0.));
#89030=CARTESIAN_POINT('Ctrl Pts',(-67.3644514770373,29.0991471719172,0.));
#89031=CARTESIAN_POINT('Ctrl Pts',(-67.3908331857313,29.0994041438715,0.));
#89032=CARTESIAN_POINT('Ctrl Pts',(-67.4172524429726,29.0996369822418,0.));
#89033=CARTESIAN_POINT('Ctrl Pts',(-67.4437091546869,29.0998456363687,0.));
#89034=CARTESIAN_POINT('Ctrl Pts',(-67.4702032270063,29.1000300557961,0.));
#89035=CARTESIAN_POINT('Ctrl Pts',(-67.496734566311,29.1001901902915,0.));
#89036=CARTESIAN_POINT('Ctrl Pts',(-67.5233030792714,29.1003259898686,0.));
#89037=CARTESIAN_POINT('Ctrl Pts',(-67.5499086728891,29.1004374048149,0.));
#89038=CARTESIAN_POINT('Ctrl Pts',(-67.5765512545277,29.1005243857137,0.));
#89039=CARTESIAN_POINT('Ctrl Pts',(-67.6032307319614,29.1005868834863,0.));
#89040=CARTESIAN_POINT('Ctrl Pts',(-67.6299470133286,29.1006248493576,0.));
#89041=CARTESIAN_POINT('Ctrl Pts',(-67.6567000070319,29.1006382347812,0.));
#89042=CARTESIAN_POINT('Ctrl Pts',(-67.6834896216458,29.1006269913747,0.));
#89043=CARTESIAN_POINT('Ctrl Pts',(-67.7103157658297,29.1005910708624,0.));
#89044=CARTESIAN_POINT('Ctrl Pts',(-67.7371783482039,29.1005304249989,0.));
#89045=CARTESIAN_POINT('Ctrl Pts',(-67.7640772773397,29.1004450055647,0.));
#89046=CARTESIAN_POINT('Ctrl Pts',(-67.7910124620149,29.1003347645299,0.));
#89047=CARTESIAN_POINT('Ctrl Pts',(-67.8179838114109,29.1001996541846,0.));
#89048=CARTESIAN_POINT('Ctrl Pts',(-67.844991235333,29.1000396272868,0.));
#89049=CARTESIAN_POINT('Ctrl Pts',(-67.8720346444111,29.0998546372027,0.));
#89050=CARTESIAN_POINT('Ctrl Pts',(-67.8991139503168,29.0996446380617,0.));
#89051=CARTESIAN_POINT('Ctrl Pts',(-67.9262290652797,29.0994095844208,0.));
#89052=CARTESIAN_POINT('Ctrl Pts',(-67.9533799016122,29.0991494309394,0.));
#89053=CARTESIAN_POINT('Ctrl Pts',(-67.9805663711845,29.0988641320243,0.));
#89054=CARTESIAN_POINT('Ctrl Pts',(-68.0077883850136,29.0985536415537,0.));
#89055=CARTESIAN_POINT('Ctrl Pts',(-68.0350458525589,29.0982179124112,0.));
#89056=CARTESIAN_POINT('Ctrl Pts',(-68.0623386822917,29.0978568968677,0.));
#89057=CARTESIAN_POINT('Ctrl Pts',(-68.089666782962,29.0974705474279,0.));
#89058=CARTESIAN_POINT('Ctrl Pts',(-68.1170300647019,29.097058817574,0.));
#89059=CARTESIAN_POINT('Ctrl Pts',(-68.1444284400734,29.096621662474,0.));
#89060=CARTESIAN_POINT('Ctrl Pts',(-68.1718618254221,29.0961590399023,0.));
#89061=CARTESIAN_POINT('Ctrl Pts',(-68.1993301411959,29.0956709104588,0.));
#89062=CARTESIAN_POINT('Ctrl Pts',(-68.2229056854495,29.0952305915108,0.));
#89063=CARTESIAN_POINT('Ctrl Pts',(-68.2409993689947,29.0948791947834,0.));
#89064=CARTESIAN_POINT('Ctrl Pts',(-68.2535957746884,29.094628043331,0.));
#89065=CARTESIAN_POINT('Ctrl Pts',(-68.2606847334624,29.0944846386548,0.));
#89066=CARTESIAN_POINT('Ctrl Pts',(-68.2622612909744,29.0944526440249,0.));
#89067=CARTESIAN_POINT('',(-63.7976679095314,28.8072485549236,12.));
#89068=CARTESIAN_POINT('',(-63.7976679095314,28.8072485549236,0.));
#89069=CARTESIAN_POINT('Ctrl Pts',(-68.2622612909744,29.0944526440249,12.));
#89070=CARTESIAN_POINT('Ctrl Pts',(-68.2606847334624,29.0944846386548,12.));
#89071=CARTESIAN_POINT('Ctrl Pts',(-68.2535957746883,29.094628043331,12.));
#89072=CARTESIAN_POINT('Ctrl Pts',(-68.2409993689947,29.0948791947834,12.));
#89073=CARTESIAN_POINT('Ctrl Pts',(-68.2229056854495,29.0952305915108,12.));
#89074=CARTESIAN_POINT('Ctrl Pts',(-68.1993301411959,29.0956709104588,12.));
#89075=CARTESIAN_POINT('Ctrl Pts',(-68.1718618254221,29.0961590399023,12.));
#89076=CARTESIAN_POINT('Ctrl Pts',(-68.1444284400734,29.096621662474,12.));
#89077=CARTESIAN_POINT('Ctrl Pts',(-68.1170300647019,29.097058817574,12.));
#89078=CARTESIAN_POINT('Ctrl Pts',(-68.089666782962,29.0974705474279,12.));
#89079=CARTESIAN_POINT('Ctrl Pts',(-68.0623386822917,29.0978568968677,12.));
#89080=CARTESIAN_POINT('Ctrl Pts',(-68.0350458525589,29.0982179124112,12.));
#89081=CARTESIAN_POINT('Ctrl Pts',(-68.0077883850136,29.0985536415537,12.));
#89082=CARTESIAN_POINT('Ctrl Pts',(-67.9805663711845,29.0988641320243,12.));
#89083=CARTESIAN_POINT('Ctrl Pts',(-67.9533799016122,29.0991494309394,12.));
#89084=CARTESIAN_POINT('Ctrl Pts',(-67.9262290652797,29.0994095844208,12.));
#89085=CARTESIAN_POINT('Ctrl Pts',(-67.8991139503168,29.0996446380617,12.));
#89086=CARTESIAN_POINT('Ctrl Pts',(-67.8720346444111,29.0998546372027,12.));
#89087=CARTESIAN_POINT('Ctrl Pts',(-67.844991235333,29.1000396272868,12.));
#89088=CARTESIAN_POINT('Ctrl Pts',(-67.8179838114109,29.1001996541846,12.));
#89089=CARTESIAN_POINT('Ctrl Pts',(-67.7910124620149,29.1003347645299,12.));
#89090=CARTESIAN_POINT('Ctrl Pts',(-67.7640772773397,29.1004450055647,12.));
#89091=CARTESIAN_POINT('Ctrl Pts',(-67.7371783482039,29.1005304249989,12.));
#89092=CARTESIAN_POINT('Ctrl Pts',(-67.7103157658297,29.1005910708624,12.));
#89093=CARTESIAN_POINT('Ctrl Pts',(-67.6834896216458,29.1006269913747,12.));
#89094=CARTESIAN_POINT('Ctrl Pts',(-67.6567000070319,29.1006382347812,12.));
#89095=CARTESIAN_POINT('Ctrl Pts',(-67.6299470133286,29.1006248493576,12.));
#89096=CARTESIAN_POINT('Ctrl Pts',(-67.6032307319614,29.1005868834863,12.));
#89097=CARTESIAN_POINT('Ctrl Pts',(-67.5765512545277,29.1005243857137,12.));
#89098=CARTESIAN_POINT('Ctrl Pts',(-67.5499086728891,29.1004374048149,12.));
#89099=CARTESIAN_POINT('Ctrl Pts',(-67.5233030792714,29.1003259898686,12.));
#89100=CARTESIAN_POINT('Ctrl Pts',(-67.496734566311,29.1001901902915,12.));
#89101=CARTESIAN_POINT('Ctrl Pts',(-67.4702032270063,29.1000300557961,12.));
#89102=CARTESIAN_POINT('Ctrl Pts',(-67.4437091546869,29.0998456363687,12.));
#89103=CARTESIAN_POINT('Ctrl Pts',(-67.4172524429726,29.0996369822418,12.));
#89104=CARTESIAN_POINT('Ctrl Pts',(-67.3908331857313,29.0994041438715,12.));
#89105=CARTESIAN_POINT('Ctrl Pts',(-67.3644514770373,29.0991471719172,12.));
#89106=CARTESIAN_POINT('Ctrl Pts',(-67.3381074112013,29.0988661172526,12.));
#89107=CARTESIAN_POINT('Ctrl Pts',(-67.311801082791,29.0985610309768,12.));
#89108=CARTESIAN_POINT('Ctrl Pts',(-67.2855325866516,29.0982319644276,12.));
#89109=CARTESIAN_POINT('Ctrl Pts',(-67.2593020179216,29.0978789691965,12.));
#89110=CARTESIAN_POINT('Ctrl Pts',(-67.2331094720482,29.0975020971473,12.));
#89111=CARTESIAN_POINT('Ctrl Pts',(-67.2069550447895,29.0971014004134,12.));
#89112=CARTESIAN_POINT('Ctrl Pts',(-67.1808388322116,29.0966769313893,12.));
#89113=CARTESIAN_POINT('Ctrl Pts',(-67.1547609306845,29.0962287427274,12.));
#89114=CARTESIAN_POINT('Ctrl Pts',(-67.1287214368743,29.0957568873357,12.));
#89115=CARTESIAN_POINT('Ctrl Pts',(-67.1027204477304,29.0952614183777,12.));
#89116=CARTESIAN_POINT('Ctrl Pts',(-67.0767580604872,29.0947423892725,12.));
#89117=CARTESIAN_POINT('Ctrl Pts',(-67.0508343726771,29.0941998536957,12.));
#89118=CARTESIAN_POINT('Ctrl Pts',(-67.0249494821361,29.0936338655828,12.));
#89119=CARTESIAN_POINT('Ctrl Pts',(-66.9991034870084,29.0930444791329,12.));
#89120=CARTESIAN_POINT('Ctrl Pts',(-66.9732964857467,29.092431748817,12.));
#89121=CARTESIAN_POINT('Ctrl Pts',(-66.9475285771133,29.0917957293824,12.));
#89122=CARTESIAN_POINT('Ctrl Pts',(-66.9217998601881,29.0911364758484,12.));
#89123=CARTESIAN_POINT('Ctrl Pts',(-66.8961104343703,29.0904540435063,12.));
#89124=CARTESIAN_POINT('Ctrl Pts',(-66.8704603993794,29.0897484879207,12.));
#89125=CARTESIAN_POINT('Ctrl Pts',(-66.8448498552508,29.0890198649327,12.));
#89126=CARTESIAN_POINT('Ctrl Pts',(-66.8192789023323,29.0882682306636,12.));
#89127=CARTESIAN_POINT('Ctrl Pts',(-66.7937476412941,29.0874936415138,12.));
#89128=CARTESIAN_POINT('Ctrl Pts',(-66.7682561731349,29.0866961541629,12.));
#89129=CARTESIAN_POINT('Ctrl Pts',(-66.7428045991841,29.0858758255729,12.));
#89130=CARTESIAN_POINT('Ctrl Pts',(-66.7173930211015,29.0850327129913,12.));
#89131=CARTESIAN_POINT('Ctrl Pts',(-66.6920215408744,29.0841668739585,12.));
#89132=CARTESIAN_POINT('Ctrl Pts',(-66.6666902608246,29.0832783663048,12.));
#89133=CARTESIAN_POINT('Ctrl Pts',(-66.6413992836148,29.0823672481508,12.));
#89134=CARTESIAN_POINT('Ctrl Pts',(-66.6161487122504,29.0814335779085,12.));
#89135=CARTESIAN_POINT('Ctrl Pts',(-66.5909386500796,29.0804774142852,12.));
#89136=CARTESIAN_POINT('Ctrl Pts',(-66.5657692007894,29.0794988162892,12.));
#89137=CARTESIAN_POINT('Ctrl Pts',(-66.5406404684116,29.0784978432294,12.));
#89138=CARTESIAN_POINT('Ctrl Pts',(-66.5155525573308,29.0774745547146,12.));
#89139=CARTESIAN_POINT('Ctrl Pts',(-66.4905055722864,29.0764290106553,12.));
#89140=CARTESIAN_POINT('Ctrl Pts',(-66.4654996183739,29.0753612712669,12.));
#89141=CARTESIAN_POINT('Ctrl Pts',(-66.4405348010404,29.0742713970762,12.));
#89142=CARTESIAN_POINT('Ctrl Pts',(-66.4156112260904,29.0731594489218,12.));
#89143=CARTESIAN_POINT('Ctrl Pts',(-66.3907289996942,29.0720254879535,12.));
#89144=CARTESIAN_POINT('Ctrl Pts',(-66.3658882283906,29.0708695756335,12.));
#89145=CARTESIAN_POINT('Ctrl Pts',(-66.3410890190879,29.0696917737397,12.));
#89146=CARTESIAN_POINT('Ctrl Pts',(-66.3163314790607,29.0684921443718,12.));
#89147=CARTESIAN_POINT('Ctrl Pts',(-66.2916157159528,29.0672707499527,12.));
#89148=CARTESIAN_POINT('Ctrl Pts',(-66.2669418377866,29.0660276532272,12.));
#89149=CARTESIAN_POINT('Ctrl Pts',(-66.2423099529668,29.0647629172645,12.));
#89150=CARTESIAN_POINT('Ctrl Pts',(-66.2177201702819,29.0634766054599,12.));
#89151=CARTESIAN_POINT('Ctrl Pts',(-66.1931725989008,29.062168781542,12.));
#89152=CARTESIAN_POINT('Ctrl Pts',(-66.1686673483755,29.0608395095745,12.));
#89153=CARTESIAN_POINT('Ctrl Pts',(-66.1442045286516,29.0594888539555,12.));
#89154=CARTESIAN_POINT('Ctrl Pts',(-66.1197842500711,29.0581168794189,12.));
#89155=CARTESIAN_POINT('Ctrl Pts',(-66.0954066233754,29.0567236510373,12.));
#89156=CARTESIAN_POINT('Ctrl Pts',(-66.0710717597009,29.0553092342278,12.));
#89157=CARTESIAN_POINT('Ctrl Pts',(-66.0467797705815,29.0538736947552,12.));
#89158=CARTESIAN_POINT('Ctrl Pts',(-66.0225307679591,29.0524170987307,12.));
#89159=CARTESIAN_POINT('Ctrl Pts',(-65.9983248641879,29.0509395126142,12.));
#89160=CARTESIAN_POINT('Ctrl Pts',(-65.974162172037,29.0494410032172,12.));
#89161=CARTESIAN_POINT('Ctrl Pts',(-65.9500428046868,29.0479216377081,12.));
#89162=CARTESIAN_POINT('Ctrl Pts',(-65.9259668757307,29.0463814836157,12.));
#89163=CARTESIAN_POINT('Ctrl Pts',(-65.9019344991854,29.0448206088288,12.));
#89164=CARTESIAN_POINT('Ctrl Pts',(-65.8779457894961,29.0432390815978,12.));
#89165=CARTESIAN_POINT('Ctrl Pts',(-65.854000861539,29.0416369705375,12.));
#89166=CARTESIAN_POINT('Ctrl Pts',(-65.8300998306191,29.0400143446338,12.));
#89167=CARTESIAN_POINT('Ctrl Pts',(-65.8062428124713,29.0383712732469,12.));
#89168=CARTESIAN_POINT('Ctrl Pts',(-65.7824299232705,29.0367078261103,12.));
#89169=CARTESIAN_POINT('Ctrl Pts',(-65.7586612796368,29.035024073333,12.));
#89170=CARTESIAN_POINT('Ctrl Pts',(-65.7349369986384,29.0333200854027,12.));
#89171=CARTESIAN_POINT('Ctrl Pts',(-65.7112571977891,29.0315959331919,12.));
#89172=CARTESIAN_POINT('Ctrl Pts',(-65.6876219950493,29.0298516879611,12.));
#89173=CARTESIAN_POINT('Ctrl Pts',(-65.6640315088388,29.0280874213596,12.));
#89174=CARTESIAN_POINT('Ctrl Pts',(-65.6404858580403,29.0263032054266,12.));
#89175=CARTESIAN_POINT('Ctrl Pts',(-65.6169851620046,29.0244991125959,12.));
#89176=CARTESIAN_POINT('Ctrl Pts',(-65.5935295405453,29.0226752157003,12.));
#89177=CARTESIAN_POINT('Ctrl Pts',(-65.5701191139418,29.0208315879764,12.));
#89178=CARTESIAN_POINT('Ctrl Pts',(-65.5467540029514,29.0189683030642,12.));
#89179=CARTESIAN_POINT('Ctrl Pts',(-65.5234343288136,29.0170854350095,12.));
#89180=CARTESIAN_POINT('Ctrl Pts',(-65.5001602132535,29.0151830582675,12.));
#89181=CARTESIAN_POINT('Ctrl Pts',(-65.4769317784789,29.013261247709,12.));
#89182=CARTESIAN_POINT('Ctrl Pts',(-65.4537491471828,29.0113200786239,12.));
#89183=CARTESIAN_POINT('Ctrl Pts',(-65.4306124425562,29.0093596267215,12.));
#89184=CARTESIAN_POINT('Ctrl Pts',(-65.4075217882934,29.0073799681342,12.));
#89185=CARTESIAN_POINT('Ctrl Pts',(-65.3844773085961,29.0053811794207,12.));
#89186=CARTESIAN_POINT('Ctrl Pts',(-65.3614791281692,29.003363337573,12.));
#89187=CARTESIAN_POINT('Ctrl Pts',(-65.3385273722242,29.0013265200185,12.));
#89188=CARTESIAN_POINT('Ctrl Pts',(-65.3156221664916,28.9992708046211,12.));
#89189=CARTESIAN_POINT('Ctrl Pts',(-65.2927636372254,28.9971962696845,12.));
#89190=CARTESIAN_POINT('Ctrl Pts',(-65.2699519112064,28.9951029939557,12.));
#89191=CARTESIAN_POINT('Ctrl Pts',(-65.2471871157397,28.9929910566325,12.));
#89192=CARTESIAN_POINT('Ctrl Pts',(-65.2244693786609,28.9908605373663,12.));
#89193=CARTESIAN_POINT('Ctrl Pts',(-65.2017988283479,28.9887115162633,12.));
#89194=CARTESIAN_POINT('Ctrl Pts',(-65.1791755937256,28.9865440738884,12.));
#89195=CARTESIAN_POINT('Ctrl Pts',(-65.1565998042697,28.9843582912692,12.));
#89196=CARTESIAN_POINT('Ctrl Pts',(-65.1340715900028,28.9821542499042,12.));
#89197=CARTESIAN_POINT('Ctrl Pts',(-65.1115910815037,28.9799320317641,12.));
#89198=CARTESIAN_POINT('Ctrl Pts',(-65.0891584099168,28.9776917192933,12.));
#89199=CARTESIAN_POINT('Ctrl Pts',(-65.0667737069563,28.9754333954135,12.));
#89200=CARTESIAN_POINT('Ctrl Pts',(-65.0444371049082,28.9731571435282,12.));
#89201=CARTESIAN_POINT('Ctrl Pts',(-65.022148736628,28.97086304753,12.));
#89202=CARTESIAN_POINT('Ctrl Pts',(-64.9999087355504,28.9685511918018,12.));
#89203=CARTESIAN_POINT('Ctrl Pts',(-64.9777172357027,28.9662216612217,12.));
#89204=CARTESIAN_POINT('Ctrl Pts',(-64.955574371711,28.9638745411677,12.));
#89205=CARTESIAN_POINT('Ctrl Pts',(-64.9334802788038,28.9615099175249,12.));
#89206=CARTESIAN_POINT('Ctrl Pts',(-64.9114350928125,28.9591278766934,12.));
#89207=CARTESIAN_POINT('Ctrl Pts',(-64.8894389501801,28.9567285055866,12.));
#89208=CARTESIAN_POINT('Ctrl Pts',(-64.8674919879648,28.9543118916328,12.));
#89209=CARTESIAN_POINT('Ctrl Pts',(-64.8455943438423,28.9518781227765,12.));
#89210=CARTESIAN_POINT('Ctrl Pts',(-64.8237461561019,28.9494272874832,12.));
#89211=CARTESIAN_POINT('Ctrl Pts',(-64.8019475636442,28.9469594747431,12.));
#89212=CARTESIAN_POINT('Ctrl Pts',(-64.7801987060084,28.944474774081,12.));
#89213=CARTESIAN_POINT('Ctrl Pts',(-64.758499723388,28.9419732755656,12.));
#89214=CARTESIAN_POINT('Ctrl Pts',(-64.7368507566467,28.9394550698204,12.));
#89215=CARTESIAN_POINT('Ctrl Pts',(-64.715251947329,28.9369202480393,12.));
#89216=CARTESIAN_POINT('Ctrl Pts',(-64.6937034376617,28.9343689019882,12.));
#89217=CARTESIAN_POINT('Ctrl Pts',(-64.672205370541,28.9318011239915,12.));
#89218=CARTESIAN_POINT('Ctrl Pts',(-64.6507578895161,28.9292170069221,12.));
#89219=CARTESIAN_POINT('Ctrl Pts',(-64.629361138774,28.926616644195,12.));
#89220=CARTESIAN_POINT('Ctrl Pts',(-64.6080152631039,28.9240001297542,12.));
#89221=CARTESIAN_POINT('Ctrl Pts',(-64.5867204079426,28.9213675580985,12.));
#89222=CARTESIAN_POINT('Ctrl Pts',(-64.5654767194472,28.9187190243224,12.));
#89223=CARTESIAN_POINT('Ctrl Pts',(-64.5442843445559,28.9160546241538,12.));
#89224=CARTESIAN_POINT('Ctrl Pts',(-64.523143431047,28.9133744539949,12.));
#89225=CARTESIAN_POINT('Ctrl Pts',(-64.5020541275951,28.910678610965,12.));
#89226=CARTESIAN_POINT('Ctrl Pts',(-64.4810165836592,28.9079671928264,12.));
#89227=CARTESIAN_POINT('Ctrl Pts',(-64.4600309493583,28.9052402979062,12.));
#89228=CARTESIAN_POINT('Ctrl Pts',(-64.4390973753634,28.9024980250307,12.));
#89229=CARTESIAN_POINT('Ctrl Pts',(-64.4182160127379,28.899740473434,12.));
#89230=CARTESIAN_POINT('Ctrl Pts',(-64.397387012917,28.8969677427504,12.));
#89231=CARTESIAN_POINT('Ctrl Pts',(-64.3766105280688,28.89417993323,12.));
#89232=CARTESIAN_POINT('Ctrl Pts',(-64.3558867114076,28.8913771459323,12.));
#89233=CARTESIAN_POINT('Ctrl Pts',(-64.3352157174619,28.8885594828926,12.));
#89234=CARTESIAN_POINT('Ctrl Pts',(-64.3145977025037,28.8857270473959,12.));
#89235=CARTESIAN_POINT('Ctrl Pts',(-64.2940328242521,28.882879943794,12.));
#89236=CARTESIAN_POINT('Ctrl Pts',(-64.2735212410711,28.8800182770065,12.));
#89237=CARTESIAN_POINT('Ctrl Pts',(-64.2530631112929,28.877142152106,12.));
#89238=CARTESIAN_POINT('Ctrl Pts',(-64.2326585925252,28.8742516738947,12.));
#89239=CARTESIAN_POINT('Ctrl Pts',(-64.2123078408461,28.8713469464185,12.));
#89240=CARTESIAN_POINT('Ctrl Pts',(-64.1920110123299,28.8684280739014,12.));
#89241=CARTESIAN_POINT('Ctrl Pts',(-64.1717682648685,28.8654951618649,12.));
#89242=CARTESIAN_POINT('Ctrl Pts',(-64.1515797596564,28.8625483180437,12.));
#89243=CARTESIAN_POINT('Ctrl Pts',(-64.1314456633381,28.8595876537148,12.));
#89244=CARTESIAN_POINT('Ctrl Pts',(-64.1113661481965,28.8566132838178,12.));
#89245=CARTESIAN_POINT('Ctrl Pts',(-64.0913413876622,28.8536253241854,12.));
#89246=CARTESIAN_POINT('Ctrl Pts',(-64.0713715523599,28.8506238891093,12.));
#89247=CARTESIAN_POINT('Ctrl Pts',(-64.0514568066637,28.8476090892232,12.));
#89248=CARTESIAN_POINT('Ctrl Pts',(-64.0315973031942,28.844581028125,12.));
#89249=CARTESIAN_POINT('Ctrl Pts',(-64.0117931881298,28.8415398056428,12.));
#89250=CARTESIAN_POINT('Ctrl Pts',(-63.9920446117582,28.8384855243243,12.));
#89251=CARTESIAN_POINT('Ctrl Pts',(-63.9723517369614,28.8354182946601,12.));
#89252=CARTESIAN_POINT('Ctrl Pts',(-63.9527147494423,28.8323382413789,12.));
#89253=CARTESIAN_POINT('Ctrl Pts',(-63.9331338646996,28.8292455077559,12.));
#89254=CARTESIAN_POINT('Ctrl Pts',(-63.9136093063786,28.8261402423291,12.));
#89255=CARTESIAN_POINT('Ctrl Pts',(-63.8941412856924,28.823022586318,12.));
#89256=CARTESIAN_POINT('Ctrl Pts',(-63.8747299825313,28.8198926619858,12.));
#89257=CARTESIAN_POINT('Ctrl Pts',(-63.8553755207487,28.8167505576681,12.));
#89258=CARTESIAN_POINT('Ctrl Pts',(-63.8360779669856,28.8135963263368,12.));
#89259=CARTESIAN_POINT('Ctrl Pts',(-63.8206854735028,28.8110632620957,12.));
#89260=CARTESIAN_POINT('Ctrl Pts',(-63.8091667271232,28.8091580239553,12.));
#89261=CARTESIAN_POINT('Ctrl Pts',(-63.8014989507494,28.8078854475432,12.));
#89262=CARTESIAN_POINT('Ctrl Pts',(-63.7976679095314,28.8072485549236,12.));
#89263=CARTESIAN_POINT('Ctrl Pts',(-68.8415926175085,27.6958230985044,-5.55111512312578E-16));
#89264=CARTESIAN_POINT('Ctrl Pts',(-68.8415926175085,27.6958230985044,4.));
#89265=CARTESIAN_POINT('Ctrl Pts',(-68.8415926175085,27.6958230985044,8.));
#89266=CARTESIAN_POINT('Ctrl Pts',(-68.8415926175085,27.6958230985044,12.));
#89267=CARTESIAN_POINT('Ctrl Pts',(-68.9176987693914,27.7750822307003,-5.55111512312578E-16));
#89268=CARTESIAN_POINT('Ctrl Pts',(-68.9176987693914,27.7750822307003,4.));
#89269=CARTESIAN_POINT('Ctrl Pts',(-68.9176987693914,27.7750822307003,8.00000000000001));
#89270=CARTESIAN_POINT('Ctrl Pts',(-68.9176987693914,27.7750822307003,12.));
#89271=CARTESIAN_POINT('Ctrl Pts',(-69.0029745467578,27.9589320265197,-5.55111512312578E-16));
#89272=CARTESIAN_POINT('Ctrl Pts',(-69.0029745467578,27.9589320265197,4.));
#89273=CARTESIAN_POINT('Ctrl Pts',(-69.0029745467578,27.9589320265197,8.));
#89274=CARTESIAN_POINT('Ctrl Pts',(-69.0029745467578,27.9589320265197,12.));
#89275=CARTESIAN_POINT('Ctrl Pts',(-68.9748773050757,28.1553386138879,-5.55111512312578E-16));
#89276=CARTESIAN_POINT('Ctrl Pts',(-68.9748773050757,28.1553386138879,4.));
#89277=CARTESIAN_POINT('Ctrl Pts',(-68.9748773050757,28.1553386138879,8.00000000000001));
#89278=CARTESIAN_POINT('Ctrl Pts',(-68.9748773050757,28.1553386138879,12.));
#89279=CARTESIAN_POINT('Ctrl Pts',(-68.943647523761,28.231604030224,-5.55111512312578E-16));
#89280=CARTESIAN_POINT('Ctrl Pts',(-68.943647523761,28.231604030224,4.));
#89281=CARTESIAN_POINT('Ctrl Pts',(-68.943647523761,28.231604030224,8.));
#89282=CARTESIAN_POINT('Ctrl Pts',(-68.943647523761,28.231604030224,12.));
#89283=CARTESIAN_POINT('',(-68.8415926175085,27.6958230985044,2.77555756156289E-16));
#89284=CARTESIAN_POINT('',(-68.9436475237613,28.2316040302241,0.));
#89285=CARTESIAN_POINT('Ctrl Pts',(-68.8415926175085,27.6958230985044,-1.38777878078145E-16));
#89286=CARTESIAN_POINT('Ctrl Pts',(-68.9176987693914,27.7750822307003,-1.38777878078145E-16));
#89287=CARTESIAN_POINT('Ctrl Pts',(-68.9664277850293,27.8801392568828,-1.38777878078145E-16));
#89288=CARTESIAN_POINT('Ctrl Pts',(-68.9781370393453,27.9892964598976,-1.38777878078145E-16));
#89289=CARTESIAN_POINT('Ctrl Pts',(-68.9869189800823,28.0711643621587,-1.38777878078145E-16));
#89290=CARTESIAN_POINT('Ctrl Pts',(-68.9748773050757,28.1553386138879,-1.38777878078145E-16));
#89291=CARTESIAN_POINT('Ctrl Pts',(-68.943647523761,28.231604030224,-1.38777878078145E-16));
#89292=CARTESIAN_POINT('',(-68.9436475237613,28.2316040302241,12.));
#89293=CARTESIAN_POINT('Ctrl Pts',(-68.943647523761,28.231604030224,-5.55111512312578E-16));
#89294=CARTESIAN_POINT('Ctrl Pts',(-68.943647523761,28.231604030224,4.));
#89295=CARTESIAN_POINT('Ctrl Pts',(-68.943647523761,28.231604030224,8.));
#89296=CARTESIAN_POINT('Ctrl Pts',(-68.943647523761,28.231604030224,12.));
#89297=CARTESIAN_POINT('',(-68.8415926175085,27.6958230985044,12.));
#89298=CARTESIAN_POINT('Ctrl Pts',(-68.943647523761,28.231604030224,12.));
#89299=CARTESIAN_POINT('Ctrl Pts',(-68.9748773050757,28.1553386138879,12.));
#89300=CARTESIAN_POINT('Ctrl Pts',(-68.9869189800823,28.0711643621587,12.));
#89301=CARTESIAN_POINT('Ctrl Pts',(-68.9781370393453,27.9892964598976,12.));
#89302=CARTESIAN_POINT('Ctrl Pts',(-68.9664277850293,27.8801392568828,12.));
#89303=CARTESIAN_POINT('Ctrl Pts',(-68.9176987693914,27.7750822307003,12.));
#89304=CARTESIAN_POINT('Ctrl Pts',(-68.8415926175085,27.6958230985044,12.));
#89305=CARTESIAN_POINT('Ctrl Pts',(-68.8415926175085,27.6958230985044,12.));
#89306=CARTESIAN_POINT('Ctrl Pts',(-68.8415926175085,27.6958230985044,8.));
#89307=CARTESIAN_POINT('Ctrl Pts',(-68.8415926175085,27.6958230985044,4.));
#89308=CARTESIAN_POINT('Ctrl Pts',(-68.8415926175085,27.6958230985044,-5.55111512312578E-16));
#89309=CARTESIAN_POINT('Origin',(-3.4634846687719E-10,1.43354795624835E-10,
0.));
#89310=CARTESIAN_POINT('Origin',(-3.4634846687719E-10,1.43354795624835E-10,
12.));
#89311=CARTESIAN_POINT('Origin',(-3.4634846687719E-10,1.43354795624835E-10,
0.));
#89312=CARTESIAN_POINT('Ctrl Pts',(-65.9427857825598,34.6669728017235,0.));
#89313=CARTESIAN_POINT('Ctrl Pts',(-65.9427857825598,34.6669728017235,4.));
#89314=CARTESIAN_POINT('Ctrl Pts',(-65.9427857825598,34.6669728017235,8.));
#89315=CARTESIAN_POINT('Ctrl Pts',(-65.9427857825598,34.6669728017235,12.));
#89316=CARTESIAN_POINT('Ctrl Pts',(-65.891654340017,34.7642339552033,0.));
#89317=CARTESIAN_POINT('Ctrl Pts',(-65.891654340017,34.7642339552033,4.));
#89318=CARTESIAN_POINT('Ctrl Pts',(-65.891654340017,34.7642339552033,8.00000000000001));
#89319=CARTESIAN_POINT('Ctrl Pts',(-65.891654340017,34.7642339552033,12.));
#89320=CARTESIAN_POINT('Ctrl Pts',(-65.7441961270806,34.9032616822021,0.));
#89321=CARTESIAN_POINT('Ctrl Pts',(-65.7441961270806,34.9032616822021,4.));
#89322=CARTESIAN_POINT('Ctrl Pts',(-65.7441961270806,34.9032616822021,7.99999999999999));
#89323=CARTESIAN_POINT('Ctrl Pts',(-65.7441961270806,34.9032616822021,12.));
#89324=CARTESIAN_POINT('Ctrl Pts',(-65.5489812297289,34.9387029822713,0.));
#89325=CARTESIAN_POINT('Ctrl Pts',(-65.5489812297289,34.9387029822713,4.));
#89326=CARTESIAN_POINT('Ctrl Pts',(-65.5489812297289,34.9387029822712,8.00000000000001));
#89327=CARTESIAN_POINT('Ctrl Pts',(-65.5489812297289,34.9387029822712,12.));
#89328=CARTESIAN_POINT('Ctrl Pts',(-65.4667541477958,34.9331875523083,0.));
#89329=CARTESIAN_POINT('Ctrl Pts',(-65.4667541477958,34.9331875523083,4.));
#89330=CARTESIAN_POINT('Ctrl Pts',(-65.4667541477958,34.9331875523082,8.));
#89331=CARTESIAN_POINT('Ctrl Pts',(-65.4667541477958,34.9331875523082,12.));
#89332=CARTESIAN_POINT('',(-65.9427857825598,34.6669728017235,0.));
#89333=CARTESIAN_POINT('',(-65.4667541477958,34.9331875523085,0.));
#89334=CARTESIAN_POINT('Ctrl Pts',(-65.9427857825598,34.6669728017235,0.));
#89335=CARTESIAN_POINT('Ctrl Pts',(-65.891654340017,34.7642339552033,0.));
#89336=CARTESIAN_POINT('Ctrl Pts',(-65.8073925040534,34.8436783706312,0.));
#89337=CARTESIAN_POINT('Ctrl Pts',(-65.7075366486888,34.8892986466535,0.));
#89338=CARTESIAN_POINT('Ctrl Pts',(-65.6326447571654,34.9235138536702,0.));
#89339=CARTESIAN_POINT('Ctrl Pts',(-65.5489812297289,34.9387029822713,0.));
#89340=CARTESIAN_POINT('Ctrl Pts',(-65.4667541477958,34.9331875523083,0.));
#89341=CARTESIAN_POINT('',(-65.4667541477958,34.9331875523085,12.));
#89342=CARTESIAN_POINT('Ctrl Pts',(-65.4667541477958,34.9331875523083,0.));
#89343=CARTESIAN_POINT('Ctrl Pts',(-65.4667541477958,34.9331875523083,4.));
#89344=CARTESIAN_POINT('Ctrl Pts',(-65.4667541477958,34.9331875523082,8.));
#89345=CARTESIAN_POINT('Ctrl Pts',(-65.4667541477958,34.9331875523082,12.));
#89346=CARTESIAN_POINT('',(-65.9427857825598,34.6669728017235,12.));
#89347=CARTESIAN_POINT('Ctrl Pts',(-65.4667541477958,34.9331875523082,12.));
#89348=CARTESIAN_POINT('Ctrl Pts',(-65.5489812297289,34.9387029822712,12.));
#89349=CARTESIAN_POINT('Ctrl Pts',(-65.6326447571654,34.9235138536702,12.));
#89350=CARTESIAN_POINT('Ctrl Pts',(-65.7075366486888,34.8892986466535,12.));
#89351=CARTESIAN_POINT('Ctrl Pts',(-65.8073925040534,34.8436783706312,12.));
#89352=CARTESIAN_POINT('Ctrl Pts',(-65.891654340017,34.7642339552033,12.));
#89353=CARTESIAN_POINT('Ctrl Pts',(-65.9427857825598,34.6669728017235,12.));
#89354=CARTESIAN_POINT('Ctrl Pts',(-65.9427857825598,34.6669728017235,12.));
#89355=CARTESIAN_POINT('Ctrl Pts',(-65.9427857825598,34.6669728017235,8.));
#89356=CARTESIAN_POINT('Ctrl Pts',(-65.9427857825598,34.6669728017235,4.));
#89357=CARTESIAN_POINT('Ctrl Pts',(-65.9427857825598,34.6669728017235,0.));
#89358=CARTESIAN_POINT('Ctrl Pts',(-61.0441813777723,34.2579614092497,0.));
#89359=CARTESIAN_POINT('Ctrl Pts',(-61.0441813777723,34.2579614092497,12.));
#89360=CARTESIAN_POINT('Ctrl Pts',(-61.0479423318725,34.2589297755433,0.));
#89361=CARTESIAN_POINT('Ctrl Pts',(-61.0479423318725,34.2589297755433,12.));
#89362=CARTESIAN_POINT('Ctrl Pts',(-61.0554700176998,34.2608658001631,0.));
#89363=CARTESIAN_POINT('Ctrl Pts',(-61.0554700176998,34.2608658001631,12.));
#89364=CARTESIAN_POINT('Ctrl Pts',(-61.0667788793266,34.2637677131934,0.));
#89365=CARTESIAN_POINT('Ctrl Pts',(-61.0667788793266,34.2637677131934,12.));
#89366=CARTESIAN_POINT('Ctrl Pts',(-61.0818920286293,34.2676326825626,0.));
#89367=CARTESIAN_POINT('Ctrl Pts',(-61.0818920286293,34.2676326825626,12.));
#89368=CARTESIAN_POINT('Ctrl Pts',(-61.1008412399997,34.2724568037227,0.));
#89369=CARTESIAN_POINT('Ctrl Pts',(-61.1008412399997,34.2724568037227,12.));
#89370=CARTESIAN_POINT('Ctrl Pts',(-61.1198481997764,34.277273803877,0.));
#89371=CARTESIAN_POINT('Ctrl Pts',(-61.1198481997764,34.277273803877,12.));
#89372=CARTESIAN_POINT('Ctrl Pts',(-61.1389128461886,34.2820836244469,0.));
#89373=CARTESIAN_POINT('Ctrl Pts',(-61.1389128461886,34.2820836244469,12.));
#89374=CARTESIAN_POINT('Ctrl Pts',(-61.1580350635533,34.2868861666384,0.));
#89375=CARTESIAN_POINT('Ctrl Pts',(-61.1580350635533,34.2868861666384,12.));
#89376=CARTESIAN_POINT('Ctrl Pts',(-61.1772146833205,34.2916812929751,0.));
#89377=CARTESIAN_POINT('Ctrl Pts',(-61.1772146833205,34.2916812929751,12.));
#89378=CARTESIAN_POINT('Ctrl Pts',(-61.1964515073891,34.2964688443663,0.));
#89379=CARTESIAN_POINT('Ctrl Pts',(-61.1964515073891,34.2964688443663,12.));
#89380=CARTESIAN_POINT('Ctrl Pts',(-61.2157453259107,34.3012486533474,0.));
#89381=CARTESIAN_POINT('Ctrl Pts',(-61.2157453259107,34.3012486533474,12.));
#89382=CARTESIAN_POINT('Ctrl Pts',(-61.235095936694,34.3060205584064,0.));
#89383=CARTESIAN_POINT('Ctrl Pts',(-61.235095936694,34.3060205584064,12.));
#89384=CARTESIAN_POINT('Ctrl Pts',(-61.2545031656133,34.3107844191043,0.));
#89385=CARTESIAN_POINT('Ctrl Pts',(-61.2545031656133,34.3107844191043,12.));
#89386=CARTESIAN_POINT('Ctrl Pts',(-61.2739668600365,34.3155401111747,0.));
#89387=CARTESIAN_POINT('Ctrl Pts',(-61.2739668600365,34.3155401111747,12.));
#89388=CARTESIAN_POINT('Ctrl Pts',(-61.2934868791855,34.3202875193617,0.));
#89389=CARTESIAN_POINT('Ctrl Pts',(-61.2934868791855,34.3202875193617,12.));
#89390=CARTESIAN_POINT('Ctrl Pts',(-61.3130630861386,34.3250265314768,0.));
#89391=CARTESIAN_POINT('Ctrl Pts',(-61.3130630861386,34.3250265314768,12.));
#89392=CARTESIAN_POINT('Ctrl Pts',(-61.3326953378851,34.3297570310146,0.));
#89393=CARTESIAN_POINT('Ctrl Pts',(-61.3326953378851,34.3297570310146,12.));
#89394=CARTESIAN_POINT('Ctrl Pts',(-61.3523834803188,34.3344788934363,0.));
#89395=CARTESIAN_POINT('Ctrl Pts',(-61.3523834803188,34.3344788934363,12.));
#89396=CARTESIAN_POINT('Ctrl Pts',(-61.3721273534257,34.339191990014,0.));
#89397=CARTESIAN_POINT('Ctrl Pts',(-61.3721273534257,34.339191990014,12.));
#89398=CARTESIAN_POINT('Ctrl Pts',(-61.3919267945302,34.3438961902405,0.));
#89399=CARTESIAN_POINT('Ctrl Pts',(-61.3919267945302,34.3438961902405,12.));
#89400=CARTESIAN_POINT('Ctrl Pts',(-61.4117816420229,34.3485913645979,0.));
#89401=CARTESIAN_POINT('Ctrl Pts',(-61.4117816420229,34.3485913645979,12.));
#89402=CARTESIAN_POINT('Ctrl Pts',(-61.4316917395918,34.3532773877089,0.));
#89403=CARTESIAN_POINT('Ctrl Pts',(-61.4316917395918,34.3532773877089,12.));
#89404=CARTESIAN_POINT('Ctrl Pts',(-61.4516569360454,34.3579541381996,0.));
#89405=CARTESIAN_POINT('Ctrl Pts',(-61.4516569360454,34.3579541381996,12.));
#89406=CARTESIAN_POINT('Ctrl Pts',(-61.4716770832897,34.3626214971888,0.));
#89407=CARTESIAN_POINT('Ctrl Pts',(-61.4716770832897,34.3626214971888,12.));
#89408=CARTESIAN_POINT('Ctrl Pts',(-61.4917520349279,34.3672793472465,0.));
#89409=CARTESIAN_POINT('Ctrl Pts',(-61.4917520349279,34.3672793472465,12.));
#89410=CARTESIAN_POINT('Ctrl Pts',(-61.5118816445437,34.3719275711195,0.));
#89411=CARTESIAN_POINT('Ctrl Pts',(-61.5118816445437,34.3719275711195,12.));
#89412=CARTESIAN_POINT('Ctrl Pts',(-61.5320657642639,34.376566050668,0.));
#89413=CARTESIAN_POINT('Ctrl Pts',(-61.5320657642639,34.376566050668,12.));
#89414=CARTESIAN_POINT('Ctrl Pts',(-61.5523042455158,34.3811946674196,0.));
#89415=CARTESIAN_POINT('Ctrl Pts',(-61.5523042455158,34.3811946674196,12.));
#89416=CARTESIAN_POINT('Ctrl Pts',(-61.5725969396829,34.3858133030518,0.));
#89417=CARTESIAN_POINT('Ctrl Pts',(-61.5725969396829,34.3858133030518,12.));
#89418=CARTESIAN_POINT('Ctrl Pts',(-61.5929436987409,34.3904218398636,0.));
#89419=CARTESIAN_POINT('Ctrl Pts',(-61.5929436987409,34.3904218398636,12.));
#89420=CARTESIAN_POINT('Ctrl Pts',(-61.6133443760142,34.3950201613432,0.));
#89421=CARTESIAN_POINT('Ctrl Pts',(-61.6133443760142,34.3950201613432,12.));
#89422=CARTESIAN_POINT('Ctrl Pts',(-61.6337988264556,34.3996081523753,0.));
#89423=CARTESIAN_POINT('Ctrl Pts',(-61.6337988264556,34.3996081523753,12.));
#89424=CARTESIAN_POINT('Ctrl Pts',(-61.6543069062416,34.4041856989316,0.));
#89425=CARTESIAN_POINT('Ctrl Pts',(-61.6543069062416,34.4041856989316,12.));
#89426=CARTESIAN_POINT('Ctrl Pts',(-61.6748684725205,34.4087526878812,0.));
#89427=CARTESIAN_POINT('Ctrl Pts',(-61.6748684725205,34.4087526878812,12.));
#89428=CARTESIAN_POINT('Ctrl Pts',(-61.695483383117,34.4133090067703,0.));
#89429=CARTESIAN_POINT('Ctrl Pts',(-61.695483383117,34.4133090067703,12.));
#89430=CARTESIAN_POINT('Ctrl Pts',(-61.7161514961915,34.4178545435766,0.));
#89431=CARTESIAN_POINT('Ctrl Pts',(-61.7161514961915,34.4178545435766,12.));
#89432=CARTESIAN_POINT('Ctrl Pts',(-61.7368726702596,34.4223891867179,0.));
#89433=CARTESIAN_POINT('Ctrl Pts',(-61.7368726702596,34.4223891867179,12.));
#89434=CARTESIAN_POINT('Ctrl Pts',(-61.7576467643432,34.4269128251576,0.));
#89435=CARTESIAN_POINT('Ctrl Pts',(-61.7576467643432,34.4269128251576,12.));
#89436=CARTESIAN_POINT('Ctrl Pts',(-61.7784736380727,34.4314253484791,0.));
#89437=CARTESIAN_POINT('Ctrl Pts',(-61.7784736380727,34.4314253484791,12.));
#89438=CARTESIAN_POINT('Ctrl Pts',(-61.7993531518037,34.4359266469749,0.));
#89439=CARTESIAN_POINT('Ctrl Pts',(-61.7993531518037,34.4359266469749,12.));
#89440=CARTESIAN_POINT('Ctrl Pts',(-61.8202851667222,34.4404166117299,0.));
#89441=CARTESIAN_POINT('Ctrl Pts',(-61.8202851667222,34.4404166117299,12.));
#89442=CARTESIAN_POINT('Ctrl Pts',(-61.8412695447926,34.4448951345739,0.));
#89443=CARTESIAN_POINT('Ctrl Pts',(-61.8412695447926,34.4448951345739,12.));
#89444=CARTESIAN_POINT('Ctrl Pts',(-61.8623061487018,34.449362108036,0.));
#89445=CARTESIAN_POINT('Ctrl Pts',(-61.8623061487018,34.449362108036,12.));
#89446=CARTESIAN_POINT('Ctrl Pts',(-61.8833948418025,34.4538174253012,0.));
#89447=CARTESIAN_POINT('Ctrl Pts',(-61.8833948418025,34.4538174253012,12.));
#89448=CARTESIAN_POINT('Ctrl Pts',(-61.9045354880445,34.4582609801637,0.));
#89449=CARTESIAN_POINT('Ctrl Pts',(-61.9045354880445,34.4582609801637,12.));
#89450=CARTESIAN_POINT('Ctrl Pts',(-61.9257279519308,34.4626926669974,0.));
#89451=CARTESIAN_POINT('Ctrl Pts',(-61.9257279519308,34.4626926669974,12.));
#89452=CARTESIAN_POINT('Ctrl Pts',(-61.9469720985531,34.4671123807717,0.));
#89453=CARTESIAN_POINT('Ctrl Pts',(-61.9469720985531,34.4671123807717,12.));
#89454=CARTESIAN_POINT('Ctrl Pts',(-61.9682677936054,34.4715200170592,0.));
#89455=CARTESIAN_POINT('Ctrl Pts',(-61.9682677936054,34.4715200170592,12.));
#89456=CARTESIAN_POINT('Ctrl Pts',(-61.9896149034001,34.4759154720473,0.));
#89457=CARTESIAN_POINT('Ctrl Pts',(-61.9896149034001,34.4759154720473,12.));
#89458=CARTESIAN_POINT('Ctrl Pts',(-62.0110132948794,34.4802986425528,0.));
#89459=CARTESIAN_POINT('Ctrl Pts',(-62.0110132948794,34.4802986425528,12.));
#89460=CARTESIAN_POINT('Ctrl Pts',(-62.0324628356141,34.4846694260199,0.));
#89461=CARTESIAN_POINT('Ctrl Pts',(-62.0324628356141,34.4846694260199,12.));
#89462=CARTESIAN_POINT('Ctrl Pts',(-62.0539633937939,34.4890277205039,0.));
#89463=CARTESIAN_POINT('Ctrl Pts',(-62.0539633937939,34.4890277205039,12.));
#89464=CARTESIAN_POINT('Ctrl Pts',(-62.0755148382135,34.4933734246592,0.));
#89465=CARTESIAN_POINT('Ctrl Pts',(-62.0755148382135,34.4933734246592,12.));
#89466=CARTESIAN_POINT('Ctrl Pts',(-62.0971170382567,34.4977064377282,0.));
#89467=CARTESIAN_POINT('Ctrl Pts',(-62.0971170382567,34.4977064377282,12.));
#89468=CARTESIAN_POINT('Ctrl Pts',(-62.1187698638707,34.5020266595293,0.));
#89469=CARTESIAN_POINT('Ctrl Pts',(-62.1187698638707,34.5020266595293,12.));
#89470=CARTESIAN_POINT('Ctrl Pts',(-62.1404731855687,34.5063339904533,0.));
#89471=CARTESIAN_POINT('Ctrl Pts',(-62.1404731855687,34.5063339904533,12.));
#89472=CARTESIAN_POINT('Ctrl Pts',(-62.1622268744337,34.5106283314594,0.));
#89473=CARTESIAN_POINT('Ctrl Pts',(-62.1622268744337,34.5106283314594,12.));
#89474=CARTESIAN_POINT('Ctrl Pts',(-62.1840308021171,34.5149095840729,0.));
#89475=CARTESIAN_POINT('Ctrl Pts',(-62.1840308021171,34.5149095840729,12.));
#89476=CARTESIAN_POINT('Ctrl Pts',(-62.2058848408346,34.5191776503843,0.));
#89477=CARTESIAN_POINT('Ctrl Pts',(-62.2058848408346,34.5191776503843,12.));
#89478=CARTESIAN_POINT('Ctrl Pts',(-62.2277888633577,34.5234324330492,0.));
#89479=CARTESIAN_POINT('Ctrl Pts',(-62.2277888633577,34.5234324330492,12.));
#89480=CARTESIAN_POINT('Ctrl Pts',(-62.2497427430136,34.527673835281,0.));
#89481=CARTESIAN_POINT('Ctrl Pts',(-62.2497427430136,34.527673835281,12.));
#89482=CARTESIAN_POINT('Ctrl Pts',(-62.2717463536828,34.5319017608434,0.));
#89483=CARTESIAN_POINT('Ctrl Pts',(-62.2717463536828,34.5319017608434,12.));
#89484=CARTESIAN_POINT('Ctrl Pts',(-62.2937995697927,34.536116114045,0.));
#89485=CARTESIAN_POINT('Ctrl Pts',(-62.2937995697927,34.536116114045,12.));
#89486=CARTESIAN_POINT('Ctrl Pts',(-62.3159022663052,34.5403167997333,0.));
#89487=CARTESIAN_POINT('Ctrl Pts',(-62.3159022663052,34.5403167997333,12.));
#89488=CARTESIAN_POINT('Ctrl Pts',(-62.3380543187067,34.5445037232928,0.));
#89489=CARTESIAN_POINT('Ctrl Pts',(-62.3380543187067,34.5445037232928,12.));
#89490=CARTESIAN_POINT('Ctrl Pts',(-62.3602556030114,34.5486767906376,0.));
#89491=CARTESIAN_POINT('Ctrl Pts',(-62.3602556030114,34.5486767906376,12.));
#89492=CARTESIAN_POINT('Ctrl Pts',(-62.3825059957593,34.552835908207,0.));
#89493=CARTESIAN_POINT('Ctrl Pts',(-62.3825059957593,34.552835908207,12.));
#89494=CARTESIAN_POINT('Ctrl Pts',(-62.4048053740129,34.5569809829615,0.));
#89495=CARTESIAN_POINT('Ctrl Pts',(-62.4048053740129,34.5569809829615,12.));
#89496=CARTESIAN_POINT('Ctrl Pts',(-62.4271536153473,34.5611119223807,0.));
#89497=CARTESIAN_POINT('Ctrl Pts',(-62.4271536153473,34.5611119223807,12.));
#89498=CARTESIAN_POINT('Ctrl Pts',(-62.4495505978415,34.5652286344606,0.));
#89499=CARTESIAN_POINT('Ctrl Pts',(-62.4495505978415,34.5652286344606,12.));
#89500=CARTESIAN_POINT('Ctrl Pts',(-62.471996200083,34.5693310277064,0.));
#89501=CARTESIAN_POINT('Ctrl Pts',(-62.471996200083,34.5693310277064,12.));
#89502=CARTESIAN_POINT('Ctrl Pts',(-62.494490301164,34.5734190111279,0.));
#89503=CARTESIAN_POINT('Ctrl Pts',(-62.494490301164,34.5734190111279,12.));
#89504=CARTESIAN_POINT('Ctrl Pts',(-62.5170327806774,34.5774924942351,0.));
#89505=CARTESIAN_POINT('Ctrl Pts',(-62.5170327806774,34.5774924942351,12.));
#89506=CARTESIAN_POINT('Ctrl Pts',(-62.5396235187053,34.5815513870363,0.));
#89507=CARTESIAN_POINT('Ctrl Pts',(-62.5396235187053,34.5815513870363,12.));
#89508=CARTESIAN_POINT('Ctrl Pts',(-62.5622623958125,34.5855956000343,0.));
#89509=CARTESIAN_POINT('Ctrl Pts',(-62.5622623958125,34.5855956000343,12.));
#89510=CARTESIAN_POINT('Ctrl Pts',(-62.5849492930501,34.5896250442199,0.));
#89511=CARTESIAN_POINT('Ctrl Pts',(-62.5849492930501,34.5896250442199,12.));
#89512=CARTESIAN_POINT('Ctrl Pts',(-62.6076840919521,34.5936396310671,0.));
#89513=CARTESIAN_POINT('Ctrl Pts',(-62.6076840919521,34.5936396310671,12.));
#89514=CARTESIAN_POINT('Ctrl Pts',(-62.6304666745319,34.5976392725303,0.));
#89515=CARTESIAN_POINT('Ctrl Pts',(-62.6304666745319,34.5976392725303,12.));
#89516=CARTESIAN_POINT('Ctrl Pts',(-62.6532969232695,34.6016238810419,0.));
#89517=CARTESIAN_POINT('Ctrl Pts',(-62.6532969232695,34.6016238810419,12.));
#89518=CARTESIAN_POINT('Ctrl Pts',(-62.6761747211081,34.6055933695093,0.));
#89519=CARTESIAN_POINT('Ctrl Pts',(-62.6761747211081,34.6055933695093,12.));
#89520=CARTESIAN_POINT('Ctrl Pts',(-62.6990999514597,34.6095476513094,0.));
#89521=CARTESIAN_POINT('Ctrl Pts',(-62.6990999514597,34.6095476513094,12.));
#89522=CARTESIAN_POINT('Ctrl Pts',(-62.7220724982005,34.6134866402842,0.));
#89523=CARTESIAN_POINT('Ctrl Pts',(-62.7220724982005,34.6134866402842,12.));
#89524=CARTESIAN_POINT('Ctrl Pts',(-62.7450922456663,34.6174102507368,0.));
#89525=CARTESIAN_POINT('Ctrl Pts',(-62.7450922456663,34.6174102507368,12.));
#89526=CARTESIAN_POINT('Ctrl Pts',(-62.7681590786398,34.6213183974302,0.));
#89527=CARTESIAN_POINT('Ctrl Pts',(-62.7681590786398,34.6213183974302,12.));
#89528=CARTESIAN_POINT('Ctrl Pts',(-62.7912728823483,34.6252109955836,0.));
#89529=CARTESIAN_POINT('Ctrl Pts',(-62.7912728823483,34.6252109955836,12.));
#89530=CARTESIAN_POINT('Ctrl Pts',(-62.8144335424671,34.629087960866,0.));
#89531=CARTESIAN_POINT('Ctrl Pts',(-62.8144335424671,34.629087960866,12.));
#89532=CARTESIAN_POINT('Ctrl Pts',(-62.8376409451167,34.6329492093931,0.));
#89533=CARTESIAN_POINT('Ctrl Pts',(-62.8376409451167,34.6329492093931,12.));
#89534=CARTESIAN_POINT('Ctrl Pts',(-62.8608949768583,34.6367946577241,0.));
#89535=CARTESIAN_POINT('Ctrl Pts',(-62.8608949768583,34.6367946577241,12.));
#89536=CARTESIAN_POINT('Ctrl Pts',(-62.884195524682,34.6406242228606,0.));
#89537=CARTESIAN_POINT('Ctrl Pts',(-62.884195524682,34.6406242228606,12.));
#89538=CARTESIAN_POINT('Ctrl Pts',(-62.9075424760042,34.6444378222425,0.));
#89539=CARTESIAN_POINT('Ctrl Pts',(-62.9075424760042,34.6444378222425,12.));
#89540=CARTESIAN_POINT('Ctrl Pts',(-62.9309357186733,34.6482353737433,0.));
#89541=CARTESIAN_POINT('Ctrl Pts',(-62.9309357186733,34.6482353737433,12.));
#89542=CARTESIAN_POINT('Ctrl Pts',(-62.9543751409648,34.6520167956656,0.));
#89543=CARTESIAN_POINT('Ctrl Pts',(-62.9543751409648,34.6520167956656,12.));
#89544=CARTESIAN_POINT('Ctrl Pts',(-62.9778606315777,34.6557820067389,0.));
#89545=CARTESIAN_POINT('Ctrl Pts',(-62.9778606315777,34.6557820067389,12.));
#89546=CARTESIAN_POINT('Ctrl Pts',(-63.0013920796225,34.6595309261185,0.));
#89547=CARTESIAN_POINT('Ctrl Pts',(-63.0013920796225,34.6595309261185,12.));
#89548=CARTESIAN_POINT('Ctrl Pts',(-63.0249693746199,34.6632634733819,0.));
#89549=CARTESIAN_POINT('Ctrl Pts',(-63.0249693746199,34.6632634733819,12.));
#89550=CARTESIAN_POINT('Ctrl Pts',(-63.0485924065039,34.6669795685225,0.));
#89551=CARTESIAN_POINT('Ctrl Pts',(-63.0485924065039,34.6669795685225,12.));
#89552=CARTESIAN_POINT('Ctrl Pts',(-63.0722610656194,34.670679131947,0.));
#89553=CARTESIAN_POINT('Ctrl Pts',(-63.0722610656194,34.670679131947,12.));
#89554=CARTESIAN_POINT('Ctrl Pts',(-63.095975242717,34.6743620844721,0.));
#89555=CARTESIAN_POINT('Ctrl Pts',(-63.095975242717,34.6743620844721,12.));
#89556=CARTESIAN_POINT('Ctrl Pts',(-63.1197348289431,34.6780283473252,0.));
#89557=CARTESIAN_POINT('Ctrl Pts',(-63.1197348289431,34.6780283473252,12.));
#89558=CARTESIAN_POINT('Ctrl Pts',(-63.1435397158386,34.68167784214,0.));
#89559=CARTESIAN_POINT('Ctrl Pts',(-63.1435397158386,34.68167784214,12.));
#89560=CARTESIAN_POINT('Ctrl Pts',(-63.1673897953425,34.6853104909516,0.));
#89561=CARTESIAN_POINT('Ctrl Pts',(-63.1673897953425,34.6853104909516,12.));
#89562=CARTESIAN_POINT('Ctrl Pts',(-63.1912849597885,34.6889262161923,0.));
#89563=CARTESIAN_POINT('Ctrl Pts',(-63.1912849597885,34.6889262161923,12.));
#89564=CARTESIAN_POINT('Ctrl Pts',(-63.2152251019014,34.6925249406898,0.));
#89565=CARTESIAN_POINT('Ctrl Pts',(-63.2152251019014,34.6925249406898,12.));
#89566=CARTESIAN_POINT('Ctrl Pts',(-63.2392101147854,34.696106587667,0.));
#89567=CARTESIAN_POINT('Ctrl Pts',(-63.2392101147854,34.696106587667,12.));
#89568=CARTESIAN_POINT('Ctrl Pts',(-63.2632398919234,34.6996710807384,0.));
#89569=CARTESIAN_POINT('Ctrl Pts',(-63.2632398919234,34.6996710807384,12.));
#89570=CARTESIAN_POINT('Ctrl Pts',(-63.2873143271813,34.7032183439045,0.));
#89571=CARTESIAN_POINT('Ctrl Pts',(-63.2873143271813,34.7032183439045,12.));
#89572=CARTESIAN_POINT('Ctrl Pts',(-63.311433314805,34.7067483015492,0.));
#89573=CARTESIAN_POINT('Ctrl Pts',(-63.311433314805,34.7067483015492,12.));
#89574=CARTESIAN_POINT('Ctrl Pts',(-63.3355967494169,34.7102608784372,0.));
#89575=CARTESIAN_POINT('Ctrl Pts',(-63.3355967494169,34.7102608784372,12.));
#89576=CARTESIAN_POINT('Ctrl Pts',(-63.359804526005,34.7137559997143,0.));
#89577=CARTESIAN_POINT('Ctrl Pts',(-63.359804526005,34.7137559997143,12.));
#89578=CARTESIAN_POINT('Ctrl Pts',(-63.3840565399207,34.7172335909037,0.));
#89579=CARTESIAN_POINT('Ctrl Pts',(-63.3840565399207,34.7172335909037,12.));
#89580=CARTESIAN_POINT('Ctrl Pts',(-63.4083526868837,34.7206935779007,0.));
#89581=CARTESIAN_POINT('Ctrl Pts',(-63.4083526868837,34.7206935779007,12.));
#89582=CARTESIAN_POINT('Ctrl Pts',(-63.4326928629797,34.7241358869701,0.));
#89583=CARTESIAN_POINT('Ctrl Pts',(-63.4326928629797,34.7241358869701,12.));
#89584=CARTESIAN_POINT('Ctrl Pts',(-63.4570769646568,34.7275604447438,0.));
#89585=CARTESIAN_POINT('Ctrl Pts',(-63.4570769646568,34.7275604447438,12.));
#89586=CARTESIAN_POINT('Ctrl Pts',(-63.4815048887161,34.7309671782211,0.));
#89587=CARTESIAN_POINT('Ctrl Pts',(-63.4815048887161,34.7309671782211,12.));
#89588=CARTESIAN_POINT('Ctrl Pts',(-63.5059765323082,34.7343560147663,0.));
#89589=CARTESIAN_POINT('Ctrl Pts',(-63.5059765323082,34.7343560147663,12.));
#89590=CARTESIAN_POINT('Ctrl Pts',(-63.5304917929378,34.7377268821022,0.));
#89591=CARTESIAN_POINT('Ctrl Pts',(-63.5304917929378,34.7377268821022,12.));
#89592=CARTESIAN_POINT('Ctrl Pts',(-63.5550505684621,34.7410797083079,0.));
#89593=CARTESIAN_POINT('Ctrl Pts',(-63.5550505684621,34.7410797083079,12.));
#89594=CARTESIAN_POINT('Ctrl Pts',(-63.5796527570874,34.7444144218162,0.));
#89595=CARTESIAN_POINT('Ctrl Pts',(-63.5796527570874,34.7444144218162,12.));
#89596=CARTESIAN_POINT('Ctrl Pts',(-63.6042982573599,34.7477309514142,0.));
#89597=CARTESIAN_POINT('Ctrl Pts',(-63.6042982573599,34.7477309514142,12.));
#89598=CARTESIAN_POINT('Ctrl Pts',(-63.628986968162,34.7510292262415,0.));
#89599=CARTESIAN_POINT('Ctrl Pts',(-63.628986968162,34.7510292262415,12.));
#89600=CARTESIAN_POINT('Ctrl Pts',(-63.6537187887174,34.7543091757841,0.));
#89601=CARTESIAN_POINT('Ctrl Pts',(-63.6537187887174,34.7543091757841,12.));
#89602=CARTESIAN_POINT('Ctrl Pts',(-63.6784936185893,34.7575707298718,0.));
#89603=CARTESIAN_POINT('Ctrl Pts',(-63.6784936185893,34.7575707298718,12.));
#89604=CARTESIAN_POINT('Ctrl Pts',(-63.7033113576782,34.7608138186757,0.));
#89605=CARTESIAN_POINT('Ctrl Pts',(-63.7033113576782,34.7608138186757,12.));
#89606=CARTESIAN_POINT('Ctrl Pts',(-63.7281719062136,34.7640383727093,0.));
#89607=CARTESIAN_POINT('Ctrl Pts',(-63.7281719062136,34.7640383727093,12.));
#89608=CARTESIAN_POINT('Ctrl Pts',(-63.7530751647479,34.7672443228266,0.));
#89609=CARTESIAN_POINT('Ctrl Pts',(-63.7530751647479,34.7672443228266,12.));
#89610=CARTESIAN_POINT('Ctrl Pts',(-63.7780210341619,34.7704316002165,0.));
#89611=CARTESIAN_POINT('Ctrl Pts',(-63.7780210341619,34.7704316002165,12.));
#89612=CARTESIAN_POINT('Ctrl Pts',(-63.8030094156635,34.7736001363991,0.));
#89613=CARTESIAN_POINT('Ctrl Pts',(-63.8030094156635,34.7736001363991,12.));
#89614=CARTESIAN_POINT('Ctrl Pts',(-63.8280402107858,34.7767498632244,0.));
#89615=CARTESIAN_POINT('Ctrl Pts',(-63.8280402107858,34.7767498632244,12.));
#89616=CARTESIAN_POINT('Ctrl Pts',(-63.8531133213794,34.7798807128715,0.));
#89617=CARTESIAN_POINT('Ctrl Pts',(-63.8531133213794,34.7798807128715,12.));
#89618=CARTESIAN_POINT('Ctrl Pts',(-63.8782286496059,34.7829926178495,0.));
#89619=CARTESIAN_POINT('Ctrl Pts',(-63.8782286496059,34.7829926178495,12.));
#89620=CARTESIAN_POINT('Ctrl Pts',(-63.9033860979429,34.7860855109907,0.));
#89621=CARTESIAN_POINT('Ctrl Pts',(-63.9033860979429,34.7860855109907,12.));
#89622=CARTESIAN_POINT('Ctrl Pts',(-63.9285855691839,34.7891593254485,0.));
#89623=CARTESIAN_POINT('Ctrl Pts',(-63.9285855691839,34.7891593254485,12.));
#89624=CARTESIAN_POINT('Ctrl Pts',(-63.9538269664366,34.7922139946943,0.));
#89625=CARTESIAN_POINT('Ctrl Pts',(-63.9538269664366,34.7922139946943,12.));
#89626=CARTESIAN_POINT('Ctrl Pts',(-63.9791101931169,34.7952494525182,0.));
#89627=CARTESIAN_POINT('Ctrl Pts',(-63.9791101931169,34.7952494525182,12.));
#89628=CARTESIAN_POINT('Ctrl Pts',(-64.0044351529413,34.79826563303,0.));
#89629=CARTESIAN_POINT('Ctrl Pts',(-64.0044351529413,34.79826563303,12.));
#89630=CARTESIAN_POINT('Ctrl Pts',(-64.0298017499305,34.8012624706533,0.));
#89631=CARTESIAN_POINT('Ctrl Pts',(-64.0298017499305,34.8012624706533,12.));
#89632=CARTESIAN_POINT('Ctrl Pts',(-64.0552098884101,34.8042399001214,0.));
#89633=CARTESIAN_POINT('Ctrl Pts',(-64.0552098884101,34.8042399001214,12.));
#89634=CARTESIAN_POINT('Ctrl Pts',(-64.0806594730085,34.8071978564748,0.));
#89635=CARTESIAN_POINT('Ctrl Pts',(-64.0806594730085,34.8071978564748,12.));
#89636=CARTESIAN_POINT('Ctrl Pts',(-64.1061504086512,34.8101362750595,0.));
#89637=CARTESIAN_POINT('Ctrl Pts',(-64.1061504086512,34.8101362750595,12.));
#89638=CARTESIAN_POINT('Ctrl Pts',(-64.1316826005502,34.8130550915283,0.));
#89639=CARTESIAN_POINT('Ctrl Pts',(-64.1316826005502,34.8130550915283,12.));
#89640=CARTESIAN_POINT('Ctrl Pts',(-64.1572559542085,34.8159542418372,0.));
#89641=CARTESIAN_POINT('Ctrl Pts',(-64.1572559542085,34.8159542418372,12.));
#89642=CARTESIAN_POINT('Ctrl Pts',(-64.1828703754237,34.8188336622418,0.));
#89643=CARTESIAN_POINT('Ctrl Pts',(-64.1828703754237,34.8188336622418,12.));
#89644=CARTESIAN_POINT('Ctrl Pts',(-64.2085257702885,34.8216932892969,0.));
#89645=CARTESIAN_POINT('Ctrl Pts',(-64.2085257702885,34.8216932892969,12.));
#89646=CARTESIAN_POINT('Ctrl Pts',(-64.2342220451878,34.8245330598559,0.));
#89647=CARTESIAN_POINT('Ctrl Pts',(-64.2342220451878,34.8245330598559,12.));
#89648=CARTESIAN_POINT('Ctrl Pts',(-64.259959106791,34.8273529110742,0.));
#89649=CARTESIAN_POINT('Ctrl Pts',(-64.259959106791,34.8273529110742,12.));
#89650=CARTESIAN_POINT('Ctrl Pts',(-64.2857368620513,34.8301527804052,0.));
#89651=CARTESIAN_POINT('Ctrl Pts',(-64.2857368620513,34.8301527804052,12.));
#89652=CARTESIAN_POINT('Ctrl Pts',(-64.3115552182056,34.8329326055916,0.));
#89653=CARTESIAN_POINT('Ctrl Pts',(-64.3115552182056,34.8329326055916,12.));
#89654=CARTESIAN_POINT('Ctrl Pts',(-64.3374140827708,34.8356923246617,0.));
#89655=CARTESIAN_POINT('Ctrl Pts',(-64.3374140827708,34.8356923246617,12.));
#89656=CARTESIAN_POINT('Ctrl Pts',(-64.3633133635385,34.8384318759249,0.));
#89657=CARTESIAN_POINT('Ctrl Pts',(-64.3633133635385,34.8384318759249,12.));
#89658=CARTESIAN_POINT('Ctrl Pts',(-64.3892529685614,34.8411511979705,0.));
#89659=CARTESIAN_POINT('Ctrl Pts',(-64.3892529685614,34.8411511979705,12.));
#89660=CARTESIAN_POINT('Ctrl Pts',(-64.4152328061526,34.8438502296669,0.));
#89661=CARTESIAN_POINT('Ctrl Pts',(-64.4152328061526,34.8438502296669,12.));
#89662=CARTESIAN_POINT('Ctrl Pts',(-64.441252784898,34.8465289101626,0.));
#89663=CARTESIAN_POINT('Ctrl Pts',(-64.441252784898,34.8465289101626,12.));
#89664=CARTESIAN_POINT('Ctrl Pts',(-64.4673128136631,34.8491871788898,0.));
#89665=CARTESIAN_POINT('Ctrl Pts',(-64.4673128136631,34.8491871788898,12.));
#89666=CARTESIAN_POINT('Ctrl Pts',(-64.4934128015983,34.8518249755679,0.));
#89667=CARTESIAN_POINT('Ctrl Pts',(-64.4934128015983,34.8518249755679,12.));
#89668=CARTESIAN_POINT('Ctrl Pts',(-64.5195526581398,34.8544422402114,0.));
#89669=CARTESIAN_POINT('Ctrl Pts',(-64.5195526581398,34.8544422402114,12.));
#89670=CARTESIAN_POINT('Ctrl Pts',(-64.5457322930074,34.8570389131334,0.));
#89671=CARTESIAN_POINT('Ctrl Pts',(-64.5457322930074,34.8570389131334,12.));
#89672=CARTESIAN_POINT('Ctrl Pts',(-64.5719516161914,34.859614934925,0.));
#89673=CARTESIAN_POINT('Ctrl Pts',(-64.5719516161914,34.859614934925,12.));
#89674=CARTESIAN_POINT('Ctrl Pts',(-64.5982105379374,34.8621702464397,0.));
#89675=CARTESIAN_POINT('Ctrl Pts',(-64.5982105379374,34.8621702464397,12.));
#89676=CARTESIAN_POINT('Ctrl Pts',(-64.6245089687276,34.8647047887774,0.));
#89677=CARTESIAN_POINT('Ctrl Pts',(-64.6245089687276,34.8647047887774,12.));
#89678=CARTESIAN_POINT('Ctrl Pts',(-64.6508468192609,34.8672185032724,0.));
#89679=CARTESIAN_POINT('Ctrl Pts',(-64.6508468192609,34.8672185032724,12.));
#89680=CARTESIAN_POINT('Ctrl Pts',(-64.6772240004241,34.8697113314797,0.));
#89681=CARTESIAN_POINT('Ctrl Pts',(-64.6772240004241,34.8697113314797,12.));
#89682=CARTESIAN_POINT('Ctrl Pts',(-64.7036404233319,34.8721832151981,0.));
#89683=CARTESIAN_POINT('Ctrl Pts',(-64.7036404233319,34.8721832151981,12.));
#89684=CARTESIAN_POINT('Ctrl Pts',(-64.7300959993662,34.8746340964976,0.));
#89685=CARTESIAN_POINT('Ctrl Pts',(-64.7300959993662,34.8746340964976,12.));
#89686=CARTESIAN_POINT('Ctrl Pts',(-64.7565906402154,34.8770639177494,0.));
#89687=CARTESIAN_POINT('Ctrl Pts',(-64.7565906402154,34.8770639177494,12.));
#89688=CARTESIAN_POINT('Ctrl Pts',(-64.7831242579023,34.8794726216511,0.));
#89689=CARTESIAN_POINT('Ctrl Pts',(-64.7831242579023,34.8794726216511,12.));
#89690=CARTESIAN_POINT('Ctrl Pts',(-64.80969676483,34.8818601512726,0.));
#89691=CARTESIAN_POINT('Ctrl Pts',(-64.80969676483,34.8818601512726,12.));
#89692=CARTESIAN_POINT('Ctrl Pts',(-64.8363080737369,34.8842264500184,0.));
#89693=CARTESIAN_POINT('Ctrl Pts',(-64.8363080737369,34.8842264500184,12.));
#89694=CARTESIAN_POINT('Ctrl Pts',(-64.8629580976057,34.8865714615433,0.));
#89695=CARTESIAN_POINT('Ctrl Pts',(-64.8629580976057,34.8865714615433,12.));
#89696=CARTESIAN_POINT('Ctrl Pts',(-64.8896467495755,34.8888951296809,0.));
#89697=CARTESIAN_POINT('Ctrl Pts',(-64.8896467495755,34.8888951296809,12.));
#89698=CARTESIAN_POINT('Ctrl Pts',(-64.9163739428606,34.8911973983785,0.));
#89699=CARTESIAN_POINT('Ctrl Pts',(-64.9163739428606,34.8911973983785,12.));
#89700=CARTESIAN_POINT('Ctrl Pts',(-64.9431395906341,34.8934782116097,0.));
#89701=CARTESIAN_POINT('Ctrl Pts',(-64.9431395906341,34.8934782116097,12.));
#89702=CARTESIAN_POINT('Ctrl Pts',(-64.9699436060178,34.8957375133702,0.));
#89703=CARTESIAN_POINT('Ctrl Pts',(-64.9699436060178,34.8957375133702,12.));
#89704=CARTESIAN_POINT('Ctrl Pts',(-64.9967859023225,34.8979752478623,0.));
#89705=CARTESIAN_POINT('Ctrl Pts',(-64.9967859023225,34.8979752478623,12.));
#89706=CARTESIAN_POINT('Ctrl Pts',(-65.0236663932338,34.9001913596421,0.));
#89707=CARTESIAN_POINT('Ctrl Pts',(-65.0236663932338,34.9001913596421,12.));
#89708=CARTESIAN_POINT('Ctrl Pts',(-65.0505849930173,34.9023857937866,0.));
#89709=CARTESIAN_POINT('Ctrl Pts',(-65.0505849930173,34.9023857937866,12.));
#89710=CARTESIAN_POINT('Ctrl Pts',(-65.0775416167073,34.9045584960503,0.));
#89711=CARTESIAN_POINT('Ctrl Pts',(-65.0775416167073,34.9045584960503,12.));
#89712=CARTESIAN_POINT('Ctrl Pts',(-65.1045361803097,34.9067094130386,0.));
#89713=CARTESIAN_POINT('Ctrl Pts',(-65.1045361803097,34.9067094130386,12.));
#89714=CARTESIAN_POINT('Ctrl Pts',(-65.1315686003485,34.9088384918321,0.));
#89715=CARTESIAN_POINT('Ctrl Pts',(-65.1315686003485,34.9088384918321,12.));
#89716=CARTESIAN_POINT('Ctrl Pts',(-65.1586387934216,34.9109456796201,0.));
#89717=CARTESIAN_POINT('Ctrl Pts',(-65.1586387934216,34.9109456796201,12.));
#89718=CARTESIAN_POINT('Ctrl Pts',(-65.1857466757082,34.9130309233017,0.));
#89719=CARTESIAN_POINT('Ctrl Pts',(-65.1857466757082,34.9130309233017,12.));
#89720=CARTESIAN_POINT('Ctrl Pts',(-65.2128921625838,34.9150941691754,0.));
#89721=CARTESIAN_POINT('Ctrl Pts',(-65.2128921625838,34.9150941691754,12.));
#89722=CARTESIAN_POINT('Ctrl Pts',(-65.2400751679586,34.9171353624131,0.));
#89723=CARTESIAN_POINT('Ctrl Pts',(-65.2400751679586,34.9171353624131,12.));
#89724=CARTESIAN_POINT('Ctrl Pts',(-65.2672956048121,34.9191544474898,0.));
#89725=CARTESIAN_POINT('Ctrl Pts',(-65.2672956048121,34.9191544474898,12.));
#89726=CARTESIAN_POINT('Ctrl Pts',(-65.2945533863812,34.921151369138,0.));
#89727=CARTESIAN_POINT('Ctrl Pts',(-65.2945533863812,34.921151369138,12.));
#89728=CARTESIAN_POINT('Ctrl Pts',(-65.3218484271941,34.9231260731846,0.));
#89729=CARTESIAN_POINT('Ctrl Pts',(-65.3218484271941,34.9231260731846,12.));
#89730=CARTESIAN_POINT('Ctrl Pts',(-65.3491806440529,34.9250785073473,0.));
#89731=CARTESIAN_POINT('Ctrl Pts',(-65.3491806440529,34.9250785073473,12.));
#89732=CARTESIAN_POINT('Ctrl Pts',(-65.3765499573019,34.9270086222703,0.));
#89733=CARTESIAN_POINT('Ctrl Pts',(-65.3765499573019,34.9270086222703,12.));
#89734=CARTESIAN_POINT('Ctrl Pts',(-65.4039562911255,34.92891637177,0.));
#89735=CARTESIAN_POINT('Ctrl Pts',(-65.4039562911255,34.92891637177,12.));
#89736=CARTESIAN_POINT('Ctrl Pts',(-65.4313995707423,34.9308017105481,0.));
#89737=CARTESIAN_POINT('Ctrl Pts',(-65.4313995707423,34.9308017105481,12.));
#89738=CARTESIAN_POINT('Ctrl Pts',(-65.4588797201884,34.9326645923897,0.));
#89739=CARTESIAN_POINT('Ctrl Pts',(-65.4588797201884,34.9326645923897,12.));
#89740=CARTESIAN_POINT('Ctrl Pts',(-65.4863966597524,34.9345049680816,0.));
#89741=CARTESIAN_POINT('Ctrl Pts',(-65.4863966597524,34.9345049680816,12.));
#89742=CARTESIAN_POINT('Ctrl Pts',(-65.5139503038116,34.9363227836621,0.));
#89743=CARTESIAN_POINT('Ctrl Pts',(-65.5139503038116,34.9363227836621,12.));
#89744=CARTESIAN_POINT('Ctrl Pts',(-65.5415405578138,34.9381179779762,0.));
#89745=CARTESIAN_POINT('Ctrl Pts',(-65.5415405578138,34.9381179779762,12.));
#89746=CARTESIAN_POINT('Ctrl Pts',(-65.5691673226051,34.9398904862278,0.));
#89747=CARTESIAN_POINT('Ctrl Pts',(-65.5691673226051,34.9398904862278,12.));
#89748=CARTESIAN_POINT('Ctrl Pts',(-65.5968304997822,34.9416402443551,0.));
#89749=CARTESIAN_POINT('Ctrl Pts',(-65.5968304997822,34.9416402443551,12.));
#89750=CARTESIAN_POINT('Ctrl Pts',(-65.6245299968636,34.9433671932982,0.));
#89751=CARTESIAN_POINT('Ctrl Pts',(-65.6245299968636,34.9433671932982,12.));
#89752=CARTESIAN_POINT('Ctrl Pts',(-65.652265732124,34.9450712829142,0.));
#89753=CARTESIAN_POINT('Ctrl Pts',(-65.652265732124,34.9450712829142,12.));
#89754=CARTESIAN_POINT('Ctrl Pts',(-65.6800376405722,34.9467524770271,0.));
#89755=CARTESIAN_POINT('Ctrl Pts',(-65.6800376405722,34.9467524770271,12.));
#89756=CARTESIAN_POINT('Ctrl Pts',(-65.707845675746,34.9484107543856,0.));
#89757=CARTESIAN_POINT('Ctrl Pts',(-65.707845675746,34.9484107543856,12.));
#89758=CARTESIAN_POINT('Ctrl Pts',(-65.7356898060478,34.9500461042919,0.));
#89759=CARTESIAN_POINT('Ctrl Pts',(-65.7356898060478,34.9500461042919,12.));
#89760=CARTESIAN_POINT('Ctrl Pts',(-65.757993971173,34.9513360397181,0.));
#89761=CARTESIAN_POINT('Ctrl Pts',(-65.757993971173,34.9513360397181,12.));
#89762=CARTESIAN_POINT('Ctrl Pts',(-65.7747383250775,34.9522931728594,0.));
#89763=CARTESIAN_POINT('Ctrl Pts',(-65.7747383250775,34.9522931728594,12.));
#89764=CARTESIAN_POINT('Ctrl Pts',(-65.7859084407494,34.9529266758405,0.));
#89765=CARTESIAN_POINT('Ctrl Pts',(-65.7859084407494,34.9529266758405,12.));
#89766=CARTESIAN_POINT('Ctrl Pts',(-65.7914953018525,34.9532422808861,0.));
#89767=CARTESIAN_POINT('Ctrl Pts',(-65.7914953018525,34.9532422808861,12.));
#89768=CARTESIAN_POINT('',(-61.0441813777723,34.2579614092497,0.));
#89769=CARTESIAN_POINT('Ctrl Pts',(-61.0441813777723,34.2579614092497,0.));
#89770=CARTESIAN_POINT('Ctrl Pts',(-61.0479423318725,34.2589297755433,0.));
#89771=CARTESIAN_POINT('Ctrl Pts',(-61.0554700176998,34.2608658001631,0.));
#89772=CARTESIAN_POINT('Ctrl Pts',(-61.0667788793266,34.2637677131934,0.));
#89773=CARTESIAN_POINT('Ctrl Pts',(-61.0818920286293,34.2676326825626,0.));
#89774=CARTESIAN_POINT('Ctrl Pts',(-61.1008412399997,34.2724568037227,0.));
#89775=CARTESIAN_POINT('Ctrl Pts',(-61.1198481997764,34.277273803877,0.));
#89776=CARTESIAN_POINT('Ctrl Pts',(-61.1389128461886,34.2820836244469,0.));
#89777=CARTESIAN_POINT('Ctrl Pts',(-61.1580350635533,34.2868861666384,0.));
#89778=CARTESIAN_POINT('Ctrl Pts',(-61.1772146833205,34.2916812929751,0.));
#89779=CARTESIAN_POINT('Ctrl Pts',(-61.1964515073891,34.2964688443663,0.));
#89780=CARTESIAN_POINT('Ctrl Pts',(-61.2157453259107,34.3012486533474,0.));
#89781=CARTESIAN_POINT('Ctrl Pts',(-61.235095936694,34.3060205584064,0.));
#89782=CARTESIAN_POINT('Ctrl Pts',(-61.2545031656133,34.3107844191043,0.));
#89783=CARTESIAN_POINT('Ctrl Pts',(-61.2739668600365,34.3155401111747,0.));
#89784=CARTESIAN_POINT('Ctrl Pts',(-61.2934868791855,34.3202875193617,0.));
#89785=CARTESIAN_POINT('Ctrl Pts',(-61.3130630861386,34.3250265314768,0.));
#89786=CARTESIAN_POINT('Ctrl Pts',(-61.3326953378851,34.3297570310146,0.));
#89787=CARTESIAN_POINT('Ctrl Pts',(-61.3523834803188,34.3344788934363,0.));
#89788=CARTESIAN_POINT('Ctrl Pts',(-61.3721273534257,34.339191990014,0.));
#89789=CARTESIAN_POINT('Ctrl Pts',(-61.3919267945302,34.3438961902405,0.));
#89790=CARTESIAN_POINT('Ctrl Pts',(-61.4117816420229,34.3485913645979,0.));
#89791=CARTESIAN_POINT('Ctrl Pts',(-61.4316917395918,34.3532773877089,0.));
#89792=CARTESIAN_POINT('Ctrl Pts',(-61.4516569360454,34.3579541381996,0.));
#89793=CARTESIAN_POINT('Ctrl Pts',(-61.4716770832897,34.3626214971888,0.));
#89794=CARTESIAN_POINT('Ctrl Pts',(-61.4917520349279,34.3672793472465,0.));
#89795=CARTESIAN_POINT('Ctrl Pts',(-61.5118816445437,34.3719275711195,0.));
#89796=CARTESIAN_POINT('Ctrl Pts',(-61.5320657642639,34.376566050668,0.));
#89797=CARTESIAN_POINT('Ctrl Pts',(-61.5523042455158,34.3811946674196,0.));
#89798=CARTESIAN_POINT('Ctrl Pts',(-61.5725969396829,34.3858133030518,0.));
#89799=CARTESIAN_POINT('Ctrl Pts',(-61.5929436987409,34.3904218398636,0.));
#89800=CARTESIAN_POINT('Ctrl Pts',(-61.6133443760142,34.3950201613432,0.));
#89801=CARTESIAN_POINT('Ctrl Pts',(-61.6337988264556,34.3996081523753,0.));
#89802=CARTESIAN_POINT('Ctrl Pts',(-61.6543069062416,34.4041856989316,0.));
#89803=CARTESIAN_POINT('Ctrl Pts',(-61.6748684725205,34.4087526878812,0.));
#89804=CARTESIAN_POINT('Ctrl Pts',(-61.695483383117,34.4133090067703,0.));
#89805=CARTESIAN_POINT('Ctrl Pts',(-61.7161514961915,34.4178545435766,0.));
#89806=CARTESIAN_POINT('Ctrl Pts',(-61.7368726702596,34.4223891867179,0.));
#89807=CARTESIAN_POINT('Ctrl Pts',(-61.7576467643432,34.4269128251576,0.));
#89808=CARTESIAN_POINT('Ctrl Pts',(-61.7784736380727,34.4314253484791,0.));
#89809=CARTESIAN_POINT('Ctrl Pts',(-61.7993531518037,34.4359266469749,0.));
#89810=CARTESIAN_POINT('Ctrl Pts',(-61.8202851667222,34.4404166117299,0.));
#89811=CARTESIAN_POINT('Ctrl Pts',(-61.8412695447926,34.4448951345739,0.));
#89812=CARTESIAN_POINT('Ctrl Pts',(-61.8623061487018,34.449362108036,0.));
#89813=CARTESIAN_POINT('Ctrl Pts',(-61.8833948418025,34.4538174253012,0.));
#89814=CARTESIAN_POINT('Ctrl Pts',(-61.9045354880445,34.4582609801637,0.));
#89815=CARTESIAN_POINT('Ctrl Pts',(-61.9257279519308,34.4626926669974,0.));
#89816=CARTESIAN_POINT('Ctrl Pts',(-61.9469720985531,34.4671123807717,0.));
#89817=CARTESIAN_POINT('Ctrl Pts',(-61.9682677936054,34.4715200170592,0.));
#89818=CARTESIAN_POINT('Ctrl Pts',(-61.9896149034001,34.4759154720473,0.));
#89819=CARTESIAN_POINT('Ctrl Pts',(-62.0110132948794,34.4802986425528,0.));
#89820=CARTESIAN_POINT('Ctrl Pts',(-62.0324628356141,34.4846694260199,0.));
#89821=CARTESIAN_POINT('Ctrl Pts',(-62.0539633937939,34.4890277205039,0.));
#89822=CARTESIAN_POINT('Ctrl Pts',(-62.0755148382135,34.4933734246592,0.));
#89823=CARTESIAN_POINT('Ctrl Pts',(-62.0971170382567,34.4977064377282,0.));
#89824=CARTESIAN_POINT('Ctrl Pts',(-62.1187698638707,34.5020266595293,0.));
#89825=CARTESIAN_POINT('Ctrl Pts',(-62.1404731855687,34.5063339904533,0.));
#89826=CARTESIAN_POINT('Ctrl Pts',(-62.1622268744337,34.5106283314594,0.));
#89827=CARTESIAN_POINT('Ctrl Pts',(-62.1840308021171,34.5149095840729,0.));
#89828=CARTESIAN_POINT('Ctrl Pts',(-62.2058848408346,34.5191776503843,0.));
#89829=CARTESIAN_POINT('Ctrl Pts',(-62.2277888633577,34.5234324330492,0.));
#89830=CARTESIAN_POINT('Ctrl Pts',(-62.2497427430136,34.527673835281,0.));
#89831=CARTESIAN_POINT('Ctrl Pts',(-62.2717463536828,34.5319017608434,0.));
#89832=CARTESIAN_POINT('Ctrl Pts',(-62.2937995697927,34.536116114045,0.));
#89833=CARTESIAN_POINT('Ctrl Pts',(-62.3159022663052,34.5403167997333,0.));
#89834=CARTESIAN_POINT('Ctrl Pts',(-62.3380543187067,34.5445037232928,0.));
#89835=CARTESIAN_POINT('Ctrl Pts',(-62.3602556030114,34.5486767906376,0.));
#89836=CARTESIAN_POINT('Ctrl Pts',(-62.3825059957593,34.552835908207,0.));
#89837=CARTESIAN_POINT('Ctrl Pts',(-62.4048053740129,34.5569809829615,0.));
#89838=CARTESIAN_POINT('Ctrl Pts',(-62.4271536153473,34.5611119223807,0.));
#89839=CARTESIAN_POINT('Ctrl Pts',(-62.4495505978415,34.5652286344606,0.));
#89840=CARTESIAN_POINT('Ctrl Pts',(-62.471996200083,34.5693310277064,0.));
#89841=CARTESIAN_POINT('Ctrl Pts',(-62.494490301164,34.5734190111279,0.));
#89842=CARTESIAN_POINT('Ctrl Pts',(-62.5170327806774,34.5774924942351,0.));
#89843=CARTESIAN_POINT('Ctrl Pts',(-62.5396235187053,34.5815513870363,0.));
#89844=CARTESIAN_POINT('Ctrl Pts',(-62.5622623958125,34.5855956000343,0.));
#89845=CARTESIAN_POINT('Ctrl Pts',(-62.5849492930501,34.5896250442199,0.));
#89846=CARTESIAN_POINT('Ctrl Pts',(-62.6076840919521,34.5936396310671,0.));
#89847=CARTESIAN_POINT('Ctrl Pts',(-62.6304666745319,34.5976392725303,0.));
#89848=CARTESIAN_POINT('Ctrl Pts',(-62.6532969232695,34.6016238810419,0.));
#89849=CARTESIAN_POINT('Ctrl Pts',(-62.6761747211081,34.6055933695093,0.));
#89850=CARTESIAN_POINT('Ctrl Pts',(-62.6990999514597,34.6095476513094,0.));
#89851=CARTESIAN_POINT('Ctrl Pts',(-62.7220724982005,34.6134866402842,0.));
#89852=CARTESIAN_POINT('Ctrl Pts',(-62.7450922456663,34.6174102507368,0.));
#89853=CARTESIAN_POINT('Ctrl Pts',(-62.7681590786398,34.6213183974302,0.));
#89854=CARTESIAN_POINT('Ctrl Pts',(-62.7912728823483,34.6252109955836,0.));
#89855=CARTESIAN_POINT('Ctrl Pts',(-62.8144335424671,34.629087960866,0.));
#89856=CARTESIAN_POINT('Ctrl Pts',(-62.8376409451167,34.6329492093931,0.));
#89857=CARTESIAN_POINT('Ctrl Pts',(-62.8608949768583,34.6367946577241,0.));
#89858=CARTESIAN_POINT('Ctrl Pts',(-62.884195524682,34.6406242228606,0.));
#89859=CARTESIAN_POINT('Ctrl Pts',(-62.9075424760042,34.6444378222425,0.));
#89860=CARTESIAN_POINT('Ctrl Pts',(-62.9309357186733,34.6482353737433,0.));
#89861=CARTESIAN_POINT('Ctrl Pts',(-62.9543751409648,34.6520167956656,0.));
#89862=CARTESIAN_POINT('Ctrl Pts',(-62.9778606315777,34.6557820067389,0.));
#89863=CARTESIAN_POINT('Ctrl Pts',(-63.0013920796225,34.6595309261185,0.));
#89864=CARTESIAN_POINT('Ctrl Pts',(-63.0249693746199,34.6632634733819,0.));
#89865=CARTESIAN_POINT('Ctrl Pts',(-63.0485924065039,34.6669795685225,0.));
#89866=CARTESIAN_POINT('Ctrl Pts',(-63.0722610656194,34.670679131947,0.));
#89867=CARTESIAN_POINT('Ctrl Pts',(-63.095975242717,34.6743620844721,0.));
#89868=CARTESIAN_POINT('Ctrl Pts',(-63.1197348289431,34.6780283473252,0.));
#89869=CARTESIAN_POINT('Ctrl Pts',(-63.1435397158386,34.68167784214,0.));
#89870=CARTESIAN_POINT('Ctrl Pts',(-63.1673897953425,34.6853104909516,0.));
#89871=CARTESIAN_POINT('Ctrl Pts',(-63.1912849597885,34.6889262161923,0.));
#89872=CARTESIAN_POINT('Ctrl Pts',(-63.2152251019014,34.6925249406898,0.));
#89873=CARTESIAN_POINT('Ctrl Pts',(-63.2392101147854,34.696106587667,0.));
#89874=CARTESIAN_POINT('Ctrl Pts',(-63.2632398919234,34.6996710807384,0.));
#89875=CARTESIAN_POINT('Ctrl Pts',(-63.2873143271813,34.7032183439045,0.));
#89876=CARTESIAN_POINT('Ctrl Pts',(-63.311433314805,34.7067483015492,0.));
#89877=CARTESIAN_POINT('Ctrl Pts',(-63.3355967494169,34.7102608784372,0.));
#89878=CARTESIAN_POINT('Ctrl Pts',(-63.359804526005,34.7137559997143,0.));
#89879=CARTESIAN_POINT('Ctrl Pts',(-63.3840565399207,34.7172335909037,0.));
#89880=CARTESIAN_POINT('Ctrl Pts',(-63.4083526868837,34.7206935779007,0.));
#89881=CARTESIAN_POINT('Ctrl Pts',(-63.4326928629797,34.7241358869701,0.));
#89882=CARTESIAN_POINT('Ctrl Pts',(-63.4570769646568,34.7275604447438,0.));
#89883=CARTESIAN_POINT('Ctrl Pts',(-63.4815048887161,34.7309671782211,0.));
#89884=CARTESIAN_POINT('Ctrl Pts',(-63.5059765323082,34.7343560147663,0.));
#89885=CARTESIAN_POINT('Ctrl Pts',(-63.5304917929378,34.7377268821022,0.));
#89886=CARTESIAN_POINT('Ctrl Pts',(-63.5550505684621,34.7410797083079,0.));
#89887=CARTESIAN_POINT('Ctrl Pts',(-63.5796527570874,34.7444144218162,0.));
#89888=CARTESIAN_POINT('Ctrl Pts',(-63.6042982573599,34.7477309514142,0.));
#89889=CARTESIAN_POINT('Ctrl Pts',(-63.628986968162,34.7510292262415,0.));
#89890=CARTESIAN_POINT('Ctrl Pts',(-63.6537187887174,34.7543091757841,0.));
#89891=CARTESIAN_POINT('Ctrl Pts',(-63.6784936185893,34.7575707298718,0.));
#89892=CARTESIAN_POINT('Ctrl Pts',(-63.7033113576782,34.7608138186757,0.));
#89893=CARTESIAN_POINT('Ctrl Pts',(-63.7281719062136,34.7640383727093,0.));
#89894=CARTESIAN_POINT('Ctrl Pts',(-63.7530751647479,34.7672443228266,0.));
#89895=CARTESIAN_POINT('Ctrl Pts',(-63.7780210341619,34.7704316002165,0.));
#89896=CARTESIAN_POINT('Ctrl Pts',(-63.8030094156635,34.7736001363991,0.));
#89897=CARTESIAN_POINT('Ctrl Pts',(-63.8280402107858,34.7767498632244,0.));
#89898=CARTESIAN_POINT('Ctrl Pts',(-63.8531133213794,34.7798807128715,0.));
#89899=CARTESIAN_POINT('Ctrl Pts',(-63.8782286496059,34.7829926178495,0.));
#89900=CARTESIAN_POINT('Ctrl Pts',(-63.9033860979429,34.7860855109907,0.));
#89901=CARTESIAN_POINT('Ctrl Pts',(-63.9285855691839,34.7891593254485,0.));
#89902=CARTESIAN_POINT('Ctrl Pts',(-63.9538269664366,34.7922139946943,0.));
#89903=CARTESIAN_POINT('Ctrl Pts',(-63.9791101931169,34.7952494525182,0.));
#89904=CARTESIAN_POINT('Ctrl Pts',(-64.0044351529413,34.79826563303,0.));
#89905=CARTESIAN_POINT('Ctrl Pts',(-64.0298017499305,34.8012624706533,0.));
#89906=CARTESIAN_POINT('Ctrl Pts',(-64.0552098884101,34.8042399001214,0.));
#89907=CARTESIAN_POINT('Ctrl Pts',(-64.0806594730085,34.8071978564748,0.));
#89908=CARTESIAN_POINT('Ctrl Pts',(-64.1061504086512,34.8101362750595,0.));
#89909=CARTESIAN_POINT('Ctrl Pts',(-64.1316826005502,34.8130550915283,0.));
#89910=CARTESIAN_POINT('Ctrl Pts',(-64.1572559542085,34.8159542418372,0.));
#89911=CARTESIAN_POINT('Ctrl Pts',(-64.1828703754237,34.8188336622418,0.));
#89912=CARTESIAN_POINT('Ctrl Pts',(-64.2085257702885,34.8216932892969,0.));
#89913=CARTESIAN_POINT('Ctrl Pts',(-64.2342220451878,34.8245330598559,0.));
#89914=CARTESIAN_POINT('Ctrl Pts',(-64.259959106791,34.8273529110742,0.));
#89915=CARTESIAN_POINT('Ctrl Pts',(-64.2857368620513,34.8301527804052,0.));
#89916=CARTESIAN_POINT('Ctrl Pts',(-64.3115552182056,34.8329326055916,0.));
#89917=CARTESIAN_POINT('Ctrl Pts',(-64.3374140827708,34.8356923246617,0.));
#89918=CARTESIAN_POINT('Ctrl Pts',(-64.3633133635385,34.8384318759249,0.));
#89919=CARTESIAN_POINT('Ctrl Pts',(-64.3892529685614,34.8411511979705,0.));
#89920=CARTESIAN_POINT('Ctrl Pts',(-64.4152328061526,34.8438502296669,0.));
#89921=CARTESIAN_POINT('Ctrl Pts',(-64.441252784898,34.8465289101626,0.));
#89922=CARTESIAN_POINT('Ctrl Pts',(-64.4673128136631,34.8491871788898,0.));
#89923=CARTESIAN_POINT('Ctrl Pts',(-64.4934128015983,34.8518249755679,0.));
#89924=CARTESIAN_POINT('Ctrl Pts',(-64.5195526581398,34.8544422402114,0.));
#89925=CARTESIAN_POINT('Ctrl Pts',(-64.5457322930074,34.8570389131334,0.));
#89926=CARTESIAN_POINT('Ctrl Pts',(-64.5719516161914,34.859614934925,0.));
#89927=CARTESIAN_POINT('Ctrl Pts',(-64.5982105379374,34.8621702464397,0.));
#89928=CARTESIAN_POINT('Ctrl Pts',(-64.6245089687276,34.8647047887774,0.));
#89929=CARTESIAN_POINT('Ctrl Pts',(-64.6508468192609,34.8672185032724,0.));
#89930=CARTESIAN_POINT('Ctrl Pts',(-64.6772240004241,34.8697113314797,0.));
#89931=CARTESIAN_POINT('Ctrl Pts',(-64.7036404233319,34.8721832151981,0.));
#89932=CARTESIAN_POINT('Ctrl Pts',(-64.7300959993662,34.8746340964976,0.));
#89933=CARTESIAN_POINT('Ctrl Pts',(-64.7565906402154,34.8770639177494,0.));
#89934=CARTESIAN_POINT('Ctrl Pts',(-64.7831242579023,34.8794726216511,0.));
#89935=CARTESIAN_POINT('Ctrl Pts',(-64.80969676483,34.8818601512726,0.));
#89936=CARTESIAN_POINT('Ctrl Pts',(-64.8363080737369,34.8842264500184,0.));
#89937=CARTESIAN_POINT('Ctrl Pts',(-64.8629580976057,34.8865714615433,0.));
#89938=CARTESIAN_POINT('Ctrl Pts',(-64.8896467495755,34.8888951296809,0.));
#89939=CARTESIAN_POINT('Ctrl Pts',(-64.9163739428606,34.8911973983785,0.));
#89940=CARTESIAN_POINT('Ctrl Pts',(-64.9431395906341,34.8934782116097,0.));
#89941=CARTESIAN_POINT('Ctrl Pts',(-64.9699436060178,34.8957375133702,0.));
#89942=CARTESIAN_POINT('Ctrl Pts',(-64.9967859023225,34.8979752478623,0.));
#89943=CARTESIAN_POINT('Ctrl Pts',(-65.0236663932338,34.9001913596421,0.));
#89944=CARTESIAN_POINT('Ctrl Pts',(-65.0505849930173,34.9023857937866,0.));
#89945=CARTESIAN_POINT('Ctrl Pts',(-65.0775416167073,34.9045584960503,0.));
#89946=CARTESIAN_POINT('Ctrl Pts',(-65.1045361803097,34.9067094130386,0.));
#89947=CARTESIAN_POINT('Ctrl Pts',(-65.1315686003485,34.9088384918321,0.));
#89948=CARTESIAN_POINT('Ctrl Pts',(-65.1586387934216,34.9109456796201,0.));
#89949=CARTESIAN_POINT('Ctrl Pts',(-65.1857466757082,34.9130309233017,0.));
#89950=CARTESIAN_POINT('Ctrl Pts',(-65.2128921625838,34.9150941691754,0.));
#89951=CARTESIAN_POINT('Ctrl Pts',(-65.2400751679586,34.9171353624131,0.));
#89952=CARTESIAN_POINT('Ctrl Pts',(-65.2672956048121,34.9191544474898,0.));
#89953=CARTESIAN_POINT('Ctrl Pts',(-65.2945533863812,34.921151369138,0.));
#89954=CARTESIAN_POINT('Ctrl Pts',(-65.3218484271941,34.9231260731846,0.));
#89955=CARTESIAN_POINT('Ctrl Pts',(-65.3491806440529,34.9250785073473,0.));
#89956=CARTESIAN_POINT('Ctrl Pts',(-65.3765499573019,34.9270086222703,0.));
#89957=CARTESIAN_POINT('Ctrl Pts',(-65.4039562911255,34.92891637177,0.));
#89958=CARTESIAN_POINT('Ctrl Pts',(-65.4274804996406,34.9305324724386,0.));
#89959=CARTESIAN_POINT('Ctrl Pts',(-65.4455359575001,34.9317593813102,0.));
#89960=CARTESIAN_POINT('Ctrl Pts',(-65.4581063193586,34.9326070346592,0.));
#89961=CARTESIAN_POINT('Ctrl Pts',(-65.4651808010454,34.9330820191483,0.));
#89962=CARTESIAN_POINT('Ctrl Pts',(-65.4667541477958,34.9331875523085,0.));
#89963=CARTESIAN_POINT('',(-61.0441813777723,34.2579614092497,12.));
#89964=CARTESIAN_POINT('',(-61.0441813777723,34.2579614092497,0.));
#89965=CARTESIAN_POINT('Ctrl Pts',(-65.4667541477958,34.9331875523085,12.));
#89966=CARTESIAN_POINT('Ctrl Pts',(-65.4651808010454,34.9330820191483,12.));
#89967=CARTESIAN_POINT('Ctrl Pts',(-65.4581063193585,34.9326070346592,12.));
#89968=CARTESIAN_POINT('Ctrl Pts',(-65.4455359575001,34.9317593813102,12.));
#89969=CARTESIAN_POINT('Ctrl Pts',(-65.4274804996406,34.9305324724386,12.));
#89970=CARTESIAN_POINT('Ctrl Pts',(-65.4039562911255,34.92891637177,12.));
#89971=CARTESIAN_POINT('Ctrl Pts',(-65.3765499573019,34.9270086222703,12.));
#89972=CARTESIAN_POINT('Ctrl Pts',(-65.3491806440529,34.9250785073473,12.));
#89973=CARTESIAN_POINT('Ctrl Pts',(-65.3218484271941,34.9231260731846,12.));
#89974=CARTESIAN_POINT('Ctrl Pts',(-65.2945533863812,34.921151369138,12.));
#89975=CARTESIAN_POINT('Ctrl Pts',(-65.2672956048121,34.9191544474898,12.));
#89976=CARTESIAN_POINT('Ctrl Pts',(-65.2400751679586,34.9171353624131,12.));
#89977=CARTESIAN_POINT('Ctrl Pts',(-65.2128921625838,34.9150941691754,12.));
#89978=CARTESIAN_POINT('Ctrl Pts',(-65.1857466757082,34.9130309233017,12.));
#89979=CARTESIAN_POINT('Ctrl Pts',(-65.1586387934216,34.9109456796201,12.));
#89980=CARTESIAN_POINT('Ctrl Pts',(-65.1315686003485,34.9088384918321,12.));
#89981=CARTESIAN_POINT('Ctrl Pts',(-65.1045361803097,34.9067094130386,12.));
#89982=CARTESIAN_POINT('Ctrl Pts',(-65.0775416167073,34.9045584960503,12.));
#89983=CARTESIAN_POINT('Ctrl Pts',(-65.0505849930173,34.9023857937866,12.));
#89984=CARTESIAN_POINT('Ctrl Pts',(-65.0236663932338,34.9001913596421,12.));
#89985=CARTESIAN_POINT('Ctrl Pts',(-64.9967859023225,34.8979752478623,12.));
#89986=CARTESIAN_POINT('Ctrl Pts',(-64.9699436060178,34.8957375133702,12.));
#89987=CARTESIAN_POINT('Ctrl Pts',(-64.9431395906341,34.8934782116097,12.));
#89988=CARTESIAN_POINT('Ctrl Pts',(-64.9163739428606,34.8911973983785,12.));
#89989=CARTESIAN_POINT('Ctrl Pts',(-64.8896467495755,34.8888951296809,12.));
#89990=CARTESIAN_POINT('Ctrl Pts',(-64.8629580976057,34.8865714615433,12.));
#89991=CARTESIAN_POINT('Ctrl Pts',(-64.8363080737369,34.8842264500184,12.));
#89992=CARTESIAN_POINT('Ctrl Pts',(-64.80969676483,34.8818601512726,12.));
#89993=CARTESIAN_POINT('Ctrl Pts',(-64.7831242579023,34.8794726216511,12.));
#89994=CARTESIAN_POINT('Ctrl Pts',(-64.7565906402154,34.8770639177494,12.));
#89995=CARTESIAN_POINT('Ctrl Pts',(-64.7300959993662,34.8746340964976,12.));
#89996=CARTESIAN_POINT('Ctrl Pts',(-64.7036404233319,34.8721832151981,12.));
#89997=CARTESIAN_POINT('Ctrl Pts',(-64.6772240004241,34.8697113314797,12.));
#89998=CARTESIAN_POINT('Ctrl Pts',(-64.6508468192609,34.8672185032724,12.));
#89999=CARTESIAN_POINT('Ctrl Pts',(-64.6245089687276,34.8647047887774,12.));
#90000=CARTESIAN_POINT('Ctrl Pts',(-64.5982105379374,34.8621702464397,12.));
#90001=CARTESIAN_POINT('Ctrl Pts',(-64.5719516161914,34.859614934925,12.));
#90002=CARTESIAN_POINT('Ctrl Pts',(-64.5457322930074,34.8570389131334,12.));
#90003=CARTESIAN_POINT('Ctrl Pts',(-64.5195526581398,34.8544422402114,12.));
#90004=CARTESIAN_POINT('Ctrl Pts',(-64.4934128015983,34.8518249755679,12.));
#90005=CARTESIAN_POINT('Ctrl Pts',(-64.4673128136631,34.8491871788898,12.));
#90006=CARTESIAN_POINT('Ctrl Pts',(-64.441252784898,34.8465289101626,12.));
#90007=CARTESIAN_POINT('Ctrl Pts',(-64.4152328061526,34.8438502296669,12.));
#90008=CARTESIAN_POINT('Ctrl Pts',(-64.3892529685614,34.8411511979705,12.));
#90009=CARTESIAN_POINT('Ctrl Pts',(-64.3633133635385,34.8384318759249,12.));
#90010=CARTESIAN_POINT('Ctrl Pts',(-64.3374140827708,34.8356923246617,12.));
#90011=CARTESIAN_POINT('Ctrl Pts',(-64.3115552182056,34.8329326055916,12.));
#90012=CARTESIAN_POINT('Ctrl Pts',(-64.2857368620513,34.8301527804052,12.));
#90013=CARTESIAN_POINT('Ctrl Pts',(-64.259959106791,34.8273529110742,12.));
#90014=CARTESIAN_POINT('Ctrl Pts',(-64.2342220451878,34.8245330598559,12.));
#90015=CARTESIAN_POINT('Ctrl Pts',(-64.2085257702885,34.8216932892969,12.));
#90016=CARTESIAN_POINT('Ctrl Pts',(-64.1828703754237,34.8188336622418,12.));
#90017=CARTESIAN_POINT('Ctrl Pts',(-64.1572559542085,34.8159542418372,12.));
#90018=CARTESIAN_POINT('Ctrl Pts',(-64.1316826005502,34.8130550915283,12.));
#90019=CARTESIAN_POINT('Ctrl Pts',(-64.1061504086512,34.8101362750595,12.));
#90020=CARTESIAN_POINT('Ctrl Pts',(-64.0806594730085,34.8071978564748,12.));
#90021=CARTESIAN_POINT('Ctrl Pts',(-64.0552098884101,34.8042399001214,12.));
#90022=CARTESIAN_POINT('Ctrl Pts',(-64.0298017499305,34.8012624706533,12.));
#90023=CARTESIAN_POINT('Ctrl Pts',(-64.0044351529413,34.79826563303,12.));
#90024=CARTESIAN_POINT('Ctrl Pts',(-63.9791101931169,34.7952494525182,12.));
#90025=CARTESIAN_POINT('Ctrl Pts',(-63.9538269664366,34.7922139946943,12.));
#90026=CARTESIAN_POINT('Ctrl Pts',(-63.9285855691839,34.7891593254485,12.));
#90027=CARTESIAN_POINT('Ctrl Pts',(-63.9033860979429,34.7860855109907,12.));
#90028=CARTESIAN_POINT('Ctrl Pts',(-63.8782286496059,34.7829926178495,12.));
#90029=CARTESIAN_POINT('Ctrl Pts',(-63.8531133213794,34.7798807128715,12.));
#90030=CARTESIAN_POINT('Ctrl Pts',(-63.8280402107858,34.7767498632244,12.));
#90031=CARTESIAN_POINT('Ctrl Pts',(-63.8030094156635,34.7736001363991,12.));
#90032=CARTESIAN_POINT('Ctrl Pts',(-63.7780210341619,34.7704316002165,12.));
#90033=CARTESIAN_POINT('Ctrl Pts',(-63.7530751647479,34.7672443228266,12.));
#90034=CARTESIAN_POINT('Ctrl Pts',(-63.7281719062136,34.7640383727093,12.));
#90035=CARTESIAN_POINT('Ctrl Pts',(-63.7033113576782,34.7608138186757,12.));
#90036=CARTESIAN_POINT('Ctrl Pts',(-63.6784936185893,34.7575707298718,12.));
#90037=CARTESIAN_POINT('Ctrl Pts',(-63.6537187887174,34.7543091757841,12.));
#90038=CARTESIAN_POINT('Ctrl Pts',(-63.628986968162,34.7510292262415,12.));
#90039=CARTESIAN_POINT('Ctrl Pts',(-63.6042982573599,34.7477309514142,12.));
#90040=CARTESIAN_POINT('Ctrl Pts',(-63.5796527570874,34.7444144218162,12.));
#90041=CARTESIAN_POINT('Ctrl Pts',(-63.5550505684621,34.7410797083079,12.));
#90042=CARTESIAN_POINT('Ctrl Pts',(-63.5304917929378,34.7377268821022,12.));
#90043=CARTESIAN_POINT('Ctrl Pts',(-63.5059765323082,34.7343560147663,12.));
#90044=CARTESIAN_POINT('Ctrl Pts',(-63.4815048887161,34.7309671782211,12.));
#90045=CARTESIAN_POINT('Ctrl Pts',(-63.4570769646568,34.7275604447438,12.));
#90046=CARTESIAN_POINT('Ctrl Pts',(-63.4326928629797,34.7241358869701,12.));
#90047=CARTESIAN_POINT('Ctrl Pts',(-63.4083526868837,34.7206935779007,12.));
#90048=CARTESIAN_POINT('Ctrl Pts',(-63.3840565399207,34.7172335909037,12.));
#90049=CARTESIAN_POINT('Ctrl Pts',(-63.359804526005,34.7137559997143,12.));
#90050=CARTESIAN_POINT('Ctrl Pts',(-63.3355967494169,34.7102608784372,12.));
#90051=CARTESIAN_POINT('Ctrl Pts',(-63.311433314805,34.7067483015492,12.));
#90052=CARTESIAN_POINT('Ctrl Pts',(-63.2873143271813,34.7032183439045,12.));
#90053=CARTESIAN_POINT('Ctrl Pts',(-63.2632398919234,34.6996710807384,12.));
#90054=CARTESIAN_POINT('Ctrl Pts',(-63.2392101147854,34.696106587667,12.));
#90055=CARTESIAN_POINT('Ctrl Pts',(-63.2152251019014,34.6925249406898,12.));
#90056=CARTESIAN_POINT('Ctrl Pts',(-63.1912849597885,34.6889262161923,12.));
#90057=CARTESIAN_POINT('Ctrl Pts',(-63.1673897953425,34.6853104909516,12.));
#90058=CARTESIAN_POINT('Ctrl Pts',(-63.1435397158386,34.68167784214,12.));
#90059=CARTESIAN_POINT('Ctrl Pts',(-63.1197348289431,34.6780283473252,12.));
#90060=CARTESIAN_POINT('Ctrl Pts',(-63.095975242717,34.6743620844721,12.));
#90061=CARTESIAN_POINT('Ctrl Pts',(-63.0722610656194,34.670679131947,12.));
#90062=CARTESIAN_POINT('Ctrl Pts',(-63.0485924065039,34.6669795685225,12.));
#90063=CARTESIAN_POINT('Ctrl Pts',(-63.0249693746199,34.6632634733819,12.));
#90064=CARTESIAN_POINT('Ctrl Pts',(-63.0013920796225,34.6595309261185,12.));
#90065=CARTESIAN_POINT('Ctrl Pts',(-62.9778606315777,34.6557820067389,12.));
#90066=CARTESIAN_POINT('Ctrl Pts',(-62.9543751409648,34.6520167956656,12.));
#90067=CARTESIAN_POINT('Ctrl Pts',(-62.9309357186733,34.6482353737433,12.));
#90068=CARTESIAN_POINT('Ctrl Pts',(-62.9075424760042,34.6444378222425,12.));
#90069=CARTESIAN_POINT('Ctrl Pts',(-62.884195524682,34.6406242228606,12.));
#90070=CARTESIAN_POINT('Ctrl Pts',(-62.8608949768583,34.6367946577241,12.));
#90071=CARTESIAN_POINT('Ctrl Pts',(-62.8376409451167,34.6329492093931,12.));
#90072=CARTESIAN_POINT('Ctrl Pts',(-62.8144335424671,34.629087960866,12.));
#90073=CARTESIAN_POINT('Ctrl Pts',(-62.7912728823483,34.6252109955836,12.));
#90074=CARTESIAN_POINT('Ctrl Pts',(-62.7681590786398,34.6213183974302,12.));
#90075=CARTESIAN_POINT('Ctrl Pts',(-62.7450922456663,34.6174102507368,12.));
#90076=CARTESIAN_POINT('Ctrl Pts',(-62.7220724982005,34.6134866402842,12.));
#90077=CARTESIAN_POINT('Ctrl Pts',(-62.6990999514597,34.6095476513094,12.));
#90078=CARTESIAN_POINT('Ctrl Pts',(-62.6761747211081,34.6055933695093,12.));
#90079=CARTESIAN_POINT('Ctrl Pts',(-62.6532969232695,34.6016238810419,12.));
#90080=CARTESIAN_POINT('Ctrl Pts',(-62.6304666745319,34.5976392725303,12.));
#90081=CARTESIAN_POINT('Ctrl Pts',(-62.6076840919521,34.5936396310671,12.));
#90082=CARTESIAN_POINT('Ctrl Pts',(-62.5849492930501,34.5896250442199,12.));
#90083=CARTESIAN_POINT('Ctrl Pts',(-62.5622623958125,34.5855956000343,12.));
#90084=CARTESIAN_POINT('Ctrl Pts',(-62.5396235187053,34.5815513870363,12.));
#90085=CARTESIAN_POINT('Ctrl Pts',(-62.5170327806774,34.5774924942351,12.));
#90086=CARTESIAN_POINT('Ctrl Pts',(-62.494490301164,34.5734190111279,12.));
#90087=CARTESIAN_POINT('Ctrl Pts',(-62.471996200083,34.5693310277064,12.));
#90088=CARTESIAN_POINT('Ctrl Pts',(-62.4495505978415,34.5652286344606,12.));
#90089=CARTESIAN_POINT('Ctrl Pts',(-62.4271536153473,34.5611119223807,12.));
#90090=CARTESIAN_POINT('Ctrl Pts',(-62.4048053740129,34.5569809829615,12.));
#90091=CARTESIAN_POINT('Ctrl Pts',(-62.3825059957593,34.552835908207,12.));
#90092=CARTESIAN_POINT('Ctrl Pts',(-62.3602556030114,34.5486767906376,12.));
#90093=CARTESIAN_POINT('Ctrl Pts',(-62.3380543187067,34.5445037232928,12.));
#90094=CARTESIAN_POINT('Ctrl Pts',(-62.3159022663052,34.5403167997333,12.));
#90095=CARTESIAN_POINT('Ctrl Pts',(-62.2937995697927,34.536116114045,12.));
#90096=CARTESIAN_POINT('Ctrl Pts',(-62.2717463536828,34.5319017608434,12.));
#90097=CARTESIAN_POINT('Ctrl Pts',(-62.2497427430136,34.527673835281,12.));
#90098=CARTESIAN_POINT('Ctrl Pts',(-62.2277888633577,34.5234324330492,12.));
#90099=CARTESIAN_POINT('Ctrl Pts',(-62.2058848408346,34.5191776503843,12.));
#90100=CARTESIAN_POINT('Ctrl Pts',(-62.1840308021171,34.5149095840729,12.));
#90101=CARTESIAN_POINT('Ctrl Pts',(-62.1622268744337,34.5106283314594,12.));
#90102=CARTESIAN_POINT('Ctrl Pts',(-62.1404731855687,34.5063339904533,12.));
#90103=CARTESIAN_POINT('Ctrl Pts',(-62.1187698638707,34.5020266595293,12.));
#90104=CARTESIAN_POINT('Ctrl Pts',(-62.0971170382567,34.4977064377282,12.));
#90105=CARTESIAN_POINT('Ctrl Pts',(-62.0755148382135,34.4933734246592,12.));
#90106=CARTESIAN_POINT('Ctrl Pts',(-62.0539633937939,34.4890277205039,12.));
#90107=CARTESIAN_POINT('Ctrl Pts',(-62.0324628356141,34.4846694260199,12.));
#90108=CARTESIAN_POINT('Ctrl Pts',(-62.0110132948794,34.4802986425528,12.));
#90109=CARTESIAN_POINT('Ctrl Pts',(-61.9896149034001,34.4759154720473,12.));
#90110=CARTESIAN_POINT('Ctrl Pts',(-61.9682677936054,34.4715200170592,12.));
#90111=CARTESIAN_POINT('Ctrl Pts',(-61.9469720985531,34.4671123807717,12.));
#90112=CARTESIAN_POINT('Ctrl Pts',(-61.9257279519308,34.4626926669974,12.));
#90113=CARTESIAN_POINT('Ctrl Pts',(-61.9045354880445,34.4582609801637,12.));
#90114=CARTESIAN_POINT('Ctrl Pts',(-61.8833948418025,34.4538174253012,12.));
#90115=CARTESIAN_POINT('Ctrl Pts',(-61.8623061487018,34.449362108036,12.));
#90116=CARTESIAN_POINT('Ctrl Pts',(-61.8412695447926,34.4448951345739,12.));
#90117=CARTESIAN_POINT('Ctrl Pts',(-61.8202851667222,34.4404166117299,12.));
#90118=CARTESIAN_POINT('Ctrl Pts',(-61.7993531518037,34.4359266469749,12.));
#90119=CARTESIAN_POINT('Ctrl Pts',(-61.7784736380727,34.4314253484791,12.));
#90120=CARTESIAN_POINT('Ctrl Pts',(-61.7576467643432,34.4269128251576,12.));
#90121=CARTESIAN_POINT('Ctrl Pts',(-61.7368726702596,34.4223891867179,12.));
#90122=CARTESIAN_POINT('Ctrl Pts',(-61.7161514961915,34.4178545435766,12.));
#90123=CARTESIAN_POINT('Ctrl Pts',(-61.695483383117,34.4133090067703,12.));
#90124=CARTESIAN_POINT('Ctrl Pts',(-61.6748684725205,34.4087526878812,12.));
#90125=CARTESIAN_POINT('Ctrl Pts',(-61.6543069062416,34.4041856989316,12.));
#90126=CARTESIAN_POINT('Ctrl Pts',(-61.6337988264556,34.3996081523753,12.));
#90127=CARTESIAN_POINT('Ctrl Pts',(-61.6133443760142,34.3950201613432,12.));
#90128=CARTESIAN_POINT('Ctrl Pts',(-61.5929436987409,34.3904218398636,12.));
#90129=CARTESIAN_POINT('Ctrl Pts',(-61.5725969396829,34.3858133030518,12.));
#90130=CARTESIAN_POINT('Ctrl Pts',(-61.5523042455158,34.3811946674196,12.));
#90131=CARTESIAN_POINT('Ctrl Pts',(-61.5320657642639,34.376566050668,12.));
#90132=CARTESIAN_POINT('Ctrl Pts',(-61.5118816445437,34.3719275711195,12.));
#90133=CARTESIAN_POINT('Ctrl Pts',(-61.4917520349279,34.3672793472465,12.));
#90134=CARTESIAN_POINT('Ctrl Pts',(-61.4716770832897,34.3626214971888,12.));
#90135=CARTESIAN_POINT('Ctrl Pts',(-61.4516569360454,34.3579541381996,12.));
#90136=CARTESIAN_POINT('Ctrl Pts',(-61.4316917395918,34.3532773877089,12.));
#90137=CARTESIAN_POINT('Ctrl Pts',(-61.4117816420229,34.3485913645979,12.));
#90138=CARTESIAN_POINT('Ctrl Pts',(-61.3919267945302,34.3438961902405,12.));
#90139=CARTESIAN_POINT('Ctrl Pts',(-61.3721273534257,34.339191990014,12.));
#90140=CARTESIAN_POINT('Ctrl Pts',(-61.3523834803188,34.3344788934363,12.));
#90141=CARTESIAN_POINT('Ctrl Pts',(-61.3326953378851,34.3297570310146,12.));
#90142=CARTESIAN_POINT('Ctrl Pts',(-61.3130630861386,34.3250265314768,12.));
#90143=CARTESIAN_POINT('Ctrl Pts',(-61.2934868791855,34.3202875193617,12.));
#90144=CARTESIAN_POINT('Ctrl Pts',(-61.2739668600365,34.3155401111747,12.));
#90145=CARTESIAN_POINT('Ctrl Pts',(-61.2545031656133,34.3107844191043,12.));
#90146=CARTESIAN_POINT('Ctrl Pts',(-61.235095936694,34.3060205584064,12.));
#90147=CARTESIAN_POINT('Ctrl Pts',(-61.2157453259107,34.3012486533474,12.));
#90148=CARTESIAN_POINT('Ctrl Pts',(-61.1964515073891,34.2964688443663,12.));
#90149=CARTESIAN_POINT('Ctrl Pts',(-61.1772146833205,34.2916812929751,12.));
#90150=CARTESIAN_POINT('Ctrl Pts',(-61.1580350635533,34.2868861666384,12.));
#90151=CARTESIAN_POINT('Ctrl Pts',(-61.1389128461886,34.2820836244469,12.));
#90152=CARTESIAN_POINT('Ctrl Pts',(-61.1198481997764,34.277273803877,12.));
#90153=CARTESIAN_POINT('Ctrl Pts',(-61.1008412399997,34.2724568037227,12.));
#90154=CARTESIAN_POINT('Ctrl Pts',(-61.0818920286293,34.2676326825626,12.));
#90155=CARTESIAN_POINT('Ctrl Pts',(-61.0667788793266,34.2637677131934,12.));
#90156=CARTESIAN_POINT('Ctrl Pts',(-61.0554700176998,34.2608658001631,12.));
#90157=CARTESIAN_POINT('Ctrl Pts',(-61.0479423318725,34.2589297755433,12.));
#90158=CARTESIAN_POINT('Ctrl Pts',(-61.0441813777723,34.2579614092497,12.));
#90159=CARTESIAN_POINT('Ctrl Pts',(-66.1657795405966,33.5903722665284,0.));
#90160=CARTESIAN_POINT('Ctrl Pts',(-66.1657795405966,33.5903722665284,4.));
#90161=CARTESIAN_POINT('Ctrl Pts',(-66.1657795405966,33.5903722665284,8.));
#90162=CARTESIAN_POINT('Ctrl Pts',(-66.1657795405966,33.5903722665284,12.));
#90163=CARTESIAN_POINT('Ctrl Pts',(-66.2346881970584,33.6759628819924,0.));
#90164=CARTESIAN_POINT('Ctrl Pts',(-66.2346881970584,33.6759628819924,4.));
#90165=CARTESIAN_POINT('Ctrl Pts',(-66.2346881970584,33.6759628819924,8.00000000000001));
#90166=CARTESIAN_POINT('Ctrl Pts',(-66.2346881970584,33.6759628819924,12.));
#90167=CARTESIAN_POINT('Ctrl Pts',(-66.3036153738446,33.8665453669337,0.));
#90168=CARTESIAN_POINT('Ctrl Pts',(-66.3036153738446,33.8665453669337,4.));
#90169=CARTESIAN_POINT('Ctrl Pts',(-66.3036153738446,33.8665453669337,7.99999999999999));
#90170=CARTESIAN_POINT('Ctrl Pts',(-66.3036153738446,33.8665453669337,12.));
#90171=CARTESIAN_POINT('Ctrl Pts',(-66.2585076236404,34.0597557125862,0.));
#90172=CARTESIAN_POINT('Ctrl Pts',(-66.2585076236404,34.0597557125862,4.));
#90173=CARTESIAN_POINT('Ctrl Pts',(-66.2585076236404,34.0597557125862,8.00000000000001));
#90174=CARTESIAN_POINT('Ctrl Pts',(-66.2585076236404,34.0597557125862,12.));
#90175=CARTESIAN_POINT('Ctrl Pts',(-66.2207497120656,34.1330090612016,0.));
#90176=CARTESIAN_POINT('Ctrl Pts',(-66.2207497120656,34.1330090612016,4.));
#90177=CARTESIAN_POINT('Ctrl Pts',(-66.2207497120656,34.1330090612016,8.));
#90178=CARTESIAN_POINT('Ctrl Pts',(-66.2207497120656,34.1330090612016,12.));
#90179=CARTESIAN_POINT('',(-66.1657795405966,33.5903722665284,0.));
#90180=CARTESIAN_POINT('',(-66.220749712065,34.1330090612013,0.));
#90181=CARTESIAN_POINT('Ctrl Pts',(-66.1657795405966,33.5903722665284,7.5239139515392E-35));
#90182=CARTESIAN_POINT('Ctrl Pts',(-66.2346881970584,33.6759628819924,7.52391395153919E-35));
#90183=CARTESIAN_POINT('Ctrl Pts',(-66.274075155222,33.7848671591017,7.5239139515392E-35));
#90184=CARTESIAN_POINT('Ctrl Pts',(-66.276226218858,33.8946295131779,7.5239139515392E-35));
#90185=CARTESIAN_POINT('Ctrl Pts',(-66.2778395165851,33.9769512787351,7.5239139515392E-35));
#90186=CARTESIAN_POINT('Ctrl Pts',(-66.2585076236404,34.0597557125862,7.52391395153919E-35));
#90187=CARTESIAN_POINT('Ctrl Pts',(-66.2207497120656,34.1330090612016,7.52391395153919E-35));
#90188=CARTESIAN_POINT('',(-66.220749712065,34.1330090612013,12.));
#90189=CARTESIAN_POINT('Ctrl Pts',(-66.2207497120656,34.1330090612016,0.));
#90190=CARTESIAN_POINT('Ctrl Pts',(-66.2207497120656,34.1330090612016,4.));
#90191=CARTESIAN_POINT('Ctrl Pts',(-66.2207497120656,34.1330090612016,8.));
#90192=CARTESIAN_POINT('Ctrl Pts',(-66.2207497120656,34.1330090612016,12.));
#90193=CARTESIAN_POINT('',(-66.1657795405966,33.5903722665284,12.));
#90194=CARTESIAN_POINT('Ctrl Pts',(-66.2207497120656,34.1330090612016,12.));
#90195=CARTESIAN_POINT('Ctrl Pts',(-66.2585076236404,34.0597557125862,12.));
#90196=CARTESIAN_POINT('Ctrl Pts',(-66.2778395165851,33.9769512787351,12.));
#90197=CARTESIAN_POINT('Ctrl Pts',(-66.276226218858,33.8946295131779,12.));
#90198=CARTESIAN_POINT('Ctrl Pts',(-66.274075155222,33.7848671591017,12.));
#90199=CARTESIAN_POINT('Ctrl Pts',(-66.2346881970584,33.6759628819924,12.));
#90200=CARTESIAN_POINT('Ctrl Pts',(-66.1657795405966,33.5903722665284,12.));
#90201=CARTESIAN_POINT('Ctrl Pts',(-66.1657795405966,33.5903722665284,12.));
#90202=CARTESIAN_POINT('Ctrl Pts',(-66.1657795405966,33.5903722665284,8.));
#90203=CARTESIAN_POINT('Ctrl Pts',(-66.1657795405966,33.5903722665284,4.));
#90204=CARTESIAN_POINT('Ctrl Pts',(-66.1657795405966,33.5903722665284,0.));
#90205=CARTESIAN_POINT('Origin',(-3.3253631270614E-10,1.72995545227681E-10,
0.));
#90206=CARTESIAN_POINT('Origin',(-3.3253631270614E-10,1.72995545227681E-10,
12.));
#90207=CARTESIAN_POINT('Origin',(-3.3253631270614E-10,1.72995545227681E-10,
0.));
#90208=CARTESIAN_POINT('Ctrl Pts',(-62.6704278106387,40.2823469776964,-5.55111512312578E-16));
#90209=CARTESIAN_POINT('Ctrl Pts',(-62.6704278106387,40.2823469776964,4.));
#90210=CARTESIAN_POINT('Ctrl Pts',(-62.6704278106387,40.2823469776964,8.));
#90211=CARTESIAN_POINT('Ctrl Pts',(-62.6704278106387,40.2823469776964,12.));
#90212=CARTESIAN_POINT('Ctrl Pts',(-62.6110140705998,40.3747816242707,-5.55111512312578E-16));
#90213=CARTESIAN_POINT('Ctrl Pts',(-62.6110140705998,40.3747816242707,3.99999999999999));
#90214=CARTESIAN_POINT('Ctrl Pts',(-62.6110140705998,40.3747816242707,8.00000000000001));
#90215=CARTESIAN_POINT('Ctrl Pts',(-62.6110140705998,40.3747816242707,12.));
#90216=CARTESIAN_POINT('Ctrl Pts',(-62.4519997852064,40.5004281293554,-6.28194844081531E-16));
#90217=CARTESIAN_POINT('Ctrl Pts',(-62.4519997852064,40.5004281293554,4.00000000000001));
#90218=CARTESIAN_POINT('Ctrl Pts',(-62.4519997852064,40.5004281293554,7.99999999999999));
#90219=CARTESIAN_POINT('Ctrl Pts',(-62.4519997852064,40.5004281293554,12.));
#90220=CARTESIAN_POINT('Ctrl Pts',(-62.2544389573118,40.5187208145703,-8.01722692544941E-16));
#90221=CARTESIAN_POINT('Ctrl Pts',(-62.2544389573118,40.5187208145703,3.99999999999999));
#90222=CARTESIAN_POINT('Ctrl Pts',(-62.2544389573118,40.5187208145703,8.00000000000001));
#90223=CARTESIAN_POINT('Ctrl Pts',(-62.2544389573118,40.5187208145703,12.));
#90224=CARTESIAN_POINT('Ctrl Pts',(-62.1730054756455,40.5060598100836,-8.85376672782334E-16));
#90225=CARTESIAN_POINT('Ctrl Pts',(-62.1730054756455,40.5060598100836,4.));
#90226=CARTESIAN_POINT('Ctrl Pts',(-62.1730054756455,40.5060598100836,8.));
#90227=CARTESIAN_POINT('Ctrl Pts',(-62.1730054756455,40.5060598100836,12.));
#90228=CARTESIAN_POINT('',(-62.6704278106387,40.2823469776964,0.));
#90229=CARTESIAN_POINT('',(-62.1730054756455,40.5060598100838,0.));
#90230=CARTESIAN_POINT('Ctrl Pts',(-62.6704278106387,40.2823469776964,-5.2766896056214E-16));
#90231=CARTESIAN_POINT('Ctrl Pts',(-62.6110140705998,40.3747816242707,-5.2766896056214E-16));
#90232=CARTESIAN_POINT('Ctrl Pts',(-62.5201487646607,40.4465796271763,-5.69430864430113E-16));
#90233=CARTESIAN_POINT('Ctrl Pts',(-62.4166968325988,40.4833233215529,-6.4399097783097E-16));
#90234=CARTESIAN_POINT('Ctrl Pts',(-62.3391078835523,40.5108810923353,-6.99911062881613E-16));
#90235=CARTESIAN_POINT('Ctrl Pts',(-62.2544389573118,40.5187208145703,-7.74280140794503E-16));
#90236=CARTESIAN_POINT('Ctrl Pts',(-62.1730054756455,40.5060598100836,-8.57934121031896E-16));
#90237=CARTESIAN_POINT('',(-62.1730054756454,40.5060598100838,12.));
#90238=CARTESIAN_POINT('Ctrl Pts',(-62.1730054756455,40.5060598100836,-8.85376672782334E-16));
#90239=CARTESIAN_POINT('Ctrl Pts',(-62.1730054756455,40.5060598100836,4.));
#90240=CARTESIAN_POINT('Ctrl Pts',(-62.1730054756455,40.5060598100836,8.));
#90241=CARTESIAN_POINT('Ctrl Pts',(-62.1730054756455,40.5060598100836,12.));
#90242=CARTESIAN_POINT('',(-62.6704278106387,40.2823469776964,12.));
#90243=CARTESIAN_POINT('Ctrl Pts',(-62.1730054756455,40.5060598100836,12.));
#90244=CARTESIAN_POINT('Ctrl Pts',(-62.2544389573118,40.5187208145703,12.));
#90245=CARTESIAN_POINT('Ctrl Pts',(-62.3391078835523,40.5108810923354,12.));
#90246=CARTESIAN_POINT('Ctrl Pts',(-62.4166968325988,40.4833233215529,12.));
#90247=CARTESIAN_POINT('Ctrl Pts',(-62.5201487646607,40.4465796271763,12.));
#90248=CARTESIAN_POINT('Ctrl Pts',(-62.6110140705998,40.3747816242707,12.));
#90249=CARTESIAN_POINT('Ctrl Pts',(-62.6704278106387,40.2823469776964,12.));
#90250=CARTESIAN_POINT('Ctrl Pts',(-62.6704278106387,40.2823469776964,12.));
#90251=CARTESIAN_POINT('Ctrl Pts',(-62.6704278106387,40.2823469776964,8.));
#90252=CARTESIAN_POINT('Ctrl Pts',(-62.6704278106387,40.2823469776964,4.));
#90253=CARTESIAN_POINT('Ctrl Pts',(-62.6704278106387,40.2823469776964,-5.55111512312578E-16));
#90254=CARTESIAN_POINT('Ctrl Pts',(-57.8261117662438,39.4479504917287,0.));
#90255=CARTESIAN_POINT('Ctrl Pts',(-57.8261117662438,39.4479504917287,12.));
#90256=CARTESIAN_POINT('Ctrl Pts',(-57.8297740100947,39.4492429618443,0.));
#90257=CARTESIAN_POINT('Ctrl Pts',(-57.8297740100947,39.4492429618443,12.));
#90258=CARTESIAN_POINT('Ctrl Pts',(-57.837104315141,39.4518277003553,0.));
#90259=CARTESIAN_POINT('Ctrl Pts',(-57.837104315141,39.4518277003553,12.));
#90260=CARTESIAN_POINT('Ctrl Pts',(-57.8481172247496,39.4557042029652,0.));
#90261=CARTESIAN_POINT('Ctrl Pts',(-57.8481172247496,39.4557042029652,12.));
#90262=CARTESIAN_POINT('Ctrl Pts',(-57.8628360096803,39.4608716627117,0.));
#90263=CARTESIAN_POINT('Ctrl Pts',(-57.8628360096803,39.4608716627117,12.));
#90264=CARTESIAN_POINT('Ctrl Pts',(-57.8812926637177,39.4673289592259,0.));
#90265=CARTESIAN_POINT('Ctrl Pts',(-57.8812926637177,39.4673289592259,12.));
#90266=CARTESIAN_POINT('Ctrl Pts',(-57.8998074670478,39.473784194937,0.));
#90267=CARTESIAN_POINT('Ctrl Pts',(-57.8998074670478,39.473784194937,12.));
#90268=CARTESIAN_POINT('Ctrl Pts',(-57.9183803632403,39.4802373061058,0.));
#90269=CARTESIAN_POINT('Ctrl Pts',(-57.9183803632403,39.4802373061058,12.));
#90270=CARTESIAN_POINT('Ctrl Pts',(-57.937011245663,39.4866881842317,0.));
#90271=CARTESIAN_POINT('Ctrl Pts',(-57.937011245663,39.4866881842317,12.));
#90272=CARTESIAN_POINT('Ctrl Pts',(-57.9556999583892,39.4931366776714,0.));
#90273=CARTESIAN_POINT('Ctrl Pts',(-57.9556999583892,39.4931366776714,12.));
#90274=CARTESIAN_POINT('Ctrl Pts',(-57.974446317937,39.499582610674,0.));
#90275=CARTESIAN_POINT('Ctrl Pts',(-57.974446317937,39.499582610674,12.));
#90276=CARTESIAN_POINT('Ctrl Pts',(-57.9932501298522,39.5060257981225,0.));
#90277=CARTESIAN_POINT('Ctrl Pts',(-57.9932501298522,39.5060257981225,12.));
#90278=CARTESIAN_POINT('Ctrl Pts',(-58.0121112067895,39.5124660614976,0.));
#90279=CARTESIAN_POINT('Ctrl Pts',(-58.0121112067895,39.5124660614976,12.));
#90280=CARTESIAN_POINT('Ctrl Pts',(-58.0310293875262,39.5189032457184,0.));
#90281=CARTESIAN_POINT('Ctrl Pts',(-58.0310293875262,39.5189032457184,12.));
#90282=CARTESIAN_POINT('Ctrl Pts',(-58.0500045308412,39.5253372136887,0.));
#90283=CARTESIAN_POINT('Ctrl Pts',(-58.0500045308412,39.5253372136887,12.));
#90284=CARTESIAN_POINT('Ctrl Pts',(-58.0690365065374,39.5317678383217,0.));
#90285=CARTESIAN_POINT('Ctrl Pts',(-58.0690365065374,39.5317678383217,12.));
#90286=CARTESIAN_POINT('Ctrl Pts',(-58.0881251879921,39.5381949959221,0.));
#90287=CARTESIAN_POINT('Ctrl Pts',(-58.0881251879921,39.5381949959221,12.));
#90288=CARTESIAN_POINT('Ctrl Pts',(-58.1072704428928,39.5446185579638,0.));
#90289=CARTESIAN_POINT('Ctrl Pts',(-58.1072704428928,39.5446185579638,12.));
#90290=CARTESIAN_POINT('Ctrl Pts',(-58.126472128574,39.5510383869505,0.));
#90291=CARTESIAN_POINT('Ctrl Pts',(-58.126472128574,39.5510383869505,12.));
#90292=CARTESIAN_POINT('Ctrl Pts',(-58.1457300968499,39.5574543406982,0.));
#90293=CARTESIAN_POINT('Ctrl Pts',(-58.1457300968499,39.5574543406982,12.));
#90294=CARTESIAN_POINT('Ctrl Pts',(-58.1650441970387,39.563866275018,0.));
#90295=CARTESIAN_POINT('Ctrl Pts',(-58.1650441970387,39.563866275018,12.));
#90296=CARTESIAN_POINT('Ctrl Pts',(-58.1844142794338,39.5702740467999,0.));
#90297=CARTESIAN_POINT('Ctrl Pts',(-58.1844142794338,39.5702740467999,12.));
#90298=CARTESIAN_POINT('Ctrl Pts',(-58.2038401992457,39.57667751752,0.));
#90299=CARTESIAN_POINT('Ctrl Pts',(-58.2038401992457,39.57667751752,12.));
#90300=CARTESIAN_POINT('Ctrl Pts',(-58.2233218164365,39.5830765530891,0.));
#90301=CARTESIAN_POINT('Ctrl Pts',(-58.2233218164365,39.5830765530891,12.));
#90302=CARTESIAN_POINT('Ctrl Pts',(-58.2428589938369,39.5894710221713,0.));
#90303=CARTESIAN_POINT('Ctrl Pts',(-58.2428589938369,39.5894710221713,12.));
#90304=CARTESIAN_POINT('Ctrl Pts',(-58.2624515958419,39.5958607950239,0.));
#90305=CARTESIAN_POINT('Ctrl Pts',(-58.2624515958419,39.5958607950239,12.));
#90306=CARTESIAN_POINT('Ctrl Pts',(-58.2820994868118,39.602245742079,0.));
#90307=CARTESIAN_POINT('Ctrl Pts',(-58.2820994868118,39.602245742079,12.));
#90308=CARTESIAN_POINT('Ctrl Pts',(-58.3018025297323,39.6086257327583,0.));
#90309=CARTESIAN_POINT('Ctrl Pts',(-58.3018025297323,39.6086257327583,12.));
#90310=CARTESIAN_POINT('Ctrl Pts',(-58.3215605869221,39.6150006360914,0.));
#90311=CARTESIAN_POINT('Ctrl Pts',(-58.3215605869221,39.6150006360914,12.));
#90312=CARTESIAN_POINT('Ctrl Pts',(-58.3413735206423,39.6213703212531,0.));
#90313=CARTESIAN_POINT('Ctrl Pts',(-58.3413735206423,39.6213703212531,12.));
#90314=CARTESIAN_POINT('Ctrl Pts',(-58.3612411936905,39.6277346580892,0.));
#90315=CARTESIAN_POINT('Ctrl Pts',(-58.3612411936905,39.6277346580892,12.));
#90316=CARTESIAN_POINT('Ctrl Pts',(-58.3811634701037,39.6340935177476,0.));
#90317=CARTESIAN_POINT('Ctrl Pts',(-58.3811634701037,39.6340935177476,12.));
#90318=CARTESIAN_POINT('Ctrl Pts',(-58.4011402154196,39.6404467729094,0.));
#90319=CARTESIAN_POINT('Ctrl Pts',(-58.4011402154196,39.6404467729094,12.));
#90320=CARTESIAN_POINT('Ctrl Pts',(-58.4211712963004,39.6467942974451,0.));
#90321=CARTESIAN_POINT('Ctrl Pts',(-58.4211712963004,39.6467942974451,12.));
#90322=CARTESIAN_POINT('Ctrl Pts',(-58.4412565802979,39.653135966204,0.));
#90323=CARTESIAN_POINT('Ctrl Pts',(-58.4412565802979,39.653135966204,12.));
#90324=CARTESIAN_POINT('Ctrl Pts',(-58.4613959355788,39.6594716547689,0.));
#90325=CARTESIAN_POINT('Ctrl Pts',(-58.4613959355788,39.6594716547689,12.));
#90326=CARTESIAN_POINT('Ctrl Pts',(-58.4815892306066,39.6658012391815,0.));
#90327=CARTESIAN_POINT('Ctrl Pts',(-58.4815892306066,39.6658012391815,12.));
#90328=CARTESIAN_POINT('Ctrl Pts',(-58.5018363341604,39.6721245959531,0.));
#90329=CARTESIAN_POINT('Ctrl Pts',(-58.5018363341604,39.6721245959531,12.));
#90330=CARTESIAN_POINT('Ctrl Pts',(-58.5221371154761,39.6784416021826,0.));
#90331=CARTESIAN_POINT('Ctrl Pts',(-58.5221371154761,39.6784416021826,12.));
#90332=CARTESIAN_POINT('Ctrl Pts',(-58.5424914443415,39.6847521356395,0.));
#90333=CARTESIAN_POINT('Ctrl Pts',(-58.5424914443415,39.6847521356395,12.));
#90334=CARTESIAN_POINT('Ctrl Pts',(-58.5628991912052,39.6910560748629,0.));
#90335=CARTESIAN_POINT('Ctrl Pts',(-58.5628991912052,39.6910560748629,12.));
#90336=CARTESIAN_POINT('Ctrl Pts',(-58.5833602272744,39.6973532992539,0.));
#90337=CARTESIAN_POINT('Ctrl Pts',(-58.5833602272744,39.6973532992539,12.));
#90338=CARTESIAN_POINT('Ctrl Pts',(-58.6038744244659,39.7036436890233,0.));
#90339=CARTESIAN_POINT('Ctrl Pts',(-58.6038744244659,39.7036436890233,12.));
#90340=CARTESIAN_POINT('Ctrl Pts',(-58.6244416553562,39.7099271251413,0.));
#90341=CARTESIAN_POINT('Ctrl Pts',(-58.6244416553562,39.7099271251413,12.));
#90342=CARTESIAN_POINT('Ctrl Pts',(-58.6450617931274,39.7162034892899,0.));
#90343=CARTESIAN_POINT('Ctrl Pts',(-58.6450617931274,39.7162034892899,12.));
#90344=CARTESIAN_POINT('Ctrl Pts',(-58.6657347115034,39.72247266381,0.));
#90345=CARTESIAN_POINT('Ctrl Pts',(-58.6657347115034,39.72247266381,12.));
#90346=CARTESIAN_POINT('Ctrl Pts',(-58.6864602847088,39.7287345316681,0.));
#90347=CARTESIAN_POINT('Ctrl Pts',(-58.6864602847088,39.7287345316681,12.));
#90348=CARTESIAN_POINT('Ctrl Pts',(-58.7072383875027,39.734988976475,0.));
#90349=CARTESIAN_POINT('Ctrl Pts',(-58.7072383875027,39.734988976475,12.));
#90350=CARTESIAN_POINT('Ctrl Pts',(-58.7280688951916,39.7412358824953,0.));
#90351=CARTESIAN_POINT('Ctrl Pts',(-58.7280688951916,39.7412358824953,12.));
#90352=CARTESIAN_POINT('Ctrl Pts',(-58.7489516836445,39.7474751346598,0.));
#90353=CARTESIAN_POINT('Ctrl Pts',(-58.7489516836445,39.7474751346598,12.));
#90354=CARTESIAN_POINT('Ctrl Pts',(-58.7698866293029,39.7537066185813,0.));
#90355=CARTESIAN_POINT('Ctrl Pts',(-58.7698866293029,39.7537066185813,12.));
#90356=CARTESIAN_POINT('Ctrl Pts',(-58.7908736091798,39.7599302205521,0.));
#90357=CARTESIAN_POINT('Ctrl Pts',(-58.7908736091798,39.7599302205521,12.));
#90358=CARTESIAN_POINT('Ctrl Pts',(-58.8119125008517,39.7661458275274,0.));
#90359=CARTESIAN_POINT('Ctrl Pts',(-58.8119125008517,39.7661458275274,12.));
#90360=CARTESIAN_POINT('Ctrl Pts',(-58.8330031824453,39.772353327112,0.));
#90361=CARTESIAN_POINT('Ctrl Pts',(-58.8330031824453,39.772353327112,12.));
#90362=CARTESIAN_POINT('Ctrl Pts',(-58.8541455326231,39.7785526075478,0.));
#90363=CARTESIAN_POINT('Ctrl Pts',(-58.8541455326231,39.7785526075478,12.));
#90364=CARTESIAN_POINT('Ctrl Pts',(-58.8753394305585,39.7847435576996,0.));
#90365=CARTESIAN_POINT('Ctrl Pts',(-58.8753394305585,39.7847435576996,12.));
#90366=CARTESIAN_POINT('Ctrl Pts',(-58.8965847559391,39.7909260670517,0.));
#90367=CARTESIAN_POINT('Ctrl Pts',(-58.8965847559391,39.7909260670517,12.));
#90368=CARTESIAN_POINT('Ctrl Pts',(-58.9178813889704,39.7971000257044,0.));
#90369=CARTESIAN_POINT('Ctrl Pts',(-58.9178813889704,39.7971000257044,12.));
#90370=CARTESIAN_POINT('Ctrl Pts',(-58.9392292103747,39.8032653243712,0.));
#90371=CARTESIAN_POINT('Ctrl Pts',(-58.9392292103747,39.8032653243712,12.));
#90372=CARTESIAN_POINT('Ctrl Pts',(-58.9606281013875,39.8094218543782,0.));
#90373=CARTESIAN_POINT('Ctrl Pts',(-58.9606281013875,39.8094218543782,12.));
#90374=CARTESIAN_POINT('Ctrl Pts',(-58.9820779437484,39.8155695076626,0.));
#90375=CARTESIAN_POINT('Ctrl Pts',(-58.9820779437484,39.8155695076626,12.));
#90376=CARTESIAN_POINT('Ctrl Pts',(-59.0035786197024,39.821708176766,0.));
#90377=CARTESIAN_POINT('Ctrl Pts',(-59.0035786197024,39.821708176766,12.));
#90378=CARTESIAN_POINT('Ctrl Pts',(-59.0251300119973,39.8278377548262,0.));
#90379=CARTESIAN_POINT('Ctrl Pts',(-59.0251300119973,39.8278377548262,12.));
#90380=CARTESIAN_POINT('Ctrl Pts',(-59.0467320038784,39.8339581355716,0.));
#90381=CARTESIAN_POINT('Ctrl Pts',(-59.0467320038784,39.8339581355716,12.));
#90382=CARTESIAN_POINT('Ctrl Pts',(-59.0683844790764,39.8400692133139,0.));
#90383=CARTESIAN_POINT('Ctrl Pts',(-59.0683844790764,39.8400692133139,12.));
#90384=CARTESIAN_POINT('Ctrl Pts',(-59.090087321798,39.8461708829456,0.));
#90385=CARTESIAN_POINT('Ctrl Pts',(-59.090087321798,39.8461708829456,12.));
#90386=CARTESIAN_POINT('Ctrl Pts',(-59.1118404167292,39.8522630399328,0.));
#90387=CARTESIAN_POINT('Ctrl Pts',(-59.1118404167292,39.8522630399328,12.));
#90388=CARTESIAN_POINT('Ctrl Pts',(-59.1336436490342,39.8583455803105,0.));
#90389=CARTESIAN_POINT('Ctrl Pts',(-59.1336436490342,39.8583455803105,12.));
#90390=CARTESIAN_POINT('Ctrl Pts',(-59.1554969043522,39.8644184006787,0.));
#90391=CARTESIAN_POINT('Ctrl Pts',(-59.1554969043522,39.8644184006787,12.));
#90392=CARTESIAN_POINT('Ctrl Pts',(-59.1774000687879,39.8704813981988,0.));
#90393=CARTESIAN_POINT('Ctrl Pts',(-59.1774000687879,39.8704813981988,12.));
#90394=CARTESIAN_POINT('Ctrl Pts',(-59.1993530289028,39.876534470591,0.));
#90395=CARTESIAN_POINT('Ctrl Pts',(-59.1993530289028,39.876534470591,12.));
#90396=CARTESIAN_POINT('Ctrl Pts',(-59.2213556717209,39.8825775161267,0.));
#90397=CARTESIAN_POINT('Ctrl Pts',(-59.2213556717209,39.8825775161267,12.));
#90398=CARTESIAN_POINT('Ctrl Pts',(-59.2434078847247,39.8886104336242,0.));
#90399=CARTESIAN_POINT('Ctrl Pts',(-59.2434078847247,39.8886104336242,12.));
#90400=CARTESIAN_POINT('Ctrl Pts',(-59.2655095558521,39.8946331224438,0.));
#90401=CARTESIAN_POINT('Ctrl Pts',(-59.2655095558521,39.8946331224438,12.));
#90402=CARTESIAN_POINT('Ctrl Pts',(-59.2876605734846,39.9006454824845,0.));
#90403=CARTESIAN_POINT('Ctrl Pts',(-59.2876605734846,39.9006454824845,12.));
#90404=CARTESIAN_POINT('Ctrl Pts',(-59.3098608264419,39.9066474141803,0.));
#90405=CARTESIAN_POINT('Ctrl Pts',(-59.3098608264419,39.9066474141803,12.));
#90406=CARTESIAN_POINT('Ctrl Pts',(-59.3321102039852,39.9126388184936,0.));
#90407=CARTESIAN_POINT('Ctrl Pts',(-59.3321102039852,39.9126388184936,12.));
#90408=CARTESIAN_POINT('Ctrl Pts',(-59.3544085958151,39.9186195969104,0.));
#90409=CARTESIAN_POINT('Ctrl Pts',(-59.3544085958151,39.9186195969104,12.));
#90410=CARTESIAN_POINT('Ctrl Pts',(-59.3767558920675,39.9245896514367,0.));
#90411=CARTESIAN_POINT('Ctrl Pts',(-59.3767558920675,39.9245896514367,12.));
#90412=CARTESIAN_POINT('Ctrl Pts',(-59.3991519833016,39.9305488845958,0.));
#90413=CARTESIAN_POINT('Ctrl Pts',(-59.3991519833016,39.9305488845958,12.));
#90414=CARTESIAN_POINT('Ctrl Pts',(-59.4215967604967,39.9364971994242,0.));
#90415=CARTESIAN_POINT('Ctrl Pts',(-59.4215967604967,39.9364971994242,12.));
#90416=CARTESIAN_POINT('Ctrl Pts',(-59.4440901150582,39.9424344994672,0.));
#90417=CARTESIAN_POINT('Ctrl Pts',(-59.4440901150582,39.9424344994672,12.));
#90418=CARTESIAN_POINT('Ctrl Pts',(-59.4666319388133,39.9483606887737,0.));
#90419=CARTESIAN_POINT('Ctrl Pts',(-59.4666319388133,39.9483606887737,12.));
#90420=CARTESIAN_POINT('Ctrl Pts',(-59.4892221240068,39.9542756718922,0.));
#90421=CARTESIAN_POINT('Ctrl Pts',(-59.4892221240068,39.9542756718922,12.));
#90422=CARTESIAN_POINT('Ctrl Pts',(-59.5118605632891,39.9601793538682,0.));
#90423=CARTESIAN_POINT('Ctrl Pts',(-59.5118605632891,39.9601793538682,12.));
#90424=CARTESIAN_POINT('Ctrl Pts',(-59.5345471497129,39.9660716402403,0.));
#90425=CARTESIAN_POINT('Ctrl Pts',(-59.5345471497129,39.9660716402403,12.));
#90426=CARTESIAN_POINT('Ctrl Pts',(-59.5572817767388,39.9719524370345,0.));
#90427=CARTESIAN_POINT('Ctrl Pts',(-59.5572817767388,39.9719524370345,12.));
#90428=CARTESIAN_POINT('Ctrl Pts',(-59.5800643382314,39.9778216507605,0.));
#90429=CARTESIAN_POINT('Ctrl Pts',(-59.5800643382314,39.9778216507605,12.));
#90430=CARTESIAN_POINT('Ctrl Pts',(-59.6028947284562,39.9836791884079,0.));
#90431=CARTESIAN_POINT('Ctrl Pts',(-59.6028947284562,39.9836791884079,12.));
#90432=CARTESIAN_POINT('Ctrl Pts',(-59.6257728420669,39.9895249574448,0.));
#90433=CARTESIAN_POINT('Ctrl Pts',(-59.6257728420669,39.9895249574448,12.));
#90434=CARTESIAN_POINT('Ctrl Pts',(-59.6486985741041,39.9953588658132,0.));
#90435=CARTESIAN_POINT('Ctrl Pts',(-59.6486985741041,39.9953588658132,12.));
#90436=CARTESIAN_POINT('Ctrl Pts',(-59.6716718200005,40.0011808219241,0.));
#90437=CARTESIAN_POINT('Ctrl Pts',(-59.6716718200005,40.0011808219241,12.));
#90438=CARTESIAN_POINT('Ctrl Pts',(-59.6946924755773,40.0069907346537,0.));
#90439=CARTESIAN_POINT('Ctrl Pts',(-59.6946924755773,40.0069907346537,12.));
#90440=CARTESIAN_POINT('Ctrl Pts',(-59.7177604370403,40.0127885133403,0.));
#90441=CARTESIAN_POINT('Ctrl Pts',(-59.7177604370403,40.0127885133403,12.));
#90442=CARTESIAN_POINT('Ctrl Pts',(-59.7408756009679,40.0185740677821,0.));
#90443=CARTESIAN_POINT('Ctrl Pts',(-59.7408756009679,40.0185740677821,12.));
#90444=CARTESIAN_POINT('Ctrl Pts',(-59.7640378643106,40.0243473082337,0.));
#90445=CARTESIAN_POINT('Ctrl Pts',(-59.7640378643106,40.0243473082337,12.));
#90446=CARTESIAN_POINT('Ctrl Pts',(-59.7872471243942,40.0301081454002,0.));
#90447=CARTESIAN_POINT('Ctrl Pts',(-59.7872471243942,40.0301081454002,12.));
#90448=CARTESIAN_POINT('Ctrl Pts',(-59.8105032789179,40.035856490434,0.));
#90449=CARTESIAN_POINT('Ctrl Pts',(-59.8105032789179,40.035856490434,12.));
#90450=CARTESIAN_POINT('Ctrl Pts',(-59.8338062259492,40.0415922549315,0.));
#90451=CARTESIAN_POINT('Ctrl Pts',(-59.8338062259492,40.0415922549315,12.));
#90452=CARTESIAN_POINT('Ctrl Pts',(-59.8571558639145,40.0473153509324,0.));
#90453=CARTESIAN_POINT('Ctrl Pts',(-59.8571558639145,40.0473153509324,12.));
#90454=CARTESIAN_POINT('Ctrl Pts',(-59.8805520915972,40.0530256909161,0.));
#90455=CARTESIAN_POINT('Ctrl Pts',(-59.8805520915972,40.0530256909161,12.));
#90456=CARTESIAN_POINT('Ctrl Pts',(-59.9039948081428,40.0587231877959,0.));
#90457=CARTESIAN_POINT('Ctrl Pts',(-59.9039948081428,40.0587231877959,12.));
#90458=CARTESIAN_POINT('Ctrl Pts',(-59.927483913055,40.0644077549158,0.));
#90459=CARTESIAN_POINT('Ctrl Pts',(-59.927483913055,40.0644077549158,12.));
#90460=CARTESIAN_POINT('Ctrl Pts',(-59.9510193061929,40.0700793060475,0.));
#90461=CARTESIAN_POINT('Ctrl Pts',(-59.9510193061929,40.0700793060475,12.));
#90462=CARTESIAN_POINT('Ctrl Pts',(-59.974600887759,40.0757377553893,0.));
#90463=CARTESIAN_POINT('Ctrl Pts',(-59.974600887759,40.0757377553893,12.));
#90464=CARTESIAN_POINT('Ctrl Pts',(-59.9982285582991,40.0813830175629,0.));
#90465=CARTESIAN_POINT('Ctrl Pts',(-59.9982285582991,40.0813830175629,12.));
#90466=CARTESIAN_POINT('Ctrl Pts',(-60.0219022187066,40.0870150076078,0.));
#90467=CARTESIAN_POINT('Ctrl Pts',(-60.0219022187066,40.0870150076078,12.));
#90468=CARTESIAN_POINT('Ctrl Pts',(-60.0456217702203,40.0926336409787,0.));
#90469=CARTESIAN_POINT('Ctrl Pts',(-60.0456217702203,40.0926336409787,12.));
#90470=CARTESIAN_POINT('Ctrl Pts',(-60.0693871144207,40.0982388335421,0.));
#90471=CARTESIAN_POINT('Ctrl Pts',(-60.0693871144207,40.0982388335421,12.));
#90472=CARTESIAN_POINT('Ctrl Pts',(-60.0931981532194,40.1038305015763,0.));
#90473=CARTESIAN_POINT('Ctrl Pts',(-60.0931981532194,40.1038305015763,12.));
#90474=CARTESIAN_POINT('Ctrl Pts',(-60.1170547888572,40.1094085617672,0.));
#90475=CARTESIAN_POINT('Ctrl Pts',(-60.1170547888572,40.1094085617672,12.));
#90476=CARTESIAN_POINT('Ctrl Pts',(-60.1409569239093,40.1149729312036,0.));
#90477=CARTESIAN_POINT('Ctrl Pts',(-60.1409569239093,40.1149729312036,12.));
#90478=CARTESIAN_POINT('Ctrl Pts',(-60.1649044612829,40.120523527374,0.));
#90479=CARTESIAN_POINT('Ctrl Pts',(-60.1649044612829,40.120523527374,12.));
#90480=CARTESIAN_POINT('Ctrl Pts',(-60.1888973042151,40.1260602681644,0.));
#90481=CARTESIAN_POINT('Ctrl Pts',(-60.1888973042151,40.1260602681644,12.));
#90482=CARTESIAN_POINT('Ctrl Pts',(-60.2129353562617,40.1315830718575,0.));
#90483=CARTESIAN_POINT('Ctrl Pts',(-60.2129353562617,40.1315830718575,12.));
#90484=CARTESIAN_POINT('Ctrl Pts',(-60.2370185212957,40.13709185713,0.));
#90485=CARTESIAN_POINT('Ctrl Pts',(-60.2370185212957,40.13709185713,12.));
#90486=CARTESIAN_POINT('Ctrl Pts',(-60.2611467035109,40.1425865430468,0.));
#90487=CARTESIAN_POINT('Ctrl Pts',(-60.2611467035109,40.1425865430468,12.));
#90488=CARTESIAN_POINT('Ctrl Pts',(-60.2853198074215,40.1480670490583,0.));
#90489=CARTESIAN_POINT('Ctrl Pts',(-60.2853198074215,40.1480670490583,12.));
#90490=CARTESIAN_POINT('Ctrl Pts',(-60.3095377378589,40.1535332949978,0.));
#90491=CARTESIAN_POINT('Ctrl Pts',(-60.3095377378589,40.1535332949978,12.));
#90492=CARTESIAN_POINT('Ctrl Pts',(-60.3338003999616,40.1589852010811,0.));
#90493=CARTESIAN_POINT('Ctrl Pts',(-60.3338003999616,40.1589852010811,12.));
#90494=CARTESIAN_POINT('Ctrl Pts',(-60.3581076991731,40.1644226879043,0.));
#90495=CARTESIAN_POINT('Ctrl Pts',(-60.3581076991731,40.1644226879043,12.));
#90496=CARTESIAN_POINT('Ctrl Pts',(-60.382459541246,40.1698456764387,0.));
#90497=CARTESIAN_POINT('Ctrl Pts',(-60.382459541246,40.1698456764387,12.));
#90498=CARTESIAN_POINT('Ctrl Pts',(-60.4068558322415,40.1752540880273,0.));
#90499=CARTESIAN_POINT('Ctrl Pts',(-60.4068558322415,40.1752540880273,12.));
#90500=CARTESIAN_POINT('Ctrl Pts',(-60.4312964785269,40.1806478443828,0.));
#90501=CARTESIAN_POINT('Ctrl Pts',(-60.4312964785269,40.1806478443828,12.));
#90502=CARTESIAN_POINT('Ctrl Pts',(-60.4557813867677,40.1860268675875,0.));
#90503=CARTESIAN_POINT('Ctrl Pts',(-60.4557813867677,40.1860268675875,12.));
#90504=CARTESIAN_POINT('Ctrl Pts',(-60.4803104639211,40.1913910800911,0.));
#90505=CARTESIAN_POINT('Ctrl Pts',(-60.4803104639211,40.1913910800911,12.));
#90506=CARTESIAN_POINT('Ctrl Pts',(-60.5048836172424,40.1967404047055,0.));
#90507=CARTESIAN_POINT('Ctrl Pts',(-60.5048836172424,40.1967404047055,12.));
#90508=CARTESIAN_POINT('Ctrl Pts',(-60.5295007542838,40.2020747646012,0.));
#90509=CARTESIAN_POINT('Ctrl Pts',(-60.5295007542838,40.2020747646012,12.));
#90510=CARTESIAN_POINT('Ctrl Pts',(-60.5541617828927,40.2073940833054,0.));
#90511=CARTESIAN_POINT('Ctrl Pts',(-60.5541617828927,40.2073940833054,12.));
#90512=CARTESIAN_POINT('Ctrl Pts',(-60.5788666112043,40.2126982847012,0.));
#90513=CARTESIAN_POINT('Ctrl Pts',(-60.5788666112043,40.2126982847012,12.));
#90514=CARTESIAN_POINT('Ctrl Pts',(-60.6036151476347,40.2179872930272,0.));
#90515=CARTESIAN_POINT('Ctrl Pts',(-60.6036151476347,40.2179872930272,12.));
#90516=CARTESIAN_POINT('Ctrl Pts',(-60.6284073008865,40.2232610328717,0.));
#90517=CARTESIAN_POINT('Ctrl Pts',(-60.6284073008865,40.2232610328717,12.));
#90518=CARTESIAN_POINT('Ctrl Pts',(-60.6532429799493,40.2285194291702,0.));
#90519=CARTESIAN_POINT('Ctrl Pts',(-60.6532429799493,40.2285194291702,12.));
#90520=CARTESIAN_POINT('Ctrl Pts',(-60.678122094098,40.2337624072029,0.));
#90521=CARTESIAN_POINT('Ctrl Pts',(-60.678122094098,40.2337624072029,12.));
#90522=CARTESIAN_POINT('Ctrl Pts',(-60.7030445528863,40.2389898925937,0.));
#90523=CARTESIAN_POINT('Ctrl Pts',(-60.7030445528863,40.2389898925937,12.));
#90524=CARTESIAN_POINT('Ctrl Pts',(-60.72801026614,40.2442018113116,0.));
#90525=CARTESIAN_POINT('Ctrl Pts',(-60.72801026614,40.2442018113116,12.));
#90526=CARTESIAN_POINT('Ctrl Pts',(-60.7530191439603,40.2493980896646,0.));
#90527=CARTESIAN_POINT('Ctrl Pts',(-60.7530191439603,40.2493980896646,12.));
#90528=CARTESIAN_POINT('Ctrl Pts',(-60.7780710967253,40.2545786542957,0.));
#90529=CARTESIAN_POINT('Ctrl Pts',(-60.7780710967253,40.2545786542957,12.));
#90530=CARTESIAN_POINT('Ctrl Pts',(-60.8031660350879,40.2597434321804,0.));
#90531=CARTESIAN_POINT('Ctrl Pts',(-60.8031660350879,40.2597434321804,12.));
#90532=CARTESIAN_POINT('Ctrl Pts',(-60.8283038699703,40.2648923506245,0.));
#90533=CARTESIAN_POINT('Ctrl Pts',(-60.8283038699703,40.2648923506245,12.));
#90534=CARTESIAN_POINT('Ctrl Pts',(-60.8534845125535,40.2700253372644,0.));
#90535=CARTESIAN_POINT('Ctrl Pts',(-60.8534845125535,40.2700253372644,12.));
#90536=CARTESIAN_POINT('Ctrl Pts',(-60.8787078742817,40.2751423200637,0.));
#90537=CARTESIAN_POINT('Ctrl Pts',(-60.8787078742817,40.2751423200637,12.));
#90538=CARTESIAN_POINT('Ctrl Pts',(-60.903973866867,40.2802432273105,0.));
#90539=CARTESIAN_POINT('Ctrl Pts',(-60.903973866867,40.2802432273105,12.));
#90540=CARTESIAN_POINT('Ctrl Pts',(-60.9292824022888,40.2853279876162,0.));
#90541=CARTESIAN_POINT('Ctrl Pts',(-60.9292824022888,40.2853279876162,12.));
#90542=CARTESIAN_POINT('Ctrl Pts',(-60.9546333927919,40.2903965299155,0.));
#90543=CARTESIAN_POINT('Ctrl Pts',(-60.9546333927919,40.2903965299155,12.));
#90544=CARTESIAN_POINT('Ctrl Pts',(-60.9800267508781,40.2954487834688,0.));
#90545=CARTESIAN_POINT('Ctrl Pts',(-60.9800267508781,40.2954487834688,12.));
#90546=CARTESIAN_POINT('Ctrl Pts',(-61.005462389306,40.3004846778577,0.));
#90547=CARTESIAN_POINT('Ctrl Pts',(-61.005462389306,40.3004846778577,12.));
#90548=CARTESIAN_POINT('Ctrl Pts',(-61.0309402210915,40.3055041429772,0.));
#90549=CARTESIAN_POINT('Ctrl Pts',(-61.0309402210915,40.3055041429772,12.));
#90550=CARTESIAN_POINT('Ctrl Pts',(-61.0564601595047,40.3105071090308,0.));
#90551=CARTESIAN_POINT('Ctrl Pts',(-61.0564601595047,40.3105071090308,12.));
#90552=CARTESIAN_POINT('Ctrl Pts',(-61.0820221180646,40.3154935065264,0.));
#90553=CARTESIAN_POINT('Ctrl Pts',(-61.0820221180646,40.3154935065264,12.));
#90554=CARTESIAN_POINT('Ctrl Pts',(-61.1076260105265,40.3204632662729,0.));
#90555=CARTESIAN_POINT('Ctrl Pts',(-61.1076260105265,40.3204632662729,12.));
#90556=CARTESIAN_POINT('Ctrl Pts',(-61.1332717508799,40.3254163193806,0.));
#90557=CARTESIAN_POINT('Ctrl Pts',(-61.1332717508799,40.3254163193806,12.));
#90558=CARTESIAN_POINT('Ctrl Pts',(-61.1589592533623,40.3303525972621,0.));
#90559=CARTESIAN_POINT('Ctrl Pts',(-61.1589592533623,40.3303525972621,12.));
#90560=CARTESIAN_POINT('Ctrl Pts',(-61.184688432465,40.3352720316373,0.));
#90561=CARTESIAN_POINT('Ctrl Pts',(-61.184688432465,40.3352720316373,12.));
#90562=CARTESIAN_POINT('Ctrl Pts',(-61.2104592029375,40.3401745545369,0.));
#90563=CARTESIAN_POINT('Ctrl Pts',(-61.2104592029375,40.3401745545369,12.));
#90564=CARTESIAN_POINT('Ctrl Pts',(-61.236271479789,40.3450600983104,0.));
#90565=CARTESIAN_POINT('Ctrl Pts',(-61.236271479789,40.3450600983104,12.));
#90566=CARTESIAN_POINT('Ctrl Pts',(-61.2621251782849,40.3499285956297,0.));
#90567=CARTESIAN_POINT('Ctrl Pts',(-61.2621251782849,40.3499285956297,12.));
#90568=CARTESIAN_POINT('Ctrl Pts',(-61.2880202139358,40.3547799794672,0.));
#90569=CARTESIAN_POINT('Ctrl Pts',(-61.2880202139358,40.3547799794672,12.));
#90570=CARTESIAN_POINT('Ctrl Pts',(-61.3139565024838,40.3596141830786,0.));
#90571=CARTESIAN_POINT('Ctrl Pts',(-61.3139565024838,40.3596141830786,12.));
#90572=CARTESIAN_POINT('Ctrl Pts',(-61.3399339598851,40.3644311399861,0.));
#90573=CARTESIAN_POINT('Ctrl Pts',(-61.3399339598851,40.3644311399861,12.));
#90574=CARTESIAN_POINT('Ctrl Pts',(-61.3659525022917,40.3692307839642,0.));
#90575=CARTESIAN_POINT('Ctrl Pts',(-61.3659525022917,40.3692307839642,12.));
#90576=CARTESIAN_POINT('Ctrl Pts',(-61.3920120460232,40.3740130490233,0.));
#90577=CARTESIAN_POINT('Ctrl Pts',(-61.3920120460232,40.3740130490233,12.));
#90578=CARTESIAN_POINT('Ctrl Pts',(-61.418112507605,40.3787778694373,0.));
#90579=CARTESIAN_POINT('Ctrl Pts',(-61.418112507605,40.3787778694373,12.));
#90580=CARTESIAN_POINT('Ctrl Pts',(-61.4442538038053,40.3835251797725,0.));
#90581=CARTESIAN_POINT('Ctrl Pts',(-61.4442538038053,40.3835251797725,12.));
#90582=CARTESIAN_POINT('Ctrl Pts',(-61.4704358516711,40.3882549149229,0.));
#90583=CARTESIAN_POINT('Ctrl Pts',(-61.4704358516711,40.3882549149229,12.));
#90584=CARTESIAN_POINT('Ctrl Pts',(-61.4966585685544,40.3929670101363,0.));
#90585=CARTESIAN_POINT('Ctrl Pts',(-61.4966585685544,40.3929670101363,12.));
#90586=CARTESIAN_POINT('Ctrl Pts',(-61.5229218721532,40.3976614010648,0.));
#90587=CARTESIAN_POINT('Ctrl Pts',(-61.5229218721532,40.3976614010648,12.));
#90588=CARTESIAN_POINT('Ctrl Pts',(-61.5492256804709,40.4023380237227,0.));
#90589=CARTESIAN_POINT('Ctrl Pts',(-61.5492256804709,40.4023380237227,12.));
#90590=CARTESIAN_POINT('Ctrl Pts',(-61.5755699117318,40.4069968143953,0.));
#90591=CARTESIAN_POINT('Ctrl Pts',(-61.5755699117318,40.4069968143953,12.));
#90592=CARTESIAN_POINT('Ctrl Pts',(-61.6019544843009,40.4116377095595,0.));
#90593=CARTESIAN_POINT('Ctrl Pts',(-61.6019544843009,40.4116377095595,12.));
#90594=CARTESIAN_POINT('Ctrl Pts',(-61.628379316608,40.4162606458119,0.));
#90595=CARTESIAN_POINT('Ctrl Pts',(-61.628379316608,40.4162606458119,12.));
#90596=CARTESIAN_POINT('Ctrl Pts',(-61.6548443270397,40.420865559772,0.));
#90597=CARTESIAN_POINT('Ctrl Pts',(-61.6548443270397,40.420865559772,12.));
#90598=CARTESIAN_POINT('Ctrl Pts',(-61.6813494339295,40.4254523880766,0.));
#90599=CARTESIAN_POINT('Ctrl Pts',(-61.6813494339295,40.4254523880766,12.));
#90600=CARTESIAN_POINT('Ctrl Pts',(-61.7078945557812,40.4300210675848,0.));
#90601=CARTESIAN_POINT('Ctrl Pts',(-61.7078945557812,40.4300210675848,12.));
#90602=CARTESIAN_POINT('Ctrl Pts',(-61.7344796114409,40.4345715355411,0.));
#90603=CARTESIAN_POINT('Ctrl Pts',(-61.7344796114409,40.4345715355411,12.));
#90604=CARTESIAN_POINT('Ctrl Pts',(-61.7611045202875,40.439103729759,0.));
#90605=CARTESIAN_POINT('Ctrl Pts',(-61.7611045202875,40.439103729759,12.));
#90606=CARTESIAN_POINT('Ctrl Pts',(-61.7877692024064,40.4436175887942,0.));
#90607=CARTESIAN_POINT('Ctrl Pts',(-61.7877692024064,40.4436175887942,12.));
#90608=CARTESIAN_POINT('Ctrl Pts',(-61.8144735787767,40.448113052135,0.));
#90609=CARTESIAN_POINT('Ctrl Pts',(-61.8144735787767,40.448113052135,12.));
#90610=CARTESIAN_POINT('Ctrl Pts',(-61.8412175708524,40.4525900597877,0.));
#90611=CARTESIAN_POINT('Ctrl Pts',(-61.8412175708524,40.4525900597877,12.));
#90612=CARTESIAN_POINT('Ctrl Pts',(-61.8680011001513,40.4570485518735,0.));
#90613=CARTESIAN_POINT('Ctrl Pts',(-61.8680011001513,40.4570485518735,12.));
#90614=CARTESIAN_POINT('Ctrl Pts',(-61.8948240877998,40.4614884681884,0.));
#90615=CARTESIAN_POINT('Ctrl Pts',(-61.8948240877998,40.4614884681884,12.));
#90616=CARTESIAN_POINT('Ctrl Pts',(-61.9216864541758,40.4659097478595,0.));
#90617=CARTESIAN_POINT('Ctrl Pts',(-61.9216864541758,40.4659097478595,12.));
#90618=CARTESIAN_POINT('Ctrl Pts',(-61.9485881182957,40.4703123287642,0.));
#90619=CARTESIAN_POINT('Ctrl Pts',(-61.9485881182957,40.4703123287642,12.));
#90620=CARTESIAN_POINT('Ctrl Pts',(-61.9755289983094,40.4746961480045,0.));
#90621=CARTESIAN_POINT('Ctrl Pts',(-61.9755289983094,40.4746961480045,12.));
#90622=CARTESIAN_POINT('Ctrl Pts',(-62.0025090126008,40.4790611429613,0.));
#90623=CARTESIAN_POINT('Ctrl Pts',(-62.0025090126008,40.4790611429613,12.));
#90624=CARTESIAN_POINT('Ctrl Pts',(-62.0295280807449,40.4834072522181,0.));
#90625=CARTESIAN_POINT('Ctrl Pts',(-62.0295280807449,40.4834072522181,12.));
#90626=CARTESIAN_POINT('Ctrl Pts',(-62.0565861244171,40.4877344164407,0.));
#90627=CARTESIAN_POINT('Ctrl Pts',(-62.0565861244171,40.4877344164407,12.));
#90628=CARTESIAN_POINT('Ctrl Pts',(-62.0836830685665,40.4920425795184,0.));
#90629=CARTESIAN_POINT('Ctrl Pts',(-62.0836830685665,40.4920425795184,12.));
#90630=CARTESIAN_POINT('Ctrl Pts',(-62.110818841691,40.4963316888357,0.));
#90631=CARTESIAN_POINT('Ctrl Pts',(-62.110818841691,40.4963316888357,12.));
#90632=CARTESIAN_POINT('Ctrl Pts',(-62.137993373242,40.5006016927489,0.));
#90633=CARTESIAN_POINT('Ctrl Pts',(-62.137993373242,40.5006016927489,12.));
#90634=CARTESIAN_POINT('Ctrl Pts',(-62.1652065915724,40.5048525385985,0.));
#90635=CARTESIAN_POINT('Ctrl Pts',(-62.1652065915724,40.5048525385985,12.));
#90636=CARTESIAN_POINT('Ctrl Pts',(-62.1924584215634,40.5090841704111,0.));
#90637=CARTESIAN_POINT('Ctrl Pts',(-62.1924584215634,40.5090841704111,12.));
#90638=CARTESIAN_POINT('Ctrl Pts',(-62.2197487826212,40.5132965269679,0.));
#90639=CARTESIAN_POINT('Ctrl Pts',(-62.2197487826212,40.5132965269679,12.));
#90640=CARTESIAN_POINT('Ctrl Pts',(-62.2470775858834,40.5174895391059,0.));
#90641=CARTESIAN_POINT('Ctrl Pts',(-62.2470775858834,40.5174895391059,12.));
#90642=CARTESIAN_POINT('Ctrl Pts',(-62.2744447382207,40.5216631336335,0.));
#90643=CARTESIAN_POINT('Ctrl Pts',(-62.2744447382207,40.5216631336335,12.));
#90644=CARTESIAN_POINT('Ctrl Pts',(-62.3018501471876,40.5258172381565,0.));
#90645=CARTESIAN_POINT('Ctrl Pts',(-62.3018501471876,40.5258172381565,12.));
#90646=CARTESIAN_POINT('Ctrl Pts',(-62.3292937258021,40.5299517857793,0.));
#90647=CARTESIAN_POINT('Ctrl Pts',(-62.3292937258021,40.5299517857793,12.));
#90648=CARTESIAN_POINT('Ctrl Pts',(-62.35677539702,40.5340667194272,0.));
#90649=CARTESIAN_POINT('Ctrl Pts',(-62.35677539702,40.5340667194272,12.));
#90650=CARTESIAN_POINT('Ctrl Pts',(-62.3842950992504,40.5381619973972,0.));
#90651=CARTESIAN_POINT('Ctrl Pts',(-62.3842950992504,40.5381619973972,12.));
#90652=CARTESIAN_POINT('Ctrl Pts',(-62.4118527880601,40.5422375944697,0.));
#90653=CARTESIAN_POINT('Ctrl Pts',(-62.4118527880601,40.5422375944697,12.));
#90654=CARTESIAN_POINT('Ctrl Pts',(-62.439448432904,40.5462934972334,0.));
#90655=CARTESIAN_POINT('Ctrl Pts',(-62.439448432904,40.5462934972334,12.));
#90656=CARTESIAN_POINT('Ctrl Pts',(-62.4615552986669,40.5495224601437,0.));
#90657=CARTESIAN_POINT('Ctrl Pts',(-62.4615552986669,40.5495224601437,12.));
#90658=CARTESIAN_POINT('Ctrl Pts',(-62.4781525155997,40.5519353177058,0.));
#90659=CARTESIAN_POINT('Ctrl Pts',(-62.4781525155997,40.5519353177058,12.));
#90660=CARTESIAN_POINT('Ctrl Pts',(-62.4892249121863,40.5535399497449,0.));
#90661=CARTESIAN_POINT('Ctrl Pts',(-62.4892249121863,40.5535399497449,12.));
#90662=CARTESIAN_POINT('Ctrl Pts',(-62.4947630068039,40.554341280847,0.));
#90663=CARTESIAN_POINT('Ctrl Pts',(-62.4947630068039,40.554341280847,12.));
#90664=CARTESIAN_POINT('',(-57.8261117662438,39.4479504917287,0.));
#90665=CARTESIAN_POINT('Ctrl Pts',(-57.8261117662438,39.4479504917287,0.));
#90666=CARTESIAN_POINT('Ctrl Pts',(-57.8297740100947,39.4492429618443,0.));
#90667=CARTESIAN_POINT('Ctrl Pts',(-57.837104315141,39.4518277003553,0.));
#90668=CARTESIAN_POINT('Ctrl Pts',(-57.8481172247496,39.4557042029652,0.));
#90669=CARTESIAN_POINT('Ctrl Pts',(-57.8628360096803,39.4608716627117,0.));
#90670=CARTESIAN_POINT('Ctrl Pts',(-57.8812926637177,39.4673289592259,0.));
#90671=CARTESIAN_POINT('Ctrl Pts',(-57.8998074670478,39.473784194937,0.));
#90672=CARTESIAN_POINT('Ctrl Pts',(-57.9183803632403,39.4802373061058,0.));
#90673=CARTESIAN_POINT('Ctrl Pts',(-57.937011245663,39.4866881842317,0.));
#90674=CARTESIAN_POINT('Ctrl Pts',(-57.9556999583892,39.4931366776714,0.));
#90675=CARTESIAN_POINT('Ctrl Pts',(-57.974446317937,39.499582610674,0.));
#90676=CARTESIAN_POINT('Ctrl Pts',(-57.9932501298522,39.5060257981225,0.));
#90677=CARTESIAN_POINT('Ctrl Pts',(-58.0121112067895,39.5124660614976,0.));
#90678=CARTESIAN_POINT('Ctrl Pts',(-58.0310293875262,39.5189032457184,0.));
#90679=CARTESIAN_POINT('Ctrl Pts',(-58.0500045308412,39.5253372136887,0.));
#90680=CARTESIAN_POINT('Ctrl Pts',(-58.0690365065374,39.5317678383217,0.));
#90681=CARTESIAN_POINT('Ctrl Pts',(-58.0881251879921,39.5381949959221,0.));
#90682=CARTESIAN_POINT('Ctrl Pts',(-58.1072704428928,39.5446185579638,0.));
#90683=CARTESIAN_POINT('Ctrl Pts',(-58.126472128574,39.5510383869505,0.));
#90684=CARTESIAN_POINT('Ctrl Pts',(-58.1457300968499,39.5574543406982,0.));
#90685=CARTESIAN_POINT('Ctrl Pts',(-58.1650441970387,39.563866275018,0.));
#90686=CARTESIAN_POINT('Ctrl Pts',(-58.1844142794338,39.5702740467999,0.));
#90687=CARTESIAN_POINT('Ctrl Pts',(-58.2038401992457,39.57667751752,0.));
#90688=CARTESIAN_POINT('Ctrl Pts',(-58.2233218164365,39.5830765530891,0.));
#90689=CARTESIAN_POINT('Ctrl Pts',(-58.2428589938369,39.5894710221713,0.));
#90690=CARTESIAN_POINT('Ctrl Pts',(-58.2624515958419,39.5958607950239,0.));
#90691=CARTESIAN_POINT('Ctrl Pts',(-58.2820994868118,39.602245742079,0.));
#90692=CARTESIAN_POINT('Ctrl Pts',(-58.3018025297323,39.6086257327583,0.));
#90693=CARTESIAN_POINT('Ctrl Pts',(-58.3215605869221,39.6150006360914,0.));
#90694=CARTESIAN_POINT('Ctrl Pts',(-58.3413735206423,39.6213703212531,0.));
#90695=CARTESIAN_POINT('Ctrl Pts',(-58.3612411936905,39.6277346580892,0.));
#90696=CARTESIAN_POINT('Ctrl Pts',(-58.3811634701037,39.6340935177476,0.));
#90697=CARTESIAN_POINT('Ctrl Pts',(-58.4011402154196,39.6404467729094,0.));
#90698=CARTESIAN_POINT('Ctrl Pts',(-58.4211712963004,39.6467942974451,0.));
#90699=CARTESIAN_POINT('Ctrl Pts',(-58.4412565802979,39.653135966204,0.));
#90700=CARTESIAN_POINT('Ctrl Pts',(-58.4613959355788,39.6594716547689,0.));
#90701=CARTESIAN_POINT('Ctrl Pts',(-58.4815892306066,39.6658012391815,0.));
#90702=CARTESIAN_POINT('Ctrl Pts',(-58.5018363341604,39.6721245959531,0.));
#90703=CARTESIAN_POINT('Ctrl Pts',(-58.5221371154761,39.6784416021826,0.));
#90704=CARTESIAN_POINT('Ctrl Pts',(-58.5424914443415,39.6847521356395,0.));
#90705=CARTESIAN_POINT('Ctrl Pts',(-58.5628991912052,39.6910560748629,0.));
#90706=CARTESIAN_POINT('Ctrl Pts',(-58.5833602272744,39.6973532992539,0.));
#90707=CARTESIAN_POINT('Ctrl Pts',(-58.6038744244659,39.7036436890233,0.));
#90708=CARTESIAN_POINT('Ctrl Pts',(-58.6244416553562,39.7099271251413,0.));
#90709=CARTESIAN_POINT('Ctrl Pts',(-58.6450617931274,39.7162034892899,0.));
#90710=CARTESIAN_POINT('Ctrl Pts',(-58.6657347115034,39.72247266381,0.));
#90711=CARTESIAN_POINT('Ctrl Pts',(-58.6864602847088,39.7287345316681,0.));
#90712=CARTESIAN_POINT('Ctrl Pts',(-58.7072383875027,39.734988976475,0.));
#90713=CARTESIAN_POINT('Ctrl Pts',(-58.7280688951916,39.7412358824953,0.));
#90714=CARTESIAN_POINT('Ctrl Pts',(-58.7489516836445,39.7474751346598,0.));
#90715=CARTESIAN_POINT('Ctrl Pts',(-58.7698866293029,39.7537066185813,0.));
#90716=CARTESIAN_POINT('Ctrl Pts',(-58.7908736091798,39.7599302205521,0.));
#90717=CARTESIAN_POINT('Ctrl Pts',(-58.8119125008517,39.7661458275274,0.));
#90718=CARTESIAN_POINT('Ctrl Pts',(-58.8330031824453,39.772353327112,0.));
#90719=CARTESIAN_POINT('Ctrl Pts',(-58.8541455326231,39.7785526075478,0.));
#90720=CARTESIAN_POINT('Ctrl Pts',(-58.8753394305585,39.7847435576996,0.));
#90721=CARTESIAN_POINT('Ctrl Pts',(-58.8965847559391,39.7909260670517,0.));
#90722=CARTESIAN_POINT('Ctrl Pts',(-58.9178813889704,39.7971000257044,0.));
#90723=CARTESIAN_POINT('Ctrl Pts',(-58.9392292103747,39.8032653243712,0.));
#90724=CARTESIAN_POINT('Ctrl Pts',(-58.9606281013875,39.8094218543782,0.));
#90725=CARTESIAN_POINT('Ctrl Pts',(-58.9820779437484,39.8155695076626,0.));
#90726=CARTESIAN_POINT('Ctrl Pts',(-59.0035786197024,39.821708176766,0.));
#90727=CARTESIAN_POINT('Ctrl Pts',(-59.0251300119973,39.8278377548262,0.));
#90728=CARTESIAN_POINT('Ctrl Pts',(-59.0467320038784,39.8339581355716,0.));
#90729=CARTESIAN_POINT('Ctrl Pts',(-59.0683844790764,39.8400692133139,0.));
#90730=CARTESIAN_POINT('Ctrl Pts',(-59.090087321798,39.8461708829456,0.));
#90731=CARTESIAN_POINT('Ctrl Pts',(-59.1118404167292,39.8522630399328,0.));
#90732=CARTESIAN_POINT('Ctrl Pts',(-59.1336436490342,39.8583455803105,0.));
#90733=CARTESIAN_POINT('Ctrl Pts',(-59.1554969043522,39.8644184006787,0.));
#90734=CARTESIAN_POINT('Ctrl Pts',(-59.1774000687879,39.8704813981988,0.));
#90735=CARTESIAN_POINT('Ctrl Pts',(-59.1993530289028,39.876534470591,0.));
#90736=CARTESIAN_POINT('Ctrl Pts',(-59.2213556717209,39.8825775161267,0.));
#90737=CARTESIAN_POINT('Ctrl Pts',(-59.2434078847247,39.8886104336242,0.));
#90738=CARTESIAN_POINT('Ctrl Pts',(-59.2655095558521,39.8946331224438,0.));
#90739=CARTESIAN_POINT('Ctrl Pts',(-59.2876605734846,39.9006454824845,0.));
#90740=CARTESIAN_POINT('Ctrl Pts',(-59.3098608264419,39.9066474141803,0.));
#90741=CARTESIAN_POINT('Ctrl Pts',(-59.3321102039852,39.9126388184936,0.));
#90742=CARTESIAN_POINT('Ctrl Pts',(-59.3544085958151,39.9186195969104,0.));
#90743=CARTESIAN_POINT('Ctrl Pts',(-59.3767558920675,39.9245896514367,0.));
#90744=CARTESIAN_POINT('Ctrl Pts',(-59.3991519833016,39.9305488845958,0.));
#90745=CARTESIAN_POINT('Ctrl Pts',(-59.4215967604967,39.9364971994242,0.));
#90746=CARTESIAN_POINT('Ctrl Pts',(-59.4440901150582,39.9424344994672,0.));
#90747=CARTESIAN_POINT('Ctrl Pts',(-59.4666319388133,39.9483606887737,0.));
#90748=CARTESIAN_POINT('Ctrl Pts',(-59.4892221240068,39.9542756718922,0.));
#90749=CARTESIAN_POINT('Ctrl Pts',(-59.5118605632891,39.9601793538682,0.));
#90750=CARTESIAN_POINT('Ctrl Pts',(-59.5345471497129,39.9660716402403,0.));
#90751=CARTESIAN_POINT('Ctrl Pts',(-59.5572817767388,39.9719524370345,0.));
#90752=CARTESIAN_POINT('Ctrl Pts',(-59.5800643382314,39.9778216507605,0.));
#90753=CARTESIAN_POINT('Ctrl Pts',(-59.6028947284562,39.9836791884079,0.));
#90754=CARTESIAN_POINT('Ctrl Pts',(-59.6257728420669,39.9895249574448,0.));
#90755=CARTESIAN_POINT('Ctrl Pts',(-59.6486985741041,39.9953588658132,0.));
#90756=CARTESIAN_POINT('Ctrl Pts',(-59.6716718200005,40.0011808219241,0.));
#90757=CARTESIAN_POINT('Ctrl Pts',(-59.6946924755773,40.0069907346537,0.));
#90758=CARTESIAN_POINT('Ctrl Pts',(-59.7177604370403,40.0127885133403,0.));
#90759=CARTESIAN_POINT('Ctrl Pts',(-59.7408756009679,40.0185740677821,0.));
#90760=CARTESIAN_POINT('Ctrl Pts',(-59.7640378643106,40.0243473082337,0.));
#90761=CARTESIAN_POINT('Ctrl Pts',(-59.7872471243942,40.0301081454002,0.));
#90762=CARTESIAN_POINT('Ctrl Pts',(-59.8105032789179,40.035856490434,0.));
#90763=CARTESIAN_POINT('Ctrl Pts',(-59.8338062259492,40.0415922549315,0.));
#90764=CARTESIAN_POINT('Ctrl Pts',(-59.8571558639145,40.0473153509324,0.));
#90765=CARTESIAN_POINT('Ctrl Pts',(-59.8805520915972,40.0530256909161,0.));
#90766=CARTESIAN_POINT('Ctrl Pts',(-59.9039948081428,40.0587231877959,0.));
#90767=CARTESIAN_POINT('Ctrl Pts',(-59.927483913055,40.0644077549158,0.));
#90768=CARTESIAN_POINT('Ctrl Pts',(-59.9510193061929,40.0700793060475,0.));
#90769=CARTESIAN_POINT('Ctrl Pts',(-59.974600887759,40.0757377553893,0.));
#90770=CARTESIAN_POINT('Ctrl Pts',(-59.9982285582991,40.0813830175629,0.));
#90771=CARTESIAN_POINT('Ctrl Pts',(-60.0219022187066,40.0870150076078,0.));
#90772=CARTESIAN_POINT('Ctrl Pts',(-60.0456217702203,40.0926336409787,0.));
#90773=CARTESIAN_POINT('Ctrl Pts',(-60.0693871144207,40.0982388335421,0.));
#90774=CARTESIAN_POINT('Ctrl Pts',(-60.0931981532194,40.1038305015763,0.));
#90775=CARTESIAN_POINT('Ctrl Pts',(-60.1170547888572,40.1094085617672,0.));
#90776=CARTESIAN_POINT('Ctrl Pts',(-60.1409569239093,40.1149729312036,0.));
#90777=CARTESIAN_POINT('Ctrl Pts',(-60.1649044612829,40.120523527374,0.));
#90778=CARTESIAN_POINT('Ctrl Pts',(-60.1888973042151,40.1260602681644,0.));
#90779=CARTESIAN_POINT('Ctrl Pts',(-60.2129353562617,40.1315830718575,0.));
#90780=CARTESIAN_POINT('Ctrl Pts',(-60.2370185212957,40.13709185713,0.));
#90781=CARTESIAN_POINT('Ctrl Pts',(-60.2611467035109,40.1425865430468,0.));
#90782=CARTESIAN_POINT('Ctrl Pts',(-60.2853198074215,40.1480670490583,0.));
#90783=CARTESIAN_POINT('Ctrl Pts',(-60.3095377378589,40.1535332949978,0.));
#90784=CARTESIAN_POINT('Ctrl Pts',(-60.3338003999616,40.1589852010811,0.));
#90785=CARTESIAN_POINT('Ctrl Pts',(-60.3581076991731,40.1644226879043,0.));
#90786=CARTESIAN_POINT('Ctrl Pts',(-60.382459541246,40.1698456764387,0.));
#90787=CARTESIAN_POINT('Ctrl Pts',(-60.4068558322415,40.1752540880273,0.));
#90788=CARTESIAN_POINT('Ctrl Pts',(-60.4312964785269,40.1806478443828,0.));
#90789=CARTESIAN_POINT('Ctrl Pts',(-60.4557813867677,40.1860268675875,0.));
#90790=CARTESIAN_POINT('Ctrl Pts',(-60.4803104639211,40.1913910800911,0.));
#90791=CARTESIAN_POINT('Ctrl Pts',(-60.5048836172424,40.1967404047055,0.));
#90792=CARTESIAN_POINT('Ctrl Pts',(-60.5295007542838,40.2020747646012,0.));
#90793=CARTESIAN_POINT('Ctrl Pts',(-60.5541617828927,40.2073940833054,0.));
#90794=CARTESIAN_POINT('Ctrl Pts',(-60.5788666112043,40.2126982847012,0.));
#90795=CARTESIAN_POINT('Ctrl Pts',(-60.6036151476347,40.2179872930272,0.));
#90796=CARTESIAN_POINT('Ctrl Pts',(-60.6284073008865,40.2232610328717,0.));
#90797=CARTESIAN_POINT('Ctrl Pts',(-60.6532429799493,40.2285194291702,0.));
#90798=CARTESIAN_POINT('Ctrl Pts',(-60.678122094098,40.2337624072029,0.));
#90799=CARTESIAN_POINT('Ctrl Pts',(-60.7030445528863,40.2389898925937,0.));
#90800=CARTESIAN_POINT('Ctrl Pts',(-60.72801026614,40.2442018113116,0.));
#90801=CARTESIAN_POINT('Ctrl Pts',(-60.7530191439603,40.2493980896646,0.));
#90802=CARTESIAN_POINT('Ctrl Pts',(-60.7780710967253,40.2545786542957,0.));
#90803=CARTESIAN_POINT('Ctrl Pts',(-60.8031660350879,40.2597434321804,0.));
#90804=CARTESIAN_POINT('Ctrl Pts',(-60.8283038699703,40.2648923506245,0.));
#90805=CARTESIAN_POINT('Ctrl Pts',(-60.8534845125535,40.2700253372644,0.));
#90806=CARTESIAN_POINT('Ctrl Pts',(-60.8787078742817,40.2751423200637,0.));
#90807=CARTESIAN_POINT('Ctrl Pts',(-60.903973866867,40.2802432273105,0.));
#90808=CARTESIAN_POINT('Ctrl Pts',(-60.9292824022888,40.2853279876162,0.));
#90809=CARTESIAN_POINT('Ctrl Pts',(-60.9546333927919,40.2903965299155,0.));
#90810=CARTESIAN_POINT('Ctrl Pts',(-60.9800267508781,40.2954487834688,0.));
#90811=CARTESIAN_POINT('Ctrl Pts',(-61.005462389306,40.3004846778577,0.));
#90812=CARTESIAN_POINT('Ctrl Pts',(-61.0309402210915,40.3055041429772,0.));
#90813=CARTESIAN_POINT('Ctrl Pts',(-61.0564601595047,40.3105071090308,0.));
#90814=CARTESIAN_POINT('Ctrl Pts',(-61.0820221180646,40.3154935065264,0.));
#90815=CARTESIAN_POINT('Ctrl Pts',(-61.1076260105265,40.3204632662729,0.));
#90816=CARTESIAN_POINT('Ctrl Pts',(-61.1332717508799,40.3254163193806,0.));
#90817=CARTESIAN_POINT('Ctrl Pts',(-61.1589592533623,40.3303525972621,0.));
#90818=CARTESIAN_POINT('Ctrl Pts',(-61.184688432465,40.3352720316373,0.));
#90819=CARTESIAN_POINT('Ctrl Pts',(-61.2104592029375,40.3401745545369,0.));
#90820=CARTESIAN_POINT('Ctrl Pts',(-61.236271479789,40.3450600983104,0.));
#90821=CARTESIAN_POINT('Ctrl Pts',(-61.2621251782849,40.3499285956297,0.));
#90822=CARTESIAN_POINT('Ctrl Pts',(-61.2880202139358,40.3547799794672,0.));
#90823=CARTESIAN_POINT('Ctrl Pts',(-61.3139565024838,40.3596141830786,0.));
#90824=CARTESIAN_POINT('Ctrl Pts',(-61.3399339598851,40.3644311399861,0.));
#90825=CARTESIAN_POINT('Ctrl Pts',(-61.3659525022917,40.3692307839642,0.));
#90826=CARTESIAN_POINT('Ctrl Pts',(-61.3920120460232,40.3740130490233,0.));
#90827=CARTESIAN_POINT('Ctrl Pts',(-61.418112507605,40.3787778694373,0.));
#90828=CARTESIAN_POINT('Ctrl Pts',(-61.4442538038053,40.3835251797725,0.));
#90829=CARTESIAN_POINT('Ctrl Pts',(-61.4704358516711,40.3882549149229,0.));
#90830=CARTESIAN_POINT('Ctrl Pts',(-61.4966585685544,40.3929670101363,0.));
#90831=CARTESIAN_POINT('Ctrl Pts',(-61.5229218721532,40.3976614010648,0.));
#90832=CARTESIAN_POINT('Ctrl Pts',(-61.5492256804709,40.4023380237227,0.));
#90833=CARTESIAN_POINT('Ctrl Pts',(-61.5755699117318,40.4069968143953,0.));
#90834=CARTESIAN_POINT('Ctrl Pts',(-61.6019544843009,40.4116377095595,0.));
#90835=CARTESIAN_POINT('Ctrl Pts',(-61.628379316608,40.4162606458119,0.));
#90836=CARTESIAN_POINT('Ctrl Pts',(-61.6548443270397,40.420865559772,0.));
#90837=CARTESIAN_POINT('Ctrl Pts',(-61.6813494339295,40.4254523880766,0.));
#90838=CARTESIAN_POINT('Ctrl Pts',(-61.7078945557812,40.4300210675848,0.));
#90839=CARTESIAN_POINT('Ctrl Pts',(-61.7344796114409,40.4345715355411,0.));
#90840=CARTESIAN_POINT('Ctrl Pts',(-61.7611045202875,40.439103729759,0.));
#90841=CARTESIAN_POINT('Ctrl Pts',(-61.7877692024064,40.4436175887942,0.));
#90842=CARTESIAN_POINT('Ctrl Pts',(-61.8144735787767,40.448113052135,0.));
#90843=CARTESIAN_POINT('Ctrl Pts',(-61.8412175708524,40.4525900597877,0.));
#90844=CARTESIAN_POINT('Ctrl Pts',(-61.8680011001513,40.4570485518735,0.));
#90845=CARTESIAN_POINT('Ctrl Pts',(-61.8948240877998,40.4614884681884,0.));
#90846=CARTESIAN_POINT('Ctrl Pts',(-61.9216864541758,40.4659097478595,0.));
#90847=CARTESIAN_POINT('Ctrl Pts',(-61.9485881182957,40.4703123287642,0.));
#90848=CARTESIAN_POINT('Ctrl Pts',(-61.9755289983094,40.4746961480045,0.));
#90849=CARTESIAN_POINT('Ctrl Pts',(-62.0025090126008,40.4790611429613,0.));
#90850=CARTESIAN_POINT('Ctrl Pts',(-62.0295280807449,40.4834072522181,0.));
#90851=CARTESIAN_POINT('Ctrl Pts',(-62.0565861244171,40.4877344164407,0.));
#90852=CARTESIAN_POINT('Ctrl Pts',(-62.0836830685665,40.4920425795184,0.));
#90853=CARTESIAN_POINT('Ctrl Pts',(-62.110818841691,40.4963316888357,0.));
#90854=CARTESIAN_POINT('Ctrl Pts',(-62.1341126810364,40.499991909619,0.));
#90855=CARTESIAN_POINT('Ctrl Pts',(-62.1519925002737,40.5027877865724,0.));
#90856=CARTESIAN_POINT('Ctrl Pts',(-62.1644411502531,40.5047277935688,0.));
#90857=CARTESIAN_POINT('Ctrl Pts',(-62.1714473137753,40.5058175523045,0.));
#90858=CARTESIAN_POINT('Ctrl Pts',(-62.1730054756455,40.5060598100838,0.));
#90859=CARTESIAN_POINT('',(-57.8261117662438,39.4479504917287,12.));
#90860=CARTESIAN_POINT('',(-57.8261117662438,39.4479504917287,0.));
#90861=CARTESIAN_POINT('Ctrl Pts',(-62.1730054756454,40.5060598100838,12.));
#90862=CARTESIAN_POINT('Ctrl Pts',(-62.1714473137753,40.5058175523045,12.));
#90863=CARTESIAN_POINT('Ctrl Pts',(-62.1644411502531,40.5047277935688,12.));
#90864=CARTESIAN_POINT('Ctrl Pts',(-62.1519925002737,40.5027877865724,12.));
#90865=CARTESIAN_POINT('Ctrl Pts',(-62.1341126810364,40.499991909619,12.));
#90866=CARTESIAN_POINT('Ctrl Pts',(-62.110818841691,40.4963316888357,12.));
#90867=CARTESIAN_POINT('Ctrl Pts',(-62.0836830685665,40.4920425795184,12.));
#90868=CARTESIAN_POINT('Ctrl Pts',(-62.0565861244171,40.4877344164407,12.));
#90869=CARTESIAN_POINT('Ctrl Pts',(-62.0295280807449,40.4834072522181,12.));
#90870=CARTESIAN_POINT('Ctrl Pts',(-62.0025090126008,40.4790611429613,12.));
#90871=CARTESIAN_POINT('Ctrl Pts',(-61.9755289983094,40.4746961480045,12.));
#90872=CARTESIAN_POINT('Ctrl Pts',(-61.9485881182957,40.4703123287642,12.));
#90873=CARTESIAN_POINT('Ctrl Pts',(-61.9216864541758,40.4659097478595,12.));
#90874=CARTESIAN_POINT('Ctrl Pts',(-61.8948240877998,40.4614884681884,12.));
#90875=CARTESIAN_POINT('Ctrl Pts',(-61.8680011001513,40.4570485518735,12.));
#90876=CARTESIAN_POINT('Ctrl Pts',(-61.8412175708524,40.4525900597877,12.));
#90877=CARTESIAN_POINT('Ctrl Pts',(-61.8144735787767,40.448113052135,12.));
#90878=CARTESIAN_POINT('Ctrl Pts',(-61.7877692024064,40.4436175887942,12.));
#90879=CARTESIAN_POINT('Ctrl Pts',(-61.7611045202875,40.439103729759,12.));
#90880=CARTESIAN_POINT('Ctrl Pts',(-61.7344796114409,40.4345715355411,12.));
#90881=CARTESIAN_POINT('Ctrl Pts',(-61.7078945557812,40.4300210675848,12.));
#90882=CARTESIAN_POINT('Ctrl Pts',(-61.6813494339295,40.4254523880766,12.));
#90883=CARTESIAN_POINT('Ctrl Pts',(-61.6548443270397,40.420865559772,12.));
#90884=CARTESIAN_POINT('Ctrl Pts',(-61.628379316608,40.4162606458119,12.));
#90885=CARTESIAN_POINT('Ctrl Pts',(-61.6019544843009,40.4116377095595,12.));
#90886=CARTESIAN_POINT('Ctrl Pts',(-61.5755699117318,40.4069968143953,12.));
#90887=CARTESIAN_POINT('Ctrl Pts',(-61.5492256804709,40.4023380237227,12.));
#90888=CARTESIAN_POINT('Ctrl Pts',(-61.5229218721532,40.3976614010648,12.));
#90889=CARTESIAN_POINT('Ctrl Pts',(-61.4966585685544,40.3929670101363,12.));
#90890=CARTESIAN_POINT('Ctrl Pts',(-61.4704358516711,40.3882549149229,12.));
#90891=CARTESIAN_POINT('Ctrl Pts',(-61.4442538038053,40.3835251797725,12.));
#90892=CARTESIAN_POINT('Ctrl Pts',(-61.418112507605,40.3787778694373,12.));
#90893=CARTESIAN_POINT('Ctrl Pts',(-61.3920120460232,40.3740130490233,12.));
#90894=CARTESIAN_POINT('Ctrl Pts',(-61.3659525022917,40.3692307839642,12.));
#90895=CARTESIAN_POINT('Ctrl Pts',(-61.3399339598851,40.3644311399861,12.));
#90896=CARTESIAN_POINT('Ctrl Pts',(-61.3139565024838,40.3596141830786,12.));
#90897=CARTESIAN_POINT('Ctrl Pts',(-61.2880202139358,40.3547799794672,12.));
#90898=CARTESIAN_POINT('Ctrl Pts',(-61.2621251782849,40.3499285956297,12.));
#90899=CARTESIAN_POINT('Ctrl Pts',(-61.236271479789,40.3450600983104,12.));
#90900=CARTESIAN_POINT('Ctrl Pts',(-61.2104592029375,40.3401745545369,12.));
#90901=CARTESIAN_POINT('Ctrl Pts',(-61.184688432465,40.3352720316373,12.));
#90902=CARTESIAN_POINT('Ctrl Pts',(-61.1589592533623,40.3303525972621,12.));
#90903=CARTESIAN_POINT('Ctrl Pts',(-61.1332717508799,40.3254163193806,12.));
#90904=CARTESIAN_POINT('Ctrl Pts',(-61.1076260105265,40.3204632662729,12.));
#90905=CARTESIAN_POINT('Ctrl Pts',(-61.0820221180646,40.3154935065264,12.));
#90906=CARTESIAN_POINT('Ctrl Pts',(-61.0564601595047,40.3105071090308,12.));
#90907=CARTESIAN_POINT('Ctrl Pts',(-61.0309402210915,40.3055041429772,12.));
#90908=CARTESIAN_POINT('Ctrl Pts',(-61.005462389306,40.3004846778577,12.));
#90909=CARTESIAN_POINT('Ctrl Pts',(-60.9800267508781,40.2954487834688,12.));
#90910=CARTESIAN_POINT('Ctrl Pts',(-60.9546333927919,40.2903965299155,12.));
#90911=CARTESIAN_POINT('Ctrl Pts',(-60.9292824022888,40.2853279876162,12.));
#90912=CARTESIAN_POINT('Ctrl Pts',(-60.903973866867,40.2802432273105,12.));
#90913=CARTESIAN_POINT('Ctrl Pts',(-60.8787078742817,40.2751423200637,12.));
#90914=CARTESIAN_POINT('Ctrl Pts',(-60.8534845125535,40.2700253372644,12.));
#90915=CARTESIAN_POINT('Ctrl Pts',(-60.8283038699703,40.2648923506245,12.));
#90916=CARTESIAN_POINT('Ctrl Pts',(-60.8031660350879,40.2597434321804,12.));
#90917=CARTESIAN_POINT('Ctrl Pts',(-60.7780710967253,40.2545786542957,12.));
#90918=CARTESIAN_POINT('Ctrl Pts',(-60.7530191439603,40.2493980896646,12.));
#90919=CARTESIAN_POINT('Ctrl Pts',(-60.72801026614,40.2442018113116,12.));
#90920=CARTESIAN_POINT('Ctrl Pts',(-60.7030445528863,40.2389898925937,12.));
#90921=CARTESIAN_POINT('Ctrl Pts',(-60.678122094098,40.2337624072029,12.));
#90922=CARTESIAN_POINT('Ctrl Pts',(-60.6532429799493,40.2285194291702,12.));
#90923=CARTESIAN_POINT('Ctrl Pts',(-60.6284073008865,40.2232610328717,12.));
#90924=CARTESIAN_POINT('Ctrl Pts',(-60.6036151476347,40.2179872930272,12.));
#90925=CARTESIAN_POINT('Ctrl Pts',(-60.5788666112043,40.2126982847012,12.));
#90926=CARTESIAN_POINT('Ctrl Pts',(-60.5541617828927,40.2073940833054,12.));
#90927=CARTESIAN_POINT('Ctrl Pts',(-60.5295007542838,40.2020747646012,12.));
#90928=CARTESIAN_POINT('Ctrl Pts',(-60.5048836172424,40.1967404047055,12.));
#90929=CARTESIAN_POINT('Ctrl Pts',(-60.4803104639211,40.1913910800911,12.));
#90930=CARTESIAN_POINT('Ctrl Pts',(-60.4557813867677,40.1860268675875,12.));
#90931=CARTESIAN_POINT('Ctrl Pts',(-60.4312964785269,40.1806478443828,12.));
#90932=CARTESIAN_POINT('Ctrl Pts',(-60.4068558322415,40.1752540880273,12.));
#90933=CARTESIAN_POINT('Ctrl Pts',(-60.382459541246,40.1698456764387,12.));
#90934=CARTESIAN_POINT('Ctrl Pts',(-60.3581076991731,40.1644226879043,12.));
#90935=CARTESIAN_POINT('Ctrl Pts',(-60.3338003999616,40.1589852010811,12.));
#90936=CARTESIAN_POINT('Ctrl Pts',(-60.3095377378589,40.1535332949978,12.));
#90937=CARTESIAN_POINT('Ctrl Pts',(-60.2853198074215,40.1480670490583,12.));
#90938=CARTESIAN_POINT('Ctrl Pts',(-60.2611467035109,40.1425865430468,12.));
#90939=CARTESIAN_POINT('Ctrl Pts',(-60.2370185212957,40.13709185713,12.));
#90940=CARTESIAN_POINT('Ctrl Pts',(-60.2129353562617,40.1315830718575,12.));
#90941=CARTESIAN_POINT('Ctrl Pts',(-60.1888973042151,40.1260602681644,12.));
#90942=CARTESIAN_POINT('Ctrl Pts',(-60.1649044612829,40.120523527374,12.));
#90943=CARTESIAN_POINT('Ctrl Pts',(-60.1409569239093,40.1149729312036,12.));
#90944=CARTESIAN_POINT('Ctrl Pts',(-60.1170547888572,40.1094085617672,12.));
#90945=CARTESIAN_POINT('Ctrl Pts',(-60.0931981532194,40.1038305015763,12.));
#90946=CARTESIAN_POINT('Ctrl Pts',(-60.0693871144207,40.0982388335421,12.));
#90947=CARTESIAN_POINT('Ctrl Pts',(-60.0456217702203,40.0926336409787,12.));
#90948=CARTESIAN_POINT('Ctrl Pts',(-60.0219022187066,40.0870150076078,12.));
#90949=CARTESIAN_POINT('Ctrl Pts',(-59.9982285582991,40.0813830175629,12.));
#90950=CARTESIAN_POINT('Ctrl Pts',(-59.974600887759,40.0757377553893,12.));
#90951=CARTESIAN_POINT('Ctrl Pts',(-59.9510193061929,40.0700793060475,12.));
#90952=CARTESIAN_POINT('Ctrl Pts',(-59.927483913055,40.0644077549158,12.));
#90953=CARTESIAN_POINT('Ctrl Pts',(-59.9039948081428,40.0587231877959,12.));
#90954=CARTESIAN_POINT('Ctrl Pts',(-59.8805520915972,40.0530256909161,12.));
#90955=CARTESIAN_POINT('Ctrl Pts',(-59.8571558639145,40.0473153509324,12.));
#90956=CARTESIAN_POINT('Ctrl Pts',(-59.8338062259492,40.0415922549315,12.));
#90957=CARTESIAN_POINT('Ctrl Pts',(-59.8105032789179,40.035856490434,12.));
#90958=CARTESIAN_POINT('Ctrl Pts',(-59.7872471243942,40.0301081454002,12.));
#90959=CARTESIAN_POINT('Ctrl Pts',(-59.7640378643106,40.0243473082337,12.));
#90960=CARTESIAN_POINT('Ctrl Pts',(-59.7408756009679,40.0185740677821,12.));
#90961=CARTESIAN_POINT('Ctrl Pts',(-59.7177604370403,40.0127885133403,12.));
#90962=CARTESIAN_POINT('Ctrl Pts',(-59.6946924755773,40.0069907346537,12.));
#90963=CARTESIAN_POINT('Ctrl Pts',(-59.6716718200005,40.0011808219241,12.));
#90964=CARTESIAN_POINT('Ctrl Pts',(-59.6486985741041,39.9953588658132,12.));
#90965=CARTESIAN_POINT('Ctrl Pts',(-59.6257728420669,39.9895249574448,12.));
#90966=CARTESIAN_POINT('Ctrl Pts',(-59.6028947284562,39.9836791884079,12.));
#90967=CARTESIAN_POINT('Ctrl Pts',(-59.5800643382314,39.9778216507605,12.));
#90968=CARTESIAN_POINT('Ctrl Pts',(-59.5572817767388,39.9719524370345,12.));
#90969=CARTESIAN_POINT('Ctrl Pts',(-59.5345471497129,39.9660716402403,12.));
#90970=CARTESIAN_POINT('Ctrl Pts',(-59.5118605632891,39.9601793538682,12.));
#90971=CARTESIAN_POINT('Ctrl Pts',(-59.4892221240068,39.9542756718922,12.));
#90972=CARTESIAN_POINT('Ctrl Pts',(-59.4666319388133,39.9483606887737,12.));
#90973=CARTESIAN_POINT('Ctrl Pts',(-59.4440901150582,39.9424344994672,12.));
#90974=CARTESIAN_POINT('Ctrl Pts',(-59.4215967604967,39.9364971994242,12.));
#90975=CARTESIAN_POINT('Ctrl Pts',(-59.3991519833016,39.9305488845958,12.));
#90976=CARTESIAN_POINT('Ctrl Pts',(-59.3767558920675,39.9245896514367,12.));
#90977=CARTESIAN_POINT('Ctrl Pts',(-59.3544085958151,39.9186195969104,12.));
#90978=CARTESIAN_POINT('Ctrl Pts',(-59.3321102039852,39.9126388184936,12.));
#90979=CARTESIAN_POINT('Ctrl Pts',(-59.3098608264419,39.9066474141803,12.));
#90980=CARTESIAN_POINT('Ctrl Pts',(-59.2876605734846,39.9006454824845,12.));
#90981=CARTESIAN_POINT('Ctrl Pts',(-59.2655095558521,39.8946331224438,12.));
#90982=CARTESIAN_POINT('Ctrl Pts',(-59.2434078847247,39.8886104336242,12.));
#90983=CARTESIAN_POINT('Ctrl Pts',(-59.2213556717209,39.8825775161267,12.));
#90984=CARTESIAN_POINT('Ctrl Pts',(-59.1993530289028,39.876534470591,12.));
#90985=CARTESIAN_POINT('Ctrl Pts',(-59.1774000687879,39.8704813981988,12.));
#90986=CARTESIAN_POINT('Ctrl Pts',(-59.1554969043522,39.8644184006787,12.));
#90987=CARTESIAN_POINT('Ctrl Pts',(-59.1336436490342,39.8583455803105,12.));
#90988=CARTESIAN_POINT('Ctrl Pts',(-59.1118404167292,39.8522630399328,12.));
#90989=CARTESIAN_POINT('Ctrl Pts',(-59.090087321798,39.8461708829456,12.));
#90990=CARTESIAN_POINT('Ctrl Pts',(-59.0683844790764,39.8400692133139,12.));
#90991=CARTESIAN_POINT('Ctrl Pts',(-59.0467320038784,39.8339581355716,12.));
#90992=CARTESIAN_POINT('Ctrl Pts',(-59.0251300119973,39.8278377548262,12.));
#90993=CARTESIAN_POINT('Ctrl Pts',(-59.0035786197024,39.821708176766,12.));
#90994=CARTESIAN_POINT('Ctrl Pts',(-58.9820779437484,39.8155695076626,12.));
#90995=CARTESIAN_POINT('Ctrl Pts',(-58.9606281013875,39.8094218543782,12.));
#90996=CARTESIAN_POINT('Ctrl Pts',(-58.9392292103747,39.8032653243712,12.));
#90997=CARTESIAN_POINT('Ctrl Pts',(-58.9178813889704,39.7971000257044,12.));
#90998=CARTESIAN_POINT('Ctrl Pts',(-58.8965847559391,39.7909260670517,12.));
#90999=CARTESIAN_POINT('Ctrl Pts',(-58.8753394305585,39.7847435576996,12.));
#91000=CARTESIAN_POINT('Ctrl Pts',(-58.8541455326231,39.7785526075478,12.));
#91001=CARTESIAN_POINT('Ctrl Pts',(-58.8330031824453,39.772353327112,12.));
#91002=CARTESIAN_POINT('Ctrl Pts',(-58.8119125008517,39.7661458275274,12.));
#91003=CARTESIAN_POINT('Ctrl Pts',(-58.7908736091798,39.7599302205521,12.));
#91004=CARTESIAN_POINT('Ctrl Pts',(-58.7698866293029,39.7537066185813,12.));
#91005=CARTESIAN_POINT('Ctrl Pts',(-58.7489516836445,39.7474751346598,12.));
#91006=CARTESIAN_POINT('Ctrl Pts',(-58.7280688951916,39.7412358824953,12.));
#91007=CARTESIAN_POINT('Ctrl Pts',(-58.7072383875027,39.734988976475,12.));
#91008=CARTESIAN_POINT('Ctrl Pts',(-58.6864602847088,39.7287345316681,12.));
#91009=CARTESIAN_POINT('Ctrl Pts',(-58.6657347115034,39.72247266381,12.));
#91010=CARTESIAN_POINT('Ctrl Pts',(-58.6450617931274,39.7162034892899,12.));
#91011=CARTESIAN_POINT('Ctrl Pts',(-58.6244416553562,39.7099271251413,12.));
#91012=CARTESIAN_POINT('Ctrl Pts',(-58.6038744244659,39.7036436890233,12.));
#91013=CARTESIAN_POINT('Ctrl Pts',(-58.5833602272744,39.6973532992539,12.));
#91014=CARTESIAN_POINT('Ctrl Pts',(-58.5628991912052,39.6910560748629,12.));
#91015=CARTESIAN_POINT('Ctrl Pts',(-58.5424914443415,39.6847521356395,12.));
#91016=CARTESIAN_POINT('Ctrl Pts',(-58.5221371154761,39.6784416021826,12.));
#91017=CARTESIAN_POINT('Ctrl Pts',(-58.5018363341604,39.6721245959531,12.));
#91018=CARTESIAN_POINT('Ctrl Pts',(-58.4815892306066,39.6658012391815,12.));
#91019=CARTESIAN_POINT('Ctrl Pts',(-58.4613959355788,39.6594716547689,12.));
#91020=CARTESIAN_POINT('Ctrl Pts',(-58.4412565802979,39.653135966204,12.));
#91021=CARTESIAN_POINT('Ctrl Pts',(-58.4211712963004,39.6467942974451,12.));
#91022=CARTESIAN_POINT('Ctrl Pts',(-58.4011402154196,39.6404467729094,12.));
#91023=CARTESIAN_POINT('Ctrl Pts',(-58.3811634701037,39.6340935177476,12.));
#91024=CARTESIAN_POINT('Ctrl Pts',(-58.3612411936905,39.6277346580892,12.));
#91025=CARTESIAN_POINT('Ctrl Pts',(-58.3413735206423,39.6213703212531,12.));
#91026=CARTESIAN_POINT('Ctrl Pts',(-58.3215605869221,39.6150006360914,12.));
#91027=CARTESIAN_POINT('Ctrl Pts',(-58.3018025297323,39.6086257327583,12.));
#91028=CARTESIAN_POINT('Ctrl Pts',(-58.2820994868118,39.602245742079,12.));
#91029=CARTESIAN_POINT('Ctrl Pts',(-58.2624515958419,39.5958607950239,12.));
#91030=CARTESIAN_POINT('Ctrl Pts',(-58.2428589938369,39.5894710221713,12.));
#91031=CARTESIAN_POINT('Ctrl Pts',(-58.2233218164365,39.5830765530891,12.));
#91032=CARTESIAN_POINT('Ctrl Pts',(-58.2038401992457,39.57667751752,12.));
#91033=CARTESIAN_POINT('Ctrl Pts',(-58.1844142794338,39.5702740467999,12.));
#91034=CARTESIAN_POINT('Ctrl Pts',(-58.1650441970387,39.563866275018,12.));
#91035=CARTESIAN_POINT('Ctrl Pts',(-58.1457300968499,39.5574543406982,12.));
#91036=CARTESIAN_POINT('Ctrl Pts',(-58.126472128574,39.5510383869505,12.));
#91037=CARTESIAN_POINT('Ctrl Pts',(-58.1072704428928,39.5446185579638,12.));
#91038=CARTESIAN_POINT('Ctrl Pts',(-58.0881251879921,39.5381949959221,12.));
#91039=CARTESIAN_POINT('Ctrl Pts',(-58.0690365065374,39.5317678383217,12.));
#91040=CARTESIAN_POINT('Ctrl Pts',(-58.0500045308412,39.5253372136887,12.));
#91041=CARTESIAN_POINT('Ctrl Pts',(-58.0310293875262,39.5189032457184,12.));
#91042=CARTESIAN_POINT('Ctrl Pts',(-58.0121112067895,39.5124660614976,12.));
#91043=CARTESIAN_POINT('Ctrl Pts',(-57.9932501298522,39.5060257981225,12.));
#91044=CARTESIAN_POINT('Ctrl Pts',(-57.974446317937,39.499582610674,12.));
#91045=CARTESIAN_POINT('Ctrl Pts',(-57.9556999583892,39.4931366776714,12.));
#91046=CARTESIAN_POINT('Ctrl Pts',(-57.937011245663,39.4866881842317,12.));
#91047=CARTESIAN_POINT('Ctrl Pts',(-57.9183803632403,39.4802373061058,12.));
#91048=CARTESIAN_POINT('Ctrl Pts',(-57.8998074670478,39.473784194937,12.));
#91049=CARTESIAN_POINT('Ctrl Pts',(-57.8812926637177,39.4673289592259,12.));
#91050=CARTESIAN_POINT('Ctrl Pts',(-57.8628360096803,39.4608716627117,12.));
#91051=CARTESIAN_POINT('Ctrl Pts',(-57.8481172247496,39.4557042029652,12.));
#91052=CARTESIAN_POINT('Ctrl Pts',(-57.837104315141,39.4518277003553,12.));
#91053=CARTESIAN_POINT('Ctrl Pts',(-57.8297740100947,39.4492429618443,12.));
#91054=CARTESIAN_POINT('Ctrl Pts',(-57.8261117662438,39.4479504917287,12.));
#91055=CARTESIAN_POINT('Ctrl Pts',(-62.9864049293893,39.2292784191812,0.));
#91056=CARTESIAN_POINT('Ctrl Pts',(-62.9864049293893,39.2292784191812,4.));
#91057=CARTESIAN_POINT('Ctrl Pts',(-62.9864049293894,39.2292784191812,8.));
#91058=CARTESIAN_POINT('Ctrl Pts',(-62.9864049293894,39.2292784191812,12.));
#91059=CARTESIAN_POINT('Ctrl Pts',(-63.0475916539464,39.3205491216485,0.));
#91060=CARTESIAN_POINT('Ctrl Pts',(-63.0475916539464,39.3205491216485,4.));
#91061=CARTESIAN_POINT('Ctrl Pts',(-63.0475916539464,39.3205491216485,8.));
#91062=CARTESIAN_POINT('Ctrl Pts',(-63.0475916539464,39.3205491216485,12.));
#91063=CARTESIAN_POINT('Ctrl Pts',(-63.0996457958585,39.5164137621549,0.));
#91064=CARTESIAN_POINT('Ctrl Pts',(-63.0996457958585,39.5164137621549,4.00000000000001));
#91065=CARTESIAN_POINT('Ctrl Pts',(-63.0996457958585,39.516413762155,7.99999999999999));
#91066=CARTESIAN_POINT('Ctrl Pts',(-63.0996457958585,39.516413762155,12.));
#91067=CARTESIAN_POINT('Ctrl Pts',(-63.0378706912077,39.7049575044677,0.));
#91068=CARTESIAN_POINT('Ctrl Pts',(-63.0378706912077,39.7049575044677,4.));
#91069=CARTESIAN_POINT('Ctrl Pts',(-63.0378706912076,39.7049575044677,8.00000000000001));
#91070=CARTESIAN_POINT('Ctrl Pts',(-63.0378706912076,39.7049575044677,12.));
#91071=CARTESIAN_POINT('Ctrl Pts',(-62.9938720098783,39.774641283148,0.));
#91072=CARTESIAN_POINT('Ctrl Pts',(-62.9938720098783,39.774641283148,4.));
#91073=CARTESIAN_POINT('Ctrl Pts',(-62.9938720098783,39.774641283148,8.));
#91074=CARTESIAN_POINT('Ctrl Pts',(-62.9938720098783,39.774641283148,12.));
#91075=CARTESIAN_POINT('',(-62.9864049293893,39.2292784191812,0.));
#91076=CARTESIAN_POINT('',(-62.9938720098781,39.7746412831479,0.));
#91077=CARTESIAN_POINT('Ctrl Pts',(-62.9864049293893,39.2292784191812,2.77555756156289E-16));
#91078=CARTESIAN_POINT('Ctrl Pts',(-63.0475916539464,39.3205491216485,2.77555756156289E-16));
#91079=CARTESIAN_POINT('Ctrl Pts',(-63.0773368778962,39.4324717733665,2.77555756156289E-16));
#91080=CARTESIAN_POINT('Ctrl Pts',(-63.0699133682744,39.5420039277151,2.77555756156289E-16));
#91081=CARTESIAN_POINT('Ctrl Pts',(-63.064345736058,39.6241530434765,2.77555756156289E-16));
#91082=CARTESIAN_POINT('Ctrl Pts',(-63.0378706912077,39.7049575044677,2.77555756156289E-16));
#91083=CARTESIAN_POINT('Ctrl Pts',(-62.9938720098783,39.774641283148,2.77555756156289E-16));
#91084=CARTESIAN_POINT('',(-62.9938720098782,39.7746412831479,12.));
#91085=CARTESIAN_POINT('Ctrl Pts',(-62.9938720098783,39.774641283148,0.));
#91086=CARTESIAN_POINT('Ctrl Pts',(-62.9938720098783,39.774641283148,4.));
#91087=CARTESIAN_POINT('Ctrl Pts',(-62.9938720098783,39.774641283148,8.));
#91088=CARTESIAN_POINT('Ctrl Pts',(-62.9938720098783,39.774641283148,12.));
#91089=CARTESIAN_POINT('',(-62.9864049293894,39.2292784191812,12.));
#91090=CARTESIAN_POINT('Ctrl Pts',(-62.9938720098783,39.774641283148,12.));
#91091=CARTESIAN_POINT('Ctrl Pts',(-63.0378706912076,39.7049575044677,12.));
#91092=CARTESIAN_POINT('Ctrl Pts',(-63.064345736058,39.6241530434765,12.));
#91093=CARTESIAN_POINT('Ctrl Pts',(-63.0699133682744,39.5420039277151,12.));
#91094=CARTESIAN_POINT('Ctrl Pts',(-63.0773368778962,39.4324717733665,12.));
#91095=CARTESIAN_POINT('Ctrl Pts',(-63.0475916539464,39.3205491216485,12.));
#91096=CARTESIAN_POINT('Ctrl Pts',(-62.9864049293894,39.2292784191812,12.));
#91097=CARTESIAN_POINT('Ctrl Pts',(-62.9864049293894,39.2292784191812,12.));
#91098=CARTESIAN_POINT('Ctrl Pts',(-62.9864049293894,39.2292784191812,8.));
#91099=CARTESIAN_POINT('Ctrl Pts',(-62.9864049293893,39.2292784191812,4.));
#91100=CARTESIAN_POINT('Ctrl Pts',(-62.9864049293893,39.2292784191812,0.));
#91101=CARTESIAN_POINT('Origin',(-3.16193356404481E-10,2.01319694273778E-10,
0.));
#91102=CARTESIAN_POINT('Origin',(-3.16193356404481E-10,2.01319694273778E-10,
12.));
#91103=CARTESIAN_POINT('Origin',(-3.16193356404481E-10,2.01319694273778E-10,
0.));
#91104=CARTESIAN_POINT('Ctrl Pts',(-58.9211100416396,45.591148170023,0.));
#91105=CARTESIAN_POINT('Ctrl Pts',(-58.9211100416396,45.591148170023,4.));
#91106=CARTESIAN_POINT('Ctrl Pts',(-58.9211100416396,45.5911481700231,8.));
#91107=CARTESIAN_POINT('Ctrl Pts',(-58.9211100416396,45.5911481700231,12.));
#91108=CARTESIAN_POINT('Ctrl Pts',(-58.8538661785413,45.6780528262179,0.));
#91109=CARTESIAN_POINT('Ctrl Pts',(-58.8538661785413,45.6780528262179,4.));
#91110=CARTESIAN_POINT('Ctrl Pts',(-58.8538661785413,45.6780528262179,8.));
#91111=CARTESIAN_POINT('Ctrl Pts',(-58.8538661785413,45.6780528262179,12.));
#91112=CARTESIAN_POINT('Ctrl Pts',(-58.6845061116499,45.7893619681937,0.));
#91113=CARTESIAN_POINT('Ctrl Pts',(-58.6845061116499,45.7893619681937,4.00000000000001));
#91114=CARTESIAN_POINT('Ctrl Pts',(-58.6845061116498,45.7893619681937,7.99999999999999));
#91115=CARTESIAN_POINT('Ctrl Pts',(-58.6845061116498,45.7893619681937,12.));
#91116=CARTESIAN_POINT('Ctrl Pts',(-58.486102814171,45.790366715598,0.));
#91117=CARTESIAN_POINT('Ctrl Pts',(-58.486102814171,45.790366715598,4.));
#91118=CARTESIAN_POINT('Ctrl Pts',(-58.486102814171,45.7903667155981,8.00000000000001));
#91119=CARTESIAN_POINT('Ctrl Pts',(-58.486102814171,45.7903667155981,12.));
#91120=CARTESIAN_POINT('Ctrl Pts',(-58.4060826907379,45.7706564944768,0.));
#91121=CARTESIAN_POINT('Ctrl Pts',(-58.4060826907379,45.7706564944768,4.));
#91122=CARTESIAN_POINT('Ctrl Pts',(-58.4060826907378,45.7706564944768,8.));
#91123=CARTESIAN_POINT('Ctrl Pts',(-58.4060826907378,45.7706564944768,12.));
#91124=CARTESIAN_POINT('',(-58.9211100416396,45.591148170023,0.));
#91125=CARTESIAN_POINT('',(-58.4060826907379,45.7706564944767,0.));
#91126=CARTESIAN_POINT('Ctrl Pts',(-58.9211100416396,45.591148170023,0.));
#91127=CARTESIAN_POINT('Ctrl Pts',(-58.8538661785413,45.6780528262179,0.));
#91128=CARTESIAN_POINT('Ctrl Pts',(-58.7570889974605,45.741658050204,0.));
#91129=CARTESIAN_POINT('Ctrl Pts',(-58.6508283125144,45.7692455126975,0.));
#91130=CARTESIAN_POINT('Ctrl Pts',(-58.5711327988048,45.7899361095676,0.));
#91131=CARTESIAN_POINT('Ctrl Pts',(-58.486102814171,45.790366715598,0.));
#91132=CARTESIAN_POINT('Ctrl Pts',(-58.4060826907379,45.7706564944768,0.));
#91133=CARTESIAN_POINT('',(-58.4060826907378,45.7706564944767,12.));
#91134=CARTESIAN_POINT('Ctrl Pts',(-58.4060826907379,45.7706564944768,0.));
#91135=CARTESIAN_POINT('Ctrl Pts',(-58.4060826907379,45.7706564944768,4.));
#91136=CARTESIAN_POINT('Ctrl Pts',(-58.4060826907378,45.7706564944768,8.));
#91137=CARTESIAN_POINT('Ctrl Pts',(-58.4060826907378,45.7706564944768,12.));
#91138=CARTESIAN_POINT('',(-58.9211100416396,45.5911481700231,12.));
#91139=CARTESIAN_POINT('Ctrl Pts',(-58.4060826907378,45.7706564944768,12.));
#91140=CARTESIAN_POINT('Ctrl Pts',(-58.486102814171,45.7903667155981,12.));
#91141=CARTESIAN_POINT('Ctrl Pts',(-58.5711327988048,45.7899361095676,12.));
#91142=CARTESIAN_POINT('Ctrl Pts',(-58.6508283125143,45.7692455126975,12.));
#91143=CARTESIAN_POINT('Ctrl Pts',(-58.7570889974604,45.7416580502041,12.));
#91144=CARTESIAN_POINT('Ctrl Pts',(-58.8538661785413,45.6780528262179,12.));
#91145=CARTESIAN_POINT('Ctrl Pts',(-58.9211100416396,45.5911481700231,12.));
#91146=CARTESIAN_POINT('Ctrl Pts',(-58.9211100416396,45.5911481700231,12.));
#91147=CARTESIAN_POINT('Ctrl Pts',(-58.9211100416396,45.5911481700231,8.));
#91148=CARTESIAN_POINT('Ctrl Pts',(-58.9211100416396,45.591148170023,4.));
#91149=CARTESIAN_POINT('Ctrl Pts',(-58.9211100416396,45.591148170023,0.));
#91150=CARTESIAN_POINT('Ctrl Pts',(-54.1679505278134,44.3377168516418,0.));
#91151=CARTESIAN_POINT('Ctrl Pts',(-54.1679505278134,44.3377168516418,12.));
#91152=CARTESIAN_POINT('Ctrl Pts',(-54.1714861895278,44.3393235891014,0.));
#91153=CARTESIAN_POINT('Ctrl Pts',(-54.1714861895278,44.3393235891014,12.));
#91154=CARTESIAN_POINT('Ctrl Pts',(-54.1785633257456,44.3425373700829,0.));
#91155=CARTESIAN_POINT('Ctrl Pts',(-54.1785633257456,44.3425373700829,12.));
#91156=CARTESIAN_POINT('Ctrl Pts',(-54.1891964684439,44.3473589597468,0.));
#91157=CARTESIAN_POINT('Ctrl Pts',(-54.1891964684439,44.3473589597468,12.));
#91158=CARTESIAN_POINT('Ctrl Pts',(-54.203408870162,44.3537895823819,0.));
#91159=CARTESIAN_POINT('Ctrl Pts',(-54.203408870162,44.3537895823819,12.));
#91160=CARTESIAN_POINT('Ctrl Pts',(-54.2212325005847,44.3618309103245,0.));
#91161=CARTESIAN_POINT('Ctrl Pts',(-54.2212325005847,44.3618309103245,12.));
#91162=CARTESIAN_POINT('Ctrl Pts',(-54.2391142386354,44.369875253351,0.));
#91163=CARTESIAN_POINT('Ctrl Pts',(-54.2391142386354,44.369875253351,12.));
#91164=CARTESIAN_POINT('Ctrl Pts',(-54.2570540336536,44.3779225430461,0.));
#91165=CARTESIAN_POINT('Ctrl Pts',(-54.2570540336536,44.3779225430461,12.));
#91166=CARTESIAN_POINT('Ctrl Pts',(-54.2750517888695,44.3859726620288,0.));
#91167=CARTESIAN_POINT('Ctrl Pts',(-54.2750517888695,44.3859726620288,12.));
#91168=CARTESIAN_POINT('Ctrl Pts',(-54.2931073621661,44.3940254456427,0.));
#91169=CARTESIAN_POINT('Ctrl Pts',(-54.2931073621661,44.3940254456427,12.));
#91170=CARTESIAN_POINT('Ctrl Pts',(-54.3112205860776,44.4020807028144,0.));
#91171=CARTESIAN_POINT('Ctrl Pts',(-54.3112205860776,44.4020807028144,12.));
#91172=CARTESIAN_POINT('Ctrl Pts',(-54.3293912830237,44.4101382321834,0.));
#91173=CARTESIAN_POINT('Ctrl Pts',(-54.3293912830237,44.4101382321834,12.));
#91174=CARTESIAN_POINT('Ctrl Pts',(-54.347619281931,44.4181978395814,0.));
#91175=CARTESIAN_POINT('Ctrl Pts',(-54.347619281931,44.4181978395814,12.));
#91176=CARTESIAN_POINT('Ctrl Pts',(-54.3659044357064,44.4262593564664,0.));
#91177=CARTESIAN_POINT('Ctrl Pts',(-54.3659044357064,44.4262593564664,12.));
#91178=CARTESIAN_POINT('Ctrl Pts',(-54.3842466156151,44.4343226339555,0.));
#91179=CARTESIAN_POINT('Ctrl Pts',(-54.3842466156151,44.4343226339555,12.));
#91180=CARTESIAN_POINT('Ctrl Pts',(-54.4026457030316,44.442387534098,0.));
#91181=CARTESIAN_POINT('Ctrl Pts',(-54.4026457030316,44.442387534098,12.));
#91182=CARTESIAN_POINT('Ctrl Pts',(-54.4211015825959,44.4504539226336,0.));
#91183=CARTESIAN_POINT('Ctrl Pts',(-54.4211015825959,44.4504539226336,12.));
#91184=CARTESIAN_POINT('Ctrl Pts',(-54.4396141337008,44.4585216599933,0.));
#91185=CARTESIAN_POINT('Ctrl Pts',(-54.4396141337008,44.4585216599933,12.));
#91186=CARTESIAN_POINT('Ctrl Pts',(-54.4581832262072,44.4665905967701,0.));
#91187=CARTESIAN_POINT('Ctrl Pts',(-54.4581832262072,44.4665905967701,12.));
#91188=CARTESIAN_POINT('Ctrl Pts',(-54.4768087248854,44.4746605784056,0.));
#91189=CARTESIAN_POINT('Ctrl Pts',(-54.4768087248854,44.4746605784056,12.));
#91190=CARTESIAN_POINT('Ctrl Pts',(-54.4954904921938,44.482731448127,0.));
#91191=CARTESIAN_POINT('Ctrl Pts',(-54.4954904921938,44.482731448127,12.));
#91192=CARTESIAN_POINT('Ctrl Pts',(-54.5142283914684,44.4908030503209,0.));
#91193=CARTESIAN_POINT('Ctrl Pts',(-54.5142283914684,44.4908030503209,12.));
#91194=CARTESIAN_POINT('Ctrl Pts',(-54.5330222905438,44.4988752343715,0.));
#91195=CARTESIAN_POINT('Ctrl Pts',(-54.5330222905438,44.4988752343715,12.));
#91196=CARTESIAN_POINT('Ctrl Pts',(-54.5518720616016,44.5069478544945,0.));
#91197=CARTESIAN_POINT('Ctrl Pts',(-54.5518720616016,44.5069478544945,12.));
#91198=CARTESIAN_POINT('Ctrl Pts',(-54.5707775794412,44.5150207678988,0.));
#91199=CARTESIAN_POINT('Ctrl Pts',(-54.5707775794412,44.5150207678988,12.));
#91200=CARTESIAN_POINT('Ctrl Pts',(-54.5897387202815,44.5230938335167,0.));
#91201=CARTESIAN_POINT('Ctrl Pts',(-54.5897387202815,44.5230938335167,12.));
#91202=CARTESIAN_POINT('Ctrl Pts',(-54.6087553602914,44.5311669104515,0.));
#91203=CARTESIAN_POINT('Ctrl Pts',(-54.6087553602914,44.5311669104515,12.));
#91204=CARTESIAN_POINT('Ctrl Pts',(-54.6278273743587,44.5392398566802,0.));
#91205=CARTESIAN_POINT('Ctrl Pts',(-54.6278273743587,44.5392398566802,12.));
#91206=CARTESIAN_POINT('Ctrl Pts',(-54.6469546367408,44.5473125297311,0.));
#91207=CARTESIAN_POINT('Ctrl Pts',(-54.6469546367408,44.5473125297311,12.));
#91208=CARTESIAN_POINT('Ctrl Pts',(-54.6661370216252,44.5553847872721,0.));
#91209=CARTESIAN_POINT('Ctrl Pts',(-54.6661370216252,44.5553847872721,12.));
#91210=CARTESIAN_POINT('Ctrl Pts',(-54.6853744036751,44.5634564876863,0.));
#91211=CARTESIAN_POINT('Ctrl Pts',(-54.6853744036751,44.5634564876863,12.));
#91212=CARTESIAN_POINT('Ctrl Pts',(-54.7046666586754,44.5715274907619,0.));
#91213=CARTESIAN_POINT('Ctrl Pts',(-54.7046666586754,44.5715274907619,12.));
#91214=CARTESIAN_POINT('Ctrl Pts',(-54.7240136637717,44.5795976579454,0.));
#91215=CARTESIAN_POINT('Ctrl Pts',(-54.7240136637717,44.5795976579454,12.));
#91216=CARTESIAN_POINT('Ctrl Pts',(-54.7434152971267,44.5876668519661,0.));
#91217=CARTESIAN_POINT('Ctrl Pts',(-54.7434152971267,44.5876668519661,12.));
#91218=CARTESIAN_POINT('Ctrl Pts',(-54.7628714377037,44.5957349366059,0.));
#91219=CARTESIAN_POINT('Ctrl Pts',(-54.7628714377037,44.5957349366059,12.));
#91220=CARTESIAN_POINT('Ctrl Pts',(-54.7823819650149,44.6038017764309,0.));
#91221=CARTESIAN_POINT('Ctrl Pts',(-54.7823819650149,44.6038017764309,12.));
#91222=CARTESIAN_POINT('Ctrl Pts',(-54.8019467588278,44.6118672364906,0.));
#91223=CARTESIAN_POINT('Ctrl Pts',(-54.8019467588278,44.6118672364906,12.));
#91224=CARTESIAN_POINT('Ctrl Pts',(-54.8215656991837,44.6199311823293,0.));
#91225=CARTESIAN_POINT('Ctrl Pts',(-54.8215656991837,44.6199311823293,12.));
#91226=CARTESIAN_POINT('Ctrl Pts',(-54.8412386665276,44.6279934801169,0.));
#91227=CARTESIAN_POINT('Ctrl Pts',(-54.8412386665276,44.6279934801169,12.));
#91228=CARTESIAN_POINT('Ctrl Pts',(-54.860965541796,44.6360539967392,0.));
#91229=CARTESIAN_POINT('Ctrl Pts',(-54.860965541796,44.6360539967392,12.));
#91230=CARTESIAN_POINT('Ctrl Pts',(-54.8807462065164,44.6441125999063,0.));
#91231=CARTESIAN_POINT('Ctrl Pts',(-54.8807462065164,44.6441125999063,12.));
#91232=CARTESIAN_POINT('Ctrl Pts',(-54.9005805428969,44.6521691582533,0.));
#91233=CARTESIAN_POINT('Ctrl Pts',(-54.9005805428969,44.6521691582533,12.));
#91234=CARTESIAN_POINT('Ctrl Pts',(-54.9204684337822,44.6602235412836,0.));
#91235=CARTESIAN_POINT('Ctrl Pts',(-54.9204684337822,44.6602235412836,12.));
#91236=CARTESIAN_POINT('Ctrl Pts',(-54.9404097626077,44.6682756193147,0.));
#91237=CARTESIAN_POINT('Ctrl Pts',(-54.9404097626077,44.6682756193147,12.));
#91238=CARTESIAN_POINT('Ctrl Pts',(-54.9604044133501,44.6763252634258,0.));
#91239=CARTESIAN_POINT('Ctrl Pts',(-54.9604044133501,44.6763252634258,12.));
#91240=CARTESIAN_POINT('Ctrl Pts',(-54.9804522704686,44.6843723454,0.));
#91241=CARTESIAN_POINT('Ctrl Pts',(-54.9804522704686,44.6843723454,12.));
#91242=CARTESIAN_POINT('Ctrl Pts',(-55.0005532188667,44.6924167376869,0.));
#91243=CARTESIAN_POINT('Ctrl Pts',(-55.0005532188667,44.6924167376869,12.));
#91244=CARTESIAN_POINT('Ctrl Pts',(-55.0207071439237,44.7004583134249,0.));
#91245=CARTESIAN_POINT('Ctrl Pts',(-55.0207071439237,44.7004583134249,12.));
#91246=CARTESIAN_POINT('Ctrl Pts',(-55.0409139315078,44.7084969464513,0.));
#91247=CARTESIAN_POINT('Ctrl Pts',(-55.0409139315078,44.7084969464513,12.));
#91248=CARTESIAN_POINT('Ctrl Pts',(-55.0611734679894,44.7165325113159,0.));
#91249=CARTESIAN_POINT('Ctrl Pts',(-55.0611734679894,44.7165325113159,12.));
#91250=CARTESIAN_POINT('Ctrl Pts',(-55.0814856402496,44.7245648832979,0.));
#91251=CARTESIAN_POINT('Ctrl Pts',(-55.0814856402496,44.7245648832979,12.));
#91252=CARTESIAN_POINT('Ctrl Pts',(-55.1018503356796,44.7325939384035,0.));
#91253=CARTESIAN_POINT('Ctrl Pts',(-55.1018503356796,44.7325939384035,12.));
#91254=CARTESIAN_POINT('Ctrl Pts',(-55.1222674421743,44.740619553348,0.));
#91255=CARTESIAN_POINT('Ctrl Pts',(-55.1222674421743,44.740619553348,12.));
#91256=CARTESIAN_POINT('Ctrl Pts',(-55.14273684812,44.748641605542,0.));
#91257=CARTESIAN_POINT('Ctrl Pts',(-55.14273684812,44.748641605542,12.));
#91258=CARTESIAN_POINT('Ctrl Pts',(-55.1632584423815,44.7566599730773,0.));
#91259=CARTESIAN_POINT('Ctrl Pts',(-55.1632584423815,44.7566599730773,12.));
#91260=CARTESIAN_POINT('Ctrl Pts',(-55.1838321142779,44.7646745347109,0.));
#91261=CARTESIAN_POINT('Ctrl Pts',(-55.1838321142779,44.7646745347109,12.));
#91262=CARTESIAN_POINT('Ctrl Pts',(-55.2044577535866,44.7726851698619,0.));
#91263=CARTESIAN_POINT('Ctrl Pts',(-55.2044577535866,44.7726851698619,12.));
#91264=CARTESIAN_POINT('Ctrl Pts',(-55.2251352505475,44.7806917586077,0.));
#91265=CARTESIAN_POINT('Ctrl Pts',(-55.2251352505475,44.7806917586077,12.));
#91266=CARTESIAN_POINT('Ctrl Pts',(-55.2458644958617,44.7886941816823,0.));
#91267=CARTESIAN_POINT('Ctrl Pts',(-55.2458644958617,44.7886941816823,12.));
#91268=CARTESIAN_POINT('Ctrl Pts',(-55.2666453806883,44.7966923204741,0.));
#91269=CARTESIAN_POINT('Ctrl Pts',(-55.2666453806883,44.7966923204741,12.));
#91270=CARTESIAN_POINT('Ctrl Pts',(-55.287477796635,44.8046860570245,0.));
#91271=CARTESIAN_POINT('Ctrl Pts',(-55.287477796635,44.8046860570245,12.));
#91272=CARTESIAN_POINT('Ctrl Pts',(-55.3083616357605,44.812675274021,0.));
#91273=CARTESIAN_POINT('Ctrl Pts',(-55.3083616357605,44.812675274021,12.));
#91274=CARTESIAN_POINT('Ctrl Pts',(-55.3292967905726,44.8206598547889,0.));
#91275=CARTESIAN_POINT('Ctrl Pts',(-55.3292967905726,44.8206598547889,12.));
#91276=CARTESIAN_POINT('Ctrl Pts',(-55.350283154023,44.8286396832849,0.));
#91277=CARTESIAN_POINT('Ctrl Pts',(-55.350283154023,44.8286396832849,12.));
#91278=CARTESIAN_POINT('Ctrl Pts',(-55.3713206194962,44.8366146440896,0.));
#91279=CARTESIAN_POINT('Ctrl Pts',(-55.3713206194962,44.8366146440896,12.));
#91280=CARTESIAN_POINT('Ctrl Pts',(-55.3924090808002,44.8445846224034,0.));
#91281=CARTESIAN_POINT('Ctrl Pts',(-55.3924090808002,44.8445846224034,12.));
#91282=CARTESIAN_POINT('Ctrl Pts',(-55.4135484321706,44.8525495040397,0.));
#91283=CARTESIAN_POINT('Ctrl Pts',(-55.4135484321706,44.8525495040397,12.));
#91284=CARTESIAN_POINT('Ctrl Pts',(-55.4347385682697,44.8605091754208,0.));
#91285=CARTESIAN_POINT('Ctrl Pts',(-55.4347385682697,44.8605091754208,12.));
#91286=CARTESIAN_POINT('Ctrl Pts',(-55.4559793841838,44.8684635235727,0.));
#91287=CARTESIAN_POINT('Ctrl Pts',(-55.4559793841838,44.8684635235727,12.));
#91288=CARTESIAN_POINT('Ctrl Pts',(-55.4772707754139,44.8764124361218,0.));
#91289=CARTESIAN_POINT('Ctrl Pts',(-55.4772707754139,44.8764124361218,12.));
#91290=CARTESIAN_POINT('Ctrl Pts',(-55.4986126378676,44.8843558012903,0.));
#91291=CARTESIAN_POINT('Ctrl Pts',(-55.4986126378676,44.8843558012903,12.));
#91292=CARTESIAN_POINT('Ctrl Pts',(-55.5200048678648,44.8922935078905,0.));
#91293=CARTESIAN_POINT('Ctrl Pts',(-55.5200048678648,44.8922935078905,12.));
#91294=CARTESIAN_POINT('Ctrl Pts',(-55.541447362135,44.9002254453192,0.));
#91295=CARTESIAN_POINT('Ctrl Pts',(-55.541447362135,44.9002254453192,12.));
#91296=CARTESIAN_POINT('Ctrl Pts',(-55.5629400178136,44.9081515035525,0.));
#91297=CARTESIAN_POINT('Ctrl Pts',(-55.5629400178136,44.9081515035525,12.));
#91298=CARTESIAN_POINT('Ctrl Pts',(-55.5844827324315,44.9160715731425,0.));
#91299=CARTESIAN_POINT('Ctrl Pts',(-55.5844827324315,44.9160715731425,12.));
#91300=CARTESIAN_POINT('Ctrl Pts',(-55.6060754039089,44.9239855452119,0.));
#91301=CARTESIAN_POINT('Ctrl Pts',(-55.6060754039089,44.9239855452119,12.));
#91302=CARTESIAN_POINT('Ctrl Pts',(-55.6277179305604,44.9318933114483,0.));
#91303=CARTESIAN_POINT('Ctrl Pts',(-55.6277179305604,44.9318933114483,12.));
#91304=CARTESIAN_POINT('Ctrl Pts',(-55.6494102110922,44.9397947640996,0.));
#91305=CARTESIAN_POINT('Ctrl Pts',(-55.6494102110922,44.9397947640996,12.));
#91306=CARTESIAN_POINT('Ctrl Pts',(-55.671152144599,44.9476897959694,0.));
#91307=CARTESIAN_POINT('Ctrl Pts',(-55.671152144599,44.9476897959694,12.));
#91308=CARTESIAN_POINT('Ctrl Pts',(-55.6929436305522,44.9555783004133,0.));
#91309=CARTESIAN_POINT('Ctrl Pts',(-55.6929436305522,44.9555783004133,12.));
#91310=CARTESIAN_POINT('Ctrl Pts',(-55.7147845687969,44.9634601713352,0.));
#91311=CARTESIAN_POINT('Ctrl Pts',(-55.7147845687969,44.9634601713352,12.));
#91312=CARTESIAN_POINT('Ctrl Pts',(-55.7366748595582,44.9713353031827,0.));
#91313=CARTESIAN_POINT('Ctrl Pts',(-55.7366748595582,44.9713353031827,12.));
#91314=CARTESIAN_POINT('Ctrl Pts',(-55.7586144034376,44.979203590942,0.));
#91315=CARTESIAN_POINT('Ctrl Pts',(-55.7586144034376,44.979203590942,12.));
#91316=CARTESIAN_POINT('Ctrl Pts',(-55.7806031014093,44.9870649301333,0.));
#91317=CARTESIAN_POINT('Ctrl Pts',(-55.7806031014093,44.9870649301333,12.));
#91318=CARTESIAN_POINT('Ctrl Pts',(-55.8026408548078,44.9949192168073,0.));
#91319=CARTESIAN_POINT('Ctrl Pts',(-55.8026408548078,44.9949192168073,12.));
#91320=CARTESIAN_POINT('Ctrl Pts',(-55.8247275653257,45.002766347541,0.));
#91321=CARTESIAN_POINT('Ctrl Pts',(-55.8247275653257,45.002766347541,12.));
#91322=CARTESIAN_POINT('Ctrl Pts',(-55.8468631350195,45.0106062194325,0.));
#91323=CARTESIAN_POINT('Ctrl Pts',(-55.8468631350195,45.0106062194325,12.));
#91324=CARTESIAN_POINT('Ctrl Pts',(-55.8690474663058,45.0184387300968,0.));
#91325=CARTESIAN_POINT('Ctrl Pts',(-55.8690474663058,45.0184387300968,12.));
#91326=CARTESIAN_POINT('Ctrl Pts',(-55.8912804619588,45.0262637776623,0.));
#91327=CARTESIAN_POINT('Ctrl Pts',(-55.8912804619588,45.0262637776623,12.));
#91328=CARTESIAN_POINT('Ctrl Pts',(-55.9135620250977,45.0340812607676,0.));
#91329=CARTESIAN_POINT('Ctrl Pts',(-55.9135620250977,45.0340812607676,12.));
#91330=CARTESIAN_POINT('Ctrl Pts',(-55.9358920591861,45.041891078557,0.));
#91331=CARTESIAN_POINT('Ctrl Pts',(-55.9358920591861,45.041891078557,12.));
#91332=CARTESIAN_POINT('Ctrl Pts',(-55.958270468037,45.0496931306766,0.));
#91333=CARTESIAN_POINT('Ctrl Pts',(-55.958270468037,45.0496931306766,12.));
#91334=CARTESIAN_POINT('Ctrl Pts',(-55.9806971558099,45.0574873172696,0.));
#91335=CARTESIAN_POINT('Ctrl Pts',(-55.9806971558099,45.0574873172696,12.));
#91336=CARTESIAN_POINT('Ctrl Pts',(-56.0031720270074,45.0652735389729,0.));
#91337=CARTESIAN_POINT('Ctrl Pts',(-56.0031720270074,45.0652735389729,12.));
#91338=CARTESIAN_POINT('Ctrl Pts',(-56.025694986463,45.0730516969142,0.));
#91339=CARTESIAN_POINT('Ctrl Pts',(-56.025694986463,45.0730516969142,12.));
#91340=CARTESIAN_POINT('Ctrl Pts',(-56.0482659393412,45.0808216927082,0.));
#91341=CARTESIAN_POINT('Ctrl Pts',(-56.0482659393412,45.0808216927082,12.));
#91342=CARTESIAN_POINT('Ctrl Pts',(-56.070884791141,45.0885834284513,0.));
#91343=CARTESIAN_POINT('Ctrl Pts',(-56.070884791141,45.0885834284513,12.));
#91344=CARTESIAN_POINT('Ctrl Pts',(-56.0935514476945,45.0963368067177,0.));
#91345=CARTESIAN_POINT('Ctrl Pts',(-56.0935514476945,45.0963368067177,12.));
#91346=CARTESIAN_POINT('Ctrl Pts',(-56.1162658151621,45.1040817305563,0.));
#91347=CARTESIAN_POINT('Ctrl Pts',(-56.1162658151621,45.1040817305563,12.));
#91348=CARTESIAN_POINT('Ctrl Pts',(-56.1390278000226,45.1118181034888,0.));
#91349=CARTESIAN_POINT('Ctrl Pts',(-56.1390278000226,45.1118181034888,12.));
#91350=CARTESIAN_POINT('Ctrl Pts',(-56.1618373090729,45.119545829506,0.));
#91351=CARTESIAN_POINT('Ctrl Pts',(-56.1618373090729,45.119545829506,12.));
#91352=CARTESIAN_POINT('Ctrl Pts',(-56.1846942494321,45.1272648130627,0.));
#91353=CARTESIAN_POINT('Ctrl Pts',(-56.1846942494321,45.1272648130627,12.));
#91354=CARTESIAN_POINT('Ctrl Pts',(-56.2075985285391,45.1349749590736,0.));
#91355=CARTESIAN_POINT('Ctrl Pts',(-56.2075985285391,45.1349749590736,12.));
#91356=CARTESIAN_POINT('Ctrl Pts',(-56.2305500541491,45.1426761729107,0.));
#91357=CARTESIAN_POINT('Ctrl Pts',(-56.2305500541491,45.1426761729107,12.));
#91358=CARTESIAN_POINT('Ctrl Pts',(-56.2535487343227,45.150368360401,0.));
#91359=CARTESIAN_POINT('Ctrl Pts',(-56.2535487343227,45.150368360401,12.));
#91360=CARTESIAN_POINT('Ctrl Pts',(-56.2765944774252,45.158051427823,0.));
#91361=CARTESIAN_POINT('Ctrl Pts',(-56.2765944774252,45.158051427823,12.));
#91362=CARTESIAN_POINT('Ctrl Pts',(-56.2996871921321,45.1657252819018,0.));
#91363=CARTESIAN_POINT('Ctrl Pts',(-56.2996871921321,45.1657252819018,12.));
#91364=CARTESIAN_POINT('Ctrl Pts',(-56.3228267874265,45.1733898298062,0.));
#91365=CARTESIAN_POINT('Ctrl Pts',(-56.3228267874265,45.1733898298062,12.));
#91366=CARTESIAN_POINT('Ctrl Pts',(-56.3460131725962,45.1810449791451,0.));
#91367=CARTESIAN_POINT('Ctrl Pts',(-56.3460131725962,45.1810449791451,12.));
#91368=CARTESIAN_POINT('Ctrl Pts',(-56.3692462572228,45.1886906379664,0.));
#91369=CARTESIAN_POINT('Ctrl Pts',(-56.3692462572228,45.1886906379664,12.));
#91370=CARTESIAN_POINT('Ctrl Pts',(-56.3925259511804,45.1963267147527,0.));
#91371=CARTESIAN_POINT('Ctrl Pts',(-56.3925259511804,45.1963267147527,12.));
#91372=CARTESIAN_POINT('Ctrl Pts',(-56.4158521646412,45.2039531184172,0.));
#91373=CARTESIAN_POINT('Ctrl Pts',(-56.4158521646412,45.2039531184172,12.));
#91374=CARTESIAN_POINT('Ctrl Pts',(-56.4392248080733,45.2115697583002,0.));
#91375=CARTESIAN_POINT('Ctrl Pts',(-56.4392248080733,45.2115697583002,12.));
#91376=CARTESIAN_POINT('Ctrl Pts',(-56.4626437922385,45.2191765441666,0.));
#91377=CARTESIAN_POINT('Ctrl Pts',(-56.4626437922385,45.2191765441666,12.));
#91378=CARTESIAN_POINT('Ctrl Pts',(-56.4861090281819,45.2267733862046,0.));
#91379=CARTESIAN_POINT('Ctrl Pts',(-56.4861090281819,45.2267733862046,12.));
#91380=CARTESIAN_POINT('Ctrl Pts',(-56.5096204272299,45.2343601950222,0.));
#91381=CARTESIAN_POINT('Ctrl Pts',(-56.5096204272299,45.2343601950222,12.));
#91382=CARTESIAN_POINT('Ctrl Pts',(-56.533177900995,45.2419368816423,0.));
#91383=CARTESIAN_POINT('Ctrl Pts',(-56.533177900995,45.2419368816423,12.));
#91384=CARTESIAN_POINT('Ctrl Pts',(-56.5567813613752,45.2495033574997,0.));
#91385=CARTESIAN_POINT('Ctrl Pts',(-56.5567813613752,45.2495033574997,12.));
#91386=CARTESIAN_POINT('Ctrl Pts',(-56.5804307205507,45.2570595344382,0.));
#91387=CARTESIAN_POINT('Ctrl Pts',(-56.5804307205507,45.2570595344382,12.));
#91388=CARTESIAN_POINT('Ctrl Pts',(-56.604125890975,45.2646053247094,0.));
#91389=CARTESIAN_POINT('Ctrl Pts',(-56.604125890975,45.2646053247094,12.));
#91390=CARTESIAN_POINT('Ctrl Pts',(-56.6278667853716,45.2721406409706,0.));
#91391=CARTESIAN_POINT('Ctrl Pts',(-56.6278667853716,45.2721406409706,12.));
#91392=CARTESIAN_POINT('Ctrl Pts',(-56.6516533167398,45.2796653962796,0.));
#91393=CARTESIAN_POINT('Ctrl Pts',(-56.6516533167398,45.2796653962796,12.));
#91394=CARTESIAN_POINT('Ctrl Pts',(-56.6754853983535,45.2871795040912,0.));
#91395=CARTESIAN_POINT('Ctrl Pts',(-56.6754853983535,45.2871795040912,12.));
#91396=CARTESIAN_POINT('Ctrl Pts',(-56.6993629437596,45.2946828782557,0.));
#91397=CARTESIAN_POINT('Ctrl Pts',(-56.6993629437596,45.2946828782557,12.));
#91398=CARTESIAN_POINT('Ctrl Pts',(-56.7232858667697,45.3021754330169,0.));
#91399=CARTESIAN_POINT('Ctrl Pts',(-56.7232858667697,45.3021754330169,12.));
#91400=CARTESIAN_POINT('Ctrl Pts',(-56.747254081454,45.3096570830107,0.));
#91401=CARTESIAN_POINT('Ctrl Pts',(-56.747254081454,45.3096570830107,12.));
#91402=CARTESIAN_POINT('Ctrl Pts',(-56.771267502148,45.3171277432592,0.));
#91403=CARTESIAN_POINT('Ctrl Pts',(-56.771267502148,45.3171277432592,12.));
#91404=CARTESIAN_POINT('Ctrl Pts',(-56.7953260434521,45.3245873291682,0.));
#91405=CARTESIAN_POINT('Ctrl Pts',(-56.7953260434521,45.3245873291682,12.));
#91406=CARTESIAN_POINT('Ctrl Pts',(-56.8194296202293,45.3320357565241,0.));
#91407=CARTESIAN_POINT('Ctrl Pts',(-56.8194296202293,45.3320357565241,12.));
#91408=CARTESIAN_POINT('Ctrl Pts',(-56.8435781475982,45.3394729414932,0.));
#91409=CARTESIAN_POINT('Ctrl Pts',(-56.8435781475982,45.3394729414932,12.));
#91410=CARTESIAN_POINT('Ctrl Pts',(-56.8677715409266,45.3468988006202,0.));
#91411=CARTESIAN_POINT('Ctrl Pts',(-56.8677715409266,45.3468988006202,12.));
#91412=CARTESIAN_POINT('Ctrl Pts',(-56.8920097158371,45.3543132508234,0.));
#91413=CARTESIAN_POINT('Ctrl Pts',(-56.8920097158371,45.3543132508234,12.));
#91414=CARTESIAN_POINT('Ctrl Pts',(-56.916292588208,45.3617162093918,0.));
#91415=CARTESIAN_POINT('Ctrl Pts',(-56.916292588208,45.3617162093918,12.));
#91416=CARTESIAN_POINT('Ctrl Pts',(-56.9406200741714,45.3691075939827,0.));
#91417=CARTESIAN_POINT('Ctrl Pts',(-56.9406200741714,45.3691075939827,12.));
#91418=CARTESIAN_POINT('Ctrl Pts',(-56.9649920901079,45.3764873226202,0.));
#91419=CARTESIAN_POINT('Ctrl Pts',(-56.9649920901079,45.3764873226202,12.));
#91420=CARTESIAN_POINT('Ctrl Pts',(-56.9894085526383,45.3838553136957,0.));
#91421=CARTESIAN_POINT('Ctrl Pts',(-56.9894085526383,45.3838553136957,12.));
#91422=CARTESIAN_POINT('Ctrl Pts',(-57.0138693786287,45.3912114859625,0.));
#91423=CARTESIAN_POINT('Ctrl Pts',(-57.0138693786287,45.3912114859625,12.));
#91424=CARTESIAN_POINT('Ctrl Pts',(-57.0383744851917,45.3985557585316,0.));
#91425=CARTESIAN_POINT('Ctrl Pts',(-57.0383744851917,45.3985557585316,12.));
#91426=CARTESIAN_POINT('Ctrl Pts',(-57.0629237896848,45.4058880508693,0.));
#91427=CARTESIAN_POINT('Ctrl Pts',(-57.0629237896848,45.4058880508693,12.));
#91428=CARTESIAN_POINT('Ctrl Pts',(-57.0875172097048,45.4132082827945,0.));
#91429=CARTESIAN_POINT('Ctrl Pts',(-57.0875172097048,45.4132082827945,12.));
#91430=CARTESIAN_POINT('Ctrl Pts',(-57.1121546630776,45.4205163744778,0.));
#91431=CARTESIAN_POINT('Ctrl Pts',(-57.1121546630776,45.4205163744778,12.));
#91432=CARTESIAN_POINT('Ctrl Pts',(-57.1368360678629,45.4278122464387,0.));
#91433=CARTESIAN_POINT('Ctrl Pts',(-57.1368360678629,45.4278122464387,12.));
#91434=CARTESIAN_POINT('Ctrl Pts',(-57.1615613423586,45.4350958195434,0.));
#91435=CARTESIAN_POINT('Ctrl Pts',(-57.1615613423586,45.4350958195434,12.));
#91436=CARTESIAN_POINT('Ctrl Pts',(-57.1863304051011,45.4423670150035,0.));
#91437=CARTESIAN_POINT('Ctrl Pts',(-57.1863304051011,45.4423670150035,12.));
#91438=CARTESIAN_POINT('Ctrl Pts',(-57.2111431748629,45.4496257543759,0.));
#91439=CARTESIAN_POINT('Ctrl Pts',(-57.2111431748629,45.4496257543759,12.));
#91440=CARTESIAN_POINT('Ctrl Pts',(-57.2359995706441,45.4568719595639,0.));
#91441=CARTESIAN_POINT('Ctrl Pts',(-57.2359995706441,45.4568719595639,12.));
#91442=CARTESIAN_POINT('Ctrl Pts',(-57.2608995116727,45.4641055528138,0.));
#91443=CARTESIAN_POINT('Ctrl Pts',(-57.2608995116727,45.4641055528138,12.));
#91444=CARTESIAN_POINT('Ctrl Pts',(-57.2858429174056,45.4713264567059,0.));
#91445=CARTESIAN_POINT('Ctrl Pts',(-57.2858429174056,45.4713264567059,12.));
#91446=CARTESIAN_POINT('Ctrl Pts',(-57.3108297075262,45.4785345941505,0.));
#91447=CARTESIAN_POINT('Ctrl Pts',(-57.3108297075262,45.4785345941505,12.));
#91448=CARTESIAN_POINT('Ctrl Pts',(-57.3358598019391,45.4857298883826,0.));
#91449=CARTESIAN_POINT('Ctrl Pts',(-57.3358598019391,45.4857298883826,12.));
#91450=CARTESIAN_POINT('Ctrl Pts',(-57.360933120758,45.4929122629576,0.));
#91451=CARTESIAN_POINT('Ctrl Pts',(-57.360933120758,45.4929122629576,12.));
#91452=CARTESIAN_POINT('Ctrl Pts',(-57.3860495843043,45.5000816417516,0.));
#91453=CARTESIAN_POINT('Ctrl Pts',(-57.3860495843043,45.5000816417516,12.));
#91454=CARTESIAN_POINT('Ctrl Pts',(-57.4112091131193,45.5072379489637,0.));
#91455=CARTESIAN_POINT('Ctrl Pts',(-57.4112091131193,45.5072379489637,12.));
#91456=CARTESIAN_POINT('Ctrl Pts',(-57.4364116279708,45.5143811091209,0.));
#91457=CARTESIAN_POINT('Ctrl Pts',(-57.4364116279708,45.5143811091209,12.));
#91458=CARTESIAN_POINT('Ctrl Pts',(-57.4616570498566,45.5215110470825,0.));
#91459=CARTESIAN_POINT('Ctrl Pts',(-57.4616570498566,45.5215110470825,12.));
#91460=CARTESIAN_POINT('Ctrl Pts',(-57.4869453000055,45.5286276880479,0.));
#91461=CARTESIAN_POINT('Ctrl Pts',(-57.4869453000055,45.5286276880479,12.));
#91462=CARTESIAN_POINT('Ctrl Pts',(-57.5122762998732,45.5357309575603,0.));
#91463=CARTESIAN_POINT('Ctrl Pts',(-57.5122762998732,45.5357309575603,12.));
#91464=CARTESIAN_POINT('Ctrl Pts',(-57.5376499711338,45.5428207814832,0.));
#91465=CARTESIAN_POINT('Ctrl Pts',(-57.5376499711338,45.5428207814832,12.));
#91466=CARTESIAN_POINT('Ctrl Pts',(-57.5630662356671,45.5498970859829,0.));
#91467=CARTESIAN_POINT('Ctrl Pts',(-57.5630662356671,45.5498970859829,12.));
#91468=CARTESIAN_POINT('Ctrl Pts',(-57.5885250155432,45.5569597975096,0.));
#91469=CARTESIAN_POINT('Ctrl Pts',(-57.5885250155432,45.5569597975096,12.));
#91470=CARTESIAN_POINT('Ctrl Pts',(-57.6140262330048,45.5640088427819,0.));
#91471=CARTESIAN_POINT('Ctrl Pts',(-57.6140262330048,45.5640088427819,12.));
#91472=CARTESIAN_POINT('Ctrl Pts',(-57.6395698104416,45.5710441487683,0.));
#91473=CARTESIAN_POINT('Ctrl Pts',(-57.6395698104416,45.5710441487683,12.));
#91474=CARTESIAN_POINT('Ctrl Pts',(-57.6651556704249,45.5780656427172,0.));
#91475=CARTESIAN_POINT('Ctrl Pts',(-57.6651556704249,45.5780656427172,12.));
#91476=CARTESIAN_POINT('Ctrl Pts',(-57.6907837357425,45.5850732521902,0.));
#91477=CARTESIAN_POINT('Ctrl Pts',(-57.6907837357425,45.5850732521902,12.));
#91478=CARTESIAN_POINT('Ctrl Pts',(-57.7164539294316,45.5920669050988,0.));
#91479=CARTESIAN_POINT('Ctrl Pts',(-57.7164539294316,45.5920669050988,12.));
#91480=CARTESIAN_POINT('Ctrl Pts',(-57.7421661748022,45.5990465297341,0.));
#91481=CARTESIAN_POINT('Ctrl Pts',(-57.7421661748022,45.5990465297341,12.));
#91482=CARTESIAN_POINT('Ctrl Pts',(-57.7679203954735,45.6060120548199,0.));
#91483=CARTESIAN_POINT('Ctrl Pts',(-57.7679203954735,45.6060120548199,12.));
#91484=CARTESIAN_POINT('Ctrl Pts',(-57.7937165153379,45.6129634094677,0.));
#91485=CARTESIAN_POINT('Ctrl Pts',(-57.7937165153379,45.6129634094677,12.));
#91486=CARTESIAN_POINT('Ctrl Pts',(-57.819554458484,45.619900523078,0.));
#91487=CARTESIAN_POINT('Ctrl Pts',(-57.819554458484,45.619900523078,12.));
#91488=CARTESIAN_POINT('Ctrl Pts',(-57.8454341491236,45.6268233252543,0.));
#91489=CARTESIAN_POINT('Ctrl Pts',(-57.8454341491236,45.6268233252543,12.));
#91490=CARTESIAN_POINT('Ctrl Pts',(-57.8713555115232,45.6337317457253,0.));
#91491=CARTESIAN_POINT('Ctrl Pts',(-57.8713555115232,45.6337317457253,12.));
#91492=CARTESIAN_POINT('Ctrl Pts',(-57.8973184699037,45.6406257142385,0.));
#91493=CARTESIAN_POINT('Ctrl Pts',(-57.8973184699037,45.6406257142385,12.));
#91494=CARTESIAN_POINT('Ctrl Pts',(-57.923322948432,45.6475051605542,0.));
#91495=CARTESIAN_POINT('Ctrl Pts',(-57.923322948432,45.6475051605542,12.));
#91496=CARTESIAN_POINT('Ctrl Pts',(-57.9493688714249,45.6543700146689,0.));
#91497=CARTESIAN_POINT('Ctrl Pts',(-57.9493688714249,45.6543700146689,12.));
#91498=CARTESIAN_POINT('Ctrl Pts',(-57.975456163507,45.6612202069927,0.));
#91499=CARTESIAN_POINT('Ctrl Pts',(-57.975456163507,45.6612202069927,12.));
#91500=CARTESIAN_POINT('Ctrl Pts',(-58.0015847497838,45.6680556685494,0.));
#91501=CARTESIAN_POINT('Ctrl Pts',(-58.0015847497838,45.6680556685494,12.));
#91502=CARTESIAN_POINT('Ctrl Pts',(-58.0277545560001,45.6748763311635,0.));
#91503=CARTESIAN_POINT('Ctrl Pts',(-58.0277545560001,45.6748763311635,12.));
#91504=CARTESIAN_POINT('Ctrl Pts',(-58.0539655087095,45.6816821276662,0.));
#91505=CARTESIAN_POINT('Ctrl Pts',(-58.0539655087095,45.6816821276662,12.));
#91506=CARTESIAN_POINT('Ctrl Pts',(-58.0802175348939,45.6884729914465,0.));
#91507=CARTESIAN_POINT('Ctrl Pts',(-58.0802175348939,45.6884729914465,12.));
#91508=CARTESIAN_POINT('Ctrl Pts',(-58.1065105615884,45.6952488560133,0.));
#91509=CARTESIAN_POINT('Ctrl Pts',(-58.1065105615884,45.6952488560133,12.));
#91510=CARTESIAN_POINT('Ctrl Pts',(-58.1328445154667,45.7020096545174,0.));
#91511=CARTESIAN_POINT('Ctrl Pts',(-58.1328445154667,45.7020096545174,12.));
#91512=CARTESIAN_POINT('Ctrl Pts',(-58.159219322515,45.708755319378,0.));
#91513=CARTESIAN_POINT('Ctrl Pts',(-58.159219322515,45.708755319378,12.));
#91514=CARTESIAN_POINT('Ctrl Pts',(-58.1856349074723,45.7154857816507,0.));
#91515=CARTESIAN_POINT('Ctrl Pts',(-58.1856349074723,45.7154857816507,12.));
#91516=CARTESIAN_POINT('Ctrl Pts',(-58.2120911942819,45.7222009715431,0.));
#91517=CARTESIAN_POINT('Ctrl Pts',(-58.2120911942819,45.7222009715431,12.));
#91518=CARTESIAN_POINT('Ctrl Pts',(-58.2385881070959,45.7289008195612,0.));
#91519=CARTESIAN_POINT('Ctrl Pts',(-58.2385881070959,45.7289008195612,12.));
#91520=CARTESIAN_POINT('Ctrl Pts',(-58.2651255711481,45.7355852575127,0.));
#91521=CARTESIAN_POINT('Ctrl Pts',(-58.2651255711481,45.7355852575127,12.));
#91522=CARTESIAN_POINT('Ctrl Pts',(-58.2917035135833,45.7422542194625,0.));
#91523=CARTESIAN_POINT('Ctrl Pts',(-58.2917035135833,45.7422542194625,12.));
#91524=CARTESIAN_POINT('Ctrl Pts',(-58.3183218645265,45.7489076429725,0.));
#91525=CARTESIAN_POINT('Ctrl Pts',(-58.3183218645265,45.7489076429725,12.));
#91526=CARTESIAN_POINT('Ctrl Pts',(-58.3449805573335,45.7555454693956,0.));
#91527=CARTESIAN_POINT('Ctrl Pts',(-58.3449805573335,45.7555454693956,12.));
#91528=CARTESIAN_POINT('Ctrl Pts',(-58.3716795262251,45.762167641136,0.));
#91529=CARTESIAN_POINT('Ctrl Pts',(-58.3716795262251,45.762167641136,12.));
#91530=CARTESIAN_POINT('Ctrl Pts',(-58.3984187044166,45.7687740994899,0.));
#91531=CARTESIAN_POINT('Ctrl Pts',(-58.3984187044166,45.7687740994899,12.));
#91532=CARTESIAN_POINT('Ctrl Pts',(-58.4251980219532,45.77536478215,0.));
#91533=CARTESIAN_POINT('Ctrl Pts',(-58.4251980219532,45.77536478215,12.));
#91534=CARTESIAN_POINT('Ctrl Pts',(-58.4520174038836,45.7819396211062,0.));
#91535=CARTESIAN_POINT('Ctrl Pts',(-58.4520174038836,45.7819396211062,12.));
#91536=CARTESIAN_POINT('Ctrl Pts',(-58.4788767677114,45.7884985397138,0.));
#91537=CARTESIAN_POINT('Ctrl Pts',(-58.4788767677114,45.7884985397138,12.));
#91538=CARTESIAN_POINT('Ctrl Pts',(-58.5057760270407,45.7950414569431,0.));
#91539=CARTESIAN_POINT('Ctrl Pts',(-58.5057760270407,45.7950414569431,12.));
#91540=CARTESIAN_POINT('Ctrl Pts',(-58.5327150960874,45.801568292618,0.));
#91541=CARTESIAN_POINT('Ctrl Pts',(-58.5327150960874,45.801568292618,12.));
#91542=CARTESIAN_POINT('Ctrl Pts',(-58.5596938940308,45.8080789725167,0.));
#91543=CARTESIAN_POINT('Ctrl Pts',(-58.5596938940308,45.8080789725167,12.));
#91544=CARTESIAN_POINT('Ctrl Pts',(-58.5867123490943,45.8145734330666,0.));
#91545=CARTESIAN_POINT('Ctrl Pts',(-58.5867123490943,45.8145734330666,12.));
#91546=CARTESIAN_POINT('Ctrl Pts',(-58.6137704035561,45.8210516273556,0.));
#91547=CARTESIAN_POINT('Ctrl Pts',(-58.6137704035561,45.8210516273556,12.));
#91548=CARTESIAN_POINT('Ctrl Pts',(-58.64086801535,45.8275135263874,0.));
#91549=CARTESIAN_POINT('Ctrl Pts',(-58.64086801535,45.8275135263874,12.));
#91550=CARTESIAN_POINT('Ctrl Pts',(-58.668005155216,45.8339591141396,0.));
#91551=CARTESIAN_POINT('Ctrl Pts',(-58.668005155216,45.8339591141396,12.));
#91552=CARTESIAN_POINT('Ctrl Pts',(-58.6897464750196,45.8391025301766,0.));
#91553=CARTESIAN_POINT('Ctrl Pts',(-58.6897464750196,45.8391025301766,12.));
#91554=CARTESIAN_POINT('Ctrl Pts',(-58.7060702401382,45.8429527488565,0.));
#91555=CARTESIAN_POINT('Ctrl Pts',(-58.7060702401382,45.8429527488565,12.));
#91556=CARTESIAN_POINT('Ctrl Pts',(-58.7169606500157,45.8455162977347,0.));
#91557=CARTESIAN_POINT('Ctrl Pts',(-58.7169606500157,45.8455162977347,12.));
#91558=CARTESIAN_POINT('Ctrl Pts',(-58.722407829904,45.8467972562798,0.));
#91559=CARTESIAN_POINT('Ctrl Pts',(-58.722407829904,45.8467972562798,12.));
#91560=CARTESIAN_POINT('',(-54.1679505278134,44.3377168516418,0.));
#91561=CARTESIAN_POINT('Ctrl Pts',(-54.1679505278134,44.3377168516418,0.));
#91562=CARTESIAN_POINT('Ctrl Pts',(-54.1714861895278,44.3393235891014,0.));
#91563=CARTESIAN_POINT('Ctrl Pts',(-54.1785633257456,44.3425373700829,0.));
#91564=CARTESIAN_POINT('Ctrl Pts',(-54.1891964684439,44.3473589597468,0.));
#91565=CARTESIAN_POINT('Ctrl Pts',(-54.203408870162,44.3537895823819,0.));
#91566=CARTESIAN_POINT('Ctrl Pts',(-54.2212325005847,44.3618309103245,0.));
#91567=CARTESIAN_POINT('Ctrl Pts',(-54.2391142386354,44.369875253351,0.));
#91568=CARTESIAN_POINT('Ctrl Pts',(-54.2570540336536,44.3779225430461,0.));
#91569=CARTESIAN_POINT('Ctrl Pts',(-54.2750517888695,44.3859726620288,0.));
#91570=CARTESIAN_POINT('Ctrl Pts',(-54.2931073621661,44.3940254456427,0.));
#91571=CARTESIAN_POINT('Ctrl Pts',(-54.3112205860776,44.4020807028144,0.));
#91572=CARTESIAN_POINT('Ctrl Pts',(-54.3293912830237,44.4101382321834,0.));
#91573=CARTESIAN_POINT('Ctrl Pts',(-54.347619281931,44.4181978395814,0.));
#91574=CARTESIAN_POINT('Ctrl Pts',(-54.3659044357064,44.4262593564664,0.));
#91575=CARTESIAN_POINT('Ctrl Pts',(-54.3842466156151,44.4343226339555,0.));
#91576=CARTESIAN_POINT('Ctrl Pts',(-54.4026457030316,44.442387534098,0.));
#91577=CARTESIAN_POINT('Ctrl Pts',(-54.4211015825959,44.4504539226336,0.));
#91578=CARTESIAN_POINT('Ctrl Pts',(-54.4396141337008,44.4585216599933,0.));
#91579=CARTESIAN_POINT('Ctrl Pts',(-54.4581832262072,44.4665905967701,0.));
#91580=CARTESIAN_POINT('Ctrl Pts',(-54.4768087248854,44.4746605784056,0.));
#91581=CARTESIAN_POINT('Ctrl Pts',(-54.4954904921938,44.482731448127,0.));
#91582=CARTESIAN_POINT('Ctrl Pts',(-54.5142283914684,44.4908030503209,0.));
#91583=CARTESIAN_POINT('Ctrl Pts',(-54.5330222905438,44.4988752343715,0.));
#91584=CARTESIAN_POINT('Ctrl Pts',(-54.5518720616016,44.5069478544945,0.));
#91585=CARTESIAN_POINT('Ctrl Pts',(-54.5707775794412,44.5150207678988,0.));
#91586=CARTESIAN_POINT('Ctrl Pts',(-54.5897387202815,44.5230938335167,0.));
#91587=CARTESIAN_POINT('Ctrl Pts',(-54.6087553602914,44.5311669104515,0.));
#91588=CARTESIAN_POINT('Ctrl Pts',(-54.6278273743587,44.5392398566802,0.));
#91589=CARTESIAN_POINT('Ctrl Pts',(-54.6469546367408,44.5473125297311,0.));
#91590=CARTESIAN_POINT('Ctrl Pts',(-54.6661370216252,44.5553847872721,0.));
#91591=CARTESIAN_POINT('Ctrl Pts',(-54.6853744036751,44.5634564876863,0.));
#91592=CARTESIAN_POINT('Ctrl Pts',(-54.7046666586754,44.5715274907619,0.));
#91593=CARTESIAN_POINT('Ctrl Pts',(-54.7240136637717,44.5795976579454,0.));
#91594=CARTESIAN_POINT('Ctrl Pts',(-54.7434152971267,44.5876668519661,0.));
#91595=CARTESIAN_POINT('Ctrl Pts',(-54.7628714377037,44.5957349366059,0.));
#91596=CARTESIAN_POINT('Ctrl Pts',(-54.7823819650149,44.6038017764309,0.));
#91597=CARTESIAN_POINT('Ctrl Pts',(-54.8019467588278,44.6118672364906,0.));
#91598=CARTESIAN_POINT('Ctrl Pts',(-54.8215656991837,44.6199311823293,0.));
#91599=CARTESIAN_POINT('Ctrl Pts',(-54.8412386665276,44.6279934801169,0.));
#91600=CARTESIAN_POINT('Ctrl Pts',(-54.860965541796,44.6360539967392,0.));
#91601=CARTESIAN_POINT('Ctrl Pts',(-54.8807462065164,44.6441125999063,0.));
#91602=CARTESIAN_POINT('Ctrl Pts',(-54.9005805428969,44.6521691582533,0.));
#91603=CARTESIAN_POINT('Ctrl Pts',(-54.9204684337822,44.6602235412836,0.));
#91604=CARTESIAN_POINT('Ctrl Pts',(-54.9404097626077,44.6682756193147,0.));
#91605=CARTESIAN_POINT('Ctrl Pts',(-54.9604044133501,44.6763252634258,0.));
#91606=CARTESIAN_POINT('Ctrl Pts',(-54.9804522704686,44.6843723454,0.));
#91607=CARTESIAN_POINT('Ctrl Pts',(-55.0005532188667,44.6924167376869,0.));
#91608=CARTESIAN_POINT('Ctrl Pts',(-55.0207071439237,44.7004583134249,0.));
#91609=CARTESIAN_POINT('Ctrl Pts',(-55.0409139315078,44.7084969464513,0.));
#91610=CARTESIAN_POINT('Ctrl Pts',(-55.0611734679894,44.7165325113159,0.));
#91611=CARTESIAN_POINT('Ctrl Pts',(-55.0814856402496,44.7245648832979,0.));
#91612=CARTESIAN_POINT('Ctrl Pts',(-55.1018503356796,44.7325939384035,0.));
#91613=CARTESIAN_POINT('Ctrl Pts',(-55.1222674421743,44.740619553348,0.));
#91614=CARTESIAN_POINT('Ctrl Pts',(-55.14273684812,44.748641605542,0.));
#91615=CARTESIAN_POINT('Ctrl Pts',(-55.1632584423815,44.7566599730773,0.));
#91616=CARTESIAN_POINT('Ctrl Pts',(-55.1838321142779,44.7646745347109,0.));
#91617=CARTESIAN_POINT('Ctrl Pts',(-55.2044577535866,44.7726851698619,0.));
#91618=CARTESIAN_POINT('Ctrl Pts',(-55.2251352505475,44.7806917586077,0.));
#91619=CARTESIAN_POINT('Ctrl Pts',(-55.2458644958617,44.7886941816823,0.));
#91620=CARTESIAN_POINT('Ctrl Pts',(-55.2666453806883,44.7966923204741,0.));
#91621=CARTESIAN_POINT('Ctrl Pts',(-55.287477796635,44.8046860570245,0.));
#91622=CARTESIAN_POINT('Ctrl Pts',(-55.3083616357605,44.812675274021,0.));
#91623=CARTESIAN_POINT('Ctrl Pts',(-55.3292967905726,44.8206598547889,0.));
#91624=CARTESIAN_POINT('Ctrl Pts',(-55.350283154023,44.8286396832849,0.));
#91625=CARTESIAN_POINT('Ctrl Pts',(-55.3713206194962,44.8366146440896,0.));
#91626=CARTESIAN_POINT('Ctrl Pts',(-55.3924090808002,44.8445846224034,0.));
#91627=CARTESIAN_POINT('Ctrl Pts',(-55.4135484321706,44.8525495040397,0.));
#91628=CARTESIAN_POINT('Ctrl Pts',(-55.4347385682697,44.8605091754208,0.));
#91629=CARTESIAN_POINT('Ctrl Pts',(-55.4559793841838,44.8684635235727,0.));
#91630=CARTESIAN_POINT('Ctrl Pts',(-55.4772707754139,44.8764124361218,0.));
#91631=CARTESIAN_POINT('Ctrl Pts',(-55.4986126378676,44.8843558012903,0.));
#91632=CARTESIAN_POINT('Ctrl Pts',(-55.5200048678648,44.8922935078905,0.));
#91633=CARTESIAN_POINT('Ctrl Pts',(-55.541447362135,44.9002254453192,0.));
#91634=CARTESIAN_POINT('Ctrl Pts',(-55.5629400178136,44.9081515035525,0.));
#91635=CARTESIAN_POINT('Ctrl Pts',(-55.5844827324315,44.9160715731425,0.));
#91636=CARTESIAN_POINT('Ctrl Pts',(-55.6060754039089,44.9239855452119,0.));
#91637=CARTESIAN_POINT('Ctrl Pts',(-55.6277179305604,44.9318933114483,0.));
#91638=CARTESIAN_POINT('Ctrl Pts',(-55.6494102110922,44.9397947640996,0.));
#91639=CARTESIAN_POINT('Ctrl Pts',(-55.671152144599,44.9476897959694,0.));
#91640=CARTESIAN_POINT('Ctrl Pts',(-55.6929436305522,44.9555783004133,0.));
#91641=CARTESIAN_POINT('Ctrl Pts',(-55.7147845687969,44.9634601713352,0.));
#91642=CARTESIAN_POINT('Ctrl Pts',(-55.7366748595582,44.9713353031827,0.));
#91643=CARTESIAN_POINT('Ctrl Pts',(-55.7586144034376,44.979203590942,0.));
#91644=CARTESIAN_POINT('Ctrl Pts',(-55.7806031014093,44.9870649301333,0.));
#91645=CARTESIAN_POINT('Ctrl Pts',(-55.8026408548078,44.9949192168073,0.));
#91646=CARTESIAN_POINT('Ctrl Pts',(-55.8247275653257,45.002766347541,0.));
#91647=CARTESIAN_POINT('Ctrl Pts',(-55.8468631350195,45.0106062194325,0.));
#91648=CARTESIAN_POINT('Ctrl Pts',(-55.8690474663058,45.0184387300968,0.));
#91649=CARTESIAN_POINT('Ctrl Pts',(-55.8912804619588,45.0262637776623,0.));
#91650=CARTESIAN_POINT('Ctrl Pts',(-55.9135620250977,45.0340812607676,0.));
#91651=CARTESIAN_POINT('Ctrl Pts',(-55.9358920591861,45.041891078557,0.));
#91652=CARTESIAN_POINT('Ctrl Pts',(-55.958270468037,45.0496931306766,0.));
#91653=CARTESIAN_POINT('Ctrl Pts',(-55.9806971558099,45.0574873172696,0.));
#91654=CARTESIAN_POINT('Ctrl Pts',(-56.0031720270074,45.0652735389729,0.));
#91655=CARTESIAN_POINT('Ctrl Pts',(-56.025694986463,45.0730516969142,0.));
#91656=CARTESIAN_POINT('Ctrl Pts',(-56.0482659393412,45.0808216927082,0.));
#91657=CARTESIAN_POINT('Ctrl Pts',(-56.070884791141,45.0885834284513,0.));
#91658=CARTESIAN_POINT('Ctrl Pts',(-56.0935514476945,45.0963368067177,0.));
#91659=CARTESIAN_POINT('Ctrl Pts',(-56.1162658151621,45.1040817305563,0.));
#91660=CARTESIAN_POINT('Ctrl Pts',(-56.1390278000226,45.1118181034888,0.));
#91661=CARTESIAN_POINT('Ctrl Pts',(-56.1618373090729,45.119545829506,0.));
#91662=CARTESIAN_POINT('Ctrl Pts',(-56.1846942494321,45.1272648130627,0.));
#91663=CARTESIAN_POINT('Ctrl Pts',(-56.2075985285391,45.1349749590736,0.));
#91664=CARTESIAN_POINT('Ctrl Pts',(-56.2305500541491,45.1426761729107,0.));
#91665=CARTESIAN_POINT('Ctrl Pts',(-56.2535487343227,45.150368360401,0.));
#91666=CARTESIAN_POINT('Ctrl Pts',(-56.2765944774252,45.158051427823,0.));
#91667=CARTESIAN_POINT('Ctrl Pts',(-56.2996871921321,45.1657252819018,0.));
#91668=CARTESIAN_POINT('Ctrl Pts',(-56.3228267874265,45.1733898298062,0.));
#91669=CARTESIAN_POINT('Ctrl Pts',(-56.3460131725962,45.1810449791451,0.));
#91670=CARTESIAN_POINT('Ctrl Pts',(-56.3692462572228,45.1886906379664,0.));
#91671=CARTESIAN_POINT('Ctrl Pts',(-56.3925259511804,45.1963267147527,0.));
#91672=CARTESIAN_POINT('Ctrl Pts',(-56.4158521646412,45.2039531184172,0.));
#91673=CARTESIAN_POINT('Ctrl Pts',(-56.4392248080733,45.2115697583002,0.));
#91674=CARTESIAN_POINT('Ctrl Pts',(-56.4626437922385,45.2191765441666,0.));
#91675=CARTESIAN_POINT('Ctrl Pts',(-56.4861090281819,45.2267733862046,0.));
#91676=CARTESIAN_POINT('Ctrl Pts',(-56.5096204272299,45.2343601950222,0.));
#91677=CARTESIAN_POINT('Ctrl Pts',(-56.533177900995,45.2419368816423,0.));
#91678=CARTESIAN_POINT('Ctrl Pts',(-56.5567813613752,45.2495033574997,0.));
#91679=CARTESIAN_POINT('Ctrl Pts',(-56.5804307205507,45.2570595344382,0.));
#91680=CARTESIAN_POINT('Ctrl Pts',(-56.604125890975,45.2646053247094,0.));
#91681=CARTESIAN_POINT('Ctrl Pts',(-56.6278667853716,45.2721406409706,0.));
#91682=CARTESIAN_POINT('Ctrl Pts',(-56.6516533167398,45.2796653962796,0.));
#91683=CARTESIAN_POINT('Ctrl Pts',(-56.6754853983535,45.2871795040912,0.));
#91684=CARTESIAN_POINT('Ctrl Pts',(-56.6993629437596,45.2946828782557,0.));
#91685=CARTESIAN_POINT('Ctrl Pts',(-56.7232858667697,45.3021754330169,0.));
#91686=CARTESIAN_POINT('Ctrl Pts',(-56.747254081454,45.3096570830107,0.));
#91687=CARTESIAN_POINT('Ctrl Pts',(-56.771267502148,45.3171277432592,0.));
#91688=CARTESIAN_POINT('Ctrl Pts',(-56.7953260434521,45.3245873291682,0.));
#91689=CARTESIAN_POINT('Ctrl Pts',(-56.8194296202293,45.3320357565241,0.));
#91690=CARTESIAN_POINT('Ctrl Pts',(-56.8435781475982,45.3394729414932,0.));
#91691=CARTESIAN_POINT('Ctrl Pts',(-56.8677715409266,45.3468988006202,0.));
#91692=CARTESIAN_POINT('Ctrl Pts',(-56.8920097158371,45.3543132508234,0.));
#91693=CARTESIAN_POINT('Ctrl Pts',(-56.916292588208,45.3617162093918,0.));
#91694=CARTESIAN_POINT('Ctrl Pts',(-56.9406200741714,45.3691075939827,0.));
#91695=CARTESIAN_POINT('Ctrl Pts',(-56.9649920901079,45.3764873226202,0.));
#91696=CARTESIAN_POINT('Ctrl Pts',(-56.9894085526383,45.3838553136957,0.));
#91697=CARTESIAN_POINT('Ctrl Pts',(-57.0138693786287,45.3912114859625,0.));
#91698=CARTESIAN_POINT('Ctrl Pts',(-57.0383744851917,45.3985557585316,0.));
#91699=CARTESIAN_POINT('Ctrl Pts',(-57.0629237896848,45.4058880508693,0.));
#91700=CARTESIAN_POINT('Ctrl Pts',(-57.0875172097048,45.4132082827945,0.));
#91701=CARTESIAN_POINT('Ctrl Pts',(-57.1121546630776,45.4205163744778,0.));
#91702=CARTESIAN_POINT('Ctrl Pts',(-57.1368360678629,45.4278122464387,0.));
#91703=CARTESIAN_POINT('Ctrl Pts',(-57.1615613423586,45.4350958195434,0.));
#91704=CARTESIAN_POINT('Ctrl Pts',(-57.1863304051011,45.4423670150035,0.));
#91705=CARTESIAN_POINT('Ctrl Pts',(-57.2111431748629,45.4496257543759,0.));
#91706=CARTESIAN_POINT('Ctrl Pts',(-57.2359995706441,45.4568719595639,0.));
#91707=CARTESIAN_POINT('Ctrl Pts',(-57.2608995116727,45.4641055528138,0.));
#91708=CARTESIAN_POINT('Ctrl Pts',(-57.2858429174056,45.4713264567059,0.));
#91709=CARTESIAN_POINT('Ctrl Pts',(-57.3108297075262,45.4785345941505,0.));
#91710=CARTESIAN_POINT('Ctrl Pts',(-57.3358598019391,45.4857298883826,0.));
#91711=CARTESIAN_POINT('Ctrl Pts',(-57.360933120758,45.4929122629576,0.));
#91712=CARTESIAN_POINT('Ctrl Pts',(-57.3860495843043,45.5000816417516,0.));
#91713=CARTESIAN_POINT('Ctrl Pts',(-57.4112091131193,45.5072379489637,0.));
#91714=CARTESIAN_POINT('Ctrl Pts',(-57.4364116279708,45.5143811091209,0.));
#91715=CARTESIAN_POINT('Ctrl Pts',(-57.4616570498566,45.5215110470825,0.));
#91716=CARTESIAN_POINT('Ctrl Pts',(-57.4869453000055,45.5286276880479,0.));
#91717=CARTESIAN_POINT('Ctrl Pts',(-57.5122762998732,45.5357309575603,0.));
#91718=CARTESIAN_POINT('Ctrl Pts',(-57.5376499711338,45.5428207814832,0.));
#91719=CARTESIAN_POINT('Ctrl Pts',(-57.5630662356671,45.5498970859829,0.));
#91720=CARTESIAN_POINT('Ctrl Pts',(-57.5885250155432,45.5569597975096,0.));
#91721=CARTESIAN_POINT('Ctrl Pts',(-57.6140262330048,45.5640088427819,0.));
#91722=CARTESIAN_POINT('Ctrl Pts',(-57.6395698104416,45.5710441487683,0.));
#91723=CARTESIAN_POINT('Ctrl Pts',(-57.6651556704249,45.5780656427172,0.));
#91724=CARTESIAN_POINT('Ctrl Pts',(-57.6907837357425,45.5850732521902,0.));
#91725=CARTESIAN_POINT('Ctrl Pts',(-57.7164539294316,45.5920669050988,0.));
#91726=CARTESIAN_POINT('Ctrl Pts',(-57.7421661748022,45.5990465297341,0.));
#91727=CARTESIAN_POINT('Ctrl Pts',(-57.7679203954735,45.6060120548199,0.));
#91728=CARTESIAN_POINT('Ctrl Pts',(-57.7937165153379,45.6129634094677,0.));
#91729=CARTESIAN_POINT('Ctrl Pts',(-57.819554458484,45.619900523078,0.));
#91730=CARTESIAN_POINT('Ctrl Pts',(-57.8454341491236,45.6268233252543,0.));
#91731=CARTESIAN_POINT('Ctrl Pts',(-57.8713555115232,45.6337317457253,0.));
#91732=CARTESIAN_POINT('Ctrl Pts',(-57.8973184699037,45.6406257142385,0.));
#91733=CARTESIAN_POINT('Ctrl Pts',(-57.923322948432,45.6475051605542,0.));
#91734=CARTESIAN_POINT('Ctrl Pts',(-57.9493688714249,45.6543700146689,0.));
#91735=CARTESIAN_POINT('Ctrl Pts',(-57.975456163507,45.6612202069927,0.));
#91736=CARTESIAN_POINT('Ctrl Pts',(-58.0015847497838,45.6680556685494,0.));
#91737=CARTESIAN_POINT('Ctrl Pts',(-58.0277545560001,45.6748763311635,0.));
#91738=CARTESIAN_POINT('Ctrl Pts',(-58.0539655087095,45.6816821276662,0.));
#91739=CARTESIAN_POINT('Ctrl Pts',(-58.0802175348939,45.6884729914465,0.));
#91740=CARTESIAN_POINT('Ctrl Pts',(-58.1065105615884,45.6952488560133,0.));
#91741=CARTESIAN_POINT('Ctrl Pts',(-58.1328445154667,45.7020096545174,0.));
#91742=CARTESIAN_POINT('Ctrl Pts',(-58.159219322515,45.708755319378,0.));
#91743=CARTESIAN_POINT('Ctrl Pts',(-58.1856349074723,45.7154857816507,0.));
#91744=CARTESIAN_POINT('Ctrl Pts',(-58.2120911942819,45.7222009715431,0.));
#91745=CARTESIAN_POINT('Ctrl Pts',(-58.2385881070959,45.7289008195612,0.));
#91746=CARTESIAN_POINT('Ctrl Pts',(-58.2651255711481,45.7355852575127,0.));
#91747=CARTESIAN_POINT('Ctrl Pts',(-58.2917035135833,45.7422542194625,0.));
#91748=CARTESIAN_POINT('Ctrl Pts',(-58.3183218645265,45.7489076429725,0.));
#91749=CARTESIAN_POINT('Ctrl Pts',(-58.3449805573335,45.7555454693956,0.));
#91750=CARTESIAN_POINT('Ctrl Pts',(-58.3678667473266,45.7612219538034,0.));
#91751=CARTESIAN_POINT('Ctrl Pts',(-58.385434851721,45.7655655205267,0.));
#91752=CARTESIAN_POINT('Ctrl Pts',(-58.3976670480781,45.7685831165459,0.));
#91753=CARTESIAN_POINT('Ctrl Pts',(-58.4045515723008,45.7702793558063,0.));
#91754=CARTESIAN_POINT('Ctrl Pts',(-58.4060826907379,45.7706564944767,0.));
#91755=CARTESIAN_POINT('',(-54.1679505278134,44.3377168516418,12.));
#91756=CARTESIAN_POINT('',(-54.1679505278134,44.3377168516418,0.));
#91757=CARTESIAN_POINT('Ctrl Pts',(-58.4060826907378,45.7706564944767,12.));
#91758=CARTESIAN_POINT('Ctrl Pts',(-58.4045515723008,45.7702793558063,12.));
#91759=CARTESIAN_POINT('Ctrl Pts',(-58.397667048078,45.7685831165459,12.));
#91760=CARTESIAN_POINT('Ctrl Pts',(-58.385434851721,45.7655655205267,12.));
#91761=CARTESIAN_POINT('Ctrl Pts',(-58.3678667473265,45.7612219538034,12.));
#91762=CARTESIAN_POINT('Ctrl Pts',(-58.3449805573335,45.7555454693956,12.));
#91763=CARTESIAN_POINT('Ctrl Pts',(-58.3183218645265,45.7489076429725,12.));
#91764=CARTESIAN_POINT('Ctrl Pts',(-58.2917035135833,45.7422542194625,12.));
#91765=CARTESIAN_POINT('Ctrl Pts',(-58.2651255711481,45.7355852575127,12.));
#91766=CARTESIAN_POINT('Ctrl Pts',(-58.2385881070959,45.7289008195612,12.));
#91767=CARTESIAN_POINT('Ctrl Pts',(-58.2120911942819,45.7222009715431,12.));
#91768=CARTESIAN_POINT('Ctrl Pts',(-58.1856349074723,45.7154857816507,12.));
#91769=CARTESIAN_POINT('Ctrl Pts',(-58.159219322515,45.708755319378,12.));
#91770=CARTESIAN_POINT('Ctrl Pts',(-58.1328445154667,45.7020096545174,12.));
#91771=CARTESIAN_POINT('Ctrl Pts',(-58.1065105615884,45.6952488560133,12.));
#91772=CARTESIAN_POINT('Ctrl Pts',(-58.0802175348939,45.6884729914465,12.));
#91773=CARTESIAN_POINT('Ctrl Pts',(-58.0539655087095,45.6816821276662,12.));
#91774=CARTESIAN_POINT('Ctrl Pts',(-58.0277545560001,45.6748763311635,12.));
#91775=CARTESIAN_POINT('Ctrl Pts',(-58.0015847497838,45.6680556685494,12.));
#91776=CARTESIAN_POINT('Ctrl Pts',(-57.975456163507,45.6612202069927,12.));
#91777=CARTESIAN_POINT('Ctrl Pts',(-57.9493688714249,45.6543700146689,12.));
#91778=CARTESIAN_POINT('Ctrl Pts',(-57.923322948432,45.6475051605542,12.));
#91779=CARTESIAN_POINT('Ctrl Pts',(-57.8973184699037,45.6406257142385,12.));
#91780=CARTESIAN_POINT('Ctrl Pts',(-57.8713555115232,45.6337317457253,12.));
#91781=CARTESIAN_POINT('Ctrl Pts',(-57.8454341491236,45.6268233252543,12.));
#91782=CARTESIAN_POINT('Ctrl Pts',(-57.819554458484,45.619900523078,12.));
#91783=CARTESIAN_POINT('Ctrl Pts',(-57.7937165153379,45.6129634094677,12.));
#91784=CARTESIAN_POINT('Ctrl Pts',(-57.7679203954735,45.6060120548199,12.));
#91785=CARTESIAN_POINT('Ctrl Pts',(-57.7421661748022,45.5990465297341,12.));
#91786=CARTESIAN_POINT('Ctrl Pts',(-57.7164539294316,45.5920669050988,12.));
#91787=CARTESIAN_POINT('Ctrl Pts',(-57.6907837357425,45.5850732521902,12.));
#91788=CARTESIAN_POINT('Ctrl Pts',(-57.6651556704249,45.5780656427172,12.));
#91789=CARTESIAN_POINT('Ctrl Pts',(-57.6395698104416,45.5710441487683,12.));
#91790=CARTESIAN_POINT('Ctrl Pts',(-57.6140262330048,45.5640088427819,12.));
#91791=CARTESIAN_POINT('Ctrl Pts',(-57.5885250155432,45.5569597975096,12.));
#91792=CARTESIAN_POINT('Ctrl Pts',(-57.5630662356671,45.5498970859829,12.));
#91793=CARTESIAN_POINT('Ctrl Pts',(-57.5376499711338,45.5428207814832,12.));
#91794=CARTESIAN_POINT('Ctrl Pts',(-57.5122762998732,45.5357309575603,12.));
#91795=CARTESIAN_POINT('Ctrl Pts',(-57.4869453000055,45.5286276880479,12.));
#91796=CARTESIAN_POINT('Ctrl Pts',(-57.4616570498566,45.5215110470825,12.));
#91797=CARTESIAN_POINT('Ctrl Pts',(-57.4364116279708,45.5143811091209,12.));
#91798=CARTESIAN_POINT('Ctrl Pts',(-57.4112091131193,45.5072379489637,12.));
#91799=CARTESIAN_POINT('Ctrl Pts',(-57.3860495843043,45.5000816417516,12.));
#91800=CARTESIAN_POINT('Ctrl Pts',(-57.360933120758,45.4929122629576,12.));
#91801=CARTESIAN_POINT('Ctrl Pts',(-57.3358598019391,45.4857298883826,12.));
#91802=CARTESIAN_POINT('Ctrl Pts',(-57.3108297075262,45.4785345941505,12.));
#91803=CARTESIAN_POINT('Ctrl Pts',(-57.2858429174056,45.4713264567059,12.));
#91804=CARTESIAN_POINT('Ctrl Pts',(-57.2608995116727,45.4641055528138,12.));
#91805=CARTESIAN_POINT('Ctrl Pts',(-57.2359995706441,45.4568719595639,12.));
#91806=CARTESIAN_POINT('Ctrl Pts',(-57.2111431748629,45.4496257543759,12.));
#91807=CARTESIAN_POINT('Ctrl Pts',(-57.1863304051011,45.4423670150035,12.));
#91808=CARTESIAN_POINT('Ctrl Pts',(-57.1615613423586,45.4350958195434,12.));
#91809=CARTESIAN_POINT('Ctrl Pts',(-57.1368360678629,45.4278122464387,12.));
#91810=CARTESIAN_POINT('Ctrl Pts',(-57.1121546630776,45.4205163744778,12.));
#91811=CARTESIAN_POINT('Ctrl Pts',(-57.0875172097048,45.4132082827945,12.));
#91812=CARTESIAN_POINT('Ctrl Pts',(-57.0629237896848,45.4058880508693,12.));
#91813=CARTESIAN_POINT('Ctrl Pts',(-57.0383744851917,45.3985557585316,12.));
#91814=CARTESIAN_POINT('Ctrl Pts',(-57.0138693786287,45.3912114859625,12.));
#91815=CARTESIAN_POINT('Ctrl Pts',(-56.9894085526383,45.3838553136957,12.));
#91816=CARTESIAN_POINT('Ctrl Pts',(-56.9649920901079,45.3764873226202,12.));
#91817=CARTESIAN_POINT('Ctrl Pts',(-56.9406200741714,45.3691075939827,12.));
#91818=CARTESIAN_POINT('Ctrl Pts',(-56.916292588208,45.3617162093918,12.));
#91819=CARTESIAN_POINT('Ctrl Pts',(-56.8920097158371,45.3543132508234,12.));
#91820=CARTESIAN_POINT('Ctrl Pts',(-56.8677715409266,45.3468988006202,12.));
#91821=CARTESIAN_POINT('Ctrl Pts',(-56.8435781475982,45.3394729414932,12.));
#91822=CARTESIAN_POINT('Ctrl Pts',(-56.8194296202293,45.3320357565241,12.));
#91823=CARTESIAN_POINT('Ctrl Pts',(-56.7953260434521,45.3245873291682,12.));
#91824=CARTESIAN_POINT('Ctrl Pts',(-56.771267502148,45.3171277432592,12.));
#91825=CARTESIAN_POINT('Ctrl Pts',(-56.747254081454,45.3096570830107,12.));
#91826=CARTESIAN_POINT('Ctrl Pts',(-56.7232858667697,45.3021754330169,12.));
#91827=CARTESIAN_POINT('Ctrl Pts',(-56.6993629437596,45.2946828782557,12.));
#91828=CARTESIAN_POINT('Ctrl Pts',(-56.6754853983535,45.2871795040912,12.));
#91829=CARTESIAN_POINT('Ctrl Pts',(-56.6516533167398,45.2796653962796,12.));
#91830=CARTESIAN_POINT('Ctrl Pts',(-56.6278667853716,45.2721406409706,12.));
#91831=CARTESIAN_POINT('Ctrl Pts',(-56.604125890975,45.2646053247094,12.));
#91832=CARTESIAN_POINT('Ctrl Pts',(-56.5804307205507,45.2570595344382,12.));
#91833=CARTESIAN_POINT('Ctrl Pts',(-56.5567813613752,45.2495033574997,12.));
#91834=CARTESIAN_POINT('Ctrl Pts',(-56.533177900995,45.2419368816423,12.));
#91835=CARTESIAN_POINT('Ctrl Pts',(-56.5096204272299,45.2343601950222,12.));
#91836=CARTESIAN_POINT('Ctrl Pts',(-56.4861090281819,45.2267733862046,12.));
#91837=CARTESIAN_POINT('Ctrl Pts',(-56.4626437922385,45.2191765441666,12.));
#91838=CARTESIAN_POINT('Ctrl Pts',(-56.4392248080733,45.2115697583002,12.));
#91839=CARTESIAN_POINT('Ctrl Pts',(-56.4158521646412,45.2039531184172,12.));
#91840=CARTESIAN_POINT('Ctrl Pts',(-56.3925259511804,45.1963267147527,12.));
#91841=CARTESIAN_POINT('Ctrl Pts',(-56.3692462572228,45.1886906379664,12.));
#91842=CARTESIAN_POINT('Ctrl Pts',(-56.3460131725962,45.1810449791451,12.));
#91843=CARTESIAN_POINT('Ctrl Pts',(-56.3228267874265,45.1733898298062,12.));
#91844=CARTESIAN_POINT('Ctrl Pts',(-56.2996871921321,45.1657252819018,12.));
#91845=CARTESIAN_POINT('Ctrl Pts',(-56.2765944774252,45.158051427823,12.));
#91846=CARTESIAN_POINT('Ctrl Pts',(-56.2535487343227,45.150368360401,12.));
#91847=CARTESIAN_POINT('Ctrl Pts',(-56.2305500541491,45.1426761729107,12.));
#91848=CARTESIAN_POINT('Ctrl Pts',(-56.2075985285391,45.1349749590736,12.));
#91849=CARTESIAN_POINT('Ctrl Pts',(-56.1846942494321,45.1272648130627,12.));
#91850=CARTESIAN_POINT('Ctrl Pts',(-56.1618373090729,45.119545829506,12.));
#91851=CARTESIAN_POINT('Ctrl Pts',(-56.1390278000226,45.1118181034888,12.));
#91852=CARTESIAN_POINT('Ctrl Pts',(-56.1162658151621,45.1040817305563,12.));
#91853=CARTESIAN_POINT('Ctrl Pts',(-56.0935514476945,45.0963368067177,12.));
#91854=CARTESIAN_POINT('Ctrl Pts',(-56.070884791141,45.0885834284513,12.));
#91855=CARTESIAN_POINT('Ctrl Pts',(-56.0482659393412,45.0808216927082,12.));
#91856=CARTESIAN_POINT('Ctrl Pts',(-56.025694986463,45.0730516969142,12.));
#91857=CARTESIAN_POINT('Ctrl Pts',(-56.0031720270074,45.0652735389729,12.));
#91858=CARTESIAN_POINT('Ctrl Pts',(-55.9806971558099,45.0574873172696,12.));
#91859=CARTESIAN_POINT('Ctrl Pts',(-55.958270468037,45.0496931306766,12.));
#91860=CARTESIAN_POINT('Ctrl Pts',(-55.9358920591861,45.041891078557,12.));
#91861=CARTESIAN_POINT('Ctrl Pts',(-55.9135620250977,45.0340812607676,12.));
#91862=CARTESIAN_POINT('Ctrl Pts',(-55.8912804619588,45.0262637776623,12.));
#91863=CARTESIAN_POINT('Ctrl Pts',(-55.8690474663058,45.0184387300968,12.));
#91864=CARTESIAN_POINT('Ctrl Pts',(-55.8468631350195,45.0106062194325,12.));
#91865=CARTESIAN_POINT('Ctrl Pts',(-55.8247275653257,45.002766347541,12.));
#91866=CARTESIAN_POINT('Ctrl Pts',(-55.8026408548078,44.9949192168073,12.));
#91867=CARTESIAN_POINT('Ctrl Pts',(-55.7806031014093,44.9870649301333,12.));
#91868=CARTESIAN_POINT('Ctrl Pts',(-55.7586144034376,44.979203590942,12.));
#91869=CARTESIAN_POINT('Ctrl Pts',(-55.7366748595582,44.9713353031827,12.));
#91870=CARTESIAN_POINT('Ctrl Pts',(-55.7147845687969,44.9634601713352,12.));
#91871=CARTESIAN_POINT('Ctrl Pts',(-55.6929436305522,44.9555783004133,12.));
#91872=CARTESIAN_POINT('Ctrl Pts',(-55.671152144599,44.9476897959694,12.));
#91873=CARTESIAN_POINT('Ctrl Pts',(-55.6494102110922,44.9397947640996,12.));
#91874=CARTESIAN_POINT('Ctrl Pts',(-55.6277179305604,44.9318933114483,12.));
#91875=CARTESIAN_POINT('Ctrl Pts',(-55.6060754039089,44.9239855452119,12.));
#91876=CARTESIAN_POINT('Ctrl Pts',(-55.5844827324315,44.9160715731425,12.));
#91877=CARTESIAN_POINT('Ctrl Pts',(-55.5629400178136,44.9081515035525,12.));
#91878=CARTESIAN_POINT('Ctrl Pts',(-55.541447362135,44.9002254453192,12.));
#91879=CARTESIAN_POINT('Ctrl Pts',(-55.5200048678648,44.8922935078905,12.));
#91880=CARTESIAN_POINT('Ctrl Pts',(-55.4986126378676,44.8843558012903,12.));
#91881=CARTESIAN_POINT('Ctrl Pts',(-55.4772707754139,44.8764124361218,12.));
#91882=CARTESIAN_POINT('Ctrl Pts',(-55.4559793841838,44.8684635235727,12.));
#91883=CARTESIAN_POINT('Ctrl Pts',(-55.4347385682697,44.8605091754208,12.));
#91884=CARTESIAN_POINT('Ctrl Pts',(-55.4135484321706,44.8525495040397,12.));
#91885=CARTESIAN_POINT('Ctrl Pts',(-55.3924090808002,44.8445846224034,12.));
#91886=CARTESIAN_POINT('Ctrl Pts',(-55.3713206194962,44.8366146440896,12.));
#91887=CARTESIAN_POINT('Ctrl Pts',(-55.350283154023,44.8286396832849,12.));
#91888=CARTESIAN_POINT('Ctrl Pts',(-55.3292967905726,44.8206598547889,12.));
#91889=CARTESIAN_POINT('Ctrl Pts',(-55.3083616357605,44.812675274021,12.));
#91890=CARTESIAN_POINT('Ctrl Pts',(-55.287477796635,44.8046860570245,12.));
#91891=CARTESIAN_POINT('Ctrl Pts',(-55.2666453806883,44.7966923204741,12.));
#91892=CARTESIAN_POINT('Ctrl Pts',(-55.2458644958617,44.7886941816823,12.));
#91893=CARTESIAN_POINT('Ctrl Pts',(-55.2251352505475,44.7806917586077,12.));
#91894=CARTESIAN_POINT('Ctrl Pts',(-55.2044577535866,44.7726851698619,12.));
#91895=CARTESIAN_POINT('Ctrl Pts',(-55.1838321142779,44.7646745347109,12.));
#91896=CARTESIAN_POINT('Ctrl Pts',(-55.1632584423815,44.7566599730773,12.));
#91897=CARTESIAN_POINT('Ctrl Pts',(-55.14273684812,44.748641605542,12.));
#91898=CARTESIAN_POINT('Ctrl Pts',(-55.1222674421743,44.740619553348,12.));
#91899=CARTESIAN_POINT('Ctrl Pts',(-55.1018503356796,44.7325939384035,12.));
#91900=CARTESIAN_POINT('Ctrl Pts',(-55.0814856402496,44.7245648832979,12.));
#91901=CARTESIAN_POINT('Ctrl Pts',(-55.0611734679894,44.7165325113159,12.));
#91902=CARTESIAN_POINT('Ctrl Pts',(-55.0409139315078,44.7084969464513,12.));
#91903=CARTESIAN_POINT('Ctrl Pts',(-55.0207071439237,44.7004583134249,12.));
#91904=CARTESIAN_POINT('Ctrl Pts',(-55.0005532188667,44.6924167376869,12.));
#91905=CARTESIAN_POINT('Ctrl Pts',(-54.9804522704686,44.6843723454,12.));
#91906=CARTESIAN_POINT('Ctrl Pts',(-54.9604044133501,44.6763252634258,12.));
#91907=CARTESIAN_POINT('Ctrl Pts',(-54.9404097626077,44.6682756193147,12.));
#91908=CARTESIAN_POINT('Ctrl Pts',(-54.9204684337822,44.6602235412836,12.));
#91909=CARTESIAN_POINT('Ctrl Pts',(-54.9005805428969,44.6521691582533,12.));
#91910=CARTESIAN_POINT('Ctrl Pts',(-54.8807462065164,44.6441125999063,12.));
#91911=CARTESIAN_POINT('Ctrl Pts',(-54.860965541796,44.6360539967392,12.));
#91912=CARTESIAN_POINT('Ctrl Pts',(-54.8412386665276,44.6279934801169,12.));
#91913=CARTESIAN_POINT('Ctrl Pts',(-54.8215656991837,44.6199311823293,12.));
#91914=CARTESIAN_POINT('Ctrl Pts',(-54.8019467588278,44.6118672364906,12.));
#91915=CARTESIAN_POINT('Ctrl Pts',(-54.7823819650149,44.6038017764309,12.));
#91916=CARTESIAN_POINT('Ctrl Pts',(-54.7628714377037,44.5957349366059,12.));
#91917=CARTESIAN_POINT('Ctrl Pts',(-54.7434152971267,44.5876668519661,12.));
#91918=CARTESIAN_POINT('Ctrl Pts',(-54.7240136637717,44.5795976579454,12.));
#91919=CARTESIAN_POINT('Ctrl Pts',(-54.7046666586754,44.5715274907619,12.));
#91920=CARTESIAN_POINT('Ctrl Pts',(-54.6853744036751,44.5634564876863,12.));
#91921=CARTESIAN_POINT('Ctrl Pts',(-54.6661370216252,44.5553847872721,12.));
#91922=CARTESIAN_POINT('Ctrl Pts',(-54.6469546367408,44.5473125297311,12.));
#91923=CARTESIAN_POINT('Ctrl Pts',(-54.6278273743587,44.5392398566802,12.));
#91924=CARTESIAN_POINT('Ctrl Pts',(-54.6087553602914,44.5311669104515,12.));
#91925=CARTESIAN_POINT('Ctrl Pts',(-54.5897387202815,44.5230938335167,12.));
#91926=CARTESIAN_POINT('Ctrl Pts',(-54.5707775794412,44.5150207678988,12.));
#91927=CARTESIAN_POINT('Ctrl Pts',(-54.5518720616016,44.5069478544945,12.));
#91928=CARTESIAN_POINT('Ctrl Pts',(-54.5330222905438,44.4988752343715,12.));
#91929=CARTESIAN_POINT('Ctrl Pts',(-54.5142283914684,44.4908030503209,12.));
#91930=CARTESIAN_POINT('Ctrl Pts',(-54.4954904921938,44.482731448127,12.));
#91931=CARTESIAN_POINT('Ctrl Pts',(-54.4768087248854,44.4746605784056,12.));
#91932=CARTESIAN_POINT('Ctrl Pts',(-54.4581832262072,44.4665905967701,12.));
#91933=CARTESIAN_POINT('Ctrl Pts',(-54.4396141337008,44.4585216599933,12.));
#91934=CARTESIAN_POINT('Ctrl Pts',(-54.4211015825959,44.4504539226336,12.));
#91935=CARTESIAN_POINT('Ctrl Pts',(-54.4026457030316,44.442387534098,12.));
#91936=CARTESIAN_POINT('Ctrl Pts',(-54.3842466156151,44.4343226339555,12.));
#91937=CARTESIAN_POINT('Ctrl Pts',(-54.3659044357064,44.4262593564664,12.));
#91938=CARTESIAN_POINT('Ctrl Pts',(-54.347619281931,44.4181978395814,12.));
#91939=CARTESIAN_POINT('Ctrl Pts',(-54.3293912830237,44.4101382321834,12.));
#91940=CARTESIAN_POINT('Ctrl Pts',(-54.3112205860776,44.4020807028144,12.));
#91941=CARTESIAN_POINT('Ctrl Pts',(-54.2931073621661,44.3940254456427,12.));
#91942=CARTESIAN_POINT('Ctrl Pts',(-54.2750517888695,44.3859726620288,12.));
#91943=CARTESIAN_POINT('Ctrl Pts',(-54.2570540336536,44.3779225430461,12.));
#91944=CARTESIAN_POINT('Ctrl Pts',(-54.2391142386354,44.369875253351,12.));
#91945=CARTESIAN_POINT('Ctrl Pts',(-54.2212325005847,44.3618309103245,12.));
#91946=CARTESIAN_POINT('Ctrl Pts',(-54.203408870162,44.3537895823819,12.));
#91947=CARTESIAN_POINT('Ctrl Pts',(-54.1891964684439,44.3473589597468,12.));
#91948=CARTESIAN_POINT('Ctrl Pts',(-54.1785633257456,44.3425373700829,12.));
#91949=CARTESIAN_POINT('Ctrl Pts',(-54.1714861895278,44.3393235891014,12.));
#91950=CARTESIAN_POINT('Ctrl Pts',(-54.1679505278134,44.3377168516418,12.));
#91951=CARTESIAN_POINT('Ctrl Pts',(-59.3276657444392,44.5696260757792,-1.11022302462516E-15));
#91952=CARTESIAN_POINT('Ctrl Pts',(-59.3276657444392,44.5696260757792,4.));
#91953=CARTESIAN_POINT('Ctrl Pts',(-59.3276657444392,44.5696260757792,8.));
#91954=CARTESIAN_POINT('Ctrl Pts',(-59.3276657444392,44.5696260757792,12.));
#91955=CARTESIAN_POINT('Ctrl Pts',(-59.3806648691719,44.6658822400933,-1.11022302462516E-15));
#91956=CARTESIAN_POINT('Ctrl Pts',(-59.3806648691719,44.6658822400933,4.));
#91957=CARTESIAN_POINT('Ctrl Pts',(-59.3806648691719,44.6658822400933,8.));
#91958=CARTESIAN_POINT('Ctrl Pts',(-59.3806648691719,44.6658822400933,12.));
#91959=CARTESIAN_POINT('Ctrl Pts',(-59.4154499491518,44.8655383388341,-1.03713949455603E-15));
#91960=CARTESIAN_POINT('Ctrl Pts',(-59.4154499491518,44.8655383388341,4.));
#91961=CARTESIAN_POINT('Ctrl Pts',(-59.4154499491518,44.8655383388341,7.99999999999999));
#91962=CARTESIAN_POINT('Ctrl Pts',(-59.4154499491518,44.8655383388341,12.));
#91963=CARTESIAN_POINT('Ctrl Pts',(-59.3374774995081,45.047980595232,-8.63611844427577E-16));
#91964=CARTESIAN_POINT('Ctrl Pts',(-59.3374774995081,45.047980595232,4.));
#91965=CARTESIAN_POINT('Ctrl Pts',(-59.3374774995081,45.0479805952321,8.00000000000001));
#91966=CARTESIAN_POINT('Ctrl Pts',(-59.3374774995081,45.0479805952321,12.));
#91967=CARTESIAN_POINT('Ctrl Pts',(-59.2875729049565,45.1135644683452,-7.79957864199761E-16));
#91968=CARTESIAN_POINT('Ctrl Pts',(-59.2875729049565,45.1135644683452,4.));
#91969=CARTESIAN_POINT('Ctrl Pts',(-59.2875729049565,45.1135644683452,8.));
#91970=CARTESIAN_POINT('Ctrl Pts',(-59.2875729049565,45.1135644683452,12.));
#91971=CARTESIAN_POINT('',(-59.3276657444392,44.5696260757792,2.77555756156289E-16));
#91972=CARTESIAN_POINT('',(-59.2875729049561,45.1135644683449,2.77555756156289E-16));
#91973=CARTESIAN_POINT('Ctrl Pts',(-59.3276657444392,44.5696260757792,-3.21795698712167E-17));
#91974=CARTESIAN_POINT('Ctrl Pts',(-59.3806648691719,44.6658822400933,-3.2179569871217E-17));
#91975=CARTESIAN_POINT('Ctrl Pts',(-59.4005420577319,44.7799714393737,9.58244731114085E-18));
#91976=CARTESIAN_POINT('Ctrl Pts',(-59.3836004611086,44.8884397921749,8.41425445128705E-17));
#91977=CARTESIAN_POINT('Ctrl Pts',(-59.3708942636411,44.9697910567758,1.40062617414167E-16));
#91978=CARTESIAN_POINT('Ctrl Pts',(-59.3374774995081,45.047980595232,2.14431610326361E-16));
#91979=CARTESIAN_POINT('Ctrl Pts',(-59.2875729049565,45.1135644683452,2.98085590554179E-16));
#91980=CARTESIAN_POINT('',(-59.2875729049561,45.1135644683449,12.));
#91981=CARTESIAN_POINT('Ctrl Pts',(-59.2875729049565,45.1135644683452,-7.79957864199761E-16));
#91982=CARTESIAN_POINT('Ctrl Pts',(-59.2875729049565,45.1135644683452,4.));
#91983=CARTESIAN_POINT('Ctrl Pts',(-59.2875729049565,45.1135644683452,8.));
#91984=CARTESIAN_POINT('Ctrl Pts',(-59.2875729049565,45.1135644683452,12.));
#91985=CARTESIAN_POINT('',(-59.3276657444392,44.5696260757792,12.));
#91986=CARTESIAN_POINT('Ctrl Pts',(-59.2875729049565,45.1135644683452,12.));
#91987=CARTESIAN_POINT('Ctrl Pts',(-59.3374774995081,45.0479805952321,12.));
#91988=CARTESIAN_POINT('Ctrl Pts',(-59.3708942636412,44.9697910567758,12.));
#91989=CARTESIAN_POINT('Ctrl Pts',(-59.3836004611086,44.8884397921749,12.));
#91990=CARTESIAN_POINT('Ctrl Pts',(-59.4005420577319,44.7799714393738,12.));
#91991=CARTESIAN_POINT('Ctrl Pts',(-59.3806648691719,44.6658822400933,12.));
#91992=CARTESIAN_POINT('Ctrl Pts',(-59.3276657444392,44.5696260757792,12.));
#91993=CARTESIAN_POINT('Ctrl Pts',(-59.3276657444392,44.5696260757792,12.));
#91994=CARTESIAN_POINT('Ctrl Pts',(-59.3276657444392,44.5696260757792,8.));
#91995=CARTESIAN_POINT('Ctrl Pts',(-59.3276657444392,44.5696260757792,4.));
#91996=CARTESIAN_POINT('Ctrl Pts',(-59.3276657444392,44.5696260757792,-1.11022302462516E-15));
#91997=CARTESIAN_POINT('Origin',(-2.97443977737815E-10,2.28111678886296E-10,
0.));
#91998=CARTESIAN_POINT('Origin',(-2.97443977737815E-10,2.28111678886296E-10,
12.));
#91999=CARTESIAN_POINT('Origin',(-2.97443977737815E-10,2.28111678886296E-10,
0.));
#92000=CARTESIAN_POINT('Ctrl Pts',(-54.7233670476849,50.5529731960876,0.));
#92001=CARTESIAN_POINT('Ctrl Pts',(-54.7233670476849,50.5529731960876,4.));
#92002=CARTESIAN_POINT('Ctrl Pts',(-54.7233670476849,50.5529731960876,8.));
#92003=CARTESIAN_POINT('Ctrl Pts',(-54.7233670476849,50.5529731960876,12.));
#92004=CARTESIAN_POINT('Ctrl Pts',(-54.6488048279283,50.6336864649947,0.));
#92005=CARTESIAN_POINT('Ctrl Pts',(-54.6488048279283,50.6336864649947,4.));
#92006=CARTESIAN_POINT('Ctrl Pts',(-54.6488048279283,50.6336864649947,8.));
#92007=CARTESIAN_POINT('Ctrl Pts',(-54.6488048279283,50.6336864649947,12.));
#92008=CARTESIAN_POINT('Ctrl Pts',(-54.4703879751555,50.7298112257545,0.));
#92009=CARTESIAN_POINT('Ctrl Pts',(-54.4703879751555,50.7298112257545,4.00000000000001));
#92010=CARTESIAN_POINT('Ctrl Pts',(-54.4703879751555,50.7298112257545,8.));
#92011=CARTESIAN_POINT('Ctrl Pts',(-54.4703879751555,50.7298112257545,12.));
#92012=CARTESIAN_POINT('Ctrl Pts',(-54.2726521137411,50.7135202769403,0.));
#92013=CARTESIAN_POINT('Ctrl Pts',(-54.2726521137411,50.7135202769403,4.));
#92014=CARTESIAN_POINT('Ctrl Pts',(-54.2726521137411,50.7135202769403,8.));
#92015=CARTESIAN_POINT('Ctrl Pts',(-54.2726521137411,50.7135202769403,12.));
#92016=CARTESIAN_POINT('Ctrl Pts',(-54.1946543499979,50.6869108458687,0.));
#92017=CARTESIAN_POINT('Ctrl Pts',(-54.1946543499979,50.6869108458687,4.));
#92018=CARTESIAN_POINT('Ctrl Pts',(-54.1946543499979,50.6869108458687,8.));
#92019=CARTESIAN_POINT('Ctrl Pts',(-54.1946543499979,50.6869108458687,12.));
#92020=CARTESIAN_POINT('',(-54.7233670476849,50.5529731960876,0.));
#92021=CARTESIAN_POINT('',(-54.1946543499978,50.6869108458688,0.));
#92022=CARTESIAN_POINT('Ctrl Pts',(-54.7233670476849,50.5529731960876,1.38777878078145E-16));
#92023=CARTESIAN_POINT('Ctrl Pts',(-54.6488048279283,50.6336864649947,1.38777878078144E-16));
#92024=CARTESIAN_POINT('Ctrl Pts',(-54.5468523406296,50.6886148997146,1.38777878078145E-16));
#92025=CARTESIAN_POINT('Ctrl Pts',(-54.4385916056111,50.7068361639613,1.38777878078145E-16));
#92026=CARTESIAN_POINT('Ctrl Pts',(-54.3573960543472,50.7205021121464,1.38777878078145E-16));
#92027=CARTESIAN_POINT('Ctrl Pts',(-54.2726521137411,50.7135202769403,1.38777878078144E-16));
#92028=CARTESIAN_POINT('Ctrl Pts',(-54.1946543499979,50.6869108458687,1.38777878078145E-16));
#92029=CARTESIAN_POINT('',(-54.1946543499978,50.6869108458688,12.));
#92030=CARTESIAN_POINT('Ctrl Pts',(-54.1946543499979,50.6869108458687,0.));
#92031=CARTESIAN_POINT('Ctrl Pts',(-54.1946543499979,50.6869108458687,4.));
#92032=CARTESIAN_POINT('Ctrl Pts',(-54.1946543499979,50.6869108458687,8.));
#92033=CARTESIAN_POINT('Ctrl Pts',(-54.1946543499979,50.6869108458687,12.));
#92034=CARTESIAN_POINT('',(-54.7233670476849,50.5529731960876,12.));
#92035=CARTESIAN_POINT('Ctrl Pts',(-54.1946543499979,50.6869108458687,12.));
#92036=CARTESIAN_POINT('Ctrl Pts',(-54.2726521137411,50.7135202769403,12.));
#92037=CARTESIAN_POINT('Ctrl Pts',(-54.3573960543472,50.7205021121464,12.));
#92038=CARTESIAN_POINT('Ctrl Pts',(-54.4385916056111,50.7068361639613,12.));
#92039=CARTESIAN_POINT('Ctrl Pts',(-54.5468523406296,50.6886148997146,12.));
#92040=CARTESIAN_POINT('Ctrl Pts',(-54.6488048279283,50.6336864649947,12.));
#92041=CARTESIAN_POINT('Ctrl Pts',(-54.7233670476849,50.5529731960876,12.));
#92042=CARTESIAN_POINT('Ctrl Pts',(-54.7233670476849,50.5529731960876,12.));
#92043=CARTESIAN_POINT('Ctrl Pts',(-54.7233670476849,50.5529731960876,8.));
#92044=CARTESIAN_POINT('Ctrl Pts',(-54.7233670476849,50.5529731960876,4.));
#92045=CARTESIAN_POINT('Ctrl Pts',(-54.7233670476849,50.5529731960876,0.));
#92046=CARTESIAN_POINT('Ctrl Pts',(-50.0975384783634,48.8900464144686,0.));
#92047=CARTESIAN_POINT('Ctrl Pts',(-50.0975384783634,48.8900464144686,12.));
#92048=CARTESIAN_POINT('Ctrl Pts',(-50.1009206494209,48.8919551910299,0.));
#92049=CARTESIAN_POINT('Ctrl Pts',(-50.1009206494209,48.8919551910299,12.));
#92050=CARTESIAN_POINT('Ctrl Pts',(-50.1076907555303,48.8957735556681,0.));
#92051=CARTESIAN_POINT('Ctrl Pts',(-50.1076907555303,48.8957735556681,12.));
#92052=CARTESIAN_POINT('Ctrl Pts',(-50.1178632066821,48.9015035371772,0.));
#92053=CARTESIAN_POINT('Ctrl Pts',(-50.1178632066821,48.9015035371772,12.));
#92054=CARTESIAN_POINT('Ctrl Pts',(-50.1314610602286,48.9091483817797,0.));
#92055=CARTESIAN_POINT('Ctrl Pts',(-50.1314610602286,48.9091483817797,12.));
#92056=CARTESIAN_POINT('Ctrl Pts',(-50.148516018447,48.9187125417897,0.));
#92057=CARTESIAN_POINT('Ctrl Pts',(-50.148516018447,48.9187125417897,12.));
#92058=CARTESIAN_POINT('Ctrl Pts',(-50.1656286003943,48.9282847698237,0.));
#92059=CARTESIAN_POINT('Ctrl Pts',(-50.1656286003943,48.9282847698237,12.));
#92060=CARTESIAN_POINT('Ctrl Pts',(-50.1827987615659,48.9378649933116,0.));
#92061=CARTESIAN_POINT('Ctrl Pts',(-50.1827987615659,48.9378649933116,12.));
#92062=CARTESIAN_POINT('Ctrl Pts',(-50.2000264157903,48.9474530868847,0.));
#92063=CARTESIAN_POINT('Ctrl Pts',(-50.2000264157903,48.9474530868847,12.));
#92064=CARTESIAN_POINT('Ctrl Pts',(-50.2173114358423,48.9570488741273,0.));
#92065=CARTESIAN_POINT('Ctrl Pts',(-50.2173114358423,48.9570488741273,12.));
#92066=CARTESIAN_POINT('Ctrl Pts',(-50.2346536715465,48.9666521500969,0.));
#92067=CARTESIAN_POINT('Ctrl Pts',(-50.2346536715465,48.9666521500969,12.));
#92068=CARTESIAN_POINT('Ctrl Pts',(-50.252052963548,48.9762626987227,0.));
#92069=CARTESIAN_POINT('Ctrl Pts',(-50.252052963548,48.9762626987227,12.));
#92070=CARTESIAN_POINT('Ctrl Pts',(-50.2695091583473,48.9858803116649,0.));
#92071=CARTESIAN_POINT('Ctrl Pts',(-50.2695091583473,48.9858803116649,12.));
#92072=CARTESIAN_POINT('Ctrl Pts',(-50.2870221241003,48.9955048082028,0.));
#92073=CARTESIAN_POINT('Ctrl Pts',(-50.2870221241003,48.9955048082028,12.));
#92074=CARTESIAN_POINT('Ctrl Pts',(-50.3045917455383,49.0051360288002,0.));
#92075=CARTESIAN_POINT('Ctrl Pts',(-50.3045917455383,49.0051360288002,12.));
#92076=CARTESIAN_POINT('Ctrl Pts',(-50.3222179165102,49.0147738256925,0.));
#92077=CARTESIAN_POINT('Ctrl Pts',(-50.3222179165102,49.0147738256925,12.));
#92078=CARTESIAN_POINT('Ctrl Pts',(-50.3399005337967,49.0244180550759,0.));
#92079=CARTESIAN_POINT('Ctrl Pts',(-50.3399005337967,49.0244180550759,12.));
#92080=CARTESIAN_POINT('Ctrl Pts',(-50.3576394894136,49.034068567401,0.));
#92081=CARTESIAN_POINT('Ctrl Pts',(-50.3576394894136,49.034068567401,12.));
#92082=CARTESIAN_POINT('Ctrl Pts',(-50.3754346667389,49.0437252024868,0.));
#92083=CARTESIAN_POINT('Ctrl Pts',(-50.3754346667389,49.0437252024868,12.));
#92084=CARTESIAN_POINT('Ctrl Pts',(-50.393285944528,49.0533877945771,0.));
#92085=CARTESIAN_POINT('Ctrl Pts',(-50.393285944528,49.0533877945771,12.));
#92086=CARTESIAN_POINT('Ctrl Pts',(-50.4111931994264,49.0630561755082,0.));
#92087=CARTESIAN_POINT('Ctrl Pts',(-50.4111931994264,49.0630561755082,12.));
#92088=CARTESIAN_POINT('Ctrl Pts',(-50.4291563088528,49.0727301783477,0.));
#92089=CARTESIAN_POINT('Ctrl Pts',(-50.4291563088528,49.0727301783477,12.));
#92090=CARTESIAN_POINT('Ctrl Pts',(-50.4471751542717,49.0824096415339,0.));
#92091=CARTESIAN_POINT('Ctrl Pts',(-50.4471751542717,49.0824096415339,12.));
#92092=CARTESIAN_POINT('Ctrl Pts',(-50.465249621057,49.0920944086973,0.));
#92093=CARTESIAN_POINT('Ctrl Pts',(-50.465249621057,49.0920944086973,12.));
#92094=CARTESIAN_POINT('Ctrl Pts',(-50.4833795969296,49.1017843266782,0.));
#92095=CARTESIAN_POINT('Ctrl Pts',(-50.4833795969296,49.1017843266782,12.));
#92096=CARTESIAN_POINT('Ctrl Pts',(-50.5015649708742,49.1114792441573,0.));
#92097=CARTESIAN_POINT('Ctrl Pts',(-50.5015649708742,49.1114792441573,12.));
#92098=CARTESIAN_POINT('Ctrl Pts',(-50.5198056318111,49.1211790099817,0.));
#92099=CARTESIAN_POINT('Ctrl Pts',(-50.5198056318111,49.1211790099817,12.));
#92100=CARTESIAN_POINT('Ctrl Pts',(-50.5381014674822,49.1308834717645,0.));
#92101=CARTESIAN_POINT('Ctrl Pts',(-50.5381014674822,49.1308834717645,12.));
#92102=CARTESIAN_POINT('Ctrl Pts',(-50.5564523650406,49.1405924766169,0.));
#92103=CARTESIAN_POINT('Ctrl Pts',(-50.5564523650406,49.1405924766169,12.));
#92104=CARTESIAN_POINT('Ctrl Pts',(-50.5748582115575,49.1503058717831,0.));
#92105=CARTESIAN_POINT('Ctrl Pts',(-50.5748582115575,49.1503058717831,12.));
#92106=CARTESIAN_POINT('Ctrl Pts',(-50.593318894516,49.1600235052613,0.));
#92107=CARTESIAN_POINT('Ctrl Pts',(-50.593318894516,49.1600235052613,12.));
#92108=CARTESIAN_POINT('Ctrl Pts',(-50.6118343023937,49.1697452265473,0.));
#92109=CARTESIAN_POINT('Ctrl Pts',(-50.6118343023937,49.1697452265473,12.));
#92110=CARTESIAN_POINT('Ctrl Pts',(-50.6304043248796,49.1794708869074,0.));
#92111=CARTESIAN_POINT('Ctrl Pts',(-50.6304043248796,49.1794708869074,12.));
#92112=CARTESIAN_POINT('Ctrl Pts',(-50.6490288525639,49.1892003389743,0.));
#92113=CARTESIAN_POINT('Ctrl Pts',(-50.6490288525639,49.1892003389743,12.));
#92114=CARTESIAN_POINT('Ctrl Pts',(-50.6677077767427,49.1989334364991,0.));
#92115=CARTESIAN_POINT('Ctrl Pts',(-50.6677077767427,49.1989334364991,12.));
#92116=CARTESIAN_POINT('Ctrl Pts',(-50.6864409891905,49.2086700340625,0.));
#92117=CARTESIAN_POINT('Ctrl Pts',(-50.6864409891905,49.2086700340625,12.));
#92118=CARTESIAN_POINT('Ctrl Pts',(-50.7052283818941,49.218409986748,0.));
#92119=CARTESIAN_POINT('Ctrl Pts',(-50.7052283818941,49.218409986748,12.));
#92120=CARTESIAN_POINT('Ctrl Pts',(-50.7240698470698,49.2281531501569,0.));
#92121=CARTESIAN_POINT('Ctrl Pts',(-50.7240698470698,49.2281531501569,12.));
#92122=CARTESIAN_POINT('Ctrl Pts',(-50.7429652772816,49.2378993805482,0.));
#92123=CARTESIAN_POINT('Ctrl Pts',(-50.7429652772816,49.2378993805482,12.));
#92124=CARTESIAN_POINT('Ctrl Pts',(-50.7619145655207,49.2476485349373,0.));
#92125=CARTESIAN_POINT('Ctrl Pts',(-50.7619145655207,49.2476485349373,12.));
#92126=CARTESIAN_POINT('Ctrl Pts',(-50.7809176052954,49.2574004712122,0.));
#92127=CARTESIAN_POINT('Ctrl Pts',(-50.7809176052954,49.2574004712122,12.));
#92128=CARTESIAN_POINT('Ctrl Pts',(-50.7999742907111,49.2671550482415,0.));
#92129=CARTESIAN_POINT('Ctrl Pts',(-50.7999742907111,49.2671550482415,12.));
#92130=CARTESIAN_POINT('Ctrl Pts',(-50.8190845164319,49.2769121258144,0.));
#92131=CARTESIAN_POINT('Ctrl Pts',(-50.8190845164319,49.2769121258144,12.));
#92132=CARTESIAN_POINT('Ctrl Pts',(-50.8382481776392,49.2866715645828,0.));
#92133=CARTESIAN_POINT('Ctrl Pts',(-50.8382481776392,49.2866715645828,12.));
#92134=CARTESIAN_POINT('Ctrl Pts',(-50.8574651699877,49.2964332260043,0.));
#92135=CARTESIAN_POINT('Ctrl Pts',(-50.8574651699877,49.2964332260043,12.));
#92136=CARTESIAN_POINT('Ctrl Pts',(-50.8767353895509,49.3061969722798,0.));
#92137=CARTESIAN_POINT('Ctrl Pts',(-50.8767353895509,49.3061969722798,12.));
#92138=CARTESIAN_POINT('Ctrl Pts',(-50.8960587327869,49.3159626663129,0.));
#92139=CARTESIAN_POINT('Ctrl Pts',(-50.8960587327869,49.3159626663129,12.));
#92140=CARTESIAN_POINT('Ctrl Pts',(-50.9154350965681,49.325730171735,0.));
#92141=CARTESIAN_POINT('Ctrl Pts',(-50.9154350965681,49.325730171735,12.));
#92142=CARTESIAN_POINT('Ctrl Pts',(-50.9348643781928,49.3354993529163,0.));
#92143=CARTESIAN_POINT('Ctrl Pts',(-50.9348643781928,49.3354993529163,12.));
#92144=CARTESIAN_POINT('Ctrl Pts',(-50.9543464753974,49.3452700749804,0.));
#92145=CARTESIAN_POINT('Ctrl Pts',(-50.9543464753974,49.3452700749804,12.));
#92146=CARTESIAN_POINT('Ctrl Pts',(-50.9738812863636,49.3550422038221,0.));
#92147=CARTESIAN_POINT('Ctrl Pts',(-50.9738812863636,49.3550422038221,12.));
#92148=CARTESIAN_POINT('Ctrl Pts',(-50.9934687097179,49.3648156061049,0.));
#92149=CARTESIAN_POINT('Ctrl Pts',(-50.9934687097179,49.3648156061049,12.));
#92150=CARTESIAN_POINT('Ctrl Pts',(-51.0131086445268,49.3745901492428,0.));
#92151=CARTESIAN_POINT('Ctrl Pts',(-51.0131086445268,49.3745901492428,12.));
#92152=CARTESIAN_POINT('Ctrl Pts',(-51.0328009902857,49.3843657013851,0.));
#92153=CARTESIAN_POINT('Ctrl Pts',(-51.0328009902857,49.3843657013851,12.));
#92154=CARTESIAN_POINT('Ctrl Pts',(-51.0525456469072,49.3941421314014,0.));
#92155=CARTESIAN_POINT('Ctrl Pts',(-51.0525456469072,49.3941421314014,12.));
#92156=CARTESIAN_POINT('Ctrl Pts',(-51.0723425146987,49.4039193088635,0.));
#92157=CARTESIAN_POINT('Ctrl Pts',(-51.0723425146987,49.4039193088635,12.));
#92158=CARTESIAN_POINT('Ctrl Pts',(-51.0921914943663,49.4136971040428,0.));
#92159=CARTESIAN_POINT('Ctrl Pts',(-51.0921914943663,49.4136971040428,12.));
#92160=CARTESIAN_POINT('Ctrl Pts',(-51.1120924870196,49.4234753879071,0.));
#92161=CARTESIAN_POINT('Ctrl Pts',(-51.1120924870196,49.4234753879071,12.));
#92162=CARTESIAN_POINT('Ctrl Pts',(-51.1320453941702,49.4332540321178,0.));
#92163=CARTESIAN_POINT('Ctrl Pts',(-51.1320453941702,49.4332540321178,12.));
#92164=CARTESIAN_POINT('Ctrl Pts',(-51.1520501177291,49.4430329090288,0.));
#92165=CARTESIAN_POINT('Ctrl Pts',(-51.1520501177291,49.4430329090288,12.));
#92166=CARTESIAN_POINT('Ctrl Pts',(-51.1721065599972,49.4528118916833,0.));
#92167=CARTESIAN_POINT('Ctrl Pts',(-51.1721065599972,49.4528118916833,12.));
#92168=CARTESIAN_POINT('Ctrl Pts',(-51.1922146236686,49.4625908538076,0.));
#92169=CARTESIAN_POINT('Ctrl Pts',(-51.1922146236686,49.4625908538076,12.));
#92170=CARTESIAN_POINT('Ctrl Pts',(-51.2123742118288,49.4723696698022,0.));
#92171=CARTESIAN_POINT('Ctrl Pts',(-51.2123742118288,49.4723696698022,12.));
#92172=CARTESIAN_POINT('Ctrl Pts',(-51.2325852279507,49.4821482147357,0.));
#92173=CARTESIAN_POINT('Ctrl Pts',(-51.2325852279507,49.4821482147357,12.));
#92174=CARTESIAN_POINT('Ctrl Pts',(-51.2528475758841,49.4919263643357,0.));
#92175=CARTESIAN_POINT('Ctrl Pts',(-51.2528475758841,49.4919263643357,12.));
#92176=CARTESIAN_POINT('Ctrl Pts',(-51.2731611598465,49.5017039949841,0.));
#92177=CARTESIAN_POINT('Ctrl Pts',(-51.2731611598465,49.5017039949841,12.));
#92178=CARTESIAN_POINT('Ctrl Pts',(-51.2935258844278,49.5114809837111,0.));
#92179=CARTESIAN_POINT('Ctrl Pts',(-51.2935258844278,49.5114809837111,12.));
#92180=CARTESIAN_POINT('Ctrl Pts',(-51.3139416545903,49.5212572081901,0.));
#92181=CARTESIAN_POINT('Ctrl Pts',(-51.3139416545903,49.5212572081901,12.));
#92182=CARTESIAN_POINT('Ctrl Pts',(-51.3344083756659,49.5310325467334,0.));
#92183=CARTESIAN_POINT('Ctrl Pts',(-51.3344083756659,49.5310325467334,12.));
#92184=CARTESIAN_POINT('Ctrl Pts',(-51.354925953347,49.5408068782871,0.));
#92185=CARTESIAN_POINT('Ctrl Pts',(-51.354925953347,49.5408068782871,12.));
#92186=CARTESIAN_POINT('Ctrl Pts',(-51.3754942936796,49.5505800824268,0.));
#92187=CARTESIAN_POINT('Ctrl Pts',(-51.3754942936796,49.5505800824268,12.));
#92188=CARTESIAN_POINT('Ctrl Pts',(-51.3961133030688,49.5603520393514,0.));
#92189=CARTESIAN_POINT('Ctrl Pts',(-51.3961133030688,49.5603520393514,12.));
#92190=CARTESIAN_POINT('Ctrl Pts',(-51.4167828882765,49.5701226298779,0.));
#92191=CARTESIAN_POINT('Ctrl Pts',(-51.4167828882765,49.5701226298779,12.));
#92192=CARTESIAN_POINT('Ctrl Pts',(-51.4375029564191,49.579891735436,0.));
#92193=CARTESIAN_POINT('Ctrl Pts',(-51.4375029564191,49.579891735436,12.));
#92194=CARTESIAN_POINT('Ctrl Pts',(-51.4582734149562,49.5896592380634,0.));
#92195=CARTESIAN_POINT('Ctrl Pts',(-51.4582734149562,49.5896592380634,12.));
#92196=CARTESIAN_POINT('Ctrl Pts',(-51.4790941716859,49.5994250204003,0.));
#92197=CARTESIAN_POINT('Ctrl Pts',(-51.4790941716859,49.5994250204003,12.));
#92198=CARTESIAN_POINT('Ctrl Pts',(-51.4999651347496,49.609188965684,0.));
#92199=CARTESIAN_POINT('Ctrl Pts',(-51.4999651347496,49.609188965684,12.));
#92200=CARTESIAN_POINT('Ctrl Pts',(-51.5208862126303,49.6189509577441,0.));
#92201=CARTESIAN_POINT('Ctrl Pts',(-51.5208862126303,49.6189509577441,12.));
#92202=CARTESIAN_POINT('Ctrl Pts',(-51.5418573141494,49.6287108809975,0.));
#92203=CARTESIAN_POINT('Ctrl Pts',(-51.5418573141494,49.6287108809975,12.));
#92204=CARTESIAN_POINT('Ctrl Pts',(-51.5628783484556,49.6384686204443,0.));
#92205=CARTESIAN_POINT('Ctrl Pts',(-51.5628783484556,49.6384686204443,12.));
#92206=CARTESIAN_POINT('Ctrl Pts',(-51.5839492250218,49.6482240616627,0.));
#92207=CARTESIAN_POINT('Ctrl Pts',(-51.5839492250218,49.6482240616627,12.));
#92208=CARTESIAN_POINT('Ctrl Pts',(-51.6050698536525,49.6579770908063,0.));
#92209=CARTESIAN_POINT('Ctrl Pts',(-51.6050698536525,49.6579770908063,12.));
#92210=CARTESIAN_POINT('Ctrl Pts',(-51.6262401444799,49.6677275945975,0.));
#92211=CARTESIAN_POINT('Ctrl Pts',(-51.6262401444799,49.6677275945975,12.));
#92212=CARTESIAN_POINT('Ctrl Pts',(-51.6474600079611,49.6774754603235,0.));
#92213=CARTESIAN_POINT('Ctrl Pts',(-51.6474600079611,49.6774754603235,12.));
#92214=CARTESIAN_POINT('Ctrl Pts',(-51.6687293548656,49.6872205758314,0.));
#92215=CARTESIAN_POINT('Ctrl Pts',(-51.6687293548656,49.6872205758314,12.));
#92216=CARTESIAN_POINT('Ctrl Pts',(-51.6900480962744,49.6969628295236,0.));
#92217=CARTESIAN_POINT('Ctrl Pts',(-51.6900480962744,49.6969628295236,12.));
#92218=CARTESIAN_POINT('Ctrl Pts',(-51.7114161435848,49.7067021103534,0.));
#92219=CARTESIAN_POINT('Ctrl Pts',(-51.7114161435848,49.7067021103534,12.));
#92220=CARTESIAN_POINT('Ctrl Pts',(-51.7328334085084,49.7164383078206,0.));
#92221=CARTESIAN_POINT('Ctrl Pts',(-51.7328334085084,49.7164383078206,12.));
#92222=CARTESIAN_POINT('Ctrl Pts',(-51.754299803068,49.7261713119672,0.));
#92223=CARTESIAN_POINT('Ctrl Pts',(-51.754299803068,49.7261713119672,12.));
#92224=CARTESIAN_POINT('Ctrl Pts',(-51.7758152395857,49.7359010133741,0.));
#92225=CARTESIAN_POINT('Ctrl Pts',(-51.7758152395857,49.7359010133741,12.));
#92226=CARTESIAN_POINT('Ctrl Pts',(-51.7973796306826,49.7456273031555,0.));
#92227=CARTESIAN_POINT('Ctrl Pts',(-51.7973796306826,49.7456273031555,12.));
#92228=CARTESIAN_POINT('Ctrl Pts',(-51.8189928892841,49.7553500729563,0.));
#92229=CARTESIAN_POINT('Ctrl Pts',(-51.8189928892841,49.7553500729563,12.));
#92230=CARTESIAN_POINT('Ctrl Pts',(-51.8406549286177,49.7650692149464,0.));
#92231=CARTESIAN_POINT('Ctrl Pts',(-51.8406549286177,49.7650692149464,12.));
#92232=CARTESIAN_POINT('Ctrl Pts',(-51.8623656622092,49.7747846218177,0.));
#92233=CARTESIAN_POINT('Ctrl Pts',(-51.8623656622092,49.7747846218177,12.));
#92234=CARTESIAN_POINT('Ctrl Pts',(-51.8841250038716,49.78449618678,0.));
#92235=CARTESIAN_POINT('Ctrl Pts',(-51.8841250038716,49.78449618678,12.));
#92236=CARTESIAN_POINT('Ctrl Pts',(-51.9059328677051,49.7942038035568,0.));
#92237=CARTESIAN_POINT('Ctrl Pts',(-51.9059328677051,49.7942038035568,12.));
#92238=CARTESIAN_POINT('Ctrl Pts',(-51.9277891681014,49.8039073663808,0.));
#92239=CARTESIAN_POINT('Ctrl Pts',(-51.9277891681014,49.8039073663808,12.));
#92240=CARTESIAN_POINT('Ctrl Pts',(-51.9496938197418,49.8136067699896,0.));
#92241=CARTESIAN_POINT('Ctrl Pts',(-51.9496938197418,49.8136067699896,12.));
#92242=CARTESIAN_POINT('Ctrl Pts',(-51.9716467375938,49.8233019096224,0.));
#92243=CARTESIAN_POINT('Ctrl Pts',(-51.9716467375938,49.8233019096224,12.));
#92244=CARTESIAN_POINT('Ctrl Pts',(-51.9936478369008,49.8329926810172,0.));
#92245=CARTESIAN_POINT('Ctrl Pts',(-51.9936478369008,49.8329926810172,12.));
#92246=CARTESIAN_POINT('Ctrl Pts',(-52.015697033182,49.8426789804068,0.));
#92247=CARTESIAN_POINT('Ctrl Pts',(-52.015697033182,49.8426789804068,12.));
#92248=CARTESIAN_POINT('Ctrl Pts',(-52.0377942422373,49.8523607045146,0.));
#92249=CARTESIAN_POINT('Ctrl Pts',(-52.0377942422373,49.8523607045146,12.));
#92250=CARTESIAN_POINT('Ctrl Pts',(-52.059939380145,49.8620377505498,0.));
#92251=CARTESIAN_POINT('Ctrl Pts',(-52.059939380145,49.8620377505498,12.));
#92252=CARTESIAN_POINT('Ctrl Pts',(-52.0821323632588,49.871710016205,0.));
#92253=CARTESIAN_POINT('Ctrl Pts',(-52.0821323632588,49.871710016205,12.));
#92254=CARTESIAN_POINT('Ctrl Pts',(-52.1043731081968,49.8813773996523,0.));
#92255=CARTESIAN_POINT('Ctrl Pts',(-52.1043731081968,49.8813773996523,12.));
#92256=CARTESIAN_POINT('Ctrl Pts',(-52.1266615318414,49.8910397995404,0.));
#92257=CARTESIAN_POINT('Ctrl Pts',(-52.1266615318414,49.8910397995404,12.));
#92258=CARTESIAN_POINT('Ctrl Pts',(-52.1489975513449,49.90069711499,0.));
#92259=CARTESIAN_POINT('Ctrl Pts',(-52.1489975513449,49.90069711499,12.));
#92260=CARTESIAN_POINT('Ctrl Pts',(-52.1713810841277,49.9103492455904,0.));
#92261=CARTESIAN_POINT('Ctrl Pts',(-52.1713810841277,49.9103492455904,12.));
#92262=CARTESIAN_POINT('Ctrl Pts',(-52.1938120478752,49.919996091396,0.));
#92263=CARTESIAN_POINT('Ctrl Pts',(-52.1938120478752,49.919996091396,12.));
#92264=CARTESIAN_POINT('Ctrl Pts',(-52.2162903605272,49.9296375529241,0.));
#92265=CARTESIAN_POINT('Ctrl Pts',(-52.2162903605272,49.9296375529241,12.));
#92266=CARTESIAN_POINT('Ctrl Pts',(-52.238815940277,49.9392735311507,0.));
#92267=CARTESIAN_POINT('Ctrl Pts',(-52.238815940277,49.9392735311507,12.));
#92268=CARTESIAN_POINT('Ctrl Pts',(-52.2613887055773,49.9489039275064,0.));
#92269=CARTESIAN_POINT('Ctrl Pts',(-52.2613887055773,49.9489039275064,12.));
#92270=CARTESIAN_POINT('Ctrl Pts',(-52.2840085751385,49.9585286438734,0.));
#92271=CARTESIAN_POINT('Ctrl Pts',(-52.2840085751385,49.9585286438734,12.));
#92272=CARTESIAN_POINT('Ctrl Pts',(-52.3066754679265,49.9681475825824,0.));
#92273=CARTESIAN_POINT('Ctrl Pts',(-52.3066754679265,49.9681475825824,12.));
#92274=CARTESIAN_POINT('Ctrl Pts',(-52.3293893031524,49.9777606464103,0.));
#92275=CARTESIAN_POINT('Ctrl Pts',(-52.3293893031524,49.9777606464103,12.));
#92276=CARTESIAN_POINT('Ctrl Pts',(-52.3521500002711,49.9873677385769,0.));
#92277=CARTESIAN_POINT('Ctrl Pts',(-52.3521500002711,49.9873677385769,12.));
#92278=CARTESIAN_POINT('Ctrl Pts',(-52.3749574789865,49.9969687627402,0.));
#92279=CARTESIAN_POINT('Ctrl Pts',(-52.3749574789865,49.9969687627402,12.));
#92280=CARTESIAN_POINT('Ctrl Pts',(-52.3978116592505,50.0065636229934,0.));
#92281=CARTESIAN_POINT('Ctrl Pts',(-52.3978116592505,50.0065636229934,12.));
#92282=CARTESIAN_POINT('Ctrl Pts',(-52.420712461261,50.0161522238619,0.));
#92283=CARTESIAN_POINT('Ctrl Pts',(-52.420712461261,50.0161522238619,12.));
#92284=CARTESIAN_POINT('Ctrl Pts',(-52.4436598054523,50.0257344703008,0.));
#92285=CARTESIAN_POINT('Ctrl Pts',(-52.4436598054523,50.0257344703008,12.));
#92286=CARTESIAN_POINT('Ctrl Pts',(-52.4666536124926,50.0353102676933,0.));
#92287=CARTESIAN_POINT('Ctrl Pts',(-52.4666536124926,50.0353102676933,12.));
#92288=CARTESIAN_POINT('Ctrl Pts',(-52.4896938032896,50.0448795218453,0.));
#92289=CARTESIAN_POINT('Ctrl Pts',(-52.4896938032896,50.0448795218453,12.));
#92290=CARTESIAN_POINT('Ctrl Pts',(-52.5127802989903,50.0544421389824,0.));
#92291=CARTESIAN_POINT('Ctrl Pts',(-52.5127802989903,50.0544421389824,12.));
#92292=CARTESIAN_POINT('Ctrl Pts',(-52.5359130209789,50.0639980257477,0.));
#92293=CARTESIAN_POINT('Ctrl Pts',(-52.5359130209789,50.0639980257477,12.));
#92294=CARTESIAN_POINT('Ctrl Pts',(-52.5590918908691,50.0735470891996,0.));
#92295=CARTESIAN_POINT('Ctrl Pts',(-52.5590918908691,50.0735470891996,12.));
#92296=CARTESIAN_POINT('Ctrl Pts',(-52.5823168304981,50.0830892368095,0.));
#92297=CARTESIAN_POINT('Ctrl Pts',(-52.5823168304981,50.0830892368095,12.));
#92298=CARTESIAN_POINT('Ctrl Pts',(-52.6055877619338,50.0926243764569,0.));
#92299=CARTESIAN_POINT('Ctrl Pts',(-52.6055877619338,50.0926243764569,12.));
#92300=CARTESIAN_POINT('Ctrl Pts',(-52.6289046074743,50.1021524164261,0.));
#92301=CARTESIAN_POINT('Ctrl Pts',(-52.6289046074743,50.1021524164261,12.));
#92302=CARTESIAN_POINT('Ctrl Pts',(-52.6522672896462,50.1116732654041,0.));
#92303=CARTESIAN_POINT('Ctrl Pts',(-52.6522672896462,50.1116732654041,12.));
#92304=CARTESIAN_POINT('Ctrl Pts',(-52.6756757311979,50.1211868324781,0.));
#92305=CARTESIAN_POINT('Ctrl Pts',(-52.6756757311979,50.1211868324781,12.));
#92306=CARTESIAN_POINT('Ctrl Pts',(-52.6991298550928,50.1306930271343,0.));
#92307=CARTESIAN_POINT('Ctrl Pts',(-52.6991298550928,50.1306930271343,12.));
#92308=CARTESIAN_POINT('Ctrl Pts',(-52.7226295845156,50.1401917592532,0.));
#92309=CARTESIAN_POINT('Ctrl Pts',(-52.7226295845156,50.1401917592532,12.));
#92310=CARTESIAN_POINT('Ctrl Pts',(-52.7461748428733,50.1496829391068,0.));
#92311=CARTESIAN_POINT('Ctrl Pts',(-52.7461748428733,50.1496829391068,12.));
#92312=CARTESIAN_POINT('Ctrl Pts',(-52.769765553794,50.1591664773561,0.));
#92313=CARTESIAN_POINT('Ctrl Pts',(-52.769765553794,50.1591664773561,12.));
#92314=CARTESIAN_POINT('Ctrl Pts',(-52.793401641121,50.1686422850493,0.));
#92315=CARTESIAN_POINT('Ctrl Pts',(-52.793401641121,50.1686422850493,12.));
#92316=CARTESIAN_POINT('Ctrl Pts',(-52.8170830289052,50.1781102736215,0.));
#92317=CARTESIAN_POINT('Ctrl Pts',(-52.8170830289052,50.1781102736215,12.));
#92318=CARTESIAN_POINT('Ctrl Pts',(-52.8408096414101,50.1875703548893,0.));
#92319=CARTESIAN_POINT('Ctrl Pts',(-52.8408096414101,50.1875703548893,12.));
#92320=CARTESIAN_POINT('Ctrl Pts',(-52.8645814031137,50.1970224410476,0.));
#92321=CARTESIAN_POINT('Ctrl Pts',(-52.8645814031137,50.1970224410476,12.));
#92322=CARTESIAN_POINT('Ctrl Pts',(-52.8883982387068,50.2064664446663,0.));
#92323=CARTESIAN_POINT('Ctrl Pts',(-52.8883982387068,50.2064664446663,12.));
#92324=CARTESIAN_POINT('Ctrl Pts',(-52.9122600730882,50.2159022786876,0.));
#92325=CARTESIAN_POINT('Ctrl Pts',(-52.9122600730882,50.2159022786876,12.));
#92326=CARTESIAN_POINT('Ctrl Pts',(-52.9361668313539,50.2253298564237,0.));
#92327=CARTESIAN_POINT('Ctrl Pts',(-52.9361668313539,50.2253298564237,12.));
#92328=CARTESIAN_POINT('Ctrl Pts',(-52.9601184388027,50.2347490915553,0.));
#92329=CARTESIAN_POINT('Ctrl Pts',(-52.9601184388027,50.2347490915553,12.));
#92330=CARTESIAN_POINT('Ctrl Pts',(-52.9841148209404,50.2441598981286,0.));
#92331=CARTESIAN_POINT('Ctrl Pts',(-52.9841148209404,50.2441598981286,12.));
#92332=CARTESIAN_POINT('Ctrl Pts',(-53.0081559034802,50.2535621905553,0.));
#92333=CARTESIAN_POINT('Ctrl Pts',(-53.0081559034802,50.2535621905553,12.));
#92334=CARTESIAN_POINT('Ctrl Pts',(-53.0322416123404,50.262955883611,0.));
#92335=CARTESIAN_POINT('Ctrl Pts',(-53.0322416123404,50.262955883611,12.));
#92336=CARTESIAN_POINT('Ctrl Pts',(-53.0563718736361,50.272340892437,0.));
#92337=CARTESIAN_POINT('Ctrl Pts',(-53.0563718736361,50.272340892437,12.));
#92338=CARTESIAN_POINT('Ctrl Pts',(-53.0805466136791,50.2817171325354,0.));
#92339=CARTESIAN_POINT('Ctrl Pts',(-53.0805466136791,50.2817171325354,12.));
#92340=CARTESIAN_POINT('Ctrl Pts',(-53.1047657589806,50.2910845197615,0.));
#92341=CARTESIAN_POINT('Ctrl Pts',(-53.1047657589806,50.2910845197615,12.));
#92342=CARTESIAN_POINT('Ctrl Pts',(-53.1290292362482,50.3004429703188,0.));
#92343=CARTESIAN_POINT('Ctrl Pts',(-53.1290292362482,50.3004429703188,12.));
#92344=CARTESIAN_POINT('Ctrl Pts',(-53.153336972382,50.3097924007535,0.));
#92345=CARTESIAN_POINT('Ctrl Pts',(-53.153336972382,50.3097924007535,12.));
#92346=CARTESIAN_POINT('Ctrl Pts',(-53.1776888944622,50.3191327279497,0.));
#92347=CARTESIAN_POINT('Ctrl Pts',(-53.1776888944622,50.3191327279497,12.));
#92348=CARTESIAN_POINT('Ctrl Pts',(-53.202084929748,50.3284638691285,0.));
#92349=CARTESIAN_POINT('Ctrl Pts',(-53.202084929748,50.3284638691285,12.));
#92350=CARTESIAN_POINT('Ctrl Pts',(-53.2265250056896,50.3377857418522,0.));
#92351=CARTESIAN_POINT('Ctrl Pts',(-53.2265250056896,50.3377857418522,12.));
#92352=CARTESIAN_POINT('Ctrl Pts',(-53.2510090499341,50.3470982640293,0.));
#92353=CARTESIAN_POINT('Ctrl Pts',(-53.2510090499341,50.3470982640293,12.));
#92354=CARTESIAN_POINT('Ctrl Pts',(-53.2755369903291,50.3564013539198,0.));
#92355=CARTESIAN_POINT('Ctrl Pts',(-53.2755369903291,50.3564013539198,12.));
#92356=CARTESIAN_POINT('Ctrl Pts',(-53.3001087549222,50.3656949301423,0.));
#92357=CARTESIAN_POINT('Ctrl Pts',(-53.3001087549222,50.3656949301423,12.));
#92358=CARTESIAN_POINT('Ctrl Pts',(-53.3247242719575,50.3749789116777,0.));
#92359=CARTESIAN_POINT('Ctrl Pts',(-53.3247242719575,50.3749789116777,12.));
#92360=CARTESIAN_POINT('Ctrl Pts',(-53.3493834698685,50.384253217845,0.));
#92361=CARTESIAN_POINT('Ctrl Pts',(-53.3493834698685,50.384253217845,12.));
#92362=CARTESIAN_POINT('Ctrl Pts',(-53.3740862772673,50.393517768283,0.));
#92363=CARTESIAN_POINT('Ctrl Pts',(-53.3740862772673,50.393517768283,12.));
#92364=CARTESIAN_POINT('Ctrl Pts',(-53.3988326229308,50.4027724829296,0.));
#92365=CARTESIAN_POINT('Ctrl Pts',(-53.3988326229308,50.4027724829296,12.));
#92366=CARTESIAN_POINT('Ctrl Pts',(-53.4236224357846,50.4120172820054,0.));
#92367=CARTESIAN_POINT('Ctrl Pts',(-53.4236224357846,50.4120172820054,12.));
#92368=CARTESIAN_POINT('Ctrl Pts',(-53.4484556448787,50.4212520859924,0.));
#92369=CARTESIAN_POINT('Ctrl Pts',(-53.4484556448787,50.4212520859924,12.));
#92370=CARTESIAN_POINT('Ctrl Pts',(-53.4733321794199,50.4304768156677,0.));
#92371=CARTESIAN_POINT('Ctrl Pts',(-53.4733321794199,50.4304768156677,12.));
#92372=CARTESIAN_POINT('Ctrl Pts',(-53.4982519688032,50.4396913921389,0.));
#92373=CARTESIAN_POINT('Ctrl Pts',(-53.4982519688032,50.4396913921389,12.));
#92374=CARTESIAN_POINT('Ctrl Pts',(-53.5232149426415,50.4488957368841,0.));
#92375=CARTESIAN_POINT('Ctrl Pts',(-53.5232149426415,50.4488957368841,12.));
#92376=CARTESIAN_POINT('Ctrl Pts',(-53.5482210307864,50.4580897717835,0.));
#92377=CARTESIAN_POINT('Ctrl Pts',(-53.5482210307864,50.4580897717835,12.));
#92378=CARTESIAN_POINT('Ctrl Pts',(-53.5732701633603,50.4672734191749,0.));
#92379=CARTESIAN_POINT('Ctrl Pts',(-53.5732701633603,50.4672734191749,12.));
#92380=CARTESIAN_POINT('Ctrl Pts',(-53.5983622707231,50.4764466018064,0.));
#92381=CARTESIAN_POINT('Ctrl Pts',(-53.5983622707231,50.4764466018064,12.));
#92382=CARTESIAN_POINT('Ctrl Pts',(-53.6234972834055,50.4856092427309,0.));
#92383=CARTESIAN_POINT('Ctrl Pts',(-53.6234972834055,50.4856092427309,12.));
#92384=CARTESIAN_POINT('Ctrl Pts',(-53.6486751320434,50.4947612652147,0.));
#92385=CARTESIAN_POINT('Ctrl Pts',(-53.6486751320434,50.4947612652147,12.));
#92386=CARTESIAN_POINT('Ctrl Pts',(-53.6738957473158,50.5039025926531,0.));
#92387=CARTESIAN_POINT('Ctrl Pts',(-53.6738957473158,50.5039025926531,12.));
#92388=CARTESIAN_POINT('Ctrl Pts',(-53.6991590598551,50.5130331484563,0.));
#92389=CARTESIAN_POINT('Ctrl Pts',(-53.6991590598551,50.5130331484563,12.));
#92390=CARTESIAN_POINT('Ctrl Pts',(-53.7244650002382,50.5221528560427,0.));
#92391=CARTESIAN_POINT('Ctrl Pts',(-53.7244650002382,50.5221528560427,12.));
#92392=CARTESIAN_POINT('Ctrl Pts',(-53.7498134991714,50.5312616390789,0.));
#92393=CARTESIAN_POINT('Ctrl Pts',(-53.7498134991714,50.5312616390789,12.));
#92394=CARTESIAN_POINT('Ctrl Pts',(-53.7752044876313,50.5403594216706,0.));
#92395=CARTESIAN_POINT('Ctrl Pts',(-53.7752044876313,50.5403594216706,12.));
#92396=CARTESIAN_POINT('Ctrl Pts',(-53.8006378970198,50.5494461285762,0.));
#92397=CARTESIAN_POINT('Ctrl Pts',(-53.8006378970198,50.5494461285762,12.));
#92398=CARTESIAN_POINT('Ctrl Pts',(-53.8261136593064,50.5585216854082,0.));
#92399=CARTESIAN_POINT('Ctrl Pts',(-53.8261136593064,50.5585216854082,12.));
#92400=CARTESIAN_POINT('Ctrl Pts',(-53.8516317071783,50.567586018852,0.));
#92401=CARTESIAN_POINT('Ctrl Pts',(-53.8516317071783,50.567586018852,12.));
#92402=CARTESIAN_POINT('Ctrl Pts',(-53.8771919737007,50.5766390561861,0.));
#92403=CARTESIAN_POINT('Ctrl Pts',(-53.8771919737007,50.5766390561861,12.));
#92404=CARTESIAN_POINT('Ctrl Pts',(-53.9027943919814,50.5856807248133,0.));
#92405=CARTESIAN_POINT('Ctrl Pts',(-53.9027943919814,50.5856807248133,12.));
#92406=CARTESIAN_POINT('Ctrl Pts',(-53.9284388947996,50.5947109517476,0.));
#92407=CARTESIAN_POINT('Ctrl Pts',(-53.9284388947996,50.5947109517476,12.));
#92408=CARTESIAN_POINT('Ctrl Pts',(-53.9541254143131,50.603729663215,0.));
#92409=CARTESIAN_POINT('Ctrl Pts',(-53.9541254143131,50.603729663215,12.));
#92410=CARTESIAN_POINT('Ctrl Pts',(-53.9798538815561,50.6127367839738,0.));
#92411=CARTESIAN_POINT('Ctrl Pts',(-53.9798538815561,50.6127367839738,12.));
#92412=CARTESIAN_POINT('Ctrl Pts',(-54.0056242268443,50.6217322378686,0.));
#92413=CARTESIAN_POINT('Ctrl Pts',(-54.0056242268443,50.6217322378686,12.));
#92414=CARTESIAN_POINT('Ctrl Pts',(-54.0314363806751,50.630715949059,0.));
#92415=CARTESIAN_POINT('Ctrl Pts',(-54.0314363806751,50.630715949059,12.));
#92416=CARTESIAN_POINT('Ctrl Pts',(-54.0572902745101,50.6396878430961,0.));
#92417=CARTESIAN_POINT('Ctrl Pts',(-54.0572902745101,50.6396878430961,12.));
#92418=CARTESIAN_POINT('Ctrl Pts',(-54.0831858415182,50.6486478479459,0.));
#92419=CARTESIAN_POINT('Ctrl Pts',(-54.0831858415182,50.6486478479459,12.));
#92420=CARTESIAN_POINT('Ctrl Pts',(-54.1091230175319,50.657595895318,0.));
#92421=CARTESIAN_POINT('Ctrl Pts',(-54.1091230175319,50.657595895318,12.));
#92422=CARTESIAN_POINT('Ctrl Pts',(-54.1351017412722,50.6665319209798,0.));
#92423=CARTESIAN_POINT('Ctrl Pts',(-54.1351017412722,50.6665319209798,12.));
#92424=CARTESIAN_POINT('Ctrl Pts',(-54.1611219522299,50.6754558618218,0.));
#92425=CARTESIAN_POINT('Ctrl Pts',(-54.1611219522299,50.6754558618218,12.));
#92426=CARTESIAN_POINT('Ctrl Pts',(-54.1871835889908,50.6843676535428,0.));
#92427=CARTESIAN_POINT('Ctrl Pts',(-54.1871835889908,50.6843676535428,12.));
#92428=CARTESIAN_POINT('Ctrl Pts',(-54.2132865872968,50.6932672279758,0.));
#92429=CARTESIAN_POINT('Ctrl Pts',(-54.2132865872968,50.6932672279758,12.));
#92430=CARTESIAN_POINT('Ctrl Pts',(-54.2394308784093,50.7021545108369,0.));
#92431=CARTESIAN_POINT('Ctrl Pts',(-54.2394308784093,50.7021545108369,12.));
#92432=CARTESIAN_POINT('Ctrl Pts',(-54.2656163868258,50.7110294185832,0.));
#92433=CARTESIAN_POINT('Ctrl Pts',(-54.2656163868258,50.7110294185832,12.));
#92434=CARTESIAN_POINT('Ctrl Pts',(-54.2918430335414,50.7198918629632,0.));
#92435=CARTESIAN_POINT('Ctrl Pts',(-54.2918430335414,50.7198918629632,12.));
#92436=CARTESIAN_POINT('Ctrl Pts',(-54.3181107400862,50.7287417566296,0.));
#92437=CARTESIAN_POINT('Ctrl Pts',(-54.3181107400862,50.7287417566296,12.));
#92438=CARTESIAN_POINT('Ctrl Pts',(-54.344419432416,50.7375790185988,0.));
#92439=CARTESIAN_POINT('Ctrl Pts',(-54.344419432416,50.7375790185988,12.));
#92440=CARTESIAN_POINT('Ctrl Pts',(-54.3707690445679,50.7464035792846,0.));
#92441=CARTESIAN_POINT('Ctrl Pts',(-54.3707690445679,50.7464035792846,12.));
#92442=CARTESIAN_POINT('Ctrl Pts',(-54.3971595231285,50.7552153869224,0.));
#92443=CARTESIAN_POINT('Ctrl Pts',(-54.3971595231285,50.7552153869224,12.));
#92444=CARTESIAN_POINT('Ctrl Pts',(-54.4235908287188,50.7640144089601,0.));
#92445=CARTESIAN_POINT('Ctrl Pts',(-54.4235908287188,50.7640144089601,12.));
#92446=CARTESIAN_POINT('Ctrl Pts',(-54.4500629335867,50.772800626886,0.));
#92447=CARTESIAN_POINT('Ctrl Pts',(-54.4500629335867,50.772800626886,12.));
#92448=CARTESIAN_POINT('Ctrl Pts',(-54.4712732428597,50.7798193515479,0.));
#92449=CARTESIAN_POINT('Ctrl Pts',(-54.4712732428597,50.7798193515479,12.));
#92450=CARTESIAN_POINT('Ctrl Pts',(-54.4871993224549,50.7850776288567,0.));
#92451=CARTESIAN_POINT('Ctrl Pts',(-54.4871993224549,50.7850776288567,12.));
#92452=CARTESIAN_POINT('Ctrl Pts',(-54.4978248630284,50.7885805844191,0.));
#92453=CARTESIAN_POINT('Ctrl Pts',(-54.4978248630284,50.7885805844191,12.));
#92454=CARTESIAN_POINT('Ctrl Pts',(-54.5031396718592,50.7903314215393,0.));
#92455=CARTESIAN_POINT('Ctrl Pts',(-54.5031396718592,50.7903314215393,12.));
#92456=CARTESIAN_POINT('',(-50.0975384783634,48.8900464144686,0.));
#92457=CARTESIAN_POINT('Ctrl Pts',(-50.0975384783634,48.8900464144686,0.));
#92458=CARTESIAN_POINT('Ctrl Pts',(-50.1009206494209,48.8919551910299,0.));
#92459=CARTESIAN_POINT('Ctrl Pts',(-50.1076907555303,48.8957735556681,0.));
#92460=CARTESIAN_POINT('Ctrl Pts',(-50.1178632066821,48.9015035371772,0.));
#92461=CARTESIAN_POINT('Ctrl Pts',(-50.1314610602286,48.9091483817797,0.));
#92462=CARTESIAN_POINT('Ctrl Pts',(-50.148516018447,48.9187125417897,0.));
#92463=CARTESIAN_POINT('Ctrl Pts',(-50.1656286003943,48.9282847698237,0.));
#92464=CARTESIAN_POINT('Ctrl Pts',(-50.1827987615659,48.9378649933116,0.));
#92465=CARTESIAN_POINT('Ctrl Pts',(-50.2000264157903,48.9474530868847,0.));
#92466=CARTESIAN_POINT('Ctrl Pts',(-50.2173114358423,48.9570488741273,0.));
#92467=CARTESIAN_POINT('Ctrl Pts',(-50.2346536715465,48.9666521500969,0.));
#92468=CARTESIAN_POINT('Ctrl Pts',(-50.252052963548,48.9762626987227,0.));
#92469=CARTESIAN_POINT('Ctrl Pts',(-50.2695091583473,48.9858803116649,0.));
#92470=CARTESIAN_POINT('Ctrl Pts',(-50.2870221241003,48.9955048082028,0.));
#92471=CARTESIAN_POINT('Ctrl Pts',(-50.3045917455383,49.0051360288002,0.));
#92472=CARTESIAN_POINT('Ctrl Pts',(-50.3222179165102,49.0147738256925,0.));
#92473=CARTESIAN_POINT('Ctrl Pts',(-50.3399005337967,49.0244180550759,0.));
#92474=CARTESIAN_POINT('Ctrl Pts',(-50.3576394894136,49.034068567401,0.));
#92475=CARTESIAN_POINT('Ctrl Pts',(-50.3754346667389,49.0437252024868,0.));
#92476=CARTESIAN_POINT('Ctrl Pts',(-50.393285944528,49.0533877945771,0.));
#92477=CARTESIAN_POINT('Ctrl Pts',(-50.4111931994264,49.0630561755082,0.));
#92478=CARTESIAN_POINT('Ctrl Pts',(-50.4291563088528,49.0727301783477,0.));
#92479=CARTESIAN_POINT('Ctrl Pts',(-50.4471751542717,49.0824096415339,0.));
#92480=CARTESIAN_POINT('Ctrl Pts',(-50.465249621057,49.0920944086973,0.));
#92481=CARTESIAN_POINT('Ctrl Pts',(-50.4833795969296,49.1017843266782,0.));
#92482=CARTESIAN_POINT('Ctrl Pts',(-50.5015649708742,49.1114792441573,0.));
#92483=CARTESIAN_POINT('Ctrl Pts',(-50.5198056318111,49.1211790099817,0.));
#92484=CARTESIAN_POINT('Ctrl Pts',(-50.5381014674822,49.1308834717645,0.));
#92485=CARTESIAN_POINT('Ctrl Pts',(-50.5564523650406,49.1405924766169,0.));
#92486=CARTESIAN_POINT('Ctrl Pts',(-50.5748582115575,49.1503058717831,0.));
#92487=CARTESIAN_POINT('Ctrl Pts',(-50.593318894516,49.1600235052613,0.));
#92488=CARTESIAN_POINT('Ctrl Pts',(-50.6118343023937,49.1697452265473,0.));
#92489=CARTESIAN_POINT('Ctrl Pts',(-50.6304043248796,49.1794708869074,0.));
#92490=CARTESIAN_POINT('Ctrl Pts',(-50.6490288525639,49.1892003389743,0.));
#92491=CARTESIAN_POINT('Ctrl Pts',(-50.6677077767427,49.1989334364991,0.));
#92492=CARTESIAN_POINT('Ctrl Pts',(-50.6864409891905,49.2086700340625,0.));
#92493=CARTESIAN_POINT('Ctrl Pts',(-50.7052283818941,49.218409986748,0.));
#92494=CARTESIAN_POINT('Ctrl Pts',(-50.7240698470698,49.2281531501569,0.));
#92495=CARTESIAN_POINT('Ctrl Pts',(-50.7429652772816,49.2378993805482,0.));
#92496=CARTESIAN_POINT('Ctrl Pts',(-50.7619145655207,49.2476485349373,0.));
#92497=CARTESIAN_POINT('Ctrl Pts',(-50.7809176052954,49.2574004712122,0.));
#92498=CARTESIAN_POINT('Ctrl Pts',(-50.7999742907111,49.2671550482415,0.));
#92499=CARTESIAN_POINT('Ctrl Pts',(-50.8190845164319,49.2769121258144,0.));
#92500=CARTESIAN_POINT('Ctrl Pts',(-50.8382481776392,49.2866715645828,0.));
#92501=CARTESIAN_POINT('Ctrl Pts',(-50.8574651699877,49.2964332260043,0.));
#92502=CARTESIAN_POINT('Ctrl Pts',(-50.8767353895509,49.3061969722798,0.));
#92503=CARTESIAN_POINT('Ctrl Pts',(-50.8960587327869,49.3159626663129,0.));
#92504=CARTESIAN_POINT('Ctrl Pts',(-50.9154350965681,49.325730171735,0.));
#92505=CARTESIAN_POINT('Ctrl Pts',(-50.9348643781928,49.3354993529163,0.));
#92506=CARTESIAN_POINT('Ctrl Pts',(-50.9543464753974,49.3452700749804,0.));
#92507=CARTESIAN_POINT('Ctrl Pts',(-50.9738812863636,49.3550422038221,0.));
#92508=CARTESIAN_POINT('Ctrl Pts',(-50.9934687097179,49.3648156061049,0.));
#92509=CARTESIAN_POINT('Ctrl Pts',(-51.0131086445268,49.3745901492428,0.));
#92510=CARTESIAN_POINT('Ctrl Pts',(-51.0328009902857,49.3843657013851,0.));
#92511=CARTESIAN_POINT('Ctrl Pts',(-51.0525456469072,49.3941421314014,0.));
#92512=CARTESIAN_POINT('Ctrl Pts',(-51.0723425146987,49.4039193088635,0.));
#92513=CARTESIAN_POINT('Ctrl Pts',(-51.0921914943663,49.4136971040428,0.));
#92514=CARTESIAN_POINT('Ctrl Pts',(-51.1120924870196,49.4234753879071,0.));
#92515=CARTESIAN_POINT('Ctrl Pts',(-51.1320453941702,49.4332540321178,0.));
#92516=CARTESIAN_POINT('Ctrl Pts',(-51.1520501177291,49.4430329090288,0.));
#92517=CARTESIAN_POINT('Ctrl Pts',(-51.1721065599972,49.4528118916833,0.));
#92518=CARTESIAN_POINT('Ctrl Pts',(-51.1922146236686,49.4625908538076,0.));
#92519=CARTESIAN_POINT('Ctrl Pts',(-51.2123742118288,49.4723696698022,0.));
#92520=CARTESIAN_POINT('Ctrl Pts',(-51.2325852279507,49.4821482147357,0.));
#92521=CARTESIAN_POINT('Ctrl Pts',(-51.2528475758841,49.4919263643357,0.));
#92522=CARTESIAN_POINT('Ctrl Pts',(-51.2731611598465,49.5017039949841,0.));
#92523=CARTESIAN_POINT('Ctrl Pts',(-51.2935258844278,49.5114809837111,0.));
#92524=CARTESIAN_POINT('Ctrl Pts',(-51.3139416545903,49.5212572081901,0.));
#92525=CARTESIAN_POINT('Ctrl Pts',(-51.3344083756659,49.5310325467334,0.));
#92526=CARTESIAN_POINT('Ctrl Pts',(-51.354925953347,49.5408068782871,0.));
#92527=CARTESIAN_POINT('Ctrl Pts',(-51.3754942936796,49.5505800824268,0.));
#92528=CARTESIAN_POINT('Ctrl Pts',(-51.3961133030688,49.5603520393514,0.));
#92529=CARTESIAN_POINT('Ctrl Pts',(-51.4167828882765,49.5701226298779,0.));
#92530=CARTESIAN_POINT('Ctrl Pts',(-51.4375029564191,49.579891735436,0.));
#92531=CARTESIAN_POINT('Ctrl Pts',(-51.4582734149562,49.5896592380634,0.));
#92532=CARTESIAN_POINT('Ctrl Pts',(-51.4790941716859,49.5994250204003,0.));
#92533=CARTESIAN_POINT('Ctrl Pts',(-51.4999651347496,49.609188965684,0.));
#92534=CARTESIAN_POINT('Ctrl Pts',(-51.5208862126303,49.6189509577441,0.));
#92535=CARTESIAN_POINT('Ctrl Pts',(-51.5418573141494,49.6287108809975,0.));
#92536=CARTESIAN_POINT('Ctrl Pts',(-51.5628783484556,49.6384686204443,0.));
#92537=CARTESIAN_POINT('Ctrl Pts',(-51.5839492250218,49.6482240616627,0.));
#92538=CARTESIAN_POINT('Ctrl Pts',(-51.6050698536525,49.6579770908063,0.));
#92539=CARTESIAN_POINT('Ctrl Pts',(-51.6262401444799,49.6677275945975,0.));
#92540=CARTESIAN_POINT('Ctrl Pts',(-51.6474600079611,49.6774754603235,0.));
#92541=CARTESIAN_POINT('Ctrl Pts',(-51.6687293548656,49.6872205758314,0.));
#92542=CARTESIAN_POINT('Ctrl Pts',(-51.6900480962744,49.6969628295236,0.));
#92543=CARTESIAN_POINT('Ctrl Pts',(-51.7114161435848,49.7067021103534,0.));
#92544=CARTESIAN_POINT('Ctrl Pts',(-51.7328334085084,49.7164383078206,0.));
#92545=CARTESIAN_POINT('Ctrl Pts',(-51.754299803068,49.7261713119672,0.));
#92546=CARTESIAN_POINT('Ctrl Pts',(-51.7758152395857,49.7359010133741,0.));
#92547=CARTESIAN_POINT('Ctrl Pts',(-51.7973796306826,49.7456273031555,0.));
#92548=CARTESIAN_POINT('Ctrl Pts',(-51.8189928892841,49.7553500729563,0.));
#92549=CARTESIAN_POINT('Ctrl Pts',(-51.8406549286177,49.7650692149464,0.));
#92550=CARTESIAN_POINT('Ctrl Pts',(-51.8623656622092,49.7747846218177,0.));
#92551=CARTESIAN_POINT('Ctrl Pts',(-51.8841250038716,49.78449618678,0.));
#92552=CARTESIAN_POINT('Ctrl Pts',(-51.9059328677051,49.7942038035568,0.));
#92553=CARTESIAN_POINT('Ctrl Pts',(-51.9277891681014,49.8039073663808,0.));
#92554=CARTESIAN_POINT('Ctrl Pts',(-51.9496938197418,49.8136067699896,0.));
#92555=CARTESIAN_POINT('Ctrl Pts',(-51.9716467375938,49.8233019096224,0.));
#92556=CARTESIAN_POINT('Ctrl Pts',(-51.9936478369008,49.8329926810172,0.));
#92557=CARTESIAN_POINT('Ctrl Pts',(-52.015697033182,49.8426789804068,0.));
#92558=CARTESIAN_POINT('Ctrl Pts',(-52.0377942422373,49.8523607045146,0.));
#92559=CARTESIAN_POINT('Ctrl Pts',(-52.059939380145,49.8620377505498,0.));
#92560=CARTESIAN_POINT('Ctrl Pts',(-52.0821323632588,49.871710016205,0.));
#92561=CARTESIAN_POINT('Ctrl Pts',(-52.1043731081968,49.8813773996523,0.));
#92562=CARTESIAN_POINT('Ctrl Pts',(-52.1266615318414,49.8910397995404,0.));
#92563=CARTESIAN_POINT('Ctrl Pts',(-52.1489975513449,49.90069711499,0.));
#92564=CARTESIAN_POINT('Ctrl Pts',(-52.1713810841277,49.9103492455904,0.));
#92565=CARTESIAN_POINT('Ctrl Pts',(-52.1938120478752,49.919996091396,0.));
#92566=CARTESIAN_POINT('Ctrl Pts',(-52.2162903605272,49.9296375529241,0.));
#92567=CARTESIAN_POINT('Ctrl Pts',(-52.238815940277,49.9392735311507,0.));
#92568=CARTESIAN_POINT('Ctrl Pts',(-52.2613887055773,49.9489039275064,0.));
#92569=CARTESIAN_POINT('Ctrl Pts',(-52.2840085751385,49.9585286438734,0.));
#92570=CARTESIAN_POINT('Ctrl Pts',(-52.3066754679265,49.9681475825824,0.));
#92571=CARTESIAN_POINT('Ctrl Pts',(-52.3293893031524,49.9777606464103,0.));
#92572=CARTESIAN_POINT('Ctrl Pts',(-52.3521500002711,49.9873677385769,0.));
#92573=CARTESIAN_POINT('Ctrl Pts',(-52.3749574789865,49.9969687627402,0.));
#92574=CARTESIAN_POINT('Ctrl Pts',(-52.3978116592505,50.0065636229934,0.));
#92575=CARTESIAN_POINT('Ctrl Pts',(-52.420712461261,50.0161522238619,0.));
#92576=CARTESIAN_POINT('Ctrl Pts',(-52.4436598054523,50.0257344703008,0.));
#92577=CARTESIAN_POINT('Ctrl Pts',(-52.4666536124926,50.0353102676933,0.));
#92578=CARTESIAN_POINT('Ctrl Pts',(-52.4896938032896,50.0448795218453,0.));
#92579=CARTESIAN_POINT('Ctrl Pts',(-52.5127802989903,50.0544421389824,0.));
#92580=CARTESIAN_POINT('Ctrl Pts',(-52.5359130209789,50.0639980257477,0.));
#92581=CARTESIAN_POINT('Ctrl Pts',(-52.5590918908691,50.0735470891996,0.));
#92582=CARTESIAN_POINT('Ctrl Pts',(-52.5823168304981,50.0830892368095,0.));
#92583=CARTESIAN_POINT('Ctrl Pts',(-52.6055877619338,50.0926243764569,0.));
#92584=CARTESIAN_POINT('Ctrl Pts',(-52.6289046074743,50.1021524164261,0.));
#92585=CARTESIAN_POINT('Ctrl Pts',(-52.6522672896462,50.1116732654041,0.));
#92586=CARTESIAN_POINT('Ctrl Pts',(-52.6756757311979,50.1211868324781,0.));
#92587=CARTESIAN_POINT('Ctrl Pts',(-52.6991298550928,50.1306930271343,0.));
#92588=CARTESIAN_POINT('Ctrl Pts',(-52.7226295845156,50.1401917592532,0.));
#92589=CARTESIAN_POINT('Ctrl Pts',(-52.7461748428733,50.1496829391068,0.));
#92590=CARTESIAN_POINT('Ctrl Pts',(-52.769765553794,50.1591664773561,0.));
#92591=CARTESIAN_POINT('Ctrl Pts',(-52.793401641121,50.1686422850493,0.));
#92592=CARTESIAN_POINT('Ctrl Pts',(-52.8170830289052,50.1781102736215,0.));
#92593=CARTESIAN_POINT('Ctrl Pts',(-52.8408096414101,50.1875703548893,0.));
#92594=CARTESIAN_POINT('Ctrl Pts',(-52.8645814031137,50.1970224410476,0.));
#92595=CARTESIAN_POINT('Ctrl Pts',(-52.8883982387068,50.2064664446663,0.));
#92596=CARTESIAN_POINT('Ctrl Pts',(-52.9122600730882,50.2159022786876,0.));
#92597=CARTESIAN_POINT('Ctrl Pts',(-52.9361668313539,50.2253298564237,0.));
#92598=CARTESIAN_POINT('Ctrl Pts',(-52.9601184388027,50.2347490915553,0.));
#92599=CARTESIAN_POINT('Ctrl Pts',(-52.9841148209404,50.2441598981286,0.));
#92600=CARTESIAN_POINT('Ctrl Pts',(-53.0081559034802,50.2535621905553,0.));
#92601=CARTESIAN_POINT('Ctrl Pts',(-53.0322416123404,50.262955883611,0.));
#92602=CARTESIAN_POINT('Ctrl Pts',(-53.0563718736361,50.272340892437,0.));
#92603=CARTESIAN_POINT('Ctrl Pts',(-53.0805466136791,50.2817171325354,0.));
#92604=CARTESIAN_POINT('Ctrl Pts',(-53.1047657589806,50.2910845197615,0.));
#92605=CARTESIAN_POINT('Ctrl Pts',(-53.1290292362482,50.3004429703188,0.));
#92606=CARTESIAN_POINT('Ctrl Pts',(-53.153336972382,50.3097924007535,0.));
#92607=CARTESIAN_POINT('Ctrl Pts',(-53.1776888944622,50.3191327279497,0.));
#92608=CARTESIAN_POINT('Ctrl Pts',(-53.202084929748,50.3284638691285,0.));
#92609=CARTESIAN_POINT('Ctrl Pts',(-53.2265250056896,50.3377857418522,0.));
#92610=CARTESIAN_POINT('Ctrl Pts',(-53.2510090499341,50.3470982640293,0.));
#92611=CARTESIAN_POINT('Ctrl Pts',(-53.2755369903291,50.3564013539198,0.));
#92612=CARTESIAN_POINT('Ctrl Pts',(-53.3001087549222,50.3656949301423,0.));
#92613=CARTESIAN_POINT('Ctrl Pts',(-53.3247242719575,50.3749789116777,0.));
#92614=CARTESIAN_POINT('Ctrl Pts',(-53.3493834698685,50.384253217845,0.));
#92615=CARTESIAN_POINT('Ctrl Pts',(-53.3740862772673,50.393517768283,0.));
#92616=CARTESIAN_POINT('Ctrl Pts',(-53.3988326229308,50.4027724829296,0.));
#92617=CARTESIAN_POINT('Ctrl Pts',(-53.4236224357846,50.4120172820054,0.));
#92618=CARTESIAN_POINT('Ctrl Pts',(-53.4484556448787,50.4212520859924,0.));
#92619=CARTESIAN_POINT('Ctrl Pts',(-53.4733321794199,50.4304768156677,0.));
#92620=CARTESIAN_POINT('Ctrl Pts',(-53.4982519688032,50.4396913921389,0.));
#92621=CARTESIAN_POINT('Ctrl Pts',(-53.5232149426415,50.4488957368841,0.));
#92622=CARTESIAN_POINT('Ctrl Pts',(-53.5482210307864,50.4580897717835,0.));
#92623=CARTESIAN_POINT('Ctrl Pts',(-53.5732701633603,50.4672734191749,0.));
#92624=CARTESIAN_POINT('Ctrl Pts',(-53.5983622707231,50.4764466018064,0.));
#92625=CARTESIAN_POINT('Ctrl Pts',(-53.6234972834055,50.4856092427309,0.));
#92626=CARTESIAN_POINT('Ctrl Pts',(-53.6486751320434,50.4947612652147,0.));
#92627=CARTESIAN_POINT('Ctrl Pts',(-53.6738957473158,50.5039025926531,0.));
#92628=CARTESIAN_POINT('Ctrl Pts',(-53.6991590598551,50.5130331484563,0.));
#92629=CARTESIAN_POINT('Ctrl Pts',(-53.7244650002382,50.5221528560427,0.));
#92630=CARTESIAN_POINT('Ctrl Pts',(-53.7498134991714,50.5312616390789,0.));
#92631=CARTESIAN_POINT('Ctrl Pts',(-53.7752044876313,50.5403594216706,0.));
#92632=CARTESIAN_POINT('Ctrl Pts',(-53.8006378970198,50.5494461285762,0.));
#92633=CARTESIAN_POINT('Ctrl Pts',(-53.8261136593064,50.5585216854082,0.));
#92634=CARTESIAN_POINT('Ctrl Pts',(-53.8516317071783,50.567586018852,0.));
#92635=CARTESIAN_POINT('Ctrl Pts',(-53.8771919737007,50.5766390561861,0.));
#92636=CARTESIAN_POINT('Ctrl Pts',(-53.9027943919814,50.5856807248133,0.));
#92637=CARTESIAN_POINT('Ctrl Pts',(-53.9284388947996,50.5947109517476,0.));
#92638=CARTESIAN_POINT('Ctrl Pts',(-53.9541254143131,50.603729663215,0.));
#92639=CARTESIAN_POINT('Ctrl Pts',(-53.9798538815561,50.6127367839738,0.));
#92640=CARTESIAN_POINT('Ctrl Pts',(-54.0056242268443,50.6217322378686,0.));
#92641=CARTESIAN_POINT('Ctrl Pts',(-54.0314363806751,50.630715949059,0.));
#92642=CARTESIAN_POINT('Ctrl Pts',(-54.0572902745101,50.6396878430961,0.));
#92643=CARTESIAN_POINT('Ctrl Pts',(-54.0831858415182,50.6486478479459,0.));
#92644=CARTESIAN_POINT('Ctrl Pts',(-54.1091230175319,50.657595895318,0.));
#92645=CARTESIAN_POINT('Ctrl Pts',(-54.1351017412722,50.6665319209798,0.));
#92646=CARTESIAN_POINT('Ctrl Pts',(-54.1574061041882,50.6741814675382,0.));
#92647=CARTESIAN_POINT('Ctrl Pts',(-54.1745287898577,50.6800396668659,0.));
#92648=CARTESIAN_POINT('Ctrl Pts',(-54.1864514381924,50.6841118861803,0.));
#92649=CARTESIAN_POINT('Ctrl Pts',(-54.1931619277295,50.6864016965603,0.));
#92650=CARTESIAN_POINT('Ctrl Pts',(-54.1946543499978,50.6869108458688,0.));
#92651=CARTESIAN_POINT('',(-50.0975384783634,48.8900464144686,12.));
#92652=CARTESIAN_POINT('',(-50.0975384783634,48.8900464144686,0.));
#92653=CARTESIAN_POINT('Ctrl Pts',(-54.1946543499978,50.6869108458688,12.));
#92654=CARTESIAN_POINT('Ctrl Pts',(-54.1931619277295,50.6864016965603,12.));
#92655=CARTESIAN_POINT('Ctrl Pts',(-54.1864514381924,50.6841118861803,12.));
#92656=CARTESIAN_POINT('Ctrl Pts',(-54.1745287898577,50.6800396668659,12.));
#92657=CARTESIAN_POINT('Ctrl Pts',(-54.1574061041882,50.6741814675382,12.));
#92658=CARTESIAN_POINT('Ctrl Pts',(-54.1351017412722,50.6665319209798,12.));
#92659=CARTESIAN_POINT('Ctrl Pts',(-54.1091230175319,50.657595895318,12.));
#92660=CARTESIAN_POINT('Ctrl Pts',(-54.0831858415182,50.6486478479459,12.));
#92661=CARTESIAN_POINT('Ctrl Pts',(-54.0572902745101,50.6396878430961,12.));
#92662=CARTESIAN_POINT('Ctrl Pts',(-54.0314363806751,50.630715949059,12.));
#92663=CARTESIAN_POINT('Ctrl Pts',(-54.0056242268443,50.6217322378686,12.));
#92664=CARTESIAN_POINT('Ctrl Pts',(-53.9798538815561,50.6127367839738,12.));
#92665=CARTESIAN_POINT('Ctrl Pts',(-53.9541254143131,50.603729663215,12.));
#92666=CARTESIAN_POINT('Ctrl Pts',(-53.9284388947996,50.5947109517476,12.));
#92667=CARTESIAN_POINT('Ctrl Pts',(-53.9027943919814,50.5856807248133,12.));
#92668=CARTESIAN_POINT('Ctrl Pts',(-53.8771919737007,50.5766390561861,12.));
#92669=CARTESIAN_POINT('Ctrl Pts',(-53.8516317071783,50.567586018852,12.));
#92670=CARTESIAN_POINT('Ctrl Pts',(-53.8261136593064,50.5585216854082,12.));
#92671=CARTESIAN_POINT('Ctrl Pts',(-53.8006378970198,50.5494461285762,12.));
#92672=CARTESIAN_POINT('Ctrl Pts',(-53.7752044876313,50.5403594216706,12.));
#92673=CARTESIAN_POINT('Ctrl Pts',(-53.7498134991714,50.5312616390789,12.));
#92674=CARTESIAN_POINT('Ctrl Pts',(-53.7244650002382,50.5221528560427,12.));
#92675=CARTESIAN_POINT('Ctrl Pts',(-53.6991590598551,50.5130331484563,12.));
#92676=CARTESIAN_POINT('Ctrl Pts',(-53.6738957473158,50.5039025926531,12.));
#92677=CARTESIAN_POINT('Ctrl Pts',(-53.6486751320434,50.4947612652147,12.));
#92678=CARTESIAN_POINT('Ctrl Pts',(-53.6234972834055,50.4856092427309,12.));
#92679=CARTESIAN_POINT('Ctrl Pts',(-53.5983622707231,50.4764466018064,12.));
#92680=CARTESIAN_POINT('Ctrl Pts',(-53.5732701633603,50.4672734191749,12.));
#92681=CARTESIAN_POINT('Ctrl Pts',(-53.5482210307864,50.4580897717835,12.));
#92682=CARTESIAN_POINT('Ctrl Pts',(-53.5232149426415,50.4488957368841,12.));
#92683=CARTESIAN_POINT('Ctrl Pts',(-53.4982519688032,50.4396913921389,12.));
#92684=CARTESIAN_POINT('Ctrl Pts',(-53.4733321794199,50.4304768156677,12.));
#92685=CARTESIAN_POINT('Ctrl Pts',(-53.4484556448787,50.4212520859924,12.));
#92686=CARTESIAN_POINT('Ctrl Pts',(-53.4236224357846,50.4120172820054,12.));
#92687=CARTESIAN_POINT('Ctrl Pts',(-53.3988326229308,50.4027724829296,12.));
#92688=CARTESIAN_POINT('Ctrl Pts',(-53.3740862772673,50.393517768283,12.));
#92689=CARTESIAN_POINT('Ctrl Pts',(-53.3493834698685,50.384253217845,12.));
#92690=CARTESIAN_POINT('Ctrl Pts',(-53.3247242719575,50.3749789116777,12.));
#92691=CARTESIAN_POINT('Ctrl Pts',(-53.3001087549222,50.3656949301423,12.));
#92692=CARTESIAN_POINT('Ctrl Pts',(-53.2755369903291,50.3564013539198,12.));
#92693=CARTESIAN_POINT('Ctrl Pts',(-53.2510090499341,50.3470982640293,12.));
#92694=CARTESIAN_POINT('Ctrl Pts',(-53.2265250056896,50.3377857418522,12.));
#92695=CARTESIAN_POINT('Ctrl Pts',(-53.202084929748,50.3284638691285,12.));
#92696=CARTESIAN_POINT('Ctrl Pts',(-53.1776888944622,50.3191327279497,12.));
#92697=CARTESIAN_POINT('Ctrl Pts',(-53.153336972382,50.3097924007535,12.));
#92698=CARTESIAN_POINT('Ctrl Pts',(-53.1290292362482,50.3004429703188,12.));
#92699=CARTESIAN_POINT('Ctrl Pts',(-53.1047657589806,50.2910845197615,12.));
#92700=CARTESIAN_POINT('Ctrl Pts',(-53.0805466136791,50.2817171325354,12.));
#92701=CARTESIAN_POINT('Ctrl Pts',(-53.0563718736361,50.272340892437,12.));
#92702=CARTESIAN_POINT('Ctrl Pts',(-53.0322416123404,50.262955883611,12.));
#92703=CARTESIAN_POINT('Ctrl Pts',(-53.0081559034802,50.2535621905553,12.));
#92704=CARTESIAN_POINT('Ctrl Pts',(-52.9841148209404,50.2441598981286,12.));
#92705=CARTESIAN_POINT('Ctrl Pts',(-52.9601184388027,50.2347490915553,12.));
#92706=CARTESIAN_POINT('Ctrl Pts',(-52.9361668313539,50.2253298564237,12.));
#92707=CARTESIAN_POINT('Ctrl Pts',(-52.9122600730882,50.2159022786876,12.));
#92708=CARTESIAN_POINT('Ctrl Pts',(-52.8883982387068,50.2064664446663,12.));
#92709=CARTESIAN_POINT('Ctrl Pts',(-52.8645814031137,50.1970224410476,12.));
#92710=CARTESIAN_POINT('Ctrl Pts',(-52.8408096414101,50.1875703548893,12.));
#92711=CARTESIAN_POINT('Ctrl Pts',(-52.8170830289052,50.1781102736215,12.));
#92712=CARTESIAN_POINT('Ctrl Pts',(-52.793401641121,50.1686422850493,12.));
#92713=CARTESIAN_POINT('Ctrl Pts',(-52.769765553794,50.1591664773561,12.));
#92714=CARTESIAN_POINT('Ctrl Pts',(-52.7461748428733,50.1496829391068,12.));
#92715=CARTESIAN_POINT('Ctrl Pts',(-52.7226295845156,50.1401917592532,12.));
#92716=CARTESIAN_POINT('Ctrl Pts',(-52.6991298550928,50.1306930271343,12.));
#92717=CARTESIAN_POINT('Ctrl Pts',(-52.6756757311979,50.1211868324781,12.));
#92718=CARTESIAN_POINT('Ctrl Pts',(-52.6522672896462,50.1116732654041,12.));
#92719=CARTESIAN_POINT('Ctrl Pts',(-52.6289046074743,50.1021524164261,12.));
#92720=CARTESIAN_POINT('Ctrl Pts',(-52.6055877619338,50.0926243764569,12.));
#92721=CARTESIAN_POINT('Ctrl Pts',(-52.5823168304981,50.0830892368095,12.));
#92722=CARTESIAN_POINT('Ctrl Pts',(-52.5590918908691,50.0735470891996,12.));
#92723=CARTESIAN_POINT('Ctrl Pts',(-52.5359130209789,50.0639980257477,12.));
#92724=CARTESIAN_POINT('Ctrl Pts',(-52.5127802989903,50.0544421389824,12.));
#92725=CARTESIAN_POINT('Ctrl Pts',(-52.4896938032896,50.0448795218453,12.));
#92726=CARTESIAN_POINT('Ctrl Pts',(-52.4666536124926,50.0353102676933,12.));
#92727=CARTESIAN_POINT('Ctrl Pts',(-52.4436598054523,50.0257344703008,12.));
#92728=CARTESIAN_POINT('Ctrl Pts',(-52.420712461261,50.0161522238619,12.));
#92729=CARTESIAN_POINT('Ctrl Pts',(-52.3978116592505,50.0065636229934,12.));
#92730=CARTESIAN_POINT('Ctrl Pts',(-52.3749574789865,49.9969687627402,12.));
#92731=CARTESIAN_POINT('Ctrl Pts',(-52.3521500002711,49.9873677385769,12.));
#92732=CARTESIAN_POINT('Ctrl Pts',(-52.3293893031524,49.9777606464103,12.));
#92733=CARTESIAN_POINT('Ctrl Pts',(-52.3066754679265,49.9681475825824,12.));
#92734=CARTESIAN_POINT('Ctrl Pts',(-52.2840085751385,49.9585286438734,12.));
#92735=CARTESIAN_POINT('Ctrl Pts',(-52.2613887055773,49.9489039275064,12.));
#92736=CARTESIAN_POINT('Ctrl Pts',(-52.238815940277,49.9392735311507,12.));
#92737=CARTESIAN_POINT('Ctrl Pts',(-52.2162903605272,49.9296375529241,12.));
#92738=CARTESIAN_POINT('Ctrl Pts',(-52.1938120478752,49.919996091396,12.));
#92739=CARTESIAN_POINT('Ctrl Pts',(-52.1713810841277,49.9103492455904,12.));
#92740=CARTESIAN_POINT('Ctrl Pts',(-52.1489975513449,49.90069711499,12.));
#92741=CARTESIAN_POINT('Ctrl Pts',(-52.1266615318414,49.8910397995404,12.));
#92742=CARTESIAN_POINT('Ctrl Pts',(-52.1043731081968,49.8813773996523,12.));
#92743=CARTESIAN_POINT('Ctrl Pts',(-52.0821323632588,49.871710016205,12.));
#92744=CARTESIAN_POINT('Ctrl Pts',(-52.059939380145,49.8620377505498,12.));
#92745=CARTESIAN_POINT('Ctrl Pts',(-52.0377942422373,49.8523607045146,12.));
#92746=CARTESIAN_POINT('Ctrl Pts',(-52.015697033182,49.8426789804068,12.));
#92747=CARTESIAN_POINT('Ctrl Pts',(-51.9936478369008,49.8329926810172,12.));
#92748=CARTESIAN_POINT('Ctrl Pts',(-51.9716467375938,49.8233019096224,12.));
#92749=CARTESIAN_POINT('Ctrl Pts',(-51.9496938197418,49.8136067699896,12.));
#92750=CARTESIAN_POINT('Ctrl Pts',(-51.9277891681014,49.8039073663808,12.));
#92751=CARTESIAN_POINT('Ctrl Pts',(-51.9059328677051,49.7942038035568,12.));
#92752=CARTESIAN_POINT('Ctrl Pts',(-51.8841250038716,49.78449618678,12.));
#92753=CARTESIAN_POINT('Ctrl Pts',(-51.8623656622092,49.7747846218177,12.));
#92754=CARTESIAN_POINT('Ctrl Pts',(-51.8406549286177,49.7650692149464,12.));
#92755=CARTESIAN_POINT('Ctrl Pts',(-51.8189928892841,49.7553500729563,12.));
#92756=CARTESIAN_POINT('Ctrl Pts',(-51.7973796306826,49.7456273031555,12.));
#92757=CARTESIAN_POINT('Ctrl Pts',(-51.7758152395857,49.7359010133741,12.));
#92758=CARTESIAN_POINT('Ctrl Pts',(-51.754299803068,49.7261713119672,12.));
#92759=CARTESIAN_POINT('Ctrl Pts',(-51.7328334085084,49.7164383078206,12.));
#92760=CARTESIAN_POINT('Ctrl Pts',(-51.7114161435848,49.7067021103534,12.));
#92761=CARTESIAN_POINT('Ctrl Pts',(-51.6900480962744,49.6969628295236,12.));
#92762=CARTESIAN_POINT('Ctrl Pts',(-51.6687293548656,49.6872205758314,12.));
#92763=CARTESIAN_POINT('Ctrl Pts',(-51.6474600079611,49.6774754603235,12.));
#92764=CARTESIAN_POINT('Ctrl Pts',(-51.6262401444799,49.6677275945975,12.));
#92765=CARTESIAN_POINT('Ctrl Pts',(-51.6050698536525,49.6579770908063,12.));
#92766=CARTESIAN_POINT('Ctrl Pts',(-51.5839492250218,49.6482240616627,12.));
#92767=CARTESIAN_POINT('Ctrl Pts',(-51.5628783484556,49.6384686204443,12.));
#92768=CARTESIAN_POINT('Ctrl Pts',(-51.5418573141494,49.6287108809975,12.));
#92769=CARTESIAN_POINT('Ctrl Pts',(-51.5208862126303,49.6189509577441,12.));
#92770=CARTESIAN_POINT('Ctrl Pts',(-51.4999651347496,49.609188965684,12.));
#92771=CARTESIAN_POINT('Ctrl Pts',(-51.4790941716859,49.5994250204003,12.));
#92772=CARTESIAN_POINT('Ctrl Pts',(-51.4582734149562,49.5896592380634,12.));
#92773=CARTESIAN_POINT('Ctrl Pts',(-51.4375029564191,49.579891735436,12.));
#92774=CARTESIAN_POINT('Ctrl Pts',(-51.4167828882765,49.5701226298779,12.));
#92775=CARTESIAN_POINT('Ctrl Pts',(-51.3961133030688,49.5603520393514,12.));
#92776=CARTESIAN_POINT('Ctrl Pts',(-51.3754942936796,49.5505800824268,12.));
#92777=CARTESIAN_POINT('Ctrl Pts',(-51.354925953347,49.5408068782871,12.));
#92778=CARTESIAN_POINT('Ctrl Pts',(-51.3344083756659,49.5310325467334,12.));
#92779=CARTESIAN_POINT('Ctrl Pts',(-51.3139416545903,49.5212572081901,12.));
#92780=CARTESIAN_POINT('Ctrl Pts',(-51.2935258844278,49.5114809837111,12.));
#92781=CARTESIAN_POINT('Ctrl Pts',(-51.2731611598465,49.5017039949841,12.));
#92782=CARTESIAN_POINT('Ctrl Pts',(-51.2528475758841,49.4919263643357,12.));
#92783=CARTESIAN_POINT('Ctrl Pts',(-51.2325852279507,49.4821482147357,12.));
#92784=CARTESIAN_POINT('Ctrl Pts',(-51.2123742118288,49.4723696698022,12.));
#92785=CARTESIAN_POINT('Ctrl Pts',(-51.1922146236686,49.4625908538076,12.));
#92786=CARTESIAN_POINT('Ctrl Pts',(-51.1721065599972,49.4528118916833,12.));
#92787=CARTESIAN_POINT('Ctrl Pts',(-51.1520501177291,49.4430329090288,12.));
#92788=CARTESIAN_POINT('Ctrl Pts',(-51.1320453941702,49.4332540321178,12.));
#92789=CARTESIAN_POINT('Ctrl Pts',(-51.1120924870196,49.4234753879071,12.));
#92790=CARTESIAN_POINT('Ctrl Pts',(-51.0921914943663,49.4136971040428,12.));
#92791=CARTESIAN_POINT('Ctrl Pts',(-51.0723425146987,49.4039193088635,12.));
#92792=CARTESIAN_POINT('Ctrl Pts',(-51.0525456469072,49.3941421314014,12.));
#92793=CARTESIAN_POINT('Ctrl Pts',(-51.0328009902857,49.3843657013851,12.));
#92794=CARTESIAN_POINT('Ctrl Pts',(-51.0131086445268,49.3745901492428,12.));
#92795=CARTESIAN_POINT('Ctrl Pts',(-50.9934687097179,49.3648156061049,12.));
#92796=CARTESIAN_POINT('Ctrl Pts',(-50.9738812863636,49.3550422038221,12.));
#92797=CARTESIAN_POINT('Ctrl Pts',(-50.9543464753974,49.3452700749804,12.));
#92798=CARTESIAN_POINT('Ctrl Pts',(-50.9348643781928,49.3354993529163,12.));
#92799=CARTESIAN_POINT('Ctrl Pts',(-50.9154350965681,49.325730171735,12.));
#92800=CARTESIAN_POINT('Ctrl Pts',(-50.8960587327869,49.3159626663129,12.));
#92801=CARTESIAN_POINT('Ctrl Pts',(-50.8767353895509,49.3061969722798,12.));
#92802=CARTESIAN_POINT('Ctrl Pts',(-50.8574651699877,49.2964332260043,12.));
#92803=CARTESIAN_POINT('Ctrl Pts',(-50.8382481776392,49.2866715645828,12.));
#92804=CARTESIAN_POINT('Ctrl Pts',(-50.8190845164319,49.2769121258144,12.));
#92805=CARTESIAN_POINT('Ctrl Pts',(-50.7999742907111,49.2671550482415,12.));
#92806=CARTESIAN_POINT('Ctrl Pts',(-50.7809176052954,49.2574004712122,12.));
#92807=CARTESIAN_POINT('Ctrl Pts',(-50.7619145655207,49.2476485349373,12.));
#92808=CARTESIAN_POINT('Ctrl Pts',(-50.7429652772816,49.2378993805482,12.));
#92809=CARTESIAN_POINT('Ctrl Pts',(-50.7240698470698,49.2281531501569,12.));
#92810=CARTESIAN_POINT('Ctrl Pts',(-50.7052283818941,49.218409986748,12.));
#92811=CARTESIAN_POINT('Ctrl Pts',(-50.6864409891905,49.2086700340625,12.));
#92812=CARTESIAN_POINT('Ctrl Pts',(-50.6677077767427,49.1989334364991,12.));
#92813=CARTESIAN_POINT('Ctrl Pts',(-50.6490288525639,49.1892003389743,12.));
#92814=CARTESIAN_POINT('Ctrl Pts',(-50.6304043248796,49.1794708869074,12.));
#92815=CARTESIAN_POINT('Ctrl Pts',(-50.6118343023937,49.1697452265473,12.));
#92816=CARTESIAN_POINT('Ctrl Pts',(-50.593318894516,49.1600235052613,12.));
#92817=CARTESIAN_POINT('Ctrl Pts',(-50.5748582115575,49.1503058717831,12.));
#92818=CARTESIAN_POINT('Ctrl Pts',(-50.5564523650406,49.1405924766169,12.));
#92819=CARTESIAN_POINT('Ctrl Pts',(-50.5381014674822,49.1308834717645,12.));
#92820=CARTESIAN_POINT('Ctrl Pts',(-50.5198056318111,49.1211790099817,12.));
#92821=CARTESIAN_POINT('Ctrl Pts',(-50.5015649708742,49.1114792441573,12.));
#92822=CARTESIAN_POINT('Ctrl Pts',(-50.4833795969296,49.1017843266782,12.));
#92823=CARTESIAN_POINT('Ctrl Pts',(-50.465249621057,49.0920944086973,12.));
#92824=CARTESIAN_POINT('Ctrl Pts',(-50.4471751542717,49.0824096415339,12.));
#92825=CARTESIAN_POINT('Ctrl Pts',(-50.4291563088528,49.0727301783477,12.));
#92826=CARTESIAN_POINT('Ctrl Pts',(-50.4111931994264,49.0630561755082,12.));
#92827=CARTESIAN_POINT('Ctrl Pts',(-50.393285944528,49.0533877945771,12.));
#92828=CARTESIAN_POINT('Ctrl Pts',(-50.3754346667389,49.0437252024868,12.));
#92829=CARTESIAN_POINT('Ctrl Pts',(-50.3576394894136,49.034068567401,12.));
#92830=CARTESIAN_POINT('Ctrl Pts',(-50.3399005337967,49.0244180550759,12.));
#92831=CARTESIAN_POINT('Ctrl Pts',(-50.3222179165102,49.0147738256925,12.));
#92832=CARTESIAN_POINT('Ctrl Pts',(-50.3045917455383,49.0051360288002,12.));
#92833=CARTESIAN_POINT('Ctrl Pts',(-50.2870221241003,48.9955048082028,12.));
#92834=CARTESIAN_POINT('Ctrl Pts',(-50.2695091583473,48.9858803116649,12.));
#92835=CARTESIAN_POINT('Ctrl Pts',(-50.252052963548,48.9762626987227,12.));
#92836=CARTESIAN_POINT('Ctrl Pts',(-50.2346536715465,48.9666521500969,12.));
#92837=CARTESIAN_POINT('Ctrl Pts',(-50.2173114358423,48.9570488741273,12.));
#92838=CARTESIAN_POINT('Ctrl Pts',(-50.2000264157903,48.9474530868847,12.));
#92839=CARTESIAN_POINT('Ctrl Pts',(-50.1827987615659,48.9378649933116,12.));
#92840=CARTESIAN_POINT('Ctrl Pts',(-50.1656286003943,48.9282847698237,12.));
#92841=CARTESIAN_POINT('Ctrl Pts',(-50.148516018447,48.9187125417897,12.));
#92842=CARTESIAN_POINT('Ctrl Pts',(-50.1314610602286,48.9091483817797,12.));
#92843=CARTESIAN_POINT('Ctrl Pts',(-50.1178632066821,48.9015035371772,12.));
#92844=CARTESIAN_POINT('Ctrl Pts',(-50.1076907555303,48.8957735556681,12.));
#92845=CARTESIAN_POINT('Ctrl Pts',(-50.1009206494209,48.8919551910299,12.));
#92846=CARTESIAN_POINT('Ctrl Pts',(-50.0975384783634,48.8900464144686,12.));
#92847=CARTESIAN_POINT('Ctrl Pts',(-55.2174072001495,49.5707719660639,-5.55111512312578E-16));
#92848=CARTESIAN_POINT('Ctrl Pts',(-55.2174072001495,49.5707719660639,4.));
#92849=CARTESIAN_POINT('Ctrl Pts',(-55.2174072001495,49.5707719660639,8.));
#92850=CARTESIAN_POINT('Ctrl Pts',(-55.2174072001495,49.5707719660639,12.));
#92851=CARTESIAN_POINT('Ctrl Pts',(-55.2618153697169,49.6712810246933,-5.55111512312578E-16));
#92852=CARTESIAN_POINT('Ctrl Pts',(-55.2618153697169,49.6712810246933,4.));
#92853=CARTESIAN_POINT('Ctrl Pts',(-55.2618153697169,49.6712810246933,8.));
#92854=CARTESIAN_POINT('Ctrl Pts',(-55.2618153697169,49.6712810246933,12.));
#92855=CARTESIAN_POINT('Ctrl Pts',(-55.2790667815473,49.8732090625342,-5.55111512312578E-16));
#92856=CARTESIAN_POINT('Ctrl Pts',(-55.2790667815473,49.8732090625342,4.));
#92857=CARTESIAN_POINT('Ctrl Pts',(-55.2790667815473,49.8732090625342,7.99999999999999));
#92858=CARTESIAN_POINT('Ctrl Pts',(-55.2790667815473,49.8732090625342,12.));
#92859=CARTESIAN_POINT('Ctrl Pts',(-55.1854902750885,50.0481613529516,-5.55111512312578E-16));
#92860=CARTESIAN_POINT('Ctrl Pts',(-55.1854902750885,50.0481613529516,4.));
#92861=CARTESIAN_POINT('Ctrl Pts',(-55.1854902750885,50.0481613529516,8.00000000000001));
#92862=CARTESIAN_POINT('Ctrl Pts',(-55.1854902750885,50.0481613529516,12.));
#92863=CARTESIAN_POINT('Ctrl Pts',(-55.1300595714123,50.1091461876225,-5.55111512312578E-16));
#92864=CARTESIAN_POINT('Ctrl Pts',(-55.1300595714123,50.1091461876225,4.));
#92865=CARTESIAN_POINT('Ctrl Pts',(-55.1300595714123,50.1091461876225,8.));
#92866=CARTESIAN_POINT('Ctrl Pts',(-55.1300595714123,50.1091461876225,12.));
#92867=CARTESIAN_POINT('',(-55.2174072001495,49.5707719660639,-2.77555756156289E-16));
#92868=CARTESIAN_POINT('',(-55.1300595714124,50.1091461876225,2.77555756156289E-16));
#92869=CARTESIAN_POINT('Ctrl Pts',(-55.2174072001495,49.5707719660639,-5.55111512312578E-16));
#92870=CARTESIAN_POINT('Ctrl Pts',(-55.2618153697169,49.6712810246933,-5.55111512312578E-16));
#92871=CARTESIAN_POINT('Ctrl Pts',(-55.2716733193343,49.7866684748881,-5.55111512312578E-16));
#92872=CARTESIAN_POINT('Ctrl Pts',(-55.2453425609388,49.8932475177609,-5.55111512312578E-16));
#92873=CARTESIAN_POINT('Ctrl Pts',(-55.2255944921423,49.9731817999155,-5.55111512312578E-16));
#92874=CARTESIAN_POINT('Ctrl Pts',(-55.1854902750885,50.0481613529516,-5.55111512312578E-16));
#92875=CARTESIAN_POINT('Ctrl Pts',(-55.1300595714123,50.1091461876225,-5.55111512312578E-16));
#92876=CARTESIAN_POINT('',(-55.1300595714124,50.1091461876225,12.));
#92877=CARTESIAN_POINT('Ctrl Pts',(-55.1300595714123,50.1091461876225,-5.55111512312578E-16));
#92878=CARTESIAN_POINT('Ctrl Pts',(-55.1300595714123,50.1091461876225,4.));
#92879=CARTESIAN_POINT('Ctrl Pts',(-55.1300595714123,50.1091461876225,8.));
#92880=CARTESIAN_POINT('Ctrl Pts',(-55.1300595714123,50.1091461876225,12.));
#92881=CARTESIAN_POINT('',(-55.2174072001495,49.5707719660639,12.));
#92882=CARTESIAN_POINT('Ctrl Pts',(-55.1300595714123,50.1091461876225,12.));
#92883=CARTESIAN_POINT('Ctrl Pts',(-55.1854902750885,50.0481613529516,12.));
#92884=CARTESIAN_POINT('Ctrl Pts',(-55.2255944921423,49.9731817999155,12.));
#92885=CARTESIAN_POINT('Ctrl Pts',(-55.2453425609388,49.8932475177609,12.));
#92886=CARTESIAN_POINT('Ctrl Pts',(-55.2716733193343,49.7866684748881,12.));
#92887=CARTESIAN_POINT('Ctrl Pts',(-55.2618153697169,49.6712810246933,12.));
#92888=CARTESIAN_POINT('Ctrl Pts',(-55.2174072001495,49.5707719660639,12.));
#92889=CARTESIAN_POINT('Ctrl Pts',(-55.2174072001495,49.5707719660639,12.));
#92890=CARTESIAN_POINT('Ctrl Pts',(-55.2174072001495,49.5707719660639,8.));
#92891=CARTESIAN_POINT('Ctrl Pts',(-55.2174072001495,49.5707719660639,4.));
#92892=CARTESIAN_POINT('Ctrl Pts',(-55.2174072001495,49.5707719660639,-5.55111512312578E-16));
#92893=CARTESIAN_POINT('Origin',(-2.7643087079898E-10,2.53167595884892E-10,
0.));
#92894=CARTESIAN_POINT('Origin',(-2.7643087079898E-10,2.53167595884892E-10,
12.));
#92895=CARTESIAN_POINT('Origin',(-2.7643087079898E-10,2.53167595884892E-10,
0.));
#92896=CARTESIAN_POINT('Ctrl Pts',(-50.1091461876247,55.1300595714104,0.));
#92897=CARTESIAN_POINT('Ctrl Pts',(-50.1091461876247,55.1300595714104,4.));
#92898=CARTESIAN_POINT('Ctrl Pts',(-50.1091461876247,55.1300595714104,8.));
#92899=CARTESIAN_POINT('Ctrl Pts',(-50.1091461876247,55.1300595714104,12.));
#92900=CARTESIAN_POINT('Ctrl Pts',(-50.0278330747241,55.2039671763175,0.));
#92901=CARTESIAN_POINT('Ctrl Pts',(-50.0278330747241,55.2039671763175,4.));
#92902=CARTESIAN_POINT('Ctrl Pts',(-50.027833074724,55.2039671763175,8.));
#92903=CARTESIAN_POINT('Ctrl Pts',(-50.027833074724,55.2039671763175,12.));
#92904=CARTESIAN_POINT('Ctrl Pts',(-49.8417173275619,55.2841761056302,0.));
#92905=CARTESIAN_POINT('Ctrl Pts',(-49.8417173275619,55.2841761056302,4.00000000000001));
#92906=CARTESIAN_POINT('Ctrl Pts',(-49.8417173275619,55.2841761056302,8.));
#92907=CARTESIAN_POINT('Ctrl Pts',(-49.8417173275619,55.2841761056302,12.));
#92908=CARTESIAN_POINT('Ctrl Pts',(-49.6461537600013,55.2507133273147,0.));
#92909=CARTESIAN_POINT('Ctrl Pts',(-49.6461537600013,55.2507133273147,4.));
#92910=CARTESIAN_POINT('Ctrl Pts',(-49.6461537600013,55.2507133273147,8.));
#92911=CARTESIAN_POINT('Ctrl Pts',(-49.6461537600013,55.2507133273147,12.));
#92912=CARTESIAN_POINT('Ctrl Pts',(-49.5707719660265,55.2174072001301,0.));
#92913=CARTESIAN_POINT('Ctrl Pts',(-49.5707719660265,55.2174072001301,4.));
#92914=CARTESIAN_POINT('Ctrl Pts',(-49.5707719660265,55.2174072001302,8.));
#92915=CARTESIAN_POINT('Ctrl Pts',(-49.5707719660265,55.2174072001302,12.));
#92916=CARTESIAN_POINT('',(-50.1091461876247,55.1300595714104,0.));
#92917=CARTESIAN_POINT('',(-49.5707719660265,55.2174072001301,0.));
#92918=CARTESIAN_POINT('Ctrl Pts',(-50.1091461876247,55.1300595714104,0.));
#92919=CARTESIAN_POINT('Ctrl Pts',(-50.0278330747241,55.2039671763175,0.));
#92920=CARTESIAN_POINT('Ctrl Pts',(-49.9214812192028,55.2498008502105,0.));
#92921=CARTESIAN_POINT('Ctrl Pts',(-49.8120443611025,55.2585172318167,0.));
#92922=CARTESIAN_POINT('Ctrl Pts',(-49.7299667175273,55.2650545180213,0.));
#92923=CARTESIAN_POINT('Ctrl Pts',(-49.6461537600013,55.2507133273147,0.));
#92924=CARTESIAN_POINT('Ctrl Pts',(-49.5707719660265,55.2174072001301,0.));
#92925=CARTESIAN_POINT('',(-49.5707719660265,55.2174072001301,12.));
#92926=CARTESIAN_POINT('Ctrl Pts',(-49.5707719660265,55.2174072001301,0.));
#92927=CARTESIAN_POINT('Ctrl Pts',(-49.5707719660265,55.2174072001301,4.));
#92928=CARTESIAN_POINT('Ctrl Pts',(-49.5707719660265,55.2174072001302,8.));
#92929=CARTESIAN_POINT('Ctrl Pts',(-49.5707719660265,55.2174072001302,12.));
#92930=CARTESIAN_POINT('',(-50.1091461876247,55.1300595714104,12.));
#92931=CARTESIAN_POINT('Ctrl Pts',(-49.5707719660265,55.2174072001302,12.));
#92932=CARTESIAN_POINT('Ctrl Pts',(-49.6461537600013,55.2507133273147,12.));
#92933=CARTESIAN_POINT('Ctrl Pts',(-49.7299667175272,55.2650545180214,12.));
#92934=CARTESIAN_POINT('Ctrl Pts',(-49.8120443611025,55.2585172318167,12.));
#92935=CARTESIAN_POINT('Ctrl Pts',(-49.9214812192028,55.2498008502105,12.));
#92936=CARTESIAN_POINT('Ctrl Pts',(-50.027833074724,55.2039671763175,12.));
#92937=CARTESIAN_POINT('Ctrl Pts',(-50.1091461876247,55.1300595714104,12.));
#92938=CARTESIAN_POINT('Ctrl Pts',(-50.1091461876247,55.1300595714104,12.));
#92939=CARTESIAN_POINT('Ctrl Pts',(-50.1091461876247,55.1300595714104,8.));
#92940=CARTESIAN_POINT('Ctrl Pts',(-50.1091461876247,55.1300595714104,4.));
#92941=CARTESIAN_POINT('Ctrl Pts',(-50.1091461876247,55.1300595714104,0.));
#92942=CARTESIAN_POINT('Ctrl Pts',(-45.6458539113724,53.0702932034641,0.));
#92943=CARTESIAN_POINT('Ctrl Pts',(-45.6458539113724,53.0702932034641,12.));
#92944=CARTESIAN_POINT('Ctrl Pts',(-45.6490568514089,53.0724894921849,0.));
#92945=CARTESIAN_POINT('Ctrl Pts',(-45.6490568514089,53.0724894921849,12.));
#92946=CARTESIAN_POINT('Ctrl Pts',(-45.6554684028145,53.0768833804193,0.));
#92947=CARTESIAN_POINT('Ctrl Pts',(-45.6554684028145,53.0768833804193,12.));
#92948=CARTESIAN_POINT('Ctrl Pts',(-45.6651027439241,53.0834781451546,0.));
#92949=CARTESIAN_POINT('Ctrl Pts',(-45.6651027439241,53.0834781451546,12.));
#92950=CARTESIAN_POINT('Ctrl Pts',(-45.6779825614231,53.0922790298409,0.));
#92951=CARTESIAN_POINT('Ctrl Pts',(-45.6779825614231,53.0922790298409,12.));
#92952=CARTESIAN_POINT('Ctrl Pts',(-45.694139048907,53.1032932328857,0.));
#92953=CARTESIAN_POINT('Ctrl Pts',(-45.694139048907,53.1032932328857,12.));
#92954=CARTESIAN_POINT('Ctrl Pts',(-45.7103522376696,53.114320495492,0.));
#92955=CARTESIAN_POINT('Ctrl Pts',(-45.7103522376696,53.114320495492,12.));
#92956=CARTESIAN_POINT('Ctrl Pts',(-45.7266220897003,53.1253607414872,0.));
#92957=CARTESIAN_POINT('Ctrl Pts',(-45.7266220897003,53.1253607414872,12.));
#92958=CARTESIAN_POINT('Ctrl Pts',(-45.7429485300823,53.1364138384693,0.));
#92959=CARTESIAN_POINT('Ctrl Pts',(-45.7429485300823,53.1364138384693,12.));
#92960=CARTESIAN_POINT('Ctrl Pts',(-45.7593314474501,53.1474795996053,0.));
#92961=CARTESIAN_POINT('Ctrl Pts',(-45.7593314474501,53.1474795996053,12.));
#92962=CARTESIAN_POINT('Ctrl Pts',(-45.7757707100618,53.1585578076444,0.));
#92963=CARTESIAN_POINT('Ctrl Pts',(-45.7757707100618,53.1585578076444,12.));
#92964=CARTESIAN_POINT('Ctrl Pts',(-45.7922661780005,53.1696482334487,0.));
#92965=CARTESIAN_POINT('Ctrl Pts',(-45.7922661780005,53.1696482334487,12.));
#92966=CARTESIAN_POINT('Ctrl Pts',(-45.808817716509,53.1807506560933,0.));
#92967=CARTESIAN_POINT('Ctrl Pts',(-45.808817716509,53.1807506560933,12.));
#92968=CARTESIAN_POINT('Ctrl Pts',(-45.8254252099957,53.1918648840541,0.));
#92969=CARTESIAN_POINT('Ctrl Pts',(-45.8254252099957,53.1918648840541,12.));
#92970=CARTESIAN_POINT('Ctrl Pts',(-45.8420885575349,53.2029907483557,0.));
#92971=CARTESIAN_POINT('Ctrl Pts',(-45.8420885575349,53.2029907483557,12.));
#92972=CARTESIAN_POINT('Ctrl Pts',(-45.8588076662582,53.2141280925439,0.));
#92973=CARTESIAN_POINT('Ctrl Pts',(-45.8588076662582,53.2141280925439,12.));
#92974=CARTESIAN_POINT('Ctrl Pts',(-45.8755824458723,53.2252767643662,0.));
#92975=CARTESIAN_POINT('Ctrl Pts',(-45.8755824458723,53.2252767643662,12.));
#92976=CARTESIAN_POINT('Ctrl Pts',(-45.892412801838,53.2364366054306,0.));
#92977=CARTESIAN_POINT('Ctrl Pts',(-45.892412801838,53.2364366054306,12.));
#92978=CARTESIAN_POINT('Ctrl Pts',(-45.9092986319377,53.2476074460017,0.));
#92979=CARTESIAN_POINT('Ctrl Pts',(-45.9092986319377,53.2476074460017,12.));
#92980=CARTESIAN_POINT('Ctrl Pts',(-45.9262398298349,53.2587891103866,0.));
#92981=CARTESIAN_POINT('Ctrl Pts',(-45.9262398298349,53.2587891103866,12.));
#92982=CARTESIAN_POINT('Ctrl Pts',(-45.9432362873008,53.2699814203105,0.));
#92983=CARTESIAN_POINT('Ctrl Pts',(-45.9432362873008,53.2699814203105,12.));
#92984=CARTESIAN_POINT('Ctrl Pts',(-45.9602878967698,53.2811841987926,0.));
#92985=CARTESIAN_POINT('Ctrl Pts',(-45.9602878967698,53.2811841987926,12.));
#92986=CARTESIAN_POINT('Ctrl Pts',(-45.9773945542384,53.292397274555,0.));
#92987=CARTESIAN_POINT('Ctrl Pts',(-45.9773945542384,53.292397274555,12.));
#92988=CARTESIAN_POINT('Ctrl Pts',(-45.9945561591453,53.3036204818329,0.));
#92989=CARTESIAN_POINT('Ctrl Pts',(-45.9945561591453,53.3036204818329,12.));
#92990=CARTESIAN_POINT('Ctrl Pts',(-46.0117726129873,53.3148536582635,0.));
#92991=CARTESIAN_POINT('Ctrl Pts',(-46.0117726129873,53.3148536582635,12.));
#92992=CARTESIAN_POINT('Ctrl Pts',(-46.02904381836,53.326096643428,0.));
#92993=CARTESIAN_POINT('Ctrl Pts',(-46.02904381836,53.326096643428,12.));
#92994=CARTESIAN_POINT('Ctrl Pts',(-46.0463696777801,53.3373492770671,0.));
#92995=CARTESIAN_POINT('Ctrl Pts',(-46.0463696777801,53.3373492770671,12.));
#92996=CARTESIAN_POINT('Ctrl Pts',(-46.0637500926982,53.3486113975901,0.));
#92997=CARTESIAN_POINT('Ctrl Pts',(-46.0637500926982,53.3486113975901,12.));
#92998=CARTESIAN_POINT('Ctrl Pts',(-46.0811849640218,53.3598828428546,0.));
#92999=CARTESIAN_POINT('Ctrl Pts',(-46.0811849640218,53.3598828428546,12.));
#93000=CARTESIAN_POINT('Ctrl Pts',(-46.0986741925656,53.3711634508437,0.));
#93001=CARTESIAN_POINT('Ctrl Pts',(-46.0986741925656,53.3711634508437,12.));
#93002=CARTESIAN_POINT('Ctrl Pts',(-46.1162176794884,53.3824530603276,0.));
#93003=CARTESIAN_POINT('Ctrl Pts',(-46.1162176794884,53.3824530603276,12.));
#93004=CARTESIAN_POINT('Ctrl Pts',(-46.1338153268097,53.3937515116549,0.));
#93005=CARTESIAN_POINT('Ctrl Pts',(-46.1338153268097,53.3937515116549,12.));
#93006=CARTESIAN_POINT('Ctrl Pts',(-46.1514670376012,53.4050586470436,0.));
#93007=CARTESIAN_POINT('Ctrl Pts',(-46.1514670376012,53.4050586470436,12.));
#93008=CARTESIAN_POINT('Ctrl Pts',(-46.1691727157134,53.4163743101517,0.));
#93009=CARTESIAN_POINT('Ctrl Pts',(-46.1691727157134,53.4163743101517,12.));
#93010=CARTESIAN_POINT('Ctrl Pts',(-46.1869322656024,53.4276983458125,0.));
#93011=CARTESIAN_POINT('Ctrl Pts',(-46.1869322656024,53.4276983458125,12.));
#93012=CARTESIAN_POINT('Ctrl Pts',(-46.2047455921286,53.4390305997274,0.));
#93013=CARTESIAN_POINT('Ctrl Pts',(-46.2047455921286,53.4390305997274,12.));
#93014=CARTESIAN_POINT('Ctrl Pts',(-46.2226126003202,53.4503709181178,0.));
#93015=CARTESIAN_POINT('Ctrl Pts',(-46.2226126003202,53.4503709181178,12.));
#93016=CARTESIAN_POINT('Ctrl Pts',(-46.2405331953889,53.4617191477402,0.));
#93017=CARTESIAN_POINT('Ctrl Pts',(-46.2405331953889,53.4617191477402,12.));
#93018=CARTESIAN_POINT('Ctrl Pts',(-46.2585072828353,53.4730751360371,0.));
#93019=CARTESIAN_POINT('Ctrl Pts',(-46.2585072828353,53.4730751360371,12.));
#93020=CARTESIAN_POINT('Ctrl Pts',(-46.2765347685198,53.4844387312414,0.));
#93021=CARTESIAN_POINT('Ctrl Pts',(-46.2765347685198,53.4844387312414,12.));
#93022=CARTESIAN_POINT('Ctrl Pts',(-46.2946155587417,53.4958097825006,0.));
#93023=CARTESIAN_POINT('Ctrl Pts',(-46.2946155587417,53.4958097825006,12.));
#93024=CARTESIAN_POINT('Ctrl Pts',(-46.3127495603098,53.5071881399911,0.));
#93025=CARTESIAN_POINT('Ctrl Pts',(-46.3127495603098,53.5071881399911,12.));
#93026=CARTESIAN_POINT('Ctrl Pts',(-46.3309366805093,53.5185736548548,0.));
#93027=CARTESIAN_POINT('Ctrl Pts',(-46.3309366805093,53.5185736548548,12.));
#93028=CARTESIAN_POINT('Ctrl Pts',(-46.3491768270655,53.5299661791385,0.));
#93029=CARTESIAN_POINT('Ctrl Pts',(-46.3491768270655,53.5299661791385,12.));
#93030=CARTESIAN_POINT('Ctrl Pts',(-46.3674699081046,53.5413655657327,0.));
#93031=CARTESIAN_POINT('Ctrl Pts',(-46.3674699081046,53.5413655657327,12.));
#93032=CARTESIAN_POINT('Ctrl Pts',(-46.3858158321059,53.5527716683047,0.));
#93033=CARTESIAN_POINT('Ctrl Pts',(-46.3858158321059,53.5527716683047,12.));
#93034=CARTESIAN_POINT('Ctrl Pts',(-46.4042145078701,53.5641843412559,0.));
#93035=CARTESIAN_POINT('Ctrl Pts',(-46.4042145078701,53.5641843412559,12.));
#93036=CARTESIAN_POINT('Ctrl Pts',(-46.4226658445474,53.5756034397481,0.));
#93037=CARTESIAN_POINT('Ctrl Pts',(-46.4226658445474,53.5756034397481,12.));
#93038=CARTESIAN_POINT('Ctrl Pts',(-46.4411697516478,53.5870288197166,0.));
#93039=CARTESIAN_POINT('Ctrl Pts',(-46.4411697516478,53.5870288197166,12.));
#93040=CARTESIAN_POINT('Ctrl Pts',(-46.459726139052,53.5984603378855,0.));
#93041=CARTESIAN_POINT('Ctrl Pts',(-46.459726139052,53.5984603378855,12.));
#93042=CARTESIAN_POINT('Ctrl Pts',(-46.4783349170173,53.6098978517859,0.));
#93043=CARTESIAN_POINT('Ctrl Pts',(-46.4783349170173,53.6098978517859,12.));
#93044=CARTESIAN_POINT('Ctrl Pts',(-46.496995996177,53.6213412197533,0.));
#93045=CARTESIAN_POINT('Ctrl Pts',(-46.496995996177,53.6213412197533,12.));
#93046=CARTESIAN_POINT('Ctrl Pts',(-46.5157092875373,53.6327903009094,0.));
#93047=CARTESIAN_POINT('Ctrl Pts',(-46.5157092875373,53.6327903009094,12.));
#93048=CARTESIAN_POINT('Ctrl Pts',(-46.5344747024676,53.6442449551455,0.));
#93049=CARTESIAN_POINT('Ctrl Pts',(-46.5344747024676,53.6442449551455,12.));
#93050=CARTESIAN_POINT('Ctrl Pts',(-46.5532921526901,53.6557050431071,0.));
#93051=CARTESIAN_POINT('Ctrl Pts',(-46.5532921526901,53.6557050431071,12.));
#93052=CARTESIAN_POINT('Ctrl Pts',(-46.5721615502591,53.6671704261737,0.));
#93053=CARTESIAN_POINT('Ctrl Pts',(-46.5721615502591,53.6671704261737,12.));
#93054=CARTESIAN_POINT('Ctrl Pts',(-46.5910828075653,53.678640966456,0.));
#93055=CARTESIAN_POINT('Ctrl Pts',(-46.5910828075653,53.678640966456,12.));
#93056=CARTESIAN_POINT('Ctrl Pts',(-46.6100558373402,53.6901165267941,0.));
#93057=CARTESIAN_POINT('Ctrl Pts',(-46.6100558373402,53.6901165267941,12.));
#93058=CARTESIAN_POINT('Ctrl Pts',(-46.6290805526559,53.701596970754,0.));
#93059=CARTESIAN_POINT('Ctrl Pts',(-46.6290805526559,53.701596970754,12.));
#93060=CARTESIAN_POINT('Ctrl Pts',(-46.6481568669216,53.7130821626263,0.));
#93061=CARTESIAN_POINT('Ctrl Pts',(-46.6481568669216,53.7130821626263,12.));
#93062=CARTESIAN_POINT('Ctrl Pts',(-46.6672846938752,53.7245719674222,0.));
#93063=CARTESIAN_POINT('Ctrl Pts',(-46.6672846938752,53.7245719674222,12.));
#93064=CARTESIAN_POINT('Ctrl Pts',(-46.6864639475863,53.7360662508677,0.));
#93065=CARTESIAN_POINT('Ctrl Pts',(-46.6864639475863,53.7360662508677,12.));
#93066=CARTESIAN_POINT('Ctrl Pts',(-46.7056945424559,53.7475648793948,0.));
#93067=CARTESIAN_POINT('Ctrl Pts',(-46.7056945424559,53.7475648793948,12.));
#93068=CARTESIAN_POINT('Ctrl Pts',(-46.724976393213,53.7590677201344,0.));
#93069=CARTESIAN_POINT('Ctrl Pts',(-46.724976393213,53.7590677201344,12.));
#93070=CARTESIAN_POINT('Ctrl Pts',(-46.7443094149041,53.770574640907,0.));
#93071=CARTESIAN_POINT('Ctrl Pts',(-46.7443094149041,53.770574640907,12.));
#93072=CARTESIAN_POINT('Ctrl Pts',(-46.7636935228851,53.7820855102169,0.));
#93073=CARTESIAN_POINT('Ctrl Pts',(-46.7636935228851,53.7820855102169,12.));
#93074=CARTESIAN_POINT('Ctrl Pts',(-46.7831286328268,53.7936001972468,0.));
#93075=CARTESIAN_POINT('Ctrl Pts',(-46.7831286328268,53.7936001972468,12.));
#93076=CARTESIAN_POINT('Ctrl Pts',(-46.8026146607144,53.8051185718524,0.));
#93077=CARTESIAN_POINT('Ctrl Pts',(-46.8026146607144,53.8051185718524,12.));
#93078=CARTESIAN_POINT('Ctrl Pts',(-46.8221515228459,53.8166405045582,0.));
#93079=CARTESIAN_POINT('Ctrl Pts',(-46.8221515228459,53.8166405045582,12.));
#93080=CARTESIAN_POINT('Ctrl Pts',(-46.8417391358231,53.8281658665517,0.));
#93081=CARTESIAN_POINT('Ctrl Pts',(-46.8417391358231,53.8281658665517,12.));
#93082=CARTESIAN_POINT('Ctrl Pts',(-46.8613774165452,53.8396945296777,0.));
#93083=CARTESIAN_POINT('Ctrl Pts',(-46.8613774165452,53.8396945296777,12.));
#93084=CARTESIAN_POINT('Ctrl Pts',(-46.8810662822147,53.851226366434,0.));
#93085=CARTESIAN_POINT('Ctrl Pts',(-46.8810662822147,53.851226366434,12.));
#93086=CARTESIAN_POINT('Ctrl Pts',(-46.900805650336,53.8627612499648,0.));
#93087=CARTESIAN_POINT('Ctrl Pts',(-46.900805650336,53.8627612499648,12.));
#93088=CARTESIAN_POINT('Ctrl Pts',(-46.9205954387128,53.8742990540557,0.));
#93089=CARTESIAN_POINT('Ctrl Pts',(-46.9205954387128,53.8742990540557,12.));
#93090=CARTESIAN_POINT('Ctrl Pts',(-46.9404355654381,53.8858396531277,0.));
#93091=CARTESIAN_POINT('Ctrl Pts',(-46.9404355654381,53.8858396531277,12.));
#93092=CARTESIAN_POINT('Ctrl Pts',(-46.9603259488894,53.8973829222317,0.));
#93093=CARTESIAN_POINT('Ctrl Pts',(-46.9603259488894,53.8973829222317,12.));
#93094=CARTESIAN_POINT('Ctrl Pts',(-46.9802665077342,53.9089287370435,0.));
#93095=CARTESIAN_POINT('Ctrl Pts',(-46.9802665077342,53.9089287370435,12.));
#93096=CARTESIAN_POINT('Ctrl Pts',(-47.0002571609286,53.9204769738583,0.));
#93097=CARTESIAN_POINT('Ctrl Pts',(-47.0002571609286,53.9204769738583,12.));
#93098=CARTESIAN_POINT('Ctrl Pts',(-47.0202978277148,53.9320275095864,0.));
#93099=CARTESIAN_POINT('Ctrl Pts',(-47.0202978277148,53.9320275095864,12.));
#93100=CARTESIAN_POINT('Ctrl Pts',(-47.04038842761,53.9435802217468,0.));
#93101=CARTESIAN_POINT('Ctrl Pts',(-47.04038842761,53.9435802217468,12.));
#93102=CARTESIAN_POINT('Ctrl Pts',(-47.0605288804042,53.9551349884637,0.));
#93103=CARTESIAN_POINT('Ctrl Pts',(-47.0605288804042,53.9551349884637,12.));
#93104=CARTESIAN_POINT('Ctrl Pts',(-47.0807191061674,53.9666916884624,0.));
#93105=CARTESIAN_POINT('Ctrl Pts',(-47.0807191061674,53.9666916884624,12.));
#93106=CARTESIAN_POINT('Ctrl Pts',(-47.1009590252466,53.9782502010642,0.));
#93107=CARTESIAN_POINT('Ctrl Pts',(-47.1009590252466,53.9782502010642,12.));
#93108=CARTESIAN_POINT('Ctrl Pts',(-47.1212485582632,53.9898104061809,0.));
#93109=CARTESIAN_POINT('Ctrl Pts',(-47.1212485582632,53.9898104061809,12.));
#93110=CARTESIAN_POINT('Ctrl Pts',(-47.1415876261012,54.0013721843094,0.));
#93111=CARTESIAN_POINT('Ctrl Pts',(-47.1415876261012,54.0013721843094,12.));
#93112=CARTESIAN_POINT('Ctrl Pts',(-47.161976149906,54.0129354165269,0.));
#93113=CARTESIAN_POINT('Ctrl Pts',(-47.161976149906,54.0129354165269,12.));
#93114=CARTESIAN_POINT('Ctrl Pts',(-47.1824140510906,54.0244999844872,0.));
#93115=CARTESIAN_POINT('Ctrl Pts',(-47.1824140510906,54.0244999844872,12.));
#93116=CARTESIAN_POINT('Ctrl Pts',(-47.2029012513334,54.0360657704156,0.));
#93117=CARTESIAN_POINT('Ctrl Pts',(-47.2029012513334,54.0360657704156,12.));
#93118=CARTESIAN_POINT('Ctrl Pts',(-47.2234376725752,54.047632657105,0.));
#93119=CARTESIAN_POINT('Ctrl Pts',(-47.2234376725752,54.047632657105,12.));
#93120=CARTESIAN_POINT('Ctrl Pts',(-47.2440232370085,54.0592005279108,0.));
#93121=CARTESIAN_POINT('Ctrl Pts',(-47.2440232370085,54.0592005279108,12.));
#93122=CARTESIAN_POINT('Ctrl Pts',(-47.2646578670767,54.0707692667461,0.));
#93123=CARTESIAN_POINT('Ctrl Pts',(-47.2646578670767,54.0707692667461,12.));
#93124=CARTESIAN_POINT('Ctrl Pts',(-47.2853414854805,54.082338758079,0.));
#93125=CARTESIAN_POINT('Ctrl Pts',(-47.2853414854805,54.082338758079,12.));
#93126=CARTESIAN_POINT('Ctrl Pts',(-47.3060740151754,54.093908886927,0.));
#93127=CARTESIAN_POINT('Ctrl Pts',(-47.3060740151754,54.093908886927,12.));
#93128=CARTESIAN_POINT('Ctrl Pts',(-47.326855379369,54.1054795388538,0.));
#93129=CARTESIAN_POINT('Ctrl Pts',(-47.326855379369,54.1054795388538,12.));
#93130=CARTESIAN_POINT('Ctrl Pts',(-47.3476855015095,54.1170505999637,0.));
#93131=CARTESIAN_POINT('Ctrl Pts',(-47.3476855015095,54.1170505999637,12.));
#93132=CARTESIAN_POINT('Ctrl Pts',(-47.3685643052867,54.128621956898,0.));
#93133=CARTESIAN_POINT('Ctrl Pts',(-47.3685643052867,54.128621956898,12.));
#93134=CARTESIAN_POINT('Ctrl Pts',(-47.3894917146361,54.1401934968306,0.));
#93135=CARTESIAN_POINT('Ctrl Pts',(-47.3894917146361,54.1401934968306,12.));
#93136=CARTESIAN_POINT('Ctrl Pts',(-47.4104676537381,54.1517651074638,0.));
#93137=CARTESIAN_POINT('Ctrl Pts',(-47.4104676537381,54.1517651074638,12.));
#93138=CARTESIAN_POINT('Ctrl Pts',(-47.4314920470142,54.163336677024,0.));
#93139=CARTESIAN_POINT('Ctrl Pts',(-47.4314920470142,54.163336677024,12.));
#93140=CARTESIAN_POINT('Ctrl Pts',(-47.4525648191173,54.1749080942593,0.));
#93141=CARTESIAN_POINT('Ctrl Pts',(-47.4525648191173,54.1749080942593,12.));
#93142=CARTESIAN_POINT('Ctrl Pts',(-47.473685894932,54.1864792484343,0.));
#93143=CARTESIAN_POINT('Ctrl Pts',(-47.473685894932,54.1864792484343,12.));
#93144=CARTESIAN_POINT('Ctrl Pts',(-47.4948551995799,54.1980500293267,0.));
#93145=CARTESIAN_POINT('Ctrl Pts',(-47.4948551995799,54.1980500293267,12.));
#93146=CARTESIAN_POINT('Ctrl Pts',(-47.5160726584172,54.2096203272228,0.));
#93147=CARTESIAN_POINT('Ctrl Pts',(-47.5160726584172,54.2096203272228,12.));
#93148=CARTESIAN_POINT('Ctrl Pts',(-47.5373381970328,54.221190032914,0.));
#93149=CARTESIAN_POINT('Ctrl Pts',(-47.5373381970328,54.221190032914,12.));
#93150=CARTESIAN_POINT('Ctrl Pts',(-47.5586517412368,54.232759037693,0.));
#93151=CARTESIAN_POINT('Ctrl Pts',(-47.5586517412368,54.232759037693,12.));
#93152=CARTESIAN_POINT('Ctrl Pts',(-47.5800132170614,54.2443272333498,0.));
#93153=CARTESIAN_POINT('Ctrl Pts',(-47.5800132170614,54.2443272333498,12.));
#93154=CARTESIAN_POINT('Ctrl Pts',(-47.6014225507664,54.2558945121684,0.));
#93155=CARTESIAN_POINT('Ctrl Pts',(-47.6014225507664,54.2558945121684,12.));
#93156=CARTESIAN_POINT('Ctrl Pts',(-47.6228796688376,54.2674607669227,0.));
#93157=CARTESIAN_POINT('Ctrl Pts',(-47.6228796688376,54.2674607669227,12.));
#93158=CARTESIAN_POINT('Ctrl Pts',(-47.6443844979846,54.2790258908736,0.));
#93159=CARTESIAN_POINT('Ctrl Pts',(-47.6443844979846,54.2790258908736,12.));
#93160=CARTESIAN_POINT('Ctrl Pts',(-47.6659369651299,54.2905897777647,0.));
#93161=CARTESIAN_POINT('Ctrl Pts',(-47.6659369651299,54.2905897777647,12.));
#93162=CARTESIAN_POINT('Ctrl Pts',(-47.6875369974086,54.3021523218188,0.));
#93163=CARTESIAN_POINT('Ctrl Pts',(-47.6875369974086,54.3021523218188,12.));
#93164=CARTESIAN_POINT('Ctrl Pts',(-47.7091845221747,54.3137134177345,0.));
#93165=CARTESIAN_POINT('Ctrl Pts',(-47.7091845221747,54.3137134177345,12.));
#93166=CARTESIAN_POINT('Ctrl Pts',(-47.7308794669994,54.3252729606824,0.));
#93167=CARTESIAN_POINT('Ctrl Pts',(-47.7308794669994,54.3252729606824,12.));
#93168=CARTESIAN_POINT('Ctrl Pts',(-47.7526217596694,54.3368308463023,0.));
#93169=CARTESIAN_POINT('Ctrl Pts',(-47.7526217596694,54.3368308463023,12.));
#93170=CARTESIAN_POINT('Ctrl Pts',(-47.7744113281768,54.3483869706998,0.));
#93171=CARTESIAN_POINT('Ctrl Pts',(-47.7744113281768,54.3483869706998,12.));
#93172=CARTESIAN_POINT('Ctrl Pts',(-47.7962481007179,54.3599412304431,0.));
#93173=CARTESIAN_POINT('Ctrl Pts',(-47.7962481007179,54.3599412304431,12.));
#93174=CARTESIAN_POINT('Ctrl Pts',(-47.8181320056988,54.3714935225585,0.));
#93175=CARTESIAN_POINT('Ctrl Pts',(-47.8181320056988,54.3714935225585,12.));
#93176=CARTESIAN_POINT('Ctrl Pts',(-47.8400629717352,54.3830437445275,0.));
#93177=CARTESIAN_POINT('Ctrl Pts',(-47.8400629717352,54.3830437445275,12.));
#93178=CARTESIAN_POINT('Ctrl Pts',(-47.8620409276495,54.3945917942835,0.));
#93179=CARTESIAN_POINT('Ctrl Pts',(-47.8620409276495,54.3945917942835,12.));
#93180=CARTESIAN_POINT('Ctrl Pts',(-47.8840658024626,54.4061375702088,0.));
#93181=CARTESIAN_POINT('Ctrl Pts',(-47.8840658024626,54.4061375702088,12.));
#93182=CARTESIAN_POINT('Ctrl Pts',(-47.9061375253909,54.4176809711324,0.));
#93183=CARTESIAN_POINT('Ctrl Pts',(-47.9061375253909,54.4176809711324,12.));
#93184=CARTESIAN_POINT('Ctrl Pts',(-47.9282560258528,54.4292218963253,0.));
#93185=CARTESIAN_POINT('Ctrl Pts',(-47.9282560258528,54.4292218963253,12.));
#93186=CARTESIAN_POINT('Ctrl Pts',(-47.9504212334681,54.4407602454974,0.));
#93187=CARTESIAN_POINT('Ctrl Pts',(-47.9504212334681,54.4407602454974,12.));
#93188=CARTESIAN_POINT('Ctrl Pts',(-47.972633078057,54.4522959187952,0.));
#93189=CARTESIAN_POINT('Ctrl Pts',(-47.972633078057,54.4522959187952,12.));
#93190=CARTESIAN_POINT('Ctrl Pts',(-47.9948914896316,54.4638288167991,0.));
#93191=CARTESIAN_POINT('Ctrl Pts',(-47.9948914896316,54.4638288167991,12.));
#93192=CARTESIAN_POINT('Ctrl Pts',(-48.0171963983912,54.4753588405202,0.));
#93193=CARTESIAN_POINT('Ctrl Pts',(-48.0171963983912,54.4753588405202,12.));
#93194=CARTESIAN_POINT('Ctrl Pts',(-48.039547734729,54.4868858913961,0.));
#93195=CARTESIAN_POINT('Ctrl Pts',(-48.039547734729,54.4868858913961,12.));
#93196=CARTESIAN_POINT('Ctrl Pts',(-48.0619454292321,54.4984098712883,0.));
#93197=CARTESIAN_POINT('Ctrl Pts',(-48.0619454292321,54.4984098712883,12.));
#93198=CARTESIAN_POINT('Ctrl Pts',(-48.0843894126807,54.5099306824788,0.));
#93199=CARTESIAN_POINT('Ctrl Pts',(-48.0843894126807,54.5099306824788,12.));
#93200=CARTESIAN_POINT('Ctrl Pts',(-48.1068796160406,54.5214482276679,0.));
#93201=CARTESIAN_POINT('Ctrl Pts',(-48.1068796160406,54.5214482276679,12.));
#93202=CARTESIAN_POINT('Ctrl Pts',(-48.1294159704571,54.5329624099719,0.));
#93203=CARTESIAN_POINT('Ctrl Pts',(-48.1294159704571,54.5329624099719,12.));
#93204=CARTESIAN_POINT('Ctrl Pts',(-48.1519984072617,54.5444731329196,0.));
#93205=CARTESIAN_POINT('Ctrl Pts',(-48.1519984072617,54.5444731329196,12.));
#93206=CARTESIAN_POINT('Ctrl Pts',(-48.1746268579732,54.5559803004487,0.));
#93207=CARTESIAN_POINT('Ctrl Pts',(-48.1746268579732,54.5559803004487,12.));
#93208=CARTESIAN_POINT('Ctrl Pts',(-48.1973012542966,54.5674838169041,0.));
#93209=CARTESIAN_POINT('Ctrl Pts',(-48.1973012542966,54.5674838169041,12.));
#93210=CARTESIAN_POINT('Ctrl Pts',(-48.2200215281178,54.5789835870348,0.));
#93211=CARTESIAN_POINT('Ctrl Pts',(-48.2200215281178,54.5789835870348,12.));
#93212=CARTESIAN_POINT('Ctrl Pts',(-48.2427876114955,54.5904795159936,0.));
#93213=CARTESIAN_POINT('Ctrl Pts',(-48.2427876114955,54.5904795159936,12.));
#93214=CARTESIAN_POINT('Ctrl Pts',(-48.2655994366672,54.6019715093319,0.));
#93215=CARTESIAN_POINT('Ctrl Pts',(-48.2655994366672,54.6019715093319,12.));
#93216=CARTESIAN_POINT('Ctrl Pts',(-48.288456936051,54.6134594729964,0.));
#93217=CARTESIAN_POINT('Ctrl Pts',(-48.288456936051,54.6134594729964,12.));
#93218=CARTESIAN_POINT('Ctrl Pts',(-48.3113600422443,54.6249433133262,0.));
#93219=CARTESIAN_POINT('Ctrl Pts',(-48.3113600422443,54.6249433133262,12.));
#93220=CARTESIAN_POINT('Ctrl Pts',(-48.3343086880192,54.636422937049,0.));
#93221=CARTESIAN_POINT('Ctrl Pts',(-48.3343086880192,54.636422937049,12.));
#93222=CARTESIAN_POINT('Ctrl Pts',(-48.3573028063122,54.647898251279,0.));
#93223=CARTESIAN_POINT('Ctrl Pts',(-48.3573028063122,54.647898251279,12.));
#93224=CARTESIAN_POINT('Ctrl Pts',(-48.3803423302294,54.6593691635143,0.));
#93225=CARTESIAN_POINT('Ctrl Pts',(-48.3803423302294,54.6593691635143,12.));
#93226=CARTESIAN_POINT('Ctrl Pts',(-48.4034271930516,54.6708355816359,0.));
#93227=CARTESIAN_POINT('Ctrl Pts',(-48.4034271930516,54.6708355816359,12.));
#93228=CARTESIAN_POINT('Ctrl Pts',(-48.4265573282342,54.6822974139065,0.));
#93229=CARTESIAN_POINT('Ctrl Pts',(-48.4265573282342,54.6822974139065,12.));
#93230=CARTESIAN_POINT('Ctrl Pts',(-48.4497326694051,54.6937545689694,0.));
#93231=CARTESIAN_POINT('Ctrl Pts',(-48.4497326694051,54.6937545689694,12.));
#93232=CARTESIAN_POINT('Ctrl Pts',(-48.4729531503565,54.7052069558493,0.));
#93233=CARTESIAN_POINT('Ctrl Pts',(-48.4729531503565,54.7052069558493,12.));
#93234=CARTESIAN_POINT('Ctrl Pts',(-48.4962187050452,54.7166544839475,0.));
#93235=CARTESIAN_POINT('Ctrl Pts',(-48.4962187050452,54.7166544839475,12.));
#93236=CARTESIAN_POINT('Ctrl Pts',(-48.5195292675955,54.7280970630346,0.));
#93237=CARTESIAN_POINT('Ctrl Pts',(-48.5195292675955,54.7280970630346,12.));
#93238=CARTESIAN_POINT('Ctrl Pts',(-48.5428847722974,54.7395346032451,0.));
#93239=CARTESIAN_POINT('Ctrl Pts',(-48.5428847722974,54.7395346032451,12.));
#93240=CARTESIAN_POINT('Ctrl Pts',(-48.5662851536027,54.7509670150716,0.));
#93241=CARTESIAN_POINT('Ctrl Pts',(-48.5662851536027,54.7509670150716,12.));
#93242=CARTESIAN_POINT('Ctrl Pts',(-48.5897303461131,54.7623942093591,0.));
#93243=CARTESIAN_POINT('Ctrl Pts',(-48.5897303461131,54.7623942093591,12.));
#93244=CARTESIAN_POINT('Ctrl Pts',(-48.6132202845792,54.773816097304,0.));
#93245=CARTESIAN_POINT('Ctrl Pts',(-48.6132202845792,54.773816097304,12.));
#93246=CARTESIAN_POINT('Ctrl Pts',(-48.6367549039121,54.7852325904591,0.));
#93247=CARTESIAN_POINT('Ctrl Pts',(-48.6367549039121,54.7852325904591,12.));
#93248=CARTESIAN_POINT('Ctrl Pts',(-48.6603341391891,54.7966436007395,0.));
#93249=CARTESIAN_POINT('Ctrl Pts',(-48.6603341391891,54.7966436007395,12.));
#93250=CARTESIAN_POINT('Ctrl Pts',(-48.6839579256565,54.8080490404274,0.));
#93251=CARTESIAN_POINT('Ctrl Pts',(-48.6839579256565,54.8080490404274,12.));
#93252=CARTESIAN_POINT('Ctrl Pts',(-48.7076261987284,54.8194488221803,0.));
#93253=CARTESIAN_POINT('Ctrl Pts',(-48.7076261987284,54.8194488221803,12.));
#93254=CARTESIAN_POINT('Ctrl Pts',(-48.7313388939834,54.8308428590333,0.));
#93255=CARTESIAN_POINT('Ctrl Pts',(-48.7313388939834,54.8308428590333,12.));
#93256=CARTESIAN_POINT('Ctrl Pts',(-48.755095947159,54.8422310643752,0.));
#93257=CARTESIAN_POINT('Ctrl Pts',(-48.755095947159,54.8422310643752,12.));
#93258=CARTESIAN_POINT('Ctrl Pts',(-48.7788972941431,54.8536133519285,0.));
#93259=CARTESIAN_POINT('Ctrl Pts',(-48.7788972941431,54.8536133519285,12.));
#93260=CARTESIAN_POINT('Ctrl Pts',(-48.8027428709613,54.8649896357284,0.));
#93261=CARTESIAN_POINT('Ctrl Pts',(-48.8027428709613,54.8649896357284,12.));
#93262=CARTESIAN_POINT('Ctrl Pts',(-48.8266326137629,54.8763598301045,0.));
#93263=CARTESIAN_POINT('Ctrl Pts',(-48.8266326137629,54.8763598301045,12.));
#93264=CARTESIAN_POINT('Ctrl Pts',(-48.8505664587985,54.8877238496576,0.));
#93265=CARTESIAN_POINT('Ctrl Pts',(-48.8505664587985,54.8877238496576,12.));
#93266=CARTESIAN_POINT('Ctrl Pts',(-48.8745443424488,54.8990816092964,0.));
#93267=CARTESIAN_POINT('Ctrl Pts',(-48.8745443424488,54.8990816092964,12.));
#93268=CARTESIAN_POINT('Ctrl Pts',(-48.8985662012535,54.910433024275,0.));
#93269=CARTESIAN_POINT('Ctrl Pts',(-48.8985662012535,54.910433024275,12.));
#93270=CARTESIAN_POINT('Ctrl Pts',(-48.922631971937,54.9217780102357,0.));
#93271=CARTESIAN_POINT('Ctrl Pts',(-48.922631971937,54.9217780102357,12.));
#93272=CARTESIAN_POINT('Ctrl Pts',(-48.9467415914266,54.933116483242,0.));
#93273=CARTESIAN_POINT('Ctrl Pts',(-48.9467415914266,54.933116483242,12.));
#93274=CARTESIAN_POINT('Ctrl Pts',(-48.9708949968789,54.9444483598372,0.));
#93275=CARTESIAN_POINT('Ctrl Pts',(-48.9708949968789,54.9444483598372,12.));
#93276=CARTESIAN_POINT('Ctrl Pts',(-48.995092125652,54.9557735569936,0.));
#93277=CARTESIAN_POINT('Ctrl Pts',(-48.995092125652,54.9557735569936,12.));
#93278=CARTESIAN_POINT('Ctrl Pts',(-49.0193329152475,54.9670919920024,0.));
#93279=CARTESIAN_POINT('Ctrl Pts',(-49.0193329152475,54.9670919920024,12.));
#93280=CARTESIAN_POINT('Ctrl Pts',(-49.0436173032527,54.9784035823764,0.));
#93281=CARTESIAN_POINT('Ctrl Pts',(-49.0436173032527,54.9784035823764,12.));
#93282=CARTESIAN_POINT('Ctrl Pts',(-49.0679452272871,54.9897082457606,0.));
#93283=CARTESIAN_POINT('Ctrl Pts',(-49.0679452272871,54.9897082457606,12.));
#93284=CARTESIAN_POINT('Ctrl Pts',(-49.0923166249222,55.0010058998111,0.));
#93285=CARTESIAN_POINT('Ctrl Pts',(-49.0923166249222,55.0010058998111,12.));
#93286=CARTESIAN_POINT('Ctrl Pts',(-49.1167314336737,55.0122964621868,0.));
#93287=CARTESIAN_POINT('Ctrl Pts',(-49.1167314336737,55.0122964621868,12.));
#93288=CARTESIAN_POINT('Ctrl Pts',(-49.1411895911646,55.0235798508056,0.));
#93289=CARTESIAN_POINT('Ctrl Pts',(-49.1411895911646,55.0235798508056,12.));
#93290=CARTESIAN_POINT('Ctrl Pts',(-49.1656910352484,55.0348559840461,0.));
#93291=CARTESIAN_POINT('Ctrl Pts',(-49.1656910352484,55.0348559840461,12.));
#93292=CARTESIAN_POINT('Ctrl Pts',(-49.1902357041462,55.0461247809745,0.));
#93293=CARTESIAN_POINT('Ctrl Pts',(-49.1902357041462,55.0461247809745,12.));
#93294=CARTESIAN_POINT('Ctrl Pts',(-49.2148235365694,55.0573861615569,0.));
#93295=CARTESIAN_POINT('Ctrl Pts',(-49.2148235365694,55.0573861615569,12.));
#93296=CARTESIAN_POINT('Ctrl Pts',(-49.2394544718513,55.0686400468911,0.));
#93297=CARTESIAN_POINT('Ctrl Pts',(-49.2394544718513,55.0686400468911,12.));
#93298=CARTESIAN_POINT('Ctrl Pts',(-49.2641284496496,55.0798863586986,0.));
#93299=CARTESIAN_POINT('Ctrl Pts',(-49.2641284496496,55.0798863586986,12.));
#93300=CARTESIAN_POINT('Ctrl Pts',(-49.2888454096544,55.0911250188282,0.));
#93301=CARTESIAN_POINT('Ctrl Pts',(-49.2888454096544,55.0911250188282,12.));
#93302=CARTESIAN_POINT('Ctrl Pts',(-49.3136052912614,55.1023559487133,0.));
#93303=CARTESIAN_POINT('Ctrl Pts',(-49.3136052912614,55.1023559487133,12.));
#93304=CARTESIAN_POINT('Ctrl Pts',(-49.3384080333166,55.1135790689475,0.));
#93305=CARTESIAN_POINT('Ctrl Pts',(-49.3384080333166,55.1135790689475,12.));
#93306=CARTESIAN_POINT('Ctrl Pts',(-49.3632535736744,55.1247942985649,0.));
#93307=CARTESIAN_POINT('Ctrl Pts',(-49.3632535736744,55.1247942985649,12.));
#93308=CARTESIAN_POINT('Ctrl Pts',(-49.3881418495529,55.1360015556262,0.));
#93309=CARTESIAN_POINT('Ctrl Pts',(-49.3881418495529,55.1360015556262,12.));
#93310=CARTESIAN_POINT('Ctrl Pts',(-49.413072798324,55.1472007585223,0.));
#93311=CARTESIAN_POINT('Ctrl Pts',(-49.413072798324,55.1472007585223,12.));
#93312=CARTESIAN_POINT('Ctrl Pts',(-49.4380463581989,55.158391827114,0.));
#93313=CARTESIAN_POINT('Ctrl Pts',(-49.4380463581989,55.158391827114,12.));
#93314=CARTESIAN_POINT('Ctrl Pts',(-49.4630624688787,55.1695746838168,0.));
#93315=CARTESIAN_POINT('Ctrl Pts',(-49.4630624688787,55.1695746838168,12.));
#93316=CARTESIAN_POINT('Ctrl Pts',(-49.4881210723921,55.1807492550073,0.));
#93317=CARTESIAN_POINT('Ctrl Pts',(-49.4881210723921,55.1807492550073,12.));
#93318=CARTESIAN_POINT('Ctrl Pts',(-49.5132221132916,55.1919154713569,0.));
#93319=CARTESIAN_POINT('Ctrl Pts',(-49.5132221132916,55.1919154713569,12.));
#93320=CARTESIAN_POINT('Ctrl Pts',(-49.5383655367987,55.2030732647222,0.));
#93321=CARTESIAN_POINT('Ctrl Pts',(-49.5383655367987,55.2030732647222,12.));
#93322=CARTESIAN_POINT('Ctrl Pts',(-49.5635512873368,55.2142225656943,0.));
#93323=CARTESIAN_POINT('Ctrl Pts',(-49.5635512873368,55.2142225656943,12.));
#93324=CARTESIAN_POINT('Ctrl Pts',(-49.5887793068337,55.225363300765,0.));
#93325=CARTESIAN_POINT('Ctrl Pts',(-49.5887793068337,55.225363300765,12.));
#93326=CARTESIAN_POINT('Ctrl Pts',(-49.6140495332865,55.2364953899423,0.));
#93327=CARTESIAN_POINT('Ctrl Pts',(-49.6140495332865,55.2364953899423,12.));
#93328=CARTESIAN_POINT('Ctrl Pts',(-49.6393618987614,55.2476187434204,0.));
#93329=CARTESIAN_POINT('Ctrl Pts',(-49.6393618987614,55.2476187434204,12.));
#93330=CARTESIAN_POINT('Ctrl Pts',(-49.6647163322457,55.2587332663982,0.));
#93331=CARTESIAN_POINT('Ctrl Pts',(-49.6647163322457,55.2587332663982,12.));
#93332=CARTESIAN_POINT('Ctrl Pts',(-49.690112763181,55.2698388650215,0.));
#93333=CARTESIAN_POINT('Ctrl Pts',(-49.690112763181,55.2698388650215,12.));
#93334=CARTESIAN_POINT('Ctrl Pts',(-49.7155511248629,55.2809354521616,0.));
#93335=CARTESIAN_POINT('Ctrl Pts',(-49.7155511248629,55.2809354521616,12.));
#93336=CARTESIAN_POINT('Ctrl Pts',(-49.7410313576444,55.292022952748,0.));
#93337=CARTESIAN_POINT('Ctrl Pts',(-49.7410313576444,55.292022952748,12.));
#93338=CARTESIAN_POINT('Ctrl Pts',(-49.7665534128269,55.3031013105578,0.));
#93339=CARTESIAN_POINT('Ctrl Pts',(-49.7665534128269,55.3031013105578,12.));
#93340=CARTESIAN_POINT('Ctrl Pts',(-49.7921172540185,55.3141704897307,0.));
#93341=CARTESIAN_POINT('Ctrl Pts',(-49.7921172540185,55.3141704897307,12.));
#93342=CARTESIAN_POINT('Ctrl Pts',(-49.817722855186,55.3252304694066,0.));
#93343=CARTESIAN_POINT('Ctrl Pts',(-49.817722855186,55.3252304694066,12.));
#93344=CARTESIAN_POINT('Ctrl Pts',(-49.8382407306675,55.3340710859607,0.));
#93345=CARTESIAN_POINT('Ctrl Pts',(-49.8382407306675,55.3340710859607,12.));
#93346=CARTESIAN_POINT('Ctrl Pts',(-49.8536479176573,55.340697403233,0.));
#93347=CARTESIAN_POINT('Ctrl Pts',(-49.8536479176573,55.340697403233,12.));
#93348=CARTESIAN_POINT('Ctrl Pts',(-49.8639277221471,55.3451131058727,0.));
#93349=CARTESIAN_POINT('Ctrl Pts',(-49.8639277221471,55.3451131058727,12.));
#93350=CARTESIAN_POINT('Ctrl Pts',(-49.8690697110161,55.3473204966403,0.));
#93351=CARTESIAN_POINT('Ctrl Pts',(-49.8690697110161,55.3473204966403,12.));
#93352=CARTESIAN_POINT('',(-45.6458539113724,53.0702932034641,0.));
#93353=CARTESIAN_POINT('Ctrl Pts',(-45.6458539113724,53.0702932034641,0.));
#93354=CARTESIAN_POINT('Ctrl Pts',(-45.6490568514089,53.0724894921849,0.));
#93355=CARTESIAN_POINT('Ctrl Pts',(-45.6554684028145,53.0768833804193,0.));
#93356=CARTESIAN_POINT('Ctrl Pts',(-45.6651027439241,53.0834781451546,0.));
#93357=CARTESIAN_POINT('Ctrl Pts',(-45.6779825614231,53.0922790298409,0.));
#93358=CARTESIAN_POINT('Ctrl Pts',(-45.694139048907,53.1032932328857,0.));
#93359=CARTESIAN_POINT('Ctrl Pts',(-45.7103522376696,53.114320495492,0.));
#93360=CARTESIAN_POINT('Ctrl Pts',(-45.7266220897003,53.1253607414872,0.));
#93361=CARTESIAN_POINT('Ctrl Pts',(-45.7429485300823,53.1364138384693,0.));
#93362=CARTESIAN_POINT('Ctrl Pts',(-45.7593314474501,53.1474795996053,0.));
#93363=CARTESIAN_POINT('Ctrl Pts',(-45.7757707100618,53.1585578076444,0.));
#93364=CARTESIAN_POINT('Ctrl Pts',(-45.7922661780005,53.1696482334487,0.));
#93365=CARTESIAN_POINT('Ctrl Pts',(-45.808817716509,53.1807506560933,0.));
#93366=CARTESIAN_POINT('Ctrl Pts',(-45.8254252099957,53.1918648840541,0.));
#93367=CARTESIAN_POINT('Ctrl Pts',(-45.8420885575349,53.2029907483557,0.));
#93368=CARTESIAN_POINT('Ctrl Pts',(-45.8588076662582,53.2141280925439,0.));
#93369=CARTESIAN_POINT('Ctrl Pts',(-45.8755824458723,53.2252767643662,0.));
#93370=CARTESIAN_POINT('Ctrl Pts',(-45.892412801838,53.2364366054306,0.));
#93371=CARTESIAN_POINT('Ctrl Pts',(-45.9092986319377,53.2476074460017,0.));
#93372=CARTESIAN_POINT('Ctrl Pts',(-45.9262398298349,53.2587891103866,0.));
#93373=CARTESIAN_POINT('Ctrl Pts',(-45.9432362873008,53.2699814203105,0.));
#93374=CARTESIAN_POINT('Ctrl Pts',(-45.9602878967698,53.2811841987926,0.));
#93375=CARTESIAN_POINT('Ctrl Pts',(-45.9773945542384,53.292397274555,0.));
#93376=CARTESIAN_POINT('Ctrl Pts',(-45.9945561591453,53.3036204818329,0.));
#93377=CARTESIAN_POINT('Ctrl Pts',(-46.0117726129873,53.3148536582635,0.));
#93378=CARTESIAN_POINT('Ctrl Pts',(-46.02904381836,53.326096643428,0.));
#93379=CARTESIAN_POINT('Ctrl Pts',(-46.0463696777801,53.3373492770671,0.));
#93380=CARTESIAN_POINT('Ctrl Pts',(-46.0637500926982,53.3486113975901,0.));
#93381=CARTESIAN_POINT('Ctrl Pts',(-46.0811849640218,53.3598828428546,0.));
#93382=CARTESIAN_POINT('Ctrl Pts',(-46.0986741925656,53.3711634508437,0.));
#93383=CARTESIAN_POINT('Ctrl Pts',(-46.1162176794884,53.3824530603276,0.));
#93384=CARTESIAN_POINT('Ctrl Pts',(-46.1338153268097,53.3937515116549,0.));
#93385=CARTESIAN_POINT('Ctrl Pts',(-46.1514670376012,53.4050586470436,0.));
#93386=CARTESIAN_POINT('Ctrl Pts',(-46.1691727157134,53.4163743101517,0.));
#93387=CARTESIAN_POINT('Ctrl Pts',(-46.1869322656024,53.4276983458125,0.));
#93388=CARTESIAN_POINT('Ctrl Pts',(-46.2047455921286,53.4390305997274,0.));
#93389=CARTESIAN_POINT('Ctrl Pts',(-46.2226126003202,53.4503709181178,0.));
#93390=CARTESIAN_POINT('Ctrl Pts',(-46.2405331953889,53.4617191477402,0.));
#93391=CARTESIAN_POINT('Ctrl Pts',(-46.2585072828353,53.4730751360371,0.));
#93392=CARTESIAN_POINT('Ctrl Pts',(-46.2765347685198,53.4844387312414,0.));
#93393=CARTESIAN_POINT('Ctrl Pts',(-46.2946155587417,53.4958097825006,0.));
#93394=CARTESIAN_POINT('Ctrl Pts',(-46.3127495603098,53.5071881399911,0.));
#93395=CARTESIAN_POINT('Ctrl Pts',(-46.3309366805093,53.5185736548548,0.));
#93396=CARTESIAN_POINT('Ctrl Pts',(-46.3491768270655,53.5299661791385,0.));
#93397=CARTESIAN_POINT('Ctrl Pts',(-46.3674699081046,53.5413655657327,0.));
#93398=CARTESIAN_POINT('Ctrl Pts',(-46.3858158321059,53.5527716683047,0.));
#93399=CARTESIAN_POINT('Ctrl Pts',(-46.4042145078701,53.5641843412559,0.));
#93400=CARTESIAN_POINT('Ctrl Pts',(-46.4226658445474,53.5756034397481,0.));
#93401=CARTESIAN_POINT('Ctrl Pts',(-46.4411697516478,53.5870288197166,0.));
#93402=CARTESIAN_POINT('Ctrl Pts',(-46.459726139052,53.5984603378855,0.));
#93403=CARTESIAN_POINT('Ctrl Pts',(-46.4783349170173,53.6098978517859,0.));
#93404=CARTESIAN_POINT('Ctrl Pts',(-46.496995996177,53.6213412197533,0.));
#93405=CARTESIAN_POINT('Ctrl Pts',(-46.5157092875373,53.6327903009094,0.));
#93406=CARTESIAN_POINT('Ctrl Pts',(-46.5344747024676,53.6442449551455,0.));
#93407=CARTESIAN_POINT('Ctrl Pts',(-46.5532921526901,53.6557050431071,0.));
#93408=CARTESIAN_POINT('Ctrl Pts',(-46.5721615502591,53.6671704261737,0.));
#93409=CARTESIAN_POINT('Ctrl Pts',(-46.5910828075653,53.678640966456,0.));
#93410=CARTESIAN_POINT('Ctrl Pts',(-46.6100558373402,53.6901165267941,0.));
#93411=CARTESIAN_POINT('Ctrl Pts',(-46.6290805526559,53.701596970754,0.));
#93412=CARTESIAN_POINT('Ctrl Pts',(-46.6481568669216,53.7130821626263,0.));
#93413=CARTESIAN_POINT('Ctrl Pts',(-46.6672846938752,53.7245719674222,0.));
#93414=CARTESIAN_POINT('Ctrl Pts',(-46.6864639475863,53.7360662508677,0.));
#93415=CARTESIAN_POINT('Ctrl Pts',(-46.7056945424559,53.7475648793948,0.));
#93416=CARTESIAN_POINT('Ctrl Pts',(-46.724976393213,53.7590677201344,0.));
#93417=CARTESIAN_POINT('Ctrl Pts',(-46.7443094149041,53.770574640907,0.));
#93418=CARTESIAN_POINT('Ctrl Pts',(-46.7636935228851,53.7820855102169,0.));
#93419=CARTESIAN_POINT('Ctrl Pts',(-46.7831286328268,53.7936001972468,0.));
#93420=CARTESIAN_POINT('Ctrl Pts',(-46.8026146607144,53.8051185718524,0.));
#93421=CARTESIAN_POINT('Ctrl Pts',(-46.8221515228459,53.8166405045582,0.));
#93422=CARTESIAN_POINT('Ctrl Pts',(-46.8417391358231,53.8281658665517,0.));
#93423=CARTESIAN_POINT('Ctrl Pts',(-46.8613774165452,53.8396945296777,0.));
#93424=CARTESIAN_POINT('Ctrl Pts',(-46.8810662822147,53.851226366434,0.));
#93425=CARTESIAN_POINT('Ctrl Pts',(-46.900805650336,53.8627612499648,0.));
#93426=CARTESIAN_POINT('Ctrl Pts',(-46.9205954387128,53.8742990540557,0.));
#93427=CARTESIAN_POINT('Ctrl Pts',(-46.9404355654381,53.8858396531277,0.));
#93428=CARTESIAN_POINT('Ctrl Pts',(-46.9603259488894,53.8973829222317,0.));
#93429=CARTESIAN_POINT('Ctrl Pts',(-46.9802665077342,53.9089287370435,0.));
#93430=CARTESIAN_POINT('Ctrl Pts',(-47.0002571609286,53.9204769738583,0.));
#93431=CARTESIAN_POINT('Ctrl Pts',(-47.0202978277148,53.9320275095864,0.));
#93432=CARTESIAN_POINT('Ctrl Pts',(-47.04038842761,53.9435802217468,0.));
#93433=CARTESIAN_POINT('Ctrl Pts',(-47.0605288804042,53.9551349884637,0.));
#93434=CARTESIAN_POINT('Ctrl Pts',(-47.0807191061674,53.9666916884624,0.));
#93435=CARTESIAN_POINT('Ctrl Pts',(-47.1009590252466,53.9782502010642,0.));
#93436=CARTESIAN_POINT('Ctrl Pts',(-47.1212485582632,53.9898104061809,0.));
#93437=CARTESIAN_POINT('Ctrl Pts',(-47.1415876261012,54.0013721843094,0.));
#93438=CARTESIAN_POINT('Ctrl Pts',(-47.161976149906,54.0129354165269,0.));
#93439=CARTESIAN_POINT('Ctrl Pts',(-47.1824140510906,54.0244999844872,0.));
#93440=CARTESIAN_POINT('Ctrl Pts',(-47.2029012513334,54.0360657704156,0.));
#93441=CARTESIAN_POINT('Ctrl Pts',(-47.2234376725752,54.047632657105,0.));
#93442=CARTESIAN_POINT('Ctrl Pts',(-47.2440232370085,54.0592005279108,0.));
#93443=CARTESIAN_POINT('Ctrl Pts',(-47.2646578670767,54.0707692667461,0.));
#93444=CARTESIAN_POINT('Ctrl Pts',(-47.2853414854805,54.082338758079,0.));
#93445=CARTESIAN_POINT('Ctrl Pts',(-47.3060740151754,54.093908886927,0.));
#93446=CARTESIAN_POINT('Ctrl Pts',(-47.326855379369,54.1054795388538,0.));
#93447=CARTESIAN_POINT('Ctrl Pts',(-47.3476855015095,54.1170505999637,0.));
#93448=CARTESIAN_POINT('Ctrl Pts',(-47.3685643052867,54.128621956898,0.));
#93449=CARTESIAN_POINT('Ctrl Pts',(-47.3894917146361,54.1401934968306,0.));
#93450=CARTESIAN_POINT('Ctrl Pts',(-47.4104676537381,54.1517651074638,0.));
#93451=CARTESIAN_POINT('Ctrl Pts',(-47.4314920470142,54.163336677024,0.));
#93452=CARTESIAN_POINT('Ctrl Pts',(-47.4525648191173,54.1749080942593,0.));
#93453=CARTESIAN_POINT('Ctrl Pts',(-47.473685894932,54.1864792484343,0.));
#93454=CARTESIAN_POINT('Ctrl Pts',(-47.4948551995799,54.1980500293267,0.));
#93455=CARTESIAN_POINT('Ctrl Pts',(-47.5160726584172,54.2096203272228,0.));
#93456=CARTESIAN_POINT('Ctrl Pts',(-47.5373381970328,54.221190032914,0.));
#93457=CARTESIAN_POINT('Ctrl Pts',(-47.5586517412368,54.232759037693,0.));
#93458=CARTESIAN_POINT('Ctrl Pts',(-47.5800132170614,54.2443272333498,0.));
#93459=CARTESIAN_POINT('Ctrl Pts',(-47.6014225507664,54.2558945121684,0.));
#93460=CARTESIAN_POINT('Ctrl Pts',(-47.6228796688376,54.2674607669227,0.));
#93461=CARTESIAN_POINT('Ctrl Pts',(-47.6443844979846,54.2790258908736,0.));
#93462=CARTESIAN_POINT('Ctrl Pts',(-47.6659369651299,54.2905897777647,0.));
#93463=CARTESIAN_POINT('Ctrl Pts',(-47.6875369974086,54.3021523218188,0.));
#93464=CARTESIAN_POINT('Ctrl Pts',(-47.7091845221747,54.3137134177345,0.));
#93465=CARTESIAN_POINT('Ctrl Pts',(-47.7308794669994,54.3252729606824,0.));
#93466=CARTESIAN_POINT('Ctrl Pts',(-47.7526217596694,54.3368308463023,0.));
#93467=CARTESIAN_POINT('Ctrl Pts',(-47.7744113281768,54.3483869706998,0.));
#93468=CARTESIAN_POINT('Ctrl Pts',(-47.7962481007179,54.3599412304431,0.));
#93469=CARTESIAN_POINT('Ctrl Pts',(-47.8181320056988,54.3714935225585,0.));
#93470=CARTESIAN_POINT('Ctrl Pts',(-47.8400629717352,54.3830437445275,0.));
#93471=CARTESIAN_POINT('Ctrl Pts',(-47.8620409276495,54.3945917942835,0.));
#93472=CARTESIAN_POINT('Ctrl Pts',(-47.8840658024626,54.4061375702088,0.));
#93473=CARTESIAN_POINT('Ctrl Pts',(-47.9061375253909,54.4176809711324,0.));
#93474=CARTESIAN_POINT('Ctrl Pts',(-47.9282560258528,54.4292218963253,0.));
#93475=CARTESIAN_POINT('Ctrl Pts',(-47.9504212334681,54.4407602454974,0.));
#93476=CARTESIAN_POINT('Ctrl Pts',(-47.972633078057,54.4522959187952,0.));
#93477=CARTESIAN_POINT('Ctrl Pts',(-47.9948914896316,54.4638288167991,0.));
#93478=CARTESIAN_POINT('Ctrl Pts',(-48.0171963983912,54.4753588405202,0.));
#93479=CARTESIAN_POINT('Ctrl Pts',(-48.039547734729,54.4868858913961,0.));
#93480=CARTESIAN_POINT('Ctrl Pts',(-48.0619454292321,54.4984098712883,0.));
#93481=CARTESIAN_POINT('Ctrl Pts',(-48.0843894126807,54.5099306824788,0.));
#93482=CARTESIAN_POINT('Ctrl Pts',(-48.1068796160406,54.5214482276679,0.));
#93483=CARTESIAN_POINT('Ctrl Pts',(-48.1294159704571,54.5329624099719,0.));
#93484=CARTESIAN_POINT('Ctrl Pts',(-48.1519984072617,54.5444731329196,0.));
#93485=CARTESIAN_POINT('Ctrl Pts',(-48.1746268579732,54.5559803004487,0.));
#93486=CARTESIAN_POINT('Ctrl Pts',(-48.1973012542966,54.5674838169041,0.));
#93487=CARTESIAN_POINT('Ctrl Pts',(-48.2200215281178,54.5789835870348,0.));
#93488=CARTESIAN_POINT('Ctrl Pts',(-48.2427876114955,54.5904795159936,0.));
#93489=CARTESIAN_POINT('Ctrl Pts',(-48.2655994366672,54.6019715093319,0.));
#93490=CARTESIAN_POINT('Ctrl Pts',(-48.288456936051,54.6134594729964,0.));
#93491=CARTESIAN_POINT('Ctrl Pts',(-48.3113600422443,54.6249433133262,0.));
#93492=CARTESIAN_POINT('Ctrl Pts',(-48.3343086880192,54.636422937049,0.));
#93493=CARTESIAN_POINT('Ctrl Pts',(-48.3573028063122,54.647898251279,0.));
#93494=CARTESIAN_POINT('Ctrl Pts',(-48.3803423302294,54.6593691635143,0.));
#93495=CARTESIAN_POINT('Ctrl Pts',(-48.4034271930516,54.6708355816359,0.));
#93496=CARTESIAN_POINT('Ctrl Pts',(-48.4265573282342,54.6822974139065,0.));
#93497=CARTESIAN_POINT('Ctrl Pts',(-48.4497326694051,54.6937545689694,0.));
#93498=CARTESIAN_POINT('Ctrl Pts',(-48.4729531503565,54.7052069558493,0.));
#93499=CARTESIAN_POINT('Ctrl Pts',(-48.4962187050452,54.7166544839475,0.));
#93500=CARTESIAN_POINT('Ctrl Pts',(-48.5195292675955,54.7280970630346,0.));
#93501=CARTESIAN_POINT('Ctrl Pts',(-48.5428847722974,54.7395346032451,0.));
#93502=CARTESIAN_POINT('Ctrl Pts',(-48.5662851536027,54.7509670150716,0.));
#93503=CARTESIAN_POINT('Ctrl Pts',(-48.5897303461131,54.7623942093591,0.));
#93504=CARTESIAN_POINT('Ctrl Pts',(-48.6132202845792,54.773816097304,0.));
#93505=CARTESIAN_POINT('Ctrl Pts',(-48.6367549039121,54.7852325904591,0.));
#93506=CARTESIAN_POINT('Ctrl Pts',(-48.6603341391891,54.7966436007395,0.));
#93507=CARTESIAN_POINT('Ctrl Pts',(-48.6839579256565,54.8080490404274,0.));
#93508=CARTESIAN_POINT('Ctrl Pts',(-48.7076261987284,54.8194488221803,0.));
#93509=CARTESIAN_POINT('Ctrl Pts',(-48.7313388939834,54.8308428590333,0.));
#93510=CARTESIAN_POINT('Ctrl Pts',(-48.755095947159,54.8422310643752,0.));
#93511=CARTESIAN_POINT('Ctrl Pts',(-48.7788972941431,54.8536133519285,0.));
#93512=CARTESIAN_POINT('Ctrl Pts',(-48.8027428709613,54.8649896357284,0.));
#93513=CARTESIAN_POINT('Ctrl Pts',(-48.8266326137629,54.8763598301045,0.));
#93514=CARTESIAN_POINT('Ctrl Pts',(-48.8505664587985,54.8877238496576,0.));
#93515=CARTESIAN_POINT('Ctrl Pts',(-48.8745443424488,54.8990816092964,0.));
#93516=CARTESIAN_POINT('Ctrl Pts',(-48.8985662012535,54.910433024275,0.));
#93517=CARTESIAN_POINT('Ctrl Pts',(-48.922631971937,54.9217780102357,0.));
#93518=CARTESIAN_POINT('Ctrl Pts',(-48.9467415914266,54.933116483242,0.));
#93519=CARTESIAN_POINT('Ctrl Pts',(-48.9708949968789,54.9444483598372,0.));
#93520=CARTESIAN_POINT('Ctrl Pts',(-48.995092125652,54.9557735569936,0.));
#93521=CARTESIAN_POINT('Ctrl Pts',(-49.0193329152475,54.9670919920024,0.));
#93522=CARTESIAN_POINT('Ctrl Pts',(-49.0436173032527,54.9784035823764,0.));
#93523=CARTESIAN_POINT('Ctrl Pts',(-49.0679452272871,54.9897082457606,0.));
#93524=CARTESIAN_POINT('Ctrl Pts',(-49.0923166249222,55.0010058998111,0.));
#93525=CARTESIAN_POINT('Ctrl Pts',(-49.1167314336737,55.0122964621868,0.));
#93526=CARTESIAN_POINT('Ctrl Pts',(-49.1411895911646,55.0235798508056,0.));
#93527=CARTESIAN_POINT('Ctrl Pts',(-49.1656910352484,55.0348559840461,0.));
#93528=CARTESIAN_POINT('Ctrl Pts',(-49.1902357041462,55.0461247809745,0.));
#93529=CARTESIAN_POINT('Ctrl Pts',(-49.2148235365694,55.0573861615569,0.));
#93530=CARTESIAN_POINT('Ctrl Pts',(-49.2394544718513,55.0686400468911,0.));
#93531=CARTESIAN_POINT('Ctrl Pts',(-49.2641284496496,55.0798863586986,0.));
#93532=CARTESIAN_POINT('Ctrl Pts',(-49.2888454096544,55.0911250188282,0.));
#93533=CARTESIAN_POINT('Ctrl Pts',(-49.3136052912614,55.1023559487133,0.));
#93534=CARTESIAN_POINT('Ctrl Pts',(-49.3384080333166,55.1135790689475,0.));
#93535=CARTESIAN_POINT('Ctrl Pts',(-49.3632535736744,55.1247942985649,0.));
#93536=CARTESIAN_POINT('Ctrl Pts',(-49.3881418495529,55.1360015556262,0.));
#93537=CARTESIAN_POINT('Ctrl Pts',(-49.413072798324,55.1472007585223,0.));
#93538=CARTESIAN_POINT('Ctrl Pts',(-49.4380463581989,55.158391827114,0.));
#93539=CARTESIAN_POINT('Ctrl Pts',(-49.4630624688787,55.1695746838168,0.));
#93540=CARTESIAN_POINT('Ctrl Pts',(-49.4881210723921,55.1807492550073,0.));
#93541=CARTESIAN_POINT('Ctrl Pts',(-49.5132221132916,55.1919154713569,0.));
#93542=CARTESIAN_POINT('Ctrl Pts',(-49.5347748994609,55.2014798623976,0.));
#93543=CARTESIAN_POINT('Ctrl Pts',(-49.5513218524283,55.2088081098956,0.));
#93544=CARTESIAN_POINT('Ctrl Pts',(-49.5628442141876,55.2139039604571,0.));
#93545=CARTESIAN_POINT('Ctrl Pts',(-49.5693295981616,55.2167699151171,0.));
#93546=CARTESIAN_POINT('Ctrl Pts',(-49.5707719660265,55.2174072001301,0.));
#93547=CARTESIAN_POINT('',(-45.6458539113724,53.0702932034641,12.));
#93548=CARTESIAN_POINT('',(-45.6458539113724,53.0702932034641,0.));
#93549=CARTESIAN_POINT('Ctrl Pts',(-49.5707719660265,55.2174072001301,12.));
#93550=CARTESIAN_POINT('Ctrl Pts',(-49.5693295981616,55.2167699151171,12.));
#93551=CARTESIAN_POINT('Ctrl Pts',(-49.5628442141876,55.2139039604571,12.));
#93552=CARTESIAN_POINT('Ctrl Pts',(-49.5513218524283,55.2088081098956,12.));
#93553=CARTESIAN_POINT('Ctrl Pts',(-49.5347748994609,55.2014798623976,12.));
#93554=CARTESIAN_POINT('Ctrl Pts',(-49.5132221132916,55.1919154713569,12.));
#93555=CARTESIAN_POINT('Ctrl Pts',(-49.4881210723921,55.1807492550073,12.));
#93556=CARTESIAN_POINT('Ctrl Pts',(-49.4630624688787,55.1695746838168,12.));
#93557=CARTESIAN_POINT('Ctrl Pts',(-49.4380463581989,55.158391827114,12.));
#93558=CARTESIAN_POINT('Ctrl Pts',(-49.413072798324,55.1472007585223,12.));
#93559=CARTESIAN_POINT('Ctrl Pts',(-49.3881418495529,55.1360015556262,12.));
#93560=CARTESIAN_POINT('Ctrl Pts',(-49.3632535736744,55.1247942985649,12.));
#93561=CARTESIAN_POINT('Ctrl Pts',(-49.3384080333166,55.1135790689475,12.));
#93562=CARTESIAN_POINT('Ctrl Pts',(-49.3136052912614,55.1023559487133,12.));
#93563=CARTESIAN_POINT('Ctrl Pts',(-49.2888454096544,55.0911250188282,12.));
#93564=CARTESIAN_POINT('Ctrl Pts',(-49.2641284496496,55.0798863586986,12.));
#93565=CARTESIAN_POINT('Ctrl Pts',(-49.2394544718513,55.0686400468911,12.));
#93566=CARTESIAN_POINT('Ctrl Pts',(-49.2148235365694,55.0573861615569,12.));
#93567=CARTESIAN_POINT('Ctrl Pts',(-49.1902357041462,55.0461247809745,12.));
#93568=CARTESIAN_POINT('Ctrl Pts',(-49.1656910352484,55.0348559840461,12.));
#93569=CARTESIAN_POINT('Ctrl Pts',(-49.1411895911646,55.0235798508056,12.));
#93570=CARTESIAN_POINT('Ctrl Pts',(-49.1167314336737,55.0122964621868,12.));
#93571=CARTESIAN_POINT('Ctrl Pts',(-49.0923166249222,55.0010058998111,12.));
#93572=CARTESIAN_POINT('Ctrl Pts',(-49.0679452272871,54.9897082457606,12.));
#93573=CARTESIAN_POINT('Ctrl Pts',(-49.0436173032527,54.9784035823764,12.));
#93574=CARTESIAN_POINT('Ctrl Pts',(-49.0193329152475,54.9670919920024,12.));
#93575=CARTESIAN_POINT('Ctrl Pts',(-48.995092125652,54.9557735569936,12.));
#93576=CARTESIAN_POINT('Ctrl Pts',(-48.9708949968789,54.9444483598372,12.));
#93577=CARTESIAN_POINT('Ctrl Pts',(-48.9467415914266,54.933116483242,12.));
#93578=CARTESIAN_POINT('Ctrl Pts',(-48.922631971937,54.9217780102357,12.));
#93579=CARTESIAN_POINT('Ctrl Pts',(-48.8985662012535,54.910433024275,12.));
#93580=CARTESIAN_POINT('Ctrl Pts',(-48.8745443424488,54.8990816092964,12.));
#93581=CARTESIAN_POINT('Ctrl Pts',(-48.8505664587985,54.8877238496576,12.));
#93582=CARTESIAN_POINT('Ctrl Pts',(-48.8266326137629,54.8763598301045,12.));
#93583=CARTESIAN_POINT('Ctrl Pts',(-48.8027428709613,54.8649896357284,12.));
#93584=CARTESIAN_POINT('Ctrl Pts',(-48.7788972941431,54.8536133519285,12.));
#93585=CARTESIAN_POINT('Ctrl Pts',(-48.755095947159,54.8422310643752,12.));
#93586=CARTESIAN_POINT('Ctrl Pts',(-48.7313388939834,54.8308428590333,12.));
#93587=CARTESIAN_POINT('Ctrl Pts',(-48.7076261987284,54.8194488221803,12.));
#93588=CARTESIAN_POINT('Ctrl Pts',(-48.6839579256565,54.8080490404274,12.));
#93589=CARTESIAN_POINT('Ctrl Pts',(-48.6603341391891,54.7966436007395,12.));
#93590=CARTESIAN_POINT('Ctrl Pts',(-48.6367549039121,54.7852325904591,12.));
#93591=CARTESIAN_POINT('Ctrl Pts',(-48.6132202845792,54.773816097304,12.));
#93592=CARTESIAN_POINT('Ctrl Pts',(-48.5897303461131,54.7623942093591,12.));
#93593=CARTESIAN_POINT('Ctrl Pts',(-48.5662851536027,54.7509670150716,12.));
#93594=CARTESIAN_POINT('Ctrl Pts',(-48.5428847722974,54.7395346032451,12.));
#93595=CARTESIAN_POINT('Ctrl Pts',(-48.5195292675955,54.7280970630346,12.));
#93596=CARTESIAN_POINT('Ctrl Pts',(-48.4962187050452,54.7166544839475,12.));
#93597=CARTESIAN_POINT('Ctrl Pts',(-48.4729531503565,54.7052069558493,12.));
#93598=CARTESIAN_POINT('Ctrl Pts',(-48.4497326694051,54.6937545689694,12.));
#93599=CARTESIAN_POINT('Ctrl Pts',(-48.4265573282342,54.6822974139065,12.));
#93600=CARTESIAN_POINT('Ctrl Pts',(-48.4034271930516,54.6708355816359,12.));
#93601=CARTESIAN_POINT('Ctrl Pts',(-48.3803423302294,54.6593691635143,12.));
#93602=CARTESIAN_POINT('Ctrl Pts',(-48.3573028063122,54.647898251279,12.));
#93603=CARTESIAN_POINT('Ctrl Pts',(-48.3343086880192,54.636422937049,12.));
#93604=CARTESIAN_POINT('Ctrl Pts',(-48.3113600422443,54.6249433133262,12.));
#93605=CARTESIAN_POINT('Ctrl Pts',(-48.288456936051,54.6134594729964,12.));
#93606=CARTESIAN_POINT('Ctrl Pts',(-48.2655994366672,54.6019715093319,12.));
#93607=CARTESIAN_POINT('Ctrl Pts',(-48.2427876114955,54.5904795159936,12.));
#93608=CARTESIAN_POINT('Ctrl Pts',(-48.2200215281178,54.5789835870348,12.));
#93609=CARTESIAN_POINT('Ctrl Pts',(-48.1973012542966,54.5674838169041,12.));
#93610=CARTESIAN_POINT('Ctrl Pts',(-48.1746268579732,54.5559803004487,12.));
#93611=CARTESIAN_POINT('Ctrl Pts',(-48.1519984072617,54.5444731329196,12.));
#93612=CARTESIAN_POINT('Ctrl Pts',(-48.1294159704571,54.5329624099719,12.));
#93613=CARTESIAN_POINT('Ctrl Pts',(-48.1068796160406,54.5214482276679,12.));
#93614=CARTESIAN_POINT('Ctrl Pts',(-48.0843894126807,54.5099306824788,12.));
#93615=CARTESIAN_POINT('Ctrl Pts',(-48.0619454292321,54.4984098712883,12.));
#93616=CARTESIAN_POINT('Ctrl Pts',(-48.039547734729,54.4868858913961,12.));
#93617=CARTESIAN_POINT('Ctrl Pts',(-48.0171963983912,54.4753588405202,12.));
#93618=CARTESIAN_POINT('Ctrl Pts',(-47.9948914896316,54.4638288167991,12.));
#93619=CARTESIAN_POINT('Ctrl Pts',(-47.972633078057,54.4522959187952,12.));
#93620=CARTESIAN_POINT('Ctrl Pts',(-47.9504212334681,54.4407602454974,12.));
#93621=CARTESIAN_POINT('Ctrl Pts',(-47.9282560258528,54.4292218963253,12.));
#93622=CARTESIAN_POINT('Ctrl Pts',(-47.9061375253909,54.4176809711324,12.));
#93623=CARTESIAN_POINT('Ctrl Pts',(-47.8840658024626,54.4061375702088,12.));
#93624=CARTESIAN_POINT('Ctrl Pts',(-47.8620409276495,54.3945917942835,12.));
#93625=CARTESIAN_POINT('Ctrl Pts',(-47.8400629717352,54.3830437445275,12.));
#93626=CARTESIAN_POINT('Ctrl Pts',(-47.8181320056988,54.3714935225585,12.));
#93627=CARTESIAN_POINT('Ctrl Pts',(-47.7962481007179,54.3599412304431,12.));
#93628=CARTESIAN_POINT('Ctrl Pts',(-47.7744113281768,54.3483869706998,12.));
#93629=CARTESIAN_POINT('Ctrl Pts',(-47.7526217596694,54.3368308463023,12.));
#93630=CARTESIAN_POINT('Ctrl Pts',(-47.7308794669994,54.3252729606824,12.));
#93631=CARTESIAN_POINT('Ctrl Pts',(-47.7091845221747,54.3137134177345,12.));
#93632=CARTESIAN_POINT('Ctrl Pts',(-47.6875369974086,54.3021523218188,12.));
#93633=CARTESIAN_POINT('Ctrl Pts',(-47.6659369651299,54.2905897777647,12.));
#93634=CARTESIAN_POINT('Ctrl Pts',(-47.6443844979846,54.2790258908736,12.));
#93635=CARTESIAN_POINT('Ctrl Pts',(-47.6228796688376,54.2674607669227,12.));
#93636=CARTESIAN_POINT('Ctrl Pts',(-47.6014225507664,54.2558945121684,12.));
#93637=CARTESIAN_POINT('Ctrl Pts',(-47.5800132170614,54.2443272333498,12.));
#93638=CARTESIAN_POINT('Ctrl Pts',(-47.5586517412368,54.232759037693,12.));
#93639=CARTESIAN_POINT('Ctrl Pts',(-47.5373381970328,54.221190032914,12.));
#93640=CARTESIAN_POINT('Ctrl Pts',(-47.5160726584172,54.2096203272228,12.));
#93641=CARTESIAN_POINT('Ctrl Pts',(-47.4948551995799,54.1980500293267,12.));
#93642=CARTESIAN_POINT('Ctrl Pts',(-47.473685894932,54.1864792484343,12.));
#93643=CARTESIAN_POINT('Ctrl Pts',(-47.4525648191173,54.1749080942593,12.));
#93644=CARTESIAN_POINT('Ctrl Pts',(-47.4314920470142,54.163336677024,12.));
#93645=CARTESIAN_POINT('Ctrl Pts',(-47.4104676537381,54.1517651074638,12.));
#93646=CARTESIAN_POINT('Ctrl Pts',(-47.3894917146361,54.1401934968306,12.));
#93647=CARTESIAN_POINT('Ctrl Pts',(-47.3685643052867,54.128621956898,12.));
#93648=CARTESIAN_POINT('Ctrl Pts',(-47.3476855015095,54.1170505999637,12.));
#93649=CARTESIAN_POINT('Ctrl Pts',(-47.326855379369,54.1054795388538,12.));
#93650=CARTESIAN_POINT('Ctrl Pts',(-47.3060740151754,54.093908886927,12.));
#93651=CARTESIAN_POINT('Ctrl Pts',(-47.2853414854805,54.082338758079,12.));
#93652=CARTESIAN_POINT('Ctrl Pts',(-47.2646578670767,54.0707692667461,12.));
#93653=CARTESIAN_POINT('Ctrl Pts',(-47.2440232370085,54.0592005279108,12.));
#93654=CARTESIAN_POINT('Ctrl Pts',(-47.2234376725752,54.047632657105,12.));
#93655=CARTESIAN_POINT('Ctrl Pts',(-47.2029012513334,54.0360657704156,12.));
#93656=CARTESIAN_POINT('Ctrl Pts',(-47.1824140510906,54.0244999844872,12.));
#93657=CARTESIAN_POINT('Ctrl Pts',(-47.161976149906,54.0129354165269,12.));
#93658=CARTESIAN_POINT('Ctrl Pts',(-47.1415876261012,54.0013721843094,12.));
#93659=CARTESIAN_POINT('Ctrl Pts',(-47.1212485582632,53.9898104061809,12.));
#93660=CARTESIAN_POINT('Ctrl Pts',(-47.1009590252466,53.9782502010642,12.));
#93661=CARTESIAN_POINT('Ctrl Pts',(-47.0807191061674,53.9666916884624,12.));
#93662=CARTESIAN_POINT('Ctrl Pts',(-47.0605288804042,53.9551349884637,12.));
#93663=CARTESIAN_POINT('Ctrl Pts',(-47.04038842761,53.9435802217468,12.));
#93664=CARTESIAN_POINT('Ctrl Pts',(-47.0202978277148,53.9320275095864,12.));
#93665=CARTESIAN_POINT('Ctrl Pts',(-47.0002571609286,53.9204769738583,12.));
#93666=CARTESIAN_POINT('Ctrl Pts',(-46.9802665077342,53.9089287370435,12.));
#93667=CARTESIAN_POINT('Ctrl Pts',(-46.9603259488894,53.8973829222317,12.));
#93668=CARTESIAN_POINT('Ctrl Pts',(-46.9404355654381,53.8858396531277,12.));
#93669=CARTESIAN_POINT('Ctrl Pts',(-46.9205954387128,53.8742990540557,12.));
#93670=CARTESIAN_POINT('Ctrl Pts',(-46.900805650336,53.8627612499648,12.));
#93671=CARTESIAN_POINT('Ctrl Pts',(-46.8810662822147,53.851226366434,12.));
#93672=CARTESIAN_POINT('Ctrl Pts',(-46.8613774165452,53.8396945296777,12.));
#93673=CARTESIAN_POINT('Ctrl Pts',(-46.8417391358231,53.8281658665517,12.));
#93674=CARTESIAN_POINT('Ctrl Pts',(-46.8221515228459,53.8166405045582,12.));
#93675=CARTESIAN_POINT('Ctrl Pts',(-46.8026146607144,53.8051185718524,12.));
#93676=CARTESIAN_POINT('Ctrl Pts',(-46.7831286328268,53.7936001972468,12.));
#93677=CARTESIAN_POINT('Ctrl Pts',(-46.7636935228851,53.7820855102169,12.));
#93678=CARTESIAN_POINT('Ctrl Pts',(-46.7443094149041,53.770574640907,12.));
#93679=CARTESIAN_POINT('Ctrl Pts',(-46.724976393213,53.7590677201344,12.));
#93680=CARTESIAN_POINT('Ctrl Pts',(-46.7056945424559,53.7475648793948,12.));
#93681=CARTESIAN_POINT('Ctrl Pts',(-46.6864639475863,53.7360662508677,12.));
#93682=CARTESIAN_POINT('Ctrl Pts',(-46.6672846938752,53.7245719674222,12.));
#93683=CARTESIAN_POINT('Ctrl Pts',(-46.6481568669216,53.7130821626263,12.));
#93684=CARTESIAN_POINT('Ctrl Pts',(-46.6290805526559,53.701596970754,12.));
#93685=CARTESIAN_POINT('Ctrl Pts',(-46.6100558373402,53.6901165267941,12.));
#93686=CARTESIAN_POINT('Ctrl Pts',(-46.5910828075653,53.678640966456,12.));
#93687=CARTESIAN_POINT('Ctrl Pts',(-46.5721615502591,53.6671704261737,12.));
#93688=CARTESIAN_POINT('Ctrl Pts',(-46.5532921526901,53.6557050431071,12.));
#93689=CARTESIAN_POINT('Ctrl Pts',(-46.5344747024676,53.6442449551455,12.));
#93690=CARTESIAN_POINT('Ctrl Pts',(-46.5157092875373,53.6327903009094,12.));
#93691=CARTESIAN_POINT('Ctrl Pts',(-46.496995996177,53.6213412197533,12.));
#93692=CARTESIAN_POINT('Ctrl Pts',(-46.4783349170173,53.6098978517859,12.));
#93693=CARTESIAN_POINT('Ctrl Pts',(-46.459726139052,53.5984603378855,12.));
#93694=CARTESIAN_POINT('Ctrl Pts',(-46.4411697516478,53.5870288197166,12.));
#93695=CARTESIAN_POINT('Ctrl Pts',(-46.4226658445474,53.5756034397481,12.));
#93696=CARTESIAN_POINT('Ctrl Pts',(-46.4042145078701,53.5641843412559,12.));
#93697=CARTESIAN_POINT('Ctrl Pts',(-46.3858158321059,53.5527716683047,12.));
#93698=CARTESIAN_POINT('Ctrl Pts',(-46.3674699081046,53.5413655657327,12.));
#93699=CARTESIAN_POINT('Ctrl Pts',(-46.3491768270655,53.5299661791385,12.));
#93700=CARTESIAN_POINT('Ctrl Pts',(-46.3309366805093,53.5185736548548,12.));
#93701=CARTESIAN_POINT('Ctrl Pts',(-46.3127495603098,53.5071881399911,12.));
#93702=CARTESIAN_POINT('Ctrl Pts',(-46.2946155587417,53.4958097825006,12.));
#93703=CARTESIAN_POINT('Ctrl Pts',(-46.2765347685198,53.4844387312414,12.));
#93704=CARTESIAN_POINT('Ctrl Pts',(-46.2585072828353,53.4730751360371,12.));
#93705=CARTESIAN_POINT('Ctrl Pts',(-46.2405331953889,53.4617191477402,12.));
#93706=CARTESIAN_POINT('Ctrl Pts',(-46.2226126003202,53.4503709181178,12.));
#93707=CARTESIAN_POINT('Ctrl Pts',(-46.2047455921286,53.4390305997274,12.));
#93708=CARTESIAN_POINT('Ctrl Pts',(-46.1869322656024,53.4276983458125,12.));
#93709=CARTESIAN_POINT('Ctrl Pts',(-46.1691727157134,53.4163743101517,12.));
#93710=CARTESIAN_POINT('Ctrl Pts',(-46.1514670376012,53.4050586470436,12.));
#93711=CARTESIAN_POINT('Ctrl Pts',(-46.1338153268097,53.3937515116549,12.));
#93712=CARTESIAN_POINT('Ctrl Pts',(-46.1162176794884,53.3824530603276,12.));
#93713=CARTESIAN_POINT('Ctrl Pts',(-46.0986741925656,53.3711634508437,12.));
#93714=CARTESIAN_POINT('Ctrl Pts',(-46.0811849640218,53.3598828428546,12.));
#93715=CARTESIAN_POINT('Ctrl Pts',(-46.0637500926982,53.3486113975901,12.));
#93716=CARTESIAN_POINT('Ctrl Pts',(-46.0463696777801,53.3373492770671,12.));
#93717=CARTESIAN_POINT('Ctrl Pts',(-46.02904381836,53.326096643428,12.));
#93718=CARTESIAN_POINT('Ctrl Pts',(-46.0117726129873,53.3148536582635,12.));
#93719=CARTESIAN_POINT('Ctrl Pts',(-45.9945561591453,53.3036204818329,12.));
#93720=CARTESIAN_POINT('Ctrl Pts',(-45.9773945542384,53.292397274555,12.));
#93721=CARTESIAN_POINT('Ctrl Pts',(-45.9602878967698,53.2811841987926,12.));
#93722=CARTESIAN_POINT('Ctrl Pts',(-45.9432362873008,53.2699814203105,12.));
#93723=CARTESIAN_POINT('Ctrl Pts',(-45.9262398298349,53.2587891103866,12.));
#93724=CARTESIAN_POINT('Ctrl Pts',(-45.9092986319377,53.2476074460017,12.));
#93725=CARTESIAN_POINT('Ctrl Pts',(-45.892412801838,53.2364366054306,12.));
#93726=CARTESIAN_POINT('Ctrl Pts',(-45.8755824458723,53.2252767643662,12.));
#93727=CARTESIAN_POINT('Ctrl Pts',(-45.8588076662582,53.2141280925439,12.));
#93728=CARTESIAN_POINT('Ctrl Pts',(-45.8420885575349,53.2029907483557,12.));
#93729=CARTESIAN_POINT('Ctrl Pts',(-45.8254252099957,53.1918648840541,12.));
#93730=CARTESIAN_POINT('Ctrl Pts',(-45.808817716509,53.1807506560933,12.));
#93731=CARTESIAN_POINT('Ctrl Pts',(-45.7922661780005,53.1696482334487,12.));
#93732=CARTESIAN_POINT('Ctrl Pts',(-45.7757707100618,53.1585578076444,12.));
#93733=CARTESIAN_POINT('Ctrl Pts',(-45.7593314474501,53.1474795996053,12.));
#93734=CARTESIAN_POINT('Ctrl Pts',(-45.7429485300823,53.1364138384693,12.));
#93735=CARTESIAN_POINT('Ctrl Pts',(-45.7266220897003,53.1253607414872,12.));
#93736=CARTESIAN_POINT('Ctrl Pts',(-45.7103522376696,53.114320495492,12.));
#93737=CARTESIAN_POINT('Ctrl Pts',(-45.694139048907,53.1032932328857,12.));
#93738=CARTESIAN_POINT('Ctrl Pts',(-45.6779825614231,53.0922790298409,12.));
#93739=CARTESIAN_POINT('Ctrl Pts',(-45.6651027439241,53.0834781451546,12.));
#93740=CARTESIAN_POINT('Ctrl Pts',(-45.6554684028145,53.0768833804193,12.));
#93741=CARTESIAN_POINT('Ctrl Pts',(-45.6490568514089,53.0724894921849,12.));
#93742=CARTESIAN_POINT('Ctrl Pts',(-45.6458539113724,53.0702932034641,12.));
#93743=CARTESIAN_POINT('Ctrl Pts',(-50.6869108458849,54.1946543500369,-5.55111512312578E-16));
#93744=CARTESIAN_POINT('Ctrl Pts',(-50.6869108458849,54.1946543500369,4.));
#93745=CARTESIAN_POINT('Ctrl Pts',(-50.6869108458849,54.194654350037,8.));
#93746=CARTESIAN_POINT('Ctrl Pts',(-50.6869108458849,54.194654350037,12.));
#93747=CARTESIAN_POINT('Ctrl Pts',(-50.7223900873019,54.2986513683563,-5.55111512312578E-16));
#93748=CARTESIAN_POINT('Ctrl Pts',(-50.7223900873019,54.2986513683563,4.));
#93749=CARTESIAN_POINT('Ctrl Pts',(-50.722390087302,54.2986513683564,8.));
#93750=CARTESIAN_POINT('Ctrl Pts',(-50.722390087302,54.2986513683564,12.));
#93751=CARTESIAN_POINT('Ctrl Pts',(-50.7219766588191,54.5013145669259,-5.55111512312578E-16));
#93752=CARTESIAN_POINT('Ctrl Pts',(-50.7219766588191,54.5013145669259,4.));
#93753=CARTESIAN_POINT('Ctrl Pts',(-50.7219766588192,54.501314566926,8.00000000000001));
#93754=CARTESIAN_POINT('Ctrl Pts',(-50.7219766588192,54.501314566926,12.));
#93755=CARTESIAN_POINT('Ctrl Pts',(-50.6135081477653,54.667445382869,-5.55111512312578E-16));
#93756=CARTESIAN_POINT('Ctrl Pts',(-50.6135081477653,54.667445382869,4.));
#93757=CARTESIAN_POINT('Ctrl Pts',(-50.6135081477653,54.6674453828691,8.));
#93758=CARTESIAN_POINT('Ctrl Pts',(-50.6135081477653,54.6674453828691,12.));
#93759=CARTESIAN_POINT('Ctrl Pts',(-50.5529731960896,54.7233670476822,-5.55111512312578E-16));
#93760=CARTESIAN_POINT('Ctrl Pts',(-50.5529731960896,54.7233670476822,4.));
#93761=CARTESIAN_POINT('Ctrl Pts',(-50.5529731960896,54.7233670476823,8.));
#93762=CARTESIAN_POINT('Ctrl Pts',(-50.5529731960896,54.7233670476823,12.));
#93763=CARTESIAN_POINT('',(-50.6869108458849,54.1946543500369,-2.77555756156289E-16));
#93764=CARTESIAN_POINT('',(-50.5529731960901,54.7233670476827,0.));
#93765=CARTESIAN_POINT('Ctrl Pts',(-50.6869108458849,54.1946543500369,-5.55111512312578E-16));
#93766=CARTESIAN_POINT('Ctrl Pts',(-50.7223900873019,54.2986513683563,-5.55111512312578E-16));
#93767=CARTESIAN_POINT('Ctrl Pts',(-50.7221538424546,54.4144589103961,-5.55111512312578E-16));
#93768=CARTESIAN_POINT('Ctrl Pts',(-50.6866343053392,54.51833751117,-5.55111512312578E-16));
#93769=CARTESIAN_POINT('Ctrl Pts',(-50.6599946525026,54.5962464617505,-5.55111512312578E-16));
#93770=CARTESIAN_POINT('Ctrl Pts',(-50.6135081477653,54.667445382869,-5.55111512312578E-16));
#93771=CARTESIAN_POINT('Ctrl Pts',(-50.5529731960896,54.7233670476822,-5.55111512312578E-16));
#93772=CARTESIAN_POINT('',(-50.55297319609,54.7233670476827,12.));
#93773=CARTESIAN_POINT('Ctrl Pts',(-50.5529731960896,54.7233670476822,-5.55111512312578E-16));
#93774=CARTESIAN_POINT('Ctrl Pts',(-50.5529731960896,54.7233670476822,4.));
#93775=CARTESIAN_POINT('Ctrl Pts',(-50.5529731960896,54.7233670476823,8.));
#93776=CARTESIAN_POINT('Ctrl Pts',(-50.5529731960896,54.7233670476823,12.));
#93777=CARTESIAN_POINT('',(-50.6869108458849,54.194654350037,12.));
#93778=CARTESIAN_POINT('Ctrl Pts',(-50.5529731960896,54.7233670476823,12.));
#93779=CARTESIAN_POINT('Ctrl Pts',(-50.6135081477653,54.6674453828691,12.));
#93780=CARTESIAN_POINT('Ctrl Pts',(-50.6599946525027,54.5962464617506,12.));
#93781=CARTESIAN_POINT('Ctrl Pts',(-50.6866343053393,54.5183375111701,12.));
#93782=CARTESIAN_POINT('Ctrl Pts',(-50.7221538424547,54.4144589103961,12.));
#93783=CARTESIAN_POINT('Ctrl Pts',(-50.722390087302,54.2986513683564,12.));
#93784=CARTESIAN_POINT('Ctrl Pts',(-50.6869108458849,54.194654350037,12.));
#93785=CARTESIAN_POINT('Ctrl Pts',(-50.6869108458849,54.194654350037,12.));
#93786=CARTESIAN_POINT('Ctrl Pts',(-50.6869108458849,54.194654350037,8.));
#93787=CARTESIAN_POINT('Ctrl Pts',(-50.6869108458849,54.1946543500369,4.));
#93788=CARTESIAN_POINT('Ctrl Pts',(-50.6869108458849,54.1946543500369,-5.55111512312578E-16));
#93789=CARTESIAN_POINT('Origin',(-2.53313958019842E-10,2.7629675461203E-10,
0.));
#93790=CARTESIAN_POINT('Origin',(-2.53313958019842E-10,2.7629675461203E-10,
12.));
#93791=CARTESIAN_POINT('Origin',(-2.53313958019842E-10,2.7629675461203E-10,
0.));
#93792=CARTESIAN_POINT('Ctrl Pts',(-45.1135644683471,59.2875729049545,-5.55111512312578E-16));
#93793=CARTESIAN_POINT('Ctrl Pts',(-45.1135644683471,59.2875729049545,4.));
#93794=CARTESIAN_POINT('Ctrl Pts',(-45.113564468347,59.2875729049545,8.));
#93795=CARTESIAN_POINT('Ctrl Pts',(-45.113564468347,59.2875729049545,12.));
#93796=CARTESIAN_POINT('Ctrl Pts',(-45.0261193041895,59.3541123643618,-5.55111512312578E-16));
#93797=CARTESIAN_POINT('Ctrl Pts',(-45.0261193041895,59.3541123643618,4.));
#93798=CARTESIAN_POINT('Ctrl Pts',(-45.0261193041895,59.3541123643618,8.));
#93799=CARTESIAN_POINT('Ctrl Pts',(-45.0261193041895,59.3541123643618,12.));
#93800=CARTESIAN_POINT('Ctrl Pts',(-44.8337211159574,59.4177951463802,-5.55111512312578E-16));
#93801=CARTESIAN_POINT('Ctrl Pts',(-44.8337211159574,59.4177951463802,4.));
#93802=CARTESIAN_POINT('Ctrl Pts',(-44.8337211159573,59.4177951463802,8.));
#93803=CARTESIAN_POINT('Ctrl Pts',(-44.8337211159573,59.4177951463802,12.));
#93804=CARTESIAN_POINT('Ctrl Pts',(-44.6418181989797,59.3674150879747,-5.55111512312578E-16));
#93805=CARTESIAN_POINT('Ctrl Pts',(-44.6418181989797,59.3674150879747,4.));
#93806=CARTESIAN_POINT('Ctrl Pts',(-44.6418181989796,59.3674150879747,8.00000000000001));
#93807=CARTESIAN_POINT('Ctrl Pts',(-44.6418181989796,59.3674150879747,12.));
#93808=CARTESIAN_POINT('Ctrl Pts',(-44.5696260757421,59.3276657444156,-5.55111512312578E-16));
#93809=CARTESIAN_POINT('Ctrl Pts',(-44.5696260757421,59.3276657444156,4.));
#93810=CARTESIAN_POINT('Ctrl Pts',(-44.5696260757421,59.3276657444156,8.));
#93811=CARTESIAN_POINT('Ctrl Pts',(-44.5696260757421,59.3276657444156,12.));
#93812=CARTESIAN_POINT('',(-45.1135644683471,59.2875729049545,0.));
#93813=CARTESIAN_POINT('',(-44.5696260757421,59.3276657444158,0.));
#93814=CARTESIAN_POINT('Ctrl Pts',(-45.1135644683471,59.2875729049545,-5.55111512312578E-16));
#93815=CARTESIAN_POINT('Ctrl Pts',(-45.0261193041895,59.3541123643618,-5.55111512312578E-16));
#93816=CARTESIAN_POINT('Ctrl Pts',(-44.9161774823426,59.3905025255151,-5.55111512312578E-16));
#93817=CARTESIAN_POINT('Ctrl Pts',(-44.8063973817216,59.3896476775505,-5.55111512312578E-16));
#93818=CARTESIAN_POINT('Ctrl Pts',(-44.7240623062559,59.389006541577,-5.55111512312578E-16));
#93819=CARTESIAN_POINT('Ctrl Pts',(-44.6418181989797,59.3674150879747,-5.55111512312578E-16));
#93820=CARTESIAN_POINT('Ctrl Pts',(-44.5696260757421,59.3276657444156,-5.55111512312578E-16));
#93821=CARTESIAN_POINT('',(-44.569626075742,59.3276657444158,12.));
#93822=CARTESIAN_POINT('Ctrl Pts',(-44.5696260757421,59.3276657444156,-5.55111512312578E-16));
#93823=CARTESIAN_POINT('Ctrl Pts',(-44.5696260757421,59.3276657444156,4.));
#93824=CARTESIAN_POINT('Ctrl Pts',(-44.5696260757421,59.3276657444156,8.));
#93825=CARTESIAN_POINT('Ctrl Pts',(-44.5696260757421,59.3276657444156,12.));
#93826=CARTESIAN_POINT('',(-45.113564468347,59.2875729049545,12.));
#93827=CARTESIAN_POINT('Ctrl Pts',(-44.5696260757421,59.3276657444156,12.));
#93828=CARTESIAN_POINT('Ctrl Pts',(-44.6418181989796,59.3674150879747,12.));
#93829=CARTESIAN_POINT('Ctrl Pts',(-44.7240623062558,59.3890065415771,12.));
#93830=CARTESIAN_POINT('Ctrl Pts',(-44.8063973817216,59.3896476775505,12.));
#93831=CARTESIAN_POINT('Ctrl Pts',(-44.9161774823425,59.3905025255152,12.));
#93832=CARTESIAN_POINT('Ctrl Pts',(-45.0261193041895,59.3541123643618,12.));
#93833=CARTESIAN_POINT('Ctrl Pts',(-45.113564468347,59.2875729049545,12.));
#93834=CARTESIAN_POINT('Ctrl Pts',(-45.113564468347,59.2875729049545,12.));
#93835=CARTESIAN_POINT('Ctrl Pts',(-45.113564468347,59.2875729049545,8.));
#93836=CARTESIAN_POINT('Ctrl Pts',(-45.1135644683471,59.2875729049545,4.));
#93837=CARTESIAN_POINT('Ctrl Pts',(-45.1135644683471,59.2875729049545,-5.55111512312578E-16));
#93838=CARTESIAN_POINT('Ctrl Pts',(-40.8467768343956,56.8466430164621,0.));
#93839=CARTESIAN_POINT('Ctrl Pts',(-40.8467768343956,56.8466430164621,12.));
#93840=CARTESIAN_POINT('Ctrl Pts',(-40.8497761671036,56.8491101022591,0.));
#93841=CARTESIAN_POINT('Ctrl Pts',(-40.8497761671036,56.8491101022591,12.));
#93842=CARTESIAN_POINT('Ctrl Pts',(-40.8557803680277,56.8540460739472,0.));
#93843=CARTESIAN_POINT('Ctrl Pts',(-40.8557803680277,56.8540460739472,12.));
#93844=CARTESIAN_POINT('Ctrl Pts',(-40.864803275942,56.8614554317668,0.));
#93845=CARTESIAN_POINT('Ctrl Pts',(-40.864803275942,56.8614554317668,12.));
#93846=CARTESIAN_POINT('Ctrl Pts',(-40.8768670342052,56.8713453764905,0.));
#93847=CARTESIAN_POINT('Ctrl Pts',(-40.8768670342052,56.8713453764905,12.));
#93848=CARTESIAN_POINT('Ctrl Pts',(-40.8920020903293,56.8837257978343,0.));
#93849=CARTESIAN_POINT('Ctrl Pts',(-40.8920020903293,56.8837257978343,12.));
#93850=CARTESIAN_POINT('Ctrl Pts',(-40.9071924937508,56.8961241708861,0.));
#93851=CARTESIAN_POINT('Ctrl Pts',(-40.9071924937508,56.8961241708861,12.));
#93852=CARTESIAN_POINT('Ctrl Pts',(-40.9224382132427,56.9085404164502,0.));
#93853=CARTESIAN_POINT('Ctrl Pts',(-40.9224382132427,56.9085404164502,12.));
#93854=CARTESIAN_POINT('Ctrl Pts',(-40.9377391857128,56.9209743960992,0.));
#93855=CARTESIAN_POINT('Ctrl Pts',(-40.9377391857128,56.9209743960992,12.));
#93856=CARTESIAN_POINT('Ctrl Pts',(-40.9530953165031,56.9334259140049,0.));
#93857=CARTESIAN_POINT('Ctrl Pts',(-40.9530953165031,56.9334259140049,12.));
#93858=CARTESIAN_POINT('Ctrl Pts',(-40.9685064933074,56.9458947422608,0.));
#93859=CARTESIAN_POINT('Ctrl Pts',(-40.9685064933074,56.9458947422608,12.));
#93860=CARTESIAN_POINT('Ctrl Pts',(-40.9839725967121,56.9583806404069,0.));
#93861=CARTESIAN_POINT('Ctrl Pts',(-40.9839725967121,56.9583806404069,12.));
#93862=CARTESIAN_POINT('Ctrl Pts',(-40.9994935117276,56.9708833766137,0.));
#93863=CARTESIAN_POINT('Ctrl Pts',(-40.9994935117276,56.9708833766137,12.));
#93864=CARTESIAN_POINT('Ctrl Pts',(-41.0150691398947,56.9834027500117,0.));
#93865=CARTESIAN_POINT('Ctrl Pts',(-41.0150691398947,56.9834027500117,12.));
#93866=CARTESIAN_POINT('Ctrl Pts',(-41.0306993953988,56.995938583472,0.));
#93867=CARTESIAN_POINT('Ctrl Pts',(-41.0306993953988,56.995938583472,12.));
#93868=CARTESIAN_POINT('Ctrl Pts',(-41.0463841993608,57.008490713042,0.));
#93869=CARTESIAN_POINT('Ctrl Pts',(-41.0463841993608,57.008490713042,12.));
#93870=CARTESIAN_POINT('Ctrl Pts',(-41.0621234751007,57.0210589791788,0.));
#93871=CARTESIAN_POINT('Ctrl Pts',(-41.0621234751007,57.0210589791788,12.));
#93872=CARTESIAN_POINT('Ctrl Pts',(-41.0779171422438,57.0336432158536,0.));
#93873=CARTESIAN_POINT('Ctrl Pts',(-41.0779171422438,57.0336432158536,12.));
#93874=CARTESIAN_POINT('Ctrl Pts',(-41.0937651137549,57.046243245068,0.));
#93875=CARTESIAN_POINT('Ctrl Pts',(-41.0937651137549,57.046243245068,12.));
#93876=CARTESIAN_POINT('Ctrl Pts',(-41.1096672990148,57.0588588825298,0.));
#93877=CARTESIAN_POINT('Ctrl Pts',(-41.1096672990148,57.0588588825298,12.));
#93878=CARTESIAN_POINT('Ctrl Pts',(-41.1256236057442,57.0714899412099,0.));
#93879=CARTESIAN_POINT('Ctrl Pts',(-41.1256236057442,57.0714899412099,12.));
#93880=CARTESIAN_POINT('Ctrl Pts',(-41.1416339422117,57.084136235426,0.));
#93881=CARTESIAN_POINT('Ctrl Pts',(-41.1416339422117,57.084136235426,12.));
#93882=CARTESIAN_POINT('Ctrl Pts',(-41.1576982197374,57.0967975854874,0.));
#93883=CARTESIAN_POINT('Ctrl Pts',(-41.1576982197374,57.0967975854874,12.));
#93884=CARTESIAN_POINT('Ctrl Pts',(-41.1738163525901,57.1094738174957,0.));
#93885=CARTESIAN_POINT('Ctrl Pts',(-41.1738163525901,57.1094738174957,12.));
#93886=CARTESIAN_POINT('Ctrl Pts',(-41.1899882567923,57.1221647611207,0.));
#93887=CARTESIAN_POINT('Ctrl Pts',(-41.1899882567923,57.1221647611207,12.));
#93888=CARTESIAN_POINT('Ctrl Pts',(-41.2062138492915,57.1348702480647,0.));
#93889=CARTESIAN_POINT('Ctrl Pts',(-41.2062138492915,57.1348702480647,12.));
#93890=CARTESIAN_POINT('Ctrl Pts',(-41.222493046943,57.147590110182,0.));
#93891=CARTESIAN_POINT('Ctrl Pts',(-41.222493046943,57.147590110182,12.));
#93892=CARTESIAN_POINT('Ctrl Pts',(-41.2388257656559,57.1603241779077,0.));
#93893=CARTESIAN_POINT('Ctrl Pts',(-41.2388257656559,57.1603241779077,12.));
#93894=CARTESIAN_POINT('Ctrl Pts',(-41.2552119208465,57.17307228108,0.));
#93895=CARTESIAN_POINT('Ctrl Pts',(-41.2552119208465,57.17307228108,12.));
#93896=CARTESIAN_POINT('Ctrl Pts',(-41.2716514278276,57.1858342496538,0.));
#93897=CARTESIAN_POINT('Ctrl Pts',(-41.2716514278276,57.1858342496538,12.));
#93898=CARTESIAN_POINT('Ctrl Pts',(-41.2881442021863,57.1986099143983,0.));
#93899=CARTESIAN_POINT('Ctrl Pts',(-41.2881442021863,57.1986099143983,12.));
#93900=CARTESIAN_POINT('Ctrl Pts',(-41.3046901602293,57.2113991077302,0.));
#93901=CARTESIAN_POINT('Ctrl Pts',(-41.3046901602293,57.2113991077302,12.));
#93902=CARTESIAN_POINT('Ctrl Pts',(-41.321289219149,57.2242016640198,0.));
#93903=CARTESIAN_POINT('Ctrl Pts',(-41.321289219149,57.2242016640198,12.));
#93904=CARTESIAN_POINT('Ctrl Pts',(-41.3379412967875,57.2370174191401,0.));
#93905=CARTESIAN_POINT('Ctrl Pts',(-41.3379412967875,57.2370174191401,12.));
#93906=CARTESIAN_POINT('Ctrl Pts',(-41.3546463114885,57.2498462101879,0.));
#93907=CARTESIAN_POINT('Ctrl Pts',(-41.3546463114885,57.2498462101879,12.));
#93908=CARTESIAN_POINT('Ctrl Pts',(-41.3714041819223,57.2626878751596,0.));
#93909=CARTESIAN_POINT('Ctrl Pts',(-41.3714041819223,57.2626878751596,12.));
#93910=CARTESIAN_POINT('Ctrl Pts',(-41.3882148268813,57.2755422525844,0.));
#93911=CARTESIAN_POINT('Ctrl Pts',(-41.3882148268813,57.2755422525844,12.));
#93912=CARTESIAN_POINT('Ctrl Pts',(-41.4050781652938,57.2884091815406,0.));
#93913=CARTESIAN_POINT('Ctrl Pts',(-41.4050781652938,57.2884091815406,12.));
#93914=CARTESIAN_POINT('Ctrl Pts',(-41.4219941163163,57.3012885018151,0.));
#93915=CARTESIAN_POINT('Ctrl Pts',(-41.4219941163163,57.3012885018151,12.));
#93916=CARTESIAN_POINT('Ctrl Pts',(-41.4389625993948,57.3141800540137,0.));
#93917=CARTESIAN_POINT('Ctrl Pts',(-41.4389625993948,57.3141800540137,12.));
#93918=CARTESIAN_POINT('Ctrl Pts',(-41.4559835343328,57.3270836796911,0.));
#93919=CARTESIAN_POINT('Ctrl Pts',(-41.4559835343328,57.3270836796911,12.));
#93920=CARTESIAN_POINT('Ctrl Pts',(-41.4730568413518,57.3399992214717,0.));
#93921=CARTESIAN_POINT('Ctrl Pts',(-41.4730568413518,57.3399992214717,12.));
#93922=CARTESIAN_POINT('Ctrl Pts',(-41.4901824410636,57.3529265229835,0.));
#93923=CARTESIAN_POINT('Ctrl Pts',(-41.4901824410636,57.3529265229835,12.));
#93924=CARTESIAN_POINT('Ctrl Pts',(-41.5073602544396,57.3658654287937,0.));
#93925=CARTESIAN_POINT('Ctrl Pts',(-41.5073602544396,57.3658654287937,12.));
#93926=CARTESIAN_POINT('Ctrl Pts',(-41.524590202777,57.3788157843454,0.));
#93927=CARTESIAN_POINT('Ctrl Pts',(-41.524590202777,57.3788157843454,12.));
#93928=CARTESIAN_POINT('Ctrl Pts',(-41.5418722076572,57.3917774358863,0.));
#93929=CARTESIAN_POINT('Ctrl Pts',(-41.5418722076572,57.3917774358863,12.));
#93930=CARTESIAN_POINT('Ctrl Pts',(-41.5592061909176,57.4047502304231,0.));
#93931=CARTESIAN_POINT('Ctrl Pts',(-41.5592061909176,57.4047502304231,12.));
#93932=CARTESIAN_POINT('Ctrl Pts',(-41.5765920746777,57.4177340157508,0.));
#93933=CARTESIAN_POINT('Ctrl Pts',(-41.5765920746777,57.4177340157508,12.));
#93934=CARTESIAN_POINT('Ctrl Pts',(-41.5940297813477,57.4307286404662,0.));
#93935=CARTESIAN_POINT('Ctrl Pts',(-41.5940297813477,57.4307286404662,12.));
#93936=CARTESIAN_POINT('Ctrl Pts',(-41.6115192336388,57.4437339539841,0.));
#93937=CARTESIAN_POINT('Ctrl Pts',(-41.6115192336388,57.4437339539841,12.));
#93938=CARTESIAN_POINT('Ctrl Pts',(-41.6290603545666,57.4567498065562,0.));
#93939=CARTESIAN_POINT('Ctrl Pts',(-41.6290603545666,57.4567498065562,12.));
#93940=CARTESIAN_POINT('Ctrl Pts',(-41.6466530674514,57.4697760492683,0.));
#93941=CARTESIAN_POINT('Ctrl Pts',(-41.6466530674514,57.4697760492683,12.));
#93942=CARTESIAN_POINT('Ctrl Pts',(-41.6642972959165,57.4828125340218,0.));
#93943=CARTESIAN_POINT('Ctrl Pts',(-41.6642972959165,57.4828125340218,12.));
#93944=CARTESIAN_POINT('Ctrl Pts',(-41.6819929638797,57.4958591135165,0.));
#93945=CARTESIAN_POINT('Ctrl Pts',(-41.6819929638797,57.4958591135165,12.));
#93946=CARTESIAN_POINT('Ctrl Pts',(-41.6997399955447,57.5089156412343,0.));
#93947=CARTESIAN_POINT('Ctrl Pts',(-41.6997399955447,57.5089156412343,12.));
#93948=CARTESIAN_POINT('Ctrl Pts',(-41.7175383153821,57.5219819714171,0.));
#93949=CARTESIAN_POINT('Ctrl Pts',(-41.7175383153821,57.5219819714171,12.));
#93950=CARTESIAN_POINT('Ctrl Pts',(-41.7353878481336,57.5350579590649,0.));
#93951=CARTESIAN_POINT('Ctrl Pts',(-41.7353878481336,57.5350579590649,12.));
#93952=CARTESIAN_POINT('Ctrl Pts',(-41.7532885188174,57.5481434599335,0.));
#93953=CARTESIAN_POINT('Ctrl Pts',(-41.7532885188174,57.5481434599335,12.));
#93954=CARTESIAN_POINT('Ctrl Pts',(-41.7712402527273,57.561238330532,0.));
#93955=CARTESIAN_POINT('Ctrl Pts',(-41.7712402527273,57.561238330532,12.));
#93956=CARTESIAN_POINT('Ctrl Pts',(-41.7892429754297,57.5743424281205,0.));
#93957=CARTESIAN_POINT('Ctrl Pts',(-41.7892429754297,57.5743424281205,12.));
#93958=CARTESIAN_POINT('Ctrl Pts',(-41.8072966127558,57.5874556107056,0.));
#93959=CARTESIAN_POINT('Ctrl Pts',(-41.8072966127558,57.5874556107056,12.));
#93960=CARTESIAN_POINT('Ctrl Pts',(-41.8254010908051,57.6005777370349,0.));
#93961=CARTESIAN_POINT('Ctrl Pts',(-41.8254010908051,57.6005777370349,12.));
#93962=CARTESIAN_POINT('Ctrl Pts',(-41.8435563359456,57.6137086665882,0.));
#93963=CARTESIAN_POINT('Ctrl Pts',(-41.8435563359456,57.6137086665882,12.));
#93964=CARTESIAN_POINT('Ctrl Pts',(-41.8617622748108,57.6268482595702,0.));
#93965=CARTESIAN_POINT('Ctrl Pts',(-41.8617622748108,57.6268482595702,12.));
#93966=CARTESIAN_POINT('Ctrl Pts',(-41.8800188342908,57.6399963769003,0.));
#93967=CARTESIAN_POINT('Ctrl Pts',(-41.8800188342908,57.6399963769003,12.));
#93968=CARTESIAN_POINT('Ctrl Pts',(-41.8983259415244,57.6531528802059,0.));
#93969=CARTESIAN_POINT('Ctrl Pts',(-41.8983259415244,57.6531528802059,12.));
#93970=CARTESIAN_POINT('Ctrl Pts',(-41.9166835239046,57.6663176318176,0.));
#93971=CARTESIAN_POINT('Ctrl Pts',(-41.9166835239046,57.6663176318176,12.));
#93972=CARTESIAN_POINT('Ctrl Pts',(-41.9350915090791,57.6794904947641,0.));
#93973=CARTESIAN_POINT('Ctrl Pts',(-41.9350915090791,57.6794904947641,12.));
#93974=CARTESIAN_POINT('Ctrl Pts',(-41.9535498249489,57.6926713327674,0.));
#93975=CARTESIAN_POINT('Ctrl Pts',(-41.9535498249489,57.6926713327674,12.));
#93976=CARTESIAN_POINT('Ctrl Pts',(-41.9720583996601,57.7058600102365,0.));
#93977=CARTESIAN_POINT('Ctrl Pts',(-41.9720583996601,57.7058600102365,12.));
#93978=CARTESIAN_POINT('Ctrl Pts',(-41.9906171615974,57.7190563922614,0.));
#93979=CARTESIAN_POINT('Ctrl Pts',(-41.9906171615974,57.7190563922614,12.));
#93980=CARTESIAN_POINT('Ctrl Pts',(-42.0092260393911,57.7322603446086,0.));
#93981=CARTESIAN_POINT('Ctrl Pts',(-42.0092260393911,57.7322603446086,12.));
#93982=CARTESIAN_POINT('Ctrl Pts',(-42.0278849619156,57.7454717337151,0.));
#93983=CARTESIAN_POINT('Ctrl Pts',(-42.0278849619156,57.7454717337151,12.));
#93984=CARTESIAN_POINT('Ctrl Pts',(-42.0465938582877,57.7586904266828,0.));
#93985=CARTESIAN_POINT('Ctrl Pts',(-42.0465938582877,57.7586904266828,12.));
#93986=CARTESIAN_POINT('Ctrl Pts',(-42.0653526578571,57.7719162912721,0.));
#93987=CARTESIAN_POINT('Ctrl Pts',(-42.0653526578571,57.7719162912721,12.));
#93988=CARTESIAN_POINT('Ctrl Pts',(-42.0841612902018,57.7851491958954,0.));
#93989=CARTESIAN_POINT('Ctrl Pts',(-42.0841612902018,57.7851491958954,12.));
#93990=CARTESIAN_POINT('Ctrl Pts',(-42.1030196851344,57.798389009613,0.));
#93991=CARTESIAN_POINT('Ctrl Pts',(-42.1030196851344,57.798389009613,12.));
#93992=CARTESIAN_POINT('Ctrl Pts',(-42.121927772701,57.8116356021274,0.));
#93993=CARTESIAN_POINT('Ctrl Pts',(-42.121927772701,57.8116356021274,12.));
#93994=CARTESIAN_POINT('Ctrl Pts',(-42.1408854831791,57.8248888437787,0.));
#93995=CARTESIAN_POINT('Ctrl Pts',(-42.1408854831791,57.8248888437787,12.));
#93996=CARTESIAN_POINT('Ctrl Pts',(-42.1598927470671,57.8381486055376,0.));
#93997=CARTESIAN_POINT('Ctrl Pts',(-42.1598927470671,57.8381486055376,12.));
#93998=CARTESIAN_POINT('Ctrl Pts',(-42.1789494950824,57.8514147590012,0.));
#93999=CARTESIAN_POINT('Ctrl Pts',(-42.1789494950824,57.8514147590012,12.));
#94000=CARTESIAN_POINT('Ctrl Pts',(-42.1980556581688,57.86468717639,0.));
#94001=CARTESIAN_POINT('Ctrl Pts',(-42.1980556581688,57.86468717639,12.));
#94002=CARTESIAN_POINT('Ctrl Pts',(-42.2172111674945,57.8779657305423,0.));
#94003=CARTESIAN_POINT('Ctrl Pts',(-42.2172111674945,57.8779657305423,12.));
#94004=CARTESIAN_POINT('Ctrl Pts',(-42.2364159544492,57.8912502949084,0.));
#94005=CARTESIAN_POINT('Ctrl Pts',(-42.2364159544492,57.8912502949084,12.));
#94006=CARTESIAN_POINT('Ctrl Pts',(-42.2556699506332,57.9045407435447,0.));
#94007=CARTESIAN_POINT('Ctrl Pts',(-42.2556699506332,57.9045407435447,12.));
#94008=CARTESIAN_POINT('Ctrl Pts',(-42.274973087857,57.9178369511084,0.));
#94009=CARTESIAN_POINT('Ctrl Pts',(-42.274973087857,57.9178369511084,12.));
#94010=CARTESIAN_POINT('Ctrl Pts',(-42.2943252981471,57.9311387928541,0.));
#94011=CARTESIAN_POINT('Ctrl Pts',(-42.2943252981471,57.9311387928541,12.));
#94012=CARTESIAN_POINT('Ctrl Pts',(-42.3137265137446,57.9444461446292,0.));
#94013=CARTESIAN_POINT('Ctrl Pts',(-42.3137265137446,57.9444461446292,12.));
#94014=CARTESIAN_POINT('Ctrl Pts',(-42.3331766671028,57.9577588828693,0.));
#94015=CARTESIAN_POINT('Ctrl Pts',(-42.3331766671028,57.9577588828693,12.));
#94016=CARTESIAN_POINT('Ctrl Pts',(-42.3526756908764,57.9710768845923,0.));
#94017=CARTESIAN_POINT('Ctrl Pts',(-42.3526756908764,57.9710768845923,12.));
#94018=CARTESIAN_POINT('Ctrl Pts',(-42.3722235179216,57.9844000273936,0.));
#94019=CARTESIAN_POINT('Ctrl Pts',(-42.3722235179216,57.9844000273936,12.));
#94020=CARTESIAN_POINT('Ctrl Pts',(-42.3918200813024,57.9977281894437,0.));
#94021=CARTESIAN_POINT('Ctrl Pts',(-42.3918200813024,57.9977281894437,12.));
#94022=CARTESIAN_POINT('Ctrl Pts',(-42.4114653142891,58.011061249483,0.));
#94023=CARTESIAN_POINT('Ctrl Pts',(-42.4114653142891,58.011061249483,12.));
#94024=CARTESIAN_POINT('Ctrl Pts',(-42.4311591503551,58.0243990868175,0.));
#94025=CARTESIAN_POINT('Ctrl Pts',(-42.4311591503551,58.0243990868175,12.));
#94026=CARTESIAN_POINT('Ctrl Pts',(-42.4509015231667,58.0377415813132,0.));
#94027=CARTESIAN_POINT('Ctrl Pts',(-42.4509015231667,58.0377415813132,12.));
#94028=CARTESIAN_POINT('Ctrl Pts',(-42.4706923665838,58.0510886133917,0.));
#94029=CARTESIAN_POINT('Ctrl Pts',(-42.4706923665838,58.0510886133917,12.));
#94030=CARTESIAN_POINT('Ctrl Pts',(-42.4905316146649,58.064440064027,0.));
#94031=CARTESIAN_POINT('Ctrl Pts',(-42.4905316146649,58.064440064027,12.));
#94032=CARTESIAN_POINT('Ctrl Pts',(-42.5104192016664,58.0777958147404,0.));
#94033=CARTESIAN_POINT('Ctrl Pts',(-42.5104192016664,58.0777958147404,12.));
#94034=CARTESIAN_POINT('Ctrl Pts',(-42.5303550620388,58.0911557475967,0.));
#94035=CARTESIAN_POINT('Ctrl Pts',(-42.5303550620388,58.0911557475967,12.));
#94036=CARTESIAN_POINT('Ctrl Pts',(-42.5503391304182,58.1045197452003,0.));
#94037=CARTESIAN_POINT('Ctrl Pts',(-42.5503391304182,58.1045197452003,12.));
#94038=CARTESIAN_POINT('Ctrl Pts',(-42.5703713416263,58.1178876906905,0.));
#94039=CARTESIAN_POINT('Ctrl Pts',(-42.5703713416263,58.1178876906905,12.));
#94040=CARTESIAN_POINT('Ctrl Pts',(-42.5904516306759,58.1312594677383,0.));
#94041=CARTESIAN_POINT('Ctrl Pts',(-42.5904516306759,58.1312594677383,12.));
#94042=CARTESIAN_POINT('Ctrl Pts',(-42.6105799327697,58.1446349605419,0.));
#94043=CARTESIAN_POINT('Ctrl Pts',(-42.6105799327697,58.1446349605419,12.));
#94044=CARTESIAN_POINT('Ctrl Pts',(-42.6307561832977,58.158014053823,0.));
#94045=CARTESIAN_POINT('Ctrl Pts',(-42.6307561832977,58.158014053823,12.));
#94046=CARTESIAN_POINT('Ctrl Pts',(-42.6509803178269,58.1713966328217,0.));
#94047=CARTESIAN_POINT('Ctrl Pts',(-42.6509803178269,58.1713966328217,12.));
#94048=CARTESIAN_POINT('Ctrl Pts',(-42.6712522721021,58.1847825832932,0.));
#94049=CARTESIAN_POINT('Ctrl Pts',(-42.6712522721021,58.1847825832932,12.));
#94050=CARTESIAN_POINT('Ctrl Pts',(-42.6915719820516,58.1981717915043,0.));
#94051=CARTESIAN_POINT('Ctrl Pts',(-42.6915719820516,58.1981717915043,12.));
#94052=CARTESIAN_POINT('Ctrl Pts',(-42.7119393837866,58.2115641442302,0.));
#94053=CARTESIAN_POINT('Ctrl Pts',(-42.7119393837866,58.2115641442302,12.));
#94054=CARTESIAN_POINT('Ctrl Pts',(-42.7323544135983,58.2249595287497,0.));
#94055=CARTESIAN_POINT('Ctrl Pts',(-42.7323544135983,58.2249595287497,12.));
#94056=CARTESIAN_POINT('Ctrl Pts',(-42.7528170079482,58.238357832842,0.));
#94057=CARTESIAN_POINT('Ctrl Pts',(-42.7528170079482,58.238357832842,12.));
#94058=CARTESIAN_POINT('Ctrl Pts',(-42.7733271034678,58.2517589447818,0.));
#94059=CARTESIAN_POINT('Ctrl Pts',(-42.7733271034678,58.2517589447818,12.));
#94060=CARTESIAN_POINT('Ctrl Pts',(-42.7938846369651,58.2651627533368,0.));
#94061=CARTESIAN_POINT('Ctrl Pts',(-42.7938846369651,58.2651627533368,12.));
#94062=CARTESIAN_POINT('Ctrl Pts',(-42.8144895454234,58.278569147764,0.));
#94063=CARTESIAN_POINT('Ctrl Pts',(-42.8144895454234,58.278569147764,12.));
#94064=CARTESIAN_POINT('Ctrl Pts',(-42.8351417659998,58.2919780178063,0.));
#94065=CARTESIAN_POINT('Ctrl Pts',(-42.8351417659998,58.2919780178063,12.));
#94066=CARTESIAN_POINT('Ctrl Pts',(-42.8558412360154,58.305389253689,0.));
#94067=CARTESIAN_POINT('Ctrl Pts',(-42.8558412360154,58.305389253689,12.));
#94068=CARTESIAN_POINT('Ctrl Pts',(-42.8765878929545,58.3188027461158,0.));
#94069=CARTESIAN_POINT('Ctrl Pts',(-42.8765878929545,58.3188027461158,12.));
#94070=CARTESIAN_POINT('Ctrl Pts',(-42.8973816744703,58.3322183862647,0.));
#94071=CARTESIAN_POINT('Ctrl Pts',(-42.8973816744703,58.3322183862647,12.));
#94072=CARTESIAN_POINT('Ctrl Pts',(-42.9182225183851,58.3456360657861,0.));
#94073=CARTESIAN_POINT('Ctrl Pts',(-42.9182225183851,58.3456360657861,12.));
#94074=CARTESIAN_POINT('Ctrl Pts',(-42.9391103626881,58.3590556767981,0.));
#94075=CARTESIAN_POINT('Ctrl Pts',(-42.9391103626881,58.3590556767981,12.));
#94076=CARTESIAN_POINT('Ctrl Pts',(-42.9600451455267,58.3724771118835,0.));
#94077=CARTESIAN_POINT('Ctrl Pts',(-42.9600451455267,58.3724771118835,12.));
#94078=CARTESIAN_POINT('Ctrl Pts',(-42.9810268052043,58.3859002640871,0.));
#94079=CARTESIAN_POINT('Ctrl Pts',(-42.9810268052043,58.3859002640871,12.));
#94080=CARTESIAN_POINT('Ctrl Pts',(-43.0020552801869,58.3993250269115,0.));
#94081=CARTESIAN_POINT('Ctrl Pts',(-43.0020552801869,58.3993250269115,12.));
#94082=CARTESIAN_POINT('Ctrl Pts',(-43.0231305091032,58.4127512943144,0.));
#94083=CARTESIAN_POINT('Ctrl Pts',(-43.0231305091032,58.4127512943144,12.));
#94084=CARTESIAN_POINT('Ctrl Pts',(-43.0442524307432,58.4261789607055,0.));
#94085=CARTESIAN_POINT('Ctrl Pts',(-43.0442524307432,58.4261789607055,12.));
#94086=CARTESIAN_POINT('Ctrl Pts',(-43.0654209840502,58.4396079209438,0.));
#94087=CARTESIAN_POINT('Ctrl Pts',(-43.0654209840502,58.4396079209438,12.));
#94088=CARTESIAN_POINT('Ctrl Pts',(-43.0866361081166,58.4530380703335,0.));
#94089=CARTESIAN_POINT('Ctrl Pts',(-43.0866361081166,58.4530380703335,12.));
#94090=CARTESIAN_POINT('Ctrl Pts',(-43.1078977421908,58.4664693046206,0.));
#94091=CARTESIAN_POINT('Ctrl Pts',(-43.1078977421908,58.4664693046206,12.));
#94092=CARTESIAN_POINT('Ctrl Pts',(-43.1292058256774,58.4799015199904,0.));
#94093=CARTESIAN_POINT('Ctrl Pts',(-43.1292058256774,58.4799015199904,12.));
#94094=CARTESIAN_POINT('Ctrl Pts',(-43.1505602981366,58.4933346130638,0.));
#94095=CARTESIAN_POINT('Ctrl Pts',(-43.1505602981366,58.4933346130638,12.));
#94096=CARTESIAN_POINT('Ctrl Pts',(-43.1719610992771,58.5067684808946,0.));
#94097=CARTESIAN_POINT('Ctrl Pts',(-43.1719610992771,58.5067684808946,12.));
#94098=CARTESIAN_POINT('Ctrl Pts',(-43.1934081689503,58.5202030209667,0.));
#94099=CARTESIAN_POINT('Ctrl Pts',(-43.1934081689503,58.5202030209667,12.));
#94100=CARTESIAN_POINT('Ctrl Pts',(-43.214901447157,58.5336381311911,0.));
#94101=CARTESIAN_POINT('Ctrl Pts',(-43.214901447157,58.5336381311911,12.));
#94102=CARTESIAN_POINT('Ctrl Pts',(-43.2364408740488,58.5470737099027,0.));
#94103=CARTESIAN_POINT('Ctrl Pts',(-43.2364408740488,58.5470737099027,12.));
#94104=CARTESIAN_POINT('Ctrl Pts',(-43.2580263899278,58.5605096558578,0.));
#94105=CARTESIAN_POINT('Ctrl Pts',(-43.2580263899278,58.5605096558578,12.));
#94106=CARTESIAN_POINT('Ctrl Pts',(-43.2796579352405,58.5739458682317,0.));
#94107=CARTESIAN_POINT('Ctrl Pts',(-43.2796579352405,58.5739458682317,12.));
#94108=CARTESIAN_POINT('Ctrl Pts',(-43.3013354505707,58.5873822466163,0.));
#94109=CARTESIAN_POINT('Ctrl Pts',(-43.3013354505707,58.5873822466163,12.));
#94110=CARTESIAN_POINT('Ctrl Pts',(-43.3230588766455,58.6008186910166,0.));
#94111=CARTESIAN_POINT('Ctrl Pts',(-43.3230588766455,58.6008186910166,12.));
#94112=CARTESIAN_POINT('Ctrl Pts',(-43.3448281543374,58.6142551018473,0.));
#94113=CARTESIAN_POINT('Ctrl Pts',(-43.3448281543374,58.6142551018473,12.));
#94114=CARTESIAN_POINT('Ctrl Pts',(-43.3666432246634,58.627691379929,0.));
#94115=CARTESIAN_POINT('Ctrl Pts',(-43.3666432246634,58.627691379929,12.));
#94116=CARTESIAN_POINT('Ctrl Pts',(-43.3885040287808,58.6411274264854,0.));
#94117=CARTESIAN_POINT('Ctrl Pts',(-43.3885040287808,58.6411274264854,12.));
#94118=CARTESIAN_POINT('Ctrl Pts',(-43.4104105079766,58.6545631431388,0.));
#94119=CARTESIAN_POINT('Ctrl Pts',(-43.4104105079766,58.6545631431388,12.));
#94120=CARTESIAN_POINT('Ctrl Pts',(-43.4323626036736,58.6679984319095,0.));
#94121=CARTESIAN_POINT('Ctrl Pts',(-43.4323626036736,58.6679984319095,12.));
#94122=CARTESIAN_POINT('Ctrl Pts',(-43.4543602574352,58.6814331952138,0.));
#94123=CARTESIAN_POINT('Ctrl Pts',(-43.4543602574352,58.6814331952138,12.));
#94124=CARTESIAN_POINT('Ctrl Pts',(-43.4764034109654,58.6948673358639,0.));
#94125=CARTESIAN_POINT('Ctrl Pts',(-43.4764034109654,58.6948673358639,12.));
#94126=CARTESIAN_POINT('Ctrl Pts',(-43.4984920061071,58.708300757066,0.));
#94127=CARTESIAN_POINT('Ctrl Pts',(-43.4984920061071,58.708300757066,12.));
#94128=CARTESIAN_POINT('Ctrl Pts',(-43.5206259848333,58.7217333624206,0.));
#94129=CARTESIAN_POINT('Ctrl Pts',(-43.5206259848333,58.7217333624206,12.));
#94130=CARTESIAN_POINT('Ctrl Pts',(-43.5428052892483,58.7351650559176,0.));
#94131=CARTESIAN_POINT('Ctrl Pts',(-43.5428052892483,58.7351650559176,12.));
#94132=CARTESIAN_POINT('Ctrl Pts',(-43.5650298615911,58.7485957419296,0.));
#94133=CARTESIAN_POINT('Ctrl Pts',(-43.5650298615911,58.7485957419296,12.));
#94134=CARTESIAN_POINT('Ctrl Pts',(-43.5872996442343,58.7620253252059,0.));
#94135=CARTESIAN_POINT('Ctrl Pts',(-43.5872996442343,58.7620253252059,12.));
#94136=CARTESIAN_POINT('Ctrl Pts',(-43.6096145796798,58.7754537108672,0.));
#94137=CARTESIAN_POINT('Ctrl Pts',(-43.6096145796798,58.7754537108672,12.));
#94138=CARTESIAN_POINT('Ctrl Pts',(-43.6319746105487,58.7888808043976,0.));
#94139=CARTESIAN_POINT('Ctrl Pts',(-43.6319746105487,58.7888808043976,12.));
#94140=CARTESIAN_POINT('Ctrl Pts',(-43.6543796795797,58.8023065116446,0.));
#94141=CARTESIAN_POINT('Ctrl Pts',(-43.6543796795797,58.8023065116446,12.));
#94142=CARTESIAN_POINT('Ctrl Pts',(-43.6768297296402,58.8157307388247,0.));
#94143=CARTESIAN_POINT('Ctrl Pts',(-43.6768297296402,58.8157307388247,12.));
#94144=CARTESIAN_POINT('Ctrl Pts',(-43.6993247037318,58.8291533925299,0.));
#94145=CARTESIAN_POINT('Ctrl Pts',(-43.6993247037318,58.8291533925299,12.));
#94146=CARTESIAN_POINT('Ctrl Pts',(-43.7218645449921,58.8425743797325,0.));
#94147=CARTESIAN_POINT('Ctrl Pts',(-43.7218645449921,58.8425743797325,12.));
#94148=CARTESIAN_POINT('Ctrl Pts',(-43.7444491966935,58.8559936077933,0.));
#94149=CARTESIAN_POINT('Ctrl Pts',(-43.7444491966935,58.8559936077933,12.));
#94150=CARTESIAN_POINT('Ctrl Pts',(-43.7670786022392,58.8694109844636,0.));
#94151=CARTESIAN_POINT('Ctrl Pts',(-43.7670786022392,58.8694109844636,12.));
#94152=CARTESIAN_POINT('Ctrl Pts',(-43.7897527051599,58.882826417861,0.));
#94153=CARTESIAN_POINT('Ctrl Pts',(-43.7897527051599,58.882826417861,12.));
#94154=CARTESIAN_POINT('Ctrl Pts',(-43.8124714491069,58.8962398164486,0.));
#94155=CARTESIAN_POINT('Ctrl Pts',(-43.8124714491069,58.8962398164486,12.));
#94156=CARTESIAN_POINT('Ctrl Pts',(-43.8352347778419,58.9096510890128,0.));
#94157=CARTESIAN_POINT('Ctrl Pts',(-43.8352347778419,58.9096510890128,12.));
#94158=CARTESIAN_POINT('Ctrl Pts',(-43.8580426352236,58.9230601446445,0.));
#94159=CARTESIAN_POINT('Ctrl Pts',(-43.8580426352236,58.9230601446445,12.));
#94160=CARTESIAN_POINT('Ctrl Pts',(-43.8808949651882,58.9364668927132,0.));
#94161=CARTESIAN_POINT('Ctrl Pts',(-43.8808949651882,58.9364668927132,12.));
#94162=CARTESIAN_POINT('Ctrl Pts',(-43.9037917117748,58.9498712429066,0.));
#94163=CARTESIAN_POINT('Ctrl Pts',(-43.9037917117748,58.9498712429066,12.));
#94164=CARTESIAN_POINT('Ctrl Pts',(-43.9267328191507,58.9632731052704,0.));
#94165=CARTESIAN_POINT('Ctrl Pts',(-43.9267328191507,58.9632731052704,12.));
#94166=CARTESIAN_POINT('Ctrl Pts',(-43.9497182316333,58.9766723902531,0.));
#94167=CARTESIAN_POINT('Ctrl Pts',(-43.9497182316333,58.9766723902531,12.));
#94168=CARTESIAN_POINT('Ctrl Pts',(-43.9727478937053,58.9900690087404,0.));
#94169=CARTESIAN_POINT('Ctrl Pts',(-43.9727478937053,58.9900690087404,12.));
#94170=CARTESIAN_POINT('Ctrl Pts',(-43.9958217500363,59.0034628721161,0.));
#94171=CARTESIAN_POINT('Ctrl Pts',(-43.9958217500363,59.0034628721161,12.));
#94172=CARTESIAN_POINT('Ctrl Pts',(-44.0189397454593,59.0168538922087,0.));
#94173=CARTESIAN_POINT('Ctrl Pts',(-44.0189397454593,59.0168538922087,12.));
#94174=CARTESIAN_POINT('Ctrl Pts',(-44.0421018249219,59.0302419811772,0.));
#94175=CARTESIAN_POINT('Ctrl Pts',(-44.0421018249219,59.0302419811772,12.));
#94176=CARTESIAN_POINT('Ctrl Pts',(-44.0653079334384,59.0436270514085,0.));
#94177=CARTESIAN_POINT('Ctrl Pts',(-44.0653079334384,59.0436270514085,12.));
#94178=CARTESIAN_POINT('Ctrl Pts',(-44.0885580160433,59.0570090154243,0.));
#94179=CARTESIAN_POINT('Ctrl Pts',(-44.0885580160433,59.0570090154243,12.));
#94180=CARTESIAN_POINT('Ctrl Pts',(-44.1118520177223,59.0703877857529,0.));
#94181=CARTESIAN_POINT('Ctrl Pts',(-44.1118520177223,59.0703877857529,12.));
#94182=CARTESIAN_POINT('Ctrl Pts',(-44.1351898834057,59.0837632749209,0.));
#94183=CARTESIAN_POINT('Ctrl Pts',(-44.1351898834057,59.0837632749209,12.));
#94184=CARTESIAN_POINT('Ctrl Pts',(-44.1585715581073,59.0971353957218,0.));
#94185=CARTESIAN_POINT('Ctrl Pts',(-44.1585715581073,59.0971353957218,12.));
#94186=CARTESIAN_POINT('Ctrl Pts',(-44.1819969870314,59.1105040614285,0.));
#94187=CARTESIAN_POINT('Ctrl Pts',(-44.1819969870314,59.1105040614285,12.));
#94188=CARTESIAN_POINT('Ctrl Pts',(-44.2054661156876,59.1238691860307,0.));
#94189=CARTESIAN_POINT('Ctrl Pts',(-44.2054661156876,59.1238691860307,12.));
#94190=CARTESIAN_POINT('Ctrl Pts',(-44.2289788899962,59.1372306844575,0.));
#94191=CARTESIAN_POINT('Ctrl Pts',(-44.2289788899962,59.1372306844575,12.));
#94192=CARTESIAN_POINT('Ctrl Pts',(-44.2525352563979,59.1505884728194,0.));
#94193=CARTESIAN_POINT('Ctrl Pts',(-44.2525352563979,59.1505884728194,12.));
#94194=CARTESIAN_POINT('Ctrl Pts',(-44.2761351616027,59.1639424678766,0.));
#94195=CARTESIAN_POINT('Ctrl Pts',(-44.2761351616027,59.1639424678766,12.));
#94196=CARTESIAN_POINT('Ctrl Pts',(-44.2997785523413,59.1772925865191,0.));
#94197=CARTESIAN_POINT('Ctrl Pts',(-44.2997785523413,59.1772925865191,12.));
#94198=CARTESIAN_POINT('Ctrl Pts',(-44.3234653750877,59.1906387451971,0.));
#94199=CARTESIAN_POINT('Ctrl Pts',(-44.3234653750877,59.1906387451971,12.));
#94200=CARTESIAN_POINT('Ctrl Pts',(-44.3471955758412,59.2039808594765,0.));
#94201=CARTESIAN_POINT('Ctrl Pts',(-44.3471955758412,59.2039808594765,12.));
#94202=CARTESIAN_POINT('Ctrl Pts',(-44.3709690997495,59.217318843283,0.));
#94203=CARTESIAN_POINT('Ctrl Pts',(-44.3709690997495,59.217318843283,12.));
#94204=CARTESIAN_POINT('Ctrl Pts',(-44.394785891411,59.2306526095175,0.));
#94205=CARTESIAN_POINT('Ctrl Pts',(-44.394785891411,59.2306526095175,12.));
#94206=CARTESIAN_POINT('Ctrl Pts',(-44.4186458955486,59.2439820714231,0.));
#94207=CARTESIAN_POINT('Ctrl Pts',(-44.4186458955486,59.2439820714231,12.));
#94208=CARTESIAN_POINT('Ctrl Pts',(-44.4425490575932,59.2573071437801,0.));
#94209=CARTESIAN_POINT('Ctrl Pts',(-44.4425490575932,59.2573071437801,12.));
#94210=CARTESIAN_POINT('Ctrl Pts',(-44.4664953242373,59.2706277440438,0.));
#94211=CARTESIAN_POINT('Ctrl Pts',(-44.4664953242373,59.2706277440438,12.));
#94212=CARTESIAN_POINT('Ctrl Pts',(-44.490484644147,59.2839437938187,0.));
#94213=CARTESIAN_POINT('Ctrl Pts',(-44.490484644147,59.2839437938187,12.));
#94214=CARTESIAN_POINT('Ctrl Pts',(-44.514516968128,59.2972552192072,0.));
#94215=CARTESIAN_POINT('Ctrl Pts',(-44.514516968128,59.2972552192072,12.));
#94216=CARTESIAN_POINT('Ctrl Pts',(-44.5385922475494,59.3105619475512,0.));
#94217=CARTESIAN_POINT('Ctrl Pts',(-44.5385922475494,59.3105619475512,12.));
#94218=CARTESIAN_POINT('Ctrl Pts',(-44.5627104330956,59.3238639048618,0.));
#94219=CARTESIAN_POINT('Ctrl Pts',(-44.5627104330956,59.3238639048618,12.));
#94220=CARTESIAN_POINT('Ctrl Pts',(-44.5868714733219,59.3371610128494,0.));
#94221=CARTESIAN_POINT('Ctrl Pts',(-44.5868714733219,59.3371610128494,12.));
#94222=CARTESIAN_POINT('Ctrl Pts',(-44.6110753134333,59.3504531864223,0.));
#94223=CARTESIAN_POINT('Ctrl Pts',(-44.6110753134333,59.3504531864223,12.));
#94224=CARTESIAN_POINT('Ctrl Pts',(-44.6353218935813,59.3637403301959,0.));
#94225=CARTESIAN_POINT('Ctrl Pts',(-44.6353218935813,59.3637403301959,12.));
#94226=CARTESIAN_POINT('Ctrl Pts',(-44.659611151286,59.3770223435405,0.));
#94227=CARTESIAN_POINT('Ctrl Pts',(-44.659611151286,59.3770223435405,12.));
#94228=CARTESIAN_POINT('Ctrl Pts',(-44.6839430244375,59.3902991268094,0.));
#94229=CARTESIAN_POINT('Ctrl Pts',(-44.6839430244375,59.3902991268094,12.));
#94230=CARTESIAN_POINT('Ctrl Pts',(-44.708317454179,59.403570587392,0.));
#94231=CARTESIAN_POINT('Ctrl Pts',(-44.708317454179,59.403570587392,12.));
#94232=CARTESIAN_POINT('Ctrl Pts',(-44.7327343876333,59.4168366453047,0.));
#94233=CARTESIAN_POINT('Ctrl Pts',(-44.7327343876333,59.4168366453047,12.));
#94234=CARTESIAN_POINT('Ctrl Pts',(-44.7571937811872,59.4300972402943,0.));
#94235=CARTESIAN_POINT('Ctrl Pts',(-44.7571937811872,59.4300972402943,12.));
#94236=CARTESIAN_POINT('Ctrl Pts',(-44.7816956017126,59.4433523334651,0.));
#94237=CARTESIAN_POINT('Ctrl Pts',(-44.7816956017126,59.4433523334651,12.));
#94238=CARTESIAN_POINT('Ctrl Pts',(-44.8062398250937,59.4566019017674,0.));
#94239=CARTESIAN_POINT('Ctrl Pts',(-44.8062398250937,59.4566019017674,12.));
#94240=CARTESIAN_POINT('Ctrl Pts',(-44.8259091133624,59.4671971277837,0.));
#94241=CARTESIAN_POINT('Ctrl Pts',(-44.8259091133624,59.4671971277837,12.));
#94242=CARTESIAN_POINT('Ctrl Pts',(-44.8406801497506,59.475141054744,0.));
#94243=CARTESIAN_POINT('Ctrl Pts',(-44.8406801497506,59.475141054744,12.));
#94244=CARTESIAN_POINT('Ctrl Pts',(-44.8505359826374,59.4804358982977,0.));
#94245=CARTESIAN_POINT('Ctrl Pts',(-44.8505359826374,59.4804358982977,12.));
#94246=CARTESIAN_POINT('Ctrl Pts',(-44.8554660179045,59.483083043136,0.));
#94247=CARTESIAN_POINT('Ctrl Pts',(-44.8554660179045,59.483083043136,12.));
#94248=CARTESIAN_POINT('',(-40.8467768343956,56.8466430164621,0.));
#94249=CARTESIAN_POINT('Ctrl Pts',(-40.8467768343956,56.8466430164621,0.));
#94250=CARTESIAN_POINT('Ctrl Pts',(-40.8497761671036,56.8491101022591,0.));
#94251=CARTESIAN_POINT('Ctrl Pts',(-40.8557803680277,56.8540460739472,0.));
#94252=CARTESIAN_POINT('Ctrl Pts',(-40.864803275942,56.8614554317668,0.));
#94253=CARTESIAN_POINT('Ctrl Pts',(-40.8768670342052,56.8713453764905,0.));
#94254=CARTESIAN_POINT('Ctrl Pts',(-40.8920020903293,56.8837257978343,0.));
#94255=CARTESIAN_POINT('Ctrl Pts',(-40.9071924937508,56.8961241708861,0.));
#94256=CARTESIAN_POINT('Ctrl Pts',(-40.9224382132427,56.9085404164502,0.));
#94257=CARTESIAN_POINT('Ctrl Pts',(-40.9377391857128,56.9209743960992,0.));
#94258=CARTESIAN_POINT('Ctrl Pts',(-40.9530953165031,56.9334259140049,0.));
#94259=CARTESIAN_POINT('Ctrl Pts',(-40.9685064933074,56.9458947422608,0.));
#94260=CARTESIAN_POINT('Ctrl Pts',(-40.9839725967121,56.9583806404069,0.));
#94261=CARTESIAN_POINT('Ctrl Pts',(-40.9994935117276,56.9708833766137,0.));
#94262=CARTESIAN_POINT('Ctrl Pts',(-41.0150691398947,56.9834027500117,0.));
#94263=CARTESIAN_POINT('Ctrl Pts',(-41.0306993953988,56.995938583472,0.));
#94264=CARTESIAN_POINT('Ctrl Pts',(-41.0463841993608,57.008490713042,0.));
#94265=CARTESIAN_POINT('Ctrl Pts',(-41.0621234751007,57.0210589791788,0.));
#94266=CARTESIAN_POINT('Ctrl Pts',(-41.0779171422438,57.0336432158536,0.));
#94267=CARTESIAN_POINT('Ctrl Pts',(-41.0937651137549,57.046243245068,0.));
#94268=CARTESIAN_POINT('Ctrl Pts',(-41.1096672990148,57.0588588825298,0.));
#94269=CARTESIAN_POINT('Ctrl Pts',(-41.1256236057442,57.0714899412099,0.));
#94270=CARTESIAN_POINT('Ctrl Pts',(-41.1416339422117,57.084136235426,0.));
#94271=CARTESIAN_POINT('Ctrl Pts',(-41.1576982197374,57.0967975854874,0.));
#94272=CARTESIAN_POINT('Ctrl Pts',(-41.1738163525901,57.1094738174957,0.));
#94273=CARTESIAN_POINT('Ctrl Pts',(-41.1899882567923,57.1221647611207,0.));
#94274=CARTESIAN_POINT('Ctrl Pts',(-41.2062138492915,57.1348702480647,0.));
#94275=CARTESIAN_POINT('Ctrl Pts',(-41.222493046943,57.147590110182,0.));
#94276=CARTESIAN_POINT('Ctrl Pts',(-41.2388257656559,57.1603241779077,0.));
#94277=CARTESIAN_POINT('Ctrl Pts',(-41.2552119208465,57.17307228108,0.));
#94278=CARTESIAN_POINT('Ctrl Pts',(-41.2716514278276,57.1858342496538,0.));
#94279=CARTESIAN_POINT('Ctrl Pts',(-41.2881442021863,57.1986099143983,0.));
#94280=CARTESIAN_POINT('Ctrl Pts',(-41.3046901602293,57.2113991077302,0.));
#94281=CARTESIAN_POINT('Ctrl Pts',(-41.321289219149,57.2242016640198,0.));
#94282=CARTESIAN_POINT('Ctrl Pts',(-41.3379412967875,57.2370174191401,0.));
#94283=CARTESIAN_POINT('Ctrl Pts',(-41.3546463114885,57.2498462101879,0.));
#94284=CARTESIAN_POINT('Ctrl Pts',(-41.3714041819223,57.2626878751596,0.));
#94285=CARTESIAN_POINT('Ctrl Pts',(-41.3882148268813,57.2755422525844,0.));
#94286=CARTESIAN_POINT('Ctrl Pts',(-41.4050781652938,57.2884091815406,0.));
#94287=CARTESIAN_POINT('Ctrl Pts',(-41.4219941163163,57.3012885018151,0.));
#94288=CARTESIAN_POINT('Ctrl Pts',(-41.4389625993948,57.3141800540137,0.));
#94289=CARTESIAN_POINT('Ctrl Pts',(-41.4559835343328,57.3270836796911,0.));
#94290=CARTESIAN_POINT('Ctrl Pts',(-41.4730568413518,57.3399992214717,0.));
#94291=CARTESIAN_POINT('Ctrl Pts',(-41.4901824410636,57.3529265229835,0.));
#94292=CARTESIAN_POINT('Ctrl Pts',(-41.5073602544396,57.3658654287937,0.));
#94293=CARTESIAN_POINT('Ctrl Pts',(-41.524590202777,57.3788157843454,0.));
#94294=CARTESIAN_POINT('Ctrl Pts',(-41.5418722076572,57.3917774358863,0.));
#94295=CARTESIAN_POINT('Ctrl Pts',(-41.5592061909176,57.4047502304231,0.));
#94296=CARTESIAN_POINT('Ctrl Pts',(-41.5765920746777,57.4177340157508,0.));
#94297=CARTESIAN_POINT('Ctrl Pts',(-41.5940297813477,57.4307286404662,0.));
#94298=CARTESIAN_POINT('Ctrl Pts',(-41.6115192336388,57.4437339539841,0.));
#94299=CARTESIAN_POINT('Ctrl Pts',(-41.6290603545666,57.4567498065562,0.));
#94300=CARTESIAN_POINT('Ctrl Pts',(-41.6466530674514,57.4697760492683,0.));
#94301=CARTESIAN_POINT('Ctrl Pts',(-41.6642972959165,57.4828125340218,0.));
#94302=CARTESIAN_POINT('Ctrl Pts',(-41.6819929638797,57.4958591135165,0.));
#94303=CARTESIAN_POINT('Ctrl Pts',(-41.6997399955447,57.5089156412343,0.));
#94304=CARTESIAN_POINT('Ctrl Pts',(-41.7175383153821,57.5219819714171,0.));
#94305=CARTESIAN_POINT('Ctrl Pts',(-41.7353878481336,57.5350579590649,0.));
#94306=CARTESIAN_POINT('Ctrl Pts',(-41.7532885188174,57.5481434599335,0.));
#94307=CARTESIAN_POINT('Ctrl Pts',(-41.7712402527273,57.561238330532,0.));
#94308=CARTESIAN_POINT('Ctrl Pts',(-41.7892429754297,57.5743424281205,0.));
#94309=CARTESIAN_POINT('Ctrl Pts',(-41.8072966127558,57.5874556107056,0.));
#94310=CARTESIAN_POINT('Ctrl Pts',(-41.8254010908051,57.6005777370349,0.));
#94311=CARTESIAN_POINT('Ctrl Pts',(-41.8435563359456,57.6137086665882,0.));
#94312=CARTESIAN_POINT('Ctrl Pts',(-41.8617622748108,57.6268482595702,0.));
#94313=CARTESIAN_POINT('Ctrl Pts',(-41.8800188342908,57.6399963769003,0.));
#94314=CARTESIAN_POINT('Ctrl Pts',(-41.8983259415244,57.6531528802059,0.));
#94315=CARTESIAN_POINT('Ctrl Pts',(-41.9166835239046,57.6663176318176,0.));
#94316=CARTESIAN_POINT('Ctrl Pts',(-41.9350915090791,57.6794904947641,0.));
#94317=CARTESIAN_POINT('Ctrl Pts',(-41.9535498249489,57.6926713327674,0.));
#94318=CARTESIAN_POINT('Ctrl Pts',(-41.9720583996601,57.7058600102365,0.));
#94319=CARTESIAN_POINT('Ctrl Pts',(-41.9906171615974,57.7190563922614,0.));
#94320=CARTESIAN_POINT('Ctrl Pts',(-42.0092260393911,57.7322603446086,0.));
#94321=CARTESIAN_POINT('Ctrl Pts',(-42.0278849619156,57.7454717337151,0.));
#94322=CARTESIAN_POINT('Ctrl Pts',(-42.0465938582877,57.7586904266828,0.));
#94323=CARTESIAN_POINT('Ctrl Pts',(-42.0653526578571,57.7719162912721,0.));
#94324=CARTESIAN_POINT('Ctrl Pts',(-42.0841612902018,57.7851491958954,0.));
#94325=CARTESIAN_POINT('Ctrl Pts',(-42.1030196851344,57.798389009613,0.));
#94326=CARTESIAN_POINT('Ctrl Pts',(-42.121927772701,57.8116356021274,0.));
#94327=CARTESIAN_POINT('Ctrl Pts',(-42.1408854831791,57.8248888437787,0.));
#94328=CARTESIAN_POINT('Ctrl Pts',(-42.1598927470671,57.8381486055376,0.));
#94329=CARTESIAN_POINT('Ctrl Pts',(-42.1789494950824,57.8514147590012,0.));
#94330=CARTESIAN_POINT('Ctrl Pts',(-42.1980556581688,57.86468717639,0.));
#94331=CARTESIAN_POINT('Ctrl Pts',(-42.2172111674945,57.8779657305423,0.));
#94332=CARTESIAN_POINT('Ctrl Pts',(-42.2364159544492,57.8912502949084,0.));
#94333=CARTESIAN_POINT('Ctrl Pts',(-42.2556699506332,57.9045407435447,0.));
#94334=CARTESIAN_POINT('Ctrl Pts',(-42.274973087857,57.9178369511084,0.));
#94335=CARTESIAN_POINT('Ctrl Pts',(-42.2943252981471,57.9311387928541,0.));
#94336=CARTESIAN_POINT('Ctrl Pts',(-42.3137265137446,57.9444461446292,0.));
#94337=CARTESIAN_POINT('Ctrl Pts',(-42.3331766671028,57.9577588828693,0.));
#94338=CARTESIAN_POINT('Ctrl Pts',(-42.3526756908764,57.9710768845923,0.));
#94339=CARTESIAN_POINT('Ctrl Pts',(-42.3722235179216,57.9844000273936,0.));
#94340=CARTESIAN_POINT('Ctrl Pts',(-42.3918200813024,57.9977281894437,0.));
#94341=CARTESIAN_POINT('Ctrl Pts',(-42.4114653142891,58.011061249483,0.));
#94342=CARTESIAN_POINT('Ctrl Pts',(-42.4311591503551,58.0243990868175,0.));
#94343=CARTESIAN_POINT('Ctrl Pts',(-42.4509015231667,58.0377415813132,0.));
#94344=CARTESIAN_POINT('Ctrl Pts',(-42.4706923665838,58.0510886133917,0.));
#94345=CARTESIAN_POINT('Ctrl Pts',(-42.4905316146649,58.064440064027,0.));
#94346=CARTESIAN_POINT('Ctrl Pts',(-42.5104192016664,58.0777958147404,0.));
#94347=CARTESIAN_POINT('Ctrl Pts',(-42.5303550620388,58.0911557475967,0.));
#94348=CARTESIAN_POINT('Ctrl Pts',(-42.5503391304182,58.1045197452003,0.));
#94349=CARTESIAN_POINT('Ctrl Pts',(-42.5703713416263,58.1178876906905,0.));
#94350=CARTESIAN_POINT('Ctrl Pts',(-42.5904516306759,58.1312594677383,0.));
#94351=CARTESIAN_POINT('Ctrl Pts',(-42.6105799327697,58.1446349605419,0.));
#94352=CARTESIAN_POINT('Ctrl Pts',(-42.6307561832977,58.158014053823,0.));
#94353=CARTESIAN_POINT('Ctrl Pts',(-42.6509803178269,58.1713966328217,0.));
#94354=CARTESIAN_POINT('Ctrl Pts',(-42.6712522721021,58.1847825832932,0.));
#94355=CARTESIAN_POINT('Ctrl Pts',(-42.6915719820516,58.1981717915043,0.));
#94356=CARTESIAN_POINT('Ctrl Pts',(-42.7119393837866,58.2115641442302,0.));
#94357=CARTESIAN_POINT('Ctrl Pts',(-42.7323544135983,58.2249595287497,0.));
#94358=CARTESIAN_POINT('Ctrl Pts',(-42.7528170079482,58.238357832842,0.));
#94359=CARTESIAN_POINT('Ctrl Pts',(-42.7733271034678,58.2517589447818,0.));
#94360=CARTESIAN_POINT('Ctrl Pts',(-42.7938846369651,58.2651627533368,0.));
#94361=CARTESIAN_POINT('Ctrl Pts',(-42.8144895454234,58.278569147764,0.));
#94362=CARTESIAN_POINT('Ctrl Pts',(-42.8351417659998,58.2919780178063,0.));
#94363=CARTESIAN_POINT('Ctrl Pts',(-42.8558412360154,58.305389253689,0.));
#94364=CARTESIAN_POINT('Ctrl Pts',(-42.8765878929545,58.3188027461158,0.));
#94365=CARTESIAN_POINT('Ctrl Pts',(-42.8973816744703,58.3322183862647,0.));
#94366=CARTESIAN_POINT('Ctrl Pts',(-42.9182225183851,58.3456360657861,0.));
#94367=CARTESIAN_POINT('Ctrl Pts',(-42.9391103626881,58.3590556767981,0.));
#94368=CARTESIAN_POINT('Ctrl Pts',(-42.9600451455267,58.3724771118835,0.));
#94369=CARTESIAN_POINT('Ctrl Pts',(-42.9810268052043,58.3859002640871,0.));
#94370=CARTESIAN_POINT('Ctrl Pts',(-43.0020552801869,58.3993250269115,0.));
#94371=CARTESIAN_POINT('Ctrl Pts',(-43.0231305091032,58.4127512943144,0.));
#94372=CARTESIAN_POINT('Ctrl Pts',(-43.0442524307432,58.4261789607055,0.));
#94373=CARTESIAN_POINT('Ctrl Pts',(-43.0654209840502,58.4396079209438,0.));
#94374=CARTESIAN_POINT('Ctrl Pts',(-43.0866361081166,58.4530380703335,0.));
#94375=CARTESIAN_POINT('Ctrl Pts',(-43.1078977421908,58.4664693046206,0.));
#94376=CARTESIAN_POINT('Ctrl Pts',(-43.1292058256774,58.4799015199904,0.));
#94377=CARTESIAN_POINT('Ctrl Pts',(-43.1505602981366,58.4933346130638,0.));
#94378=CARTESIAN_POINT('Ctrl Pts',(-43.1719610992771,58.5067684808946,0.));
#94379=CARTESIAN_POINT('Ctrl Pts',(-43.1934081689503,58.5202030209667,0.));
#94380=CARTESIAN_POINT('Ctrl Pts',(-43.214901447157,58.5336381311911,0.));
#94381=CARTESIAN_POINT('Ctrl Pts',(-43.2364408740488,58.5470737099027,0.));
#94382=CARTESIAN_POINT('Ctrl Pts',(-43.2580263899278,58.5605096558578,0.));
#94383=CARTESIAN_POINT('Ctrl Pts',(-43.2796579352405,58.5739458682317,0.));
#94384=CARTESIAN_POINT('Ctrl Pts',(-43.3013354505707,58.5873822466163,0.));
#94385=CARTESIAN_POINT('Ctrl Pts',(-43.3230588766455,58.6008186910166,0.));
#94386=CARTESIAN_POINT('Ctrl Pts',(-43.3448281543374,58.6142551018473,0.));
#94387=CARTESIAN_POINT('Ctrl Pts',(-43.3666432246634,58.627691379929,0.));
#94388=CARTESIAN_POINT('Ctrl Pts',(-43.3885040287808,58.6411274264854,0.));
#94389=CARTESIAN_POINT('Ctrl Pts',(-43.4104105079766,58.6545631431388,0.));
#94390=CARTESIAN_POINT('Ctrl Pts',(-43.4323626036736,58.6679984319095,0.));
#94391=CARTESIAN_POINT('Ctrl Pts',(-43.4543602574352,58.6814331952138,0.));
#94392=CARTESIAN_POINT('Ctrl Pts',(-43.4764034109654,58.6948673358639,0.));
#94393=CARTESIAN_POINT('Ctrl Pts',(-43.4984920061071,58.708300757066,0.));
#94394=CARTESIAN_POINT('Ctrl Pts',(-43.5206259848333,58.7217333624206,0.));
#94395=CARTESIAN_POINT('Ctrl Pts',(-43.5428052892483,58.7351650559176,0.));
#94396=CARTESIAN_POINT('Ctrl Pts',(-43.5650298615911,58.7485957419296,0.));
#94397=CARTESIAN_POINT('Ctrl Pts',(-43.5872996442343,58.7620253252059,0.));
#94398=CARTESIAN_POINT('Ctrl Pts',(-43.6096145796798,58.7754537108672,0.));
#94399=CARTESIAN_POINT('Ctrl Pts',(-43.6319746105487,58.7888808043976,0.));
#94400=CARTESIAN_POINT('Ctrl Pts',(-43.6543796795797,58.8023065116446,0.));
#94401=CARTESIAN_POINT('Ctrl Pts',(-43.6768297296402,58.8157307388247,0.));
#94402=CARTESIAN_POINT('Ctrl Pts',(-43.6993247037318,58.8291533925299,0.));
#94403=CARTESIAN_POINT('Ctrl Pts',(-43.7218645449921,58.8425743797325,0.));
#94404=CARTESIAN_POINT('Ctrl Pts',(-43.7444491966935,58.8559936077933,0.));
#94405=CARTESIAN_POINT('Ctrl Pts',(-43.7670786022392,58.8694109844636,0.));
#94406=CARTESIAN_POINT('Ctrl Pts',(-43.7897527051599,58.882826417861,0.));
#94407=CARTESIAN_POINT('Ctrl Pts',(-43.8124714491069,58.8962398164486,0.));
#94408=CARTESIAN_POINT('Ctrl Pts',(-43.8352347778419,58.9096510890128,0.));
#94409=CARTESIAN_POINT('Ctrl Pts',(-43.8580426352236,58.9230601446445,0.));
#94410=CARTESIAN_POINT('Ctrl Pts',(-43.8808949651882,58.9364668927132,0.));
#94411=CARTESIAN_POINT('Ctrl Pts',(-43.9037917117748,58.9498712429066,0.));
#94412=CARTESIAN_POINT('Ctrl Pts',(-43.9267328191507,58.9632731052704,0.));
#94413=CARTESIAN_POINT('Ctrl Pts',(-43.9497182316333,58.9766723902531,0.));
#94414=CARTESIAN_POINT('Ctrl Pts',(-43.9727478937053,58.9900690087404,0.));
#94415=CARTESIAN_POINT('Ctrl Pts',(-43.9958217500363,59.0034628721161,0.));
#94416=CARTESIAN_POINT('Ctrl Pts',(-44.0189397454593,59.0168538922087,0.));
#94417=CARTESIAN_POINT('Ctrl Pts',(-44.0421018249219,59.0302419811772,0.));
#94418=CARTESIAN_POINT('Ctrl Pts',(-44.0653079334384,59.0436270514085,0.));
#94419=CARTESIAN_POINT('Ctrl Pts',(-44.0885580160433,59.0570090154243,0.));
#94420=CARTESIAN_POINT('Ctrl Pts',(-44.1118520177223,59.0703877857529,0.));
#94421=CARTESIAN_POINT('Ctrl Pts',(-44.1351898834057,59.0837632749209,0.));
#94422=CARTESIAN_POINT('Ctrl Pts',(-44.1585715581073,59.0971353957218,0.));
#94423=CARTESIAN_POINT('Ctrl Pts',(-44.1819969870314,59.1105040614285,0.));
#94424=CARTESIAN_POINT('Ctrl Pts',(-44.2054661156876,59.1238691860307,0.));
#94425=CARTESIAN_POINT('Ctrl Pts',(-44.2289788899962,59.1372306844575,0.));
#94426=CARTESIAN_POINT('Ctrl Pts',(-44.2525352563979,59.1505884728194,0.));
#94427=CARTESIAN_POINT('Ctrl Pts',(-44.2761351616027,59.1639424678766,0.));
#94428=CARTESIAN_POINT('Ctrl Pts',(-44.2997785523413,59.1772925865191,0.));
#94429=CARTESIAN_POINT('Ctrl Pts',(-44.3234653750877,59.1906387451971,0.));
#94430=CARTESIAN_POINT('Ctrl Pts',(-44.3471955758412,59.2039808594765,0.));
#94431=CARTESIAN_POINT('Ctrl Pts',(-44.3709690997495,59.217318843283,0.));
#94432=CARTESIAN_POINT('Ctrl Pts',(-44.394785891411,59.2306526095175,0.));
#94433=CARTESIAN_POINT('Ctrl Pts',(-44.4186458955486,59.2439820714231,0.));
#94434=CARTESIAN_POINT('Ctrl Pts',(-44.4425490575932,59.2573071437801,0.));
#94435=CARTESIAN_POINT('Ctrl Pts',(-44.4664953242373,59.2706277440438,0.));
#94436=CARTESIAN_POINT('Ctrl Pts',(-44.490484644147,59.2839437938187,0.));
#94437=CARTESIAN_POINT('Ctrl Pts',(-44.514516968128,59.2972552192072,0.));
#94438=CARTESIAN_POINT('Ctrl Pts',(-44.5351541478336,59.3086616639392,0.));
#94439=CARTESIAN_POINT('Ctrl Pts',(-44.5509994357954,59.317404187219,0.));
#94440=CARTESIAN_POINT('Ctrl Pts',(-44.5620338188485,59.3234848865278,0.));
#94441=CARTESIAN_POINT('Ctrl Pts',(-44.5682447395713,59.3269051738222,0.));
#94442=CARTESIAN_POINT('Ctrl Pts',(-44.569626075742,59.3276657444158,0.));
#94443=CARTESIAN_POINT('',(-40.8467768343956,56.8466430164621,12.));
#94444=CARTESIAN_POINT('',(-40.8467768343956,56.8466430164621,0.));
#94445=CARTESIAN_POINT('Ctrl Pts',(-44.569626075742,59.3276657444158,12.));
#94446=CARTESIAN_POINT('Ctrl Pts',(-44.5682447395712,59.3269051738222,12.));
#94447=CARTESIAN_POINT('Ctrl Pts',(-44.5620338188485,59.3234848865278,12.));
#94448=CARTESIAN_POINT('Ctrl Pts',(-44.5509994357953,59.317404187219,12.));
#94449=CARTESIAN_POINT('Ctrl Pts',(-44.5351541478336,59.3086616639392,12.));
#94450=CARTESIAN_POINT('Ctrl Pts',(-44.514516968128,59.2972552192072,12.));
#94451=CARTESIAN_POINT('Ctrl Pts',(-44.490484644147,59.2839437938187,12.));
#94452=CARTESIAN_POINT('Ctrl Pts',(-44.4664953242373,59.2706277440438,12.));
#94453=CARTESIAN_POINT('Ctrl Pts',(-44.4425490575932,59.2573071437801,12.));
#94454=CARTESIAN_POINT('Ctrl Pts',(-44.4186458955486,59.2439820714231,12.));
#94455=CARTESIAN_POINT('Ctrl Pts',(-44.394785891411,59.2306526095175,12.));
#94456=CARTESIAN_POINT('Ctrl Pts',(-44.3709690997495,59.217318843283,12.));
#94457=CARTESIAN_POINT('Ctrl Pts',(-44.3471955758412,59.2039808594765,12.));
#94458=CARTESIAN_POINT('Ctrl Pts',(-44.3234653750877,59.1906387451971,12.));
#94459=CARTESIAN_POINT('Ctrl Pts',(-44.2997785523413,59.1772925865191,12.));
#94460=CARTESIAN_POINT('Ctrl Pts',(-44.2761351616027,59.1639424678766,12.));
#94461=CARTESIAN_POINT('Ctrl Pts',(-44.2525352563979,59.1505884728194,12.));
#94462=CARTESIAN_POINT('Ctrl Pts',(-44.2289788899962,59.1372306844575,12.));
#94463=CARTESIAN_POINT('Ctrl Pts',(-44.2054661156876,59.1238691860307,12.));
#94464=CARTESIAN_POINT('Ctrl Pts',(-44.1819969870314,59.1105040614285,12.));
#94465=CARTESIAN_POINT('Ctrl Pts',(-44.1585715581073,59.0971353957218,12.));
#94466=CARTESIAN_POINT('Ctrl Pts',(-44.1351898834057,59.0837632749209,12.));
#94467=CARTESIAN_POINT('Ctrl Pts',(-44.1118520177223,59.0703877857529,12.));
#94468=CARTESIAN_POINT('Ctrl Pts',(-44.0885580160433,59.0570090154243,12.));
#94469=CARTESIAN_POINT('Ctrl Pts',(-44.0653079334384,59.0436270514085,12.));
#94470=CARTESIAN_POINT('Ctrl Pts',(-44.0421018249219,59.0302419811772,12.));
#94471=CARTESIAN_POINT('Ctrl Pts',(-44.0189397454593,59.0168538922087,12.));
#94472=CARTESIAN_POINT('Ctrl Pts',(-43.9958217500363,59.0034628721161,12.));
#94473=CARTESIAN_POINT('Ctrl Pts',(-43.9727478937053,58.9900690087404,12.));
#94474=CARTESIAN_POINT('Ctrl Pts',(-43.9497182316333,58.9766723902531,12.));
#94475=CARTESIAN_POINT('Ctrl Pts',(-43.9267328191507,58.9632731052704,12.));
#94476=CARTESIAN_POINT('Ctrl Pts',(-43.9037917117748,58.9498712429066,12.));
#94477=CARTESIAN_POINT('Ctrl Pts',(-43.8808949651882,58.9364668927132,12.));
#94478=CARTESIAN_POINT('Ctrl Pts',(-43.8580426352236,58.9230601446445,12.));
#94479=CARTESIAN_POINT('Ctrl Pts',(-43.8352347778419,58.9096510890128,12.));
#94480=CARTESIAN_POINT('Ctrl Pts',(-43.8124714491069,58.8962398164486,12.));
#94481=CARTESIAN_POINT('Ctrl Pts',(-43.7897527051599,58.882826417861,12.));
#94482=CARTESIAN_POINT('Ctrl Pts',(-43.7670786022392,58.8694109844636,12.));
#94483=CARTESIAN_POINT('Ctrl Pts',(-43.7444491966935,58.8559936077933,12.));
#94484=CARTESIAN_POINT('Ctrl Pts',(-43.7218645449921,58.8425743797325,12.));
#94485=CARTESIAN_POINT('Ctrl Pts',(-43.6993247037318,58.8291533925299,12.));
#94486=CARTESIAN_POINT('Ctrl Pts',(-43.6768297296402,58.8157307388247,12.));
#94487=CARTESIAN_POINT('Ctrl Pts',(-43.6543796795797,58.8023065116446,12.));
#94488=CARTESIAN_POINT('Ctrl Pts',(-43.6319746105487,58.7888808043976,12.));
#94489=CARTESIAN_POINT('Ctrl Pts',(-43.6096145796798,58.7754537108672,12.));
#94490=CARTESIAN_POINT('Ctrl Pts',(-43.5872996442343,58.7620253252059,12.));
#94491=CARTESIAN_POINT('Ctrl Pts',(-43.5650298615911,58.7485957419296,12.));
#94492=CARTESIAN_POINT('Ctrl Pts',(-43.5428052892483,58.7351650559176,12.));
#94493=CARTESIAN_POINT('Ctrl Pts',(-43.5206259848333,58.7217333624206,12.));
#94494=CARTESIAN_POINT('Ctrl Pts',(-43.4984920061071,58.708300757066,12.));
#94495=CARTESIAN_POINT('Ctrl Pts',(-43.4764034109654,58.6948673358639,12.));
#94496=CARTESIAN_POINT('Ctrl Pts',(-43.4543602574352,58.6814331952138,12.));
#94497=CARTESIAN_POINT('Ctrl Pts',(-43.4323626036736,58.6679984319095,12.));
#94498=CARTESIAN_POINT('Ctrl Pts',(-43.4104105079766,58.6545631431388,12.));
#94499=CARTESIAN_POINT('Ctrl Pts',(-43.3885040287808,58.6411274264854,12.));
#94500=CARTESIAN_POINT('Ctrl Pts',(-43.3666432246634,58.627691379929,12.));
#94501=CARTESIAN_POINT('Ctrl Pts',(-43.3448281543374,58.6142551018473,12.));
#94502=CARTESIAN_POINT('Ctrl Pts',(-43.3230588766455,58.6008186910166,12.));
#94503=CARTESIAN_POINT('Ctrl Pts',(-43.3013354505707,58.5873822466163,12.));
#94504=CARTESIAN_POINT('Ctrl Pts',(-43.2796579352405,58.5739458682317,12.));
#94505=CARTESIAN_POINT('Ctrl Pts',(-43.2580263899278,58.5605096558578,12.));
#94506=CARTESIAN_POINT('Ctrl Pts',(-43.2364408740488,58.5470737099027,12.));
#94507=CARTESIAN_POINT('Ctrl Pts',(-43.214901447157,58.5336381311911,12.));
#94508=CARTESIAN_POINT('Ctrl Pts',(-43.1934081689503,58.5202030209667,12.));
#94509=CARTESIAN_POINT('Ctrl Pts',(-43.1719610992771,58.5067684808946,12.));
#94510=CARTESIAN_POINT('Ctrl Pts',(-43.1505602981366,58.4933346130638,12.));
#94511=CARTESIAN_POINT('Ctrl Pts',(-43.1292058256774,58.4799015199904,12.));
#94512=CARTESIAN_POINT('Ctrl Pts',(-43.1078977421908,58.4664693046206,12.));
#94513=CARTESIAN_POINT('Ctrl Pts',(-43.0866361081166,58.4530380703335,12.));
#94514=CARTESIAN_POINT('Ctrl Pts',(-43.0654209840502,58.4396079209438,12.));
#94515=CARTESIAN_POINT('Ctrl Pts',(-43.0442524307432,58.4261789607055,12.));
#94516=CARTESIAN_POINT('Ctrl Pts',(-43.0231305091032,58.4127512943144,12.));
#94517=CARTESIAN_POINT('Ctrl Pts',(-43.0020552801869,58.3993250269115,12.));
#94518=CARTESIAN_POINT('Ctrl Pts',(-42.9810268052043,58.3859002640871,12.));
#94519=CARTESIAN_POINT('Ctrl Pts',(-42.9600451455267,58.3724771118835,12.));
#94520=CARTESIAN_POINT('Ctrl Pts',(-42.9391103626881,58.3590556767981,12.));
#94521=CARTESIAN_POINT('Ctrl Pts',(-42.9182225183851,58.3456360657861,12.));
#94522=CARTESIAN_POINT('Ctrl Pts',(-42.8973816744703,58.3322183862647,12.));
#94523=CARTESIAN_POINT('Ctrl Pts',(-42.8765878929545,58.3188027461158,12.));
#94524=CARTESIAN_POINT('Ctrl Pts',(-42.8558412360154,58.305389253689,12.));
#94525=CARTESIAN_POINT('Ctrl Pts',(-42.8351417659998,58.2919780178063,12.));
#94526=CARTESIAN_POINT('Ctrl Pts',(-42.8144895454234,58.278569147764,12.));
#94527=CARTESIAN_POINT('Ctrl Pts',(-42.7938846369651,58.2651627533368,12.));
#94528=CARTESIAN_POINT('Ctrl Pts',(-42.7733271034678,58.2517589447818,12.));
#94529=CARTESIAN_POINT('Ctrl Pts',(-42.7528170079482,58.238357832842,12.));
#94530=CARTESIAN_POINT('Ctrl Pts',(-42.7323544135983,58.2249595287497,12.));
#94531=CARTESIAN_POINT('Ctrl Pts',(-42.7119393837866,58.2115641442302,12.));
#94532=CARTESIAN_POINT('Ctrl Pts',(-42.6915719820516,58.1981717915043,12.));
#94533=CARTESIAN_POINT('Ctrl Pts',(-42.6712522721021,58.1847825832932,12.));
#94534=CARTESIAN_POINT('Ctrl Pts',(-42.6509803178269,58.1713966328217,12.));
#94535=CARTESIAN_POINT('Ctrl Pts',(-42.6307561832977,58.158014053823,12.));
#94536=CARTESIAN_POINT('Ctrl Pts',(-42.6105799327697,58.1446349605419,12.));
#94537=CARTESIAN_POINT('Ctrl Pts',(-42.5904516306759,58.1312594677383,12.));
#94538=CARTESIAN_POINT('Ctrl Pts',(-42.5703713416263,58.1178876906905,12.));
#94539=CARTESIAN_POINT('Ctrl Pts',(-42.5503391304182,58.1045197452003,12.));
#94540=CARTESIAN_POINT('Ctrl Pts',(-42.5303550620388,58.0911557475967,12.));
#94541=CARTESIAN_POINT('Ctrl Pts',(-42.5104192016664,58.0777958147404,12.));
#94542=CARTESIAN_POINT('Ctrl Pts',(-42.4905316146649,58.064440064027,12.));
#94543=CARTESIAN_POINT('Ctrl Pts',(-42.4706923665838,58.0510886133917,12.));
#94544=CARTESIAN_POINT('Ctrl Pts',(-42.4509015231667,58.0377415813132,12.));
#94545=CARTESIAN_POINT('Ctrl Pts',(-42.4311591503551,58.0243990868175,12.));
#94546=CARTESIAN_POINT('Ctrl Pts',(-42.4114653142891,58.011061249483,12.));
#94547=CARTESIAN_POINT('Ctrl Pts',(-42.3918200813024,57.9977281894437,12.));
#94548=CARTESIAN_POINT('Ctrl Pts',(-42.3722235179216,57.9844000273936,12.));
#94549=CARTESIAN_POINT('Ctrl Pts',(-42.3526756908764,57.9710768845923,12.));
#94550=CARTESIAN_POINT('Ctrl Pts',(-42.3331766671028,57.9577588828693,12.));
#94551=CARTESIAN_POINT('Ctrl Pts',(-42.3137265137446,57.9444461446292,12.));
#94552=CARTESIAN_POINT('Ctrl Pts',(-42.2943252981471,57.9311387928541,12.));
#94553=CARTESIAN_POINT('Ctrl Pts',(-42.274973087857,57.9178369511084,12.));
#94554=CARTESIAN_POINT('Ctrl Pts',(-42.2556699506332,57.9045407435447,12.));
#94555=CARTESIAN_POINT('Ctrl Pts',(-42.2364159544492,57.8912502949084,12.));
#94556=CARTESIAN_POINT('Ctrl Pts',(-42.2172111674945,57.8779657305423,12.));
#94557=CARTESIAN_POINT('Ctrl Pts',(-42.1980556581688,57.86468717639,12.));
#94558=CARTESIAN_POINT('Ctrl Pts',(-42.1789494950824,57.8514147590012,12.));
#94559=CARTESIAN_POINT('Ctrl Pts',(-42.1598927470671,57.8381486055376,12.));
#94560=CARTESIAN_POINT('Ctrl Pts',(-42.1408854831791,57.8248888437787,12.));
#94561=CARTESIAN_POINT('Ctrl Pts',(-42.121927772701,57.8116356021274,12.));
#94562=CARTESIAN_POINT('Ctrl Pts',(-42.1030196851344,57.798389009613,12.));
#94563=CARTESIAN_POINT('Ctrl Pts',(-42.0841612902018,57.7851491958954,12.));
#94564=CARTESIAN_POINT('Ctrl Pts',(-42.0653526578571,57.7719162912721,12.));
#94565=CARTESIAN_POINT('Ctrl Pts',(-42.0465938582877,57.7586904266828,12.));
#94566=CARTESIAN_POINT('Ctrl Pts',(-42.0278849619156,57.7454717337151,12.));
#94567=CARTESIAN_POINT('Ctrl Pts',(-42.0092260393911,57.7322603446086,12.));
#94568=CARTESIAN_POINT('Ctrl Pts',(-41.9906171615974,57.7190563922614,12.));
#94569=CARTESIAN_POINT('Ctrl Pts',(-41.9720583996601,57.7058600102365,12.));
#94570=CARTESIAN_POINT('Ctrl Pts',(-41.9535498249489,57.6926713327674,12.));
#94571=CARTESIAN_POINT('Ctrl Pts',(-41.9350915090791,57.6794904947641,12.));
#94572=CARTESIAN_POINT('Ctrl Pts',(-41.9166835239046,57.6663176318176,12.));
#94573=CARTESIAN_POINT('Ctrl Pts',(-41.8983259415244,57.6531528802059,12.));
#94574=CARTESIAN_POINT('Ctrl Pts',(-41.8800188342908,57.6399963769003,12.));
#94575=CARTESIAN_POINT('Ctrl Pts',(-41.8617622748108,57.6268482595702,12.));
#94576=CARTESIAN_POINT('Ctrl Pts',(-41.8435563359456,57.6137086665882,12.));
#94577=CARTESIAN_POINT('Ctrl Pts',(-41.8254010908051,57.6005777370349,12.));
#94578=CARTESIAN_POINT('Ctrl Pts',(-41.8072966127558,57.5874556107056,12.));
#94579=CARTESIAN_POINT('Ctrl Pts',(-41.7892429754297,57.5743424281205,12.));
#94580=CARTESIAN_POINT('Ctrl Pts',(-41.7712402527273,57.561238330532,12.));
#94581=CARTESIAN_POINT('Ctrl Pts',(-41.7532885188174,57.5481434599335,12.));
#94582=CARTESIAN_POINT('Ctrl Pts',(-41.7353878481336,57.5350579590649,12.));
#94583=CARTESIAN_POINT('Ctrl Pts',(-41.7175383153821,57.5219819714171,12.));
#94584=CARTESIAN_POINT('Ctrl Pts',(-41.6997399955447,57.5089156412343,12.));
#94585=CARTESIAN_POINT('Ctrl Pts',(-41.6819929638797,57.4958591135165,12.));
#94586=CARTESIAN_POINT('Ctrl Pts',(-41.6642972959165,57.4828125340218,12.));
#94587=CARTESIAN_POINT('Ctrl Pts',(-41.6466530674514,57.4697760492683,12.));
#94588=CARTESIAN_POINT('Ctrl Pts',(-41.6290603545666,57.4567498065562,12.));
#94589=CARTESIAN_POINT('Ctrl Pts',(-41.6115192336388,57.4437339539841,12.));
#94590=CARTESIAN_POINT('Ctrl Pts',(-41.5940297813477,57.4307286404662,12.));
#94591=CARTESIAN_POINT('Ctrl Pts',(-41.5765920746777,57.4177340157508,12.));
#94592=CARTESIAN_POINT('Ctrl Pts',(-41.5592061909176,57.4047502304231,12.));
#94593=CARTESIAN_POINT('Ctrl Pts',(-41.5418722076572,57.3917774358863,12.));
#94594=CARTESIAN_POINT('Ctrl Pts',(-41.524590202777,57.3788157843454,12.));
#94595=CARTESIAN_POINT('Ctrl Pts',(-41.5073602544396,57.3658654287937,12.));
#94596=CARTESIAN_POINT('Ctrl Pts',(-41.4901824410636,57.3529265229835,12.));
#94597=CARTESIAN_POINT('Ctrl Pts',(-41.4730568413518,57.3399992214717,12.));
#94598=CARTESIAN_POINT('Ctrl Pts',(-41.4559835343328,57.3270836796911,12.));
#94599=CARTESIAN_POINT('Ctrl Pts',(-41.4389625993948,57.3141800540137,12.));
#94600=CARTESIAN_POINT('Ctrl Pts',(-41.4219941163163,57.3012885018151,12.));
#94601=CARTESIAN_POINT('Ctrl Pts',(-41.4050781652938,57.2884091815406,12.));
#94602=CARTESIAN_POINT('Ctrl Pts',(-41.3882148268813,57.2755422525844,12.));
#94603=CARTESIAN_POINT('Ctrl Pts',(-41.3714041819223,57.2626878751596,12.));
#94604=CARTESIAN_POINT('Ctrl Pts',(-41.3546463114885,57.2498462101879,12.));
#94605=CARTESIAN_POINT('Ctrl Pts',(-41.3379412967875,57.2370174191401,12.));
#94606=CARTESIAN_POINT('Ctrl Pts',(-41.321289219149,57.2242016640198,12.));
#94607=CARTESIAN_POINT('Ctrl Pts',(-41.3046901602293,57.2113991077302,12.));
#94608=CARTESIAN_POINT('Ctrl Pts',(-41.2881442021863,57.1986099143983,12.));
#94609=CARTESIAN_POINT('Ctrl Pts',(-41.2716514278276,57.1858342496538,12.));
#94610=CARTESIAN_POINT('Ctrl Pts',(-41.2552119208465,57.17307228108,12.));
#94611=CARTESIAN_POINT('Ctrl Pts',(-41.2388257656559,57.1603241779077,12.));
#94612=CARTESIAN_POINT('Ctrl Pts',(-41.222493046943,57.147590110182,12.));
#94613=CARTESIAN_POINT('Ctrl Pts',(-41.2062138492915,57.1348702480647,12.));
#94614=CARTESIAN_POINT('Ctrl Pts',(-41.1899882567923,57.1221647611207,12.));
#94615=CARTESIAN_POINT('Ctrl Pts',(-41.1738163525901,57.1094738174957,12.));
#94616=CARTESIAN_POINT('Ctrl Pts',(-41.1576982197374,57.0967975854874,12.));
#94617=CARTESIAN_POINT('Ctrl Pts',(-41.1416339422117,57.084136235426,12.));
#94618=CARTESIAN_POINT('Ctrl Pts',(-41.1256236057442,57.0714899412099,12.));
#94619=CARTESIAN_POINT('Ctrl Pts',(-41.1096672990148,57.0588588825298,12.));
#94620=CARTESIAN_POINT('Ctrl Pts',(-41.0937651137549,57.046243245068,12.));
#94621=CARTESIAN_POINT('Ctrl Pts',(-41.0779171422438,57.0336432158536,12.));
#94622=CARTESIAN_POINT('Ctrl Pts',(-41.0621234751007,57.0210589791788,12.));
#94623=CARTESIAN_POINT('Ctrl Pts',(-41.0463841993608,57.008490713042,12.));
#94624=CARTESIAN_POINT('Ctrl Pts',(-41.0306993953988,56.995938583472,12.));
#94625=CARTESIAN_POINT('Ctrl Pts',(-41.0150691398947,56.9834027500117,12.));
#94626=CARTESIAN_POINT('Ctrl Pts',(-40.9994935117276,56.9708833766137,12.));
#94627=CARTESIAN_POINT('Ctrl Pts',(-40.9839725967121,56.9583806404069,12.));
#94628=CARTESIAN_POINT('Ctrl Pts',(-40.9685064933074,56.9458947422608,12.));
#94629=CARTESIAN_POINT('Ctrl Pts',(-40.9530953165031,56.9334259140049,12.));
#94630=CARTESIAN_POINT('Ctrl Pts',(-40.9377391857128,56.9209743960992,12.));
#94631=CARTESIAN_POINT('Ctrl Pts',(-40.9224382132427,56.9085404164502,12.));
#94632=CARTESIAN_POINT('Ctrl Pts',(-40.9071924937508,56.8961241708861,12.));
#94633=CARTESIAN_POINT('Ctrl Pts',(-40.8920020903293,56.8837257978343,12.));
#94634=CARTESIAN_POINT('Ctrl Pts',(-40.8768670342052,56.8713453764905,12.));
#94635=CARTESIAN_POINT('Ctrl Pts',(-40.864803275942,56.8614554317668,12.));
#94636=CARTESIAN_POINT('Ctrl Pts',(-40.8557803680277,56.8540460739472,12.));
#94637=CARTESIAN_POINT('Ctrl Pts',(-40.8497761671036,56.8491101022591,12.));
#94638=CARTESIAN_POINT('Ctrl Pts',(-40.8467768343956,56.8466430164621,12.));
#94639=CARTESIAN_POINT('Ctrl Pts',(-45.7706564944896,58.4060826907797,-5.55111512312578E-16));
#94640=CARTESIAN_POINT('Ctrl Pts',(-45.7706564944896,58.4060826907797,4.));
#94641=CARTESIAN_POINT('Ctrl Pts',(-45.7706564944896,58.4060826907797,8.));
#94642=CARTESIAN_POINT('Ctrl Pts',(-45.7706564944896,58.4060826907797,12.));
#94643=CARTESIAN_POINT('Ctrl Pts',(-45.7969367893064,58.5127761886847,-5.55111512312578E-16));
#94644=CARTESIAN_POINT('Ctrl Pts',(-45.7969367893064,58.5127761886847,4.));
#94645=CARTESIAN_POINT('Ctrl Pts',(-45.7969367893064,58.5127761886847,8.00000000000001));
#94646=CARTESIAN_POINT('Ctrl Pts',(-45.7969367893064,58.5127761886847,12.));
#94647=CARTESIAN_POINT('Ctrl Pts',(-45.7788617791411,58.714632205056,-5.55111512312578E-16));
#94648=CARTESIAN_POINT('Ctrl Pts',(-45.7788617791411,58.714632205056,4.));
#94649=CARTESIAN_POINT('Ctrl Pts',(-45.7788617791411,58.714632205056,7.99999999999999));
#94650=CARTESIAN_POINT('Ctrl Pts',(-45.7788617791411,58.714632205056,12.));
#94651=CARTESIAN_POINT('Ctrl Pts',(-45.6563266621663,58.870677144318,-5.55111512312578E-16));
#94652=CARTESIAN_POINT('Ctrl Pts',(-45.6563266621663,58.870677144318,4.));
#94653=CARTESIAN_POINT('Ctrl Pts',(-45.6563266621663,58.870677144318,8.00000000000001));
#94654=CARTESIAN_POINT('Ctrl Pts',(-45.6563266621663,58.870677144318,12.));
#94655=CARTESIAN_POINT('Ctrl Pts',(-45.5911481700252,58.9211100416378,-5.55111512312578E-16));
#94656=CARTESIAN_POINT('Ctrl Pts',(-45.5911481700252,58.9211100416378,4.));
#94657=CARTESIAN_POINT('Ctrl Pts',(-45.5911481700252,58.9211100416378,8.));
#94658=CARTESIAN_POINT('Ctrl Pts',(-45.5911481700252,58.9211100416378,12.));
#94659=CARTESIAN_POINT('',(-45.7706564944896,58.4060826907797,2.77555756156289E-16));
#94660=CARTESIAN_POINT('',(-45.5911481700253,58.9211100416379,0.));
#94661=CARTESIAN_POINT('Ctrl Pts',(-45.7706564944896,58.4060826907797,-1.38777878078145E-16));
#94662=CARTESIAN_POINT('Ctrl Pts',(-45.7969367893064,58.5127761886847,-1.38777878078145E-16));
#94663=CARTESIAN_POINT('Ctrl Pts',(-45.7866082120691,58.628122483754,-1.38777878078144E-16));
#94664=CARTESIAN_POINT('Ctrl Pts',(-45.7421702122001,58.7285100597672,-1.38777878078145E-16));
#94665=CARTESIAN_POINT('Ctrl Pts',(-45.7088417122983,58.8038007417772,-1.38777878078145E-16));
#94666=CARTESIAN_POINT('Ctrl Pts',(-45.6563266621663,58.870677144318,-1.38777878078145E-16));
#94667=CARTESIAN_POINT('Ctrl Pts',(-45.5911481700252,58.9211100416378,-1.38777878078145E-16));
#94668=CARTESIAN_POINT('',(-45.5911481700253,58.9211100416379,12.));
#94669=CARTESIAN_POINT('Ctrl Pts',(-45.5911481700252,58.9211100416378,-5.55111512312578E-16));
#94670=CARTESIAN_POINT('Ctrl Pts',(-45.5911481700252,58.9211100416378,4.));
#94671=CARTESIAN_POINT('Ctrl Pts',(-45.5911481700252,58.9211100416378,8.));
#94672=CARTESIAN_POINT('Ctrl Pts',(-45.5911481700252,58.9211100416378,12.));
#94673=CARTESIAN_POINT('',(-45.7706564944896,58.4060826907797,12.));
#94674=CARTESIAN_POINT('Ctrl Pts',(-45.5911481700252,58.9211100416378,12.));
#94675=CARTESIAN_POINT('Ctrl Pts',(-45.6563266621663,58.870677144318,12.));
#94676=CARTESIAN_POINT('Ctrl Pts',(-45.7088417122983,58.8038007417772,12.));
#94677=CARTESIAN_POINT('Ctrl Pts',(-45.7421702122001,58.7285100597672,12.));
#94678=CARTESIAN_POINT('Ctrl Pts',(-45.7866082120691,58.628122483754,12.));
#94679=CARTESIAN_POINT('Ctrl Pts',(-45.7969367893064,58.5127761886847,12.));
#94680=CARTESIAN_POINT('Ctrl Pts',(-45.7706564944896,58.4060826907797,12.));
#94681=CARTESIAN_POINT('Ctrl Pts',(-45.7706564944896,58.4060826907797,12.));
#94682=CARTESIAN_POINT('Ctrl Pts',(-45.7706564944896,58.4060826907797,8.));
#94683=CARTESIAN_POINT('Ctrl Pts',(-45.7706564944896,58.4060826907797,4.));
#94684=CARTESIAN_POINT('Ctrl Pts',(-45.7706564944896,58.4060826907797,-5.55111512312578E-16));
#94685=CARTESIAN_POINT('Origin',(-2.28269173065022E-10,2.97323128204029E-10,
0.));
#94686=CARTESIAN_POINT('Origin',(-2.28269173065022E-10,2.97323128204029E-10,
12.));
#94687=CARTESIAN_POINT('Origin',(-2.28269173065022E-10,2.97323128204029E-10,
0.));
#94688=CARTESIAN_POINT('Ctrl Pts',(-39.7746412831503,62.9938720098766,-5.55111512312578E-16));
#94689=CARTESIAN_POINT('Ctrl Pts',(-39.7746412831503,62.9938720098766,4.));
#94690=CARTESIAN_POINT('Ctrl Pts',(-39.7746412831503,62.9938720098766,8.));
#94691=CARTESIAN_POINT('Ctrl Pts',(-39.7746412831503,62.9938720098766,12.));
#94692=CARTESIAN_POINT('Ctrl Pts',(-39.6817295782362,63.0525369183202,-5.55111512312578E-16));
#94693=CARTESIAN_POINT('Ctrl Pts',(-39.6817295782362,63.0525369183202,4.));
#94694=CARTESIAN_POINT('Ctrl Pts',(-39.6817295782362,63.0525369183202,8.));
#94695=CARTESIAN_POINT('Ctrl Pts',(-39.6817295782362,63.0525369183202,12.));
#94696=CARTESIAN_POINT('Ctrl Pts',(-39.4845131830972,63.0992090147607,-5.55111512312578E-16));
#94697=CARTESIAN_POINT('Ctrl Pts',(-39.4845131830972,63.0992090147607,4.));
#94698=CARTESIAN_POINT('Ctrl Pts',(-39.4845131830972,63.0992090147607,7.99999999999999));
#94699=CARTESIAN_POINT('Ctrl Pts',(-39.4845131830972,63.0992090147607,12.));
#94700=CARTESIAN_POINT('Ctrl Pts',(-39.2977314459988,63.0322949727905,-5.55111512312578E-16));
#94701=CARTESIAN_POINT('Ctrl Pts',(-39.2977314459988,63.0322949727905,4.));
#94702=CARTESIAN_POINT('Ctrl Pts',(-39.2977314459988,63.0322949727905,8.00000000000001));
#94703=CARTESIAN_POINT('Ctrl Pts',(-39.2977314459988,63.0322949727905,12.));
#94704=CARTESIAN_POINT('Ctrl Pts',(-39.2292784191472,62.9864049293631,-5.55111512312578E-16));
#94705=CARTESIAN_POINT('Ctrl Pts',(-39.2292784191472,62.9864049293631,4.));
#94706=CARTESIAN_POINT('Ctrl Pts',(-39.2292784191471,62.9864049293632,8.));
#94707=CARTESIAN_POINT('Ctrl Pts',(-39.2292784191471,62.9864049293632,12.));
#94708=CARTESIAN_POINT('',(-39.7746412831503,62.9938720098766,0.));
#94709=CARTESIAN_POINT('',(-39.2292784191471,62.9864049293634,0.));
#94710=CARTESIAN_POINT('Ctrl Pts',(-39.7746412831503,62.9938720098766,4.16333634234434E-16));
#94711=CARTESIAN_POINT('Ctrl Pts',(-39.6817295782362,63.0525369183202,4.16333634234433E-16));
#94712=CARTESIAN_POINT('Ctrl Pts',(-39.5690344952996,63.0792066877147,4.16333634234434E-16));
#94713=CARTESIAN_POINT('Ctrl Pts',(-39.4597466476417,63.0687871057915,4.16333634234434E-16));
#94714=CARTESIAN_POINT('Ctrl Pts',(-39.3777807618982,63.0609724193491,4.16333634234434E-16));
#94715=CARTESIAN_POINT('Ctrl Pts',(-39.2977314459988,63.0322949727905,4.16333634234433E-16));
#94716=CARTESIAN_POINT('Ctrl Pts',(-39.2292784191472,62.9864049293631,4.16333634234434E-16));
#94717=CARTESIAN_POINT('',(-39.229278419147,62.9864049293633,12.));
#94718=CARTESIAN_POINT('Ctrl Pts',(-39.2292784191472,62.9864049293631,-5.55111512312578E-16));
#94719=CARTESIAN_POINT('Ctrl Pts',(-39.2292784191472,62.9864049293631,4.));
#94720=CARTESIAN_POINT('Ctrl Pts',(-39.2292784191471,62.9864049293632,8.));
#94721=CARTESIAN_POINT('Ctrl Pts',(-39.2292784191471,62.9864049293632,12.));
#94722=CARTESIAN_POINT('',(-39.7746412831503,62.9938720098766,12.));
#94723=CARTESIAN_POINT('Ctrl Pts',(-39.2292784191471,62.9864049293632,12.));
#94724=CARTESIAN_POINT('Ctrl Pts',(-39.2977314459988,63.0322949727905,12.));
#94725=CARTESIAN_POINT('Ctrl Pts',(-39.3777807618981,63.0609724193492,12.));
#94726=CARTESIAN_POINT('Ctrl Pts',(-39.4597466476416,63.0687871057916,12.));
#94727=CARTESIAN_POINT('Ctrl Pts',(-39.5690344952996,63.0792066877148,12.));
#94728=CARTESIAN_POINT('Ctrl Pts',(-39.6817295782362,63.0525369183202,12.));
#94729=CARTESIAN_POINT('Ctrl Pts',(-39.7746412831503,62.9938720098766,12.));
#94730=CARTESIAN_POINT('Ctrl Pts',(-39.7746412831503,62.9938720098766,12.));
#94731=CARTESIAN_POINT('Ctrl Pts',(-39.7746412831503,62.9938720098766,8.));
#94732=CARTESIAN_POINT('Ctrl Pts',(-39.7746412831503,62.9938720098766,4.));
#94733=CARTESIAN_POINT('Ctrl Pts',(-39.7746412831503,62.9938720098766,-5.55111512312578E-16));
#94734=CARTESIAN_POINT('Ctrl Pts',(-35.7368311217509,60.1903555511633,0.));
#94735=CARTESIAN_POINT('Ctrl Pts',(-35.7368311217509,60.1903555511633,12.));
#94736=CARTESIAN_POINT('Ctrl Pts',(-35.7396040203973,60.1930746580239,0.));
#94737=CARTESIAN_POINT('Ctrl Pts',(-35.7396040203973,60.1930746580239,12.));
#94738=CARTESIAN_POINT('Ctrl Pts',(-35.7451551752456,60.1985151474406,0.));
#94739=CARTESIAN_POINT('Ctrl Pts',(-35.7451551752456,60.1985151474406,12.));
#94740=CARTESIAN_POINT('Ctrl Pts',(-35.7534979801871,60.2066827086579,0.));
#94741=CARTESIAN_POINT('Ctrl Pts',(-35.7534979801871,60.2066827086579,12.));
#94742=CARTESIAN_POINT('Ctrl Pts',(-35.7646538667299,60.2175864449678,0.));
#94743=CARTESIAN_POINT('Ctrl Pts',(-35.7646538667299,60.2175864449678,12.));
#94744=CARTESIAN_POINT('Ctrl Pts',(-35.7786523045782,60.2312388621286,0.));
#94745=CARTESIAN_POINT('Ctrl Pts',(-35.7786523045782,60.2312388621286,12.));
#94746=CARTESIAN_POINT('Ctrl Pts',(-35.7927043145164,60.2449139865206,0.));
#94747=CARTESIAN_POINT('Ctrl Pts',(-35.7927043145164,60.2449139865206,12.));
#94748=CARTESIAN_POINT('Ctrl Pts',(-35.8068098723386,60.2586117365278,0.));
#94749=CARTESIAN_POINT('Ctrl Pts',(-35.8068098723386,60.2586117365278,12.));
#94750=CARTESIAN_POINT('Ctrl Pts',(-35.8209689272574,60.2723319687507,0.));
#94751=CARTESIAN_POINT('Ctrl Pts',(-35.8209689272574,60.2723319687507,12.));
#94752=CARTESIAN_POINT('Ctrl Pts',(-35.8351814020424,60.2860744798563,0.));
#94753=CARTESIAN_POINT('Ctrl Pts',(-35.8351814020424,60.2860744798563,12.));
#94754=CARTESIAN_POINT('Ctrl Pts',(-35.8494472046783,60.2998390330173,0.));
#94755=CARTESIAN_POINT('Ctrl Pts',(-35.8494472046783,60.2998390330173,12.));
#94756=CARTESIAN_POINT('Ctrl Pts',(-35.8637662371635,60.313625378281,0.));
#94757=CARTESIAN_POINT('Ctrl Pts',(-35.8637662371635,60.313625378281,12.));
#94758=CARTESIAN_POINT('Ctrl Pts',(-35.878138405151,60.3274332746782,0.));
#94759=CARTESIAN_POINT('Ctrl Pts',(-35.878138405151,60.3274332746782,12.));
#94760=CARTESIAN_POINT('Ctrl Pts',(-35.8925636280632,60.3412625135223,0.));
#94761=CARTESIAN_POINT('Ctrl Pts',(-35.8925636280632,60.3412625135223,12.));
#94762=CARTESIAN_POINT('Ctrl Pts',(-35.9070418358501,60.3551129108794,0.));
#94763=CARTESIAN_POINT('Ctrl Pts',(-35.9070418358501,60.3551129108794,12.));
#94764=CARTESIAN_POINT('Ctrl Pts',(-35.9215729642219,60.368984296546,0.));
#94765=CARTESIAN_POINT('Ctrl Pts',(-35.9215729642219,60.368984296546,12.));
#94766=CARTESIAN_POINT('Ctrl Pts',(-35.9361569506955,60.3828765049031,0.));
#94767=CARTESIAN_POINT('Ctrl Pts',(-35.9361569506955,60.3828765049031,12.));
#94768=CARTESIAN_POINT('Ctrl Pts',(-35.9507937296726,60.3967893635487,0.));
#94769=CARTESIAN_POINT('Ctrl Pts',(-35.9507937296726,60.3967893635487,12.));
#94770=CARTESIAN_POINT('Ctrl Pts',(-35.9654832299627,60.4107226875759,0.));
#94771=CARTESIAN_POINT('Ctrl Pts',(-35.9654832299627,60.4107226875759,12.));
#94772=CARTESIAN_POINT('Ctrl Pts',(-35.9802253773534,60.4246762854961,0.));
#94773=CARTESIAN_POINT('Ctrl Pts',(-35.9802253773534,60.4246762854961,12.));
#94774=CARTESIAN_POINT('Ctrl Pts',(-35.9950200962175,60.438649962949,0.));
#94775=CARTESIAN_POINT('Ctrl Pts',(-35.9950200962175,60.438649962949,12.));
#94776=CARTESIAN_POINT('Ctrl Pts',(-36.0098673113556,60.452643526964,0.));
#94777=CARTESIAN_POINT('Ctrl Pts',(-36.0098673113556,60.452643526964,12.));
#94778=CARTESIAN_POINT('Ctrl Pts',(-36.0247669500867,60.4666567908053,0.));
#94779=CARTESIAN_POINT('Ctrl Pts',(-36.0247669500867,60.4666567908053,12.));
#94780=CARTESIAN_POINT('Ctrl Pts',(-36.0397189421617,60.4806895737643,0.));
#94781=CARTESIAN_POINT('Ctrl Pts',(-36.0397189421617,60.4806895737643,12.));
#94782=CARTESIAN_POINT('Ctrl Pts',(-36.0547232187681,60.4947416988396,0.));
#94783=CARTESIAN_POINT('Ctrl Pts',(-36.0547232187681,60.4947416988396,12.));
#94784=CARTESIAN_POINT('Ctrl Pts',(-36.0697797118377,60.5088129911357,0.));
#94785=CARTESIAN_POINT('Ctrl Pts',(-36.0697797118377,60.5088129911357,12.));
#94786=CARTESIAN_POINT('Ctrl Pts',(-36.0848883531968,60.5229032759001,0.));
#94787=CARTESIAN_POINT('Ctrl Pts',(-36.0848883531968,60.5229032759001,12.));
#94788=CARTESIAN_POINT('Ctrl Pts',(-36.1000490738532,60.5370123768841,0.));
#94789=CARTESIAN_POINT('Ctrl Pts',(-36.1000490738532,60.5370123768841,12.));
#94790=CARTESIAN_POINT('Ctrl Pts',(-36.1152618043756,60.5511401172014,0.));
#94791=CARTESIAN_POINT('Ctrl Pts',(-36.1152618043756,60.5511401172014,12.));
#94792=CARTESIAN_POINT('Ctrl Pts',(-36.1305264752195,60.5652863200732,0.));
#94793=CARTESIAN_POINT('Ctrl Pts',(-36.1305264752195,60.5652863200732,12.));
#94794=CARTESIAN_POINT('Ctrl Pts',(-36.1458430170425,60.5794508095555,0.));
#94795=CARTESIAN_POINT('Ctrl Pts',(-36.1458430170425,60.5794508095555,12.));
#94796=CARTESIAN_POINT('Ctrl Pts',(-36.1612113610758,60.5936334114083,0.));
#94797=CARTESIAN_POINT('Ctrl Pts',(-36.1612113610758,60.5936334114083,12.));
#94798=CARTESIAN_POINT('Ctrl Pts',(-36.1766314392624,60.6078339534151,0.));
#94799=CARTESIAN_POINT('Ctrl Pts',(-36.1766314392624,60.6078339534151,12.));
#94800=CARTESIAN_POINT('Ctrl Pts',(-36.1921031840617,60.6220522649129,0.));
#94801=CARTESIAN_POINT('Ctrl Pts',(-36.1921031840617,60.6220522649129,12.));
#94802=CARTESIAN_POINT('Ctrl Pts',(-36.2076265283261,60.6362881765014,0.));
#94803=CARTESIAN_POINT('Ctrl Pts',(-36.2076265283261,60.6362881765014,12.));
#94804=CARTESIAN_POINT('Ctrl Pts',(-36.2232014051549,60.6505415197055,0.));
#94805=CARTESIAN_POINT('Ctrl Pts',(-36.2232014051549,60.6505415197055,12.));
#94806=CARTESIAN_POINT('Ctrl Pts',(-36.2388277477225,60.6648121265908,0.));
#94807=CARTESIAN_POINT('Ctrl Pts',(-36.2388277477225,60.6648121265908,12.));
#94808=CARTESIAN_POINT('Ctrl Pts',(-36.2545054892911,60.6790998297823,0.));
#94809=CARTESIAN_POINT('Ctrl Pts',(-36.2545054892911,60.6790998297823,12.));
#94810=CARTESIAN_POINT('Ctrl Pts',(-36.2702345632882,60.6934044626304,0.));
#94811=CARTESIAN_POINT('Ctrl Pts',(-36.2702345632882,60.6934044626304,12.));
#94812=CARTESIAN_POINT('Ctrl Pts',(-36.2860149033586,60.7077258593268,0.));
#94813=CARTESIAN_POINT('Ctrl Pts',(-36.2860149033586,60.7077258593268,12.));
#94814=CARTESIAN_POINT('Ctrl Pts',(-36.3018464434204,60.7220638550396,0.));
#94815=CARTESIAN_POINT('Ctrl Pts',(-36.3018464434204,60.7220638550396,12.));
#94816=CARTESIAN_POINT('Ctrl Pts',(-36.3177291177148,60.7364182860388,0.));
#94817=CARTESIAN_POINT('Ctrl Pts',(-36.3177291177148,60.7364182860388,12.));
#94818=CARTESIAN_POINT('Ctrl Pts',(-36.3336628607844,60.7507889896283,0.));
#94819=CARTESIAN_POINT('Ctrl Pts',(-36.3336628607844,60.7507889896283,12.));
#94820=CARTESIAN_POINT('Ctrl Pts',(-36.349647607448,60.7651758040791,0.));
#94821=CARTESIAN_POINT('Ctrl Pts',(-36.349647607448,60.7651758040791,12.));
#94822=CARTESIAN_POINT('Ctrl Pts',(-36.3656832927733,60.7795785685631,0.));
#94823=CARTESIAN_POINT('Ctrl Pts',(-36.3656832927733,60.7795785685631,12.));
#94824=CARTESIAN_POINT('Ctrl Pts',(-36.38176985204,60.7939971230781,0.));
#94825=CARTESIAN_POINT('Ctrl Pts',(-36.38176985204,60.7939971230781,12.));
#94826=CARTESIAN_POINT('Ctrl Pts',(-36.3979072207174,60.8084313084009,0.));
#94827=CARTESIAN_POINT('Ctrl Pts',(-36.3979072207174,60.8084313084009,12.));
#94828=CARTESIAN_POINT('Ctrl Pts',(-36.4140953344869,60.8228809661179,0.));
#94829=CARTESIAN_POINT('Ctrl Pts',(-36.4140953344869,60.8228809661179,12.));
#94830=CARTESIAN_POINT('Ctrl Pts',(-36.4303341292497,60.8373459386397,0.));
#94831=CARTESIAN_POINT('Ctrl Pts',(-36.4303341292497,60.8373459386397,12.));
#94832=CARTESIAN_POINT('Ctrl Pts',(-36.4466235411353,60.851826069218,0.));
#94833=CARTESIAN_POINT('Ctrl Pts',(-36.4466235411353,60.851826069218,12.));
#94834=CARTESIAN_POINT('Ctrl Pts',(-36.4629635065037,60.8663212019646,0.));
#94835=CARTESIAN_POINT('Ctrl Pts',(-36.4629635065037,60.8663212019646,12.));
#94836=CARTESIAN_POINT('Ctrl Pts',(-36.4793539619459,60.8808311818489,0.));
#94837=CARTESIAN_POINT('Ctrl Pts',(-36.4793539619459,60.8808311818489,12.));
#94838=CARTESIAN_POINT('Ctrl Pts',(-36.4957948442832,60.8953558546791,0.));
#94839=CARTESIAN_POINT('Ctrl Pts',(-36.4957948442832,60.8953558546791,12.));
#94840=CARTESIAN_POINT('Ctrl Pts',(-36.5122860905611,60.9098950670847,0.));
#94841=CARTESIAN_POINT('Ctrl Pts',(-36.5122860905611,60.9098950670847,12.));
#94842=CARTESIAN_POINT('Ctrl Pts',(-36.5288276380417,60.924448666499,0.));
#94843=CARTESIAN_POINT('Ctrl Pts',(-36.5288276380417,60.924448666499,12.));
#94844=CARTESIAN_POINT('Ctrl Pts',(-36.5454194241866,60.9390165011357,0.));
#94845=CARTESIAN_POINT('Ctrl Pts',(-36.5454194241866,60.9390165011357,12.));
#94846=CARTESIAN_POINT('Ctrl Pts',(-36.5620613866615,60.9535984199874,0.));
#94847=CARTESIAN_POINT('Ctrl Pts',(-36.5620613866615,60.9535984199874,12.));
#94848=CARTESIAN_POINT('Ctrl Pts',(-36.5787534633416,60.9681942728237,0.));
#94849=CARTESIAN_POINT('Ctrl Pts',(-36.5787534633416,60.9681942728237,12.));
#94850=CARTESIAN_POINT('Ctrl Pts',(-36.5954955923109,60.9828039101887,0.));
#94851=CARTESIAN_POINT('Ctrl Pts',(-36.5954955923109,60.9828039101887,12.));
#94852=CARTESIAN_POINT('Ctrl Pts',(-36.6122877118599,60.9974271833982,0.));
#94853=CARTESIAN_POINT('Ctrl Pts',(-36.6122877118599,60.9974271833982,12.));
#94854=CARTESIAN_POINT('Ctrl Pts',(-36.6291297604775,61.012063944535,0.));
#94855=CARTESIAN_POINT('Ctrl Pts',(-36.6291297604775,61.012063944535,12.));
#94856=CARTESIAN_POINT('Ctrl Pts',(-36.6460216768553,61.0267140464434,0.));
#94857=CARTESIAN_POINT('Ctrl Pts',(-36.6460216768553,61.0267140464434,12.));
#94858=CARTESIAN_POINT('Ctrl Pts',(-36.6629633998885,61.0413773427204,0.));
#94859=CARTESIAN_POINT('Ctrl Pts',(-36.6629633998885,61.0413773427204,12.));
#94860=CARTESIAN_POINT('Ctrl Pts',(-36.6799548686741,61.0560536877084,0.));
#94861=CARTESIAN_POINT('Ctrl Pts',(-36.6799548686741,61.0560536877084,12.));
#94862=CARTESIAN_POINT('Ctrl Pts',(-36.6969960225019,61.0707429364841,0.));
#94863=CARTESIAN_POINT('Ctrl Pts',(-36.6969960225019,61.0707429364841,12.));
#94864=CARTESIAN_POINT('Ctrl Pts',(-36.7140868008479,61.085444944851,0.));
#94865=CARTESIAN_POINT('Ctrl Pts',(-36.7140868008479,61.085444944851,12.));
#94866=CARTESIAN_POINT('Ctrl Pts',(-36.7312271433799,61.1001595693357,0.));
#94867=CARTESIAN_POINT('Ctrl Pts',(-36.7312271433799,61.1001595693357,12.));
#94868=CARTESIAN_POINT('Ctrl Pts',(-36.7484169899591,61.1148866671821,0.));
#94869=CARTESIAN_POINT('Ctrl Pts',(-36.7484169899591,61.1148866671821,12.));
#94870=CARTESIAN_POINT('Ctrl Pts',(-36.7656562806381,61.1296260963468,0.));
#94871=CARTESIAN_POINT('Ctrl Pts',(-36.7656562806381,61.1296260963468,12.));
#94872=CARTESIAN_POINT('Ctrl Pts',(-36.782944955654,61.1443777154926,0.));
#94873=CARTESIAN_POINT('Ctrl Pts',(-36.782944955654,61.1443777154926,12.));
#94874=CARTESIAN_POINT('Ctrl Pts',(-36.8002829554221,61.1591413839809,0.));
#94875=CARTESIAN_POINT('Ctrl Pts',(-36.8002829554221,61.1591413839809,12.));
#94876=CARTESIAN_POINT('Ctrl Pts',(-36.8176702205436,61.1739169618688,0.));
#94877=CARTESIAN_POINT('Ctrl Pts',(-36.8176702205436,61.1739169618688,12.));
#94878=CARTESIAN_POINT('Ctrl Pts',(-36.8351066918043,61.1887043099026,0.));
#94879=CARTESIAN_POINT('Ctrl Pts',(-36.8351066918043,61.1887043099026,12.));
#94880=CARTESIAN_POINT('Ctrl Pts',(-36.8525923101736,61.2035032895121,0.));
#94881=CARTESIAN_POINT('Ctrl Pts',(-36.8525923101736,61.2035032895121,12.));
#94882=CARTESIAN_POINT('Ctrl Pts',(-36.8701270167954,61.2183137628031,0.));
#94883=CARTESIAN_POINT('Ctrl Pts',(-36.8701270167954,61.2183137628031,12.));
#94884=CARTESIAN_POINT('Ctrl Pts',(-36.8877107529844,61.2331355925513,0.));
#94885=CARTESIAN_POINT('Ctrl Pts',(-36.8877107529844,61.2331355925513,12.));
#94886=CARTESIAN_POINT('Ctrl Pts',(-36.9053434602324,61.2479686421979,0.));
#94887=CARTESIAN_POINT('Ctrl Pts',(-36.9053434602324,61.2479686421979,12.));
#94888=CARTESIAN_POINT('Ctrl Pts',(-36.9230250802078,61.2628127758443,0.));
#94889=CARTESIAN_POINT('Ctrl Pts',(-36.9230250802078,61.2628127758443,12.));
#94890=CARTESIAN_POINT('Ctrl Pts',(-36.9407555547542,61.2776678582474,0.));
#94891=CARTESIAN_POINT('Ctrl Pts',(-36.9407555547542,61.2776678582474,12.));
#94892=CARTESIAN_POINT('Ctrl Pts',(-36.9585348258798,61.2925337548113,0.));
#94893=CARTESIAN_POINT('Ctrl Pts',(-36.9585348258798,61.2925337548113,12.));
#94894=CARTESIAN_POINT('Ctrl Pts',(-36.976362835757,61.3074103315834,0.));
#94895=CARTESIAN_POINT('Ctrl Pts',(-36.976362835757,61.3074103315834,12.));
#94896=CARTESIAN_POINT('Ctrl Pts',(-36.994239526729,61.3222974552519,0.));
#94897=CARTESIAN_POINT('Ctrl Pts',(-36.994239526729,61.3222974552519,12.));
#94898=CARTESIAN_POINT('Ctrl Pts',(-37.0121648413088,61.3371949931396,0.));
#94899=CARTESIAN_POINT('Ctrl Pts',(-37.0121648413088,61.3371949931396,12.));
#94900=CARTESIAN_POINT('Ctrl Pts',(-37.0301387221766,61.352102813199,0.));
#94901=CARTESIAN_POINT('Ctrl Pts',(-37.0301387221766,61.352102813199,12.));
#94902=CARTESIAN_POINT('Ctrl Pts',(-37.0481611121698,61.3670207840041,0.));
#94903=CARTESIAN_POINT('Ctrl Pts',(-37.0481611121698,61.3670207840041,12.));
#94904=CARTESIAN_POINT('Ctrl Pts',(-37.0662319542827,61.3819487747458,0.));
#94905=CARTESIAN_POINT('Ctrl Pts',(-37.0662319542827,61.3819487747458,12.));
#94906=CARTESIAN_POINT('Ctrl Pts',(-37.0843511916728,61.3968866552294,0.));
#94907=CARTESIAN_POINT('Ctrl Pts',(-37.0843511916728,61.3968866552294,12.));
#94908=CARTESIAN_POINT('Ctrl Pts',(-37.1025187676597,61.411834295869,0.));
#94909=CARTESIAN_POINT('Ctrl Pts',(-37.1025187676597,61.411834295869,12.));
#94910=CARTESIAN_POINT('Ctrl Pts',(-37.1207346257228,61.4267915676834,0.));
#94911=CARTESIAN_POINT('Ctrl Pts',(-37.1207346257228,61.4267915676834,12.));
#94912=CARTESIAN_POINT('Ctrl Pts',(-37.138998709492,61.4417583422888,0.));
#94913=CARTESIAN_POINT('Ctrl Pts',(-37.138998709492,61.4417583422888,12.));
#94914=CARTESIAN_POINT('Ctrl Pts',(-37.157310962747,61.4567344918946,0.));
#94915=CARTESIAN_POINT('Ctrl Pts',(-37.157310962747,61.4567344918946,12.));
#94916=CARTESIAN_POINT('Ctrl Pts',(-37.1756713294249,61.471719889301,0.));
#94917=CARTESIAN_POINT('Ctrl Pts',(-37.1756713294249,61.471719889301,12.));
#94918=CARTESIAN_POINT('Ctrl Pts',(-37.1940797536182,61.4867144078939,0.));
#94919=CARTESIAN_POINT('Ctrl Pts',(-37.1940797536182,61.4867144078939,12.));
#94920=CARTESIAN_POINT('Ctrl Pts',(-37.2125361795727,61.5017179216404,0.));
#94921=CARTESIAN_POINT('Ctrl Pts',(-37.2125361795727,61.5017179216404,12.));
#94922=CARTESIAN_POINT('Ctrl Pts',(-37.2310405516775,61.5167303050823,0.));
#94923=CARTESIAN_POINT('Ctrl Pts',(-37.2310405516775,61.5167303050823,12.));
#94924=CARTESIAN_POINT('Ctrl Pts',(-37.2495928144661,61.5317514333319,0.));
#94925=CARTESIAN_POINT('Ctrl Pts',(-37.2495928144661,61.5317514333319,12.));
#94926=CARTESIAN_POINT('Ctrl Pts',(-37.2681929126218,61.5467811820686,0.));
#94927=CARTESIAN_POINT('Ctrl Pts',(-37.2681929126218,61.5467811820686,12.));
#94928=CARTESIAN_POINT('Ctrl Pts',(-37.286840790977,61.5618194275349,0.));
#94929=CARTESIAN_POINT('Ctrl Pts',(-37.286840790977,61.5618194275349,12.));
#94930=CARTESIAN_POINT('Ctrl Pts',(-37.3055363945108,61.5768660465313,0.));
#94931=CARTESIAN_POINT('Ctrl Pts',(-37.3055363945108,61.5768660465313,12.));
#94932=CARTESIAN_POINT('Ctrl Pts',(-37.3242796683395,61.591920916412,0.));
#94933=CARTESIAN_POINT('Ctrl Pts',(-37.3242796683395,61.591920916412,12.));
#94934=CARTESIAN_POINT('Ctrl Pts',(-37.3430705577178,61.6069839150804,0.));
#94935=CARTESIAN_POINT('Ctrl Pts',(-37.3430705577178,61.6069839150804,12.));
#94936=CARTESIAN_POINT('Ctrl Pts',(-37.3619090080447,61.6220549209862,0.));
#94937=CARTESIAN_POINT('Ctrl Pts',(-37.3619090080447,61.6220549209862,12.));
#94938=CARTESIAN_POINT('Ctrl Pts',(-37.3807949648622,61.6371338131208,0.));
#94939=CARTESIAN_POINT('Ctrl Pts',(-37.3807949648622,61.6371338131208,12.));
#94940=CARTESIAN_POINT('Ctrl Pts',(-37.3997283738534,61.6522204710133,0.));
#94941=CARTESIAN_POINT('Ctrl Pts',(-37.3997283738534,61.6522204710133,12.));
#94942=CARTESIAN_POINT('Ctrl Pts',(-37.4187091808324,61.667314774725,0.));
#94943=CARTESIAN_POINT('Ctrl Pts',(-37.4187091808324,61.667314774725,12.));
#94944=CARTESIAN_POINT('Ctrl Pts',(-37.4377373317456,61.6824166048453,0.));
#94945=CARTESIAN_POINT('Ctrl Pts',(-37.4377373317456,61.6824166048453,12.));
#94946=CARTESIAN_POINT('Ctrl Pts',(-37.4568127726776,61.69752584249,0.));
#94947=CARTESIAN_POINT('Ctrl Pts',(-37.4568127726776,61.69752584249,12.));
#94948=CARTESIAN_POINT('Ctrl Pts',(-37.4759354498509,61.7126423692965,0.));
#94949=CARTESIAN_POINT('Ctrl Pts',(-37.4759354498509,61.7126423692965,12.));
#94950=CARTESIAN_POINT('Ctrl Pts',(-37.4951053096235,61.7277660674203,0.));
#94951=CARTESIAN_POINT('Ctrl Pts',(-37.4951053096235,61.7277660674203,12.));
#94952=CARTESIAN_POINT('Ctrl Pts',(-37.5143222984794,61.7428968195296,0.));
#94953=CARTESIAN_POINT('Ctrl Pts',(-37.5143222984794,61.7428968195296,12.));
#94954=CARTESIAN_POINT('Ctrl Pts',(-37.5335863630286,61.7580345088014,0.));
#94955=CARTESIAN_POINT('Ctrl Pts',(-37.5335863630286,61.7580345088014,12.));
#94956=CARTESIAN_POINT('Ctrl Pts',(-37.5528974500142,61.7731790189191,0.));
#94957=CARTESIAN_POINT('Ctrl Pts',(-37.5528974500142,61.7731790189191,12.));
#94958=CARTESIAN_POINT('Ctrl Pts',(-37.5722555063112,61.7883302340689,0.));
#94959=CARTESIAN_POINT('Ctrl Pts',(-37.5722555063112,61.7883302340689,12.));
#94960=CARTESIAN_POINT('Ctrl Pts',(-37.5916604789252,61.8034880389362,0.));
#94961=CARTESIAN_POINT('Ctrl Pts',(-37.5916604789252,61.8034880389362,12.));
#94962=CARTESIAN_POINT('Ctrl Pts',(-37.6111123149836,61.8186523187011,0.));
#94963=CARTESIAN_POINT('Ctrl Pts',(-37.6111123149836,61.8186523187011,12.));
#94964=CARTESIAN_POINT('Ctrl Pts',(-37.6306109617341,61.8338229590345,0.));
#94965=CARTESIAN_POINT('Ctrl Pts',(-37.6306109617341,61.8338229590345,12.));
#94966=CARTESIAN_POINT('Ctrl Pts',(-37.6501563665518,61.848999846095,0.));
#94967=CARTESIAN_POINT('Ctrl Pts',(-37.6501563665518,61.848999846095,12.));
#94968=CARTESIAN_POINT('Ctrl Pts',(-37.6697484769389,61.8641828665257,0.));
#94969=CARTESIAN_POINT('Ctrl Pts',(-37.6697484769389,61.8641828665257,12.));
#94970=CARTESIAN_POINT('Ctrl Pts',(-37.6893872405229,61.879371907451,0.));
#94971=CARTESIAN_POINT('Ctrl Pts',(-37.6893872405229,61.879371907451,12.));
#94972=CARTESIAN_POINT('Ctrl Pts',(-37.7090726050488,61.8945668564714,0.));
#94973=CARTESIAN_POINT('Ctrl Pts',(-37.7090726050488,61.8945668564714,12.));
#94974=CARTESIAN_POINT('Ctrl Pts',(-37.7288045183765,61.9097676016616,0.));
#94975=CARTESIAN_POINT('Ctrl Pts',(-37.7288045183765,61.9097676016616,12.));
#94976=CARTESIAN_POINT('Ctrl Pts',(-37.748582928488,61.9249740315664,0.));
#94977=CARTESIAN_POINT('Ctrl Pts',(-37.748582928488,61.9249740315664,12.));
#94978=CARTESIAN_POINT('Ctrl Pts',(-37.7684077834877,61.940186035198,0.));
#94979=CARTESIAN_POINT('Ctrl Pts',(-37.7684077834877,61.940186035198,12.));
#94980=CARTESIAN_POINT('Ctrl Pts',(-37.7882790316012,61.9554035020335,0.));
#94981=CARTESIAN_POINT('Ctrl Pts',(-37.7882790316012,61.9554035020335,12.));
#94982=CARTESIAN_POINT('Ctrl Pts',(-37.808196621168,61.9706263220101,0.));
#94983=CARTESIAN_POINT('Ctrl Pts',(-37.808196621168,61.9706263220101,12.));
#94984=CARTESIAN_POINT('Ctrl Pts',(-37.8281605006371,61.9858543855221,0.));
#94985=CARTESIAN_POINT('Ctrl Pts',(-37.8281605006371,61.9858543855221,12.));
#94986=CARTESIAN_POINT('Ctrl Pts',(-37.8481706185742,62.0010875834176,0.));
#94987=CARTESIAN_POINT('Ctrl Pts',(-37.8481706185742,62.0010875834176,12.));
#94988=CARTESIAN_POINT('Ctrl Pts',(-37.8682269236628,62.0163258069954,0.));
#94989=CARTESIAN_POINT('Ctrl Pts',(-37.8682269236628,62.0163258069954,12.));
#94990=CARTESIAN_POINT('Ctrl Pts',(-37.888329364703,62.0315689480022,0.));
#94991=CARTESIAN_POINT('Ctrl Pts',(-37.888329364703,62.0315689480022,12.));
#94992=CARTESIAN_POINT('Ctrl Pts',(-37.9084778906053,62.0468168986289,0.));
#94993=CARTESIAN_POINT('Ctrl Pts',(-37.9084778906053,62.0468168986289,12.));
#94994=CARTESIAN_POINT('Ctrl Pts',(-37.9286724503849,62.0620695515072,0.));
#94995=CARTESIAN_POINT('Ctrl Pts',(-37.9286724503849,62.0620695515072,12.));
#94996=CARTESIAN_POINT('Ctrl Pts',(-37.9489129931685,62.0773267997072,0.));
#94997=CARTESIAN_POINT('Ctrl Pts',(-37.9489129931685,62.0773267997072,12.));
#94998=CARTESIAN_POINT('Ctrl Pts',(-37.9691994681962,62.0925885367346,0.));
#94999=CARTESIAN_POINT('Ctrl Pts',(-37.9691994681962,62.0925885367346,12.));
#95000=CARTESIAN_POINT('Ctrl Pts',(-37.9895318248212,62.107854656528,0.));
#95001=CARTESIAN_POINT('Ctrl Pts',(-37.9895318248212,62.107854656528,12.));
#95002=CARTESIAN_POINT('Ctrl Pts',(-38.0099100125041,62.1231250534558,0.));
#95003=CARTESIAN_POINT('Ctrl Pts',(-38.0099100125041,62.1231250534558,12.));
#95004=CARTESIAN_POINT('Ctrl Pts',(-38.0303339808059,62.1383996223136,0.));
#95005=CARTESIAN_POINT('Ctrl Pts',(-38.0303339808059,62.1383996223136,12.));
#95006=CARTESIAN_POINT('Ctrl Pts',(-38.0508036793944,62.153678258321,0.));
#95007=CARTESIAN_POINT('Ctrl Pts',(-38.0508036793944,62.153678258321,12.));
#95008=CARTESIAN_POINT('Ctrl Pts',(-38.0713190580466,62.1689608571182,0.));
#95009=CARTESIAN_POINT('Ctrl Pts',(-38.0713190580466,62.1689608571182,12.));
#95010=CARTESIAN_POINT('Ctrl Pts',(-38.0918800666479,62.1842473147627,0.));
#95011=CARTESIAN_POINT('Ctrl Pts',(-38.0918800666479,62.1842473147627,12.));
#95012=CARTESIAN_POINT('Ctrl Pts',(-38.1124866551883,62.1995375277253,0.));
#95013=CARTESIAN_POINT('Ctrl Pts',(-38.1124866551883,62.1995375277253,12.));
#95014=CARTESIAN_POINT('Ctrl Pts',(-38.1331387737528,62.2148313928859,0.));
#95015=CARTESIAN_POINT('Ctrl Pts',(-38.1331387737528,62.2148313928859,12.));
#95016=CARTESIAN_POINT('Ctrl Pts',(-38.1538363725263,62.2301288075319,0.));
#95017=CARTESIAN_POINT('Ctrl Pts',(-38.1538363725263,62.2301288075319,12.));
#95018=CARTESIAN_POINT('Ctrl Pts',(-38.1745794017997,62.2454296693581,0.));
#95019=CARTESIAN_POINT('Ctrl Pts',(-38.1745794017997,62.2454296693581,12.));
#95020=CARTESIAN_POINT('Ctrl Pts',(-38.1953678119692,62.2607338764655,0.));
#95021=CARTESIAN_POINT('Ctrl Pts',(-38.1953678119692,62.2607338764655,12.));
#95022=CARTESIAN_POINT('Ctrl Pts',(-38.2162015535351,62.2760413273601,0.));
#95023=CARTESIAN_POINT('Ctrl Pts',(-38.2162015535351,62.2760413273601,12.));
#95024=CARTESIAN_POINT('Ctrl Pts',(-38.2370805770931,62.2913519209517,0.));
#95025=CARTESIAN_POINT('Ctrl Pts',(-38.2370805770931,62.2913519209517,12.));
#95026=CARTESIAN_POINT('Ctrl Pts',(-38.2580048333356,62.3066655565497,0.));
#95027=CARTESIAN_POINT('Ctrl Pts',(-38.2580048333356,62.3066655565497,12.));
#95028=CARTESIAN_POINT('Ctrl Pts',(-38.2789742730559,62.3219821338564,0.));
#95029=CARTESIAN_POINT('Ctrl Pts',(-38.2789742730559,62.3219821338564,12.));
#95030=CARTESIAN_POINT('Ctrl Pts',(-38.2999888471474,62.337301552961,0.));
#95031=CARTESIAN_POINT('Ctrl Pts',(-38.2999888471474,62.337301552961,12.));
#95032=CARTESIAN_POINT('Ctrl Pts',(-38.3210485066003,62.3526237143338,0.));
#95033=CARTESIAN_POINT('Ctrl Pts',(-38.3210485066003,62.3526237143338,12.));
#95034=CARTESIAN_POINT('Ctrl Pts',(-38.3421532024915,62.3679485188178,0.));
#95035=CARTESIAN_POINT('Ctrl Pts',(-38.3421532024915,62.3679485188178,12.));
#95036=CARTESIAN_POINT('Ctrl Pts',(-38.3633028859835,62.3832758676281,0.));
#95037=CARTESIAN_POINT('Ctrl Pts',(-38.3633028859835,62.3832758676281,12.));
#95038=CARTESIAN_POINT('Ctrl Pts',(-38.384497508335,62.3986056623587,0.));
#95039=CARTESIAN_POINT('Ctrl Pts',(-38.384497508335,62.3986056623587,12.));
#95040=CARTESIAN_POINT('Ctrl Pts',(-38.4057370209054,62.4139378049891,0.));
#95041=CARTESIAN_POINT('Ctrl Pts',(-38.4057370209054,62.4139378049891,12.));
#95042=CARTESIAN_POINT('Ctrl Pts',(-38.4270213751567,62.42927219789,0.));
#95043=CARTESIAN_POINT('Ctrl Pts',(-38.4270213751567,62.42927219789,12.));
#95044=CARTESIAN_POINT('Ctrl Pts',(-38.4483505226511,62.4446087438304,0.));
#95045=CARTESIAN_POINT('Ctrl Pts',(-38.4483505226511,62.4446087438304,12.));
#95046=CARTESIAN_POINT('Ctrl Pts',(-38.4697244150473,62.4599473459799,0.));
#95047=CARTESIAN_POINT('Ctrl Pts',(-38.4697244150473,62.4599473459799,12.));
#95048=CARTESIAN_POINT('Ctrl Pts',(-38.4911430040988,62.4752879078842,0.));
#95049=CARTESIAN_POINT('Ctrl Pts',(-38.4911430040988,62.4752879078842,12.));
#95050=CARTESIAN_POINT('Ctrl Pts',(-38.5126062416496,62.4906303334435,0.));
#95051=CARTESIAN_POINT('Ctrl Pts',(-38.5126062416496,62.4906303334435,12.));
#95052=CARTESIAN_POINT('Ctrl Pts',(-38.5341140796247,62.50597452689,0.));
#95053=CARTESIAN_POINT('Ctrl Pts',(-38.5341140796247,62.50597452689,12.));
#95054=CARTESIAN_POINT('Ctrl Pts',(-38.5556664700201,62.5213203927672,0.));
#95055=CARTESIAN_POINT('Ctrl Pts',(-38.5556664700201,62.5213203927672,12.));
#95056=CARTESIAN_POINT('Ctrl Pts',(-38.5772633648841,62.5366678359036,0.));
#95057=CARTESIAN_POINT('Ctrl Pts',(-38.5772633648841,62.5366678359036,12.));
#95058=CARTESIAN_POINT('Ctrl Pts',(-38.5989047163401,62.5520167614529,0.));
#95059=CARTESIAN_POINT('Ctrl Pts',(-38.5989047163401,62.5520167614529,12.));
#95060=CARTESIAN_POINT('Ctrl Pts',(-38.6205904766078,62.567367074937,0.));
#95061=CARTESIAN_POINT('Ctrl Pts',(-38.6205904766078,62.567367074937,12.));
#95062=CARTESIAN_POINT('Ctrl Pts',(-38.6423205980214,62.5827186822923,0.));
#95063=CARTESIAN_POINT('Ctrl Pts',(-38.6423205980214,62.5827186822923,12.));
#95064=CARTESIAN_POINT('Ctrl Pts',(-38.6640950330418,62.5980714899048,0.));
#95065=CARTESIAN_POINT('Ctrl Pts',(-38.6640950330418,62.5980714899048,12.));
#95066=CARTESIAN_POINT('Ctrl Pts',(-38.6859137342726,62.6134254046732,0.));
#95067=CARTESIAN_POINT('Ctrl Pts',(-38.6859137342726,62.6134254046732,12.));
#95068=CARTESIAN_POINT('Ctrl Pts',(-38.7077766544411,62.6287803339534,0.));
#95069=CARTESIAN_POINT('Ctrl Pts',(-38.7077766544411,62.6287803339534,12.));
#95070=CARTESIAN_POINT('Ctrl Pts',(-38.7296837463605,62.6441361854406,0.));
#95071=CARTESIAN_POINT('Ctrl Pts',(-38.7296837463605,62.6441361854406,12.));
#95072=CARTESIAN_POINT('Ctrl Pts',(-38.7516349628902,62.6594928670626,0.));
#95073=CARTESIAN_POINT('Ctrl Pts',(-38.7516349628902,62.6594928670626,12.));
#95074=CARTESIAN_POINT('Ctrl Pts',(-38.7736302568982,62.6748502868836,0.));
#95075=CARTESIAN_POINT('Ctrl Pts',(-38.7736302568982,62.6748502868836,12.));
#95076=CARTESIAN_POINT('Ctrl Pts',(-38.7956695812032,62.6902083529698,0.));
#95077=CARTESIAN_POINT('Ctrl Pts',(-38.7956695812032,62.6902083529698,12.));
#95078=CARTESIAN_POINT('Ctrl Pts',(-38.8177528885686,62.7055669733811,0.));
#95079=CARTESIAN_POINT('Ctrl Pts',(-38.8177528885686,62.7055669733811,12.));
#95080=CARTESIAN_POINT('Ctrl Pts',(-38.8398801318184,62.7209260564506,0.));
#95081=CARTESIAN_POINT('Ctrl Pts',(-38.8398801318184,62.7209260564506,12.));
#95082=CARTESIAN_POINT('Ctrl Pts',(-38.8620512639239,62.7362855110052,0.));
#95083=CARTESIAN_POINT('Ctrl Pts',(-38.8620512639239,62.7362855110052,12.));
#95084=CARTESIAN_POINT('Ctrl Pts',(-38.8842662380984,62.7516452466129,0.));
#95085=CARTESIAN_POINT('Ctrl Pts',(-38.8842662380984,62.7516452466129,12.));
#95086=CARTESIAN_POINT('Ctrl Pts',(-38.9065250078824,62.7670051738132,0.));
#95087=CARTESIAN_POINT('Ctrl Pts',(-38.9065250078824,62.7670051738132,12.));
#95088=CARTESIAN_POINT('Ctrl Pts',(-38.928827527232,62.7823652043677,0.));
#95089=CARTESIAN_POINT('Ctrl Pts',(-38.928827527232,62.7823652043677,12.));
#95090=CARTESIAN_POINT('Ctrl Pts',(-38.9511737503146,62.797725250709,0.));
#95091=CARTESIAN_POINT('Ctrl Pts',(-38.9511737503146,62.797725250709,12.));
#95092=CARTESIAN_POINT('Ctrl Pts',(-38.9735636313073,62.8130852254004,0.));
#95093=CARTESIAN_POINT('Ctrl Pts',(-38.9735636313073,62.8130852254004,12.));
#95094=CARTESIAN_POINT('Ctrl Pts',(-38.9959971241695,62.8284450405451,0.));
#95095=CARTESIAN_POINT('Ctrl Pts',(-38.9959971241695,62.8284450405451,12.));
#95096=CARTESIAN_POINT('Ctrl Pts',(-39.0184741824649,62.8438046073237,0.));
#95097=CARTESIAN_POINT('Ctrl Pts',(-39.0184741824649,62.8438046073237,12.));
#95098=CARTESIAN_POINT('Ctrl Pts',(-39.0409947590519,62.859163835209,0.));
#95099=CARTESIAN_POINT('Ctrl Pts',(-39.0409947590519,62.859163835209,12.));
#95100=CARTESIAN_POINT('Ctrl Pts',(-39.0635588063308,62.8745226326046,0.));
#95101=CARTESIAN_POINT('Ctrl Pts',(-39.0635588063308,62.8745226326046,12.));
#95102=CARTESIAN_POINT('Ctrl Pts',(-39.0861662767964,62.8898809082659,0.));
#95103=CARTESIAN_POINT('Ctrl Pts',(-39.0861662767964,62.8898809082659,12.));
#95104=CARTESIAN_POINT('Ctrl Pts',(-39.1088171235144,62.9052385725416,0.));
#95105=CARTESIAN_POINT('Ctrl Pts',(-39.1088171235144,62.9052385725416,12.));
#95106=CARTESIAN_POINT('Ctrl Pts',(-39.1315113005745,62.9205955385551,0.));
#95107=CARTESIAN_POINT('Ctrl Pts',(-39.1315113005745,62.9205955385551,12.));
#95108=CARTESIAN_POINT('Ctrl Pts',(-39.1542487636708,62.9359517237352,0.));
#95109=CARTESIAN_POINT('Ctrl Pts',(-39.1542487636708,62.9359517237352,12.));
#95110=CARTESIAN_POINT('Ctrl Pts',(-39.1770294702367,62.9513070501777,0.));
#95111=CARTESIAN_POINT('Ctrl Pts',(-39.1770294702367,62.9513070501777,12.));
#95112=CARTESIAN_POINT('Ctrl Pts',(-39.199853378159,62.9666614412627,0.));
#95113=CARTESIAN_POINT('Ctrl Pts',(-39.199853378159,62.9666614412627,12.));
#95114=CARTESIAN_POINT('Ctrl Pts',(-39.2227204447583,62.9820148189849,0.));
#95115=CARTESIAN_POINT('Ctrl Pts',(-39.2227204447583,62.9820148189849,12.));
#95116=CARTESIAN_POINT('Ctrl Pts',(-39.2456306256092,62.9973671008685,0.));
#95117=CARTESIAN_POINT('Ctrl Pts',(-39.2456306256092,62.9973671008685,12.));
#95118=CARTESIAN_POINT('Ctrl Pts',(-39.268583873541,63.0127181973702,0.));
#95119=CARTESIAN_POINT('Ctrl Pts',(-39.268583873541,63.0127181973702,12.));
#95120=CARTESIAN_POINT('Ctrl Pts',(-39.2915801372468,63.0280680082522,0.));
#95121=CARTESIAN_POINT('Ctrl Pts',(-39.2915801372468,63.0280680082522,12.));
#95122=CARTESIAN_POINT('Ctrl Pts',(-39.3146193632546,63.0434164278221,0.));
#95123=CARTESIAN_POINT('Ctrl Pts',(-39.3146193632546,63.0434164278221,12.));
#95124=CARTESIAN_POINT('Ctrl Pts',(-39.3377014983757,63.0587633513993,0.));
#95125=CARTESIAN_POINT('Ctrl Pts',(-39.3377014983757,63.0587633513993,12.));
#95126=CARTESIAN_POINT('Ctrl Pts',(-39.3608264920487,63.0741086815957,0.));
#95127=CARTESIAN_POINT('Ctrl Pts',(-39.3608264920487,63.0741086815957,12.));
#95128=CARTESIAN_POINT('Ctrl Pts',(-39.3839942985688,63.0894523341238,0.));
#95129=CARTESIAN_POINT('Ctrl Pts',(-39.3839942985688,63.0894523341238,12.));
#95130=CARTESIAN_POINT('Ctrl Pts',(-39.4072048797401,63.1047942451583,0.));
#95131=CARTESIAN_POINT('Ctrl Pts',(-39.4072048797401,63.1047942451583,12.));
#95132=CARTESIAN_POINT('Ctrl Pts',(-39.4304582059507,63.1201343730643,0.));
#95133=CARTESIAN_POINT('Ctrl Pts',(-39.4304582059507,63.1201343730643,12.));
#95134=CARTESIAN_POINT('Ctrl Pts',(-39.4537542551852,63.1354726927781,0.));
#95135=CARTESIAN_POINT('Ctrl Pts',(-39.4537542551852,63.1354726927781,12.));
#95136=CARTESIAN_POINT('Ctrl Pts',(-39.4724252610807,63.147741892189,0.));
#95137=CARTESIAN_POINT('Ctrl Pts',(-39.4724252610807,63.147741892189,12.));
#95138=CARTESIAN_POINT('Ctrl Pts',(-39.4864477303613,63.1569429707564,0.));
#95139=CARTESIAN_POINT('Ctrl Pts',(-39.4864477303613,63.1569429707564,12.));
#95140=CARTESIAN_POINT('Ctrl Pts',(-39.4958045828059,63.1630766582674,0.));
#95141=CARTESIAN_POINT('Ctrl Pts',(-39.4958045828059,63.1630766582674,12.));
#95142=CARTESIAN_POINT('Ctrl Pts',(-39.5004851439257,63.1661434108059,0.));
#95143=CARTESIAN_POINT('Ctrl Pts',(-39.5004851439257,63.1661434108059,12.));
#95144=CARTESIAN_POINT('',(-35.7368311217509,60.1903555511633,0.));
#95145=CARTESIAN_POINT('Ctrl Pts',(-35.7368311217509,60.1903555511633,0.));
#95146=CARTESIAN_POINT('Ctrl Pts',(-35.7396040203973,60.1930746580239,0.));
#95147=CARTESIAN_POINT('Ctrl Pts',(-35.7451551752456,60.1985151474406,0.));
#95148=CARTESIAN_POINT('Ctrl Pts',(-35.7534979801871,60.2066827086579,0.));
#95149=CARTESIAN_POINT('Ctrl Pts',(-35.7646538667299,60.2175864449678,0.));
#95150=CARTESIAN_POINT('Ctrl Pts',(-35.7786523045782,60.2312388621286,0.));
#95151=CARTESIAN_POINT('Ctrl Pts',(-35.7927043145164,60.2449139865206,0.));
#95152=CARTESIAN_POINT('Ctrl Pts',(-35.8068098723386,60.2586117365278,0.));
#95153=CARTESIAN_POINT('Ctrl Pts',(-35.8209689272574,60.2723319687507,0.));
#95154=CARTESIAN_POINT('Ctrl Pts',(-35.8351814020424,60.2860744798563,0.));
#95155=CARTESIAN_POINT('Ctrl Pts',(-35.8494472046783,60.2998390330173,0.));
#95156=CARTESIAN_POINT('Ctrl Pts',(-35.8637662371635,60.313625378281,0.));
#95157=CARTESIAN_POINT('Ctrl Pts',(-35.878138405151,60.3274332746782,0.));
#95158=CARTESIAN_POINT('Ctrl Pts',(-35.8925636280632,60.3412625135223,0.));
#95159=CARTESIAN_POINT('Ctrl Pts',(-35.9070418358501,60.3551129108794,0.));
#95160=CARTESIAN_POINT('Ctrl Pts',(-35.9215729642219,60.368984296546,0.));
#95161=CARTESIAN_POINT('Ctrl Pts',(-35.9361569506955,60.3828765049031,0.));
#95162=CARTESIAN_POINT('Ctrl Pts',(-35.9507937296726,60.3967893635487,0.));
#95163=CARTESIAN_POINT('Ctrl Pts',(-35.9654832299627,60.4107226875759,0.));
#95164=CARTESIAN_POINT('Ctrl Pts',(-35.9802253773534,60.4246762854961,0.));
#95165=CARTESIAN_POINT('Ctrl Pts',(-35.9950200962175,60.438649962949,0.));
#95166=CARTESIAN_POINT('Ctrl Pts',(-36.0098673113556,60.452643526964,0.));
#95167=CARTESIAN_POINT('Ctrl Pts',(-36.0247669500867,60.4666567908053,0.));
#95168=CARTESIAN_POINT('Ctrl Pts',(-36.0397189421617,60.4806895737643,0.));
#95169=CARTESIAN_POINT('Ctrl Pts',(-36.0547232187681,60.4947416988396,0.));
#95170=CARTESIAN_POINT('Ctrl Pts',(-36.0697797118377,60.5088129911357,0.));
#95171=CARTESIAN_POINT('Ctrl Pts',(-36.0848883531968,60.5229032759001,0.));
#95172=CARTESIAN_POINT('Ctrl Pts',(-36.1000490738532,60.5370123768841,0.));
#95173=CARTESIAN_POINT('Ctrl Pts',(-36.1152618043756,60.5511401172014,0.));
#95174=CARTESIAN_POINT('Ctrl Pts',(-36.1305264752195,60.5652863200732,0.));
#95175=CARTESIAN_POINT('Ctrl Pts',(-36.1458430170425,60.5794508095555,0.));
#95176=CARTESIAN_POINT('Ctrl Pts',(-36.1612113610758,60.5936334114083,0.));
#95177=CARTESIAN_POINT('Ctrl Pts',(-36.1766314392624,60.6078339534151,0.));
#95178=CARTESIAN_POINT('Ctrl Pts',(-36.1921031840617,60.6220522649129,0.));
#95179=CARTESIAN_POINT('Ctrl Pts',(-36.2076265283261,60.6362881765014,0.));
#95180=CARTESIAN_POINT('Ctrl Pts',(-36.2232014051549,60.6505415197055,0.));
#95181=CARTESIAN_POINT('Ctrl Pts',(-36.2388277477225,60.6648121265908,0.));
#95182=CARTESIAN_POINT('Ctrl Pts',(-36.2545054892911,60.6790998297823,0.));
#95183=CARTESIAN_POINT('Ctrl Pts',(-36.2702345632882,60.6934044626304,0.));
#95184=CARTESIAN_POINT('Ctrl Pts',(-36.2860149033586,60.7077258593268,0.));
#95185=CARTESIAN_POINT('Ctrl Pts',(-36.3018464434204,60.7220638550396,0.));
#95186=CARTESIAN_POINT('Ctrl Pts',(-36.3177291177148,60.7364182860388,0.));
#95187=CARTESIAN_POINT('Ctrl Pts',(-36.3336628607844,60.7507889896283,0.));
#95188=CARTESIAN_POINT('Ctrl Pts',(-36.349647607448,60.7651758040791,0.));
#95189=CARTESIAN_POINT('Ctrl Pts',(-36.3656832927733,60.7795785685631,0.));
#95190=CARTESIAN_POINT('Ctrl Pts',(-36.38176985204,60.7939971230781,0.));
#95191=CARTESIAN_POINT('Ctrl Pts',(-36.3979072207174,60.8084313084009,0.));
#95192=CARTESIAN_POINT('Ctrl Pts',(-36.4140953344869,60.8228809661179,0.));
#95193=CARTESIAN_POINT('Ctrl Pts',(-36.4303341292497,60.8373459386397,0.));
#95194=CARTESIAN_POINT('Ctrl Pts',(-36.4466235411353,60.851826069218,0.));
#95195=CARTESIAN_POINT('Ctrl Pts',(-36.4629635065037,60.8663212019646,0.));
#95196=CARTESIAN_POINT('Ctrl Pts',(-36.4793539619459,60.8808311818489,0.));
#95197=CARTESIAN_POINT('Ctrl Pts',(-36.4957948442832,60.8953558546791,0.));
#95198=CARTESIAN_POINT('Ctrl Pts',(-36.5122860905611,60.9098950670847,0.));
#95199=CARTESIAN_POINT('Ctrl Pts',(-36.5288276380417,60.924448666499,0.));
#95200=CARTESIAN_POINT('Ctrl Pts',(-36.5454194241866,60.9390165011357,0.));
#95201=CARTESIAN_POINT('Ctrl Pts',(-36.5620613866615,60.9535984199874,0.));
#95202=CARTESIAN_POINT('Ctrl Pts',(-36.5787534633416,60.9681942728237,0.));
#95203=CARTESIAN_POINT('Ctrl Pts',(-36.5954955923109,60.9828039101887,0.));
#95204=CARTESIAN_POINT('Ctrl Pts',(-36.6122877118599,60.9974271833982,0.));
#95205=CARTESIAN_POINT('Ctrl Pts',(-36.6291297604775,61.012063944535,0.));
#95206=CARTESIAN_POINT('Ctrl Pts',(-36.6460216768553,61.0267140464434,0.));
#95207=CARTESIAN_POINT('Ctrl Pts',(-36.6629633998885,61.0413773427204,0.));
#95208=CARTESIAN_POINT('Ctrl Pts',(-36.6799548686741,61.0560536877084,0.));
#95209=CARTESIAN_POINT('Ctrl Pts',(-36.6969960225019,61.0707429364841,0.));
#95210=CARTESIAN_POINT('Ctrl Pts',(-36.7140868008479,61.085444944851,0.));
#95211=CARTESIAN_POINT('Ctrl Pts',(-36.7312271433799,61.1001595693357,0.));
#95212=CARTESIAN_POINT('Ctrl Pts',(-36.7484169899591,61.1148866671821,0.));
#95213=CARTESIAN_POINT('Ctrl Pts',(-36.7656562806381,61.1296260963468,0.));
#95214=CARTESIAN_POINT('Ctrl Pts',(-36.782944955654,61.1443777154926,0.));
#95215=CARTESIAN_POINT('Ctrl Pts',(-36.8002829554221,61.1591413839809,0.));
#95216=CARTESIAN_POINT('Ctrl Pts',(-36.8176702205436,61.1739169618688,0.));
#95217=CARTESIAN_POINT('Ctrl Pts',(-36.8351066918043,61.1887043099026,0.));
#95218=CARTESIAN_POINT('Ctrl Pts',(-36.8525923101736,61.2035032895121,0.));
#95219=CARTESIAN_POINT('Ctrl Pts',(-36.8701270167954,61.2183137628031,0.));
#95220=CARTESIAN_POINT('Ctrl Pts',(-36.8877107529844,61.2331355925513,0.));
#95221=CARTESIAN_POINT('Ctrl Pts',(-36.9053434602324,61.2479686421979,0.));
#95222=CARTESIAN_POINT('Ctrl Pts',(-36.9230250802078,61.2628127758443,0.));
#95223=CARTESIAN_POINT('Ctrl Pts',(-36.9407555547542,61.2776678582474,0.));
#95224=CARTESIAN_POINT('Ctrl Pts',(-36.9585348258798,61.2925337548113,0.));
#95225=CARTESIAN_POINT('Ctrl Pts',(-36.976362835757,61.3074103315834,0.));
#95226=CARTESIAN_POINT('Ctrl Pts',(-36.994239526729,61.3222974552519,0.));
#95227=CARTESIAN_POINT('Ctrl Pts',(-37.0121648413088,61.3371949931396,0.));
#95228=CARTESIAN_POINT('Ctrl Pts',(-37.0301387221766,61.352102813199,0.));
#95229=CARTESIAN_POINT('Ctrl Pts',(-37.0481611121698,61.3670207840041,0.));
#95230=CARTESIAN_POINT('Ctrl Pts',(-37.0662319542827,61.3819487747458,0.));
#95231=CARTESIAN_POINT('Ctrl Pts',(-37.0843511916728,61.3968866552294,0.));
#95232=CARTESIAN_POINT('Ctrl Pts',(-37.1025187676597,61.411834295869,0.));
#95233=CARTESIAN_POINT('Ctrl Pts',(-37.1207346257228,61.4267915676834,0.));
#95234=CARTESIAN_POINT('Ctrl Pts',(-37.138998709492,61.4417583422888,0.));
#95235=CARTESIAN_POINT('Ctrl Pts',(-37.157310962747,61.4567344918946,0.));
#95236=CARTESIAN_POINT('Ctrl Pts',(-37.1756713294249,61.471719889301,0.));
#95237=CARTESIAN_POINT('Ctrl Pts',(-37.1940797536182,61.4867144078939,0.));
#95238=CARTESIAN_POINT('Ctrl Pts',(-37.2125361795727,61.5017179216404,0.));
#95239=CARTESIAN_POINT('Ctrl Pts',(-37.2310405516775,61.5167303050823,0.));
#95240=CARTESIAN_POINT('Ctrl Pts',(-37.2495928144661,61.5317514333319,0.));
#95241=CARTESIAN_POINT('Ctrl Pts',(-37.2681929126218,61.5467811820686,0.));
#95242=CARTESIAN_POINT('Ctrl Pts',(-37.286840790977,61.5618194275349,0.));
#95243=CARTESIAN_POINT('Ctrl Pts',(-37.3055363945108,61.5768660465313,0.));
#95244=CARTESIAN_POINT('Ctrl Pts',(-37.3242796683395,61.591920916412,0.));
#95245=CARTESIAN_POINT('Ctrl Pts',(-37.3430705577178,61.6069839150804,0.));
#95246=CARTESIAN_POINT('Ctrl Pts',(-37.3619090080447,61.6220549209862,0.));
#95247=CARTESIAN_POINT('Ctrl Pts',(-37.3807949648622,61.6371338131208,0.));
#95248=CARTESIAN_POINT('Ctrl Pts',(-37.3997283738534,61.6522204710133,0.));
#95249=CARTESIAN_POINT('Ctrl Pts',(-37.4187091808324,61.667314774725,0.));
#95250=CARTESIAN_POINT('Ctrl Pts',(-37.4377373317456,61.6824166048453,0.));
#95251=CARTESIAN_POINT('Ctrl Pts',(-37.4568127726776,61.69752584249,0.));
#95252=CARTESIAN_POINT('Ctrl Pts',(-37.4759354498509,61.7126423692965,0.));
#95253=CARTESIAN_POINT('Ctrl Pts',(-37.4951053096235,61.7277660674203,0.));
#95254=CARTESIAN_POINT('Ctrl Pts',(-37.5143222984794,61.7428968195296,0.));
#95255=CARTESIAN_POINT('Ctrl Pts',(-37.5335863630286,61.7580345088014,0.));
#95256=CARTESIAN_POINT('Ctrl Pts',(-37.5528974500142,61.7731790189191,0.));
#95257=CARTESIAN_POINT('Ctrl Pts',(-37.5722555063112,61.7883302340689,0.));
#95258=CARTESIAN_POINT('Ctrl Pts',(-37.5916604789252,61.8034880389362,0.));
#95259=CARTESIAN_POINT('Ctrl Pts',(-37.6111123149836,61.8186523187011,0.));
#95260=CARTESIAN_POINT('Ctrl Pts',(-37.6306109617341,61.8338229590345,0.));
#95261=CARTESIAN_POINT('Ctrl Pts',(-37.6501563665518,61.848999846095,0.));
#95262=CARTESIAN_POINT('Ctrl Pts',(-37.6697484769389,61.8641828665257,0.));
#95263=CARTESIAN_POINT('Ctrl Pts',(-37.6893872405229,61.879371907451,0.));
#95264=CARTESIAN_POINT('Ctrl Pts',(-37.7090726050488,61.8945668564714,0.));
#95265=CARTESIAN_POINT('Ctrl Pts',(-37.7288045183765,61.9097676016616,0.));
#95266=CARTESIAN_POINT('Ctrl Pts',(-37.748582928488,61.9249740315664,0.));
#95267=CARTESIAN_POINT('Ctrl Pts',(-37.7684077834877,61.940186035198,0.));
#95268=CARTESIAN_POINT('Ctrl Pts',(-37.7882790316012,61.9554035020335,0.));
#95269=CARTESIAN_POINT('Ctrl Pts',(-37.808196621168,61.9706263220101,0.));
#95270=CARTESIAN_POINT('Ctrl Pts',(-37.8281605006371,61.9858543855221,0.));
#95271=CARTESIAN_POINT('Ctrl Pts',(-37.8481706185742,62.0010875834176,0.));
#95272=CARTESIAN_POINT('Ctrl Pts',(-37.8682269236628,62.0163258069954,0.));
#95273=CARTESIAN_POINT('Ctrl Pts',(-37.888329364703,62.0315689480022,0.));
#95274=CARTESIAN_POINT('Ctrl Pts',(-37.9084778906053,62.0468168986289,0.));
#95275=CARTESIAN_POINT('Ctrl Pts',(-37.9286724503849,62.0620695515072,0.));
#95276=CARTESIAN_POINT('Ctrl Pts',(-37.9489129931685,62.0773267997072,0.));
#95277=CARTESIAN_POINT('Ctrl Pts',(-37.9691994681962,62.0925885367346,0.));
#95278=CARTESIAN_POINT('Ctrl Pts',(-37.9895318248212,62.107854656528,0.));
#95279=CARTESIAN_POINT('Ctrl Pts',(-38.0099100125041,62.1231250534558,0.));
#95280=CARTESIAN_POINT('Ctrl Pts',(-38.0303339808059,62.1383996223136,0.));
#95281=CARTESIAN_POINT('Ctrl Pts',(-38.0508036793944,62.153678258321,0.));
#95282=CARTESIAN_POINT('Ctrl Pts',(-38.0713190580466,62.1689608571182,0.));
#95283=CARTESIAN_POINT('Ctrl Pts',(-38.0918800666479,62.1842473147627,0.));
#95284=CARTESIAN_POINT('Ctrl Pts',(-38.1124866551883,62.1995375277253,0.));
#95285=CARTESIAN_POINT('Ctrl Pts',(-38.1331387737528,62.2148313928859,0.));
#95286=CARTESIAN_POINT('Ctrl Pts',(-38.1538363725263,62.2301288075319,0.));
#95287=CARTESIAN_POINT('Ctrl Pts',(-38.1745794017997,62.2454296693581,0.));
#95288=CARTESIAN_POINT('Ctrl Pts',(-38.1953678119692,62.2607338764655,0.));
#95289=CARTESIAN_POINT('Ctrl Pts',(-38.2162015535351,62.2760413273601,0.));
#95290=CARTESIAN_POINT('Ctrl Pts',(-38.2370805770931,62.2913519209517,0.));
#95291=CARTESIAN_POINT('Ctrl Pts',(-38.2580048333356,62.3066655565497,0.));
#95292=CARTESIAN_POINT('Ctrl Pts',(-38.2789742730559,62.3219821338564,0.));
#95293=CARTESIAN_POINT('Ctrl Pts',(-38.2999888471474,62.337301552961,0.));
#95294=CARTESIAN_POINT('Ctrl Pts',(-38.3210485066003,62.3526237143338,0.));
#95295=CARTESIAN_POINT('Ctrl Pts',(-38.3421532024915,62.3679485188178,0.));
#95296=CARTESIAN_POINT('Ctrl Pts',(-38.3633028859835,62.3832758676281,0.));
#95297=CARTESIAN_POINT('Ctrl Pts',(-38.384497508335,62.3986056623587,0.));
#95298=CARTESIAN_POINT('Ctrl Pts',(-38.4057370209054,62.4139378049891,0.));
#95299=CARTESIAN_POINT('Ctrl Pts',(-38.4270213751567,62.42927219789,0.));
#95300=CARTESIAN_POINT('Ctrl Pts',(-38.4483505226511,62.4446087438304,0.));
#95301=CARTESIAN_POINT('Ctrl Pts',(-38.4697244150473,62.4599473459799,0.));
#95302=CARTESIAN_POINT('Ctrl Pts',(-38.4911430040988,62.4752879078842,0.));
#95303=CARTESIAN_POINT('Ctrl Pts',(-38.5126062416496,62.4906303334435,0.));
#95304=CARTESIAN_POINT('Ctrl Pts',(-38.5341140796247,62.50597452689,0.));
#95305=CARTESIAN_POINT('Ctrl Pts',(-38.5556664700201,62.5213203927672,0.));
#95306=CARTESIAN_POINT('Ctrl Pts',(-38.5772633648841,62.5366678359036,0.));
#95307=CARTESIAN_POINT('Ctrl Pts',(-38.5989047163401,62.5520167614529,0.));
#95308=CARTESIAN_POINT('Ctrl Pts',(-38.6205904766078,62.567367074937,0.));
#95309=CARTESIAN_POINT('Ctrl Pts',(-38.6423205980214,62.5827186822923,0.));
#95310=CARTESIAN_POINT('Ctrl Pts',(-38.6640950330418,62.5980714899048,0.));
#95311=CARTESIAN_POINT('Ctrl Pts',(-38.6859137342726,62.6134254046732,0.));
#95312=CARTESIAN_POINT('Ctrl Pts',(-38.7077766544411,62.6287803339534,0.));
#95313=CARTESIAN_POINT('Ctrl Pts',(-38.7296837463605,62.6441361854406,0.));
#95314=CARTESIAN_POINT('Ctrl Pts',(-38.7516349628902,62.6594928670626,0.));
#95315=CARTESIAN_POINT('Ctrl Pts',(-38.7736302568982,62.6748502868836,0.));
#95316=CARTESIAN_POINT('Ctrl Pts',(-38.7956695812032,62.6902083529698,0.));
#95317=CARTESIAN_POINT('Ctrl Pts',(-38.8177528885686,62.7055669733811,0.));
#95318=CARTESIAN_POINT('Ctrl Pts',(-38.8398801318184,62.7209260564506,0.));
#95319=CARTESIAN_POINT('Ctrl Pts',(-38.8620512639239,62.7362855110052,0.));
#95320=CARTESIAN_POINT('Ctrl Pts',(-38.8842662380984,62.7516452466129,0.));
#95321=CARTESIAN_POINT('Ctrl Pts',(-38.9065250078824,62.7670051738132,0.));
#95322=CARTESIAN_POINT('Ctrl Pts',(-38.928827527232,62.7823652043677,0.));
#95323=CARTESIAN_POINT('Ctrl Pts',(-38.9511737503146,62.797725250709,0.));
#95324=CARTESIAN_POINT('Ctrl Pts',(-38.9735636313073,62.8130852254004,0.));
#95325=CARTESIAN_POINT('Ctrl Pts',(-38.9959971241695,62.8284450405451,0.));
#95326=CARTESIAN_POINT('Ctrl Pts',(-39.0184741824649,62.8438046073237,0.));
#95327=CARTESIAN_POINT('Ctrl Pts',(-39.0409947590519,62.859163835209,0.));
#95328=CARTESIAN_POINT('Ctrl Pts',(-39.0635588063308,62.8745226326046,0.));
#95329=CARTESIAN_POINT('Ctrl Pts',(-39.0861662767964,62.8898809082659,0.));
#95330=CARTESIAN_POINT('Ctrl Pts',(-39.1088171235144,62.9052385725416,0.));
#95331=CARTESIAN_POINT('Ctrl Pts',(-39.1315113005745,62.9205955385551,0.));
#95332=CARTESIAN_POINT('Ctrl Pts',(-39.1542487636708,62.9359517237352,0.));
#95333=CARTESIAN_POINT('Ctrl Pts',(-39.1770294702367,62.9513070501777,0.));
#95334=CARTESIAN_POINT('Ctrl Pts',(-39.1965939820804,62.9644687386694,0.));
#95335=CARTESIAN_POINT('Ctrl Pts',(-39.2116170128278,62.9745590018501,0.));
#95336=CARTESIAN_POINT('Ctrl Pts',(-39.2220794388575,62.9815782721131,0.));
#95337=CARTESIAN_POINT('Ctrl Pts',(-39.2279686274723,62.9855268615905,0.));
#95338=CARTESIAN_POINT('Ctrl Pts',(-39.2292784191471,62.9864049293634,0.));
#95339=CARTESIAN_POINT('',(-35.7368311217509,60.1903555511633,12.));
#95340=CARTESIAN_POINT('',(-35.7368311217509,60.1903555511633,0.));
#95341=CARTESIAN_POINT('Ctrl Pts',(-39.229278419147,62.9864049293633,12.));
#95342=CARTESIAN_POINT('Ctrl Pts',(-39.2279686274723,62.9855268615905,12.));
#95343=CARTESIAN_POINT('Ctrl Pts',(-39.2220794388575,62.9815782721131,12.));
#95344=CARTESIAN_POINT('Ctrl Pts',(-39.2116170128278,62.9745590018501,12.));
#95345=CARTESIAN_POINT('Ctrl Pts',(-39.1965939820804,62.9644687386693,12.));
#95346=CARTESIAN_POINT('Ctrl Pts',(-39.1770294702367,62.9513070501777,12.));
#95347=CARTESIAN_POINT('Ctrl Pts',(-39.1542487636708,62.9359517237352,12.));
#95348=CARTESIAN_POINT('Ctrl Pts',(-39.1315113005745,62.9205955385551,12.));
#95349=CARTESIAN_POINT('Ctrl Pts',(-39.1088171235144,62.9052385725416,12.));
#95350=CARTESIAN_POINT('Ctrl Pts',(-39.0861662767964,62.8898809082659,12.));
#95351=CARTESIAN_POINT('Ctrl Pts',(-39.0635588063308,62.8745226326046,12.));
#95352=CARTESIAN_POINT('Ctrl Pts',(-39.0409947590519,62.859163835209,12.));
#95353=CARTESIAN_POINT('Ctrl Pts',(-39.0184741824649,62.8438046073237,12.));
#95354=CARTESIAN_POINT('Ctrl Pts',(-38.9959971241695,62.8284450405451,12.));
#95355=CARTESIAN_POINT('Ctrl Pts',(-38.9735636313073,62.8130852254004,12.));
#95356=CARTESIAN_POINT('Ctrl Pts',(-38.9511737503146,62.797725250709,12.));
#95357=CARTESIAN_POINT('Ctrl Pts',(-38.928827527232,62.7823652043677,12.));
#95358=CARTESIAN_POINT('Ctrl Pts',(-38.9065250078824,62.7670051738132,12.));
#95359=CARTESIAN_POINT('Ctrl Pts',(-38.8842662380984,62.7516452466129,12.));
#95360=CARTESIAN_POINT('Ctrl Pts',(-38.8620512639239,62.7362855110052,12.));
#95361=CARTESIAN_POINT('Ctrl Pts',(-38.8398801318184,62.7209260564506,12.));
#95362=CARTESIAN_POINT('Ctrl Pts',(-38.8177528885686,62.7055669733811,12.));
#95363=CARTESIAN_POINT('Ctrl Pts',(-38.7956695812032,62.6902083529698,12.));
#95364=CARTESIAN_POINT('Ctrl Pts',(-38.7736302568982,62.6748502868836,12.));
#95365=CARTESIAN_POINT('Ctrl Pts',(-38.7516349628902,62.6594928670626,12.));
#95366=CARTESIAN_POINT('Ctrl Pts',(-38.7296837463605,62.6441361854406,12.));
#95367=CARTESIAN_POINT('Ctrl Pts',(-38.7077766544411,62.6287803339534,12.));
#95368=CARTESIAN_POINT('Ctrl Pts',(-38.6859137342726,62.6134254046732,12.));
#95369=CARTESIAN_POINT('Ctrl Pts',(-38.6640950330418,62.5980714899048,12.));
#95370=CARTESIAN_POINT('Ctrl Pts',(-38.6423205980214,62.5827186822923,12.));
#95371=CARTESIAN_POINT('Ctrl Pts',(-38.6205904766078,62.567367074937,12.));
#95372=CARTESIAN_POINT('Ctrl Pts',(-38.5989047163401,62.5520167614529,12.));
#95373=CARTESIAN_POINT('Ctrl Pts',(-38.5772633648841,62.5366678359036,12.));
#95374=CARTESIAN_POINT('Ctrl Pts',(-38.5556664700201,62.5213203927672,12.));
#95375=CARTESIAN_POINT('Ctrl Pts',(-38.5341140796247,62.50597452689,12.));
#95376=CARTESIAN_POINT('Ctrl Pts',(-38.5126062416496,62.4906303334435,12.));
#95377=CARTESIAN_POINT('Ctrl Pts',(-38.4911430040988,62.4752879078842,12.));
#95378=CARTESIAN_POINT('Ctrl Pts',(-38.4697244150473,62.4599473459799,12.));
#95379=CARTESIAN_POINT('Ctrl Pts',(-38.4483505226511,62.4446087438304,12.));
#95380=CARTESIAN_POINT('Ctrl Pts',(-38.4270213751567,62.42927219789,12.));
#95381=CARTESIAN_POINT('Ctrl Pts',(-38.4057370209054,62.4139378049891,12.));
#95382=CARTESIAN_POINT('Ctrl Pts',(-38.384497508335,62.3986056623587,12.));
#95383=CARTESIAN_POINT('Ctrl Pts',(-38.3633028859835,62.3832758676281,12.));
#95384=CARTESIAN_POINT('Ctrl Pts',(-38.3421532024915,62.3679485188178,12.));
#95385=CARTESIAN_POINT('Ctrl Pts',(-38.3210485066003,62.3526237143338,12.));
#95386=CARTESIAN_POINT('Ctrl Pts',(-38.2999888471474,62.337301552961,12.));
#95387=CARTESIAN_POINT('Ctrl Pts',(-38.2789742730559,62.3219821338564,12.));
#95388=CARTESIAN_POINT('Ctrl Pts',(-38.2580048333356,62.3066655565497,12.));
#95389=CARTESIAN_POINT('Ctrl Pts',(-38.2370805770931,62.2913519209517,12.));
#95390=CARTESIAN_POINT('Ctrl Pts',(-38.2162015535351,62.2760413273601,12.));
#95391=CARTESIAN_POINT('Ctrl Pts',(-38.1953678119692,62.2607338764655,12.));
#95392=CARTESIAN_POINT('Ctrl Pts',(-38.1745794017997,62.2454296693581,12.));
#95393=CARTESIAN_POINT('Ctrl Pts',(-38.1538363725263,62.2301288075319,12.));
#95394=CARTESIAN_POINT('Ctrl Pts',(-38.1331387737528,62.2148313928859,12.));
#95395=CARTESIAN_POINT('Ctrl Pts',(-38.1124866551883,62.1995375277253,12.));
#95396=CARTESIAN_POINT('Ctrl Pts',(-38.0918800666479,62.1842473147627,12.));
#95397=CARTESIAN_POINT('Ctrl Pts',(-38.0713190580466,62.1689608571182,12.));
#95398=CARTESIAN_POINT('Ctrl Pts',(-38.0508036793944,62.153678258321,12.));
#95399=CARTESIAN_POINT('Ctrl Pts',(-38.0303339808059,62.1383996223136,12.));
#95400=CARTESIAN_POINT('Ctrl Pts',(-38.0099100125041,62.1231250534558,12.));
#95401=CARTESIAN_POINT('Ctrl Pts',(-37.9895318248212,62.107854656528,12.));
#95402=CARTESIAN_POINT('Ctrl Pts',(-37.9691994681962,62.0925885367346,12.));
#95403=CARTESIAN_POINT('Ctrl Pts',(-37.9489129931685,62.0773267997072,12.));
#95404=CARTESIAN_POINT('Ctrl Pts',(-37.9286724503849,62.0620695515072,12.));
#95405=CARTESIAN_POINT('Ctrl Pts',(-37.9084778906053,62.0468168986289,12.));
#95406=CARTESIAN_POINT('Ctrl Pts',(-37.888329364703,62.0315689480022,12.));
#95407=CARTESIAN_POINT('Ctrl Pts',(-37.8682269236628,62.0163258069954,12.));
#95408=CARTESIAN_POINT('Ctrl Pts',(-37.8481706185742,62.0010875834176,12.));
#95409=CARTESIAN_POINT('Ctrl Pts',(-37.8281605006371,61.9858543855221,12.));
#95410=CARTESIAN_POINT('Ctrl Pts',(-37.808196621168,61.9706263220101,12.));
#95411=CARTESIAN_POINT('Ctrl Pts',(-37.7882790316012,61.9554035020335,12.));
#95412=CARTESIAN_POINT('Ctrl Pts',(-37.7684077834877,61.940186035198,12.));
#95413=CARTESIAN_POINT('Ctrl Pts',(-37.748582928488,61.9249740315664,12.));
#95414=CARTESIAN_POINT('Ctrl Pts',(-37.7288045183765,61.9097676016616,12.));
#95415=CARTESIAN_POINT('Ctrl Pts',(-37.7090726050488,61.8945668564714,12.));
#95416=CARTESIAN_POINT('Ctrl Pts',(-37.6893872405229,61.879371907451,12.));
#95417=CARTESIAN_POINT('Ctrl Pts',(-37.6697484769389,61.8641828665257,12.));
#95418=CARTESIAN_POINT('Ctrl Pts',(-37.6501563665518,61.848999846095,12.));
#95419=CARTESIAN_POINT('Ctrl Pts',(-37.6306109617341,61.8338229590345,12.));
#95420=CARTESIAN_POINT('Ctrl Pts',(-37.6111123149836,61.8186523187011,12.));
#95421=CARTESIAN_POINT('Ctrl Pts',(-37.5916604789252,61.8034880389362,12.));
#95422=CARTESIAN_POINT('Ctrl Pts',(-37.5722555063112,61.7883302340689,12.));
#95423=CARTESIAN_POINT('Ctrl Pts',(-37.5528974500142,61.7731790189191,12.));
#95424=CARTESIAN_POINT('Ctrl Pts',(-37.5335863630286,61.7580345088014,12.));
#95425=CARTESIAN_POINT('Ctrl Pts',(-37.5143222984794,61.7428968195296,12.));
#95426=CARTESIAN_POINT('Ctrl Pts',(-37.4951053096235,61.7277660674203,12.));
#95427=CARTESIAN_POINT('Ctrl Pts',(-37.4759354498509,61.7126423692965,12.));
#95428=CARTESIAN_POINT('Ctrl Pts',(-37.4568127726776,61.69752584249,12.));
#95429=CARTESIAN_POINT('Ctrl Pts',(-37.4377373317456,61.6824166048453,12.));
#95430=CARTESIAN_POINT('Ctrl Pts',(-37.4187091808324,61.667314774725,12.));
#95431=CARTESIAN_POINT('Ctrl Pts',(-37.3997283738534,61.6522204710133,12.));
#95432=CARTESIAN_POINT('Ctrl Pts',(-37.3807949648622,61.6371338131208,12.));
#95433=CARTESIAN_POINT('Ctrl Pts',(-37.3619090080447,61.6220549209862,12.));
#95434=CARTESIAN_POINT('Ctrl Pts',(-37.3430705577178,61.6069839150804,12.));
#95435=CARTESIAN_POINT('Ctrl Pts',(-37.3242796683395,61.591920916412,12.));
#95436=CARTESIAN_POINT('Ctrl Pts',(-37.3055363945108,61.5768660465313,12.));
#95437=CARTESIAN_POINT('Ctrl Pts',(-37.286840790977,61.5618194275349,12.));
#95438=CARTESIAN_POINT('Ctrl Pts',(-37.2681929126218,61.5467811820686,12.));
#95439=CARTESIAN_POINT('Ctrl Pts',(-37.2495928144661,61.5317514333319,12.));
#95440=CARTESIAN_POINT('Ctrl Pts',(-37.2310405516775,61.5167303050823,12.));
#95441=CARTESIAN_POINT('Ctrl Pts',(-37.2125361795727,61.5017179216404,12.));
#95442=CARTESIAN_POINT('Ctrl Pts',(-37.1940797536182,61.4867144078939,12.));
#95443=CARTESIAN_POINT('Ctrl Pts',(-37.1756713294249,61.471719889301,12.));
#95444=CARTESIAN_POINT('Ctrl Pts',(-37.157310962747,61.4567344918946,12.));
#95445=CARTESIAN_POINT('Ctrl Pts',(-37.138998709492,61.4417583422888,12.));
#95446=CARTESIAN_POINT('Ctrl Pts',(-37.1207346257228,61.4267915676834,12.));
#95447=CARTESIAN_POINT('Ctrl Pts',(-37.1025187676597,61.411834295869,12.));
#95448=CARTESIAN_POINT('Ctrl Pts',(-37.0843511916728,61.3968866552294,12.));
#95449=CARTESIAN_POINT('Ctrl Pts',(-37.0662319542827,61.3819487747458,12.));
#95450=CARTESIAN_POINT('Ctrl Pts',(-37.0481611121698,61.3670207840041,12.));
#95451=CARTESIAN_POINT('Ctrl Pts',(-37.0301387221766,61.352102813199,12.));
#95452=CARTESIAN_POINT('Ctrl Pts',(-37.0121648413088,61.3371949931396,12.));
#95453=CARTESIAN_POINT('Ctrl Pts',(-36.994239526729,61.3222974552519,12.));
#95454=CARTESIAN_POINT('Ctrl Pts',(-36.976362835757,61.3074103315834,12.));
#95455=CARTESIAN_POINT('Ctrl Pts',(-36.9585348258798,61.2925337548113,12.));
#95456=CARTESIAN_POINT('Ctrl Pts',(-36.9407555547542,61.2776678582474,12.));
#95457=CARTESIAN_POINT('Ctrl Pts',(-36.9230250802078,61.2628127758443,12.));
#95458=CARTESIAN_POINT('Ctrl Pts',(-36.9053434602324,61.2479686421979,12.));
#95459=CARTESIAN_POINT('Ctrl Pts',(-36.8877107529844,61.2331355925513,12.));
#95460=CARTESIAN_POINT('Ctrl Pts',(-36.8701270167954,61.2183137628031,12.));
#95461=CARTESIAN_POINT('Ctrl Pts',(-36.8525923101736,61.2035032895121,12.));
#95462=CARTESIAN_POINT('Ctrl Pts',(-36.8351066918043,61.1887043099026,12.));
#95463=CARTESIAN_POINT('Ctrl Pts',(-36.8176702205436,61.1739169618688,12.));
#95464=CARTESIAN_POINT('Ctrl Pts',(-36.8002829554221,61.1591413839809,12.));
#95465=CARTESIAN_POINT('Ctrl Pts',(-36.782944955654,61.1443777154926,12.));
#95466=CARTESIAN_POINT('Ctrl Pts',(-36.7656562806381,61.1296260963468,12.));
#95467=CARTESIAN_POINT('Ctrl Pts',(-36.7484169899591,61.1148866671821,12.));
#95468=CARTESIAN_POINT('Ctrl Pts',(-36.7312271433799,61.1001595693357,12.));
#95469=CARTESIAN_POINT('Ctrl Pts',(-36.7140868008479,61.085444944851,12.));
#95470=CARTESIAN_POINT('Ctrl Pts',(-36.6969960225019,61.0707429364841,12.));
#95471=CARTESIAN_POINT('Ctrl Pts',(-36.6799548686741,61.0560536877084,12.));
#95472=CARTESIAN_POINT('Ctrl Pts',(-36.6629633998885,61.0413773427204,12.));
#95473=CARTESIAN_POINT('Ctrl Pts',(-36.6460216768553,61.0267140464434,12.));
#95474=CARTESIAN_POINT('Ctrl Pts',(-36.6291297604775,61.012063944535,12.));
#95475=CARTESIAN_POINT('Ctrl Pts',(-36.6122877118599,60.9974271833982,12.));
#95476=CARTESIAN_POINT('Ctrl Pts',(-36.5954955923109,60.9828039101887,12.));
#95477=CARTESIAN_POINT('Ctrl Pts',(-36.5787534633416,60.9681942728237,12.));
#95478=CARTESIAN_POINT('Ctrl Pts',(-36.5620613866615,60.9535984199874,12.));
#95479=CARTESIAN_POINT('Ctrl Pts',(-36.5454194241866,60.9390165011357,12.));
#95480=CARTESIAN_POINT('Ctrl Pts',(-36.5288276380417,60.924448666499,12.));
#95481=CARTESIAN_POINT('Ctrl Pts',(-36.5122860905611,60.9098950670847,12.));
#95482=CARTESIAN_POINT('Ctrl Pts',(-36.4957948442832,60.8953558546791,12.));
#95483=CARTESIAN_POINT('Ctrl Pts',(-36.4793539619459,60.8808311818489,12.));
#95484=CARTESIAN_POINT('Ctrl Pts',(-36.4629635065037,60.8663212019646,12.));
#95485=CARTESIAN_POINT('Ctrl Pts',(-36.4466235411353,60.851826069218,12.));
#95486=CARTESIAN_POINT('Ctrl Pts',(-36.4303341292497,60.8373459386397,12.));
#95487=CARTESIAN_POINT('Ctrl Pts',(-36.4140953344869,60.8228809661179,12.));
#95488=CARTESIAN_POINT('Ctrl Pts',(-36.3979072207174,60.8084313084009,12.));
#95489=CARTESIAN_POINT('Ctrl Pts',(-36.38176985204,60.7939971230781,12.));
#95490=CARTESIAN_POINT('Ctrl Pts',(-36.3656832927733,60.7795785685631,12.));
#95491=CARTESIAN_POINT('Ctrl Pts',(-36.349647607448,60.7651758040791,12.));
#95492=CARTESIAN_POINT('Ctrl Pts',(-36.3336628607844,60.7507889896283,12.));
#95493=CARTESIAN_POINT('Ctrl Pts',(-36.3177291177148,60.7364182860388,12.));
#95494=CARTESIAN_POINT('Ctrl Pts',(-36.3018464434204,60.7220638550396,12.));
#95495=CARTESIAN_POINT('Ctrl Pts',(-36.2860149033586,60.7077258593268,12.));
#95496=CARTESIAN_POINT('Ctrl Pts',(-36.2702345632882,60.6934044626304,12.));
#95497=CARTESIAN_POINT('Ctrl Pts',(-36.2545054892911,60.6790998297823,12.));
#95498=CARTESIAN_POINT('Ctrl Pts',(-36.2388277477225,60.6648121265908,12.));
#95499=CARTESIAN_POINT('Ctrl Pts',(-36.2232014051549,60.6505415197055,12.));
#95500=CARTESIAN_POINT('Ctrl Pts',(-36.2076265283261,60.6362881765014,12.));
#95501=CARTESIAN_POINT('Ctrl Pts',(-36.1921031840617,60.6220522649129,12.));
#95502=CARTESIAN_POINT('Ctrl Pts',(-36.1766314392624,60.6078339534151,12.));
#95503=CARTESIAN_POINT('Ctrl Pts',(-36.1612113610758,60.5936334114083,12.));
#95504=CARTESIAN_POINT('Ctrl Pts',(-36.1458430170425,60.5794508095555,12.));
#95505=CARTESIAN_POINT('Ctrl Pts',(-36.1305264752195,60.5652863200732,12.));
#95506=CARTESIAN_POINT('Ctrl Pts',(-36.1152618043756,60.5511401172014,12.));
#95507=CARTESIAN_POINT('Ctrl Pts',(-36.1000490738532,60.5370123768841,12.));
#95508=CARTESIAN_POINT('Ctrl Pts',(-36.0848883531968,60.5229032759001,12.));
#95509=CARTESIAN_POINT('Ctrl Pts',(-36.0697797118377,60.5088129911357,12.));
#95510=CARTESIAN_POINT('Ctrl Pts',(-36.0547232187681,60.4947416988396,12.));
#95511=CARTESIAN_POINT('Ctrl Pts',(-36.0397189421617,60.4806895737643,12.));
#95512=CARTESIAN_POINT('Ctrl Pts',(-36.0247669500867,60.4666567908053,12.));
#95513=CARTESIAN_POINT('Ctrl Pts',(-36.0098673113556,60.452643526964,12.));
#95514=CARTESIAN_POINT('Ctrl Pts',(-35.9950200962175,60.438649962949,12.));
#95515=CARTESIAN_POINT('Ctrl Pts',(-35.9802253773534,60.4246762854961,12.));
#95516=CARTESIAN_POINT('Ctrl Pts',(-35.9654832299627,60.4107226875759,12.));
#95517=CARTESIAN_POINT('Ctrl Pts',(-35.9507937296726,60.3967893635487,12.));
#95518=CARTESIAN_POINT('Ctrl Pts',(-35.9361569506955,60.3828765049031,12.));
#95519=CARTESIAN_POINT('Ctrl Pts',(-35.9215729642219,60.368984296546,12.));
#95520=CARTESIAN_POINT('Ctrl Pts',(-35.9070418358501,60.3551129108794,12.));
#95521=CARTESIAN_POINT('Ctrl Pts',(-35.8925636280632,60.3412625135223,12.));
#95522=CARTESIAN_POINT('Ctrl Pts',(-35.878138405151,60.3274332746782,12.));
#95523=CARTESIAN_POINT('Ctrl Pts',(-35.8637662371635,60.313625378281,12.));
#95524=CARTESIAN_POINT('Ctrl Pts',(-35.8494472046783,60.2998390330173,12.));
#95525=CARTESIAN_POINT('Ctrl Pts',(-35.8351814020424,60.2860744798563,12.));
#95526=CARTESIAN_POINT('Ctrl Pts',(-35.8209689272574,60.2723319687507,12.));
#95527=CARTESIAN_POINT('Ctrl Pts',(-35.8068098723386,60.2586117365278,12.));
#95528=CARTESIAN_POINT('Ctrl Pts',(-35.7927043145164,60.2449139865206,12.));
#95529=CARTESIAN_POINT('Ctrl Pts',(-35.7786523045782,60.2312388621286,12.));
#95530=CARTESIAN_POINT('Ctrl Pts',(-35.7646538667299,60.2175864449678,12.));
#95531=CARTESIAN_POINT('Ctrl Pts',(-35.7534979801871,60.2066827086579,12.));
#95532=CARTESIAN_POINT('Ctrl Pts',(-35.7451551752456,60.1985151474406,12.));
#95533=CARTESIAN_POINT('Ctrl Pts',(-35.7396040203973,60.1930746580239,12.));
#95534=CARTESIAN_POINT('Ctrl Pts',(-35.7368311217509,60.1903555511633,12.));
#95535=CARTESIAN_POINT('Ctrl Pts',(-40.5060598100929,62.1730054756869,-5.55111512312578E-16));
#95536=CARTESIAN_POINT('Ctrl Pts',(-40.5060598100929,62.1730054756869,4.));
#95537=CARTESIAN_POINT('Ctrl Pts',(-40.5060598100929,62.1730054756869,8.));
#95538=CARTESIAN_POINT('Ctrl Pts',(-40.5060598100929,62.1730054756869,12.));
#95539=CARTESIAN_POINT('Ctrl Pts',(-40.5229411493977,62.2815834512352,-5.55111512312578E-16));
#95540=CARTESIAN_POINT('Ctrl Pts',(-40.5229411493977,62.2815834512352,4.));
#95541=CARTESIAN_POINT('Ctrl Pts',(-40.5229411493977,62.2815834512352,8.));
#95542=CARTESIAN_POINT('Ctrl Pts',(-40.5229411493977,62.2815834512352,12.));
#95543=CARTESIAN_POINT('Ctrl Pts',(-40.4873422218648,62.4810961163743,-5.55111512312578E-16));
#95544=CARTESIAN_POINT('Ctrl Pts',(-40.4873422218648,62.4810961163743,4.));
#95545=CARTESIAN_POINT('Ctrl Pts',(-40.4873422218648,62.4810961163743,7.99999999999999));
#95546=CARTESIAN_POINT('Ctrl Pts',(-40.4873422218648,62.4810961163743,12.));
#95547=CARTESIAN_POINT('Ctrl Pts',(-40.3516729626244,62.6258675056113,-5.55111512312578E-16));
#95548=CARTESIAN_POINT('Ctrl Pts',(-40.3516729626244,62.6258675056113,4.));
#95549=CARTESIAN_POINT('Ctrl Pts',(-40.3516729626244,62.6258675056113,8.00000000000001));
#95550=CARTESIAN_POINT('Ctrl Pts',(-40.3516729626244,62.6258675056113,12.));
#95551=CARTESIAN_POINT('Ctrl Pts',(-40.2823469776989,62.6704278106371,-5.55111512312578E-16));
#95552=CARTESIAN_POINT('Ctrl Pts',(-40.2823469776989,62.6704278106371,4.));
#95553=CARTESIAN_POINT('Ctrl Pts',(-40.2823469776989,62.6704278106371,8.));
#95554=CARTESIAN_POINT('Ctrl Pts',(-40.2823469776989,62.6704278106371,12.));
#95555=CARTESIAN_POINT('',(-40.5060598100929,62.1730054756869,2.77555756156289E-16));
#95556=CARTESIAN_POINT('',(-40.2823469776989,62.6704278106371,0.));
#95557=CARTESIAN_POINT('Ctrl Pts',(-40.5060598100929,62.1730054756869,-1.38777878078145E-16));
#95558=CARTESIAN_POINT('Ctrl Pts',(-40.5229411493977,62.2815834512352,-1.38777878078145E-16));
#95559=CARTESIAN_POINT('Ctrl Pts',(-40.5025989050932,62.3955906884575,-1.38777878078144E-16));
#95560=CARTESIAN_POINT('Ctrl Pts',(-40.4495806341086,62.4917232233445,-1.38777878078145E-16));
#95561=CARTESIAN_POINT('Ctrl Pts',(-40.4098169308703,62.5638226245097,-1.38777878078145E-16));
#95562=CARTESIAN_POINT('Ctrl Pts',(-40.3516729626244,62.6258675056113,-1.38777878078145E-16));
#95563=CARTESIAN_POINT('Ctrl Pts',(-40.2823469776989,62.6704278106371,-1.38777878078145E-16));
#95564=CARTESIAN_POINT('',(-40.2823469776989,62.6704278106371,12.));
#95565=CARTESIAN_POINT('Ctrl Pts',(-40.2823469776989,62.6704278106371,-5.55111512312578E-16));
#95566=CARTESIAN_POINT('Ctrl Pts',(-40.2823469776989,62.6704278106371,4.));
#95567=CARTESIAN_POINT('Ctrl Pts',(-40.2823469776989,62.6704278106371,8.));
#95568=CARTESIAN_POINT('Ctrl Pts',(-40.2823469776989,62.6704278106371,12.));
#95569=CARTESIAN_POINT('',(-40.5060598100929,62.1730054756869,12.));
#95570=CARTESIAN_POINT('Ctrl Pts',(-40.2823469776989,62.6704278106371,12.));
#95571=CARTESIAN_POINT('Ctrl Pts',(-40.3516729626244,62.6258675056113,12.));
#95572=CARTESIAN_POINT('Ctrl Pts',(-40.4098169308703,62.5638226245097,12.));
#95573=CARTESIAN_POINT('Ctrl Pts',(-40.4495806341086,62.4917232233445,12.));
#95574=CARTESIAN_POINT('Ctrl Pts',(-40.5025989050932,62.3955906884575,12.));
#95575=CARTESIAN_POINT('Ctrl Pts',(-40.5229411493977,62.2815834512352,12.));
#95576=CARTESIAN_POINT('Ctrl Pts',(-40.5060598100929,62.1730054756869,12.));
#95577=CARTESIAN_POINT('Ctrl Pts',(-40.5060598100929,62.1730054756869,12.));
#95578=CARTESIAN_POINT('Ctrl Pts',(-40.5060598100929,62.1730054756869,8.));
#95579=CARTESIAN_POINT('Ctrl Pts',(-40.5060598100929,62.1730054756869,4.));
#95580=CARTESIAN_POINT('Ctrl Pts',(-40.5060598100929,62.1730054756869,-5.55111512312578E-16));
#95581=CARTESIAN_POINT('Origin',(-2.01487121870483E-10,3.16086693261782E-10,
0.));
#95582=CARTESIAN_POINT('Origin',(-2.01487121870483E-10,3.16086693261782E-10,
12.));
#95583=CARTESIAN_POINT('Origin',(-2.01487121870483E-10,3.16086693261782E-10,
0.));
#95584=CARTESIAN_POINT('Ctrl Pts',(-34.1330090612035,66.2207497120638,0.));
#95585=CARTESIAN_POINT('Ctrl Pts',(-34.1330090612035,66.2207497120638,4.));
#95586=CARTESIAN_POINT('Ctrl Pts',(-34.1330090612036,66.2207497120638,8.));
#95587=CARTESIAN_POINT('Ctrl Pts',(-34.1330090612036,66.2207497120638,12.));
#95588=CARTESIAN_POINT('Ctrl Pts',(-34.0353379297088,66.2710935941676,0.));
#95589=CARTESIAN_POINT('Ctrl Pts',(-34.0353379297088,66.2710935941676,3.99999999999999));
#95590=CARTESIAN_POINT('Ctrl Pts',(-34.0353379297089,66.2710935941675,8.));
#95591=CARTESIAN_POINT('Ctrl Pts',(-34.0353379297089,66.2710935941675,12.));
#95592=CARTESIAN_POINT('Ctrl Pts',(-33.8348041971634,66.3003999311009,0.));
#95593=CARTESIAN_POINT('Ctrl Pts',(-33.8348041971634,66.3003999311009,4.00000000000001));
#95594=CARTESIAN_POINT('Ctrl Pts',(-33.8348041971635,66.3003999311009,7.99999999999999));
#95595=CARTESIAN_POINT('Ctrl Pts',(-33.8348041971635,66.3003999311009,12.));
#95596=CARTESIAN_POINT('Ctrl Pts',(-33.6545652280941,66.2174610329232,0.));
#95597=CARTESIAN_POINT('Ctrl Pts',(-33.6545652280941,66.2174610329232,3.99999999999999));
#95598=CARTESIAN_POINT('Ctrl Pts',(-33.6545652280943,66.2174610329232,8.00000000000001));
#95599=CARTESIAN_POINT('Ctrl Pts',(-33.6545652280943,66.2174610329232,12.));
#95600=CARTESIAN_POINT('Ctrl Pts',(-33.5903722664958,66.1657795405671,0.));
#95601=CARTESIAN_POINT('Ctrl Pts',(-33.5903722664958,66.1657795405671,4.));
#95602=CARTESIAN_POINT('Ctrl Pts',(-33.590372266496,66.1657795405672,8.));
#95603=CARTESIAN_POINT('Ctrl Pts',(-33.590372266496,66.1657795405672,12.));
#95604=CARTESIAN_POINT('',(-34.1330090612035,66.2207497120638,0.));
#95605=CARTESIAN_POINT('',(-33.5903722664959,66.1657795405671,0.));
#95606=CARTESIAN_POINT('Ctrl Pts',(-34.1330090612035,66.2207497120638,1.38777878078144E-16));
#95607=CARTESIAN_POINT('Ctrl Pts',(-34.0353379297088,66.2710935941676,1.38777878078144E-16));
#95608=CARTESIAN_POINT('Ctrl Pts',(-33.9207472253972,66.2878400724152,1.38777878078145E-16));
#95609=CARTESIAN_POINT('Ctrl Pts',(-33.8127833826287,66.2679350453204,1.38777878078144E-16));
#95610=CARTESIAN_POINT('Ctrl Pts',(-33.7318105005524,66.2530062749994,1.38777878078144E-16));
#95611=CARTESIAN_POINT('Ctrl Pts',(-33.6545652280941,66.2174610329232,1.38777878078144E-16));
#95612=CARTESIAN_POINT('Ctrl Pts',(-33.5903722664958,66.1657795405671,1.38777878078144E-16));
#95613=CARTESIAN_POINT('',(-33.590372266496,66.1657795405671,12.));
#95614=CARTESIAN_POINT('Ctrl Pts',(-33.5903722664958,66.1657795405671,0.));
#95615=CARTESIAN_POINT('Ctrl Pts',(-33.5903722664958,66.1657795405671,4.));
#95616=CARTESIAN_POINT('Ctrl Pts',(-33.590372266496,66.1657795405672,8.));
#95617=CARTESIAN_POINT('Ctrl Pts',(-33.590372266496,66.1657795405672,12.));
#95618=CARTESIAN_POINT('',(-34.1330090612036,66.2207497120638,12.));
#95619=CARTESIAN_POINT('Ctrl Pts',(-33.590372266496,66.1657795405672,12.));
#95620=CARTESIAN_POINT('Ctrl Pts',(-33.6545652280943,66.2174610329232,12.));
#95621=CARTESIAN_POINT('Ctrl Pts',(-33.7318105005525,66.2530062749993,12.));
#95622=CARTESIAN_POINT('Ctrl Pts',(-33.8127833826288,66.2679350453204,12.));
#95623=CARTESIAN_POINT('Ctrl Pts',(-33.9207472253972,66.2878400724152,12.));
#95624=CARTESIAN_POINT('Ctrl Pts',(-34.0353379297089,66.2710935941675,12.));
#95625=CARTESIAN_POINT('Ctrl Pts',(-34.1330090612036,66.2207497120638,12.));
#95626=CARTESIAN_POINT('Ctrl Pts',(-34.1330090612036,66.2207497120638,12.));
#95627=CARTESIAN_POINT('Ctrl Pts',(-34.1330090612036,66.2207497120638,8.));
#95628=CARTESIAN_POINT('Ctrl Pts',(-34.1330090612035,66.2207497120638,4.));
#95629=CARTESIAN_POINT('Ctrl Pts',(-34.1330090612035,66.2207497120638,0.));
#95630=CARTESIAN_POINT('Ctrl Pts',(-30.3549065457811,63.0759831361898,0.));
#95631=CARTESIAN_POINT('Ctrl Pts',(-30.3549065457811,63.0759831361898,12.));
#95632=CARTESIAN_POINT('Ctrl Pts',(-30.357431906933,63.078933570069,0.));
#95633=CARTESIAN_POINT('Ctrl Pts',(-30.357431906933,63.078933570069,12.));
#95634=CARTESIAN_POINT('Ctrl Pts',(-30.3624877680651,63.0848371718048,0.));
#95635=CARTESIAN_POINT('Ctrl Pts',(-30.3624877680651,63.0848371718048,12.));
#95636=CARTESIAN_POINT('Ctrl Pts',(-30.3700869762507,63.0937007763471,0.));
#95637=CARTESIAN_POINT('Ctrl Pts',(-30.3700869762507,63.0937007763471,12.));
#95638=CARTESIAN_POINT('Ctrl Pts',(-30.3802500880403,63.105535320226,0.));
#95639=CARTESIAN_POINT('Ctrl Pts',(-30.3802500880403,63.105535320226,12.));
#95640=CARTESIAN_POINT('Ctrl Pts',(-30.3930053710484,63.1203558300657,0.));
#95641=CARTESIAN_POINT('Ctrl Pts',(-30.3930053710484,63.1203558300657,12.));
#95642=CARTESIAN_POINT('Ctrl Pts',(-30.4058120432228,63.135203629844,0.));
#95643=CARTESIAN_POINT('Ctrl Pts',(-30.4058120432228,63.135203629844,12.));
#95644=CARTESIAN_POINT('Ctrl Pts',(-30.418670087563,63.1500786361459,0.));
#95645=CARTESIAN_POINT('Ctrl Pts',(-30.418670087563,63.1500786361459,12.));
#95646=CARTESIAN_POINT('Ctrl Pts',(-30.4315794659731,63.164980701691,0.));
#95647=CARTESIAN_POINT('Ctrl Pts',(-30.4315794659731,63.164980701691,12.));
#95648=CARTESIAN_POINT('Ctrl Pts',(-30.4445401192381,63.179909617189,0.));
#95649=CARTESIAN_POINT('Ctrl Pts',(-30.4445401192381,63.179909617189,12.));
#95650=CARTESIAN_POINT('Ctrl Pts',(-30.4575519763337,63.1948651386942,0.));
#95651=CARTESIAN_POINT('Ctrl Pts',(-30.4575519763337,63.1948651386942,12.));
#95652=CARTESIAN_POINT('Ctrl Pts',(-30.470614961416,63.2098470086636,0.));
#95653=CARTESIAN_POINT('Ctrl Pts',(-30.470614961416,63.2098470086636,12.));
#95654=CARTESIAN_POINT('Ctrl Pts',(-30.4837290014989,63.2248549788221,0.));
#95655=CARTESIAN_POINT('Ctrl Pts',(-30.4837290014989,63.2248549788221,12.));
#95656=CARTESIAN_POINT('Ctrl Pts',(-30.4968940344998,63.2398888342545,0.));
#95657=CARTESIAN_POINT('Ctrl Pts',(-30.4968940344998,63.2398888342545,12.));
#95658=CARTESIAN_POINT('Ctrl Pts',(-30.5101100066659,63.2549483856215,0.));
#95659=CARTESIAN_POINT('Ctrl Pts',(-30.5101100066659,63.2549483856215,12.));
#95660=CARTESIAN_POINT('Ctrl Pts',(-30.5233768687865,63.2700334577639,0.));
#95661=CARTESIAN_POINT('Ctrl Pts',(-30.5233768687865,63.2700334577639,12.));
#95662=CARTESIAN_POINT('Ctrl Pts',(-30.5366945730508,63.2851438802473,0.));
#95663=CARTESIAN_POINT('Ctrl Pts',(-30.5366945730508,63.2851438802473,12.));
#95664=CARTESIAN_POINT('Ctrl Pts',(-30.5500630691359,63.3002794756086,0.));
#95665=CARTESIAN_POINT('Ctrl Pts',(-30.5500630691359,63.3002794756086,12.));
#95666=CARTESIAN_POINT('Ctrl Pts',(-30.563482302238,63.3154400534397,0.));
#95667=CARTESIAN_POINT('Ctrl Pts',(-30.563482302238,63.3154400534397,12.));
#95668=CARTESIAN_POINT('Ctrl Pts',(-30.5769522151164,63.3306254165126,0.));
#95669=CARTESIAN_POINT('Ctrl Pts',(-30.5769522151164,63.3306254165126,12.));
#95670=CARTESIAN_POINT('Ctrl Pts',(-30.5904727493712,63.3458353646154,0.));
#95671=CARTESIAN_POINT('Ctrl Pts',(-30.5904727493712,63.3458353646154,12.));
#95672=CARTESIAN_POINT('Ctrl Pts',(-30.6040438469078,63.3610696989577,0.));
#95673=CARTESIAN_POINT('Ctrl Pts',(-30.6040438469078,63.3610696989577,12.));
#95674=CARTESIAN_POINT('Ctrl Pts',(-30.6176654515967,63.3763282271796,0.));
#95675=CARTESIAN_POINT('Ctrl Pts',(-30.6176654515967,63.3763282271796,12.));
#95676=CARTESIAN_POINT('Ctrl Pts',(-30.6313375092062,63.3916107631376,0.));
#95677=CARTESIAN_POINT('Ctrl Pts',(-30.6313375092062,63.3916107631376,12.));
#95678=CARTESIAN_POINT('Ctrl Pts',(-30.6450599666121,63.4069171245066,0.));
#95679=CARTESIAN_POINT('Ctrl Pts',(-30.6450599666121,63.4069171245066,12.));
#95680=CARTESIAN_POINT('Ctrl Pts',(-30.6588327712484,63.4222471311239,0.));
#95681=CARTESIAN_POINT('Ctrl Pts',(-30.6588327712484,63.4222471311239,12.));
#95682=CARTESIAN_POINT('Ctrl Pts',(-30.6726558704315,63.4376006029604,0.));
#95683=CARTESIAN_POINT('Ctrl Pts',(-30.6726558704315,63.4376006029604,12.));
#95684=CARTESIAN_POINT('Ctrl Pts',(-30.6865292107929,63.4529773584249,0.));
#95685=CARTESIAN_POINT('Ctrl Pts',(-30.6865292107929,63.4529773584249,12.));
#95686=CARTESIAN_POINT('Ctrl Pts',(-30.7004527385821,63.4683772152529,0.));
#95687=CARTESIAN_POINT('Ctrl Pts',(-30.7004527385821,63.4683772152529,12.));
#95688=CARTESIAN_POINT('Ctrl Pts',(-30.7144263999265,63.4837999912771,0.));
#95689=CARTESIAN_POINT('Ctrl Pts',(-30.7144263999265,63.4837999912771,12.));
#95690=CARTESIAN_POINT('Ctrl Pts',(-30.7284501410822,63.4992455051795,0.));
#95691=CARTESIAN_POINT('Ctrl Pts',(-30.7284501410822,63.4992455051795,12.));
#95692=CARTESIAN_POINT('Ctrl Pts',(-30.7425239087281,63.5147135773894,0.));
#95693=CARTESIAN_POINT('Ctrl Pts',(-30.7425239087281,63.5147135773894,12.));
#95694=CARTESIAN_POINT('Ctrl Pts',(-30.7566476500757,63.5302040304142,0.));
#95695=CARTESIAN_POINT('Ctrl Pts',(-30.7566476500757,63.5302040304142,12.));
#95696=CARTESIAN_POINT('Ctrl Pts',(-30.7708213127159,63.5457166883537,0.));
#95697=CARTESIAN_POINT('Ctrl Pts',(-30.7708213127159,63.5457166883537,12.));
#95698=CARTESIAN_POINT('Ctrl Pts',(-30.7850448445205,63.5612513766,0.));
#95699=CARTESIAN_POINT('Ctrl Pts',(-30.7850448445205,63.5612513766,12.));
#95700=CARTESIAN_POINT('Ctrl Pts',(-30.7993181935271,63.5768079214881,0.));
#95701=CARTESIAN_POINT('Ctrl Pts',(-30.7993181935271,63.5768079214881,12.));
#95702=CARTESIAN_POINT('Ctrl Pts',(-30.813641307801,63.5923861498987,0.));
#95703=CARTESIAN_POINT('Ctrl Pts',(-30.813641307801,63.5923861498987,12.));
#95704=CARTESIAN_POINT('Ctrl Pts',(-30.8280141354459,63.6079858892771,0.));
#95705=CARTESIAN_POINT('Ctrl Pts',(-30.8280141354459,63.6079858892771,12.));
#95706=CARTESIAN_POINT('Ctrl Pts',(-30.8424366246671,63.6236069678055,0.));
#95707=CARTESIAN_POINT('Ctrl Pts',(-30.8424366246671,63.6236069678055,12.));
#95708=CARTESIAN_POINT('Ctrl Pts',(-30.8569087238131,63.6392492145233,0.));
#95709=CARTESIAN_POINT('Ctrl Pts',(-30.8569087238131,63.6392492145233,12.));
#95710=CARTESIAN_POINT('Ctrl Pts',(-30.8714303814194,63.6549124594666,0.));
#95711=CARTESIAN_POINT('Ctrl Pts',(-30.8714303814194,63.6549124594666,12.));
#95712=CARTESIAN_POINT('Ctrl Pts',(-30.8860015462475,63.6705965337971,0.));
#95713=CARTESIAN_POINT('Ctrl Pts',(-30.8860015462475,63.6705965337971,12.));
#95714=CARTESIAN_POINT('Ctrl Pts',(-30.900622167269,63.6863012697328,0.));
#95715=CARTESIAN_POINT('Ctrl Pts',(-30.900622167269,63.6863012697328,12.));
#95716=CARTESIAN_POINT('Ctrl Pts',(-30.9152921936465,63.7020265004792,0.));
#95717=CARTESIAN_POINT('Ctrl Pts',(-30.9152921936465,63.7020265004792,12.));
#95718=CARTESIAN_POINT('Ctrl Pts',(-30.9300115747115,63.7177720601609,0.));
#95719=CARTESIAN_POINT('Ctrl Pts',(-30.9300115747115,63.7177720601609,12.));
#95720=CARTESIAN_POINT('Ctrl Pts',(-30.9447802599355,63.7335377837441,0.));
#95721=CARTESIAN_POINT('Ctrl Pts',(-30.9447802599355,63.7335377837441,12.));
#95722=CARTESIAN_POINT('Ctrl Pts',(-30.9595981989104,63.749323506987,0.));
#95723=CARTESIAN_POINT('Ctrl Pts',(-30.9595981989104,63.749323506987,12.));
#95724=CARTESIAN_POINT('Ctrl Pts',(-30.9744653413689,63.7651290664733,0.));
#95725=CARTESIAN_POINT('Ctrl Pts',(-30.9744653413689,63.7651290664733,12.));
#95726=CARTESIAN_POINT('Ctrl Pts',(-30.989381637191,63.7809542996264,0.));
#95727=CARTESIAN_POINT('Ctrl Pts',(-30.989381637191,63.7809542996264,12.));
#95728=CARTESIAN_POINT('Ctrl Pts',(-31.0043470364108,63.796799044728,0.));
#95729=CARTESIAN_POINT('Ctrl Pts',(-31.0043470364108,63.796799044728,12.));
#95730=CARTESIAN_POINT('Ctrl Pts',(-31.0193614892171,63.8126631409364,0.));
#95731=CARTESIAN_POINT('Ctrl Pts',(-31.0193614892171,63.8126631409364,12.));
#95732=CARTESIAN_POINT('Ctrl Pts',(-31.0344249459538,63.8285464282846,0.));
#95733=CARTESIAN_POINT('Ctrl Pts',(-31.0344249459538,63.8285464282846,12.));
#95734=CARTESIAN_POINT('Ctrl Pts',(-31.0495373571215,63.8444487476611,0.));
#95735=CARTESIAN_POINT('Ctrl Pts',(-31.0495373571215,63.8444487476611,12.));
#95736=CARTESIAN_POINT('Ctrl Pts',(-31.0646986733723,63.8603699407922,0.));
#95737=CARTESIAN_POINT('Ctrl Pts',(-31.0646986733723,63.8603699407922,12.));
#95738=CARTESIAN_POINT('Ctrl Pts',(-31.0799088455041,63.8763098502237,0.));
#95739=CARTESIAN_POINT('Ctrl Pts',(-31.0799088455041,63.8763098502237,12.));
#95740=CARTESIAN_POINT('Ctrl Pts',(-31.0951678244455,63.8922683192964,0.));
#95741=CARTESIAN_POINT('Ctrl Pts',(-31.0951678244455,63.8922683192964,12.));
#95742=CARTESIAN_POINT('Ctrl Pts',(-31.1104755612607,63.9082451921448,0.));
#95743=CARTESIAN_POINT('Ctrl Pts',(-31.1104755612607,63.9082451921448,12.));
#95744=CARTESIAN_POINT('Ctrl Pts',(-31.1258320071545,63.9242403136955,0.));
#95745=CARTESIAN_POINT('Ctrl Pts',(-31.1258320071545,63.9242403136955,12.));
#95746=CARTESIAN_POINT('Ctrl Pts',(-31.1412371134727,63.940253529665,0.));
#95747=CARTESIAN_POINT('Ctrl Pts',(-31.1412371134727,63.940253529665,12.));
#95748=CARTESIAN_POINT('Ctrl Pts',(-31.1566908316992,63.9562846865567,0.));
#95749=CARTESIAN_POINT('Ctrl Pts',(-31.1566908316992,63.9562846865567,12.));
#95750=CARTESIAN_POINT('Ctrl Pts',(-31.1721931134487,63.9723336316551,0.));
#95751=CARTESIAN_POINT('Ctrl Pts',(-31.1721931134487,63.9723336316551,12.));
#95752=CARTESIAN_POINT('Ctrl Pts',(-31.1877439104717,63.9884002130211,0.));
#95753=CARTESIAN_POINT('Ctrl Pts',(-31.1877439104717,63.9884002130211,12.));
#95754=CARTESIAN_POINT('Ctrl Pts',(-31.2033431746558,64.0044842794831,0.));
#95755=CARTESIAN_POINT('Ctrl Pts',(-31.2033431746558,64.0044842794831,12.));
#95756=CARTESIAN_POINT('Ctrl Pts',(-31.2189908580245,64.02058568063,0.));
#95757=CARTESIAN_POINT('Ctrl Pts',(-31.2189908580245,64.02058568063,12.));
#95758=CARTESIAN_POINT('Ctrl Pts',(-31.2346869127297,64.0367042667984,0.));
#95759=CARTESIAN_POINT('Ctrl Pts',(-31.2346869127297,64.0367042667984,12.));
#95760=CARTESIAN_POINT('Ctrl Pts',(-31.2504312910451,64.0528398890657,0.));
#95761=CARTESIAN_POINT('Ctrl Pts',(-31.2504312910451,64.0528398890657,12.));
#95762=CARTESIAN_POINT('Ctrl Pts',(-31.2662239453728,64.0689923992461,0.));
#95763=CARTESIAN_POINT('Ctrl Pts',(-31.2662239453728,64.0689923992461,12.));
#95764=CARTESIAN_POINT('Ctrl Pts',(-31.2820648282447,64.0851616498852,0.));
#95765=CARTESIAN_POINT('Ctrl Pts',(-31.2820648282447,64.0851616498852,12.));
#95766=CARTESIAN_POINT('Ctrl Pts',(-31.2979538923214,64.1013474942556,0.));
#95767=CARTESIAN_POINT('Ctrl Pts',(-31.2979538923214,64.1013474942556,12.));
#95768=CARTESIAN_POINT('Ctrl Pts',(-31.3138910903859,64.117549786349,0.));
#95769=CARTESIAN_POINT('Ctrl Pts',(-31.3138910903859,64.117549786349,12.));
#95770=CARTESIAN_POINT('Ctrl Pts',(-31.3298763753377,64.133768380869,0.));
#95771=CARTESIAN_POINT('Ctrl Pts',(-31.3298763753377,64.133768380869,12.));
#95772=CARTESIAN_POINT('Ctrl Pts',(-31.3459097002006,64.1500031332282,0.));
#95773=CARTESIAN_POINT('Ctrl Pts',(-31.3459097002006,64.1500031332282,12.));
#95774=CARTESIAN_POINT('Ctrl Pts',(-31.3619910181228,64.166253899542,0.));
#95775=CARTESIAN_POINT('Ctrl Pts',(-31.3619910181228,64.166253899542,12.));
#95776=CARTESIAN_POINT('Ctrl Pts',(-31.3781202823754,64.1825205366224,0.));
#95777=CARTESIAN_POINT('Ctrl Pts',(-31.3781202823754,64.1825205366224,12.));
#95778=CARTESIAN_POINT('Ctrl Pts',(-31.3942974463445,64.1988029019707,0.));
#95779=CARTESIAN_POINT('Ctrl Pts',(-31.3942974463445,64.1988029019707,12.));
#95780=CARTESIAN_POINT('Ctrl Pts',(-31.410522463528,64.2151008537697,0.));
#95781=CARTESIAN_POINT('Ctrl Pts',(-31.410522463528,64.2151008537697,12.));
#95782=CARTESIAN_POINT('Ctrl Pts',(-31.4267952875423,64.231414250881,0.));
#95783=CARTESIAN_POINT('Ctrl Pts',(-31.4267952875423,64.231414250881,12.));
#95784=CARTESIAN_POINT('Ctrl Pts',(-31.4431158721222,64.2477429528393,0.));
#95785=CARTESIAN_POINT('Ctrl Pts',(-31.4431158721222,64.2477429528393,12.));
#95786=CARTESIAN_POINT('Ctrl Pts',(-31.4594841711195,64.2640868198473,0.));
#95787=CARTESIAN_POINT('Ctrl Pts',(-31.4594841711195,64.2640868198473,12.));
#95788=CARTESIAN_POINT('Ctrl Pts',(-31.4759001384941,64.2804457127671,0.));
#95789=CARTESIAN_POINT('Ctrl Pts',(-31.4759001384941,64.2804457127671,12.));
#95790=CARTESIAN_POINT('Ctrl Pts',(-31.4923637283132,64.2968194931158,0.));
#95791=CARTESIAN_POINT('Ctrl Pts',(-31.4923637283132,64.2968194931158,12.));
#95792=CARTESIAN_POINT('Ctrl Pts',(-31.5088748947582,64.3132080230637,0.));
#95793=CARTESIAN_POINT('Ctrl Pts',(-31.5088748947582,64.3132080230637,12.));
#95794=CARTESIAN_POINT('Ctrl Pts',(-31.5254335921245,64.3296111654283,0.));
#95795=CARTESIAN_POINT('Ctrl Pts',(-31.5254335921245,64.3296111654283,12.));
#95796=CARTESIAN_POINT('Ctrl Pts',(-31.5420397748191,64.3460287836687,0.));
#95797=CARTESIAN_POINT('Ctrl Pts',(-31.5420397748191,64.3460287836687,12.));
#95798=CARTESIAN_POINT('Ctrl Pts',(-31.5586933973515,64.3624607418768,0.));
#95799=CARTESIAN_POINT('Ctrl Pts',(-31.5586933973515,64.3624607418768,12.));
#95800=CARTESIAN_POINT('Ctrl Pts',(-31.5753944143336,64.3789069047733,0.));
#95801=CARTESIAN_POINT('Ctrl Pts',(-31.5753944143336,64.3789069047733,12.));
#95802=CARTESIAN_POINT('Ctrl Pts',(-31.5921427804865,64.3953671377046,0.));
#95803=CARTESIAN_POINT('Ctrl Pts',(-31.5921427804865,64.3953671377046,12.));
#95804=CARTESIAN_POINT('Ctrl Pts',(-31.6089384506395,64.4118413066378,0.));
#95805=CARTESIAN_POINT('Ctrl Pts',(-31.6089384506395,64.4118413066378,12.));
#95806=CARTESIAN_POINT('Ctrl Pts',(-31.6257813797287,64.4283292781565,0.));
#95807=CARTESIAN_POINT('Ctrl Pts',(-31.6257813797287,64.4283292781565,12.));
#95808=CARTESIAN_POINT('Ctrl Pts',(-31.6426715227878,64.4448309194525,0.));
#95809=CARTESIAN_POINT('Ctrl Pts',(-31.6426715227878,64.4448309194525,12.));
#95810=CARTESIAN_POINT('Ctrl Pts',(-31.6596088349482,64.4613460983214,0.));
#95811=CARTESIAN_POINT('Ctrl Pts',(-31.6596088349482,64.4613460983214,12.));
#95812=CARTESIAN_POINT('Ctrl Pts',(-31.6765932714464,64.4778746831614,0.));
#95813=CARTESIAN_POINT('Ctrl Pts',(-31.6765932714464,64.4778746831614,12.));
#95814=CARTESIAN_POINT('Ctrl Pts',(-31.6936247876229,64.4944165429675,0.));
#95815=CARTESIAN_POINT('Ctrl Pts',(-31.6936247876229,64.4944165429675,12.));
#95816=CARTESIAN_POINT('Ctrl Pts',(-31.7107033389201,64.510971547327,0.));
#95817=CARTESIAN_POINT('Ctrl Pts',(-31.7107033389201,64.510971547327,12.));
#95818=CARTESIAN_POINT('Ctrl Pts',(-31.7278288808731,64.5275395664124,0.));
#95819=CARTESIAN_POINT('Ctrl Pts',(-31.7278288808731,64.5275395664124,12.));
#95820=CARTESIAN_POINT('Ctrl Pts',(-31.7450013691112,64.544120470977,0.));
#95821=CARTESIAN_POINT('Ctrl Pts',(-31.7450013691112,64.544120470977,12.));
#95822=CARTESIAN_POINT('Ctrl Pts',(-31.7622207593634,64.5607141323521,0.));
#95823=CARTESIAN_POINT('Ctrl Pts',(-31.7622207593634,64.5607141323521,12.));
#95824=CARTESIAN_POINT('Ctrl Pts',(-31.7794870074583,64.5773204224429,0.));
#95825=CARTESIAN_POINT('Ctrl Pts',(-31.7794870074583,64.5773204224429,12.));
#95826=CARTESIAN_POINT('Ctrl Pts',(-31.7968000693218,64.5939392137235,0.));
#95827=CARTESIAN_POINT('Ctrl Pts',(-31.7968000693218,64.5939392137235,12.));
#95828=CARTESIAN_POINT('Ctrl Pts',(-31.8141599009684,64.6105703792312,0.));
#95829=CARTESIAN_POINT('Ctrl Pts',(-31.8141599009684,64.6105703792312,12.));
#95830=CARTESIAN_POINT('Ctrl Pts',(-31.8315664585026,64.6272137925627,0.));
#95831=CARTESIAN_POINT('Ctrl Pts',(-31.8315664585026,64.6272137925627,12.));
#95832=CARTESIAN_POINT('Ctrl Pts',(-31.8490196981248,64.6438693278714,0.));
#95833=CARTESIAN_POINT('Ctrl Pts',(-31.8490196981248,64.6438693278714,12.));
#95834=CARTESIAN_POINT('Ctrl Pts',(-31.866519576131,64.6605368598629,0.));
#95835=CARTESIAN_POINT('Ctrl Pts',(-31.866519576131,64.6605368598629,12.));
#95836=CARTESIAN_POINT('Ctrl Pts',(-31.8840660489107,64.6772162637907,0.));
#95837=CARTESIAN_POINT('Ctrl Pts',(-31.8840660489107,64.6772162637907,12.));
#95838=CARTESIAN_POINT('Ctrl Pts',(-31.9016590729374,64.6939074154498,0.));
#95839=CARTESIAN_POINT('Ctrl Pts',(-31.9016590729374,64.6939074154498,12.));
#95840=CARTESIAN_POINT('Ctrl Pts',(-31.9192986047706,64.7106101911732,0.));
#95841=CARTESIAN_POINT('Ctrl Pts',(-31.9192986047706,64.7106101911732,12.));
#95842=CARTESIAN_POINT('Ctrl Pts',(-31.9369846010615,64.7273244678297,0.));
#95843=CARTESIAN_POINT('Ctrl Pts',(-31.9369846010615,64.7273244678297,12.));
#95844=CARTESIAN_POINT('Ctrl Pts',(-31.9547170185534,64.7440501228202,0.));
#95845=CARTESIAN_POINT('Ctrl Pts',(-31.9547170185534,64.7440501228202,12.));
#95846=CARTESIAN_POINT('Ctrl Pts',(-31.9724958140789,64.7607870340735,0.));
#95847=CARTESIAN_POINT('Ctrl Pts',(-31.9724958140789,64.7607870340735,12.));
#95848=CARTESIAN_POINT('Ctrl Pts',(-31.990320944552,64.77753508004,0.));
#95849=CARTESIAN_POINT('Ctrl Pts',(-31.990320944552,64.77753508004,12.));
#95850=CARTESIAN_POINT('Ctrl Pts',(-32.0081923669677,64.7942941396881,0.));
#95851=CARTESIAN_POINT('Ctrl Pts',(-32.0081923669677,64.7942941396881,12.));
#95852=CARTESIAN_POINT('Ctrl Pts',(-32.0261100384092,64.8110640925021,0.));
#95853=CARTESIAN_POINT('Ctrl Pts',(-32.0261100384092,64.8110640925021,12.));
#95854=CARTESIAN_POINT('Ctrl Pts',(-32.0440739160477,64.8278448184786,0.));
#95855=CARTESIAN_POINT('Ctrl Pts',(-32.0440739160477,64.8278448184786,12.));
#95856=CARTESIAN_POINT('Ctrl Pts',(-32.0620839571408,64.8446361981234,0.));
#95857=CARTESIAN_POINT('Ctrl Pts',(-32.0620839571408,64.8446361981234,12.));
#95858=CARTESIAN_POINT('Ctrl Pts',(-32.0801401190241,64.861438112445,0.));
#95859=CARTESIAN_POINT('Ctrl Pts',(-32.0801401190241,64.861438112445,12.));
#95860=CARTESIAN_POINT('Ctrl Pts',(-32.0982423591108,64.878250442952,0.));
#95861=CARTESIAN_POINT('Ctrl Pts',(-32.0982423591108,64.878250442952,12.));
#95862=CARTESIAN_POINT('Ctrl Pts',(-32.1163906348979,64.8950730716493,0.));
#95863=CARTESIAN_POINT('Ctrl Pts',(-32.1163906348979,64.8950730716493,12.));
#95864=CARTESIAN_POINT('Ctrl Pts',(-32.1345849039671,64.9119058810362,0.));
#95865=CARTESIAN_POINT('Ctrl Pts',(-32.1345849039671,64.9119058810362,12.));
#95866=CARTESIAN_POINT('Ctrl Pts',(-32.1528251239832,64.9287487541018,0.));
#95867=CARTESIAN_POINT('Ctrl Pts',(-32.1528251239832,64.9287487541018,12.));
#95868=CARTESIAN_POINT('Ctrl Pts',(-32.171111252686,64.9456015743203,0.));
#95869=CARTESIAN_POINT('Ctrl Pts',(-32.171111252686,64.9456015743203,12.));
#95870=CARTESIAN_POINT('Ctrl Pts',(-32.1894432478889,64.9624642256477,0.));
#95871=CARTESIAN_POINT('Ctrl Pts',(-32.1894432478889,64.9624642256477,12.));
#95872=CARTESIAN_POINT('Ctrl Pts',(-32.2078210674857,64.9793365925194,0.));
#95873=CARTESIAN_POINT('Ctrl Pts',(-32.2078210674857,64.9793365925194,12.));
#95874=CARTESIAN_POINT('Ctrl Pts',(-32.2262446694516,64.996218559847,0.));
#95875=CARTESIAN_POINT('Ctrl Pts',(-32.2262446694516,64.996218559847,12.));
#95876=CARTESIAN_POINT('Ctrl Pts',(-32.244714011842,65.0131100130155,0.));
#95877=CARTESIAN_POINT('Ctrl Pts',(-32.244714011842,65.0131100130155,12.));
#95878=CARTESIAN_POINT('Ctrl Pts',(-32.2632290527855,65.0300108378786,0.));
#95879=CARTESIAN_POINT('Ctrl Pts',(-32.2632290527855,65.0300108378786,12.));
#95880=CARTESIAN_POINT('Ctrl Pts',(-32.2817897504799,65.0469209207548,0.));
#95881=CARTESIAN_POINT('Ctrl Pts',(-32.2817897504799,65.0469209207548,12.));
#95882=CARTESIAN_POINT('Ctrl Pts',(-32.3003960632,65.0638401484245,0.));
#95883=CARTESIAN_POINT('Ctrl Pts',(-32.3003960632,65.0638401484245,12.));
#95884=CARTESIAN_POINT('Ctrl Pts',(-32.3190479492985,65.0807684081278,0.));
#95885=CARTESIAN_POINT('Ctrl Pts',(-32.3190479492985,65.0807684081278,12.));
#95886=CARTESIAN_POINT('Ctrl Pts',(-32.3377453672052,65.097705587561,0.));
#95887=CARTESIAN_POINT('Ctrl Pts',(-32.3377453672052,65.097705587561,12.));
#95888=CARTESIAN_POINT('Ctrl Pts',(-32.3564882754212,65.1146515748723,0.));
#95889=CARTESIAN_POINT('Ctrl Pts',(-32.3564882754212,65.1146515748723,12.));
#95890=CARTESIAN_POINT('Ctrl Pts',(-32.3752766325135,65.1316062586586,0.));
#95891=CARTESIAN_POINT('Ctrl Pts',(-32.3752766325135,65.1316062586586,12.));
#95892=CARTESIAN_POINT('Ctrl Pts',(-32.3941103971218,65.1485695279628,0.));
#95893=CARTESIAN_POINT('Ctrl Pts',(-32.3941103971218,65.1485695279628,12.));
#95894=CARTESIAN_POINT('Ctrl Pts',(-32.4129895279612,65.165541272272,0.));
#95895=CARTESIAN_POINT('Ctrl Pts',(-32.4129895279612,65.165541272272,12.));
#95896=CARTESIAN_POINT('Ctrl Pts',(-32.4319139838212,65.182521381514,0.));
#95897=CARTESIAN_POINT('Ctrl Pts',(-32.4319139838212,65.182521381514,12.));
#95898=CARTESIAN_POINT('Ctrl Pts',(-32.4508837235613,65.1995097460546,0.));
#95899=CARTESIAN_POINT('Ctrl Pts',(-32.4508837235613,65.1995097460546,12.));
#95900=CARTESIAN_POINT('Ctrl Pts',(-32.4698987061037,65.2165062566936,0.));
#95901=CARTESIAN_POINT('Ctrl Pts',(-32.4698987061037,65.2165062566936,12.));
#95902=CARTESIAN_POINT('Ctrl Pts',(-32.4889588904397,65.2335108046625,0.));
#95903=CARTESIAN_POINT('Ctrl Pts',(-32.4889588904397,65.2335108046625,12.));
#95904=CARTESIAN_POINT('Ctrl Pts',(-32.508064235633,65.2505232816215,0.));
#95905=CARTESIAN_POINT('Ctrl Pts',(-32.508064235633,65.2505232816215,12.));
#95906=CARTESIAN_POINT('Ctrl Pts',(-32.5272147008191,65.2675435796558,0.));
#95907=CARTESIAN_POINT('Ctrl Pts',(-32.5272147008191,65.2675435796558,12.));
#95908=CARTESIAN_POINT('Ctrl Pts',(-32.5464102452013,65.2845715912717,0.));
#95909=CARTESIAN_POINT('Ctrl Pts',(-32.5464102452013,65.2845715912717,12.));
#95910=CARTESIAN_POINT('Ctrl Pts',(-32.565650828042,65.3016072093907,0.));
#95911=CARTESIAN_POINT('Ctrl Pts',(-32.565650828042,65.3016072093907,12.));
#95912=CARTESIAN_POINT('Ctrl Pts',(-32.5849364086679,65.3186503273498,0.));
#95913=CARTESIAN_POINT('Ctrl Pts',(-32.5849364086679,65.3186503273498,12.));
#95914=CARTESIAN_POINT('Ctrl Pts',(-32.6042669464752,65.3357008389004,0.));
#95915=CARTESIAN_POINT('Ctrl Pts',(-32.6042669464752,65.3357008389004,12.));
#95916=CARTESIAN_POINT('Ctrl Pts',(-32.6236424009302,65.3527586382082,0.));
#95917=CARTESIAN_POINT('Ctrl Pts',(-32.6236424009302,65.3527586382082,12.));
#95918=CARTESIAN_POINT('Ctrl Pts',(-32.6430627315673,65.3698236198511,0.));
#95919=CARTESIAN_POINT('Ctrl Pts',(-32.6430627315673,65.3698236198511,12.));
#95920=CARTESIAN_POINT('Ctrl Pts',(-32.6625278979807,65.3868956788178,0.));
#95921=CARTESIAN_POINT('Ctrl Pts',(-32.6625278979807,65.3868956788178,12.));
#95922=CARTESIAN_POINT('Ctrl Pts',(-32.6820378598262,65.4039747105033,0.));
#95923=CARTESIAN_POINT('Ctrl Pts',(-32.6820378598262,65.4039747105033,12.));
#95924=CARTESIAN_POINT('Ctrl Pts',(-32.7015925768261,65.4210606107029,0.));
#95925=CARTESIAN_POINT('Ctrl Pts',(-32.7015925768261,65.4210606107029,12.));
#95926=CARTESIAN_POINT('Ctrl Pts',(-32.7211920087682,65.4381532756062,0.));
#95927=CARTESIAN_POINT('Ctrl Pts',(-32.7211920087682,65.4381532756062,12.));
#95928=CARTESIAN_POINT('Ctrl Pts',(-32.7408361155038,65.4552526017907,0.));
#95929=CARTESIAN_POINT('Ctrl Pts',(-32.7408361155038,65.4552526017907,12.));
#95930=CARTESIAN_POINT('Ctrl Pts',(-32.7605248569382,65.4723584862129,0.));
#95931=CARTESIAN_POINT('Ctrl Pts',(-32.7605248569382,65.4723584862129,12.));
#95932=CARTESIAN_POINT('Ctrl Pts',(-32.7802581930293,65.4894708262071,0.));
#95933=CARTESIAN_POINT('Ctrl Pts',(-32.7802581930293,65.4894708262071,12.));
#95934=CARTESIAN_POINT('Ctrl Pts',(-32.8000360837981,65.5065895194938,0.));
#95935=CARTESIAN_POINT('Ctrl Pts',(-32.8000360837981,65.5065895194938,12.));
#95936=CARTESIAN_POINT('Ctrl Pts',(-32.8198584893319,65.5237144641864,0.));
#95937=CARTESIAN_POINT('Ctrl Pts',(-32.8198584893319,65.5237144641864,12.));
#95938=CARTESIAN_POINT('Ctrl Pts',(-32.8397253697864,65.5408455587963,0.));
#95939=CARTESIAN_POINT('Ctrl Pts',(-32.8397253697864,65.5408455587963,12.));
#95940=CARTESIAN_POINT('Ctrl Pts',(-32.8596366853826,65.5579827022412,0.));
#95941=CARTESIAN_POINT('Ctrl Pts',(-32.8596366853826,65.5579827022412,12.));
#95942=CARTESIAN_POINT('Ctrl Pts',(-32.8795923964022,65.575125793846,0.));
#95943=CARTESIAN_POINT('Ctrl Pts',(-32.8795923964022,65.575125793846,12.));
#95944=CARTESIAN_POINT('Ctrl Pts',(-32.899592463189,65.5922747333181,0.));
#95945=CARTESIAN_POINT('Ctrl Pts',(-32.899592463189,65.5922747333181,12.));
#95946=CARTESIAN_POINT('Ctrl Pts',(-32.9196368461457,65.6094294207267,0.));
#95947=CARTESIAN_POINT('Ctrl Pts',(-32.9196368461457,65.6094294207267,12.));
#95948=CARTESIAN_POINT('Ctrl Pts',(-32.9397255057273,65.6265897564782,0.));
#95949=CARTESIAN_POINT('Ctrl Pts',(-32.9397255057273,65.6265897564782,12.));
#95950=CARTESIAN_POINT('Ctrl Pts',(-32.9598584024318,65.6437556412956,0.));
#95951=CARTESIAN_POINT('Ctrl Pts',(-32.9598584024318,65.6437556412956,12.));
#95952=CARTESIAN_POINT('Ctrl Pts',(-32.9800354967847,65.6609269761902,0.));
#95953=CARTESIAN_POINT('Ctrl Pts',(-32.9800354967847,65.6609269761902,12.));
#95954=CARTESIAN_POINT('Ctrl Pts',(-33.0002567493581,65.6781036625041,0.));
#95955=CARTESIAN_POINT('Ctrl Pts',(-33.0002567493581,65.6781036625041,12.));
#95956=CARTESIAN_POINT('Ctrl Pts',(-33.0205221207877,65.6952856019542,0.));
#95957=CARTESIAN_POINT('Ctrl Pts',(-33.0205221207877,65.6952856019542,12.));
#95958=CARTESIAN_POINT('Ctrl Pts',(-33.0408315717874,65.7124726966805,0.));
#95959=CARTESIAN_POINT('Ctrl Pts',(-33.0408315717874,65.7124726966805,12.));
#95960=CARTESIAN_POINT('Ctrl Pts',(-33.061185063158,65.729664849282,0.));
#95961=CARTESIAN_POINT('Ctrl Pts',(-33.061185063158,65.729664849282,12.));
#95962=CARTESIAN_POINT('Ctrl Pts',(-33.0815825557976,65.7468619628808,0.));
#95963=CARTESIAN_POINT('Ctrl Pts',(-33.0815825557976,65.7468619628808,12.));
#95964=CARTESIAN_POINT('Ctrl Pts',(-33.102024010688,65.7640639410653,0.));
#95965=CARTESIAN_POINT('Ctrl Pts',(-33.102024010688,65.7640639410653,12.));
#95966=CARTESIAN_POINT('Ctrl Pts',(-33.1225093888669,65.7812706877691,0.));
#95967=CARTESIAN_POINT('Ctrl Pts',(-33.1225093888669,65.7812706877691,12.));
#95968=CARTESIAN_POINT('Ctrl Pts',(-33.1430386513975,65.7984821071621,0.));
#95969=CARTESIAN_POINT('Ctrl Pts',(-33.1430386513975,65.7984821071621,12.));
#95970=CARTESIAN_POINT('Ctrl Pts',(-33.16361175934,65.8156981035504,0.));
#95971=CARTESIAN_POINT('Ctrl Pts',(-33.16361175934,65.8156981035504,12.));
#95972=CARTESIAN_POINT('Ctrl Pts',(-33.1842286737053,65.8329185812379,0.));
#95973=CARTESIAN_POINT('Ctrl Pts',(-33.1842286737053,65.8329185812379,12.));
#95974=CARTESIAN_POINT('Ctrl Pts',(-33.2048893554496,65.8501434445174,0.));
#95975=CARTESIAN_POINT('Ctrl Pts',(-33.2048893554496,65.8501434445174,12.));
#95976=CARTESIAN_POINT('Ctrl Pts',(-33.2255937655656,65.8673725979591,0.));
#95977=CARTESIAN_POINT('Ctrl Pts',(-33.2255937655656,65.8673725979591,12.));
#95978=CARTESIAN_POINT('Ctrl Pts',(-33.2463418651498,65.8846059466382,0.));
#95979=CARTESIAN_POINT('Ctrl Pts',(-33.2463418651498,65.8846059466382,12.));
#95980=CARTESIAN_POINT('Ctrl Pts',(-33.2671336154754,65.901843396389,0.));
#95981=CARTESIAN_POINT('Ctrl Pts',(-33.2671336154754,65.901843396389,12.));
#95982=CARTESIAN_POINT('Ctrl Pts',(-33.2879689780566,65.9190848540422,0.));
#95983=CARTESIAN_POINT('Ctrl Pts',(-33.2879689780566,65.9190848540422,12.));
#95984=CARTESIAN_POINT('Ctrl Pts',(-33.3088479147151,65.9363302276822,0.));
#95985=CARTESIAN_POINT('Ctrl Pts',(-33.3088479147151,65.9363302276822,12.));
#95986=CARTESIAN_POINT('Ctrl Pts',(-33.3297703874249,65.9535794260802,0.));
#95987=CARTESIAN_POINT('Ctrl Pts',(-33.3297703874249,65.9535794260802,12.));
#95988=CARTESIAN_POINT('Ctrl Pts',(-33.3507363581579,65.9708323581385,0.));
#95989=CARTESIAN_POINT('Ctrl Pts',(-33.3507363581579,65.9708323581385,12.));
#95990=CARTESIAN_POINT('Ctrl Pts',(-33.3717457887095,65.9880889322822,0.));
#95991=CARTESIAN_POINT('Ctrl Pts',(-33.3717457887095,65.9880889322822,12.));
#95992=CARTESIAN_POINT('Ctrl Pts',(-33.3927986405612,66.0053490559826,0.));
#95993=CARTESIAN_POINT('Ctrl Pts',(-33.3927986405612,66.0053490559826,12.));
#95994=CARTESIAN_POINT('Ctrl Pts',(-33.4138948746408,66.0226126349482,0.));
#95995=CARTESIAN_POINT('Ctrl Pts',(-33.4138948746408,66.0226126349482,12.));
#95996=CARTESIAN_POINT('Ctrl Pts',(-33.4350344515128,66.0398795737827,0.));
#95997=CARTESIAN_POINT('Ctrl Pts',(-33.4350344515128,66.0398795737827,12.));
#95998=CARTESIAN_POINT('Ctrl Pts',(-33.4562173318053,66.0571497774484,0.));
#95999=CARTESIAN_POINT('Ctrl Pts',(-33.4562173318053,66.0571497774484,12.));
#96000=CARTESIAN_POINT('Ctrl Pts',(-33.4774434765762,66.0744231525445,0.));
#96001=CARTESIAN_POINT('Ctrl Pts',(-33.4774434765762,66.0744231525445,12.));
#96002=CARTESIAN_POINT('Ctrl Pts',(-33.4987128476618,66.0916996085237,0.));
#96003=CARTESIAN_POINT('Ctrl Pts',(-33.4987128476618,66.0916996085237,12.));
#96004=CARTESIAN_POINT('Ctrl Pts',(-33.5200254081212,66.1089790592673,0.));
#96005=CARTESIAN_POINT('Ctrl Pts',(-33.5200254081212,66.1089790592673,12.));
#96006=CARTESIAN_POINT('Ctrl Pts',(-33.5413811223398,66.1262614234579,0.));
#96007=CARTESIAN_POINT('Ctrl Pts',(-33.5413811223398,66.1262614234579,12.));
#96008=CARTESIAN_POINT('Ctrl Pts',(-33.5627799550422,66.1435466210966,0.));
#96009=CARTESIAN_POINT('Ctrl Pts',(-33.5627799550422,66.1435466210966,12.));
#96010=CARTESIAN_POINT('Ctrl Pts',(-33.5842218705103,66.1608345707552,0.));
#96011=CARTESIAN_POINT('Ctrl Pts',(-33.5842218705103,66.1608345707552,12.));
#96012=CARTESIAN_POINT('Ctrl Pts',(-33.6057068316758,66.1781251863998,0.));
#96013=CARTESIAN_POINT('Ctrl Pts',(-33.6057068316758,66.1781251863998,12.));
#96014=CARTESIAN_POINT('Ctrl Pts',(-33.6272347993519,66.1954183747167,0.));
#96015=CARTESIAN_POINT('Ctrl Pts',(-33.6272347993519,66.1954183747167,12.));
#96016=CARTESIAN_POINT('Ctrl Pts',(-33.648805731163,66.2127140313777,0.));
#96017=CARTESIAN_POINT('Ctrl Pts',(-33.648805731163,66.2127140313777,12.));
#96018=CARTESIAN_POINT('Ctrl Pts',(-33.6704195830526,66.2300120464323,0.));
#96019=CARTESIAN_POINT('Ctrl Pts',(-33.6704195830526,66.2300120464323,12.));
#96020=CARTESIAN_POINT('Ctrl Pts',(-33.6920763111575,66.2473123109626,0.));
#96021=CARTESIAN_POINT('Ctrl Pts',(-33.6920763111575,66.2473123109626,12.));
#96022=CARTESIAN_POINT('Ctrl Pts',(-33.713775873597,66.2646147235444,0.));
#96023=CARTESIAN_POINT('Ctrl Pts',(-33.713775873597,66.2646147235444,12.));
#96024=CARTESIAN_POINT('Ctrl Pts',(-33.7355182321862,66.2819191962273,0.));
#96025=CARTESIAN_POINT('Ctrl Pts',(-33.7355182321862,66.2819191962273,12.));
#96026=CARTESIAN_POINT('Ctrl Pts',(-33.7573033544374,66.2992256621001,0.));
#96027=CARTESIAN_POINT('Ctrl Pts',(-33.7573033544374,66.2992256621001,12.));
#96028=CARTESIAN_POINT('Ctrl Pts',(-33.7791312144798,66.3165340771053,0.));
#96029=CARTESIAN_POINT('Ctrl Pts',(-33.7791312144798,66.3165340771053,12.));
#96030=CARTESIAN_POINT('Ctrl Pts',(-33.8010017925666,66.3338444143559,0.));
#96031=CARTESIAN_POINT('Ctrl Pts',(-33.8010017925666,66.3338444143559,12.));
#96032=CARTESIAN_POINT('Ctrl Pts',(-33.8185324184602,66.3476942111456,0.));
#96033=CARTESIAN_POINT('Ctrl Pts',(-33.8185324184602,66.3476942111456,12.));
#96034=CARTESIAN_POINT('Ctrl Pts',(-33.831699601175,66.3580824155565,0.));
#96035=CARTESIAN_POINT('Ctrl Pts',(-33.831699601175,66.3580824155565,12.));
#96036=CARTESIAN_POINT('Ctrl Pts',(-33.8404862618803,66.3650082659593,0.));
#96037=CARTESIAN_POINT('Ctrl Pts',(-33.8404862618803,66.3650082659593,12.));
#96038=CARTESIAN_POINT('Ctrl Pts',(-33.8448817269567,66.3684712863594,0.));
#96039=CARTESIAN_POINT('Ctrl Pts',(-33.8448817269567,66.3684712863594,12.));
#96040=CARTESIAN_POINT('',(-30.3549065457811,63.0759831361898,0.));
#96041=CARTESIAN_POINT('Ctrl Pts',(-30.3549065457811,63.0759831361898,0.));
#96042=CARTESIAN_POINT('Ctrl Pts',(-30.357431906933,63.078933570069,0.));
#96043=CARTESIAN_POINT('Ctrl Pts',(-30.3624877680651,63.0848371718048,0.));
#96044=CARTESIAN_POINT('Ctrl Pts',(-30.3700869762507,63.0937007763471,0.));
#96045=CARTESIAN_POINT('Ctrl Pts',(-30.3802500880403,63.105535320226,0.));
#96046=CARTESIAN_POINT('Ctrl Pts',(-30.3930053710484,63.1203558300657,0.));
#96047=CARTESIAN_POINT('Ctrl Pts',(-30.4058120432228,63.135203629844,0.));
#96048=CARTESIAN_POINT('Ctrl Pts',(-30.418670087563,63.1500786361459,0.));
#96049=CARTESIAN_POINT('Ctrl Pts',(-30.4315794659731,63.164980701691,0.));
#96050=CARTESIAN_POINT('Ctrl Pts',(-30.4445401192381,63.179909617189,0.));
#96051=CARTESIAN_POINT('Ctrl Pts',(-30.4575519763337,63.1948651386942,0.));
#96052=CARTESIAN_POINT('Ctrl Pts',(-30.470614961416,63.2098470086636,0.));
#96053=CARTESIAN_POINT('Ctrl Pts',(-30.4837290014989,63.2248549788221,0.));
#96054=CARTESIAN_POINT('Ctrl Pts',(-30.4968940344998,63.2398888342545,0.));
#96055=CARTESIAN_POINT('Ctrl Pts',(-30.5101100066659,63.2549483856215,0.));
#96056=CARTESIAN_POINT('Ctrl Pts',(-30.5233768687865,63.2700334577639,0.));
#96057=CARTESIAN_POINT('Ctrl Pts',(-30.5366945730508,63.2851438802473,0.));
#96058=CARTESIAN_POINT('Ctrl Pts',(-30.5500630691359,63.3002794756086,0.));
#96059=CARTESIAN_POINT('Ctrl Pts',(-30.563482302238,63.3154400534397,0.));
#96060=CARTESIAN_POINT('Ctrl Pts',(-30.5769522151164,63.3306254165126,0.));
#96061=CARTESIAN_POINT('Ctrl Pts',(-30.5904727493712,63.3458353646154,0.));
#96062=CARTESIAN_POINT('Ctrl Pts',(-30.6040438469078,63.3610696989577,0.));
#96063=CARTESIAN_POINT('Ctrl Pts',(-30.6176654515967,63.3763282271796,0.));
#96064=CARTESIAN_POINT('Ctrl Pts',(-30.6313375092062,63.3916107631376,0.));
#96065=CARTESIAN_POINT('Ctrl Pts',(-30.6450599666121,63.4069171245066,0.));
#96066=CARTESIAN_POINT('Ctrl Pts',(-30.6588327712484,63.4222471311239,0.));
#96067=CARTESIAN_POINT('Ctrl Pts',(-30.6726558704315,63.4376006029604,0.));
#96068=CARTESIAN_POINT('Ctrl Pts',(-30.6865292107929,63.4529773584249,0.));
#96069=CARTESIAN_POINT('Ctrl Pts',(-30.7004527385821,63.4683772152529,0.));
#96070=CARTESIAN_POINT('Ctrl Pts',(-30.7144263999265,63.4837999912771,0.));
#96071=CARTESIAN_POINT('Ctrl Pts',(-30.7284501410822,63.4992455051795,0.));
#96072=CARTESIAN_POINT('Ctrl Pts',(-30.7425239087281,63.5147135773894,0.));
#96073=CARTESIAN_POINT('Ctrl Pts',(-30.7566476500757,63.5302040304142,0.));
#96074=CARTESIAN_POINT('Ctrl Pts',(-30.7708213127159,63.5457166883537,0.));
#96075=CARTESIAN_POINT('Ctrl Pts',(-30.7850448445205,63.5612513766,0.));
#96076=CARTESIAN_POINT('Ctrl Pts',(-30.7993181935271,63.5768079214881,0.));
#96077=CARTESIAN_POINT('Ctrl Pts',(-30.813641307801,63.5923861498987,0.));
#96078=CARTESIAN_POINT('Ctrl Pts',(-30.8280141354459,63.6079858892771,0.));
#96079=CARTESIAN_POINT('Ctrl Pts',(-30.8424366246671,63.6236069678055,0.));
#96080=CARTESIAN_POINT('Ctrl Pts',(-30.8569087238131,63.6392492145233,0.));
#96081=CARTESIAN_POINT('Ctrl Pts',(-30.8714303814194,63.6549124594666,0.));
#96082=CARTESIAN_POINT('Ctrl Pts',(-30.8860015462475,63.6705965337971,0.));
#96083=CARTESIAN_POINT('Ctrl Pts',(-30.900622167269,63.6863012697328,0.));
#96084=CARTESIAN_POINT('Ctrl Pts',(-30.9152921936465,63.7020265004792,0.));
#96085=CARTESIAN_POINT('Ctrl Pts',(-30.9300115747115,63.7177720601609,0.));
#96086=CARTESIAN_POINT('Ctrl Pts',(-30.9447802599355,63.7335377837441,0.));
#96087=CARTESIAN_POINT('Ctrl Pts',(-30.9595981989104,63.749323506987,0.));
#96088=CARTESIAN_POINT('Ctrl Pts',(-30.9744653413689,63.7651290664733,0.));
#96089=CARTESIAN_POINT('Ctrl Pts',(-30.989381637191,63.7809542996264,0.));
#96090=CARTESIAN_POINT('Ctrl Pts',(-31.0043470364108,63.796799044728,0.));
#96091=CARTESIAN_POINT('Ctrl Pts',(-31.0193614892171,63.8126631409364,0.));
#96092=CARTESIAN_POINT('Ctrl Pts',(-31.0344249459538,63.8285464282846,0.));
#96093=CARTESIAN_POINT('Ctrl Pts',(-31.0495373571215,63.8444487476611,0.));
#96094=CARTESIAN_POINT('Ctrl Pts',(-31.0646986733723,63.8603699407922,0.));
#96095=CARTESIAN_POINT('Ctrl Pts',(-31.0799088455041,63.8763098502237,0.));
#96096=CARTESIAN_POINT('Ctrl Pts',(-31.0951678244455,63.8922683192964,0.));
#96097=CARTESIAN_POINT('Ctrl Pts',(-31.1104755612607,63.9082451921448,0.));
#96098=CARTESIAN_POINT('Ctrl Pts',(-31.1258320071545,63.9242403136955,0.));
#96099=CARTESIAN_POINT('Ctrl Pts',(-31.1412371134727,63.940253529665,0.));
#96100=CARTESIAN_POINT('Ctrl Pts',(-31.1566908316992,63.9562846865567,0.));
#96101=CARTESIAN_POINT('Ctrl Pts',(-31.1721931134487,63.9723336316551,0.));
#96102=CARTESIAN_POINT('Ctrl Pts',(-31.1877439104717,63.9884002130211,0.));
#96103=CARTESIAN_POINT('Ctrl Pts',(-31.2033431746558,64.0044842794831,0.));
#96104=CARTESIAN_POINT('Ctrl Pts',(-31.2189908580245,64.02058568063,0.));
#96105=CARTESIAN_POINT('Ctrl Pts',(-31.2346869127297,64.0367042667984,0.));
#96106=CARTESIAN_POINT('Ctrl Pts',(-31.2504312910451,64.0528398890657,0.));
#96107=CARTESIAN_POINT('Ctrl Pts',(-31.2662239453728,64.0689923992461,0.));
#96108=CARTESIAN_POINT('Ctrl Pts',(-31.2820648282447,64.0851616498852,0.));
#96109=CARTESIAN_POINT('Ctrl Pts',(-31.2979538923214,64.1013474942556,0.));
#96110=CARTESIAN_POINT('Ctrl Pts',(-31.3138910903859,64.117549786349,0.));
#96111=CARTESIAN_POINT('Ctrl Pts',(-31.3298763753377,64.133768380869,0.));
#96112=CARTESIAN_POINT('Ctrl Pts',(-31.3459097002006,64.1500031332282,0.));
#96113=CARTESIAN_POINT('Ctrl Pts',(-31.3619910181228,64.166253899542,0.));
#96114=CARTESIAN_POINT('Ctrl Pts',(-31.3781202823754,64.1825205366224,0.));
#96115=CARTESIAN_POINT('Ctrl Pts',(-31.3942974463445,64.1988029019707,0.));
#96116=CARTESIAN_POINT('Ctrl Pts',(-31.410522463528,64.2151008537697,0.));
#96117=CARTESIAN_POINT('Ctrl Pts',(-31.4267952875423,64.231414250881,0.));
#96118=CARTESIAN_POINT('Ctrl Pts',(-31.4431158721222,64.2477429528393,0.));
#96119=CARTESIAN_POINT('Ctrl Pts',(-31.4594841711195,64.2640868198473,0.));
#96120=CARTESIAN_POINT('Ctrl Pts',(-31.4759001384941,64.2804457127671,0.));
#96121=CARTESIAN_POINT('Ctrl Pts',(-31.4923637283132,64.2968194931158,0.));
#96122=CARTESIAN_POINT('Ctrl Pts',(-31.5088748947582,64.3132080230637,0.));
#96123=CARTESIAN_POINT('Ctrl Pts',(-31.5254335921245,64.3296111654283,0.));
#96124=CARTESIAN_POINT('Ctrl Pts',(-31.5420397748191,64.3460287836687,0.));
#96125=CARTESIAN_POINT('Ctrl Pts',(-31.5586933973515,64.3624607418768,0.));
#96126=CARTESIAN_POINT('Ctrl Pts',(-31.5753944143336,64.3789069047733,0.));
#96127=CARTESIAN_POINT('Ctrl Pts',(-31.5921427804865,64.3953671377046,0.));
#96128=CARTESIAN_POINT('Ctrl Pts',(-31.6089384506395,64.4118413066378,0.));
#96129=CARTESIAN_POINT('Ctrl Pts',(-31.6257813797287,64.4283292781565,0.));
#96130=CARTESIAN_POINT('Ctrl Pts',(-31.6426715227878,64.4448309194525,0.));
#96131=CARTESIAN_POINT('Ctrl Pts',(-31.6596088349482,64.4613460983214,0.));
#96132=CARTESIAN_POINT('Ctrl Pts',(-31.6765932714464,64.4778746831614,0.));
#96133=CARTESIAN_POINT('Ctrl Pts',(-31.6936247876229,64.4944165429675,0.));
#96134=CARTESIAN_POINT('Ctrl Pts',(-31.7107033389201,64.510971547327,0.));
#96135=CARTESIAN_POINT('Ctrl Pts',(-31.7278288808731,64.5275395664124,0.));
#96136=CARTESIAN_POINT('Ctrl Pts',(-31.7450013691112,64.544120470977,0.));
#96137=CARTESIAN_POINT('Ctrl Pts',(-31.7622207593634,64.5607141323521,0.));
#96138=CARTESIAN_POINT('Ctrl Pts',(-31.7794870074583,64.5773204224429,0.));
#96139=CARTESIAN_POINT('Ctrl Pts',(-31.7968000693218,64.5939392137235,0.));
#96140=CARTESIAN_POINT('Ctrl Pts',(-31.8141599009684,64.6105703792312,0.));
#96141=CARTESIAN_POINT('Ctrl Pts',(-31.8315664585026,64.6272137925627,0.));
#96142=CARTESIAN_POINT('Ctrl Pts',(-31.8490196981248,64.6438693278714,0.));
#96143=CARTESIAN_POINT('Ctrl Pts',(-31.866519576131,64.6605368598629,0.));
#96144=CARTESIAN_POINT('Ctrl Pts',(-31.8840660489107,64.6772162637907,0.));
#96145=CARTESIAN_POINT('Ctrl Pts',(-31.9016590729374,64.6939074154498,0.));
#96146=CARTESIAN_POINT('Ctrl Pts',(-31.9192986047706,64.7106101911732,0.));
#96147=CARTESIAN_POINT('Ctrl Pts',(-31.9369846010615,64.7273244678297,0.));
#96148=CARTESIAN_POINT('Ctrl Pts',(-31.9547170185534,64.7440501228202,0.));
#96149=CARTESIAN_POINT('Ctrl Pts',(-31.9724958140789,64.7607870340735,0.));
#96150=CARTESIAN_POINT('Ctrl Pts',(-31.990320944552,64.77753508004,0.));
#96151=CARTESIAN_POINT('Ctrl Pts',(-32.0081923669677,64.7942941396881,0.));
#96152=CARTESIAN_POINT('Ctrl Pts',(-32.0261100384092,64.8110640925021,0.));
#96153=CARTESIAN_POINT('Ctrl Pts',(-32.0440739160477,64.8278448184786,0.));
#96154=CARTESIAN_POINT('Ctrl Pts',(-32.0620839571408,64.8446361981234,0.));
#96155=CARTESIAN_POINT('Ctrl Pts',(-32.0801401190241,64.861438112445,0.));
#96156=CARTESIAN_POINT('Ctrl Pts',(-32.0982423591108,64.878250442952,0.));
#96157=CARTESIAN_POINT('Ctrl Pts',(-32.1163906348979,64.8950730716493,0.));
#96158=CARTESIAN_POINT('Ctrl Pts',(-32.1345849039671,64.9119058810362,0.));
#96159=CARTESIAN_POINT('Ctrl Pts',(-32.1528251239832,64.9287487541018,0.));
#96160=CARTESIAN_POINT('Ctrl Pts',(-32.171111252686,64.9456015743203,0.));
#96161=CARTESIAN_POINT('Ctrl Pts',(-32.1894432478889,64.9624642256477,0.));
#96162=CARTESIAN_POINT('Ctrl Pts',(-32.2078210674857,64.9793365925194,0.));
#96163=CARTESIAN_POINT('Ctrl Pts',(-32.2262446694516,64.996218559847,0.));
#96164=CARTESIAN_POINT('Ctrl Pts',(-32.244714011842,65.0131100130155,0.));
#96165=CARTESIAN_POINT('Ctrl Pts',(-32.2632290527855,65.0300108378786,0.));
#96166=CARTESIAN_POINT('Ctrl Pts',(-32.2817897504799,65.0469209207548,0.));
#96167=CARTESIAN_POINT('Ctrl Pts',(-32.3003960632,65.0638401484245,0.));
#96168=CARTESIAN_POINT('Ctrl Pts',(-32.3190479492985,65.0807684081278,0.));
#96169=CARTESIAN_POINT('Ctrl Pts',(-32.3377453672052,65.097705587561,0.));
#96170=CARTESIAN_POINT('Ctrl Pts',(-32.3564882754212,65.1146515748723,0.));
#96171=CARTESIAN_POINT('Ctrl Pts',(-32.3752766325135,65.1316062586586,0.));
#96172=CARTESIAN_POINT('Ctrl Pts',(-32.3941103971218,65.1485695279628,0.));
#96173=CARTESIAN_POINT('Ctrl Pts',(-32.4129895279612,65.165541272272,0.));
#96174=CARTESIAN_POINT('Ctrl Pts',(-32.4319139838212,65.182521381514,0.));
#96175=CARTESIAN_POINT('Ctrl Pts',(-32.4508837235613,65.1995097460546,0.));
#96176=CARTESIAN_POINT('Ctrl Pts',(-32.4698987061037,65.2165062566936,0.));
#96177=CARTESIAN_POINT('Ctrl Pts',(-32.4889588904397,65.2335108046625,0.));
#96178=CARTESIAN_POINT('Ctrl Pts',(-32.508064235633,65.2505232816215,0.));
#96179=CARTESIAN_POINT('Ctrl Pts',(-32.5272147008191,65.2675435796558,0.));
#96180=CARTESIAN_POINT('Ctrl Pts',(-32.5464102452013,65.2845715912717,0.));
#96181=CARTESIAN_POINT('Ctrl Pts',(-32.565650828042,65.3016072093907,0.));
#96182=CARTESIAN_POINT('Ctrl Pts',(-32.5849364086679,65.3186503273498,0.));
#96183=CARTESIAN_POINT('Ctrl Pts',(-32.6042669464752,65.3357008389004,0.));
#96184=CARTESIAN_POINT('Ctrl Pts',(-32.6236424009302,65.3527586382082,0.));
#96185=CARTESIAN_POINT('Ctrl Pts',(-32.6430627315673,65.3698236198511,0.));
#96186=CARTESIAN_POINT('Ctrl Pts',(-32.6625278979807,65.3868956788178,0.));
#96187=CARTESIAN_POINT('Ctrl Pts',(-32.6820378598262,65.4039747105033,0.));
#96188=CARTESIAN_POINT('Ctrl Pts',(-32.7015925768261,65.4210606107029,0.));
#96189=CARTESIAN_POINT('Ctrl Pts',(-32.7211920087682,65.4381532756062,0.));
#96190=CARTESIAN_POINT('Ctrl Pts',(-32.7408361155038,65.4552526017907,0.));
#96191=CARTESIAN_POINT('Ctrl Pts',(-32.7605248569382,65.4723584862129,0.));
#96192=CARTESIAN_POINT('Ctrl Pts',(-32.7802581930293,65.4894708262071,0.));
#96193=CARTESIAN_POINT('Ctrl Pts',(-32.8000360837981,65.5065895194938,0.));
#96194=CARTESIAN_POINT('Ctrl Pts',(-32.8198584893319,65.5237144641864,0.));
#96195=CARTESIAN_POINT('Ctrl Pts',(-32.8397253697864,65.5408455587963,0.));
#96196=CARTESIAN_POINT('Ctrl Pts',(-32.8596366853826,65.5579827022412,0.));
#96197=CARTESIAN_POINT('Ctrl Pts',(-32.8795923964022,65.575125793846,0.));
#96198=CARTESIAN_POINT('Ctrl Pts',(-32.899592463189,65.5922747333181,0.));
#96199=CARTESIAN_POINT('Ctrl Pts',(-32.9196368461457,65.6094294207267,0.));
#96200=CARTESIAN_POINT('Ctrl Pts',(-32.9397255057273,65.6265897564782,0.));
#96201=CARTESIAN_POINT('Ctrl Pts',(-32.9598584024318,65.6437556412956,0.));
#96202=CARTESIAN_POINT('Ctrl Pts',(-32.9800354967847,65.6609269761902,0.));
#96203=CARTESIAN_POINT('Ctrl Pts',(-33.0002567493581,65.6781036625041,0.));
#96204=CARTESIAN_POINT('Ctrl Pts',(-33.0205221207877,65.6952856019542,0.));
#96205=CARTESIAN_POINT('Ctrl Pts',(-33.0408315717874,65.7124726966805,0.));
#96206=CARTESIAN_POINT('Ctrl Pts',(-33.061185063158,65.729664849282,0.));
#96207=CARTESIAN_POINT('Ctrl Pts',(-33.0815825557976,65.7468619628808,0.));
#96208=CARTESIAN_POINT('Ctrl Pts',(-33.102024010688,65.7640639410653,0.));
#96209=CARTESIAN_POINT('Ctrl Pts',(-33.1225093888669,65.7812706877691,0.));
#96210=CARTESIAN_POINT('Ctrl Pts',(-33.1430386513975,65.7984821071621,0.));
#96211=CARTESIAN_POINT('Ctrl Pts',(-33.16361175934,65.8156981035504,0.));
#96212=CARTESIAN_POINT('Ctrl Pts',(-33.1842286737053,65.8329185812379,0.));
#96213=CARTESIAN_POINT('Ctrl Pts',(-33.2048893554496,65.8501434445174,0.));
#96214=CARTESIAN_POINT('Ctrl Pts',(-33.2255937655656,65.8673725979591,0.));
#96215=CARTESIAN_POINT('Ctrl Pts',(-33.2463418651498,65.8846059466382,0.));
#96216=CARTESIAN_POINT('Ctrl Pts',(-33.2671336154754,65.901843396389,0.));
#96217=CARTESIAN_POINT('Ctrl Pts',(-33.2879689780566,65.9190848540422,0.));
#96218=CARTESIAN_POINT('Ctrl Pts',(-33.3088479147151,65.9363302276822,0.));
#96219=CARTESIAN_POINT('Ctrl Pts',(-33.3297703874249,65.9535794260802,0.));
#96220=CARTESIAN_POINT('Ctrl Pts',(-33.3507363581579,65.9708323581385,0.));
#96221=CARTESIAN_POINT('Ctrl Pts',(-33.3717457887095,65.9880889322822,0.));
#96222=CARTESIAN_POINT('Ctrl Pts',(-33.3927986405612,66.0053490559826,0.));
#96223=CARTESIAN_POINT('Ctrl Pts',(-33.4138948746408,66.0226126349482,0.));
#96224=CARTESIAN_POINT('Ctrl Pts',(-33.4350344515128,66.0398795737827,0.));
#96225=CARTESIAN_POINT('Ctrl Pts',(-33.4562173318053,66.0571497774484,0.));
#96226=CARTESIAN_POINT('Ctrl Pts',(-33.4774434765762,66.0744231525445,0.));
#96227=CARTESIAN_POINT('Ctrl Pts',(-33.4987128476618,66.0916996085237,0.));
#96228=CARTESIAN_POINT('Ctrl Pts',(-33.5200254081212,66.1089790592673,0.));
#96229=CARTESIAN_POINT('Ctrl Pts',(-33.5413811223398,66.1262614234579,0.));
#96230=CARTESIAN_POINT('Ctrl Pts',(-33.5597240685729,66.1410781873125,0.));
#96231=CARTESIAN_POINT('Ctrl Pts',(-33.5738105077707,66.1524393973986,0.));
#96232=CARTESIAN_POINT('Ctrl Pts',(-33.5836213513974,66.1603438177306,0.));
#96233=CARTESIAN_POINT('Ctrl Pts',(-33.5891439876228,66.1647906582409,0.));
#96234=CARTESIAN_POINT('Ctrl Pts',(-33.5903722664959,66.165779540567,0.));
#96235=CARTESIAN_POINT('',(-30.3549065457811,63.0759831361898,12.));
#96236=CARTESIAN_POINT('',(-30.3549065457811,63.0759831361898,0.));
#96237=CARTESIAN_POINT('Ctrl Pts',(-33.590372266496,66.1657795405671,12.));
#96238=CARTESIAN_POINT('Ctrl Pts',(-33.5891439876229,66.164790658241,12.));
#96239=CARTESIAN_POINT('Ctrl Pts',(-33.5836213513975,66.1603438177307,12.));
#96240=CARTESIAN_POINT('Ctrl Pts',(-33.5738105077708,66.1524393973986,12.));
#96241=CARTESIAN_POINT('Ctrl Pts',(-33.5597240685729,66.1410781873125,12.));
#96242=CARTESIAN_POINT('Ctrl Pts',(-33.5413811223398,66.1262614234579,12.));
#96243=CARTESIAN_POINT('Ctrl Pts',(-33.5200254081212,66.1089790592673,12.));
#96244=CARTESIAN_POINT('Ctrl Pts',(-33.4987128476618,66.0916996085237,12.));
#96245=CARTESIAN_POINT('Ctrl Pts',(-33.4774434765762,66.0744231525445,12.));
#96246=CARTESIAN_POINT('Ctrl Pts',(-33.4562173318053,66.0571497774484,12.));
#96247=CARTESIAN_POINT('Ctrl Pts',(-33.4350344515128,66.0398795737827,12.));
#96248=CARTESIAN_POINT('Ctrl Pts',(-33.4138948746408,66.0226126349482,12.));
#96249=CARTESIAN_POINT('Ctrl Pts',(-33.3927986405612,66.0053490559826,12.));
#96250=CARTESIAN_POINT('Ctrl Pts',(-33.3717457887095,65.9880889322822,12.));
#96251=CARTESIAN_POINT('Ctrl Pts',(-33.3507363581579,65.9708323581385,12.));
#96252=CARTESIAN_POINT('Ctrl Pts',(-33.3297703874249,65.9535794260802,12.));
#96253=CARTESIAN_POINT('Ctrl Pts',(-33.3088479147151,65.9363302276822,12.));
#96254=CARTESIAN_POINT('Ctrl Pts',(-33.2879689780566,65.9190848540422,12.));
#96255=CARTESIAN_POINT('Ctrl Pts',(-33.2671336154754,65.901843396389,12.));
#96256=CARTESIAN_POINT('Ctrl Pts',(-33.2463418651498,65.8846059466382,12.));
#96257=CARTESIAN_POINT('Ctrl Pts',(-33.2255937655656,65.8673725979591,12.));
#96258=CARTESIAN_POINT('Ctrl Pts',(-33.2048893554496,65.8501434445174,12.));
#96259=CARTESIAN_POINT('Ctrl Pts',(-33.1842286737053,65.8329185812379,12.));
#96260=CARTESIAN_POINT('Ctrl Pts',(-33.16361175934,65.8156981035504,12.));
#96261=CARTESIAN_POINT('Ctrl Pts',(-33.1430386513975,65.7984821071621,12.));
#96262=CARTESIAN_POINT('Ctrl Pts',(-33.1225093888669,65.7812706877691,12.));
#96263=CARTESIAN_POINT('Ctrl Pts',(-33.102024010688,65.7640639410653,12.));
#96264=CARTESIAN_POINT('Ctrl Pts',(-33.0815825557976,65.7468619628808,12.));
#96265=CARTESIAN_POINT('Ctrl Pts',(-33.061185063158,65.729664849282,12.));
#96266=CARTESIAN_POINT('Ctrl Pts',(-33.0408315717874,65.7124726966805,12.));
#96267=CARTESIAN_POINT('Ctrl Pts',(-33.0205221207877,65.6952856019542,12.));
#96268=CARTESIAN_POINT('Ctrl Pts',(-33.0002567493581,65.6781036625041,12.));
#96269=CARTESIAN_POINT('Ctrl Pts',(-32.9800354967847,65.6609269761902,12.));
#96270=CARTESIAN_POINT('Ctrl Pts',(-32.9598584024318,65.6437556412956,12.));
#96271=CARTESIAN_POINT('Ctrl Pts',(-32.9397255057273,65.6265897564782,12.));
#96272=CARTESIAN_POINT('Ctrl Pts',(-32.9196368461457,65.6094294207267,12.));
#96273=CARTESIAN_POINT('Ctrl Pts',(-32.899592463189,65.5922747333181,12.));
#96274=CARTESIAN_POINT('Ctrl Pts',(-32.8795923964022,65.575125793846,12.));
#96275=CARTESIAN_POINT('Ctrl Pts',(-32.8596366853826,65.5579827022412,12.));
#96276=CARTESIAN_POINT('Ctrl Pts',(-32.8397253697864,65.5408455587963,12.));
#96277=CARTESIAN_POINT('Ctrl Pts',(-32.8198584893319,65.5237144641864,12.));
#96278=CARTESIAN_POINT('Ctrl Pts',(-32.8000360837981,65.5065895194938,12.));
#96279=CARTESIAN_POINT('Ctrl Pts',(-32.7802581930293,65.4894708262071,12.));
#96280=CARTESIAN_POINT('Ctrl Pts',(-32.7605248569382,65.4723584862129,12.));
#96281=CARTESIAN_POINT('Ctrl Pts',(-32.7408361155038,65.4552526017907,12.));
#96282=CARTESIAN_POINT('Ctrl Pts',(-32.7211920087682,65.4381532756062,12.));
#96283=CARTESIAN_POINT('Ctrl Pts',(-32.7015925768261,65.4210606107029,12.));
#96284=CARTESIAN_POINT('Ctrl Pts',(-32.6820378598262,65.4039747105033,12.));
#96285=CARTESIAN_POINT('Ctrl Pts',(-32.6625278979807,65.3868956788178,12.));
#96286=CARTESIAN_POINT('Ctrl Pts',(-32.6430627315673,65.3698236198511,12.));
#96287=CARTESIAN_POINT('Ctrl Pts',(-32.6236424009302,65.3527586382082,12.));
#96288=CARTESIAN_POINT('Ctrl Pts',(-32.6042669464752,65.3357008389004,12.));
#96289=CARTESIAN_POINT('Ctrl Pts',(-32.5849364086679,65.3186503273498,12.));
#96290=CARTESIAN_POINT('Ctrl Pts',(-32.565650828042,65.3016072093907,12.));
#96291=CARTESIAN_POINT('Ctrl Pts',(-32.5464102452013,65.2845715912717,12.));
#96292=CARTESIAN_POINT('Ctrl Pts',(-32.5272147008191,65.2675435796558,12.));
#96293=CARTESIAN_POINT('Ctrl Pts',(-32.508064235633,65.2505232816215,12.));
#96294=CARTESIAN_POINT('Ctrl Pts',(-32.4889588904397,65.2335108046625,12.));
#96295=CARTESIAN_POINT('Ctrl Pts',(-32.4698987061037,65.2165062566936,12.));
#96296=CARTESIAN_POINT('Ctrl Pts',(-32.4508837235613,65.1995097460546,12.));
#96297=CARTESIAN_POINT('Ctrl Pts',(-32.4319139838212,65.182521381514,12.));
#96298=CARTESIAN_POINT('Ctrl Pts',(-32.4129895279612,65.165541272272,12.));
#96299=CARTESIAN_POINT('Ctrl Pts',(-32.3941103971218,65.1485695279628,12.));
#96300=CARTESIAN_POINT('Ctrl Pts',(-32.3752766325135,65.1316062586586,12.));
#96301=CARTESIAN_POINT('Ctrl Pts',(-32.3564882754212,65.1146515748723,12.));
#96302=CARTESIAN_POINT('Ctrl Pts',(-32.3377453672052,65.097705587561,12.));
#96303=CARTESIAN_POINT('Ctrl Pts',(-32.3190479492985,65.0807684081278,12.));
#96304=CARTESIAN_POINT('Ctrl Pts',(-32.3003960632,65.0638401484245,12.));
#96305=CARTESIAN_POINT('Ctrl Pts',(-32.2817897504799,65.0469209207548,12.));
#96306=CARTESIAN_POINT('Ctrl Pts',(-32.2632290527855,65.0300108378786,12.));
#96307=CARTESIAN_POINT('Ctrl Pts',(-32.244714011842,65.0131100130155,12.));
#96308=CARTESIAN_POINT('Ctrl Pts',(-32.2262446694516,64.996218559847,12.));
#96309=CARTESIAN_POINT('Ctrl Pts',(-32.2078210674857,64.9793365925194,12.));
#96310=CARTESIAN_POINT('Ctrl Pts',(-32.1894432478889,64.9624642256477,12.));
#96311=CARTESIAN_POINT('Ctrl Pts',(-32.171111252686,64.9456015743203,12.));
#96312=CARTESIAN_POINT('Ctrl Pts',(-32.1528251239832,64.9287487541018,12.));
#96313=CARTESIAN_POINT('Ctrl Pts',(-32.1345849039671,64.9119058810362,12.));
#96314=CARTESIAN_POINT('Ctrl Pts',(-32.1163906348979,64.8950730716493,12.));
#96315=CARTESIAN_POINT('Ctrl Pts',(-32.0982423591108,64.878250442952,12.));
#96316=CARTESIAN_POINT('Ctrl Pts',(-32.0801401190241,64.861438112445,12.));
#96317=CARTESIAN_POINT('Ctrl Pts',(-32.0620839571408,64.8446361981234,12.));
#96318=CARTESIAN_POINT('Ctrl Pts',(-32.0440739160477,64.8278448184786,12.));
#96319=CARTESIAN_POINT('Ctrl Pts',(-32.0261100384092,64.8110640925021,12.));
#96320=CARTESIAN_POINT('Ctrl Pts',(-32.0081923669677,64.7942941396881,12.));
#96321=CARTESIAN_POINT('Ctrl Pts',(-31.990320944552,64.77753508004,12.));
#96322=CARTESIAN_POINT('Ctrl Pts',(-31.9724958140789,64.7607870340735,12.));
#96323=CARTESIAN_POINT('Ctrl Pts',(-31.9547170185534,64.7440501228202,12.));
#96324=CARTESIAN_POINT('Ctrl Pts',(-31.9369846010615,64.7273244678297,12.));
#96325=CARTESIAN_POINT('Ctrl Pts',(-31.9192986047706,64.7106101911732,12.));
#96326=CARTESIAN_POINT('Ctrl Pts',(-31.9016590729374,64.6939074154498,12.));
#96327=CARTESIAN_POINT('Ctrl Pts',(-31.8840660489107,64.6772162637907,12.));
#96328=CARTESIAN_POINT('Ctrl Pts',(-31.866519576131,64.6605368598629,12.));
#96329=CARTESIAN_POINT('Ctrl Pts',(-31.8490196981248,64.6438693278714,12.));
#96330=CARTESIAN_POINT('Ctrl Pts',(-31.8315664585026,64.6272137925627,12.));
#96331=CARTESIAN_POINT('Ctrl Pts',(-31.8141599009684,64.6105703792312,12.));
#96332=CARTESIAN_POINT('Ctrl Pts',(-31.7968000693218,64.5939392137235,12.));
#96333=CARTESIAN_POINT('Ctrl Pts',(-31.7794870074583,64.5773204224429,12.));
#96334=CARTESIAN_POINT('Ctrl Pts',(-31.7622207593634,64.5607141323521,12.));
#96335=CARTESIAN_POINT('Ctrl Pts',(-31.7450013691112,64.544120470977,12.));
#96336=CARTESIAN_POINT('Ctrl Pts',(-31.7278288808731,64.5275395664124,12.));
#96337=CARTESIAN_POINT('Ctrl Pts',(-31.7107033389201,64.510971547327,12.));
#96338=CARTESIAN_POINT('Ctrl Pts',(-31.6936247876229,64.4944165429675,12.));
#96339=CARTESIAN_POINT('Ctrl Pts',(-31.6765932714464,64.4778746831614,12.));
#96340=CARTESIAN_POINT('Ctrl Pts',(-31.6596088349482,64.4613460983214,12.));
#96341=CARTESIAN_POINT('Ctrl Pts',(-31.6426715227878,64.4448309194525,12.));
#96342=CARTESIAN_POINT('Ctrl Pts',(-31.6257813797287,64.4283292781565,12.));
#96343=CARTESIAN_POINT('Ctrl Pts',(-31.6089384506395,64.4118413066378,12.));
#96344=CARTESIAN_POINT('Ctrl Pts',(-31.5921427804865,64.3953671377046,12.));
#96345=CARTESIAN_POINT('Ctrl Pts',(-31.5753944143336,64.3789069047733,12.));
#96346=CARTESIAN_POINT('Ctrl Pts',(-31.5586933973515,64.3624607418768,12.));
#96347=CARTESIAN_POINT('Ctrl Pts',(-31.5420397748191,64.3460287836687,12.));
#96348=CARTESIAN_POINT('Ctrl Pts',(-31.5254335921245,64.3296111654283,12.));
#96349=CARTESIAN_POINT('Ctrl Pts',(-31.5088748947582,64.3132080230637,12.));
#96350=CARTESIAN_POINT('Ctrl Pts',(-31.4923637283132,64.2968194931158,12.));
#96351=CARTESIAN_POINT('Ctrl Pts',(-31.4759001384941,64.2804457127671,12.));
#96352=CARTESIAN_POINT('Ctrl Pts',(-31.4594841711195,64.2640868198473,12.));
#96353=CARTESIAN_POINT('Ctrl Pts',(-31.4431158721222,64.2477429528393,12.));
#96354=CARTESIAN_POINT('Ctrl Pts',(-31.4267952875423,64.231414250881,12.));
#96355=CARTESIAN_POINT('Ctrl Pts',(-31.410522463528,64.2151008537697,12.));
#96356=CARTESIAN_POINT('Ctrl Pts',(-31.3942974463445,64.1988029019707,12.));
#96357=CARTESIAN_POINT('Ctrl Pts',(-31.3781202823754,64.1825205366224,12.));
#96358=CARTESIAN_POINT('Ctrl Pts',(-31.3619910181228,64.166253899542,12.));
#96359=CARTESIAN_POINT('Ctrl Pts',(-31.3459097002006,64.1500031332282,12.));
#96360=CARTESIAN_POINT('Ctrl Pts',(-31.3298763753377,64.133768380869,12.));
#96361=CARTESIAN_POINT('Ctrl Pts',(-31.3138910903859,64.117549786349,12.));
#96362=CARTESIAN_POINT('Ctrl Pts',(-31.2979538923214,64.1013474942556,12.));
#96363=CARTESIAN_POINT('Ctrl Pts',(-31.2820648282447,64.0851616498852,12.));
#96364=CARTESIAN_POINT('Ctrl Pts',(-31.2662239453728,64.0689923992461,12.));
#96365=CARTESIAN_POINT('Ctrl Pts',(-31.2504312910451,64.0528398890657,12.));
#96366=CARTESIAN_POINT('Ctrl Pts',(-31.2346869127297,64.0367042667984,12.));
#96367=CARTESIAN_POINT('Ctrl Pts',(-31.2189908580245,64.02058568063,12.));
#96368=CARTESIAN_POINT('Ctrl Pts',(-31.2033431746558,64.0044842794831,12.));
#96369=CARTESIAN_POINT('Ctrl Pts',(-31.1877439104717,63.9884002130211,12.));
#96370=CARTESIAN_POINT('Ctrl Pts',(-31.1721931134487,63.9723336316551,12.));
#96371=CARTESIAN_POINT('Ctrl Pts',(-31.1566908316992,63.9562846865567,12.));
#96372=CARTESIAN_POINT('Ctrl Pts',(-31.1412371134727,63.940253529665,12.));
#96373=CARTESIAN_POINT('Ctrl Pts',(-31.1258320071545,63.9242403136955,12.));
#96374=CARTESIAN_POINT('Ctrl Pts',(-31.1104755612607,63.9082451921448,12.));
#96375=CARTESIAN_POINT('Ctrl Pts',(-31.0951678244455,63.8922683192964,12.));
#96376=CARTESIAN_POINT('Ctrl Pts',(-31.0799088455041,63.8763098502237,12.));
#96377=CARTESIAN_POINT('Ctrl Pts',(-31.0646986733723,63.8603699407922,12.));
#96378=CARTESIAN_POINT('Ctrl Pts',(-31.0495373571215,63.8444487476611,12.));
#96379=CARTESIAN_POINT('Ctrl Pts',(-31.0344249459538,63.8285464282846,12.));
#96380=CARTESIAN_POINT('Ctrl Pts',(-31.0193614892171,63.8126631409364,12.));
#96381=CARTESIAN_POINT('Ctrl Pts',(-31.0043470364108,63.796799044728,12.));
#96382=CARTESIAN_POINT('Ctrl Pts',(-30.989381637191,63.7809542996264,12.));
#96383=CARTESIAN_POINT('Ctrl Pts',(-30.9744653413689,63.7651290664733,12.));
#96384=CARTESIAN_POINT('Ctrl Pts',(-30.9595981989104,63.749323506987,12.));
#96385=CARTESIAN_POINT('Ctrl Pts',(-30.9447802599355,63.7335377837441,12.));
#96386=CARTESIAN_POINT('Ctrl Pts',(-30.9300115747115,63.7177720601609,12.));
#96387=CARTESIAN_POINT('Ctrl Pts',(-30.9152921936465,63.7020265004792,12.));
#96388=CARTESIAN_POINT('Ctrl Pts',(-30.900622167269,63.6863012697328,12.));
#96389=CARTESIAN_POINT('Ctrl Pts',(-30.8860015462475,63.6705965337971,12.));
#96390=CARTESIAN_POINT('Ctrl Pts',(-30.8714303814194,63.6549124594666,12.));
#96391=CARTESIAN_POINT('Ctrl Pts',(-30.8569087238131,63.6392492145233,12.));
#96392=CARTESIAN_POINT('Ctrl Pts',(-30.8424366246671,63.6236069678055,12.));
#96393=CARTESIAN_POINT('Ctrl Pts',(-30.8280141354459,63.6079858892771,12.));
#96394=CARTESIAN_POINT('Ctrl Pts',(-30.813641307801,63.5923861498987,12.));
#96395=CARTESIAN_POINT('Ctrl Pts',(-30.7993181935271,63.5768079214881,12.));
#96396=CARTESIAN_POINT('Ctrl Pts',(-30.7850448445205,63.5612513766,12.));
#96397=CARTESIAN_POINT('Ctrl Pts',(-30.7708213127159,63.5457166883537,12.));
#96398=CARTESIAN_POINT('Ctrl Pts',(-30.7566476500757,63.5302040304142,12.));
#96399=CARTESIAN_POINT('Ctrl Pts',(-30.7425239087281,63.5147135773894,12.));
#96400=CARTESIAN_POINT('Ctrl Pts',(-30.7284501410822,63.4992455051795,12.));
#96401=CARTESIAN_POINT('Ctrl Pts',(-30.7144263999265,63.4837999912771,12.));
#96402=CARTESIAN_POINT('Ctrl Pts',(-30.7004527385821,63.4683772152529,12.));
#96403=CARTESIAN_POINT('Ctrl Pts',(-30.6865292107929,63.4529773584249,12.));
#96404=CARTESIAN_POINT('Ctrl Pts',(-30.6726558704315,63.4376006029604,12.));
#96405=CARTESIAN_POINT('Ctrl Pts',(-30.6588327712484,63.4222471311239,12.));
#96406=CARTESIAN_POINT('Ctrl Pts',(-30.6450599666121,63.4069171245066,12.));
#96407=CARTESIAN_POINT('Ctrl Pts',(-30.6313375092062,63.3916107631376,12.));
#96408=CARTESIAN_POINT('Ctrl Pts',(-30.6176654515967,63.3763282271796,12.));
#96409=CARTESIAN_POINT('Ctrl Pts',(-30.6040438469078,63.3610696989577,12.));
#96410=CARTESIAN_POINT('Ctrl Pts',(-30.5904727493712,63.3458353646154,12.));
#96411=CARTESIAN_POINT('Ctrl Pts',(-30.5769522151164,63.3306254165126,12.));
#96412=CARTESIAN_POINT('Ctrl Pts',(-30.563482302238,63.3154400534397,12.));
#96413=CARTESIAN_POINT('Ctrl Pts',(-30.5500630691359,63.3002794756086,12.));
#96414=CARTESIAN_POINT('Ctrl Pts',(-30.5366945730508,63.2851438802473,12.));
#96415=CARTESIAN_POINT('Ctrl Pts',(-30.5233768687865,63.2700334577639,12.));
#96416=CARTESIAN_POINT('Ctrl Pts',(-30.5101100066659,63.2549483856215,12.));
#96417=CARTESIAN_POINT('Ctrl Pts',(-30.4968940344998,63.2398888342545,12.));
#96418=CARTESIAN_POINT('Ctrl Pts',(-30.4837290014989,63.2248549788221,12.));
#96419=CARTESIAN_POINT('Ctrl Pts',(-30.470614961416,63.2098470086636,12.));
#96420=CARTESIAN_POINT('Ctrl Pts',(-30.4575519763337,63.1948651386942,12.));
#96421=CARTESIAN_POINT('Ctrl Pts',(-30.4445401192381,63.179909617189,12.));
#96422=CARTESIAN_POINT('Ctrl Pts',(-30.4315794659731,63.164980701691,12.));
#96423=CARTESIAN_POINT('Ctrl Pts',(-30.418670087563,63.1500786361459,12.));
#96424=CARTESIAN_POINT('Ctrl Pts',(-30.4058120432228,63.135203629844,12.));
#96425=CARTESIAN_POINT('Ctrl Pts',(-30.3930053710484,63.1203558300657,12.));
#96426=CARTESIAN_POINT('Ctrl Pts',(-30.3802500880403,63.105535320226,12.));
#96427=CARTESIAN_POINT('Ctrl Pts',(-30.3700869762507,63.0937007763471,12.));
#96428=CARTESIAN_POINT('Ctrl Pts',(-30.3624877680651,63.0848371718048,12.));
#96429=CARTESIAN_POINT('Ctrl Pts',(-30.357431906933,63.078933570069,12.));
#96430=CARTESIAN_POINT('Ctrl Pts',(-30.3549065457811,63.0759831361898,12.));
#96431=CARTESIAN_POINT('Ctrl Pts',(-34.933187552314,65.4667541478384,-5.55111512312578E-16));
#96432=CARTESIAN_POINT('Ctrl Pts',(-34.933187552314,65.4667541478384,4.));
#96433=CARTESIAN_POINT('Ctrl Pts',(-34.933187552314,65.4667541478384,8.));
#96434=CARTESIAN_POINT('Ctrl Pts',(-34.933187552314,65.4667541478384,12.));
#96435=CARTESIAN_POINT('Ctrl Pts',(-34.940541458921,65.5763902570748,-5.55111512312578E-16));
#96436=CARTESIAN_POINT('Ctrl Pts',(-34.940541458921,65.5763902570748,4.));
#96437=CARTESIAN_POINT('Ctrl Pts',(-34.940541458921,65.5763902570748,8.));
#96438=CARTESIAN_POINT('Ctrl Pts',(-34.940541458921,65.5763902570748,12.));
#96439=CARTESIAN_POINT('Ctrl Pts',(-34.8876896346299,65.7720412680587,-5.55111512312578E-16));
#96440=CARTESIAN_POINT('Ctrl Pts',(-34.8876896346299,65.7720412680587,4.00000000000001));
#96441=CARTESIAN_POINT('Ctrl Pts',(-34.8876896346299,65.7720412680587,7.99999999999999));
#96442=CARTESIAN_POINT('Ctrl Pts',(-34.8876896346299,65.7720412680587,12.));
#96443=CARTESIAN_POINT('Ctrl Pts',(-34.7399186668304,65.9044372006541,-5.55111512312578E-16));
#96444=CARTESIAN_POINT('Ctrl Pts',(-34.7399186668304,65.9044372006541,4.));
#96445=CARTESIAN_POINT('Ctrl Pts',(-34.7399186668304,65.9044372006541,8.00000000000001));
#96446=CARTESIAN_POINT('Ctrl Pts',(-34.7399186668304,65.9044372006541,12.));
#96447=CARTESIAN_POINT('Ctrl Pts',(-34.6669728017261,65.9427857825583,-5.55111512312578E-16));
#96448=CARTESIAN_POINT('Ctrl Pts',(-34.6669728017261,65.9427857825583,4.));
#96449=CARTESIAN_POINT('Ctrl Pts',(-34.6669728017261,65.9427857825583,8.));
#96450=CARTESIAN_POINT('Ctrl Pts',(-34.6669728017261,65.9427857825583,12.));
#96451=CARTESIAN_POINT('',(-34.933187552314,65.4667541478384,0.));
#96452=CARTESIAN_POINT('',(-34.6669728017262,65.9427857825584,2.77555756156289E-16));
#96453=CARTESIAN_POINT('Ctrl Pts',(-34.933187552314,65.4667541478384,4.16333634234434E-16));
#96454=CARTESIAN_POINT('Ctrl Pts',(-34.940541458921,65.5763902570748,4.16333634234433E-16));
#96455=CARTESIAN_POINT('Ctrl Pts',(-34.910340416469,65.6881908347799,4.16333634234434E-16));
#96456=CARTESIAN_POINT('Ctrl Pts',(-34.8491453679733,65.7793366930112,4.16333634234434E-16));
#96457=CARTESIAN_POINT('Ctrl Pts',(-34.8032490816016,65.8476960866847,4.16333634234434E-16));
#96458=CARTESIAN_POINT('Ctrl Pts',(-34.7399186668304,65.9044372006541,4.16333634234433E-16));
#96459=CARTESIAN_POINT('Ctrl Pts',(-34.6669728017261,65.9427857825583,4.16333634234434E-16));
#96460=CARTESIAN_POINT('',(-34.6669728017262,65.9427857825584,12.));
#96461=CARTESIAN_POINT('Ctrl Pts',(-34.6669728017261,65.9427857825583,-5.55111512312578E-16));
#96462=CARTESIAN_POINT('Ctrl Pts',(-34.6669728017261,65.9427857825583,4.));
#96463=CARTESIAN_POINT('Ctrl Pts',(-34.6669728017261,65.9427857825583,8.));
#96464=CARTESIAN_POINT('Ctrl Pts',(-34.6669728017261,65.9427857825583,12.));
#96465=CARTESIAN_POINT('',(-34.933187552314,65.4667541478384,12.));
#96466=CARTESIAN_POINT('Ctrl Pts',(-34.6669728017261,65.9427857825583,12.));
#96467=CARTESIAN_POINT('Ctrl Pts',(-34.7399186668304,65.9044372006541,12.));
#96468=CARTESIAN_POINT('Ctrl Pts',(-34.8032490816016,65.8476960866846,12.));
#96469=CARTESIAN_POINT('Ctrl Pts',(-34.8491453679733,65.7793366930112,12.));
#96470=CARTESIAN_POINT('Ctrl Pts',(-34.910340416469,65.6881908347799,12.));
#96471=CARTESIAN_POINT('Ctrl Pts',(-34.940541458921,65.5763902570748,12.));
#96472=CARTESIAN_POINT('Ctrl Pts',(-34.933187552314,65.4667541478384,12.));
#96473=CARTESIAN_POINT('Ctrl Pts',(-34.933187552314,65.4667541478384,12.));
#96474=CARTESIAN_POINT('Ctrl Pts',(-34.933187552314,65.4667541478384,8.));
#96475=CARTESIAN_POINT('Ctrl Pts',(-34.933187552314,65.4667541478384,4.));
#96476=CARTESIAN_POINT('Ctrl Pts',(-34.933187552314,65.4667541478384,-5.55111512312578E-16));
#96477=CARTESIAN_POINT('Origin',(-1.73171632017259E-10,3.32444647725448E-10,
0.));
#96478=CARTESIAN_POINT('Origin',(-1.73171632017259E-10,3.32444647725448E-10,
12.));
#96479=CARTESIAN_POINT('Origin',(-1.73171632017259E-10,3.32444647725448E-10,
0.));
#96480=CARTESIAN_POINT('Ctrl Pts',(-28.2316040302268,68.9436475237602,-5.55111512312578E-16));
#96481=CARTESIAN_POINT('Ctrl Pts',(-28.2316040302268,68.9436475237602,4.));
#96482=CARTESIAN_POINT('Ctrl Pts',(-28.2316040302269,68.9436475237602,8.));
#96483=CARTESIAN_POINT('Ctrl Pts',(-28.2316040302269,68.9436475237602,12.));
#96484=CARTESIAN_POINT('Ctrl Pts',(-28.1299168084378,68.9852872321828,-5.55111512312578E-16));
#96485=CARTESIAN_POINT('Ctrl Pts',(-28.1299168084378,68.9852872321828,4.));
#96486=CARTESIAN_POINT('Ctrl Pts',(-28.1299168084378,68.9852872321828,8.00000000000001));
#96487=CARTESIAN_POINT('Ctrl Pts',(-28.1299168084378,68.9852872321828,12.));
#96488=CARTESIAN_POINT('Ctrl Pts',(-27.9275918177432,68.9970049015576,-5.55111512312578E-16));
#96489=CARTESIAN_POINT('Ctrl Pts',(-27.9275918177432,68.9970049015576,4.));
#96490=CARTESIAN_POINT('Ctrl Pts',(-27.9275918177433,68.9970049015576,7.99999999999999));
#96491=CARTESIAN_POINT('Ctrl Pts',(-27.9275918177433,68.9970049015576,12.));
#96492=CARTESIAN_POINT('Ctrl Pts',(-27.7552674476222,68.8986722313991,-5.55111512312578E-16));
#96493=CARTESIAN_POINT('Ctrl Pts',(-27.7552674476222,68.8986722313991,4.));
#96494=CARTESIAN_POINT('Ctrl Pts',(-27.7552674476223,68.8986722313991,8.00000000000001));
#96495=CARTESIAN_POINT('Ctrl Pts',(-27.7552674476223,68.8986722313991,12.));
#96496=CARTESIAN_POINT('Ctrl Pts',(-27.6958230984758,68.8415926174774,-5.55111512312578E-16));
#96497=CARTESIAN_POINT('Ctrl Pts',(-27.6958230984758,68.8415926174774,4.));
#96498=CARTESIAN_POINT('Ctrl Pts',(-27.6958230984758,68.8415926174774,8.));
#96499=CARTESIAN_POINT('Ctrl Pts',(-27.6958230984758,68.8415926174774,12.));
#96500=CARTESIAN_POINT('',(-28.2316040302268,68.9436475237602,0.));
#96501=CARTESIAN_POINT('',(-27.6958230984757,68.8415926174774,2.77555756156289E-16));
#96502=CARTESIAN_POINT('Ctrl Pts',(-28.2316040302268,68.9436475237602,-5.55111512312578E-16));
#96503=CARTESIAN_POINT('Ctrl Pts',(-28.1299168084378,68.9852872321828,-5.55111512312578E-16));
#96504=CARTESIAN_POINT('Ctrl Pts',(-28.0143025280409,68.9919830432541,-5.55111512312578E-16));
#96505=CARTESIAN_POINT('Ctrl Pts',(-27.9084843686476,68.9627440495799,-5.55111512312578E-16));
#96506=CARTESIAN_POINT('Ctrl Pts',(-27.8291207491026,68.9408148043242,-5.55111512312578E-16));
#96507=CARTESIAN_POINT('Ctrl Pts',(-27.7552674476222,68.8986722313991,-5.55111512312578E-16));
#96508=CARTESIAN_POINT('Ctrl Pts',(-27.6958230984758,68.8415926174774,-5.55111512312578E-16));
#96509=CARTESIAN_POINT('',(-27.6958230984758,68.8415926174774,12.));
#96510=CARTESIAN_POINT('Ctrl Pts',(-27.6958230984758,68.8415926174774,-5.55111512312578E-16));
#96511=CARTESIAN_POINT('Ctrl Pts',(-27.6958230984758,68.8415926174774,4.));
#96512=CARTESIAN_POINT('Ctrl Pts',(-27.6958230984758,68.8415926174774,8.));
#96513=CARTESIAN_POINT('Ctrl Pts',(-27.6958230984758,68.8415926174774,12.));
#96514=CARTESIAN_POINT('',(-28.2316040302269,68.9436475237602,12.));
#96515=CARTESIAN_POINT('Ctrl Pts',(-27.6958230984758,68.8415926174774,12.));
#96516=CARTESIAN_POINT('Ctrl Pts',(-27.7552674476223,68.8986722313991,12.));
#96517=CARTESIAN_POINT('Ctrl Pts',(-27.8291207491027,68.9408148043242,12.));
#96518=CARTESIAN_POINT('Ctrl Pts',(-27.9084843686477,68.9627440495799,12.));
#96519=CARTESIAN_POINT('Ctrl Pts',(-28.0143025280409,68.9919830432541,12.));
#96520=CARTESIAN_POINT('Ctrl Pts',(-28.1299168084378,68.9852872321828,12.));
#96521=CARTESIAN_POINT('Ctrl Pts',(-28.2316040302269,68.9436475237602,12.));
#96522=CARTESIAN_POINT('Ctrl Pts',(-28.2316040302269,68.9436475237602,12.));
#96523=CARTESIAN_POINT('Ctrl Pts',(-28.2316040302269,68.9436475237602,8.));
#96524=CARTESIAN_POINT('Ctrl Pts',(-28.2316040302268,68.9436475237602,4.));
#96525=CARTESIAN_POINT('Ctrl Pts',(-28.2316040302268,68.9436475237602,-5.55111512312578E-16));
#96526=CARTESIAN_POINT('Ctrl Pts',(-24.7419628022042,65.4815644032299,0.));
#96527=CARTESIAN_POINT('Ctrl Pts',(-24.7419628022042,65.4815644032299,12.));
#96528=CARTESIAN_POINT('Ctrl Pts',(-24.7442214063382,65.4847237095443,0.));
#96529=CARTESIAN_POINT('Ctrl Pts',(-24.7442214063382,65.4847237095443,12.));
#96530=CARTESIAN_POINT('Ctrl Pts',(-24.7487434955982,65.4910454936254,0.));
#96531=CARTESIAN_POINT('Ctrl Pts',(-24.7487434955982,65.4910454936254,12.));
#96532=CARTESIAN_POINT('Ctrl Pts',(-24.7555412724651,65.5005376841101,0.));
#96533=CARTESIAN_POINT('Ctrl Pts',(-24.7555412724651,65.5005376841101,12.));
#96534=CARTESIAN_POINT('Ctrl Pts',(-24.7646342620841,65.5132129675333,0.));
#96535=CARTESIAN_POINT('Ctrl Pts',(-24.7646342620841,65.5132129675333,12.));
#96536=CARTESIAN_POINT('Ctrl Pts',(-24.7760493148465,65.5290887770232,0.));
#96537=CARTESIAN_POINT('Ctrl Pts',(-24.7760493148465,65.5290887770232,12.));
#96538=CARTESIAN_POINT('Ctrl Pts',(-24.7875131827491,65.5449962514661,0.));
#96539=CARTESIAN_POINT('Ctrl Pts',(-24.7875131827491,65.5449962514661,12.));
#96540=CARTESIAN_POINT('Ctrl Pts',(-24.799025856126,65.5609353062829,0.));
#96541=CARTESIAN_POINT('Ctrl Pts',(-24.799025856126,65.5609353062829,12.));
#96542=CARTESIAN_POINT('Ctrl Pts',(-24.8105873098626,65.5769057914333,0.));
#96543=CARTESIAN_POINT('Ctrl Pts',(-24.8105873098626,65.5769057914333,12.));
#96544=CARTESIAN_POINT('Ctrl Pts',(-24.8221975032104,65.5929074932624,0.));
#96545=CARTESIAN_POINT('Ctrl Pts',(-24.8221975032104,65.5929074932624,12.));
#96546=CARTESIAN_POINT('Ctrl Pts',(-24.8338563866764,65.6089401625628,0.));
#96547=CARTESIAN_POINT('Ctrl Pts',(-24.8338563866764,65.6089401625628,12.));
#96548=CARTESIAN_POINT('Ctrl Pts',(-24.8455639071517,65.6250035361612,0.));
#96549=CARTESIAN_POINT('Ctrl Pts',(-24.8455639071517,65.6250035361612,12.));
#96550=CARTESIAN_POINT('Ctrl Pts',(-24.8573200135666,65.6410973603661,0.));
#96551=CARTESIAN_POINT('Ctrl Pts',(-24.8573200135666,65.6410973603661,12.));
#96552=CARTESIAN_POINT('Ctrl Pts',(-24.8691246628057,65.6572214156692,0.));
#96553=CARTESIAN_POINT('Ctrl Pts',(-24.8691246628057,65.6572214156692,12.));
#96554=CARTESIAN_POINT('Ctrl Pts',(-24.8809778178229,65.6733755087669,0.));
#96555=CARTESIAN_POINT('Ctrl Pts',(-24.8809778178229,65.6733755087669,12.));
#96556=CARTESIAN_POINT('Ctrl Pts',(-24.8928794448607,65.6895594608775,0.));
#96557=CARTESIAN_POINT('Ctrl Pts',(-24.8928794448607,65.6895594608775,12.));
#96558=CARTESIAN_POINT('Ctrl Pts',(-24.9048295111448,65.7057730980483,0.));
#96559=CARTESIAN_POINT('Ctrl Pts',(-24.9048295111448,65.7057730980483,12.));
#96560=CARTESIAN_POINT('Ctrl Pts',(-24.9168279820106,65.7220162391053,0.));
#96561=CARTESIAN_POINT('Ctrl Pts',(-24.9168279820106,65.7220162391053,12.));
#96562=CARTESIAN_POINT('Ctrl Pts',(-24.928874819458,65.7382886895888,0.));
#96563=CARTESIAN_POINT('Ctrl Pts',(-24.928874819458,65.7382886895888,12.));
#96564=CARTESIAN_POINT('Ctrl Pts',(-24.9409699836537,65.7545902480323,0.));
#96565=CARTESIAN_POINT('Ctrl Pts',(-24.9409699836537,65.7545902480323,12.));
#96566=CARTESIAN_POINT('Ctrl Pts',(-24.9531134338696,65.7709207098959,0.));
#96567=CARTESIAN_POINT('Ctrl Pts',(-24.9531134338696,65.7709207098959,12.));
#96568=CARTESIAN_POINT('Ctrl Pts',(-24.9653051295581,65.7872798720823,0.));
#96569=CARTESIAN_POINT('Ctrl Pts',(-24.9653051295581,65.7872798720823,12.));
#96570=CARTESIAN_POINT('Ctrl Pts',(-24.9775450315683,65.8036675380718,0.));
#96571=CARTESIAN_POINT('Ctrl Pts',(-24.9775450315683,65.8036675380718,12.));
#96572=CARTESIAN_POINT('Ctrl Pts',(-24.9898331020983,65.8200835177024,0.));
#96573=CARTESIAN_POINT('Ctrl Pts',(-24.9898331020983,65.8200835177024,12.));
#96574=CARTESIAN_POINT('Ctrl Pts',(-25.002169304117,65.8365276247128,0.));
#96575=CARTESIAN_POINT('Ctrl Pts',(-25.002169304117,65.8365276247128,12.));
#96576=CARTESIAN_POINT('Ctrl Pts',(-25.0145536009604,65.8529996750445,0.));
#96577=CARTESIAN_POINT('Ctrl Pts',(-25.0145536009604,65.8529996750445,12.));
#96578=CARTESIAN_POINT('Ctrl Pts',(-25.0269859558363,65.8694994847616,0.));
#96579=CARTESIAN_POINT('Ctrl Pts',(-25.0269859558363,65.8694994847616,12.));
#96580=CARTESIAN_POINT('Ctrl Pts',(-25.0394663314055,65.8860268683128,0.));
#96581=CARTESIAN_POINT('Ctrl Pts',(-25.0394663314055,65.8860268683128,12.));
#96582=CARTESIAN_POINT('Ctrl Pts',(-25.0519946900078,65.9025816394424,0.));
#96583=CARTESIAN_POINT('Ctrl Pts',(-25.0519946900078,65.9025816394424,12.));
#96584=CARTESIAN_POINT('Ctrl Pts',(-25.0645709938524,65.919163611981,0.));
#96585=CARTESIAN_POINT('Ctrl Pts',(-25.0645709938524,65.919163611981,12.));
#96586=CARTESIAN_POINT('Ctrl Pts',(-25.0771952052028,65.9357726006163,0.));
#96587=CARTESIAN_POINT('Ctrl Pts',(-25.0771952052028,65.9357726006163,12.));
#96588=CARTESIAN_POINT('Ctrl Pts',(-25.0898672865915,65.9524084218139,0.));
#96589=CARTESIAN_POINT('Ctrl Pts',(-25.0898672865915,65.9524084218139,12.));
#96590=CARTESIAN_POINT('Ctrl Pts',(-25.1025872009004,65.9690708941558,0.));
#96591=CARTESIAN_POINT('Ctrl Pts',(-25.1025872009004,65.9690708941558,12.));
#96592=CARTESIAN_POINT('Ctrl Pts',(-25.1153549112503,65.9857598378433,0.));
#96593=CARTESIAN_POINT('Ctrl Pts',(-25.1153549112503,65.9857598378433,12.));
#96594=CARTESIAN_POINT('Ctrl Pts',(-25.1281703809297,66.0024750743897,0.));
#96595=CARTESIAN_POINT('Ctrl Pts',(-25.1281703809297,66.0024750743897,12.));
#96596=CARTESIAN_POINT('Ctrl Pts',(-25.1410335733099,66.0192164262621,0.));
#96597=CARTESIAN_POINT('Ctrl Pts',(-25.1410335733099,66.0192164262621,12.));
#96598=CARTESIAN_POINT('Ctrl Pts',(-25.1539444517419,66.0359837164734,0.));
#96599=CARTESIAN_POINT('Ctrl Pts',(-25.1539444517419,66.0359837164734,12.));
#96600=CARTESIAN_POINT('Ctrl Pts',(-25.1669029795661,66.0527767686025,0.));
#96601=CARTESIAN_POINT('Ctrl Pts',(-25.1669029795661,66.0527767686025,12.));
#96602=CARTESIAN_POINT('Ctrl Pts',(-25.1799091201599,66.0695954069713,0.));
#96603=CARTESIAN_POINT('Ctrl Pts',(-25.1799091201599,66.0695954069713,12.));
#96604=CARTESIAN_POINT('Ctrl Pts',(-25.1929628369685,66.086439456768,0.));
#96605=CARTESIAN_POINT('Ctrl Pts',(-25.1929628369685,66.086439456768,12.));
#96606=CARTESIAN_POINT('Ctrl Pts',(-25.2060640935365,66.10330874419,0.));
#96607=CARTESIAN_POINT('Ctrl Pts',(-25.2060640935365,66.10330874419,12.));
#96608=CARTESIAN_POINT('Ctrl Pts',(-25.2192128535357,66.1202030965758,0.));
#96609=CARTESIAN_POINT('Ctrl Pts',(-25.2192128535357,66.1202030965758,12.));
#96610=CARTESIAN_POINT('Ctrl Pts',(-25.232409080755,66.1371223423345,0.));
#96611=CARTESIAN_POINT('Ctrl Pts',(-25.232409080755,66.1371223423345,12.));
#96612=CARTESIAN_POINT('Ctrl Pts',(-25.2456527390875,66.1540663108754,0.));
#96613=CARTESIAN_POINT('Ctrl Pts',(-25.2456527390875,66.1540663108754,12.));
#96614=CARTESIAN_POINT('Ctrl Pts',(-25.2589437925147,66.1710348325384,0.));
#96615=CARTESIAN_POINT('Ctrl Pts',(-25.2589437925147,66.1710348325384,12.));
#96616=CARTESIAN_POINT('Ctrl Pts',(-25.2722822050837,66.1880277385136,0.));
#96617=CARTESIAN_POINT('Ctrl Pts',(-25.2722822050837,66.1880277385136,12.));
#96618=CARTESIAN_POINT('Ctrl Pts',(-25.285667940893,66.2050448607911,0.));
#96619=CARTESIAN_POINT('Ctrl Pts',(-25.285667940893,66.2050448607911,12.));
#96620=CARTESIAN_POINT('Ctrl Pts',(-25.2991009641094,66.2220860321952,0.));
#96621=CARTESIAN_POINT('Ctrl Pts',(-25.2991009641094,66.2220860321952,12.));
#96622=CARTESIAN_POINT('Ctrl Pts',(-25.312581238973,66.2391510863998,0.));
#96623=CARTESIAN_POINT('Ctrl Pts',(-25.312581238973,66.2391510863998,12.));
#96624=CARTESIAN_POINT('Ctrl Pts',(-25.3261087298026,66.2562398579471,0.));
#96625=CARTESIAN_POINT('Ctrl Pts',(-25.3261087298026,66.2562398579471,12.));
#96626=CARTESIAN_POINT('Ctrl Pts',(-25.3396834009949,66.2733521822662,0.));
#96627=CARTESIAN_POINT('Ctrl Pts',(-25.3396834009949,66.2733521822662,12.));
#96628=CARTESIAN_POINT('Ctrl Pts',(-25.3533052170249,66.290487895671,0.));
#96629=CARTESIAN_POINT('Ctrl Pts',(-25.3533052170249,66.290487895671,12.));
#96630=CARTESIAN_POINT('Ctrl Pts',(-25.3669741424488,66.3076468353412,0.));
#96631=CARTESIAN_POINT('Ctrl Pts',(-25.3669741424488,66.3076468353412,12.));
#96632=CARTESIAN_POINT('Ctrl Pts',(-25.3806901419012,66.3248288393046,0.));
#96633=CARTESIAN_POINT('Ctrl Pts',(-25.3806901419012,66.3248288393046,12.));
#96634=CARTESIAN_POINT('Ctrl Pts',(-25.3944531800901,66.3420337464178,0.));
#96635=CARTESIAN_POINT('Ctrl Pts',(-25.3944531800901,66.3420337464178,12.));
#96636=CARTESIAN_POINT('Ctrl Pts',(-25.4082632217847,66.359261396341,0.));
#96637=CARTESIAN_POINT('Ctrl Pts',(-25.4082632217847,66.359261396341,12.));
#96638=CARTESIAN_POINT('Ctrl Pts',(-25.4221202318199,66.3765116295364,0.));
#96639=CARTESIAN_POINT('Ctrl Pts',(-25.4221202318199,66.3765116295364,12.));
#96640=CARTESIAN_POINT('Ctrl Pts',(-25.4360241751018,66.3937842872685,0.));
#96641=CARTESIAN_POINT('Ctrl Pts',(-25.4360241751018,66.3937842872685,12.));
#96642=CARTESIAN_POINT('Ctrl Pts',(-25.4499750166079,66.4110792116,0.));
#96643=CARTESIAN_POINT('Ctrl Pts',(-25.4499750166079,66.4110792116,12.));
#96644=CARTESIAN_POINT('Ctrl Pts',(-25.4639727213849,66.4283962453899,0.));
#96645=CARTESIAN_POINT('Ctrl Pts',(-25.4639727213849,66.4283962453899,12.));
#96646=CARTESIAN_POINT('Ctrl Pts',(-25.4780172545417,66.4457352322871,0.));
#96647=CARTESIAN_POINT('Ctrl Pts',(-25.4780172545417,66.4457352322871,12.));
#96648=CARTESIAN_POINT('Ctrl Pts',(-25.4921085812548,66.4630960167252,0.));
#96649=CARTESIAN_POINT('Ctrl Pts',(-25.4921085812548,66.4630960167252,12.));
#96650=CARTESIAN_POINT('Ctrl Pts',(-25.5062466667702,66.4804784439148,0.));
#96651=CARTESIAN_POINT('Ctrl Pts',(-25.5062466667702,66.4804784439148,12.));
#96652=CARTESIAN_POINT('Ctrl Pts',(-25.5204314764033,66.4978823598354,0.));
#96653=CARTESIAN_POINT('Ctrl Pts',(-25.5204314764033,66.4978823598354,12.));
#96654=CARTESIAN_POINT('Ctrl Pts',(-25.534662975532,66.5153076112231,0.));
#96655=CARTESIAN_POINT('Ctrl Pts',(-25.534662975532,66.5153076112231,12.));
#96656=CARTESIAN_POINT('Ctrl Pts',(-25.5489411295912,66.5327540455624,0.));
#96657=CARTESIAN_POINT('Ctrl Pts',(-25.5489411295912,66.5327540455624,12.));
#96658=CARTESIAN_POINT('Ctrl Pts',(-25.5632659040792,66.5502215110829,0.));
#96659=CARTESIAN_POINT('Ctrl Pts',(-25.5632659040792,66.5502215110829,12.));
#96660=CARTESIAN_POINT('Ctrl Pts',(-25.5776372645601,66.5677098567542,0.));
#96661=CARTESIAN_POINT('Ctrl Pts',(-25.5776372645601,66.5677098567542,12.));
#96662=CARTESIAN_POINT('Ctrl Pts',(-25.5920551766629,66.5852189322813,0.));
#96663=CARTESIAN_POINT('Ctrl Pts',(-25.5920551766629,66.5852189322813,12.));
#96664=CARTESIAN_POINT('Ctrl Pts',(-25.6065196060756,66.6027485880963,0.));
#96665=CARTESIAN_POINT('Ctrl Pts',(-25.6065196060756,66.6027485880963,12.));
#96666=CARTESIAN_POINT('Ctrl Pts',(-25.6210305185403,66.6202986753506,0.));
#96667=CARTESIAN_POINT('Ctrl Pts',(-25.6210305185403,66.6202986753506,12.));
#96668=CARTESIAN_POINT('Ctrl Pts',(-25.6355878798614,66.6378690459129,0.));
#96669=CARTESIAN_POINT('Ctrl Pts',(-25.6355878798614,66.6378690459129,12.));
#96670=CARTESIAN_POINT('Ctrl Pts',(-25.6501916559055,66.6554595523624,0.));
#96671=CARTESIAN_POINT('Ctrl Pts',(-25.6501916559055,66.6554595523624,12.));
#96672=CARTESIAN_POINT('Ctrl Pts',(-25.6648418126013,66.6730700479837,0.));
#96673=CARTESIAN_POINT('Ctrl Pts',(-25.6648418126013,66.6730700479837,12.));
#96674=CARTESIAN_POINT('Ctrl Pts',(-25.6795383159319,66.6907003867572,0.));
#96675=CARTESIAN_POINT('Ctrl Pts',(-25.6795383159319,66.6907003867572,12.));
#96676=CARTESIAN_POINT('Ctrl Pts',(-25.6942811319322,66.7083504233529,0.));
#96677=CARTESIAN_POINT('Ctrl Pts',(-25.6942811319322,66.7083504233529,12.));
#96678=CARTESIAN_POINT('Ctrl Pts',(-25.7090702266963,66.7260200131266,0.));
#96679=CARTESIAN_POINT('Ctrl Pts',(-25.7090702266963,66.7260200131266,12.));
#96680=CARTESIAN_POINT('Ctrl Pts',(-25.7239055663772,66.7437090121153,0.));
#96681=CARTESIAN_POINT('Ctrl Pts',(-25.7239055663772,66.7437090121153,12.));
#96682=CARTESIAN_POINT('Ctrl Pts',(-25.7387871171866,66.7614172770316,0.));
#96683=CARTESIAN_POINT('Ctrl Pts',(-25.7387871171866,66.7614172770316,12.));
#96684=CARTESIAN_POINT('Ctrl Pts',(-25.7537148453864,66.7791446652545,0.));
#96685=CARTESIAN_POINT('Ctrl Pts',(-25.7537148453864,66.7791446652545,12.));
#96686=CARTESIAN_POINT('Ctrl Pts',(-25.7686887172878,66.7968910348245,0.));
#96687=CARTESIAN_POINT('Ctrl Pts',(-25.7686887172878,66.7968910348245,12.));
#96688=CARTESIAN_POINT('Ctrl Pts',(-25.7837086992595,66.8146562444433,0.));
#96689=CARTESIAN_POINT('Ctrl Pts',(-25.7837086992595,66.8146562444433,12.));
#96690=CARTESIAN_POINT('Ctrl Pts',(-25.7987747577269,66.8324401534668,0.));
#96691=CARTESIAN_POINT('Ctrl Pts',(-25.7987747577269,66.8324401534668,12.));
#96692=CARTESIAN_POINT('Ctrl Pts',(-25.8138868591709,66.8502426219001,0.));
#96693=CARTESIAN_POINT('Ctrl Pts',(-25.8138868591709,66.8502426219001,12.));
#96694=CARTESIAN_POINT('Ctrl Pts',(-25.8290449701193,66.8680635103876,0.));
#96695=CARTESIAN_POINT('Ctrl Pts',(-25.8290449701193,66.8680635103876,12.));
#96696=CARTESIAN_POINT('Ctrl Pts',(-25.844249057147,66.8859026802088,0.));
#96697=CARTESIAN_POINT('Ctrl Pts',(-25.844249057147,66.8859026802088,12.));
#96698=CARTESIAN_POINT('Ctrl Pts',(-25.8594990868833,66.9037599932761,0.));
#96699=CARTESIAN_POINT('Ctrl Pts',(-25.8594990868833,66.9037599932761,12.));
#96700=CARTESIAN_POINT('Ctrl Pts',(-25.8747950260111,66.92163531213,0.));
#96701=CARTESIAN_POINT('Ctrl Pts',(-25.8747950260111,66.92163531213,12.));
#96702=CARTESIAN_POINT('Ctrl Pts',(-25.890136841266,66.939528499934,0.));
#96703=CARTESIAN_POINT('Ctrl Pts',(-25.890136841266,66.939528499934,12.));
#96704=CARTESIAN_POINT('Ctrl Pts',(-25.9055244994277,66.9574394204663,0.));
#96705=CARTESIAN_POINT('Ctrl Pts',(-25.9055244994277,66.9574394204663,12.));
#96706=CARTESIAN_POINT('Ctrl Pts',(-25.9209579673209,66.975367938115,0.));
#96707=CARTESIAN_POINT('Ctrl Pts',(-25.9209579673209,66.975367938115,12.));
#96708=CARTESIAN_POINT('Ctrl Pts',(-25.9364372118222,66.9933139178778,0.));
#96709=CARTESIAN_POINT('Ctrl Pts',(-25.9364372118222,66.9933139178778,12.));
#96710=CARTESIAN_POINT('Ctrl Pts',(-25.9519621998598,67.0112772253556,0.));
#96711=CARTESIAN_POINT('Ctrl Pts',(-25.9519621998598,67.0112772253556,12.));
#96712=CARTESIAN_POINT('Ctrl Pts',(-25.9675328984121,67.0292577267489,0.));
#96713=CARTESIAN_POINT('Ctrl Pts',(-25.9675328984121,67.0292577267489,12.));
#96714=CARTESIAN_POINT('Ctrl Pts',(-25.9831492744984,67.0472552888485,0.));
#96715=CARTESIAN_POINT('Ctrl Pts',(-25.9831492744984,67.0472552888485,12.));
#96716=CARTESIAN_POINT('Ctrl Pts',(-25.9988112951814,67.0652697790325,0.));
#96717=CARTESIAN_POINT('Ctrl Pts',(-25.9988112951814,67.0652697790325,12.));
#96718=CARTESIAN_POINT('Ctrl Pts',(-26.014518927573,67.0833010652634,0.));
#96719=CARTESIAN_POINT('Ctrl Pts',(-26.014518927573,67.0833010652634,12.));
#96720=CARTESIAN_POINT('Ctrl Pts',(-26.030272138834,67.101349016084,0.));
#96721=CARTESIAN_POINT('Ctrl Pts',(-26.030272138834,67.101349016084,12.));
#96722=CARTESIAN_POINT('Ctrl Pts',(-26.0460708961725,67.1194135006124,0.));
#96723=CARTESIAN_POINT('Ctrl Pts',(-26.0460708961725,67.1194135006124,12.));
#96724=CARTESIAN_POINT('Ctrl Pts',(-26.061915166836,67.1374943885354,0.));
#96725=CARTESIAN_POINT('Ctrl Pts',(-26.061915166836,67.1374943885354,12.));
#96726=CARTESIAN_POINT('Ctrl Pts',(-26.0778049181128,67.1555915501049,0.));
#96727=CARTESIAN_POINT('Ctrl Pts',(-26.0778049181128,67.1555915501049,12.));
#96728=CARTESIAN_POINT('Ctrl Pts',(-26.0937401173383,67.173704856136,0.));
#96729=CARTESIAN_POINT('Ctrl Pts',(-26.0937401173383,67.173704856136,12.));
#96730=CARTESIAN_POINT('Ctrl Pts',(-26.1097207318949,67.1918341780018,0.));
#96731=CARTESIAN_POINT('Ctrl Pts',(-26.1097207318949,67.1918341780018,12.));
#96732=CARTESIAN_POINT('Ctrl Pts',(-26.1257467292102,67.2099793876297,0.));
#96733=CARTESIAN_POINT('Ctrl Pts',(-26.1257467292102,67.2099793876297,12.));
#96734=CARTESIAN_POINT('Ctrl Pts',(-26.1418180767489,67.2281403574938,0.));
#96735=CARTESIAN_POINT('Ctrl Pts',(-26.1418180767489,67.2281403574938,12.));
#96736=CARTESIAN_POINT('Ctrl Pts',(-26.1579347420138,67.2463169606115,0.));
#96737=CARTESIAN_POINT('Ctrl Pts',(-26.1579347420138,67.2463169606115,12.));
#96738=CARTESIAN_POINT('Ctrl Pts',(-26.1740966925529,67.2645090705421,0.));
#96739=CARTESIAN_POINT('Ctrl Pts',(-26.1740966925529,67.2645090705421,12.));
#96740=CARTESIAN_POINT('Ctrl Pts',(-26.1903038959589,67.282716561383,0.));
#96741=CARTESIAN_POINT('Ctrl Pts',(-26.1903038959589,67.282716561383,12.));
#96742=CARTESIAN_POINT('Ctrl Pts',(-26.2065563198683,67.3009393077651,0.));
#96743=CARTESIAN_POINT('Ctrl Pts',(-26.2065563198683,67.3009393077651,12.));
#96744=CARTESIAN_POINT('Ctrl Pts',(-26.2228539319526,67.3191771848463,0.));
#96745=CARTESIAN_POINT('Ctrl Pts',(-26.2228539319526,67.3191771848463,12.));
#96746=CARTESIAN_POINT('Ctrl Pts',(-26.2391966999191,67.3374300683073,0.));
#96747=CARTESIAN_POINT('Ctrl Pts',(-26.2391966999191,67.3374300683073,12.));
#96748=CARTESIAN_POINT('Ctrl Pts',(-26.255584591518,67.3556978343507,0.));
#96749=CARTESIAN_POINT('Ctrl Pts',(-26.255584591518,67.3556978343507,12.));
#96750=CARTESIAN_POINT('Ctrl Pts',(-26.2720175745423,67.3739803596969,0.));
#96751=CARTESIAN_POINT('Ctrl Pts',(-26.2720175745423,67.3739803596969,12.));
#96752=CARTESIAN_POINT('Ctrl Pts',(-26.288495616827,67.392277521581,0.));
#96753=CARTESIAN_POINT('Ctrl Pts',(-26.288495616827,67.392277521581,12.));
#96754=CARTESIAN_POINT('Ctrl Pts',(-26.3050186862407,67.4105891977461,0.));
#96755=CARTESIAN_POINT('Ctrl Pts',(-26.3050186862407,67.4105891977461,12.));
#96756=CARTESIAN_POINT('Ctrl Pts',(-26.321586750686,67.4289152664398,0.));
#96757=CARTESIAN_POINT('Ctrl Pts',(-26.321586750686,67.4289152664398,12.));
#96758=CARTESIAN_POINT('Ctrl Pts',(-26.3381997781055,67.4472556064119,0.));
#96759=CARTESIAN_POINT('Ctrl Pts',(-26.3381997781055,67.4472556064119,12.));
#96760=CARTESIAN_POINT('Ctrl Pts',(-26.3548577364833,67.4656100969116,0.));
#96761=CARTESIAN_POINT('Ctrl Pts',(-26.3548577364833,67.4656100969116,12.));
#96762=CARTESIAN_POINT('Ctrl Pts',(-26.3715605938433,67.4839786176836,0.));
#96763=CARTESIAN_POINT('Ctrl Pts',(-26.3715605938433,67.4839786176836,12.));
#96764=CARTESIAN_POINT('Ctrl Pts',(-26.3883083182421,67.5023610489622,0.));
#96765=CARTESIAN_POINT('Ctrl Pts',(-26.3883083182421,67.5023610489622,12.));
#96766=CARTESIAN_POINT('Ctrl Pts',(-26.4051008777675,67.5207572714683,0.));
#96767=CARTESIAN_POINT('Ctrl Pts',(-26.4051008777675,67.5207572714683,12.));
#96768=CARTESIAN_POINT('Ctrl Pts',(-26.4219382405458,67.5391671664072,0.));
#96769=CARTESIAN_POINT('Ctrl Pts',(-26.4219382405458,67.5391671664072,12.));
#96770=CARTESIAN_POINT('Ctrl Pts',(-26.4388203747425,67.5575906154657,0.));
#96771=CARTESIAN_POINT('Ctrl Pts',(-26.4388203747425,67.5575906154657,12.));
#96772=CARTESIAN_POINT('Ctrl Pts',(-26.4557472485621,67.5760275008093,0.));
#96773=CARTESIAN_POINT('Ctrl Pts',(-26.4557472485621,67.5760275008093,12.));
#96774=CARTESIAN_POINT('Ctrl Pts',(-26.4727188302409,67.5944777050768,0.));
#96775=CARTESIAN_POINT('Ctrl Pts',(-26.4727188302409,67.5944777050768,12.));
#96776=CARTESIAN_POINT('Ctrl Pts',(-26.489735088044,67.6129411113757,0.));
#96777=CARTESIAN_POINT('Ctrl Pts',(-26.489735088044,67.6129411113757,12.));
#96778=CARTESIAN_POINT('Ctrl Pts',(-26.5067959902725,67.6314176032811,0.));
#96779=CARTESIAN_POINT('Ctrl Pts',(-26.5067959902725,67.6314176032811,12.));
#96780=CARTESIAN_POINT('Ctrl Pts',(-26.5239015052654,67.649907064832,0.));
#96781=CARTESIAN_POINT('Ctrl Pts',(-26.5239015052654,67.649907064832,12.));
#96782=CARTESIAN_POINT('Ctrl Pts',(-26.5410516013985,67.6684093805291,0.));
#96783=CARTESIAN_POINT('Ctrl Pts',(-26.5410516013985,67.6684093805291,12.));
#96784=CARTESIAN_POINT('Ctrl Pts',(-26.5582462470794,67.6869244353294,0.));
#96785=CARTESIAN_POINT('Ctrl Pts',(-26.5582462470794,67.6869244353294,12.));
#96786=CARTESIAN_POINT('Ctrl Pts',(-26.5754854107421,67.7054521146424,0.));
#96787=CARTESIAN_POINT('Ctrl Pts',(-26.5754854107421,67.7054521146424,12.));
#96788=CARTESIAN_POINT('Ctrl Pts',(-26.5927690608544,67.7239923043288,0.));
#96789=CARTESIAN_POINT('Ctrl Pts',(-26.5927690608544,67.7239923043288,12.));
#96790=CARTESIAN_POINT('Ctrl Pts',(-26.6100971659202,67.7425448906977,0.));
#96791=CARTESIAN_POINT('Ctrl Pts',(-26.6100971659202,67.7425448906977,12.));
#96792=CARTESIAN_POINT('Ctrl Pts',(-26.6274696944793,67.7611097605042,0.));
#96793=CARTESIAN_POINT('Ctrl Pts',(-26.6274696944793,67.7611097605042,12.));
#96794=CARTESIAN_POINT('Ctrl Pts',(-26.6448866151029,67.7796868009455,0.));
#96795=CARTESIAN_POINT('Ctrl Pts',(-26.6448866151029,67.7796868009455,12.));
#96796=CARTESIAN_POINT('Ctrl Pts',(-26.6623478963871,67.798275899657,0.));
#96797=CARTESIAN_POINT('Ctrl Pts',(-26.6623478963871,67.798275899657,12.));
#96798=CARTESIAN_POINT('Ctrl Pts',(-26.6798535069589,67.8168769447098,0.));
#96799=CARTESIAN_POINT('Ctrl Pts',(-26.6798535069589,67.8168769447098,12.));
#96800=CARTESIAN_POINT('Ctrl Pts',(-26.6974034154804,67.8354898246086,0.));
#96801=CARTESIAN_POINT('Ctrl Pts',(-26.6974034154804,67.8354898246086,12.));
#96802=CARTESIAN_POINT('Ctrl Pts',(-26.7149975906478,67.8541144282875,0.));
#96803=CARTESIAN_POINT('Ctrl Pts',(-26.7149975906478,67.8541144282875,12.));
#96804=CARTESIAN_POINT('Ctrl Pts',(-26.7326360011885,67.8727506451063,0.));
#96805=CARTESIAN_POINT('Ctrl Pts',(-26.7326360011885,67.8727506451063,12.));
#96806=CARTESIAN_POINT('Ctrl Pts',(-26.7503186158522,67.8913983648436,0.));
#96807=CARTESIAN_POINT('Ctrl Pts',(-26.7503186158522,67.8913983648436,12.));
#96808=CARTESIAN_POINT('Ctrl Pts',(-26.7680454034169,67.9100574776972,0.));
#96809=CARTESIAN_POINT('Ctrl Pts',(-26.7680454034169,67.9100574776972,12.));
#96810=CARTESIAN_POINT('Ctrl Pts',(-26.7858163326934,67.928727874284,0.));
#96811=CARTESIAN_POINT('Ctrl Pts',(-26.7858163326934,67.928727874284,12.));
#96812=CARTESIAN_POINT('Ctrl Pts',(-26.8036313725262,67.9474094456396,0.));
#96813=CARTESIAN_POINT('Ctrl Pts',(-26.8036313725262,67.9474094456396,12.));
#96814=CARTESIAN_POINT('Ctrl Pts',(-26.821490491792,67.9661020832164,0.));
#96815=CARTESIAN_POINT('Ctrl Pts',(-26.821490491792,67.9661020832164,12.));
#96816=CARTESIAN_POINT('Ctrl Pts',(-26.8393936593911,67.9848056788809,0.));
#96817=CARTESIAN_POINT('Ctrl Pts',(-26.8393936593911,67.9848056788809,12.));
#96818=CARTESIAN_POINT('Ctrl Pts',(-26.8573408442496,68.0035201249102,0.));
#96819=CARTESIAN_POINT('Ctrl Pts',(-26.8573408442496,68.0035201249102,12.));
#96820=CARTESIAN_POINT('Ctrl Pts',(-26.8753320153252,68.0222453139856,0.));
#96821=CARTESIAN_POINT('Ctrl Pts',(-26.8753320153252,68.0222453139856,12.));
#96822=CARTESIAN_POINT('Ctrl Pts',(-26.8933671416063,68.0409811391869,0.));
#96823=CARTESIAN_POINT('Ctrl Pts',(-26.8933671416063,68.0409811391869,12.));
#96824=CARTESIAN_POINT('Ctrl Pts',(-26.911446192111,68.0597274939859,0.));
#96825=CARTESIAN_POINT('Ctrl Pts',(-26.911446192111,68.0597274939859,12.));
#96826=CARTESIAN_POINT('Ctrl Pts',(-26.9295691358779,68.0784842722369,0.));
#96827=CARTESIAN_POINT('Ctrl Pts',(-26.9295691358779,68.0784842722369,12.));
#96828=CARTESIAN_POINT('Ctrl Pts',(-26.9477359419652,68.0972513681751,0.));
#96829=CARTESIAN_POINT('Ctrl Pts',(-26.9477359419652,68.0972513681751,12.));
#96830=CARTESIAN_POINT('Ctrl Pts',(-26.9659465794601,68.1160286764255,0.));
#96831=CARTESIAN_POINT('Ctrl Pts',(-26.9659465794601,68.1160286764255,12.));
#96832=CARTESIAN_POINT('Ctrl Pts',(-26.9842010174822,68.1348160920106,0.));
#96833=CARTESIAN_POINT('Ctrl Pts',(-26.9842010174822,68.1348160920106,12.));
#96834=CARTESIAN_POINT('Ctrl Pts',(-27.0024992251838,68.1536135103557,0.));
#96835=CARTESIAN_POINT('Ctrl Pts',(-27.0024992251838,68.1536135103557,12.));
#96836=CARTESIAN_POINT('Ctrl Pts',(-27.0208411717472,68.1724208272958,0.));
#96837=CARTESIAN_POINT('Ctrl Pts',(-27.0208411717472,68.1724208272958,12.));
#96838=CARTESIAN_POINT('Ctrl Pts',(-27.0392268263798,68.1912379390773,0.));
#96839=CARTESIAN_POINT('Ctrl Pts',(-27.0392268263798,68.1912379390773,12.));
#96840=CARTESIAN_POINT('Ctrl Pts',(-27.0576561583172,68.2100647423332,0.));
#96841=CARTESIAN_POINT('Ctrl Pts',(-27.0576561583172,68.2100647423332,12.));
#96842=CARTESIAN_POINT('Ctrl Pts',(-27.0761291368226,68.2289011340615,0.));
#96843=CARTESIAN_POINT('Ctrl Pts',(-27.0761291368226,68.2289011340615,12.));
#96844=CARTESIAN_POINT('Ctrl Pts',(-27.0946457311813,68.2477470116012,0.));
#96845=CARTESIAN_POINT('Ctrl Pts',(-27.0946457311813,68.2477470116012,12.));
#96846=CARTESIAN_POINT('Ctrl Pts',(-27.1132059106943,68.2666022726104,0.));
#96847=CARTESIAN_POINT('Ctrl Pts',(-27.1132059106943,68.2666022726104,12.));
#96848=CARTESIAN_POINT('Ctrl Pts',(-27.1318096446649,68.2854668150364,0.));
#96849=CARTESIAN_POINT('Ctrl Pts',(-27.1318096446649,68.2854668150364,12.));
#96850=CARTESIAN_POINT('Ctrl Pts',(-27.1504569024136,68.3043405371603,0.));
#96851=CARTESIAN_POINT('Ctrl Pts',(-27.1504569024136,68.3043405371603,12.));
#96852=CARTESIAN_POINT('Ctrl Pts',(-27.1691476532921,68.3232233376425,0.));
#96853=CARTESIAN_POINT('Ctrl Pts',(-27.1691476532921,68.3232233376425,12.));
#96854=CARTESIAN_POINT('Ctrl Pts',(-27.1878818666926,68.3421151155711,0.));
#96855=CARTESIAN_POINT('Ctrl Pts',(-27.1878818666926,68.3421151155711,12.));
#96856=CARTESIAN_POINT('Ctrl Pts',(-27.2066595120542,68.3610157704994,0.));
#96857=CARTESIAN_POINT('Ctrl Pts',(-27.2066595120542,68.3610157704994,12.));
#96858=CARTESIAN_POINT('Ctrl Pts',(-27.2254805588673,68.3799252025102,0.));
#96859=CARTESIAN_POINT('Ctrl Pts',(-27.2254805588673,68.3799252025102,12.));
#96860=CARTESIAN_POINT('Ctrl Pts',(-27.244344976665,68.3988433121581,0.));
#96861=CARTESIAN_POINT('Ctrl Pts',(-27.244344976665,68.3988433121581,12.));
#96862=CARTESIAN_POINT('Ctrl Pts',(-27.263252735006,68.4177700003465,0.));
#96863=CARTESIAN_POINT('Ctrl Pts',(-27.263252735006,68.4177700003465,12.));
#96864=CARTESIAN_POINT('Ctrl Pts',(-27.2822038034538,68.4367051682164,0.));
#96865=CARTESIAN_POINT('Ctrl Pts',(-27.2822038034538,68.4367051682164,12.));
#96866=CARTESIAN_POINT('Ctrl Pts',(-27.301198151557,68.4556487170441,0.));
#96867=CARTESIAN_POINT('Ctrl Pts',(-27.301198151557,68.4556487170441,12.));
#96868=CARTESIAN_POINT('Ctrl Pts',(-27.3202357488154,68.4746005480997,0.));
#96869=CARTESIAN_POINT('Ctrl Pts',(-27.3202357488154,68.4746005480997,12.));
#96870=CARTESIAN_POINT('Ctrl Pts',(-27.3393165646752,68.4935605626372,0.));
#96871=CARTESIAN_POINT('Ctrl Pts',(-27.3393165646752,68.4935605626372,12.));
#96872=CARTESIAN_POINT('Ctrl Pts',(-27.3584405685947,68.5125286621902,0.));
#96873=CARTESIAN_POINT('Ctrl Pts',(-27.3584405685947,68.5125286621902,12.));
#96874=CARTESIAN_POINT('Ctrl Pts',(-27.3776077300918,68.5315047488046,0.));
#96875=CARTESIAN_POINT('Ctrl Pts',(-27.3776077300918,68.5315047488046,12.));
#96876=CARTESIAN_POINT('Ctrl Pts',(-27.3968180187941,68.5504887252976,0.));
#96877=CARTESIAN_POINT('Ctrl Pts',(-27.3968180187941,68.5504887252976,12.));
#96878=CARTESIAN_POINT('Ctrl Pts',(-27.4160714044825,68.5694804955002,0.));
#96879=CARTESIAN_POINT('Ctrl Pts',(-27.4160714044825,68.5694804955002,12.));
#96880=CARTESIAN_POINT('Ctrl Pts',(-27.4353678571349,68.5884799645193,0.));
#96881=CARTESIAN_POINT('Ctrl Pts',(-27.4353678571349,68.5884799645193,12.));
#96882=CARTESIAN_POINT('Ctrl Pts',(-27.4547073468213,68.6074870381588,0.));
#96883=CARTESIAN_POINT('Ctrl Pts',(-27.4547073468213,68.6074870381588,12.));
#96884=CARTESIAN_POINT('Ctrl Pts',(-27.4740898435977,68.6265016223536,0.));
#96885=CARTESIAN_POINT('Ctrl Pts',(-27.4740898435977,68.6265016223536,12.));
#96886=CARTESIAN_POINT('Ctrl Pts',(-27.4935153173863,68.6455236225471,0.));
#96887=CARTESIAN_POINT('Ctrl Pts',(-27.4935153173863,68.6455236225471,12.));
#96888=CARTESIAN_POINT('Ctrl Pts',(-27.5129837378798,68.6645529432059,0.));
#96889=CARTESIAN_POINT('Ctrl Pts',(-27.5129837378798,68.6645529432059,12.));
#96890=CARTESIAN_POINT('Ctrl Pts',(-27.5324950743723,68.683589486992,0.));
#96891=CARTESIAN_POINT('Ctrl Pts',(-27.5324950743723,68.683589486992,12.));
#96892=CARTESIAN_POINT('Ctrl Pts',(-27.552049295893,68.7026331554348,0.));
#96893=CARTESIAN_POINT('Ctrl Pts',(-27.552049295893,68.7026331554348,12.));
#96894=CARTESIAN_POINT('Ctrl Pts',(-27.5716463715027,68.721683850427,0.));
#96895=CARTESIAN_POINT('Ctrl Pts',(-27.5716463715027,68.721683850427,12.));
#96896=CARTESIAN_POINT('Ctrl Pts',(-27.5912862705482,68.7407414755291,0.));
#96897=CARTESIAN_POINT('Ctrl Pts',(-27.5912862705482,68.7407414755291,12.));
#96898=CARTESIAN_POINT('Ctrl Pts',(-27.6109689629025,68.7598059372121,0.));
#96899=CARTESIAN_POINT('Ctrl Pts',(-27.6109689629025,68.7598059372121,12.));
#96900=CARTESIAN_POINT('Ctrl Pts',(-27.6306944192711,68.7788771464655,0.));
#96901=CARTESIAN_POINT('Ctrl Pts',(-27.6306944192711,68.7788771464655,12.));
#96902=CARTESIAN_POINT('Ctrl Pts',(-27.6504626112621,68.7979550191773,0.));
#96903=CARTESIAN_POINT('Ctrl Pts',(-27.6504626112621,68.7979550191773,12.));
#96904=CARTESIAN_POINT('Ctrl Pts',(-27.670273510707,68.8170394725786,0.));
#96905=CARTESIAN_POINT('Ctrl Pts',(-27.670273510707,68.8170394725786,12.));
#96906=CARTESIAN_POINT('Ctrl Pts',(-27.6901270891201,68.8361304224378,0.));
#96907=CARTESIAN_POINT('Ctrl Pts',(-27.6901270891201,68.8361304224378,12.));
#96908=CARTESIAN_POINT('Ctrl Pts',(-27.7100233170728,68.855227779818,0.));
#96909=CARTESIAN_POINT('Ctrl Pts',(-27.7100233170728,68.855227779818,12.));
#96910=CARTESIAN_POINT('Ctrl Pts',(-27.7299621636602,68.8743314483451,0.));
#96911=CARTESIAN_POINT('Ctrl Pts',(-27.7299621636602,68.8743314483451,12.));
#96912=CARTESIAN_POINT('Ctrl Pts',(-27.7499435957608,68.8934413203945,0.));
#96913=CARTESIAN_POINT('Ctrl Pts',(-27.7499435957608,68.8934413203945,12.));
#96914=CARTESIAN_POINT('Ctrl Pts',(-27.7699675790683,68.9125572825946,0.));
#96915=CARTESIAN_POINT('Ctrl Pts',(-27.7699675790683,68.9125572825946,12.));
#96916=CARTESIAN_POINT('Ctrl Pts',(-27.7900340793796,68.9316792226187,0.));
#96917=CARTESIAN_POINT('Ctrl Pts',(-27.7900340793796,68.9316792226187,12.));
#96918=CARTESIAN_POINT('Ctrl Pts',(-27.8101430638128,68.9508070357786,0.));
#96919=CARTESIAN_POINT('Ctrl Pts',(-27.8101430638128,68.9508070357786,12.));
#96920=CARTESIAN_POINT('Ctrl Pts',(-27.8302945019939,68.9699406311305,0.));
#96921=CARTESIAN_POINT('Ctrl Pts',(-27.8302945019939,68.9699406311305,12.));
#96922=CARTESIAN_POINT('Ctrl Pts',(-27.8504883673903,68.9890799391863,0.));
#96923=CARTESIAN_POINT('Ctrl Pts',(-27.8504883673903,68.9890799391863,12.));
#96924=CARTESIAN_POINT('Ctrl Pts',(-27.8707246380697,69.0082249138015,0.));
#96925=CARTESIAN_POINT('Ctrl Pts',(-27.8707246380697,69.0082249138015,12.));
#96926=CARTESIAN_POINT('Ctrl Pts',(-27.8910032967037,69.0273755264702,0.));
#96927=CARTESIAN_POINT('Ctrl Pts',(-27.8910032967037,69.0273755264702,12.));
#96928=CARTESIAN_POINT('Ctrl Pts',(-27.9072601239469,69.0427005153223,0.));
#96929=CARTESIAN_POINT('Ctrl Pts',(-27.9072601239469,69.0427005153223,12.));
#96930=CARTESIAN_POINT('Ctrl Pts',(-27.9194718098851,69.0541967850685,0.));
#96931=CARTESIAN_POINT('Ctrl Pts',(-27.9194718098851,69.0541967850685,12.));
#96932=CARTESIAN_POINT('Ctrl Pts',(-27.9276214070576,69.0618620884596,0.));
#96933=CARTESIAN_POINT('Ctrl Pts',(-27.9276214070576,69.0618620884596,12.));
#96934=CARTESIAN_POINT('Ctrl Pts',(-27.9316983239472,69.065695021045,0.));
#96935=CARTESIAN_POINT('Ctrl Pts',(-27.9316983239472,69.065695021045,12.));
#96936=CARTESIAN_POINT('',(-24.7419628022042,65.4815644032299,0.));
#96937=CARTESIAN_POINT('Ctrl Pts',(-24.7419628022042,65.4815644032299,0.));
#96938=CARTESIAN_POINT('Ctrl Pts',(-24.7442214063382,65.4847237095443,0.));
#96939=CARTESIAN_POINT('Ctrl Pts',(-24.7487434955982,65.4910454936254,0.));
#96940=CARTESIAN_POINT('Ctrl Pts',(-24.7555412724651,65.5005376841101,0.));
#96941=CARTESIAN_POINT('Ctrl Pts',(-24.7646342620841,65.5132129675333,0.));
#96942=CARTESIAN_POINT('Ctrl Pts',(-24.7760493148465,65.5290887770232,0.));
#96943=CARTESIAN_POINT('Ctrl Pts',(-24.7875131827491,65.5449962514661,0.));
#96944=CARTESIAN_POINT('Ctrl Pts',(-24.799025856126,65.5609353062829,0.));
#96945=CARTESIAN_POINT('Ctrl Pts',(-24.8105873098626,65.5769057914333,0.));
#96946=CARTESIAN_POINT('Ctrl Pts',(-24.8221975032104,65.5929074932624,0.));
#96947=CARTESIAN_POINT('Ctrl Pts',(-24.8338563866764,65.6089401625628,0.));
#96948=CARTESIAN_POINT('Ctrl Pts',(-24.8455639071517,65.6250035361612,0.));
#96949=CARTESIAN_POINT('Ctrl Pts',(-24.8573200135666,65.6410973603661,0.));
#96950=CARTESIAN_POINT('Ctrl Pts',(-24.8691246628057,65.6572214156692,0.));
#96951=CARTESIAN_POINT('Ctrl Pts',(-24.8809778178229,65.6733755087669,0.));
#96952=CARTESIAN_POINT('Ctrl Pts',(-24.8928794448607,65.6895594608775,0.));
#96953=CARTESIAN_POINT('Ctrl Pts',(-24.9048295111448,65.7057730980483,0.));
#96954=CARTESIAN_POINT('Ctrl Pts',(-24.9168279820106,65.7220162391053,0.));
#96955=CARTESIAN_POINT('Ctrl Pts',(-24.928874819458,65.7382886895888,0.));
#96956=CARTESIAN_POINT('Ctrl Pts',(-24.9409699836537,65.7545902480323,0.));
#96957=CARTESIAN_POINT('Ctrl Pts',(-24.9531134338696,65.7709207098959,0.));
#96958=CARTESIAN_POINT('Ctrl Pts',(-24.9653051295581,65.7872798720823,0.));
#96959=CARTESIAN_POINT('Ctrl Pts',(-24.9775450315683,65.8036675380718,0.));
#96960=CARTESIAN_POINT('Ctrl Pts',(-24.9898331020983,65.8200835177024,0.));
#96961=CARTESIAN_POINT('Ctrl Pts',(-25.002169304117,65.8365276247128,0.));
#96962=CARTESIAN_POINT('Ctrl Pts',(-25.0145536009604,65.8529996750445,0.));
#96963=CARTESIAN_POINT('Ctrl Pts',(-25.0269859558363,65.8694994847616,0.));
#96964=CARTESIAN_POINT('Ctrl Pts',(-25.0394663314055,65.8860268683128,0.));
#96965=CARTESIAN_POINT('Ctrl Pts',(-25.0519946900078,65.9025816394424,0.));
#96966=CARTESIAN_POINT('Ctrl Pts',(-25.0645709938524,65.919163611981,0.));
#96967=CARTESIAN_POINT('Ctrl Pts',(-25.0771952052028,65.9357726006163,0.));
#96968=CARTESIAN_POINT('Ctrl Pts',(-25.0898672865915,65.9524084218139,0.));
#96969=CARTESIAN_POINT('Ctrl Pts',(-25.1025872009004,65.9690708941558,0.));
#96970=CARTESIAN_POINT('Ctrl Pts',(-25.1153549112503,65.9857598378433,0.));
#96971=CARTESIAN_POINT('Ctrl Pts',(-25.1281703809297,66.0024750743897,0.));
#96972=CARTESIAN_POINT('Ctrl Pts',(-25.1410335733099,66.0192164262621,0.));
#96973=CARTESIAN_POINT('Ctrl Pts',(-25.1539444517419,66.0359837164734,0.));
#96974=CARTESIAN_POINT('Ctrl Pts',(-25.1669029795661,66.0527767686025,0.));
#96975=CARTESIAN_POINT('Ctrl Pts',(-25.1799091201599,66.0695954069713,0.));
#96976=CARTESIAN_POINT('Ctrl Pts',(-25.1929628369685,66.086439456768,0.));
#96977=CARTESIAN_POINT('Ctrl Pts',(-25.2060640935365,66.10330874419,0.));
#96978=CARTESIAN_POINT('Ctrl Pts',(-25.2192128535357,66.1202030965758,0.));
#96979=CARTESIAN_POINT('Ctrl Pts',(-25.232409080755,66.1371223423345,0.));
#96980=CARTESIAN_POINT('Ctrl Pts',(-25.2456527390875,66.1540663108754,0.));
#96981=CARTESIAN_POINT('Ctrl Pts',(-25.2589437925147,66.1710348325384,0.));
#96982=CARTESIAN_POINT('Ctrl Pts',(-25.2722822050837,66.1880277385136,0.));
#96983=CARTESIAN_POINT('Ctrl Pts',(-25.285667940893,66.2050448607911,0.));
#96984=CARTESIAN_POINT('Ctrl Pts',(-25.2991009641094,66.2220860321952,0.));
#96985=CARTESIAN_POINT('Ctrl Pts',(-25.312581238973,66.2391510863998,0.));
#96986=CARTESIAN_POINT('Ctrl Pts',(-25.3261087298026,66.2562398579471,0.));
#96987=CARTESIAN_POINT('Ctrl Pts',(-25.3396834009949,66.2733521822662,0.));
#96988=CARTESIAN_POINT('Ctrl Pts',(-25.3533052170249,66.290487895671,0.));
#96989=CARTESIAN_POINT('Ctrl Pts',(-25.3669741424488,66.3076468353412,0.));
#96990=CARTESIAN_POINT('Ctrl Pts',(-25.3806901419012,66.3248288393046,0.));
#96991=CARTESIAN_POINT('Ctrl Pts',(-25.3944531800901,66.3420337464178,0.));
#96992=CARTESIAN_POINT('Ctrl Pts',(-25.4082632217847,66.359261396341,0.));
#96993=CARTESIAN_POINT('Ctrl Pts',(-25.4221202318199,66.3765116295364,0.));
#96994=CARTESIAN_POINT('Ctrl Pts',(-25.4360241751018,66.3937842872685,0.));
#96995=CARTESIAN_POINT('Ctrl Pts',(-25.4499750166079,66.4110792116,0.));
#96996=CARTESIAN_POINT('Ctrl Pts',(-25.4639727213849,66.4283962453899,0.));
#96997=CARTESIAN_POINT('Ctrl Pts',(-25.4780172545417,66.4457352322871,0.));
#96998=CARTESIAN_POINT('Ctrl Pts',(-25.4921085812548,66.4630960167252,0.));
#96999=CARTESIAN_POINT('Ctrl Pts',(-25.5062466667702,66.4804784439148,0.));
#97000=CARTESIAN_POINT('Ctrl Pts',(-25.5204314764033,66.4978823598354,0.));
#97001=CARTESIAN_POINT('Ctrl Pts',(-25.534662975532,66.5153076112231,0.));
#97002=CARTESIAN_POINT('Ctrl Pts',(-25.5489411295912,66.5327540455624,0.));
#97003=CARTESIAN_POINT('Ctrl Pts',(-25.5632659040792,66.5502215110829,0.));
#97004=CARTESIAN_POINT('Ctrl Pts',(-25.5776372645601,66.5677098567542,0.));
#97005=CARTESIAN_POINT('Ctrl Pts',(-25.5920551766629,66.5852189322813,0.));
#97006=CARTESIAN_POINT('Ctrl Pts',(-25.6065196060756,66.6027485880963,0.));
#97007=CARTESIAN_POINT('Ctrl Pts',(-25.6210305185403,66.6202986753506,0.));
#97008=CARTESIAN_POINT('Ctrl Pts',(-25.6355878798614,66.6378690459129,0.));
#97009=CARTESIAN_POINT('Ctrl Pts',(-25.6501916559055,66.6554595523624,0.));
#97010=CARTESIAN_POINT('Ctrl Pts',(-25.6648418126013,66.6730700479837,0.));
#97011=CARTESIAN_POINT('Ctrl Pts',(-25.6795383159319,66.6907003867572,0.));
#97012=CARTESIAN_POINT('Ctrl Pts',(-25.6942811319322,66.7083504233529,0.));
#97013=CARTESIAN_POINT('Ctrl Pts',(-25.7090702266963,66.7260200131266,0.));
#97014=CARTESIAN_POINT('Ctrl Pts',(-25.7239055663772,66.7437090121153,0.));
#97015=CARTESIAN_POINT('Ctrl Pts',(-25.7387871171866,66.7614172770316,0.));
#97016=CARTESIAN_POINT('Ctrl Pts',(-25.7537148453864,66.7791446652545,0.));
#97017=CARTESIAN_POINT('Ctrl Pts',(-25.7686887172878,66.7968910348245,0.));
#97018=CARTESIAN_POINT('Ctrl Pts',(-25.7837086992595,66.8146562444433,0.));
#97019=CARTESIAN_POINT('Ctrl Pts',(-25.7987747577269,66.8324401534668,0.));
#97020=CARTESIAN_POINT('Ctrl Pts',(-25.8138868591709,66.8502426219001,0.));
#97021=CARTESIAN_POINT('Ctrl Pts',(-25.8290449701193,66.8680635103876,0.));
#97022=CARTESIAN_POINT('Ctrl Pts',(-25.844249057147,66.8859026802088,0.));
#97023=CARTESIAN_POINT('Ctrl Pts',(-25.8594990868833,66.9037599932761,0.));
#97024=CARTESIAN_POINT('Ctrl Pts',(-25.8747950260111,66.92163531213,0.));
#97025=CARTESIAN_POINT('Ctrl Pts',(-25.890136841266,66.939528499934,0.));
#97026=CARTESIAN_POINT('Ctrl Pts',(-25.9055244994277,66.9574394204663,0.));
#97027=CARTESIAN_POINT('Ctrl Pts',(-25.9209579673209,66.975367938115,0.));
#97028=CARTESIAN_POINT('Ctrl Pts',(-25.9364372118222,66.9933139178778,0.));
#97029=CARTESIAN_POINT('Ctrl Pts',(-25.9519621998598,67.0112772253556,0.));
#97030=CARTESIAN_POINT('Ctrl Pts',(-25.9675328984121,67.0292577267489,0.));
#97031=CARTESIAN_POINT('Ctrl Pts',(-25.9831492744984,67.0472552888485,0.));
#97032=CARTESIAN_POINT('Ctrl Pts',(-25.9988112951814,67.0652697790325,0.));
#97033=CARTESIAN_POINT('Ctrl Pts',(-26.014518927573,67.0833010652634,0.));
#97034=CARTESIAN_POINT('Ctrl Pts',(-26.030272138834,67.101349016084,0.));
#97035=CARTESIAN_POINT('Ctrl Pts',(-26.0460708961725,67.1194135006124,0.));
#97036=CARTESIAN_POINT('Ctrl Pts',(-26.061915166836,67.1374943885354,0.));
#97037=CARTESIAN_POINT('Ctrl Pts',(-26.0778049181128,67.1555915501049,0.));
#97038=CARTESIAN_POINT('Ctrl Pts',(-26.0937401173383,67.173704856136,0.));
#97039=CARTESIAN_POINT('Ctrl Pts',(-26.1097207318949,67.1918341780018,0.));
#97040=CARTESIAN_POINT('Ctrl Pts',(-26.1257467292102,67.2099793876297,0.));
#97041=CARTESIAN_POINT('Ctrl Pts',(-26.1418180767489,67.2281403574938,0.));
#97042=CARTESIAN_POINT('Ctrl Pts',(-26.1579347420138,67.2463169606115,0.));
#97043=CARTESIAN_POINT('Ctrl Pts',(-26.1740966925529,67.2645090705421,0.));
#97044=CARTESIAN_POINT('Ctrl Pts',(-26.1903038959589,67.282716561383,0.));
#97045=CARTESIAN_POINT('Ctrl Pts',(-26.2065563198683,67.3009393077651,0.));
#97046=CARTESIAN_POINT('Ctrl Pts',(-26.2228539319526,67.3191771848463,0.));
#97047=CARTESIAN_POINT('Ctrl Pts',(-26.2391966999191,67.3374300683073,0.));
#97048=CARTESIAN_POINT('Ctrl Pts',(-26.255584591518,67.3556978343507,0.));
#97049=CARTESIAN_POINT('Ctrl Pts',(-26.2720175745423,67.3739803596969,0.));
#97050=CARTESIAN_POINT('Ctrl Pts',(-26.288495616827,67.392277521581,0.));
#97051=CARTESIAN_POINT('Ctrl Pts',(-26.3050186862407,67.4105891977461,0.));
#97052=CARTESIAN_POINT('Ctrl Pts',(-26.321586750686,67.4289152664398,0.));
#97053=CARTESIAN_POINT('Ctrl Pts',(-26.3381997781055,67.4472556064119,0.));
#97054=CARTESIAN_POINT('Ctrl Pts',(-26.3548577364833,67.4656100969116,0.));
#97055=CARTESIAN_POINT('Ctrl Pts',(-26.3715605938433,67.4839786176836,0.));
#97056=CARTESIAN_POINT('Ctrl Pts',(-26.3883083182421,67.5023610489622,0.));
#97057=CARTESIAN_POINT('Ctrl Pts',(-26.4051008777675,67.5207572714683,0.));
#97058=CARTESIAN_POINT('Ctrl Pts',(-26.4219382405458,67.5391671664072,0.));
#97059=CARTESIAN_POINT('Ctrl Pts',(-26.4388203747425,67.5575906154657,0.));
#97060=CARTESIAN_POINT('Ctrl Pts',(-26.4557472485621,67.5760275008093,0.));
#97061=CARTESIAN_POINT('Ctrl Pts',(-26.4727188302409,67.5944777050768,0.));
#97062=CARTESIAN_POINT('Ctrl Pts',(-26.489735088044,67.6129411113757,0.));
#97063=CARTESIAN_POINT('Ctrl Pts',(-26.5067959902725,67.6314176032811,0.));
#97064=CARTESIAN_POINT('Ctrl Pts',(-26.5239015052654,67.649907064832,0.));
#97065=CARTESIAN_POINT('Ctrl Pts',(-26.5410516013985,67.6684093805291,0.));
#97066=CARTESIAN_POINT('Ctrl Pts',(-26.5582462470794,67.6869244353294,0.));
#97067=CARTESIAN_POINT('Ctrl Pts',(-26.5754854107421,67.7054521146424,0.));
#97068=CARTESIAN_POINT('Ctrl Pts',(-26.5927690608544,67.7239923043288,0.));
#97069=CARTESIAN_POINT('Ctrl Pts',(-26.6100971659202,67.7425448906977,0.));
#97070=CARTESIAN_POINT('Ctrl Pts',(-26.6274696944793,67.7611097605042,0.));
#97071=CARTESIAN_POINT('Ctrl Pts',(-26.6448866151029,67.7796868009455,0.));
#97072=CARTESIAN_POINT('Ctrl Pts',(-26.6623478963871,67.798275899657,0.));
#97073=CARTESIAN_POINT('Ctrl Pts',(-26.6798535069589,67.8168769447098,0.));
#97074=CARTESIAN_POINT('Ctrl Pts',(-26.6974034154804,67.8354898246086,0.));
#97075=CARTESIAN_POINT('Ctrl Pts',(-26.7149975906478,67.8541144282875,0.));
#97076=CARTESIAN_POINT('Ctrl Pts',(-26.7326360011885,67.8727506451063,0.));
#97077=CARTESIAN_POINT('Ctrl Pts',(-26.7503186158522,67.8913983648436,0.));
#97078=CARTESIAN_POINT('Ctrl Pts',(-26.7680454034169,67.9100574776972,0.));
#97079=CARTESIAN_POINT('Ctrl Pts',(-26.7858163326934,67.928727874284,0.));
#97080=CARTESIAN_POINT('Ctrl Pts',(-26.8036313725262,67.9474094456396,0.));
#97081=CARTESIAN_POINT('Ctrl Pts',(-26.821490491792,67.9661020832164,0.));
#97082=CARTESIAN_POINT('Ctrl Pts',(-26.8393936593911,67.9848056788809,0.));
#97083=CARTESIAN_POINT('Ctrl Pts',(-26.8573408442496,68.0035201249102,0.));
#97084=CARTESIAN_POINT('Ctrl Pts',(-26.8753320153252,68.0222453139856,0.));
#97085=CARTESIAN_POINT('Ctrl Pts',(-26.8933671416063,68.0409811391869,0.));
#97086=CARTESIAN_POINT('Ctrl Pts',(-26.911446192111,68.0597274939859,0.));
#97087=CARTESIAN_POINT('Ctrl Pts',(-26.9295691358779,68.0784842722369,0.));
#97088=CARTESIAN_POINT('Ctrl Pts',(-26.9477359419652,68.0972513681751,0.));
#97089=CARTESIAN_POINT('Ctrl Pts',(-26.9659465794601,68.1160286764255,0.));
#97090=CARTESIAN_POINT('Ctrl Pts',(-26.9842010174822,68.1348160920106,0.));
#97091=CARTESIAN_POINT('Ctrl Pts',(-27.0024992251838,68.1536135103557,0.));
#97092=CARTESIAN_POINT('Ctrl Pts',(-27.0208411717472,68.1724208272958,0.));
#97093=CARTESIAN_POINT('Ctrl Pts',(-27.0392268263798,68.1912379390773,0.));
#97094=CARTESIAN_POINT('Ctrl Pts',(-27.0576561583172,68.2100647423332,0.));
#97095=CARTESIAN_POINT('Ctrl Pts',(-27.0761291368226,68.2289011340615,0.));
#97096=CARTESIAN_POINT('Ctrl Pts',(-27.0946457311813,68.2477470116012,0.));
#97097=CARTESIAN_POINT('Ctrl Pts',(-27.1132059106943,68.2666022726104,0.));
#97098=CARTESIAN_POINT('Ctrl Pts',(-27.1318096446649,68.2854668150364,0.));
#97099=CARTESIAN_POINT('Ctrl Pts',(-27.1504569024136,68.3043405371603,0.));
#97100=CARTESIAN_POINT('Ctrl Pts',(-27.1691476532921,68.3232233376425,0.));
#97101=CARTESIAN_POINT('Ctrl Pts',(-27.1878818666926,68.3421151155711,0.));
#97102=CARTESIAN_POINT('Ctrl Pts',(-27.2066595120542,68.3610157704994,0.));
#97103=CARTESIAN_POINT('Ctrl Pts',(-27.2254805588673,68.3799252025102,0.));
#97104=CARTESIAN_POINT('Ctrl Pts',(-27.244344976665,68.3988433121581,0.));
#97105=CARTESIAN_POINT('Ctrl Pts',(-27.263252735006,68.4177700003465,0.));
#97106=CARTESIAN_POINT('Ctrl Pts',(-27.2822038034538,68.4367051682164,0.));
#97107=CARTESIAN_POINT('Ctrl Pts',(-27.301198151557,68.4556487170441,0.));
#97108=CARTESIAN_POINT('Ctrl Pts',(-27.3202357488154,68.4746005480997,0.));
#97109=CARTESIAN_POINT('Ctrl Pts',(-27.3393165646752,68.4935605626372,0.));
#97110=CARTESIAN_POINT('Ctrl Pts',(-27.3584405685947,68.5125286621902,0.));
#97111=CARTESIAN_POINT('Ctrl Pts',(-27.3776077300918,68.5315047488046,0.));
#97112=CARTESIAN_POINT('Ctrl Pts',(-27.3968180187941,68.5504887252976,0.));
#97113=CARTESIAN_POINT('Ctrl Pts',(-27.4160714044825,68.5694804955002,0.));
#97114=CARTESIAN_POINT('Ctrl Pts',(-27.4353678571349,68.5884799645193,0.));
#97115=CARTESIAN_POINT('Ctrl Pts',(-27.4547073468213,68.6074870381588,0.));
#97116=CARTESIAN_POINT('Ctrl Pts',(-27.4740898435977,68.6265016223536,0.));
#97117=CARTESIAN_POINT('Ctrl Pts',(-27.4935153173863,68.6455236225471,0.));
#97118=CARTESIAN_POINT('Ctrl Pts',(-27.5129837378798,68.6645529432059,0.));
#97119=CARTESIAN_POINT('Ctrl Pts',(-27.5324950743723,68.683589486992,0.));
#97120=CARTESIAN_POINT('Ctrl Pts',(-27.552049295893,68.7026331554348,0.));
#97121=CARTESIAN_POINT('Ctrl Pts',(-27.5716463715027,68.721683850427,0.));
#97122=CARTESIAN_POINT('Ctrl Pts',(-27.5912862705482,68.7407414755291,0.));
#97123=CARTESIAN_POINT('Ctrl Pts',(-27.6109689629025,68.7598059372121,0.));
#97124=CARTESIAN_POINT('Ctrl Pts',(-27.6306944192711,68.7788771464655,0.));
#97125=CARTESIAN_POINT('Ctrl Pts',(-27.6504626112621,68.7979550191773,0.));
#97126=CARTESIAN_POINT('Ctrl Pts',(-27.6674443909882,68.8143140938753,0.));
#97127=CARTESIAN_POINT('Ctrl Pts',(-27.6804870323286,68.826859785198,0.));
#97128=CARTESIAN_POINT('Ctrl Pts',(-27.6895716271084,68.8355891981877,0.));
#97129=CARTESIAN_POINT('Ctrl Pts',(-27.6946856803482,68.8405004465895,0.));
#97130=CARTESIAN_POINT('Ctrl Pts',(-27.6958230984757,68.8415926174774,0.));
#97131=CARTESIAN_POINT('',(-24.7419628022042,65.4815644032299,12.));
#97132=CARTESIAN_POINT('',(-24.7419628022042,65.4815644032299,0.));
#97133=CARTESIAN_POINT('Ctrl Pts',(-27.6958230984758,68.8415926174774,12.));
#97134=CARTESIAN_POINT('Ctrl Pts',(-27.6946856803482,68.8405004465895,12.));
#97135=CARTESIAN_POINT('Ctrl Pts',(-27.6895716271084,68.8355891981877,12.));
#97136=CARTESIAN_POINT('Ctrl Pts',(-27.6804870323286,68.826859785198,12.));
#97137=CARTESIAN_POINT('Ctrl Pts',(-27.6674443909882,68.8143140938753,12.));
#97138=CARTESIAN_POINT('Ctrl Pts',(-27.6504626112621,68.7979550191773,12.));
#97139=CARTESIAN_POINT('Ctrl Pts',(-27.6306944192711,68.7788771464655,12.));
#97140=CARTESIAN_POINT('Ctrl Pts',(-27.6109689629025,68.7598059372121,12.));
#97141=CARTESIAN_POINT('Ctrl Pts',(-27.5912862705482,68.7407414755291,12.));
#97142=CARTESIAN_POINT('Ctrl Pts',(-27.5716463715027,68.721683850427,12.));
#97143=CARTESIAN_POINT('Ctrl Pts',(-27.552049295893,68.7026331554348,12.));
#97144=CARTESIAN_POINT('Ctrl Pts',(-27.5324950743723,68.683589486992,12.));
#97145=CARTESIAN_POINT('Ctrl Pts',(-27.5129837378798,68.6645529432059,12.));
#97146=CARTESIAN_POINT('Ctrl Pts',(-27.4935153173863,68.6455236225471,12.));
#97147=CARTESIAN_POINT('Ctrl Pts',(-27.4740898435977,68.6265016223536,12.));
#97148=CARTESIAN_POINT('Ctrl Pts',(-27.4547073468213,68.6074870381588,12.));
#97149=CARTESIAN_POINT('Ctrl Pts',(-27.4353678571349,68.5884799645193,12.));
#97150=CARTESIAN_POINT('Ctrl Pts',(-27.4160714044825,68.5694804955002,12.));
#97151=CARTESIAN_POINT('Ctrl Pts',(-27.3968180187941,68.5504887252976,12.));
#97152=CARTESIAN_POINT('Ctrl Pts',(-27.3776077300918,68.5315047488046,12.));
#97153=CARTESIAN_POINT('Ctrl Pts',(-27.3584405685947,68.5125286621902,12.));
#97154=CARTESIAN_POINT('Ctrl Pts',(-27.3393165646752,68.4935605626372,12.));
#97155=CARTESIAN_POINT('Ctrl Pts',(-27.3202357488154,68.4746005480997,12.));
#97156=CARTESIAN_POINT('Ctrl Pts',(-27.301198151557,68.4556487170441,12.));
#97157=CARTESIAN_POINT('Ctrl Pts',(-27.2822038034538,68.4367051682164,12.));
#97158=CARTESIAN_POINT('Ctrl Pts',(-27.263252735006,68.4177700003465,12.));
#97159=CARTESIAN_POINT('Ctrl Pts',(-27.244344976665,68.3988433121581,12.));
#97160=CARTESIAN_POINT('Ctrl Pts',(-27.2254805588673,68.3799252025102,12.));
#97161=CARTESIAN_POINT('Ctrl Pts',(-27.2066595120542,68.3610157704994,12.));
#97162=CARTESIAN_POINT('Ctrl Pts',(-27.1878818666926,68.3421151155711,12.));
#97163=CARTESIAN_POINT('Ctrl Pts',(-27.1691476532921,68.3232233376425,12.));
#97164=CARTESIAN_POINT('Ctrl Pts',(-27.1504569024136,68.3043405371603,12.));
#97165=CARTESIAN_POINT('Ctrl Pts',(-27.1318096446649,68.2854668150364,12.));
#97166=CARTESIAN_POINT('Ctrl Pts',(-27.1132059106943,68.2666022726104,12.));
#97167=CARTESIAN_POINT('Ctrl Pts',(-27.0946457311813,68.2477470116012,12.));
#97168=CARTESIAN_POINT('Ctrl Pts',(-27.0761291368226,68.2289011340615,12.));
#97169=CARTESIAN_POINT('Ctrl Pts',(-27.0576561583172,68.2100647423332,12.));
#97170=CARTESIAN_POINT('Ctrl Pts',(-27.0392268263798,68.1912379390773,12.));
#97171=CARTESIAN_POINT('Ctrl Pts',(-27.0208411717472,68.1724208272958,12.));
#97172=CARTESIAN_POINT('Ctrl Pts',(-27.0024992251838,68.1536135103557,12.));
#97173=CARTESIAN_POINT('Ctrl Pts',(-26.9842010174822,68.1348160920106,12.));
#97174=CARTESIAN_POINT('Ctrl Pts',(-26.9659465794601,68.1160286764255,12.));
#97175=CARTESIAN_POINT('Ctrl Pts',(-26.9477359419652,68.0972513681751,12.));
#97176=CARTESIAN_POINT('Ctrl Pts',(-26.9295691358779,68.0784842722369,12.));
#97177=CARTESIAN_POINT('Ctrl Pts',(-26.911446192111,68.0597274939859,12.));
#97178=CARTESIAN_POINT('Ctrl Pts',(-26.8933671416063,68.0409811391869,12.));
#97179=CARTESIAN_POINT('Ctrl Pts',(-26.8753320153252,68.0222453139856,12.));
#97180=CARTESIAN_POINT('Ctrl Pts',(-26.8573408442496,68.0035201249102,12.));
#97181=CARTESIAN_POINT('Ctrl Pts',(-26.8393936593911,67.9848056788809,12.));
#97182=CARTESIAN_POINT('Ctrl Pts',(-26.821490491792,67.9661020832164,12.));
#97183=CARTESIAN_POINT('Ctrl Pts',(-26.8036313725262,67.9474094456396,12.));
#97184=CARTESIAN_POINT('Ctrl Pts',(-26.7858163326934,67.928727874284,12.));
#97185=CARTESIAN_POINT('Ctrl Pts',(-26.7680454034169,67.9100574776972,12.));
#97186=CARTESIAN_POINT('Ctrl Pts',(-26.7503186158522,67.8913983648436,12.));
#97187=CARTESIAN_POINT('Ctrl Pts',(-26.7326360011885,67.8727506451063,12.));
#97188=CARTESIAN_POINT('Ctrl Pts',(-26.7149975906478,67.8541144282875,12.));
#97189=CARTESIAN_POINT('Ctrl Pts',(-26.6974034154804,67.8354898246086,12.));
#97190=CARTESIAN_POINT('Ctrl Pts',(-26.6798535069589,67.8168769447098,12.));
#97191=CARTESIAN_POINT('Ctrl Pts',(-26.6623478963871,67.798275899657,12.));
#97192=CARTESIAN_POINT('Ctrl Pts',(-26.6448866151029,67.7796868009455,12.));
#97193=CARTESIAN_POINT('Ctrl Pts',(-26.6274696944793,67.7611097605042,12.));
#97194=CARTESIAN_POINT('Ctrl Pts',(-26.6100971659202,67.7425448906977,12.));
#97195=CARTESIAN_POINT('Ctrl Pts',(-26.5927690608544,67.7239923043288,12.));
#97196=CARTESIAN_POINT('Ctrl Pts',(-26.5754854107421,67.7054521146424,12.));
#97197=CARTESIAN_POINT('Ctrl Pts',(-26.5582462470794,67.6869244353294,12.));
#97198=CARTESIAN_POINT('Ctrl Pts',(-26.5410516013985,67.6684093805291,12.));
#97199=CARTESIAN_POINT('Ctrl Pts',(-26.5239015052654,67.649907064832,12.));
#97200=CARTESIAN_POINT('Ctrl Pts',(-26.5067959902725,67.6314176032811,12.));
#97201=CARTESIAN_POINT('Ctrl Pts',(-26.489735088044,67.6129411113757,12.));
#97202=CARTESIAN_POINT('Ctrl Pts',(-26.4727188302409,67.5944777050768,12.));
#97203=CARTESIAN_POINT('Ctrl Pts',(-26.4557472485621,67.5760275008093,12.));
#97204=CARTESIAN_POINT('Ctrl Pts',(-26.4388203747425,67.5575906154657,12.));
#97205=CARTESIAN_POINT('Ctrl Pts',(-26.4219382405458,67.5391671664072,12.));
#97206=CARTESIAN_POINT('Ctrl Pts',(-26.4051008777675,67.5207572714683,12.));
#97207=CARTESIAN_POINT('Ctrl Pts',(-26.3883083182421,67.5023610489622,12.));
#97208=CARTESIAN_POINT('Ctrl Pts',(-26.3715605938433,67.4839786176836,12.));
#97209=CARTESIAN_POINT('Ctrl Pts',(-26.3548577364833,67.4656100969116,12.));
#97210=CARTESIAN_POINT('Ctrl Pts',(-26.3381997781055,67.4472556064119,12.));
#97211=CARTESIAN_POINT('Ctrl Pts',(-26.321586750686,67.4289152664398,12.));
#97212=CARTESIAN_POINT('Ctrl Pts',(-26.3050186862407,67.4105891977461,12.));
#97213=CARTESIAN_POINT('Ctrl Pts',(-26.288495616827,67.392277521581,12.));
#97214=CARTESIAN_POINT('Ctrl Pts',(-26.2720175745423,67.3739803596969,12.));
#97215=CARTESIAN_POINT('Ctrl Pts',(-26.255584591518,67.3556978343507,12.));
#97216=CARTESIAN_POINT('Ctrl Pts',(-26.2391966999191,67.3374300683073,12.));
#97217=CARTESIAN_POINT('Ctrl Pts',(-26.2228539319526,67.3191771848463,12.));
#97218=CARTESIAN_POINT('Ctrl Pts',(-26.2065563198683,67.3009393077651,12.));
#97219=CARTESIAN_POINT('Ctrl Pts',(-26.1903038959589,67.282716561383,12.));
#97220=CARTESIAN_POINT('Ctrl Pts',(-26.1740966925529,67.2645090705421,12.));
#97221=CARTESIAN_POINT('Ctrl Pts',(-26.1579347420138,67.2463169606115,12.));
#97222=CARTESIAN_POINT('Ctrl Pts',(-26.1418180767489,67.2281403574938,12.));
#97223=CARTESIAN_POINT('Ctrl Pts',(-26.1257467292102,67.2099793876297,12.));
#97224=CARTESIAN_POINT('Ctrl Pts',(-26.1097207318949,67.1918341780018,12.));
#97225=CARTESIAN_POINT('Ctrl Pts',(-26.0937401173383,67.173704856136,12.));
#97226=CARTESIAN_POINT('Ctrl Pts',(-26.0778049181128,67.1555915501049,12.));
#97227=CARTESIAN_POINT('Ctrl Pts',(-26.061915166836,67.1374943885354,12.));
#97228=CARTESIAN_POINT('Ctrl Pts',(-26.0460708961725,67.1194135006124,12.));
#97229=CARTESIAN_POINT('Ctrl Pts',(-26.030272138834,67.101349016084,12.));
#97230=CARTESIAN_POINT('Ctrl Pts',(-26.014518927573,67.0833010652634,12.));
#97231=CARTESIAN_POINT('Ctrl Pts',(-25.9988112951814,67.0652697790325,12.));
#97232=CARTESIAN_POINT('Ctrl Pts',(-25.9831492744984,67.0472552888485,12.));
#97233=CARTESIAN_POINT('Ctrl Pts',(-25.9675328984121,67.0292577267489,12.));
#97234=CARTESIAN_POINT('Ctrl Pts',(-25.9519621998598,67.0112772253556,12.));
#97235=CARTESIAN_POINT('Ctrl Pts',(-25.9364372118222,66.9933139178778,12.));
#97236=CARTESIAN_POINT('Ctrl Pts',(-25.9209579673209,66.975367938115,12.));
#97237=CARTESIAN_POINT('Ctrl Pts',(-25.9055244994277,66.9574394204663,12.));
#97238=CARTESIAN_POINT('Ctrl Pts',(-25.890136841266,66.939528499934,12.));
#97239=CARTESIAN_POINT('Ctrl Pts',(-25.8747950260111,66.92163531213,12.));
#97240=CARTESIAN_POINT('Ctrl Pts',(-25.8594990868833,66.9037599932761,12.));
#97241=CARTESIAN_POINT('Ctrl Pts',(-25.844249057147,66.8859026802088,12.));
#97242=CARTESIAN_POINT('Ctrl Pts',(-25.8290449701193,66.8680635103876,12.));
#97243=CARTESIAN_POINT('Ctrl Pts',(-25.8138868591709,66.8502426219001,12.));
#97244=CARTESIAN_POINT('Ctrl Pts',(-25.7987747577269,66.8324401534668,12.));
#97245=CARTESIAN_POINT('Ctrl Pts',(-25.7837086992595,66.8146562444433,12.));
#97246=CARTESIAN_POINT('Ctrl Pts',(-25.7686887172878,66.7968910348245,12.));
#97247=CARTESIAN_POINT('Ctrl Pts',(-25.7537148453864,66.7791446652545,12.));
#97248=CARTESIAN_POINT('Ctrl Pts',(-25.7387871171866,66.7614172770316,12.));
#97249=CARTESIAN_POINT('Ctrl Pts',(-25.7239055663772,66.7437090121153,12.));
#97250=CARTESIAN_POINT('Ctrl Pts',(-25.7090702266963,66.7260200131266,12.));
#97251=CARTESIAN_POINT('Ctrl Pts',(-25.6942811319322,66.7083504233529,12.));
#97252=CARTESIAN_POINT('Ctrl Pts',(-25.6795383159319,66.6907003867572,12.));
#97253=CARTESIAN_POINT('Ctrl Pts',(-25.6648418126013,66.6730700479837,12.));
#97254=CARTESIAN_POINT('Ctrl Pts',(-25.6501916559055,66.6554595523624,12.));
#97255=CARTESIAN_POINT('Ctrl Pts',(-25.6355878798614,66.6378690459129,12.));
#97256=CARTESIAN_POINT('Ctrl Pts',(-25.6210305185403,66.6202986753506,12.));
#97257=CARTESIAN_POINT('Ctrl Pts',(-25.6065196060756,66.6027485880963,12.));
#97258=CARTESIAN_POINT('Ctrl Pts',(-25.5920551766629,66.5852189322813,12.));
#97259=CARTESIAN_POINT('Ctrl Pts',(-25.5776372645601,66.5677098567542,12.));
#97260=CARTESIAN_POINT('Ctrl Pts',(-25.5632659040792,66.5502215110829,12.));
#97261=CARTESIAN_POINT('Ctrl Pts',(-25.5489411295912,66.5327540455624,12.));
#97262=CARTESIAN_POINT('Ctrl Pts',(-25.534662975532,66.5153076112231,12.));
#97263=CARTESIAN_POINT('Ctrl Pts',(-25.5204314764033,66.4978823598354,12.));
#97264=CARTESIAN_POINT('Ctrl Pts',(-25.5062466667702,66.4804784439148,12.));
#97265=CARTESIAN_POINT('Ctrl Pts',(-25.4921085812548,66.4630960167252,12.));
#97266=CARTESIAN_POINT('Ctrl Pts',(-25.4780172545417,66.4457352322871,12.));
#97267=CARTESIAN_POINT('Ctrl Pts',(-25.4639727213849,66.4283962453899,12.));
#97268=CARTESIAN_POINT('Ctrl Pts',(-25.4499750166079,66.4110792116,12.));
#97269=CARTESIAN_POINT('Ctrl Pts',(-25.4360241751018,66.3937842872685,12.));
#97270=CARTESIAN_POINT('Ctrl Pts',(-25.4221202318199,66.3765116295364,12.));
#97271=CARTESIAN_POINT('Ctrl Pts',(-25.4082632217847,66.359261396341,12.));
#97272=CARTESIAN_POINT('Ctrl Pts',(-25.3944531800901,66.3420337464178,12.));
#97273=CARTESIAN_POINT('Ctrl Pts',(-25.3806901419012,66.3248288393046,12.));
#97274=CARTESIAN_POINT('Ctrl Pts',(-25.3669741424488,66.3076468353412,12.));
#97275=CARTESIAN_POINT('Ctrl Pts',(-25.3533052170249,66.290487895671,12.));
#97276=CARTESIAN_POINT('Ctrl Pts',(-25.3396834009949,66.2733521822662,12.));
#97277=CARTESIAN_POINT('Ctrl Pts',(-25.3261087298026,66.2562398579471,12.));
#97278=CARTESIAN_POINT('Ctrl Pts',(-25.312581238973,66.2391510863998,12.));
#97279=CARTESIAN_POINT('Ctrl Pts',(-25.2991009641094,66.2220860321952,12.));
#97280=CARTESIAN_POINT('Ctrl Pts',(-25.285667940893,66.2050448607911,12.));
#97281=CARTESIAN_POINT('Ctrl Pts',(-25.2722822050837,66.1880277385136,12.));
#97282=CARTESIAN_POINT('Ctrl Pts',(-25.2589437925147,66.1710348325384,12.));
#97283=CARTESIAN_POINT('Ctrl Pts',(-25.2456527390875,66.1540663108754,12.));
#97284=CARTESIAN_POINT('Ctrl Pts',(-25.232409080755,66.1371223423345,12.));
#97285=CARTESIAN_POINT('Ctrl Pts',(-25.2192128535357,66.1202030965758,12.));
#97286=CARTESIAN_POINT('Ctrl Pts',(-25.2060640935365,66.10330874419,12.));
#97287=CARTESIAN_POINT('Ctrl Pts',(-25.1929628369685,66.086439456768,12.));
#97288=CARTESIAN_POINT('Ctrl Pts',(-25.1799091201599,66.0695954069713,12.));
#97289=CARTESIAN_POINT('Ctrl Pts',(-25.1669029795661,66.0527767686025,12.));
#97290=CARTESIAN_POINT('Ctrl Pts',(-25.1539444517419,66.0359837164734,12.));
#97291=CARTESIAN_POINT('Ctrl Pts',(-25.1410335733099,66.0192164262621,12.));
#97292=CARTESIAN_POINT('Ctrl Pts',(-25.1281703809297,66.0024750743897,12.));
#97293=CARTESIAN_POINT('Ctrl Pts',(-25.1153549112503,65.9857598378433,12.));
#97294=CARTESIAN_POINT('Ctrl Pts',(-25.1025872009004,65.9690708941558,12.));
#97295=CARTESIAN_POINT('Ctrl Pts',(-25.0898672865915,65.9524084218139,12.));
#97296=CARTESIAN_POINT('Ctrl Pts',(-25.0771952052028,65.9357726006163,12.));
#97297=CARTESIAN_POINT('Ctrl Pts',(-25.0645709938524,65.919163611981,12.));
#97298=CARTESIAN_POINT('Ctrl Pts',(-25.0519946900078,65.9025816394424,12.));
#97299=CARTESIAN_POINT('Ctrl Pts',(-25.0394663314055,65.8860268683128,12.));
#97300=CARTESIAN_POINT('Ctrl Pts',(-25.0269859558363,65.8694994847616,12.));
#97301=CARTESIAN_POINT('Ctrl Pts',(-25.0145536009604,65.8529996750445,12.));
#97302=CARTESIAN_POINT('Ctrl Pts',(-25.002169304117,65.8365276247128,12.));
#97303=CARTESIAN_POINT('Ctrl Pts',(-24.9898331020983,65.8200835177024,12.));
#97304=CARTESIAN_POINT('Ctrl Pts',(-24.9775450315683,65.8036675380718,12.));
#97305=CARTESIAN_POINT('Ctrl Pts',(-24.9653051295581,65.7872798720823,12.));
#97306=CARTESIAN_POINT('Ctrl Pts',(-24.9531134338696,65.7709207098959,12.));
#97307=CARTESIAN_POINT('Ctrl Pts',(-24.9409699836537,65.7545902480323,12.));
#97308=CARTESIAN_POINT('Ctrl Pts',(-24.928874819458,65.7382886895888,12.));
#97309=CARTESIAN_POINT('Ctrl Pts',(-24.9168279820106,65.7220162391053,12.));
#97310=CARTESIAN_POINT('Ctrl Pts',(-24.9048295111448,65.7057730980483,12.));
#97311=CARTESIAN_POINT('Ctrl Pts',(-24.8928794448607,65.6895594608775,12.));
#97312=CARTESIAN_POINT('Ctrl Pts',(-24.8809778178229,65.6733755087669,12.));
#97313=CARTESIAN_POINT('Ctrl Pts',(-24.8691246628057,65.6572214156692,12.));
#97314=CARTESIAN_POINT('Ctrl Pts',(-24.8573200135666,65.6410973603661,12.));
#97315=CARTESIAN_POINT('Ctrl Pts',(-24.8455639071517,65.6250035361612,12.));
#97316=CARTESIAN_POINT('Ctrl Pts',(-24.8338563866764,65.6089401625628,12.));
#97317=CARTESIAN_POINT('Ctrl Pts',(-24.8221975032104,65.5929074932624,12.));
#97318=CARTESIAN_POINT('Ctrl Pts',(-24.8105873098626,65.5769057914333,12.));
#97319=CARTESIAN_POINT('Ctrl Pts',(-24.799025856126,65.5609353062829,12.));
#97320=CARTESIAN_POINT('Ctrl Pts',(-24.7875131827491,65.5449962514661,12.));
#97321=CARTESIAN_POINT('Ctrl Pts',(-24.7760493148465,65.5290887770232,12.));
#97322=CARTESIAN_POINT('Ctrl Pts',(-24.7646342620841,65.5132129675333,12.));
#97323=CARTESIAN_POINT('Ctrl Pts',(-24.7555412724651,65.5005376841101,12.));
#97324=CARTESIAN_POINT('Ctrl Pts',(-24.7487434955982,65.4910454936254,12.));
#97325=CARTESIAN_POINT('Ctrl Pts',(-24.7442214063382,65.4847237095443,12.));
#97326=CARTESIAN_POINT('Ctrl Pts',(-24.7419628022042,65.4815644032299,12.));
#97327=CARTESIAN_POINT('Ctrl Pts',(-29.0944526440266,68.2622612910177,0.));
#97328=CARTESIAN_POINT('Ctrl Pts',(-29.0944526440266,68.2622612910177,4.));
#97329=CARTESIAN_POINT('Ctrl Pts',(-29.0944526440266,68.2622612910177,8.));
#97330=CARTESIAN_POINT('Ctrl Pts',(-29.0944526440266,68.2622612910177,12.));
#97331=CARTESIAN_POINT('Ctrl Pts',(-29.0922231502663,68.3721211369508,0.));
#97332=CARTESIAN_POINT('Ctrl Pts',(-29.0922231502663,68.3721211369508,4.));
#97333=CARTESIAN_POINT('Ctrl Pts',(-29.0922231502664,68.3721211369509,8.00000000000001));
#97334=CARTESIAN_POINT('Ctrl Pts',(-29.0922231502664,68.3721211369509,12.));
#97335=CARTESIAN_POINT('Ctrl Pts',(-29.0225207419381,68.5624216146675,0.));
#97336=CARTESIAN_POINT('Ctrl Pts',(-29.0225207419381,68.5624216146675,4.00000000000001));
#97337=CARTESIAN_POINT('Ctrl Pts',(-29.0225207419382,68.5624216146676,7.99999999999999));
#97338=CARTESIAN_POINT('Ctrl Pts',(-29.0225207419382,68.5624216146676,12.));
#97339=CARTESIAN_POINT('Ctrl Pts',(-28.8637726134455,68.6814343344131,0.));
#97340=CARTESIAN_POINT('Ctrl Pts',(-28.8637726134455,68.6814343344131,3.99999999999999));
#97341=CARTESIAN_POINT('Ctrl Pts',(-28.8637726134455,68.6814343344132,8.00000000000001));
#97342=CARTESIAN_POINT('Ctrl Pts',(-28.8637726134455,68.6814343344132,12.));
#97343=CARTESIAN_POINT('Ctrl Pts',(-28.7877620302417,68.7132793373318,0.));
#97344=CARTESIAN_POINT('Ctrl Pts',(-28.7877620302417,68.7132793373318,4.));
#97345=CARTESIAN_POINT('Ctrl Pts',(-28.7877620302417,68.7132793373319,8.));
#97346=CARTESIAN_POINT('Ctrl Pts',(-28.7877620302417,68.7132793373319,12.));
#97347=CARTESIAN_POINT('',(-29.0944526440266,68.2622612910177,0.));
#97348=CARTESIAN_POINT('',(-28.7877620302417,68.7132793373317,0.));
#97349=CARTESIAN_POINT('Ctrl Pts',(-29.0944526440266,68.2622612910177,0.));
#97350=CARTESIAN_POINT('Ctrl Pts',(-29.0922231502663,68.3721211369508,0.));
#97351=CARTESIAN_POINT('Ctrl Pts',(-29.0523932026502,68.4808642670747,0.));
#97352=CARTESIAN_POINT('Ctrl Pts',(-28.983487101511,68.5663297619426,0.));
#97353=CARTESIAN_POINT('Ctrl Pts',(-28.9318075256566,68.6304288830936,0.));
#97354=CARTESIAN_POINT('Ctrl Pts',(-28.8637726134455,68.6814343344131,0.));
#97355=CARTESIAN_POINT('Ctrl Pts',(-28.7877620302417,68.7132793373318,0.));
#97356=CARTESIAN_POINT('',(-28.7877620302417,68.7132793373317,12.));
#97357=CARTESIAN_POINT('Ctrl Pts',(-28.7877620302417,68.7132793373318,0.));
#97358=CARTESIAN_POINT('Ctrl Pts',(-28.7877620302417,68.7132793373318,4.));
#97359=CARTESIAN_POINT('Ctrl Pts',(-28.7877620302417,68.7132793373319,8.));
#97360=CARTESIAN_POINT('Ctrl Pts',(-28.7877620302417,68.7132793373319,12.));
#97361=CARTESIAN_POINT('',(-29.0944526440266,68.2622612910177,12.));
#97362=CARTESIAN_POINT('Ctrl Pts',(-28.7877620302417,68.7132793373319,12.));
#97363=CARTESIAN_POINT('Ctrl Pts',(-28.8637726134455,68.6814343344132,12.));
#97364=CARTESIAN_POINT('Ctrl Pts',(-28.9318075256567,68.6304288830936,12.));
#97365=CARTESIAN_POINT('Ctrl Pts',(-28.9834871015111,68.5663297619426,12.));
#97366=CARTESIAN_POINT('Ctrl Pts',(-29.0523932026503,68.4808642670747,12.));
#97367=CARTESIAN_POINT('Ctrl Pts',(-29.0922231502664,68.3721211369509,12.));
#97368=CARTESIAN_POINT('Ctrl Pts',(-29.0944526440266,68.2622612910177,12.));
#97369=CARTESIAN_POINT('Ctrl Pts',(-29.0944526440266,68.2622612910177,12.));
#97370=CARTESIAN_POINT('Ctrl Pts',(-29.0944526440266,68.2622612910177,8.));
#97371=CARTESIAN_POINT('Ctrl Pts',(-29.0944526440266,68.2622612910177,4.));
#97372=CARTESIAN_POINT('Ctrl Pts',(-29.0944526440266,68.2622612910177,0.));
#97373=CARTESIAN_POINT('Origin',(-1.43538201480493E-10,3.46272497684358E-10,
0.));
#97374=CARTESIAN_POINT('Origin',(-1.43538201480493E-10,3.46272497684358E-10,
12.));
#97375=CARTESIAN_POINT('Origin',(-1.43538201480493E-10,3.46272497684358E-10,
0.));
#97376=CARTESIAN_POINT('Ctrl Pts',(-22.1153394458717,71.1418425484881,0.));
#97377=CARTESIAN_POINT('Ctrl Pts',(-22.1153394458717,71.1418425484881,4.));
#97378=CARTESIAN_POINT('Ctrl Pts',(-22.1153394458717,71.1418425484881,8.));
#97379=CARTESIAN_POINT('Ctrl Pts',(-22.1153394458717,71.1418425484881,12.));
#97380=CARTESIAN_POINT('Ctrl Pts',(-22.0104100349463,71.1744611799059,0.));
#97381=CARTESIAN_POINT('Ctrl Pts',(-22.0104100349463,71.1744611799059,4.));
#97382=CARTESIAN_POINT('Ctrl Pts',(-22.0104100349463,71.1744611799059,8.));
#97383=CARTESIAN_POINT('Ctrl Pts',(-22.0104100349463,71.1744611799059,12.));
#97384=CARTESIAN_POINT('Ctrl Pts',(-21.8078334561031,71.1685011351939,0.));
#97385=CARTESIAN_POINT('Ctrl Pts',(-21.8078334561031,71.1685011351939,4.00000000000001));
#97386=CARTESIAN_POINT('Ctrl Pts',(-21.8078334561031,71.1685011351939,8.));
#97387=CARTESIAN_POINT('Ctrl Pts',(-21.8078334561031,71.1685011351939,12.));
#97388=CARTESIAN_POINT('Ctrl Pts',(-21.6447353227844,71.0555229320374,0.));
#97389=CARTESIAN_POINT('Ctrl Pts',(-21.6447353227844,71.0555229320374,4.));
#97390=CARTESIAN_POINT('Ctrl Pts',(-21.6447353227845,71.0555229320374,8.00000000000001));
#97391=CARTESIAN_POINT('Ctrl Pts',(-21.6447353227845,71.0555229320374,12.));
#97392=CARTESIAN_POINT('Ctrl Pts',(-21.5904919934804,70.9934796068773,0.));
#97393=CARTESIAN_POINT('Ctrl Pts',(-21.5904919934804,70.9934796068773,4.));
#97394=CARTESIAN_POINT('Ctrl Pts',(-21.5904919934805,70.9934796068772,8.));
#97395=CARTESIAN_POINT('Ctrl Pts',(-21.5904919934805,70.9934796068772,12.));
#97396=CARTESIAN_POINT('',(-22.1153394458717,71.1418425484881,0.));
#97397=CARTESIAN_POINT('',(-21.59049199348,70.9934796068777,0.));
#97398=CARTESIAN_POINT('Ctrl Pts',(-22.1153394458717,71.1418425484881,1.38777878078145E-16));
#97399=CARTESIAN_POINT('Ctrl Pts',(-22.0104100349463,71.1744611799059,1.38777878078144E-16));
#97400=CARTESIAN_POINT('Ctrl Pts',(-21.894651989893,71.1710554400705,1.38777878078145E-16));
#97401=CARTESIAN_POINT('Ctrl Pts',(-21.7917848658274,71.1327049954369,1.38777878078145E-16));
#97402=CARTESIAN_POINT('Ctrl Pts',(-21.7146345227781,71.1039421619616,1.38777878078145E-16));
#97403=CARTESIAN_POINT('Ctrl Pts',(-21.6447353227844,71.0555229320374,1.38777878078144E-16));
#97404=CARTESIAN_POINT('Ctrl Pts',(-21.5904919934804,70.9934796068773,1.38777878078145E-16));
#97405=CARTESIAN_POINT('',(-21.59049199348,70.9934796068777,12.));
#97406=CARTESIAN_POINT('Ctrl Pts',(-21.5904919934804,70.9934796068773,0.));
#97407=CARTESIAN_POINT('Ctrl Pts',(-21.5904919934804,70.9934796068773,4.));
#97408=CARTESIAN_POINT('Ctrl Pts',(-21.5904919934805,70.9934796068772,8.));
#97409=CARTESIAN_POINT('Ctrl Pts',(-21.5904919934805,70.9934796068772,12.));
#97410=CARTESIAN_POINT('',(-22.1153394458717,71.1418425484881,12.));
#97411=CARTESIAN_POINT('Ctrl Pts',(-21.5904919934805,70.9934796068772,12.));
#97412=CARTESIAN_POINT('Ctrl Pts',(-21.6447353227845,71.0555229320374,12.));
#97413=CARTESIAN_POINT('Ctrl Pts',(-21.7146345227782,71.1039421619616,12.));
#97414=CARTESIAN_POINT('Ctrl Pts',(-21.7917848658274,71.1327049954368,12.));
#97415=CARTESIAN_POINT('Ctrl Pts',(-21.894651989893,71.1710554400705,12.));
#97416=CARTESIAN_POINT('Ctrl Pts',(-22.0104100349463,71.1744611799059,12.));
#97417=CARTESIAN_POINT('Ctrl Pts',(-22.1153394458717,71.1418425484881,12.));
#97418=CARTESIAN_POINT('Ctrl Pts',(-22.1153394458717,71.1418425484881,12.));
#97419=CARTESIAN_POINT('Ctrl Pts',(-22.1153394458717,71.1418425484881,8.));
#97420=CARTESIAN_POINT('Ctrl Pts',(-22.1153394458717,71.1418425484881,4.));
#97421=CARTESIAN_POINT('Ctrl Pts',(-22.1153394458717,71.1418425484881,0.));
#97422=CARTESIAN_POINT('Ctrl Pts',(-18.9407177820969,67.3887914263118,0.));
#97423=CARTESIAN_POINT('Ctrl Pts',(-18.9407177820969,67.3887914263118,12.));
#97424=CARTESIAN_POINT('Ctrl Pts',(-18.9426924398719,67.3921355608328,0.));
#97425=CARTESIAN_POINT('Ctrl Pts',(-18.9426924398719,67.3921355608328,12.));
#97426=CARTESIAN_POINT('Ctrl Pts',(-18.9466463414299,67.3988274146651,0.));
#97427=CARTESIAN_POINT('Ctrl Pts',(-18.9466463414299,67.3988274146651,12.));
#97428=CARTESIAN_POINT('Ctrl Pts',(-18.9525909517915,67.4088759497911,0.));
#97429=CARTESIAN_POINT('Ctrl Pts',(-18.9525909517915,67.4088759497911,12.));
#97430=CARTESIAN_POINT('Ctrl Pts',(-18.9605446160985,67.4222955061981,0.));
#97431=CARTESIAN_POINT('Ctrl Pts',(-18.9605446160985,67.4222955061981,12.));
#97432=CARTESIAN_POINT('Ctrl Pts',(-18.9705325631711,67.4391057908418,0.));
#97433=CARTESIAN_POINT('Ctrl Pts',(-18.9705325631711,67.4391057908418,12.));
#97434=CARTESIAN_POINT('Ctrl Pts',(-18.9805663798448,67.4559518744638,0.));
#97435=CARTESIAN_POINT('Ctrl Pts',(-18.9805663798448,67.4559518744638,12.));
#97436=CARTESIAN_POINT('Ctrl Pts',(-18.9906460638625,67.472833671964,0.));
#97437=CARTESIAN_POINT('Ctrl Pts',(-18.9906460638625,67.472833671964,12.));
#97438=CARTESIAN_POINT('Ctrl Pts',(-19.0007716032819,67.4897510316844,0.));
#97439=CARTESIAN_POINT('Ctrl Pts',(-19.0007716032819,67.4897510316844,12.));
#97440=CARTESIAN_POINT('Ctrl Pts',(-19.0109429761306,67.5067037372317,0.));
#97441=CARTESIAN_POINT('Ctrl Pts',(-19.0109429761306,67.5067037372317,12.));
#97442=CARTESIAN_POINT('Ctrl Pts',(-19.021160154824,67.5236915360331,0.));
#97443=CARTESIAN_POINT('Ctrl Pts',(-19.021160154824,67.5236915360331,12.));
#97444=CARTESIAN_POINT('Ctrl Pts',(-19.0314231093923,67.540714161288,0.));
#97445=CARTESIAN_POINT('Ctrl Pts',(-19.0314231093923,67.540714161288,12.));
#97446=CARTESIAN_POINT('Ctrl Pts',(-19.0417318110708,67.5577713558194,0.));
#97447=CARTESIAN_POINT('Ctrl Pts',(-19.0417318110708,67.5577713558194,12.));
#97448=CARTESIAN_POINT('Ctrl Pts',(-19.0520862360396,67.5748628971964,0.));
#97449=CARTESIAN_POINT('Ctrl Pts',(-19.0520862360396,67.5748628971964,12.));
#97450=CARTESIAN_POINT('Ctrl Pts',(-19.062486364241,67.5919885896222,0.));
#97451=CARTESIAN_POINT('Ctrl Pts',(-19.062486364241,67.5919885896222,12.));
#97452=CARTESIAN_POINT('Ctrl Pts',(-19.072932177628,67.6091482520534,0.));
#97453=CARTESIAN_POINT('Ctrl Pts',(-19.072932177628,67.6091482520534,12.));
#97454=CARTESIAN_POINT('Ctrl Pts',(-19.0834236587118,67.6263417083426,0.));
#97455=CARTESIAN_POINT('Ctrl Pts',(-19.0834236587118,67.6263417083426,12.));
#97456=CARTESIAN_POINT('Ctrl Pts',(-19.0939607887501,67.6435687749841,0.));
#97457=CARTESIAN_POINT('Ctrl Pts',(-19.0939607887501,67.6435687749841,12.));
#97458=CARTESIAN_POINT('Ctrl Pts',(-19.1045435468358,67.6608292549462,0.));
#97459=CARTESIAN_POINT('Ctrl Pts',(-19.1045435468358,67.6608292549462,12.));
#97460=CARTESIAN_POINT('Ctrl Pts',(-19.115171910846,67.6781229440573,0.));
#97461=CARTESIAN_POINT('Ctrl Pts',(-19.115171910846,67.6781229440573,12.));
#97462=CARTESIAN_POINT('Ctrl Pts',(-19.1258458580345,67.6954496350063,0.));
#97463=CARTESIAN_POINT('Ctrl Pts',(-19.1258458580345,67.6954496350063,12.));
#97464=CARTESIAN_POINT('Ctrl Pts',(-19.136565365709,67.7128091219348,0.));
#97465=CARTESIAN_POINT('Ctrl Pts',(-19.136565365709,67.7128091219348,12.));
#97466=CARTESIAN_POINT('Ctrl Pts',(-19.1473304119955,67.7302012056584,0.));
#97467=CARTESIAN_POINT('Ctrl Pts',(-19.1473304119955,67.7302012056584,12.));
#97468=CARTESIAN_POINT('Ctrl Pts',(-19.1581409758097,67.7476256934444,0.));
#97469=CARTESIAN_POINT('Ctrl Pts',(-19.1581409758097,67.7476256934444,12.));
#97470=CARTESIAN_POINT('Ctrl Pts',(-19.168997036495,67.7650823965127,0.));
#97471=CARTESIAN_POINT('Ctrl Pts',(-19.168997036495,67.7650823965127,12.));
#97472=CARTESIAN_POINT('Ctrl Pts',(-19.1798985735688,67.7825711283096,0.));
#97473=CARTESIAN_POINT('Ctrl Pts',(-19.1798985735688,67.7825711283096,12.));
#97474=CARTESIAN_POINT('Ctrl Pts',(-19.1908455664098,67.8000917023926,0.));
#97475=CARTESIAN_POINT('Ctrl Pts',(-19.1908455664098,67.8000917023926,12.));
#97476=CARTESIAN_POINT('Ctrl Pts',(-19.201837993993,67.8176439306621,0.));
#97477=CARTESIAN_POINT('Ctrl Pts',(-19.201837993993,67.8176439306621,12.));
#97478=CARTESIAN_POINT('Ctrl Pts',(-19.2128758350346,67.835227624289,0.));
#97479=CARTESIAN_POINT('Ctrl Pts',(-19.2128758350346,67.835227624289,12.));
#97480=CARTESIAN_POINT('Ctrl Pts',(-19.2239590681133,67.8528425945184,0.));
#97481=CARTESIAN_POINT('Ctrl Pts',(-19.2239590681133,67.8528425945184,12.));
#97482=CARTESIAN_POINT('Ctrl Pts',(-19.2350876717874,67.8704886534544,0.));
#97483=CARTESIAN_POINT('Ctrl Pts',(-19.2350876717874,67.8704886534544,12.));
#97484=CARTESIAN_POINT('Ctrl Pts',(-19.2462616247279,67.8881656149955,0.));
#97485=CARTESIAN_POINT('Ctrl Pts',(-19.2462616247279,67.8881656149955,12.));
#97486=CARTESIAN_POINT('Ctrl Pts',(-19.2574809057696,67.9058732951788,0.));
#97487=CARTESIAN_POINT('Ctrl Pts',(-19.2574809057696,67.9058732951788,12.));
#97488=CARTESIAN_POINT('Ctrl Pts',(-19.2687454938442,67.9236115116758,0.));
#97489=CARTESIAN_POINT('Ctrl Pts',(-19.2687454938442,67.9236115116758,12.));
#97490=CARTESIAN_POINT('Ctrl Pts',(-19.280055367936,67.9413800834793,0.));
#97491=CARTESIAN_POINT('Ctrl Pts',(-19.280055367936,67.9413800834793,12.));
#97492=CARTESIAN_POINT('Ctrl Pts',(-19.2914105070286,67.9591788305394,0.));
#97493=CARTESIAN_POINT('Ctrl Pts',(-19.2914105070286,67.9591788305394,12.));
#97494=CARTESIAN_POINT('Ctrl Pts',(-19.302810890038,67.9770075733485,0.));
#97495=CARTESIAN_POINT('Ctrl Pts',(-19.302810890038,67.9770075733485,12.));
#97496=CARTESIAN_POINT('Ctrl Pts',(-19.3142564958203,67.9948661329617,0.));
#97497=CARTESIAN_POINT('Ctrl Pts',(-19.3142564958203,67.9948661329617,12.));
#97498=CARTESIAN_POINT('Ctrl Pts',(-19.3257473032034,68.0127543311776,0.));
#97499=CARTESIAN_POINT('Ctrl Pts',(-19.3257473032034,68.0127543311776,12.));
#97500=CARTESIAN_POINT('Ctrl Pts',(-19.3372832910076,68.0306719906636,0.));
#97501=CARTESIAN_POINT('Ctrl Pts',(-19.3372832910076,68.0306719906636,12.));
#97502=CARTESIAN_POINT('Ctrl Pts',(-19.3488644380641,68.0486189351011,0.));
#97503=CARTESIAN_POINT('Ctrl Pts',(-19.3488644380641,68.0486189351011,12.));
#97504=CARTESIAN_POINT('Ctrl Pts',(-19.3604907232314,68.0665949893195,0.));
#97505=CARTESIAN_POINT('Ctrl Pts',(-19.3604907232314,68.0665949893195,12.));
#97506=CARTESIAN_POINT('Ctrl Pts',(-19.3721621253912,68.0845999792247,0.));
#97507=CARTESIAN_POINT('Ctrl Pts',(-19.3721621253912,68.0845999792247,12.));
#97508=CARTESIAN_POINT('Ctrl Pts',(-19.3838786234421,68.1026337317285,0.));
#97509=CARTESIAN_POINT('Ctrl Pts',(-19.3838786234421,68.1026337317285,12.));
#97510=CARTESIAN_POINT('Ctrl Pts',(-19.3956401962895,68.1206960746769,0.));
#97511=CARTESIAN_POINT('Ctrl Pts',(-19.3956401962895,68.1206960746769,12.));
#97512=CARTESIAN_POINT('Ctrl Pts',(-19.40744682283,68.1387868367691,0.));
#97513=CARTESIAN_POINT('Ctrl Pts',(-19.40744682283,68.1387868367691,12.));
#97514=CARTESIAN_POINT('Ctrl Pts',(-19.4192984819418,68.1569058475054,0.));
#97515=CARTESIAN_POINT('Ctrl Pts',(-19.4192984819418,68.1569058475054,12.));
#97516=CARTESIAN_POINT('Ctrl Pts',(-19.4311951524983,68.1750529372232,0.));
#97517=CARTESIAN_POINT('Ctrl Pts',(-19.4311951524983,68.1750529372232,12.));
#97518=CARTESIAN_POINT('Ctrl Pts',(-19.4431368133719,68.1932279371127,0.));
#97519=CARTESIAN_POINT('Ctrl Pts',(-19.4431368133719,68.1932279371127,12.));
#97520=CARTESIAN_POINT('Ctrl Pts',(-19.455123443438,68.2114306792358,0.));
#97521=CARTESIAN_POINT('Ctrl Pts',(-19.455123443438,68.2114306792358,12.));
#97522=CARTESIAN_POINT('Ctrl Pts',(-19.467155021572,68.2296609965448,0.));
#97523=CARTESIAN_POINT('Ctrl Pts',(-19.467155021572,68.2296609965448,12.));
#97524=CARTESIAN_POINT('Ctrl Pts',(-19.4792315266501,68.2479187228803,0.));
#97525=CARTESIAN_POINT('Ctrl Pts',(-19.4792315266501,68.2479187228803,12.));
#97526=CARTESIAN_POINT('Ctrl Pts',(-19.4913529375543,68.2662036929526,0.));
#97527=CARTESIAN_POINT('Ctrl Pts',(-19.4913529375543,68.2662036929526,12.));
#97528=CARTESIAN_POINT('Ctrl Pts',(-19.5035192331705,68.2845157423233,0.));
#97529=CARTESIAN_POINT('Ctrl Pts',(-19.5035192331705,68.2845157423233,12.));
#97530=CARTESIAN_POINT('Ctrl Pts',(-19.5157303923856,68.3028547073864,0.));
#97531=CARTESIAN_POINT('Ctrl Pts',(-19.5157303923856,68.3028547073864,12.));
#97532=CARTESIAN_POINT('Ctrl Pts',(-19.5279863940773,68.3212204253417,0.));
#97533=CARTESIAN_POINT('Ctrl Pts',(-19.5279863940773,68.3212204253417,12.));
#97534=CARTESIAN_POINT('Ctrl Pts',(-19.5402872171191,68.3396127341938,0.));
#97535=CARTESIAN_POINT('Ctrl Pts',(-19.5402872171191,68.3396127341938,12.));
#97536=CARTESIAN_POINT('Ctrl Pts',(-19.5526328403852,68.3580314727523,0.));
#97537=CARTESIAN_POINT('Ctrl Pts',(-19.5526328403852,68.3580314727523,12.));
#97538=CARTESIAN_POINT('Ctrl Pts',(-19.5650232427516,68.3764764806287,0.));
#97539=CARTESIAN_POINT('Ctrl Pts',(-19.5650232427516,68.3764764806287,12.));
#97540=CARTESIAN_POINT('Ctrl Pts',(-19.5774584030938,68.3949475982335,0.));
#97541=CARTESIAN_POINT('Ctrl Pts',(-19.5774584030938,68.3949475982335,12.));
#97542=CARTESIAN_POINT('Ctrl Pts',(-19.5899383002802,68.4134446667696,0.));
#97543=CARTESIAN_POINT('Ctrl Pts',(-19.5899383002802,68.4134446667696,12.));
#97544=CARTESIAN_POINT('Ctrl Pts',(-19.6024629131785,68.4319675282275,0.));
#97545=CARTESIAN_POINT('Ctrl Pts',(-19.6024629131785,68.4319675282275,12.));
#97546=CARTESIAN_POINT('Ctrl Pts',(-19.6150322206577,68.4505160253778,0.));
#97547=CARTESIAN_POINT('Ctrl Pts',(-19.6150322206577,68.4505160253778,12.));
#97548=CARTESIAN_POINT('Ctrl Pts',(-19.6276462015888,68.4690900017632,0.));
#97549=CARTESIAN_POINT('Ctrl Pts',(-19.6276462015888,68.4690900017632,12.));
#97550=CARTESIAN_POINT('Ctrl Pts',(-19.6403048348395,68.4876893016856,0.));
#97551=CARTESIAN_POINT('Ctrl Pts',(-19.6403048348395,68.4876893016856,12.));
#97552=CARTESIAN_POINT('Ctrl Pts',(-19.6530080992686,68.5063137701971,0.));
#97553=CARTESIAN_POINT('Ctrl Pts',(-19.6530080992686,68.5063137701971,12.));
#97554=CARTESIAN_POINT('Ctrl Pts',(-19.6657559737336,68.5249632530979,0.));
#97555=CARTESIAN_POINT('Ctrl Pts',(-19.6657559737336,68.5249632530979,12.));
#97556=CARTESIAN_POINT('Ctrl Pts',(-19.6785484370927,68.5436375969311,0.));
#97557=CARTESIAN_POINT('Ctrl Pts',(-19.6785484370927,68.5436375969311,12.));
#97558=CARTESIAN_POINT('Ctrl Pts',(-19.6913854682046,68.5623366489779,0.));
#97559=CARTESIAN_POINT('Ctrl Pts',(-19.6913854682046,68.5623366489779,12.));
#97560=CARTESIAN_POINT('Ctrl Pts',(-19.7042670459237,68.581060257249,0.));
#97561=CARTESIAN_POINT('Ctrl Pts',(-19.7042670459237,68.581060257249,12.));
#97562=CARTESIAN_POINT('Ctrl Pts',(-19.7171931490956,68.5998082704766,0.));
#97563=CARTESIAN_POINT('Ctrl Pts',(-19.7171931490956,68.5998082704766,12.));
#97564=CARTESIAN_POINT('Ctrl Pts',(-19.7301637565652,68.6185805381126,0.));
#97565=CARTESIAN_POINT('Ctrl Pts',(-19.7301637565652,68.6185805381126,12.));
#97566=CARTESIAN_POINT('Ctrl Pts',(-19.7431788471776,68.6373769103224,0.));
#97567=CARTESIAN_POINT('Ctrl Pts',(-19.7431788471776,68.6373769103224,12.));
#97568=CARTESIAN_POINT('Ctrl Pts',(-19.7562383997781,68.6561972379793,0.));
#97569=CARTESIAN_POINT('Ctrl Pts',(-19.7562383997781,68.6561972379793,12.));
#97570=CARTESIAN_POINT('Ctrl Pts',(-19.7693423932058,68.6750413726547,0.));
#97571=CARTESIAN_POINT('Ctrl Pts',(-19.7693423932058,68.6750413726547,12.));
#97572=CARTESIAN_POINT('Ctrl Pts',(-19.7824908062913,68.6939091666111,0.));
#97573=CARTESIAN_POINT('Ctrl Pts',(-19.7824908062913,68.6939091666111,12.));
#97574=CARTESIAN_POINT('Ctrl Pts',(-19.795683617864,68.7128004727998,0.));
#97575=CARTESIAN_POINT('Ctrl Pts',(-19.795683617864,68.7128004727998,12.));
#97576=CARTESIAN_POINT('Ctrl Pts',(-19.8089208067532,68.7317151448557,0.));
#97577=CARTESIAN_POINT('Ctrl Pts',(-19.8089208067532,68.7317151448557,12.));
#97578=CARTESIAN_POINT('Ctrl Pts',(-19.8222023517874,68.7506530370918,0.));
#97579=CARTESIAN_POINT('Ctrl Pts',(-19.8222023517874,68.7506530370918,12.));
#97580=CARTESIAN_POINT('Ctrl Pts',(-19.835528231787,68.7696140044892,0.));
#97581=CARTESIAN_POINT('Ctrl Pts',(-19.835528231787,68.7696140044892,12.));
#97582=CARTESIAN_POINT('Ctrl Pts',(-19.8488984255641,68.7885979026927,0.));
#97583=CARTESIAN_POINT('Ctrl Pts',(-19.8488984255641,68.7885979026927,12.));
#97584=CARTESIAN_POINT('Ctrl Pts',(-19.8623129119304,68.8076045880102,0.));
#97585=CARTESIAN_POINT('Ctrl Pts',(-19.8623129119304,68.8076045880102,12.));
#97586=CARTESIAN_POINT('Ctrl Pts',(-19.8757716696969,68.8266339174068,0.));
#97587=CARTESIAN_POINT('Ctrl Pts',(-19.8757716696969,68.8266339174068,12.));
#97588=CARTESIAN_POINT('Ctrl Pts',(-19.8892746776734,68.8456857484988,0.));
#97589=CARTESIAN_POINT('Ctrl Pts',(-19.8892746776734,68.8456857484988,12.));
#97590=CARTESIAN_POINT('Ctrl Pts',(-19.9028219146607,68.8647599395437,0.));
#97591=CARTESIAN_POINT('Ctrl Pts',(-19.9028219146607,68.8647599395437,12.));
#97592=CARTESIAN_POINT('Ctrl Pts',(-19.9164133594513,68.8838563494356,0.));
#97593=CARTESIAN_POINT('Ctrl Pts',(-19.9164133594513,68.8838563494356,12.));
#97594=CARTESIAN_POINT('Ctrl Pts',(-19.9300489908364,68.902974837704,0.));
#97595=CARTESIAN_POINT('Ctrl Pts',(-19.9300489908364,68.902974837704,12.));
#97596=CARTESIAN_POINT('Ctrl Pts',(-19.9437287876063,68.9221152645086,0.));
#97597=CARTESIAN_POINT('Ctrl Pts',(-19.9437287876063,68.9221152645086,12.));
#97598=CARTESIAN_POINT('Ctrl Pts',(-19.9574527285492,68.9412774906346,0.));
#97599=CARTESIAN_POINT('Ctrl Pts',(-19.9574527285492,68.9412774906346,12.));
#97600=CARTESIAN_POINT('Ctrl Pts',(-19.9712207924437,68.960461377483,0.));
#97601=CARTESIAN_POINT('Ctrl Pts',(-19.9712207924437,68.960461377483,12.));
#97602=CARTESIAN_POINT('Ctrl Pts',(-19.98503295806,68.9796667870667,0.));
#97603=CARTESIAN_POINT('Ctrl Pts',(-19.98503295806,68.9796667870667,12.));
#97604=CARTESIAN_POINT('Ctrl Pts',(-19.9988892041671,68.9988935820101,0.));
#97605=CARTESIAN_POINT('Ctrl Pts',(-19.9988892041671,68.9988935820101,12.));
#97606=CARTESIAN_POINT('Ctrl Pts',(-20.0127895095327,69.0181416255433,0.));
#97607=CARTESIAN_POINT('Ctrl Pts',(-20.0127895095327,69.0181416255433,12.));
#97608=CARTESIAN_POINT('Ctrl Pts',(-20.0267338529221,69.0374107814977,0.));
#97609=CARTESIAN_POINT('Ctrl Pts',(-20.0267338529221,69.0374107814977,12.));
#97610=CARTESIAN_POINT('Ctrl Pts',(-20.0407222130902,69.0567009142968,0.));
#97611=CARTESIAN_POINT('Ctrl Pts',(-20.0407222130902,69.0567009142968,12.));
#97612=CARTESIAN_POINT('Ctrl Pts',(-20.0547545687839,69.0760118889525,0.));
#97613=CARTESIAN_POINT('Ctrl Pts',(-20.0547545687839,69.0760118889525,12.));
#97614=CARTESIAN_POINT('Ctrl Pts',(-20.0688308987478,69.0953435710634,0.));
#97615=CARTESIAN_POINT('Ctrl Pts',(-20.0688308987478,69.0953435710634,12.));
#97616=CARTESIAN_POINT('Ctrl Pts',(-20.082951181725,69.1146958268104,0.));
#97617=CARTESIAN_POINT('Ctrl Pts',(-20.082951181725,69.1146958268104,12.));
#97618=CARTESIAN_POINT('Ctrl Pts',(-20.0971153964557,69.1340685229516,0.));
#97619=CARTESIAN_POINT('Ctrl Pts',(-20.0971153964557,69.1340685229516,12.));
#97620=CARTESIAN_POINT('Ctrl Pts',(-20.1113235216694,69.1534615268153,0.));
#97621=CARTESIAN_POINT('Ctrl Pts',(-20.1113235216694,69.1534615268153,12.));
#97622=CARTESIAN_POINT('Ctrl Pts',(-20.1255755360871,69.172874706296,0.));
#97623=CARTESIAN_POINT('Ctrl Pts',(-20.1255755360871,69.172874706296,12.));
#97624=CARTESIAN_POINT('Ctrl Pts',(-20.1398714184278,69.1923079298534,0.));
#97625=CARTESIAN_POINT('Ctrl Pts',(-20.1398714184278,69.1923079298534,12.));
#97626=CARTESIAN_POINT('Ctrl Pts',(-20.1542111474086,69.2117610665073,0.));
#97627=CARTESIAN_POINT('Ctrl Pts',(-20.1542111474086,69.2117610665073,12.));
#97628=CARTESIAN_POINT('Ctrl Pts',(-20.1685947017433,69.2312339858337,0.));
#97629=CARTESIAN_POINT('Ctrl Pts',(-20.1685947017433,69.2312339858337,12.));
#97630=CARTESIAN_POINT('Ctrl Pts',(-20.183022060135,69.2507265579562,0.));
#97631=CARTESIAN_POINT('Ctrl Pts',(-20.183022060135,69.2507265579562,12.));
#97632=CARTESIAN_POINT('Ctrl Pts',(-20.1974932012775,69.2702386535432,0.));
#97633=CARTESIAN_POINT('Ctrl Pts',(-20.1974932012775,69.2702386535432,12.));
#97634=CARTESIAN_POINT('Ctrl Pts',(-20.2120081038622,69.2897701438066,0.));
#97635=CARTESIAN_POINT('Ctrl Pts',(-20.2120081038622,69.2897701438066,12.));
#97636=CARTESIAN_POINT('Ctrl Pts',(-20.2265667465784,69.3093209004986,0.));
#97637=CARTESIAN_POINT('Ctrl Pts',(-20.2265667465784,69.3093209004986,12.));
#97638=CARTESIAN_POINT('Ctrl Pts',(-20.2411691081122,69.3288907959065,0.));
#97639=CARTESIAN_POINT('Ctrl Pts',(-20.2411691081122,69.3288907959065,12.));
#97640=CARTESIAN_POINT('Ctrl Pts',(-20.255815167139,69.3484797028454,0.));
#97641=CARTESIAN_POINT('Ctrl Pts',(-20.255815167139,69.3484797028454,12.));
#97642=CARTESIAN_POINT('Ctrl Pts',(-20.2705049023241,69.3680874946548,0.));
#97643=CARTESIAN_POINT('Ctrl Pts',(-20.2705049023241,69.3680874946548,12.));
#97644=CARTESIAN_POINT('Ctrl Pts',(-20.2852382923299,69.3877140451975,0.));
#97645=CARTESIAN_POINT('Ctrl Pts',(-20.2852382923299,69.3877140451975,12.));
#97646=CARTESIAN_POINT('Ctrl Pts',(-20.3000153158167,69.4073592288562,0.));
#97647=CARTESIAN_POINT('Ctrl Pts',(-20.3000153158167,69.4073592288562,12.));
#97648=CARTESIAN_POINT('Ctrl Pts',(-20.3148359514414,69.4270229205296,0.));
#97649=CARTESIAN_POINT('Ctrl Pts',(-20.3148359514414,69.4270229205296,12.));
#97650=CARTESIAN_POINT('Ctrl Pts',(-20.3297001778505,69.4467049956257,0.));
#97651=CARTESIAN_POINT('Ctrl Pts',(-20.3297001778505,69.4467049956257,12.));
#97652=CARTESIAN_POINT('Ctrl Pts',(-20.3446079736799,69.4664053300579,0.));
#97653=CARTESIAN_POINT('Ctrl Pts',(-20.3446079736799,69.4664053300579,12.));
#97654=CARTESIAN_POINT('Ctrl Pts',(-20.3595593175619,69.4861238002433,0.));
#97655=CARTESIAN_POINT('Ctrl Pts',(-20.3595593175619,69.4861238002433,12.));
#97656=CARTESIAN_POINT('Ctrl Pts',(-20.3745541881266,69.5058602831004,0.));
#97657=CARTESIAN_POINT('Ctrl Pts',(-20.3745541881266,69.5058602831004,12.));
#97658=CARTESIAN_POINT('Ctrl Pts',(-20.3895925640006,69.5256146560444,0.));
#97659=CARTESIAN_POINT('Ctrl Pts',(-20.3895925640006,69.5256146560444,12.));
#97660=CARTESIAN_POINT('Ctrl Pts',(-20.4046744238002,69.5453867969815,0.));
#97661=CARTESIAN_POINT('Ctrl Pts',(-20.4046744238002,69.5453867969815,12.));
#97662=CARTESIAN_POINT('Ctrl Pts',(-20.4197997461305,69.565176584305,0.));
#97663=CARTESIAN_POINT('Ctrl Pts',(-20.4197997461305,69.565176584305,12.));
#97664=CARTESIAN_POINT('Ctrl Pts',(-20.4349685095928,69.5849838968944,0.));
#97665=CARTESIAN_POINT('Ctrl Pts',(-20.4349685095928,69.5849838968944,12.));
#97666=CARTESIAN_POINT('Ctrl Pts',(-20.4501806927854,69.6048086141122,0.));
#97667=CARTESIAN_POINT('Ctrl Pts',(-20.4501806927854,69.6048086141122,12.));
#97668=CARTESIAN_POINT('Ctrl Pts',(-20.4654362743036,69.6246506158009,0.));
#97669=CARTESIAN_POINT('Ctrl Pts',(-20.4654362743036,69.6246506158009,12.));
#97670=CARTESIAN_POINT('Ctrl Pts',(-20.4807352327335,69.6445097822778,0.));
#97671=CARTESIAN_POINT('Ctrl Pts',(-20.4807352327335,69.6445097822778,12.));
#97672=CARTESIAN_POINT('Ctrl Pts',(-20.4960775466487,69.6643859943291,0.));
#97673=CARTESIAN_POINT('Ctrl Pts',(-20.4960775466487,69.6643859943291,12.));
#97674=CARTESIAN_POINT('Ctrl Pts',(-20.511463194618,69.6842791332102,0.));
#97675=CARTESIAN_POINT('Ctrl Pts',(-20.511463194618,69.6842791332102,12.));
#97676=CARTESIAN_POINT('Ctrl Pts',(-20.5268921552075,69.7041890806421,0.));
#97677=CARTESIAN_POINT('Ctrl Pts',(-20.5268921552075,69.7041890806421,12.));
#97678=CARTESIAN_POINT('Ctrl Pts',(-20.54236440698,69.7241157188086,0.));
#97679=CARTESIAN_POINT('Ctrl Pts',(-20.54236440698,69.7241157188086,12.));
#97680=CARTESIAN_POINT('Ctrl Pts',(-20.5578799284898,69.7440589303511,0.));
#97681=CARTESIAN_POINT('Ctrl Pts',(-20.5578799284898,69.7440589303511,12.));
#97682=CARTESIAN_POINT('Ctrl Pts',(-20.5734386982781,69.7640185983641,0.));
#97683=CARTESIAN_POINT('Ctrl Pts',(-20.5734386982781,69.7640185983641,12.));
#97684=CARTESIAN_POINT('Ctrl Pts',(-20.5890406948809,69.7839946063942,0.));
#97685=CARTESIAN_POINT('Ctrl Pts',(-20.5890406948809,69.7839946063942,12.));
#97686=CARTESIAN_POINT('Ctrl Pts',(-20.6046858968305,69.8039868384382,0.));
#97687=CARTESIAN_POINT('Ctrl Pts',(-20.6046858968305,69.8039868384382,12.));
#97688=CARTESIAN_POINT('Ctrl Pts',(-20.6203742826566,69.8239951789402,0.));
#97689=CARTESIAN_POINT('Ctrl Pts',(-20.6203742826566,69.8239951789402,12.));
#97690=CARTESIAN_POINT('Ctrl Pts',(-20.6361058308812,69.8440195127874,0.));
#97691=CARTESIAN_POINT('Ctrl Pts',(-20.6361058308812,69.8440195127874,12.));
#97692=CARTESIAN_POINT('Ctrl Pts',(-20.6518805200132,69.8640597253058,0.));
#97693=CARTESIAN_POINT('Ctrl Pts',(-20.6518805200132,69.8640597253058,12.));
#97694=CARTESIAN_POINT('Ctrl Pts',(-20.6676983285542,69.884115702258,0.));
#97695=CARTESIAN_POINT('Ctrl Pts',(-20.6676983285542,69.884115702258,12.));
#97696=CARTESIAN_POINT('Ctrl Pts',(-20.6835592350031,69.9041873298416,0.));
#97697=CARTESIAN_POINT('Ctrl Pts',(-20.6835592350031,69.9041873298416,12.));
#97698=CARTESIAN_POINT('Ctrl Pts',(-20.6994632178551,69.9242744946854,0.));
#97699=CARTESIAN_POINT('Ctrl Pts',(-20.6994632178551,69.9242744946854,12.));
#97700=CARTESIAN_POINT('Ctrl Pts',(-20.7154102555996,69.9443770838444,0.));
#97701=CARTESIAN_POINT('Ctrl Pts',(-20.7154102555996,69.9443770838444,12.));
#97702=CARTESIAN_POINT('Ctrl Pts',(-20.7314003267118,69.9644949847929,0.));
#97703=CARTESIAN_POINT('Ctrl Pts',(-20.7314003267118,69.9644949847929,12.));
#97704=CARTESIAN_POINT('Ctrl Pts',(-20.7474334096581,69.9846280854254,0.));
#97705=CARTESIAN_POINT('Ctrl Pts',(-20.7474334096581,69.9846280854254,12.));
#97706=CARTESIAN_POINT('Ctrl Pts',(-20.7635094829016,70.0047762740569,0.));
#97707=CARTESIAN_POINT('Ctrl Pts',(-20.7635094829016,70.0047762740569,12.));
#97708=CARTESIAN_POINT('Ctrl Pts',(-20.7796285249023,70.0249394394221,0.));
#97709=CARTESIAN_POINT('Ctrl Pts',(-20.7796285249023,70.0249394394221,12.));
#97710=CARTESIAN_POINT('Ctrl Pts',(-20.7957905141155,70.0451174706739,0.));
#97711=CARTESIAN_POINT('Ctrl Pts',(-20.7957905141155,70.0451174706739,12.));
#97712=CARTESIAN_POINT('Ctrl Pts',(-20.8119954289845,70.0653102573798,0.));
#97713=CARTESIAN_POINT('Ctrl Pts',(-20.8119954289845,70.0653102573798,12.));
#97714=CARTESIAN_POINT('Ctrl Pts',(-20.8282432479425,70.0855176895185,0.));
#97715=CARTESIAN_POINT('Ctrl Pts',(-20.8282432479425,70.0855176895185,12.));
#97716=CARTESIAN_POINT('Ctrl Pts',(-20.8445339494184,70.1057396574741,0.));
#97717=CARTESIAN_POINT('Ctrl Pts',(-20.8445339494184,70.1057396574741,12.));
#97718=CARTESIAN_POINT('Ctrl Pts',(-20.8608675118377,70.1259760520306,0.));
#97719=CARTESIAN_POINT('Ctrl Pts',(-20.8608675118377,70.1259760520306,12.));
#97720=CARTESIAN_POINT('Ctrl Pts',(-20.8772439136207,70.1462267643649,0.));
#97721=CARTESIAN_POINT('Ctrl Pts',(-20.8772439136207,70.1462267643649,12.));
#97722=CARTESIAN_POINT('Ctrl Pts',(-20.8936631331751,70.1664916860366,0.));
#97723=CARTESIAN_POINT('Ctrl Pts',(-20.8936631331751,70.1664916860366,12.));
#97724=CARTESIAN_POINT('Ctrl Pts',(-20.9101251488948,70.1867707089866,0.));
#97725=CARTESIAN_POINT('Ctrl Pts',(-20.9101251488948,70.1867707089866,12.));
#97726=CARTESIAN_POINT('Ctrl Pts',(-20.9266299391688,70.2070637255469,0.));
#97727=CARTESIAN_POINT('Ctrl Pts',(-20.9266299391688,70.2070637255469,12.));
#97728=CARTESIAN_POINT('Ctrl Pts',(-20.9431774823833,70.2273706284479,0.));
#97729=CARTESIAN_POINT('Ctrl Pts',(-20.9431774823833,70.2273706284479,12.));
#97730=CARTESIAN_POINT('Ctrl Pts',(-20.9597677569227,70.2476913108242,0.));
#97731=CARTESIAN_POINT('Ctrl Pts',(-20.9597677569227,70.2476913108242,12.));
#97732=CARTESIAN_POINT('Ctrl Pts',(-20.9764007411648,70.2680256662215,0.));
#97733=CARTESIAN_POINT('Ctrl Pts',(-20.9764007411648,70.2680256662215,12.));
#97734=CARTESIAN_POINT('Ctrl Pts',(-20.993076413477,70.288373588597,0.));
#97735=CARTESIAN_POINT('Ctrl Pts',(-20.993076413477,70.288373588597,12.));
#97736=CARTESIAN_POINT('Ctrl Pts',(-21.0097947522212,70.3087349722959,0.));
#97737=CARTESIAN_POINT('Ctrl Pts',(-21.0097947522212,70.3087349722959,12.));
#97738=CARTESIAN_POINT('Ctrl Pts',(-21.0265557357544,70.3291097120293,0.));
#97739=CARTESIAN_POINT('Ctrl Pts',(-21.0265557357544,70.3291097120293,12.));
#97740=CARTESIAN_POINT('Ctrl Pts',(-21.0433593424266,70.3494977028497,0.));
#97741=CARTESIAN_POINT('Ctrl Pts',(-21.0433593424266,70.3494977028497,12.));
#97742=CARTESIAN_POINT('Ctrl Pts',(-21.0602055505751,70.3698988401291,0.));
#97743=CARTESIAN_POINT('Ctrl Pts',(-21.0602055505751,70.3698988401291,12.));
#97744=CARTESIAN_POINT('Ctrl Pts',(-21.0770943385146,70.3903130195279,0.));
#97745=CARTESIAN_POINT('Ctrl Pts',(-21.0770943385146,70.3903130195279,12.));
#97746=CARTESIAN_POINT('Ctrl Pts',(-21.0940256845477,70.4107401370403,0.));
#97747=CARTESIAN_POINT('Ctrl Pts',(-21.0940256845477,70.4107401370403,12.));
#97748=CARTESIAN_POINT('Ctrl Pts',(-21.110999566975,70.4311800890411,0.));
#97749=CARTESIAN_POINT('Ctrl Pts',(-21.110999566975,70.4311800890411,12.));
#97750=CARTESIAN_POINT('Ctrl Pts',(-21.1280159641003,70.4516327723349,0.));
#97751=CARTESIAN_POINT('Ctrl Pts',(-21.1280159641003,70.4516327723349,12.));
#97752=CARTESIAN_POINT('Ctrl Pts',(-21.1450748542335,70.4720980841934,0.));
#97753=CARTESIAN_POINT('Ctrl Pts',(-21.1450748542335,70.4720980841934,12.));
#97754=CARTESIAN_POINT('Ctrl Pts',(-21.1621762156894,70.4925759224208,0.));
#97755=CARTESIAN_POINT('Ctrl Pts',(-21.1621762156894,70.4925759224208,12.));
#97756=CARTESIAN_POINT('Ctrl Pts',(-21.1793200267843,70.5130661852946,0.));
#97757=CARTESIAN_POINT('Ctrl Pts',(-21.1793200267843,70.5130661852946,12.));
#97758=CARTESIAN_POINT('Ctrl Pts',(-21.1965062658296,70.5335687714422,0.));
#97759=CARTESIAN_POINT('Ctrl Pts',(-21.1965062658296,70.5335687714422,12.));
#97760=CARTESIAN_POINT('Ctrl Pts',(-21.2137349111207,70.5540835797281,0.));
#97761=CARTESIAN_POINT('Ctrl Pts',(-21.2137349111207,70.5540835797281,12.));
#97762=CARTESIAN_POINT('Ctrl Pts',(-21.2310059409265,70.5746105091503,0.));
#97763=CARTESIAN_POINT('Ctrl Pts',(-21.2310059409265,70.5746105091503,12.));
#97764=CARTESIAN_POINT('Ctrl Pts',(-21.2483193334676,70.5951494586961,0.));
#97765=CARTESIAN_POINT('Ctrl Pts',(-21.2483193334676,70.5951494586961,12.));
#97766=CARTESIAN_POINT('Ctrl Pts',(-21.2656750669129,70.6157003273326,0.));
#97767=CARTESIAN_POINT('Ctrl Pts',(-21.2656750669129,70.6157003273326,12.));
#97768=CARTESIAN_POINT('Ctrl Pts',(-21.2830731194187,70.6362630143062,0.));
#97769=CARTESIAN_POINT('Ctrl Pts',(-21.2830731194187,70.6362630143062,12.));
#97770=CARTESIAN_POINT('Ctrl Pts',(-21.3005134691563,70.6568374193786,0.));
#97771=CARTESIAN_POINT('Ctrl Pts',(-21.3005134691563,70.6568374193786,12.));
#97772=CARTESIAN_POINT('Ctrl Pts',(-21.3179960943388,70.6774234430899,0.));
#97773=CARTESIAN_POINT('Ctrl Pts',(-21.3179960943388,70.6774234430899,12.));
#97774=CARTESIAN_POINT('Ctrl Pts',(-21.3355209732438,70.6980209870032,0.));
#97775=CARTESIAN_POINT('Ctrl Pts',(-21.3355209732438,70.6980209870032,12.));
#97776=CARTESIAN_POINT('Ctrl Pts',(-21.353088084234,70.7186299539698,0.));
#97777=CARTESIAN_POINT('Ctrl Pts',(-21.353088084234,70.7186299539698,12.));
#97778=CARTESIAN_POINT('Ctrl Pts',(-21.3706974057028,70.7392502475438,0.));
#97779=CARTESIAN_POINT('Ctrl Pts',(-21.3706974057028,70.7392502475438,12.));
#97780=CARTESIAN_POINT('Ctrl Pts',(-21.3883489160187,70.7598817714078,0.));
#97781=CARTESIAN_POINT('Ctrl Pts',(-21.3883489160187,70.7598817714078,12.));
#97782=CARTESIAN_POINT('Ctrl Pts',(-21.4060425934595,70.780524428744,0.));
#97783=CARTESIAN_POINT('Ctrl Pts',(-21.4060425934595,70.780524428744,12.));
#97784=CARTESIAN_POINT('Ctrl Pts',(-21.4237784161592,70.8011781217409,0.));
#97785=CARTESIAN_POINT('Ctrl Pts',(-21.4237784161592,70.8011781217409,12.));
#97786=CARTESIAN_POINT('Ctrl Pts',(-21.4415563620127,70.8218427507545,0.));
#97787=CARTESIAN_POINT('Ctrl Pts',(-21.4415563620127,70.8218427507545,12.));
#97788=CARTESIAN_POINT('Ctrl Pts',(-21.4593764087492,70.84251821499,0.));
#97789=CARTESIAN_POINT('Ctrl Pts',(-21.4593764087492,70.84251821499,12.));
#97790=CARTESIAN_POINT('Ctrl Pts',(-21.4772385340978,70.8632044140166,0.));
#97791=CARTESIAN_POINT('Ctrl Pts',(-21.4772385340978,70.8632044140166,12.));
#97792=CARTESIAN_POINT('Ctrl Pts',(-21.4951427159272,70.8839012490903,0.));
#97793=CARTESIAN_POINT('Ctrl Pts',(-21.4951427159272,70.8839012490903,12.));
#97794=CARTESIAN_POINT('Ctrl Pts',(-21.5130889323767,70.9046086244123,0.));
#97795=CARTESIAN_POINT('Ctrl Pts',(-21.5130889323767,70.9046086244123,12.));
#97796=CARTESIAN_POINT('Ctrl Pts',(-21.5310771620209,70.9253264487576,0.));
#97797=CARTESIAN_POINT('Ctrl Pts',(-21.5310771620209,70.9253264487576,12.));
#97798=CARTESIAN_POINT('Ctrl Pts',(-21.549107383907,70.9460546358597,0.));
#97799=CARTESIAN_POINT('Ctrl Pts',(-21.549107383907,70.9460546358597,12.));
#97800=CARTESIAN_POINT('Ctrl Pts',(-21.5671795771873,70.9667931008097,0.));
#97801=CARTESIAN_POINT('Ctrl Pts',(-21.5671795771873,70.9667931008097,12.));
#97802=CARTESIAN_POINT('Ctrl Pts',(-21.5852937208258,70.9875417572138,0.));
#97803=CARTESIAN_POINT('Ctrl Pts',(-21.5852937208258,70.9875417572138,12.));
#97804=CARTESIAN_POINT('Ctrl Pts',(-21.6034497932573,71.0083005139086,0.));
#97805=CARTESIAN_POINT('Ctrl Pts',(-21.6034497932573,71.0083005139086,12.));
#97806=CARTESIAN_POINT('Ctrl Pts',(-21.6216477720941,71.0290692721932,0.));
#97807=CARTESIAN_POINT('Ctrl Pts',(-21.6216477720941,71.0290692721932,12.));
#97808=CARTESIAN_POINT('Ctrl Pts',(-21.6398876337207,71.0498479219659,0.));
#97809=CARTESIAN_POINT('Ctrl Pts',(-21.6398876337207,71.0498479219659,12.));
#97810=CARTESIAN_POINT('Ctrl Pts',(-21.6581693538424,71.0706363472965,0.));
#97811=CARTESIAN_POINT('Ctrl Pts',(-21.6581693538424,71.0706363472965,12.));
#97812=CARTESIAN_POINT('Ctrl Pts',(-21.6764929081762,71.0914344333048,0.));
#97813=CARTESIAN_POINT('Ctrl Pts',(-21.6764929081762,71.0914344333048,12.));
#97814=CARTESIAN_POINT('Ctrl Pts',(-21.6948582730895,71.1122420728349,0.));
#97815=CARTESIAN_POINT('Ctrl Pts',(-21.6948582730895,71.1122420728349,12.));
#97816=CARTESIAN_POINT('Ctrl Pts',(-21.7132654262501,71.133059172642,0.));
#97817=CARTESIAN_POINT('Ctrl Pts',(-21.7132654262501,71.133059172642,12.));
#97818=CARTESIAN_POINT('Ctrl Pts',(-21.7317143472827,71.1538856611899,0.));
#97819=CARTESIAN_POINT('Ctrl Pts',(-21.7317143472827,71.1538856611899,12.));
#97820=CARTESIAN_POINT('Ctrl Pts',(-21.7502050183602,71.1747214905981,0.));
#97821=CARTESIAN_POINT('Ctrl Pts',(-21.7502050183602,71.1747214905981,12.));
#97822=CARTESIAN_POINT('Ctrl Pts',(-21.7687374247045,71.1955666309591,0.));
#97823=CARTESIAN_POINT('Ctrl Pts',(-21.7687374247045,71.1955666309591,12.));
#97824=CARTESIAN_POINT('Ctrl Pts',(-21.7835967290261,71.212250179455,0.));
#97825=CARTESIAN_POINT('Ctrl Pts',(-21.7835967290261,71.212250179455,12.));
#97826=CARTESIAN_POINT('Ctrl Pts',(-21.7947599798839,71.2247670209821,0.));
#97827=CARTESIAN_POINT('Ctrl Pts',(-21.7947599798839,71.2247670209821,12.));
#97828=CARTESIAN_POINT('Ctrl Pts',(-21.8022104901682,71.2331134397743,0.));
#97829=CARTESIAN_POINT('Ctrl Pts',(-21.8022104901682,71.2331134397743,12.));
#97830=CARTESIAN_POINT('Ctrl Pts',(-21.8059378310719,71.2372871136137,0.));
#97831=CARTESIAN_POINT('Ctrl Pts',(-21.8059378310719,71.2372871136137,12.));
#97832=CARTESIAN_POINT('',(-18.9407177820969,67.3887914263118,0.));
#97833=CARTESIAN_POINT('Ctrl Pts',(-18.9407177820969,67.3887914263118,0.));
#97834=CARTESIAN_POINT('Ctrl Pts',(-18.9426924398719,67.3921355608328,0.));
#97835=CARTESIAN_POINT('Ctrl Pts',(-18.9466463414299,67.3988274146651,0.));
#97836=CARTESIAN_POINT('Ctrl Pts',(-18.9525909517915,67.4088759497911,0.));
#97837=CARTESIAN_POINT('Ctrl Pts',(-18.9605446160985,67.4222955061981,0.));
#97838=CARTESIAN_POINT('Ctrl Pts',(-18.9705325631711,67.4391057908418,0.));
#97839=CARTESIAN_POINT('Ctrl Pts',(-18.9805663798448,67.4559518744638,0.));
#97840=CARTESIAN_POINT('Ctrl Pts',(-18.9906460638625,67.472833671964,0.));
#97841=CARTESIAN_POINT('Ctrl Pts',(-19.0007716032819,67.4897510316844,0.));
#97842=CARTESIAN_POINT('Ctrl Pts',(-19.0109429761306,67.5067037372317,0.));
#97843=CARTESIAN_POINT('Ctrl Pts',(-19.021160154824,67.5236915360331,0.));
#97844=CARTESIAN_POINT('Ctrl Pts',(-19.0314231093923,67.540714161288,0.));
#97845=CARTESIAN_POINT('Ctrl Pts',(-19.0417318110708,67.5577713558194,0.));
#97846=CARTESIAN_POINT('Ctrl Pts',(-19.0520862360396,67.5748628971964,0.));
#97847=CARTESIAN_POINT('Ctrl Pts',(-19.062486364241,67.5919885896222,0.));
#97848=CARTESIAN_POINT('Ctrl Pts',(-19.072932177628,67.6091482520534,0.));
#97849=CARTESIAN_POINT('Ctrl Pts',(-19.0834236587118,67.6263417083426,0.));
#97850=CARTESIAN_POINT('Ctrl Pts',(-19.0939607887501,67.6435687749841,0.));
#97851=CARTESIAN_POINT('Ctrl Pts',(-19.1045435468358,67.6608292549462,0.));
#97852=CARTESIAN_POINT('Ctrl Pts',(-19.115171910846,67.6781229440573,0.));
#97853=CARTESIAN_POINT('Ctrl Pts',(-19.1258458580345,67.6954496350063,0.));
#97854=CARTESIAN_POINT('Ctrl Pts',(-19.136565365709,67.7128091219348,0.));
#97855=CARTESIAN_POINT('Ctrl Pts',(-19.1473304119955,67.7302012056584,0.));
#97856=CARTESIAN_POINT('Ctrl Pts',(-19.1581409758097,67.7476256934444,0.));
#97857=CARTESIAN_POINT('Ctrl Pts',(-19.168997036495,67.7650823965127,0.));
#97858=CARTESIAN_POINT('Ctrl Pts',(-19.1798985735688,67.7825711283096,0.));
#97859=CARTESIAN_POINT('Ctrl Pts',(-19.1908455664098,67.8000917023926,0.));
#97860=CARTESIAN_POINT('Ctrl Pts',(-19.201837993993,67.8176439306621,0.));
#97861=CARTESIAN_POINT('Ctrl Pts',(-19.2128758350346,67.835227624289,0.));
#97862=CARTESIAN_POINT('Ctrl Pts',(-19.2239590681133,67.8528425945184,0.));
#97863=CARTESIAN_POINT('Ctrl Pts',(-19.2350876717874,67.8704886534544,0.));
#97864=CARTESIAN_POINT('Ctrl Pts',(-19.2462616247279,67.8881656149955,0.));
#97865=CARTESIAN_POINT('Ctrl Pts',(-19.2574809057696,67.9058732951788,0.));
#97866=CARTESIAN_POINT('Ctrl Pts',(-19.2687454938442,67.9236115116758,0.));
#97867=CARTESIAN_POINT('Ctrl Pts',(-19.280055367936,67.9413800834793,0.));
#97868=CARTESIAN_POINT('Ctrl Pts',(-19.2914105070286,67.9591788305394,0.));
#97869=CARTESIAN_POINT('Ctrl Pts',(-19.302810890038,67.9770075733485,0.));
#97870=CARTESIAN_POINT('Ctrl Pts',(-19.3142564958203,67.9948661329617,0.));
#97871=CARTESIAN_POINT('Ctrl Pts',(-19.3257473032034,68.0127543311776,0.));
#97872=CARTESIAN_POINT('Ctrl Pts',(-19.3372832910076,68.0306719906636,0.));
#97873=CARTESIAN_POINT('Ctrl Pts',(-19.3488644380641,68.0486189351011,0.));
#97874=CARTESIAN_POINT('Ctrl Pts',(-19.3604907232314,68.0665949893195,0.));
#97875=CARTESIAN_POINT('Ctrl Pts',(-19.3721621253912,68.0845999792247,0.));
#97876=CARTESIAN_POINT('Ctrl Pts',(-19.3838786234421,68.1026337317285,0.));
#97877=CARTESIAN_POINT('Ctrl Pts',(-19.3956401962895,68.1206960746769,0.));
#97878=CARTESIAN_POINT('Ctrl Pts',(-19.40744682283,68.1387868367691,0.));
#97879=CARTESIAN_POINT('Ctrl Pts',(-19.4192984819418,68.1569058475054,0.));
#97880=CARTESIAN_POINT('Ctrl Pts',(-19.4311951524983,68.1750529372232,0.));
#97881=CARTESIAN_POINT('Ctrl Pts',(-19.4431368133719,68.1932279371127,0.));
#97882=CARTESIAN_POINT('Ctrl Pts',(-19.455123443438,68.2114306792358,0.));
#97883=CARTESIAN_POINT('Ctrl Pts',(-19.467155021572,68.2296609965448,0.));
#97884=CARTESIAN_POINT('Ctrl Pts',(-19.4792315266501,68.2479187228803,0.));
#97885=CARTESIAN_POINT('Ctrl Pts',(-19.4913529375543,68.2662036929526,0.));
#97886=CARTESIAN_POINT('Ctrl Pts',(-19.5035192331705,68.2845157423233,0.));
#97887=CARTESIAN_POINT('Ctrl Pts',(-19.5157303923856,68.3028547073864,0.));
#97888=CARTESIAN_POINT('Ctrl Pts',(-19.5279863940773,68.3212204253417,0.));
#97889=CARTESIAN_POINT('Ctrl Pts',(-19.5402872171191,68.3396127341938,0.));
#97890=CARTESIAN_POINT('Ctrl Pts',(-19.5526328403852,68.3580314727523,0.));
#97891=CARTESIAN_POINT('Ctrl Pts',(-19.5650232427516,68.3764764806287,0.));
#97892=CARTESIAN_POINT('Ctrl Pts',(-19.5774584030938,68.3949475982335,0.));
#97893=CARTESIAN_POINT('Ctrl Pts',(-19.5899383002802,68.4134446667696,0.));
#97894=CARTESIAN_POINT('Ctrl Pts',(-19.6024629131785,68.4319675282275,0.));
#97895=CARTESIAN_POINT('Ctrl Pts',(-19.6150322206577,68.4505160253778,0.));
#97896=CARTESIAN_POINT('Ctrl Pts',(-19.6276462015888,68.4690900017632,0.));
#97897=CARTESIAN_POINT('Ctrl Pts',(-19.6403048348395,68.4876893016856,0.));
#97898=CARTESIAN_POINT('Ctrl Pts',(-19.6530080992686,68.5063137701971,0.));
#97899=CARTESIAN_POINT('Ctrl Pts',(-19.6657559737336,68.5249632530979,0.));
#97900=CARTESIAN_POINT('Ctrl Pts',(-19.6785484370927,68.5436375969311,0.));
#97901=CARTESIAN_POINT('Ctrl Pts',(-19.6913854682046,68.5623366489779,0.));
#97902=CARTESIAN_POINT('Ctrl Pts',(-19.7042670459237,68.581060257249,0.));
#97903=CARTESIAN_POINT('Ctrl Pts',(-19.7171931490956,68.5998082704766,0.));
#97904=CARTESIAN_POINT('Ctrl Pts',(-19.7301637565652,68.6185805381126,0.));
#97905=CARTESIAN_POINT('Ctrl Pts',(-19.7431788471776,68.6373769103224,0.));
#97906=CARTESIAN_POINT('Ctrl Pts',(-19.7562383997781,68.6561972379793,0.));
#97907=CARTESIAN_POINT('Ctrl Pts',(-19.7693423932058,68.6750413726547,0.));
#97908=CARTESIAN_POINT('Ctrl Pts',(-19.7824908062913,68.6939091666111,0.));
#97909=CARTESIAN_POINT('Ctrl Pts',(-19.795683617864,68.7128004727998,0.));
#97910=CARTESIAN_POINT('Ctrl Pts',(-19.8089208067532,68.7317151448557,0.));
#97911=CARTESIAN_POINT('Ctrl Pts',(-19.8222023517874,68.7506530370918,0.));
#97912=CARTESIAN_POINT('Ctrl Pts',(-19.835528231787,68.7696140044892,0.));
#97913=CARTESIAN_POINT('Ctrl Pts',(-19.8488984255641,68.7885979026927,0.));
#97914=CARTESIAN_POINT('Ctrl Pts',(-19.8623129119304,68.8076045880102,0.));
#97915=CARTESIAN_POINT('Ctrl Pts',(-19.8757716696969,68.8266339174068,0.));
#97916=CARTESIAN_POINT('Ctrl Pts',(-19.8892746776734,68.8456857484988,0.));
#97917=CARTESIAN_POINT('Ctrl Pts',(-19.9028219146607,68.8647599395437,0.));
#97918=CARTESIAN_POINT('Ctrl Pts',(-19.9164133594513,68.8838563494356,0.));
#97919=CARTESIAN_POINT('Ctrl Pts',(-19.9300489908364,68.902974837704,0.));
#97920=CARTESIAN_POINT('Ctrl Pts',(-19.9437287876063,68.9221152645086,0.));
#97921=CARTESIAN_POINT('Ctrl Pts',(-19.9574527285492,68.9412774906346,0.));
#97922=CARTESIAN_POINT('Ctrl Pts',(-19.9712207924437,68.960461377483,0.));
#97923=CARTESIAN_POINT('Ctrl Pts',(-19.98503295806,68.9796667870667,0.));
#97924=CARTESIAN_POINT('Ctrl Pts',(-19.9988892041671,68.9988935820101,0.));
#97925=CARTESIAN_POINT('Ctrl Pts',(-20.0127895095327,69.0181416255433,0.));
#97926=CARTESIAN_POINT('Ctrl Pts',(-20.0267338529221,69.0374107814977,0.));
#97927=CARTESIAN_POINT('Ctrl Pts',(-20.0407222130902,69.0567009142968,0.));
#97928=CARTESIAN_POINT('Ctrl Pts',(-20.0547545687839,69.0760118889525,0.));
#97929=CARTESIAN_POINT('Ctrl Pts',(-20.0688308987478,69.0953435710634,0.));
#97930=CARTESIAN_POINT('Ctrl Pts',(-20.082951181725,69.1146958268104,0.));
#97931=CARTESIAN_POINT('Ctrl Pts',(-20.0971153964557,69.1340685229516,0.));
#97932=CARTESIAN_POINT('Ctrl Pts',(-20.1113235216694,69.1534615268153,0.));
#97933=CARTESIAN_POINT('Ctrl Pts',(-20.1255755360871,69.172874706296,0.));
#97934=CARTESIAN_POINT('Ctrl Pts',(-20.1398714184278,69.1923079298534,0.));
#97935=CARTESIAN_POINT('Ctrl Pts',(-20.1542111474086,69.2117610665073,0.));
#97936=CARTESIAN_POINT('Ctrl Pts',(-20.1685947017433,69.2312339858337,0.));
#97937=CARTESIAN_POINT('Ctrl Pts',(-20.183022060135,69.2507265579562,0.));
#97938=CARTESIAN_POINT('Ctrl Pts',(-20.1974932012775,69.2702386535432,0.));
#97939=CARTESIAN_POINT('Ctrl Pts',(-20.2120081038622,69.2897701438066,0.));
#97940=CARTESIAN_POINT('Ctrl Pts',(-20.2265667465784,69.3093209004986,0.));
#97941=CARTESIAN_POINT('Ctrl Pts',(-20.2411691081122,69.3288907959065,0.));
#97942=CARTESIAN_POINT('Ctrl Pts',(-20.255815167139,69.3484797028454,0.));
#97943=CARTESIAN_POINT('Ctrl Pts',(-20.2705049023241,69.3680874946548,0.));
#97944=CARTESIAN_POINT('Ctrl Pts',(-20.2852382923299,69.3877140451975,0.));
#97945=CARTESIAN_POINT('Ctrl Pts',(-20.3000153158167,69.4073592288562,0.));
#97946=CARTESIAN_POINT('Ctrl Pts',(-20.3148359514414,69.4270229205296,0.));
#97947=CARTESIAN_POINT('Ctrl Pts',(-20.3297001778505,69.4467049956257,0.));
#97948=CARTESIAN_POINT('Ctrl Pts',(-20.3446079736799,69.4664053300579,0.));
#97949=CARTESIAN_POINT('Ctrl Pts',(-20.3595593175619,69.4861238002433,0.));
#97950=CARTESIAN_POINT('Ctrl Pts',(-20.3745541881266,69.5058602831004,0.));
#97951=CARTESIAN_POINT('Ctrl Pts',(-20.3895925640006,69.5256146560444,0.));
#97952=CARTESIAN_POINT('Ctrl Pts',(-20.4046744238002,69.5453867969815,0.));
#97953=CARTESIAN_POINT('Ctrl Pts',(-20.4197997461305,69.565176584305,0.));
#97954=CARTESIAN_POINT('Ctrl Pts',(-20.4349685095928,69.5849838968944,0.));
#97955=CARTESIAN_POINT('Ctrl Pts',(-20.4501806927854,69.6048086141122,0.));
#97956=CARTESIAN_POINT('Ctrl Pts',(-20.4654362743036,69.6246506158009,0.));
#97957=CARTESIAN_POINT('Ctrl Pts',(-20.4807352327335,69.6445097822778,0.));
#97958=CARTESIAN_POINT('Ctrl Pts',(-20.4960775466487,69.6643859943291,0.));
#97959=CARTESIAN_POINT('Ctrl Pts',(-20.511463194618,69.6842791332102,0.));
#97960=CARTESIAN_POINT('Ctrl Pts',(-20.5268921552075,69.7041890806421,0.));
#97961=CARTESIAN_POINT('Ctrl Pts',(-20.54236440698,69.7241157188086,0.));
#97962=CARTESIAN_POINT('Ctrl Pts',(-20.5578799284898,69.7440589303511,0.));
#97963=CARTESIAN_POINT('Ctrl Pts',(-20.5734386982781,69.7640185983641,0.));
#97964=CARTESIAN_POINT('Ctrl Pts',(-20.5890406948809,69.7839946063942,0.));
#97965=CARTESIAN_POINT('Ctrl Pts',(-20.6046858968305,69.8039868384382,0.));
#97966=CARTESIAN_POINT('Ctrl Pts',(-20.6203742826566,69.8239951789402,0.));
#97967=CARTESIAN_POINT('Ctrl Pts',(-20.6361058308812,69.8440195127874,0.));
#97968=CARTESIAN_POINT('Ctrl Pts',(-20.6518805200132,69.8640597253058,0.));
#97969=CARTESIAN_POINT('Ctrl Pts',(-20.6676983285542,69.884115702258,0.));
#97970=CARTESIAN_POINT('Ctrl Pts',(-20.6835592350031,69.9041873298416,0.));
#97971=CARTESIAN_POINT('Ctrl Pts',(-20.6994632178551,69.9242744946854,0.));
#97972=CARTESIAN_POINT('Ctrl Pts',(-20.7154102555996,69.9443770838444,0.));
#97973=CARTESIAN_POINT('Ctrl Pts',(-20.7314003267118,69.9644949847929,0.));
#97974=CARTESIAN_POINT('Ctrl Pts',(-20.7474334096581,69.9846280854254,0.));
#97975=CARTESIAN_POINT('Ctrl Pts',(-20.7635094829016,70.0047762740569,0.));
#97976=CARTESIAN_POINT('Ctrl Pts',(-20.7796285249023,70.0249394394221,0.));
#97977=CARTESIAN_POINT('Ctrl Pts',(-20.7957905141155,70.0451174706739,0.));
#97978=CARTESIAN_POINT('Ctrl Pts',(-20.8119954289845,70.0653102573798,0.));
#97979=CARTESIAN_POINT('Ctrl Pts',(-20.8282432479425,70.0855176895185,0.));
#97980=CARTESIAN_POINT('Ctrl Pts',(-20.8445339494184,70.1057396574741,0.));
#97981=CARTESIAN_POINT('Ctrl Pts',(-20.8608675118377,70.1259760520306,0.));
#97982=CARTESIAN_POINT('Ctrl Pts',(-20.8772439136207,70.1462267643649,0.));
#97983=CARTESIAN_POINT('Ctrl Pts',(-20.8936631331751,70.1664916860366,0.));
#97984=CARTESIAN_POINT('Ctrl Pts',(-20.9101251488948,70.1867707089866,0.));
#97985=CARTESIAN_POINT('Ctrl Pts',(-20.9266299391688,70.2070637255469,0.));
#97986=CARTESIAN_POINT('Ctrl Pts',(-20.9431774823833,70.2273706284479,0.));
#97987=CARTESIAN_POINT('Ctrl Pts',(-20.9597677569227,70.2476913108242,0.));
#97988=CARTESIAN_POINT('Ctrl Pts',(-20.9764007411648,70.2680256662215,0.));
#97989=CARTESIAN_POINT('Ctrl Pts',(-20.993076413477,70.288373588597,0.));
#97990=CARTESIAN_POINT('Ctrl Pts',(-21.0097947522212,70.3087349722959,0.));
#97991=CARTESIAN_POINT('Ctrl Pts',(-21.0265557357544,70.3291097120293,0.));
#97992=CARTESIAN_POINT('Ctrl Pts',(-21.0433593424266,70.3494977028497,0.));
#97993=CARTESIAN_POINT('Ctrl Pts',(-21.0602055505751,70.3698988401291,0.));
#97994=CARTESIAN_POINT('Ctrl Pts',(-21.0770943385146,70.3903130195279,0.));
#97995=CARTESIAN_POINT('Ctrl Pts',(-21.0940256845477,70.4107401370403,0.));
#97996=CARTESIAN_POINT('Ctrl Pts',(-21.110999566975,70.4311800890411,0.));
#97997=CARTESIAN_POINT('Ctrl Pts',(-21.1280159641003,70.4516327723349,0.));
#97998=CARTESIAN_POINT('Ctrl Pts',(-21.1450748542335,70.4720980841934,0.));
#97999=CARTESIAN_POINT('Ctrl Pts',(-21.1621762156894,70.4925759224208,0.));
#98000=CARTESIAN_POINT('Ctrl Pts',(-21.1793200267843,70.5130661852946,0.));
#98001=CARTESIAN_POINT('Ctrl Pts',(-21.1965062658296,70.5335687714422,0.));
#98002=CARTESIAN_POINT('Ctrl Pts',(-21.2137349111207,70.5540835797281,0.));
#98003=CARTESIAN_POINT('Ctrl Pts',(-21.2310059409265,70.5746105091503,0.));
#98004=CARTESIAN_POINT('Ctrl Pts',(-21.2483193334676,70.5951494586961,0.));
#98005=CARTESIAN_POINT('Ctrl Pts',(-21.2656750669129,70.6157003273326,0.));
#98006=CARTESIAN_POINT('Ctrl Pts',(-21.2830731194187,70.6362630143062,0.));
#98007=CARTESIAN_POINT('Ctrl Pts',(-21.3005134691563,70.6568374193786,0.));
#98008=CARTESIAN_POINT('Ctrl Pts',(-21.3179960943388,70.6774234430899,0.));
#98009=CARTESIAN_POINT('Ctrl Pts',(-21.3355209732438,70.6980209870032,0.));
#98010=CARTESIAN_POINT('Ctrl Pts',(-21.353088084234,70.7186299539698,0.));
#98011=CARTESIAN_POINT('Ctrl Pts',(-21.3706974057028,70.7392502475438,0.));
#98012=CARTESIAN_POINT('Ctrl Pts',(-21.3883489160187,70.7598817714078,0.));
#98013=CARTESIAN_POINT('Ctrl Pts',(-21.4060425934595,70.780524428744,0.));
#98014=CARTESIAN_POINT('Ctrl Pts',(-21.4237784161592,70.8011781217409,0.));
#98015=CARTESIAN_POINT('Ctrl Pts',(-21.4415563620127,70.8218427507545,0.));
#98016=CARTESIAN_POINT('Ctrl Pts',(-21.4593764087492,70.84251821499,0.));
#98017=CARTESIAN_POINT('Ctrl Pts',(-21.4772385340978,70.8632044140166,0.));
#98018=CARTESIAN_POINT('Ctrl Pts',(-21.4951427159272,70.8839012490903,0.));
#98019=CARTESIAN_POINT('Ctrl Pts',(-21.5130889323767,70.9046086244123,0.));
#98020=CARTESIAN_POINT('Ctrl Pts',(-21.5310771620209,70.9253264487576,0.));
#98021=CARTESIAN_POINT('Ctrl Pts',(-21.549107383907,70.9460546358597,0.));
#98022=CARTESIAN_POINT('Ctrl Pts',(-21.5645987555282,70.9638315189646,0.));
#98023=CARTESIAN_POINT('Ctrl Pts',(-21.576498336635,70.9774662112375,0.));
#98024=CARTESIAN_POINT('Ctrl Pts',(-21.5847875433159,70.9869541807807,0.));
#98025=CARTESIAN_POINT('Ctrl Pts',(-21.5894540925368,70.9922924595081,0.));
#98026=CARTESIAN_POINT('Ctrl Pts',(-21.59049199348,70.9934796068777,0.));
#98027=CARTESIAN_POINT('',(-18.9407177820969,67.3887914263118,12.));
#98028=CARTESIAN_POINT('',(-18.9407177820969,67.3887914263118,0.));
#98029=CARTESIAN_POINT('Ctrl Pts',(-21.59049199348,70.9934796068777,12.));
#98030=CARTESIAN_POINT('Ctrl Pts',(-21.5894540925368,70.9922924595081,12.));
#98031=CARTESIAN_POINT('Ctrl Pts',(-21.5847875433159,70.9869541807807,12.));
#98032=CARTESIAN_POINT('Ctrl Pts',(-21.576498336635,70.9774662112375,12.));
#98033=CARTESIAN_POINT('Ctrl Pts',(-21.5645987555282,70.9638315189647,12.));
#98034=CARTESIAN_POINT('Ctrl Pts',(-21.549107383907,70.9460546358597,12.));
#98035=CARTESIAN_POINT('Ctrl Pts',(-21.5310771620209,70.9253264487576,12.));
#98036=CARTESIAN_POINT('Ctrl Pts',(-21.5130889323767,70.9046086244123,12.));
#98037=CARTESIAN_POINT('Ctrl Pts',(-21.4951427159272,70.8839012490903,12.));
#98038=CARTESIAN_POINT('Ctrl Pts',(-21.4772385340978,70.8632044140166,12.));
#98039=CARTESIAN_POINT('Ctrl Pts',(-21.4593764087492,70.84251821499,12.));
#98040=CARTESIAN_POINT('Ctrl Pts',(-21.4415563620127,70.8218427507545,12.));
#98041=CARTESIAN_POINT('Ctrl Pts',(-21.4237784161592,70.8011781217409,12.));
#98042=CARTESIAN_POINT('Ctrl Pts',(-21.4060425934595,70.780524428744,12.));
#98043=CARTESIAN_POINT('Ctrl Pts',(-21.3883489160187,70.7598817714078,12.));
#98044=CARTESIAN_POINT('Ctrl Pts',(-21.3706974057028,70.7392502475438,12.));
#98045=CARTESIAN_POINT('Ctrl Pts',(-21.353088084234,70.7186299539698,12.));
#98046=CARTESIAN_POINT('Ctrl Pts',(-21.3355209732438,70.6980209870032,12.));
#98047=CARTESIAN_POINT('Ctrl Pts',(-21.3179960943388,70.6774234430899,12.));
#98048=CARTESIAN_POINT('Ctrl Pts',(-21.3005134691563,70.6568374193786,12.));
#98049=CARTESIAN_POINT('Ctrl Pts',(-21.2830731194187,70.6362630143062,12.));
#98050=CARTESIAN_POINT('Ctrl Pts',(-21.2656750669129,70.6157003273326,12.));
#98051=CARTESIAN_POINT('Ctrl Pts',(-21.2483193334676,70.5951494586961,12.));
#98052=CARTESIAN_POINT('Ctrl Pts',(-21.2310059409265,70.5746105091503,12.));
#98053=CARTESIAN_POINT('Ctrl Pts',(-21.2137349111207,70.5540835797281,12.));
#98054=CARTESIAN_POINT('Ctrl Pts',(-21.1965062658296,70.5335687714422,12.));
#98055=CARTESIAN_POINT('Ctrl Pts',(-21.1793200267843,70.5130661852946,12.));
#98056=CARTESIAN_POINT('Ctrl Pts',(-21.1621762156894,70.4925759224208,12.));
#98057=CARTESIAN_POINT('Ctrl Pts',(-21.1450748542335,70.4720980841934,12.));
#98058=CARTESIAN_POINT('Ctrl Pts',(-21.1280159641003,70.4516327723349,12.));
#98059=CARTESIAN_POINT('Ctrl Pts',(-21.110999566975,70.4311800890411,12.));
#98060=CARTESIAN_POINT('Ctrl Pts',(-21.0940256845477,70.4107401370403,12.));
#98061=CARTESIAN_POINT('Ctrl Pts',(-21.0770943385146,70.3903130195279,12.));
#98062=CARTESIAN_POINT('Ctrl Pts',(-21.0602055505751,70.3698988401291,12.));
#98063=CARTESIAN_POINT('Ctrl Pts',(-21.0433593424266,70.3494977028497,12.));
#98064=CARTESIAN_POINT('Ctrl Pts',(-21.0265557357544,70.3291097120293,12.));
#98065=CARTESIAN_POINT('Ctrl Pts',(-21.0097947522212,70.3087349722959,12.));
#98066=CARTESIAN_POINT('Ctrl Pts',(-20.993076413477,70.288373588597,12.));
#98067=CARTESIAN_POINT('Ctrl Pts',(-20.9764007411648,70.2680256662215,12.));
#98068=CARTESIAN_POINT('Ctrl Pts',(-20.9597677569227,70.2476913108242,12.));
#98069=CARTESIAN_POINT('Ctrl Pts',(-20.9431774823833,70.2273706284479,12.));
#98070=CARTESIAN_POINT('Ctrl Pts',(-20.9266299391688,70.2070637255469,12.));
#98071=CARTESIAN_POINT('Ctrl Pts',(-20.9101251488948,70.1867707089866,12.));
#98072=CARTESIAN_POINT('Ctrl Pts',(-20.8936631331751,70.1664916860366,12.));
#98073=CARTESIAN_POINT('Ctrl Pts',(-20.8772439136207,70.1462267643649,12.));
#98074=CARTESIAN_POINT('Ctrl Pts',(-20.8608675118377,70.1259760520306,12.));
#98075=CARTESIAN_POINT('Ctrl Pts',(-20.8445339494184,70.1057396574741,12.));
#98076=CARTESIAN_POINT('Ctrl Pts',(-20.8282432479425,70.0855176895185,12.));
#98077=CARTESIAN_POINT('Ctrl Pts',(-20.8119954289845,70.0653102573798,12.));
#98078=CARTESIAN_POINT('Ctrl Pts',(-20.7957905141155,70.0451174706739,12.));
#98079=CARTESIAN_POINT('Ctrl Pts',(-20.7796285249023,70.0249394394221,12.));
#98080=CARTESIAN_POINT('Ctrl Pts',(-20.7635094829016,70.0047762740569,12.));
#98081=CARTESIAN_POINT('Ctrl Pts',(-20.7474334096581,69.9846280854254,12.));
#98082=CARTESIAN_POINT('Ctrl Pts',(-20.7314003267118,69.9644949847929,12.));
#98083=CARTESIAN_POINT('Ctrl Pts',(-20.7154102555996,69.9443770838444,12.));
#98084=CARTESIAN_POINT('Ctrl Pts',(-20.6994632178551,69.9242744946854,12.));
#98085=CARTESIAN_POINT('Ctrl Pts',(-20.6835592350031,69.9041873298416,12.));
#98086=CARTESIAN_POINT('Ctrl Pts',(-20.6676983285542,69.884115702258,12.));
#98087=CARTESIAN_POINT('Ctrl Pts',(-20.6518805200132,69.8640597253058,12.));
#98088=CARTESIAN_POINT('Ctrl Pts',(-20.6361058308812,69.8440195127874,12.));
#98089=CARTESIAN_POINT('Ctrl Pts',(-20.6203742826566,69.8239951789402,12.));
#98090=CARTESIAN_POINT('Ctrl Pts',(-20.6046858968305,69.8039868384382,12.));
#98091=CARTESIAN_POINT('Ctrl Pts',(-20.5890406948809,69.7839946063942,12.));
#98092=CARTESIAN_POINT('Ctrl Pts',(-20.5734386982781,69.7640185983641,12.));
#98093=CARTESIAN_POINT('Ctrl Pts',(-20.5578799284898,69.7440589303511,12.));
#98094=CARTESIAN_POINT('Ctrl Pts',(-20.54236440698,69.7241157188086,12.));
#98095=CARTESIAN_POINT('Ctrl Pts',(-20.5268921552075,69.7041890806421,12.));
#98096=CARTESIAN_POINT('Ctrl Pts',(-20.511463194618,69.6842791332102,12.));
#98097=CARTESIAN_POINT('Ctrl Pts',(-20.4960775466487,69.6643859943291,12.));
#98098=CARTESIAN_POINT('Ctrl Pts',(-20.4807352327335,69.6445097822778,12.));
#98099=CARTESIAN_POINT('Ctrl Pts',(-20.4654362743036,69.6246506158009,12.));
#98100=CARTESIAN_POINT('Ctrl Pts',(-20.4501806927854,69.6048086141122,12.));
#98101=CARTESIAN_POINT('Ctrl Pts',(-20.4349685095928,69.5849838968944,12.));
#98102=CARTESIAN_POINT('Ctrl Pts',(-20.4197997461305,69.565176584305,12.));
#98103=CARTESIAN_POINT('Ctrl Pts',(-20.4046744238002,69.5453867969815,12.));
#98104=CARTESIAN_POINT('Ctrl Pts',(-20.3895925640006,69.5256146560444,12.));
#98105=CARTESIAN_POINT('Ctrl Pts',(-20.3745541881266,69.5058602831004,12.));
#98106=CARTESIAN_POINT('Ctrl Pts',(-20.3595593175619,69.4861238002433,12.));
#98107=CARTESIAN_POINT('Ctrl Pts',(-20.3446079736799,69.4664053300579,12.));
#98108=CARTESIAN_POINT('Ctrl Pts',(-20.3297001778505,69.4467049956257,12.));
#98109=CARTESIAN_POINT('Ctrl Pts',(-20.3148359514414,69.4270229205296,12.));
#98110=CARTESIAN_POINT('Ctrl Pts',(-20.3000153158167,69.4073592288562,12.));
#98111=CARTESIAN_POINT('Ctrl Pts',(-20.2852382923299,69.3877140451975,12.));
#98112=CARTESIAN_POINT('Ctrl Pts',(-20.2705049023241,69.3680874946548,12.));
#98113=CARTESIAN_POINT('Ctrl Pts',(-20.255815167139,69.3484797028454,12.));
#98114=CARTESIAN_POINT('Ctrl Pts',(-20.2411691081122,69.3288907959065,12.));
#98115=CARTESIAN_POINT('Ctrl Pts',(-20.2265667465784,69.3093209004986,12.));
#98116=CARTESIAN_POINT('Ctrl Pts',(-20.2120081038622,69.2897701438066,12.));
#98117=CARTESIAN_POINT('Ctrl Pts',(-20.1974932012775,69.2702386535432,12.));
#98118=CARTESIAN_POINT('Ctrl Pts',(-20.183022060135,69.2507265579562,12.));
#98119=CARTESIAN_POINT('Ctrl Pts',(-20.1685947017433,69.2312339858337,12.));
#98120=CARTESIAN_POINT('Ctrl Pts',(-20.1542111474086,69.2117610665073,12.));
#98121=CARTESIAN_POINT('Ctrl Pts',(-20.1398714184278,69.1923079298534,12.));
#98122=CARTESIAN_POINT('Ctrl Pts',(-20.1255755360871,69.172874706296,12.));
#98123=CARTESIAN_POINT('Ctrl Pts',(-20.1113235216694,69.1534615268153,12.));
#98124=CARTESIAN_POINT('Ctrl Pts',(-20.0971153964557,69.1340685229516,12.));
#98125=CARTESIAN_POINT('Ctrl Pts',(-20.082951181725,69.1146958268104,12.));
#98126=CARTESIAN_POINT('Ctrl Pts',(-20.0688308987478,69.0953435710634,12.));
#98127=CARTESIAN_POINT('Ctrl Pts',(-20.0547545687839,69.0760118889525,12.));
#98128=CARTESIAN_POINT('Ctrl Pts',(-20.0407222130902,69.0567009142968,12.));
#98129=CARTESIAN_POINT('Ctrl Pts',(-20.0267338529221,69.0374107814977,12.));
#98130=CARTESIAN_POINT('Ctrl Pts',(-20.0127895095327,69.0181416255433,12.));
#98131=CARTESIAN_POINT('Ctrl Pts',(-19.9988892041671,68.9988935820101,12.));
#98132=CARTESIAN_POINT('Ctrl Pts',(-19.98503295806,68.9796667870667,12.));
#98133=CARTESIAN_POINT('Ctrl Pts',(-19.9712207924437,68.960461377483,12.));
#98134=CARTESIAN_POINT('Ctrl Pts',(-19.9574527285492,68.9412774906346,12.));
#98135=CARTESIAN_POINT('Ctrl Pts',(-19.9437287876063,68.9221152645086,12.));
#98136=CARTESIAN_POINT('Ctrl Pts',(-19.9300489908364,68.902974837704,12.));
#98137=CARTESIAN_POINT('Ctrl Pts',(-19.9164133594513,68.8838563494356,12.));
#98138=CARTESIAN_POINT('Ctrl Pts',(-19.9028219146607,68.8647599395437,12.));
#98139=CARTESIAN_POINT('Ctrl Pts',(-19.8892746776734,68.8456857484988,12.));
#98140=CARTESIAN_POINT('Ctrl Pts',(-19.8757716696969,68.8266339174068,12.));
#98141=CARTESIAN_POINT('Ctrl Pts',(-19.8623129119304,68.8076045880102,12.));
#98142=CARTESIAN_POINT('Ctrl Pts',(-19.8488984255641,68.7885979026927,12.));
#98143=CARTESIAN_POINT('Ctrl Pts',(-19.835528231787,68.7696140044892,12.));
#98144=CARTESIAN_POINT('Ctrl Pts',(-19.8222023517874,68.7506530370918,12.));
#98145=CARTESIAN_POINT('Ctrl Pts',(-19.8089208067532,68.7317151448557,12.));
#98146=CARTESIAN_POINT('Ctrl Pts',(-19.795683617864,68.7128004727998,12.));
#98147=CARTESIAN_POINT('Ctrl Pts',(-19.7824908062913,68.6939091666111,12.));
#98148=CARTESIAN_POINT('Ctrl Pts',(-19.7693423932058,68.6750413726547,12.));
#98149=CARTESIAN_POINT('Ctrl Pts',(-19.7562383997781,68.6561972379793,12.));
#98150=CARTESIAN_POINT('Ctrl Pts',(-19.7431788471776,68.6373769103224,12.));
#98151=CARTESIAN_POINT('Ctrl Pts',(-19.7301637565652,68.6185805381126,12.));
#98152=CARTESIAN_POINT('Ctrl Pts',(-19.7171931490956,68.5998082704766,12.));
#98153=CARTESIAN_POINT('Ctrl Pts',(-19.7042670459237,68.581060257249,12.));
#98154=CARTESIAN_POINT('Ctrl Pts',(-19.6913854682046,68.5623366489779,12.));
#98155=CARTESIAN_POINT('Ctrl Pts',(-19.6785484370927,68.5436375969311,12.));
#98156=CARTESIAN_POINT('Ctrl Pts',(-19.6657559737336,68.5249632530979,12.));
#98157=CARTESIAN_POINT('Ctrl Pts',(-19.6530080992686,68.5063137701971,12.));
#98158=CARTESIAN_POINT('Ctrl Pts',(-19.6403048348395,68.4876893016856,12.));
#98159=CARTESIAN_POINT('Ctrl Pts',(-19.6276462015888,68.4690900017632,12.));
#98160=CARTESIAN_POINT('Ctrl Pts',(-19.6150322206577,68.4505160253778,12.));
#98161=CARTESIAN_POINT('Ctrl Pts',(-19.6024629131785,68.4319675282275,12.));
#98162=CARTESIAN_POINT('Ctrl Pts',(-19.5899383002802,68.4134446667696,12.));
#98163=CARTESIAN_POINT('Ctrl Pts',(-19.5774584030938,68.3949475982335,12.));
#98164=CARTESIAN_POINT('Ctrl Pts',(-19.5650232427516,68.3764764806287,12.));
#98165=CARTESIAN_POINT('Ctrl Pts',(-19.5526328403852,68.3580314727523,12.));
#98166=CARTESIAN_POINT('Ctrl Pts',(-19.5402872171191,68.3396127341938,12.));
#98167=CARTESIAN_POINT('Ctrl Pts',(-19.5279863940773,68.3212204253417,12.));
#98168=CARTESIAN_POINT('Ctrl Pts',(-19.5157303923856,68.3028547073864,12.));
#98169=CARTESIAN_POINT('Ctrl Pts',(-19.5035192331705,68.2845157423233,12.));
#98170=CARTESIAN_POINT('Ctrl Pts',(-19.4913529375543,68.2662036929526,12.));
#98171=CARTESIAN_POINT('Ctrl Pts',(-19.4792315266501,68.2479187228803,12.));
#98172=CARTESIAN_POINT('Ctrl Pts',(-19.467155021572,68.2296609965448,12.));
#98173=CARTESIAN_POINT('Ctrl Pts',(-19.455123443438,68.2114306792358,12.));
#98174=CARTESIAN_POINT('Ctrl Pts',(-19.4431368133719,68.1932279371127,12.));
#98175=CARTESIAN_POINT('Ctrl Pts',(-19.4311951524983,68.1750529372232,12.));
#98176=CARTESIAN_POINT('Ctrl Pts',(-19.4192984819418,68.1569058475054,12.));
#98177=CARTESIAN_POINT('Ctrl Pts',(-19.40744682283,68.1387868367691,12.));
#98178=CARTESIAN_POINT('Ctrl Pts',(-19.3956401962895,68.1206960746769,12.));
#98179=CARTESIAN_POINT('Ctrl Pts',(-19.3838786234421,68.1026337317285,12.));
#98180=CARTESIAN_POINT('Ctrl Pts',(-19.3721621253912,68.0845999792247,12.));
#98181=CARTESIAN_POINT('Ctrl Pts',(-19.3604907232314,68.0665949893195,12.));
#98182=CARTESIAN_POINT('Ctrl Pts',(-19.3488644380641,68.0486189351011,12.));
#98183=CARTESIAN_POINT('Ctrl Pts',(-19.3372832910076,68.0306719906636,12.));
#98184=CARTESIAN_POINT('Ctrl Pts',(-19.3257473032034,68.0127543311776,12.));
#98185=CARTESIAN_POINT('Ctrl Pts',(-19.3142564958203,67.9948661329617,12.));
#98186=CARTESIAN_POINT('Ctrl Pts',(-19.302810890038,67.9770075733485,12.));
#98187=CARTESIAN_POINT('Ctrl Pts',(-19.2914105070286,67.9591788305394,12.));
#98188=CARTESIAN_POINT('Ctrl Pts',(-19.280055367936,67.9413800834793,12.));
#98189=CARTESIAN_POINT('Ctrl Pts',(-19.2687454938442,67.9236115116758,12.));
#98190=CARTESIAN_POINT('Ctrl Pts',(-19.2574809057696,67.9058732951788,12.));
#98191=CARTESIAN_POINT('Ctrl Pts',(-19.2462616247279,67.8881656149955,12.));
#98192=CARTESIAN_POINT('Ctrl Pts',(-19.2350876717874,67.8704886534544,12.));
#98193=CARTESIAN_POINT('Ctrl Pts',(-19.2239590681133,67.8528425945184,12.));
#98194=CARTESIAN_POINT('Ctrl Pts',(-19.2128758350346,67.835227624289,12.));
#98195=CARTESIAN_POINT('Ctrl Pts',(-19.201837993993,67.8176439306621,12.));
#98196=CARTESIAN_POINT('Ctrl Pts',(-19.1908455664098,67.8000917023926,12.));
#98197=CARTESIAN_POINT('Ctrl Pts',(-19.1798985735688,67.7825711283096,12.));
#98198=CARTESIAN_POINT('Ctrl Pts',(-19.168997036495,67.7650823965127,12.));
#98199=CARTESIAN_POINT('Ctrl Pts',(-19.1581409758097,67.7476256934444,12.));
#98200=CARTESIAN_POINT('Ctrl Pts',(-19.1473304119955,67.7302012056584,12.));
#98201=CARTESIAN_POINT('Ctrl Pts',(-19.136565365709,67.7128091219348,12.));
#98202=CARTESIAN_POINT('Ctrl Pts',(-19.1258458580345,67.6954496350063,12.));
#98203=CARTESIAN_POINT('Ctrl Pts',(-19.115171910846,67.6781229440573,12.));
#98204=CARTESIAN_POINT('Ctrl Pts',(-19.1045435468358,67.6608292549462,12.));
#98205=CARTESIAN_POINT('Ctrl Pts',(-19.0939607887501,67.6435687749841,12.));
#98206=CARTESIAN_POINT('Ctrl Pts',(-19.0834236587118,67.6263417083426,12.));
#98207=CARTESIAN_POINT('Ctrl Pts',(-19.072932177628,67.6091482520534,12.));
#98208=CARTESIAN_POINT('Ctrl Pts',(-19.062486364241,67.5919885896222,12.));
#98209=CARTESIAN_POINT('Ctrl Pts',(-19.0520862360396,67.5748628971964,12.));
#98210=CARTESIAN_POINT('Ctrl Pts',(-19.0417318110708,67.5577713558194,12.));
#98211=CARTESIAN_POINT('Ctrl Pts',(-19.0314231093923,67.540714161288,12.));
#98212=CARTESIAN_POINT('Ctrl Pts',(-19.021160154824,67.5236915360331,12.));
#98213=CARTESIAN_POINT('Ctrl Pts',(-19.0109429761306,67.5067037372317,12.));
#98214=CARTESIAN_POINT('Ctrl Pts',(-19.0007716032819,67.4897510316844,12.));
#98215=CARTESIAN_POINT('Ctrl Pts',(-18.9906460638625,67.472833671964,12.));
#98216=CARTESIAN_POINT('Ctrl Pts',(-18.9805663798448,67.4559518744638,12.));
#98217=CARTESIAN_POINT('Ctrl Pts',(-18.9705325631711,67.4391057908418,12.));
#98218=CARTESIAN_POINT('Ctrl Pts',(-18.9605446160985,67.4222955061981,12.));
#98219=CARTESIAN_POINT('Ctrl Pts',(-18.9525909517915,67.4088759497911,12.));
#98220=CARTESIAN_POINT('Ctrl Pts',(-18.9466463414299,67.3988274146651,12.));
#98221=CARTESIAN_POINT('Ctrl Pts',(-18.9426924398719,67.3921355608328,12.));
#98222=CARTESIAN_POINT('Ctrl Pts',(-18.9407177820969,67.3887914263118,12.));
#98223=CARTESIAN_POINT('Ctrl Pts',(-23.0342913834073,70.5382514078919,-5.55111512312578E-16));
#98224=CARTESIAN_POINT('Ctrl Pts',(-23.0342913834073,70.5382514078919,4.));
#98225=CARTESIAN_POINT('Ctrl Pts',(-23.0342913834073,70.5382514078919,8.));
#98226=CARTESIAN_POINT('Ctrl Pts',(-23.0342913834073,70.5382514078919,12.));
#98227=CARTESIAN_POINT('Ctrl Pts',(-23.0224954570735,70.6474988907591,-5.55111512312578E-16));
#98228=CARTESIAN_POINT('Ctrl Pts',(-23.0224954570735,70.6474988907591,4.));
#98229=CARTESIAN_POINT('Ctrl Pts',(-23.0224954570735,70.647498890759,8.));
#98230=CARTESIAN_POINT('Ctrl Pts',(-23.0224954570735,70.647498890759,12.));
#98231=CARTESIAN_POINT('Ctrl Pts',(-22.9364730048791,70.8310007146901,-5.55111512312578E-16));
#98232=CARTESIAN_POINT('Ctrl Pts',(-22.9364730048791,70.8310007146901,4.));
#98233=CARTESIAN_POINT('Ctrl Pts',(-22.9364730048791,70.83100071469,7.99999999999999));
#98234=CARTESIAN_POINT('Ctrl Pts',(-22.9364730048791,70.83100071469,12.));
#98235=CARTESIAN_POINT('Ctrl Pts',(-22.7679558220499,70.9357242819031,-5.55111512312578E-16));
#98236=CARTESIAN_POINT('Ctrl Pts',(-22.7679558220499,70.9357242819031,4.));
#98237=CARTESIAN_POINT('Ctrl Pts',(-22.7679558220499,70.9357242819031,8.00000000000001));
#98238=CARTESIAN_POINT('Ctrl Pts',(-22.7679558220499,70.9357242819031,12.));
#98239=CARTESIAN_POINT('Ctrl Pts',(-22.6894590071812,70.9608233461356,-5.55111512312578E-16));
#98240=CARTESIAN_POINT('Ctrl Pts',(-22.6894590071812,70.9608233461356,4.));
#98241=CARTESIAN_POINT('Ctrl Pts',(-22.6894590071812,70.9608233461356,8.));
#98242=CARTESIAN_POINT('Ctrl Pts',(-22.6894590071812,70.9608233461356,12.));
#98243=CARTESIAN_POINT('',(-23.0342913834073,70.5382514078919,0.));
#98244=CARTESIAN_POINT('',(-22.6894590071812,70.9608233461355,2.77555756156289E-16));
#98245=CARTESIAN_POINT('Ctrl Pts',(-23.0342913834073,70.5382514078919,-1.38777878078145E-16));
#98246=CARTESIAN_POINT('Ctrl Pts',(-23.0224954570735,70.6474988907591,-1.38777878078145E-16));
#98247=CARTESIAN_POINT('Ctrl Pts',(-22.9733397701052,70.7523570758625,-1.38777878078145E-16));
#98248=CARTESIAN_POINT('Ctrl Pts',(-22.8972470282358,70.8314917485682,-1.38777878078145E-16));
#98249=CARTESIAN_POINT('Ctrl Pts',(-22.8401774718338,70.8908427530975,-1.38777878078145E-16));
#98250=CARTESIAN_POINT('Ctrl Pts',(-22.7679558220499,70.9357242819031,-1.38777878078145E-16));
#98251=CARTESIAN_POINT('Ctrl Pts',(-22.6894590071812,70.9608233461356,-1.38777878078145E-16));
#98252=CARTESIAN_POINT('',(-22.6894590071812,70.9608233461355,12.));
#98253=CARTESIAN_POINT('Ctrl Pts',(-22.6894590071812,70.9608233461356,-5.55111512312578E-16));
#98254=CARTESIAN_POINT('Ctrl Pts',(-22.6894590071812,70.9608233461356,4.));
#98255=CARTESIAN_POINT('Ctrl Pts',(-22.6894590071812,70.9608233461356,8.));
#98256=CARTESIAN_POINT('Ctrl Pts',(-22.6894590071812,70.9608233461356,12.));
#98257=CARTESIAN_POINT('',(-23.0342913834073,70.5382514078919,12.));
#98258=CARTESIAN_POINT('Ctrl Pts',(-22.6894590071812,70.9608233461356,12.));
#98259=CARTESIAN_POINT('Ctrl Pts',(-22.7679558220499,70.9357242819031,12.));
#98260=CARTESIAN_POINT('Ctrl Pts',(-22.8401774718338,70.8908427530975,12.));
#98261=CARTESIAN_POINT('Ctrl Pts',(-22.8972470282358,70.8314917485682,12.));
#98262=CARTESIAN_POINT('Ctrl Pts',(-22.9733397701052,70.7523570758625,12.));
#98263=CARTESIAN_POINT('Ctrl Pts',(-23.0224954570735,70.647498890759,12.));
#98264=CARTESIAN_POINT('Ctrl Pts',(-23.0342913834073,70.5382514078919,12.));
#98265=CARTESIAN_POINT('Ctrl Pts',(-23.0342913834073,70.5382514078919,12.));
#98266=CARTESIAN_POINT('Ctrl Pts',(-23.0342913834073,70.5382514078919,8.));
#98267=CARTESIAN_POINT('Ctrl Pts',(-23.0342913834073,70.5382514078919,4.));
#98268=CARTESIAN_POINT('Ctrl Pts',(-23.0342913834073,70.5382514078919,-5.55111512312578E-16));
#98269=CARTESIAN_POINT('Origin',(-1.12812358559725E-10,3.57465004850839E-10,
0.));
#98270=CARTESIAN_POINT('Origin',(-1.12812358559725E-10,3.57465004850839E-10,
12.));
#98271=CARTESIAN_POINT('Origin',(-1.12812358559725E-10,3.57465004850839E-10,
0.));
#98272=CARTESIAN_POINT('Ctrl Pts',(-15.8307637747257,72.7986051948032,0.));
#98273=CARTESIAN_POINT('Ctrl Pts',(-15.8307637747257,72.7986051948032,4.));
#98274=CARTESIAN_POINT('Ctrl Pts',(-15.8307637747257,72.7986051948032,8.));
#98275=CARTESIAN_POINT('Ctrl Pts',(-15.8307637747257,72.7986051948032,12.));
#98276=CARTESIAN_POINT('Ctrl Pts',(-15.7233907508393,72.8219545017354,0.));
#98277=CARTESIAN_POINT('Ctrl Pts',(-15.7233907508393,72.8219545017354,4.));
#98278=CARTESIAN_POINT('Ctrl Pts',(-15.7233907508393,72.8219545017354,8.));
#98279=CARTESIAN_POINT('Ctrl Pts',(-15.7233907508393,72.8219545017354,12.));
#98280=CARTESIAN_POINT('Ctrl Pts',(-15.5221041200717,72.7983622347337,0.));
#98281=CARTESIAN_POINT('Ctrl Pts',(-15.5221041200717,72.7983622347337,4.00000000000001));
#98282=CARTESIAN_POINT('Ctrl Pts',(-15.5221041200718,72.7983622347338,7.99999999999999));
#98283=CARTESIAN_POINT('Ctrl Pts',(-15.5221041200718,72.7983622347338,12.));
#98284=CARTESIAN_POINT('Ctrl Pts',(-15.3694736926913,72.6715981986664,0.));
#98285=CARTESIAN_POINT('Ctrl Pts',(-15.3694736926913,72.6715981986664,4.));
#98286=CARTESIAN_POINT('Ctrl Pts',(-15.3694736926914,72.6715981986665,8.00000000000001));
#98287=CARTESIAN_POINT('Ctrl Pts',(-15.3694736926914,72.6715981986665,12.));
#98288=CARTESIAN_POINT('Ctrl Pts',(-15.3208442077185,72.6050633494354,0.));
#98289=CARTESIAN_POINT('Ctrl Pts',(-15.3208442077185,72.6050633494354,4.));
#98290=CARTESIAN_POINT('Ctrl Pts',(-15.3208442077186,72.6050633494355,8.));
#98291=CARTESIAN_POINT('Ctrl Pts',(-15.3208442077186,72.6050633494355,12.));
#98292=CARTESIAN_POINT('',(-15.8307637747257,72.7986051948032,0.));
#98293=CARTESIAN_POINT('',(-15.3208442077189,72.6050633494351,0.));
#98294=CARTESIAN_POINT('Ctrl Pts',(-15.8307637747257,72.7986051948032,0.));
#98295=CARTESIAN_POINT('Ctrl Pts',(-15.7233907508393,72.8219545017354,0.));
#98296=CARTESIAN_POINT('Ctrl Pts',(-15.6083698189721,72.8084732063059,0.));
#98297=CARTESIAN_POINT('Ctrl Pts',(-15.5092366269864,72.7613031699569,0.));
#98298=CARTESIAN_POINT('Ctrl Pts',(-15.4348867329972,72.7259256426953,0.));
#98299=CARTESIAN_POINT('Ctrl Pts',(-15.3694736926913,72.6715981986664,0.));
#98300=CARTESIAN_POINT('Ctrl Pts',(-15.3208442077185,72.6050633494354,0.));
#98301=CARTESIAN_POINT('',(-15.320844207719,72.6050633494352,12.));
#98302=CARTESIAN_POINT('Ctrl Pts',(-15.3208442077185,72.6050633494354,0.));
#98303=CARTESIAN_POINT('Ctrl Pts',(-15.3208442077185,72.6050633494354,4.));
#98304=CARTESIAN_POINT('Ctrl Pts',(-15.3208442077186,72.6050633494355,8.));
#98305=CARTESIAN_POINT('Ctrl Pts',(-15.3208442077186,72.6050633494355,12.));
#98306=CARTESIAN_POINT('',(-15.8307637747257,72.7986051948032,12.));
#98307=CARTESIAN_POINT('Ctrl Pts',(-15.3208442077186,72.6050633494355,12.));
#98308=CARTESIAN_POINT('Ctrl Pts',(-15.3694736926914,72.6715981986665,12.));
#98309=CARTESIAN_POINT('Ctrl Pts',(-15.4348867329973,72.7259256426953,12.));
#98310=CARTESIAN_POINT('Ctrl Pts',(-15.5092366269865,72.761303169957,12.));
#98311=CARTESIAN_POINT('Ctrl Pts',(-15.6083698189722,72.8084732063059,12.));
#98312=CARTESIAN_POINT('Ctrl Pts',(-15.7233907508393,72.8219545017354,12.));
#98313=CARTESIAN_POINT('Ctrl Pts',(-15.8307637747257,72.7986051948032,12.));
#98314=CARTESIAN_POINT('Ctrl Pts',(-15.8307637747257,72.7986051948032,12.));
#98315=CARTESIAN_POINT('Ctrl Pts',(-15.8307637747257,72.7986051948032,8.));
#98316=CARTESIAN_POINT('Ctrl Pts',(-15.8307637747257,72.7986051948032,4.));
#98317=CARTESIAN_POINT('Ctrl Pts',(-15.8307637747257,72.7986051948032,0.));
#98318=CARTESIAN_POINT('Ctrl Pts',(-12.9953224629497,68.7831490561748,0.));
#98319=CARTESIAN_POINT('Ctrl Pts',(-12.9953224629497,68.7831490561748,12.));
#98320=CARTESIAN_POINT('Ctrl Pts',(-12.9969981460277,68.7866525680193,0.));
#98321=CARTESIAN_POINT('Ctrl Pts',(-12.9969981460277,68.7866525680193,12.));
#98322=CARTESIAN_POINT('Ctrl Pts',(-13.0003537683055,68.7936635625545,0.));
#98323=CARTESIAN_POINT('Ctrl Pts',(-13.0003537683055,68.7936635625545,12.));
#98324=CARTESIAN_POINT('Ctrl Pts',(-13.0053999700875,68.804191966902,0.));
#98325=CARTESIAN_POINT('Ctrl Pts',(-13.0053999700875,68.804191966902,12.));
#98326=CARTESIAN_POINT('Ctrl Pts',(-13.0121537768946,68.8182536653656,0.));
#98327=CARTESIAN_POINT('Ctrl Pts',(-13.0121537768946,68.8182536653656,12.));
#98328=CARTESIAN_POINT('Ctrl Pts',(-13.0206386039691,68.8358704887468,0.));
#98329=CARTESIAN_POINT('Ctrl Pts',(-13.0206386039691,68.8358704887468,12.));
#98330=CARTESIAN_POINT('Ctrl Pts',(-13.0291660060107,68.8535269726794,0.));
#98331=CARTESIAN_POINT('Ctrl Pts',(-13.0291660060107,68.8535269726794,12.));
#98332=CARTESIAN_POINT('Ctrl Pts',(-13.0377359881875,68.8712230321906,0.));
#98333=CARTESIAN_POINT('Ctrl Pts',(-13.0377359881875,68.8712230321906,12.));
#98334=CARTESIAN_POINT('Ctrl Pts',(-13.0463485518207,68.8889585151585,0.));
#98335=CARTESIAN_POINT('Ctrl Pts',(-13.0463485518207,68.8889585151585,12.));
#98336=CARTESIAN_POINT('Ctrl Pts',(-13.0550036938813,68.9067332040985,0.));
#98337=CARTESIAN_POINT('Ctrl Pts',(-13.0550036938813,68.9067332040985,12.));
#98338=CARTESIAN_POINT('Ctrl Pts',(-13.0637014089029,68.9245468449945,0.));
#98339=CARTESIAN_POINT('Ctrl Pts',(-13.0637014089029,68.9245468449945,12.));
#98340=CARTESIAN_POINT('Ctrl Pts',(-13.072441690283,68.9423991694492,0.));
#98341=CARTESIAN_POINT('Ctrl Pts',(-13.072441690283,68.9423991694492,12.));
#98342=CARTESIAN_POINT('Ctrl Pts',(-13.0812245317808,68.9602899187573,0.));
#98343=CARTESIAN_POINT('Ctrl Pts',(-13.0812245317808,68.9602899187573,12.));
#98344=CARTESIAN_POINT('Ctrl Pts',(-13.090049929053,68.9782188692581,0.));
#98345=CARTESIAN_POINT('Ctrl Pts',(-13.090049929053,68.9782188692581,12.));
#98346=CARTESIAN_POINT('Ctrl Pts',(-13.0989178791834,68.9961858241519,0.));
#98347=CARTESIAN_POINT('Ctrl Pts',(-13.0989178791834,68.9961858241519,12.));
#98348=CARTESIAN_POINT('Ctrl Pts',(-13.1078283799722,69.0141906015113,0.));
#98349=CARTESIAN_POINT('Ctrl Pts',(-13.1078283799722,69.0141906015113,12.));
#98350=CARTESIAN_POINT('Ctrl Pts',(-13.1167814293497,69.0322330243348,0.));
#98351=CARTESIAN_POINT('Ctrl Pts',(-13.1167814293497,69.0322330243348,12.));
#98352=CARTESIAN_POINT('Ctrl Pts',(-13.1257770246385,69.0503129081817,0.));
#98353=CARTESIAN_POINT('Ctrl Pts',(-13.1257770246385,69.0503129081817,12.));
#98354=CARTESIAN_POINT('Ctrl Pts',(-13.1348151621834,69.0684300549477,0.));
#98355=CARTESIAN_POINT('Ctrl Pts',(-13.1348151621834,69.0684300549477,12.));
#98356=CARTESIAN_POINT('Ctrl Pts',(-13.1438958377404,69.0865842593102,0.));
#98357=CARTESIAN_POINT('Ctrl Pts',(-13.1438958377404,69.0865842593102,12.));
#98358=CARTESIAN_POINT('Ctrl Pts',(-13.1530190467183,69.1047753127643,0.));
#98359=CARTESIAN_POINT('Ctrl Pts',(-13.1530190467183,69.1047753127643,12.));
#98360=CARTESIAN_POINT('Ctrl Pts',(-13.1621847844528,69.1230030082573,0.));
#98361=CARTESIAN_POINT('Ctrl Pts',(-13.1621847844528,69.1230030082573,12.));
#98362=CARTESIAN_POINT('Ctrl Pts',(-13.1713930465133,69.1412671454564,0.));
#98363=CARTESIAN_POINT('Ctrl Pts',(-13.1713930465133,69.1412671454564,12.));
#98364=CARTESIAN_POINT('Ctrl Pts',(-13.1806438286934,69.1595675305245,0.));
#98365=CARTESIAN_POINT('Ctrl Pts',(-13.1806438286934,69.1595675305245,12.));
#98366=CARTESIAN_POINT('Ctrl Pts',(-13.1899371268683,69.1779039735996,0.));
#98367=CARTESIAN_POINT('Ctrl Pts',(-13.1899371268683,69.1779039735996,12.));
#98368=CARTESIAN_POINT('Ctrl Pts',(-13.1992729368928,69.1962762870527,0.));
#98369=CARTESIAN_POINT('Ctrl Pts',(-13.1992729368928,69.1962762870527,12.));
#98370=CARTESIAN_POINT('Ctrl Pts',(-13.2086512544735,69.2146842833537,0.));
#98371=CARTESIAN_POINT('Ctrl Pts',(-13.2086512544735,69.2146842833537,12.));
#98372=CARTESIAN_POINT('Ctrl Pts',(-13.2180720750594,69.2331277732861,0.));
#98373=CARTESIAN_POINT('Ctrl Pts',(-13.2180720750594,69.2331277732861,12.));
#98374=CARTESIAN_POINT('Ctrl Pts',(-13.2275353939051,69.2516065668844,0.));
#98375=CARTESIAN_POINT('Ctrl Pts',(-13.2275353939051,69.2516065668844,12.));
#98376=CARTESIAN_POINT('Ctrl Pts',(-13.237041206122,69.270120474245,0.));
#98377=CARTESIAN_POINT('Ctrl Pts',(-13.237041206122,69.270120474245,12.));
#98378=CARTESIAN_POINT('Ctrl Pts',(-13.2465895067262,69.2886693063182,0.));
#98379=CARTESIAN_POINT('Ctrl Pts',(-13.2465895067262,69.2886693063182,12.));
#98380=CARTESIAN_POINT('Ctrl Pts',(-13.2561802906896,69.3072528758518,0.));
#98381=CARTESIAN_POINT('Ctrl Pts',(-13.2561802906896,69.3072528758518,12.));
#98382=CARTESIAN_POINT('Ctrl Pts',(-13.265813552961,69.3258709977382,0.));
#98383=CARTESIAN_POINT('Ctrl Pts',(-13.265813552961,69.3258709977382,12.));
#98384=CARTESIAN_POINT('Ctrl Pts',(-13.2754892884433,69.3445234885065,0.));
#98385=CARTESIAN_POINT('Ctrl Pts',(-13.2754892884433,69.3445234885065,12.));
#98386=CARTESIAN_POINT('Ctrl Pts',(-13.2852074919766,69.3632101660066,0.));
#98387=CARTESIAN_POINT('Ctrl Pts',(-13.2852074919766,69.3632101660066,12.));
#98388=CARTESIAN_POINT('Ctrl Pts',(-13.2949681583167,69.3819308490422,0.));
#98389=CARTESIAN_POINT('Ctrl Pts',(-13.2949681583167,69.3819308490422,12.));
#98390=CARTESIAN_POINT('Ctrl Pts',(-13.3047712821051,69.4006853569511,0.));
#98391=CARTESIAN_POINT('Ctrl Pts',(-13.3047712821051,69.4006853569511,12.));
#98392=CARTESIAN_POINT('Ctrl Pts',(-13.3146168578743,69.4194735096265,0.));
#98393=CARTESIAN_POINT('Ctrl Pts',(-13.3146168578743,69.4194735096265,12.));
#98394=CARTESIAN_POINT('Ctrl Pts',(-13.3245048800643,69.4382951276998,0.));
#98395=CARTESIAN_POINT('Ctrl Pts',(-13.3245048800643,69.4382951276998,12.));
#98396=CARTESIAN_POINT('Ctrl Pts',(-13.3344353430313,69.4571500326673,0.));
#98397=CARTESIAN_POINT('Ctrl Pts',(-13.3344353430313,69.4571500326673,12.));
#98398=CARTESIAN_POINT('Ctrl Pts',(-13.3444082410543,69.4760380470365,0.));
#98399=CARTESIAN_POINT('Ctrl Pts',(-13.3444082410543,69.4760380470365,12.));
#98400=CARTESIAN_POINT('Ctrl Pts',(-13.3544235683394,69.4949589944606,0.));
#98401=CARTESIAN_POINT('Ctrl Pts',(-13.3544235683394,69.4949589944606,12.));
#98402=CARTESIAN_POINT('Ctrl Pts',(-13.3644813190219,69.5139126996675,0.));
#98403=CARTESIAN_POINT('Ctrl Pts',(-13.3644813190219,69.5139126996675,12.));
#98404=CARTESIAN_POINT('Ctrl Pts',(-13.3745814871665,69.5328989883885,0.));
#98405=CARTESIAN_POINT('Ctrl Pts',(-13.3745814871665,69.5328989883885,12.));
#98406=CARTESIAN_POINT('Ctrl Pts',(-13.3847240667628,69.5519176872862,0.));
#98407=CARTESIAN_POINT('Ctrl Pts',(-13.3847240667628,69.5519176872862,12.));
#98408=CARTESIAN_POINT('Ctrl Pts',(-13.3949090517177,69.5709686238724,0.));
#98409=CARTESIAN_POINT('Ctrl Pts',(-13.3949090517177,69.5709686238724,12.));
#98410=CARTESIAN_POINT('Ctrl Pts',(-13.40513643585,69.5900516264553,0.));
#98411=CARTESIAN_POINT('Ctrl Pts',(-13.40513643585,69.5900516264553,12.));
#98412=CARTESIAN_POINT('Ctrl Pts',(-13.4154062129002,69.6091665241765,0.));
#98413=CARTESIAN_POINT('Ctrl Pts',(-13.4154062129002,69.6091665241765,12.));
#98414=CARTESIAN_POINT('Ctrl Pts',(-13.4257183765341,69.6283131470273,0.));
#98415=CARTESIAN_POINT('Ctrl Pts',(-13.4257183765341,69.6283131470273,12.));
#98416=CARTESIAN_POINT('Ctrl Pts',(-13.4360729203442,69.6474913258675,0.));
#98417=CARTESIAN_POINT('Ctrl Pts',(-13.4360729203442,69.6474913258675,12.));
#98418=CARTESIAN_POINT('Ctrl Pts',(-13.4464698378453,69.666700892444,0.));
#98419=CARTESIAN_POINT('Ctrl Pts',(-13.4464698378453,69.666700892444,12.));
#98420=CARTESIAN_POINT('Ctrl Pts',(-13.456909122476,69.6859416793885,0.));
#98421=CARTESIAN_POINT('Ctrl Pts',(-13.456909122476,69.6859416793885,12.));
#98422=CARTESIAN_POINT('Ctrl Pts',(-13.4673907676044,69.7052135201998,0.));
#98423=CARTESIAN_POINT('Ctrl Pts',(-13.4673907676044,69.7052135201998,12.));
#98424=CARTESIAN_POINT('Ctrl Pts',(-13.4779147665285,69.724516249225,0.));
#98425=CARTESIAN_POINT('Ctrl Pts',(-13.4779147665285,69.724516249225,12.));
#98426=CARTESIAN_POINT('Ctrl Pts',(-13.4884811124748,69.7438497016406,0.));
#98427=CARTESIAN_POINT('Ctrl Pts',(-13.4884811124748,69.7438497016406,12.));
#98428=CARTESIAN_POINT('Ctrl Pts',(-13.4990897985905,69.7632137134249,0.));
#98429=CARTESIAN_POINT('Ctrl Pts',(-13.4990897985905,69.7632137134249,12.));
#98430=CARTESIAN_POINT('Ctrl Pts',(-13.5097408179479,69.7826081213576,0.));
#98431=CARTESIAN_POINT('Ctrl Pts',(-13.5097408179479,69.7826081213576,12.));
#98432=CARTESIAN_POINT('Ctrl Pts',(-13.5204341635507,69.8020327630205,0.));
#98433=CARTESIAN_POINT('Ctrl Pts',(-13.5204341635507,69.8020327630205,12.));
#98434=CARTESIAN_POINT('Ctrl Pts',(-13.5311698283339,69.8214874767944,0.));
#98435=CARTESIAN_POINT('Ctrl Pts',(-13.5311698283339,69.8214874767944,12.));
#98436=CARTESIAN_POINT('Ctrl Pts',(-13.5419478051625,69.840972101856,0.));
#98437=CARTESIAN_POINT('Ctrl Pts',(-13.5419478051625,69.840972101856,12.));
#98438=CARTESIAN_POINT('Ctrl Pts',(-13.5527680868255,69.8604864781706,0.));
#98439=CARTESIAN_POINT('Ctrl Pts',(-13.5527680868255,69.8604864781706,12.));
#98440=CARTESIAN_POINT('Ctrl Pts',(-13.5636306660422,69.8800304464882,0.));
#98441=CARTESIAN_POINT('Ctrl Pts',(-13.5636306660422,69.8800304464882,12.));
#98442=CARTESIAN_POINT('Ctrl Pts',(-13.5745355354657,69.8996038483361,0.));
#98443=CARTESIAN_POINT('Ctrl Pts',(-13.5745355354657,69.8996038483361,12.));
#98444=CARTESIAN_POINT('Ctrl Pts',(-13.5854826876835,69.9192065260108,0.));
#98445=CARTESIAN_POINT('Ctrl Pts',(-13.5854826876835,69.9192065260108,12.));
#98446=CARTESIAN_POINT('Ctrl Pts',(-13.5964721152135,69.9388383225648,0.));
#98447=CARTESIAN_POINT('Ctrl Pts',(-13.5964721152135,69.9388383225648,12.));
#98448=CARTESIAN_POINT('Ctrl Pts',(-13.6075038104999,69.9584990817974,0.));
#98449=CARTESIAN_POINT('Ctrl Pts',(-13.6075038104999,69.9584990817974,12.));
#98450=CARTESIAN_POINT('Ctrl Pts',(-13.6185777659198,69.9781886482528,0.));
#98451=CARTESIAN_POINT('Ctrl Pts',(-13.6185777659198,69.9781886482528,12.));
#98452=CARTESIAN_POINT('Ctrl Pts',(-13.6296939737865,69.9979068672153,0.));
#98453=CARTESIAN_POINT('Ctrl Pts',(-13.6296939737865,69.9979068672153,12.));
#98454=CARTESIAN_POINT('Ctrl Pts',(-13.6408524263496,70.0176535847049,0.));
#98455=CARTESIAN_POINT('Ctrl Pts',(-13.6408524263496,70.0176535847049,12.));
#98456=CARTESIAN_POINT('Ctrl Pts',(-13.6520531157907,70.0374286474677,0.));
#98457=CARTESIAN_POINT('Ctrl Pts',(-13.6520531157907,70.0374286474677,12.));
#98458=CARTESIAN_POINT('Ctrl Pts',(-13.6632960342196,70.0572319029676,0.));
#98459=CARTESIAN_POINT('Ctrl Pts',(-13.6632960342196,70.0572319029676,12.));
#98460=CARTESIAN_POINT('Ctrl Pts',(-13.674581173683,70.0770631993856,0.));
#98461=CARTESIAN_POINT('Ctrl Pts',(-13.674581173683,70.0770631993856,12.));
#98462=CARTESIAN_POINT('Ctrl Pts',(-13.6859085261653,70.0969223856136,0.));
#98463=CARTESIAN_POINT('Ctrl Pts',(-13.6859085261653,70.0969223856136,12.));
#98464=CARTESIAN_POINT('Ctrl Pts',(-13.6972780835897,70.1168093112486,0.));
#98465=CARTESIAN_POINT('Ctrl Pts',(-13.6972780835897,70.1168093112486,12.));
#98466=CARTESIAN_POINT('Ctrl Pts',(-13.7086898378122,70.1367238265825,0.));
#98467=CARTESIAN_POINT('Ctrl Pts',(-13.7086898378122,70.1367238265825,12.));
#98468=CARTESIAN_POINT('Ctrl Pts',(-13.7201437806199,70.156665782595,0.));
#98469=CARTESIAN_POINT('Ctrl Pts',(-13.7201437806199,70.156665782595,12.));
#98470=CARTESIAN_POINT('Ctrl Pts',(-13.7316399037393,70.1766350309518,0.));
#98471=CARTESIAN_POINT('Ctrl Pts',(-13.7316399037393,70.1766350309518,12.));
#98472=CARTESIAN_POINT('Ctrl Pts',(-13.7431781988365,70.1966314239995,0.));
#98473=CARTESIAN_POINT('Ctrl Pts',(-13.7431781988365,70.1966314239995,12.));
#98474=CARTESIAN_POINT('Ctrl Pts',(-13.7547586575181,70.2166548147604,0.));
#98475=CARTESIAN_POINT('Ctrl Pts',(-13.7547586575181,70.2166548147604,12.));
#98476=CARTESIAN_POINT('Ctrl Pts',(-13.7663812713243,70.2367050569216,0.));
#98477=CARTESIAN_POINT('Ctrl Pts',(-13.7663812713243,70.2367050569216,12.));
#98478=CARTESIAN_POINT('Ctrl Pts',(-13.7780460317294,70.2567820048303,0.));
#98479=CARTESIAN_POINT('Ctrl Pts',(-13.7780460317294,70.2567820048303,12.));
#98480=CARTESIAN_POINT('Ctrl Pts',(-13.7897529301491,70.2768855134947,0.));
#98481=CARTESIAN_POINT('Ctrl Pts',(-13.7897529301491,70.2768855134947,12.));
#98482=CARTESIAN_POINT('Ctrl Pts',(-13.8015019579414,70.2970154385774,0.));
#98483=CARTESIAN_POINT('Ctrl Pts',(-13.8015019579414,70.2970154385774,12.));
#98484=CARTESIAN_POINT('Ctrl Pts',(-13.8132931064064,70.3171716363897,0.));
#98485=CARTESIAN_POINT('Ctrl Pts',(-13.8132931064064,70.3171716363897,12.));
#98486=CARTESIAN_POINT('Ctrl Pts',(-13.8251263667791,70.3373539638809,0.));
#98487=CARTESIAN_POINT('Ctrl Pts',(-13.8251263667791,70.3373539638809,12.));
#98488=CARTESIAN_POINT('Ctrl Pts',(-13.8370017302309,70.3575622786335,0.));
#98489=CARTESIAN_POINT('Ctrl Pts',(-13.8370017302309,70.3575622786335,12.));
#98490=CARTESIAN_POINT('Ctrl Pts',(-13.8489191878767,70.3777964388632,0.));
#98491=CARTESIAN_POINT('Ctrl Pts',(-13.8489191878767,70.3777964388632,12.));
#98492=CARTESIAN_POINT('Ctrl Pts',(-13.8608787307752,70.3980563034133,0.));
#98493=CARTESIAN_POINT('Ctrl Pts',(-13.8608787307752,70.3980563034133,12.));
#98494=CARTESIAN_POINT('Ctrl Pts',(-13.8728803499287,70.41834173175,0.));
#98495=CARTESIAN_POINT('Ctrl Pts',(-13.8728803499287,70.41834173175,12.));
#98496=CARTESIAN_POINT('Ctrl Pts',(-13.8849240362763,70.4386525839521,0.));
#98497=CARTESIAN_POINT('Ctrl Pts',(-13.8849240362763,70.4386525839521,12.));
#98498=CARTESIAN_POINT('Ctrl Pts',(-13.8970097806954,70.4589887207073,0.));
#98499=CARTESIAN_POINT('Ctrl Pts',(-13.8970097806954,70.4589887207073,12.));
#98500=CARTESIAN_POINT('Ctrl Pts',(-13.9091375740088,70.4793500033124,0.));
#98501=CARTESIAN_POINT('Ctrl Pts',(-13.9091375740088,70.4793500033124,12.));
#98502=CARTESIAN_POINT('Ctrl Pts',(-13.9213074069853,70.4997362936673,0.));
#98503=CARTESIAN_POINT('Ctrl Pts',(-13.9213074069853,70.4997362936673,12.));
#98504=CARTESIAN_POINT('Ctrl Pts',(-13.9335192703388,70.520147454271,0.));
#98505=CARTESIAN_POINT('Ctrl Pts',(-13.9335192703388,70.520147454271,12.));
#98506=CARTESIAN_POINT('Ctrl Pts',(-13.9457731547215,70.5405833482112,0.));
#98507=CARTESIAN_POINT('Ctrl Pts',(-13.9457731547215,70.5405833482112,12.));
#98508=CARTESIAN_POINT('Ctrl Pts',(-13.958069050726,70.5610438391612,0.));
#98509=CARTESIAN_POINT('Ctrl Pts',(-13.958069050726,70.5610438391612,12.));
#98510=CARTESIAN_POINT('Ctrl Pts',(-13.9704069488917,70.5815287913784,0.));
#98511=CARTESIAN_POINT('Ctrl Pts',(-13.9704069488917,70.5815287913784,12.));
#98512=CARTESIAN_POINT('Ctrl Pts',(-13.9827868397057,70.6020380697005,0.));
#98513=CARTESIAN_POINT('Ctrl Pts',(-13.9827868397057,70.6020380697005,12.));
#98514=CARTESIAN_POINT('Ctrl Pts',(-13.9952087136018,70.6225715395394,0.));
#98515=CARTESIAN_POINT('Ctrl Pts',(-13.9952087136018,70.6225715395394,12.));
#98516=CARTESIAN_POINT('Ctrl Pts',(-14.0076725609537,70.6431290668745,0.));
#98517=CARTESIAN_POINT('Ctrl Pts',(-14.0076725609537,70.6431290668745,12.));
#98518=CARTESIAN_POINT('Ctrl Pts',(-14.020178372077,70.6637105182484,0.));
#98519=CARTESIAN_POINT('Ctrl Pts',(-14.020178372077,70.6637105182484,12.));
#98520=CARTESIAN_POINT('Ctrl Pts',(-14.0327261372362,70.6843157607668,0.));
#98521=CARTESIAN_POINT('Ctrl Pts',(-14.0327261372362,70.6843157607668,12.));
#98522=CARTESIAN_POINT('Ctrl Pts',(-14.0453158466451,70.7049446620928,0.));
#98523=CARTESIAN_POINT('Ctrl Pts',(-14.0453158466451,70.7049446620928,12.));
#98524=CARTESIAN_POINT('Ctrl Pts',(-14.0579474904657,70.7255970904436,0.));
#98525=CARTESIAN_POINT('Ctrl Pts',(-14.0579474904657,70.7255970904436,12.));
#98526=CARTESIAN_POINT('Ctrl Pts',(-14.0706210588016,70.7462729145807,0.));
#98527=CARTESIAN_POINT('Ctrl Pts',(-14.0706210588016,70.7462729145807,12.));
#98528=CARTESIAN_POINT('Ctrl Pts',(-14.0833365416996,70.7669720038077,0.));
#98529=CARTESIAN_POINT('Ctrl Pts',(-14.0833365416996,70.7669720038077,12.));
#98530=CARTESIAN_POINT('Ctrl Pts',(-14.0960939291569,70.7876942279697,0.));
#98531=CARTESIAN_POINT('Ctrl Pts',(-14.0960939291569,70.7876942279697,12.));
#98532=CARTESIAN_POINT('Ctrl Pts',(-14.1088932111214,70.8084394574493,0.));
#98533=CARTESIAN_POINT('Ctrl Pts',(-14.1088932111214,70.8084394574493,12.));
#98534=CARTESIAN_POINT('Ctrl Pts',(-14.1217343774913,70.8292075631621,0.));
#98535=CARTESIAN_POINT('Ctrl Pts',(-14.1217343774913,70.8292075631621,12.));
#98536=CARTESIAN_POINT('Ctrl Pts',(-14.1346174181079,70.8499984165489,0.));
#98537=CARTESIAN_POINT('Ctrl Pts',(-14.1346174181079,70.8499984165489,12.));
#98538=CARTESIAN_POINT('Ctrl Pts',(-14.1475423227568,70.8708118895715,0.));
#98539=CARTESIAN_POINT('Ctrl Pts',(-14.1475423227568,70.8708118895715,12.));
#98540=CARTESIAN_POINT('Ctrl Pts',(-14.1605090811754,70.8916478547132,0.));
#98541=CARTESIAN_POINT('Ctrl Pts',(-14.1605090811754,70.8916478547132,12.));
#98542=CARTESIAN_POINT('Ctrl Pts',(-14.1735176830533,70.9125061849745,0.));
#98543=CARTESIAN_POINT('Ctrl Pts',(-14.1735176830533,70.9125061849745,12.));
#98544=CARTESIAN_POINT('Ctrl Pts',(-14.1865681180321,70.9333867538704,0.));
#98545=CARTESIAN_POINT('Ctrl Pts',(-14.1865681180321,70.9333867538704,12.));
#98546=CARTESIAN_POINT('Ctrl Pts',(-14.1996603756982,70.9542894354216,0.));
#98547=CARTESIAN_POINT('Ctrl Pts',(-14.1996603756982,70.9542894354216,12.));
#98548=CARTESIAN_POINT('Ctrl Pts',(-14.2127944455839,70.9752141041518,0.));
#98549=CARTESIAN_POINT('Ctrl Pts',(-14.2127944455839,70.9752141041518,12.));
#98550=CARTESIAN_POINT('Ctrl Pts',(-14.2259703171737,70.9961606350861,0.));
#98551=CARTESIAN_POINT('Ctrl Pts',(-14.2259703171737,70.9961606350861,12.));
#98552=CARTESIAN_POINT('Ctrl Pts',(-14.2391879799062,71.0171289037488,0.));
#98553=CARTESIAN_POINT('Ctrl Pts',(-14.2391879799062,71.0171289037488,12.));
#98554=CARTESIAN_POINT('Ctrl Pts',(-14.2524474231733,71.0381187861588,0.));
#98555=CARTESIAN_POINT('Ctrl Pts',(-14.2524474231733,71.0381187861588,12.));
#98556=CARTESIAN_POINT('Ctrl Pts',(-14.2657486363139,71.0591301588231,0.));
#98557=CARTESIAN_POINT('Ctrl Pts',(-14.2657486363139,71.0591301588231,12.));
#98558=CARTESIAN_POINT('Ctrl Pts',(-14.2790916086133,71.0801628987332,0.));
#98559=CARTESIAN_POINT('Ctrl Pts',(-14.2790916086133,71.0801628987332,12.));
#98560=CARTESIAN_POINT('Ctrl Pts',(-14.2924763293105,71.1012168833643,0.));
#98561=CARTESIAN_POINT('Ctrl Pts',(-14.2924763293105,71.1012168833643,12.));
#98562=CARTESIAN_POINT('Ctrl Pts',(-14.3059027875994,71.1222919906727,0.));
#98563=CARTESIAN_POINT('Ctrl Pts',(-14.3059027875994,71.1222919906727,12.));
#98564=CARTESIAN_POINT('Ctrl Pts',(-14.3193709726294,71.1433880990929,0.));
#98565=CARTESIAN_POINT('Ctrl Pts',(-14.3193709726294,71.1433880990929,12.));
#98566=CARTESIAN_POINT('Ctrl Pts',(-14.332880873499,71.1645050875308,0.));
#98567=CARTESIAN_POINT('Ctrl Pts',(-14.332880873499,71.1645050875308,12.));
#98568=CARTESIAN_POINT('Ctrl Pts',(-14.3464324792534,71.1856428353593,0.));
#98569=CARTESIAN_POINT('Ctrl Pts',(-14.3464324792534,71.1856428353593,12.));
#98570=CARTESIAN_POINT('Ctrl Pts',(-14.3600257788924,71.2068012224174,0.));
#98571=CARTESIAN_POINT('Ctrl Pts',(-14.3600257788924,71.2068012224174,12.));
#98572=CARTESIAN_POINT('Ctrl Pts',(-14.3736607613722,71.2279801290084,0.));
#98573=CARTESIAN_POINT('Ctrl Pts',(-14.3736607613722,71.2279801290084,12.));
#98574=CARTESIAN_POINT('Ctrl Pts',(-14.3873374156056,71.2491794358958,0.));
#98575=CARTESIAN_POINT('Ctrl Pts',(-14.3873374156056,71.2491794358958,12.));
#98576=CARTESIAN_POINT('Ctrl Pts',(-14.401055730457,71.2703990242988,0.));
#98577=CARTESIAN_POINT('Ctrl Pts',(-14.401055730457,71.2703990242988,12.));
#98578=CARTESIAN_POINT('Ctrl Pts',(-14.4148156947384,71.2916387758861,0.));
#98579=CARTESIAN_POINT('Ctrl Pts',(-14.4148156947384,71.2916387758861,12.));
#98580=CARTESIAN_POINT('Ctrl Pts',(-14.4286172972167,71.312898572777,0.));
#98581=CARTESIAN_POINT('Ctrl Pts',(-14.4286172972167,71.312898572777,12.));
#98582=CARTESIAN_POINT('Ctrl Pts',(-14.4424605266165,71.3341782975386,0.));
#98583=CARTESIAN_POINT('Ctrl Pts',(-14.4424605266165,71.3341782975386,12.));
#98584=CARTESIAN_POINT('Ctrl Pts',(-14.4563453716204,71.3554778331835,0.));
#98585=CARTESIAN_POINT('Ctrl Pts',(-14.4563453716204,71.3554778331835,12.));
#98586=CARTESIAN_POINT('Ctrl Pts',(-14.4702718208651,71.376797063165,0.));
#98587=CARTESIAN_POINT('Ctrl Pts',(-14.4702718208651,71.376797063165,12.));
#98588=CARTESIAN_POINT('Ctrl Pts',(-14.4842398629355,71.3981358713723,0.));
#98589=CARTESIAN_POINT('Ctrl Pts',(-14.4842398629355,71.3981358713723,12.));
#98590=CARTESIAN_POINT('Ctrl Pts',(-14.4982494863718,71.4194941421292,0.));
#98591=CARTESIAN_POINT('Ctrl Pts',(-14.4982494863718,71.4194941421292,12.));
#98592=CARTESIAN_POINT('Ctrl Pts',(-14.5123006796728,71.4408717601923,0.));
#98593=CARTESIAN_POINT('Ctrl Pts',(-14.5123006796728,71.4408717601923,12.));
#98594=CARTESIAN_POINT('Ctrl Pts',(-14.5263934312969,71.4622686107475,0.));
#98595=CARTESIAN_POINT('Ctrl Pts',(-14.5263934312969,71.4622686107475,12.));
#98596=CARTESIAN_POINT('Ctrl Pts',(-14.540527729659,71.4836845794048,0.));
#98597=CARTESIAN_POINT('Ctrl Pts',(-14.540527729659,71.4836845794048,12.));
#98598=CARTESIAN_POINT('Ctrl Pts',(-14.5547035631234,71.5051195521909,0.));
#98599=CARTESIAN_POINT('Ctrl Pts',(-14.5547035631234,71.5051195521909,12.));
#98600=CARTESIAN_POINT('Ctrl Pts',(-14.5689209200091,71.5265734155498,0.));
#98601=CARTESIAN_POINT('Ctrl Pts',(-14.5689209200091,71.5265734155498,12.));
#98602=CARTESIAN_POINT('Ctrl Pts',(-14.5831797885952,71.5480460563447,0.));
#98603=CARTESIAN_POINT('Ctrl Pts',(-14.5831797885952,71.5480460563447,12.));
#98604=CARTESIAN_POINT('Ctrl Pts',(-14.597480157121,71.5695373618562,0.));
#98605=CARTESIAN_POINT('Ctrl Pts',(-14.597480157121,71.5695373618562,12.));
#98606=CARTESIAN_POINT('Ctrl Pts',(-14.6118220137849,71.5910472197813,0.));
#98607=CARTESIAN_POINT('Ctrl Pts',(-14.6118220137849,71.5910472197813,12.));
#98608=CARTESIAN_POINT('Ctrl Pts',(-14.626205346737,71.612575518229,0.));
#98609=CARTESIAN_POINT('Ctrl Pts',(-14.626205346737,71.612575518229,12.));
#98610=CARTESIAN_POINT('Ctrl Pts',(-14.6406301440814,71.6341221457169,0.));
#98611=CARTESIAN_POINT('Ctrl Pts',(-14.6406301440814,71.6341221457169,12.));
#98612=CARTESIAN_POINT('Ctrl Pts',(-14.6550963938829,71.6556869911662,0.));
#98613=CARTESIAN_POINT('Ctrl Pts',(-14.6550963938829,71.6556869911662,12.));
#98614=CARTESIAN_POINT('Ctrl Pts',(-14.6696040841678,71.6772699438963,0.));
#98615=CARTESIAN_POINT('Ctrl Pts',(-14.6696040841678,71.6772699438963,12.));
#98616=CARTESIAN_POINT('Ctrl Pts',(-14.6841532029232,71.6988708936172,0.));
#98617=CARTESIAN_POINT('Ctrl Pts',(-14.6841532029232,71.6988708936172,12.));
#98618=CARTESIAN_POINT('Ctrl Pts',(-14.6987437380901,71.7204897304194,0.));
#98619=CARTESIAN_POINT('Ctrl Pts',(-14.6987437380901,71.7204897304194,12.));
#98620=CARTESIAN_POINT('Ctrl Pts',(-14.7133756775626,71.7421263447719,0.));
#98621=CARTESIAN_POINT('Ctrl Pts',(-14.7133756775626,71.7421263447719,12.));
#98622=CARTESIAN_POINT('Ctrl Pts',(-14.7280490091957,71.7637806275328,0.));
#98623=CARTESIAN_POINT('Ctrl Pts',(-14.7280490091957,71.7637806275328,12.));
#98624=CARTESIAN_POINT('Ctrl Pts',(-14.7427637208073,71.7854524699569,0.));
#98625=CARTESIAN_POINT('Ctrl Pts',(-14.7427637208073,71.7854524699569,12.));
#98626=CARTESIAN_POINT('Ctrl Pts',(-14.7575198001776,71.8071417637017,0.));
#98627=CARTESIAN_POINT('Ctrl Pts',(-14.7575198001776,71.8071417637017,12.));
#98628=CARTESIAN_POINT('Ctrl Pts',(-14.7723172350451,71.8288484008333,0.));
#98629=CARTESIAN_POINT('Ctrl Pts',(-14.7723172350451,71.8288484008333,12.));
#98630=CARTESIAN_POINT('Ctrl Pts',(-14.7871560131017,71.8505722738272,0.));
#98631=CARTESIAN_POINT('Ctrl Pts',(-14.7871560131017,71.8505722738272,12.));
#98632=CARTESIAN_POINT('Ctrl Pts',(-14.8020361219998,71.8723132755446,0.));
#98633=CARTESIAN_POINT('Ctrl Pts',(-14.8020361219998,71.8723132755446,12.));
#98634=CARTESIAN_POINT('Ctrl Pts',(-14.8169575493557,71.8940712992109,0.));
#98635=CARTESIAN_POINT('Ctrl Pts',(-14.8169575493557,71.8940712992109,12.));
#98636=CARTESIAN_POINT('Ctrl Pts',(-14.8319202827482,71.9158462383914,0.));
#98637=CARTESIAN_POINT('Ctrl Pts',(-14.8319202827482,71.9158462383914,12.));
#98638=CARTESIAN_POINT('Ctrl Pts',(-14.8469243097163,71.9376379869678,0.));
#98639=CARTESIAN_POINT('Ctrl Pts',(-14.8469243097163,71.9376379869678,12.));
#98640=CARTESIAN_POINT('Ctrl Pts',(-14.8619696177506,71.9594464391078,0.));
#98641=CARTESIAN_POINT('Ctrl Pts',(-14.8619696177506,71.9594464391078,12.));
#98642=CARTESIAN_POINT('Ctrl Pts',(-14.8770561943014,71.9812714893102,0.));
#98643=CARTESIAN_POINT('Ctrl Pts',(-14.8770561943014,71.9812714893102,12.));
#98644=CARTESIAN_POINT('Ctrl Pts',(-14.8921840267832,72.0031130324529,0.));
#98645=CARTESIAN_POINT('Ctrl Pts',(-14.8921840267832,72.0031130324529,12.));
#98646=CARTESIAN_POINT('Ctrl Pts',(-14.9073531025764,72.0249709638422,0.));
#98647=CARTESIAN_POINT('Ctrl Pts',(-14.9073531025764,72.0249709638422,12.));
#98648=CARTESIAN_POINT('Ctrl Pts',(-14.9225634090268,72.0468451792505,0.));
#98649=CARTESIAN_POINT('Ctrl Pts',(-14.9225634090268,72.0468451792505,12.));
#98650=CARTESIAN_POINT('Ctrl Pts',(-14.9378149334388,72.0687355749807,0.));
#98651=CARTESIAN_POINT('Ctrl Pts',(-14.9378149334388,72.0687355749807,12.));
#98652=CARTESIAN_POINT('Ctrl Pts',(-14.9531076630768,72.0906420478076,0.));
#98653=CARTESIAN_POINT('Ctrl Pts',(-14.9531076630768,72.0906420478076,12.));
#98654=CARTESIAN_POINT('Ctrl Pts',(-14.9684415851698,72.112564494854,0.));
#98655=CARTESIAN_POINT('Ctrl Pts',(-14.9684415851698,72.112564494854,12.));
#98656=CARTESIAN_POINT('Ctrl Pts',(-14.9838166869107,72.1345028134777,0.));
#98657=CARTESIAN_POINT('Ctrl Pts',(-14.9838166869107,72.1345028134777,12.));
#98658=CARTESIAN_POINT('Ctrl Pts',(-14.9992329554537,72.1564569011669,0.));
#98659=CARTESIAN_POINT('Ctrl Pts',(-14.9992329554537,72.1564569011669,12.));
#98660=CARTESIAN_POINT('Ctrl Pts',(-15.0146903779062,72.1784266553953,0.));
#98661=CARTESIAN_POINT('Ctrl Pts',(-15.0146903779062,72.1784266553953,12.));
#98662=CARTESIAN_POINT('Ctrl Pts',(-15.0301889413257,72.2004119736115,0.));
#98663=CARTESIAN_POINT('Ctrl Pts',(-15.0301889413257,72.2004119736115,12.));
#98664=CARTESIAN_POINT('Ctrl Pts',(-15.0457286327331,72.2224127535415,0.));
#98665=CARTESIAN_POINT('Ctrl Pts',(-15.0457286327331,72.2224127535415,12.));
#98666=CARTESIAN_POINT('Ctrl Pts',(-15.0613094391189,72.2444288934262,0.));
#98667=CARTESIAN_POINT('Ctrl Pts',(-15.0613094391189,72.2444288934262,12.));
#98668=CARTESIAN_POINT('Ctrl Pts',(-15.0769313474477,72.2664602922852,0.));
#98669=CARTESIAN_POINT('Ctrl Pts',(-15.0769313474477,72.2664602922852,12.));
#98670=CARTESIAN_POINT('Ctrl Pts',(-15.092594344659,72.2885068501628,0.));
#98671=CARTESIAN_POINT('Ctrl Pts',(-15.092594344659,72.2885068501628,12.));
#98672=CARTESIAN_POINT('Ctrl Pts',(-15.1082984176649,72.3105684683944,0.));
#98673=CARTESIAN_POINT('Ctrl Pts',(-15.1082984176649,72.3105684683944,12.));
#98674=CARTESIAN_POINT('Ctrl Pts',(-15.124043553347,72.3326450490177,0.));
#98675=CARTESIAN_POINT('Ctrl Pts',(-15.124043553347,72.3326450490177,12.));
#98676=CARTESIAN_POINT('Ctrl Pts',(-15.1398297385506,72.3547364941969,0.));
#98677=CARTESIAN_POINT('Ctrl Pts',(-15.1398297385506,72.3547364941969,12.));
#98678=CARTESIAN_POINT('Ctrl Pts',(-15.1556569600745,72.376842705589,0.));
#98679=CARTESIAN_POINT('Ctrl Pts',(-15.1556569600745,72.376842705589,12.));
#98680=CARTESIAN_POINT('Ctrl Pts',(-15.1715252046606,72.3989635838492,0.));
#98681=CARTESIAN_POINT('Ctrl Pts',(-15.1715252046606,72.3989635838492,12.));
#98682=CARTESIAN_POINT('Ctrl Pts',(-15.1874344589726,72.421099027786,0.));
#98683=CARTESIAN_POINT('Ctrl Pts',(-15.1874344589726,72.421099027786,12.));
#98684=CARTESIAN_POINT('Ctrl Pts',(-15.2033847096091,72.4432489350471,0.));
#98685=CARTESIAN_POINT('Ctrl Pts',(-15.2033847096091,72.4432489350471,12.));
#98686=CARTESIAN_POINT('Ctrl Pts',(-15.2193759431373,72.4654132036428,0.));
#98687=CARTESIAN_POINT('Ctrl Pts',(-15.2193759431373,72.4654132036428,12.));
#98688=CARTESIAN_POINT('Ctrl Pts',(-15.235408146116,72.4875917332762,0.));
#98689=CARTESIAN_POINT('Ctrl Pts',(-15.235408146116,72.4875917332762,12.));
#98690=CARTESIAN_POINT('Ctrl Pts',(-15.2514813051172,72.5097844266075,0.));
#98691=CARTESIAN_POINT('Ctrl Pts',(-15.2514813051172,72.5097844266075,12.));
#98692=CARTESIAN_POINT('Ctrl Pts',(-15.2675954067479,72.5319911908917,0.));
#98693=CARTESIAN_POINT('Ctrl Pts',(-15.2675954067479,72.5319911908917,12.));
#98694=CARTESIAN_POINT('Ctrl Pts',(-15.2837504376536,72.5542119383642,0.));
#98695=CARTESIAN_POINT('Ctrl Pts',(-15.2837504376536,72.5542119383642,12.));
#98696=CARTESIAN_POINT('Ctrl Pts',(-15.2999463844661,72.5764465826224,0.));
#98697=CARTESIAN_POINT('Ctrl Pts',(-15.2999463844661,72.5764465826224,12.));
#98698=CARTESIAN_POINT('Ctrl Pts',(-15.3161832337594,72.5986950357677,0.));
#98699=CARTESIAN_POINT('Ctrl Pts',(-15.3161832337594,72.5986950357677,12.));
#98700=CARTESIAN_POINT('Ctrl Pts',(-15.3324609719956,72.6209572051042,0.));
#98701=CARTESIAN_POINT('Ctrl Pts',(-15.3324609719956,72.6209572051042,12.));
#98702=CARTESIAN_POINT('Ctrl Pts',(-15.3487795854745,72.6432329903553,0.));
#98703=CARTESIAN_POINT('Ctrl Pts',(-15.3487795854745,72.6432329903553,12.));
#98704=CARTESIAN_POINT('Ctrl Pts',(-15.3651390602666,72.6655222797801,0.));
#98705=CARTESIAN_POINT('Ctrl Pts',(-15.3651390602666,72.6655222797801,12.));
#98706=CARTESIAN_POINT('Ctrl Pts',(-15.3815393822736,72.687824955772,0.));
#98707=CARTESIAN_POINT('Ctrl Pts',(-15.3815393822736,72.687824955772,12.));
#98708=CARTESIAN_POINT('Ctrl Pts',(-15.3979805373174,72.7101409017716,0.));
#98709=CARTESIAN_POINT('Ctrl Pts',(-15.3979805373174,72.7101409017716,12.));
#98710=CARTESIAN_POINT('Ctrl Pts',(-15.4144625111944,72.7324700089712,0.));
#98711=CARTESIAN_POINT('Ctrl Pts',(-15.4144625111944,72.7324700089712,12.));
#98712=CARTESIAN_POINT('Ctrl Pts',(-15.4309852897844,72.7548121825342,0.));
#98713=CARTESIAN_POINT('Ctrl Pts',(-15.4309852897844,72.7548121825342,12.));
#98714=CARTESIAN_POINT('Ctrl Pts',(-15.4475488590244,72.777167349421,0.));
#98715=CARTESIAN_POINT('Ctrl Pts',(-15.4475488590244,72.777167349421,12.));
#98716=CARTESIAN_POINT('Ctrl Pts',(-15.4641532053281,72.7995354603795,0.));
#98717=CARTESIAN_POINT('Ctrl Pts',(-15.4641532053281,72.7995354603795,12.));
#98718=CARTESIAN_POINT('Ctrl Pts',(-15.4807983165804,72.8219164843279,0.));
#98719=CARTESIAN_POINT('Ctrl Pts',(-15.4807983165804,72.8219164843279,12.));
#98720=CARTESIAN_POINT('Ctrl Pts',(-15.494147009702,72.8398316205897,0.));
#98721=CARTESIAN_POINT('Ctrl Pts',(-15.494147009702,72.8398316205897,12.));
#98722=CARTESIAN_POINT('Ctrl Pts',(-15.5041768663999,72.8532737731759,0.));
#98723=CARTESIAN_POINT('Ctrl Pts',(-15.5041768663999,72.8532737731759,12.));
#98724=CARTESIAN_POINT('Ctrl Pts',(-15.5108715869141,72.8622377860824,0.));
#98725=CARTESIAN_POINT('Ctrl Pts',(-15.5108715869141,72.8622377860824,12.));
#98726=CARTESIAN_POINT('Ctrl Pts',(-15.5142209845168,72.8667204369977,0.));
#98727=CARTESIAN_POINT('Ctrl Pts',(-15.5142209845168,72.8667204369977,12.));
#98728=CARTESIAN_POINT('',(-12.9953224629497,68.7831490561748,0.));
#98729=CARTESIAN_POINT('Ctrl Pts',(-12.9953224629497,68.7831490561748,0.));
#98730=CARTESIAN_POINT('Ctrl Pts',(-12.9969981460277,68.7866525680193,0.));
#98731=CARTESIAN_POINT('Ctrl Pts',(-13.0003537683055,68.7936635625545,0.));
#98732=CARTESIAN_POINT('Ctrl Pts',(-13.0053999700875,68.804191966902,0.));
#98733=CARTESIAN_POINT('Ctrl Pts',(-13.0121537768946,68.8182536653656,0.));
#98734=CARTESIAN_POINT('Ctrl Pts',(-13.0206386039691,68.8358704887468,0.));
#98735=CARTESIAN_POINT('Ctrl Pts',(-13.0291660060107,68.8535269726794,0.));
#98736=CARTESIAN_POINT('Ctrl Pts',(-13.0377359881875,68.8712230321906,0.));
#98737=CARTESIAN_POINT('Ctrl Pts',(-13.0463485518207,68.8889585151585,0.));
#98738=CARTESIAN_POINT('Ctrl Pts',(-13.0550036938813,68.9067332040985,0.));
#98739=CARTESIAN_POINT('Ctrl Pts',(-13.0637014089029,68.9245468449945,0.));
#98740=CARTESIAN_POINT('Ctrl Pts',(-13.072441690283,68.9423991694492,0.));
#98741=CARTESIAN_POINT('Ctrl Pts',(-13.0812245317808,68.9602899187573,0.));
#98742=CARTESIAN_POINT('Ctrl Pts',(-13.090049929053,68.9782188692581,0.));
#98743=CARTESIAN_POINT('Ctrl Pts',(-13.0989178791834,68.9961858241519,0.));
#98744=CARTESIAN_POINT('Ctrl Pts',(-13.1078283799722,69.0141906015113,0.));
#98745=CARTESIAN_POINT('Ctrl Pts',(-13.1167814293497,69.0322330243348,0.));
#98746=CARTESIAN_POINT('Ctrl Pts',(-13.1257770246385,69.0503129081817,0.));
#98747=CARTESIAN_POINT('Ctrl Pts',(-13.1348151621834,69.0684300549477,0.));
#98748=CARTESIAN_POINT('Ctrl Pts',(-13.1438958377404,69.0865842593102,0.));
#98749=CARTESIAN_POINT('Ctrl Pts',(-13.1530190467183,69.1047753127643,0.));
#98750=CARTESIAN_POINT('Ctrl Pts',(-13.1621847844528,69.1230030082573,0.));
#98751=CARTESIAN_POINT('Ctrl Pts',(-13.1713930465133,69.1412671454564,0.));
#98752=CARTESIAN_POINT('Ctrl Pts',(-13.1806438286934,69.1595675305245,0.));
#98753=CARTESIAN_POINT('Ctrl Pts',(-13.1899371268683,69.1779039735996,0.));
#98754=CARTESIAN_POINT('Ctrl Pts',(-13.1992729368928,69.1962762870527,0.));
#98755=CARTESIAN_POINT('Ctrl Pts',(-13.2086512544735,69.2146842833537,0.));
#98756=CARTESIAN_POINT('Ctrl Pts',(-13.2180720750594,69.2331277732861,0.));
#98757=CARTESIAN_POINT('Ctrl Pts',(-13.2275353939051,69.2516065668844,0.));
#98758=CARTESIAN_POINT('Ctrl Pts',(-13.237041206122,69.270120474245,0.));
#98759=CARTESIAN_POINT('Ctrl Pts',(-13.2465895067262,69.2886693063182,0.));
#98760=CARTESIAN_POINT('Ctrl Pts',(-13.2561802906896,69.3072528758518,0.));
#98761=CARTESIAN_POINT('Ctrl Pts',(-13.265813552961,69.3258709977382,0.));
#98762=CARTESIAN_POINT('Ctrl Pts',(-13.2754892884433,69.3445234885065,0.));
#98763=CARTESIAN_POINT('Ctrl Pts',(-13.2852074919766,69.3632101660066,0.));
#98764=CARTESIAN_POINT('Ctrl Pts',(-13.2949681583167,69.3819308490422,0.));
#98765=CARTESIAN_POINT('Ctrl Pts',(-13.3047712821051,69.4006853569511,0.));
#98766=CARTESIAN_POINT('Ctrl Pts',(-13.3146168578743,69.4194735096265,0.));
#98767=CARTESIAN_POINT('Ctrl Pts',(-13.3245048800643,69.4382951276998,0.));
#98768=CARTESIAN_POINT('Ctrl Pts',(-13.3344353430313,69.4571500326673,0.));
#98769=CARTESIAN_POINT('Ctrl Pts',(-13.3444082410543,69.4760380470365,0.));
#98770=CARTESIAN_POINT('Ctrl Pts',(-13.3544235683394,69.4949589944606,0.));
#98771=CARTESIAN_POINT('Ctrl Pts',(-13.3644813190219,69.5139126996675,0.));
#98772=CARTESIAN_POINT('Ctrl Pts',(-13.3745814871665,69.5328989883885,0.));
#98773=CARTESIAN_POINT('Ctrl Pts',(-13.3847240667628,69.5519176872862,0.));
#98774=CARTESIAN_POINT('Ctrl Pts',(-13.3949090517177,69.5709686238724,0.));
#98775=CARTESIAN_POINT('Ctrl Pts',(-13.40513643585,69.5900516264553,0.));
#98776=CARTESIAN_POINT('Ctrl Pts',(-13.4154062129002,69.6091665241765,0.));
#98777=CARTESIAN_POINT('Ctrl Pts',(-13.4257183765341,69.6283131470273,0.));
#98778=CARTESIAN_POINT('Ctrl Pts',(-13.4360729203442,69.6474913258675,0.));
#98779=CARTESIAN_POINT('Ctrl Pts',(-13.4464698378453,69.666700892444,0.));
#98780=CARTESIAN_POINT('Ctrl Pts',(-13.456909122476,69.6859416793885,0.));
#98781=CARTESIAN_POINT('Ctrl Pts',(-13.4673907676044,69.7052135201998,0.));
#98782=CARTESIAN_POINT('Ctrl Pts',(-13.4779147665285,69.724516249225,0.));
#98783=CARTESIAN_POINT('Ctrl Pts',(-13.4884811124748,69.7438497016406,0.));
#98784=CARTESIAN_POINT('Ctrl Pts',(-13.4990897985905,69.7632137134249,0.));
#98785=CARTESIAN_POINT('Ctrl Pts',(-13.5097408179479,69.7826081213576,0.));
#98786=CARTESIAN_POINT('Ctrl Pts',(-13.5204341635507,69.8020327630205,0.));
#98787=CARTESIAN_POINT('Ctrl Pts',(-13.5311698283339,69.8214874767944,0.));
#98788=CARTESIAN_POINT('Ctrl Pts',(-13.5419478051625,69.840972101856,0.));
#98789=CARTESIAN_POINT('Ctrl Pts',(-13.5527680868255,69.8604864781706,0.));
#98790=CARTESIAN_POINT('Ctrl Pts',(-13.5636306660422,69.8800304464882,0.));
#98791=CARTESIAN_POINT('Ctrl Pts',(-13.5745355354657,69.8996038483361,0.));
#98792=CARTESIAN_POINT('Ctrl Pts',(-13.5854826876835,69.9192065260108,0.));
#98793=CARTESIAN_POINT('Ctrl Pts',(-13.5964721152135,69.9388383225648,0.));
#98794=CARTESIAN_POINT('Ctrl Pts',(-13.6075038104999,69.9584990817974,0.));
#98795=CARTESIAN_POINT('Ctrl Pts',(-13.6185777659198,69.9781886482528,0.));
#98796=CARTESIAN_POINT('Ctrl Pts',(-13.6296939737865,69.9979068672153,0.));
#98797=CARTESIAN_POINT('Ctrl Pts',(-13.6408524263496,70.0176535847049,0.));
#98798=CARTESIAN_POINT('Ctrl Pts',(-13.6520531157907,70.0374286474677,0.));
#98799=CARTESIAN_POINT('Ctrl Pts',(-13.6632960342196,70.0572319029676,0.));
#98800=CARTESIAN_POINT('Ctrl Pts',(-13.674581173683,70.0770631993856,0.));
#98801=CARTESIAN_POINT('Ctrl Pts',(-13.6859085261653,70.0969223856136,0.));
#98802=CARTESIAN_POINT('Ctrl Pts',(-13.6972780835897,70.1168093112486,0.));
#98803=CARTESIAN_POINT('Ctrl Pts',(-13.7086898378122,70.1367238265825,0.));
#98804=CARTESIAN_POINT('Ctrl Pts',(-13.7201437806199,70.156665782595,0.));
#98805=CARTESIAN_POINT('Ctrl Pts',(-13.7316399037393,70.1766350309518,0.));
#98806=CARTESIAN_POINT('Ctrl Pts',(-13.7431781988365,70.1966314239995,0.));
#98807=CARTESIAN_POINT('Ctrl Pts',(-13.7547586575181,70.2166548147604,0.));
#98808=CARTESIAN_POINT('Ctrl Pts',(-13.7663812713243,70.2367050569216,0.));
#98809=CARTESIAN_POINT('Ctrl Pts',(-13.7780460317294,70.2567820048303,0.));
#98810=CARTESIAN_POINT('Ctrl Pts',(-13.7897529301491,70.2768855134947,0.));
#98811=CARTESIAN_POINT('Ctrl Pts',(-13.8015019579414,70.2970154385774,0.));
#98812=CARTESIAN_POINT('Ctrl Pts',(-13.8132931064064,70.3171716363897,0.));
#98813=CARTESIAN_POINT('Ctrl Pts',(-13.8251263667791,70.3373539638809,0.));
#98814=CARTESIAN_POINT('Ctrl Pts',(-13.8370017302309,70.3575622786335,0.));
#98815=CARTESIAN_POINT('Ctrl Pts',(-13.8489191878767,70.3777964388632,0.));
#98816=CARTESIAN_POINT('Ctrl Pts',(-13.8608787307752,70.3980563034133,0.));
#98817=CARTESIAN_POINT('Ctrl Pts',(-13.8728803499287,70.41834173175,0.));
#98818=CARTESIAN_POINT('Ctrl Pts',(-13.8849240362763,70.4386525839521,0.));
#98819=CARTESIAN_POINT('Ctrl Pts',(-13.8970097806954,70.4589887207073,0.));
#98820=CARTESIAN_POINT('Ctrl Pts',(-13.9091375740088,70.4793500033124,0.));
#98821=CARTESIAN_POINT('Ctrl Pts',(-13.9213074069853,70.4997362936673,0.));
#98822=CARTESIAN_POINT('Ctrl Pts',(-13.9335192703388,70.520147454271,0.));
#98823=CARTESIAN_POINT('Ctrl Pts',(-13.9457731547215,70.5405833482112,0.));
#98824=CARTESIAN_POINT('Ctrl Pts',(-13.958069050726,70.5610438391612,0.));
#98825=CARTESIAN_POINT('Ctrl Pts',(-13.9704069488917,70.5815287913784,0.));
#98826=CARTESIAN_POINT('Ctrl Pts',(-13.9827868397057,70.6020380697005,0.));
#98827=CARTESIAN_POINT('Ctrl Pts',(-13.9952087136018,70.6225715395394,0.));
#98828=CARTESIAN_POINT('Ctrl Pts',(-14.0076725609537,70.6431290668745,0.));
#98829=CARTESIAN_POINT('Ctrl Pts',(-14.020178372077,70.6637105182484,0.));
#98830=CARTESIAN_POINT('Ctrl Pts',(-14.0327261372362,70.6843157607668,0.));
#98831=CARTESIAN_POINT('Ctrl Pts',(-14.0453158466451,70.7049446620928,0.));
#98832=CARTESIAN_POINT('Ctrl Pts',(-14.0579474904657,70.7255970904436,0.));
#98833=CARTESIAN_POINT('Ctrl Pts',(-14.0706210588016,70.7462729145807,0.));
#98834=CARTESIAN_POINT('Ctrl Pts',(-14.0833365416996,70.7669720038077,0.));
#98835=CARTESIAN_POINT('Ctrl Pts',(-14.0960939291569,70.7876942279697,0.));
#98836=CARTESIAN_POINT('Ctrl Pts',(-14.1088932111214,70.8084394574493,0.));
#98837=CARTESIAN_POINT('Ctrl Pts',(-14.1217343774913,70.8292075631621,0.));
#98838=CARTESIAN_POINT('Ctrl Pts',(-14.1346174181079,70.8499984165489,0.));
#98839=CARTESIAN_POINT('Ctrl Pts',(-14.1475423227568,70.8708118895715,0.));
#98840=CARTESIAN_POINT('Ctrl Pts',(-14.1605090811754,70.8916478547132,0.));
#98841=CARTESIAN_POINT('Ctrl Pts',(-14.1735176830533,70.9125061849745,0.));
#98842=CARTESIAN_POINT('Ctrl Pts',(-14.1865681180321,70.9333867538704,0.));
#98843=CARTESIAN_POINT('Ctrl Pts',(-14.1996603756982,70.9542894354216,0.));
#98844=CARTESIAN_POINT('Ctrl Pts',(-14.2127944455839,70.9752141041518,0.));
#98845=CARTESIAN_POINT('Ctrl Pts',(-14.2259703171737,70.9961606350861,0.));
#98846=CARTESIAN_POINT('Ctrl Pts',(-14.2391879799062,71.0171289037488,0.));
#98847=CARTESIAN_POINT('Ctrl Pts',(-14.2524474231733,71.0381187861588,0.));
#98848=CARTESIAN_POINT('Ctrl Pts',(-14.2657486363139,71.0591301588231,0.));
#98849=CARTESIAN_POINT('Ctrl Pts',(-14.2790916086133,71.0801628987332,0.));
#98850=CARTESIAN_POINT('Ctrl Pts',(-14.2924763293105,71.1012168833643,0.));
#98851=CARTESIAN_POINT('Ctrl Pts',(-14.3059027875994,71.1222919906727,0.));
#98852=CARTESIAN_POINT('Ctrl Pts',(-14.3193709726294,71.1433880990929,0.));
#98853=CARTESIAN_POINT('Ctrl Pts',(-14.332880873499,71.1645050875308,0.));
#98854=CARTESIAN_POINT('Ctrl Pts',(-14.3464324792534,71.1856428353593,0.));
#98855=CARTESIAN_POINT('Ctrl Pts',(-14.3600257788924,71.2068012224174,0.));
#98856=CARTESIAN_POINT('Ctrl Pts',(-14.3736607613722,71.2279801290084,0.));
#98857=CARTESIAN_POINT('Ctrl Pts',(-14.3873374156056,71.2491794358958,0.));
#98858=CARTESIAN_POINT('Ctrl Pts',(-14.401055730457,71.2703990242988,0.));
#98859=CARTESIAN_POINT('Ctrl Pts',(-14.4148156947384,71.2916387758861,0.));
#98860=CARTESIAN_POINT('Ctrl Pts',(-14.4286172972167,71.312898572777,0.));
#98861=CARTESIAN_POINT('Ctrl Pts',(-14.4424605266165,71.3341782975386,0.));
#98862=CARTESIAN_POINT('Ctrl Pts',(-14.4563453716204,71.3554778331835,0.));
#98863=CARTESIAN_POINT('Ctrl Pts',(-14.4702718208651,71.376797063165,0.));
#98864=CARTESIAN_POINT('Ctrl Pts',(-14.4842398629355,71.3981358713723,0.));
#98865=CARTESIAN_POINT('Ctrl Pts',(-14.4982494863718,71.4194941421292,0.));
#98866=CARTESIAN_POINT('Ctrl Pts',(-14.5123006796728,71.4408717601923,0.));
#98867=CARTESIAN_POINT('Ctrl Pts',(-14.5263934312969,71.4622686107475,0.));
#98868=CARTESIAN_POINT('Ctrl Pts',(-14.540527729659,71.4836845794048,0.));
#98869=CARTESIAN_POINT('Ctrl Pts',(-14.5547035631234,71.5051195521909,0.));
#98870=CARTESIAN_POINT('Ctrl Pts',(-14.5689209200091,71.5265734155498,0.));
#98871=CARTESIAN_POINT('Ctrl Pts',(-14.5831797885952,71.5480460563447,0.));
#98872=CARTESIAN_POINT('Ctrl Pts',(-14.597480157121,71.5695373618562,0.));
#98873=CARTESIAN_POINT('Ctrl Pts',(-14.6118220137849,71.5910472197813,0.));
#98874=CARTESIAN_POINT('Ctrl Pts',(-14.626205346737,71.612575518229,0.));
#98875=CARTESIAN_POINT('Ctrl Pts',(-14.6406301440814,71.6341221457169,0.));
#98876=CARTESIAN_POINT('Ctrl Pts',(-14.6550963938829,71.6556869911662,0.));
#98877=CARTESIAN_POINT('Ctrl Pts',(-14.6696040841678,71.6772699438963,0.));
#98878=CARTESIAN_POINT('Ctrl Pts',(-14.6841532029232,71.6988708936172,0.));
#98879=CARTESIAN_POINT('Ctrl Pts',(-14.6987437380901,71.7204897304194,0.));
#98880=CARTESIAN_POINT('Ctrl Pts',(-14.7133756775626,71.7421263447719,0.));
#98881=CARTESIAN_POINT('Ctrl Pts',(-14.7280490091957,71.7637806275328,0.));
#98882=CARTESIAN_POINT('Ctrl Pts',(-14.7427637208073,71.7854524699569,0.));
#98883=CARTESIAN_POINT('Ctrl Pts',(-14.7575198001776,71.8071417637017,0.));
#98884=CARTESIAN_POINT('Ctrl Pts',(-14.7723172350451,71.8288484008333,0.));
#98885=CARTESIAN_POINT('Ctrl Pts',(-14.7871560131017,71.8505722738272,0.));
#98886=CARTESIAN_POINT('Ctrl Pts',(-14.8020361219998,71.8723132755446,0.));
#98887=CARTESIAN_POINT('Ctrl Pts',(-14.8169575493557,71.8940712992109,0.));
#98888=CARTESIAN_POINT('Ctrl Pts',(-14.8319202827482,71.9158462383914,0.));
#98889=CARTESIAN_POINT('Ctrl Pts',(-14.8469243097163,71.9376379869678,0.));
#98890=CARTESIAN_POINT('Ctrl Pts',(-14.8619696177506,71.9594464391078,0.));
#98891=CARTESIAN_POINT('Ctrl Pts',(-14.8770561943014,71.9812714893102,0.));
#98892=CARTESIAN_POINT('Ctrl Pts',(-14.8921840267832,72.0031130324529,0.));
#98893=CARTESIAN_POINT('Ctrl Pts',(-14.9073531025764,72.0249709638422,0.));
#98894=CARTESIAN_POINT('Ctrl Pts',(-14.9225634090268,72.0468451792505,0.));
#98895=CARTESIAN_POINT('Ctrl Pts',(-14.9378149334388,72.0687355749807,0.));
#98896=CARTESIAN_POINT('Ctrl Pts',(-14.9531076630768,72.0906420478076,0.));
#98897=CARTESIAN_POINT('Ctrl Pts',(-14.9684415851698,72.112564494854,0.));
#98898=CARTESIAN_POINT('Ctrl Pts',(-14.9838166869107,72.1345028134777,0.));
#98899=CARTESIAN_POINT('Ctrl Pts',(-14.9992329554537,72.1564569011669,0.));
#98900=CARTESIAN_POINT('Ctrl Pts',(-15.0146903779062,72.1784266553953,0.));
#98901=CARTESIAN_POINT('Ctrl Pts',(-15.0301889413257,72.2004119736115,0.));
#98902=CARTESIAN_POINT('Ctrl Pts',(-15.0457286327331,72.2224127535415,0.));
#98903=CARTESIAN_POINT('Ctrl Pts',(-15.0613094391189,72.2444288934262,0.));
#98904=CARTESIAN_POINT('Ctrl Pts',(-15.0769313474477,72.2664602922852,0.));
#98905=CARTESIAN_POINT('Ctrl Pts',(-15.092594344659,72.2885068501628,0.));
#98906=CARTESIAN_POINT('Ctrl Pts',(-15.1082984176649,72.3105684683944,0.));
#98907=CARTESIAN_POINT('Ctrl Pts',(-15.124043553347,72.3326450490177,0.));
#98908=CARTESIAN_POINT('Ctrl Pts',(-15.1398297385506,72.3547364941969,0.));
#98909=CARTESIAN_POINT('Ctrl Pts',(-15.1556569600745,72.376842705589,0.));
#98910=CARTESIAN_POINT('Ctrl Pts',(-15.1715252046606,72.3989635838492,0.));
#98911=CARTESIAN_POINT('Ctrl Pts',(-15.1874344589726,72.421099027786,0.));
#98912=CARTESIAN_POINT('Ctrl Pts',(-15.2033847096091,72.4432489350471,0.));
#98913=CARTESIAN_POINT('Ctrl Pts',(-15.2193759431373,72.4654132036428,0.));
#98914=CARTESIAN_POINT('Ctrl Pts',(-15.235408146116,72.4875917332762,0.));
#98915=CARTESIAN_POINT('Ctrl Pts',(-15.2514813051172,72.5097844266075,0.));
#98916=CARTESIAN_POINT('Ctrl Pts',(-15.2675954067479,72.5319911908917,0.));
#98917=CARTESIAN_POINT('Ctrl Pts',(-15.2837504376536,72.5542119383642,0.));
#98918=CARTESIAN_POINT('Ctrl Pts',(-15.297633502478,72.5732713370618,0.));
#98919=CARTESIAN_POINT('Ctrl Pts',(-15.3082994603539,72.5878912620439,0.));
#98920=CARTESIAN_POINT('Ctrl Pts',(-15.3157301930682,72.5980655789635,0.));
#98921=CARTESIAN_POINT('Ctrl Pts',(-15.3199137230129,72.6037902604921,0.));
#98922=CARTESIAN_POINT('Ctrl Pts',(-15.3208442077189,72.6050633494351,0.));
#98923=CARTESIAN_POINT('',(-12.9953224629497,68.7831490561748,12.));
#98924=CARTESIAN_POINT('',(-12.9953224629497,68.7831490561748,0.));
#98925=CARTESIAN_POINT('Ctrl Pts',(-15.320844207719,72.6050633494352,12.));
#98926=CARTESIAN_POINT('Ctrl Pts',(-15.319913723013,72.6037902604922,12.));
#98927=CARTESIAN_POINT('Ctrl Pts',(-15.3157301930682,72.5980655789636,12.));
#98928=CARTESIAN_POINT('Ctrl Pts',(-15.308299460354,72.5878912620439,12.));
#98929=CARTESIAN_POINT('Ctrl Pts',(-15.297633502478,72.5732713370618,12.));
#98930=CARTESIAN_POINT('Ctrl Pts',(-15.2837504376536,72.5542119383642,12.));
#98931=CARTESIAN_POINT('Ctrl Pts',(-15.2675954067479,72.5319911908917,12.));
#98932=CARTESIAN_POINT('Ctrl Pts',(-15.2514813051172,72.5097844266075,12.));
#98933=CARTESIAN_POINT('Ctrl Pts',(-15.235408146116,72.4875917332762,12.));
#98934=CARTESIAN_POINT('Ctrl Pts',(-15.2193759431373,72.4654132036428,12.));
#98935=CARTESIAN_POINT('Ctrl Pts',(-15.2033847096091,72.4432489350471,12.));
#98936=CARTESIAN_POINT('Ctrl Pts',(-15.1874344589726,72.421099027786,12.));
#98937=CARTESIAN_POINT('Ctrl Pts',(-15.1715252046606,72.3989635838492,12.));
#98938=CARTESIAN_POINT('Ctrl Pts',(-15.1556569600745,72.376842705589,12.));
#98939=CARTESIAN_POINT('Ctrl Pts',(-15.1398297385506,72.3547364941969,12.));
#98940=CARTESIAN_POINT('Ctrl Pts',(-15.124043553347,72.3326450490177,12.));
#98941=CARTESIAN_POINT('Ctrl Pts',(-15.1082984176649,72.3105684683944,12.));
#98942=CARTESIAN_POINT('Ctrl Pts',(-15.092594344659,72.2885068501628,12.));
#98943=CARTESIAN_POINT('Ctrl Pts',(-15.0769313474477,72.2664602922852,12.));
#98944=CARTESIAN_POINT('Ctrl Pts',(-15.0613094391189,72.2444288934262,12.));
#98945=CARTESIAN_POINT('Ctrl Pts',(-15.0457286327331,72.2224127535415,12.));
#98946=CARTESIAN_POINT('Ctrl Pts',(-15.0301889413257,72.2004119736115,12.));
#98947=CARTESIAN_POINT('Ctrl Pts',(-15.0146903779062,72.1784266553953,12.));
#98948=CARTESIAN_POINT('Ctrl Pts',(-14.9992329554537,72.1564569011669,12.));
#98949=CARTESIAN_POINT('Ctrl Pts',(-14.9838166869107,72.1345028134777,12.));
#98950=CARTESIAN_POINT('Ctrl Pts',(-14.9684415851698,72.112564494854,12.));
#98951=CARTESIAN_POINT('Ctrl Pts',(-14.9531076630768,72.0906420478076,12.));
#98952=CARTESIAN_POINT('Ctrl Pts',(-14.9378149334388,72.0687355749807,12.));
#98953=CARTESIAN_POINT('Ctrl Pts',(-14.9225634090268,72.0468451792505,12.));
#98954=CARTESIAN_POINT('Ctrl Pts',(-14.9073531025764,72.0249709638422,12.));
#98955=CARTESIAN_POINT('Ctrl Pts',(-14.8921840267832,72.0031130324529,12.));
#98956=CARTESIAN_POINT('Ctrl Pts',(-14.8770561943014,71.9812714893102,12.));
#98957=CARTESIAN_POINT('Ctrl Pts',(-14.8619696177506,71.9594464391078,12.));
#98958=CARTESIAN_POINT('Ctrl Pts',(-14.8469243097163,71.9376379869678,12.));
#98959=CARTESIAN_POINT('Ctrl Pts',(-14.8319202827482,71.9158462383914,12.));
#98960=CARTESIAN_POINT('Ctrl Pts',(-14.8169575493557,71.8940712992109,12.));
#98961=CARTESIAN_POINT('Ctrl Pts',(-14.8020361219998,71.8723132755446,12.));
#98962=CARTESIAN_POINT('Ctrl Pts',(-14.7871560131017,71.8505722738272,12.));
#98963=CARTESIAN_POINT('Ctrl Pts',(-14.7723172350451,71.8288484008333,12.));
#98964=CARTESIAN_POINT('Ctrl Pts',(-14.7575198001776,71.8071417637017,12.));
#98965=CARTESIAN_POINT('Ctrl Pts',(-14.7427637208073,71.7854524699569,12.));
#98966=CARTESIAN_POINT('Ctrl Pts',(-14.7280490091957,71.7637806275328,12.));
#98967=CARTESIAN_POINT('Ctrl Pts',(-14.7133756775626,71.7421263447719,12.));
#98968=CARTESIAN_POINT('Ctrl Pts',(-14.6987437380901,71.7204897304194,12.));
#98969=CARTESIAN_POINT('Ctrl Pts',(-14.6841532029232,71.6988708936172,12.));
#98970=CARTESIAN_POINT('Ctrl Pts',(-14.6696040841678,71.6772699438963,12.));
#98971=CARTESIAN_POINT('Ctrl Pts',(-14.6550963938829,71.6556869911662,12.));
#98972=CARTESIAN_POINT('Ctrl Pts',(-14.6406301440814,71.6341221457169,12.));
#98973=CARTESIAN_POINT('Ctrl Pts',(-14.626205346737,71.612575518229,12.));
#98974=CARTESIAN_POINT('Ctrl Pts',(-14.6118220137849,71.5910472197813,12.));
#98975=CARTESIAN_POINT('Ctrl Pts',(-14.597480157121,71.5695373618562,12.));
#98976=CARTESIAN_POINT('Ctrl Pts',(-14.5831797885952,71.5480460563447,12.));
#98977=CARTESIAN_POINT('Ctrl Pts',(-14.5689209200091,71.5265734155498,12.));
#98978=CARTESIAN_POINT('Ctrl Pts',(-14.5547035631234,71.5051195521909,12.));
#98979=CARTESIAN_POINT('Ctrl Pts',(-14.540527729659,71.4836845794048,12.));
#98980=CARTESIAN_POINT('Ctrl Pts',(-14.5263934312969,71.4622686107475,12.));
#98981=CARTESIAN_POINT('Ctrl Pts',(-14.5123006796728,71.4408717601923,12.));
#98982=CARTESIAN_POINT('Ctrl Pts',(-14.4982494863718,71.4194941421292,12.));
#98983=CARTESIAN_POINT('Ctrl Pts',(-14.4842398629355,71.3981358713723,12.));
#98984=CARTESIAN_POINT('Ctrl Pts',(-14.4702718208651,71.376797063165,12.));
#98985=CARTESIAN_POINT('Ctrl Pts',(-14.4563453716204,71.3554778331835,12.));
#98986=CARTESIAN_POINT('Ctrl Pts',(-14.4424605266165,71.3341782975386,12.));
#98987=CARTESIAN_POINT('Ctrl Pts',(-14.4286172972167,71.312898572777,12.));
#98988=CARTESIAN_POINT('Ctrl Pts',(-14.4148156947384,71.2916387758861,12.));
#98989=CARTESIAN_POINT('Ctrl Pts',(-14.401055730457,71.2703990242988,12.));
#98990=CARTESIAN_POINT('Ctrl Pts',(-14.3873374156056,71.2491794358958,12.));
#98991=CARTESIAN_POINT('Ctrl Pts',(-14.3736607613722,71.2279801290084,12.));
#98992=CARTESIAN_POINT('Ctrl Pts',(-14.3600257788924,71.2068012224174,12.));
#98993=CARTESIAN_POINT('Ctrl Pts',(-14.3464324792534,71.1856428353593,12.));
#98994=CARTESIAN_POINT('Ctrl Pts',(-14.332880873499,71.1645050875308,12.));
#98995=CARTESIAN_POINT('Ctrl Pts',(-14.3193709726294,71.1433880990929,12.));
#98996=CARTESIAN_POINT('Ctrl Pts',(-14.3059027875994,71.1222919906727,12.));
#98997=CARTESIAN_POINT('Ctrl Pts',(-14.2924763293105,71.1012168833643,12.));
#98998=CARTESIAN_POINT('Ctrl Pts',(-14.2790916086133,71.0801628987332,12.));
#98999=CARTESIAN_POINT('Ctrl Pts',(-14.2657486363139,71.0591301588231,12.));
#99000=CARTESIAN_POINT('Ctrl Pts',(-14.2524474231733,71.0381187861588,12.));
#99001=CARTESIAN_POINT('Ctrl Pts',(-14.2391879799062,71.0171289037488,12.));
#99002=CARTESIAN_POINT('Ctrl Pts',(-14.2259703171737,70.9961606350861,12.));
#99003=CARTESIAN_POINT('Ctrl Pts',(-14.2127944455839,70.9752141041518,12.));
#99004=CARTESIAN_POINT('Ctrl Pts',(-14.1996603756982,70.9542894354216,12.));
#99005=CARTESIAN_POINT('Ctrl Pts',(-14.1865681180321,70.9333867538704,12.));
#99006=CARTESIAN_POINT('Ctrl Pts',(-14.1735176830533,70.9125061849745,12.));
#99007=CARTESIAN_POINT('Ctrl Pts',(-14.1605090811754,70.8916478547132,12.));
#99008=CARTESIAN_POINT('Ctrl Pts',(-14.1475423227568,70.8708118895715,12.));
#99009=CARTESIAN_POINT('Ctrl Pts',(-14.1346174181079,70.8499984165489,12.));
#99010=CARTESIAN_POINT('Ctrl Pts',(-14.1217343774913,70.8292075631621,12.));
#99011=CARTESIAN_POINT('Ctrl Pts',(-14.1088932111214,70.8084394574493,12.));
#99012=CARTESIAN_POINT('Ctrl Pts',(-14.0960939291569,70.7876942279697,12.));
#99013=CARTESIAN_POINT('Ctrl Pts',(-14.0833365416996,70.7669720038077,12.));
#99014=CARTESIAN_POINT('Ctrl Pts',(-14.0706210588016,70.7462729145807,12.));
#99015=CARTESIAN_POINT('Ctrl Pts',(-14.0579474904657,70.7255970904436,12.));
#99016=CARTESIAN_POINT('Ctrl Pts',(-14.0453158466451,70.7049446620928,12.));
#99017=CARTESIAN_POINT('Ctrl Pts',(-14.0327261372362,70.6843157607668,12.));
#99018=CARTESIAN_POINT('Ctrl Pts',(-14.020178372077,70.6637105182484,12.));
#99019=CARTESIAN_POINT('Ctrl Pts',(-14.0076725609537,70.6431290668745,12.));
#99020=CARTESIAN_POINT('Ctrl Pts',(-13.9952087136018,70.6225715395394,12.));
#99021=CARTESIAN_POINT('Ctrl Pts',(-13.9827868397057,70.6020380697005,12.));
#99022=CARTESIAN_POINT('Ctrl Pts',(-13.9704069488917,70.5815287913784,12.));
#99023=CARTESIAN_POINT('Ctrl Pts',(-13.958069050726,70.5610438391612,12.));
#99024=CARTESIAN_POINT('Ctrl Pts',(-13.9457731547215,70.5405833482112,12.));
#99025=CARTESIAN_POINT('Ctrl Pts',(-13.9335192703388,70.520147454271,12.));
#99026=CARTESIAN_POINT('Ctrl Pts',(-13.9213074069853,70.4997362936673,12.));
#99027=CARTESIAN_POINT('Ctrl Pts',(-13.9091375740088,70.4793500033124,12.));
#99028=CARTESIAN_POINT('Ctrl Pts',(-13.8970097806954,70.4589887207073,12.));
#99029=CARTESIAN_POINT('Ctrl Pts',(-13.8849240362763,70.4386525839521,12.));
#99030=CARTESIAN_POINT('Ctrl Pts',(-13.8728803499287,70.41834173175,12.));
#99031=CARTESIAN_POINT('Ctrl Pts',(-13.8608787307752,70.3980563034133,12.));
#99032=CARTESIAN_POINT('Ctrl Pts',(-13.8489191878767,70.3777964388632,12.));
#99033=CARTESIAN_POINT('Ctrl Pts',(-13.8370017302309,70.3575622786335,12.));
#99034=CARTESIAN_POINT('Ctrl Pts',(-13.8251263667791,70.3373539638809,12.));
#99035=CARTESIAN_POINT('Ctrl Pts',(-13.8132931064064,70.3171716363897,12.));
#99036=CARTESIAN_POINT('Ctrl Pts',(-13.8015019579414,70.2970154385774,12.));
#99037=CARTESIAN_POINT('Ctrl Pts',(-13.7897529301491,70.2768855134947,12.));
#99038=CARTESIAN_POINT('Ctrl Pts',(-13.7780460317294,70.2567820048303,12.));
#99039=CARTESIAN_POINT('Ctrl Pts',(-13.7663812713243,70.2367050569216,12.));
#99040=CARTESIAN_POINT('Ctrl Pts',(-13.7547586575181,70.2166548147604,12.));
#99041=CARTESIAN_POINT('Ctrl Pts',(-13.7431781988365,70.1966314239995,12.));
#99042=CARTESIAN_POINT('Ctrl Pts',(-13.7316399037393,70.1766350309518,12.));
#99043=CARTESIAN_POINT('Ctrl Pts',(-13.7201437806199,70.156665782595,12.));
#99044=CARTESIAN_POINT('Ctrl Pts',(-13.7086898378122,70.1367238265825,12.));
#99045=CARTESIAN_POINT('Ctrl Pts',(-13.6972780835897,70.1168093112486,12.));
#99046=CARTESIAN_POINT('Ctrl Pts',(-13.6859085261653,70.0969223856136,12.));
#99047=CARTESIAN_POINT('Ctrl Pts',(-13.674581173683,70.0770631993856,12.));
#99048=CARTESIAN_POINT('Ctrl Pts',(-13.6632960342196,70.0572319029676,12.));
#99049=CARTESIAN_POINT('Ctrl Pts',(-13.6520531157907,70.0374286474677,12.));
#99050=CARTESIAN_POINT('Ctrl Pts',(-13.6408524263496,70.0176535847049,12.));
#99051=CARTESIAN_POINT('Ctrl Pts',(-13.6296939737865,69.9979068672153,12.));
#99052=CARTESIAN_POINT('Ctrl Pts',(-13.6185777659198,69.9781886482528,12.));
#99053=CARTESIAN_POINT('Ctrl Pts',(-13.6075038104999,69.9584990817974,12.));
#99054=CARTESIAN_POINT('Ctrl Pts',(-13.5964721152135,69.9388383225648,12.));
#99055=CARTESIAN_POINT('Ctrl Pts',(-13.5854826876835,69.9192065260108,12.));
#99056=CARTESIAN_POINT('Ctrl Pts',(-13.5745355354657,69.8996038483361,12.));
#99057=CARTESIAN_POINT('Ctrl Pts',(-13.5636306660422,69.8800304464882,12.));
#99058=CARTESIAN_POINT('Ctrl Pts',(-13.5527680868255,69.8604864781706,12.));
#99059=CARTESIAN_POINT('Ctrl Pts',(-13.5419478051625,69.840972101856,12.));
#99060=CARTESIAN_POINT('Ctrl Pts',(-13.5311698283339,69.8214874767944,12.));
#99061=CARTESIAN_POINT('Ctrl Pts',(-13.5204341635507,69.8020327630205,12.));
#99062=CARTESIAN_POINT('Ctrl Pts',(-13.5097408179479,69.7826081213576,12.));
#99063=CARTESIAN_POINT('Ctrl Pts',(-13.4990897985905,69.7632137134249,12.));
#99064=CARTESIAN_POINT('Ctrl Pts',(-13.4884811124748,69.7438497016406,12.));
#99065=CARTESIAN_POINT('Ctrl Pts',(-13.4779147665285,69.724516249225,12.));
#99066=CARTESIAN_POINT('Ctrl Pts',(-13.4673907676044,69.7052135201998,12.));
#99067=CARTESIAN_POINT('Ctrl Pts',(-13.456909122476,69.6859416793885,12.));
#99068=CARTESIAN_POINT('Ctrl Pts',(-13.4464698378453,69.666700892444,12.));
#99069=CARTESIAN_POINT('Ctrl Pts',(-13.4360729203442,69.6474913258675,12.));
#99070=CARTESIAN_POINT('Ctrl Pts',(-13.4257183765341,69.6283131470273,12.));
#99071=CARTESIAN_POINT('Ctrl Pts',(-13.4154062129002,69.6091665241765,12.));
#99072=CARTESIAN_POINT('Ctrl Pts',(-13.40513643585,69.5900516264553,12.));
#99073=CARTESIAN_POINT('Ctrl Pts',(-13.3949090517177,69.5709686238724,12.));
#99074=CARTESIAN_POINT('Ctrl Pts',(-13.3847240667628,69.5519176872862,12.));
#99075=CARTESIAN_POINT('Ctrl Pts',(-13.3745814871665,69.5328989883885,12.));
#99076=CARTESIAN_POINT('Ctrl Pts',(-13.3644813190219,69.5139126996675,12.));
#99077=CARTESIAN_POINT('Ctrl Pts',(-13.3544235683394,69.4949589944606,12.));
#99078=CARTESIAN_POINT('Ctrl Pts',(-13.3444082410543,69.4760380470365,12.));
#99079=CARTESIAN_POINT('Ctrl Pts',(-13.3344353430313,69.4571500326673,12.));
#99080=CARTESIAN_POINT('Ctrl Pts',(-13.3245048800643,69.4382951276998,12.));
#99081=CARTESIAN_POINT('Ctrl Pts',(-13.3146168578743,69.4194735096265,12.));
#99082=CARTESIAN_POINT('Ctrl Pts',(-13.3047712821051,69.4006853569511,12.));
#99083=CARTESIAN_POINT('Ctrl Pts',(-13.2949681583167,69.3819308490422,12.));
#99084=CARTESIAN_POINT('Ctrl Pts',(-13.2852074919766,69.3632101660066,12.));
#99085=CARTESIAN_POINT('Ctrl Pts',(-13.2754892884433,69.3445234885065,12.));
#99086=CARTESIAN_POINT('Ctrl Pts',(-13.265813552961,69.3258709977382,12.));
#99087=CARTESIAN_POINT('Ctrl Pts',(-13.2561802906896,69.3072528758518,12.));
#99088=CARTESIAN_POINT('Ctrl Pts',(-13.2465895067262,69.2886693063182,12.));
#99089=CARTESIAN_POINT('Ctrl Pts',(-13.237041206122,69.270120474245,12.));
#99090=CARTESIAN_POINT('Ctrl Pts',(-13.2275353939051,69.2516065668844,12.));
#99091=CARTESIAN_POINT('Ctrl Pts',(-13.2180720750594,69.2331277732861,12.));
#99092=CARTESIAN_POINT('Ctrl Pts',(-13.2086512544735,69.2146842833537,12.));
#99093=CARTESIAN_POINT('Ctrl Pts',(-13.1992729368928,69.1962762870527,12.));
#99094=CARTESIAN_POINT('Ctrl Pts',(-13.1899371268683,69.1779039735996,12.));
#99095=CARTESIAN_POINT('Ctrl Pts',(-13.1806438286934,69.1595675305245,12.));
#99096=CARTESIAN_POINT('Ctrl Pts',(-13.1713930465133,69.1412671454564,12.));
#99097=CARTESIAN_POINT('Ctrl Pts',(-13.1621847844528,69.1230030082573,12.));
#99098=CARTESIAN_POINT('Ctrl Pts',(-13.1530190467183,69.1047753127643,12.));
#99099=CARTESIAN_POINT('Ctrl Pts',(-13.1438958377404,69.0865842593102,12.));
#99100=CARTESIAN_POINT('Ctrl Pts',(-13.1348151621834,69.0684300549477,12.));
#99101=CARTESIAN_POINT('Ctrl Pts',(-13.1257770246385,69.0503129081817,12.));
#99102=CARTESIAN_POINT('Ctrl Pts',(-13.1167814293497,69.0322330243348,12.));
#99103=CARTESIAN_POINT('Ctrl Pts',(-13.1078283799722,69.0141906015113,12.));
#99104=CARTESIAN_POINT('Ctrl Pts',(-13.0989178791834,68.9961858241519,12.));
#99105=CARTESIAN_POINT('Ctrl Pts',(-13.090049929053,68.9782188692581,12.));
#99106=CARTESIAN_POINT('Ctrl Pts',(-13.0812245317808,68.9602899187573,12.));
#99107=CARTESIAN_POINT('Ctrl Pts',(-13.072441690283,68.9423991694492,12.));
#99108=CARTESIAN_POINT('Ctrl Pts',(-13.0637014089029,68.9245468449945,12.));
#99109=CARTESIAN_POINT('Ctrl Pts',(-13.0550036938813,68.9067332040985,12.));
#99110=CARTESIAN_POINT('Ctrl Pts',(-13.0463485518207,68.8889585151585,12.));
#99111=CARTESIAN_POINT('Ctrl Pts',(-13.0377359881875,68.8712230321906,12.));
#99112=CARTESIAN_POINT('Ctrl Pts',(-13.0291660060107,68.8535269726794,12.));
#99113=CARTESIAN_POINT('Ctrl Pts',(-13.0206386039691,68.8358704887468,12.));
#99114=CARTESIAN_POINT('Ctrl Pts',(-13.0121537768946,68.8182536653656,12.));
#99115=CARTESIAN_POINT('Ctrl Pts',(-13.0053999700875,68.804191966902,12.));
#99116=CARTESIAN_POINT('Ctrl Pts',(-13.0003537683055,68.7936635625545,12.));
#99117=CARTESIAN_POINT('Ctrl Pts',(-12.9969981460277,68.7866525680193,12.));
#99118=CARTESIAN_POINT('Ctrl Pts',(-12.9953224629497,68.7831490561748,12.));
#99119=CARTESIAN_POINT('Ctrl Pts',(-16.7988252568748,72.2774028393914,0.));
#99120=CARTESIAN_POINT('Ctrl Pts',(-16.7988252568748,72.2774028393914,4.));
#99121=CARTESIAN_POINT('Ctrl Pts',(-16.7988252568748,72.2774028393914,8.));
#99122=CARTESIAN_POINT('Ctrl Pts',(-16.7988252568748,72.2774028393914,12.));
#99123=CARTESIAN_POINT('Ctrl Pts',(-16.7775526720894,72.3852065198825,0.));
#99124=CARTESIAN_POINT('Ctrl Pts',(-16.7775526720894,72.3852065198825,4.));
#99125=CARTESIAN_POINT('Ctrl Pts',(-16.7775526720894,72.3852065198825,8.));
#99126=CARTESIAN_POINT('Ctrl Pts',(-16.7775526720894,72.3852065198825,12.));
#99127=CARTESIAN_POINT('Ctrl Pts',(-16.6758649025559,72.5605133546289,0.));
#99128=CARTESIAN_POINT('Ctrl Pts',(-16.6758649025559,72.5605133546289,4.00000000000001));
#99129=CARTESIAN_POINT('Ctrl Pts',(-16.6758649025559,72.5605133546289,7.99999999999999));
#99130=CARTESIAN_POINT('Ctrl Pts',(-16.6758649025559,72.5605133546289,12.));
#99131=CARTESIAN_POINT('Ctrl Pts',(-16.4988611391808,72.6501505354462,0.));
#99132=CARTESIAN_POINT('Ctrl Pts',(-16.4988611391808,72.6501505354462,3.99999999999999));
#99133=CARTESIAN_POINT('Ctrl Pts',(-16.4988611391808,72.6501505354462,8.00000000000001));
#99134=CARTESIAN_POINT('Ctrl Pts',(-16.4988611391808,72.6501505354462,12.));
#99135=CARTESIAN_POINT('Ctrl Pts',(-16.4184755008061,72.6683126419585,0.));
#99136=CARTESIAN_POINT('Ctrl Pts',(-16.4184755008061,72.6683126419585,4.));
#99137=CARTESIAN_POINT('Ctrl Pts',(-16.4184755008061,72.6683126419585,8.));
#99138=CARTESIAN_POINT('Ctrl Pts',(-16.4184755008061,72.6683126419585,12.));
#99139=CARTESIAN_POINT('',(-16.7988252568748,72.2774028393914,0.));
#99140=CARTESIAN_POINT('',(-16.4184755008061,72.6683126419586,0.));
#99141=CARTESIAN_POINT('Ctrl Pts',(-16.7988252568748,72.2774028393914,2.03133674691991E-34));
#99142=CARTESIAN_POINT('Ctrl Pts',(-16.7775526720894,72.3852065198825,2.03133674691991E-34));
#99143=CARTESIAN_POINT('Ctrl Pts',(-16.7194453752131,72.4853818540233,2.03133674691991E-34));
#99144=CARTESIAN_POINT('Ctrl Pts',(-16.6367451007559,72.5575834236158,2.03133674691991E-34));
#99145=CARTESIAN_POINT('Ctrl Pts',(-16.574719894913,72.6117346008102,2.03133674691991E-34));
#99146=CARTESIAN_POINT('Ctrl Pts',(-16.4988611391808,72.6501505354462,2.03133674691991E-34));
#99147=CARTESIAN_POINT('Ctrl Pts',(-16.4184755008061,72.6683126419585,2.03133674691991E-34));
#99148=CARTESIAN_POINT('',(-16.4184755008061,72.6683126419586,12.));
#99149=CARTESIAN_POINT('Ctrl Pts',(-16.4184755008061,72.6683126419585,0.));
#99150=CARTESIAN_POINT('Ctrl Pts',(-16.4184755008061,72.6683126419585,4.));
#99151=CARTESIAN_POINT('Ctrl Pts',(-16.4184755008061,72.6683126419585,8.));
#99152=CARTESIAN_POINT('Ctrl Pts',(-16.4184755008061,72.6683126419585,12.));
#99153=CARTESIAN_POINT('',(-16.7988252568748,72.2774028393914,12.));
#99154=CARTESIAN_POINT('Ctrl Pts',(-16.4184755008061,72.6683126419585,12.));
#99155=CARTESIAN_POINT('Ctrl Pts',(-16.4988611391808,72.6501505354462,12.));
#99156=CARTESIAN_POINT('Ctrl Pts',(-16.574719894913,72.6117346008102,12.));
#99157=CARTESIAN_POINT('Ctrl Pts',(-16.6367451007559,72.5575834236158,12.));
#99158=CARTESIAN_POINT('Ctrl Pts',(-16.7194453752131,72.4853818540233,12.));
#99159=CARTESIAN_POINT('Ctrl Pts',(-16.7775526720894,72.3852065198825,12.));
#99160=CARTESIAN_POINT('Ctrl Pts',(-16.7988252568748,72.2774028393914,12.));
#99161=CARTESIAN_POINT('Ctrl Pts',(-16.7988252568748,72.2774028393914,12.));
#99162=CARTESIAN_POINT('Ctrl Pts',(-16.7988252568748,72.2774028393914,8.));
#99163=CARTESIAN_POINT('Ctrl Pts',(-16.7988252568748,72.2774028393914,4.));
#99164=CARTESIAN_POINT('Ctrl Pts',(-16.7988252568748,72.2774028393914,0.));
#99165=CARTESIAN_POINT('Origin',(-8.12279454723526E-11,3.65936987487134E-10,
0.));
#99166=CARTESIAN_POINT('Origin',(-8.12279454723526E-11,3.65936987487134E-10,
12.));
#99167=CARTESIAN_POINT('Origin',(-8.12279454723526E-11,3.65936987487134E-10,
0.));
#99168=CARTESIAN_POINT('Ctrl Pts',(-9.42570643237823,73.9013264985861,5.55111512312578E-16));
#99169=CARTESIAN_POINT('Ctrl Pts',(-9.42570643237823,73.9013264985861,4.));
#99170=CARTESIAN_POINT('Ctrl Pts',(-9.42570643237823,73.9013264985861,8.));
#99171=CARTESIAN_POINT('Ctrl Pts',(-9.42570643237823,73.9013264985861,12.));
#99172=CARTESIAN_POINT('Ctrl Pts',(-9.31670696907609,73.9152287787081,5.55111512312578E-16));
#99173=CARTESIAN_POINT('Ctrl Pts',(-9.31670696907609,73.9152287787081,4.));
#99174=CARTESIAN_POINT('Ctrl Pts',(-9.31670696907609,73.9152287787081,8.00000000000001));
#99175=CARTESIAN_POINT('Ctrl Pts',(-9.31670696907609,73.9152287787081,12.));
#99176=CARTESIAN_POINT('Ctrl Pts',(-9.11824194722539,73.8741839722667,4.82031436765098E-16));
#99177=CARTESIAN_POINT('Ctrl Pts',(-9.11824194722539,73.8741839722667,4.00000000000001));
#99178=CARTESIAN_POINT('Ctrl Pts',(-9.11824194722539,73.8741839722667,7.99999999999999));
#99179=CARTESIAN_POINT('Ctrl Pts',(-9.11824194722539,73.8741839722667,12.));
#99180=CARTESIAN_POINT('Ctrl Pts',(-8.9772410874556,73.7345987226918,3.08500332079893E-16));
#99181=CARTESIAN_POINT('Ctrl Pts',(-8.9772410874556,73.7345987226918,4.));
#99182=CARTESIAN_POINT('Ctrl Pts',(-8.9772410874556,73.7345987226918,8.00000000000001));
#99183=CARTESIAN_POINT('Ctrl Pts',(-8.9772410874556,73.7345987226918,12.));
#99184=CARTESIAN_POINT('Ctrl Pts',(-8.93459554655819,73.6640787197672,2.24846351842411E-16));
#99185=CARTESIAN_POINT('Ctrl Pts',(-8.93459554655819,73.6640787197672,4.));
#99186=CARTESIAN_POINT('Ctrl Pts',(-8.93459554655819,73.6640787197672,8.));
#99187=CARTESIAN_POINT('Ctrl Pts',(-8.93459554655819,73.6640787197672,12.));
#99188=CARTESIAN_POINT('',(-9.42570643237823,73.9013264985861,2.77555756156289E-16));
#99189=CARTESIAN_POINT('',(-8.93459554655823,73.6640787197672,0.));
#99190=CARTESIAN_POINT('Ctrl Pts',(-9.42570643237823,73.9013264985861,5.82554064063016E-16));
#99191=CARTESIAN_POINT('Ctrl Pts',(-9.31670696907609,73.9152287787081,5.82554064063016E-16));
#99192=CARTESIAN_POINT('Ctrl Pts',(-9.20329838516141,73.8917746035987,5.40794020893028E-16));
#99193=CARTESIAN_POINT('Ctrl Pts',(-9.10865360927314,73.8361439572621,4.66233641678068E-16));
#99194=CARTESIAN_POINT('Ctrl Pts',(-9.03767002735694,73.7944209725096,4.10313357266848E-16));
#99195=CARTESIAN_POINT('Ctrl Pts',(-8.9772410874556,73.7345987226918,3.35942883830331E-16));
#99196=CARTESIAN_POINT('Ctrl Pts',(-8.93459554655819,73.6640787197672,2.5228890359285E-16));
#99197=CARTESIAN_POINT('',(-8.93459554655823,73.6640787197672,12.));
#99198=CARTESIAN_POINT('Ctrl Pts',(-8.93459554655819,73.6640787197672,2.24846351842411E-16));
#99199=CARTESIAN_POINT('Ctrl Pts',(-8.93459554655819,73.6640787197672,4.));
#99200=CARTESIAN_POINT('Ctrl Pts',(-8.93459554655819,73.6640787197672,8.));
#99201=CARTESIAN_POINT('Ctrl Pts',(-8.93459554655819,73.6640787197672,12.));
#99202=CARTESIAN_POINT('',(-9.42570643237823,73.9013264985861,12.));
#99203=CARTESIAN_POINT('Ctrl Pts',(-8.93459554655819,73.6640787197672,12.));
#99204=CARTESIAN_POINT('Ctrl Pts',(-8.9772410874556,73.7345987226918,12.));
#99205=CARTESIAN_POINT('Ctrl Pts',(-9.03767002735694,73.7944209725096,12.));
#99206=CARTESIAN_POINT('Ctrl Pts',(-9.10865360927314,73.8361439572621,12.));
#99207=CARTESIAN_POINT('Ctrl Pts',(-9.20329838516141,73.8917746035987,12.));
#99208=CARTESIAN_POINT('Ctrl Pts',(-9.31670696907609,73.9152287787081,12.));
#99209=CARTESIAN_POINT('Ctrl Pts',(-9.42570643237823,73.9013264985861,12.));
#99210=CARTESIAN_POINT('Ctrl Pts',(-9.42570643237823,73.9013264985861,12.));
#99211=CARTESIAN_POINT('Ctrl Pts',(-9.42570643237823,73.9013264985861,8.));
#99212=CARTESIAN_POINT('Ctrl Pts',(-9.42570643237823,73.9013264985861,4.));
#99213=CARTESIAN_POINT('Ctrl Pts',(-9.42570643237823,73.9013264985861,5.55111512312578E-16));
#99214=CARTESIAN_POINT('Ctrl Pts',(-6.95102489306926,69.6540253893192,0.));
#99215=CARTESIAN_POINT('Ctrl Pts',(-6.95102489306926,69.6540253893192,12.));
#99216=CARTESIAN_POINT('Ctrl Pts',(-6.95238884849025,69.6576616146467,0.));
#99217=CARTESIAN_POINT('Ctrl Pts',(-6.95238884849025,69.6576616146467,12.));
#99218=CARTESIAN_POINT('Ctrl Pts',(-6.955120653176,69.664938391983,0.));
#99219=CARTESIAN_POINT('Ctrl Pts',(-6.955120653176,69.664938391983,12.));
#99220=CARTESIAN_POINT('Ctrl Pts',(-6.95923004173591,69.6758665380378,0.));
#99221=CARTESIAN_POINT('Ctrl Pts',(-6.95923004173591,69.6758665380378,12.));
#99222=CARTESIAN_POINT('Ctrl Pts',(-6.96473259049513,69.6904633605421,0.));
#99223=CARTESIAN_POINT('Ctrl Pts',(-6.96473259049513,69.6904633605421,12.));
#99224=CARTESIAN_POINT('Ctrl Pts',(-6.9716497229144,69.7087526479973,0.));
#99225=CARTESIAN_POINT('Ctrl Pts',(-6.9716497229144,69.7087526479973,12.));
#99226=CARTESIAN_POINT('Ctrl Pts',(-6.97860581164527,69.7270851557366,0.));
#99227=CARTESIAN_POINT('Ctrl Pts',(-6.97860581164527,69.7270851557366,12.));
#99228=CARTESIAN_POINT('Ctrl Pts',(-6.98560086924214,69.7454607995607,0.));
#99229=CARTESIAN_POINT('Ctrl Pts',(-6.98560086924214,69.7454607995607,12.));
#99230=CARTESIAN_POINT('Ctrl Pts',(-6.9926349102794,69.7638794280419,0.));
#99231=CARTESIAN_POINT('Ctrl Pts',(-6.9926349102794,69.7638794280419,12.));
#99232=CARTESIAN_POINT('Ctrl Pts',(-6.99970795069476,69.782340824259,0.));
#99233=CARTESIAN_POINT('Ctrl Pts',(-6.99970795069476,69.782340824259,12.));
#99234=CARTESIAN_POINT('Ctrl Pts',(-7.00682000718151,69.8008447346863,0.));
#99235=CARTESIAN_POINT('Ctrl Pts',(-7.00682000718151,69.8008447346863,12.));
#99236=CARTESIAN_POINT('Ctrl Pts',(-7.01397109655455,69.8193908913722,0.));
#99237=CARTESIAN_POINT('Ctrl Pts',(-7.01397109655455,69.8193908913722,12.));
#99238=CARTESIAN_POINT('Ctrl Pts',(-7.02116123514452,69.8379790360518,0.));
#99239=CARTESIAN_POINT('Ctrl Pts',(-7.02116123514452,69.8379790360518,12.));
#99240=CARTESIAN_POINT('Ctrl Pts',(-7.02839043811812,69.8566089455375,0.));
#99241=CARTESIAN_POINT('Ctrl Pts',(-7.02839043811812,69.8566089455375,12.));
#99242=CARTESIAN_POINT('Ctrl Pts',(-7.03565871972221,69.8752804235238,0.));
#99243=CARTESIAN_POINT('Ctrl Pts',(-7.03565871972221,69.8752804235238,12.));
#99244=CARTESIAN_POINT('Ctrl Pts',(-7.04296609362166,69.8939932885841,0.));
#99245=CARTESIAN_POINT('Ctrl Pts',(-7.04296609362166,69.8939932885841,12.));
#99246=CARTESIAN_POINT('Ctrl Pts',(-7.05031257318115,69.9127473642099,0.));
#99247=CARTESIAN_POINT('Ctrl Pts',(-7.05031257318115,69.9127473642099,12.));
#99248=CARTESIAN_POINT('Ctrl Pts',(-7.05769817180857,69.9315424664291,0.));
#99249=CARTESIAN_POINT('Ctrl Pts',(-7.05769817180857,69.9315424664291,12.));
#99250=CARTESIAN_POINT('Ctrl Pts',(-7.0651229031285,69.9503783975727,0.));
#99251=CARTESIAN_POINT('Ctrl Pts',(-7.0651229031285,69.9503783975727,12.));
#99252=CARTESIAN_POINT('Ctrl Pts',(-7.07258678080831,69.9692549527296,0.));
#99253=CARTESIAN_POINT('Ctrl Pts',(-7.07258678080831,69.9692549527296,12.));
#99254=CARTESIAN_POINT('Ctrl Pts',(-7.08008981844652,69.988171923788,0.));
#99255=CARTESIAN_POINT('Ctrl Pts',(-7.08008981844652,69.988171923788,12.));
#99256=CARTESIAN_POINT('Ctrl Pts',(-7.08763202944246,70.0071291040766,0.));
#99257=CARTESIAN_POINT('Ctrl Pts',(-7.08763202944246,70.0071291040766,12.));
#99258=CARTESIAN_POINT('Ctrl Pts',(-7.09521342684249,70.0261262936388,0.));
#99259=CARTESIAN_POINT('Ctrl Pts',(-7.09521342684249,70.0261262936388,12.));
#99260=CARTESIAN_POINT('Ctrl Pts',(-7.10283402335034,70.0451632990086,0.));
#99261=CARTESIAN_POINT('Ctrl Pts',(-7.10283402335034,70.0451632990086,12.));
#99262=CARTESIAN_POINT('Ctrl Pts',(-7.11049383140446,70.0642399306869,0.));
#99263=CARTESIAN_POINT('Ctrl Pts',(-7.11049383140446,70.0642399306869,12.));
#99264=CARTESIAN_POINT('Ctrl Pts',(-7.11819286322826,70.0833560013975,0.));
#99265=CARTESIAN_POINT('Ctrl Pts',(-7.11819286322826,70.0833560013975,12.));
#99266=CARTESIAN_POINT('Ctrl Pts',(-7.12593113088904,70.1025113239495,0.));
#99267=CARTESIAN_POINT('Ctrl Pts',(-7.12593113088904,70.1025113239495,12.));
#99268=CARTESIAN_POINT('Ctrl Pts',(-7.13370864634442,70.1217057094499,0.));
#99269=CARTESIAN_POINT('Ctrl Pts',(-7.13370864634442,70.1217057094499,12.));
#99270=CARTESIAN_POINT('Ctrl Pts',(-7.14152542142374,70.1409389682424,0.));
#99271=CARTESIAN_POINT('Ctrl Pts',(-7.14152542142374,70.1409389682424,12.));
#99272=CARTESIAN_POINT('Ctrl Pts',(-7.14938146780813,70.1602109107202,0.));
#99273=CARTESIAN_POINT('Ctrl Pts',(-7.14938146780813,70.1602109107202,12.));
#99274=CARTESIAN_POINT('Ctrl Pts',(-7.15727679700933,70.1795213481185,0.));
#99275=CARTESIAN_POINT('Ctrl Pts',(-7.15727679700933,70.1795213481185,12.));
#99276=CARTESIAN_POINT('Ctrl Pts',(-7.16521142033864,70.1988700934593,0.));
#99277=CARTESIAN_POINT('Ctrl Pts',(-7.16521142033864,70.1988700934593,12.));
#99278=CARTESIAN_POINT('Ctrl Pts',(-7.17318534889716,70.2182569618994,0.));
#99279=CARTESIAN_POINT('Ctrl Pts',(-7.17318534889716,70.2182569618994,12.));
#99280=CARTESIAN_POINT('Ctrl Pts',(-7.18119859359778,70.2376817702215,0.));
#99281=CARTESIAN_POINT('Ctrl Pts',(-7.18119859359778,70.2376817702215,12.));
#99282=CARTESIAN_POINT('Ctrl Pts',(-7.18925116517555,70.2571443365192,0.));
#99283=CARTESIAN_POINT('Ctrl Pts',(-7.18925116517555,70.2571443365192,12.));
#99284=CARTESIAN_POINT('Ctrl Pts',(-7.19734307419873,70.2766444798285,0.));
#99285=CARTESIAN_POINT('Ctrl Pts',(-7.19734307419873,70.2766444798285,12.));
#99286=CARTESIAN_POINT('Ctrl Pts',(-7.20547433107483,70.2961820197077,0.));
#99287=CARTESIAN_POINT('Ctrl Pts',(-7.20547433107483,70.2961820197077,12.));
#99288=CARTESIAN_POINT('Ctrl Pts',(-7.2136449460545,70.3157567762588,0.));
#99289=CARTESIAN_POINT('Ctrl Pts',(-7.2136449460545,70.3157567762588,12.));
#99290=CARTESIAN_POINT('Ctrl Pts',(-7.22185492923191,70.3353685703112,0.));
#99291=CARTESIAN_POINT('Ctrl Pts',(-7.22185492923191,70.3353685703112,12.));
#99292=CARTESIAN_POINT('Ctrl Pts',(-7.23010429054229,70.3550172235486,0.));
#99293=CARTESIAN_POINT('Ctrl Pts',(-7.23010429054229,70.3550172235486,12.));
#99294=CARTESIAN_POINT('Ctrl Pts',(-7.23839303975607,70.3747025586552,0.));
#99295=CARTESIAN_POINT('Ctrl Pts',(-7.23839303975607,70.3747025586552,12.));
#99296=CARTESIAN_POINT('Ctrl Pts',(-7.24672118647085,70.3944243994504,0.));
#99297=CARTESIAN_POINT('Ctrl Pts',(-7.24672118647085,70.3944243994504,12.));
#99298=CARTESIAN_POINT('Ctrl Pts',(-7.25508874012043,70.4141825708178,0.));
#99299=CARTESIAN_POINT('Ctrl Pts',(-7.25508874012043,70.4141825708178,12.));
#99300=CARTESIAN_POINT('Ctrl Pts',(-7.26349570998033,70.4339768986346,0.));
#99301=CARTESIAN_POINT('Ctrl Pts',(-7.26349570998033,70.4339768986346,12.));
#99302=CARTESIAN_POINT('Ctrl Pts',(-7.27194210517063,70.4538072096992,0.));
#99303=CARTESIAN_POINT('Ctrl Pts',(-7.27194210517063,70.4538072096992,12.));
#99304=CARTESIAN_POINT('Ctrl Pts',(-7.28042793465471,70.4736733316487,0.));
#99305=CARTESIAN_POINT('Ctrl Pts',(-7.28042793465471,70.4736733316487,12.));
#99306=CARTESIAN_POINT('Ctrl Pts',(-7.28895320723862,70.4935750929058,0.));
#99307=CARTESIAN_POINT('Ctrl Pts',(-7.28895320723862,70.4935750929058,12.));
#99308=CARTESIAN_POINT('Ctrl Pts',(-7.29751793157823,70.5135123227169,0.));
#99309=CARTESIAN_POINT('Ctrl Pts',(-7.29751793157823,70.5135123227169,12.));
#99310=CARTESIAN_POINT('Ctrl Pts',(-7.30612211618053,70.5334848511681,0.));
#99311=CARTESIAN_POINT('Ctrl Pts',(-7.30612211618053,70.5334848511681,12.));
#99312=CARTESIAN_POINT('Ctrl Pts',(-7.31476576940392,70.5534925092043,0.));
#99313=CARTESIAN_POINT('Ctrl Pts',(-7.31476576940392,70.5534925092043,12.));
#99314=CARTESIAN_POINT('Ctrl Pts',(-7.3234488994522,70.5735351286476,0.));
#99315=CARTESIAN_POINT('Ctrl Pts',(-7.3234488994522,70.5735351286476,12.));
#99316=CARTESIAN_POINT('Ctrl Pts',(-7.3321715143759,70.5936125421946,0.));
#99317=CARTESIAN_POINT('Ctrl Pts',(-7.3321715143759,70.5936125421946,12.));
#99318=CARTESIAN_POINT('Ctrl Pts',(-7.34093362208008,70.6137245833996,0.));
#99319=CARTESIAN_POINT('Ctrl Pts',(-7.34093362208008,70.6137245833996,12.));
#99320=CARTESIAN_POINT('Ctrl Pts',(-7.34973523032577,70.6338710866562,0.));
#99321=CARTESIAN_POINT('Ctrl Pts',(-7.34973523032577,70.6338710866562,12.));
#99322=CARTESIAN_POINT('Ctrl Pts',(-7.35857634673055,70.6540518871775,0.));
#99323=CARTESIAN_POINT('Ctrl Pts',(-7.35857634673055,70.6540518871775,12.));
#99324=CARTESIAN_POINT('Ctrl Pts',(-7.36745697876301,70.6742668209687,0.));
#99325=CARTESIAN_POINT('Ctrl Pts',(-7.36745697876301,70.6742668209687,12.));
#99326=CARTESIAN_POINT('Ctrl Pts',(-7.37637713374768,70.694515724827,0.));
#99327=CARTESIAN_POINT('Ctrl Pts',(-7.37637713374768,70.694515724827,12.));
#99328=CARTESIAN_POINT('Ctrl Pts',(-7.38533681887033,70.7147984363424,0.));
#99329=CARTESIAN_POINT('Ctrl Pts',(-7.38533681887033,70.7147984363424,12.));
#99330=CARTESIAN_POINT('Ctrl Pts',(-7.39433604117891,70.735114793895,0.));
#99331=CARTESIAN_POINT('Ctrl Pts',(-7.39433604117891,70.735114793895,12.));
#99332=CARTESIAN_POINT('Ctrl Pts',(-7.4033748075823,70.7554646366514,0.));
#99333=CARTESIAN_POINT('Ctrl Pts',(-7.4033748075823,70.7554646366514,12.));
#99334=CARTESIAN_POINT('Ctrl Pts',(-7.41245312484487,70.7758478045576,0.));
#99335=CARTESIAN_POINT('Ctrl Pts',(-7.41245312484487,70.7758478045576,12.));
#99336=CARTESIAN_POINT('Ctrl Pts',(-7.42157099959316,70.7962641383351,0.));
#99337=CARTESIAN_POINT('Ctrl Pts',(-7.42157099959316,70.7962641383351,12.));
#99338=CARTESIAN_POINT('Ctrl Pts',(-7.43072843832008,70.8167134794738,0.));
#99339=CARTESIAN_POINT('Ctrl Pts',(-7.43072843832008,70.8167134794738,12.));
#99340=CARTESIAN_POINT('Ctrl Pts',(-7.43992544738607,70.8371956702242,0.));
#99341=CARTESIAN_POINT('Ctrl Pts',(-7.43992544738607,70.8371956702242,12.));
#99342=CARTESIAN_POINT('Ctrl Pts',(-7.44916203301645,70.8577105535841,0.));
#99343=CARTESIAN_POINT('Ctrl Pts',(-7.44916203301645,70.8577105535841,12.));
#99344=CARTESIAN_POINT('Ctrl Pts',(-7.45843820129776,70.8782579732885,0.));
#99345=CARTESIAN_POINT('Ctrl Pts',(-7.45843820129776,70.8782579732885,12.));
#99346=CARTESIAN_POINT('Ctrl Pts',(-7.46775395818519,70.8988377738088,0.));
#99347=CARTESIAN_POINT('Ctrl Pts',(-7.46775395818519,70.8988377738088,12.));
#99348=CARTESIAN_POINT('Ctrl Pts',(-7.47710930950554,70.9194498003483,0.));
#99349=CARTESIAN_POINT('Ctrl Pts',(-7.47710930950554,70.9194498003483,12.));
#99350=CARTESIAN_POINT('Ctrl Pts',(-7.48650426095823,70.9400938988373,0.));
#99351=CARTESIAN_POINT('Ctrl Pts',(-7.48650426095823,70.9400938988373,12.));
#99352=CARTESIAN_POINT('Ctrl Pts',(-7.49593881811141,70.9607699159234,0.));
#99353=CARTESIAN_POINT('Ctrl Pts',(-7.49593881811141,70.9607699159234,12.));
#99354=CARTESIAN_POINT('Ctrl Pts',(-7.50541298639948,70.9814776989637,0.));
#99355=CARTESIAN_POINT('Ctrl Pts',(-7.50541298639948,70.9814776989637,12.));
#99356=CARTESIAN_POINT('Ctrl Pts',(-7.51492677113112,71.0022170960235,0.));
#99357=CARTESIAN_POINT('Ctrl Pts',(-7.51492677113112,71.0022170960235,12.));
#99358=CARTESIAN_POINT('Ctrl Pts',(-7.52448017749136,71.0229879558713,0.));
#99359=CARTESIAN_POINT('Ctrl Pts',(-7.52448017749136,71.0229879558713,12.));
#99360=CARTESIAN_POINT('Ctrl Pts',(-7.53407321054254,71.0437901279722,0.));
#99361=CARTESIAN_POINT('Ctrl Pts',(-7.53407321054254,71.0437901279722,12.));
#99362=CARTESIAN_POINT('Ctrl Pts',(-7.54370587521948,71.0646234624783,0.));
#99363=CARTESIAN_POINT('Ctrl Pts',(-7.54370587521948,71.0646234624783,12.));
#99364=CARTESIAN_POINT('Ctrl Pts',(-7.55337817632873,71.0854878102203,0.));
#99365=CARTESIAN_POINT('Ctrl Pts',(-7.55337817632873,71.0854878102203,12.));
#99366=CARTESIAN_POINT('Ctrl Pts',(-7.56309011855617,71.1063830227074,0.));
#99367=CARTESIAN_POINT('Ctrl Pts',(-7.56309011855617,71.1063830227074,12.));
#99368=CARTESIAN_POINT('Ctrl Pts',(-7.57284170646866,71.1273089521218,0.));
#99369=CARTESIAN_POINT('Ctrl Pts',(-7.57284170646866,71.1273089521218,12.));
#99370=CARTESIAN_POINT('Ctrl Pts',(-7.58263294451465,71.1482654513133,0.));
#99371=CARTESIAN_POINT('Ctrl Pts',(-7.58263294451465,71.1482654513133,12.));
#99372=CARTESIAN_POINT('Ctrl Pts',(-7.5924638370186,71.1692523737887,0.));
#99373=CARTESIAN_POINT('Ctrl Pts',(-7.5924638370186,71.1692523737887,12.));
#99374=CARTESIAN_POINT('Ctrl Pts',(-7.60233438818156,71.1902695737063,0.));
#99375=CARTESIAN_POINT('Ctrl Pts',(-7.60233438818156,71.1902695737063,12.));
#99376=CARTESIAN_POINT('Ctrl Pts',(-7.61224460208887,71.2113169058778,0.));
#99377=CARTESIAN_POINT('Ctrl Pts',(-7.61224460208887,71.2113169058778,12.));
#99378=CARTESIAN_POINT('Ctrl Pts',(-7.62219448271125,71.232394225762,0.));
#99379=CARTESIAN_POINT('Ctrl Pts',(-7.62219448271125,71.232394225762,12.));
#99380=CARTESIAN_POINT('Ctrl Pts',(-7.63218403390515,71.2535013894587,0.));
#99381=CARTESIAN_POINT('Ctrl Pts',(-7.63218403390515,71.2535013894587,12.));
#99382=CARTESIAN_POINT('Ctrl Pts',(-7.64221325940672,71.2746382536974,0.));
#99383=CARTESIAN_POINT('Ctrl Pts',(-7.64221325940672,71.2746382536974,12.));
#99384=CARTESIAN_POINT('Ctrl Pts',(-7.65228216283343,71.2958046758334,0.));
#99385=CARTESIAN_POINT('Ctrl Pts',(-7.65228216283343,71.2958046758334,12.));
#99386=CARTESIAN_POINT('Ctrl Pts',(-7.66239074769119,71.3170005138474,0.));
#99387=CARTESIAN_POINT('Ctrl Pts',(-7.66239074769119,71.3170005138474,12.));
#99388=CARTESIAN_POINT('Ctrl Pts',(-7.67253901737539,71.3382256263405,0.));
#99389=CARTESIAN_POINT('Ctrl Pts',(-7.67253901737539,71.3382256263405,12.));
#99390=CARTESIAN_POINT('Ctrl Pts',(-7.68272697517103,71.3594798725294,0.));
#99391=CARTESIAN_POINT('Ctrl Pts',(-7.68272697517103,71.3594798725294,12.));
#99392=CARTESIAN_POINT('Ctrl Pts',(-7.69295462424647,71.380763112236,0.));
#99393=CARTESIAN_POINT('Ctrl Pts',(-7.69295462424647,71.380763112236,12.));
#99394=CARTESIAN_POINT('Ctrl Pts',(-7.70322196765573,71.4020752058827,0.));
#99395=CARTESIAN_POINT('Ctrl Pts',(-7.70322196765573,71.4020752058827,12.));
#99396=CARTESIAN_POINT('Ctrl Pts',(-7.71352900834538,71.4234160144943,0.));
#99397=CARTESIAN_POINT('Ctrl Pts',(-7.71352900834538,71.4234160144943,12.));
#99398=CARTESIAN_POINT('Ctrl Pts',(-7.72387574915544,71.4447853996919,0.));
#99399=CARTESIAN_POINT('Ctrl Pts',(-7.72387574915544,71.4447853996919,12.));
#99400=CARTESIAN_POINT('Ctrl Pts',(-7.73426219281932,71.4661832236881,0.));
#99401=CARTESIAN_POINT('Ctrl Pts',(-7.73426219281932,71.4661832236881,12.));
#99402=CARTESIAN_POINT('Ctrl Pts',(-7.74468834195734,71.487609349277,0.));
#99403=CARTESIAN_POINT('Ctrl Pts',(-7.74468834195734,71.487609349277,12.));
#99404=CARTESIAN_POINT('Ctrl Pts',(-7.75515419907955,71.5090636398307,0.));
#99405=CARTESIAN_POINT('Ctrl Pts',(-7.75515419907955,71.5090636398307,12.));
#99406=CARTESIAN_POINT('Ctrl Pts',(-7.76565976659218,71.5305459592987,0.));
#99407=CARTESIAN_POINT('Ctrl Pts',(-7.76565976659218,71.5305459592987,12.));
#99408=CARTESIAN_POINT('Ctrl Pts',(-7.77620504679868,71.5520561722039,0.));
#99409=CARTESIAN_POINT('Ctrl Pts',(-7.77620504679868,71.5520561722039,12.));
#99410=CARTESIAN_POINT('Ctrl Pts',(-7.78679004189935,71.5735941436366,0.));
#99411=CARTESIAN_POINT('Ctrl Pts',(-7.78679004189935,71.5735941436366,12.));
#99412=CARTESIAN_POINT('Ctrl Pts',(-7.79741475398512,71.5951597392471,0.));
#99413=CARTESIAN_POINT('Ctrl Pts',(-7.79741475398512,71.5951597392471,12.));
#99414=CARTESIAN_POINT('Ctrl Pts',(-7.80807918504017,71.616752825242,0.));
#99415=CARTESIAN_POINT('Ctrl Pts',(-7.80807918504017,71.616752825242,12.));
#99416=CARTESIAN_POINT('Ctrl Pts',(-7.81878333694856,71.638373268384,0.));
#99417=CARTESIAN_POINT('Ctrl Pts',(-7.81878333694856,71.638373268384,12.));
#99418=CARTESIAN_POINT('Ctrl Pts',(-7.82952721149504,71.6600209359869,0.));
#99419=CARTESIAN_POINT('Ctrl Pts',(-7.82952721149504,71.6600209359869,12.));
#99420=CARTESIAN_POINT('Ctrl Pts',(-7.84031081036489,71.681695695912,0.));
#99421=CARTESIAN_POINT('Ctrl Pts',(-7.84031081036489,71.681695695912,12.));
#99422=CARTESIAN_POINT('Ctrl Pts',(-7.85113413513739,71.7033974165576,0.));
#99423=CARTESIAN_POINT('Ctrl Pts',(-7.85113413513739,71.7033974165576,12.));
#99424=CARTESIAN_POINT('Ctrl Pts',(-7.8619971872883,71.7251259668573,0.));
#99425=CARTESIAN_POINT('Ctrl Pts',(-7.8619971872883,71.7251259668573,12.));
#99426=CARTESIAN_POINT('Ctrl Pts',(-7.87289996819654,71.7468812162795,0.));
#99427=CARTESIAN_POINT('Ctrl Pts',(-7.87289996819654,71.7468812162795,12.));
#99428=CARTESIAN_POINT('Ctrl Pts',(-7.88384247914522,71.768663034824,0.));
#99429=CARTESIAN_POINT('Ctrl Pts',(-7.88384247914522,71.768663034824,12.));
#99430=CARTESIAN_POINT('Ctrl Pts',(-7.89482472132135,71.7904712930172,0.));
#99431=CARTESIAN_POINT('Ctrl Pts',(-7.89482472132135,71.7904712930172,12.));
#99432=CARTESIAN_POINT('Ctrl Pts',(-7.90584669580955,71.8123058619038,0.));
#99433=CARTESIAN_POINT('Ctrl Pts',(-7.90584669580955,71.8123058619038,12.));
#99434=CARTESIAN_POINT('Ctrl Pts',(-7.91690840359371,71.8341666130424,0.));
#99435=CARTESIAN_POINT('Ctrl Pts',(-7.91690840359371,71.8341666130424,12.));
#99436=CARTESIAN_POINT('Ctrl Pts',(-7.928009845564,71.8560534185071,0.));
#99437=CARTESIAN_POINT('Ctrl Pts',(-7.928009845564,71.8560534185071,12.));
#99438=CARTESIAN_POINT('Ctrl Pts',(-7.93915102251796,71.8779661508833,0.));
#99439=CARTESIAN_POINT('Ctrl Pts',(-7.93915102251796,71.8779661508833,12.));
#99440=CARTESIAN_POINT('Ctrl Pts',(-7.95033193516046,71.8999046832642,0.));
#99441=CARTESIAN_POINT('Ctrl Pts',(-7.95033193516046,71.8999046832642,12.));
#99442=CARTESIAN_POINT('Ctrl Pts',(-7.96155258409752,71.9218688892426,0.));
#99443=CARTESIAN_POINT('Ctrl Pts',(-7.96155258409752,71.9218688892426,12.));
#99444=CARTESIAN_POINT('Ctrl Pts',(-7.97281296983702,71.9438586429072,0.));
#99445=CARTESIAN_POINT('Ctrl Pts',(-7.97281296983702,71.9438586429072,12.));
#99446=CARTESIAN_POINT('Ctrl Pts',(-7.98411309279598,71.9658738188421,0.));
#99447=CARTESIAN_POINT('Ctrl Pts',(-7.98411309279598,71.9658738188421,12.));
#99448=CARTESIAN_POINT('Ctrl Pts',(-7.99545295330182,71.9879142921248,0.));
#99449=CARTESIAN_POINT('Ctrl Pts',(-7.99545295330182,71.9879142921248,12.));
#99450=CARTESIAN_POINT('Ctrl Pts',(-8.0068325515925,72.0099799383216,0.));
#99451=CARTESIAN_POINT('Ctrl Pts',(-8.0068325515925,72.0099799383216,12.));
#99452=CARTESIAN_POINT('Ctrl Pts',(-8.0182518878107,72.0320706334802,0.));
#99453=CARTESIAN_POINT('Ctrl Pts',(-8.0182518878107,72.0320706334802,12.));
#99454=CARTESIAN_POINT('Ctrl Pts',(-8.02971096200329,72.0541862541262,0.));
#99455=CARTESIAN_POINT('Ctrl Pts',(-8.02971096200329,72.0541862541262,12.));
#99456=CARTESIAN_POINT('Ctrl Pts',(-8.04120977412891,72.0763266772632,0.));
#99457=CARTESIAN_POINT('Ctrl Pts',(-8.04120977412891,72.0763266772632,12.));
#99458=CARTESIAN_POINT('Ctrl Pts',(-8.05274832405957,72.0984917803702,0.));
#99459=CARTESIAN_POINT('Ctrl Pts',(-8.05274832405957,72.0984917803702,12.));
#99460=CARTESIAN_POINT('Ctrl Pts',(-8.06432661158089,72.1206814413985,0.));
#99461=CARTESIAN_POINT('Ctrl Pts',(-8.06432661158089,72.1206814413985,12.));
#99462=CARTESIAN_POINT('Ctrl Pts',(-8.07594463638699,72.1428955387648,0.));
#99463=CARTESIAN_POINT('Ctrl Pts',(-8.07594463638699,72.1428955387648,12.));
#99464=CARTESIAN_POINT('Ctrl Pts',(-8.08760239807815,72.165133951346,0.));
#99465=CARTESIAN_POINT('Ctrl Pts',(-8.08760239807815,72.165133951346,12.));
#99466=CARTESIAN_POINT('Ctrl Pts',(-8.09929989616874,72.18739655848,0.));
#99467=CARTESIAN_POINT('Ctrl Pts',(-8.09929989616874,72.18739655848,12.));
#99468=CARTESIAN_POINT('Ctrl Pts',(-8.11103713008922,72.2096832399626,0.));
#99469=CARTESIAN_POINT('Ctrl Pts',(-8.11103713008922,72.2096832399626,12.));
#99470=CARTESIAN_POINT('Ctrl Pts',(-8.12281409918662,72.2319938760451,0.));
#99471=CARTESIAN_POINT('Ctrl Pts',(-8.12281409918662,72.2319938760451,12.));
#99472=CARTESIAN_POINT('Ctrl Pts',(-8.13463080272029,72.2543283474279,0.));
#99473=CARTESIAN_POINT('Ctrl Pts',(-8.13463080272029,72.2543283474279,12.));
#99474=CARTESIAN_POINT('Ctrl Pts',(-8.14648723985793,72.2766865352552,0.));
#99475=CARTESIAN_POINT('Ctrl Pts',(-8.14648723985793,72.2766865352552,12.));
#99476=CARTESIAN_POINT('Ctrl Pts',(-8.15838340968328,72.2990683211155,0.));
#99477=CARTESIAN_POINT('Ctrl Pts',(-8.15838340968328,72.2990683211155,12.));
#99478=CARTESIAN_POINT('Ctrl Pts',(-8.17031931119882,72.3214735870402,0.));
#99479=CARTESIAN_POINT('Ctrl Pts',(-8.17031931119882,72.3214735870402,12.));
#99480=CARTESIAN_POINT('Ctrl Pts',(-8.18229494332622,72.3439022155007,0.));
#99481=CARTESIAN_POINT('Ctrl Pts',(-8.18229494332622,72.3439022155007,12.));
#99482=CARTESIAN_POINT('Ctrl Pts',(-8.19431030490319,72.3663540894034,0.));
#99483=CARTESIAN_POINT('Ctrl Pts',(-8.19431030490319,72.3663540894034,12.));
#99484=CARTESIAN_POINT('Ctrl Pts',(-8.20636539467782,72.3888290920845,0.));
#99485=CARTESIAN_POINT('Ctrl Pts',(-8.20636539467782,72.3888290920845,12.));
#99486=CARTESIAN_POINT('Ctrl Pts',(-8.21846021131564,72.4113271073091,0.));
#99487=CARTESIAN_POINT('Ctrl Pts',(-8.21846021131564,72.4113271073091,12.));
#99488=CARTESIAN_POINT('Ctrl Pts',(-8.23059475340354,72.4338480192701,0.));
#99489=CARTESIAN_POINT('Ctrl Pts',(-8.23059475340354,72.4338480192701,12.));
#99490=CARTESIAN_POINT('Ctrl Pts',(-8.24276901945037,72.4563917125842,0.));
#99491=CARTESIAN_POINT('Ctrl Pts',(-8.24276901945037,72.4563917125842,12.));
#99492=CARTESIAN_POINT('Ctrl Pts',(-8.25498300788493,72.4789580722871,0.));
#99493=CARTESIAN_POINT('Ctrl Pts',(-8.25498300788493,72.4789580722871,12.));
#99494=CARTESIAN_POINT('Ctrl Pts',(-8.26723671704924,72.501546983825,0.));
#99495=CARTESIAN_POINT('Ctrl Pts',(-8.26723671704924,72.501546983825,12.));
#99496=CARTESIAN_POINT('Ctrl Pts',(-8.27953014520385,72.524158333056,0.));
#99497=CARTESIAN_POINT('Ctrl Pts',(-8.27953014520385,72.524158333056,12.));
#99498=CARTESIAN_POINT('Ctrl Pts',(-8.29186329053289,72.5467920062522,0.));
#99499=CARTESIAN_POINT('Ctrl Pts',(-8.29186329053289,72.5467920062522,12.));
#99500=CARTESIAN_POINT('Ctrl Pts',(-8.30423615114455,72.5694478900983,0.));
#99501=CARTESIAN_POINT('Ctrl Pts',(-8.30423615114455,72.5694478900983,12.));
#99502=CARTESIAN_POINT('Ctrl Pts',(-8.31664872507008,72.5921258716899,0.));
#99503=CARTESIAN_POINT('Ctrl Pts',(-8.31664872507008,72.5921258716899,12.));
#99504=CARTESIAN_POINT('Ctrl Pts',(-8.32910101025653,72.614825838529,0.));
#99505=CARTESIAN_POINT('Ctrl Pts',(-8.32910101025653,72.614825838529,12.));
#99506=CARTESIAN_POINT('Ctrl Pts',(-8.34159300456965,72.6375476785208,0.));
#99507=CARTESIAN_POINT('Ctrl Pts',(-8.34159300456965,72.6375476785208,12.));
#99508=CARTESIAN_POINT('Ctrl Pts',(-8.35412470580083,72.6602912799689,0.));
#99509=CARTESIAN_POINT('Ctrl Pts',(-8.35412470580083,72.6602912799689,12.));
#99510=CARTESIAN_POINT('Ctrl Pts',(-8.36669611166834,72.68305653157,0.));
#99511=CARTESIAN_POINT('Ctrl Pts',(-8.36669611166834,72.68305653157,12.));
#99512=CARTESIAN_POINT('Ctrl Pts',(-8.37930721981735,72.7058433224072,0.));
#99513=CARTESIAN_POINT('Ctrl Pts',(-8.37930721981735,72.7058433224072,12.));
#99514=CARTESIAN_POINT('Ctrl Pts',(-8.39195802781407,72.728651541938,0.));
#99515=CARTESIAN_POINT('Ctrl Pts',(-8.39195802781407,72.728651541938,12.));
#99516=CARTESIAN_POINT('Ctrl Pts',(-8.40464853314493,72.7514810799932,0.));
#99517=CARTESIAN_POINT('Ctrl Pts',(-8.40464853314493,72.7514810799932,12.));
#99518=CARTESIAN_POINT('Ctrl Pts',(-8.41737873322353,72.7743318267876,0.));
#99519=CARTESIAN_POINT('Ctrl Pts',(-8.41737873322353,72.7743318267876,12.));
#99520=CARTESIAN_POINT('Ctrl Pts',(-8.43014862539171,72.7972036729283,0.));
#99521=CARTESIAN_POINT('Ctrl Pts',(-8.43014862539171,72.7972036729283,12.));
#99522=CARTESIAN_POINT('Ctrl Pts',(-8.44295820691907,72.8200965094197,0.));
#99523=CARTESIAN_POINT('Ctrl Pts',(-8.44295820691907,72.8200965094197,12.));
#99524=CARTESIAN_POINT('Ctrl Pts',(-8.45580747499771,72.8430102276703,0.));
#99525=CARTESIAN_POINT('Ctrl Pts',(-8.45580747499771,72.8430102276703,12.));
#99526=CARTESIAN_POINT('Ctrl Pts',(-8.46869642673763,72.8659447194918,0.));
#99527=CARTESIAN_POINT('Ctrl Pts',(-8.46869642673763,72.8659447194918,12.));
#99528=CARTESIAN_POINT('Ctrl Pts',(-8.48162505917628,72.888899877077,0.));
#99529=CARTESIAN_POINT('Ctrl Pts',(-8.48162505917628,72.888899877077,12.));
#99530=CARTESIAN_POINT('Ctrl Pts',(-8.49459336928276,72.9118755929785,0.));
#99531=CARTESIAN_POINT('Ctrl Pts',(-8.49459336928276,72.9118755929785,12.));
#99532=CARTESIAN_POINT('Ctrl Pts',(-8.50760135395979,72.9348717600837,0.));
#99533=CARTESIAN_POINT('Ctrl Pts',(-8.50760135395979,72.9348717600837,12.));
#99534=CARTESIAN_POINT('Ctrl Pts',(-8.52064901004244,72.9578882715923,0.));
#99535=CARTESIAN_POINT('Ctrl Pts',(-8.52064901004244,72.9578882715923,12.));
#99536=CARTESIAN_POINT('Ctrl Pts',(-8.53373633429303,72.9809250209843,0.));
#99537=CARTESIAN_POINT('Ctrl Pts',(-8.53373633429303,72.9809250209843,12.));
#99538=CARTESIAN_POINT('Ctrl Pts',(-8.54686332340439,73.0039819020663,0.));
#99539=CARTESIAN_POINT('Ctrl Pts',(-8.54686332340439,73.0039819020663,12.));
#99540=CARTESIAN_POINT('Ctrl Pts',(-8.56002997400096,73.0270588090193,0.));
#99541=CARTESIAN_POINT('Ctrl Pts',(-8.56002997400096,73.0270588090193,12.));
#99542=CARTESIAN_POINT('Ctrl Pts',(-8.57323628263595,73.0501556364482,0.));
#99543=CARTESIAN_POINT('Ctrl Pts',(-8.57323628263595,73.0501556364482,12.));
#99544=CARTESIAN_POINT('Ctrl Pts',(-8.58648224578723,73.073272279419,0.));
#99545=CARTESIAN_POINT('Ctrl Pts',(-8.58648224578723,73.073272279419,12.));
#99546=CARTESIAN_POINT('Ctrl Pts',(-8.59976785984539,73.0964086335226,0.));
#99547=CARTESIAN_POINT('Ctrl Pts',(-8.59976785984539,73.0964086335226,12.));
#99548=CARTESIAN_POINT('Ctrl Pts',(-8.61309312111989,73.1195645948169,0.));
#99549=CARTESIAN_POINT('Ctrl Pts',(-8.61309312111989,73.1195645948169,12.));
#99550=CARTESIAN_POINT('Ctrl Pts',(-8.62645802585475,73.142740059703,0.));
#99551=CARTESIAN_POINT('Ctrl Pts',(-8.62645802585475,73.142740059703,12.));
#99552=CARTESIAN_POINT('Ctrl Pts',(-8.63986257023735,73.165934924813,0.));
#99553=CARTESIAN_POINT('Ctrl Pts',(-8.63986257023735,73.165934924813,12.));
#99554=CARTESIAN_POINT('Ctrl Pts',(-8.65330675040535,73.1891490869057,0.));
#99555=CARTESIAN_POINT('Ctrl Pts',(-8.65330675040535,73.1891490869057,12.));
#99556=CARTESIAN_POINT('Ctrl Pts',(-8.66679056245095,73.2123824427212,0.));
#99557=CARTESIAN_POINT('Ctrl Pts',(-8.66679056245095,73.2123824427212,12.));
#99558=CARTESIAN_POINT('Ctrl Pts',(-8.68031400241884,73.2356348889704,0.));
#99559=CARTESIAN_POINT('Ctrl Pts',(-8.68031400241884,73.2356348889704,12.));
#99560=CARTESIAN_POINT('Ctrl Pts',(-8.69387706629304,73.2589063226373,0.));
#99561=CARTESIAN_POINT('Ctrl Pts',(-8.69387706629304,73.2589063226373,12.));
#99562=CARTESIAN_POINT('Ctrl Pts',(-8.70747974998245,73.282196641216,0.));
#99563=CARTESIAN_POINT('Ctrl Pts',(-8.70747974998245,73.282196641216,12.));
#99564=CARTESIAN_POINT('Ctrl Pts',(-8.72112204930232,73.3055057429744,0.));
#99565=CARTESIAN_POINT('Ctrl Pts',(-8.72112204930232,73.3055057429744,12.));
#99566=CARTESIAN_POINT('Ctrl Pts',(-8.7348039599536,73.3288335271989,0.));
#99567=CARTESIAN_POINT('Ctrl Pts',(-8.7348039599536,73.3288335271989,12.));
#99568=CARTESIAN_POINT('Ctrl Pts',(-8.74852547749736,73.3521798944595,0.));
#99569=CARTESIAN_POINT('Ctrl Pts',(-8.74852547749736,73.3521798944595,12.));
#99570=CARTESIAN_POINT('Ctrl Pts',(-8.76228659740305,73.3755447460235,0.));
#99571=CARTESIAN_POINT('Ctrl Pts',(-8.76228659740305,73.3755447460235,12.));
#99572=CARTESIAN_POINT('Ctrl Pts',(-8.77608731509304,73.3989279832808,0.));
#99573=CARTESIAN_POINT('Ctrl Pts',(-8.77608731509304,73.3989279832808,12.));
#99574=CARTESIAN_POINT('Ctrl Pts',(-8.78992762598738,73.422329507112,0.));
#99575=CARTESIAN_POINT('Ctrl Pts',(-8.78992762598738,73.422329507112,12.));
#99576=CARTESIAN_POINT('Ctrl Pts',(-8.80380752553714,73.4457492173949,0.));
#99577=CARTESIAN_POINT('Ctrl Pts',(-8.80380752553714,73.4457492173949,12.));
#99578=CARTESIAN_POINT('Ctrl Pts',(-8.81772700927593,73.4691870121608,0.));
#99579=CARTESIAN_POINT('Ctrl Pts',(-8.81772700927593,73.4691870121608,12.));
#99580=CARTESIAN_POINT('Ctrl Pts',(-8.83168607277415,73.4926427882787,0.));
#99581=CARTESIAN_POINT('Ctrl Pts',(-8.83168607277415,73.4926427882787,12.));
#99582=CARTESIAN_POINT('Ctrl Pts',(-8.84568471153894,73.5161164429765,0.));
#99583=CARTESIAN_POINT('Ctrl Pts',(-8.84568471153894,73.5161164429765,12.));
#99584=CARTESIAN_POINT('Ctrl Pts',(-8.85972292092183,73.5396078751672,0.));
#99585=CARTESIAN_POINT('Ctrl Pts',(-8.85972292092183,73.5396078751672,12.));
#99586=CARTESIAN_POINT('Ctrl Pts',(-8.87380069602955,73.5631169867113,0.));
#99587=CARTESIAN_POINT('Ctrl Pts',(-8.87380069602955,73.5631169867113,12.));
#99588=CARTESIAN_POINT('Ctrl Pts',(-8.88791803160341,73.5866436840493,0.));
#99589=CARTESIAN_POINT('Ctrl Pts',(-8.88791803160341,73.5866436840493,12.));
#99590=CARTESIAN_POINT('Ctrl Pts',(-8.90207492198871,73.6101878785868,0.));
#99591=CARTESIAN_POINT('Ctrl Pts',(-8.90207492198871,73.6101878785868,12.));
#99592=CARTESIAN_POINT('Ctrl Pts',(-8.91627136139887,73.6337494830846,0.));
#99593=CARTESIAN_POINT('Ctrl Pts',(-8.91627136139887,73.6337494830846,12.));
#99594=CARTESIAN_POINT('Ctrl Pts',(-8.93050734411971,73.6573284088088,0.));
#99595=CARTESIAN_POINT('Ctrl Pts',(-8.93050734411971,73.6573284088088,12.));
#99596=CARTESIAN_POINT('Ctrl Pts',(-8.94478286474383,73.6809245622361,0.));
#99597=CARTESIAN_POINT('Ctrl Pts',(-8.94478286474383,73.6809245622361,12.));
#99598=CARTESIAN_POINT('Ctrl Pts',(-8.9590979183629,73.7045378422775,0.));
#99599=CARTESIAN_POINT('Ctrl Pts',(-8.9590979183629,73.7045378422775,12.));
#99600=CARTESIAN_POINT('Ctrl Pts',(-8.97345250083918,73.7281681364031,0.));
#99601=CARTESIAN_POINT('Ctrl Pts',(-8.97345250083918,73.7281681364031,12.));
#99602=CARTESIAN_POINT('Ctrl Pts',(-8.98784660837828,73.7518153262253,0.));
#99603=CARTESIAN_POINT('Ctrl Pts',(-8.98784660837828,73.7518153262253,12.));
#99604=CARTESIAN_POINT('Ctrl Pts',(-9.00228023701466,73.7754792943925,0.));
#99605=CARTESIAN_POINT('Ctrl Pts',(-9.00228023701466,73.7754792943925,12.));
#99606=CARTESIAN_POINT('Ctrl Pts',(-9.01675338208222,73.7991599312731,0.));
#99607=CARTESIAN_POINT('Ctrl Pts',(-9.01675338208222,73.7991599312731,12.));
#99608=CARTESIAN_POINT('Ctrl Pts',(-9.03126603777981,73.8228571411607,0.));
#99609=CARTESIAN_POINT('Ctrl Pts',(-9.03126603777981,73.8228571411607,12.));
#99610=CARTESIAN_POINT('Ctrl Pts',(-9.04581819646385,73.8465708500679,0.));
#99611=CARTESIAN_POINT('Ctrl Pts',(-9.04581819646385,73.8465708500679,12.));
#99612=CARTESIAN_POINT('Ctrl Pts',(-9.0604098488925,73.870301007746,0.));
#99613=CARTESIAN_POINT('Ctrl Pts',(-9.0604098488925,73.870301007746,12.));
#99614=CARTESIAN_POINT('Ctrl Pts',(-9.07504098570547,73.8940475821756,0.));
#99615=CARTESIAN_POINT('Ctrl Pts',(-9.07504098570547,73.8940475821756,12.));
#99616=CARTESIAN_POINT('Ctrl Pts',(-9.08677747601238,73.9130579611989,0.));
#99617=CARTESIAN_POINT('Ctrl Pts',(-9.08677747601238,73.9130579611989,12.));
#99618=CARTESIAN_POINT('Ctrl Pts',(-9.09559760528458,73.9273231219464,0.));
#99619=CARTESIAN_POINT('Ctrl Pts',(-9.09559760528458,73.9273231219464,12.));
#99620=CARTESIAN_POINT('Ctrl Pts',(-9.10148558516324,73.9368365074164,0.));
#99621=CARTESIAN_POINT('Ctrl Pts',(-9.10148558516324,73.9368365074164,12.));
#99622=CARTESIAN_POINT('Ctrl Pts',(-9.10443154852687,73.9415940197274,0.));
#99623=CARTESIAN_POINT('Ctrl Pts',(-9.10443154852687,73.9415940197274,12.));
#99624=CARTESIAN_POINT('',(-6.95102489306926,69.6540253893192,0.));
#99625=CARTESIAN_POINT('Ctrl Pts',(-6.95102489306926,69.6540253893192,0.));
#99626=CARTESIAN_POINT('Ctrl Pts',(-6.95238884849025,69.6576616146467,0.));
#99627=CARTESIAN_POINT('Ctrl Pts',(-6.955120653176,69.664938391983,0.));
#99628=CARTESIAN_POINT('Ctrl Pts',(-6.95923004173591,69.6758665380378,0.));
#99629=CARTESIAN_POINT('Ctrl Pts',(-6.96473259049513,69.6904633605421,0.));
#99630=CARTESIAN_POINT('Ctrl Pts',(-6.9716497229144,69.7087526479973,0.));
#99631=CARTESIAN_POINT('Ctrl Pts',(-6.97860581164527,69.7270851557366,0.));
#99632=CARTESIAN_POINT('Ctrl Pts',(-6.98560086924214,69.7454607995607,0.));
#99633=CARTESIAN_POINT('Ctrl Pts',(-6.9926349102794,69.7638794280419,0.));
#99634=CARTESIAN_POINT('Ctrl Pts',(-6.99970795069476,69.782340824259,0.));
#99635=CARTESIAN_POINT('Ctrl Pts',(-7.00682000718151,69.8008447346863,0.));
#99636=CARTESIAN_POINT('Ctrl Pts',(-7.01397109655455,69.8193908913722,0.));
#99637=CARTESIAN_POINT('Ctrl Pts',(-7.02116123514452,69.8379790360518,0.));
#99638=CARTESIAN_POINT('Ctrl Pts',(-7.02839043811812,69.8566089455375,0.));
#99639=CARTESIAN_POINT('Ctrl Pts',(-7.03565871972221,69.8752804235238,0.));
#99640=CARTESIAN_POINT('Ctrl Pts',(-7.04296609362166,69.8939932885841,0.));
#99641=CARTESIAN_POINT('Ctrl Pts',(-7.05031257318115,69.9127473642099,0.));
#99642=CARTESIAN_POINT('Ctrl Pts',(-7.05769817180857,69.9315424664291,0.));
#99643=CARTESIAN_POINT('Ctrl Pts',(-7.0651229031285,69.9503783975727,0.));
#99644=CARTESIAN_POINT('Ctrl Pts',(-7.07258678080831,69.9692549527296,0.));
#99645=CARTESIAN_POINT('Ctrl Pts',(-7.08008981844652,69.988171923788,0.));
#99646=CARTESIAN_POINT('Ctrl Pts',(-7.08763202944246,70.0071291040766,0.));
#99647=CARTESIAN_POINT('Ctrl Pts',(-7.09521342684249,70.0261262936388,0.));
#99648=CARTESIAN_POINT('Ctrl Pts',(-7.10283402335034,70.0451632990086,0.));
#99649=CARTESIAN_POINT('Ctrl Pts',(-7.11049383140446,70.0642399306869,0.));
#99650=CARTESIAN_POINT('Ctrl Pts',(-7.11819286322826,70.0833560013975,0.));
#99651=CARTESIAN_POINT('Ctrl Pts',(-7.12593113088904,70.1025113239495,0.));
#99652=CARTESIAN_POINT('Ctrl Pts',(-7.13370864634442,70.1217057094499,0.));
#99653=CARTESIAN_POINT('Ctrl Pts',(-7.14152542142374,70.1409389682424,0.));
#99654=CARTESIAN_POINT('Ctrl Pts',(-7.14938146780813,70.1602109107202,0.));
#99655=CARTESIAN_POINT('Ctrl Pts',(-7.15727679700933,70.1795213481185,0.));
#99656=CARTESIAN_POINT('Ctrl Pts',(-7.16521142033864,70.1988700934593,0.));
#99657=CARTESIAN_POINT('Ctrl Pts',(-7.17318534889716,70.2182569618994,0.));
#99658=CARTESIAN_POINT('Ctrl Pts',(-7.18119859359778,70.2376817702215,0.));
#99659=CARTESIAN_POINT('Ctrl Pts',(-7.18925116517555,70.2571443365192,0.));
#99660=CARTESIAN_POINT('Ctrl Pts',(-7.19734307419873,70.2766444798285,0.));
#99661=CARTESIAN_POINT('Ctrl Pts',(-7.20547433107483,70.2961820197077,0.));
#99662=CARTESIAN_POINT('Ctrl Pts',(-7.2136449460545,70.3157567762588,0.));
#99663=CARTESIAN_POINT('Ctrl Pts',(-7.22185492923191,70.3353685703112,0.));
#99664=CARTESIAN_POINT('Ctrl Pts',(-7.23010429054229,70.3550172235486,0.));
#99665=CARTESIAN_POINT('Ctrl Pts',(-7.23839303975607,70.3747025586552,0.));
#99666=CARTESIAN_POINT('Ctrl Pts',(-7.24672118647085,70.3944243994504,0.));
#99667=CARTESIAN_POINT('Ctrl Pts',(-7.25508874012043,70.4141825708178,0.));
#99668=CARTESIAN_POINT('Ctrl Pts',(-7.26349570998033,70.4339768986346,0.));
#99669=CARTESIAN_POINT('Ctrl Pts',(-7.27194210517063,70.4538072096992,0.));
#99670=CARTESIAN_POINT('Ctrl Pts',(-7.28042793465471,70.4736733316487,0.));
#99671=CARTESIAN_POINT('Ctrl Pts',(-7.28895320723862,70.4935750929058,0.));
#99672=CARTESIAN_POINT('Ctrl Pts',(-7.29751793157823,70.5135123227169,0.));
#99673=CARTESIAN_POINT('Ctrl Pts',(-7.30612211618053,70.5334848511681,0.));
#99674=CARTESIAN_POINT('Ctrl Pts',(-7.31476576940392,70.5534925092043,0.));
#99675=CARTESIAN_POINT('Ctrl Pts',(-7.3234488994522,70.5735351286476,0.));
#99676=CARTESIAN_POINT('Ctrl Pts',(-7.3321715143759,70.5936125421946,0.));
#99677=CARTESIAN_POINT('Ctrl Pts',(-7.34093362208008,70.6137245833996,0.));
#99678=CARTESIAN_POINT('Ctrl Pts',(-7.34973523032577,70.6338710866562,0.));
#99679=CARTESIAN_POINT('Ctrl Pts',(-7.35857634673055,70.6540518871775,0.));
#99680=CARTESIAN_POINT('Ctrl Pts',(-7.36745697876301,70.6742668209687,0.));
#99681=CARTESIAN_POINT('Ctrl Pts',(-7.37637713374768,70.694515724827,0.));
#99682=CARTESIAN_POINT('Ctrl Pts',(-7.38533681887033,70.7147984363424,0.));
#99683=CARTESIAN_POINT('Ctrl Pts',(-7.39433604117891,70.735114793895,0.));
#99684=CARTESIAN_POINT('Ctrl Pts',(-7.4033748075823,70.7554646366514,0.));
#99685=CARTESIAN_POINT('Ctrl Pts',(-7.41245312484487,70.7758478045576,0.));
#99686=CARTESIAN_POINT('Ctrl Pts',(-7.42157099959316,70.7962641383351,0.));
#99687=CARTESIAN_POINT('Ctrl Pts',(-7.43072843832008,70.8167134794738,0.));
#99688=CARTESIAN_POINT('Ctrl Pts',(-7.43992544738607,70.8371956702242,0.));
#99689=CARTESIAN_POINT('Ctrl Pts',(-7.44916203301645,70.8577105535841,0.));
#99690=CARTESIAN_POINT('Ctrl Pts',(-7.45843820129776,70.8782579732885,0.));
#99691=CARTESIAN_POINT('Ctrl Pts',(-7.46775395818519,70.8988377738088,0.));
#99692=CARTESIAN_POINT('Ctrl Pts',(-7.47710930950554,70.9194498003483,0.));
#99693=CARTESIAN_POINT('Ctrl Pts',(-7.48650426095823,70.9400938988373,0.));
#99694=CARTESIAN_POINT('Ctrl Pts',(-7.49593881811141,70.9607699159234,0.));
#99695=CARTESIAN_POINT('Ctrl Pts',(-7.50541298639948,70.9814776989637,0.));
#99696=CARTESIAN_POINT('Ctrl Pts',(-7.51492677113112,71.0022170960235,0.));
#99697=CARTESIAN_POINT('Ctrl Pts',(-7.52448017749136,71.0229879558713,0.));
#99698=CARTESIAN_POINT('Ctrl Pts',(-7.53407321054254,71.0437901279722,0.));
#99699=CARTESIAN_POINT('Ctrl Pts',(-7.54370587521948,71.0646234624783,0.));
#99700=CARTESIAN_POINT('Ctrl Pts',(-7.55337817632873,71.0854878102203,0.));
#99701=CARTESIAN_POINT('Ctrl Pts',(-7.56309011855617,71.1063830227074,0.));
#99702=CARTESIAN_POINT('Ctrl Pts',(-7.57284170646866,71.1273089521218,0.));
#99703=CARTESIAN_POINT('Ctrl Pts',(-7.58263294451465,71.1482654513133,0.));
#99704=CARTESIAN_POINT('Ctrl Pts',(-7.5924638370186,71.1692523737887,0.));
#99705=CARTESIAN_POINT('Ctrl Pts',(-7.60233438818156,71.1902695737063,0.));
#99706=CARTESIAN_POINT('Ctrl Pts',(-7.61224460208887,71.2113169058778,0.));
#99707=CARTESIAN_POINT('Ctrl Pts',(-7.62219448271125,71.232394225762,0.));
#99708=CARTESIAN_POINT('Ctrl Pts',(-7.63218403390515,71.2535013894587,0.));
#99709=CARTESIAN_POINT('Ctrl Pts',(-7.64221325940672,71.2746382536974,0.));
#99710=CARTESIAN_POINT('Ctrl Pts',(-7.65228216283343,71.2958046758334,0.));
#99711=CARTESIAN_POINT('Ctrl Pts',(-7.66239074769119,71.3170005138474,0.));
#99712=CARTESIAN_POINT('Ctrl Pts',(-7.67253901737539,71.3382256263405,0.));
#99713=CARTESIAN_POINT('Ctrl Pts',(-7.68272697517103,71.3594798725294,0.));
#99714=CARTESIAN_POINT('Ctrl Pts',(-7.69295462424647,71.380763112236,0.));
#99715=CARTESIAN_POINT('Ctrl Pts',(-7.70322196765573,71.4020752058827,0.));
#99716=CARTESIAN_POINT('Ctrl Pts',(-7.71352900834538,71.4234160144943,0.));
#99717=CARTESIAN_POINT('Ctrl Pts',(-7.72387574915544,71.4447853996919,0.));
#99718=CARTESIAN_POINT('Ctrl Pts',(-7.73426219281932,71.4661832236881,0.));
#99719=CARTESIAN_POINT('Ctrl Pts',(-7.74468834195734,71.487609349277,0.));
#99720=CARTESIAN_POINT('Ctrl Pts',(-7.75515419907955,71.5090636398307,0.));
#99721=CARTESIAN_POINT('Ctrl Pts',(-7.76565976659218,71.5305459592987,0.));
#99722=CARTESIAN_POINT('Ctrl Pts',(-7.77620504679868,71.5520561722039,0.));
#99723=CARTESIAN_POINT('Ctrl Pts',(-7.78679004189935,71.5735941436366,0.));
#99724=CARTESIAN_POINT('Ctrl Pts',(-7.79741475398512,71.5951597392471,0.));
#99725=CARTESIAN_POINT('Ctrl Pts',(-7.80807918504017,71.616752825242,0.));
#99726=CARTESIAN_POINT('Ctrl Pts',(-7.81878333694856,71.638373268384,0.));
#99727=CARTESIAN_POINT('Ctrl Pts',(-7.82952721149504,71.6600209359869,0.));
#99728=CARTESIAN_POINT('Ctrl Pts',(-7.84031081036489,71.681695695912,0.));
#99729=CARTESIAN_POINT('Ctrl Pts',(-7.85113413513739,71.7033974165576,0.));
#99730=CARTESIAN_POINT('Ctrl Pts',(-7.8619971872883,71.7251259668573,0.));
#99731=CARTESIAN_POINT('Ctrl Pts',(-7.87289996819654,71.7468812162795,0.));
#99732=CARTESIAN_POINT('Ctrl Pts',(-7.88384247914522,71.768663034824,0.));
#99733=CARTESIAN_POINT('Ctrl Pts',(-7.89482472132135,71.7904712930172,0.));
#99734=CARTESIAN_POINT('Ctrl Pts',(-7.90584669580955,71.8123058619038,0.));
#99735=CARTESIAN_POINT('Ctrl Pts',(-7.91690840359371,71.8341666130424,0.));
#99736=CARTESIAN_POINT('Ctrl Pts',(-7.928009845564,71.8560534185071,0.));
#99737=CARTESIAN_POINT('Ctrl Pts',(-7.93915102251796,71.8779661508833,0.));
#99738=CARTESIAN_POINT('Ctrl Pts',(-7.95033193516046,71.8999046832642,0.));
#99739=CARTESIAN_POINT('Ctrl Pts',(-7.96155258409752,71.9218688892426,0.));
#99740=CARTESIAN_POINT('Ctrl Pts',(-7.97281296983702,71.9438586429072,0.));
#99741=CARTESIAN_POINT('Ctrl Pts',(-7.98411309279598,71.9658738188421,0.));
#99742=CARTESIAN_POINT('Ctrl Pts',(-7.99545295330182,71.9879142921248,0.));
#99743=CARTESIAN_POINT('Ctrl Pts',(-8.0068325515925,72.0099799383216,0.));
#99744=CARTESIAN_POINT('Ctrl Pts',(-8.0182518878107,72.0320706334802,0.));
#99745=CARTESIAN_POINT('Ctrl Pts',(-8.02971096200329,72.0541862541262,0.));
#99746=CARTESIAN_POINT('Ctrl Pts',(-8.04120977412891,72.0763266772632,0.));
#99747=CARTESIAN_POINT('Ctrl Pts',(-8.05274832405957,72.0984917803702,0.));
#99748=CARTESIAN_POINT('Ctrl Pts',(-8.06432661158089,72.1206814413985,0.));
#99749=CARTESIAN_POINT('Ctrl Pts',(-8.07594463638699,72.1428955387648,0.));
#99750=CARTESIAN_POINT('Ctrl Pts',(-8.08760239807815,72.165133951346,0.));
#99751=CARTESIAN_POINT('Ctrl Pts',(-8.09929989616874,72.18739655848,0.));
#99752=CARTESIAN_POINT('Ctrl Pts',(-8.11103713008922,72.2096832399626,0.));
#99753=CARTESIAN_POINT('Ctrl Pts',(-8.12281409918662,72.2319938760451,0.));
#99754=CARTESIAN_POINT('Ctrl Pts',(-8.13463080272029,72.2543283474279,0.));
#99755=CARTESIAN_POINT('Ctrl Pts',(-8.14648723985793,72.2766865352552,0.));
#99756=CARTESIAN_POINT('Ctrl Pts',(-8.15838340968328,72.2990683211155,0.));
#99757=CARTESIAN_POINT('Ctrl Pts',(-8.17031931119882,72.3214735870402,0.));
#99758=CARTESIAN_POINT('Ctrl Pts',(-8.18229494332622,72.3439022155007,0.));
#99759=CARTESIAN_POINT('Ctrl Pts',(-8.19431030490319,72.3663540894034,0.));
#99760=CARTESIAN_POINT('Ctrl Pts',(-8.20636539467782,72.3888290920845,0.));
#99761=CARTESIAN_POINT('Ctrl Pts',(-8.21846021131564,72.4113271073091,0.));
#99762=CARTESIAN_POINT('Ctrl Pts',(-8.23059475340354,72.4338480192701,0.));
#99763=CARTESIAN_POINT('Ctrl Pts',(-8.24276901945037,72.4563917125842,0.));
#99764=CARTESIAN_POINT('Ctrl Pts',(-8.25498300788493,72.4789580722871,0.));
#99765=CARTESIAN_POINT('Ctrl Pts',(-8.26723671704924,72.501546983825,0.));
#99766=CARTESIAN_POINT('Ctrl Pts',(-8.27953014520385,72.524158333056,0.));
#99767=CARTESIAN_POINT('Ctrl Pts',(-8.29186329053289,72.5467920062522,0.));
#99768=CARTESIAN_POINT('Ctrl Pts',(-8.30423615114455,72.5694478900983,0.));
#99769=CARTESIAN_POINT('Ctrl Pts',(-8.31664872507008,72.5921258716899,0.));
#99770=CARTESIAN_POINT('Ctrl Pts',(-8.32910101025653,72.614825838529,0.));
#99771=CARTESIAN_POINT('Ctrl Pts',(-8.34159300456965,72.6375476785208,0.));
#99772=CARTESIAN_POINT('Ctrl Pts',(-8.35412470580083,72.6602912799689,0.));
#99773=CARTESIAN_POINT('Ctrl Pts',(-8.36669611166834,72.68305653157,0.));
#99774=CARTESIAN_POINT('Ctrl Pts',(-8.37930721981735,72.7058433224072,0.));
#99775=CARTESIAN_POINT('Ctrl Pts',(-8.39195802781407,72.728651541938,0.));
#99776=CARTESIAN_POINT('Ctrl Pts',(-8.40464853314493,72.7514810799932,0.));
#99777=CARTESIAN_POINT('Ctrl Pts',(-8.41737873322353,72.7743318267876,0.));
#99778=CARTESIAN_POINT('Ctrl Pts',(-8.43014862539171,72.7972036729283,0.));
#99779=CARTESIAN_POINT('Ctrl Pts',(-8.44295820691907,72.8200965094197,0.));
#99780=CARTESIAN_POINT('Ctrl Pts',(-8.45580747499771,72.8430102276703,0.));
#99781=CARTESIAN_POINT('Ctrl Pts',(-8.46869642673763,72.8659447194918,0.));
#99782=CARTESIAN_POINT('Ctrl Pts',(-8.48162505917628,72.888899877077,0.));
#99783=CARTESIAN_POINT('Ctrl Pts',(-8.49459336928276,72.9118755929785,0.));
#99784=CARTESIAN_POINT('Ctrl Pts',(-8.50760135395979,72.9348717600837,0.));
#99785=CARTESIAN_POINT('Ctrl Pts',(-8.52064901004244,72.9578882715923,0.));
#99786=CARTESIAN_POINT('Ctrl Pts',(-8.53373633429303,72.9809250209843,0.));
#99787=CARTESIAN_POINT('Ctrl Pts',(-8.54686332340439,73.0039819020663,0.));
#99788=CARTESIAN_POINT('Ctrl Pts',(-8.56002997400096,73.0270588090193,0.));
#99789=CARTESIAN_POINT('Ctrl Pts',(-8.57323628263595,73.0501556364482,0.));
#99790=CARTESIAN_POINT('Ctrl Pts',(-8.58648224578723,73.073272279419,0.));
#99791=CARTESIAN_POINT('Ctrl Pts',(-8.59976785984539,73.0964086335226,0.));
#99792=CARTESIAN_POINT('Ctrl Pts',(-8.61309312111989,73.1195645948169,0.));
#99793=CARTESIAN_POINT('Ctrl Pts',(-8.62645802585475,73.142740059703,0.));
#99794=CARTESIAN_POINT('Ctrl Pts',(-8.63986257023735,73.165934924813,0.));
#99795=CARTESIAN_POINT('Ctrl Pts',(-8.65330675040535,73.1891490869057,0.));
#99796=CARTESIAN_POINT('Ctrl Pts',(-8.66679056245095,73.2123824427212,0.));
#99797=CARTESIAN_POINT('Ctrl Pts',(-8.68031400241884,73.2356348889704,0.));
#99798=CARTESIAN_POINT('Ctrl Pts',(-8.69387706629304,73.2589063226373,0.));
#99799=CARTESIAN_POINT('Ctrl Pts',(-8.70747974998245,73.282196641216,0.));
#99800=CARTESIAN_POINT('Ctrl Pts',(-8.72112204930232,73.3055057429744,0.));
#99801=CARTESIAN_POINT('Ctrl Pts',(-8.7348039599536,73.3288335271989,0.));
#99802=CARTESIAN_POINT('Ctrl Pts',(-8.74852547749736,73.3521798944595,0.));
#99803=CARTESIAN_POINT('Ctrl Pts',(-8.76228659740305,73.3755447460235,0.));
#99804=CARTESIAN_POINT('Ctrl Pts',(-8.77608731509304,73.3989279832808,0.));
#99805=CARTESIAN_POINT('Ctrl Pts',(-8.78992762598738,73.422329507112,0.));
#99806=CARTESIAN_POINT('Ctrl Pts',(-8.80380752553714,73.4457492173949,0.));
#99807=CARTESIAN_POINT('Ctrl Pts',(-8.81772700927593,73.4691870121608,0.));
#99808=CARTESIAN_POINT('Ctrl Pts',(-8.83168607277415,73.4926427882787,0.));
#99809=CARTESIAN_POINT('Ctrl Pts',(-8.84568471153894,73.5161164429765,0.));
#99810=CARTESIAN_POINT('Ctrl Pts',(-8.85972292092183,73.5396078751672,0.));
#99811=CARTESIAN_POINT('Ctrl Pts',(-8.87380069602955,73.5631169867113,0.));
#99812=CARTESIAN_POINT('Ctrl Pts',(-8.88791803160341,73.5866436840493,0.));
#99813=CARTESIAN_POINT('Ctrl Pts',(-8.90207492198871,73.6101878785868,0.));
#99814=CARTESIAN_POINT('Ctrl Pts',(-8.91424402151025,73.6303847393445,0.));
#99815=CARTESIAN_POINT('Ctrl Pts',(-8.92359518177556,73.6458786305789,0.));
#99816=CARTESIAN_POINT('Ctrl Pts',(-8.93011088816032,73.6566618621798,0.));
#99817=CARTESIAN_POINT('Ctrl Pts',(-8.93377955963992,73.6627293782263,0.));
#99818=CARTESIAN_POINT('Ctrl Pts',(-8.93459554655822,73.6640787197672,0.));
#99819=CARTESIAN_POINT('',(-6.95102489306926,69.6540253893192,12.));
#99820=CARTESIAN_POINT('',(-6.95102489306926,69.6540253893192,0.));
#99821=CARTESIAN_POINT('Ctrl Pts',(-8.93459554655822,73.6640787197672,12.));
#99822=CARTESIAN_POINT('Ctrl Pts',(-8.93377955963992,73.6627293782263,12.));
#99823=CARTESIAN_POINT('Ctrl Pts',(-8.93011088816032,73.6566618621798,12.));
#99824=CARTESIAN_POINT('Ctrl Pts',(-8.92359518177556,73.6458786305789,12.));
#99825=CARTESIAN_POINT('Ctrl Pts',(-8.91424402151025,73.6303847393445,12.));
#99826=CARTESIAN_POINT('Ctrl Pts',(-8.90207492198871,73.6101878785868,12.));
#99827=CARTESIAN_POINT('Ctrl Pts',(-8.88791803160341,73.5866436840493,12.));
#99828=CARTESIAN_POINT('Ctrl Pts',(-8.87380069602955,73.5631169867113,12.));
#99829=CARTESIAN_POINT('Ctrl Pts',(-8.85972292092183,73.5396078751672,12.));
#99830=CARTESIAN_POINT('Ctrl Pts',(-8.84568471153894,73.5161164429765,12.));
#99831=CARTESIAN_POINT('Ctrl Pts',(-8.83168607277415,73.4926427882787,12.));
#99832=CARTESIAN_POINT('Ctrl Pts',(-8.81772700927593,73.4691870121608,12.));
#99833=CARTESIAN_POINT('Ctrl Pts',(-8.80380752553714,73.4457492173949,12.));
#99834=CARTESIAN_POINT('Ctrl Pts',(-8.78992762598738,73.422329507112,12.));
#99835=CARTESIAN_POINT('Ctrl Pts',(-8.77608731509304,73.3989279832808,12.));
#99836=CARTESIAN_POINT('Ctrl Pts',(-8.76228659740305,73.3755447460235,12.));
#99837=CARTESIAN_POINT('Ctrl Pts',(-8.74852547749736,73.3521798944595,12.));
#99838=CARTESIAN_POINT('Ctrl Pts',(-8.7348039599536,73.3288335271989,12.));
#99839=CARTESIAN_POINT('Ctrl Pts',(-8.72112204930232,73.3055057429744,12.));
#99840=CARTESIAN_POINT('Ctrl Pts',(-8.70747974998245,73.282196641216,12.));
#99841=CARTESIAN_POINT('Ctrl Pts',(-8.69387706629304,73.2589063226373,12.));
#99842=CARTESIAN_POINT('Ctrl Pts',(-8.68031400241884,73.2356348889704,12.));
#99843=CARTESIAN_POINT('Ctrl Pts',(-8.66679056245095,73.2123824427212,12.));
#99844=CARTESIAN_POINT('Ctrl Pts',(-8.65330675040535,73.1891490869057,12.));
#99845=CARTESIAN_POINT('Ctrl Pts',(-8.63986257023735,73.165934924813,12.));
#99846=CARTESIAN_POINT('Ctrl Pts',(-8.62645802585475,73.142740059703,12.));
#99847=CARTESIAN_POINT('Ctrl Pts',(-8.61309312111989,73.1195645948169,12.));
#99848=CARTESIAN_POINT('Ctrl Pts',(-8.59976785984539,73.0964086335226,12.));
#99849=CARTESIAN_POINT('Ctrl Pts',(-8.58648224578723,73.073272279419,12.));
#99850=CARTESIAN_POINT('Ctrl Pts',(-8.57323628263595,73.0501556364482,12.));
#99851=CARTESIAN_POINT('Ctrl Pts',(-8.56002997400096,73.0270588090193,12.));
#99852=CARTESIAN_POINT('Ctrl Pts',(-8.54686332340439,73.0039819020663,12.));
#99853=CARTESIAN_POINT('Ctrl Pts',(-8.53373633429303,72.9809250209843,12.));
#99854=CARTESIAN_POINT('Ctrl Pts',(-8.52064901004244,72.9578882715923,12.));
#99855=CARTESIAN_POINT('Ctrl Pts',(-8.50760135395979,72.9348717600837,12.));
#99856=CARTESIAN_POINT('Ctrl Pts',(-8.49459336928276,72.9118755929785,12.));
#99857=CARTESIAN_POINT('Ctrl Pts',(-8.48162505917628,72.888899877077,12.));
#99858=CARTESIAN_POINT('Ctrl Pts',(-8.46869642673763,72.8659447194918,12.));
#99859=CARTESIAN_POINT('Ctrl Pts',(-8.45580747499771,72.8430102276703,12.));
#99860=CARTESIAN_POINT('Ctrl Pts',(-8.44295820691907,72.8200965094197,12.));
#99861=CARTESIAN_POINT('Ctrl Pts',(-8.43014862539171,72.7972036729283,12.));
#99862=CARTESIAN_POINT('Ctrl Pts',(-8.41737873322353,72.7743318267876,12.));
#99863=CARTESIAN_POINT('Ctrl Pts',(-8.40464853314493,72.7514810799932,12.));
#99864=CARTESIAN_POINT('Ctrl Pts',(-8.39195802781407,72.728651541938,12.));
#99865=CARTESIAN_POINT('Ctrl Pts',(-8.37930721981735,72.7058433224072,12.));
#99866=CARTESIAN_POINT('Ctrl Pts',(-8.36669611166834,72.68305653157,12.));
#99867=CARTESIAN_POINT('Ctrl Pts',(-8.35412470580083,72.6602912799689,12.));
#99868=CARTESIAN_POINT('Ctrl Pts',(-8.34159300456965,72.6375476785208,12.));
#99869=CARTESIAN_POINT('Ctrl Pts',(-8.32910101025653,72.614825838529,12.));
#99870=CARTESIAN_POINT('Ctrl Pts',(-8.31664872507008,72.5921258716899,12.));
#99871=CARTESIAN_POINT('Ctrl Pts',(-8.30423615114455,72.5694478900983,12.));
#99872=CARTESIAN_POINT('Ctrl Pts',(-8.29186329053289,72.5467920062522,12.));
#99873=CARTESIAN_POINT('Ctrl Pts',(-8.27953014520385,72.524158333056,12.));
#99874=CARTESIAN_POINT('Ctrl Pts',(-8.26723671704924,72.501546983825,12.));
#99875=CARTESIAN_POINT('Ctrl Pts',(-8.25498300788493,72.4789580722871,12.));
#99876=CARTESIAN_POINT('Ctrl Pts',(-8.24276901945037,72.4563917125842,12.));
#99877=CARTESIAN_POINT('Ctrl Pts',(-8.23059475340354,72.4338480192701,12.));
#99878=CARTESIAN_POINT('Ctrl Pts',(-8.21846021131564,72.4113271073091,12.));
#99879=CARTESIAN_POINT('Ctrl Pts',(-8.20636539467782,72.3888290920845,12.));
#99880=CARTESIAN_POINT('Ctrl Pts',(-8.19431030490319,72.3663540894034,12.));
#99881=CARTESIAN_POINT('Ctrl Pts',(-8.18229494332622,72.3439022155007,12.));
#99882=CARTESIAN_POINT('Ctrl Pts',(-8.17031931119882,72.3214735870402,12.));
#99883=CARTESIAN_POINT('Ctrl Pts',(-8.15838340968328,72.2990683211155,12.));
#99884=CARTESIAN_POINT('Ctrl Pts',(-8.14648723985793,72.2766865352552,12.));
#99885=CARTESIAN_POINT('Ctrl Pts',(-8.13463080272029,72.2543283474279,12.));
#99886=CARTESIAN_POINT('Ctrl Pts',(-8.12281409918662,72.2319938760451,12.));
#99887=CARTESIAN_POINT('Ctrl Pts',(-8.11103713008922,72.2096832399626,12.));
#99888=CARTESIAN_POINT('Ctrl Pts',(-8.09929989616874,72.18739655848,12.));
#99889=CARTESIAN_POINT('Ctrl Pts',(-8.08760239807815,72.165133951346,12.));
#99890=CARTESIAN_POINT('Ctrl Pts',(-8.07594463638699,72.1428955387648,12.));
#99891=CARTESIAN_POINT('Ctrl Pts',(-8.06432661158089,72.1206814413985,12.));
#99892=CARTESIAN_POINT('Ctrl Pts',(-8.05274832405957,72.0984917803702,12.));
#99893=CARTESIAN_POINT('Ctrl Pts',(-8.04120977412891,72.0763266772632,12.));
#99894=CARTESIAN_POINT('Ctrl Pts',(-8.02971096200329,72.0541862541262,12.));
#99895=CARTESIAN_POINT('Ctrl Pts',(-8.0182518878107,72.0320706334802,12.));
#99896=CARTESIAN_POINT('Ctrl Pts',(-8.0068325515925,72.0099799383216,12.));
#99897=CARTESIAN_POINT('Ctrl Pts',(-7.99545295330182,71.9879142921248,12.));
#99898=CARTESIAN_POINT('Ctrl Pts',(-7.98411309279598,71.9658738188421,12.));
#99899=CARTESIAN_POINT('Ctrl Pts',(-7.97281296983702,71.9438586429072,12.));
#99900=CARTESIAN_POINT('Ctrl Pts',(-7.96155258409752,71.9218688892426,12.));
#99901=CARTESIAN_POINT('Ctrl Pts',(-7.95033193516046,71.8999046832642,12.));
#99902=CARTESIAN_POINT('Ctrl Pts',(-7.93915102251796,71.8779661508833,12.));
#99903=CARTESIAN_POINT('Ctrl Pts',(-7.928009845564,71.8560534185071,12.));
#99904=CARTESIAN_POINT('Ctrl Pts',(-7.91690840359371,71.8341666130424,12.));
#99905=CARTESIAN_POINT('Ctrl Pts',(-7.90584669580955,71.8123058619038,12.));
#99906=CARTESIAN_POINT('Ctrl Pts',(-7.89482472132135,71.7904712930172,12.));
#99907=CARTESIAN_POINT('Ctrl Pts',(-7.88384247914522,71.768663034824,12.));
#99908=CARTESIAN_POINT('Ctrl Pts',(-7.87289996819654,71.7468812162795,12.));
#99909=CARTESIAN_POINT('Ctrl Pts',(-7.8619971872883,71.7251259668573,12.));
#99910=CARTESIAN_POINT('Ctrl Pts',(-7.85113413513739,71.7033974165576,12.));
#99911=CARTESIAN_POINT('Ctrl Pts',(-7.84031081036489,71.681695695912,12.));
#99912=CARTESIAN_POINT('Ctrl Pts',(-7.82952721149504,71.6600209359869,12.));
#99913=CARTESIAN_POINT('Ctrl Pts',(-7.81878333694856,71.638373268384,12.));
#99914=CARTESIAN_POINT('Ctrl Pts',(-7.80807918504017,71.616752825242,12.));
#99915=CARTESIAN_POINT('Ctrl Pts',(-7.79741475398512,71.5951597392471,12.));
#99916=CARTESIAN_POINT('Ctrl Pts',(-7.78679004189935,71.5735941436366,12.));
#99917=CARTESIAN_POINT('Ctrl Pts',(-7.77620504679868,71.5520561722039,12.));
#99918=CARTESIAN_POINT('Ctrl Pts',(-7.76565976659218,71.5305459592987,12.));
#99919=CARTESIAN_POINT('Ctrl Pts',(-7.75515419907955,71.5090636398307,12.));
#99920=CARTESIAN_POINT('Ctrl Pts',(-7.74468834195734,71.487609349277,12.));
#99921=CARTESIAN_POINT('Ctrl Pts',(-7.73426219281932,71.4661832236881,12.));
#99922=CARTESIAN_POINT('Ctrl Pts',(-7.72387574915544,71.4447853996919,12.));
#99923=CARTESIAN_POINT('Ctrl Pts',(-7.71352900834538,71.4234160144943,12.));
#99924=CARTESIAN_POINT('Ctrl Pts',(-7.70322196765573,71.4020752058827,12.));
#99925=CARTESIAN_POINT('Ctrl Pts',(-7.69295462424647,71.380763112236,12.));
#99926=CARTESIAN_POINT('Ctrl Pts',(-7.68272697517103,71.3594798725294,12.));
#99927=CARTESIAN_POINT('Ctrl Pts',(-7.67253901737539,71.3382256263405,12.));
#99928=CARTESIAN_POINT('Ctrl Pts',(-7.66239074769119,71.3170005138474,12.));
#99929=CARTESIAN_POINT('Ctrl Pts',(-7.65228216283343,71.2958046758334,12.));
#99930=CARTESIAN_POINT('Ctrl Pts',(-7.64221325940672,71.2746382536974,12.));
#99931=CARTESIAN_POINT('Ctrl Pts',(-7.63218403390515,71.2535013894587,12.));
#99932=CARTESIAN_POINT('Ctrl Pts',(-7.62219448271125,71.232394225762,12.));
#99933=CARTESIAN_POINT('Ctrl Pts',(-7.61224460208887,71.2113169058778,12.));
#99934=CARTESIAN_POINT('Ctrl Pts',(-7.60233438818156,71.1902695737063,12.));
#99935=CARTESIAN_POINT('Ctrl Pts',(-7.5924638370186,71.1692523737887,12.));
#99936=CARTESIAN_POINT('Ctrl Pts',(-7.58263294451465,71.1482654513133,12.));
#99937=CARTESIAN_POINT('Ctrl Pts',(-7.57284170646866,71.1273089521218,12.));
#99938=CARTESIAN_POINT('Ctrl Pts',(-7.56309011855617,71.1063830227074,12.));
#99939=CARTESIAN_POINT('Ctrl Pts',(-7.55337817632873,71.0854878102203,12.));
#99940=CARTESIAN_POINT('Ctrl Pts',(-7.54370587521948,71.0646234624783,12.));
#99941=CARTESIAN_POINT('Ctrl Pts',(-7.53407321054254,71.0437901279722,12.));
#99942=CARTESIAN_POINT('Ctrl Pts',(-7.52448017749136,71.0229879558713,12.));
#99943=CARTESIAN_POINT('Ctrl Pts',(-7.51492677113112,71.0022170960235,12.));
#99944=CARTESIAN_POINT('Ctrl Pts',(-7.50541298639948,70.9814776989637,12.));
#99945=CARTESIAN_POINT('Ctrl Pts',(-7.49593881811141,70.9607699159234,12.));
#99946=CARTESIAN_POINT('Ctrl Pts',(-7.48650426095823,70.9400938988373,12.));
#99947=CARTESIAN_POINT('Ctrl Pts',(-7.47710930950554,70.9194498003483,12.));
#99948=CARTESIAN_POINT('Ctrl Pts',(-7.46775395818519,70.8988377738088,12.));
#99949=CARTESIAN_POINT('Ctrl Pts',(-7.45843820129776,70.8782579732885,12.));
#99950=CARTESIAN_POINT('Ctrl Pts',(-7.44916203301645,70.8577105535841,12.));
#99951=CARTESIAN_POINT('Ctrl Pts',(-7.43992544738607,70.8371956702242,12.));
#99952=CARTESIAN_POINT('Ctrl Pts',(-7.43072843832008,70.8167134794738,12.));
#99953=CARTESIAN_POINT('Ctrl Pts',(-7.42157099959316,70.7962641383351,12.));
#99954=CARTESIAN_POINT('Ctrl Pts',(-7.41245312484487,70.7758478045576,12.));
#99955=CARTESIAN_POINT('Ctrl Pts',(-7.4033748075823,70.7554646366514,12.));
#99956=CARTESIAN_POINT('Ctrl Pts',(-7.39433604117891,70.735114793895,12.));
#99957=CARTESIAN_POINT('Ctrl Pts',(-7.38533681887033,70.7147984363424,12.));
#99958=CARTESIAN_POINT('Ctrl Pts',(-7.37637713374768,70.694515724827,12.));
#99959=CARTESIAN_POINT('Ctrl Pts',(-7.36745697876301,70.6742668209687,12.));
#99960=CARTESIAN_POINT('Ctrl Pts',(-7.35857634673055,70.6540518871775,12.));
#99961=CARTESIAN_POINT('Ctrl Pts',(-7.34973523032577,70.6338710866562,12.));
#99962=CARTESIAN_POINT('Ctrl Pts',(-7.34093362208008,70.6137245833996,12.));
#99963=CARTESIAN_POINT('Ctrl Pts',(-7.3321715143759,70.5936125421946,12.));
#99964=CARTESIAN_POINT('Ctrl Pts',(-7.3234488994522,70.5735351286476,12.));
#99965=CARTESIAN_POINT('Ctrl Pts',(-7.31476576940392,70.5534925092043,12.));
#99966=CARTESIAN_POINT('Ctrl Pts',(-7.30612211618053,70.5334848511681,12.));
#99967=CARTESIAN_POINT('Ctrl Pts',(-7.29751793157823,70.5135123227169,12.));
#99968=CARTESIAN_POINT('Ctrl Pts',(-7.28895320723862,70.4935750929058,12.));
#99969=CARTESIAN_POINT('Ctrl Pts',(-7.28042793465471,70.4736733316487,12.));
#99970=CARTESIAN_POINT('Ctrl Pts',(-7.27194210517063,70.4538072096992,12.));
#99971=CARTESIAN_POINT('Ctrl Pts',(-7.26349570998033,70.4339768986346,12.));
#99972=CARTESIAN_POINT('Ctrl Pts',(-7.25508874012043,70.4141825708178,12.));
#99973=CARTESIAN_POINT('Ctrl Pts',(-7.24672118647085,70.3944243994504,12.));
#99974=CARTESIAN_POINT('Ctrl Pts',(-7.23839303975607,70.3747025586552,12.));
#99975=CARTESIAN_POINT('Ctrl Pts',(-7.23010429054229,70.3550172235486,12.));
#99976=CARTESIAN_POINT('Ctrl Pts',(-7.22185492923191,70.3353685703112,12.));
#99977=CARTESIAN_POINT('Ctrl Pts',(-7.2136449460545,70.3157567762588,12.));
#99978=CARTESIAN_POINT('Ctrl Pts',(-7.20547433107483,70.2961820197077,12.));
#99979=CARTESIAN_POINT('Ctrl Pts',(-7.19734307419873,70.2766444798285,12.));
#99980=CARTESIAN_POINT('Ctrl Pts',(-7.18925116517555,70.2571443365192,12.));
#99981=CARTESIAN_POINT('Ctrl Pts',(-7.18119859359778,70.2376817702215,12.));
#99982=CARTESIAN_POINT('Ctrl Pts',(-7.17318534889716,70.2182569618994,12.));
#99983=CARTESIAN_POINT('Ctrl Pts',(-7.16521142033864,70.1988700934593,12.));
#99984=CARTESIAN_POINT('Ctrl Pts',(-7.15727679700933,70.1795213481185,12.));
#99985=CARTESIAN_POINT('Ctrl Pts',(-7.14938146780813,70.1602109107202,12.));
#99986=CARTESIAN_POINT('Ctrl Pts',(-7.14152542142374,70.1409389682424,12.));
#99987=CARTESIAN_POINT('Ctrl Pts',(-7.13370864634442,70.1217057094499,12.));
#99988=CARTESIAN_POINT('Ctrl Pts',(-7.12593113088904,70.1025113239495,12.));
#99989=CARTESIAN_POINT('Ctrl Pts',(-7.11819286322826,70.0833560013975,12.));
#99990=CARTESIAN_POINT('Ctrl Pts',(-7.11049383140446,70.0642399306869,12.));
#99991=CARTESIAN_POINT('Ctrl Pts',(-7.10283402335034,70.0451632990086,12.));
#99992=CARTESIAN_POINT('Ctrl Pts',(-7.09521342684249,70.0261262936388,12.));
#99993=CARTESIAN_POINT('Ctrl Pts',(-7.08763202944246,70.0071291040766,12.));
#99994=CARTESIAN_POINT('Ctrl Pts',(-7.08008981844652,69.988171923788,12.));
#99995=CARTESIAN_POINT('Ctrl Pts',(-7.07258678080831,69.9692549527296,12.));
#99996=CARTESIAN_POINT('Ctrl Pts',(-7.0651229031285,69.9503783975727,12.));
#99997=CARTESIAN_POINT('Ctrl Pts',(-7.05769817180857,69.9315424664291,12.));
#99998=CARTESIAN_POINT('Ctrl Pts',(-7.05031257318115,69.9127473642099,12.));
#99999=CARTESIAN_POINT('Ctrl Pts',(-7.04296609362166,69.8939932885841,12.));
#100000=CARTESIAN_POINT('Ctrl Pts',(-7.03565871972221,69.8752804235238,
12.));
#100001=CARTESIAN_POINT('Ctrl Pts',(-7.02839043811812,69.8566089455375,
12.));
#100002=CARTESIAN_POINT('Ctrl Pts',(-7.02116123514452,69.8379790360518,
12.));
#100003=CARTESIAN_POINT('Ctrl Pts',(-7.01397109655455,69.8193908913722,
12.));
#100004=CARTESIAN_POINT('Ctrl Pts',(-7.00682000718151,69.8008447346863,
12.));
#100005=CARTESIAN_POINT('Ctrl Pts',(-6.99970795069476,69.782340824259,12.));
#100006=CARTESIAN_POINT('Ctrl Pts',(-6.9926349102794,69.7638794280419,12.));
#100007=CARTESIAN_POINT('Ctrl Pts',(-6.98560086924214,69.7454607995607,
12.));
#100008=CARTESIAN_POINT('Ctrl Pts',(-6.97860581164527,69.7270851557366,
12.));
#100009=CARTESIAN_POINT('Ctrl Pts',(-6.9716497229144,69.7087526479973,12.));
#100010=CARTESIAN_POINT('Ctrl Pts',(-6.96473259049513,69.6904633605421,
12.));
#100011=CARTESIAN_POINT('Ctrl Pts',(-6.95923004173591,69.6758665380378,
12.));
#100012=CARTESIAN_POINT('Ctrl Pts',(-6.955120653176,69.664938391983,12.));
#100013=CARTESIAN_POINT('Ctrl Pts',(-6.95238884849025,69.6576616146467,
12.));
#100014=CARTESIAN_POINT('Ctrl Pts',(-6.95102489306926,69.6540253893192,
12.));
#100015=CARTESIAN_POINT('Ctrl Pts',(-10.4355099267296,73.4664795929939,
-5.55111512312578E-16));
#100016=CARTESIAN_POINT('Ctrl Pts',(-10.4355099267296,73.4664795929939,
4.));
#100017=CARTESIAN_POINT('Ctrl Pts',(-10.4355099267296,73.4664795929939,
8.));
#100018=CARTESIAN_POINT('Ctrl Pts',(-10.4355099267296,73.4664795929939,
12.));
#100019=CARTESIAN_POINT('Ctrl Pts',(-10.4049225807075,73.5720190200068,
-5.55111512312578E-16));
#100020=CARTESIAN_POINT('Ctrl Pts',(-10.4049225807075,73.5720190200068,
4.));
#100021=CARTESIAN_POINT('Ctrl Pts',(-10.4049225807075,73.5720190200068,
8.));
#100022=CARTESIAN_POINT('Ctrl Pts',(-10.4049225807075,73.5720190200068,
12.));
#100023=CARTESIAN_POINT('Ctrl Pts',(-10.2883434191783,73.7377969500799,
-5.55111512312578E-16));
#100024=CARTESIAN_POINT('Ctrl Pts',(-10.2883434191783,73.7377969500799,
4.00000000000001));
#100025=CARTESIAN_POINT('Ctrl Pts',(-10.2883434191783,73.7377969500799,
7.99999999999999));
#100026=CARTESIAN_POINT('Ctrl Pts',(-10.2883434191783,73.7377969500799,
12.));
#100027=CARTESIAN_POINT('Ctrl Pts',(-10.1042001607579,73.8116652760546,
-5.55111512312578E-16));
#100028=CARTESIAN_POINT('Ctrl Pts',(-10.1042001607579,73.8116652760546,
4.));
#100029=CARTESIAN_POINT('Ctrl Pts',(-10.1042001607579,73.8116652760546,
8.00000000000001));
#100030=CARTESIAN_POINT('Ctrl Pts',(-10.1042001607579,73.8116652760546,
12.));
#100031=CARTESIAN_POINT('Ctrl Pts',(-10.0225374821233,73.8227522002495,
-5.55111512312578E-16));
#100032=CARTESIAN_POINT('Ctrl Pts',(-10.0225374821233,73.8227522002495,
4.));
#100033=CARTESIAN_POINT('Ctrl Pts',(-10.0225374821233,73.8227522002495,
8.));
#100034=CARTESIAN_POINT('Ctrl Pts',(-10.0225374821233,73.8227522002495,
12.));
#100035=CARTESIAN_POINT('',(-10.4355099267296,73.4664795929939,0.));
#100036=CARTESIAN_POINT('',(-10.0225374821233,73.8227522002494,2.77555756156289E-16));
#100037=CARTESIAN_POINT('Ctrl Pts',(-10.4355099267296,73.4664795929939,
4.16333634234434E-16));
#100038=CARTESIAN_POINT('Ctrl Pts',(-10.4049225807075,73.5720190200068,
4.16333634234433E-16));
#100039=CARTESIAN_POINT('Ctrl Pts',(-10.3383059169765,73.6667492657628,
4.16333634234434E-16));
#100040=CARTESIAN_POINT('Ctrl Pts',(-10.2496275073219,73.7314682122214,
4.16333634234434E-16));
#100041=CARTESIAN_POINT('Ctrl Pts',(-10.1831187000809,73.7800074220654,
4.16333634234434E-16));
#100042=CARTESIAN_POINT('Ctrl Pts',(-10.1042001607579,73.8116652760546,
4.16333634234433E-16));
#100043=CARTESIAN_POINT('Ctrl Pts',(-10.0225374821233,73.8227522002495,
4.16333634234434E-16));
#100044=CARTESIAN_POINT('',(-10.0225374821233,73.8227522002494,12.));
#100045=CARTESIAN_POINT('Ctrl Pts',(-10.0225374821233,73.8227522002495,
-5.55111512312578E-16));
#100046=CARTESIAN_POINT('Ctrl Pts',(-10.0225374821233,73.8227522002495,
4.));
#100047=CARTESIAN_POINT('Ctrl Pts',(-10.0225374821233,73.8227522002495,
8.));
#100048=CARTESIAN_POINT('Ctrl Pts',(-10.0225374821233,73.8227522002495,
12.));
#100049=CARTESIAN_POINT('',(-10.4355099267296,73.4664795929939,12.));
#100050=CARTESIAN_POINT('Ctrl Pts',(-10.0225374821233,73.8227522002495,
12.));
#100051=CARTESIAN_POINT('Ctrl Pts',(-10.1042001607579,73.8116652760546,
12.));
#100052=CARTESIAN_POINT('Ctrl Pts',(-10.1831187000809,73.7800074220654,
12.));
#100053=CARTESIAN_POINT('Ctrl Pts',(-10.2496275073219,73.7314682122214,
12.));
#100054=CARTESIAN_POINT('Ctrl Pts',(-10.3383059169765,73.6667492657628,
12.));
#100055=CARTESIAN_POINT('Ctrl Pts',(-10.4049225807075,73.5720190200068,
12.));
#100056=CARTESIAN_POINT('Ctrl Pts',(-10.4355099267296,73.4664795929939,
12.));
#100057=CARTESIAN_POINT('Ctrl Pts',(-10.4355099267296,73.4664795929939,
12.));
#100058=CARTESIAN_POINT('Ctrl Pts',(-10.4355099267296,73.4664795929939,
8.));
#100059=CARTESIAN_POINT('Ctrl Pts',(-10.4355099267296,73.4664795929939,
4.));
#100060=CARTESIAN_POINT('Ctrl Pts',(-10.4355099267296,73.4664795929939,
-5.55111512312578E-16));
#100061=CARTESIAN_POINT('Origin',(-4.90253386731614E-11,3.71623968689858E-10,
0.));
#100062=CARTESIAN_POINT('Origin',(-4.90253386731614E-11,3.71623968689858E-10,
12.));
#100063=CARTESIAN_POINT('Origin',(-4.90253386731614E-11,3.71623968689858E-10,
0.));
#100064=CARTESIAN_POINT('Ctrl Pts',(-2.94891377268295,74.4416140848738,
0.));
#100065=CARTESIAN_POINT('Ctrl Pts',(-2.94891377268295,74.4416140848738,
4.));
#100066=CARTESIAN_POINT('Ctrl Pts',(-2.94891377268296,74.4416140848738,
8.));
#100067=CARTESIAN_POINT('Ctrl Pts',(-2.94891377268296,74.4416140848738,
12.));
#100068=CARTESIAN_POINT('Ctrl Pts',(-2.83911742169671,74.4459635334396,
0.));
#100069=CARTESIAN_POINT('Ctrl Pts',(-2.83911742169671,74.4459635334396,
4.));
#100070=CARTESIAN_POINT('Ctrl Pts',(-2.83911742169673,74.4459635334396,
8.00000000000001));
#100071=CARTESIAN_POINT('Ctrl Pts',(-2.83911742169673,74.4459635334396,
12.));
#100072=CARTESIAN_POINT('Ctrl Pts',(-2.64498412359367,74.3877786926473,
0.));
#100073=CARTESIAN_POINT('Ctrl Pts',(-2.64498412359367,74.3877786926473,
4.));
#100074=CARTESIAN_POINT('Ctrl Pts',(-2.6449841235937,74.3877786926473,7.99999999999999));
#100075=CARTESIAN_POINT('Ctrl Pts',(-2.6449841235937,74.3877786926473,12.));
#100076=CARTESIAN_POINT('Ctrl Pts',(-2.51668625693817,74.2364344282704,
0.));
#100077=CARTESIAN_POINT('Ctrl Pts',(-2.51668625693817,74.2364344282704,
4.));
#100078=CARTESIAN_POINT('Ctrl Pts',(-2.51668625693821,74.2364344282705,
8.00000000000001));
#100079=CARTESIAN_POINT('Ctrl Pts',(-2.51668625693821,74.2364344282705,
12.));
#100080=CARTESIAN_POINT('Ctrl Pts',(-2.48034921843231,74.1624659714559,
0.));
#100081=CARTESIAN_POINT('Ctrl Pts',(-2.48034921843231,74.1624659714559,
4.));
#100082=CARTESIAN_POINT('Ctrl Pts',(-2.48034921843235,74.1624659714559,
8.));
#100083=CARTESIAN_POINT('Ctrl Pts',(-2.48034921843235,74.1624659714559,
12.));
#100084=CARTESIAN_POINT('',(-2.94891377268295,74.4416140848738,0.));
#100085=CARTESIAN_POINT('',(-2.48034921843244,74.1624659714558,0.));
#100086=CARTESIAN_POINT('Ctrl Pts',(-2.94891377268295,74.4416140848738,
1.38777878078145E-16));
#100087=CARTESIAN_POINT('Ctrl Pts',(-2.83911742169671,74.4459635334396,
1.38777878078145E-16));
#100088=CARTESIAN_POINT('Ctrl Pts',(-2.72818410849497,74.4127150529868,
1.38777878078145E-16));
#100089=CARTESIAN_POINT('Ctrl Pts',(-2.63874807903121,74.3490471689147,
1.38777878078145E-16));
#100090=CARTESIAN_POINT('Ctrl Pts',(-2.57167105693338,74.3012962558605,
1.38777878078145E-16));
#100091=CARTESIAN_POINT('Ctrl Pts',(-2.51668625693817,74.2364344282704,
1.38777878078144E-16));
#100092=CARTESIAN_POINT('Ctrl Pts',(-2.48034921843231,74.1624659714559,
1.38777878078145E-16));
#100093=CARTESIAN_POINT('',(-2.48034921843246,74.1624659714559,12.));
#100094=CARTESIAN_POINT('Ctrl Pts',(-2.48034921843231,74.1624659714559,
0.));
#100095=CARTESIAN_POINT('Ctrl Pts',(-2.48034921843231,74.1624659714559,
4.));
#100096=CARTESIAN_POINT('Ctrl Pts',(-2.48034921843235,74.1624659714559,
8.));
#100097=CARTESIAN_POINT('Ctrl Pts',(-2.48034921843235,74.1624659714559,
12.));
#100098=CARTESIAN_POINT('',(-2.94891377268296,74.4416140848738,12.));
#100099=CARTESIAN_POINT('Ctrl Pts',(-2.48034921843235,74.1624659714559,
12.));
#100100=CARTESIAN_POINT('Ctrl Pts',(-2.51668625693821,74.2364344282705,
12.));
#100101=CARTESIAN_POINT('Ctrl Pts',(-2.57167105693342,74.3012962558605,
12.));
#100102=CARTESIAN_POINT('Ctrl Pts',(-2.63874807903124,74.3490471689147,
12.));
#100103=CARTESIAN_POINT('Ctrl Pts',(-2.728184108495,74.4127150529868,12.));
#100104=CARTESIAN_POINT('Ctrl Pts',(-2.83911742169673,74.4459635334396,
12.));
#100105=CARTESIAN_POINT('Ctrl Pts',(-2.94891377268296,74.4416140848738,
12.));
#100106=CARTESIAN_POINT('Ctrl Pts',(-2.94891377268296,74.4416140848738,
12.));
#100107=CARTESIAN_POINT('Ctrl Pts',(-2.94891377268296,74.4416140848738,
8.));
#100108=CARTESIAN_POINT('Ctrl Pts',(-2.94891377268295,74.4416140848738,
4.));
#100109=CARTESIAN_POINT('Ctrl Pts',(-2.94891377268295,74.4416140848738,
0.));
#100110=CARTESIAN_POINT('Ctrl Pts',(-0.853825826608985,69.9947925310006,
0.));
#100111=CARTESIAN_POINT('Ctrl Pts',(-0.853825826608985,69.9947925310006,
12.));
#100112=CARTESIAN_POINT('Ctrl Pts',(-0.854867673848596,69.9985337959407,
0.));
#100113=CARTESIAN_POINT('Ctrl Pts',(-0.854867673848596,69.9985337959407,
12.));
#100114=CARTESIAN_POINT('Ctrl Pts',(-0.856954870259207,70.0060209754087,
0.));
#100115=CARTESIAN_POINT('Ctrl Pts',(-0.856954870259207,70.0060209754087,
12.));
#100116=CARTESIAN_POINT('Ctrl Pts',(-0.860096170668736,70.0172656933806,
0.));
#100117=CARTESIAN_POINT('Ctrl Pts',(-0.860096170668736,70.0172656933806,
12.));
#100118=CARTESIAN_POINT('Ctrl Pts',(-0.864305583661547,70.0322865492925,
0.));
#100119=CARTESIAN_POINT('Ctrl Pts',(-0.864305583661547,70.0322865492925,
12.));
#100120=CARTESIAN_POINT('Ctrl Pts',(-0.869602377871126,70.051109108301,
0.));
#100121=CARTESIAN_POINT('Ctrl Pts',(-0.869602377871126,70.051109108301,
12.));
#100122=CARTESIAN_POINT('Ctrl Pts',(-0.874934213255839,70.0699781183935,
0.));
#100123=CARTESIAN_POINT('Ctrl Pts',(-0.874934213255839,70.0699781183935,
12.));
#100124=CARTESIAN_POINT('Ctrl Pts',(-0.880301109660729,70.0888934967855,
0.));
#100125=CARTESIAN_POINT('Ctrl Pts',(-0.880301109660729,70.0888934967855,
12.));
#100126=CARTESIAN_POINT('Ctrl Pts',(-0.885703094802537,70.1078550938958,
0.));
#100127=CARTESIAN_POINT('Ctrl Pts',(-0.885703094802537,70.1078550938958,
12.));
#100128=CARTESIAN_POINT('Ctrl Pts',(-0.891140203464243,70.1268626950175,
0.));
#100129=CARTESIAN_POINT('Ctrl Pts',(-0.891140203464243,70.1268626950175,
12.));
#100130=CARTESIAN_POINT('Ctrl Pts',(-0.896612474371846,70.1459160490446,
0.));
#100131=CARTESIAN_POINT('Ctrl Pts',(-0.896612474371846,70.1459160490446,
12.));
#100132=CARTESIAN_POINT('Ctrl Pts',(-0.902119947629773,70.1650148905109,
0.));
#100133=CARTESIAN_POINT('Ctrl Pts',(-0.902119947629773,70.1650148905109,
12.));
#100134=CARTESIAN_POINT('Ctrl Pts',(-0.907662662015787,70.1841589635574,
0.));
#100135=CARTESIAN_POINT('Ctrl Pts',(-0.907662662015787,70.1841589635574,
12.));
#100136=CARTESIAN_POINT('Ctrl Pts',(-0.913240652090982,70.2033480471676,
0.));
#100137=CARTESIAN_POINT('Ctrl Pts',(-0.913240652090982,70.2033480471676,
12.));
#100138=CARTESIAN_POINT('Ctrl Pts',(-0.91885394915712,70.2225819470248,
0.));
#100139=CARTESIAN_POINT('Ctrl Pts',(-0.91885394915712,70.2225819470248,
12.));
#100140=CARTESIAN_POINT('Ctrl Pts',(-0.924502582639457,70.2418604835837,
0.));
#100141=CARTESIAN_POINT('Ctrl Pts',(-0.924502582639457,70.2418604835837,
12.));
#100142=CARTESIAN_POINT('Ctrl Pts',(-0.930186581235549,70.2611834821724,
0.));
#100143=CARTESIAN_POINT('Ctrl Pts',(-0.930186581235549,70.2611834821724,
12.));
#100144=CARTESIAN_POINT('Ctrl Pts',(-0.935905974336482,70.2805507606872,
0.));
#100145=CARTESIAN_POINT('Ctrl Pts',(-0.935905974336482,70.2805507606872,
12.));
#100146=CARTESIAN_POINT('Ctrl Pts',(-0.941660792742981,70.299962123399,
0.));
#100147=CARTESIAN_POINT('Ctrl Pts',(-0.941660792742981,70.299962123399,
12.));
#100148=CARTESIAN_POINT('Ctrl Pts',(-0.947451067929606,70.3194173673674,
0.));
#100149=CARTESIAN_POINT('Ctrl Pts',(-0.947451067929606,70.3194173673674,
12.));
#100150=CARTESIAN_POINT('Ctrl Pts',(-0.953276831581243,70.338916286458,
0.));
#100151=CARTESIAN_POINT('Ctrl Pts',(-0.953276831581243,70.338916286458,
12.));
#100152=CARTESIAN_POINT('Ctrl Pts',(-0.959138115058833,70.3584586759536,
0.));
#100153=CARTESIAN_POINT('Ctrl Pts',(-0.959138115058833,70.3584586759536,
12.));
#100154=CARTESIAN_POINT('Ctrl Pts',(-0.965034948786451,70.3780443377956,
0.));
#100155=CARTESIAN_POINT('Ctrl Pts',(-0.965034948786451,70.3780443377956,
12.));
#100156=CARTESIAN_POINT('Ctrl Pts',(-0.970967362281175,70.3976730803614,
0.));
#100157=CARTESIAN_POINT('Ctrl Pts',(-0.970967362281175,70.3976730803614,
12.));
#100158=CARTESIAN_POINT('Ctrl Pts',(-0.976935384450043,70.417344715957,
0.));
#100159=CARTESIAN_POINT('Ctrl Pts',(-0.976935384450043,70.417344715957,
12.));
#100160=CARTESIAN_POINT('Ctrl Pts',(-0.982939043792157,70.4370590590842,
0.));
#100161=CARTESIAN_POINT('Ctrl Pts',(-0.982939043792157,70.4370590590842,
12.));
#100162=CARTESIAN_POINT('Ctrl Pts',(-0.98897836864365,70.4568159243163,
0.));
#100163=CARTESIAN_POINT('Ctrl Pts',(-0.98897836864365,70.4568159243163,
12.));
#100164=CARTESIAN_POINT('Ctrl Pts',(-0.995053387379757,70.4766151245212,
0.));
#100165=CARTESIAN_POINT('Ctrl Pts',(-0.995053387379757,70.4766151245212,
12.));
#100166=CARTESIAN_POINT('Ctrl Pts',(-1.00116412831442,70.4964564717953,
0.));
#100167=CARTESIAN_POINT('Ctrl Pts',(-1.00116412831442,70.4964564717953,
12.));
#100168=CARTESIAN_POINT('Ctrl Pts',(-1.00731061960968,70.5163397782713,
0.));
#100169=CARTESIAN_POINT('Ctrl Pts',(-1.00731061960968,70.5163397782713,
12.));
#100170=CARTESIAN_POINT('Ctrl Pts',(-1.01349288918537,70.5362648569061,
0.));
#100171=CARTESIAN_POINT('Ctrl Pts',(-1.01349288918537,70.5362648569061,
12.));
#100172=CARTESIAN_POINT('Ctrl Pts',(-1.01971096460597,70.556231522419,0.));
#100173=CARTESIAN_POINT('Ctrl Pts',(-1.01971096460597,70.556231522419,12.));
#100174=CARTESIAN_POINT('Ctrl Pts',(-1.02596487304049,70.5762395916377,
0.));
#100175=CARTESIAN_POINT('Ctrl Pts',(-1.02596487304049,70.5762395916377,
12.));
#100176=CARTESIAN_POINT('Ctrl Pts',(-1.0322546413287,70.5962888829934,0.));
#100177=CARTESIAN_POINT('Ctrl Pts',(-1.0322546413287,70.5962888829934,12.));
#100178=CARTESIAN_POINT('Ctrl Pts',(-1.03858029601904,70.6163792162073,
0.));
#100179=CARTESIAN_POINT('Ctrl Pts',(-1.03858029601904,70.6163792162073,
12.));
#100180=CARTESIAN_POINT('Ctrl Pts',(-1.04494186341156,70.6365104119252,
0.));
#100181=CARTESIAN_POINT('Ctrl Pts',(-1.04494186341156,70.6365104119252,
12.));
#100182=CARTESIAN_POINT('Ctrl Pts',(-1.05133936960072,70.6566822912991,
0.));
#100183=CARTESIAN_POINT('Ctrl Pts',(-1.05133936960072,70.6566822912991,
12.));
#100184=CARTESIAN_POINT('Ctrl Pts',(-1.0577728404773,70.676894676009,0.));
#100185=CARTESIAN_POINT('Ctrl Pts',(-1.0577728404773,70.676894676009,12.));
#100186=CARTESIAN_POINT('Ctrl Pts',(-1.06424230171281,70.6971473884459,
0.));
#100187=CARTESIAN_POINT('Ctrl Pts',(-1.06424230171281,70.6971473884459,
12.));
#100188=CARTESIAN_POINT('Ctrl Pts',(-1.07074777874596,70.7174402518378,
0.));
#100189=CARTESIAN_POINT('Ctrl Pts',(-1.07074777874596,70.7174402518378,
12.));
#100190=CARTESIAN_POINT('Ctrl Pts',(-1.07728929676408,70.7377730903953,
0.));
#100191=CARTESIAN_POINT('Ctrl Pts',(-1.07728929676408,70.7377730903953,
12.));
#100192=CARTESIAN_POINT('Ctrl Pts',(-1.08386688068342,70.7581457294447,
0.));
#100193=CARTESIAN_POINT('Ctrl Pts',(-1.08386688068342,70.7581457294447,
12.));
#100194=CARTESIAN_POINT('Ctrl Pts',(-1.09048055516427,70.7785579953583,
0.));
#100195=CARTESIAN_POINT('Ctrl Pts',(-1.09048055516427,70.7785579953583,
12.));
#100196=CARTESIAN_POINT('Ctrl Pts',(-1.09713034462265,70.799009715484,0.));
#100197=CARTESIAN_POINT('Ctrl Pts',(-1.09713034462265,70.799009715484,12.));
#100198=CARTESIAN_POINT('Ctrl Pts',(-1.10381627323947,70.8195007180745,
0.));
#100199=CARTESIAN_POINT('Ctrl Pts',(-1.10381627323947,70.8195007180745,
12.));
#100200=CARTESIAN_POINT('Ctrl Pts',(-1.1105383649664,70.8400308322037,0.));
#100201=CARTESIAN_POINT('Ctrl Pts',(-1.1105383649664,70.8400308322037,12.));
#100202=CARTESIAN_POINT('Ctrl Pts',(-1.11729664352993,70.8605998877149,
0.));
#100203=CARTESIAN_POINT('Ctrl Pts',(-1.11729664352993,70.8605998877149,
12.));
#100204=CARTESIAN_POINT('Ctrl Pts',(-1.12409113243514,70.8812077152586,
0.));
#100205=CARTESIAN_POINT('Ctrl Pts',(-1.12409113243514,70.8812077152586,
12.));
#100206=CARTESIAN_POINT('Ctrl Pts',(-1.13092185496565,70.9018541463089,
0.));
#100207=CARTESIAN_POINT('Ctrl Pts',(-1.13092185496565,70.9018541463089,
12.));
#100208=CARTESIAN_POINT('Ctrl Pts',(-1.13778883418214,70.9225390131826,
0.));
#100209=CARTESIAN_POINT('Ctrl Pts',(-1.13778883418214,70.9225390131826,
12.));
#100210=CARTESIAN_POINT('Ctrl Pts',(-1.14469209291489,70.9432621490566,
0.));
#100211=CARTESIAN_POINT('Ctrl Pts',(-1.14469209291489,70.9432621490566,
12.));
#100212=CARTESIAN_POINT('Ctrl Pts',(-1.15163165376524,70.9640233879659,
0.));
#100213=CARTESIAN_POINT('Ctrl Pts',(-1.15163165376524,70.9640233879659,
12.));
#100214=CARTESIAN_POINT('Ctrl Pts',(-1.15860753911485,70.9848225647871,
0.));
#100215=CARTESIAN_POINT('Ctrl Pts',(-1.15860753911485,70.9848225647871,
12.));
#100216=CARTESIAN_POINT('Ctrl Pts',(-1.1656197711288,71.0056595152204,0.));
#100217=CARTESIAN_POINT('Ctrl Pts',(-1.1656197711288,71.0056595152204,12.));
#100218=CARTESIAN_POINT('Ctrl Pts',(-1.17266837175777,71.0265340757699,
0.));
#100219=CARTESIAN_POINT('Ctrl Pts',(-1.17266837175777,71.0265340757699,
12.));
#100220=CARTESIAN_POINT('Ctrl Pts',(-1.17975336273504,71.0474460837159,
0.));
#100221=CARTESIAN_POINT('Ctrl Pts',(-1.17975336273504,71.0474460837159,
12.));
#100222=CARTESIAN_POINT('Ctrl Pts',(-1.18687476558133,71.0683953771149,
0.));
#100223=CARTESIAN_POINT('Ctrl Pts',(-1.18687476558133,71.0683953771149,
12.));
#100224=CARTESIAN_POINT('Ctrl Pts',(-1.19403260161002,71.089381794801,0.));
#100225=CARTESIAN_POINT('Ctrl Pts',(-1.19403260161002,71.089381794801,12.));
#100226=CARTESIAN_POINT('Ctrl Pts',(-1.20122689192836,71.1104051763839,
0.));
#100227=CARTESIAN_POINT('Ctrl Pts',(-1.20122689192836,71.1104051763839,
12.));
#100228=CARTESIAN_POINT('Ctrl Pts',(-1.20845765743648,71.1314653622442,
0.));
#100229=CARTESIAN_POINT('Ctrl Pts',(-1.20845765743648,71.1314653622442,
12.));
#100230=CARTESIAN_POINT('Ctrl Pts',(-1.21572491882263,71.1525621935267,
0.));
#100231=CARTESIAN_POINT('Ctrl Pts',(-1.21572491882263,71.1525621935267,
12.));
#100232=CARTESIAN_POINT('Ctrl Pts',(-1.22302869657018,71.1736955121362,
0.));
#100233=CARTESIAN_POINT('Ctrl Pts',(-1.22302869657018,71.1736955121362,
12.));
#100234=CARTESIAN_POINT('Ctrl Pts',(-1.23036901096239,71.194865160732,0.));
#100235=CARTESIAN_POINT('Ctrl Pts',(-1.23036901096239,71.194865160732,12.));
#100236=CARTESIAN_POINT('Ctrl Pts',(-1.23774588208427,71.2160709827191,
0.));
#100237=CARTESIAN_POINT('Ctrl Pts',(-1.23774588208427,71.2160709827191,
12.));
#100238=CARTESIAN_POINT('Ctrl Pts',(-1.24515932982113,71.2373128222352,
0.));
#100239=CARTESIAN_POINT('Ctrl Pts',(-1.24515932982113,71.2373128222352,
12.));
#100240=CARTESIAN_POINT('Ctrl Pts',(-1.25260937385569,71.2585905241406,
0.));
#100241=CARTESIAN_POINT('Ctrl Pts',(-1.25260937385569,71.2585905241406,
12.));
#100242=CARTESIAN_POINT('Ctrl Pts',(-1.26009603367571,71.2799039340175,
0.));
#100243=CARTESIAN_POINT('Ctrl Pts',(-1.26009603367571,71.2799039340175,
12.));
#100244=CARTESIAN_POINT('Ctrl Pts',(-1.26761932857724,71.3012528981661,
0.));
#100245=CARTESIAN_POINT('Ctrl Pts',(-1.26761932857724,71.3012528981661,
12.));
#100246=CARTESIAN_POINT('Ctrl Pts',(-1.27517927766608,71.3226372635996,
0.));
#100247=CARTESIAN_POINT('Ctrl Pts',(-1.27517927766608,71.3226372635996,
12.));
#100248=CARTESIAN_POINT('Ctrl Pts',(-1.28277589985472,71.3440568780347,
0.));
#100249=CARTESIAN_POINT('Ctrl Pts',(-1.28277589985472,71.3440568780347,
12.));
#100250=CARTESIAN_POINT('Ctrl Pts',(-1.29040921386059,71.3655115898827,
0.));
#100251=CARTESIAN_POINT('Ctrl Pts',(-1.29040921386059,71.3655115898827,
12.));
#100252=CARTESIAN_POINT('Ctrl Pts',(-1.29807923821414,71.3870012482499,
0.));
#100253=CARTESIAN_POINT('Ctrl Pts',(-1.29807923821414,71.3870012482499,
12.));
#100254=CARTESIAN_POINT('Ctrl Pts',(-1.3057859912614,71.4085257029322,0.));
#100255=CARTESIAN_POINT('Ctrl Pts',(-1.3057859912614,71.4085257029322,12.));
#100256=CARTESIAN_POINT('Ctrl Pts',(-1.31352949116537,71.4300848044087,
0.));
#100257=CARTESIAN_POINT('Ctrl Pts',(-1.31352949116537,71.4300848044087,
12.));
#100258=CARTESIAN_POINT('Ctrl Pts',(-1.32130975590226,71.4516784038317,
0.));
#100259=CARTESIAN_POINT('Ctrl Pts',(-1.32130975590226,71.4516784038317,
12.));
#100260=CARTESIAN_POINT('Ctrl Pts',(-1.32912680326124,71.4733063530187,
0.));
#100261=CARTESIAN_POINT('Ctrl Pts',(-1.32912680326124,71.4733063530187,
12.));
#100262=CARTESIAN_POINT('Ctrl Pts',(-1.3369806508522,71.4949685044522,0.));
#100263=CARTESIAN_POINT('Ctrl Pts',(-1.3369806508522,71.4949685044522,12.));
#100264=CARTESIAN_POINT('Ctrl Pts',(-1.34487131610781,71.516664711275,0.));
#100265=CARTESIAN_POINT('Ctrl Pts',(-1.34487131610781,71.516664711275,12.));
#100266=CARTESIAN_POINT('Ctrl Pts',(-1.35279881628455,71.5383948272845,
0.));
#100267=CARTESIAN_POINT('Ctrl Pts',(-1.35279881628455,71.5383948272845,
12.));
#100268=CARTESIAN_POINT('Ctrl Pts',(-1.36076316845816,71.5601587069217,
0.));
#100269=CARTESIAN_POINT('Ctrl Pts',(-1.36076316845816,71.5601587069217,
12.));
#100270=CARTESIAN_POINT('Ctrl Pts',(-1.36876438952466,71.5819562052663,
0.));
#100271=CARTESIAN_POINT('Ctrl Pts',(-1.36876438952466,71.5819562052663,
12.));
#100272=CARTESIAN_POINT('Ctrl Pts',(-1.3768024962078,71.6037871780385,0.));
#100273=CARTESIAN_POINT('Ctrl Pts',(-1.3768024962078,71.6037871780385,12.));
#100274=CARTESIAN_POINT('Ctrl Pts',(-1.38487750506082,71.625651481593,0.));
#100275=CARTESIAN_POINT('Ctrl Pts',(-1.38487750506082,71.625651481593,12.));
#100276=CARTESIAN_POINT('Ctrl Pts',(-1.39298943246722,71.6475489729134,
0.));
#100277=CARTESIAN_POINT('Ctrl Pts',(-1.39298943246722,71.6475489729134,
12.));
#100278=CARTESIAN_POINT('Ctrl Pts',(-1.40113829463577,71.6694795096001,
0.));
#100279=CARTESIAN_POINT('Ctrl Pts',(-1.40113829463577,71.6694795096001,
12.));
#100280=CARTESIAN_POINT('Ctrl Pts',(-1.40932410760248,71.6914429498663,
0.));
#100281=CARTESIAN_POINT('Ctrl Pts',(-1.40932410760248,71.6914429498663,
12.));
#100282=CARTESIAN_POINT('Ctrl Pts',(-1.41754688723773,71.7134391525389,
0.));
#100283=CARTESIAN_POINT('Ctrl Pts',(-1.41754688723773,71.7134391525389,
12.));
#100284=CARTESIAN_POINT('Ctrl Pts',(-1.4258066492477,71.7354679770528,0.));
#100285=CARTESIAN_POINT('Ctrl Pts',(-1.4258066492477,71.7354679770528,12.));
#100286=CARTESIAN_POINT('Ctrl Pts',(-1.43410340917496,71.7575292834469,
0.));
#100287=CARTESIAN_POINT('Ctrl Pts',(-1.43410340917496,71.7575292834469,
12.));
#100288=CARTESIAN_POINT('Ctrl Pts',(-1.44243718239315,71.7796229323526,
0.));
#100289=CARTESIAN_POINT('Ctrl Pts',(-1.44243718239315,71.7796229323526,
12.));
#100290=CARTESIAN_POINT('Ctrl Pts',(-1.45080798410965,71.8017487849895,
0.));
#100291=CARTESIAN_POINT('Ctrl Pts',(-1.45080798410965,71.8017487849895,
12.));
#100292=CARTESIAN_POINT('Ctrl Pts',(-1.45921582937232,71.8239067031683,
0.));
#100293=CARTESIAN_POINT('Ctrl Pts',(-1.45921582937232,71.8239067031683,
12.));
#100294=CARTESIAN_POINT('Ctrl Pts',(-1.46766073307088,71.8460965492839,
0.));
#100295=CARTESIAN_POINT('Ctrl Pts',(-1.46766073307088,71.8460965492839,
12.));
#100296=CARTESIAN_POINT('Ctrl Pts',(-1.47614270993729,71.8683181863116,
0.));
#100297=CARTESIAN_POINT('Ctrl Pts',(-1.47614270993729,71.8683181863116,
12.));
#100298=CARTESIAN_POINT('Ctrl Pts',(-1.4846617745402,71.8905714777961,0.));
#100299=CARTESIAN_POINT('Ctrl Pts',(-1.4846617745402,71.8905714777961,12.));
#100300=CARTESIAN_POINT('Ctrl Pts',(-1.49321794128799,71.912856287848,0.));
#100301=CARTESIAN_POINT('Ctrl Pts',(-1.49321794128799,71.912856287848,12.));
#100302=CARTESIAN_POINT('Ctrl Pts',(-1.50181122443534,71.9351724811443,
0.));
#100303=CARTESIAN_POINT('Ctrl Pts',(-1.50181122443534,71.9351724811443,
12.));
#100304=CARTESIAN_POINT('Ctrl Pts',(-1.51044163808454,71.9575199229241,
0.));
#100305=CARTESIAN_POINT('Ctrl Pts',(-1.51044163808454,71.9575199229241,
12.));
#100306=CARTESIAN_POINT('Ctrl Pts',(-1.51910919618566,71.979898478983,0.));
#100307=CARTESIAN_POINT('Ctrl Pts',(-1.51910919618566,71.979898478983,12.));
#100308=CARTESIAN_POINT('Ctrl Pts',(-1.52781391253102,72.0023080156647,
0.));
#100309=CARTESIAN_POINT('Ctrl Pts',(-1.52781391253102,72.0023080156647,
12.));
#100310=CARTESIAN_POINT('Ctrl Pts',(-1.53655580075813,72.0247483998578,
0.));
#100311=CARTESIAN_POINT('Ctrl Pts',(-1.53655580075813,72.0247483998578,
12.));
#100312=CARTESIAN_POINT('Ctrl Pts',(-1.54533487435626,72.0472194989963,
0.));
#100313=CARTESIAN_POINT('Ctrl Pts',(-1.54533487435626,72.0472194989963,
12.));
#100314=CARTESIAN_POINT('Ctrl Pts',(-1.55415114666774,72.0697211810545,
0.));
#100315=CARTESIAN_POINT('Ctrl Pts',(-1.55415114666774,72.0697211810545,
12.));
#100316=CARTESIAN_POINT('Ctrl Pts',(-1.56300463088809,72.0922533145433,
0.));
#100317=CARTESIAN_POINT('Ctrl Pts',(-1.56300463088809,72.0922533145433,
12.));
#100318=CARTESIAN_POINT('Ctrl Pts',(-1.5718953400604,72.1148157684995,0.));
#100319=CARTESIAN_POINT('Ctrl Pts',(-1.5718953400604,72.1148157684995,12.));
#100320=CARTESIAN_POINT('Ctrl Pts',(-1.58082328707803,72.1374084124839,
0.));
#100321=CARTESIAN_POINT('Ctrl Pts',(-1.58082328707803,72.1374084124839,
12.));
#100322=CARTESIAN_POINT('Ctrl Pts',(-1.58978848469123,72.1600311165821,
0.));
#100323=CARTESIAN_POINT('Ctrl Pts',(-1.58978848469123,72.1600311165821,
12.));
#100324=CARTESIAN_POINT('Ctrl Pts',(-1.59879094550847,72.1826837514001,
0.));
#100325=CARTESIAN_POINT('Ctrl Pts',(-1.59879094550847,72.1826837514001,
12.));
#100326=CARTESIAN_POINT('Ctrl Pts',(-1.60783068199663,72.2053661880608,
0.));
#100327=CARTESIAN_POINT('Ctrl Pts',(-1.60783068199663,72.2053661880608,
12.));
#100328=CARTESIAN_POINT('Ctrl Pts',(-1.6169077064754,72.2280782981937,0.));
#100329=CARTESIAN_POINT('Ctrl Pts',(-1.6169077064754,72.2280782981937,12.));
#100330=CARTESIAN_POINT('Ctrl Pts',(-1.6260220311193,72.2508199539323,0.));
#100331=CARTESIAN_POINT('Ctrl Pts',(-1.6260220311193,72.2508199539323,12.));
#100332=CARTESIAN_POINT('Ctrl Pts',(-1.63517366796463,72.2735910279149,
0.));
#100333=CARTESIAN_POINT('Ctrl Pts',(-1.63517366796463,72.2735910279149,
12.));
#100334=CARTESIAN_POINT('Ctrl Pts',(-1.64436262891079,72.2963913932813,
0.));
#100335=CARTESIAN_POINT('Ctrl Pts',(-1.64436262891079,72.2963913932813,
12.));
#100336=CARTESIAN_POINT('Ctrl Pts',(-1.65358892572063,72.319220923669,0.));
#100337=CARTESIAN_POINT('Ctrl Pts',(-1.65358892572063,72.319220923669,12.));
#100338=CARTESIAN_POINT('Ctrl Pts',(-1.66285257001496,72.3420794932047,
0.));
#100339=CARTESIAN_POINT('Ctrl Pts',(-1.66285257001496,72.3420794932047,
12.));
#100340=CARTESIAN_POINT('Ctrl Pts',(-1.67215357327365,72.3649669765004,
0.));
#100341=CARTESIAN_POINT('Ctrl Pts',(-1.67215357327365,72.3649669765004,
12.));
#100342=CARTESIAN_POINT('Ctrl Pts',(-1.68149194684282,72.387883248654,0.));
#100343=CARTESIAN_POINT('Ctrl Pts',(-1.68149194684282,72.387883248654,12.));
#100344=CARTESIAN_POINT('Ctrl Pts',(-1.69086770193637,72.4108281852467,
0.));
#100345=CARTESIAN_POINT('Ctrl Pts',(-1.69086770193637,72.4108281852467,
12.));
#100346=CARTESIAN_POINT('Ctrl Pts',(-1.70028084963647,72.4338016623391,
0.));
#100347=CARTESIAN_POINT('Ctrl Pts',(-1.70028084963647,72.4338016623391,
12.));
#100348=CARTESIAN_POINT('Ctrl Pts',(-1.70973140088842,72.456803556463,0.));
#100349=CARTESIAN_POINT('Ctrl Pts',(-1.70973140088842,72.456803556463,12.));
#100350=CARTESIAN_POINT('Ctrl Pts',(-1.71921936650038,72.479833744618,0.));
#100351=CARTESIAN_POINT('Ctrl Pts',(-1.71921936650038,72.479833744618,12.));
#100352=CARTESIAN_POINT('Ctrl Pts',(-1.72874475715103,72.5028921042721,
0.));
#100353=CARTESIAN_POINT('Ctrl Pts',(-1.72874475715103,72.5028921042721,
12.));
#100354=CARTESIAN_POINT('Ctrl Pts',(-1.73830758339125,72.5259785133595,
0.));
#100355=CARTESIAN_POINT('Ctrl Pts',(-1.73830758339125,72.5259785133595,
12.));
#100356=CARTESIAN_POINT('Ctrl Pts',(-1.74790785564474,72.5490928502769,
0.));
#100357=CARTESIAN_POINT('Ctrl Pts',(-1.74790785564474,72.5490928502769,
12.));
#100358=CARTESIAN_POINT('Ctrl Pts',(-1.75754558420344,72.5722349938774,
0.));
#100359=CARTESIAN_POINT('Ctrl Pts',(-1.75754558420344,72.5722349938774,
12.));
#100360=CARTESIAN_POINT('Ctrl Pts',(-1.76722077922574,72.5954048234638,
0.));
#100361=CARTESIAN_POINT('Ctrl Pts',(-1.76722077922574,72.5954048234638,
12.));
#100362=CARTESIAN_POINT('Ctrl Pts',(-1.77693345074427,72.6186022187907,
0.));
#100363=CARTESIAN_POINT('Ctrl Pts',(-1.77693345074427,72.6186022187907,
12.));
#100364=CARTESIAN_POINT('Ctrl Pts',(-1.78668360866811,72.6418270600619,
0.));
#100365=CARTESIAN_POINT('Ctrl Pts',(-1.78668360866811,72.6418270600619,
12.));
#100366=CARTESIAN_POINT('Ctrl Pts',(-1.79647126278359,72.6650792279274,
0.));
#100367=CARTESIAN_POINT('Ctrl Pts',(-1.79647126278359,72.6650792279274,
12.));
#100368=CARTESIAN_POINT('Ctrl Pts',(-1.80629642275051,72.6883586034769,
0.));
#100369=CARTESIAN_POINT('Ctrl Pts',(-1.80629642275051,72.6883586034769,
12.));
#100370=CARTESIAN_POINT('Ctrl Pts',(-1.81615909809871,72.7116650682344,
0.));
#100371=CARTESIAN_POINT('Ctrl Pts',(-1.81615909809871,72.7116650682344,
12.));
#100372=CARTESIAN_POINT('Ctrl Pts',(-1.82605929823564,72.7349985041592,
0.));
#100373=CARTESIAN_POINT('Ctrl Pts',(-1.82605929823564,72.7349985041592,
12.));
#100374=CARTESIAN_POINT('Ctrl Pts',(-1.83599703244924,72.7583587936447,
0.));
#100375=CARTESIAN_POINT('Ctrl Pts',(-1.83599703244924,72.7583587936447,
12.));
#100376=CARTESIAN_POINT('Ctrl Pts',(-1.84597230990857,72.7817458195155,
0.));
#100377=CARTESIAN_POINT('Ctrl Pts',(-1.84597230990857,72.7817458195155,
12.));
#100378=CARTESIAN_POINT('Ctrl Pts',(-1.85598513966114,72.8051594650222,
0.));
#100379=CARTESIAN_POINT('Ctrl Pts',(-1.85598513966114,72.8051594650222,
12.));
#100380=CARTESIAN_POINT('Ctrl Pts',(-1.86603553062771,72.8285996138359,
0.));
#100381=CARTESIAN_POINT('Ctrl Pts',(-1.86603553062771,72.8285996138359,
12.));
#100382=CARTESIAN_POINT('Ctrl Pts',(-1.87612349160945,72.8520661500477,
0.));
#100383=CARTESIAN_POINT('Ctrl Pts',(-1.87612349160945,72.8520661500477,
12.));
#100384=CARTESIAN_POINT('Ctrl Pts',(-1.88624903129188,72.875558958168,0.));
#100385=CARTESIAN_POINT('Ctrl Pts',(-1.88624903129188,72.875558958168,12.));
#100386=CARTESIAN_POINT('Ctrl Pts',(-1.89641215824582,72.8990779231226,
0.));
#100387=CARTESIAN_POINT('Ctrl Pts',(-1.89641215824582,72.8990779231226,
12.));
#100388=CARTESIAN_POINT('Ctrl Pts',(-1.90661288092587,72.9226229302478,
0.));
#100389=CARTESIAN_POINT('Ctrl Pts',(-1.90661288092587,72.9226229302478,
12.));
#100390=CARTESIAN_POINT('Ctrl Pts',(-1.91685120766437,72.9461938652811,
0.));
#100391=CARTESIAN_POINT('Ctrl Pts',(-1.91685120766437,72.9461938652811,
12.));
#100392=CARTESIAN_POINT('Ctrl Pts',(-1.9271271466766,72.9697906143636,0.));
#100393=CARTESIAN_POINT('Ctrl Pts',(-1.9271271466766,72.9697906143636,12.));
#100394=CARTESIAN_POINT('Ctrl Pts',(-1.93744070606566,72.9934130640415,
0.));
#100395=CARTESIAN_POINT('Ctrl Pts',(-1.93744070606566,72.9934130640415,
12.));
#100396=CARTESIAN_POINT('Ctrl Pts',(-1.94779189382302,73.0170611012661,
0.));
#100397=CARTESIAN_POINT('Ctrl Pts',(-1.94779189382302,73.0170611012661,
12.));
#100398=CARTESIAN_POINT('Ctrl Pts',(-1.95818071782767,73.040734613391,0.));
#100399=CARTESIAN_POINT('Ctrl Pts',(-1.95818071782767,73.040734613391,12.));
#100400=CARTESIAN_POINT('Ctrl Pts',(-1.96860718583932,73.0644334881673,
0.));
#100401=CARTESIAN_POINT('Ctrl Pts',(-1.96860718583932,73.0644334881673,
12.));
#100402=CARTESIAN_POINT('Ctrl Pts',(-1.97907130550158,73.0881576137407,
0.));
#100403=CARTESIAN_POINT('Ctrl Pts',(-1.97907130550158,73.0881576137407,
12.));
#100404=CARTESIAN_POINT('Ctrl Pts',(-1.98957308434918,73.1119068786475,
0.));
#100405=CARTESIAN_POINT('Ctrl Pts',(-1.98957308434918,73.1119068786475,
12.));
#100406=CARTESIAN_POINT('Ctrl Pts',(-2.00011252980982,73.1356811718091,
0.));
#100407=CARTESIAN_POINT('Ctrl Pts',(-2.00011252980982,73.1356811718091,
12.));
#100408=CARTESIAN_POINT('Ctrl Pts',(-2.01068964920467,73.1594803825252,
0.));
#100409=CARTESIAN_POINT('Ctrl Pts',(-2.01068964920467,73.1594803825252,
12.));
#100410=CARTESIAN_POINT('Ctrl Pts',(-2.02130444974362,73.183304400462,0.));
#100411=CARTESIAN_POINT('Ctrl Pts',(-2.02130444974362,73.183304400462,12.));
#100412=CARTESIAN_POINT('Ctrl Pts',(-2.03195693852455,73.2071531156504,
0.));
#100413=CARTESIAN_POINT('Ctrl Pts',(-2.03195693852455,73.2071531156504,
12.));
#100414=CARTESIAN_POINT('Ctrl Pts',(-2.04264712253929,73.2310264184976,
0.));
#100415=CARTESIAN_POINT('Ctrl Pts',(-2.04264712253929,73.2310264184976,
12.));
#100416=CARTESIAN_POINT('Ctrl Pts',(-2.05337500867403,73.2549241997953,
0.));
#100417=CARTESIAN_POINT('Ctrl Pts',(-2.05337500867403,73.2549241997953,
12.));
#100418=CARTESIAN_POINT('Ctrl Pts',(-2.06414060370835,73.2788463507246,
0.));
#100419=CARTESIAN_POINT('Ctrl Pts',(-2.06414060370835,73.2788463507246,
12.));
#100420=CARTESIAN_POINT('Ctrl Pts',(-2.07494391430941,73.3027927628626,
0.));
#100421=CARTESIAN_POINT('Ctrl Pts',(-2.07494391430941,73.3027927628626,
12.));
#100422=CARTESIAN_POINT('Ctrl Pts',(-2.08578494702744,73.3267633281807,
0.));
#100423=CARTESIAN_POINT('Ctrl Pts',(-2.08578494702744,73.3267633281807,
12.));
#100424=CARTESIAN_POINT('Ctrl Pts',(-2.09666370830716,73.3507579390239,
0.));
#100425=CARTESIAN_POINT('Ctrl Pts',(-2.09666370830716,73.3507579390239,
12.));
#100426=CARTESIAN_POINT('Ctrl Pts',(-2.1075802044939,73.3747764880893,0.));
#100427=CARTESIAN_POINT('Ctrl Pts',(-2.1075802044939,73.3747764880893,12.));
#100428=CARTESIAN_POINT('Ctrl Pts',(-2.11853444183762,73.3988188684021,
0.));
#100429=CARTESIAN_POINT('Ctrl Pts',(-2.11853444183762,73.3988188684021,
12.));
#100430=CARTESIAN_POINT('Ctrl Pts',(-2.12952642649368,73.4228849732925,
0.));
#100431=CARTESIAN_POINT('Ctrl Pts',(-2.12952642649368,73.4228849732925,
12.));
#100432=CARTESIAN_POINT('Ctrl Pts',(-2.14055616452058,73.4469746963637,
0.));
#100433=CARTESIAN_POINT('Ctrl Pts',(-2.14055616452058,73.4469746963637,
12.));
#100434=CARTESIAN_POINT('Ctrl Pts',(-2.15162366187907,73.4710879315382,
0.));
#100435=CARTESIAN_POINT('Ctrl Pts',(-2.15162366187907,73.4710879315382,
12.));
#100436=CARTESIAN_POINT('Ctrl Pts',(-2.1627289244292,73.4952245731054,0.));
#100437=CARTESIAN_POINT('Ctrl Pts',(-2.1627289244292,73.4952245731054,12.));
#100438=CARTESIAN_POINT('Ctrl Pts',(-2.17387195792306,73.5193845157708,
0.));
#100439=CARTESIAN_POINT('Ctrl Pts',(-2.17387195792306,73.5193845157708,
12.));
#100440=CARTESIAN_POINT('Ctrl Pts',(-2.18505276799753,73.5435676546929,
0.));
#100441=CARTESIAN_POINT('Ctrl Pts',(-2.18505276799753,73.5435676546929,
12.));
#100442=CARTESIAN_POINT('Ctrl Pts',(-2.19627136015678,73.5677738855452,
0.));
#100443=CARTESIAN_POINT('Ctrl Pts',(-2.19627136015678,73.5677738855452,
12.));
#100444=CARTESIAN_POINT('Ctrl Pts',(-2.20752773978349,73.5920031044595,
0.));
#100445=CARTESIAN_POINT('Ctrl Pts',(-2.20752773978349,73.5920031044595,
12.));
#100446=CARTESIAN_POINT('Ctrl Pts',(-2.21882191216518,73.6162552079038,
0.));
#100447=CARTESIAN_POINT('Ctrl Pts',(-2.21882191216518,73.6162552079038,
12.));
#100448=CARTESIAN_POINT('Ctrl Pts',(-2.23015388251288,73.6405300925712,
0.));
#100449=CARTESIAN_POINT('Ctrl Pts',(-2.23015388251288,73.6405300925712,
12.));
#100450=CARTESIAN_POINT('Ctrl Pts',(-2.24152365597698,73.6648276552767,
0.));
#100451=CARTESIAN_POINT('Ctrl Pts',(-2.24152365597698,73.6648276552767,
12.));
#100452=CARTESIAN_POINT('Ctrl Pts',(-2.25293123766425,73.6891477928129,
0.));
#100453=CARTESIAN_POINT('Ctrl Pts',(-2.25293123766425,73.6891477928129,
12.));
#100454=CARTESIAN_POINT('Ctrl Pts',(-2.26437663263667,73.7134904019389,
0.));
#100455=CARTESIAN_POINT('Ctrl Pts',(-2.26437663263667,73.7134904019389,
12.));
#100456=CARTESIAN_POINT('Ctrl Pts',(-2.27585984587199,73.7378553796807,
0.));
#100457=CARTESIAN_POINT('Ctrl Pts',(-2.27585984587199,73.7378553796807,
12.));
#100458=CARTESIAN_POINT('Ctrl Pts',(-2.28738088222864,73.762242623566,0.));
#100459=CARTESIAN_POINT('Ctrl Pts',(-2.28738088222864,73.762242623566,12.));
#100460=CARTESIAN_POINT('Ctrl Pts',(-2.29893974640434,73.786652031885,0.));
#100461=CARTESIAN_POINT('Ctrl Pts',(-2.29893974640434,73.786652031885,12.));
#100462=CARTESIAN_POINT('Ctrl Pts',(-2.31053644289417,73.8110835039327,
0.));
#100463=CARTESIAN_POINT('Ctrl Pts',(-2.31053644289417,73.8110835039327,
12.));
#100464=CARTESIAN_POINT('Ctrl Pts',(-2.32217097594198,73.8355369402706,
0.));
#100465=CARTESIAN_POINT('Ctrl Pts',(-2.32217097594198,73.8355369402706,
12.));
#100466=CARTESIAN_POINT('Ctrl Pts',(-2.33384334963958,73.8600122421468,
0.));
#100467=CARTESIAN_POINT('Ctrl Pts',(-2.33384334963958,73.8600122421468,
12.));
#100468=CARTESIAN_POINT('Ctrl Pts',(-2.34555356802121,73.8845093109274,
0.));
#100469=CARTESIAN_POINT('Ctrl Pts',(-2.34555356802121,73.8845093109274,
12.));
#100470=CARTESIAN_POINT('Ctrl Pts',(-2.35730163516316,73.9090280474712,
0.));
#100471=CARTESIAN_POINT('Ctrl Pts',(-2.35730163516316,73.9090280474712,
12.));
#100472=CARTESIAN_POINT('Ctrl Pts',(-2.36908755526003,73.9335683516404,
0.));
#100473=CARTESIAN_POINT('Ctrl Pts',(-2.36908755526003,73.9335683516404,
12.));
#100474=CARTESIAN_POINT('Ctrl Pts',(-2.38091133274961,73.958130121465,0.));
#100475=CARTESIAN_POINT('Ctrl Pts',(-2.38091133274961,73.958130121465,12.));
#100476=CARTESIAN_POINT('Ctrl Pts',(-2.39277297220757,73.9827132538206,
0.));
#100477=CARTESIAN_POINT('Ctrl Pts',(-2.39277297220757,73.9827132538206,
12.));
#100478=CARTESIAN_POINT('Ctrl Pts',(-2.40467247811536,74.0073176459344,
0.));
#100479=CARTESIAN_POINT('Ctrl Pts',(-2.40467247811536,74.0073176459344,
12.));
#100480=CARTESIAN_POINT('Ctrl Pts',(-2.41660985465252,74.0319431966989,
0.));
#100481=CARTESIAN_POINT('Ctrl Pts',(-2.41660985465252,74.0319431966989,
12.));
#100482=CARTESIAN_POINT('Ctrl Pts',(-2.42858510549779,74.0565898079218,
0.));
#100483=CARTESIAN_POINT('Ctrl Pts',(-2.42858510549779,74.0565898079218,
12.));
#100484=CARTESIAN_POINT('Ctrl Pts',(-2.44059823356676,74.0812573859411,
0.));
#100485=CARTESIAN_POINT('Ctrl Pts',(-2.44059823356676,74.0812573859411,
12.));
#100486=CARTESIAN_POINT('Ctrl Pts',(-2.45264924094775,74.1059458420067,
0.));
#100487=CARTESIAN_POINT('Ctrl Pts',(-2.45264924094775,74.1059458420067,
12.));
#100488=CARTESIAN_POINT('Ctrl Pts',(-2.4647381294796,74.1306550887071,0.));
#100489=CARTESIAN_POINT('Ctrl Pts',(-2.4647381294796,74.1306550887071,12.));
#100490=CARTESIAN_POINT('Ctrl Pts',(-2.47686490120354,74.155385037148,0.));
#100491=CARTESIAN_POINT('Ctrl Pts',(-2.47686490120354,74.155385037148,12.));
#100492=CARTESIAN_POINT('Ctrl Pts',(-2.48902955888385,74.1801355936907,
0.));
#100493=CARTESIAN_POINT('Ctrl Pts',(-2.48902955888385,74.1801355936907,
12.));
#100494=CARTESIAN_POINT('Ctrl Pts',(-2.50123210644135,74.2049066572031,
0.));
#100495=CARTESIAN_POINT('Ctrl Pts',(-2.50123210644135,74.2049066572031,
12.));
#100496=CARTESIAN_POINT('Ctrl Pts',(-2.51347254956167,74.229698115223,0.));
#100497=CARTESIAN_POINT('Ctrl Pts',(-2.51347254956167,74.229698115223,12.));
#100498=CARTESIAN_POINT('Ctrl Pts',(-2.52575089478304,74.2545098494824,
0.));
#100499=CARTESIAN_POINT('Ctrl Pts',(-2.52575089478304,74.2545098494824,
12.));
#100500=CARTESIAN_POINT('Ctrl Pts',(-2.53806714838286,74.2793417427308,
0.));
#100501=CARTESIAN_POINT('Ctrl Pts',(-2.53806714838286,74.2793417427308,
12.));
#100502=CARTESIAN_POINT('Ctrl Pts',(-2.55042131526781,74.3041936853468,
0.));
#100503=CARTESIAN_POINT('Ctrl Pts',(-2.55042131526781,74.3041936853468,
12.));
#100504=CARTESIAN_POINT('Ctrl Pts',(-2.56281339800018,74.3290655814831,
0.));
#100505=CARTESIAN_POINT('Ctrl Pts',(-2.56281339800018,74.3290655814831,
12.));
#100506=CARTESIAN_POINT('Ctrl Pts',(-2.5752433954139,74.3539573567672,0.));
#100507=CARTESIAN_POINT('Ctrl Pts',(-2.5752433954139,74.3539573567672,12.));
#100508=CARTESIAN_POINT('Ctrl Pts',(-2.58771130268176,74.3788689603363,
0.));
#100509=CARTESIAN_POINT('Ctrl Pts',(-2.58771130268176,74.3788689603363,
12.));
#100510=CARTESIAN_POINT('Ctrl Pts',(-2.60021711326977,74.4038003594771,
0.));
#100511=CARTESIAN_POINT('Ctrl Pts',(-2.60021711326977,74.4038003594771,
12.));
#100512=CARTESIAN_POINT('Ctrl Pts',(-2.61025207898403,74.4237613007988,
0.));
#100513=CARTESIAN_POINT('Ctrl Pts',(-2.61025207898403,74.4237613007988,
12.));
#100514=CARTESIAN_POINT('Ctrl Pts',(-2.61779535432112,74.4387409032207,
0.));
#100515=CARTESIAN_POINT('Ctrl Pts',(-2.61779535432112,74.4387409032207,
12.));
#100516=CARTESIAN_POINT('Ctrl Pts',(-2.62283178248203,74.4487312586464,
0.));
#100517=CARTESIAN_POINT('Ctrl Pts',(-2.62283178248203,74.4487312586464,
12.));
#100518=CARTESIAN_POINT('Ctrl Pts',(-2.62535189104655,74.4537274248118,
0.));
#100519=CARTESIAN_POINT('Ctrl Pts',(-2.62535189104655,74.4537274248118,
12.));
#100520=CARTESIAN_POINT('',(-0.853825826608985,69.9947925310006,0.));
#100521=CARTESIAN_POINT('Ctrl Pts',(-0.853825826608985,69.9947925310006,
0.));
#100522=CARTESIAN_POINT('Ctrl Pts',(-0.854867673848596,69.9985337959407,
0.));
#100523=CARTESIAN_POINT('Ctrl Pts',(-0.856954870259207,70.0060209754087,
0.));
#100524=CARTESIAN_POINT('Ctrl Pts',(-0.860096170668736,70.0172656933806,
0.));
#100525=CARTESIAN_POINT('Ctrl Pts',(-0.864305583661547,70.0322865492925,
0.));
#100526=CARTESIAN_POINT('Ctrl Pts',(-0.869602377871126,70.051109108301,
0.));
#100527=CARTESIAN_POINT('Ctrl Pts',(-0.874934213255839,70.0699781183935,
0.));
#100528=CARTESIAN_POINT('Ctrl Pts',(-0.880301109660729,70.0888934967855,
0.));
#100529=CARTESIAN_POINT('Ctrl Pts',(-0.885703094802537,70.1078550938958,
0.));
#100530=CARTESIAN_POINT('Ctrl Pts',(-0.891140203464243,70.1268626950175,
0.));
#100531=CARTESIAN_POINT('Ctrl Pts',(-0.896612474371846,70.1459160490446,
0.));
#100532=CARTESIAN_POINT('Ctrl Pts',(-0.902119947629773,70.1650148905109,
0.));
#100533=CARTESIAN_POINT('Ctrl Pts',(-0.907662662015787,70.1841589635574,
0.));
#100534=CARTESIAN_POINT('Ctrl Pts',(-0.913240652090982,70.2033480471676,
0.));
#100535=CARTESIAN_POINT('Ctrl Pts',(-0.91885394915712,70.2225819470248,
0.));
#100536=CARTESIAN_POINT('Ctrl Pts',(-0.924502582639457,70.2418604835837,
0.));
#100537=CARTESIAN_POINT('Ctrl Pts',(-0.930186581235549,70.2611834821724,
0.));
#100538=CARTESIAN_POINT('Ctrl Pts',(-0.935905974336482,70.2805507606872,
0.));
#100539=CARTESIAN_POINT('Ctrl Pts',(-0.941660792742981,70.299962123399,
0.));
#100540=CARTESIAN_POINT('Ctrl Pts',(-0.947451067929606,70.3194173673674,
0.));
#100541=CARTESIAN_POINT('Ctrl Pts',(-0.953276831581243,70.338916286458,
0.));
#100542=CARTESIAN_POINT('Ctrl Pts',(-0.959138115058833,70.3584586759536,
0.));
#100543=CARTESIAN_POINT('Ctrl Pts',(-0.965034948786451,70.3780443377956,
0.));
#100544=CARTESIAN_POINT('Ctrl Pts',(-0.970967362281175,70.3976730803614,
0.));
#100545=CARTESIAN_POINT('Ctrl Pts',(-0.976935384450043,70.417344715957,
0.));
#100546=CARTESIAN_POINT('Ctrl Pts',(-0.982939043792157,70.4370590590842,
0.));
#100547=CARTESIAN_POINT('Ctrl Pts',(-0.98897836864365,70.4568159243163,
0.));
#100548=CARTESIAN_POINT('Ctrl Pts',(-0.995053387379757,70.4766151245212,
0.));
#100549=CARTESIAN_POINT('Ctrl Pts',(-1.00116412831442,70.4964564717953,
0.));
#100550=CARTESIAN_POINT('Ctrl Pts',(-1.00731061960968,70.5163397782713,
0.));
#100551=CARTESIAN_POINT('Ctrl Pts',(-1.01349288918537,70.5362648569061,
0.));
#100552=CARTESIAN_POINT('Ctrl Pts',(-1.01971096460597,70.556231522419,0.));
#100553=CARTESIAN_POINT('Ctrl Pts',(-1.02596487304049,70.5762395916377,
0.));
#100554=CARTESIAN_POINT('Ctrl Pts',(-1.0322546413287,70.5962888829934,0.));
#100555=CARTESIAN_POINT('Ctrl Pts',(-1.03858029601904,70.6163792162073,
0.));
#100556=CARTESIAN_POINT('Ctrl Pts',(-1.04494186341156,70.6365104119252,
0.));
#100557=CARTESIAN_POINT('Ctrl Pts',(-1.05133936960072,70.6566822912991,
0.));
#100558=CARTESIAN_POINT('Ctrl Pts',(-1.0577728404773,70.676894676009,0.));
#100559=CARTESIAN_POINT('Ctrl Pts',(-1.06424230171281,70.6971473884459,
0.));
#100560=CARTESIAN_POINT('Ctrl Pts',(-1.07074777874596,70.7174402518378,
0.));
#100561=CARTESIAN_POINT('Ctrl Pts',(-1.07728929676408,70.7377730903953,
0.));
#100562=CARTESIAN_POINT('Ctrl Pts',(-1.08386688068342,70.7581457294447,
0.));
#100563=CARTESIAN_POINT('Ctrl Pts',(-1.09048055516427,70.7785579953583,
0.));
#100564=CARTESIAN_POINT('Ctrl Pts',(-1.09713034462265,70.799009715484,0.));
#100565=CARTESIAN_POINT('Ctrl Pts',(-1.10381627323947,70.8195007180745,
0.));
#100566=CARTESIAN_POINT('Ctrl Pts',(-1.1105383649664,70.8400308322037,0.));
#100567=CARTESIAN_POINT('Ctrl Pts',(-1.11729664352993,70.8605998877149,
0.));
#100568=CARTESIAN_POINT('Ctrl Pts',(-1.12409113243514,70.8812077152586,
0.));
#100569=CARTESIAN_POINT('Ctrl Pts',(-1.13092185496565,70.9018541463089,
0.));
#100570=CARTESIAN_POINT('Ctrl Pts',(-1.13778883418214,70.9225390131826,
0.));
#100571=CARTESIAN_POINT('Ctrl Pts',(-1.14469209291489,70.9432621490566,
0.));
#100572=CARTESIAN_POINT('Ctrl Pts',(-1.15163165376524,70.9640233879659,
0.));
#100573=CARTESIAN_POINT('Ctrl Pts',(-1.15860753911485,70.9848225647871,
0.));
#100574=CARTESIAN_POINT('Ctrl Pts',(-1.1656197711288,71.0056595152204,0.));
#100575=CARTESIAN_POINT('Ctrl Pts',(-1.17266837175777,71.0265340757699,
0.));
#100576=CARTESIAN_POINT('Ctrl Pts',(-1.17975336273504,71.0474460837159,
0.));
#100577=CARTESIAN_POINT('Ctrl Pts',(-1.18687476558133,71.0683953771149,
0.));
#100578=CARTESIAN_POINT('Ctrl Pts',(-1.19403260161002,71.089381794801,0.));
#100579=CARTESIAN_POINT('Ctrl Pts',(-1.20122689192836,71.1104051763839,
0.));
#100580=CARTESIAN_POINT('Ctrl Pts',(-1.20845765743648,71.1314653622442,
0.));
#100581=CARTESIAN_POINT('Ctrl Pts',(-1.21572491882263,71.1525621935267,
0.));
#100582=CARTESIAN_POINT('Ctrl Pts',(-1.22302869657018,71.1736955121362,
0.));
#100583=CARTESIAN_POINT('Ctrl Pts',(-1.23036901096239,71.194865160732,0.));
#100584=CARTESIAN_POINT('Ctrl Pts',(-1.23774588208427,71.2160709827191,
0.));
#100585=CARTESIAN_POINT('Ctrl Pts',(-1.24515932982113,71.2373128222352,
0.));
#100586=CARTESIAN_POINT('Ctrl Pts',(-1.25260937385569,71.2585905241406,
0.));
#100587=CARTESIAN_POINT('Ctrl Pts',(-1.26009603367571,71.2799039340175,
0.));
#100588=CARTESIAN_POINT('Ctrl Pts',(-1.26761932857724,71.3012528981661,
0.));
#100589=CARTESIAN_POINT('Ctrl Pts',(-1.27517927766608,71.3226372635996,
0.));
#100590=CARTESIAN_POINT('Ctrl Pts',(-1.28277589985472,71.3440568780347,
0.));
#100591=CARTESIAN_POINT('Ctrl Pts',(-1.29040921386059,71.3655115898827,
0.));
#100592=CARTESIAN_POINT('Ctrl Pts',(-1.29807923821414,71.3870012482499,
0.));
#100593=CARTESIAN_POINT('Ctrl Pts',(-1.3057859912614,71.4085257029322,0.));
#100594=CARTESIAN_POINT('Ctrl Pts',(-1.31352949116537,71.4300848044087,
0.));
#100595=CARTESIAN_POINT('Ctrl Pts',(-1.32130975590226,71.4516784038317,
0.));
#100596=CARTESIAN_POINT('Ctrl Pts',(-1.32912680326124,71.4733063530187,
0.));
#100597=CARTESIAN_POINT('Ctrl Pts',(-1.3369806508522,71.4949685044522,0.));
#100598=CARTESIAN_POINT('Ctrl Pts',(-1.34487131610781,71.516664711275,0.));
#100599=CARTESIAN_POINT('Ctrl Pts',(-1.35279881628455,71.5383948272845,
0.));
#100600=CARTESIAN_POINT('Ctrl Pts',(-1.36076316845816,71.5601587069217,
0.));
#100601=CARTESIAN_POINT('Ctrl Pts',(-1.36876438952466,71.5819562052663,
0.));
#100602=CARTESIAN_POINT('Ctrl Pts',(-1.3768024962078,71.6037871780385,0.));
#100603=CARTESIAN_POINT('Ctrl Pts',(-1.38487750506082,71.625651481593,0.));
#100604=CARTESIAN_POINT('Ctrl Pts',(-1.39298943246722,71.6475489729134,
0.));
#100605=CARTESIAN_POINT('Ctrl Pts',(-1.40113829463577,71.6694795096001,
0.));
#100606=CARTESIAN_POINT('Ctrl Pts',(-1.40932410760248,71.6914429498663,
0.));
#100607=CARTESIAN_POINT('Ctrl Pts',(-1.41754688723773,71.7134391525389,
0.));
#100608=CARTESIAN_POINT('Ctrl Pts',(-1.4258066492477,71.7354679770528,0.));
#100609=CARTESIAN_POINT('Ctrl Pts',(-1.43410340917496,71.7575292834469,
0.));
#100610=CARTESIAN_POINT('Ctrl Pts',(-1.44243718239315,71.7796229323526,
0.));
#100611=CARTESIAN_POINT('Ctrl Pts',(-1.45080798410965,71.8017487849895,
0.));
#100612=CARTESIAN_POINT('Ctrl Pts',(-1.45921582937232,71.8239067031683,
0.));
#100613=CARTESIAN_POINT('Ctrl Pts',(-1.46766073307088,71.8460965492839,
0.));
#100614=CARTESIAN_POINT('Ctrl Pts',(-1.47614270993729,71.8683181863116,
0.));
#100615=CARTESIAN_POINT('Ctrl Pts',(-1.4846617745402,71.8905714777961,0.));
#100616=CARTESIAN_POINT('Ctrl Pts',(-1.49321794128799,71.912856287848,0.));
#100617=CARTESIAN_POINT('Ctrl Pts',(-1.50181122443534,71.9351724811443,
0.));
#100618=CARTESIAN_POINT('Ctrl Pts',(-1.51044163808454,71.9575199229241,
0.));
#100619=CARTESIAN_POINT('Ctrl Pts',(-1.51910919618566,71.979898478983,0.));
#100620=CARTESIAN_POINT('Ctrl Pts',(-1.52781391253102,72.0023080156647,
0.));
#100621=CARTESIAN_POINT('Ctrl Pts',(-1.53655580075813,72.0247483998578,
0.));
#100622=CARTESIAN_POINT('Ctrl Pts',(-1.54533487435626,72.0472194989963,
0.));
#100623=CARTESIAN_POINT('Ctrl Pts',(-1.55415114666774,72.0697211810545,
0.));
#100624=CARTESIAN_POINT('Ctrl Pts',(-1.56300463088809,72.0922533145433,
0.));
#100625=CARTESIAN_POINT('Ctrl Pts',(-1.5718953400604,72.1148157684995,0.));
#100626=CARTESIAN_POINT('Ctrl Pts',(-1.58082328707803,72.1374084124839,
0.));
#100627=CARTESIAN_POINT('Ctrl Pts',(-1.58978848469123,72.1600311165821,
0.));
#100628=CARTESIAN_POINT('Ctrl Pts',(-1.59879094550847,72.1826837514001,
0.));
#100629=CARTESIAN_POINT('Ctrl Pts',(-1.60783068199663,72.2053661880608,
0.));
#100630=CARTESIAN_POINT('Ctrl Pts',(-1.6169077064754,72.2280782981937,0.));
#100631=CARTESIAN_POINT('Ctrl Pts',(-1.6260220311193,72.2508199539323,0.));
#100632=CARTESIAN_POINT('Ctrl Pts',(-1.63517366796463,72.2735910279149,
0.));
#100633=CARTESIAN_POINT('Ctrl Pts',(-1.64436262891079,72.2963913932813,
0.));
#100634=CARTESIAN_POINT('Ctrl Pts',(-1.65358892572063,72.319220923669,0.));
#100635=CARTESIAN_POINT('Ctrl Pts',(-1.66285257001496,72.3420794932047,
0.));
#100636=CARTESIAN_POINT('Ctrl Pts',(-1.67215357327365,72.3649669765004,
0.));
#100637=CARTESIAN_POINT('Ctrl Pts',(-1.68149194684282,72.387883248654,0.));
#100638=CARTESIAN_POINT('Ctrl Pts',(-1.69086770193637,72.4108281852467,
0.));
#100639=CARTESIAN_POINT('Ctrl Pts',(-1.70028084963647,72.4338016623391,
0.));
#100640=CARTESIAN_POINT('Ctrl Pts',(-1.70973140088842,72.456803556463,0.));
#100641=CARTESIAN_POINT('Ctrl Pts',(-1.71921936650038,72.479833744618,0.));
#100642=CARTESIAN_POINT('Ctrl Pts',(-1.72874475715103,72.5028921042721,
0.));
#100643=CARTESIAN_POINT('Ctrl Pts',(-1.73830758339125,72.5259785133595,
0.));
#100644=CARTESIAN_POINT('Ctrl Pts',(-1.74790785564474,72.5490928502769,
0.));
#100645=CARTESIAN_POINT('Ctrl Pts',(-1.75754558420344,72.5722349938774,
0.));
#100646=CARTESIAN_POINT('Ctrl Pts',(-1.76722077922574,72.5954048234638,
0.));
#100647=CARTESIAN_POINT('Ctrl Pts',(-1.77693345074427,72.6186022187907,
0.));
#100648=CARTESIAN_POINT('Ctrl Pts',(-1.78668360866811,72.6418270600619,
0.));
#100649=CARTESIAN_POINT('Ctrl Pts',(-1.79647126278359,72.6650792279274,
0.));
#100650=CARTESIAN_POINT('Ctrl Pts',(-1.80629642275051,72.6883586034769,
0.));
#100651=CARTESIAN_POINT('Ctrl Pts',(-1.81615909809871,72.7116650682344,
0.));
#100652=CARTESIAN_POINT('Ctrl Pts',(-1.82605929823564,72.7349985041592,
0.));
#100653=CARTESIAN_POINT('Ctrl Pts',(-1.83599703244924,72.7583587936447,
0.));
#100654=CARTESIAN_POINT('Ctrl Pts',(-1.84597230990857,72.7817458195155,
0.));
#100655=CARTESIAN_POINT('Ctrl Pts',(-1.85598513966114,72.8051594650222,
0.));
#100656=CARTESIAN_POINT('Ctrl Pts',(-1.86603553062771,72.8285996138359,
0.));
#100657=CARTESIAN_POINT('Ctrl Pts',(-1.87612349160945,72.8520661500477,
0.));
#100658=CARTESIAN_POINT('Ctrl Pts',(-1.88624903129188,72.875558958168,0.));
#100659=CARTESIAN_POINT('Ctrl Pts',(-1.89641215824582,72.8990779231226,
0.));
#100660=CARTESIAN_POINT('Ctrl Pts',(-1.90661288092587,72.9226229302478,
0.));
#100661=CARTESIAN_POINT('Ctrl Pts',(-1.91685120766437,72.9461938652811,
0.));
#100662=CARTESIAN_POINT('Ctrl Pts',(-1.9271271466766,72.9697906143636,0.));
#100663=CARTESIAN_POINT('Ctrl Pts',(-1.93744070606566,72.9934130640415,
0.));
#100664=CARTESIAN_POINT('Ctrl Pts',(-1.94779189382302,73.0170611012661,
0.));
#100665=CARTESIAN_POINT('Ctrl Pts',(-1.95818071782767,73.040734613391,0.));
#100666=CARTESIAN_POINT('Ctrl Pts',(-1.96860718583932,73.0644334881673,
0.));
#100667=CARTESIAN_POINT('Ctrl Pts',(-1.97907130550158,73.0881576137407,
0.));
#100668=CARTESIAN_POINT('Ctrl Pts',(-1.98957308434918,73.1119068786475,
0.));
#100669=CARTESIAN_POINT('Ctrl Pts',(-2.00011252980982,73.1356811718091,
0.));
#100670=CARTESIAN_POINT('Ctrl Pts',(-2.01068964920467,73.1594803825252,
0.));
#100671=CARTESIAN_POINT('Ctrl Pts',(-2.02130444974362,73.183304400462,0.));
#100672=CARTESIAN_POINT('Ctrl Pts',(-2.03195693852455,73.2071531156504,
0.));
#100673=CARTESIAN_POINT('Ctrl Pts',(-2.04264712253929,73.2310264184976,
0.));
#100674=CARTESIAN_POINT('Ctrl Pts',(-2.05337500867403,73.2549241997953,
0.));
#100675=CARTESIAN_POINT('Ctrl Pts',(-2.06414060370835,73.2788463507246,
0.));
#100676=CARTESIAN_POINT('Ctrl Pts',(-2.07494391430941,73.3027927628626,
0.));
#100677=CARTESIAN_POINT('Ctrl Pts',(-2.08578494702744,73.3267633281807,
0.));
#100678=CARTESIAN_POINT('Ctrl Pts',(-2.09666370830716,73.3507579390239,
0.));
#100679=CARTESIAN_POINT('Ctrl Pts',(-2.1075802044939,73.3747764880893,0.));
#100680=CARTESIAN_POINT('Ctrl Pts',(-2.11853444183762,73.3988188684021,
0.));
#100681=CARTESIAN_POINT('Ctrl Pts',(-2.12952642649368,73.4228849732925,
0.));
#100682=CARTESIAN_POINT('Ctrl Pts',(-2.14055616452058,73.4469746963637,
0.));
#100683=CARTESIAN_POINT('Ctrl Pts',(-2.15162366187907,73.4710879315382,
0.));
#100684=CARTESIAN_POINT('Ctrl Pts',(-2.1627289244292,73.4952245731054,0.));
#100685=CARTESIAN_POINT('Ctrl Pts',(-2.17387195792306,73.5193845157708,
0.));
#100686=CARTESIAN_POINT('Ctrl Pts',(-2.18505276799753,73.5435676546929,
0.));
#100687=CARTESIAN_POINT('Ctrl Pts',(-2.19627136015678,73.5677738855452,
0.));
#100688=CARTESIAN_POINT('Ctrl Pts',(-2.20752773978349,73.5920031044595,
0.));
#100689=CARTESIAN_POINT('Ctrl Pts',(-2.21882191216518,73.6162552079038,
0.));
#100690=CARTESIAN_POINT('Ctrl Pts',(-2.23015388251288,73.6405300925712,
0.));
#100691=CARTESIAN_POINT('Ctrl Pts',(-2.24152365597698,73.6648276552767,
0.));
#100692=CARTESIAN_POINT('Ctrl Pts',(-2.25293123766425,73.6891477928129,
0.));
#100693=CARTESIAN_POINT('Ctrl Pts',(-2.26437663263667,73.7134904019389,
0.));
#100694=CARTESIAN_POINT('Ctrl Pts',(-2.27585984587199,73.7378553796807,
0.));
#100695=CARTESIAN_POINT('Ctrl Pts',(-2.28738088222864,73.762242623566,0.));
#100696=CARTESIAN_POINT('Ctrl Pts',(-2.29893974640434,73.786652031885,0.));
#100697=CARTESIAN_POINT('Ctrl Pts',(-2.31053644289417,73.8110835039327,
0.));
#100698=CARTESIAN_POINT('Ctrl Pts',(-2.32217097594198,73.8355369402706,
0.));
#100699=CARTESIAN_POINT('Ctrl Pts',(-2.33384334963958,73.8600122421468,
0.));
#100700=CARTESIAN_POINT('Ctrl Pts',(-2.34555356802121,73.8845093109274,
0.));
#100701=CARTESIAN_POINT('Ctrl Pts',(-2.35730163516316,73.9090280474712,
0.));
#100702=CARTESIAN_POINT('Ctrl Pts',(-2.36908755526003,73.9335683516404,
0.));
#100703=CARTESIAN_POINT('Ctrl Pts',(-2.38091133274961,73.958130121465,0.));
#100704=CARTESIAN_POINT('Ctrl Pts',(-2.39277297220757,73.9827132538206,
0.));
#100705=CARTESIAN_POINT('Ctrl Pts',(-2.40467247811536,74.0073176459344,
0.));
#100706=CARTESIAN_POINT('Ctrl Pts',(-2.41660985465252,74.0319431966989,
0.));
#100707=CARTESIAN_POINT('Ctrl Pts',(-2.42858510549779,74.0565898079218,
0.));
#100708=CARTESIAN_POINT('Ctrl Pts',(-2.44059823356676,74.0812573859411,
0.));
#100709=CARTESIAN_POINT('Ctrl Pts',(-2.45264924094775,74.1059458420067,
0.));
#100710=CARTESIAN_POINT('Ctrl Pts',(-2.46301176097121,74.127126454519,0.));
#100711=CARTESIAN_POINT('Ctrl Pts',(-2.47097695564999,74.1433763941381,
0.));
#100712=CARTESIAN_POINT('Ctrl Pts',(-2.47652804724547,74.1546864735168,
0.));
#100713=CARTESIAN_POINT('Ctrl Pts',(-2.47965393945487,74.1610506466209,
0.));
#100714=CARTESIAN_POINT('Ctrl Pts',(-2.48034921843244,74.1624659714558,
0.));
#100715=CARTESIAN_POINT('',(-0.853825826608985,69.9947925310006,12.));
#100716=CARTESIAN_POINT('',(-0.853825826608985,69.9947925310006,0.));
#100717=CARTESIAN_POINT('Ctrl Pts',(-2.48034921843246,74.1624659714558,
12.));
#100718=CARTESIAN_POINT('Ctrl Pts',(-2.47965393945489,74.1610506466209,
12.));
#100719=CARTESIAN_POINT('Ctrl Pts',(-2.47652804724548,74.1546864735169,
12.));
#100720=CARTESIAN_POINT('Ctrl Pts',(-2.47097695565,74.1433763941382,12.));
#100721=CARTESIAN_POINT('Ctrl Pts',(-2.46301176097121,74.127126454519,12.));
#100722=CARTESIAN_POINT('Ctrl Pts',(-2.45264924094775,74.1059458420067,
12.));
#100723=CARTESIAN_POINT('Ctrl Pts',(-2.44059823356676,74.0812573859411,
12.));
#100724=CARTESIAN_POINT('Ctrl Pts',(-2.42858510549779,74.0565898079218,
12.));
#100725=CARTESIAN_POINT('Ctrl Pts',(-2.41660985465252,74.0319431966989,
12.));
#100726=CARTESIAN_POINT('Ctrl Pts',(-2.40467247811536,74.0073176459344,
12.));
#100727=CARTESIAN_POINT('Ctrl Pts',(-2.39277297220757,73.9827132538206,
12.));
#100728=CARTESIAN_POINT('Ctrl Pts',(-2.38091133274961,73.958130121465,12.));
#100729=CARTESIAN_POINT('Ctrl Pts',(-2.36908755526003,73.9335683516404,
12.));
#100730=CARTESIAN_POINT('Ctrl Pts',(-2.35730163516316,73.9090280474712,
12.));
#100731=CARTESIAN_POINT('Ctrl Pts',(-2.34555356802121,73.8845093109274,
12.));
#100732=CARTESIAN_POINT('Ctrl Pts',(-2.33384334963958,73.8600122421468,
12.));
#100733=CARTESIAN_POINT('Ctrl Pts',(-2.32217097594198,73.8355369402706,
12.));
#100734=CARTESIAN_POINT('Ctrl Pts',(-2.31053644289417,73.8110835039327,
12.));
#100735=CARTESIAN_POINT('Ctrl Pts',(-2.29893974640434,73.786652031885,12.));
#100736=CARTESIAN_POINT('Ctrl Pts',(-2.28738088222864,73.762242623566,12.));
#100737=CARTESIAN_POINT('Ctrl Pts',(-2.27585984587199,73.7378553796807,
12.));
#100738=CARTESIAN_POINT('Ctrl Pts',(-2.26437663263667,73.7134904019389,
12.));
#100739=CARTESIAN_POINT('Ctrl Pts',(-2.25293123766425,73.6891477928129,
12.));
#100740=CARTESIAN_POINT('Ctrl Pts',(-2.24152365597698,73.6648276552767,
12.));
#100741=CARTESIAN_POINT('Ctrl Pts',(-2.23015388251288,73.6405300925712,
12.));
#100742=CARTESIAN_POINT('Ctrl Pts',(-2.21882191216518,73.6162552079038,
12.));
#100743=CARTESIAN_POINT('Ctrl Pts',(-2.20752773978349,73.5920031044595,
12.));
#100744=CARTESIAN_POINT('Ctrl Pts',(-2.19627136015678,73.5677738855452,
12.));
#100745=CARTESIAN_POINT('Ctrl Pts',(-2.18505276799753,73.5435676546929,
12.));
#100746=CARTESIAN_POINT('Ctrl Pts',(-2.17387195792306,73.5193845157708,
12.));
#100747=CARTESIAN_POINT('Ctrl Pts',(-2.1627289244292,73.4952245731054,12.));
#100748=CARTESIAN_POINT('Ctrl Pts',(-2.15162366187907,73.4710879315382,
12.));
#100749=CARTESIAN_POINT('Ctrl Pts',(-2.14055616452058,73.4469746963637,
12.));
#100750=CARTESIAN_POINT('Ctrl Pts',(-2.12952642649368,73.4228849732925,
12.));
#100751=CARTESIAN_POINT('Ctrl Pts',(-2.11853444183762,73.3988188684021,
12.));
#100752=CARTESIAN_POINT('Ctrl Pts',(-2.1075802044939,73.3747764880893,12.));
#100753=CARTESIAN_POINT('Ctrl Pts',(-2.09666370830716,73.3507579390239,
12.));
#100754=CARTESIAN_POINT('Ctrl Pts',(-2.08578494702744,73.3267633281807,
12.));
#100755=CARTESIAN_POINT('Ctrl Pts',(-2.07494391430941,73.3027927628626,
12.));
#100756=CARTESIAN_POINT('Ctrl Pts',(-2.06414060370835,73.2788463507246,
12.));
#100757=CARTESIAN_POINT('Ctrl Pts',(-2.05337500867403,73.2549241997953,
12.));
#100758=CARTESIAN_POINT('Ctrl Pts',(-2.04264712253929,73.2310264184976,
12.));
#100759=CARTESIAN_POINT('Ctrl Pts',(-2.03195693852455,73.2071531156504,
12.));
#100760=CARTESIAN_POINT('Ctrl Pts',(-2.02130444974362,73.183304400462,12.));
#100761=CARTESIAN_POINT('Ctrl Pts',(-2.01068964920467,73.1594803825252,
12.));
#100762=CARTESIAN_POINT('Ctrl Pts',(-2.00011252980982,73.1356811718091,
12.));
#100763=CARTESIAN_POINT('Ctrl Pts',(-1.98957308434918,73.1119068786475,
12.));
#100764=CARTESIAN_POINT('Ctrl Pts',(-1.97907130550158,73.0881576137407,
12.));
#100765=CARTESIAN_POINT('Ctrl Pts',(-1.96860718583932,73.0644334881673,
12.));
#100766=CARTESIAN_POINT('Ctrl Pts',(-1.95818071782767,73.040734613391,12.));
#100767=CARTESIAN_POINT('Ctrl Pts',(-1.94779189382302,73.0170611012661,
12.));
#100768=CARTESIAN_POINT('Ctrl Pts',(-1.93744070606566,72.9934130640415,
12.));
#100769=CARTESIAN_POINT('Ctrl Pts',(-1.9271271466766,72.9697906143636,12.));
#100770=CARTESIAN_POINT('Ctrl Pts',(-1.91685120766437,72.9461938652811,
12.));
#100771=CARTESIAN_POINT('Ctrl Pts',(-1.90661288092587,72.9226229302478,
12.));
#100772=CARTESIAN_POINT('Ctrl Pts',(-1.89641215824582,72.8990779231226,
12.));
#100773=CARTESIAN_POINT('Ctrl Pts',(-1.88624903129188,72.875558958168,12.));
#100774=CARTESIAN_POINT('Ctrl Pts',(-1.87612349160945,72.8520661500477,
12.));
#100775=CARTESIAN_POINT('Ctrl Pts',(-1.86603553062771,72.8285996138359,
12.));
#100776=CARTESIAN_POINT('Ctrl Pts',(-1.85598513966114,72.8051594650222,
12.));
#100777=CARTESIAN_POINT('Ctrl Pts',(-1.84597230990857,72.7817458195155,
12.));
#100778=CARTESIAN_POINT('Ctrl Pts',(-1.83599703244924,72.7583587936447,
12.));
#100779=CARTESIAN_POINT('Ctrl Pts',(-1.82605929823564,72.7349985041592,
12.));
#100780=CARTESIAN_POINT('Ctrl Pts',(-1.81615909809871,72.7116650682344,
12.));
#100781=CARTESIAN_POINT('Ctrl Pts',(-1.80629642275051,72.6883586034769,
12.));
#100782=CARTESIAN_POINT('Ctrl Pts',(-1.79647126278359,72.6650792279274,
12.));
#100783=CARTESIAN_POINT('Ctrl Pts',(-1.78668360866811,72.6418270600619,
12.));
#100784=CARTESIAN_POINT('Ctrl Pts',(-1.77693345074427,72.6186022187907,
12.));
#100785=CARTESIAN_POINT('Ctrl Pts',(-1.76722077922574,72.5954048234638,
12.));
#100786=CARTESIAN_POINT('Ctrl Pts',(-1.75754558420344,72.5722349938774,
12.));
#100787=CARTESIAN_POINT('Ctrl Pts',(-1.74790785564474,72.5490928502769,
12.));
#100788=CARTESIAN_POINT('Ctrl Pts',(-1.73830758339125,72.5259785133595,
12.));
#100789=CARTESIAN_POINT('Ctrl Pts',(-1.72874475715103,72.5028921042721,
12.));
#100790=CARTESIAN_POINT('Ctrl Pts',(-1.71921936650038,72.479833744618,12.));
#100791=CARTESIAN_POINT('Ctrl Pts',(-1.70973140088842,72.456803556463,12.));
#100792=CARTESIAN_POINT('Ctrl Pts',(-1.70028084963647,72.4338016623391,
12.));
#100793=CARTESIAN_POINT('Ctrl Pts',(-1.69086770193637,72.4108281852467,
12.));
#100794=CARTESIAN_POINT('Ctrl Pts',(-1.68149194684282,72.387883248654,12.));
#100795=CARTESIAN_POINT('Ctrl Pts',(-1.67215357327365,72.3649669765004,
12.));
#100796=CARTESIAN_POINT('Ctrl Pts',(-1.66285257001496,72.3420794932047,
12.));
#100797=CARTESIAN_POINT('Ctrl Pts',(-1.65358892572063,72.319220923669,12.));
#100798=CARTESIAN_POINT('Ctrl Pts',(-1.64436262891079,72.2963913932813,
12.));
#100799=CARTESIAN_POINT('Ctrl Pts',(-1.63517366796463,72.2735910279149,
12.));
#100800=CARTESIAN_POINT('Ctrl Pts',(-1.6260220311193,72.2508199539323,12.));
#100801=CARTESIAN_POINT('Ctrl Pts',(-1.6169077064754,72.2280782981937,12.));
#100802=CARTESIAN_POINT('Ctrl Pts',(-1.60783068199663,72.2053661880608,
12.));
#100803=CARTESIAN_POINT('Ctrl Pts',(-1.59879094550847,72.1826837514001,
12.));
#100804=CARTESIAN_POINT('Ctrl Pts',(-1.58978848469123,72.1600311165821,
12.));
#100805=CARTESIAN_POINT('Ctrl Pts',(-1.58082328707803,72.1374084124839,
12.));
#100806=CARTESIAN_POINT('Ctrl Pts',(-1.5718953400604,72.1148157684995,12.));
#100807=CARTESIAN_POINT('Ctrl Pts',(-1.56300463088809,72.0922533145433,
12.));
#100808=CARTESIAN_POINT('Ctrl Pts',(-1.55415114666774,72.0697211810545,
12.));
#100809=CARTESIAN_POINT('Ctrl Pts',(-1.54533487435626,72.0472194989963,
12.));
#100810=CARTESIAN_POINT('Ctrl Pts',(-1.53655580075813,72.0247483998578,
12.));
#100811=CARTESIAN_POINT('Ctrl Pts',(-1.52781391253102,72.0023080156647,
12.));
#100812=CARTESIAN_POINT('Ctrl Pts',(-1.51910919618566,71.979898478983,12.));
#100813=CARTESIAN_POINT('Ctrl Pts',(-1.51044163808454,71.9575199229241,
12.));
#100814=CARTESIAN_POINT('Ctrl Pts',(-1.50181122443534,71.9351724811443,
12.));
#100815=CARTESIAN_POINT('Ctrl Pts',(-1.49321794128799,71.912856287848,12.));
#100816=CARTESIAN_POINT('Ctrl Pts',(-1.4846617745402,71.8905714777961,12.));
#100817=CARTESIAN_POINT('Ctrl Pts',(-1.47614270993729,71.8683181863116,
12.));
#100818=CARTESIAN_POINT('Ctrl Pts',(-1.46766073307088,71.8460965492839,
12.));
#100819=CARTESIAN_POINT('Ctrl Pts',(-1.45921582937232,71.8239067031683,
12.));
#100820=CARTESIAN_POINT('Ctrl Pts',(-1.45080798410965,71.8017487849895,
12.));
#100821=CARTESIAN_POINT('Ctrl Pts',(-1.44243718239315,71.7796229323526,
12.));
#100822=CARTESIAN_POINT('Ctrl Pts',(-1.43410340917496,71.7575292834469,
12.));
#100823=CARTESIAN_POINT('Ctrl Pts',(-1.4258066492477,71.7354679770528,12.));
#100824=CARTESIAN_POINT('Ctrl Pts',(-1.41754688723773,71.7134391525389,
12.));
#100825=CARTESIAN_POINT('Ctrl Pts',(-1.40932410760248,71.6914429498663,
12.));
#100826=CARTESIAN_POINT('Ctrl Pts',(-1.40113829463577,71.6694795096001,
12.));
#100827=CARTESIAN_POINT('Ctrl Pts',(-1.39298943246722,71.6475489729134,
12.));
#100828=CARTESIAN_POINT('Ctrl Pts',(-1.38487750506082,71.625651481593,12.));
#100829=CARTESIAN_POINT('Ctrl Pts',(-1.3768024962078,71.6037871780385,12.));
#100830=CARTESIAN_POINT('Ctrl Pts',(-1.36876438952466,71.5819562052663,
12.));
#100831=CARTESIAN_POINT('Ctrl Pts',(-1.36076316845816,71.5601587069217,
12.));
#100832=CARTESIAN_POINT('Ctrl Pts',(-1.35279881628455,71.5383948272845,
12.));
#100833=CARTESIAN_POINT('Ctrl Pts',(-1.34487131610781,71.516664711275,12.));
#100834=CARTESIAN_POINT('Ctrl Pts',(-1.3369806508522,71.4949685044522,12.));
#100835=CARTESIAN_POINT('Ctrl Pts',(-1.32912680326124,71.4733063530187,
12.));
#100836=CARTESIAN_POINT('Ctrl Pts',(-1.32130975590226,71.4516784038317,
12.));
#100837=CARTESIAN_POINT('Ctrl Pts',(-1.31352949116537,71.4300848044087,
12.));
#100838=CARTESIAN_POINT('Ctrl Pts',(-1.3057859912614,71.4085257029322,12.));
#100839=CARTESIAN_POINT('Ctrl Pts',(-1.29807923821414,71.3870012482499,
12.));
#100840=CARTESIAN_POINT('Ctrl Pts',(-1.29040921386059,71.3655115898827,
12.));
#100841=CARTESIAN_POINT('Ctrl Pts',(-1.28277589985472,71.3440568780347,
12.));
#100842=CARTESIAN_POINT('Ctrl Pts',(-1.27517927766608,71.3226372635996,
12.));
#100843=CARTESIAN_POINT('Ctrl Pts',(-1.26761932857724,71.3012528981661,
12.));
#100844=CARTESIAN_POINT('Ctrl Pts',(-1.26009603367571,71.2799039340175,
12.));
#100845=CARTESIAN_POINT('Ctrl Pts',(-1.25260937385569,71.2585905241406,
12.));
#100846=CARTESIAN_POINT('Ctrl Pts',(-1.24515932982113,71.2373128222352,
12.));
#100847=CARTESIAN_POINT('Ctrl Pts',(-1.23774588208427,71.2160709827191,
12.));
#100848=CARTESIAN_POINT('Ctrl Pts',(-1.23036901096239,71.194865160732,12.));
#100849=CARTESIAN_POINT('Ctrl Pts',(-1.22302869657018,71.1736955121362,
12.));
#100850=CARTESIAN_POINT('Ctrl Pts',(-1.21572491882263,71.1525621935267,
12.));
#100851=CARTESIAN_POINT('Ctrl Pts',(-1.20845765743648,71.1314653622442,
12.));
#100852=CARTESIAN_POINT('Ctrl Pts',(-1.20122689192836,71.1104051763839,
12.));
#100853=CARTESIAN_POINT('Ctrl Pts',(-1.19403260161002,71.089381794801,12.));
#100854=CARTESIAN_POINT('Ctrl Pts',(-1.18687476558133,71.0683953771149,
12.));
#100855=CARTESIAN_POINT('Ctrl Pts',(-1.17975336273504,71.0474460837159,
12.));
#100856=CARTESIAN_POINT('Ctrl Pts',(-1.17266837175777,71.0265340757699,
12.));
#100857=CARTESIAN_POINT('Ctrl Pts',(-1.1656197711288,71.0056595152204,12.));
#100858=CARTESIAN_POINT('Ctrl Pts',(-1.15860753911485,70.9848225647871,
12.));
#100859=CARTESIAN_POINT('Ctrl Pts',(-1.15163165376524,70.9640233879659,
12.));
#100860=CARTESIAN_POINT('Ctrl Pts',(-1.14469209291489,70.9432621490566,
12.));
#100861=CARTESIAN_POINT('Ctrl Pts',(-1.13778883418214,70.9225390131826,
12.));
#100862=CARTESIAN_POINT('Ctrl Pts',(-1.13092185496565,70.9018541463089,
12.));
#100863=CARTESIAN_POINT('Ctrl Pts',(-1.12409113243514,70.8812077152586,
12.));
#100864=CARTESIAN_POINT('Ctrl Pts',(-1.11729664352993,70.8605998877149,
12.));
#100865=CARTESIAN_POINT('Ctrl Pts',(-1.1105383649664,70.8400308322037,12.));
#100866=CARTESIAN_POINT('Ctrl Pts',(-1.10381627323947,70.8195007180745,
12.));
#100867=CARTESIAN_POINT('Ctrl Pts',(-1.09713034462265,70.799009715484,12.));
#100868=CARTESIAN_POINT('Ctrl Pts',(-1.09048055516427,70.7785579953583,
12.));
#100869=CARTESIAN_POINT('Ctrl Pts',(-1.08386688068342,70.7581457294447,
12.));
#100870=CARTESIAN_POINT('Ctrl Pts',(-1.07728929676408,70.7377730903953,
12.));
#100871=CARTESIAN_POINT('Ctrl Pts',(-1.07074777874596,70.7174402518378,
12.));
#100872=CARTESIAN_POINT('Ctrl Pts',(-1.06424230171281,70.6971473884459,
12.));
#100873=CARTESIAN_POINT('Ctrl Pts',(-1.0577728404773,70.676894676009,12.));
#100874=CARTESIAN_POINT('Ctrl Pts',(-1.05133936960072,70.6566822912991,
12.));
#100875=CARTESIAN_POINT('Ctrl Pts',(-1.04494186341156,70.6365104119252,
12.));
#100876=CARTESIAN_POINT('Ctrl Pts',(-1.03858029601904,70.6163792162073,
12.));
#100877=CARTESIAN_POINT('Ctrl Pts',(-1.0322546413287,70.5962888829934,12.));
#100878=CARTESIAN_POINT('Ctrl Pts',(-1.02596487304049,70.5762395916377,
12.));
#100879=CARTESIAN_POINT('Ctrl Pts',(-1.01971096460597,70.556231522419,12.));
#100880=CARTESIAN_POINT('Ctrl Pts',(-1.01349288918537,70.5362648569061,
12.));
#100881=CARTESIAN_POINT('Ctrl Pts',(-1.00731061960968,70.5163397782713,
12.));
#100882=CARTESIAN_POINT('Ctrl Pts',(-1.00116412831442,70.4964564717953,
12.));
#100883=CARTESIAN_POINT('Ctrl Pts',(-0.995053387379757,70.4766151245212,
12.));
#100884=CARTESIAN_POINT('Ctrl Pts',(-0.98897836864365,70.4568159243163,
12.));
#100885=CARTESIAN_POINT('Ctrl Pts',(-0.982939043792157,70.4370590590842,
12.));
#100886=CARTESIAN_POINT('Ctrl Pts',(-0.976935384450043,70.417344715957,
12.));
#100887=CARTESIAN_POINT('Ctrl Pts',(-0.970967362281175,70.3976730803614,
12.));
#100888=CARTESIAN_POINT('Ctrl Pts',(-0.965034948786451,70.3780443377956,
12.));
#100889=CARTESIAN_POINT('Ctrl Pts',(-0.959138115058833,70.3584586759536,
12.));
#100890=CARTESIAN_POINT('Ctrl Pts',(-0.953276831581243,70.338916286458,
12.));
#100891=CARTESIAN_POINT('Ctrl Pts',(-0.947451067929606,70.3194173673674,
12.));
#100892=CARTESIAN_POINT('Ctrl Pts',(-0.941660792742981,70.299962123399,
12.));
#100893=CARTESIAN_POINT('Ctrl Pts',(-0.935905974336482,70.2805507606872,
12.));
#100894=CARTESIAN_POINT('Ctrl Pts',(-0.930186581235549,70.2611834821724,
12.));
#100895=CARTESIAN_POINT('Ctrl Pts',(-0.924502582639457,70.2418604835837,
12.));
#100896=CARTESIAN_POINT('Ctrl Pts',(-0.91885394915712,70.2225819470248,
12.));
#100897=CARTESIAN_POINT('Ctrl Pts',(-0.913240652090982,70.2033480471676,
12.));
#100898=CARTESIAN_POINT('Ctrl Pts',(-0.907662662015787,70.1841589635574,
12.));
#100899=CARTESIAN_POINT('Ctrl Pts',(-0.902119947629773,70.1650148905109,
12.));
#100900=CARTESIAN_POINT('Ctrl Pts',(-0.896612474371846,70.1459160490446,
12.));
#100901=CARTESIAN_POINT('Ctrl Pts',(-0.891140203464243,70.1268626950175,
12.));
#100902=CARTESIAN_POINT('Ctrl Pts',(-0.885703094802537,70.1078550938958,
12.));
#100903=CARTESIAN_POINT('Ctrl Pts',(-0.880301109660729,70.0888934967855,
12.));
#100904=CARTESIAN_POINT('Ctrl Pts',(-0.874934213255839,70.0699781183935,
12.));
#100905=CARTESIAN_POINT('Ctrl Pts',(-0.869602377871126,70.051109108301,
12.));
#100906=CARTESIAN_POINT('Ctrl Pts',(-0.864305583661547,70.0322865492925,
12.));
#100907=CARTESIAN_POINT('Ctrl Pts',(-0.860096170668736,70.0172656933806,
12.));
#100908=CARTESIAN_POINT('Ctrl Pts',(-0.856954870259207,70.0060209754087,
12.));
#100909=CARTESIAN_POINT('Ctrl Pts',(-0.854867673848596,69.9985337959407,
12.));
#100910=CARTESIAN_POINT('Ctrl Pts',(-0.853825826608985,69.9947925310006,
12.));
#100911=CARTESIAN_POINT('Ctrl Pts',(-3.99277406490868,74.0964320766208,
0.));
#100912=CARTESIAN_POINT('Ctrl Pts',(-3.99277406490868,74.0964320766208,
4.));
#100913=CARTESIAN_POINT('Ctrl Pts',(-3.99277406490873,74.0964320766207,
8.));
#100914=CARTESIAN_POINT('Ctrl Pts',(-3.99277406490873,74.0964320766207,
12.));
#100915=CARTESIAN_POINT('Ctrl Pts',(-3.95310474582227,74.1989040313893,
0.));
#100916=CARTESIAN_POINT('Ctrl Pts',(-3.95310474582227,74.1989040313893,
4.));
#100917=CARTESIAN_POINT('Ctrl Pts',(-3.95310474582232,74.1989040313892,
8.00000000000001));
#100918=CARTESIAN_POINT('Ctrl Pts',(-3.95310474582232,74.1989040313892,
12.));
#100919=CARTESIAN_POINT('Ctrl Pts',(-3.8225214201853,74.3538917248566,0.));
#100920=CARTESIAN_POINT('Ctrl Pts',(-3.8225214201853,74.3538917248566,4.));
#100921=CARTESIAN_POINT('Ctrl Pts',(-3.82252142018534,74.3538917248565,
7.99999999999999));
#100922=CARTESIAN_POINT('Ctrl Pts',(-3.82252142018534,74.3538917248565,
12.));
#100923=CARTESIAN_POINT('Ctrl Pts',(-3.63264011802871,74.4114286752098,
0.));
#100924=CARTESIAN_POINT('Ctrl Pts',(-3.63264011802871,74.4114286752098,
4.));
#100925=CARTESIAN_POINT('Ctrl Pts',(-3.63264011802875,74.4114286752097,
8.00000000000001));
#100926=CARTESIAN_POINT('Ctrl Pts',(-3.63264011802875,74.4114286752097,
12.));
#100927=CARTESIAN_POINT('Ctrl Pts',(-3.55032190142806,74.4153560388998,
0.));
#100928=CARTESIAN_POINT('Ctrl Pts',(-3.55032190142806,74.4153560388998,
4.));
#100929=CARTESIAN_POINT('Ctrl Pts',(-3.55032190142811,74.4153560388997,
8.));
#100930=CARTESIAN_POINT('Ctrl Pts',(-3.55032190142811,74.4153560388997,
12.));
#100931=CARTESIAN_POINT('',(-3.99277406490868,74.0964320766208,0.));
#100932=CARTESIAN_POINT('',(-3.55032190142807,74.4153560388999,0.));
#100933=CARTESIAN_POINT('Ctrl Pts',(-3.99277406490868,74.0964320766208,
2.77555756156289E-16));
#100934=CARTESIAN_POINT('Ctrl Pts',(-3.95310474582227,74.1989040313893,
2.77555756156289E-16));
#100935=CARTESIAN_POINT('Ctrl Pts',(-3.87848570260114,74.2874684276564,
2.77555756156289E-16));
#100936=CARTESIAN_POINT('Ctrl Pts',(-3.78450405480218,74.3442121731106,
2.77555756156289E-16));
#100937=CARTESIAN_POINT('Ctrl Pts',(-3.71401781895296,74.3867699822013,
2.77555756156289E-16));
#100938=CARTESIAN_POINT('Ctrl Pts',(-3.63264011802871,74.4114286752098,
2.77555756156289E-16));
#100939=CARTESIAN_POINT('Ctrl Pts',(-3.55032190142806,74.4153560388998,
2.77555756156289E-16));
#100940=CARTESIAN_POINT('',(-3.55032190142812,74.4153560388999,12.));
#100941=CARTESIAN_POINT('Ctrl Pts',(-3.55032190142806,74.4153560388998,
0.));
#100942=CARTESIAN_POINT('Ctrl Pts',(-3.55032190142806,74.4153560388998,
4.));
#100943=CARTESIAN_POINT('Ctrl Pts',(-3.55032190142811,74.4153560388997,
8.));
#100944=CARTESIAN_POINT('Ctrl Pts',(-3.55032190142811,74.4153560388997,
12.));
#100945=CARTESIAN_POINT('',(-3.99277406490873,74.0964320766207,12.));
#100946=CARTESIAN_POINT('Ctrl Pts',(-3.55032190142811,74.4153560388997,
12.));
#100947=CARTESIAN_POINT('Ctrl Pts',(-3.63264011802875,74.4114286752097,
12.));
#100948=CARTESIAN_POINT('Ctrl Pts',(-3.714017818953,74.3867699822012,12.));
#100949=CARTESIAN_POINT('Ctrl Pts',(-3.78450405480223,74.3442121731105,
12.));
#100950=CARTESIAN_POINT('Ctrl Pts',(-3.87848570260119,74.2874684276563,
12.));
#100951=CARTESIAN_POINT('Ctrl Pts',(-3.95310474582232,74.1989040313892,
12.));
#100952=CARTESIAN_POINT('Ctrl Pts',(-3.99277406490873,74.0964320766207,
12.));
#100953=CARTESIAN_POINT('Ctrl Pts',(-3.99277406490873,74.0964320766207,
12.));
#100954=CARTESIAN_POINT('Ctrl Pts',(-3.99277406490873,74.0964320766207,
8.));
#100955=CARTESIAN_POINT('Ctrl Pts',(-3.99277406490868,74.0964320766208,
4.));
#100956=CARTESIAN_POINT('Ctrl Pts',(-3.99277406490868,74.0964320766208,
0.));
#100957=CARTESIAN_POINT('Origin',(-1.64496194443586E-11,3.74482667098164E-10,
0.));
#100958=CARTESIAN_POINT('Origin',(-1.64496194443586E-11,3.74482667098164E-10,
12.));
#100959=CARTESIAN_POINT('Origin',(-1.64496194443586E-11,3.74482667098164E-10,
0.));
#100960=CARTESIAN_POINT('Ctrl Pts',(3.55032190142515,74.4153560389001,-5.55111512312578E-16));
#100961=CARTESIAN_POINT('Ctrl Pts',(3.55032190142515,74.4153560389001,4.));
#100962=CARTESIAN_POINT('Ctrl Pts',(3.55032190142515,74.4153560389001,8.));
#100963=CARTESIAN_POINT('Ctrl Pts',(3.55032190142515,74.4153560389001,12.));
#100964=CARTESIAN_POINT('Ctrl Pts',(3.66007952356777,74.4101195539797,-5.55111512312578E-16));
#100965=CARTESIAN_POINT('Ctrl Pts',(3.66007952356777,74.4101195539797,4.));
#100966=CARTESIAN_POINT('Ctrl Pts',(3.66007952356776,74.4101195539797,8.00000000000001));
#100967=CARTESIAN_POINT('Ctrl Pts',(3.66007952356776,74.4101195539797,12.));
#100968=CARTESIAN_POINT('Ctrl Pts',(3.8484028241923,74.3352361483148,-5.55111512312578E-16));
#100969=CARTESIAN_POINT('Ctrl Pts',(3.8484028241923,74.3352361483148,4.));
#100970=CARTESIAN_POINT('Ctrl Pts',(3.84840282419229,74.3352361483148,7.99999999999999));
#100971=CARTESIAN_POINT('Ctrl Pts',(3.84840282419229,74.3352361483148,12.));
#100972=CARTESIAN_POINT('Ctrl Pts',(3.96302207561147,74.1732860426647,-5.55111512312578E-16));
#100973=CARTESIAN_POINT('Ctrl Pts',(3.96302207561147,74.1732860426647,4.));
#100974=CARTESIAN_POINT('Ctrl Pts',(3.96302207561146,74.1732860426647,8.00000000000001));
#100975=CARTESIAN_POINT('Ctrl Pts',(3.96302207561146,74.1732860426647,12.));
#100976=CARTESIAN_POINT('Ctrl Pts',(3.99277406492175,74.0964320765798,-5.55111512312578E-16));
#100977=CARTESIAN_POINT('Ctrl Pts',(3.99277406492175,74.0964320765798,4.));
#100978=CARTESIAN_POINT('Ctrl Pts',(3.99277406492174,74.0964320765798,8.));
#100979=CARTESIAN_POINT('Ctrl Pts',(3.99277406492174,74.0964320765798,12.));
#100980=CARTESIAN_POINT('',(3.55032190142515,74.4153560389001,0.));
#100981=CARTESIAN_POINT('',(3.99277406492179,74.0964320765798,0.));
#100982=CARTESIAN_POINT('Ctrl Pts',(3.55032190142515,74.4153560389001,0.));
#100983=CARTESIAN_POINT('Ctrl Pts',(3.66007952356777,74.4101195539797,-1.54074395550979E-31));
#100984=CARTESIAN_POINT('Ctrl Pts',(3.76769283821036,74.3673290364569,1.54074395550979E-31));
#100985=CARTESIAN_POINT('Ctrl Pts',(3.85123952454099,74.2961085760818,7.70371977754893E-32));
#100986=CARTESIAN_POINT('Ctrl Pts',(3.91389953928897,74.2426932308005,-7.70371977754894E-32));
#100987=CARTESIAN_POINT('Ctrl Pts',(3.96302207561147,74.1732860426647,-5.39260384428426E-31));
#100988=CARTESIAN_POINT('Ctrl Pts',(3.99277406492175,74.0964320765798,-7.70371977754895E-32));
#100989=CARTESIAN_POINT('',(3.99277406492179,74.0964320765798,12.));
#100990=CARTESIAN_POINT('Ctrl Pts',(3.99277406492175,74.0964320765798,-5.55111512312578E-16));
#100991=CARTESIAN_POINT('Ctrl Pts',(3.99277406492175,74.0964320765798,4.));
#100992=CARTESIAN_POINT('Ctrl Pts',(3.99277406492174,74.0964320765798,8.));
#100993=CARTESIAN_POINT('Ctrl Pts',(3.99277406492174,74.0964320765798,12.));
#100994=CARTESIAN_POINT('',(3.55032190142515,74.4153560389001,12.));
#100995=CARTESIAN_POINT('Ctrl Pts',(3.99277406492174,74.0964320765798,12.));
#100996=CARTESIAN_POINT('Ctrl Pts',(3.96302207561146,74.1732860426647,12.));
#100997=CARTESIAN_POINT('Ctrl Pts',(3.91389953928896,74.2426932308005,12.));
#100998=CARTESIAN_POINT('Ctrl Pts',(3.85123952454098,74.2961085760818,12.));
#100999=CARTESIAN_POINT('Ctrl Pts',(3.76769283821035,74.3673290364569,12.));
#101000=CARTESIAN_POINT('Ctrl Pts',(3.66007952356776,74.4101195539797,12.));
#101001=CARTESIAN_POINT('Ctrl Pts',(3.55032190142515,74.4153560389001,12.));
#101002=CARTESIAN_POINT('Ctrl Pts',(3.55032190142515,74.4153560389001,12.));
#101003=CARTESIAN_POINT('Ctrl Pts',(3.55032190142515,74.4153560389001,8.));
#101004=CARTESIAN_POINT('Ctrl Pts',(3.55032190142515,74.4153560389001,4.));
#101005=CARTESIAN_POINT('Ctrl Pts',(3.55032190142515,74.4153560389001,-5.55111512312578E-16));
#101006=CARTESIAN_POINT('Ctrl Pts',(5.24987136994593,69.8028570375097,0.));
#101007=CARTESIAN_POINT('Ctrl Pts',(5.24987136994593,69.8028570375097,12.));
#101008=CARTESIAN_POINT('Ctrl Pts',(5.24915955997427,69.8066748687772,0.));
#101009=CARTESIAN_POINT('Ctrl Pts',(5.24915955997427,69.8066748687772,12.));
#101010=CARTESIAN_POINT('Ctrl Pts',(5.24773285666377,69.8143154684204,0.));
#101011=CARTESIAN_POINT('Ctrl Pts',(5.24773285666377,69.8143154684204,12.));
#101012=CARTESIAN_POINT('Ctrl Pts',(5.24558355159751,69.8257911792159,0.));
#101013=CARTESIAN_POINT('Ctrl Pts',(5.24558355159751,69.8257911792159,12.));
#101014=CARTESIAN_POINT('Ctrl Pts',(5.2426993105457,69.841121750752,0.));
#101015=CARTESIAN_POINT('Ctrl Pts',(5.2426993105457,69.841121750752,12.));
#101016=CARTESIAN_POINT('Ctrl Pts',(5.23906316634803,69.8603343302743,0.));
#101017=CARTESIAN_POINT('Ctrl Pts',(5.23906316634803,69.8603343302743,12.));
#101018=CARTESIAN_POINT('Ctrl Pts',(5.23539616279621,69.8795962381599,0.));
#101019=CARTESIAN_POINT('Ctrl Pts',(5.23539616279621,69.8795962381599,12.));
#101020=CARTESIAN_POINT('Ctrl Pts',(5.23169827290556,69.8989073936688,0.));
#101021=CARTESIAN_POINT('Ctrl Pts',(5.23169827290556,69.8989073936688,12.));
#101022=CARTESIAN_POINT('Ctrl Pts',(5.22796945602795,69.9182676502048,0.));
#101023=CARTESIAN_POINT('Ctrl Pts',(5.22796945602795,69.9182676502048,12.));
#101024=CARTESIAN_POINT('Ctrl Pts',(5.22420965879982,69.9376767969095,0.));
#101025=CARTESIAN_POINT('Ctrl Pts',(5.22420965879982,69.9376767969095,12.));
#101026=CARTESIAN_POINT('Ctrl Pts',(5.22041882075722,69.9571345870076,0.));
#101027=CARTESIAN_POINT('Ctrl Pts',(5.22041882075722,69.9571345870076,12.));
#101028=CARTESIAN_POINT('Ctrl Pts',(5.2165968788114,69.9766407595385,0.));
#101029=CARTESIAN_POINT('Ctrl Pts',(5.2165968788114,69.9766407595385,12.));
#101030=CARTESIAN_POINT('Ctrl Pts',(5.2127437720326,69.9961950629965,0.));
#101031=CARTESIAN_POINT('Ctrl Pts',(5.2127437720326,69.9961950629965,12.));
#101032=CARTESIAN_POINT('Ctrl Pts',(5.20885944672837,70.0157972802182,0.));
#101033=CARTESIAN_POINT('Ctrl Pts',(5.20885944672837,70.0157972802182,12.));
#101034=CARTESIAN_POINT('Ctrl Pts',(5.20494385478026,70.0354472203546,0.));
#101035=CARTESIAN_POINT('Ctrl Pts',(5.20494385478026,70.0354472203546,12.));
#101036=CARTESIAN_POINT('Ctrl Pts',(5.20099695122657,70.0551447071082,0.));
#101037=CARTESIAN_POINT('Ctrl Pts',(5.20099695122657,70.0551447071082,12.));
#101038=CARTESIAN_POINT('Ctrl Pts',(5.19701869225529,70.0748895689729,0.));
#101039=CARTESIAN_POINT('Ctrl Pts',(5.19701869225529,70.0748895689729,12.));
#101040=CARTESIAN_POINT('Ctrl Pts',(5.19300903271581,70.0946816270997,0.));
#101041=CARTESIAN_POINT('Ctrl Pts',(5.19300903271581,70.0946816270997,12.));
#101042=CARTESIAN_POINT('Ctrl Pts',(5.18896792486566,70.1145206891885,0.));
#101043=CARTESIAN_POINT('Ctrl Pts',(5.18896792486566,70.1145206891885,12.));
#101044=CARTESIAN_POINT('Ctrl Pts',(5.18489531966266,70.1344065558145,0.));
#101045=CARTESIAN_POINT('Ctrl Pts',(5.18489531966266,70.1344065558145,12.));
#101046=CARTESIAN_POINT('Ctrl Pts',(5.18079116757667,70.1543390243892,0.));
#101047=CARTESIAN_POINT('Ctrl Pts',(5.18079116757667,70.1543390243892,12.));
#101048=CARTESIAN_POINT('Ctrl Pts',(5.17665541952384,70.1743178937077,0.));
#101049=CARTESIAN_POINT('Ctrl Pts',(5.17665541952384,70.1743178937077,12.));
#101050=CARTESIAN_POINT('Ctrl Pts',(5.1724880279339,70.1943429691167,0.));
#101051=CARTESIAN_POINT('Ctrl Pts',(5.1724880279339,70.1943429691167,12.));
#101052=CARTESIAN_POINT('Ctrl Pts',(5.16828894670109,70.2144140622953,0.));
#101053=CARTESIAN_POINT('Ctrl Pts',(5.16828894670109,70.2144140622953,12.));
#101054=CARTESIAN_POINT('Ctrl Pts',(5.16405813066977,70.2345309887833,0.));
#101055=CARTESIAN_POINT('Ctrl Pts',(5.16405813066977,70.2345309887833,12.));
#101056=CARTESIAN_POINT('Ctrl Pts',(5.15979553528204,70.2546935662722,0.));
#101057=CARTESIAN_POINT('Ctrl Pts',(5.15979553528204,70.2546935662722,12.));
#101058=CARTESIAN_POINT('Ctrl Pts',(5.1555011161486,70.2749016125105,0.));
#101059=CARTESIAN_POINT('Ctrl Pts',(5.1555011161486,70.2749016125105,12.));
#101060=CARTESIAN_POINT('Ctrl Pts',(5.15117482869255,70.2951549435512,0.));
#101061=CARTESIAN_POINT('Ctrl Pts',(5.15117482869255,70.2951549435512,12.));
#101062=CARTESIAN_POINT('Ctrl Pts',(5.14681662833081,70.3154533746736,0.));
#101063=CARTESIAN_POINT('Ctrl Pts',(5.14681662833081,70.3154533746736,12.));
#101064=CARTESIAN_POINT('Ctrl Pts',(5.1424264706348,70.3357967211796,0.));
#101065=CARTESIAN_POINT('Ctrl Pts',(5.1424264706348,70.3357967211796,12.));
#101066=CARTESIAN_POINT('Ctrl Pts',(5.13800431148904,70.3561847991714,0.));
#101067=CARTESIAN_POINT('Ctrl Pts',(5.13800431148904,70.3561847991714,12.));
#101068=CARTESIAN_POINT('Ctrl Pts',(5.13355010728568,70.3766174264757,0.));
#101069=CARTESIAN_POINT('Ctrl Pts',(5.13355010728568,70.3766174264757,12.));
#101070=CARTESIAN_POINT('Ctrl Pts',(5.12906381499457,70.3970944229851,0.));
#101071=CARTESIAN_POINT('Ctrl Pts',(5.12906381499457,70.3970944229851,12.));
#101072=CARTESIAN_POINT('Ctrl Pts',(5.12454539205329,70.417615610161,0.));
#101073=CARTESIAN_POINT('Ctrl Pts',(5.12454539205329,70.417615610161,12.));
#101074=CARTESIAN_POINT('Ctrl Pts',(5.11999479630212,70.4381808107245,0.));
#101075=CARTESIAN_POINT('Ctrl Pts',(5.11999479630212,70.4381808107245,12.));
#101076=CARTESIAN_POINT('Ctrl Pts',(5.11541198590933,70.458789848296,0.));
#101077=CARTESIAN_POINT('Ctrl Pts',(5.11541198590933,70.458789848296,12.));
#101078=CARTESIAN_POINT('Ctrl Pts',(5.11079691929214,70.4794425469825,0.));
#101079=CARTESIAN_POINT('Ctrl Pts',(5.11079691929214,70.4794425469825,12.));
#101080=CARTESIAN_POINT('Ctrl Pts',(5.10614955511665,70.500138731399,0.));
#101081=CARTESIAN_POINT('Ctrl Pts',(5.10614955511665,70.500138731399,12.));
#101082=CARTESIAN_POINT('Ctrl Pts',(5.10146985232942,70.5208782268497,0.));
#101083=CARTESIAN_POINT('Ctrl Pts',(5.10146985232942,70.5208782268497,12.));
#101084=CARTESIAN_POINT('Ctrl Pts',(5.09675777018184,70.5416608594526,0.));
#101085=CARTESIAN_POINT('Ctrl Pts',(5.09675777018184,70.5416608594526,12.));
#101086=CARTESIAN_POINT('Ctrl Pts',(5.09201326826135,70.5624864562824,0.));
#101087=CARTESIAN_POINT('Ctrl Pts',(5.09201326826135,70.5624864562824,12.));
#101088=CARTESIAN_POINT('Ctrl Pts',(5.08723630652274,70.5833548455014,0.));
#101089=CARTESIAN_POINT('Ctrl Pts',(5.08723630652274,70.5833548455014,12.));
#101090=CARTESIAN_POINT('Ctrl Pts',(5.08242684526687,70.6042658562923,0.));
#101091=CARTESIAN_POINT('Ctrl Pts',(5.08242684526687,70.6042658562923,12.));
#101092=CARTESIAN_POINT('Ctrl Pts',(5.07758484512303,70.6252193187878,0.));
#101093=CARTESIAN_POINT('Ctrl Pts',(5.07758484512303,70.6252193187878,12.));
#101094=CARTESIAN_POINT('Ctrl Pts',(5.07271026703356,70.6462150640015,0.));
#101095=CARTESIAN_POINT('Ctrl Pts',(5.07271026703356,70.6462150640015,12.));
#101096=CARTESIAN_POINT('Ctrl Pts',(5.06780307224073,70.6672529237455,0.));
#101097=CARTESIAN_POINT('Ctrl Pts',(5.06780307224073,70.6672529237455,12.));
#101098=CARTESIAN_POINT('Ctrl Pts',(5.06286322227821,70.6883327305784,0.));
#101099=CARTESIAN_POINT('Ctrl Pts',(5.06286322227821,70.6883327305784,12.));
#101100=CARTESIAN_POINT('Ctrl Pts',(5.05789067897058,70.7094543178438,0.));
#101101=CARTESIAN_POINT('Ctrl Pts',(5.05789067897058,70.7094543178438,12.));
#101102=CARTESIAN_POINT('Ctrl Pts',(5.05288540443483,70.7306175196863,0.));
#101103=CARTESIAN_POINT('Ctrl Pts',(5.05288540443483,70.7306175196863,12.));
#101104=CARTESIAN_POINT('Ctrl Pts',(5.04784736108347,70.7518221710706,0.));
#101105=CARTESIAN_POINT('Ctrl Pts',(5.04784736108347,70.7518221710706,12.));
#101106=CARTESIAN_POINT('Ctrl Pts',(5.0427765116335,70.7730681077983,0.));
#101107=CARTESIAN_POINT('Ctrl Pts',(5.0427765116335,70.7730681077983,12.));
#101108=CARTESIAN_POINT('Ctrl Pts',(5.0376728191048,70.7943551665059,0.));
#101109=CARTESIAN_POINT('Ctrl Pts',(5.0376728191048,70.7943551665059,12.));
#101110=CARTESIAN_POINT('Ctrl Pts',(5.03253624680942,70.8156831846488,0.));
#101111=CARTESIAN_POINT('Ctrl Pts',(5.03253624680942,70.8156831846488,12.));
#101112=CARTESIAN_POINT('Ctrl Pts',(5.02736675834694,70.8370520004843,0.));
#101113=CARTESIAN_POINT('Ctrl Pts',(5.02736675834694,70.8370520004843,12.));
#101114=CARTESIAN_POINT('Ctrl Pts',(5.02216431760061,70.8584614530519,0.));
#101115=CARTESIAN_POINT('Ctrl Pts',(5.02216431760061,70.8584614530519,12.));
#101116=CARTESIAN_POINT('Ctrl Pts',(5.01692888873791,70.8799113821452,0.));
#101117=CARTESIAN_POINT('Ctrl Pts',(5.01692888873791,70.8799113821452,12.));
#101118=CARTESIAN_POINT('Ctrl Pts',(5.01166043620568,70.9014016283124,0.));
#101119=CARTESIAN_POINT('Ctrl Pts',(5.01166043620568,70.9014016283124,12.));
#101120=CARTESIAN_POINT('Ctrl Pts',(5.00635892472514,70.9229320328589,0.));
#101121=CARTESIAN_POINT('Ctrl Pts',(5.00635892472514,70.9229320328589,12.));
#101122=CARTESIAN_POINT('Ctrl Pts',(5.0010243192904,70.9445024378439,0.));
#101123=CARTESIAN_POINT('Ctrl Pts',(5.0010243192904,70.9445024378439,12.));
#101124=CARTESIAN_POINT('Ctrl Pts',(4.99565658516914,70.9661126860773,0.));
#101125=CARTESIAN_POINT('Ctrl Pts',(4.99565658516914,70.9661126860773,12.));
#101126=CARTESIAN_POINT('Ctrl Pts',(4.99025568790665,70.9877626211113,0.));
#101127=CARTESIAN_POINT('Ctrl Pts',(4.99025568790665,70.9877626211113,12.));
#101128=CARTESIAN_POINT('Ctrl Pts',(4.98482159331864,71.0094520872377,0.));
#101129=CARTESIAN_POINT('Ctrl Pts',(4.98482159331864,71.0094520872377,12.));
#101130=CARTESIAN_POINT('Ctrl Pts',(4.97935426748585,71.0311809294821,0.));
#101131=CARTESIAN_POINT('Ctrl Pts',(4.97935426748585,71.0311809294821,12.));
#101132=CARTESIAN_POINT('Ctrl Pts',(4.97385367675159,71.0529489935961,0.));
#101133=CARTESIAN_POINT('Ctrl Pts',(4.97385367675159,71.0529489935961,12.));
#101134=CARTESIAN_POINT('Ctrl Pts',(4.96831978772191,71.0747561260436,0.));
#101135=CARTESIAN_POINT('Ctrl Pts',(4.96831978772191,71.0747561260436,12.));
#101136=CARTESIAN_POINT('Ctrl Pts',(4.96275256726767,71.0966021739907,0.));
#101137=CARTESIAN_POINT('Ctrl Pts',(4.96275256726767,71.0966021739907,12.));
#101138=CARTESIAN_POINT('Ctrl Pts',(4.95715198251685,71.1184869853056,0.));
#101139=CARTESIAN_POINT('Ctrl Pts',(4.95715198251685,71.1184869853056,12.));
#101140=CARTESIAN_POINT('Ctrl Pts',(4.95151800085102,71.1404104085552,0.));
#101141=CARTESIAN_POINT('Ctrl Pts',(4.95151800085102,71.1404104085552,12.));
#101142=CARTESIAN_POINT('Ctrl Pts',(4.94585058990342,71.1623722930001,0.));
#101143=CARTESIAN_POINT('Ctrl Pts',(4.94585058990342,71.1623722930001,12.));
#101144=CARTESIAN_POINT('Ctrl Pts',(4.94014971756115,71.1843724885847,0.));
#101145=CARTESIAN_POINT('Ctrl Pts',(4.94014971756115,71.1843724885847,12.));
#101146=CARTESIAN_POINT('Ctrl Pts',(4.93441535196618,71.2064108459286,0.));
#101147=CARTESIAN_POINT('Ctrl Pts',(4.93441535196618,71.2064108459286,12.));
#101148=CARTESIAN_POINT('Ctrl Pts',(4.92864746150733,71.2284872163273,0.));
#101149=CARTESIAN_POINT('Ctrl Pts',(4.92864746150733,71.2284872163273,12.));
#101150=CARTESIAN_POINT('Ctrl Pts',(4.92284601481722,71.250601451747,0.));
#101151=CARTESIAN_POINT('Ctrl Pts',(4.92284601481722,71.250601451747,12.));
#101152=CARTESIAN_POINT('Ctrl Pts',(4.91701098077037,71.2727534048192,0.));
#101153=CARTESIAN_POINT('Ctrl Pts',(4.91701098077037,71.2727534048192,12.));
#101154=CARTESIAN_POINT('Ctrl Pts',(4.91114232848604,71.294942928829,0.));
#101155=CARTESIAN_POINT('Ctrl Pts',(4.91114232848604,71.294942928829,12.));
#101156=CARTESIAN_POINT('Ctrl Pts',(4.9052400273278,71.3171698777084,0.));
#101157=CARTESIAN_POINT('Ctrl Pts',(4.9052400273278,71.3171698777084,12.));
#101158=CARTESIAN_POINT('Ctrl Pts',(4.89930404689576,71.3394341060359,0.));
#101159=CARTESIAN_POINT('Ctrl Pts',(4.89930404689576,71.3394341060359,12.));
#101160=CARTESIAN_POINT('Ctrl Pts',(4.89333435702414,71.3617354690325,0.));
#101161=CARTESIAN_POINT('Ctrl Pts',(4.89333435702414,71.3617354690325,12.));
#101162=CARTESIAN_POINT('Ctrl Pts',(4.88733092777976,71.3840738225562,0.));
#101163=CARTESIAN_POINT('Ctrl Pts',(4.88733092777976,71.3840738225562,12.));
#101164=CARTESIAN_POINT('Ctrl Pts',(4.88129372946552,71.4064490230899,0.));
#101165=CARTESIAN_POINT('Ctrl Pts',(4.88129372946552,71.4064490230899,12.));
#101166=CARTESIAN_POINT('Ctrl Pts',(4.87522273261908,71.4288609277374,0.));
#101167=CARTESIAN_POINT('Ctrl Pts',(4.87522273261908,71.4288609277374,12.));
#101168=CARTESIAN_POINT('Ctrl Pts',(4.86911790800551,71.4513093942255,0.));
#101169=CARTESIAN_POINT('Ctrl Pts',(4.86911790800551,71.4513093942255,12.));
#101170=CARTESIAN_POINT('Ctrl Pts',(4.86297922661503,71.4737942808982,0.));
#101171=CARTESIAN_POINT('Ctrl Pts',(4.86297922661503,71.4737942808982,12.));
#101172=CARTESIAN_POINT('Ctrl Pts',(4.85680665966181,71.4963154467113,0.));
#101173=CARTESIAN_POINT('Ctrl Pts',(4.85680665966181,71.4963154467113,12.));
#101174=CARTESIAN_POINT('Ctrl Pts',(4.85060017858781,71.5188727512197,0.));
#101175=CARTESIAN_POINT('Ctrl Pts',(4.85060017858781,71.5188727512197,12.));
#101176=CARTESIAN_POINT('Ctrl Pts',(4.84435975506049,71.5414660545739,0.));
#101177=CARTESIAN_POINT('Ctrl Pts',(4.84435975506049,71.5414660545739,12.));
#101178=CARTESIAN_POINT('Ctrl Pts',(4.83808536096584,71.564095217521,0.));
#101179=CARTESIAN_POINT('Ctrl Pts',(4.83808536096584,71.564095217521,12.));
#101180=CARTESIAN_POINT('Ctrl Pts',(4.83177696840638,71.5867601014,0.));
#101181=CARTESIAN_POINT('Ctrl Pts',(4.83177696840638,71.5867601014,12.));
#101182=CARTESIAN_POINT('Ctrl Pts',(4.82543454970027,71.6094605681366,0.));
#101183=CARTESIAN_POINT('Ctrl Pts',(4.82543454970027,71.6094605681366,12.));
#101184=CARTESIAN_POINT('Ctrl Pts',(4.81905807738558,71.6321964802326,0.));
#101185=CARTESIAN_POINT('Ctrl Pts',(4.81905807738558,71.6321964802326,12.));
#101186=CARTESIAN_POINT('Ctrl Pts',(4.81264752421732,71.6549677007613,0.));
#101187=CARTESIAN_POINT('Ctrl Pts',(4.81264752421732,71.6549677007613,12.));
#101188=CARTESIAN_POINT('Ctrl Pts',(4.80620286316089,71.6777740933705,0.));
#101189=CARTESIAN_POINT('Ctrl Pts',(4.80620286316089,71.6777740933705,12.));
#101190=CARTESIAN_POINT('Ctrl Pts',(4.79972406739015,71.7006155222766,0.));
#101191=CARTESIAN_POINT('Ctrl Pts',(4.79972406739015,71.7006155222766,12.));
#101192=CARTESIAN_POINT('Ctrl Pts',(4.79321111028673,71.7234918522604,0.));
#101193=CARTESIAN_POINT('Ctrl Pts',(4.79321111028673,71.7234918522604,12.));
#101194=CARTESIAN_POINT('Ctrl Pts',(4.78666396544451,71.7464029486552,0.));
#101195=CARTESIAN_POINT('Ctrl Pts',(4.78666396544451,71.7464029486552,12.));
#101196=CARTESIAN_POINT('Ctrl Pts',(4.78008260666643,71.7693486773449,0.));
#101197=CARTESIAN_POINT('Ctrl Pts',(4.78008260666643,71.7693486773449,12.));
#101198=CARTESIAN_POINT('Ctrl Pts',(4.77346700795788,71.7923289047636,0.));
#101199=CARTESIAN_POINT('Ctrl Pts',(4.77346700795788,71.7923289047636,12.));
#101200=CARTESIAN_POINT('Ctrl Pts',(4.76681714352504,71.8153434978924,0.));
#101201=CARTESIAN_POINT('Ctrl Pts',(4.76681714352504,71.8153434978924,12.));
#101202=CARTESIAN_POINT('Ctrl Pts',(4.76013298777423,71.8383923242533,0.));
#101203=CARTESIAN_POINT('Ctrl Pts',(4.76013298777423,71.8383923242533,12.));
#101204=CARTESIAN_POINT('Ctrl Pts',(4.75341451531672,71.8614752519008,0.));
#101205=CARTESIAN_POINT('Ctrl Pts',(4.75341451531672,71.8614752519008,12.));
#101206=CARTESIAN_POINT('Ctrl Pts',(4.74666170096546,71.8845921494186,0.));
#101207=CARTESIAN_POINT('Ctrl Pts',(4.74666170096546,71.8845921494186,12.));
#101208=CARTESIAN_POINT('Ctrl Pts',(4.73987451972861,71.9077428859207,0.));
#101209=CARTESIAN_POINT('Ctrl Pts',(4.73987451972861,71.9077428859207,12.));
#101210=CARTESIAN_POINT('Ctrl Pts',(4.73305294680784,71.9309273310469,0.));
#101211=CARTESIAN_POINT('Ctrl Pts',(4.73305294680784,71.9309273310469,12.));
#101212=CARTESIAN_POINT('Ctrl Pts',(4.72619695759779,71.9541453549582,0.));
#101213=CARTESIAN_POINT('Ctrl Pts',(4.72619695759779,71.9541453549582,12.));
#101214=CARTESIAN_POINT('Ctrl Pts',(4.71930652769081,71.9773968283267,0.));
#101215=CARTESIAN_POINT('Ctrl Pts',(4.71930652769081,71.9773968283267,12.));
#101216=CARTESIAN_POINT('Ctrl Pts',(4.71238163287411,72.0006816223335,0.));
#101217=CARTESIAN_POINT('Ctrl Pts',(4.71238163287411,72.0006816223335,12.));
#101218=CARTESIAN_POINT('Ctrl Pts',(4.70542224912313,72.0239996086694,0.));
#101219=CARTESIAN_POINT('Ctrl Pts',(4.70542224912313,72.0239996086694,12.));
#101220=CARTESIAN_POINT('Ctrl Pts',(4.69842835259998,72.047350659532,0.));
#101221=CARTESIAN_POINT('Ctrl Pts',(4.69842835259998,72.047350659532,12.));
#101222=CARTESIAN_POINT('Ctrl Pts',(4.69139991965281,72.070734647621,0.));
#101223=CARTESIAN_POINT('Ctrl Pts',(4.69139991965281,72.070734647621,12.));
#101224=CARTESIAN_POINT('Ctrl Pts',(4.68433692682061,72.0941514461283,0.));
#101225=CARTESIAN_POINT('Ctrl Pts',(4.68433692682061,72.0941514461283,12.));
#101226=CARTESIAN_POINT('Ctrl Pts',(4.67723935083088,72.1176009287349,0.));
#101227=CARTESIAN_POINT('Ctrl Pts',(4.67723935083088,72.1176009287349,12.));
#101228=CARTESIAN_POINT('Ctrl Pts',(4.67010716859282,72.1410829696129,0.));
#101229=CARTESIAN_POINT('Ctrl Pts',(4.67010716859282,72.1410829696129,12.));
#101230=CARTESIAN_POINT('Ctrl Pts',(4.66294035719571,72.1645974434218,0.));
#101231=CARTESIAN_POINT('Ctrl Pts',(4.66294035719571,72.1645974434218,12.));
#101232=CARTESIAN_POINT('Ctrl Pts',(4.65573889390825,72.1881442253052,0.));
#101233=CARTESIAN_POINT('Ctrl Pts',(4.65573889390825,72.1881442253052,12.));
#101234=CARTESIAN_POINT('Ctrl Pts',(4.64850275618326,72.2117231908816,0.));
#101235=CARTESIAN_POINT('Ctrl Pts',(4.64850275618326,72.2117231908816,12.));
#101236=CARTESIAN_POINT('Ctrl Pts',(4.64123192165628,72.2353342162408,0.));
#101237=CARTESIAN_POINT('Ctrl Pts',(4.64123192165628,72.2353342162408,12.));
#101238=CARTESIAN_POINT('Ctrl Pts',(4.63392636813843,72.2589771779447,0.));
#101239=CARTESIAN_POINT('Ctrl Pts',(4.63392636813843,72.2589771779447,12.));
#101240=CARTESIAN_POINT('Ctrl Pts',(4.62658607361466,72.2826519530254,0.));
#101241=CARTESIAN_POINT('Ctrl Pts',(4.62658607361466,72.2826519530254,12.));
#101242=CARTESIAN_POINT('Ctrl Pts',(4.61921101624295,72.306358418981,0.));
#101243=CARTESIAN_POINT('Ctrl Pts',(4.61921101624295,72.306358418981,12.));
#101244=CARTESIAN_POINT('Ctrl Pts',(4.61180117435869,72.330096453767,0.));
#101245=CARTESIAN_POINT('Ctrl Pts',(4.61180117435869,72.330096453767,12.));
#101246=CARTESIAN_POINT('Ctrl Pts',(4.60435652647464,72.3538659357932,0.));
#101247=CARTESIAN_POINT('Ctrl Pts',(4.60435652647464,72.3538659357932,12.));
#101248=CARTESIAN_POINT('Ctrl Pts',(4.59687705127341,72.3776667439244,0.));
#101249=CARTESIAN_POINT('Ctrl Pts',(4.59687705127341,72.3776667439244,12.));
#101250=CARTESIAN_POINT('Ctrl Pts',(4.58936272760551,72.4014987574789,0.));
#101251=CARTESIAN_POINT('Ctrl Pts',(4.58936272760551,72.4014987574789,12.));
#101252=CARTESIAN_POINT('Ctrl Pts',(4.58181353448852,72.4253618562249,0.));
#101253=CARTESIAN_POINT('Ctrl Pts',(4.58181353448852,72.4253618562249,12.));
#101254=CARTESIAN_POINT('Ctrl Pts',(4.57422945111095,72.449255920373,0.));
#101255=CARTESIAN_POINT('Ctrl Pts',(4.57422945111095,72.449255920373,12.));
#101256=CARTESIAN_POINT('Ctrl Pts',(4.56661045683367,72.473180830571,0.));
#101257=CARTESIAN_POINT('Ctrl Pts',(4.56661045683367,72.473180830571,12.));
#101258=CARTESIAN_POINT('Ctrl Pts',(4.55895653118214,72.4971364679055,0.));
#101259=CARTESIAN_POINT('Ctrl Pts',(4.55895653118214,72.4971364679055,12.));
#101260=CARTESIAN_POINT('Ctrl Pts',(4.55126765384403,72.5211227138997,0.));
#101261=CARTESIAN_POINT('Ctrl Pts',(4.55126765384403,72.5211227138997,12.));
#101262=CARTESIAN_POINT('Ctrl Pts',(4.54354380466826,72.5451394505106,0.));
#101263=CARTESIAN_POINT('Ctrl Pts',(4.54354380466826,72.5451394505106,12.));
#101264=CARTESIAN_POINT('Ctrl Pts',(4.53578496366802,72.5691865601225,0.));
#101265=CARTESIAN_POINT('Ctrl Pts',(4.53578496366802,72.5691865601225,12.));
#101266=CARTESIAN_POINT('Ctrl Pts',(4.52799111102391,72.5932639255406,0.));
#101267=CARTESIAN_POINT('Ctrl Pts',(4.52799111102391,72.5932639255406,12.));
#101268=CARTESIAN_POINT('Ctrl Pts',(4.52016222707633,72.6173714299935,0.));
#101269=CARTESIAN_POINT('Ctrl Pts',(4.52016222707633,72.6173714299935,12.));
#101270=CARTESIAN_POINT('Ctrl Pts',(4.5122982923226,72.6415089571314,0.));
#101271=CARTESIAN_POINT('Ctrl Pts',(4.5122982923226,72.6415089571314,12.));
#101272=CARTESIAN_POINT('Ctrl Pts',(4.50439928741605,72.6656763910241,0.));
#101273=CARTESIAN_POINT('Ctrl Pts',(4.50439928741605,72.6656763910241,12.));
#101274=CARTESIAN_POINT('Ctrl Pts',(4.49646519316822,72.689873616155,0.));
#101275=CARTESIAN_POINT('Ctrl Pts',(4.49646519316822,72.689873616155,12.));
#101276=CARTESIAN_POINT('Ctrl Pts',(4.48849599055354,72.7141005174153,0.));
#101277=CARTESIAN_POINT('Ctrl Pts',(4.48849599055354,72.7141005174153,12.));
#101278=CARTESIAN_POINT('Ctrl Pts',(4.48049166070224,72.7383569801042,0.));
#101279=CARTESIAN_POINT('Ctrl Pts',(4.48049166070224,72.7383569801042,12.));
#101280=CARTESIAN_POINT('Ctrl Pts',(4.47245218489623,72.7626428899287,0.));
#101281=CARTESIAN_POINT('Ctrl Pts',(4.47245218489623,72.7626428899287,12.));
#101282=CARTESIAN_POINT('Ctrl Pts',(4.46437754456796,72.7869581329994,0.));
#101283=CARTESIAN_POINT('Ctrl Pts',(4.46437754456796,72.7869581329994,12.));
#101284=CARTESIAN_POINT('Ctrl Pts',(4.45626772130139,72.8113025958258,0.));
#101285=CARTESIAN_POINT('Ctrl Pts',(4.45626772130139,72.8113025958258,12.));
#101286=CARTESIAN_POINT('Ctrl Pts',(4.44812269683725,72.8356761653064,0.));
#101287=CARTESIAN_POINT('Ctrl Pts',(4.44812269683725,72.8356761653064,12.));
#101288=CARTESIAN_POINT('Ctrl Pts',(4.43994245306805,72.8600787287316,0.));
#101289=CARTESIAN_POINT('Ctrl Pts',(4.43994245306805,72.8600787287316,12.));
#101290=CARTESIAN_POINT('Ctrl Pts',(4.43172697203342,72.8845101737856,0.));
#101291=CARTESIAN_POINT('Ctrl Pts',(4.43172697203342,72.8845101737856,12.));
#101292=CARTESIAN_POINT('Ctrl Pts',(4.42347623591942,72.9089703885464,0.));
#101293=CARTESIAN_POINT('Ctrl Pts',(4.42347623591942,72.9089703885464,12.));
#101294=CARTESIAN_POINT('Ctrl Pts',(4.41519022705927,72.9334592614828,0.));
#101295=CARTESIAN_POINT('Ctrl Pts',(4.41519022705927,72.9334592614828,12.));
#101296=CARTESIAN_POINT('Ctrl Pts',(4.40686892793966,72.9579766814495,0.));
#101297=CARTESIAN_POINT('Ctrl Pts',(4.40686892793966,72.9579766814495,12.));
#101298=CARTESIAN_POINT('Ctrl Pts',(4.39851232119731,72.9825225376839,0.));
#101299=CARTESIAN_POINT('Ctrl Pts',(4.39851232119731,72.9825225376839,12.));
#101300=CARTESIAN_POINT('Ctrl Pts',(4.39012038961145,73.0070967198033,0.));
#101301=CARTESIAN_POINT('Ctrl Pts',(4.39012038961145,73.0070967198033,12.));
#101302=CARTESIAN_POINT('Ctrl Pts',(4.38169311610154,73.031699117799,0.));
#101303=CARTESIAN_POINT('Ctrl Pts',(4.38169311610154,73.031699117799,12.));
#101304=CARTESIAN_POINT('Ctrl Pts',(4.37323048372607,73.0563296220301,0.));
#101305=CARTESIAN_POINT('Ctrl Pts',(4.37323048372607,73.0563296220301,12.));
#101306=CARTESIAN_POINT('Ctrl Pts',(4.36473247568639,73.0809881232111,0.));
#101307=CARTESIAN_POINT('Ctrl Pts',(4.36473247568639,73.0809881232111,12.));
#101308=CARTESIAN_POINT('Ctrl Pts',(4.35619907532716,73.1056745124099,0.));
#101309=CARTESIAN_POINT('Ctrl Pts',(4.35619907532716,73.1056745124099,12.));
#101310=CARTESIAN_POINT('Ctrl Pts',(4.34763026613155,73.1303886810602,0.));
#101311=CARTESIAN_POINT('Ctrl Pts',(4.34763026613155,73.1303886810602,12.));
#101312=CARTESIAN_POINT('Ctrl Pts',(4.3390260317214,73.1551305209692,0.));
#101313=CARTESIAN_POINT('Ctrl Pts',(4.3390260317214,73.1551305209692,12.));
#101314=CARTESIAN_POINT('Ctrl Pts',(4.33038635585878,73.1798999243234,0.));
#101315=CARTESIAN_POINT('Ctrl Pts',(4.33038635585878,73.1798999243234,12.));
#101316=CARTESIAN_POINT('Ctrl Pts',(4.32171122245219,73.204696783693,0.));
#101317=CARTESIAN_POINT('Ctrl Pts',(4.32171122245219,73.204696783693,12.));
#101318=CARTESIAN_POINT('Ctrl Pts',(4.31300061556103,73.2295209920319,0.));
#101319=CARTESIAN_POINT('Ctrl Pts',(4.31300061556103,73.2295209920319,12.));
#101320=CARTESIAN_POINT('Ctrl Pts',(4.30425451938235,73.2543724426562,0.));
#101321=CARTESIAN_POINT('Ctrl Pts',(4.30425451938235,73.2543724426562,12.));
#101322=CARTESIAN_POINT('Ctrl Pts',(4.29547291824289,73.2792510292243,0.));
#101323=CARTESIAN_POINT('Ctrl Pts',(4.29547291824289,73.2792510292243,12.));
#101324=CARTESIAN_POINT('Ctrl Pts',(4.28665579659303,73.3041566457134,0.));
#101325=CARTESIAN_POINT('Ctrl Pts',(4.28665579659303,73.3041566457134,12.));
#101326=CARTESIAN_POINT('Ctrl Pts',(4.27780313900392,73.3290891863959,0.));
#101327=CARTESIAN_POINT('Ctrl Pts',(4.27780313900392,73.3290891863959,12.));
#101328=CARTESIAN_POINT('Ctrl Pts',(4.26891493016704,73.354048545808,0.));
#101329=CARTESIAN_POINT('Ctrl Pts',(4.26891493016704,73.354048545808,12.));
#101330=CARTESIAN_POINT('Ctrl Pts',(4.25999115489905,73.3790346187953,0.));
#101331=CARTESIAN_POINT('Ctrl Pts',(4.25999115489905,73.3790346187953,12.));
#101332=CARTESIAN_POINT('Ctrl Pts',(4.25103179814892,73.4040473005603,0.));
#101333=CARTESIAN_POINT('Ctrl Pts',(4.25103179814892,73.4040473005603,12.));
#101334=CARTESIAN_POINT('Ctrl Pts',(4.24203684500942,73.4290864867103,0.));
#101335=CARTESIAN_POINT('Ctrl Pts',(4.24203684500942,73.4290864867103,12.));
#101336=CARTESIAN_POINT('Ctrl Pts',(4.23300628072758,73.4541520732943,0.));
#101337=CARTESIAN_POINT('Ctrl Pts',(4.23300628072758,73.4541520732943,12.));
#101338=CARTESIAN_POINT('Ctrl Pts',(4.22394009072754,73.4792439568624,0.));
#101339=CARTESIAN_POINT('Ctrl Pts',(4.22394009072754,73.4792439568624,12.));
#101340=CARTESIAN_POINT('Ctrl Pts',(4.21483826059437,73.5043620344107,0.));
#101341=CARTESIAN_POINT('Ctrl Pts',(4.21483826059437,73.5043620344107,12.));
#101342=CARTESIAN_POINT('Ctrl Pts',(4.20570077603728,73.5295062032621,0.));
#101343=CARTESIAN_POINT('Ctrl Pts',(4.20570077603728,73.5295062032621,12.));
#101344=CARTESIAN_POINT('Ctrl Pts',(4.19652762286127,73.554676360957,0.));
#101345=CARTESIAN_POINT('Ctrl Pts',(4.19652762286127,73.554676360957,12.));
#101346=CARTESIAN_POINT('Ctrl Pts',(4.18731878694239,73.5798724051519,0.));
#101347=CARTESIAN_POINT('Ctrl Pts',(4.18731878694239,73.5798724051519,12.));
#101348=CARTESIAN_POINT('Ctrl Pts',(4.17807425419817,73.6050942334773,0.));
#101349=CARTESIAN_POINT('Ctrl Pts',(4.17807425419817,73.6050942334773,12.));
#101350=CARTESIAN_POINT('Ctrl Pts',(4.16879401058787,73.6303417435262,0.));
#101351=CARTESIAN_POINT('Ctrl Pts',(4.16879401058787,73.6303417435262,12.));
#101352=CARTESIAN_POINT('Ctrl Pts',(4.15947804217791,73.6556148331504,0.));
#101353=CARTESIAN_POINT('Ctrl Pts',(4.15947804217791,73.6556148331504,12.));
#101354=CARTESIAN_POINT('Ctrl Pts',(4.15012633519729,73.6809134006909,0.));
#101355=CARTESIAN_POINT('Ctrl Pts',(4.15012633519729,73.6809134006909,12.));
#101356=CARTESIAN_POINT('Ctrl Pts',(4.14073887610155,73.7062373452344,0.));
#101357=CARTESIAN_POINT('Ctrl Pts',(4.14073887610155,73.7062373452344,12.));
#101358=CARTESIAN_POINT('Ctrl Pts',(4.13131565163575,73.7315865668508,0.));
#101359=CARTESIAN_POINT('Ctrl Pts',(4.13131565163575,73.7315865668508,12.));
#101360=CARTESIAN_POINT('Ctrl Pts',(4.12185664890552,73.7569609668501,0.));
#101361=CARTESIAN_POINT('Ctrl Pts',(4.12185664890552,73.7569609668501,12.));
#101362=CARTESIAN_POINT('Ctrl Pts',(4.11236185522781,73.7823604472126,0.));
#101363=CARTESIAN_POINT('Ctrl Pts',(4.11236185522781,73.7823604472126,12.));
#101364=CARTESIAN_POINT('Ctrl Pts',(4.10283125798725,73.8077849100314,0.));
#101365=CARTESIAN_POINT('Ctrl Pts',(4.10283125798725,73.8077849100314,12.));
#101366=CARTESIAN_POINT('Ctrl Pts',(4.09326484448232,73.8332342568978,0.));
#101367=CARTESIAN_POINT('Ctrl Pts',(4.09326484448232,73.8332342568978,12.));
#101368=CARTESIAN_POINT('Ctrl Pts',(4.0836626018068,73.8587083884208,0.));
#101369=CARTESIAN_POINT('Ctrl Pts',(4.0836626018068,73.8587083884208,12.));
#101370=CARTESIAN_POINT('Ctrl Pts',(4.07402451665254,73.884207203405,0.));
#101371=CARTESIAN_POINT('Ctrl Pts',(4.07402451665254,73.884207203405,12.));
#101372=CARTESIAN_POINT('Ctrl Pts',(4.06435057547335,73.9097305995173,0.));
#101373=CARTESIAN_POINT('Ctrl Pts',(4.06435057547335,73.9097305995173,12.));
#101374=CARTESIAN_POINT('Ctrl Pts',(4.05464076484762,73.9352784747665,0.));
#101375=CARTESIAN_POINT('Ctrl Pts',(4.05464076484762,73.9352784747665,12.));
#101376=CARTESIAN_POINT('Ctrl Pts',(4.04489507179964,73.9608507287943,0.));
#101377=CARTESIAN_POINT('Ctrl Pts',(4.04489507179964,73.9608507287943,12.));
#101378=CARTESIAN_POINT('Ctrl Pts',(4.03511348410661,73.9864472641025,0.));
#101379=CARTESIAN_POINT('Ctrl Pts',(4.03511348410661,73.9864472641025,12.));
#101380=CARTESIAN_POINT('Ctrl Pts',(4.02529599070086,74.0120679876396,0.));
#101381=CARTESIAN_POINT('Ctrl Pts',(4.02529599070086,74.0120679876396,12.));
#101382=CARTESIAN_POINT('Ctrl Pts',(4.01544258176694,74.0377128111754,0.));
#101383=CARTESIAN_POINT('Ctrl Pts',(4.01544258176694,74.0377128111754,12.));
#101384=CARTESIAN_POINT('Ctrl Pts',(4.0055532478546,74.0633816477912,0.));
#101385=CARTESIAN_POINT('Ctrl Pts',(4.0055532478546,74.0633816477912,12.));
#101386=CARTESIAN_POINT('Ctrl Pts',(3.99562797918272,74.0890744091088,0.));
#101387=CARTESIAN_POINT('Ctrl Pts',(3.99562797918272,74.0890744091088,12.));
#101388=CARTESIAN_POINT('Ctrl Pts',(3.98566676483639,74.1147910020869,0.));
#101389=CARTESIAN_POINT('Ctrl Pts',(3.98566676483639,74.1147910020869,12.));
#101390=CARTESIAN_POINT('Ctrl Pts',(3.97566959209547,74.1405313263198,0.));
#101391=CARTESIAN_POINT('Ctrl Pts',(3.97566959209547,74.1405313263198,12.));
#101392=CARTESIAN_POINT('Ctrl Pts',(3.96563644549423,74.1662952702689,0.));
#101393=CARTESIAN_POINT('Ctrl Pts',(3.96563644549423,74.1662952702689,12.));
#101394=CARTESIAN_POINT('Ctrl Pts',(3.95556730821161,74.1920827166861,0.));
#101395=CARTESIAN_POINT('Ctrl Pts',(3.95556730821161,74.1920827166861,12.));
#101396=CARTESIAN_POINT('Ctrl Pts',(3.94546216377499,74.217893549314,0.));
#101397=CARTESIAN_POINT('Ctrl Pts',(3.94546216377499,74.217893549314,12.));
#101398=CARTESIAN_POINT('Ctrl Pts',(3.9353209977423,74.2437276593763,0.));
#101399=CARTESIAN_POINT('Ctrl Pts',(3.9353209977423,74.2437276593763,12.));
#101400=CARTESIAN_POINT('Ctrl Pts',(3.92514379920729,74.2695849516134,0.));
#101401=CARTESIAN_POINT('Ctrl Pts',(3.92514379920729,74.2695849516134,12.));
#101402=CARTESIAN_POINT('Ctrl Pts',(3.91493056284965,74.2954653518346,0.));
#101403=CARTESIAN_POINT('Ctrl Pts',(3.91493056284965,74.2954653518346,12.));
#101404=CARTESIAN_POINT('Ctrl Pts',(3.90468128904521,74.3213688089495,0.));
#101405=CARTESIAN_POINT('Ctrl Pts',(3.90468128904521,74.3213688089495,12.));
#101406=CARTESIAN_POINT('Ctrl Pts',(3.89439598145194,74.3472952898,0.));
#101407=CARTESIAN_POINT('Ctrl Pts',(3.89439598145194,74.3472952898,12.));
#101408=CARTESIAN_POINT('Ctrl Pts',(3.8861389124787,74.3680548786039,0.));
#101409=CARTESIAN_POINT('Ctrl Pts',(3.8861389124787,74.3680548786039,12.));
#101410=CARTESIAN_POINT('Ctrl Pts',(3.87992989995679,74.3836349188809,0.));
#101411=CARTESIAN_POINT('Ctrl Pts',(3.87992989995679,74.3836349188809,12.));
#101412=CARTESIAN_POINT('Ctrl Pts',(3.87578335377302,74.3940262116251,0.));
#101413=CARTESIAN_POINT('Ctrl Pts',(3.87578335377302,74.3940262116251,12.));
#101414=CARTESIAN_POINT('Ctrl Pts',(3.87370827955545,74.3992230078037,0.));
#101415=CARTESIAN_POINT('Ctrl Pts',(3.87370827955545,74.3992230078037,12.));
#101416=CARTESIAN_POINT('',(5.24987136994593,69.8028570375097,0.));
#101417=CARTESIAN_POINT('Ctrl Pts',(5.24987136994593,69.8028570375097,0.));
#101418=CARTESIAN_POINT('Ctrl Pts',(5.24915955997427,69.8066748687772,0.));
#101419=CARTESIAN_POINT('Ctrl Pts',(5.24773285666377,69.8143154684204,0.));
#101420=CARTESIAN_POINT('Ctrl Pts',(5.24558355159751,69.8257911792159,0.));
#101421=CARTESIAN_POINT('Ctrl Pts',(5.2426993105457,69.841121750752,0.));
#101422=CARTESIAN_POINT('Ctrl Pts',(5.23906316634803,69.8603343302743,0.));
#101423=CARTESIAN_POINT('Ctrl Pts',(5.23539616279621,69.8795962381599,0.));
#101424=CARTESIAN_POINT('Ctrl Pts',(5.23169827290556,69.8989073936688,0.));
#101425=CARTESIAN_POINT('Ctrl Pts',(5.22796945602795,69.9182676502048,0.));
#101426=CARTESIAN_POINT('Ctrl Pts',(5.22420965879982,69.9376767969095,0.));
#101427=CARTESIAN_POINT('Ctrl Pts',(5.22041882075722,69.9571345870076,0.));
#101428=CARTESIAN_POINT('Ctrl Pts',(5.2165968788114,69.9766407595385,0.));
#101429=CARTESIAN_POINT('Ctrl Pts',(5.2127437720326,69.9961950629965,0.));
#101430=CARTESIAN_POINT('Ctrl Pts',(5.20885944672837,70.0157972802182,0.));
#101431=CARTESIAN_POINT('Ctrl Pts',(5.20494385478026,70.0354472203546,0.));
#101432=CARTESIAN_POINT('Ctrl Pts',(5.20099695122657,70.0551447071082,0.));
#101433=CARTESIAN_POINT('Ctrl Pts',(5.19701869225529,70.0748895689729,0.));
#101434=CARTESIAN_POINT('Ctrl Pts',(5.19300903271581,70.0946816270997,0.));
#101435=CARTESIAN_POINT('Ctrl Pts',(5.18896792486566,70.1145206891885,0.));
#101436=CARTESIAN_POINT('Ctrl Pts',(5.18489531966266,70.1344065558145,0.));
#101437=CARTESIAN_POINT('Ctrl Pts',(5.18079116757667,70.1543390243892,0.));
#101438=CARTESIAN_POINT('Ctrl Pts',(5.17665541952384,70.1743178937077,0.));
#101439=CARTESIAN_POINT('Ctrl Pts',(5.1724880279339,70.1943429691167,0.));
#101440=CARTESIAN_POINT('Ctrl Pts',(5.16828894670109,70.2144140622953,0.));
#101441=CARTESIAN_POINT('Ctrl Pts',(5.16405813066977,70.2345309887833,0.));
#101442=CARTESIAN_POINT('Ctrl Pts',(5.15979553528204,70.2546935662722,0.));
#101443=CARTESIAN_POINT('Ctrl Pts',(5.1555011161486,70.2749016125105,0.));
#101444=CARTESIAN_POINT('Ctrl Pts',(5.15117482869255,70.2951549435512,0.));
#101445=CARTESIAN_POINT('Ctrl Pts',(5.14681662833081,70.3154533746736,0.));
#101446=CARTESIAN_POINT('Ctrl Pts',(5.1424264706348,70.3357967211796,0.));
#101447=CARTESIAN_POINT('Ctrl Pts',(5.13800431148904,70.3561847991714,0.));
#101448=CARTESIAN_POINT('Ctrl Pts',(5.13355010728568,70.3766174264757,0.));
#101449=CARTESIAN_POINT('Ctrl Pts',(5.12906381499457,70.3970944229851,0.));
#101450=CARTESIAN_POINT('Ctrl Pts',(5.12454539205329,70.417615610161,0.));
#101451=CARTESIAN_POINT('Ctrl Pts',(5.11999479630212,70.4381808107245,0.));
#101452=CARTESIAN_POINT('Ctrl Pts',(5.11541198590933,70.458789848296,0.));
#101453=CARTESIAN_POINT('Ctrl Pts',(5.11079691929214,70.4794425469825,0.));
#101454=CARTESIAN_POINT('Ctrl Pts',(5.10614955511665,70.500138731399,0.));
#101455=CARTESIAN_POINT('Ctrl Pts',(5.10146985232942,70.5208782268497,0.));
#101456=CARTESIAN_POINT('Ctrl Pts',(5.09675777018184,70.5416608594526,0.));
#101457=CARTESIAN_POINT('Ctrl Pts',(5.09201326826135,70.5624864562824,0.));
#101458=CARTESIAN_POINT('Ctrl Pts',(5.08723630652274,70.5833548455014,0.));
#101459=CARTESIAN_POINT('Ctrl Pts',(5.08242684526687,70.6042658562923,0.));
#101460=CARTESIAN_POINT('Ctrl Pts',(5.07758484512303,70.6252193187878,0.));
#101461=CARTESIAN_POINT('Ctrl Pts',(5.07271026703356,70.6462150640015,0.));
#101462=CARTESIAN_POINT('Ctrl Pts',(5.06780307224073,70.6672529237455,0.));
#101463=CARTESIAN_POINT('Ctrl Pts',(5.06286322227821,70.6883327305784,0.));
#101464=CARTESIAN_POINT('Ctrl Pts',(5.05789067897058,70.7094543178438,0.));
#101465=CARTESIAN_POINT('Ctrl Pts',(5.05288540443483,70.7306175196863,0.));
#101466=CARTESIAN_POINT('Ctrl Pts',(5.04784736108347,70.7518221710706,0.));
#101467=CARTESIAN_POINT('Ctrl Pts',(5.0427765116335,70.7730681077983,0.));
#101468=CARTESIAN_POINT('Ctrl Pts',(5.0376728191048,70.7943551665059,0.));
#101469=CARTESIAN_POINT('Ctrl Pts',(5.03253624680942,70.8156831846488,0.));
#101470=CARTESIAN_POINT('Ctrl Pts',(5.02736675834694,70.8370520004843,0.));
#101471=CARTESIAN_POINT('Ctrl Pts',(5.02216431760061,70.8584614530519,0.));
#101472=CARTESIAN_POINT('Ctrl Pts',(5.01692888873791,70.8799113821452,0.));
#101473=CARTESIAN_POINT('Ctrl Pts',(5.01166043620568,70.9014016283124,0.));
#101474=CARTESIAN_POINT('Ctrl Pts',(5.00635892472514,70.9229320328589,0.));
#101475=CARTESIAN_POINT('Ctrl Pts',(5.0010243192904,70.9445024378439,0.));
#101476=CARTESIAN_POINT('Ctrl Pts',(4.99565658516914,70.9661126860773,0.));
#101477=CARTESIAN_POINT('Ctrl Pts',(4.99025568790665,70.9877626211113,0.));
#101478=CARTESIAN_POINT('Ctrl Pts',(4.98482159331864,71.0094520872377,0.));
#101479=CARTESIAN_POINT('Ctrl Pts',(4.97935426748585,71.0311809294821,0.));
#101480=CARTESIAN_POINT('Ctrl Pts',(4.97385367675159,71.0529489935961,0.));
#101481=CARTESIAN_POINT('Ctrl Pts',(4.96831978772191,71.0747561260436,0.));
#101482=CARTESIAN_POINT('Ctrl Pts',(4.96275256726767,71.0966021739907,0.));
#101483=CARTESIAN_POINT('Ctrl Pts',(4.95715198251685,71.1184869853056,0.));
#101484=CARTESIAN_POINT('Ctrl Pts',(4.95151800085102,71.1404104085552,0.));
#101485=CARTESIAN_POINT('Ctrl Pts',(4.94585058990342,71.1623722930001,0.));
#101486=CARTESIAN_POINT('Ctrl Pts',(4.94014971756115,71.1843724885847,0.));
#101487=CARTESIAN_POINT('Ctrl Pts',(4.93441535196618,71.2064108459286,0.));
#101488=CARTESIAN_POINT('Ctrl Pts',(4.92864746150733,71.2284872163273,0.));
#101489=CARTESIAN_POINT('Ctrl Pts',(4.92284601481722,71.250601451747,0.));
#101490=CARTESIAN_POINT('Ctrl Pts',(4.91701098077037,71.2727534048192,0.));
#101491=CARTESIAN_POINT('Ctrl Pts',(4.91114232848604,71.294942928829,0.));
#101492=CARTESIAN_POINT('Ctrl Pts',(4.9052400273278,71.3171698777084,0.));
#101493=CARTESIAN_POINT('Ctrl Pts',(4.89930404689576,71.3394341060359,0.));
#101494=CARTESIAN_POINT('Ctrl Pts',(4.89333435702414,71.3617354690325,0.));
#101495=CARTESIAN_POINT('Ctrl Pts',(4.88733092777976,71.3840738225562,0.));
#101496=CARTESIAN_POINT('Ctrl Pts',(4.88129372946552,71.4064490230899,0.));
#101497=CARTESIAN_POINT('Ctrl Pts',(4.87522273261908,71.4288609277374,0.));
#101498=CARTESIAN_POINT('Ctrl Pts',(4.86911790800551,71.4513093942255,0.));
#101499=CARTESIAN_POINT('Ctrl Pts',(4.86297922661503,71.4737942808982,0.));
#101500=CARTESIAN_POINT('Ctrl Pts',(4.85680665966181,71.4963154467113,0.));
#101501=CARTESIAN_POINT('Ctrl Pts',(4.85060017858781,71.5188727512197,0.));
#101502=CARTESIAN_POINT('Ctrl Pts',(4.84435975506049,71.5414660545739,0.));
#101503=CARTESIAN_POINT('Ctrl Pts',(4.83808536096584,71.564095217521,0.));
#101504=CARTESIAN_POINT('Ctrl Pts',(4.83177696840638,71.5867601014,0.));
#101505=CARTESIAN_POINT('Ctrl Pts',(4.82543454970027,71.6094605681366,0.));
#101506=CARTESIAN_POINT('Ctrl Pts',(4.81905807738558,71.6321964802326,0.));
#101507=CARTESIAN_POINT('Ctrl Pts',(4.81264752421732,71.6549677007613,0.));
#101508=CARTESIAN_POINT('Ctrl Pts',(4.80620286316089,71.6777740933705,0.));
#101509=CARTESIAN_POINT('Ctrl Pts',(4.79972406739015,71.7006155222766,0.));
#101510=CARTESIAN_POINT('Ctrl Pts',(4.79321111028673,71.7234918522604,0.));
#101511=CARTESIAN_POINT('Ctrl Pts',(4.78666396544451,71.7464029486552,0.));
#101512=CARTESIAN_POINT('Ctrl Pts',(4.78008260666643,71.7693486773449,0.));
#101513=CARTESIAN_POINT('Ctrl Pts',(4.77346700795788,71.7923289047636,0.));
#101514=CARTESIAN_POINT('Ctrl Pts',(4.76681714352504,71.8153434978924,0.));
#101515=CARTESIAN_POINT('Ctrl Pts',(4.76013298777423,71.8383923242533,0.));
#101516=CARTESIAN_POINT('Ctrl Pts',(4.75341451531672,71.8614752519008,0.));
#101517=CARTESIAN_POINT('Ctrl Pts',(4.74666170096546,71.8845921494186,0.));
#101518=CARTESIAN_POINT('Ctrl Pts',(4.73987451972861,71.9077428859207,0.));
#101519=CARTESIAN_POINT('Ctrl Pts',(4.73305294680784,71.9309273310469,0.));
#101520=CARTESIAN_POINT('Ctrl Pts',(4.72619695759779,71.9541453549582,0.));
#101521=CARTESIAN_POINT('Ctrl Pts',(4.71930652769081,71.9773968283267,0.));
#101522=CARTESIAN_POINT('Ctrl Pts',(4.71238163287411,72.0006816223335,0.));
#101523=CARTESIAN_POINT('Ctrl Pts',(4.70542224912313,72.0239996086694,0.));
#101524=CARTESIAN_POINT('Ctrl Pts',(4.69842835259998,72.047350659532,0.));
#101525=CARTESIAN_POINT('Ctrl Pts',(4.69139991965281,72.070734647621,0.));
#101526=CARTESIAN_POINT('Ctrl Pts',(4.68433692682061,72.0941514461283,0.));
#101527=CARTESIAN_POINT('Ctrl Pts',(4.67723935083088,72.1176009287349,0.));
#101528=CARTESIAN_POINT('Ctrl Pts',(4.67010716859282,72.1410829696129,0.));
#101529=CARTESIAN_POINT('Ctrl Pts',(4.66294035719571,72.1645974434218,0.));
#101530=CARTESIAN_POINT('Ctrl Pts',(4.65573889390825,72.1881442253052,0.));
#101531=CARTESIAN_POINT('Ctrl Pts',(4.64850275618326,72.2117231908816,0.));
#101532=CARTESIAN_POINT('Ctrl Pts',(4.64123192165628,72.2353342162408,0.));
#101533=CARTESIAN_POINT('Ctrl Pts',(4.63392636813843,72.2589771779447,0.));
#101534=CARTESIAN_POINT('Ctrl Pts',(4.62658607361466,72.2826519530254,0.));
#101535=CARTESIAN_POINT('Ctrl Pts',(4.61921101624295,72.306358418981,0.));
#101536=CARTESIAN_POINT('Ctrl Pts',(4.61180117435869,72.330096453767,0.));
#101537=CARTESIAN_POINT('Ctrl Pts',(4.60435652647464,72.3538659357932,0.));
#101538=CARTESIAN_POINT('Ctrl Pts',(4.59687705127341,72.3776667439244,0.));
#101539=CARTESIAN_POINT('Ctrl Pts',(4.58936272760551,72.4014987574789,0.));
#101540=CARTESIAN_POINT('Ctrl Pts',(4.58181353448852,72.4253618562249,0.));
#101541=CARTESIAN_POINT('Ctrl Pts',(4.57422945111095,72.449255920373,0.));
#101542=CARTESIAN_POINT('Ctrl Pts',(4.56661045683367,72.473180830571,0.));
#101543=CARTESIAN_POINT('Ctrl Pts',(4.55895653118214,72.4971364679055,0.));
#101544=CARTESIAN_POINT('Ctrl Pts',(4.55126765384403,72.5211227138997,0.));
#101545=CARTESIAN_POINT('Ctrl Pts',(4.54354380466826,72.5451394505106,0.));
#101546=CARTESIAN_POINT('Ctrl Pts',(4.53578496366802,72.5691865601225,0.));
#101547=CARTESIAN_POINT('Ctrl Pts',(4.52799111102391,72.5932639255406,0.));
#101548=CARTESIAN_POINT('Ctrl Pts',(4.52016222707633,72.6173714299935,0.));
#101549=CARTESIAN_POINT('Ctrl Pts',(4.5122982923226,72.6415089571314,0.));
#101550=CARTESIAN_POINT('Ctrl Pts',(4.50439928741605,72.6656763910241,0.));
#101551=CARTESIAN_POINT('Ctrl Pts',(4.49646519316822,72.689873616155,0.));
#101552=CARTESIAN_POINT('Ctrl Pts',(4.48849599055354,72.7141005174153,0.));
#101553=CARTESIAN_POINT('Ctrl Pts',(4.48049166070224,72.7383569801042,0.));
#101554=CARTESIAN_POINT('Ctrl Pts',(4.47245218489623,72.7626428899287,0.));
#101555=CARTESIAN_POINT('Ctrl Pts',(4.46437754456796,72.7869581329994,0.));
#101556=CARTESIAN_POINT('Ctrl Pts',(4.45626772130139,72.8113025958258,0.));
#101557=CARTESIAN_POINT('Ctrl Pts',(4.44812269683725,72.8356761653064,0.));
#101558=CARTESIAN_POINT('Ctrl Pts',(4.43994245306805,72.8600787287316,0.));
#101559=CARTESIAN_POINT('Ctrl Pts',(4.43172697203342,72.8845101737856,0.));
#101560=CARTESIAN_POINT('Ctrl Pts',(4.42347623591942,72.9089703885464,0.));
#101561=CARTESIAN_POINT('Ctrl Pts',(4.41519022705927,72.9334592614828,0.));
#101562=CARTESIAN_POINT('Ctrl Pts',(4.40686892793966,72.9579766814495,0.));
#101563=CARTESIAN_POINT('Ctrl Pts',(4.39851232119731,72.9825225376839,0.));
#101564=CARTESIAN_POINT('Ctrl Pts',(4.39012038961145,73.0070967198033,0.));
#101565=CARTESIAN_POINT('Ctrl Pts',(4.38169311610154,73.031699117799,0.));
#101566=CARTESIAN_POINT('Ctrl Pts',(4.37323048372607,73.0563296220301,0.));
#101567=CARTESIAN_POINT('Ctrl Pts',(4.36473247568639,73.0809881232111,0.));
#101568=CARTESIAN_POINT('Ctrl Pts',(4.35619907532716,73.1056745124099,0.));
#101569=CARTESIAN_POINT('Ctrl Pts',(4.34763026613155,73.1303886810602,0.));
#101570=CARTESIAN_POINT('Ctrl Pts',(4.3390260317214,73.1551305209692,0.));
#101571=CARTESIAN_POINT('Ctrl Pts',(4.33038635585878,73.1798999243234,0.));
#101572=CARTESIAN_POINT('Ctrl Pts',(4.32171122245219,73.204696783693,0.));
#101573=CARTESIAN_POINT('Ctrl Pts',(4.31300061556103,73.2295209920319,0.));
#101574=CARTESIAN_POINT('Ctrl Pts',(4.30425451938235,73.2543724426562,0.));
#101575=CARTESIAN_POINT('Ctrl Pts',(4.29547291824289,73.2792510292243,0.));
#101576=CARTESIAN_POINT('Ctrl Pts',(4.28665579659303,73.3041566457134,0.));
#101577=CARTESIAN_POINT('Ctrl Pts',(4.27780313900392,73.3290891863959,0.));
#101578=CARTESIAN_POINT('Ctrl Pts',(4.26891493016704,73.354048545808,0.));
#101579=CARTESIAN_POINT('Ctrl Pts',(4.25999115489905,73.3790346187953,0.));
#101580=CARTESIAN_POINT('Ctrl Pts',(4.25103179814892,73.4040473005603,0.));
#101581=CARTESIAN_POINT('Ctrl Pts',(4.24203684500942,73.4290864867103,0.));
#101582=CARTESIAN_POINT('Ctrl Pts',(4.23300628072758,73.4541520732943,0.));
#101583=CARTESIAN_POINT('Ctrl Pts',(4.22394009072754,73.4792439568624,0.));
#101584=CARTESIAN_POINT('Ctrl Pts',(4.21483826059437,73.5043620344107,0.));
#101585=CARTESIAN_POINT('Ctrl Pts',(4.20570077603728,73.5295062032621,0.));
#101586=CARTESIAN_POINT('Ctrl Pts',(4.19652762286127,73.554676360957,0.));
#101587=CARTESIAN_POINT('Ctrl Pts',(4.18731878694239,73.5798724051519,0.));
#101588=CARTESIAN_POINT('Ctrl Pts',(4.17807425419817,73.6050942334773,0.));
#101589=CARTESIAN_POINT('Ctrl Pts',(4.16879401058787,73.6303417435262,0.));
#101590=CARTESIAN_POINT('Ctrl Pts',(4.15947804217791,73.6556148331504,0.));
#101591=CARTESIAN_POINT('Ctrl Pts',(4.15012633519729,73.6809134006909,0.));
#101592=CARTESIAN_POINT('Ctrl Pts',(4.14073887610155,73.7062373452344,0.));
#101593=CARTESIAN_POINT('Ctrl Pts',(4.13131565163575,73.7315865668508,0.));
#101594=CARTESIAN_POINT('Ctrl Pts',(4.12185664890552,73.7569609668501,0.));
#101595=CARTESIAN_POINT('Ctrl Pts',(4.11236185522781,73.7823604472126,0.));
#101596=CARTESIAN_POINT('Ctrl Pts',(4.10283125798725,73.8077849100314,0.));
#101597=CARTESIAN_POINT('Ctrl Pts',(4.09326484448232,73.8332342568978,0.));
#101598=CARTESIAN_POINT('Ctrl Pts',(4.0836626018068,73.8587083884208,0.));
#101599=CARTESIAN_POINT('Ctrl Pts',(4.07402451665254,73.884207203405,0.));
#101600=CARTESIAN_POINT('Ctrl Pts',(4.06435057547335,73.9097305995173,0.));
#101601=CARTESIAN_POINT('Ctrl Pts',(4.05464076484762,73.9352784747665,0.));
#101602=CARTESIAN_POINT('Ctrl Pts',(4.04489507179964,73.9608507287943,0.));
#101603=CARTESIAN_POINT('Ctrl Pts',(4.03511348410661,73.9864472641025,0.));
#101604=CARTESIAN_POINT('Ctrl Pts',(4.02529599070086,74.0120679876396,0.));
#101605=CARTESIAN_POINT('Ctrl Pts',(4.01544258176694,74.0377128111754,0.));
#101606=CARTESIAN_POINT('Ctrl Pts',(4.00696550627606,74.0597159781919,0.));
#101607=CARTESIAN_POINT('Ctrl Pts',(4.00044689712491,74.0765982943431,0.));
#101608=CARTESIAN_POINT('Ctrl Pts',(3.99590266747766,74.0883491449662,0.));
#101609=CARTESIAN_POINT('Ctrl Pts',(3.9933433444657,74.0949615399274,0.));
#101610=CARTESIAN_POINT('Ctrl Pts',(3.99277406492178,74.0964320765798,0.));
#101611=CARTESIAN_POINT('',(5.24987136994593,69.8028570375097,12.));
#101612=CARTESIAN_POINT('',(5.24987136994593,69.8028570375097,0.));
#101613=CARTESIAN_POINT('Ctrl Pts',(3.99277406492178,74.0964320765798,12.));
#101614=CARTESIAN_POINT('Ctrl Pts',(3.9933433444657,74.0949615399274,12.));
#101615=CARTESIAN_POINT('Ctrl Pts',(3.99590266747766,74.0883491449662,12.));
#101616=CARTESIAN_POINT('Ctrl Pts',(4.00044689712491,74.0765982943431,12.));
#101617=CARTESIAN_POINT('Ctrl Pts',(4.00696550627606,74.0597159781919,12.));
#101618=CARTESIAN_POINT('Ctrl Pts',(4.01544258176694,74.0377128111754,12.));
#101619=CARTESIAN_POINT('Ctrl Pts',(4.02529599070086,74.0120679876396,12.));
#101620=CARTESIAN_POINT('Ctrl Pts',(4.03511348410661,73.9864472641025,12.));
#101621=CARTESIAN_POINT('Ctrl Pts',(4.04489507179964,73.9608507287943,12.));
#101622=CARTESIAN_POINT('Ctrl Pts',(4.05464076484762,73.9352784747665,12.));
#101623=CARTESIAN_POINT('Ctrl Pts',(4.06435057547335,73.9097305995173,12.));
#101624=CARTESIAN_POINT('Ctrl Pts',(4.07402451665254,73.884207203405,12.));
#101625=CARTESIAN_POINT('Ctrl Pts',(4.0836626018068,73.8587083884208,12.));
#101626=CARTESIAN_POINT('Ctrl Pts',(4.09326484448232,73.8332342568978,12.));
#101627=CARTESIAN_POINT('Ctrl Pts',(4.10283125798725,73.8077849100314,12.));
#101628=CARTESIAN_POINT('Ctrl Pts',(4.11236185522781,73.7823604472126,12.));
#101629=CARTESIAN_POINT('Ctrl Pts',(4.12185664890552,73.7569609668501,12.));
#101630=CARTESIAN_POINT('Ctrl Pts',(4.13131565163575,73.7315865668508,12.));
#101631=CARTESIAN_POINT('Ctrl Pts',(4.14073887610155,73.7062373452344,12.));
#101632=CARTESIAN_POINT('Ctrl Pts',(4.15012633519729,73.6809134006909,12.));
#101633=CARTESIAN_POINT('Ctrl Pts',(4.15947804217791,73.6556148331504,12.));
#101634=CARTESIAN_POINT('Ctrl Pts',(4.16879401058787,73.6303417435262,12.));
#101635=CARTESIAN_POINT('Ctrl Pts',(4.17807425419817,73.6050942334773,12.));
#101636=CARTESIAN_POINT('Ctrl Pts',(4.18731878694239,73.5798724051519,12.));
#101637=CARTESIAN_POINT('Ctrl Pts',(4.19652762286127,73.554676360957,12.));
#101638=CARTESIAN_POINT('Ctrl Pts',(4.20570077603728,73.5295062032621,12.));
#101639=CARTESIAN_POINT('Ctrl Pts',(4.21483826059437,73.5043620344107,12.));
#101640=CARTESIAN_POINT('Ctrl Pts',(4.22394009072754,73.4792439568624,12.));
#101641=CARTESIAN_POINT('Ctrl Pts',(4.23300628072758,73.4541520732943,12.));
#101642=CARTESIAN_POINT('Ctrl Pts',(4.24203684500942,73.4290864867103,12.));
#101643=CARTESIAN_POINT('Ctrl Pts',(4.25103179814892,73.4040473005603,12.));
#101644=CARTESIAN_POINT('Ctrl Pts',(4.25999115489905,73.3790346187953,12.));
#101645=CARTESIAN_POINT('Ctrl Pts',(4.26891493016704,73.354048545808,12.));
#101646=CARTESIAN_POINT('Ctrl Pts',(4.27780313900392,73.3290891863959,12.));
#101647=CARTESIAN_POINT('Ctrl Pts',(4.28665579659303,73.3041566457134,12.));
#101648=CARTESIAN_POINT('Ctrl Pts',(4.29547291824289,73.2792510292243,12.));
#101649=CARTESIAN_POINT('Ctrl Pts',(4.30425451938235,73.2543724426562,12.));
#101650=CARTESIAN_POINT('Ctrl Pts',(4.31300061556103,73.2295209920319,12.));
#101651=CARTESIAN_POINT('Ctrl Pts',(4.32171122245219,73.204696783693,12.));
#101652=CARTESIAN_POINT('Ctrl Pts',(4.33038635585878,73.1798999243234,12.));
#101653=CARTESIAN_POINT('Ctrl Pts',(4.3390260317214,73.1551305209692,12.));
#101654=CARTESIAN_POINT('Ctrl Pts',(4.34763026613155,73.1303886810602,12.));
#101655=CARTESIAN_POINT('Ctrl Pts',(4.35619907532716,73.1056745124099,12.));
#101656=CARTESIAN_POINT('Ctrl Pts',(4.36473247568639,73.0809881232111,12.));
#101657=CARTESIAN_POINT('Ctrl Pts',(4.37323048372607,73.0563296220301,12.));
#101658=CARTESIAN_POINT('Ctrl Pts',(4.38169311610154,73.031699117799,12.));
#101659=CARTESIAN_POINT('Ctrl Pts',(4.39012038961145,73.0070967198033,12.));
#101660=CARTESIAN_POINT('Ctrl Pts',(4.39851232119731,72.9825225376839,12.));
#101661=CARTESIAN_POINT('Ctrl Pts',(4.40686892793966,72.9579766814495,12.));
#101662=CARTESIAN_POINT('Ctrl Pts',(4.41519022705927,72.9334592614828,12.));
#101663=CARTESIAN_POINT('Ctrl Pts',(4.42347623591942,72.9089703885464,12.));
#101664=CARTESIAN_POINT('Ctrl Pts',(4.43172697203342,72.8845101737856,12.));
#101665=CARTESIAN_POINT('Ctrl Pts',(4.43994245306805,72.8600787287316,12.));
#101666=CARTESIAN_POINT('Ctrl Pts',(4.44812269683725,72.8356761653064,12.));
#101667=CARTESIAN_POINT('Ctrl Pts',(4.45626772130139,72.8113025958258,12.));
#101668=CARTESIAN_POINT('Ctrl Pts',(4.46437754456796,72.7869581329994,12.));
#101669=CARTESIAN_POINT('Ctrl Pts',(4.47245218489623,72.7626428899287,12.));
#101670=CARTESIAN_POINT('Ctrl Pts',(4.48049166070224,72.7383569801042,12.));
#101671=CARTESIAN_POINT('Ctrl Pts',(4.48849599055354,72.7141005174153,12.));
#101672=CARTESIAN_POINT('Ctrl Pts',(4.49646519316822,72.689873616155,12.));
#101673=CARTESIAN_POINT('Ctrl Pts',(4.50439928741605,72.6656763910241,12.));
#101674=CARTESIAN_POINT('Ctrl Pts',(4.5122982923226,72.6415089571314,12.));
#101675=CARTESIAN_POINT('Ctrl Pts',(4.52016222707633,72.6173714299935,12.));
#101676=CARTESIAN_POINT('Ctrl Pts',(4.52799111102391,72.5932639255406,12.));
#101677=CARTESIAN_POINT('Ctrl Pts',(4.53578496366802,72.5691865601225,12.));
#101678=CARTESIAN_POINT('Ctrl Pts',(4.54354380466826,72.5451394505106,12.));
#101679=CARTESIAN_POINT('Ctrl Pts',(4.55126765384403,72.5211227138997,12.));
#101680=CARTESIAN_POINT('Ctrl Pts',(4.55895653118214,72.4971364679055,12.));
#101681=CARTESIAN_POINT('Ctrl Pts',(4.56661045683367,72.473180830571,12.));
#101682=CARTESIAN_POINT('Ctrl Pts',(4.57422945111095,72.449255920373,12.));
#101683=CARTESIAN_POINT('Ctrl Pts',(4.58181353448852,72.4253618562249,12.));
#101684=CARTESIAN_POINT('Ctrl Pts',(4.58936272760551,72.4014987574789,12.));
#101685=CARTESIAN_POINT('Ctrl Pts',(4.59687705127341,72.3776667439244,12.));
#101686=CARTESIAN_POINT('Ctrl Pts',(4.60435652647464,72.3538659357932,12.));
#101687=CARTESIAN_POINT('Ctrl Pts',(4.61180117435869,72.330096453767,12.));
#101688=CARTESIAN_POINT('Ctrl Pts',(4.61921101624295,72.306358418981,12.));
#101689=CARTESIAN_POINT('Ctrl Pts',(4.62658607361466,72.2826519530254,12.));
#101690=CARTESIAN_POINT('Ctrl Pts',(4.63392636813843,72.2589771779447,12.));
#101691=CARTESIAN_POINT('Ctrl Pts',(4.64123192165628,72.2353342162408,12.));
#101692=CARTESIAN_POINT('Ctrl Pts',(4.64850275618326,72.2117231908816,12.));
#101693=CARTESIAN_POINT('Ctrl Pts',(4.65573889390825,72.1881442253052,12.));
#101694=CARTESIAN_POINT('Ctrl Pts',(4.66294035719571,72.1645974434218,12.));
#101695=CARTESIAN_POINT('Ctrl Pts',(4.67010716859282,72.1410829696129,12.));
#101696=CARTESIAN_POINT('Ctrl Pts',(4.67723935083088,72.1176009287349,12.));
#101697=CARTESIAN_POINT('Ctrl Pts',(4.68433692682061,72.0941514461283,12.));
#101698=CARTESIAN_POINT('Ctrl Pts',(4.69139991965281,72.070734647621,12.));
#101699=CARTESIAN_POINT('Ctrl Pts',(4.69842835259998,72.047350659532,12.));
#101700=CARTESIAN_POINT('Ctrl Pts',(4.70542224912313,72.0239996086694,12.));
#101701=CARTESIAN_POINT('Ctrl Pts',(4.71238163287411,72.0006816223335,12.));
#101702=CARTESIAN_POINT('Ctrl Pts',(4.71930652769081,71.9773968283267,12.));
#101703=CARTESIAN_POINT('Ctrl Pts',(4.72619695759779,71.9541453549582,12.));
#101704=CARTESIAN_POINT('Ctrl Pts',(4.73305294680784,71.9309273310469,12.));
#101705=CARTESIAN_POINT('Ctrl Pts',(4.73987451972861,71.9077428859207,12.));
#101706=CARTESIAN_POINT('Ctrl Pts',(4.74666170096546,71.8845921494186,12.));
#101707=CARTESIAN_POINT('Ctrl Pts',(4.75341451531672,71.8614752519008,12.));
#101708=CARTESIAN_POINT('Ctrl Pts',(4.76013298777423,71.8383923242533,12.));
#101709=CARTESIAN_POINT('Ctrl Pts',(4.76681714352504,71.8153434978924,12.));
#101710=CARTESIAN_POINT('Ctrl Pts',(4.77346700795788,71.7923289047636,12.));
#101711=CARTESIAN_POINT('Ctrl Pts',(4.78008260666643,71.7693486773449,12.));
#101712=CARTESIAN_POINT('Ctrl Pts',(4.78666396544451,71.7464029486552,12.));
#101713=CARTESIAN_POINT('Ctrl Pts',(4.79321111028673,71.7234918522604,12.));
#101714=CARTESIAN_POINT('Ctrl Pts',(4.79972406739015,71.7006155222766,12.));
#101715=CARTESIAN_POINT('Ctrl Pts',(4.80620286316089,71.6777740933705,12.));
#101716=CARTESIAN_POINT('Ctrl Pts',(4.81264752421732,71.6549677007613,12.));
#101717=CARTESIAN_POINT('Ctrl Pts',(4.81905807738558,71.6321964802326,12.));
#101718=CARTESIAN_POINT('Ctrl Pts',(4.82543454970027,71.6094605681366,12.));
#101719=CARTESIAN_POINT('Ctrl Pts',(4.83177696840638,71.5867601014,12.));
#101720=CARTESIAN_POINT('Ctrl Pts',(4.83808536096584,71.564095217521,12.));
#101721=CARTESIAN_POINT('Ctrl Pts',(4.84435975506049,71.5414660545739,12.));
#101722=CARTESIAN_POINT('Ctrl Pts',(4.85060017858781,71.5188727512197,12.));
#101723=CARTESIAN_POINT('Ctrl Pts',(4.85680665966181,71.4963154467113,12.));
#101724=CARTESIAN_POINT('Ctrl Pts',(4.86297922661503,71.4737942808982,12.));
#101725=CARTESIAN_POINT('Ctrl Pts',(4.86911790800551,71.4513093942255,12.));
#101726=CARTESIAN_POINT('Ctrl Pts',(4.87522273261908,71.4288609277374,12.));
#101727=CARTESIAN_POINT('Ctrl Pts',(4.88129372946552,71.4064490230899,12.));
#101728=CARTESIAN_POINT('Ctrl Pts',(4.88733092777976,71.3840738225562,12.));
#101729=CARTESIAN_POINT('Ctrl Pts',(4.89333435702414,71.3617354690325,12.));
#101730=CARTESIAN_POINT('Ctrl Pts',(4.89930404689576,71.3394341060359,12.));
#101731=CARTESIAN_POINT('Ctrl Pts',(4.9052400273278,71.3171698777084,12.));
#101732=CARTESIAN_POINT('Ctrl Pts',(4.91114232848604,71.294942928829,12.));
#101733=CARTESIAN_POINT('Ctrl Pts',(4.91701098077037,71.2727534048192,12.));
#101734=CARTESIAN_POINT('Ctrl Pts',(4.92284601481722,71.250601451747,12.));
#101735=CARTESIAN_POINT('Ctrl Pts',(4.92864746150733,71.2284872163273,12.));
#101736=CARTESIAN_POINT('Ctrl Pts',(4.93441535196618,71.2064108459286,12.));
#101737=CARTESIAN_POINT('Ctrl Pts',(4.94014971756115,71.1843724885847,12.));
#101738=CARTESIAN_POINT('Ctrl Pts',(4.94585058990342,71.1623722930001,12.));
#101739=CARTESIAN_POINT('Ctrl Pts',(4.95151800085102,71.1404104085552,12.));
#101740=CARTESIAN_POINT('Ctrl Pts',(4.95715198251685,71.1184869853056,12.));
#101741=CARTESIAN_POINT('Ctrl Pts',(4.96275256726767,71.0966021739907,12.));
#101742=CARTESIAN_POINT('Ctrl Pts',(4.96831978772191,71.0747561260436,12.));
#101743=CARTESIAN_POINT('Ctrl Pts',(4.97385367675159,71.0529489935961,12.));
#101744=CARTESIAN_POINT('Ctrl Pts',(4.97935426748585,71.0311809294821,12.));
#101745=CARTESIAN_POINT('Ctrl Pts',(4.98482159331864,71.0094520872377,12.));
#101746=CARTESIAN_POINT('Ctrl Pts',(4.99025568790665,70.9877626211113,12.));
#101747=CARTESIAN_POINT('Ctrl Pts',(4.99565658516914,70.9661126860773,12.));
#101748=CARTESIAN_POINT('Ctrl Pts',(5.0010243192904,70.9445024378439,12.));
#101749=CARTESIAN_POINT('Ctrl Pts',(5.00635892472514,70.9229320328589,12.));
#101750=CARTESIAN_POINT('Ctrl Pts',(5.01166043620568,70.9014016283124,12.));
#101751=CARTESIAN_POINT('Ctrl Pts',(5.01692888873791,70.8799113821452,12.));
#101752=CARTESIAN_POINT('Ctrl Pts',(5.02216431760061,70.8584614530519,12.));
#101753=CARTESIAN_POINT('Ctrl Pts',(5.02736675834694,70.8370520004843,12.));
#101754=CARTESIAN_POINT('Ctrl Pts',(5.03253624680942,70.8156831846488,12.));
#101755=CARTESIAN_POINT('Ctrl Pts',(5.0376728191048,70.7943551665059,12.));
#101756=CARTESIAN_POINT('Ctrl Pts',(5.0427765116335,70.7730681077983,12.));
#101757=CARTESIAN_POINT('Ctrl Pts',(5.04784736108347,70.7518221710706,12.));
#101758=CARTESIAN_POINT('Ctrl Pts',(5.05288540443483,70.7306175196863,12.));
#101759=CARTESIAN_POINT('Ctrl Pts',(5.05789067897058,70.7094543178438,12.));
#101760=CARTESIAN_POINT('Ctrl Pts',(5.06286322227821,70.6883327305784,12.));
#101761=CARTESIAN_POINT('Ctrl Pts',(5.06780307224073,70.6672529237455,12.));
#101762=CARTESIAN_POINT('Ctrl Pts',(5.07271026703356,70.6462150640015,12.));
#101763=CARTESIAN_POINT('Ctrl Pts',(5.07758484512303,70.6252193187878,12.));
#101764=CARTESIAN_POINT('Ctrl Pts',(5.08242684526687,70.6042658562923,12.));
#101765=CARTESIAN_POINT('Ctrl Pts',(5.08723630652274,70.5833548455014,12.));
#101766=CARTESIAN_POINT('Ctrl Pts',(5.09201326826135,70.5624864562824,12.));
#101767=CARTESIAN_POINT('Ctrl Pts',(5.09675777018184,70.5416608594526,12.));
#101768=CARTESIAN_POINT('Ctrl Pts',(5.10146985232942,70.5208782268497,12.));
#101769=CARTESIAN_POINT('Ctrl Pts',(5.10614955511665,70.500138731399,12.));
#101770=CARTESIAN_POINT('Ctrl Pts',(5.11079691929214,70.4794425469825,12.));
#101771=CARTESIAN_POINT('Ctrl Pts',(5.11541198590933,70.458789848296,12.));
#101772=CARTESIAN_POINT('Ctrl Pts',(5.11999479630212,70.4381808107245,12.));
#101773=CARTESIAN_POINT('Ctrl Pts',(5.12454539205329,70.417615610161,12.));
#101774=CARTESIAN_POINT('Ctrl Pts',(5.12906381499457,70.3970944229851,12.));
#101775=CARTESIAN_POINT('Ctrl Pts',(5.13355010728568,70.3766174264757,12.));
#101776=CARTESIAN_POINT('Ctrl Pts',(5.13800431148904,70.3561847991714,12.));
#101777=CARTESIAN_POINT('Ctrl Pts',(5.1424264706348,70.3357967211796,12.));
#101778=CARTESIAN_POINT('Ctrl Pts',(5.14681662833081,70.3154533746736,12.));
#101779=CARTESIAN_POINT('Ctrl Pts',(5.15117482869255,70.2951549435512,12.));
#101780=CARTESIAN_POINT('Ctrl Pts',(5.1555011161486,70.2749016125105,12.));
#101781=CARTESIAN_POINT('Ctrl Pts',(5.15979553528204,70.2546935662722,12.));
#101782=CARTESIAN_POINT('Ctrl Pts',(5.16405813066977,70.2345309887833,12.));
#101783=CARTESIAN_POINT('Ctrl Pts',(5.16828894670109,70.2144140622953,12.));
#101784=CARTESIAN_POINT('Ctrl Pts',(5.1724880279339,70.1943429691167,12.));
#101785=CARTESIAN_POINT('Ctrl Pts',(5.17665541952384,70.1743178937077,12.));
#101786=CARTESIAN_POINT('Ctrl Pts',(5.18079116757667,70.1543390243892,12.));
#101787=CARTESIAN_POINT('Ctrl Pts',(5.18489531966266,70.1344065558145,12.));
#101788=CARTESIAN_POINT('Ctrl Pts',(5.18896792486566,70.1145206891885,12.));
#101789=CARTESIAN_POINT('Ctrl Pts',(5.19300903271581,70.0946816270997,12.));
#101790=CARTESIAN_POINT('Ctrl Pts',(5.19701869225529,70.0748895689729,12.));
#101791=CARTESIAN_POINT('Ctrl Pts',(5.20099695122657,70.0551447071082,12.));
#101792=CARTESIAN_POINT('Ctrl Pts',(5.20494385478026,70.0354472203546,12.));
#101793=CARTESIAN_POINT('Ctrl Pts',(5.20885944672837,70.0157972802182,12.));
#101794=CARTESIAN_POINT('Ctrl Pts',(5.2127437720326,69.9961950629965,12.));
#101795=CARTESIAN_POINT('Ctrl Pts',(5.2165968788114,69.9766407595385,12.));
#101796=CARTESIAN_POINT('Ctrl Pts',(5.22041882075722,69.9571345870076,12.));
#101797=CARTESIAN_POINT('Ctrl Pts',(5.22420965879982,69.9376767969095,12.));
#101798=CARTESIAN_POINT('Ctrl Pts',(5.22796945602795,69.9182676502048,12.));
#101799=CARTESIAN_POINT('Ctrl Pts',(5.23169827290556,69.8989073936688,12.));
#101800=CARTESIAN_POINT('Ctrl Pts',(5.23539616279621,69.8795962381599,12.));
#101801=CARTESIAN_POINT('Ctrl Pts',(5.23906316634803,69.8603343302743,12.));
#101802=CARTESIAN_POINT('Ctrl Pts',(5.2426993105457,69.841121750752,12.));
#101803=CARTESIAN_POINT('Ctrl Pts',(5.24558355159751,69.8257911792159,12.));
#101804=CARTESIAN_POINT('Ctrl Pts',(5.24773285666377,69.8143154684204,12.));
#101805=CARTESIAN_POINT('Ctrl Pts',(5.24915955997427,69.8066748687772,12.));
#101806=CARTESIAN_POINT('Ctrl Pts',(5.24987136994593,69.8028570375097,12.));
#101807=CARTESIAN_POINT('Ctrl Pts',(2.48034921844894,74.1624659714953,0.));
#101808=CARTESIAN_POINT('Ctrl Pts',(2.48034921844894,74.1624659714953,4.));
#101809=CARTESIAN_POINT('Ctrl Pts',(2.48034921844894,74.1624659714953,8.));
#101810=CARTESIAN_POINT('Ctrl Pts',(2.48034921844894,74.1624659714953,12.));
#101811=CARTESIAN_POINT('Ctrl Pts',(2.52879860312834,74.2610905805697,0.));
#101812=CARTESIAN_POINT('Ctrl Pts',(2.52879860312834,74.2610905805697,4.));
#101813=CARTESIAN_POINT('Ctrl Pts',(2.52879860312834,74.2610905805697,8.));
#101814=CARTESIAN_POINT('Ctrl Pts',(2.52879860312834,74.2610905805697,12.));
#101815=CARTESIAN_POINT('Ctrl Pts',(2.67239300265247,74.404107577982,0.));
#101816=CARTESIAN_POINT('Ctrl Pts',(2.67239300265247,74.404107577982,4.00000000000001));
#101817=CARTESIAN_POINT('Ctrl Pts',(2.67239300265247,74.404107577982,7.99999999999999));
#101818=CARTESIAN_POINT('Ctrl Pts',(2.67239300265247,74.404107577982,12.));
#101819=CARTESIAN_POINT('Ctrl Pts',(2.86656650944678,74.4448761712981,0.));
#101820=CARTESIAN_POINT('Ctrl Pts',(2.86656650944678,74.4448761712981,3.99999999999999));
#101821=CARTESIAN_POINT('Ctrl Pts',(2.86656650944678,74.4448761712981,8.00000000000001));
#101822=CARTESIAN_POINT('Ctrl Pts',(2.86656650944678,74.4448761712981,12.));
#101823=CARTESIAN_POINT('Ctrl Pts',(2.94891377268021,74.441614084874,0.));
#101824=CARTESIAN_POINT('Ctrl Pts',(2.94891377268021,74.441614084874,4.));
#101825=CARTESIAN_POINT('Ctrl Pts',(2.94891377268021,74.441614084874,8.));
#101826=CARTESIAN_POINT('Ctrl Pts',(2.94891377268021,74.441614084874,12.));
#101827=CARTESIAN_POINT('',(2.48034921844894,74.1624659714953,0.));
#101828=CARTESIAN_POINT('',(2.94891377268021,74.4416140848739,0.));
#101829=CARTESIAN_POINT('Ctrl Pts',(2.48034921844894,74.1624659714953,1.88097848788491E-35));
#101830=CARTESIAN_POINT('Ctrl Pts',(2.52879860312834,74.2610905805697,1.88097848788491E-35));
#101831=CARTESIAN_POINT('Ctrl Pts',(2.61085254571356,74.342814579091,1.88097848788492E-35));
#101832=CARTESIAN_POINT('Ctrl Pts',(2.70942211516251,74.3911513436217,1.88097848788491E-35));
#101833=CARTESIAN_POINT('Ctrl Pts',(2.78334929224922,74.4274039170197,1.88097848788491E-35));
#101834=CARTESIAN_POINT('Ctrl Pts',(2.86656650944678,74.4448761712981,1.88097848788491E-35));
#101835=CARTESIAN_POINT('Ctrl Pts',(2.94891377268021,74.441614084874,1.88097848788491E-35));
#101836=CARTESIAN_POINT('',(2.94891377268021,74.4416140848739,12.));
#101837=CARTESIAN_POINT('Ctrl Pts',(2.94891377268021,74.441614084874,0.));
#101838=CARTESIAN_POINT('Ctrl Pts',(2.94891377268021,74.441614084874,4.));
#101839=CARTESIAN_POINT('Ctrl Pts',(2.94891377268021,74.441614084874,8.));
#101840=CARTESIAN_POINT('Ctrl Pts',(2.94891377268021,74.441614084874,12.));
#101841=CARTESIAN_POINT('',(2.48034921844894,74.1624659714953,12.));
#101842=CARTESIAN_POINT('Ctrl Pts',(2.94891377268021,74.441614084874,12.));
#101843=CARTESIAN_POINT('Ctrl Pts',(2.86656650944678,74.4448761712981,12.));
#101844=CARTESIAN_POINT('Ctrl Pts',(2.78334929224922,74.4274039170197,12.));
#101845=CARTESIAN_POINT('Ctrl Pts',(2.70942211516251,74.3911513436217,12.));
#101846=CARTESIAN_POINT('Ctrl Pts',(2.61085254571356,74.342814579091,12.));
#101847=CARTESIAN_POINT('Ctrl Pts',(2.52879860312834,74.2610905805697,12.));
#101848=CARTESIAN_POINT('Ctrl Pts',(2.48034921844894,74.1624659714953,12.));
#101849=CARTESIAN_POINT('Ctrl Pts',(2.48034921844894,74.1624659714953,12.));
#101850=CARTESIAN_POINT('Ctrl Pts',(2.48034921844894,74.1624659714953,8.));
#101851=CARTESIAN_POINT('Ctrl Pts',(2.48034921844894,74.1624659714953,4.));
#101852=CARTESIAN_POINT('Ctrl Pts',(2.48034921844894,74.1624659714953,0.));
#101853=CARTESIAN_POINT('Origin',(1.62512913209676E-11,3.74491326291036E-10,
0.));
#101854=CARTESIAN_POINT('Origin',(1.62512913209676E-11,3.74491326291036E-10,
12.));
#101855=CARTESIAN_POINT('Origin',(1.62512913209676E-11,3.74491326291036E-10,
0.));
#101856=CARTESIAN_POINT('Ctrl Pts',(10.0225374821205,73.8227522002498,-5.55111512312578E-16));
#101857=CARTESIAN_POINT('Ctrl Pts',(10.0225374821205,73.8227522002498,4.));
#101858=CARTESIAN_POINT('Ctrl Pts',(10.0225374821204,73.8227522002498,8.));
#101859=CARTESIAN_POINT('Ctrl Pts',(10.0225374821204,73.8227522002498,12.));
#101860=CARTESIAN_POINT('Ctrl Pts',(10.1314210536415,73.8079696346554,-5.55111512312578E-16));
#101861=CARTESIAN_POINT('Ctrl Pts',(10.1314210536415,73.8079696346554,4.));
#101862=CARTESIAN_POINT('Ctrl Pts',(10.1314210536415,73.8079696346554,8.00000000000001));
#101863=CARTESIAN_POINT('Ctrl Pts',(10.1314210536415,73.8079696346554,12.));
#101864=CARTESIAN_POINT('Ctrl Pts',(10.3125002643518,73.7169567649191,-5.55111512312578E-16));
#101865=CARTESIAN_POINT('Ctrl Pts',(10.3125002643518,73.7169567649191,4.));
#101866=CARTESIAN_POINT('Ctrl Pts',(10.3125002643517,73.7169567649191,7.99999999999999));
#101867=CARTESIAN_POINT('Ctrl Pts',(10.3125002643517,73.7169567649191,12.));
#101868=CARTESIAN_POINT('Ctrl Pts',(10.4125694172277,73.5456341632195,-5.55111512312578E-16));
#101869=CARTESIAN_POINT('Ctrl Pts',(10.4125694172277,73.5456341632195,4.));
#101870=CARTESIAN_POINT('Ctrl Pts',(10.4125694172276,73.5456341632195,8.00000000000001));
#101871=CARTESIAN_POINT('Ctrl Pts',(10.4125694172276,73.5456341632195,12.));
#101872=CARTESIAN_POINT('Ctrl Pts',(10.435509926739,73.4664795929517,-5.55111512312578E-16));
#101873=CARTESIAN_POINT('Ctrl Pts',(10.435509926739,73.4664795929517,4.));
#101874=CARTESIAN_POINT('Ctrl Pts',(10.4355099267389,73.4664795929517,8.));
#101875=CARTESIAN_POINT('Ctrl Pts',(10.4355099267389,73.4664795929517,12.));
#101876=CARTESIAN_POINT('',(10.0225374821205,73.8227522002498,0.));
#101877=CARTESIAN_POINT('',(10.4355099267391,73.4664795929517,2.77555756156289E-16));
#101878=CARTESIAN_POINT('Ctrl Pts',(10.0225374821205,73.8227522002498,-1.38777878078145E-16));
#101879=CARTESIAN_POINT('Ctrl Pts',(10.1314210536415,73.8079696346554,-1.38777878078145E-16));
#101880=CARTESIAN_POINT('Ctrl Pts',(10.2348948883331,73.7559622805204,-1.38777878078144E-16));
#101881=CARTESIAN_POINT('Ctrl Pts',(10.311916459242,73.6777313404381,-1.38777878078144E-16));
#101882=CARTESIAN_POINT('Ctrl Pts',(10.3696826374237,73.6190581353764,-1.38777878078145E-16));
#101883=CARTESIAN_POINT('Ctrl Pts',(10.4125694172277,73.5456341632195,-1.38777878078145E-16));
#101884=CARTESIAN_POINT('Ctrl Pts',(10.435509926739,73.4664795929517,-1.38777878078145E-16));
#101885=CARTESIAN_POINT('',(10.4355099267391,73.4664795929518,12.));
#101886=CARTESIAN_POINT('Ctrl Pts',(10.435509926739,73.4664795929517,-5.55111512312578E-16));
#101887=CARTESIAN_POINT('Ctrl Pts',(10.435509926739,73.4664795929517,4.));
#101888=CARTESIAN_POINT('Ctrl Pts',(10.4355099267389,73.4664795929517,8.));
#101889=CARTESIAN_POINT('Ctrl Pts',(10.4355099267389,73.4664795929517,12.));
#101890=CARTESIAN_POINT('',(10.0225374821204,73.8227522002498,12.));
#101891=CARTESIAN_POINT('Ctrl Pts',(10.4355099267389,73.4664795929517,12.));
#101892=CARTESIAN_POINT('Ctrl Pts',(10.4125694172276,73.5456341632195,12.));
#101893=CARTESIAN_POINT('Ctrl Pts',(10.3696826374237,73.6190581353765,12.));
#101894=CARTESIAN_POINT('Ctrl Pts',(10.311916459242,73.6777313404381,12.));
#101895=CARTESIAN_POINT('Ctrl Pts',(10.2348948883331,73.7559622805204,12.));
#101896=CARTESIAN_POINT('Ctrl Pts',(10.1314210536415,73.8079696346554,12.));
#101897=CARTESIAN_POINT('Ctrl Pts',(10.0225374821204,73.8227522002498,12.));
#101898=CARTESIAN_POINT('Ctrl Pts',(10.0225374821204,73.8227522002498,12.));
#101899=CARTESIAN_POINT('Ctrl Pts',(10.0225374821204,73.8227522002498,8.));
#101900=CARTESIAN_POINT('Ctrl Pts',(10.0225374821205,73.8227522002498,4.));
#101901=CARTESIAN_POINT('Ctrl Pts',(10.0225374821205,73.8227522002498,-5.55111512312578E-16));
#101902=CARTESIAN_POINT('Ctrl Pts',(11.3136138754165,69.079679653846,0.));
#101903=CARTESIAN_POINT('Ctrl Pts',(11.3136138754165,69.079679653846,12.));
#101904=CARTESIAN_POINT('Ctrl Pts',(11.3132375200165,69.0835449954396,0.));
#101905=CARTESIAN_POINT('Ctrl Pts',(11.3132375200165,69.0835449954396,12.));
#101906=CARTESIAN_POINT('Ctrl Pts',(11.3124821678798,69.0912808656811,0.));
#101907=CARTESIAN_POINT('Ctrl Pts',(11.3124821678798,69.0912808656811,12.));
#101908=CARTESIAN_POINT('Ctrl Pts',(11.3113412156661,69.1029002322118,0.));
#101909=CARTESIAN_POINT('Ctrl Pts',(11.3113412156661,69.1029002322118,12.));
#101910=CARTESIAN_POINT('Ctrl Pts',(11.3098040973713,69.118423844466,0.));
#101911=CARTESIAN_POINT('Ctrl Pts',(11.3098040973713,69.118423844466,12.));
#101912=CARTESIAN_POINT('Ctrl Pts',(11.3078562764384,69.1378802251711,0.));
#101913=CARTESIAN_POINT('Ctrl Pts',(11.3078562764384,69.1378802251711,12.));
#101914=CARTESIAN_POINT('Ctrl Pts',(11.3058820128307,69.1573884361,0.));
#101915=CARTESIAN_POINT('Ctrl Pts',(11.3058820128307,69.1573884361,12.));
#101916=CARTESIAN_POINT('Ctrl Pts',(11.3038812726292,69.1769483991721,0.));
#101917=CARTESIAN_POINT('Ctrl Pts',(11.3038812726292,69.1769483991721,12.));
#101918=CARTESIAN_POINT('Ctrl Pts',(11.3018540025638,69.1965599718914,0.));
#101919=CARTESIAN_POINT('Ctrl Pts',(11.3018540025638,69.1965599718914,12.));
#101920=CARTESIAN_POINT('Ctrl Pts',(11.2998001310964,69.2162229488531,0.));
#101921=CARTESIAN_POINT('Ctrl Pts',(11.2998001310964,69.2162229488531,12.));
#101922=CARTESIAN_POINT('Ctrl Pts',(11.2977195764852,69.2359370894907,0.));
#101923=CARTESIAN_POINT('Ctrl Pts',(11.2977195764852,69.2359370894907,12.));
#101924=CARTESIAN_POINT('Ctrl Pts',(11.2956122531375,69.2557021393351,0.));
#101925=CARTESIAN_POINT('Ctrl Pts',(11.2956122531375,69.2557021393351,12.));
#101926=CARTESIAN_POINT('Ctrl Pts',(11.2934780784351,69.275517853148,0.));
#101927=CARTESIAN_POINT('Ctrl Pts',(11.2934780784351,69.275517853148,12.));
#101928=CARTESIAN_POINT('Ctrl Pts',(11.2913169799628,69.295384019272,0.));
#101929=CARTESIAN_POINT('Ctrl Pts',(11.2913169799628,69.295384019272,12.));
#101930=CARTESIAN_POINT('Ctrl Pts',(11.2891288931517,69.3153004517783,0.));
#101931=CARTESIAN_POINT('Ctrl Pts',(11.2891288931517,69.3153004517783,12.));
#101932=CARTESIAN_POINT('Ctrl Pts',(11.2869137578459,69.3352669789587,0.));
#101933=CARTESIAN_POINT('Ctrl Pts',(11.2869137578459,69.3352669789587,12.));
#101934=CARTESIAN_POINT('Ctrl Pts',(11.2846715154524,69.3552834337784,0.));
#101935=CARTESIAN_POINT('Ctrl Pts',(11.2846715154524,69.3552834337784,12.));
#101936=CARTESIAN_POINT('Ctrl Pts',(11.2824021054045,69.3753496420039,0.));
#101937=CARTESIAN_POINT('Ctrl Pts',(11.2824021054045,69.3753496420039,12.));
#101938=CARTESIAN_POINT('Ctrl Pts',(11.2801054633816,69.3954654162281,0.));
#101939=CARTESIAN_POINT('Ctrl Pts',(11.2801054633816,69.3954654162281,12.));
#101940=CARTESIAN_POINT('Ctrl Pts',(11.2777815231469,69.4156305620593,0.));
#101941=CARTESIAN_POINT('Ctrl Pts',(11.2777815231469,69.4156305620593,12.));
#101942=CARTESIAN_POINT('Ctrl Pts',(11.2754302177021,69.4358448819967,0.));
#101943=CARTESIAN_POINT('Ctrl Pts',(11.2754302177021,69.4358448819967,12.));
#101944=CARTESIAN_POINT('Ctrl Pts',(11.2730514806139,69.456108179879,0.));
#101945=CARTESIAN_POINT('Ctrl Pts',(11.2730514806139,69.456108179879,12.));
#101946=CARTESIAN_POINT('Ctrl Pts',(11.270645247528,69.4764202659397,0.));
#101947=CARTESIAN_POINT('Ctrl Pts',(11.270645247528,69.4764202659397,12.));
#101948=CARTESIAN_POINT('Ctrl Pts',(11.2682114561008,69.4967809565929,0.));
#101949=CARTESIAN_POINT('Ctrl Pts',(11.2682114561008,69.4967809565929,12.));
#101950=CARTESIAN_POINT('Ctrl Pts',(11.2657500452716,69.5171900720158,0.));
#101951=CARTESIAN_POINT('Ctrl Pts',(11.2657500452716,69.5171900720158,12.));
#101952=CARTESIAN_POINT('Ctrl Pts',(11.263260954763,69.5376474344771,0.));
#101953=CARTESIAN_POINT('Ctrl Pts',(11.263260954763,69.5376474344771,12.));
#101954=CARTESIAN_POINT('Ctrl Pts',(11.2607441244703,69.5581528662877,0.));
#101955=CARTESIAN_POINT('Ctrl Pts',(11.2607441244703,69.5581528662877,12.));
#101956=CARTESIAN_POINT('Ctrl Pts',(11.2581994939541,69.5787061880857,0.));
#101957=CARTESIAN_POINT('Ctrl Pts',(11.2581994939541,69.5787061880857,12.));
#101958=CARTESIAN_POINT('Ctrl Pts',(11.2556270027016,69.599307219739,0.));
#101959=CARTESIAN_POINT('Ctrl Pts',(11.2556270027016,69.599307219739,12.));
#101960=CARTESIAN_POINT('Ctrl Pts',(11.2530265903557,69.6199557811245,0.));
#101961=CARTESIAN_POINT('Ctrl Pts',(11.2530265903557,69.6199557811245,12.));
#101962=CARTESIAN_POINT('Ctrl Pts',(11.2503981969412,69.6406516928891,0.));
#101963=CARTESIAN_POINT('Ctrl Pts',(11.2503981969412,69.6406516928891,12.));
#101964=CARTESIAN_POINT('Ctrl Pts',(11.2477417631386,69.6613947773534,0.));
#101965=CARTESIAN_POINT('Ctrl Pts',(11.2477417631386,69.6613947773534,12.));
#101966=CARTESIAN_POINT('Ctrl Pts',(11.2450572303841,69.6821848588457,0.));
#101967=CARTESIAN_POINT('Ctrl Pts',(11.2450572303841,69.6821848588457,12.));
#101968=CARTESIAN_POINT('Ctrl Pts',(11.2423445407166,69.7030217632164,0.));
#101969=CARTESIAN_POINT('Ctrl Pts',(11.2423445407166,69.7030217632164,12.));
#101970=CARTESIAN_POINT('Ctrl Pts',(11.239603636686,69.7239053175356,0.));
#101971=CARTESIAN_POINT('Ctrl Pts',(11.239603636686,69.7239053175356,12.));
#101972=CARTESIAN_POINT('Ctrl Pts',(11.2368344612472,69.7448353497408,0.));
#101973=CARTESIAN_POINT('Ctrl Pts',(11.2368344612472,69.7448353497408,12.));
#101974=CARTESIAN_POINT('Ctrl Pts',(11.2340369576456,69.7658116882324,0.));
#101975=CARTESIAN_POINT('Ctrl Pts',(11.2340369576456,69.7658116882324,12.));
#101976=CARTESIAN_POINT('Ctrl Pts',(11.2312110694187,69.7868341618954,0.));
#101977=CARTESIAN_POINT('Ctrl Pts',(11.2312110694187,69.7868341618954,12.));
#101978=CARTESIAN_POINT('Ctrl Pts',(11.2283567404437,69.8079026002768,0.));
#101979=CARTESIAN_POINT('Ctrl Pts',(11.2283567404437,69.8079026002768,12.));
#101980=CARTESIAN_POINT('Ctrl Pts',(11.225473914972,69.8290168337076,0.));
#101981=CARTESIAN_POINT('Ctrl Pts',(11.225473914972,69.8290168337076,12.));
#101982=CARTESIAN_POINT('Ctrl Pts',(11.2225625376736,69.8501766934428,0.));
#101983=CARTESIAN_POINT('Ctrl Pts',(11.2225625376736,69.8501766934428,12.));
#101984=CARTESIAN_POINT('Ctrl Pts',(11.219622553679,69.871382011789,0.));
#101985=CARTESIAN_POINT('Ctrl Pts',(11.219622553679,69.871382011789,12.));
#101986=CARTESIAN_POINT('Ctrl Pts',(11.2166539085523,69.8926326220385,0.));
#101987=CARTESIAN_POINT('Ctrl Pts',(11.2166539085523,69.8926326220385,12.));
#101988=CARTESIAN_POINT('Ctrl Pts',(11.2136565482678,69.9139283584022,0.));
#101989=CARTESIAN_POINT('Ctrl Pts',(11.2136565482678,69.9139283584022,12.));
#101990=CARTESIAN_POINT('Ctrl Pts',(11.2106304191882,69.9352690559405,0.));
#101991=CARTESIAN_POINT('Ctrl Pts',(11.2106304191882,69.9352690559405,12.));
#101992=CARTESIAN_POINT('Ctrl Pts',(11.2075754680449,69.9566545504837,0.));
#101993=CARTESIAN_POINT('Ctrl Pts',(11.2075754680449,69.9566545504837,12.));
#101994=CARTESIAN_POINT('Ctrl Pts',(11.2044916419244,69.97808467858,0.));
#101995=CARTESIAN_POINT('Ctrl Pts',(11.2044916419244,69.97808467858,12.));
#101996=CARTESIAN_POINT('Ctrl Pts',(11.2013788882714,69.9995592775343,0.));
#101997=CARTESIAN_POINT('Ctrl Pts',(11.2013788882714,69.9995592775343,12.));
#101998=CARTESIAN_POINT('Ctrl Pts',(11.1982371548919,70.0210781854243,0.));
#101999=CARTESIAN_POINT('Ctrl Pts',(11.1982371548919,70.0210781854243,12.));
#102000=CARTESIAN_POINT('Ctrl Pts',(11.1950663899576,70.0426412411185,0.));
#102001=CARTESIAN_POINT('Ctrl Pts',(11.1950663899576,70.0426412411185,12.));
#102002=CARTESIAN_POINT('Ctrl Pts',(11.1918665420166,70.0642482842928,0.));
#102003=CARTESIAN_POINT('Ctrl Pts',(11.1918665420166,70.0642482842928,12.));
#102004=CARTESIAN_POINT('Ctrl Pts',(11.1886375599914,70.0858991554283,0.));
#102005=CARTESIAN_POINT('Ctrl Pts',(11.1886375599914,70.0858991554283,12.));
#102006=CARTESIAN_POINT('Ctrl Pts',(11.185379393167,70.1075936957968,0.));
#102007=CARTESIAN_POINT('Ctrl Pts',(11.185379393167,70.1075936957968,12.));
#102008=CARTESIAN_POINT('Ctrl Pts',(11.1820919911846,70.1293317474432,0.));
#102009=CARTESIAN_POINT('Ctrl Pts',(11.1820919911846,70.1293317474432,12.));
#102010=CARTESIAN_POINT('Ctrl Pts',(11.1787753040363,70.1511131531674,0.));
#102011=CARTESIAN_POINT('Ctrl Pts',(11.1787753040363,70.1511131531674,12.));
#102012=CARTESIAN_POINT('Ctrl Pts',(11.1754292820631,70.1729377564956,0.));
#102013=CARTESIAN_POINT('Ctrl Pts',(11.1754292820631,70.1729377564956,12.));
#102014=CARTESIAN_POINT('Ctrl Pts',(11.1720538759499,70.1948054016817,0.));
#102015=CARTESIAN_POINT('Ctrl Pts',(11.1720538759499,70.1948054016817,12.));
#102016=CARTESIAN_POINT('Ctrl Pts',(11.168649036721,70.2167159337095,0.));
#102017=CARTESIAN_POINT('Ctrl Pts',(11.168649036721,70.2167159337095,12.));
#102018=CARTESIAN_POINT('Ctrl Pts',(11.1652147157383,70.2386691982902,0.));
#102019=CARTESIAN_POINT('Ctrl Pts',(11.1652147157383,70.2386691982902,12.));
#102020=CARTESIAN_POINT('Ctrl Pts',(11.1617508647017,70.2606650418589,0.));
#102021=CARTESIAN_POINT('Ctrl Pts',(11.1617508647017,70.2606650418589,12.));
#102022=CARTESIAN_POINT('Ctrl Pts',(11.1582574356522,70.2827033115662,0.));
#102023=CARTESIAN_POINT('Ctrl Pts',(11.1582574356522,70.2827033115662,12.));
#102024=CARTESIAN_POINT('Ctrl Pts',(11.1547343809647,70.3047838552758,0.));
#102025=CARTESIAN_POINT('Ctrl Pts',(11.1547343809647,70.3047838552758,12.));
#102026=CARTESIAN_POINT('Ctrl Pts',(11.1511816533422,70.3269065215591,0.));
#102027=CARTESIAN_POINT('Ctrl Pts',(11.1511816533422,70.3269065215591,12.));
#102028=CARTESIAN_POINT('Ctrl Pts',(11.1475992058124,70.3490711596882,0.));
#102029=CARTESIAN_POINT('Ctrl Pts',(11.1475992058124,70.3490711596882,12.));
#102030=CARTESIAN_POINT('Ctrl Pts',(11.1439869917269,70.3712776196216,0.));
#102031=CARTESIAN_POINT('Ctrl Pts',(11.1439869917269,70.3712776196216,12.));
#102032=CARTESIAN_POINT('Ctrl Pts',(11.1403449647622,70.3935257519945,0.));
#102033=CARTESIAN_POINT('Ctrl Pts',(11.1403449647622,70.3935257519945,12.));
#102034=CARTESIAN_POINT('Ctrl Pts',(11.1366730789122,70.415815408119,0.));
#102035=CARTESIAN_POINT('Ctrl Pts',(11.1366730789122,70.415815408119,12.));
#102036=CARTESIAN_POINT('Ctrl Pts',(11.1329712884845,70.438146439981,0.));
#102037=CARTESIAN_POINT('Ctrl Pts',(11.1329712884845,70.438146439981,12.));
#102038=CARTESIAN_POINT('Ctrl Pts',(11.1292395480975,70.4605187002356,0.));
#102039=CARTESIAN_POINT('Ctrl Pts',(11.1292395480975,70.4605187002356,12.));
#102040=CARTESIAN_POINT('Ctrl Pts',(11.1254778126824,70.4829320421973,0.));
#102041=CARTESIAN_POINT('Ctrl Pts',(11.1254778126824,70.4829320421973,12.));
#102042=CARTESIAN_POINT('Ctrl Pts',(11.121686037483,70.5053863198306,0.));
#102043=CARTESIAN_POINT('Ctrl Pts',(11.121686037483,70.5053863198306,12.));
#102044=CARTESIAN_POINT('Ctrl Pts',(11.117864178048,70.5278813877519,0.));
#102045=CARTESIAN_POINT('Ctrl Pts',(11.117864178048,70.5278813877519,12.));
#102046=CARTESIAN_POINT('Ctrl Pts',(11.1140121902274,70.5504171012247,0.));
#102047=CARTESIAN_POINT('Ctrl Pts',(11.1140121902274,70.5504171012247,12.));
#102048=CARTESIAN_POINT('Ctrl Pts',(11.11013003017,70.5729933161538,0.));
#102049=CARTESIAN_POINT('Ctrl Pts',(11.11013003017,70.5729933161538,12.));
#102050=CARTESIAN_POINT('Ctrl Pts',(11.1062176543257,70.5956098890744,0.));
#102051=CARTESIAN_POINT('Ctrl Pts',(11.1062176543257,70.5956098890744,12.));
#102052=CARTESIAN_POINT('Ctrl Pts',(11.1022750194439,70.6182666771441,0.));
#102053=CARTESIAN_POINT('Ctrl Pts',(11.1022750194439,70.6182666771441,12.));
#102054=CARTESIAN_POINT('Ctrl Pts',(11.0983020825662,70.6409635381446,0.));
#102055=CARTESIAN_POINT('Ctrl Pts',(11.0983020825662,70.6409635381446,12.));
#102056=CARTESIAN_POINT('Ctrl Pts',(11.0942988010231,70.6637003304768,0.));
#102057=CARTESIAN_POINT('Ctrl Pts',(11.0942988010231,70.6637003304768,12.));
#102058=CARTESIAN_POINT('Ctrl Pts',(11.0902651324325,70.686476913156,0.));
#102059=CARTESIAN_POINT('Ctrl Pts',(11.0902651324325,70.686476913156,12.));
#102060=CARTESIAN_POINT('Ctrl Pts',(11.0862010347022,70.7092931457996,0.));
#102061=CARTESIAN_POINT('Ctrl Pts',(11.0862010347022,70.7092931457996,12.));
#102062=CARTESIAN_POINT('Ctrl Pts',(11.0821064660276,70.7321488886229,0.));
#102063=CARTESIAN_POINT('Ctrl Pts',(11.0821064660276,70.7321488886229,12.));
#102064=CARTESIAN_POINT('Ctrl Pts',(11.0779813848851,70.7550440024422,0.));
#102065=CARTESIAN_POINT('Ctrl Pts',(11.0779813848851,70.7550440024422,12.));
#102066=CARTESIAN_POINT('Ctrl Pts',(11.0738257500292,70.7779783486689,0.));
#102067=CARTESIAN_POINT('Ctrl Pts',(11.0738257500292,70.7779783486689,12.));
#102068=CARTESIAN_POINT('Ctrl Pts',(11.0696395204908,70.8009517893042,0.));
#102069=CARTESIAN_POINT('Ctrl Pts',(11.0696395204908,70.8009517893042,12.));
#102070=CARTESIAN_POINT('Ctrl Pts',(11.0654226555798,70.8239641869266,0.));
#102071=CARTESIAN_POINT('Ctrl Pts',(11.0654226555798,70.8239641869266,12.));
#102072=CARTESIAN_POINT('Ctrl Pts',(11.061175114883,70.847015404688,0.));
#102073=CARTESIAN_POINT('Ctrl Pts',(11.061175114883,70.847015404688,12.));
#102074=CARTESIAN_POINT('Ctrl Pts',(11.0568968582566,70.8701053063158,0.));
#102075=CARTESIAN_POINT('Ctrl Pts',(11.0568968582566,70.8701053063158,12.));
#102076=CARTESIAN_POINT('Ctrl Pts',(11.0525878458242,70.8932337561078,0.));
#102077=CARTESIAN_POINT('Ctrl Pts',(11.0525878458242,70.8932337561078,12.));
#102078=CARTESIAN_POINT('Ctrl Pts',(11.0482480379752,70.9164006189283,0.));
#102079=CARTESIAN_POINT('Ctrl Pts',(11.0482480379752,70.9164006189283,12.));
#102080=CARTESIAN_POINT('Ctrl Pts',(11.0438773953686,70.9396057601953,0.));
#102081=CARTESIAN_POINT('Ctrl Pts',(11.0438773953686,70.9396057601953,12.));
#102082=CARTESIAN_POINT('Ctrl Pts',(11.039475878929,70.9628490458779,0.));
#102083=CARTESIAN_POINT('Ctrl Pts',(11.039475878929,70.9628490458779,12.));
#102084=CARTESIAN_POINT('Ctrl Pts',(11.0350434498408,70.9861303424989,0.));
#102085=CARTESIAN_POINT('Ctrl Pts',(11.0350434498408,70.9861303424989,12.));
#102086=CARTESIAN_POINT('Ctrl Pts',(11.0305800695457,71.0094495171295,0.));
#102087=CARTESIAN_POINT('Ctrl Pts',(11.0305800695457,71.0094495171295,12.));
#102088=CARTESIAN_POINT('Ctrl Pts',(11.0260856997414,71.0328064373849,0.));
#102089=CARTESIAN_POINT('Ctrl Pts',(11.0260856997414,71.0328064373849,12.));
#102090=CARTESIAN_POINT('Ctrl Pts',(11.0215603023854,71.0562009714125,0.));
#102091=CARTESIAN_POINT('Ctrl Pts',(11.0215603023854,71.0562009714125,12.));
#102092=CARTESIAN_POINT('Ctrl Pts',(11.0170038396913,71.0796329878896,0.));
#102093=CARTESIAN_POINT('Ctrl Pts',(11.0170038396913,71.0796329878896,12.));
#102094=CARTESIAN_POINT('Ctrl Pts',(11.0124162741223,71.1031023560243,0.));
#102095=CARTESIAN_POINT('Ctrl Pts',(11.0124162741223,71.1031023560243,12.));
#102096=CARTESIAN_POINT('Ctrl Pts',(11.0077975683895,71.1266089455517,0.));
#102097=CARTESIAN_POINT('Ctrl Pts',(11.0077975683895,71.1266089455517,12.));
#102098=CARTESIAN_POINT('Ctrl Pts',(11.0031476854503,71.1501526267288,0.));
#102099=CARTESIAN_POINT('Ctrl Pts',(11.0031476854503,71.1501526267288,12.));
#102100=CARTESIAN_POINT('Ctrl Pts',(10.9984665885127,71.1737332703248,0.));
#102101=CARTESIAN_POINT('Ctrl Pts',(10.9984665885127,71.1737332703248,12.));
#102102=CARTESIAN_POINT('Ctrl Pts',(10.993754241032,71.1973507476188,0.));
#102103=CARTESIAN_POINT('Ctrl Pts',(10.993754241032,71.1973507476188,12.));
#102104=CARTESIAN_POINT('Ctrl Pts',(10.9890106067038,71.221004930401,0.));
#102105=CARTESIAN_POINT('Ctrl Pts',(10.9890106067038,71.221004930401,12.));
#102106=CARTESIAN_POINT('Ctrl Pts',(10.9842356494627,71.2446956909685,0.));
#102107=CARTESIAN_POINT('Ctrl Pts',(10.9842356494627,71.2446956909685,12.));
#102108=CARTESIAN_POINT('Ctrl Pts',(10.9794293334806,71.2684229021209,0.));
#102109=CARTESIAN_POINT('Ctrl Pts',(10.9794293334806,71.2684229021209,12.));
#102110=CARTESIAN_POINT('Ctrl Pts',(10.9745916231711,71.2921864371499,0.));
#102111=CARTESIAN_POINT('Ctrl Pts',(10.9745916231711,71.2921864371499,12.));
#102112=CARTESIAN_POINT('Ctrl Pts',(10.9697224831862,71.3159861698368,0.));
#102113=CARTESIAN_POINT('Ctrl Pts',(10.9697224831862,71.3159861698368,12.));
#102114=CARTESIAN_POINT('Ctrl Pts',(10.96482187841,71.3398219744547,0.));
#102115=CARTESIAN_POINT('Ctrl Pts',(10.96482187841,71.3398219744547,12.));
#102116=CARTESIAN_POINT('Ctrl Pts',(10.9598897739565,71.3636937257651,0.));
#102117=CARTESIAN_POINT('Ctrl Pts',(10.9598897739565,71.3636937257651,12.));
#102118=CARTESIAN_POINT('Ctrl Pts',(10.954926135169,71.3876012990135,0.));
#102119=CARTESIAN_POINT('Ctrl Pts',(10.954926135169,71.3876012990135,12.));
#102120=CARTESIAN_POINT('Ctrl Pts',(10.9499309276235,71.411544569919,0.));
#102121=CARTESIAN_POINT('Ctrl Pts',(10.9499309276235,71.411544569919,12.));
#102122=CARTESIAN_POINT('Ctrl Pts',(10.9449041171269,71.4355234146718,0.));
#102123=CARTESIAN_POINT('Ctrl Pts',(10.9449041171269,71.4355234146718,12.));
#102124=CARTESIAN_POINT('Ctrl Pts',(10.9398456697095,71.4595377099352,0.));
#102125=CARTESIAN_POINT('Ctrl Pts',(10.9398456697095,71.4595377099352,12.));
#102126=CARTESIAN_POINT('Ctrl Pts',(10.9347555516236,71.4835873328425,0.));
#102127=CARTESIAN_POINT('Ctrl Pts',(10.9347555516236,71.4835873328425,12.));
#102128=CARTESIAN_POINT('Ctrl Pts',(10.9296337293425,71.5076721609936,0.));
#102129=CARTESIAN_POINT('Ctrl Pts',(10.9296337293425,71.5076721609936,12.));
#102130=CARTESIAN_POINT('Ctrl Pts',(10.9244801695642,71.5317920724453,0.));
#102131=CARTESIAN_POINT('Ctrl Pts',(10.9244801695642,71.5317920724453,12.));
#102132=CARTESIAN_POINT('Ctrl Pts',(10.9192948392099,71.5559469457082,0.));
#102133=CARTESIAN_POINT('Ctrl Pts',(10.9192948392099,71.5559469457082,12.));
#102134=CARTESIAN_POINT('Ctrl Pts',(10.9140777054169,71.5801366597479,0.));
#102135=CARTESIAN_POINT('Ctrl Pts',(10.9140777054169,71.5801366597479,12.));
#102136=CARTESIAN_POINT('Ctrl Pts',(10.9088287355364,71.604361093983,0.));
#102137=CARTESIAN_POINT('Ctrl Pts',(10.9088287355364,71.604361093983,12.));
#102138=CARTESIAN_POINT('Ctrl Pts',(10.9035478971329,71.6286201282815,0.));
#102139=CARTESIAN_POINT('Ctrl Pts',(10.9035478971329,71.6286201282815,12.));
#102140=CARTESIAN_POINT('Ctrl Pts',(10.8982351579872,71.6529136429515,0.));
#102141=CARTESIAN_POINT('Ctrl Pts',(10.8982351579872,71.6529136429515,12.));
#102142=CARTESIAN_POINT('Ctrl Pts',(10.8928904860967,71.6772415187382,0.));
#102143=CARTESIAN_POINT('Ctrl Pts',(10.8928904860967,71.6772415187382,12.));
#102144=CARTESIAN_POINT('Ctrl Pts',(10.8875138496674,71.7016036368254,0.));
#102145=CARTESIAN_POINT('Ctrl Pts',(10.8875138496674,71.7016036368254,12.));
#102146=CARTESIAN_POINT('Ctrl Pts',(10.8821052171122,71.7259998788337,0.));
#102147=CARTESIAN_POINT('Ctrl Pts',(10.8821052171122,71.7259998788337,12.));
#102148=CARTESIAN_POINT('Ctrl Pts',(10.8766645570496,71.7504301268177,0.));
#102149=CARTESIAN_POINT('Ctrl Pts',(10.8766645570496,71.7504301268177,12.));
#102150=CARTESIAN_POINT('Ctrl Pts',(10.8711918383071,71.7748942632578,0.));
#102151=CARTESIAN_POINT('Ctrl Pts',(10.8711918383071,71.7748942632578,12.));
#102152=CARTESIAN_POINT('Ctrl Pts',(10.8656870299218,71.7993921710546,0.));
#102153=CARTESIAN_POINT('Ctrl Pts',(10.8656870299218,71.7993921710546,12.));
#102154=CARTESIAN_POINT('Ctrl Pts',(10.860150101133,71.8239237335318,0.));
#102155=CARTESIAN_POINT('Ctrl Pts',(10.860150101133,71.8239237335318,12.));
#102156=CARTESIAN_POINT('Ctrl Pts',(10.8545810213799,71.8484888344335,0.));
#102157=CARTESIAN_POINT('Ctrl Pts',(10.8545810213799,71.8484888344335,12.));
#102158=CARTESIAN_POINT('Ctrl Pts',(10.8489797602998,71.8730873579226,0.));
#102159=CARTESIAN_POINT('Ctrl Pts',(10.8489797602998,71.8730873579226,12.));
#102160=CARTESIAN_POINT('Ctrl Pts',(10.8433462877312,71.8977191885726,0.));
#102161=CARTESIAN_POINT('Ctrl Pts',(10.8433462877312,71.8977191885726,12.));
#102162=CARTESIAN_POINT('Ctrl Pts',(10.8376805737158,71.9223842113622,0.));
#102163=CARTESIAN_POINT('Ctrl Pts',(10.8376805737158,71.9223842113622,12.));
#102164=CARTESIAN_POINT('Ctrl Pts',(10.8319825884917,71.9470823116777,0.));
#102165=CARTESIAN_POINT('Ctrl Pts',(10.8319825884917,71.9470823116777,12.));
#102166=CARTESIAN_POINT('Ctrl Pts',(10.8262523024897,71.971813375312,0.));
#102167=CARTESIAN_POINT('Ctrl Pts',(10.8262523024897,71.971813375312,12.));
#102168=CARTESIAN_POINT('Ctrl Pts',(10.8204896863328,71.996577288462,0.));
#102169=CARTESIAN_POINT('Ctrl Pts',(10.8204896863328,71.996577288462,12.));
#102170=CARTESIAN_POINT('Ctrl Pts',(10.8146947108376,72.0213739377231,0.));
#102171=CARTESIAN_POINT('Ctrl Pts',(10.8146947108376,72.0213739377231,12.));
#102172=CARTESIAN_POINT('Ctrl Pts',(10.8088673470187,72.0462032100828,0.));
#102173=CARTESIAN_POINT('Ctrl Pts',(10.8088673470187,72.0462032100828,12.));
#102174=CARTESIAN_POINT('Ctrl Pts',(10.8030075660811,72.0710649929214,0.));
#102175=CARTESIAN_POINT('Ctrl Pts',(10.8030075660811,72.0710649929214,12.));
#102176=CARTESIAN_POINT('Ctrl Pts',(10.7971153394168,72.095959174012,0.));
#102177=CARTESIAN_POINT('Ctrl Pts',(10.7971153394168,72.095959174012,12.));
#102178=CARTESIAN_POINT('Ctrl Pts',(10.7911906386027,72.1208856415171,0.));
#102179=CARTESIAN_POINT('Ctrl Pts',(10.7911906386027,72.1208856415171,12.));
#102180=CARTESIAN_POINT('Ctrl Pts',(10.7852334354015,72.145844283983,0.));
#102181=CARTESIAN_POINT('Ctrl Pts',(10.7852334354015,72.145844283983,12.));
#102182=CARTESIAN_POINT('Ctrl Pts',(10.779243701766,72.17083499033,0.));
#102183=CARTESIAN_POINT('Ctrl Pts',(10.779243701766,72.17083499033,12.));
#102184=CARTESIAN_POINT('Ctrl Pts',(10.7732214098343,72.1958576498556,0.));
#102185=CARTESIAN_POINT('Ctrl Pts',(10.7732214098343,72.1958576498556,12.));
#102186=CARTESIAN_POINT('Ctrl Pts',(10.7671665319254,72.2209121522367,0.));
#102187=CARTESIAN_POINT('Ctrl Pts',(10.7671665319254,72.2209121522367,12.));
#102188=CARTESIAN_POINT('Ctrl Pts',(10.7610790405385,72.2459983875298,0.));
#102189=CARTESIAN_POINT('Ctrl Pts',(10.7610790405385,72.2459983875298,12.));
#102190=CARTESIAN_POINT('Ctrl Pts',(10.7549589083535,72.2711162461679,0.));
#102191=CARTESIAN_POINT('Ctrl Pts',(10.7549589083535,72.2711162461679,12.));
#102192=CARTESIAN_POINT('Ctrl Pts',(10.7488061082368,72.296265618955,0.));
#102193=CARTESIAN_POINT('Ctrl Pts',(10.7488061082368,72.296265618955,12.));
#102194=CARTESIAN_POINT('Ctrl Pts',(10.7426206132375,72.3214463970634,0.));
#102195=CARTESIAN_POINT('Ctrl Pts',(10.7426206132375,72.3214463970634,12.));
#102196=CARTESIAN_POINT('Ctrl Pts',(10.73640239658,72.3466584720311,0.));
#102197=CARTESIAN_POINT('Ctrl Pts',(10.73640239658,72.3466584720311,12.));
#102198=CARTESIAN_POINT('Ctrl Pts',(10.7301514316607,72.3719017357568,0.));
#102199=CARTESIAN_POINT('Ctrl Pts',(10.7301514316607,72.3719017357568,12.));
#102200=CARTESIAN_POINT('Ctrl Pts',(10.7238676920469,72.3971760804935,0.));
#102201=CARTESIAN_POINT('Ctrl Pts',(10.7238676920469,72.3971760804935,12.));
#102202=CARTESIAN_POINT('Ctrl Pts',(10.7175511514789,72.4224813988355,0.));
#102203=CARTESIAN_POINT('Ctrl Pts',(10.7175511514789,72.4224813988355,12.));
#102204=CARTESIAN_POINT('Ctrl Pts',(10.7112017838707,72.4478175837168,0.));
#102205=CARTESIAN_POINT('Ctrl Pts',(10.7112017838707,72.4478175837168,12.));
#102206=CARTESIAN_POINT('Ctrl Pts',(10.7048195633062,72.4731845284238,0.));
#102207=CARTESIAN_POINT('Ctrl Pts',(10.7048195633062,72.4731845284238,12.));
#102208=CARTESIAN_POINT('Ctrl Pts',(10.6984044640399,72.4985821266031,0.));
#102209=CARTESIAN_POINT('Ctrl Pts',(10.6984044640399,72.4985821266031,12.));
#102210=CARTESIAN_POINT('Ctrl Pts',(10.691956460499,72.5240102722662,0.));
#102211=CARTESIAN_POINT('Ctrl Pts',(10.691956460499,72.5240102722662,12.));
#102212=CARTESIAN_POINT('Ctrl Pts',(10.6854755272903,72.5494688597951,0.));
#102213=CARTESIAN_POINT('Ctrl Pts',(10.6854755272903,72.5494688597951,12.));
#102214=CARTESIAN_POINT('Ctrl Pts',(10.6789616392041,72.57495778394,0.));
#102215=CARTESIAN_POINT('Ctrl Pts',(10.6789616392041,72.57495778394,12.));
#102216=CARTESIAN_POINT('Ctrl Pts',(10.6724147711994,72.6004769398004,0.));
#102217=CARTESIAN_POINT('Ctrl Pts',(10.6724147711994,72.6004769398004,12.));
#102218=CARTESIAN_POINT('Ctrl Pts',(10.6658348983944,72.6260262228055,0.));
#102219=CARTESIAN_POINT('Ctrl Pts',(10.6658348983944,72.6260262228055,12.));
#102220=CARTESIAN_POINT('Ctrl Pts',(10.659221996058,72.6516055286908,0.));
#102221=CARTESIAN_POINT('Ctrl Pts',(10.659221996058,72.6516055286908,12.));
#102222=CARTESIAN_POINT('Ctrl Pts',(10.6525760396055,72.6772147534762,0.));
#102223=CARTESIAN_POINT('Ctrl Pts',(10.6525760396055,72.6772147534762,12.));
#102224=CARTESIAN_POINT('Ctrl Pts',(10.6458970045948,72.7028537934332,0.));
#102225=CARTESIAN_POINT('Ctrl Pts',(10.6458970045948,72.7028537934332,12.));
#102226=CARTESIAN_POINT('Ctrl Pts',(10.6391848667354,72.7285225451309,0.));
#102227=CARTESIAN_POINT('Ctrl Pts',(10.6391848667354,72.7285225451309,12.));
#102228=CARTESIAN_POINT('Ctrl Pts',(10.6324396018999,72.7542209054823,0.));
#102229=CARTESIAN_POINT('Ctrl Pts',(10.6324396018999,72.7542209054823,12.));
#102230=CARTESIAN_POINT('Ctrl Pts',(10.6256611861395,72.7799487717914,0.));
#102231=CARTESIAN_POINT('Ctrl Pts',(10.6256611861395,72.7799487717914,12.));
#102232=CARTESIAN_POINT('Ctrl Pts',(10.6188495956973,72.8057060417882,0.));
#102233=CARTESIAN_POINT('Ctrl Pts',(10.6188495956973,72.8057060417882,12.));
#102234=CARTESIAN_POINT('Ctrl Pts',(10.6120048070366,72.8314926136872,0.));
#102235=CARTESIAN_POINT('Ctrl Pts',(10.6120048070366,72.8314926136872,12.));
#102236=CARTESIAN_POINT('Ctrl Pts',(10.6051267968202,72.8573083861328,0.));
#102237=CARTESIAN_POINT('Ctrl Pts',(10.6051267968202,72.8573083861328,12.));
#102238=CARTESIAN_POINT('Ctrl Pts',(10.5982155418625,72.8831532580839,0.));
#102239=CARTESIAN_POINT('Ctrl Pts',(10.5982155418625,72.8831532580839,12.));
#102240=CARTESIAN_POINT('Ctrl Pts',(10.5912710190928,72.9090271287081,0.));
#102241=CARTESIAN_POINT('Ctrl Pts',(10.5912710190928,72.9090271287081,12.));
#102242=CARTESIAN_POINT('Ctrl Pts',(10.5842932055209,72.9349298972823,0.));
#102243=CARTESIAN_POINT('Ctrl Pts',(10.5842932055209,72.9349298972823,12.));
#102244=CARTESIAN_POINT('Ctrl Pts',(10.5772820781959,72.9608614630539,0.));
#102245=CARTESIAN_POINT('Ctrl Pts',(10.5772820781959,72.9608614630539,12.));
#102246=CARTESIAN_POINT('Ctrl Pts',(10.5702376142052,72.9868217252293,0.));
#102247=CARTESIAN_POINT('Ctrl Pts',(10.5702376142052,72.9868217252293,12.));
#102248=CARTESIAN_POINT('Ctrl Pts',(10.5631597907653,73.0128105832635,0.));
#102249=CARTESIAN_POINT('Ctrl Pts',(10.5631597907653,73.0128105832635,12.));
#102250=CARTESIAN_POINT('Ctrl Pts',(10.5560485852975,73.0388279370845,0.));
#102251=CARTESIAN_POINT('Ctrl Pts',(10.5560485852975,73.0388279370845,12.));
#102252=CARTESIAN_POINT('Ctrl Pts',(10.5489039755138,73.0648736873435,0.));
#102253=CARTESIAN_POINT('Ctrl Pts',(10.5489039755138,73.0648736873435,12.));
#102254=CARTESIAN_POINT('Ctrl Pts',(10.5417259395001,73.090947735646,0.));
#102255=CARTESIAN_POINT('Ctrl Pts',(10.5417259395001,73.090947735646,12.));
#102256=CARTESIAN_POINT('Ctrl Pts',(10.5345144558097,73.1170499848012,0.));
#102257=CARTESIAN_POINT('Ctrl Pts',(10.5345144558097,73.1170499848012,12.));
#102258=CARTESIAN_POINT('Ctrl Pts',(10.5272695032649,73.1431803382677,0.));
#102259=CARTESIAN_POINT('Ctrl Pts',(10.5272695032649,73.1431803382677,12.));
#102260=CARTESIAN_POINT('Ctrl Pts',(10.5199910607652,73.169338699611,0.));
#102261=CARTESIAN_POINT('Ctrl Pts',(10.5199910607652,73.169338699611,12.));
#102262=CARTESIAN_POINT('Ctrl Pts',(10.5126791070804,73.1955249719037,0.));
#102263=CARTESIAN_POINT('Ctrl Pts',(10.5126791070804,73.1955249719037,12.));
#102264=CARTESIAN_POINT('Ctrl Pts',(10.505333620691,73.2217390572578,0.));
#102265=CARTESIAN_POINT('Ctrl Pts',(10.505333620691,73.2217390572578,12.));
#102266=CARTESIAN_POINT('Ctrl Pts',(10.4979545795197,73.247980856023,0.));
#102267=CARTESIAN_POINT('Ctrl Pts',(10.4979545795197,73.247980856023,12.));
#102268=CARTESIAN_POINT('Ctrl Pts',(10.4905419611529,73.2742502674361,0.));
#102269=CARTESIAN_POINT('Ctrl Pts',(10.4905419611529,73.2742502674361,12.));
#102270=CARTESIAN_POINT('Ctrl Pts',(10.4830957433311,73.3005471910639,0.));
#102271=CARTESIAN_POINT('Ctrl Pts',(10.4830957433311,73.3005471910639,12.));
#102272=CARTESIAN_POINT('Ctrl Pts',(10.475615904381,73.3268715280609,0.));
#102273=CARTESIAN_POINT('Ctrl Pts',(10.475615904381,73.3268715280609,12.));
#102274=CARTESIAN_POINT('Ctrl Pts',(10.4681024236288,73.353223182365,0.));
#102275=CARTESIAN_POINT('Ctrl Pts',(10.4681024236288,73.353223182365,12.));
#102276=CARTESIAN_POINT('Ctrl Pts',(10.4605552819391,73.3796020622437,0.));
#102277=CARTESIAN_POINT('Ctrl Pts',(10.4605552819391,73.3796020622437,12.));
#102278=CARTESIAN_POINT('Ctrl Pts',(10.4529744618438,73.4060080806578,0.));
#102279=CARTESIAN_POINT('Ctrl Pts',(10.4529744618438,73.4060080806578,12.));
#102280=CARTESIAN_POINT('Ctrl Pts',(10.4453599463534,73.432441151843,0.));
#102281=CARTESIAN_POINT('Ctrl Pts',(10.4453599463534,73.432441151843,12.));
#102282=CARTESIAN_POINT('Ctrl Pts',(10.4377117180212,73.45890118861,0.));
#102283=CARTESIAN_POINT('Ctrl Pts',(10.4377117180212,73.45890118861,12.));
#102284=CARTESIAN_POINT('Ctrl Pts',(10.4300297578648,73.4853880992228,0.));
#102285=CARTESIAN_POINT('Ctrl Pts',(10.4300297578648,73.4853880992228,12.));
#102286=CARTESIAN_POINT('Ctrl Pts',(10.4223140444615,73.5119017847664,0.));
#102287=CARTESIAN_POINT('Ctrl Pts',(10.4223140444615,73.5119017847664,12.));
#102288=CARTESIAN_POINT('Ctrl Pts',(10.4145645526832,73.5384421354746,0.));
#102289=CARTESIAN_POINT('Ctrl Pts',(10.4145645526832,73.5384421354746,12.));
#102290=CARTESIAN_POINT('Ctrl Pts',(10.4067812555539,73.5650090360114,0.));
#102291=CARTESIAN_POINT('Ctrl Pts',(10.4067812555539,73.5650090360114,12.));
#102292=CARTESIAN_POINT('Ctrl Pts',(10.3989641265313,73.5916023719976,0.));
#102293=CARTESIAN_POINT('Ctrl Pts',(10.3989641265313,73.5916023719976,12.));
#102294=CARTESIAN_POINT('Ctrl Pts',(10.3911131417478,73.6182220363295,0.));
#102295=CARTESIAN_POINT('Ctrl Pts',(10.3911131417478,73.6182220363295,12.));
#102296=CARTESIAN_POINT('Ctrl Pts',(10.3832282820362,73.6448679350605,0.));
#102297=CARTESIAN_POINT('Ctrl Pts',(10.3832282820362,73.6448679350605,12.));
#102298=CARTESIAN_POINT('Ctrl Pts',(10.3753095356302,73.6715399947459,0.));
#102299=CARTESIAN_POINT('Ctrl Pts',(10.3753095356302,73.6715399947459,12.));
#102300=CARTESIAN_POINT('Ctrl Pts',(10.3673568984515,73.6982381644571,0.));
#102301=CARTESIAN_POINT('Ctrl Pts',(10.3673568984515,73.6982381644571,12.));
#102302=CARTESIAN_POINT('Ctrl Pts',(10.3593703712542,73.7249624108433,0.));
#102303=CARTESIAN_POINT('Ctrl Pts',(10.3593703712542,73.7249624108433,12.));
#102304=CARTESIAN_POINT('Ctrl Pts',(10.3529540403026,73.7463626541235,0.));
#102305=CARTESIAN_POINT('Ctrl Pts',(10.3529540403026,73.7463626541235,12.));
#102306=CARTESIAN_POINT('Ctrl Pts',(10.3481265449303,73.7624245587416,0.));
#102307=CARTESIAN_POINT('Ctrl Pts',(10.3481265449303,73.7624245587416,12.));
#102308=CARTESIAN_POINT('Ctrl Pts',(10.3449014384439,73.7731377047922,0.));
#102309=CARTESIAN_POINT('Ctrl Pts',(10.3449014384439,73.7731377047922,12.));
#102310=CARTESIAN_POINT('Ctrl Pts',(10.343287191141,73.778495580227,0.));
#102311=CARTESIAN_POINT('Ctrl Pts',(10.343287191141,73.778495580227,12.));
#102312=CARTESIAN_POINT('',(11.3136138754165,69.079679653846,0.));
#102313=CARTESIAN_POINT('Ctrl Pts',(11.3136138754165,69.079679653846,0.));
#102314=CARTESIAN_POINT('Ctrl Pts',(11.3132375200165,69.0835449954396,0.));
#102315=CARTESIAN_POINT('Ctrl Pts',(11.3124821678798,69.0912808656811,0.));
#102316=CARTESIAN_POINT('Ctrl Pts',(11.3113412156661,69.1029002322118,0.));
#102317=CARTESIAN_POINT('Ctrl Pts',(11.3098040973713,69.118423844466,0.));
#102318=CARTESIAN_POINT('Ctrl Pts',(11.3078562764384,69.1378802251711,0.));
#102319=CARTESIAN_POINT('Ctrl Pts',(11.3058820128307,69.1573884361,0.));
#102320=CARTESIAN_POINT('Ctrl Pts',(11.3038812726292,69.1769483991721,0.));
#102321=CARTESIAN_POINT('Ctrl Pts',(11.3018540025638,69.1965599718914,0.));
#102322=CARTESIAN_POINT('Ctrl Pts',(11.2998001310964,69.2162229488531,0.));
#102323=CARTESIAN_POINT('Ctrl Pts',(11.2977195764852,69.2359370894907,0.));
#102324=CARTESIAN_POINT('Ctrl Pts',(11.2956122531375,69.2557021393351,0.));
#102325=CARTESIAN_POINT('Ctrl Pts',(11.2934780784351,69.275517853148,0.));
#102326=CARTESIAN_POINT('Ctrl Pts',(11.2913169799628,69.295384019272,0.));
#102327=CARTESIAN_POINT('Ctrl Pts',(11.2891288931517,69.3153004517783,0.));
#102328=CARTESIAN_POINT('Ctrl Pts',(11.2869137578459,69.3352669789587,0.));
#102329=CARTESIAN_POINT('Ctrl Pts',(11.2846715154524,69.3552834337784,0.));
#102330=CARTESIAN_POINT('Ctrl Pts',(11.2824021054045,69.3753496420039,0.));
#102331=CARTESIAN_POINT('Ctrl Pts',(11.2801054633816,69.3954654162281,0.));
#102332=CARTESIAN_POINT('Ctrl Pts',(11.2777815231469,69.4156305620593,0.));
#102333=CARTESIAN_POINT('Ctrl Pts',(11.2754302177021,69.4358448819967,0.));
#102334=CARTESIAN_POINT('Ctrl Pts',(11.2730514806139,69.456108179879,0.));
#102335=CARTESIAN_POINT('Ctrl Pts',(11.270645247528,69.4764202659397,0.));
#102336=CARTESIAN_POINT('Ctrl Pts',(11.2682114561008,69.4967809565929,0.));
#102337=CARTESIAN_POINT('Ctrl Pts',(11.2657500452716,69.5171900720158,0.));
#102338=CARTESIAN_POINT('Ctrl Pts',(11.263260954763,69.5376474344771,0.));
#102339=CARTESIAN_POINT('Ctrl Pts',(11.2607441244703,69.5581528662877,0.));
#102340=CARTESIAN_POINT('Ctrl Pts',(11.2581994939541,69.5787061880857,0.));
#102341=CARTESIAN_POINT('Ctrl Pts',(11.2556270027016,69.599307219739,0.));
#102342=CARTESIAN_POINT('Ctrl Pts',(11.2530265903557,69.6199557811245,0.));
#102343=CARTESIAN_POINT('Ctrl Pts',(11.2503981969412,69.6406516928891,0.));
#102344=CARTESIAN_POINT('Ctrl Pts',(11.2477417631386,69.6613947773534,0.));
#102345=CARTESIAN_POINT('Ctrl Pts',(11.2450572303841,69.6821848588457,0.));
#102346=CARTESIAN_POINT('Ctrl Pts',(11.2423445407166,69.7030217632164,0.));
#102347=CARTESIAN_POINT('Ctrl Pts',(11.239603636686,69.7239053175356,0.));
#102348=CARTESIAN_POINT('Ctrl Pts',(11.2368344612472,69.7448353497408,0.));
#102349=CARTESIAN_POINT('Ctrl Pts',(11.2340369576456,69.7658116882324,0.));
#102350=CARTESIAN_POINT('Ctrl Pts',(11.2312110694187,69.7868341618954,0.));
#102351=CARTESIAN_POINT('Ctrl Pts',(11.2283567404437,69.8079026002768,0.));
#102352=CARTESIAN_POINT('Ctrl Pts',(11.225473914972,69.8290168337076,0.));
#102353=CARTESIAN_POINT('Ctrl Pts',(11.2225625376736,69.8501766934428,0.));
#102354=CARTESIAN_POINT('Ctrl Pts',(11.219622553679,69.871382011789,0.));
#102355=CARTESIAN_POINT('Ctrl Pts',(11.2166539085523,69.8926326220385,0.));
#102356=CARTESIAN_POINT('Ctrl Pts',(11.2136565482678,69.9139283584022,0.));
#102357=CARTESIAN_POINT('Ctrl Pts',(11.2106304191882,69.9352690559405,0.));
#102358=CARTESIAN_POINT('Ctrl Pts',(11.2075754680449,69.9566545504837,0.));
#102359=CARTESIAN_POINT('Ctrl Pts',(11.2044916419244,69.97808467858,0.));
#102360=CARTESIAN_POINT('Ctrl Pts',(11.2013788882714,69.9995592775343,0.));
#102361=CARTESIAN_POINT('Ctrl Pts',(11.1982371548919,70.0210781854243,0.));
#102362=CARTESIAN_POINT('Ctrl Pts',(11.1950663899576,70.0426412411185,0.));
#102363=CARTESIAN_POINT('Ctrl Pts',(11.1918665420166,70.0642482842928,0.));
#102364=CARTESIAN_POINT('Ctrl Pts',(11.1886375599914,70.0858991554283,0.));
#102365=CARTESIAN_POINT('Ctrl Pts',(11.185379393167,70.1075936957968,0.));
#102366=CARTESIAN_POINT('Ctrl Pts',(11.1820919911846,70.1293317474432,0.));
#102367=CARTESIAN_POINT('Ctrl Pts',(11.1787753040363,70.1511131531674,0.));
#102368=CARTESIAN_POINT('Ctrl Pts',(11.1754292820631,70.1729377564956,0.));
#102369=CARTESIAN_POINT('Ctrl Pts',(11.1720538759499,70.1948054016817,0.));
#102370=CARTESIAN_POINT('Ctrl Pts',(11.168649036721,70.2167159337095,0.));
#102371=CARTESIAN_POINT('Ctrl Pts',(11.1652147157383,70.2386691982902,0.));
#102372=CARTESIAN_POINT('Ctrl Pts',(11.1617508647017,70.2606650418589,0.));
#102373=CARTESIAN_POINT('Ctrl Pts',(11.1582574356522,70.2827033115662,0.));
#102374=CARTESIAN_POINT('Ctrl Pts',(11.1547343809647,70.3047838552758,0.));
#102375=CARTESIAN_POINT('Ctrl Pts',(11.1511816533422,70.3269065215591,0.));
#102376=CARTESIAN_POINT('Ctrl Pts',(11.1475992058124,70.3490711596882,0.));
#102377=CARTESIAN_POINT('Ctrl Pts',(11.1439869917269,70.3712776196216,0.));
#102378=CARTESIAN_POINT('Ctrl Pts',(11.1403449647622,70.3935257519945,0.));
#102379=CARTESIAN_POINT('Ctrl Pts',(11.1366730789122,70.415815408119,0.));
#102380=CARTESIAN_POINT('Ctrl Pts',(11.1329712884845,70.438146439981,0.));
#102381=CARTESIAN_POINT('Ctrl Pts',(11.1292395480975,70.4605187002356,0.));
#102382=CARTESIAN_POINT('Ctrl Pts',(11.1254778126824,70.4829320421973,0.));
#102383=CARTESIAN_POINT('Ctrl Pts',(11.121686037483,70.5053863198306,0.));
#102384=CARTESIAN_POINT('Ctrl Pts',(11.117864178048,70.5278813877519,0.));
#102385=CARTESIAN_POINT('Ctrl Pts',(11.1140121902274,70.5504171012247,0.));
#102386=CARTESIAN_POINT('Ctrl Pts',(11.11013003017,70.5729933161538,0.));
#102387=CARTESIAN_POINT('Ctrl Pts',(11.1062176543257,70.5956098890744,0.));
#102388=CARTESIAN_POINT('Ctrl Pts',(11.1022750194439,70.6182666771441,0.));
#102389=CARTESIAN_POINT('Ctrl Pts',(11.0983020825662,70.6409635381446,0.));
#102390=CARTESIAN_POINT('Ctrl Pts',(11.0942988010231,70.6637003304768,0.));
#102391=CARTESIAN_POINT('Ctrl Pts',(11.0902651324325,70.686476913156,0.));
#102392=CARTESIAN_POINT('Ctrl Pts',(11.0862010347022,70.7092931457996,0.));
#102393=CARTESIAN_POINT('Ctrl Pts',(11.0821064660276,70.7321488886229,0.));
#102394=CARTESIAN_POINT('Ctrl Pts',(11.0779813848851,70.7550440024422,0.));
#102395=CARTESIAN_POINT('Ctrl Pts',(11.0738257500292,70.7779783486689,0.));
#102396=CARTESIAN_POINT('Ctrl Pts',(11.0696395204908,70.8009517893042,0.));
#102397=CARTESIAN_POINT('Ctrl Pts',(11.0654226555798,70.8239641869266,0.));
#102398=CARTESIAN_POINT('Ctrl Pts',(11.061175114883,70.847015404688,0.));
#102399=CARTESIAN_POINT('Ctrl Pts',(11.0568968582566,70.8701053063158,0.));
#102400=CARTESIAN_POINT('Ctrl Pts',(11.0525878458242,70.8932337561078,0.));
#102401=CARTESIAN_POINT('Ctrl Pts',(11.0482480379752,70.9164006189283,0.));
#102402=CARTESIAN_POINT('Ctrl Pts',(11.0438773953686,70.9396057601953,0.));
#102403=CARTESIAN_POINT('Ctrl Pts',(11.039475878929,70.9628490458779,0.));
#102404=CARTESIAN_POINT('Ctrl Pts',(11.0350434498408,70.9861303424989,0.));
#102405=CARTESIAN_POINT('Ctrl Pts',(11.0305800695457,71.0094495171295,0.));
#102406=CARTESIAN_POINT('Ctrl Pts',(11.0260856997414,71.0328064373849,0.));
#102407=CARTESIAN_POINT('Ctrl Pts',(11.0215603023854,71.0562009714125,0.));
#102408=CARTESIAN_POINT('Ctrl Pts',(11.0170038396913,71.0796329878896,0.));
#102409=CARTESIAN_POINT('Ctrl Pts',(11.0124162741223,71.1031023560243,0.));
#102410=CARTESIAN_POINT('Ctrl Pts',(11.0077975683895,71.1266089455517,0.));
#102411=CARTESIAN_POINT('Ctrl Pts',(11.0031476854503,71.1501526267288,0.));
#102412=CARTESIAN_POINT('Ctrl Pts',(10.9984665885127,71.1737332703248,0.));
#102413=CARTESIAN_POINT('Ctrl Pts',(10.993754241032,71.1973507476188,0.));
#102414=CARTESIAN_POINT('Ctrl Pts',(10.9890106067038,71.221004930401,0.));
#102415=CARTESIAN_POINT('Ctrl Pts',(10.9842356494627,71.2446956909685,0.));
#102416=CARTESIAN_POINT('Ctrl Pts',(10.9794293334806,71.2684229021209,0.));
#102417=CARTESIAN_POINT('Ctrl Pts',(10.9745916231711,71.2921864371499,0.));
#102418=CARTESIAN_POINT('Ctrl Pts',(10.9697224831862,71.3159861698368,0.));
#102419=CARTESIAN_POINT('Ctrl Pts',(10.96482187841,71.3398219744547,0.));
#102420=CARTESIAN_POINT('Ctrl Pts',(10.9598897739565,71.3636937257651,0.));
#102421=CARTESIAN_POINT('Ctrl Pts',(10.954926135169,71.3876012990135,0.));
#102422=CARTESIAN_POINT('Ctrl Pts',(10.9499309276235,71.411544569919,0.));
#102423=CARTESIAN_POINT('Ctrl Pts',(10.9449041171269,71.4355234146718,0.));
#102424=CARTESIAN_POINT('Ctrl Pts',(10.9398456697095,71.4595377099352,0.));
#102425=CARTESIAN_POINT('Ctrl Pts',(10.9347555516236,71.4835873328425,0.));
#102426=CARTESIAN_POINT('Ctrl Pts',(10.9296337293425,71.5076721609936,0.));
#102427=CARTESIAN_POINT('Ctrl Pts',(10.9244801695642,71.5317920724453,0.));
#102428=CARTESIAN_POINT('Ctrl Pts',(10.9192948392099,71.5559469457082,0.));
#102429=CARTESIAN_POINT('Ctrl Pts',(10.9140777054169,71.5801366597479,0.));
#102430=CARTESIAN_POINT('Ctrl Pts',(10.9088287355364,71.604361093983,0.));
#102431=CARTESIAN_POINT('Ctrl Pts',(10.9035478971329,71.6286201282815,0.));
#102432=CARTESIAN_POINT('Ctrl Pts',(10.8982351579872,71.6529136429515,0.));
#102433=CARTESIAN_POINT('Ctrl Pts',(10.8928904860967,71.6772415187382,0.));
#102434=CARTESIAN_POINT('Ctrl Pts',(10.8875138496674,71.7016036368254,0.));
#102435=CARTESIAN_POINT('Ctrl Pts',(10.8821052171122,71.7259998788337,0.));
#102436=CARTESIAN_POINT('Ctrl Pts',(10.8766645570496,71.7504301268177,0.));
#102437=CARTESIAN_POINT('Ctrl Pts',(10.8711918383071,71.7748942632578,0.));
#102438=CARTESIAN_POINT('Ctrl Pts',(10.8656870299218,71.7993921710546,0.));
#102439=CARTESIAN_POINT('Ctrl Pts',(10.860150101133,71.8239237335318,0.));
#102440=CARTESIAN_POINT('Ctrl Pts',(10.8545810213799,71.8484888344335,0.));
#102441=CARTESIAN_POINT('Ctrl Pts',(10.8489797602998,71.8730873579226,0.));
#102442=CARTESIAN_POINT('Ctrl Pts',(10.8433462877312,71.8977191885726,0.));
#102443=CARTESIAN_POINT('Ctrl Pts',(10.8376805737158,71.9223842113622,0.));
#102444=CARTESIAN_POINT('Ctrl Pts',(10.8319825884917,71.9470823116777,0.));
#102445=CARTESIAN_POINT('Ctrl Pts',(10.8262523024897,71.971813375312,0.));
#102446=CARTESIAN_POINT('Ctrl Pts',(10.8204896863328,71.996577288462,0.));
#102447=CARTESIAN_POINT('Ctrl Pts',(10.8146947108376,72.0213739377231,0.));
#102448=CARTESIAN_POINT('Ctrl Pts',(10.8088673470187,72.0462032100828,0.));
#102449=CARTESIAN_POINT('Ctrl Pts',(10.8030075660811,72.0710649929214,0.));
#102450=CARTESIAN_POINT('Ctrl Pts',(10.7971153394168,72.095959174012,0.));
#102451=CARTESIAN_POINT('Ctrl Pts',(10.7911906386027,72.1208856415171,0.));
#102452=CARTESIAN_POINT('Ctrl Pts',(10.7852334354015,72.145844283983,0.));
#102453=CARTESIAN_POINT('Ctrl Pts',(10.779243701766,72.17083499033,0.));
#102454=CARTESIAN_POINT('Ctrl Pts',(10.7732214098343,72.1958576498556,0.));
#102455=CARTESIAN_POINT('Ctrl Pts',(10.7671665319254,72.2209121522367,0.));
#102456=CARTESIAN_POINT('Ctrl Pts',(10.7610790405385,72.2459983875298,0.));
#102457=CARTESIAN_POINT('Ctrl Pts',(10.7549589083535,72.2711162461679,0.));
#102458=CARTESIAN_POINT('Ctrl Pts',(10.7488061082368,72.296265618955,0.));
#102459=CARTESIAN_POINT('Ctrl Pts',(10.7426206132375,72.3214463970634,0.));
#102460=CARTESIAN_POINT('Ctrl Pts',(10.73640239658,72.3466584720311,0.));
#102461=CARTESIAN_POINT('Ctrl Pts',(10.7301514316607,72.3719017357568,0.));
#102462=CARTESIAN_POINT('Ctrl Pts',(10.7238676920469,72.3971760804935,0.));
#102463=CARTESIAN_POINT('Ctrl Pts',(10.7175511514789,72.4224813988355,0.));
#102464=CARTESIAN_POINT('Ctrl Pts',(10.7112017838707,72.4478175837168,0.));
#102465=CARTESIAN_POINT('Ctrl Pts',(10.7048195633062,72.4731845284238,0.));
#102466=CARTESIAN_POINT('Ctrl Pts',(10.6984044640399,72.4985821266031,0.));
#102467=CARTESIAN_POINT('Ctrl Pts',(10.691956460499,72.5240102722662,0.));
#102468=CARTESIAN_POINT('Ctrl Pts',(10.6854755272903,72.5494688597951,0.));
#102469=CARTESIAN_POINT('Ctrl Pts',(10.6789616392041,72.57495778394,0.));
#102470=CARTESIAN_POINT('Ctrl Pts',(10.6724147711994,72.6004769398004,0.));
#102471=CARTESIAN_POINT('Ctrl Pts',(10.6658348983944,72.6260262228055,0.));
#102472=CARTESIAN_POINT('Ctrl Pts',(10.659221996058,72.6516055286908,0.));
#102473=CARTESIAN_POINT('Ctrl Pts',(10.6525760396055,72.6772147534762,0.));
#102474=CARTESIAN_POINT('Ctrl Pts',(10.6458970045948,72.7028537934332,0.));
#102475=CARTESIAN_POINT('Ctrl Pts',(10.6391848667354,72.7285225451309,0.));
#102476=CARTESIAN_POINT('Ctrl Pts',(10.6324396018999,72.7542209054823,0.));
#102477=CARTESIAN_POINT('Ctrl Pts',(10.6256611861395,72.7799487717914,0.));
#102478=CARTESIAN_POINT('Ctrl Pts',(10.6188495956973,72.8057060417882,0.));
#102479=CARTESIAN_POINT('Ctrl Pts',(10.6120048070366,72.8314926136872,0.));
#102480=CARTESIAN_POINT('Ctrl Pts',(10.6051267968202,72.8573083861328,0.));
#102481=CARTESIAN_POINT('Ctrl Pts',(10.5982155418625,72.8831532580839,0.));
#102482=CARTESIAN_POINT('Ctrl Pts',(10.5912710190928,72.9090271287081,0.));
#102483=CARTESIAN_POINT('Ctrl Pts',(10.5842932055209,72.9349298972823,0.));
#102484=CARTESIAN_POINT('Ctrl Pts',(10.5772820781959,72.9608614630539,0.));
#102485=CARTESIAN_POINT('Ctrl Pts',(10.5702376142052,72.9868217252293,0.));
#102486=CARTESIAN_POINT('Ctrl Pts',(10.5631597907653,73.0128105832635,0.));
#102487=CARTESIAN_POINT('Ctrl Pts',(10.5560485852975,73.0388279370845,0.));
#102488=CARTESIAN_POINT('Ctrl Pts',(10.5489039755138,73.0648736873435,0.));
#102489=CARTESIAN_POINT('Ctrl Pts',(10.5417259395001,73.090947735646,0.));
#102490=CARTESIAN_POINT('Ctrl Pts',(10.5345144558097,73.1170499848012,0.));
#102491=CARTESIAN_POINT('Ctrl Pts',(10.5272695032649,73.1431803382677,0.));
#102492=CARTESIAN_POINT('Ctrl Pts',(10.5199910607652,73.169338699611,0.));
#102493=CARTESIAN_POINT('Ctrl Pts',(10.5126791070804,73.1955249719037,0.));
#102494=CARTESIAN_POINT('Ctrl Pts',(10.505333620691,73.2217390572578,0.));
#102495=CARTESIAN_POINT('Ctrl Pts',(10.4979545795197,73.247980856023,0.));
#102496=CARTESIAN_POINT('Ctrl Pts',(10.4905419611529,73.2742502674361,0.));
#102497=CARTESIAN_POINT('Ctrl Pts',(10.4830957433311,73.3005471910639,0.));
#102498=CARTESIAN_POINT('Ctrl Pts',(10.475615904381,73.3268715280609,0.));
#102499=CARTESIAN_POINT('Ctrl Pts',(10.4681024236288,73.353223182365,0.));
#102500=CARTESIAN_POINT('Ctrl Pts',(10.4605552819391,73.3796020622437,0.));
#102501=CARTESIAN_POINT('Ctrl Pts',(10.4529744618438,73.4060080806578,0.));
#102502=CARTESIAN_POINT('Ctrl Pts',(10.4464473465487,73.4286663447915,0.));
#102503=CARTESIAN_POINT('Ctrl Pts',(10.4414249334768,73.446052552855,0.));
#102504=CARTESIAN_POINT('Ctrl Pts',(10.4379221501093,73.4581547436539,0.));
#102505=CARTESIAN_POINT('Ctrl Pts',(10.4359488742883,73.4649650361539,0.));
#102506=CARTESIAN_POINT('Ctrl Pts',(10.4355099267391,73.4664795929517,0.));
#102507=CARTESIAN_POINT('',(11.3136138754165,69.079679653846,12.));
#102508=CARTESIAN_POINT('',(11.3136138754165,69.079679653846,0.));
#102509=CARTESIAN_POINT('Ctrl Pts',(10.4355099267391,73.4664795929518,12.));
#102510=CARTESIAN_POINT('Ctrl Pts',(10.4359488742883,73.4649650361539,12.));
#102511=CARTESIAN_POINT('Ctrl Pts',(10.4379221501093,73.4581547436539,12.));
#102512=CARTESIAN_POINT('Ctrl Pts',(10.4414249334768,73.446052552855,12.));
#102513=CARTESIAN_POINT('Ctrl Pts',(10.4464473465487,73.4286663447915,12.));
#102514=CARTESIAN_POINT('Ctrl Pts',(10.4529744618438,73.4060080806578,12.));
#102515=CARTESIAN_POINT('Ctrl Pts',(10.4605552819391,73.3796020622437,12.));
#102516=CARTESIAN_POINT('Ctrl Pts',(10.4681024236288,73.353223182365,12.));
#102517=CARTESIAN_POINT('Ctrl Pts',(10.475615904381,73.3268715280609,12.));
#102518=CARTESIAN_POINT('Ctrl Pts',(10.4830957433311,73.3005471910639,12.));
#102519=CARTESIAN_POINT('Ctrl Pts',(10.4905419611529,73.2742502674361,12.));
#102520=CARTESIAN_POINT('Ctrl Pts',(10.4979545795197,73.247980856023,12.));
#102521=CARTESIAN_POINT('Ctrl Pts',(10.505333620691,73.2217390572578,12.));
#102522=CARTESIAN_POINT('Ctrl Pts',(10.5126791070804,73.1955249719037,12.));
#102523=CARTESIAN_POINT('Ctrl Pts',(10.5199910607652,73.169338699611,12.));
#102524=CARTESIAN_POINT('Ctrl Pts',(10.5272695032649,73.1431803382677,12.));
#102525=CARTESIAN_POINT('Ctrl Pts',(10.5345144558097,73.1170499848012,12.));
#102526=CARTESIAN_POINT('Ctrl Pts',(10.5417259395001,73.090947735646,12.));
#102527=CARTESIAN_POINT('Ctrl Pts',(10.5489039755138,73.0648736873435,12.));
#102528=CARTESIAN_POINT('Ctrl Pts',(10.5560485852975,73.0388279370845,12.));
#102529=CARTESIAN_POINT('Ctrl Pts',(10.5631597907653,73.0128105832635,12.));
#102530=CARTESIAN_POINT('Ctrl Pts',(10.5702376142052,72.9868217252293,12.));
#102531=CARTESIAN_POINT('Ctrl Pts',(10.5772820781959,72.9608614630539,12.));
#102532=CARTESIAN_POINT('Ctrl Pts',(10.5842932055209,72.9349298972823,12.));
#102533=CARTESIAN_POINT('Ctrl Pts',(10.5912710190928,72.9090271287081,12.));
#102534=CARTESIAN_POINT('Ctrl Pts',(10.5982155418625,72.8831532580839,12.));
#102535=CARTESIAN_POINT('Ctrl Pts',(10.6051267968202,72.8573083861328,12.));
#102536=CARTESIAN_POINT('Ctrl Pts',(10.6120048070366,72.8314926136872,12.));
#102537=CARTESIAN_POINT('Ctrl Pts',(10.6188495956973,72.8057060417882,12.));
#102538=CARTESIAN_POINT('Ctrl Pts',(10.6256611861395,72.7799487717914,12.));
#102539=CARTESIAN_POINT('Ctrl Pts',(10.6324396018999,72.7542209054823,12.));
#102540=CARTESIAN_POINT('Ctrl Pts',(10.6391848667354,72.7285225451309,12.));
#102541=CARTESIAN_POINT('Ctrl Pts',(10.6458970045948,72.7028537934332,12.));
#102542=CARTESIAN_POINT('Ctrl Pts',(10.6525760396055,72.6772147534762,12.));
#102543=CARTESIAN_POINT('Ctrl Pts',(10.659221996058,72.6516055286908,12.));
#102544=CARTESIAN_POINT('Ctrl Pts',(10.6658348983944,72.6260262228055,12.));
#102545=CARTESIAN_POINT('Ctrl Pts',(10.6724147711994,72.6004769398004,12.));
#102546=CARTESIAN_POINT('Ctrl Pts',(10.6789616392041,72.57495778394,12.));
#102547=CARTESIAN_POINT('Ctrl Pts',(10.6854755272903,72.5494688597951,12.));
#102548=CARTESIAN_POINT('Ctrl Pts',(10.691956460499,72.5240102722662,12.));
#102549=CARTESIAN_POINT('Ctrl Pts',(10.6984044640399,72.4985821266031,12.));
#102550=CARTESIAN_POINT('Ctrl Pts',(10.7048195633062,72.4731845284238,12.));
#102551=CARTESIAN_POINT('Ctrl Pts',(10.7112017838707,72.4478175837168,12.));
#102552=CARTESIAN_POINT('Ctrl Pts',(10.7175511514789,72.4224813988355,12.));
#102553=CARTESIAN_POINT('Ctrl Pts',(10.7238676920469,72.3971760804935,12.));
#102554=CARTESIAN_POINT('Ctrl Pts',(10.7301514316607,72.3719017357568,12.));
#102555=CARTESIAN_POINT('Ctrl Pts',(10.73640239658,72.3466584720311,12.));
#102556=CARTESIAN_POINT('Ctrl Pts',(10.7426206132375,72.3214463970634,12.));
#102557=CARTESIAN_POINT('Ctrl Pts',(10.7488061082368,72.296265618955,12.));
#102558=CARTESIAN_POINT('Ctrl Pts',(10.7549589083535,72.2711162461679,12.));
#102559=CARTESIAN_POINT('Ctrl Pts',(10.7610790405385,72.2459983875298,12.));
#102560=CARTESIAN_POINT('Ctrl Pts',(10.7671665319254,72.2209121522367,12.));
#102561=CARTESIAN_POINT('Ctrl Pts',(10.7732214098343,72.1958576498556,12.));
#102562=CARTESIAN_POINT('Ctrl Pts',(10.779243701766,72.17083499033,12.));
#102563=CARTESIAN_POINT('Ctrl Pts',(10.7852334354015,72.145844283983,12.));
#102564=CARTESIAN_POINT('Ctrl Pts',(10.7911906386027,72.1208856415171,12.));
#102565=CARTESIAN_POINT('Ctrl Pts',(10.7971153394168,72.095959174012,12.));
#102566=CARTESIAN_POINT('Ctrl Pts',(10.8030075660811,72.0710649929214,12.));
#102567=CARTESIAN_POINT('Ctrl Pts',(10.8088673470187,72.0462032100828,12.));
#102568=CARTESIAN_POINT('Ctrl Pts',(10.8146947108376,72.0213739377231,12.));
#102569=CARTESIAN_POINT('Ctrl Pts',(10.8204896863328,71.996577288462,12.));
#102570=CARTESIAN_POINT('Ctrl Pts',(10.8262523024897,71.971813375312,12.));
#102571=CARTESIAN_POINT('Ctrl Pts',(10.8319825884917,71.9470823116777,12.));
#102572=CARTESIAN_POINT('Ctrl Pts',(10.8376805737158,71.9223842113622,12.));
#102573=CARTESIAN_POINT('Ctrl Pts',(10.8433462877312,71.8977191885726,12.));
#102574=CARTESIAN_POINT('Ctrl Pts',(10.8489797602998,71.8730873579226,12.));
#102575=CARTESIAN_POINT('Ctrl Pts',(10.8545810213799,71.8484888344335,12.));
#102576=CARTESIAN_POINT('Ctrl Pts',(10.860150101133,71.8239237335318,12.));
#102577=CARTESIAN_POINT('Ctrl Pts',(10.8656870299218,71.7993921710546,12.));
#102578=CARTESIAN_POINT('Ctrl Pts',(10.8711918383071,71.7748942632578,12.));
#102579=CARTESIAN_POINT('Ctrl Pts',(10.8766645570496,71.7504301268177,12.));
#102580=CARTESIAN_POINT('Ctrl Pts',(10.8821052171122,71.7259998788337,12.));
#102581=CARTESIAN_POINT('Ctrl Pts',(10.8875138496674,71.7016036368254,12.));
#102582=CARTESIAN_POINT('Ctrl Pts',(10.8928904860967,71.6772415187382,12.));
#102583=CARTESIAN_POINT('Ctrl Pts',(10.8982351579872,71.6529136429515,12.));
#102584=CARTESIAN_POINT('Ctrl Pts',(10.9035478971329,71.6286201282815,12.));
#102585=CARTESIAN_POINT('Ctrl Pts',(10.9088287355364,71.604361093983,12.));
#102586=CARTESIAN_POINT('Ctrl Pts',(10.9140777054169,71.5801366597479,12.));
#102587=CARTESIAN_POINT('Ctrl Pts',(10.9192948392099,71.5559469457082,12.));
#102588=CARTESIAN_POINT('Ctrl Pts',(10.9244801695642,71.5317920724453,12.));
#102589=CARTESIAN_POINT('Ctrl Pts',(10.9296337293425,71.5076721609936,12.));
#102590=CARTESIAN_POINT('Ctrl Pts',(10.9347555516236,71.4835873328425,12.));
#102591=CARTESIAN_POINT('Ctrl Pts',(10.9398456697095,71.4595377099352,12.));
#102592=CARTESIAN_POINT('Ctrl Pts',(10.9449041171269,71.4355234146718,12.));
#102593=CARTESIAN_POINT('Ctrl Pts',(10.9499309276235,71.411544569919,12.));
#102594=CARTESIAN_POINT('Ctrl Pts',(10.954926135169,71.3876012990135,12.));
#102595=CARTESIAN_POINT('Ctrl Pts',(10.9598897739565,71.3636937257651,12.));
#102596=CARTESIAN_POINT('Ctrl Pts',(10.96482187841,71.3398219744547,12.));
#102597=CARTESIAN_POINT('Ctrl Pts',(10.9697224831862,71.3159861698368,12.));
#102598=CARTESIAN_POINT('Ctrl Pts',(10.9745916231711,71.2921864371499,12.));
#102599=CARTESIAN_POINT('Ctrl Pts',(10.9794293334806,71.2684229021209,12.));
#102600=CARTESIAN_POINT('Ctrl Pts',(10.9842356494627,71.2446956909685,12.));
#102601=CARTESIAN_POINT('Ctrl Pts',(10.9890106067038,71.221004930401,12.));
#102602=CARTESIAN_POINT('Ctrl Pts',(10.993754241032,71.1973507476188,12.));
#102603=CARTESIAN_POINT('Ctrl Pts',(10.9984665885127,71.1737332703248,12.));
#102604=CARTESIAN_POINT('Ctrl Pts',(11.0031476854503,71.1501526267288,12.));
#102605=CARTESIAN_POINT('Ctrl Pts',(11.0077975683895,71.1266089455517,12.));
#102606=CARTESIAN_POINT('Ctrl Pts',(11.0124162741223,71.1031023560243,12.));
#102607=CARTESIAN_POINT('Ctrl Pts',(11.0170038396913,71.0796329878896,12.));
#102608=CARTESIAN_POINT('Ctrl Pts',(11.0215603023854,71.0562009714125,12.));
#102609=CARTESIAN_POINT('Ctrl Pts',(11.0260856997414,71.0328064373849,12.));
#102610=CARTESIAN_POINT('Ctrl Pts',(11.0305800695457,71.0094495171295,12.));
#102611=CARTESIAN_POINT('Ctrl Pts',(11.0350434498408,70.9861303424989,12.));
#102612=CARTESIAN_POINT('Ctrl Pts',(11.039475878929,70.9628490458779,12.));
#102613=CARTESIAN_POINT('Ctrl Pts',(11.0438773953686,70.9396057601953,12.));
#102614=CARTESIAN_POINT('Ctrl Pts',(11.0482480379752,70.9164006189283,12.));
#102615=CARTESIAN_POINT('Ctrl Pts',(11.0525878458242,70.8932337561078,12.));
#102616=CARTESIAN_POINT('Ctrl Pts',(11.0568968582566,70.8701053063158,12.));
#102617=CARTESIAN_POINT('Ctrl Pts',(11.061175114883,70.847015404688,12.));
#102618=CARTESIAN_POINT('Ctrl Pts',(11.0654226555798,70.8239641869266,12.));
#102619=CARTESIAN_POINT('Ctrl Pts',(11.0696395204908,70.8009517893042,12.));
#102620=CARTESIAN_POINT('Ctrl Pts',(11.0738257500292,70.7779783486689,12.));
#102621=CARTESIAN_POINT('Ctrl Pts',(11.0779813848851,70.7550440024422,12.));
#102622=CARTESIAN_POINT('Ctrl Pts',(11.0821064660276,70.7321488886229,12.));
#102623=CARTESIAN_POINT('Ctrl Pts',(11.0862010347022,70.7092931457996,12.));
#102624=CARTESIAN_POINT('Ctrl Pts',(11.0902651324325,70.686476913156,12.));
#102625=CARTESIAN_POINT('Ctrl Pts',(11.0942988010231,70.6637003304768,12.));
#102626=CARTESIAN_POINT('Ctrl Pts',(11.0983020825662,70.6409635381446,12.));
#102627=CARTESIAN_POINT('Ctrl Pts',(11.1022750194439,70.6182666771441,12.));
#102628=CARTESIAN_POINT('Ctrl Pts',(11.1062176543257,70.5956098890744,12.));
#102629=CARTESIAN_POINT('Ctrl Pts',(11.11013003017,70.5729933161538,12.));
#102630=CARTESIAN_POINT('Ctrl Pts',(11.1140121902274,70.5504171012247,12.));
#102631=CARTESIAN_POINT('Ctrl Pts',(11.117864178048,70.5278813877519,12.));
#102632=CARTESIAN_POINT('Ctrl Pts',(11.121686037483,70.5053863198306,12.));
#102633=CARTESIAN_POINT('Ctrl Pts',(11.1254778126824,70.4829320421973,12.));
#102634=CARTESIAN_POINT('Ctrl Pts',(11.1292395480975,70.4605187002356,12.));
#102635=CARTESIAN_POINT('Ctrl Pts',(11.1329712884845,70.438146439981,12.));
#102636=CARTESIAN_POINT('Ctrl Pts',(11.1366730789122,70.415815408119,12.));
#102637=CARTESIAN_POINT('Ctrl Pts',(11.1403449647622,70.3935257519945,12.));
#102638=CARTESIAN_POINT('Ctrl Pts',(11.1439869917269,70.3712776196216,12.));
#102639=CARTESIAN_POINT('Ctrl Pts',(11.1475992058124,70.3490711596882,12.));
#102640=CARTESIAN_POINT('Ctrl Pts',(11.1511816533422,70.3269065215591,12.));
#102641=CARTESIAN_POINT('Ctrl Pts',(11.1547343809647,70.3047838552758,12.));
#102642=CARTESIAN_POINT('Ctrl Pts',(11.1582574356522,70.2827033115662,12.));
#102643=CARTESIAN_POINT('Ctrl Pts',(11.1617508647017,70.2606650418589,12.));
#102644=CARTESIAN_POINT('Ctrl Pts',(11.1652147157383,70.2386691982902,12.));
#102645=CARTESIAN_POINT('Ctrl Pts',(11.168649036721,70.2167159337095,12.));
#102646=CARTESIAN_POINT('Ctrl Pts',(11.1720538759499,70.1948054016817,12.));
#102647=CARTESIAN_POINT('Ctrl Pts',(11.1754292820631,70.1729377564956,12.));
#102648=CARTESIAN_POINT('Ctrl Pts',(11.1787753040363,70.1511131531674,12.));
#102649=CARTESIAN_POINT('Ctrl Pts',(11.1820919911846,70.1293317474432,12.));
#102650=CARTESIAN_POINT('Ctrl Pts',(11.185379393167,70.1075936957968,12.));
#102651=CARTESIAN_POINT('Ctrl Pts',(11.1886375599914,70.0858991554283,12.));
#102652=CARTESIAN_POINT('Ctrl Pts',(11.1918665420166,70.0642482842928,12.));
#102653=CARTESIAN_POINT('Ctrl Pts',(11.1950663899576,70.0426412411185,12.));
#102654=CARTESIAN_POINT('Ctrl Pts',(11.1982371548919,70.0210781854243,12.));
#102655=CARTESIAN_POINT('Ctrl Pts',(11.2013788882714,69.9995592775343,12.));
#102656=CARTESIAN_POINT('Ctrl Pts',(11.2044916419244,69.97808467858,12.));
#102657=CARTESIAN_POINT('Ctrl Pts',(11.2075754680449,69.9566545504837,12.));
#102658=CARTESIAN_POINT('Ctrl Pts',(11.2106304191882,69.9352690559405,12.));
#102659=CARTESIAN_POINT('Ctrl Pts',(11.2136565482678,69.9139283584022,12.));
#102660=CARTESIAN_POINT('Ctrl Pts',(11.2166539085523,69.8926326220385,12.));
#102661=CARTESIAN_POINT('Ctrl Pts',(11.219622553679,69.871382011789,12.));
#102662=CARTESIAN_POINT('Ctrl Pts',(11.2225625376736,69.8501766934428,12.));
#102663=CARTESIAN_POINT('Ctrl Pts',(11.225473914972,69.8290168337076,12.));
#102664=CARTESIAN_POINT('Ctrl Pts',(11.2283567404437,69.8079026002768,12.));
#102665=CARTESIAN_POINT('Ctrl Pts',(11.2312110694187,69.7868341618954,12.));
#102666=CARTESIAN_POINT('Ctrl Pts',(11.2340369576456,69.7658116882324,12.));
#102667=CARTESIAN_POINT('Ctrl Pts',(11.2368344612472,69.7448353497408,12.));
#102668=CARTESIAN_POINT('Ctrl Pts',(11.239603636686,69.7239053175356,12.));
#102669=CARTESIAN_POINT('Ctrl Pts',(11.2423445407166,69.7030217632164,12.));
#102670=CARTESIAN_POINT('Ctrl Pts',(11.2450572303841,69.6821848588457,12.));
#102671=CARTESIAN_POINT('Ctrl Pts',(11.2477417631386,69.6613947773534,12.));
#102672=CARTESIAN_POINT('Ctrl Pts',(11.2503981969412,69.6406516928891,12.));
#102673=CARTESIAN_POINT('Ctrl Pts',(11.2530265903557,69.6199557811245,12.));
#102674=CARTESIAN_POINT('Ctrl Pts',(11.2556270027016,69.599307219739,12.));
#102675=CARTESIAN_POINT('Ctrl Pts',(11.2581994939541,69.5787061880857,12.));
#102676=CARTESIAN_POINT('Ctrl Pts',(11.2607441244703,69.5581528662877,12.));
#102677=CARTESIAN_POINT('Ctrl Pts',(11.263260954763,69.5376474344771,12.));
#102678=CARTESIAN_POINT('Ctrl Pts',(11.2657500452716,69.5171900720158,12.));
#102679=CARTESIAN_POINT('Ctrl Pts',(11.2682114561008,69.4967809565929,12.));
#102680=CARTESIAN_POINT('Ctrl Pts',(11.270645247528,69.4764202659397,12.));
#102681=CARTESIAN_POINT('Ctrl Pts',(11.2730514806139,69.456108179879,12.));
#102682=CARTESIAN_POINT('Ctrl Pts',(11.2754302177021,69.4358448819967,12.));
#102683=CARTESIAN_POINT('Ctrl Pts',(11.2777815231469,69.4156305620593,12.));
#102684=CARTESIAN_POINT('Ctrl Pts',(11.2801054633816,69.3954654162281,12.));
#102685=CARTESIAN_POINT('Ctrl Pts',(11.2824021054045,69.3753496420039,12.));
#102686=CARTESIAN_POINT('Ctrl Pts',(11.2846715154524,69.3552834337784,12.));
#102687=CARTESIAN_POINT('Ctrl Pts',(11.2869137578459,69.3352669789587,12.));
#102688=CARTESIAN_POINT('Ctrl Pts',(11.2891288931517,69.3153004517783,12.));
#102689=CARTESIAN_POINT('Ctrl Pts',(11.2913169799628,69.295384019272,12.));
#102690=CARTESIAN_POINT('Ctrl Pts',(11.2934780784351,69.275517853148,12.));
#102691=CARTESIAN_POINT('Ctrl Pts',(11.2956122531375,69.2557021393351,12.));
#102692=CARTESIAN_POINT('Ctrl Pts',(11.2977195764852,69.2359370894907,12.));
#102693=CARTESIAN_POINT('Ctrl Pts',(11.2998001310964,69.2162229488531,12.));
#102694=CARTESIAN_POINT('Ctrl Pts',(11.3018540025638,69.1965599718914,12.));
#102695=CARTESIAN_POINT('Ctrl Pts',(11.3038812726292,69.1769483991721,12.));
#102696=CARTESIAN_POINT('Ctrl Pts',(11.3058820128307,69.1573884361,12.));
#102697=CARTESIAN_POINT('Ctrl Pts',(11.3078562764384,69.1378802251711,12.));
#102698=CARTESIAN_POINT('Ctrl Pts',(11.3098040973713,69.118423844466,12.));
#102699=CARTESIAN_POINT('Ctrl Pts',(11.3113412156661,69.1029002322118,12.));
#102700=CARTESIAN_POINT('Ctrl Pts',(11.3124821678798,69.0912808656811,12.));
#102701=CARTESIAN_POINT('Ctrl Pts',(11.3132375200165,69.0835449954396,12.));
#102702=CARTESIAN_POINT('Ctrl Pts',(11.3136138754165,69.079679653846,12.));
#102703=CARTESIAN_POINT('Ctrl Pts',(8.93459554657839,73.6640787198055,-5.55111512312578E-16));
#102704=CARTESIAN_POINT('Ctrl Pts',(8.93459554657839,73.6640787198055,4.));
#102705=CARTESIAN_POINT('Ctrl Pts',(8.93459554657838,73.6640787198055,8.));
#102706=CARTESIAN_POINT('Ctrl Pts',(8.93459554657838,73.6640787198055,12.));
#102707=CARTESIAN_POINT('Ctrl Pts',(8.99145626777887,73.7581053903595,-5.55111512312578E-16));
#102708=CARTESIAN_POINT('Ctrl Pts',(8.99145626777887,73.7581053903595,4.));
#102709=CARTESIAN_POINT('Ctrl Pts',(8.99145626777886,73.7581053903595,8.));
#102710=CARTESIAN_POINT('Ctrl Pts',(8.99145626777886,73.7581053903595,12.));
#102711=CARTESIAN_POINT('Ctrl Pts',(9.14696952162285,73.8880618019209,-5.55111512312578E-16));
#102712=CARTESIAN_POINT('Ctrl Pts',(9.14696952162285,73.8880618019209,4.));
#102713=CARTESIAN_POINT('Ctrl Pts',(9.14696952162285,73.888061801921,7.99999999999999));
#102714=CARTESIAN_POINT('Ctrl Pts',(9.14696952162285,73.888061801921,12.));
#102715=CARTESIAN_POINT('Ctrl Pts',(9.34395683490519,73.9117532086774,-5.55111512312578E-16));
#102716=CARTESIAN_POINT('Ctrl Pts',(9.34395683490519,73.9117532086774,4.));
#102717=CARTESIAN_POINT('Ctrl Pts',(9.34395683490521,73.9117532086774,8.00000000000001));
#102718=CARTESIAN_POINT('Ctrl Pts',(9.34395683490521,73.9117532086774,12.));
#102719=CARTESIAN_POINT('Ctrl Pts',(9.42570643237553,73.9013264985867,-5.55111512312578E-16));
#102720=CARTESIAN_POINT('Ctrl Pts',(9.42570643237553,73.9013264985867,4.));
#102721=CARTESIAN_POINT('Ctrl Pts',(9.42570643237556,73.9013264985867,8.));
#102722=CARTESIAN_POINT('Ctrl Pts',(9.42570643237556,73.9013264985867,12.));
#102723=CARTESIAN_POINT('',(8.93459554657838,73.6640787198055,0.));
#102724=CARTESIAN_POINT('',(9.4257064323755,73.9013264985864,2.77555756156289E-16));
#102725=CARTESIAN_POINT('Ctrl Pts',(8.93459554657839,73.6640787198055,4.16333634234434E-16));
#102726=CARTESIAN_POINT('Ctrl Pts',(8.99145626777887,73.7581053903595,4.16333634234433E-16));
#102727=CARTESIAN_POINT('Ctrl Pts',(9.08032098426115,73.832366196966,4.16333634234434E-16));
#102728=CARTESIAN_POINT('Ctrl Pts',(9.18272825076411,73.8719282264934,4.16333634234434E-16));
#102729=CARTESIAN_POINT('Ctrl Pts',(9.25953370064133,73.9015997486389,4.16333634234434E-16));
#102730=CARTESIAN_POINT('Ctrl Pts',(9.34395683490519,73.9117532086774,4.16333634234433E-16));
#102731=CARTESIAN_POINT('Ctrl Pts',(9.42570643237553,73.9013264985867,4.16333634234434E-16));
#102732=CARTESIAN_POINT('',(9.42570643237553,73.9013264985864,12.));
#102733=CARTESIAN_POINT('Ctrl Pts',(9.42570643237553,73.9013264985867,-5.55111512312578E-16));
#102734=CARTESIAN_POINT('Ctrl Pts',(9.42570643237553,73.9013264985867,4.));
#102735=CARTESIAN_POINT('Ctrl Pts',(9.42570643237556,73.9013264985867,8.));
#102736=CARTESIAN_POINT('Ctrl Pts',(9.42570643237556,73.9013264985867,12.));
#102737=CARTESIAN_POINT('',(8.93459554657838,73.6640787198055,12.));
#102738=CARTESIAN_POINT('Ctrl Pts',(9.42570643237556,73.9013264985867,12.));
#102739=CARTESIAN_POINT('Ctrl Pts',(9.34395683490521,73.9117532086774,12.));
#102740=CARTESIAN_POINT('Ctrl Pts',(9.25953370064134,73.901599748639,12.));
#102741=CARTESIAN_POINT('Ctrl Pts',(9.18272825076411,73.8719282264934,12.));
#102742=CARTESIAN_POINT('Ctrl Pts',(9.08032098426114,73.8323661969661,12.));
#102743=CARTESIAN_POINT('Ctrl Pts',(8.99145626777886,73.7581053903595,12.));
#102744=CARTESIAN_POINT('Ctrl Pts',(8.93459554657838,73.6640787198055,12.));
#102745=CARTESIAN_POINT('Ctrl Pts',(8.93459554657838,73.6640787198055,12.));
#102746=CARTESIAN_POINT('Ctrl Pts',(8.93459554657838,73.6640787198055,8.));
#102747=CARTESIAN_POINT('Ctrl Pts',(8.93459554657839,73.6640787198055,4.));
#102748=CARTESIAN_POINT('Ctrl Pts',(8.93459554657839,73.6640787198055,-5.55111512312578E-16));
#102749=CARTESIAN_POINT('Origin',(4.88285199465431E-11,3.71649880366789E-10,
0.));
#102750=CARTESIAN_POINT('Origin',(4.88285199465431E-11,3.71649880366789E-10,
12.));
#102751=CARTESIAN_POINT('Origin',(4.88285199465431E-11,3.71649880366789E-10,
0.));
#102752=CARTESIAN_POINT('Ctrl Pts',(16.4184755008034,72.6683126419592,-1.11022302462516E-15));
#102753=CARTESIAN_POINT('Ctrl Pts',(16.4184755008034,72.6683126419592,4.));
#102754=CARTESIAN_POINT('Ctrl Pts',(16.4184755008034,72.6683126419592,8.));
#102755=CARTESIAN_POINT('Ctrl Pts',(16.4184755008034,72.6683126419592,12.));
#102756=CARTESIAN_POINT('Ctrl Pts',(16.5256563519779,72.6440964999409,-1.11022302462516E-15));
#102757=CARTESIAN_POINT('Ctrl Pts',(16.5256563519779,72.6440964999409,3.99999999999999));
#102758=CARTESIAN_POINT('Ctrl Pts',(16.5256563519779,72.6440964999409,8.));
#102759=CARTESIAN_POINT('Ctrl Pts',(16.5256563519779,72.6440964999409,12.));
#102760=CARTESIAN_POINT('Ctrl Pts',(16.6981133841328,72.5376471652843,-1.0371418567521E-15));
#102761=CARTESIAN_POINT('Ctrl Pts',(16.6981133841328,72.5376471652843,4.00000000000001));
#102762=CARTESIAN_POINT('Ctrl Pts',(16.6981133841328,72.5376471652843,8.));
#102763=CARTESIAN_POINT('Ctrl Pts',(16.6981133841328,72.5376471652843,12.));
#102764=CARTESIAN_POINT('Ctrl Pts',(16.7828708182976,72.3582555997243,-8.63611844392621E-16));
#102765=CARTESIAN_POINT('Ctrl Pts',(16.7828708182976,72.3582555997243,3.99999999999999));
#102766=CARTESIAN_POINT('Ctrl Pts',(16.7828708182976,72.3582555997243,8.));
#102767=CARTESIAN_POINT('Ctrl Pts',(16.7828708182976,72.3582555997243,12.));
#102768=CARTESIAN_POINT('Ctrl Pts',(16.7988252568808,72.2774028393484,-7.7995786415518E-16));
#102769=CARTESIAN_POINT('Ctrl Pts',(16.7988252568808,72.2774028393484,4.));
#102770=CARTESIAN_POINT('Ctrl Pts',(16.7988252568808,72.2774028393484,8.));
#102771=CARTESIAN_POINT('Ctrl Pts',(16.7988252568808,72.2774028393484,12.));
#102772=CARTESIAN_POINT('',(16.4184755008034,72.6683126419592,0.));
#102773=CARTESIAN_POINT('',(16.7988252568807,72.2774028393484,2.77555756156289E-16));
#102774=CARTESIAN_POINT('Ctrl Pts',(16.4184755008034,72.6683126419592,-1.38777878078144E-16));
#102775=CARTESIAN_POINT('Ctrl Pts',(16.5256563519779,72.6440964999409,-1.38777878078146E-16));
#102776=CARTESIAN_POINT('Ctrl Pts',(16.624203227495,72.5832683087086,-9.70172107221101E-17));
#102777=CARTESIAN_POINT('Ctrl Pts',(16.6941134995868,72.4986222461608,-2.24569206766341E-17));
#102778=CARTESIAN_POINT('Ctrl Pts',(16.7465462036556,72.43513769925,3.34632968574728E-17));
#102779=CARTESIAN_POINT('Ctrl Pts',(16.7828708182976,72.3582555997243,1.0783330215439E-16));
#102780=CARTESIAN_POINT('Ctrl Pts',(16.7988252568808,72.2774028393484,1.91487282391832E-16));
#102781=CARTESIAN_POINT('',(16.7988252568807,72.2774028393484,12.));
#102782=CARTESIAN_POINT('Ctrl Pts',(16.7988252568808,72.2774028393484,-7.7995786415518E-16));
#102783=CARTESIAN_POINT('Ctrl Pts',(16.7988252568808,72.2774028393484,4.));
#102784=CARTESIAN_POINT('Ctrl Pts',(16.7988252568808,72.2774028393484,8.));
#102785=CARTESIAN_POINT('Ctrl Pts',(16.7988252568808,72.2774028393484,12.));
#102786=CARTESIAN_POINT('',(16.4184755008034,72.6683126419592,12.));
#102787=CARTESIAN_POINT('Ctrl Pts',(16.7988252568808,72.2774028393484,12.));
#102788=CARTESIAN_POINT('Ctrl Pts',(16.7828708182976,72.3582555997243,12.));
#102789=CARTESIAN_POINT('Ctrl Pts',(16.7465462036556,72.43513769925,12.));
#102790=CARTESIAN_POINT('Ctrl Pts',(16.6941134995867,72.4986222461608,12.));
#102791=CARTESIAN_POINT('Ctrl Pts',(16.624203227495,72.5832683087086,12.));
#102792=CARTESIAN_POINT('Ctrl Pts',(16.5256563519779,72.6440964999409,12.));
#102793=CARTESIAN_POINT('Ctrl Pts',(16.4184755008034,72.6683126419592,12.));
#102794=CARTESIAN_POINT('Ctrl Pts',(16.4184755008034,72.6683126419592,12.));
#102795=CARTESIAN_POINT('Ctrl Pts',(16.4184755008034,72.6683126419592,8.));
#102796=CARTESIAN_POINT('Ctrl Pts',(16.4184755008034,72.6683126419592,4.));
#102797=CARTESIAN_POINT('Ctrl Pts',(16.4184755008034,72.6683126419592,-1.11022302462516E-15));
#102798=CARTESIAN_POINT('Ctrl Pts',(17.2912529479484,67.8307641965655,0.));
#102799=CARTESIAN_POINT('Ctrl Pts',(17.2912529479484,67.8307641965655,12.));
#102800=CARTESIAN_POINT('Ctrl Pts',(17.2912149114119,67.8346476309018,0.));
#102801=CARTESIAN_POINT('Ctrl Pts',(17.2912149114119,67.8346476309018,12.));
#102802=CARTESIAN_POINT('Ctrl Pts',(17.2911366591348,67.842419897098,0.));
#102803=CARTESIAN_POINT('Ctrl Pts',(17.2911366591348,67.842419897098,12.));
#102804=CARTESIAN_POINT('Ctrl Pts',(17.291012743109,67.8540944889687,0.));
#102805=CARTESIAN_POINT('Ctrl Pts',(17.291012743109,67.8540944889687,12.));
#102806=CARTESIAN_POINT('Ctrl Pts',(17.2908344459694,67.8696929978782,0.));
#102807=CARTESIAN_POINT('Ctrl Pts',(17.2908344459694,67.8696929978782,12.));
#102808=CARTESIAN_POINT('Ctrl Pts',(17.2905897723949,67.8892451049608,0.));
#102809=CARTESIAN_POINT('Ctrl Pts',(17.2905897723949,67.8892451049608,12.));
#102810=CARTESIAN_POINT('Ctrl Pts',(17.2903232740694,67.9088511496686,0.));
#102811=CARTESIAN_POINT('Ctrl Pts',(17.2903232740694,67.9088511496686,12.));
#102812=CARTESIAN_POINT('Ctrl Pts',(17.2900349103981,67.9285110571741,0.));
#102813=CARTESIAN_POINT('Ctrl Pts',(17.2900349103981,67.9285110571741,12.));
#102814=CARTESIAN_POINT('Ctrl Pts',(17.2897246158941,67.9482246901667,0.));
#102815=CARTESIAN_POINT('Ctrl Pts',(17.2897246158941,67.9482246901667,12.));
#102816=CARTESIAN_POINT('Ctrl Pts',(17.2893923013894,67.9679918502579,0.));
#102817=CARTESIAN_POINT('Ctrl Pts',(17.2893923013894,67.9679918502579,12.));
#102818=CARTESIAN_POINT('Ctrl Pts',(17.2890378644866,67.987812304921,0.));
#102819=CARTESIAN_POINT('Ctrl Pts',(17.2890378644866,67.987812304921,12.));
#102820=CARTESIAN_POINT('Ctrl Pts',(17.28866119774,68.007685808115,0.));
#102821=CARTESIAN_POINT('Ctrl Pts',(17.28866119774,68.007685808115,12.));
#102822=CARTESIAN_POINT('Ctrl Pts',(17.2882621974721,68.0276121227356,0.));
#102823=CARTESIAN_POINT('Ctrl Pts',(17.2882621974721,68.0276121227356,12.));
#102824=CARTESIAN_POINT('Ctrl Pts',(17.2878407730961,68.0475910442424,0.));
#102825=CARTESIAN_POINT('Ctrl Pts',(17.2878407730961,68.0475910442424,12.));
#102826=CARTESIAN_POINT('Ctrl Pts',(17.2873968440839,68.0676223930412,0.));
#102827=CARTESIAN_POINT('Ctrl Pts',(17.2873968440839,68.0676223930412,12.));
#102828=CARTESIAN_POINT('Ctrl Pts',(17.2869303355432,68.0877060033205,0.));
#102829=CARTESIAN_POINT('Ctrl Pts',(17.2869303355432,68.0877060033205,12.));
#102830=CARTESIAN_POINT('Ctrl Pts',(17.2864411745459,68.1078417137877,0.));
#102831=CARTESIAN_POINT('Ctrl Pts',(17.2864411745459,68.1078417137877,12.));
#102832=CARTESIAN_POINT('Ctrl Pts',(17.2859292855705,68.1280293561511,0.));
#102833=CARTESIAN_POINT('Ctrl Pts',(17.2859292855705,68.1280293561511,12.));
#102834=CARTESIAN_POINT('Ctrl Pts',(17.2853945882072,68.1482687493226,0.));
#102835=CARTESIAN_POINT('Ctrl Pts',(17.2853945882072,68.1482687493226,12.));
#102836=CARTESIAN_POINT('Ctrl Pts',(17.2848369995293,68.1685597054232,0.));
#102837=CARTESIAN_POINT('Ctrl Pts',(17.2848369995293,68.1685597054232,12.));
#102838=CARTESIAN_POINT('Ctrl Pts',(17.2842564355799,68.1889020335427,0.));
#102839=CARTESIAN_POINT('Ctrl Pts',(17.2842564355799,68.1889020335427,12.));
#102840=CARTESIAN_POINT('Ctrl Pts',(17.2836528130819,68.2092955440567,0.));
#102841=CARTESIAN_POINT('Ctrl Pts',(17.2836528130819,68.2092955440567,12.));
#102842=CARTESIAN_POINT('Ctrl Pts',(17.2830260513867,68.2297400535294,0.));
#102843=CARTESIAN_POINT('Ctrl Pts',(17.2830260513867,68.2297400535294,12.));
#102844=CARTESIAN_POINT('Ctrl Pts',(17.2823760723874,68.2502353845071,0.));
#102845=CARTESIAN_POINT('Ctrl Pts',(17.2823760723874,68.2502353845071,12.));
#102846=CARTESIAN_POINT('Ctrl Pts',(17.2817027995831,68.2707813631731,0.));
#102847=CARTESIAN_POINT('Ctrl Pts',(17.2817027995831,68.2707813631731,12.));
#102848=CARTESIAN_POINT('Ctrl Pts',(17.2810061574353,68.2913778177261,0.));
#102849=CARTESIAN_POINT('Ctrl Pts',(17.2810061574353,68.2913778177261,12.));
#102850=CARTESIAN_POINT('Ctrl Pts',(17.2802860705815,68.3120245763914,0.));
#102851=CARTESIAN_POINT('Ctrl Pts',(17.2802860705815,68.3120245763914,12.));
#102852=CARTESIAN_POINT('Ctrl Pts',(17.2795424631799,68.3327214657575,0.));
#102853=CARTESIAN_POINT('Ctrl Pts',(17.2795424631799,68.3327214657575,12.));
#102854=CARTESIAN_POINT('Ctrl Pts',(17.2787752592484,68.3534683116515,0.));
#102855=CARTESIAN_POINT('Ctrl Pts',(17.2787752592484,68.3534683116515,12.));
#102856=CARTESIAN_POINT('Ctrl Pts',(17.2779843829608,68.3742649398964,0.));
#102857=CARTESIAN_POINT('Ctrl Pts',(17.2779843829608,68.3742649398964,12.));
#102858=CARTESIAN_POINT('Ctrl Pts',(17.2771697589384,68.3951111770487,0.));
#102859=CARTESIAN_POINT('Ctrl Pts',(17.2771697589384,68.3951111770487,12.));
#102860=CARTESIAN_POINT('Ctrl Pts',(17.2763313126018,68.4160068512753,0.));
#102861=CARTESIAN_POINT('Ctrl Pts',(17.2763313126018,68.4160068512753,12.));
#102862=CARTESIAN_POINT('Ctrl Pts',(17.2754689702992,68.436951792677,0.));
#102863=CARTESIAN_POINT('Ctrl Pts',(17.2754689702992,68.436951792677,12.));
#102864=CARTESIAN_POINT('Ctrl Pts',(17.2745826591119,68.4579458328185,0.));
#102865=CARTESIAN_POINT('Ctrl Pts',(17.2745826591119,68.4579458328185,12.));
#102866=CARTESIAN_POINT('Ctrl Pts',(17.2736723067365,68.4789888044351,0.));
#102867=CARTESIAN_POINT('Ctrl Pts',(17.2736723067365,68.4789888044351,12.));
#102868=CARTESIAN_POINT('Ctrl Pts',(17.2727378413489,68.5000805410911,0.));
#102869=CARTESIAN_POINT('Ctrl Pts',(17.2727378413489,68.5000805410911,12.));
#102870=CARTESIAN_POINT('Ctrl Pts',(17.2717791914544,68.521220876786,0.));
#102871=CARTESIAN_POINT('Ctrl Pts',(17.2717791914544,68.521220876786,12.));
#102872=CARTESIAN_POINT('Ctrl Pts',(17.2707962858919,68.5424096459772,0.));
#102873=CARTESIAN_POINT('Ctrl Pts',(17.2707962858919,68.5424096459772,12.));
#102874=CARTESIAN_POINT('Ctrl Pts',(17.269789053896,68.5636466837517,0.));
#102875=CARTESIAN_POINT('Ctrl Pts',(17.269789053896,68.5636466837517,12.));
#102876=CARTESIAN_POINT('Ctrl Pts',(17.2687574251429,68.5849318259449,0.));
#102877=CARTESIAN_POINT('Ctrl Pts',(17.2687574251429,68.5849318259449,12.));
#102878=CARTESIAN_POINT('Ctrl Pts',(17.2677013298057,68.6062649092764,0.));
#102879=CARTESIAN_POINT('Ctrl Pts',(17.2677013298057,68.6062649092764,12.));
#102880=CARTESIAN_POINT('Ctrl Pts',(17.2666206986084,68.6276457714729,0.));
#102881=CARTESIAN_POINT('Ctrl Pts',(17.2666206986084,68.6276457714729,12.));
#102882=CARTESIAN_POINT('Ctrl Pts',(17.2655154627928,68.6490742512057,0.));
#102883=CARTESIAN_POINT('Ctrl Pts',(17.2655154627928,68.6490742512057,12.));
#102884=CARTESIAN_POINT('Ctrl Pts',(17.2643855540892,68.6705501880249,0.));
#102885=CARTESIAN_POINT('Ctrl Pts',(17.2643855540892,68.6705501880249,12.));
#102886=CARTESIAN_POINT('Ctrl Pts',(17.2632309046892,68.6920734222938,0.));
#102887=CARTESIAN_POINT('Ctrl Pts',(17.2632309046892,68.6920734222938,12.));
#102888=CARTESIAN_POINT('Ctrl Pts',(17.2620514472182,68.7136437951097,0.));
#102889=CARTESIAN_POINT('Ctrl Pts',(17.2620514472182,68.7136437951097,12.));
#102890=CARTESIAN_POINT('Ctrl Pts',(17.2608471147185,68.7352611482547,0.));
#102891=CARTESIAN_POINT('Ctrl Pts',(17.2608471147185,68.7352611482547,12.));
#102892=CARTESIAN_POINT('Ctrl Pts',(17.259617840655,68.7569253242333,0.));
#102893=CARTESIAN_POINT('Ctrl Pts',(17.259617840655,68.7569253242333,12.));
#102894=CARTESIAN_POINT('Ctrl Pts',(17.2583635589198,68.7786361662882,0.));
#102895=CARTESIAN_POINT('Ctrl Pts',(17.2583635589198,68.7786361662882,12.));
#102896=CARTESIAN_POINT('Ctrl Pts',(17.2570842038383,68.8003935184184,0.));
#102897=CARTESIAN_POINT('Ctrl Pts',(17.2570842038383,68.8003935184184,12.));
#102898=CARTESIAN_POINT('Ctrl Pts',(17.2557797101812,68.8221972253941,0.));
#102899=CARTESIAN_POINT('Ctrl Pts',(17.2557797101812,68.8221972253941,12.));
#102900=CARTESIAN_POINT('Ctrl Pts',(17.2544500131624,68.844047132755,0.));
#102901=CARTESIAN_POINT('Ctrl Pts',(17.2544500131624,68.844047132755,12.));
#102902=CARTESIAN_POINT('Ctrl Pts',(17.2530950484258,68.8659430867972,0.));
#102903=CARTESIAN_POINT('Ctrl Pts',(17.2530950484258,68.8659430867972,12.));
#102904=CARTESIAN_POINT('Ctrl Pts',(17.2517147520376,68.8878849345557,0.));
#102905=CARTESIAN_POINT('Ctrl Pts',(17.2517147520376,68.8878849345557,12.));
#102906=CARTESIAN_POINT('Ctrl Pts',(17.2503090604792,68.909872523787,0.));
#102907=CARTESIAN_POINT('Ctrl Pts',(17.2503090604792,68.909872523787,12.));
#102908=CARTESIAN_POINT('Ctrl Pts',(17.248877910643,68.9319057029409,0.));
#102909=CARTESIAN_POINT('Ctrl Pts',(17.248877910643,68.9319057029409,12.));
#102910=CARTESIAN_POINT('Ctrl Pts',(17.2474212398275,68.9539843211619,0.));
#102911=CARTESIAN_POINT('Ctrl Pts',(17.2474212398275,68.9539843211619,12.));
#102912=CARTESIAN_POINT('Ctrl Pts',(17.2459389857327,68.9761082282922,0.));
#102913=CARTESIAN_POINT('Ctrl Pts',(17.2459389857327,68.9761082282922,12.));
#102914=CARTESIAN_POINT('Ctrl Pts',(17.2444310864585,68.9982772748694,0.));
#102915=CARTESIAN_POINT('Ctrl Pts',(17.2444310864585,68.9982772748694,12.));
#102916=CARTESIAN_POINT('Ctrl Pts',(17.2428974805044,69.0204913121225,0.));
#102917=CARTESIAN_POINT('Ctrl Pts',(17.2428974805044,69.0204913121225,12.));
#102918=CARTESIAN_POINT('Ctrl Pts',(17.2413381067723,69.0427501919636,0.));
#102919=CARTESIAN_POINT('Ctrl Pts',(17.2413381067723,69.0427501919636,12.));
#102920=CARTESIAN_POINT('Ctrl Pts',(17.2397529045589,69.065053766986,0.));
#102921=CARTESIAN_POINT('Ctrl Pts',(17.2397529045589,69.065053766986,12.));
#102922=CARTESIAN_POINT('Ctrl Pts',(17.2381418135491,69.0874018904599,0.));
#102923=CARTESIAN_POINT('Ctrl Pts',(17.2381418135491,69.0874018904599,12.));
#102924=CARTESIAN_POINT('Ctrl Pts',(17.2365047738125,69.1097944163245,0.));
#102925=CARTESIAN_POINT('Ctrl Pts',(17.2365047738125,69.1097944163245,12.));
#102926=CARTESIAN_POINT('Ctrl Pts',(17.2348417258015,69.1322311991752,0.));
#102927=CARTESIAN_POINT('Ctrl Pts',(17.2348417258015,69.1322311991752,12.));
#102928=CARTESIAN_POINT('Ctrl Pts',(17.2331526103506,69.1547120942527,0.));
#102929=CARTESIAN_POINT('Ctrl Pts',(17.2331526103506,69.1547120942527,12.));
#102930=CARTESIAN_POINT('Ctrl Pts',(17.23143736867,69.1772369574447,0.));
#102931=CARTESIAN_POINT('Ctrl Pts',(17.23143736867,69.1772369574447,12.));
#102932=CARTESIAN_POINT('Ctrl Pts',(17.2296959423407,69.1998056452828,0.));
#102933=CARTESIAN_POINT('Ctrl Pts',(17.2296959423407,69.1998056452828,12.));
#102934=CARTESIAN_POINT('Ctrl Pts',(17.227928273312,69.222418014938,0.));
#102935=CARTESIAN_POINT('Ctrl Pts',(17.227928273312,69.222418014938,12.));
#102936=CARTESIAN_POINT('Ctrl Pts',(17.226134303902,69.2450739242109,0.));
#102937=CARTESIAN_POINT('Ctrl Pts',(17.226134303902,69.2450739242109,12.));
#102938=CARTESIAN_POINT('Ctrl Pts',(17.224313976797,69.2677732315224,0.));
#102939=CARTESIAN_POINT('Ctrl Pts',(17.224313976797,69.2677732315224,12.));
#102940=CARTESIAN_POINT('Ctrl Pts',(17.2224672350438,69.2905157959166,0.));
#102941=CARTESIAN_POINT('Ctrl Pts',(17.2224672350438,69.2905157959166,12.));
#102942=CARTESIAN_POINT('Ctrl Pts',(17.2205940220459,69.3133014770555,0.));
#102943=CARTESIAN_POINT('Ctrl Pts',(17.2205940220459,69.3133014770555,12.));
#102944=CARTESIAN_POINT('Ctrl Pts',(17.2186942815602,69.3361301352141,0.));
#102945=CARTESIAN_POINT('Ctrl Pts',(17.2186942815602,69.3361301352141,12.));
#102946=CARTESIAN_POINT('Ctrl Pts',(17.2167679576984,69.3590016312692,0.));
#102947=CARTESIAN_POINT('Ctrl Pts',(17.2167679576984,69.3590016312692,12.));
#102948=CARTESIAN_POINT('Ctrl Pts',(17.2148149949252,69.3819158266916,0.));
#102949=CARTESIAN_POINT('Ctrl Pts',(17.2148149949252,69.3819158266916,12.));
#102950=CARTESIAN_POINT('Ctrl Pts',(17.2128353380502,69.404872583548,0.));
#102951=CARTESIAN_POINT('Ctrl Pts',(17.2128353380502,69.404872583548,12.));
#102952=CARTESIAN_POINT('Ctrl Pts',(17.2108289322254,69.4278717644973,0.));
#102953=CARTESIAN_POINT('Ctrl Pts',(17.2108289322254,69.4278717644973,12.));
#102954=CARTESIAN_POINT('Ctrl Pts',(17.2087957229423,69.450913232785,0.));
#102955=CARTESIAN_POINT('Ctrl Pts',(17.2087957229423,69.450913232785,12.));
#102956=CARTESIAN_POINT('Ctrl Pts',(17.2067356560336,69.4739968522313,0.));
#102957=CARTESIAN_POINT('Ctrl Pts',(17.2067356560336,69.4739968522313,12.));
#102958=CARTESIAN_POINT('Ctrl Pts',(17.2046486776708,69.4971224872269,0.));
#102959=CARTESIAN_POINT('Ctrl Pts',(17.2046486776708,69.4971224872269,12.));
#102960=CARTESIAN_POINT('Ctrl Pts',(17.2025347343577,69.5202900027367,0.));
#102961=CARTESIAN_POINT('Ctrl Pts',(17.2025347343577,69.5202900027367,12.));
#102962=CARTESIAN_POINT('Ctrl Pts',(17.2003937729268,69.5434992642944,0.));
#102963=CARTESIAN_POINT('Ctrl Pts',(17.2003937729268,69.5434992642944,12.));
#102964=CARTESIAN_POINT('Ctrl Pts',(17.1982257405377,69.5667501379969,0.));
#102965=CARTESIAN_POINT('Ctrl Pts',(17.1982257405377,69.5667501379969,12.));
#102966=CARTESIAN_POINT('Ctrl Pts',(17.196030584678,69.5900424904921,0.));
#102967=CARTESIAN_POINT('Ctrl Pts',(17.196030584678,69.5900424904921,12.));
#102968=CARTESIAN_POINT('Ctrl Pts',(17.1938082531612,69.6133761889749,0.));
#102969=CARTESIAN_POINT('Ctrl Pts',(17.1938082531612,69.6133761889749,12.));
#102970=CARTESIAN_POINT('Ctrl Pts',(17.1915586941192,69.6367511011898,0.));
#102971=CARTESIAN_POINT('Ctrl Pts',(17.1915586941192,69.6367511011898,12.));
#102972=CARTESIAN_POINT('Ctrl Pts',(17.1892818560002,69.6601670954269,0.));
#102973=CARTESIAN_POINT('Ctrl Pts',(17.1892818560002,69.6601670954269,12.));
#102974=CARTESIAN_POINT('Ctrl Pts',(17.1869776875666,69.6836240405164,0.));
#102975=CARTESIAN_POINT('Ctrl Pts',(17.1869776875666,69.6836240405164,12.));
#102976=CARTESIAN_POINT('Ctrl Pts',(17.1846461378973,69.7071218058178,0.));
#102977=CARTESIAN_POINT('Ctrl Pts',(17.1846461378973,69.7071218058178,12.));
#102978=CARTESIAN_POINT('Ctrl Pts',(17.1822871563842,69.7306602612155,0.));
#102979=CARTESIAN_POINT('Ctrl Pts',(17.1822871563842,69.7306602612155,12.));
#102980=CARTESIAN_POINT('Ctrl Pts',(17.179900692726,69.7542392771234,0.));
#102981=CARTESIAN_POINT('Ctrl Pts',(17.179900692726,69.7542392771234,12.));
#102982=CARTESIAN_POINT('Ctrl Pts',(17.1774866969256,69.777858724479,0.));
#102983=CARTESIAN_POINT('Ctrl Pts',(17.1774866969256,69.777858724479,12.));
#102984=CARTESIAN_POINT('Ctrl Pts',(17.1750451192885,69.8015184747398,0.));
#102985=CARTESIAN_POINT('Ctrl Pts',(17.1750451192885,69.8015184747398,12.));
#102986=CARTESIAN_POINT('Ctrl Pts',(17.1725759104252,69.8252183998702,0.));
#102987=CARTESIAN_POINT('Ctrl Pts',(17.1725759104252,69.8252183998702,12.));
#102988=CARTESIAN_POINT('Ctrl Pts',(17.1700790212474,69.8489583723407,0.));
#102989=CARTESIAN_POINT('Ctrl Pts',(17.1700790212474,69.8489583723407,12.));
#102990=CARTESIAN_POINT('Ctrl Pts',(17.167554402962,69.8727382651286,0.));
#102991=CARTESIAN_POINT('Ctrl Pts',(17.167554402962,69.8727382651286,12.));
#102992=CARTESIAN_POINT('Ctrl Pts',(17.1650020070686,69.8965579517147,0.));
#102993=CARTESIAN_POINT('Ctrl Pts',(17.1650020070686,69.8965579517147,12.));
#102994=CARTESIAN_POINT('Ctrl Pts',(17.1624217853578,69.9204173060781,0.));
#102995=CARTESIAN_POINT('Ctrl Pts',(17.1624217853578,69.9204173060781,12.));
#102996=CARTESIAN_POINT('Ctrl Pts',(17.1598136899144,69.9443162026865,0.));
#102997=CARTESIAN_POINT('Ctrl Pts',(17.1598136899144,69.9443162026865,12.));
#102998=CARTESIAN_POINT('Ctrl Pts',(17.157177673114,69.9682545164939,0.));
#102999=CARTESIAN_POINT('Ctrl Pts',(17.157177673114,69.9682545164939,12.));
#103000=CARTESIAN_POINT('Ctrl Pts',(17.154513687616,69.9922321229424,0.));
#103001=CARTESIAN_POINT('Ctrl Pts',(17.154513687616,69.9922321229424,12.));
#103002=CARTESIAN_POINT('Ctrl Pts',(17.1518216863623,70.0162488979584,0.));
#103003=CARTESIAN_POINT('Ctrl Pts',(17.1518216863623,70.0162488979584,12.));
#103004=CARTESIAN_POINT('Ctrl Pts',(17.1491016225749,70.0403047179483,0.));
#103005=CARTESIAN_POINT('Ctrl Pts',(17.1491016225749,70.0403047179483,12.));
#103006=CARTESIAN_POINT('Ctrl Pts',(17.1463534497594,70.0643994597873,0.));
#103007=CARTESIAN_POINT('Ctrl Pts',(17.1463534497594,70.0643994597873,12.));
#103008=CARTESIAN_POINT('Ctrl Pts',(17.1435771217018,70.0885330008179,0.));
#103009=CARTESIAN_POINT('Ctrl Pts',(17.1435771217018,70.0885330008179,12.));
#103010=CARTESIAN_POINT('Ctrl Pts',(17.1407725924617,70.1127052188522,0.));
#103011=CARTESIAN_POINT('Ctrl Pts',(17.1407725924617,70.1127052188522,12.));
#103012=CARTESIAN_POINT('Ctrl Pts',(17.1379398163709,70.1369159921687,0.));
#103013=CARTESIAN_POINT('Ctrl Pts',(17.1379398163709,70.1369159921687,12.));
#103014=CARTESIAN_POINT('Ctrl Pts',(17.1350787480312,70.1611651995083,0.));
#103015=CARTESIAN_POINT('Ctrl Pts',(17.1350787480312,70.1611651995083,12.));
#103016=CARTESIAN_POINT('Ctrl Pts',(17.1321893423182,70.1854527200631,0.));
#103017=CARTESIAN_POINT('Ctrl Pts',(17.1321893423182,70.1854527200631,12.));
#103018=CARTESIAN_POINT('Ctrl Pts',(17.1292715543778,70.2097784334747,0.));
#103019=CARTESIAN_POINT('Ctrl Pts',(17.1292715543778,70.2097784334747,12.));
#103020=CARTESIAN_POINT('Ctrl Pts',(17.1263253396202,70.2341422198363,0.));
#103021=CARTESIAN_POINT('Ctrl Pts',(17.1263253396202,70.2341422198363,12.));
#103022=CARTESIAN_POINT('Ctrl Pts',(17.1233506537176,70.2585439596901,0.));
#103023=CARTESIAN_POINT('Ctrl Pts',(17.1233506537176,70.2585439596901,12.));
#103024=CARTESIAN_POINT('Ctrl Pts',(17.1203474526031,70.2829835340238,0.));
#103025=CARTESIAN_POINT('Ctrl Pts',(17.1203474526031,70.2829835340238,12.));
#103026=CARTESIAN_POINT('Ctrl Pts',(17.1173156924733,70.3074608242608,0.));
#103027=CARTESIAN_POINT('Ctrl Pts',(17.1173156924733,70.3074608242608,12.));
#103028=CARTESIAN_POINT('Ctrl Pts',(17.1142553297867,70.3319757122568,0.));
#103029=CARTESIAN_POINT('Ctrl Pts',(17.1142553297867,70.3319757122568,12.));
#103030=CARTESIAN_POINT('Ctrl Pts',(17.1111663212568,70.3565280803022,0.));
#103031=CARTESIAN_POINT('Ctrl Pts',(17.1111663212568,70.3565280803022,12.));
#103032=CARTESIAN_POINT('Ctrl Pts',(17.1080486238499,70.3811178111201,0.));
#103033=CARTESIAN_POINT('Ctrl Pts',(17.1080486238499,70.3811178111201,12.));
#103034=CARTESIAN_POINT('Ctrl Pts',(17.1049021947834,70.4057447878624,0.));
#103035=CARTESIAN_POINT('Ctrl Pts',(17.1049021947834,70.4057447878624,12.));
#103036=CARTESIAN_POINT('Ctrl Pts',(17.1017269915292,70.430408894101,0.));
#103037=CARTESIAN_POINT('Ctrl Pts',(17.1017269915292,70.430408894101,12.));
#103038=CARTESIAN_POINT('Ctrl Pts',(17.0985229718124,70.4551100138238,0.));
#103039=CARTESIAN_POINT('Ctrl Pts',(17.0985229718124,70.4551100138238,12.));
#103040=CARTESIAN_POINT('Ctrl Pts',(17.0952900936048,70.4798480314381,0.));
#103041=CARTESIAN_POINT('Ctrl Pts',(17.0952900936048,70.4798480314381,12.));
#103042=CARTESIAN_POINT('Ctrl Pts',(17.0920283151219,70.5046228317677,0.));
#103043=CARTESIAN_POINT('Ctrl Pts',(17.0920283151219,70.5046228317677,12.));
#103044=CARTESIAN_POINT('Ctrl Pts',(17.088737594822,70.5294343000513,0.));
#103045=CARTESIAN_POINT('Ctrl Pts',(17.088737594822,70.5294343000513,12.));
#103046=CARTESIAN_POINT('Ctrl Pts',(17.0854178914087,70.5542823219331,0.));
#103047=CARTESIAN_POINT('Ctrl Pts',(17.0854178914087,70.5542823219331,12.));
#103048=CARTESIAN_POINT('Ctrl Pts',(17.082069163831,70.5791667834582,0.));
#103049=CARTESIAN_POINT('Ctrl Pts',(17.082069163831,70.5791667834582,12.));
#103050=CARTESIAN_POINT('Ctrl Pts',(17.0786913712764,70.6040875710749,0.));
#103051=CARTESIAN_POINT('Ctrl Pts',(17.0786913712764,70.6040875710749,12.));
#103052=CARTESIAN_POINT('Ctrl Pts',(17.0752844731678,70.6290445716337,0.));
#103053=CARTESIAN_POINT('Ctrl Pts',(17.0752844731678,70.6290445716337,12.));
#103054=CARTESIAN_POINT('Ctrl Pts',(17.0718484291624,70.6540376723841,0.));
#103055=CARTESIAN_POINT('Ctrl Pts',(17.0718484291624,70.6540376723841,12.));
#103056=CARTESIAN_POINT('Ctrl Pts',(17.0683831991532,70.6790667609679,0.));
#103057=CARTESIAN_POINT('Ctrl Pts',(17.0683831991532,70.6790667609679,12.));
#103058=CARTESIAN_POINT('Ctrl Pts',(17.0648887432713,70.7041317254125,0.));
#103059=CARTESIAN_POINT('Ctrl Pts',(17.0648887432713,70.7041317254125,12.));
#103060=CARTESIAN_POINT('Ctrl Pts',(17.0613650218787,70.7292324541341,0.));
#103061=CARTESIAN_POINT('Ctrl Pts',(17.0613650218787,70.7292324541341,12.));
#103062=CARTESIAN_POINT('Ctrl Pts',(17.0578119955649,70.7543688359374,0.));
#103063=CARTESIAN_POINT('Ctrl Pts',(17.0578119955649,70.7543688359374,12.));
#103064=CARTESIAN_POINT('Ctrl Pts',(17.0542296251462,70.7795407600127,0.));
#103065=CARTESIAN_POINT('Ctrl Pts',(17.0542296251462,70.7795407600127,12.));
#103066=CARTESIAN_POINT('Ctrl Pts',(17.0506178716664,70.8047481159306,0.));
#103067=CARTESIAN_POINT('Ctrl Pts',(17.0506178716664,70.8047481159306,12.));
#103068=CARTESIAN_POINT('Ctrl Pts',(17.0469766964005,70.8299907936346,0.));
#103069=CARTESIAN_POINT('Ctrl Pts',(17.0469766964005,70.8299907936346,12.));
#103070=CARTESIAN_POINT('Ctrl Pts',(17.0433060608478,70.8552686834435,0.));
#103071=CARTESIAN_POINT('Ctrl Pts',(17.0433060608478,70.8552686834435,12.));
#103072=CARTESIAN_POINT('Ctrl Pts',(17.0396059267279,70.8805816760507,0.));
#103073=CARTESIAN_POINT('Ctrl Pts',(17.0396059267279,70.8805816760507,12.));
#103074=CARTESIAN_POINT('Ctrl Pts',(17.0358762559786,70.9059296625214,0.));
#103075=CARTESIAN_POINT('Ctrl Pts',(17.0358762559786,70.9059296625214,12.));
#103076=CARTESIAN_POINT('Ctrl Pts',(17.0321170107562,70.9313125342872,0.));
#103077=CARTESIAN_POINT('Ctrl Pts',(17.0321170107562,70.9313125342872,12.));
#103078=CARTESIAN_POINT('Ctrl Pts',(17.028328153439,70.9567301831355,0.));
#103079=CARTESIAN_POINT('Ctrl Pts',(17.028328153439,70.9567301831355,12.));
#103080=CARTESIAN_POINT('Ctrl Pts',(17.0245096466228,70.9821825012134,0.));
#103081=CARTESIAN_POINT('Ctrl Pts',(17.0245096466228,70.9821825012134,12.));
#103082=CARTESIAN_POINT('Ctrl Pts',(17.0206614531165,71.0076693810303,0.));
#103083=CARTESIAN_POINT('Ctrl Pts',(17.0206614531165,71.0076693810303,12.));
#103084=CARTESIAN_POINT('Ctrl Pts',(17.0167835359419,71.0331907154575,0.));
#103085=CARTESIAN_POINT('Ctrl Pts',(17.0167835359419,71.0331907154575,12.));
#103086=CARTESIAN_POINT('Ctrl Pts',(17.0128758583335,71.0587463977266,0.));
#103087=CARTESIAN_POINT('Ctrl Pts',(17.0128758583335,71.0587463977266,12.));
#103088=CARTESIAN_POINT('Ctrl Pts',(17.0089383837437,71.0843363214216,0.));
#103089=CARTESIAN_POINT('Ctrl Pts',(17.0089383837437,71.0843363214216,12.));
#103090=CARTESIAN_POINT('Ctrl Pts',(17.0049710758393,71.1099603804779,0.));
#103091=CARTESIAN_POINT('Ctrl Pts',(17.0049710758393,71.1099603804779,12.));
#103092=CARTESIAN_POINT('Ctrl Pts',(17.0009738984935,71.1356184691799,0.));
#103093=CARTESIAN_POINT('Ctrl Pts',(17.0009738984935,71.1356184691799,12.));
#103094=CARTESIAN_POINT('Ctrl Pts',(16.9969468157824,71.1613104821565,0.));
#103095=CARTESIAN_POINT('Ctrl Pts',(16.9969468157824,71.1613104821565,12.));
#103096=CARTESIAN_POINT('Ctrl Pts',(16.9928897919829,71.1870363143742,0.));
#103097=CARTESIAN_POINT('Ctrl Pts',(16.9928897919829,71.1870363143742,12.));
#103098=CARTESIAN_POINT('Ctrl Pts',(16.9888027915743,71.2127958611248,0.));
#103099=CARTESIAN_POINT('Ctrl Pts',(16.9888027915743,71.2127958611248,12.));
#103100=CARTESIAN_POINT('Ctrl Pts',(16.9846857792385,71.2385890180233,0.));
#103101=CARTESIAN_POINT('Ctrl Pts',(16.9846857792385,71.2385890180233,12.));
#103102=CARTESIAN_POINT('Ctrl Pts',(16.9805387198573,71.2644156810209,0.));
#103103=CARTESIAN_POINT('Ctrl Pts',(16.9805387198573,71.2644156810209,12.));
#103104=CARTESIAN_POINT('Ctrl Pts',(16.9763615785138,71.2902757464127,0.));
#103105=CARTESIAN_POINT('Ctrl Pts',(16.9763615785138,71.2902757464127,12.));
#103106=CARTESIAN_POINT('Ctrl Pts',(16.9721543204951,71.3161691108425,0.));
#103107=CARTESIAN_POINT('Ctrl Pts',(16.9721543204951,71.3161691108425,12.));
#103108=CARTESIAN_POINT('Ctrl Pts',(16.9679169112993,71.3420956713072,0.));
#103109=CARTESIAN_POINT('Ctrl Pts',(16.9679169112993,71.3420956713072,12.));
#103110=CARTESIAN_POINT('Ctrl Pts',(16.9636493166395,71.3680553251548,0.));
#103111=CARTESIAN_POINT('Ctrl Pts',(16.9636493166395,71.3680553251548,12.));
#103112=CARTESIAN_POINT('Ctrl Pts',(16.9593515024274,71.3940479700663,0.));
#103113=CARTESIAN_POINT('Ctrl Pts',(16.9593515024274,71.3940479700663,12.));
#103114=CARTESIAN_POINT('Ctrl Pts',(16.9550234347619,71.4200735040374,0.));
#103115=CARTESIAN_POINT('Ctrl Pts',(16.9550234347619,71.4200735040374,12.));
#103116=CARTESIAN_POINT('Ctrl Pts',(16.9506650799188,71.4461318253561,0.));
#103117=CARTESIAN_POINT('Ctrl Pts',(16.9506650799188,71.4461318253561,12.));
#103118=CARTESIAN_POINT('Ctrl Pts',(16.9462764043445,71.4722228325805,0.));
#103119=CARTESIAN_POINT('Ctrl Pts',(16.9462764043445,71.4722228325805,12.));
#103120=CARTESIAN_POINT('Ctrl Pts',(16.9418573746492,71.498346424507,0.));
#103121=CARTESIAN_POINT('Ctrl Pts',(16.9418573746492,71.498346424507,12.));
#103122=CARTESIAN_POINT('Ctrl Pts',(16.9374079576204,71.5245025002154,0.));
#103123=CARTESIAN_POINT('Ctrl Pts',(16.9374079576204,71.5245025002154,12.));
#103124=CARTESIAN_POINT('Ctrl Pts',(16.9329281202379,71.5506909591139,0.));
#103125=CARTESIAN_POINT('Ctrl Pts',(16.9329281202379,71.5506909591139,12.));
#103126=CARTESIAN_POINT('Ctrl Pts',(16.9284178296934,71.5769117009844,0.));
#103127=CARTESIAN_POINT('Ctrl Pts',(16.9284178296934,71.5769117009844,12.));
#103128=CARTESIAN_POINT('Ctrl Pts',(16.923877053407,71.6031646260169,0.));
#103129=CARTESIAN_POINT('Ctrl Pts',(16.923877053407,71.6031646260169,12.));
#103130=CARTESIAN_POINT('Ctrl Pts',(16.9193057590605,71.6294496348644,0.));
#103131=CARTESIAN_POINT('Ctrl Pts',(16.9193057590605,71.6294496348644,12.));
#103132=CARTESIAN_POINT('Ctrl Pts',(16.9147039145715,71.6557666285908,0.));
#103133=CARTESIAN_POINT('Ctrl Pts',(16.9147039145715,71.6557666285908,12.));
#103134=CARTESIAN_POINT('Ctrl Pts',(16.9100714880367,71.6821155085605,0.));
#103135=CARTESIAN_POINT('Ctrl Pts',(16.9100714880367,71.6821155085605,12.));
#103136=CARTESIAN_POINT('Ctrl Pts',(16.9054084476847,71.7084961763355,0.));
#103137=CARTESIAN_POINT('Ctrl Pts',(16.9054084476847,71.7084961763355,12.));
#103138=CARTESIAN_POINT('Ctrl Pts',(16.9007147618344,71.7349085335796,0.));
#103139=CARTESIAN_POINT('Ctrl Pts',(16.9007147618344,71.7349085335796,12.));
#103140=CARTESIAN_POINT('Ctrl Pts',(16.8959903988411,71.761352481924,0.));
#103141=CARTESIAN_POINT('Ctrl Pts',(16.8959903988411,71.761352481924,12.));
#103142=CARTESIAN_POINT('Ctrl Pts',(16.8912353270944,71.7878279229556,0.));
#103143=CARTESIAN_POINT('Ctrl Pts',(16.8912353270944,71.7878279229556,12.));
#103144=CARTESIAN_POINT('Ctrl Pts',(16.8864495151347,71.8143347584977,0.));
#103145=CARTESIAN_POINT('Ctrl Pts',(16.8864495151347,71.8143347584977,12.));
#103146=CARTESIAN_POINT('Ctrl Pts',(16.8816329317473,71.8408728908269,0.));
#103147=CARTESIAN_POINT('Ctrl Pts',(16.8816329317473,71.8408728908269,12.));
#103148=CARTESIAN_POINT('Ctrl Pts',(16.87678554607,71.8674422229151,0.));
#103149=CARTESIAN_POINT('Ctrl Pts',(16.87678554607,71.8674422229151,12.));
#103150=CARTESIAN_POINT('Ctrl Pts',(16.8719073276967,71.8940426586521,0.));
#103151=CARTESIAN_POINT('Ctrl Pts',(16.8719073276967,71.8940426586521,12.));
#103152=CARTESIAN_POINT('Ctrl Pts',(16.8669982467915,71.920674103086,0.));
#103153=CARTESIAN_POINT('Ctrl Pts',(16.8669982467915,71.920674103086,12.));
#103154=CARTESIAN_POINT('Ctrl Pts',(16.8620582738431,71.9473364618889,0.));
#103155=CARTESIAN_POINT('Ctrl Pts',(16.8620582738431,71.9473364618889,12.));
#103156=CARTESIAN_POINT('Ctrl Pts',(16.8570873794264,71.9740296408319,0.));
#103157=CARTESIAN_POINT('Ctrl Pts',(16.8570873794264,71.9740296408319,12.));
#103158=CARTESIAN_POINT('Ctrl Pts',(16.8520855339444,72.0007535452071,0.));
#103159=CARTESIAN_POINT('Ctrl Pts',(16.8520855339444,72.0007535452071,12.));
#103160=CARTESIAN_POINT('Ctrl Pts',(16.8470527074278,72.0275080793742,0.));
#103161=CARTESIAN_POINT('Ctrl Pts',(16.8470527074278,72.0275080793742,12.));
#103162=CARTESIAN_POINT('Ctrl Pts',(16.8419888691984,72.0542931459865,0.));
#103163=CARTESIAN_POINT('Ctrl Pts',(16.8419888691984,72.0542931459865,12.));
#103164=CARTESIAN_POINT('Ctrl Pts',(16.8368939881457,72.0811086466177,0.));
#103165=CARTESIAN_POINT('Ctrl Pts',(16.8368939881457,72.0811086466177,12.));
#103166=CARTESIAN_POINT('Ctrl Pts',(16.8317680333415,72.1079544831569,0.));
#103167=CARTESIAN_POINT('Ctrl Pts',(16.8317680333415,72.1079544831569,12.));
#103168=CARTESIAN_POINT('Ctrl Pts',(16.8266109745801,72.1348305590233,0.));
#103169=CARTESIAN_POINT('Ctrl Pts',(16.8266109745801,72.1348305590233,12.));
#103170=CARTESIAN_POINT('Ctrl Pts',(16.8214227828941,72.1617367803226,0.));
#103171=CARTESIAN_POINT('Ctrl Pts',(16.8214227828941,72.1617367803226,12.));
#103172=CARTESIAN_POINT('Ctrl Pts',(16.8162034312257,72.1886730573389,0.));
#103173=CARTESIAN_POINT('Ctrl Pts',(16.8162034312257,72.1886730573389,12.));
#103174=CARTESIAN_POINT('Ctrl Pts',(16.8109528945876,72.2156393048868,0.));
#103175=CARTESIAN_POINT('Ctrl Pts',(16.8109528945876,72.2156393048868,12.));
#103176=CARTESIAN_POINT('Ctrl Pts',(16.8056711485797,72.242635439009,0.));
#103177=CARTESIAN_POINT('Ctrl Pts',(16.8056711485797,72.242635439009,12.));
#103178=CARTESIAN_POINT('Ctrl Pts',(16.800358168223,72.2696613743687,0.));
#103179=CARTESIAN_POINT('Ctrl Pts',(16.800358168223,72.2696613743687,12.));
#103180=CARTESIAN_POINT('Ctrl Pts',(16.7950139266117,72.2967170212331,0.));
#103181=CARTESIAN_POINT('Ctrl Pts',(16.7950139266117,72.2967170212331,12.));
#103182=CARTESIAN_POINT('Ctrl Pts',(16.7896383937839,72.323802282931,0.));
#103183=CARTESIAN_POINT('Ctrl Pts',(16.7896383937839,72.323802282931,12.));
#103184=CARTESIAN_POINT('Ctrl Pts',(16.7842315351402,72.3509170523038,0.));
#103185=CARTESIAN_POINT('Ctrl Pts',(16.7842315351402,72.3509170523038,12.));
#103186=CARTESIAN_POINT('Ctrl Pts',(16.7787933137551,72.3780612168057,0.));
#103187=CARTESIAN_POINT('Ctrl Pts',(16.7787933137551,72.3780612168057,12.));
#103188=CARTESIAN_POINT('Ctrl Pts',(16.7733236932185,72.4052346648058,0.));
#103189=CARTESIAN_POINT('Ctrl Pts',(16.7733236932185,72.4052346648058,12.));
#103190=CARTESIAN_POINT('Ctrl Pts',(16.7678226404189,72.4324372916884,0.));
#103191=CARTESIAN_POINT('Ctrl Pts',(16.7678226404189,72.4324372916884,12.));
#103192=CARTESIAN_POINT('Ctrl Pts',(16.7622901280741,72.4596690055347,0.));
#103193=CARTESIAN_POINT('Ctrl Pts',(16.7622901280741,72.4596690055347,12.));
#103194=CARTESIAN_POINT('Ctrl Pts',(16.7567261380614,72.4869297342051,0.));
#103195=CARTESIAN_POINT('Ctrl Pts',(16.7567261380614,72.4869297342051,12.));
#103196=CARTESIAN_POINT('Ctrl Pts',(16.7511306618793,72.5142194273203,0.));
#103197=CARTESIAN_POINT('Ctrl Pts',(16.7511306618793,72.5142194273203,12.));
#103198=CARTESIAN_POINT('Ctrl Pts',(16.7455036973724,72.5415380515905,0.));
#103199=CARTESIAN_POINT('Ctrl Pts',(16.7455036973724,72.5415380515905,12.));
#103200=CARTESIAN_POINT('Ctrl Pts',(16.7409769365953,72.563416080574,0.));
#103201=CARTESIAN_POINT('Ctrl Pts',(16.7409769365953,72.563416080574,12.));
#103202=CARTESIAN_POINT('Ctrl Pts',(16.7375676985272,72.5798376087406,0.));
#103203=CARTESIAN_POINT('Ctrl Pts',(16.7375676985272,72.5798376087406,12.));
#103204=CARTESIAN_POINT('Ctrl Pts',(16.7352885767459,72.5907910745874,0.));
#103205=CARTESIAN_POINT('Ctrl Pts',(16.7352885767459,72.5907910745874,12.));
#103206=CARTESIAN_POINT('Ctrl Pts',(16.7341474417544,72.5962692526112,0.));
#103207=CARTESIAN_POINT('Ctrl Pts',(16.7341474417544,72.5962692526112,12.));
#103208=CARTESIAN_POINT('',(17.2912529479484,67.8307641965655,0.));
#103209=CARTESIAN_POINT('Ctrl Pts',(17.2912529479484,67.8307641965655,0.));
#103210=CARTESIAN_POINT('Ctrl Pts',(17.2912149114119,67.8346476309018,0.));
#103211=CARTESIAN_POINT('Ctrl Pts',(17.2911366591348,67.842419897098,0.));
#103212=CARTESIAN_POINT('Ctrl Pts',(17.291012743109,67.8540944889687,0.));
#103213=CARTESIAN_POINT('Ctrl Pts',(17.2908344459694,67.8696929978782,0.));
#103214=CARTESIAN_POINT('Ctrl Pts',(17.2905897723949,67.8892451049608,0.));
#103215=CARTESIAN_POINT('Ctrl Pts',(17.2903232740694,67.9088511496686,0.));
#103216=CARTESIAN_POINT('Ctrl Pts',(17.2900349103981,67.9285110571741,0.));
#103217=CARTESIAN_POINT('Ctrl Pts',(17.2897246158941,67.9482246901667,0.));
#103218=CARTESIAN_POINT('Ctrl Pts',(17.2893923013894,67.9679918502579,0.));
#103219=CARTESIAN_POINT('Ctrl Pts',(17.2890378644866,67.987812304921,0.));
#103220=CARTESIAN_POINT('Ctrl Pts',(17.28866119774,68.007685808115,0.));
#103221=CARTESIAN_POINT('Ctrl Pts',(17.2882621974721,68.0276121227356,0.));
#103222=CARTESIAN_POINT('Ctrl Pts',(17.2878407730961,68.0475910442424,0.));
#103223=CARTESIAN_POINT('Ctrl Pts',(17.2873968440839,68.0676223930412,0.));
#103224=CARTESIAN_POINT('Ctrl Pts',(17.2869303355432,68.0877060033205,0.));
#103225=CARTESIAN_POINT('Ctrl Pts',(17.2864411745459,68.1078417137877,0.));
#103226=CARTESIAN_POINT('Ctrl Pts',(17.2859292855705,68.1280293561511,0.));
#103227=CARTESIAN_POINT('Ctrl Pts',(17.2853945882072,68.1482687493226,0.));
#103228=CARTESIAN_POINT('Ctrl Pts',(17.2848369995293,68.1685597054232,0.));
#103229=CARTESIAN_POINT('Ctrl Pts',(17.2842564355799,68.1889020335427,0.));
#103230=CARTESIAN_POINT('Ctrl Pts',(17.2836528130819,68.2092955440567,0.));
#103231=CARTESIAN_POINT('Ctrl Pts',(17.2830260513867,68.2297400535294,0.));
#103232=CARTESIAN_POINT('Ctrl Pts',(17.2823760723874,68.2502353845071,0.));
#103233=CARTESIAN_POINT('Ctrl Pts',(17.2817027995831,68.2707813631731,0.));
#103234=CARTESIAN_POINT('Ctrl Pts',(17.2810061574353,68.2913778177261,0.));
#103235=CARTESIAN_POINT('Ctrl Pts',(17.2802860705815,68.3120245763914,0.));
#103236=CARTESIAN_POINT('Ctrl Pts',(17.2795424631799,68.3327214657575,0.));
#103237=CARTESIAN_POINT('Ctrl Pts',(17.2787752592484,68.3534683116515,0.));
#103238=CARTESIAN_POINT('Ctrl Pts',(17.2779843829608,68.3742649398964,0.));
#103239=CARTESIAN_POINT('Ctrl Pts',(17.2771697589384,68.3951111770487,0.));
#103240=CARTESIAN_POINT('Ctrl Pts',(17.2763313126018,68.4160068512753,0.));
#103241=CARTESIAN_POINT('Ctrl Pts',(17.2754689702992,68.436951792677,0.));
#103242=CARTESIAN_POINT('Ctrl Pts',(17.2745826591119,68.4579458328185,0.));
#103243=CARTESIAN_POINT('Ctrl Pts',(17.2736723067365,68.4789888044351,0.));
#103244=CARTESIAN_POINT('Ctrl Pts',(17.2727378413489,68.5000805410911,0.));
#103245=CARTESIAN_POINT('Ctrl Pts',(17.2717791914544,68.521220876786,0.));
#103246=CARTESIAN_POINT('Ctrl Pts',(17.2707962858919,68.5424096459772,0.));
#103247=CARTESIAN_POINT('Ctrl Pts',(17.269789053896,68.5636466837517,0.));
#103248=CARTESIAN_POINT('Ctrl Pts',(17.2687574251429,68.5849318259449,0.));
#103249=CARTESIAN_POINT('Ctrl Pts',(17.2677013298057,68.6062649092764,0.));
#103250=CARTESIAN_POINT('Ctrl Pts',(17.2666206986084,68.6276457714729,0.));
#103251=CARTESIAN_POINT('Ctrl Pts',(17.2655154627928,68.6490742512057,0.));
#103252=CARTESIAN_POINT('Ctrl Pts',(17.2643855540892,68.6705501880249,0.));
#103253=CARTESIAN_POINT('Ctrl Pts',(17.2632309046892,68.6920734222938,0.));
#103254=CARTESIAN_POINT('Ctrl Pts',(17.2620514472182,68.7136437951097,0.));
#103255=CARTESIAN_POINT('Ctrl Pts',(17.2608471147185,68.7352611482547,0.));
#103256=CARTESIAN_POINT('Ctrl Pts',(17.259617840655,68.7569253242333,0.));
#103257=CARTESIAN_POINT('Ctrl Pts',(17.2583635589198,68.7786361662882,0.));
#103258=CARTESIAN_POINT('Ctrl Pts',(17.2570842038383,68.8003935184184,0.));
#103259=CARTESIAN_POINT('Ctrl Pts',(17.2557797101812,68.8221972253941,0.));
#103260=CARTESIAN_POINT('Ctrl Pts',(17.2544500131624,68.844047132755,0.));
#103261=CARTESIAN_POINT('Ctrl Pts',(17.2530950484258,68.8659430867972,0.));
#103262=CARTESIAN_POINT('Ctrl Pts',(17.2517147520376,68.8878849345557,0.));
#103263=CARTESIAN_POINT('Ctrl Pts',(17.2503090604792,68.909872523787,0.));
#103264=CARTESIAN_POINT('Ctrl Pts',(17.248877910643,68.9319057029409,0.));
#103265=CARTESIAN_POINT('Ctrl Pts',(17.2474212398275,68.9539843211619,0.));
#103266=CARTESIAN_POINT('Ctrl Pts',(17.2459389857327,68.9761082282922,0.));
#103267=CARTESIAN_POINT('Ctrl Pts',(17.2444310864585,68.9982772748694,0.));
#103268=CARTESIAN_POINT('Ctrl Pts',(17.2428974805044,69.0204913121225,0.));
#103269=CARTESIAN_POINT('Ctrl Pts',(17.2413381067723,69.0427501919636,0.));
#103270=CARTESIAN_POINT('Ctrl Pts',(17.2397529045589,69.065053766986,0.));
#103271=CARTESIAN_POINT('Ctrl Pts',(17.2381418135491,69.0874018904599,0.));
#103272=CARTESIAN_POINT('Ctrl Pts',(17.2365047738125,69.1097944163245,0.));
#103273=CARTESIAN_POINT('Ctrl Pts',(17.2348417258015,69.1322311991752,0.));
#103274=CARTESIAN_POINT('Ctrl Pts',(17.2331526103506,69.1547120942527,0.));
#103275=CARTESIAN_POINT('Ctrl Pts',(17.23143736867,69.1772369574447,0.));
#103276=CARTESIAN_POINT('Ctrl Pts',(17.2296959423407,69.1998056452828,0.));
#103277=CARTESIAN_POINT('Ctrl Pts',(17.227928273312,69.222418014938,0.));
#103278=CARTESIAN_POINT('Ctrl Pts',(17.226134303902,69.2450739242109,0.));
#103279=CARTESIAN_POINT('Ctrl Pts',(17.224313976797,69.2677732315224,0.));
#103280=CARTESIAN_POINT('Ctrl Pts',(17.2224672350438,69.2905157959166,0.));
#103281=CARTESIAN_POINT('Ctrl Pts',(17.2205940220459,69.3133014770555,0.));
#103282=CARTESIAN_POINT('Ctrl Pts',(17.2186942815602,69.3361301352141,0.));
#103283=CARTESIAN_POINT('Ctrl Pts',(17.2167679576984,69.3590016312692,0.));
#103284=CARTESIAN_POINT('Ctrl Pts',(17.2148149949252,69.3819158266916,0.));
#103285=CARTESIAN_POINT('Ctrl Pts',(17.2128353380502,69.404872583548,0.));
#103286=CARTESIAN_POINT('Ctrl Pts',(17.2108289322254,69.4278717644973,0.));
#103287=CARTESIAN_POINT('Ctrl Pts',(17.2087957229423,69.450913232785,0.));
#103288=CARTESIAN_POINT('Ctrl Pts',(17.2067356560336,69.4739968522313,0.));
#103289=CARTESIAN_POINT('Ctrl Pts',(17.2046486776708,69.4971224872269,0.));
#103290=CARTESIAN_POINT('Ctrl Pts',(17.2025347343577,69.5202900027367,0.));
#103291=CARTESIAN_POINT('Ctrl Pts',(17.2003937729268,69.5434992642944,0.));
#103292=CARTESIAN_POINT('Ctrl Pts',(17.1982257405377,69.5667501379969,0.));
#103293=CARTESIAN_POINT('Ctrl Pts',(17.196030584678,69.5900424904921,0.));
#103294=CARTESIAN_POINT('Ctrl Pts',(17.1938082531612,69.6133761889749,0.));
#103295=CARTESIAN_POINT('Ctrl Pts',(17.1915586941192,69.6367511011898,0.));
#103296=CARTESIAN_POINT('Ctrl Pts',(17.1892818560002,69.6601670954269,0.));
#103297=CARTESIAN_POINT('Ctrl Pts',(17.1869776875666,69.6836240405164,0.));
#103298=CARTESIAN_POINT('Ctrl Pts',(17.1846461378973,69.7071218058178,0.));
#103299=CARTESIAN_POINT('Ctrl Pts',(17.1822871563842,69.7306602612155,0.));
#103300=CARTESIAN_POINT('Ctrl Pts',(17.179900692726,69.7542392771234,0.));
#103301=CARTESIAN_POINT('Ctrl Pts',(17.1774866969256,69.777858724479,0.));
#103302=CARTESIAN_POINT('Ctrl Pts',(17.1750451192885,69.8015184747398,0.));
#103303=CARTESIAN_POINT('Ctrl Pts',(17.1725759104252,69.8252183998702,0.));
#103304=CARTESIAN_POINT('Ctrl Pts',(17.1700790212474,69.8489583723407,0.));
#103305=CARTESIAN_POINT('Ctrl Pts',(17.167554402962,69.8727382651286,0.));
#103306=CARTESIAN_POINT('Ctrl Pts',(17.1650020070686,69.8965579517147,0.));
#103307=CARTESIAN_POINT('Ctrl Pts',(17.1624217853578,69.9204173060781,0.));
#103308=CARTESIAN_POINT('Ctrl Pts',(17.1598136899144,69.9443162026865,0.));
#103309=CARTESIAN_POINT('Ctrl Pts',(17.157177673114,69.9682545164939,0.));
#103310=CARTESIAN_POINT('Ctrl Pts',(17.154513687616,69.9922321229424,0.));
#103311=CARTESIAN_POINT('Ctrl Pts',(17.1518216863623,70.0162488979584,0.));
#103312=CARTESIAN_POINT('Ctrl Pts',(17.1491016225749,70.0403047179483,0.));
#103313=CARTESIAN_POINT('Ctrl Pts',(17.1463534497594,70.0643994597873,0.));
#103314=CARTESIAN_POINT('Ctrl Pts',(17.1435771217018,70.0885330008179,0.));
#103315=CARTESIAN_POINT('Ctrl Pts',(17.1407725924617,70.1127052188522,0.));
#103316=CARTESIAN_POINT('Ctrl Pts',(17.1379398163709,70.1369159921687,0.));
#103317=CARTESIAN_POINT('Ctrl Pts',(17.1350787480312,70.1611651995083,0.));
#103318=CARTESIAN_POINT('Ctrl Pts',(17.1321893423182,70.1854527200631,0.));
#103319=CARTESIAN_POINT('Ctrl Pts',(17.1292715543778,70.2097784334747,0.));
#103320=CARTESIAN_POINT('Ctrl Pts',(17.1263253396202,70.2341422198363,0.));
#103321=CARTESIAN_POINT('Ctrl Pts',(17.1233506537176,70.2585439596901,0.));
#103322=CARTESIAN_POINT('Ctrl Pts',(17.1203474526031,70.2829835340238,0.));
#103323=CARTESIAN_POINT('Ctrl Pts',(17.1173156924733,70.3074608242608,0.));
#103324=CARTESIAN_POINT('Ctrl Pts',(17.1142553297867,70.3319757122568,0.));
#103325=CARTESIAN_POINT('Ctrl Pts',(17.1111663212568,70.3565280803022,0.));
#103326=CARTESIAN_POINT('Ctrl Pts',(17.1080486238499,70.3811178111201,0.));
#103327=CARTESIAN_POINT('Ctrl Pts',(17.1049021947834,70.4057447878624,0.));
#103328=CARTESIAN_POINT('Ctrl Pts',(17.1017269915292,70.430408894101,0.));
#103329=CARTESIAN_POINT('Ctrl Pts',(17.0985229718124,70.4551100138238,0.));
#103330=CARTESIAN_POINT('Ctrl Pts',(17.0952900936048,70.4798480314381,0.));
#103331=CARTESIAN_POINT('Ctrl Pts',(17.0920283151219,70.5046228317677,0.));
#103332=CARTESIAN_POINT('Ctrl Pts',(17.088737594822,70.5294343000513,0.));
#103333=CARTESIAN_POINT('Ctrl Pts',(17.0854178914087,70.5542823219331,0.));
#103334=CARTESIAN_POINT('Ctrl Pts',(17.082069163831,70.5791667834582,0.));
#103335=CARTESIAN_POINT('Ctrl Pts',(17.0786913712764,70.6040875710749,0.));
#103336=CARTESIAN_POINT('Ctrl Pts',(17.0752844731678,70.6290445716337,0.));
#103337=CARTESIAN_POINT('Ctrl Pts',(17.0718484291624,70.6540376723841,0.));
#103338=CARTESIAN_POINT('Ctrl Pts',(17.0683831991532,70.6790667609679,0.));
#103339=CARTESIAN_POINT('Ctrl Pts',(17.0648887432713,70.7041317254125,0.));
#103340=CARTESIAN_POINT('Ctrl Pts',(17.0613650218787,70.7292324541341,0.));
#103341=CARTESIAN_POINT('Ctrl Pts',(17.0578119955649,70.7543688359374,0.));
#103342=CARTESIAN_POINT('Ctrl Pts',(17.0542296251462,70.7795407600127,0.));
#103343=CARTESIAN_POINT('Ctrl Pts',(17.0506178716664,70.8047481159306,0.));
#103344=CARTESIAN_POINT('Ctrl Pts',(17.0469766964005,70.8299907936346,0.));
#103345=CARTESIAN_POINT('Ctrl Pts',(17.0433060608478,70.8552686834435,0.));
#103346=CARTESIAN_POINT('Ctrl Pts',(17.0396059267279,70.8805816760507,0.));
#103347=CARTESIAN_POINT('Ctrl Pts',(17.0358762559786,70.9059296625214,0.));
#103348=CARTESIAN_POINT('Ctrl Pts',(17.0321170107562,70.9313125342872,0.));
#103349=CARTESIAN_POINT('Ctrl Pts',(17.028328153439,70.9567301831355,0.));
#103350=CARTESIAN_POINT('Ctrl Pts',(17.0245096466228,70.9821825012134,0.));
#103351=CARTESIAN_POINT('Ctrl Pts',(17.0206614531165,71.0076693810303,0.));
#103352=CARTESIAN_POINT('Ctrl Pts',(17.0167835359419,71.0331907154575,0.));
#103353=CARTESIAN_POINT('Ctrl Pts',(17.0128758583335,71.0587463977266,0.));
#103354=CARTESIAN_POINT('Ctrl Pts',(17.0089383837437,71.0843363214216,0.));
#103355=CARTESIAN_POINT('Ctrl Pts',(17.0049710758393,71.1099603804779,0.));
#103356=CARTESIAN_POINT('Ctrl Pts',(17.0009738984935,71.1356184691799,0.));
#103357=CARTESIAN_POINT('Ctrl Pts',(16.9969468157824,71.1613104821565,0.));
#103358=CARTESIAN_POINT('Ctrl Pts',(16.9928897919829,71.1870363143742,0.));
#103359=CARTESIAN_POINT('Ctrl Pts',(16.9888027915743,71.2127958611248,0.));
#103360=CARTESIAN_POINT('Ctrl Pts',(16.9846857792385,71.2385890180233,0.));
#103361=CARTESIAN_POINT('Ctrl Pts',(16.9805387198573,71.2644156810209,0.));
#103362=CARTESIAN_POINT('Ctrl Pts',(16.9763615785138,71.2902757464127,0.));
#103363=CARTESIAN_POINT('Ctrl Pts',(16.9721543204951,71.3161691108425,0.));
#103364=CARTESIAN_POINT('Ctrl Pts',(16.9679169112993,71.3420956713072,0.));
#103365=CARTESIAN_POINT('Ctrl Pts',(16.9636493166395,71.3680553251548,0.));
#103366=CARTESIAN_POINT('Ctrl Pts',(16.9593515024274,71.3940479700663,0.));
#103367=CARTESIAN_POINT('Ctrl Pts',(16.9550234347619,71.4200735040374,0.));
#103368=CARTESIAN_POINT('Ctrl Pts',(16.9506650799188,71.4461318253561,0.));
#103369=CARTESIAN_POINT('Ctrl Pts',(16.9462764043445,71.4722228325805,0.));
#103370=CARTESIAN_POINT('Ctrl Pts',(16.9418573746492,71.498346424507,0.));
#103371=CARTESIAN_POINT('Ctrl Pts',(16.9374079576204,71.5245025002154,0.));
#103372=CARTESIAN_POINT('Ctrl Pts',(16.9329281202379,71.5506909591139,0.));
#103373=CARTESIAN_POINT('Ctrl Pts',(16.9284178296934,71.5769117009844,0.));
#103374=CARTESIAN_POINT('Ctrl Pts',(16.923877053407,71.6031646260169,0.));
#103375=CARTESIAN_POINT('Ctrl Pts',(16.9193057590605,71.6294496348644,0.));
#103376=CARTESIAN_POINT('Ctrl Pts',(16.9147039145715,71.6557666285908,0.));
#103377=CARTESIAN_POINT('Ctrl Pts',(16.9100714880367,71.6821155085605,0.));
#103378=CARTESIAN_POINT('Ctrl Pts',(16.9054084476847,71.7084961763355,0.));
#103379=CARTESIAN_POINT('Ctrl Pts',(16.9007147618344,71.7349085335796,0.));
#103380=CARTESIAN_POINT('Ctrl Pts',(16.8959903988411,71.761352481924,0.));
#103381=CARTESIAN_POINT('Ctrl Pts',(16.8912353270944,71.7878279229556,0.));
#103382=CARTESIAN_POINT('Ctrl Pts',(16.8864495151347,71.8143347584977,0.));
#103383=CARTESIAN_POINT('Ctrl Pts',(16.8816329317473,71.8408728908269,0.));
#103384=CARTESIAN_POINT('Ctrl Pts',(16.87678554607,71.8674422229151,0.));
#103385=CARTESIAN_POINT('Ctrl Pts',(16.8719073276967,71.8940426586521,0.));
#103386=CARTESIAN_POINT('Ctrl Pts',(16.8669982467915,71.920674103086,0.));
#103387=CARTESIAN_POINT('Ctrl Pts',(16.8620582738431,71.9473364618889,0.));
#103388=CARTESIAN_POINT('Ctrl Pts',(16.8570873794264,71.9740296408319,0.));
#103389=CARTESIAN_POINT('Ctrl Pts',(16.8520855339444,72.0007535452071,0.));
#103390=CARTESIAN_POINT('Ctrl Pts',(16.8470527074278,72.0275080793742,0.));
#103391=CARTESIAN_POINT('Ctrl Pts',(16.8419888691984,72.0542931459865,0.));
#103392=CARTESIAN_POINT('Ctrl Pts',(16.8368939881457,72.0811086466177,0.));
#103393=CARTESIAN_POINT('Ctrl Pts',(16.8317680333415,72.1079544831569,0.));
#103394=CARTESIAN_POINT('Ctrl Pts',(16.8266109745801,72.1348305590233,0.));
#103395=CARTESIAN_POINT('Ctrl Pts',(16.8214227828941,72.1617367803226,0.));
#103396=CARTESIAN_POINT('Ctrl Pts',(16.8162034312257,72.1886730573389,0.));
#103397=CARTESIAN_POINT('Ctrl Pts',(16.8109528945876,72.2156393048868,0.));
#103398=CARTESIAN_POINT('Ctrl Pts',(16.8064254147766,72.2387802230663,0.));
#103399=CARTESIAN_POINT('Ctrl Pts',(16.8029374213802,72.2565380035008,0.));
#103400=CARTESIAN_POINT('Ctrl Pts',(16.8005027425889,72.2688994294959,0.));
#103401=CARTESIAN_POINT('Ctrl Pts',(16.7991305317793,72.2758557890967,0.));
#103402=CARTESIAN_POINT('Ctrl Pts',(16.7988252568807,72.2774028393484,0.));
#103403=CARTESIAN_POINT('',(17.2912529479484,67.8307641965655,12.));
#103404=CARTESIAN_POINT('',(17.2912529479484,67.8307641965655,0.));
#103405=CARTESIAN_POINT('Ctrl Pts',(16.7988252568807,72.2774028393484,12.));
#103406=CARTESIAN_POINT('Ctrl Pts',(16.7991305317793,72.2758557890967,12.));
#103407=CARTESIAN_POINT('Ctrl Pts',(16.8005027425889,72.2688994294959,12.));
#103408=CARTESIAN_POINT('Ctrl Pts',(16.8029374213802,72.2565380035008,12.));
#103409=CARTESIAN_POINT('Ctrl Pts',(16.8064254147766,72.2387802230663,12.));
#103410=CARTESIAN_POINT('Ctrl Pts',(16.8109528945876,72.2156393048868,12.));
#103411=CARTESIAN_POINT('Ctrl Pts',(16.8162034312257,72.1886730573389,12.));
#103412=CARTESIAN_POINT('Ctrl Pts',(16.8214227828941,72.1617367803226,12.));
#103413=CARTESIAN_POINT('Ctrl Pts',(16.8266109745801,72.1348305590233,12.));
#103414=CARTESIAN_POINT('Ctrl Pts',(16.8317680333415,72.1079544831569,12.));
#103415=CARTESIAN_POINT('Ctrl Pts',(16.8368939881457,72.0811086466177,12.));
#103416=CARTESIAN_POINT('Ctrl Pts',(16.8419888691984,72.0542931459865,12.));
#103417=CARTESIAN_POINT('Ctrl Pts',(16.8470527074278,72.0275080793742,12.));
#103418=CARTESIAN_POINT('Ctrl Pts',(16.8520855339444,72.0007535452071,12.));
#103419=CARTESIAN_POINT('Ctrl Pts',(16.8570873794264,71.9740296408319,12.));
#103420=CARTESIAN_POINT('Ctrl Pts',(16.8620582738431,71.9473364618889,12.));
#103421=CARTESIAN_POINT('Ctrl Pts',(16.8669982467915,71.920674103086,12.));
#103422=CARTESIAN_POINT('Ctrl Pts',(16.8719073276967,71.8940426586521,12.));
#103423=CARTESIAN_POINT('Ctrl Pts',(16.87678554607,71.8674422229151,12.));
#103424=CARTESIAN_POINT('Ctrl Pts',(16.8816329317473,71.8408728908269,12.));
#103425=CARTESIAN_POINT('Ctrl Pts',(16.8864495151347,71.8143347584977,12.));
#103426=CARTESIAN_POINT('Ctrl Pts',(16.8912353270944,71.7878279229556,12.));
#103427=CARTESIAN_POINT('Ctrl Pts',(16.8959903988411,71.761352481924,12.));
#103428=CARTESIAN_POINT('Ctrl Pts',(16.9007147618344,71.7349085335796,12.));
#103429=CARTESIAN_POINT('Ctrl Pts',(16.9054084476847,71.7084961763355,12.));
#103430=CARTESIAN_POINT('Ctrl Pts',(16.9100714880367,71.6821155085605,12.));
#103431=CARTESIAN_POINT('Ctrl Pts',(16.9147039145715,71.6557666285908,12.));
#103432=CARTESIAN_POINT('Ctrl Pts',(16.9193057590605,71.6294496348644,12.));
#103433=CARTESIAN_POINT('Ctrl Pts',(16.923877053407,71.6031646260169,12.));
#103434=CARTESIAN_POINT('Ctrl Pts',(16.9284178296934,71.5769117009844,12.));
#103435=CARTESIAN_POINT('Ctrl Pts',(16.9329281202379,71.5506909591139,12.));
#103436=CARTESIAN_POINT('Ctrl Pts',(16.9374079576204,71.5245025002154,12.));
#103437=CARTESIAN_POINT('Ctrl Pts',(16.9418573746492,71.498346424507,12.));
#103438=CARTESIAN_POINT('Ctrl Pts',(16.9462764043445,71.4722228325805,12.));
#103439=CARTESIAN_POINT('Ctrl Pts',(16.9506650799188,71.4461318253561,12.));
#103440=CARTESIAN_POINT('Ctrl Pts',(16.9550234347619,71.4200735040374,12.));
#103441=CARTESIAN_POINT('Ctrl Pts',(16.9593515024274,71.3940479700663,12.));
#103442=CARTESIAN_POINT('Ctrl Pts',(16.9636493166395,71.3680553251548,12.));
#103443=CARTESIAN_POINT('Ctrl Pts',(16.9679169112993,71.3420956713072,12.));
#103444=CARTESIAN_POINT('Ctrl Pts',(16.9721543204951,71.3161691108425,12.));
#103445=CARTESIAN_POINT('Ctrl Pts',(16.9763615785138,71.2902757464127,12.));
#103446=CARTESIAN_POINT('Ctrl Pts',(16.9805387198573,71.2644156810209,12.));
#103447=CARTESIAN_POINT('Ctrl Pts',(16.9846857792385,71.2385890180233,12.));
#103448=CARTESIAN_POINT('Ctrl Pts',(16.9888027915743,71.2127958611248,12.));
#103449=CARTESIAN_POINT('Ctrl Pts',(16.9928897919829,71.1870363143742,12.));
#103450=CARTESIAN_POINT('Ctrl Pts',(16.9969468157824,71.1613104821565,12.));
#103451=CARTESIAN_POINT('Ctrl Pts',(17.0009738984935,71.1356184691799,12.));
#103452=CARTESIAN_POINT('Ctrl Pts',(17.0049710758393,71.1099603804779,12.));
#103453=CARTESIAN_POINT('Ctrl Pts',(17.0089383837437,71.0843363214216,12.));
#103454=CARTESIAN_POINT('Ctrl Pts',(17.0128758583335,71.0587463977266,12.));
#103455=CARTESIAN_POINT('Ctrl Pts',(17.0167835359419,71.0331907154575,12.));
#103456=CARTESIAN_POINT('Ctrl Pts',(17.0206614531165,71.0076693810303,12.));
#103457=CARTESIAN_POINT('Ctrl Pts',(17.0245096466228,70.9821825012134,12.));
#103458=CARTESIAN_POINT('Ctrl Pts',(17.028328153439,70.9567301831355,12.));
#103459=CARTESIAN_POINT('Ctrl Pts',(17.0321170107562,70.9313125342872,12.));
#103460=CARTESIAN_POINT('Ctrl Pts',(17.0358762559786,70.9059296625214,12.));
#103461=CARTESIAN_POINT('Ctrl Pts',(17.0396059267279,70.8805816760507,12.));
#103462=CARTESIAN_POINT('Ctrl Pts',(17.0433060608478,70.8552686834435,12.));
#103463=CARTESIAN_POINT('Ctrl Pts',(17.0469766964005,70.8299907936346,12.));
#103464=CARTESIAN_POINT('Ctrl Pts',(17.0506178716664,70.8047481159306,12.));
#103465=CARTESIAN_POINT('Ctrl Pts',(17.0542296251462,70.7795407600127,12.));
#103466=CARTESIAN_POINT('Ctrl Pts',(17.0578119955649,70.7543688359374,12.));
#103467=CARTESIAN_POINT('Ctrl Pts',(17.0613650218787,70.7292324541341,12.));
#103468=CARTESIAN_POINT('Ctrl Pts',(17.0648887432713,70.7041317254125,12.));
#103469=CARTESIAN_POINT('Ctrl Pts',(17.0683831991532,70.6790667609679,12.));
#103470=CARTESIAN_POINT('Ctrl Pts',(17.0718484291624,70.6540376723841,12.));
#103471=CARTESIAN_POINT('Ctrl Pts',(17.0752844731678,70.6290445716337,12.));
#103472=CARTESIAN_POINT('Ctrl Pts',(17.0786913712764,70.6040875710749,12.));
#103473=CARTESIAN_POINT('Ctrl Pts',(17.082069163831,70.5791667834582,12.));
#103474=CARTESIAN_POINT('Ctrl Pts',(17.0854178914087,70.5542823219331,12.));
#103475=CARTESIAN_POINT('Ctrl Pts',(17.088737594822,70.5294343000513,12.));
#103476=CARTESIAN_POINT('Ctrl Pts',(17.0920283151219,70.5046228317677,12.));
#103477=CARTESIAN_POINT('Ctrl Pts',(17.0952900936048,70.4798480314381,12.));
#103478=CARTESIAN_POINT('Ctrl Pts',(17.0985229718124,70.4551100138238,12.));
#103479=CARTESIAN_POINT('Ctrl Pts',(17.1017269915292,70.430408894101,12.));
#103480=CARTESIAN_POINT('Ctrl Pts',(17.1049021947834,70.4057447878624,12.));
#103481=CARTESIAN_POINT('Ctrl Pts',(17.1080486238499,70.3811178111201,12.));
#103482=CARTESIAN_POINT('Ctrl Pts',(17.1111663212568,70.3565280803022,12.));
#103483=CARTESIAN_POINT('Ctrl Pts',(17.1142553297867,70.3319757122568,12.));
#103484=CARTESIAN_POINT('Ctrl Pts',(17.1173156924733,70.3074608242608,12.));
#103485=CARTESIAN_POINT('Ctrl Pts',(17.1203474526031,70.2829835340238,12.));
#103486=CARTESIAN_POINT('Ctrl Pts',(17.1233506537176,70.2585439596901,12.));
#103487=CARTESIAN_POINT('Ctrl Pts',(17.1263253396202,70.2341422198363,12.));
#103488=CARTESIAN_POINT('Ctrl Pts',(17.1292715543778,70.2097784334747,12.));
#103489=CARTESIAN_POINT('Ctrl Pts',(17.1321893423182,70.1854527200631,12.));
#103490=CARTESIAN_POINT('Ctrl Pts',(17.1350787480312,70.1611651995083,12.));
#103491=CARTESIAN_POINT('Ctrl Pts',(17.1379398163709,70.1369159921687,12.));
#103492=CARTESIAN_POINT('Ctrl Pts',(17.1407725924617,70.1127052188522,12.));
#103493=CARTESIAN_POINT('Ctrl Pts',(17.1435771217018,70.0885330008179,12.));
#103494=CARTESIAN_POINT('Ctrl Pts',(17.1463534497594,70.0643994597873,12.));
#103495=CARTESIAN_POINT('Ctrl Pts',(17.1491016225749,70.0403047179483,12.));
#103496=CARTESIAN_POINT('Ctrl Pts',(17.1518216863623,70.0162488979584,12.));
#103497=CARTESIAN_POINT('Ctrl Pts',(17.154513687616,69.9922321229424,12.));
#103498=CARTESIAN_POINT('Ctrl Pts',(17.157177673114,69.9682545164939,12.));
#103499=CARTESIAN_POINT('Ctrl Pts',(17.1598136899144,69.9443162026865,12.));
#103500=CARTESIAN_POINT('Ctrl Pts',(17.1624217853578,69.9204173060781,12.));
#103501=CARTESIAN_POINT('Ctrl Pts',(17.1650020070686,69.8965579517147,12.));
#103502=CARTESIAN_POINT('Ctrl Pts',(17.167554402962,69.8727382651286,12.));
#103503=CARTESIAN_POINT('Ctrl Pts',(17.1700790212474,69.8489583723407,12.));
#103504=CARTESIAN_POINT('Ctrl Pts',(17.1725759104252,69.8252183998702,12.));
#103505=CARTESIAN_POINT('Ctrl Pts',(17.1750451192885,69.8015184747398,12.));
#103506=CARTESIAN_POINT('Ctrl Pts',(17.1774866969256,69.777858724479,12.));
#103507=CARTESIAN_POINT('Ctrl Pts',(17.179900692726,69.7542392771234,12.));
#103508=CARTESIAN_POINT('Ctrl Pts',(17.1822871563842,69.7306602612155,12.));
#103509=CARTESIAN_POINT('Ctrl Pts',(17.1846461378973,69.7071218058178,12.));
#103510=CARTESIAN_POINT('Ctrl Pts',(17.1869776875666,69.6836240405164,12.));
#103511=CARTESIAN_POINT('Ctrl Pts',(17.1892818560002,69.6601670954269,12.));
#103512=CARTESIAN_POINT('Ctrl Pts',(17.1915586941192,69.6367511011898,12.));
#103513=CARTESIAN_POINT('Ctrl Pts',(17.1938082531612,69.6133761889749,12.));
#103514=CARTESIAN_POINT('Ctrl Pts',(17.196030584678,69.5900424904921,12.));
#103515=CARTESIAN_POINT('Ctrl Pts',(17.1982257405377,69.5667501379969,12.));
#103516=CARTESIAN_POINT('Ctrl Pts',(17.2003937729268,69.5434992642944,12.));
#103517=CARTESIAN_POINT('Ctrl Pts',(17.2025347343577,69.5202900027367,12.));
#103518=CARTESIAN_POINT('Ctrl Pts',(17.2046486776708,69.4971224872269,12.));
#103519=CARTESIAN_POINT('Ctrl Pts',(17.2067356560336,69.4739968522313,12.));
#103520=CARTESIAN_POINT('Ctrl Pts',(17.2087957229423,69.450913232785,12.));
#103521=CARTESIAN_POINT('Ctrl Pts',(17.2108289322254,69.4278717644973,12.));
#103522=CARTESIAN_POINT('Ctrl Pts',(17.2128353380502,69.404872583548,12.));
#103523=CARTESIAN_POINT('Ctrl Pts',(17.2148149949252,69.3819158266916,12.));
#103524=CARTESIAN_POINT('Ctrl Pts',(17.2167679576984,69.3590016312692,12.));
#103525=CARTESIAN_POINT('Ctrl Pts',(17.2186942815602,69.3361301352141,12.));
#103526=CARTESIAN_POINT('Ctrl Pts',(17.2205940220459,69.3133014770555,12.));
#103527=CARTESIAN_POINT('Ctrl Pts',(17.2224672350438,69.2905157959166,12.));
#103528=CARTESIAN_POINT('Ctrl Pts',(17.224313976797,69.2677732315224,12.));
#103529=CARTESIAN_POINT('Ctrl Pts',(17.226134303902,69.2450739242109,12.));
#103530=CARTESIAN_POINT('Ctrl Pts',(17.227928273312,69.222418014938,12.));
#103531=CARTESIAN_POINT('Ctrl Pts',(17.2296959423407,69.1998056452828,12.));
#103532=CARTESIAN_POINT('Ctrl Pts',(17.23143736867,69.1772369574447,12.));
#103533=CARTESIAN_POINT('Ctrl Pts',(17.2331526103506,69.1547120942527,12.));
#103534=CARTESIAN_POINT('Ctrl Pts',(17.2348417258015,69.1322311991752,12.));
#103535=CARTESIAN_POINT('Ctrl Pts',(17.2365047738125,69.1097944163245,12.));
#103536=CARTESIAN_POINT('Ctrl Pts',(17.2381418135491,69.0874018904599,12.));
#103537=CARTESIAN_POINT('Ctrl Pts',(17.2397529045589,69.065053766986,12.));
#103538=CARTESIAN_POINT('Ctrl Pts',(17.2413381067723,69.0427501919636,12.));
#103539=CARTESIAN_POINT('Ctrl Pts',(17.2428974805044,69.0204913121225,12.));
#103540=CARTESIAN_POINT('Ctrl Pts',(17.2444310864585,68.9982772748694,12.));
#103541=CARTESIAN_POINT('Ctrl Pts',(17.2459389857327,68.9761082282922,12.));
#103542=CARTESIAN_POINT('Ctrl Pts',(17.2474212398275,68.9539843211619,12.));
#103543=CARTESIAN_POINT('Ctrl Pts',(17.248877910643,68.9319057029409,12.));
#103544=CARTESIAN_POINT('Ctrl Pts',(17.2503090604792,68.909872523787,12.));
#103545=CARTESIAN_POINT('Ctrl Pts',(17.2517147520376,68.8878849345557,12.));
#103546=CARTESIAN_POINT('Ctrl Pts',(17.2530950484258,68.8659430867972,12.));
#103547=CARTESIAN_POINT('Ctrl Pts',(17.2544500131624,68.844047132755,12.));
#103548=CARTESIAN_POINT('Ctrl Pts',(17.2557797101812,68.8221972253941,12.));
#103549=CARTESIAN_POINT('Ctrl Pts',(17.2570842038383,68.8003935184184,12.));
#103550=CARTESIAN_POINT('Ctrl Pts',(17.2583635589198,68.7786361662882,12.));
#103551=CARTESIAN_POINT('Ctrl Pts',(17.259617840655,68.7569253242333,12.));
#103552=CARTESIAN_POINT('Ctrl Pts',(17.2608471147185,68.7352611482547,12.));
#103553=CARTESIAN_POINT('Ctrl Pts',(17.2620514472182,68.7136437951097,12.));
#103554=CARTESIAN_POINT('Ctrl Pts',(17.2632309046892,68.6920734222938,12.));
#103555=CARTESIAN_POINT('Ctrl Pts',(17.2643855540892,68.6705501880249,12.));
#103556=CARTESIAN_POINT('Ctrl Pts',(17.2655154627928,68.6490742512057,12.));
#103557=CARTESIAN_POINT('Ctrl Pts',(17.2666206986084,68.6276457714729,12.));
#103558=CARTESIAN_POINT('Ctrl Pts',(17.2677013298057,68.6062649092764,12.));
#103559=CARTESIAN_POINT('Ctrl Pts',(17.2687574251429,68.5849318259449,12.));
#103560=CARTESIAN_POINT('Ctrl Pts',(17.269789053896,68.5636466837517,12.));
#103561=CARTESIAN_POINT('Ctrl Pts',(17.2707962858919,68.5424096459772,12.));
#103562=CARTESIAN_POINT('Ctrl Pts',(17.2717791914544,68.521220876786,12.));
#103563=CARTESIAN_POINT('Ctrl Pts',(17.2727378413489,68.5000805410911,12.));
#103564=CARTESIAN_POINT('Ctrl Pts',(17.2736723067365,68.4789888044351,12.));
#103565=CARTESIAN_POINT('Ctrl Pts',(17.2745826591119,68.4579458328185,12.));
#103566=CARTESIAN_POINT('Ctrl Pts',(17.2754689702992,68.436951792677,12.));
#103567=CARTESIAN_POINT('Ctrl Pts',(17.2763313126018,68.4160068512753,12.));
#103568=CARTESIAN_POINT('Ctrl Pts',(17.2771697589384,68.3951111770487,12.));
#103569=CARTESIAN_POINT('Ctrl Pts',(17.2779843829608,68.3742649398964,12.));
#103570=CARTESIAN_POINT('Ctrl Pts',(17.2787752592484,68.3534683116515,12.));
#103571=CARTESIAN_POINT('Ctrl Pts',(17.2795424631799,68.3327214657575,12.));
#103572=CARTESIAN_POINT('Ctrl Pts',(17.2802860705815,68.3120245763914,12.));
#103573=CARTESIAN_POINT('Ctrl Pts',(17.2810061574353,68.2913778177261,12.));
#103574=CARTESIAN_POINT('Ctrl Pts',(17.2817027995831,68.2707813631731,12.));
#103575=CARTESIAN_POINT('Ctrl Pts',(17.2823760723874,68.2502353845071,12.));
#103576=CARTESIAN_POINT('Ctrl Pts',(17.2830260513867,68.2297400535294,12.));
#103577=CARTESIAN_POINT('Ctrl Pts',(17.2836528130819,68.2092955440567,12.));
#103578=CARTESIAN_POINT('Ctrl Pts',(17.2842564355799,68.1889020335427,12.));
#103579=CARTESIAN_POINT('Ctrl Pts',(17.2848369995293,68.1685597054232,12.));
#103580=CARTESIAN_POINT('Ctrl Pts',(17.2853945882072,68.1482687493226,12.));
#103581=CARTESIAN_POINT('Ctrl Pts',(17.2859292855705,68.1280293561511,12.));
#103582=CARTESIAN_POINT('Ctrl Pts',(17.2864411745459,68.1078417137877,12.));
#103583=CARTESIAN_POINT('Ctrl Pts',(17.2869303355432,68.0877060033205,12.));
#103584=CARTESIAN_POINT('Ctrl Pts',(17.2873968440839,68.0676223930412,12.));
#103585=CARTESIAN_POINT('Ctrl Pts',(17.2878407730961,68.0475910442424,12.));
#103586=CARTESIAN_POINT('Ctrl Pts',(17.2882621974721,68.0276121227356,12.));
#103587=CARTESIAN_POINT('Ctrl Pts',(17.28866119774,68.007685808115,12.));
#103588=CARTESIAN_POINT('Ctrl Pts',(17.2890378644866,67.987812304921,12.));
#103589=CARTESIAN_POINT('Ctrl Pts',(17.2893923013894,67.9679918502579,12.));
#103590=CARTESIAN_POINT('Ctrl Pts',(17.2897246158941,67.9482246901667,12.));
#103591=CARTESIAN_POINT('Ctrl Pts',(17.2900349103981,67.9285110571741,12.));
#103592=CARTESIAN_POINT('Ctrl Pts',(17.2903232740694,67.9088511496686,12.));
#103593=CARTESIAN_POINT('Ctrl Pts',(17.2905897723949,67.8892451049608,12.));
#103594=CARTESIAN_POINT('Ctrl Pts',(17.2908344459694,67.8696929978782,12.));
#103595=CARTESIAN_POINT('Ctrl Pts',(17.291012743109,67.8540944889687,12.));
#103596=CARTESIAN_POINT('Ctrl Pts',(17.2911366591348,67.842419897098,12.));
#103597=CARTESIAN_POINT('Ctrl Pts',(17.2912149114119,67.8346476309018,12.));
#103598=CARTESIAN_POINT('Ctrl Pts',(17.2912529479484,67.8307641965655,12.));
#103599=CARTESIAN_POINT('Ctrl Pts',(15.3208442077425,72.6050633494718,0.));
#103600=CARTESIAN_POINT('Ctrl Pts',(15.3208442077425,72.6050633494718,4.));
#103601=CARTESIAN_POINT('Ctrl Pts',(15.3208442077425,72.6050633494718,8.));
#103602=CARTESIAN_POINT('Ctrl Pts',(15.3208442077425,72.6050633494718,12.));
#103603=CARTESIAN_POINT('Ctrl Pts',(15.3856835210424,72.6937764817672,0.));
#103604=CARTESIAN_POINT('Ctrl Pts',(15.3856835210424,72.6937764817672,4.));
#103605=CARTESIAN_POINT('Ctrl Pts',(15.3856835210424,72.6937764817672,8.00000000000001));
#103606=CARTESIAN_POINT('Ctrl Pts',(15.3856835210424,72.6937764817672,12.));
#103607=CARTESIAN_POINT('Ctrl Pts',(15.551931775029,72.8096834307709,0.));
#103608=CARTESIAN_POINT('Ctrl Pts',(15.551931775029,72.8096834307709,4.));
#103609=CARTESIAN_POINT('Ctrl Pts',(15.551931775029,72.809683430771,7.99999999999999));
#103610=CARTESIAN_POINT('Ctrl Pts',(15.551931775029,72.809683430771,12.));
#103611=CARTESIAN_POINT('Ctrl Pts',(15.7502340068144,72.8161171750014,0.));
#103612=CARTESIAN_POINT('Ctrl Pts',(15.7502340068144,72.8161171750014,4.));
#103613=CARTESIAN_POINT('Ctrl Pts',(15.7502340068145,72.8161171750015,8.00000000000001));
#103614=CARTESIAN_POINT('Ctrl Pts',(15.7502340068145,72.8161171750015,12.));
#103615=CARTESIAN_POINT('Ctrl Pts',(15.830763774723,72.7986051948036,0.));
#103616=CARTESIAN_POINT('Ctrl Pts',(15.830763774723,72.7986051948036,4.));
#103617=CARTESIAN_POINT('Ctrl Pts',(15.8307637747231,72.7986051948037,8.));
#103618=CARTESIAN_POINT('Ctrl Pts',(15.8307637747231,72.7986051948037,12.));
#103619=CARTESIAN_POINT('',(15.3208442077425,72.6050633494718,0.));
#103620=CARTESIAN_POINT('',(15.8307637747231,72.7986051948038,0.));
#103621=CARTESIAN_POINT('Ctrl Pts',(15.3208442077425,72.6050633494718,2.77555756156289E-16));
#103622=CARTESIAN_POINT('Ctrl Pts',(15.3856835210424,72.6937764817672,2.77555756156289E-16));
#103623=CARTESIAN_POINT('Ctrl Pts',(15.4806825233205,72.760009024055,2.77555756156289E-16));
#103624=CARTESIAN_POINT('Ctrl Pts',(15.5861481305941,72.7904952137638,2.77555756156289E-16));
#103625=CARTESIAN_POINT('Ctrl Pts',(15.6652473360493,72.8133598560455,2.77555756156289E-16));
#103626=CARTESIAN_POINT('Ctrl Pts',(15.7502340068144,72.8161171750014,2.77555756156289E-16));
#103627=CARTESIAN_POINT('Ctrl Pts',(15.830763774723,72.7986051948036,2.77555756156289E-16));
#103628=CARTESIAN_POINT('',(15.8307637747231,72.7986051948038,12.));
#103629=CARTESIAN_POINT('Ctrl Pts',(15.830763774723,72.7986051948036,0.));
#103630=CARTESIAN_POINT('Ctrl Pts',(15.830763774723,72.7986051948036,4.));
#103631=CARTESIAN_POINT('Ctrl Pts',(15.8307637747231,72.7986051948037,8.));
#103632=CARTESIAN_POINT('Ctrl Pts',(15.8307637747231,72.7986051948037,12.));
#103633=CARTESIAN_POINT('',(15.3208442077425,72.6050633494718,12.));
#103634=CARTESIAN_POINT('Ctrl Pts',(15.8307637747231,72.7986051948037,12.));
#103635=CARTESIAN_POINT('Ctrl Pts',(15.7502340068145,72.8161171750015,12.));
#103636=CARTESIAN_POINT('Ctrl Pts',(15.6652473360493,72.8133598560455,12.));
#103637=CARTESIAN_POINT('Ctrl Pts',(15.5861481305941,72.7904952137639,12.));
#103638=CARTESIAN_POINT('Ctrl Pts',(15.4806825233205,72.7600090240551,12.));
#103639=CARTESIAN_POINT('Ctrl Pts',(15.3856835210424,72.6937764817672,12.));
#103640=CARTESIAN_POINT('Ctrl Pts',(15.3208442077425,72.6050633494718,12.));
#103641=CARTESIAN_POINT('Ctrl Pts',(15.3208442077425,72.6050633494718,12.));
#103642=CARTESIAN_POINT('Ctrl Pts',(15.3208442077425,72.6050633494718,8.));
#103643=CARTESIAN_POINT('Ctrl Pts',(15.3208442077425,72.6050633494718,4.));
#103644=CARTESIAN_POINT('Ctrl Pts',(15.3208442077425,72.6050633494718,0.));
#103645=CARTESIAN_POINT('Origin',(8.10341340518591E-11,3.65979954444617E-10,
0.));
#103646=CARTESIAN_POINT('Origin',(8.10341340518591E-11,3.65979954444617E-10,
12.));
#103647=CARTESIAN_POINT('Origin',(8.10341340518591E-11,3.65979954444617E-10,
0.));
#103648=CARTESIAN_POINT('Ctrl Pts',(22.6894590071785,70.9608233461364,0.));
#103649=CARTESIAN_POINT('Ctrl Pts',(22.6894590071785,70.9608233461364,4.));
#103650=CARTESIAN_POINT('Ctrl Pts',(22.6894590071785,70.9608233461363,8.));
#103651=CARTESIAN_POINT('Ctrl Pts',(22.6894590071785,70.9608233461363,12.));
#103652=CARTESIAN_POINT('Ctrl Pts',(22.7941214270115,70.9273579271571,0.));
#103653=CARTESIAN_POINT('Ctrl Pts',(22.7941214270115,70.9273579271571,4.));
#103654=CARTESIAN_POINT('Ctrl Pts',(22.7941214270115,70.9273579271571,8.));
#103655=CARTESIAN_POINT('Ctrl Pts',(22.7941214270115,70.9273579271571,12.));
#103656=CARTESIAN_POINT('Ctrl Pts',(22.9566438338676,70.8062825417801,0.));
#103657=CARTESIAN_POINT('Ctrl Pts',(22.9566438338676,70.8062825417801,4.00000000000001));
#103658=CARTESIAN_POINT('Ctrl Pts',(22.9566438338677,70.8062825417801,7.99999999999999));
#103659=CARTESIAN_POINT('Ctrl Pts',(22.9566438338677,70.8062825417801,12.));
#103660=CARTESIAN_POINT('Ctrl Pts',(23.0254444386656,70.620187020006,0.));
#103661=CARTESIAN_POINT('Ctrl Pts',(23.0254444386656,70.620187020006,4.));
#103662=CARTESIAN_POINT('Ctrl Pts',(23.0254444386657,70.620187020006,8.00000000000001));
#103663=CARTESIAN_POINT('Ctrl Pts',(23.0254444386657,70.620187020006,12.));
#103664=CARTESIAN_POINT('Ctrl Pts',(23.0342913834094,70.5382514078485,0.));
#103665=CARTESIAN_POINT('Ctrl Pts',(23.0342913834094,70.5382514078485,4.));
#103666=CARTESIAN_POINT('Ctrl Pts',(23.0342913834094,70.5382514078485,8.));
#103667=CARTESIAN_POINT('Ctrl Pts',(23.0342913834094,70.5382514078485,12.));
#103668=CARTESIAN_POINT('',(22.6894590071785,70.9608233461364,0.));
#103669=CARTESIAN_POINT('',(23.0342913834093,70.5382514078485,0.));
#103670=CARTESIAN_POINT('Ctrl Pts',(22.6894590071785,70.9608233461364,0.));
#103671=CARTESIAN_POINT('Ctrl Pts',(22.7941214270115,70.9273579271571,0.));
#103672=CARTESIAN_POINT('Ctrl Pts',(22.8869913737864,70.858171992656,0.));
#103673=CARTESIAN_POINT('Ctrl Pts',(22.9492582831546,70.7677549932088,0.));
#103674=CARTESIAN_POINT('Ctrl Pts',(22.9959584651808,70.6999422436235,0.));
#103675=CARTESIAN_POINT('Ctrl Pts',(23.0254444386656,70.620187020006,0.));
#103676=CARTESIAN_POINT('Ctrl Pts',(23.0342913834094,70.5382514078485,0.));
#103677=CARTESIAN_POINT('',(23.0342913834094,70.5382514078485,12.));
#103678=CARTESIAN_POINT('Ctrl Pts',(23.0342913834094,70.5382514078485,0.));
#103679=CARTESIAN_POINT('Ctrl Pts',(23.0342913834094,70.5382514078485,4.));
#103680=CARTESIAN_POINT('Ctrl Pts',(23.0342913834094,70.5382514078485,8.));
#103681=CARTESIAN_POINT('Ctrl Pts',(23.0342913834094,70.5382514078485,12.));
#103682=CARTESIAN_POINT('',(22.6894590071785,70.9608233461363,12.));
#103683=CARTESIAN_POINT('Ctrl Pts',(23.0342913834094,70.5382514078485,12.));
#103684=CARTESIAN_POINT('Ctrl Pts',(23.0254444386657,70.620187020006,12.));
#103685=CARTESIAN_POINT('Ctrl Pts',(22.9959584651808,70.6999422436235,12.));
#103686=CARTESIAN_POINT('Ctrl Pts',(22.9492582831546,70.7677549932088,12.));
#103687=CARTESIAN_POINT('Ctrl Pts',(22.8869913737864,70.8581719926559,12.));
#103688=CARTESIAN_POINT('Ctrl Pts',(22.7941214270115,70.9273579271571,12.));
#103689=CARTESIAN_POINT('Ctrl Pts',(22.6894590071785,70.9608233461363,12.));
#103690=CARTESIAN_POINT('Ctrl Pts',(22.6894590071785,70.9608233461363,12.));
#103691=CARTESIAN_POINT('Ctrl Pts',(22.6894590071785,70.9608233461363,8.));
#103692=CARTESIAN_POINT('Ctrl Pts',(22.6894590071785,70.9608233461364,4.));
#103693=CARTESIAN_POINT('Ctrl Pts',(22.6894590071785,70.9608233461364,0.));
#103694=CARTESIAN_POINT('Ctrl Pts',(23.1372951448024,66.0656156664138,0.));
#103695=CARTESIAN_POINT('Ctrl Pts',(23.1372951448024,66.0656156664138,12.));
#103696=CARTESIAN_POINT('Ctrl Pts',(23.1375957166104,66.0694876382127,0.));
#103697=CARTESIAN_POINT('Ctrl Pts',(23.1375957166104,66.0694876382127,12.));
#103698=CARTESIAN_POINT('Ctrl Pts',(23.1381951597399,66.0772371487248,0.));
#103699=CARTESIAN_POINT('Ctrl Pts',(23.1381951597399,66.0772371487248,12.));
#103700=CARTESIAN_POINT('Ctrl Pts',(23.1390892229778,66.0888781152421,0.));
#103701=CARTESIAN_POINT('Ctrl Pts',(23.1390892229778,66.0888781152421,12.));
#103702=CARTESIAN_POINT('Ctrl Pts',(23.1402711039425,66.1044328067355,0.));
#103703=CARTESIAN_POINT('Ctrl Pts',(23.1402711039425,66.1044328067355,12.));
#103704=CARTESIAN_POINT('Ctrl Pts',(23.1417314398398,66.1239318368548,0.));
#103705=CARTESIAN_POINT('Ctrl Pts',(23.1417314398398,66.1239318368548,12.));
#103706=CARTESIAN_POINT('Ctrl Pts',(23.1431747350098,66.1434865015027,0.));
#103707=CARTESIAN_POINT('Ctrl Pts',(23.1431747350098,66.1434865015027,12.));
#103708=CARTESIAN_POINT('Ctrl Pts',(23.1446009424903,66.1630967296747,0.));
#103709=CARTESIAN_POINT('Ctrl Pts',(23.1446009424903,66.1630967296747,12.));
#103710=CARTESIAN_POINT('Ctrl Pts',(23.1460099850763,66.18276239029,0.));
#103711=CARTESIAN_POINT('Ctrl Pts',(23.1460099850763,66.18276239029,12.));
#103712=CARTESIAN_POINT('Ctrl Pts',(23.1474017566484,66.2024832934866,0.));
#103713=CARTESIAN_POINT('Ctrl Pts',(23.1474017566484,66.2024832934866,12.));
#103714=CARTESIAN_POINT('Ctrl Pts',(23.1487761349328,66.2222592165473,0.));
#103715=CARTESIAN_POINT('Ctrl Pts',(23.1487761349328,66.2222592165473,12.));
#103716=CARTESIAN_POINT('Ctrl Pts',(23.1501329914487,66.2420899237317,0.));
#103717=CARTESIAN_POINT('Ctrl Pts',(23.1501329914487,66.2420899237317,12.));
#103718=CARTESIAN_POINT('Ctrl Pts',(23.1514722022483,66.2619751878741,0.));
#103719=CARTESIAN_POINT('Ctrl Pts',(23.1514722022483,66.2619751878741,12.));
#103720=CARTESIAN_POINT('Ctrl Pts',(23.1527936592625,66.2819148131072,0.));
#103721=CARTESIAN_POINT('Ctrl Pts',(23.1527936592625,66.2819148131072,12.));
#103722=CARTESIAN_POINT('Ctrl Pts',(23.154097266617,66.301908627539,0.));
#103723=CARTESIAN_POINT('Ctrl Pts',(23.154097266617,66.301908627539,12.));
#103724=CARTESIAN_POINT('Ctrl Pts',(23.1553829352531,66.3219564725161,0.));
#103725=CARTESIAN_POINT('Ctrl Pts',(23.1553829352531,66.3219564725161,12.));
#103726=CARTESIAN_POINT('Ctrl Pts',(23.1566505784626,66.3420581937159,0.));
#103727=CARTESIAN_POINT('Ctrl Pts',(23.1566505784626,66.3420581937159,12.));
#103728=CARTESIAN_POINT('Ctrl Pts',(23.1579001063438,66.3622136300692,0.));
#103729=CARTESIAN_POINT('Ctrl Pts',(23.1579001063438,66.3622136300692,12.));
#103730=CARTESIAN_POINT('Ctrl Pts',(23.15913142301,66.382422608185,0.));
#103731=CARTESIAN_POINT('Ctrl Pts',(23.15913142301,66.382422608185,12.));
#103732=CARTESIAN_POINT('Ctrl Pts',(23.1603444294754,66.402684948127,0.));
#103733=CARTESIAN_POINT('Ctrl Pts',(23.1603444294754,66.402684948127,12.));
#103734=CARTESIAN_POINT('Ctrl Pts',(23.1615390254635,66.4230004670288,0.));
#103735=CARTESIAN_POINT('Ctrl Pts',(23.1615390254635,66.4230004670288,12.));
#103736=CARTESIAN_POINT('Ctrl Pts',(23.1627151114875,66.4433689832454,0.));
#103737=CARTESIAN_POINT('Ctrl Pts',(23.1627151114875,66.4433689832454,12.));
#103738=CARTESIAN_POINT('Ctrl Pts',(23.163872591218,66.4637903210682,0.));
#103739=CARTESIAN_POINT('Ctrl Pts',(23.163872591218,66.4637903210682,12.));
#103740=CARTESIAN_POINT('Ctrl Pts',(23.1650113713792,66.4842643105263,0.));
#103741=CARTESIAN_POINT('Ctrl Pts',(23.1650113713792,66.4842643105263,12.));
#103742=CARTESIAN_POINT('Ctrl Pts',(23.1661313606123,66.5047907851319,0.));
#103743=CARTESIAN_POINT('Ctrl Pts',(23.1661313606123,66.5047907851319,12.));
#103744=CARTESIAN_POINT('Ctrl Pts',(23.1672324686927,66.5253695803209,0.));
#103745=CARTESIAN_POINT('Ctrl Pts',(23.1672324686927,66.5253695803209,12.));
#103746=CARTESIAN_POINT('Ctrl Pts',(23.1683146055736,66.5460005315406,0.));
#103747=CARTESIAN_POINT('Ctrl Pts',(23.1683146055736,66.5460005315406,12.));
#103748=CARTESIAN_POINT('Ctrl Pts',(23.169377680588,66.5666834726495,0.));
#103749=CARTESIAN_POINT('Ctrl Pts',(23.169377680588,66.5666834726495,12.));
#103750=CARTESIAN_POINT('Ctrl Pts',(23.1704216028626,66.5874182367597,0.));
#103751=CARTESIAN_POINT('Ctrl Pts',(23.1704216028626,66.5874182367597,12.));
#103752=CARTESIAN_POINT('Ctrl Pts',(23.1714462816794,66.6082046569657,0.));
#103753=CARTESIAN_POINT('Ctrl Pts',(23.1714462816794,66.6082046569657,12.));
#103754=CARTESIAN_POINT('Ctrl Pts',(23.1724516268299,66.6290425670538,0.));
#103755=CARTESIAN_POINT('Ctrl Pts',(23.1724516268299,66.6290425670538,12.));
#103756=CARTESIAN_POINT('Ctrl Pts',(23.1734375490421,66.6499318023445,0.));
#103757=CARTESIAN_POINT('Ctrl Pts',(23.1734375490421,66.6499318023445,12.));
#103758=CARTESIAN_POINT('Ctrl Pts',(23.174403960137,66.6708722000046,0.));
#103759=CARTESIAN_POINT('Ctrl Pts',(23.174403960137,66.6708722000046,12.));
#103760=CARTESIAN_POINT('Ctrl Pts',(23.1753507727931,66.691863598595,0.));
#103761=CARTESIAN_POINT('Ctrl Pts',(23.1753507727931,66.691863598595,12.));
#103762=CARTESIAN_POINT('Ctrl Pts',(23.1762779004043,66.712905837789,0.));
#103763=CARTESIAN_POINT('Ctrl Pts',(23.1762779004043,66.712905837789,12.));
#103764=CARTESIAN_POINT('Ctrl Pts',(23.1771852569136,66.7339987580441,0.));
#103765=CARTESIAN_POINT('Ctrl Pts',(23.1771852569136,66.7339987580441,12.));
#103766=CARTESIAN_POINT('Ctrl Pts',(23.1780727566309,66.7551422002229,0.));
#103767=CARTESIAN_POINT('Ctrl Pts',(23.1780727566309,66.7551422002229,12.));
#103768=CARTESIAN_POINT('Ctrl Pts',(23.1789403142375,66.7763360056146,0.));
#103769=CARTESIAN_POINT('Ctrl Pts',(23.1789403142375,66.7763360056146,12.));
#103770=CARTESIAN_POINT('Ctrl Pts',(23.1797878448645,66.7975800161014,0.));
#103771=CARTESIAN_POINT('Ctrl Pts',(23.1797878448645,66.7975800161014,12.));
#103772=CARTESIAN_POINT('Ctrl Pts',(23.1806152641475,66.8188740742727,0.));
#103773=CARTESIAN_POINT('Ctrl Pts',(23.1806152641475,66.8188740742727,12.));
#103774=CARTESIAN_POINT('Ctrl Pts',(23.1814224882948,66.840218023555,0.));
#103775=CARTESIAN_POINT('Ctrl Pts',(23.1814224882948,66.840218023555,12.));
#103776=CARTESIAN_POINT('Ctrl Pts',(23.1822094341508,66.8616117083304,0.));
#103777=CARTESIAN_POINT('Ctrl Pts',(23.1822094341508,66.8616117083304,12.));
#103778=CARTESIAN_POINT('Ctrl Pts',(23.1829760191582,66.8830549738768,0.));
#103779=CARTESIAN_POINT('Ctrl Pts',(23.1829760191582,66.8830549738768,12.));
#103780=CARTESIAN_POINT('Ctrl Pts',(23.1837221613231,66.904547666305,0.));
#103781=CARTESIAN_POINT('Ctrl Pts',(23.1837221613231,66.904547666305,12.));
#103782=CARTESIAN_POINT('Ctrl Pts',(23.1844477791816,66.9260896324955,0.));
#103783=CARTESIAN_POINT('Ctrl Pts',(23.1844477791816,66.9260896324955,12.));
#103784=CARTESIAN_POINT('Ctrl Pts',(23.1851527917665,66.9476807200225,0.));
#103785=CARTESIAN_POINT('Ctrl Pts',(23.1851527917665,66.9476807200225,12.));
#103786=CARTESIAN_POINT('Ctrl Pts',(23.1858371185852,66.9693207771059,0.));
#103787=CARTESIAN_POINT('Ctrl Pts',(23.1858371185852,66.9693207771059,12.));
#103788=CARTESIAN_POINT('Ctrl Pts',(23.1865006796291,66.9910096526483,0.));
#103789=CARTESIAN_POINT('Ctrl Pts',(23.1865006796291,66.9910096526483,12.));
#103790=CARTESIAN_POINT('Ctrl Pts',(23.1871433953795,67.0127471962507,0.));
#103791=CARTESIAN_POINT('Ctrl Pts',(23.1871433953795,67.0127471962507,12.));
#103792=CARTESIAN_POINT('Ctrl Pts',(23.1877651868155,67.0345332582297,0.));
#103793=CARTESIAN_POINT('Ctrl Pts',(23.1877651868155,67.0345332582297,12.));
#103794=CARTESIAN_POINT('Ctrl Pts',(23.1883659754267,67.0563676896312,0.));
#103795=CARTESIAN_POINT('Ctrl Pts',(23.1883659754267,67.0563676896312,12.));
#103796=CARTESIAN_POINT('Ctrl Pts',(23.1889456832115,67.0782503422293,0.));
#103797=CARTESIAN_POINT('Ctrl Pts',(23.1889456832115,67.0782503422293,12.));
#103798=CARTESIAN_POINT('Ctrl Pts',(23.1895042326625,67.1001810685138,0.));
#103799=CARTESIAN_POINT('Ctrl Pts',(23.1895042326625,67.1001810685138,12.));
#103800=CARTESIAN_POINT('Ctrl Pts',(23.1900415467574,67.122159721674,0.));
#103801=CARTESIAN_POINT('Ctrl Pts',(23.1900415467574,67.122159721674,12.));
#103802=CARTESIAN_POINT('Ctrl Pts',(23.1905575489505,67.1441861555819,0.));
#103803=CARTESIAN_POINT('Ctrl Pts',(23.1905575489505,67.1441861555819,12.));
#103804=CARTESIAN_POINT('Ctrl Pts',(23.1910521631658,67.1662602247641,0.));
#103805=CARTESIAN_POINT('Ctrl Pts',(23.1910521631658,67.1662602247641,12.));
#103806=CARTESIAN_POINT('Ctrl Pts',(23.1915253137923,67.1883817844039,0.));
#103807=CARTESIAN_POINT('Ctrl Pts',(23.1915253137923,67.1883817844039,12.));
#103808=CARTESIAN_POINT('Ctrl Pts',(23.1919769256803,67.2105506903448,0.));
#103809=CARTESIAN_POINT('Ctrl Pts',(23.1919769256803,67.2105506903448,12.));
#103810=CARTESIAN_POINT('Ctrl Pts',(23.1924069241385,67.232766799088,0.));
#103811=CARTESIAN_POINT('Ctrl Pts',(23.1924069241385,67.232766799088,12.));
#103812=CARTESIAN_POINT('Ctrl Pts',(23.1928152349343,67.2550299677888,0.));
#103813=CARTESIAN_POINT('Ctrl Pts',(23.1928152349343,67.2550299677888,12.));
#103814=CARTESIAN_POINT('Ctrl Pts',(23.1932017842954,67.2773400542477,0.));
#103815=CARTESIAN_POINT('Ctrl Pts',(23.1932017842954,67.2773400542477,12.));
#103816=CARTESIAN_POINT('Ctrl Pts',(23.193566498902,67.2996969169099,0.));
#103817=CARTESIAN_POINT('Ctrl Pts',(23.193566498902,67.2996969169099,12.));
#103818=CARTESIAN_POINT('Ctrl Pts',(23.1939093058802,67.3221004148604,0.));
#103819=CARTESIAN_POINT('Ctrl Pts',(23.1939093058802,67.3221004148604,12.));
#103820=CARTESIAN_POINT('Ctrl Pts',(23.1942301327978,67.3445504078178,0.));
#103821=CARTESIAN_POINT('Ctrl Pts',(23.1942301327978,67.3445504078178,12.));
#103822=CARTESIAN_POINT('Ctrl Pts',(23.1945289076608,67.3670467561205,0.));
#103823=CARTESIAN_POINT('Ctrl Pts',(23.1945289076608,67.3670467561205,12.));
#103824=CARTESIAN_POINT('Ctrl Pts',(23.1948055589123,67.3895893207168,0.));
#103825=CARTESIAN_POINT('Ctrl Pts',(23.1948055589123,67.3895893207168,12.));
#103826=CARTESIAN_POINT('Ctrl Pts',(23.1950600154259,67.4121779631666,0.));
#103827=CARTESIAN_POINT('Ctrl Pts',(23.1950600154259,67.4121779631666,12.));
#103828=CARTESIAN_POINT('Ctrl Pts',(23.1952922065009,67.4348125456389,0.));
#103829=CARTESIAN_POINT('Ctrl Pts',(23.1952922065009,67.4348125456389,12.));
#103830=CARTESIAN_POINT('Ctrl Pts',(23.1955020618591,67.4574929309079,0.));
#103831=CARTESIAN_POINT('Ctrl Pts',(23.1955020618591,67.4574929309079,12.));
#103832=CARTESIAN_POINT('Ctrl Pts',(23.1956895116446,67.4802189823424,0.));
#103833=CARTESIAN_POINT('Ctrl Pts',(23.1956895116446,67.4802189823424,12.));
#103834=CARTESIAN_POINT('Ctrl Pts',(23.1958544864224,67.5029905638974,0.));
#103835=CARTESIAN_POINT('Ctrl Pts',(23.1958544864224,67.5029905638974,12.));
#103836=CARTESIAN_POINT('Ctrl Pts',(23.1959969171709,67.525807540117,0.));
#103837=CARTESIAN_POINT('Ctrl Pts',(23.1959969171709,67.525807540117,12.));
#103838=CARTESIAN_POINT('Ctrl Pts',(23.1961167352776,67.5486697761301,0.));
#103839=CARTESIAN_POINT('Ctrl Pts',(23.1961167352776,67.5486697761301,12.));
#103840=CARTESIAN_POINT('Ctrl Pts',(23.1962138725358,67.5715771376454,0.));
#103841=CARTESIAN_POINT('Ctrl Pts',(23.1962138725358,67.5715771376454,12.));
#103842=CARTESIAN_POINT('Ctrl Pts',(23.1962882611443,67.5945294909398,0.));
#103843=CARTESIAN_POINT('Ctrl Pts',(23.1962882611443,67.5945294909398,12.));
#103844=CARTESIAN_POINT('Ctrl Pts',(23.1963398337055,67.6175267028517,0.));
#103845=CARTESIAN_POINT('Ctrl Pts',(23.1963398337055,67.6175267028517,12.));
#103846=CARTESIAN_POINT('Ctrl Pts',(23.1963685232176,67.6405686407828,0.));
#103847=CARTESIAN_POINT('Ctrl Pts',(23.1963685232176,67.6405686407828,12.));
#103848=CARTESIAN_POINT('Ctrl Pts',(23.1963742630709,67.6636551726948,0.));
#103849=CARTESIAN_POINT('Ctrl Pts',(23.1963742630709,67.6636551726948,12.));
#103850=CARTESIAN_POINT('Ctrl Pts',(23.1963569870456,67.6867861671045,0.));
#103851=CARTESIAN_POINT('Ctrl Pts',(23.1963569870456,67.6867861671045,12.));
#103852=CARTESIAN_POINT('Ctrl Pts',(23.1963166293116,67.7099614930712,0.));
#103853=CARTESIAN_POINT('Ctrl Pts',(23.1963166293116,67.7099614930712,12.));
#103854=CARTESIAN_POINT('Ctrl Pts',(23.1962531244261,67.7331810201931,0.));
#103855=CARTESIAN_POINT('Ctrl Pts',(23.1962531244261,67.7331810201931,12.));
#103856=CARTESIAN_POINT('Ctrl Pts',(23.1961664073273,67.7564446186115,0.));
#103857=CARTESIAN_POINT('Ctrl Pts',(23.1961664073273,67.7564446186115,12.));
#103858=CARTESIAN_POINT('Ctrl Pts',(23.1960564133308,67.7797521590056,0.));
#103859=CARTESIAN_POINT('Ctrl Pts',(23.1960564133308,67.7797521590056,12.));
#103860=CARTESIAN_POINT('Ctrl Pts',(23.1959230781265,67.8031035125873,0.));
#103861=CARTESIAN_POINT('Ctrl Pts',(23.1959230781265,67.8031035125873,12.));
#103862=CARTESIAN_POINT('Ctrl Pts',(23.1957663377797,67.8264985510884,0.));
#103863=CARTESIAN_POINT('Ctrl Pts',(23.1957663377797,67.8264985510884,12.));
#103864=CARTESIAN_POINT('Ctrl Pts',(23.1955861287275,67.8499371467578,0.));
#103865=CARTESIAN_POINT('Ctrl Pts',(23.1955861287275,67.8499371467578,12.));
#103866=CARTESIAN_POINT('Ctrl Pts',(23.1953823877726,67.8734191723639,0.));
#103867=CARTESIAN_POINT('Ctrl Pts',(23.1953823877726,67.8734191723639,12.));
#103868=CARTESIAN_POINT('Ctrl Pts',(23.19515505208,67.8969445011908,0.));
#103869=CARTESIAN_POINT('Ctrl Pts',(23.19515505208,67.8969445011908,12.));
#103870=CARTESIAN_POINT('Ctrl Pts',(23.1949040591748,67.9205130070337,0.));
#103871=CARTESIAN_POINT('Ctrl Pts',(23.1949040591748,67.9205130070337,12.));
#103872=CARTESIAN_POINT('Ctrl Pts',(23.1946293469436,67.9441245641871,0.));
#103873=CARTESIAN_POINT('Ctrl Pts',(23.1946293469436,67.9441245641871,12.));
#103874=CARTESIAN_POINT('Ctrl Pts',(23.1943308536307,67.9677790474414,0.));
#103875=CARTESIAN_POINT('Ctrl Pts',(23.1943308536307,67.9677790474414,12.));
#103876=CARTESIAN_POINT('Ctrl Pts',(23.1940085178319,67.9914763320878,0.));
#103877=CARTESIAN_POINT('Ctrl Pts',(23.1940085178319,67.9914763320878,12.));
#103878=CARTESIAN_POINT('Ctrl Pts',(23.193662278492,68.0152162939123,0.));
#103879=CARTESIAN_POINT('Ctrl Pts',(23.193662278492,68.0152162939123,12.));
#103880=CARTESIAN_POINT('Ctrl Pts',(23.1932920749021,68.0389988091926,0.));
#103881=CARTESIAN_POINT('Ctrl Pts',(23.1932920749021,68.0389988091926,12.));
#103882=CARTESIAN_POINT('Ctrl Pts',(23.1928978467017,68.0628237546853,0.));
#103883=CARTESIAN_POINT('Ctrl Pts',(23.1928978467017,68.0628237546853,12.));
#103884=CARTESIAN_POINT('Ctrl Pts',(23.1924795338745,68.086691007624,0.));
#103885=CARTESIAN_POINT('Ctrl Pts',(23.1924795338745,68.086691007624,12.));
#103886=CARTESIAN_POINT('Ctrl Pts',(23.1920370767423,68.1106004457223,0.));
#103887=CARTESIAN_POINT('Ctrl Pts',(23.1920370767423,68.1106004457223,12.));
#103888=CARTESIAN_POINT('Ctrl Pts',(23.1915704159623,68.1345519471695,0.));
#103889=CARTESIAN_POINT('Ctrl Pts',(23.1915704159623,68.1345519471695,12.));
#103890=CARTESIAN_POINT('Ctrl Pts',(23.1910794925252,68.1585453906259,0.));
#103891=CARTESIAN_POINT('Ctrl Pts',(23.1910794925252,68.1585453906259,12.));
#103892=CARTESIAN_POINT('Ctrl Pts',(23.1905642477571,68.182580655213,0.));
#103893=CARTESIAN_POINT('Ctrl Pts',(23.1905642477571,68.182580655213,12.));
#103894=CARTESIAN_POINT('Ctrl Pts',(23.1900246233164,68.2066576205113,0.));
#103895=CARTESIAN_POINT('Ctrl Pts',(23.1900246233164,68.2066576205113,12.));
#103896=CARTESIAN_POINT('Ctrl Pts',(23.1894605611869,68.2307761665629,0.));
#103897=CARTESIAN_POINT('Ctrl Pts',(23.1894605611869,68.2307761665629,12.));
#103898=CARTESIAN_POINT('Ctrl Pts',(23.1888720036756,68.2549361738679,0.));
#103899=CARTESIAN_POINT('Ctrl Pts',(23.1888720036756,68.2549361738679,12.));
#103900=CARTESIAN_POINT('Ctrl Pts',(23.1882588934108,68.2791375233798,0.));
#103901=CARTESIAN_POINT('Ctrl Pts',(23.1882588934108,68.2791375233798,12.));
#103902=CARTESIAN_POINT('Ctrl Pts',(23.1876211733439,68.3033800964946,0.));
#103903=CARTESIAN_POINT('Ctrl Pts',(23.1876211733439,68.3033800964946,12.));
#103904=CARTESIAN_POINT('Ctrl Pts',(23.1869587867463,68.3276637750494,0.));
#103905=CARTESIAN_POINT('Ctrl Pts',(23.1869587867463,68.3276637750494,12.));
#103906=CARTESIAN_POINT('Ctrl Pts',(23.1862716772034,68.3519884413253,0.));
#103907=CARTESIAN_POINT('Ctrl Pts',(23.1862716772034,68.3519884413253,12.));
#103908=CARTESIAN_POINT('Ctrl Pts',(23.1855597886117,68.3763539780442,0.));
#103909=CARTESIAN_POINT('Ctrl Pts',(23.1855597886117,68.3763539780442,12.));
#103910=CARTESIAN_POINT('Ctrl Pts',(23.1848230651775,68.4007602683649,0.));
#103911=CARTESIAN_POINT('Ctrl Pts',(23.1848230651775,68.4007602683649,12.));
#103912=CARTESIAN_POINT('Ctrl Pts',(23.184061451419,68.4252071958725,0.));
#103913=CARTESIAN_POINT('Ctrl Pts',(23.184061451419,68.4252071958725,12.));
#103914=CARTESIAN_POINT('Ctrl Pts',(23.1832748921629,68.4496946445756,0.));
#103915=CARTESIAN_POINT('Ctrl Pts',(23.1832748921629,68.4496946445756,12.));
#103916=CARTESIAN_POINT('Ctrl Pts',(23.1824633325384,68.4742224989099,0.));
#103917=CARTESIAN_POINT('Ctrl Pts',(23.1824633325384,68.4742224989099,12.));
#103918=CARTESIAN_POINT('Ctrl Pts',(23.1816267179751,68.4987906437357,0.));
#103919=CARTESIAN_POINT('Ctrl Pts',(23.1816267179751,68.4987906437357,12.));
#103920=CARTESIAN_POINT('Ctrl Pts',(23.180764994201,68.5233989643344,0.));
#103921=CARTESIAN_POINT('Ctrl Pts',(23.180764994201,68.5233989643344,12.));
#103922=CARTESIAN_POINT('Ctrl Pts',(23.1798781072449,68.548047346398,0.));
#103923=CARTESIAN_POINT('Ctrl Pts',(23.1798781072449,68.548047346398,12.));
#103924=CARTESIAN_POINT('Ctrl Pts',(23.1789660034339,68.572735676027,0.));
#103925=CARTESIAN_POINT('Ctrl Pts',(23.1789660034339,68.572735676027,12.));
#103926=CARTESIAN_POINT('Ctrl Pts',(23.1780286293873,68.5974638397322,0.));
#103927=CARTESIAN_POINT('Ctrl Pts',(23.1780286293873,68.5974638397322,12.));
#103928=CARTESIAN_POINT('Ctrl Pts',(23.1770659320136,68.6222317244337,0.));
#103929=CARTESIAN_POINT('Ctrl Pts',(23.1770659320136,68.6222317244337,12.));
#103930=CARTESIAN_POINT('Ctrl Pts',(23.1760778585093,68.6470392174567,0.));
#103931=CARTESIAN_POINT('Ctrl Pts',(23.1760778585093,68.6470392174567,12.));
#103932=CARTESIAN_POINT('Ctrl Pts',(23.1750643563605,68.6718862065227,0.));
#103933=CARTESIAN_POINT('Ctrl Pts',(23.1750643563605,68.6718862065227,12.));
#103934=CARTESIAN_POINT('Ctrl Pts',(23.1740253733423,68.6967725797458,0.));
#103935=CARTESIAN_POINT('Ctrl Pts',(23.1740253733423,68.6967725797458,12.));
#103936=CARTESIAN_POINT('Ctrl Pts',(23.1729608575115,68.7216982256357,0.));
#103937=CARTESIAN_POINT('Ctrl Pts',(23.1729608575115,68.7216982256357,12.));
#103938=CARTESIAN_POINT('Ctrl Pts',(23.1718707572046,68.7466630330968,0.));
#103939=CARTESIAN_POINT('Ctrl Pts',(23.1718707572046,68.7466630330968,12.));
#103940=CARTESIAN_POINT('Ctrl Pts',(23.1707550210359,68.7716668914246,0.));
#103941=CARTESIAN_POINT('Ctrl Pts',(23.1707550210359,68.7716668914246,12.));
#103942=CARTESIAN_POINT('Ctrl Pts',(23.1696135978992,68.7967096902981,0.));
#103943=CARTESIAN_POINT('Ctrl Pts',(23.1696135978992,68.7967096902981,12.));
#103944=CARTESIAN_POINT('Ctrl Pts',(23.1684464369681,68.8217913197735,0.));
#103945=CARTESIAN_POINT('Ctrl Pts',(23.1684464369681,68.8217913197735,12.));
#103946=CARTESIAN_POINT('Ctrl Pts',(23.1672534876885,68.8469116702885,0.));
#103947=CARTESIAN_POINT('Ctrl Pts',(23.1672534876885,68.8469116702885,12.));
#103948=CARTESIAN_POINT('Ctrl Pts',(23.1660346997762,68.8720706326606,0.));
#103949=CARTESIAN_POINT('Ctrl Pts',(23.1660346997762,68.8720706326606,12.));
#103950=CARTESIAN_POINT('Ctrl Pts',(23.1647900232151,68.8972680980844,0.));
#103951=CARTESIAN_POINT('Ctrl Pts',(23.1647900232151,68.8972680980844,12.));
#103952=CARTESIAN_POINT('Ctrl Pts',(23.1635194082581,68.9225039581249,0.));
#103953=CARTESIAN_POINT('Ctrl Pts',(23.1635194082581,68.9225039581249,12.));
#103954=CARTESIAN_POINT('Ctrl Pts',(23.162222805429,68.9477781047103,0.));
#103955=CARTESIAN_POINT('Ctrl Pts',(23.162222805429,68.9477781047103,12.));
#103956=CARTESIAN_POINT('Ctrl Pts',(23.1609001655153,68.9730904301363,0.));
#103957=CARTESIAN_POINT('Ctrl Pts',(23.1609001655153,68.9730904301363,12.));
#103958=CARTESIAN_POINT('Ctrl Pts',(23.1595514395654,68.9984408270653,0.));
#103959=CARTESIAN_POINT('Ctrl Pts',(23.1595514395654,68.9984408270653,12.));
#103960=CARTESIAN_POINT('Ctrl Pts',(23.1581765788869,69.0238291885245,0.));
#103961=CARTESIAN_POINT('Ctrl Pts',(23.1581765788869,69.0238291885245,12.));
#103962=CARTESIAN_POINT('Ctrl Pts',(23.1567755350472,69.0492554078999,0.));
#103963=CARTESIAN_POINT('Ctrl Pts',(23.1567755350472,69.0492554078999,12.));
#103964=CARTESIAN_POINT('Ctrl Pts',(23.1553482598767,69.0747193789292,0.));
#103965=CARTESIAN_POINT('Ctrl Pts',(23.1553482598767,69.0747193789292,12.));
#103966=CARTESIAN_POINT('Ctrl Pts',(23.1538947054619,69.1002209957037,0.));
#103967=CARTESIAN_POINT('Ctrl Pts',(23.1538947054619,69.1002209957037,12.));
#103968=CARTESIAN_POINT('Ctrl Pts',(23.1524148241413,69.1257601526693,0.));
#103969=CARTESIAN_POINT('Ctrl Pts',(23.1524148241413,69.1257601526693,12.));
#103970=CARTESIAN_POINT('Ctrl Pts',(23.1509085685032,69.1513367446231,0.));
#103971=CARTESIAN_POINT('Ctrl Pts',(23.1509085685032,69.1513367446231,12.));
#103972=CARTESIAN_POINT('Ctrl Pts',(23.1493758913857,69.176950666708,0.));
#103973=CARTESIAN_POINT('Ctrl Pts',(23.1493758913857,69.176950666708,12.));
#103974=CARTESIAN_POINT('Ctrl Pts',(23.1478167458787,69.2026018144023,0.));
#103975=CARTESIAN_POINT('Ctrl Pts',(23.1478167458787,69.2026018144023,12.));
#103976=CARTESIAN_POINT('Ctrl Pts',(23.1462310853205,69.2282900835234,0.));
#103977=CARTESIAN_POINT('Ctrl Pts',(23.1462310853205,69.2282900835234,12.));
#103978=CARTESIAN_POINT('Ctrl Pts',(23.1446188632931,69.2540153702311,0.));
#103979=CARTESIAN_POINT('Ctrl Pts',(23.1446188632931,69.2540153702311,12.));
#103980=CARTESIAN_POINT('Ctrl Pts',(23.142980033622,69.2797775710275,0.));
#103981=CARTESIAN_POINT('Ctrl Pts',(23.142980033622,69.2797775710275,12.));
#103982=CARTESIAN_POINT('Ctrl Pts',(23.1413145503762,69.3055765827544,0.));
#103983=CARTESIAN_POINT('Ctrl Pts',(23.1413145503762,69.3055765827544,12.));
#103984=CARTESIAN_POINT('Ctrl Pts',(23.1396223678725,69.3314123025863,0.));
#103985=CARTESIAN_POINT('Ctrl Pts',(23.1396223678725,69.3314123025863,12.));
#103986=CARTESIAN_POINT('Ctrl Pts',(23.1379034406717,69.3572846280289,0.));
#103987=CARTESIAN_POINT('Ctrl Pts',(23.1379034406717,69.3572846280289,12.));
#103988=CARTESIAN_POINT('Ctrl Pts',(23.1361577235708,69.3831934569176,0.));
#103989=CARTESIAN_POINT('Ctrl Pts',(23.1361577235708,69.3831934569176,12.));
#103990=CARTESIAN_POINT('Ctrl Pts',(23.1343851715988,69.4091386874129,0.));
#103991=CARTESIAN_POINT('Ctrl Pts',(23.1343851715988,69.4091386874129,12.));
#103992=CARTESIAN_POINT('Ctrl Pts',(23.1325857400145,69.4351202179948,0.));
#103993=CARTESIAN_POINT('Ctrl Pts',(23.1325857400145,69.4351202179948,12.));
#103994=CARTESIAN_POINT('Ctrl Pts',(23.1307593843063,69.4611379474492,0.));
#103995=CARTESIAN_POINT('Ctrl Pts',(23.1307593843063,69.4611379474492,12.));
#103996=CARTESIAN_POINT('Ctrl Pts',(23.1289060601927,69.4871917748665,0.));
#103997=CARTESIAN_POINT('Ctrl Pts',(23.1289060601927,69.4871917748665,12.));
#103998=CARTESIAN_POINT('Ctrl Pts',(23.1270257236207,69.5132815996548,0.));
#103999=CARTESIAN_POINT('Ctrl Pts',(23.1270257236207,69.5132815996548,12.));
#104000=CARTESIAN_POINT('Ctrl Pts',(23.1251183307678,69.5394073215467,0.));
#104001=CARTESIAN_POINT('Ctrl Pts',(23.1251183307678,69.5394073215467,12.));
#104002=CARTESIAN_POINT('Ctrl Pts',(23.1231838380452,69.565568840605,0.));
#104003=CARTESIAN_POINT('Ctrl Pts',(23.1231838380452,69.565568840605,12.));
#104004=CARTESIAN_POINT('Ctrl Pts',(23.1212222021049,69.5917660572255,0.));
#104005=CARTESIAN_POINT('Ctrl Pts',(23.1212222021049,69.5917660572255,12.));
#104006=CARTESIAN_POINT('Ctrl Pts',(23.1192333798437,69.617998872135,0.));
#104007=CARTESIAN_POINT('Ctrl Pts',(23.1192333798437,69.617998872135,12.));
#104008=CARTESIAN_POINT('Ctrl Pts',(23.1172173283855,69.6442671863751,0.));
#104009=CARTESIAN_POINT('Ctrl Pts',(23.1172173283855,69.6442671863751,12.));
#104010=CARTESIAN_POINT('Ctrl Pts',(23.1151740050678,69.6705709012842,0.));
#104011=CARTESIAN_POINT('Ctrl Pts',(23.1151740050678,69.6705709012842,12.));
#104012=CARTESIAN_POINT('Ctrl Pts',(23.1131033674301,69.6969099184766,0.));
#104013=CARTESIAN_POINT('Ctrl Pts',(23.1131033674301,69.6969099184766,12.));
#104014=CARTESIAN_POINT('Ctrl Pts',(23.1110053732049,69.7232841398207,0.));
#104015=CARTESIAN_POINT('Ctrl Pts',(23.1110053732049,69.7232841398207,12.));
#104016=CARTESIAN_POINT('Ctrl Pts',(23.1088799803093,69.7496934674083,0.));
#104017=CARTESIAN_POINT('Ctrl Pts',(23.1088799803093,69.7496934674083,12.));
#104018=CARTESIAN_POINT('Ctrl Pts',(23.1067271468614,69.7761378035979,0.));
#104019=CARTESIAN_POINT('Ctrl Pts',(23.1067271468614,69.7761378035979,12.));
#104020=CARTESIAN_POINT('Ctrl Pts',(23.1045468311994,69.8026170510582,0.));
#104021=CARTESIAN_POINT('Ctrl Pts',(23.1045468311994,69.8026170510582,12.));
#104022=CARTESIAN_POINT('Ctrl Pts',(23.1023389919052,69.8291311128121,0.));
#104023=CARTESIAN_POINT('Ctrl Pts',(23.1023389919052,69.8291311128121,12.));
#104024=CARTESIAN_POINT('Ctrl Pts',(23.100103587824,69.8556798922688,0.));
#104025=CARTESIAN_POINT('Ctrl Pts',(23.100103587824,69.8556798922688,12.));
#104026=CARTESIAN_POINT('Ctrl Pts',(23.0978405781018,69.882263293276,0.));
#104027=CARTESIAN_POINT('Ctrl Pts',(23.0978405781018,69.882263293276,12.));
#104028=CARTESIAN_POINT('Ctrl Pts',(23.0955499221555,69.9088812200704,0.));
#104029=CARTESIAN_POINT('Ctrl Pts',(23.0955499221555,69.9088812200704,12.));
#104030=CARTESIAN_POINT('Ctrl Pts',(23.0932315796066,69.9355335771722,0.));
#104031=CARTESIAN_POINT('Ctrl Pts',(23.0932315796066,69.9355335771722,12.));
#104032=CARTESIAN_POINT('Ctrl Pts',(23.090885510225,69.9622202692871,0.));
#104033=CARTESIAN_POINT('Ctrl Pts',(23.090885510225,69.9622202692871,12.));
#104034=CARTESIAN_POINT('Ctrl Pts',(23.0885116738798,69.9889412012143,0.));
#104035=CARTESIAN_POINT('Ctrl Pts',(23.0885116738798,69.9889412012143,12.));
#104036=CARTESIAN_POINT('Ctrl Pts',(23.0861100304731,70.0156962777173,0.));
#104037=CARTESIAN_POINT('Ctrl Pts',(23.0861100304731,70.0156962777173,12.));
#104038=CARTESIAN_POINT('Ctrl Pts',(23.0836805399377,70.0424854035125,0.));
#104039=CARTESIAN_POINT('Ctrl Pts',(23.0836805399377,70.0424854035125,12.));
#104040=CARTESIAN_POINT('Ctrl Pts',(23.081223162377,70.0693084835388,0.));
#104041=CARTESIAN_POINT('Ctrl Pts',(23.081223162377,70.0693084835388,12.));
#104042=CARTESIAN_POINT('Ctrl Pts',(23.0787378581778,70.096165423165,0.));
#104043=CARTESIAN_POINT('Ctrl Pts',(23.0787378581778,70.096165423165,12.));
#104044=CARTESIAN_POINT('Ctrl Pts',(23.076224588139,70.1230561284222,0.));
#104045=CARTESIAN_POINT('Ctrl Pts',(23.076224588139,70.1230561284222,12.));
#104046=CARTESIAN_POINT('Ctrl Pts',(23.0736833135934,70.1499805062159,0.));
#104047=CARTESIAN_POINT('Ctrl Pts',(23.0736833135934,70.1499805062159,12.));
#104048=CARTESIAN_POINT('Ctrl Pts',(23.0711139965432,70.176938464556,0.));
#104049=CARTESIAN_POINT('Ctrl Pts',(23.0711139965432,70.176938464556,12.));
#104050=CARTESIAN_POINT('Ctrl Pts',(23.0685165993681,70.2039299120456,0.));
#104051=CARTESIAN_POINT('Ctrl Pts',(23.0685165993681,70.2039299120456,12.));
#104052=CARTESIAN_POINT('Ctrl Pts',(23.0658910845425,70.2309547573789,0.));
#104053=CARTESIAN_POINT('Ctrl Pts',(23.0658910845425,70.2309547573789,12.));
#104054=CARTESIAN_POINT('Ctrl Pts',(23.0632374143276,70.2580129087878,0.));
#104055=CARTESIAN_POINT('Ctrl Pts',(23.0632374143276,70.2580129087878,12.));
#104056=CARTESIAN_POINT('Ctrl Pts',(23.0605555505326,70.2851042736081,0.));
#104057=CARTESIAN_POINT('Ctrl Pts',(23.0605555505326,70.2851042736081,12.));
#104058=CARTESIAN_POINT('Ctrl Pts',(23.0578454541116,70.3122287575374,0.));
#104059=CARTESIAN_POINT('Ctrl Pts',(23.0578454541116,70.3122287575374,12.));
#104060=CARTESIAN_POINT('Ctrl Pts',(23.0551070854942,70.3393862652353,0.));
#104061=CARTESIAN_POINT('Ctrl Pts',(23.0551070854942,70.3393862652353,12.));
#104062=CARTESIAN_POINT('Ctrl Pts',(23.0523404053188,70.3665767016596,0.));
#104063=CARTESIAN_POINT('Ctrl Pts',(23.0523404053188,70.3665767016596,12.));
#104064=CARTESIAN_POINT('Ctrl Pts',(23.0495453750773,70.39379997323,0.));
#104065=CARTESIAN_POINT('Ctrl Pts',(23.0495453750773,70.39379997323,12.));
#104066=CARTESIAN_POINT('Ctrl Pts',(23.0467219577288,70.421055988934,0.));
#104067=CARTESIAN_POINT('Ctrl Pts',(23.0467219577288,70.421055988934,12.));
#104068=CARTESIAN_POINT('Ctrl Pts',(23.0438701184995,70.4483446617553,0.));
#104069=CARTESIAN_POINT('Ctrl Pts',(23.0438701184995,70.4483446617553,12.));
#104070=CARTESIAN_POINT('Ctrl Pts',(23.0409898250726,70.4756659090104,0.));
#104071=CARTESIAN_POINT('Ctrl Pts',(23.0409898250726,70.4756659090104,12.));
#104072=CARTESIAN_POINT('Ctrl Pts',(23.0380810458237,70.5030196491883,0.));
#104073=CARTESIAN_POINT('Ctrl Pts',(23.0380810458237,70.5030196491883,12.));
#104074=CARTESIAN_POINT('Ctrl Pts',(23.0351437484309,70.5304057994537,0.));
#104075=CARTESIAN_POINT('Ctrl Pts',(23.0351437484309,70.5304057994537,12.));
#104076=CARTESIAN_POINT('Ctrl Pts',(23.0321778982705,70.5578242727606,0.));
#104077=CARTESIAN_POINT('Ctrl Pts',(23.0321778982705,70.5578242727606,12.));
#104078=CARTESIAN_POINT('Ctrl Pts',(23.0291834570688,70.5852749754168,0.));
#104079=CARTESIAN_POINT('Ctrl Pts',(23.0291834570688,70.5852749754168,12.));
#104080=CARTESIAN_POINT('Ctrl Pts',(23.0261603810187,70.6127578036869,0.));
#104081=CARTESIAN_POINT('Ctrl Pts',(23.0261603810187,70.6127578036869,12.));
#104082=CARTESIAN_POINT('Ctrl Pts',(23.0231086235262,70.6402726486718,0.));
#104083=CARTESIAN_POINT('Ctrl Pts',(23.0231086235262,70.6402726486718,12.));
#104084=CARTESIAN_POINT('Ctrl Pts',(23.0200281385906,70.6678194023389,0.));
#104085=CARTESIAN_POINT('Ctrl Pts',(23.0200281385906,70.6678194023389,12.));
#104086=CARTESIAN_POINT('Ctrl Pts',(23.0169188841083,70.6953979633561,0.));
#104087=CARTESIAN_POINT('Ctrl Pts',(23.0169188841083,70.6953979633561,12.));
#104088=CARTESIAN_POINT('Ctrl Pts',(23.0137808248898,70.7230082425324,0.));
#104089=CARTESIAN_POINT('Ctrl Pts',(23.0137808248898,70.7230082425324,12.));
#104090=CARTESIAN_POINT('Ctrl Pts',(23.0106139365941,70.7506501695822,0.));
#104091=CARTESIAN_POINT('Ctrl Pts',(23.0106139365941,70.7506501695822,12.));
#104092=CARTESIAN_POINT('Ctrl Pts',(23.007418206361,70.7783236950588,0.));
#104093=CARTESIAN_POINT('Ctrl Pts',(23.007418206361,70.7783236950588,12.));
#104094=CARTESIAN_POINT('Ctrl Pts',(23.004193629142,70.806028785987,0.));
#104095=CARTESIAN_POINT('Ctrl Pts',(23.004193629142,70.806028785987,12.));
#104096=CARTESIAN_POINT('Ctrl Pts',(23.0015908899222,70.8282180956627,0.));
#104097=CARTESIAN_POINT('Ctrl Pts',(23.0015908899222,70.8282180956627,12.));
#104098=CARTESIAN_POINT('Ctrl Pts',(22.9996258555187,70.8448742696329,0.));
#104099=CARTESIAN_POINT('Ctrl Pts',(22.9996258555187,70.8448742696329,12.));
#104100=CARTESIAN_POINT('Ctrl Pts',(22.9983100639353,70.8559846927868,0.));
#104101=CARTESIAN_POINT('Ctrl Pts',(22.9983100639353,70.8559846927868,12.));
#104102=CARTESIAN_POINT('Ctrl Pts',(22.9976507259816,70.8615414811572,0.));
#104103=CARTESIAN_POINT('Ctrl Pts',(22.9976507259816,70.8615414811572,12.));
#104104=CARTESIAN_POINT('',(23.1372951448024,66.0656156664138,0.));
#104105=CARTESIAN_POINT('Ctrl Pts',(23.1372951448024,66.0656156664138,0.));
#104106=CARTESIAN_POINT('Ctrl Pts',(23.1375957166104,66.0694876382127,0.));
#104107=CARTESIAN_POINT('Ctrl Pts',(23.1381951597399,66.0772371487248,0.));
#104108=CARTESIAN_POINT('Ctrl Pts',(23.1390892229778,66.0888781152421,0.));
#104109=CARTESIAN_POINT('Ctrl Pts',(23.1402711039425,66.1044328067355,0.));
#104110=CARTESIAN_POINT('Ctrl Pts',(23.1417314398398,66.1239318368548,0.));
#104111=CARTESIAN_POINT('Ctrl Pts',(23.1431747350098,66.1434865015027,0.));
#104112=CARTESIAN_POINT('Ctrl Pts',(23.1446009424903,66.1630967296747,0.));
#104113=CARTESIAN_POINT('Ctrl Pts',(23.1460099850763,66.18276239029,0.));
#104114=CARTESIAN_POINT('Ctrl Pts',(23.1474017566484,66.2024832934866,0.));
#104115=CARTESIAN_POINT('Ctrl Pts',(23.1487761349328,66.2222592165473,0.));
#104116=CARTESIAN_POINT('Ctrl Pts',(23.1501329914487,66.2420899237317,0.));
#104117=CARTESIAN_POINT('Ctrl Pts',(23.1514722022483,66.2619751878741,0.));
#104118=CARTESIAN_POINT('Ctrl Pts',(23.1527936592625,66.2819148131072,0.));
#104119=CARTESIAN_POINT('Ctrl Pts',(23.154097266617,66.301908627539,0.));
#104120=CARTESIAN_POINT('Ctrl Pts',(23.1553829352531,66.3219564725161,0.));
#104121=CARTESIAN_POINT('Ctrl Pts',(23.1566505784626,66.3420581937159,0.));
#104122=CARTESIAN_POINT('Ctrl Pts',(23.1579001063438,66.3622136300692,0.));
#104123=CARTESIAN_POINT('Ctrl Pts',(23.15913142301,66.382422608185,0.));
#104124=CARTESIAN_POINT('Ctrl Pts',(23.1603444294754,66.402684948127,0.));
#104125=CARTESIAN_POINT('Ctrl Pts',(23.1615390254635,66.4230004670288,0.));
#104126=CARTESIAN_POINT('Ctrl Pts',(23.1627151114875,66.4433689832454,0.));
#104127=CARTESIAN_POINT('Ctrl Pts',(23.163872591218,66.4637903210682,0.));
#104128=CARTESIAN_POINT('Ctrl Pts',(23.1650113713792,66.4842643105263,0.));
#104129=CARTESIAN_POINT('Ctrl Pts',(23.1661313606123,66.5047907851319,0.));
#104130=CARTESIAN_POINT('Ctrl Pts',(23.1672324686927,66.5253695803209,0.));
#104131=CARTESIAN_POINT('Ctrl Pts',(23.1683146055736,66.5460005315406,0.));
#104132=CARTESIAN_POINT('Ctrl Pts',(23.169377680588,66.5666834726495,0.));
#104133=CARTESIAN_POINT('Ctrl Pts',(23.1704216028626,66.5874182367597,0.));
#104134=CARTESIAN_POINT('Ctrl Pts',(23.1714462816794,66.6082046569657,0.));
#104135=CARTESIAN_POINT('Ctrl Pts',(23.1724516268299,66.6290425670538,0.));
#104136=CARTESIAN_POINT('Ctrl Pts',(23.1734375490421,66.6499318023445,0.));
#104137=CARTESIAN_POINT('Ctrl Pts',(23.174403960137,66.6708722000046,0.));
#104138=CARTESIAN_POINT('Ctrl Pts',(23.1753507727931,66.691863598595,0.));
#104139=CARTESIAN_POINT('Ctrl Pts',(23.1762779004043,66.712905837789,0.));
#104140=CARTESIAN_POINT('Ctrl Pts',(23.1771852569136,66.7339987580441,0.));
#104141=CARTESIAN_POINT('Ctrl Pts',(23.1780727566309,66.7551422002229,0.));
#104142=CARTESIAN_POINT('Ctrl Pts',(23.1789403142375,66.7763360056146,0.));
#104143=CARTESIAN_POINT('Ctrl Pts',(23.1797878448645,66.7975800161014,0.));
#104144=CARTESIAN_POINT('Ctrl Pts',(23.1806152641475,66.8188740742727,0.));
#104145=CARTESIAN_POINT('Ctrl Pts',(23.1814224882948,66.840218023555,0.));
#104146=CARTESIAN_POINT('Ctrl Pts',(23.1822094341508,66.8616117083304,0.));
#104147=CARTESIAN_POINT('Ctrl Pts',(23.1829760191582,66.8830549738768,0.));
#104148=CARTESIAN_POINT('Ctrl Pts',(23.1837221613231,66.904547666305,0.));
#104149=CARTESIAN_POINT('Ctrl Pts',(23.1844477791816,66.9260896324955,0.));
#104150=CARTESIAN_POINT('Ctrl Pts',(23.1851527917665,66.9476807200225,0.));
#104151=CARTESIAN_POINT('Ctrl Pts',(23.1858371185852,66.9693207771059,0.));
#104152=CARTESIAN_POINT('Ctrl Pts',(23.1865006796291,66.9910096526483,0.));
#104153=CARTESIAN_POINT('Ctrl Pts',(23.1871433953795,67.0127471962507,0.));
#104154=CARTESIAN_POINT('Ctrl Pts',(23.1877651868155,67.0345332582297,0.));
#104155=CARTESIAN_POINT('Ctrl Pts',(23.1883659754267,67.0563676896312,0.));
#104156=CARTESIAN_POINT('Ctrl Pts',(23.1889456832115,67.0782503422293,0.));
#104157=CARTESIAN_POINT('Ctrl Pts',(23.1895042326625,67.1001810685138,0.));
#104158=CARTESIAN_POINT('Ctrl Pts',(23.1900415467574,67.122159721674,0.));
#104159=CARTESIAN_POINT('Ctrl Pts',(23.1905575489505,67.1441861555819,0.));
#104160=CARTESIAN_POINT('Ctrl Pts',(23.1910521631658,67.1662602247641,0.));
#104161=CARTESIAN_POINT('Ctrl Pts',(23.1915253137923,67.1883817844039,0.));
#104162=CARTESIAN_POINT('Ctrl Pts',(23.1919769256803,67.2105506903448,0.));
#104163=CARTESIAN_POINT('Ctrl Pts',(23.1924069241385,67.232766799088,0.));
#104164=CARTESIAN_POINT('Ctrl Pts',(23.1928152349343,67.2550299677888,0.));
#104165=CARTESIAN_POINT('Ctrl Pts',(23.1932017842954,67.2773400542477,0.));
#104166=CARTESIAN_POINT('Ctrl Pts',(23.193566498902,67.2996969169099,0.));
#104167=CARTESIAN_POINT('Ctrl Pts',(23.1939093058802,67.3221004148604,0.));
#104168=CARTESIAN_POINT('Ctrl Pts',(23.1942301327978,67.3445504078178,0.));
#104169=CARTESIAN_POINT('Ctrl Pts',(23.1945289076608,67.3670467561205,0.));
#104170=CARTESIAN_POINT('Ctrl Pts',(23.1948055589123,67.3895893207168,0.));
#104171=CARTESIAN_POINT('Ctrl Pts',(23.1950600154259,67.4121779631666,0.));
#104172=CARTESIAN_POINT('Ctrl Pts',(23.1952922065009,67.4348125456389,0.));
#104173=CARTESIAN_POINT('Ctrl Pts',(23.1955020618591,67.4574929309079,0.));
#104174=CARTESIAN_POINT('Ctrl Pts',(23.1956895116446,67.4802189823424,0.));
#104175=CARTESIAN_POINT('Ctrl Pts',(23.1958544864224,67.5029905638974,0.));
#104176=CARTESIAN_POINT('Ctrl Pts',(23.1959969171709,67.525807540117,0.));
#104177=CARTESIAN_POINT('Ctrl Pts',(23.1961167352776,67.5486697761301,0.));
#104178=CARTESIAN_POINT('Ctrl Pts',(23.1962138725358,67.5715771376454,0.));
#104179=CARTESIAN_POINT('Ctrl Pts',(23.1962882611443,67.5945294909398,0.));
#104180=CARTESIAN_POINT('Ctrl Pts',(23.1963398337055,67.6175267028517,0.));
#104181=CARTESIAN_POINT('Ctrl Pts',(23.1963685232176,67.6405686407828,0.));
#104182=CARTESIAN_POINT('Ctrl Pts',(23.1963742630709,67.6636551726948,0.));
#104183=CARTESIAN_POINT('Ctrl Pts',(23.1963569870456,67.6867861671045,0.));
#104184=CARTESIAN_POINT('Ctrl Pts',(23.1963166293116,67.7099614930712,0.));
#104185=CARTESIAN_POINT('Ctrl Pts',(23.1962531244261,67.7331810201931,0.));
#104186=CARTESIAN_POINT('Ctrl Pts',(23.1961664073273,67.7564446186115,0.));
#104187=CARTESIAN_POINT('Ctrl Pts',(23.1960564133308,67.7797521590056,0.));
#104188=CARTESIAN_POINT('Ctrl Pts',(23.1959230781265,67.8031035125873,0.));
#104189=CARTESIAN_POINT('Ctrl Pts',(23.1957663377797,67.8264985510884,0.));
#104190=CARTESIAN_POINT('Ctrl Pts',(23.1955861287275,67.8499371467578,0.));
#104191=CARTESIAN_POINT('Ctrl Pts',(23.1953823877726,67.8734191723639,0.));
#104192=CARTESIAN_POINT('Ctrl Pts',(23.19515505208,67.8969445011908,0.));
#104193=CARTESIAN_POINT('Ctrl Pts',(23.1949040591748,67.9205130070337,0.));
#104194=CARTESIAN_POINT('Ctrl Pts',(23.1946293469436,67.9441245641871,0.));
#104195=CARTESIAN_POINT('Ctrl Pts',(23.1943308536307,67.9677790474414,0.));
#104196=CARTESIAN_POINT('Ctrl Pts',(23.1940085178319,67.9914763320878,0.));
#104197=CARTESIAN_POINT('Ctrl Pts',(23.193662278492,68.0152162939123,0.));
#104198=CARTESIAN_POINT('Ctrl Pts',(23.1932920749021,68.0389988091926,0.));
#104199=CARTESIAN_POINT('Ctrl Pts',(23.1928978467017,68.0628237546853,0.));
#104200=CARTESIAN_POINT('Ctrl Pts',(23.1924795338745,68.086691007624,0.));
#104201=CARTESIAN_POINT('Ctrl Pts',(23.1920370767423,68.1106004457223,0.));
#104202=CARTESIAN_POINT('Ctrl Pts',(23.1915704159623,68.1345519471695,0.));
#104203=CARTESIAN_POINT('Ctrl Pts',(23.1910794925252,68.1585453906259,0.));
#104204=CARTESIAN_POINT('Ctrl Pts',(23.1905642477571,68.182580655213,0.));
#104205=CARTESIAN_POINT('Ctrl Pts',(23.1900246233164,68.2066576205113,0.));
#104206=CARTESIAN_POINT('Ctrl Pts',(23.1894605611869,68.2307761665629,0.));
#104207=CARTESIAN_POINT('Ctrl Pts',(23.1888720036756,68.2549361738679,0.));
#104208=CARTESIAN_POINT('Ctrl Pts',(23.1882588934108,68.2791375233798,0.));
#104209=CARTESIAN_POINT('Ctrl Pts',(23.1876211733439,68.3033800964946,0.));
#104210=CARTESIAN_POINT('Ctrl Pts',(23.1869587867463,68.3276637750494,0.));
#104211=CARTESIAN_POINT('Ctrl Pts',(23.1862716772034,68.3519884413253,0.));
#104212=CARTESIAN_POINT('Ctrl Pts',(23.1855597886117,68.3763539780442,0.));
#104213=CARTESIAN_POINT('Ctrl Pts',(23.1848230651775,68.4007602683649,0.));
#104214=CARTESIAN_POINT('Ctrl Pts',(23.184061451419,68.4252071958725,0.));
#104215=CARTESIAN_POINT('Ctrl Pts',(23.1832748921629,68.4496946445756,0.));
#104216=CARTESIAN_POINT('Ctrl Pts',(23.1824633325384,68.4742224989099,0.));
#104217=CARTESIAN_POINT('Ctrl Pts',(23.1816267179751,68.4987906437357,0.));
#104218=CARTESIAN_POINT('Ctrl Pts',(23.180764994201,68.5233989643344,0.));
#104219=CARTESIAN_POINT('Ctrl Pts',(23.1798781072449,68.548047346398,0.));
#104220=CARTESIAN_POINT('Ctrl Pts',(23.1789660034339,68.572735676027,0.));
#104221=CARTESIAN_POINT('Ctrl Pts',(23.1780286293873,68.5974638397322,0.));
#104222=CARTESIAN_POINT('Ctrl Pts',(23.1770659320136,68.6222317244337,0.));
#104223=CARTESIAN_POINT('Ctrl Pts',(23.1760778585093,68.6470392174567,0.));
#104224=CARTESIAN_POINT('Ctrl Pts',(23.1750643563605,68.6718862065227,0.));
#104225=CARTESIAN_POINT('Ctrl Pts',(23.1740253733423,68.6967725797458,0.));
#104226=CARTESIAN_POINT('Ctrl Pts',(23.1729608575115,68.7216982256357,0.));
#104227=CARTESIAN_POINT('Ctrl Pts',(23.1718707572046,68.7466630330968,0.));
#104228=CARTESIAN_POINT('Ctrl Pts',(23.1707550210359,68.7716668914246,0.));
#104229=CARTESIAN_POINT('Ctrl Pts',(23.1696135978992,68.7967096902981,0.));
#104230=CARTESIAN_POINT('Ctrl Pts',(23.1684464369681,68.8217913197735,0.));
#104231=CARTESIAN_POINT('Ctrl Pts',(23.1672534876885,68.8469116702885,0.));
#104232=CARTESIAN_POINT('Ctrl Pts',(23.1660346997762,68.8720706326606,0.));
#104233=CARTESIAN_POINT('Ctrl Pts',(23.1647900232151,68.8972680980844,0.));
#104234=CARTESIAN_POINT('Ctrl Pts',(23.1635194082581,68.9225039581249,0.));
#104235=CARTESIAN_POINT('Ctrl Pts',(23.162222805429,68.9477781047103,0.));
#104236=CARTESIAN_POINT('Ctrl Pts',(23.1609001655153,68.9730904301363,0.));
#104237=CARTESIAN_POINT('Ctrl Pts',(23.1595514395654,68.9984408270653,0.));
#104238=CARTESIAN_POINT('Ctrl Pts',(23.1581765788869,69.0238291885245,0.));
#104239=CARTESIAN_POINT('Ctrl Pts',(23.1567755350472,69.0492554078999,0.));
#104240=CARTESIAN_POINT('Ctrl Pts',(23.1553482598767,69.0747193789292,0.));
#104241=CARTESIAN_POINT('Ctrl Pts',(23.1538947054619,69.1002209957037,0.));
#104242=CARTESIAN_POINT('Ctrl Pts',(23.1524148241413,69.1257601526693,0.));
#104243=CARTESIAN_POINT('Ctrl Pts',(23.1509085685032,69.1513367446231,0.));
#104244=CARTESIAN_POINT('Ctrl Pts',(23.1493758913857,69.176950666708,0.));
#104245=CARTESIAN_POINT('Ctrl Pts',(23.1478167458787,69.2026018144023,0.));
#104246=CARTESIAN_POINT('Ctrl Pts',(23.1462310853205,69.2282900835234,0.));
#104247=CARTESIAN_POINT('Ctrl Pts',(23.1446188632931,69.2540153702311,0.));
#104248=CARTESIAN_POINT('Ctrl Pts',(23.142980033622,69.2797775710275,0.));
#104249=CARTESIAN_POINT('Ctrl Pts',(23.1413145503762,69.3055765827544,0.));
#104250=CARTESIAN_POINT('Ctrl Pts',(23.1396223678725,69.3314123025863,0.));
#104251=CARTESIAN_POINT('Ctrl Pts',(23.1379034406717,69.3572846280289,0.));
#104252=CARTESIAN_POINT('Ctrl Pts',(23.1361577235708,69.3831934569176,0.));
#104253=CARTESIAN_POINT('Ctrl Pts',(23.1343851715988,69.4091386874129,0.));
#104254=CARTESIAN_POINT('Ctrl Pts',(23.1325857400145,69.4351202179948,0.));
#104255=CARTESIAN_POINT('Ctrl Pts',(23.1307593843063,69.4611379474492,0.));
#104256=CARTESIAN_POINT('Ctrl Pts',(23.1289060601927,69.4871917748665,0.));
#104257=CARTESIAN_POINT('Ctrl Pts',(23.1270257236207,69.5132815996548,0.));
#104258=CARTESIAN_POINT('Ctrl Pts',(23.1251183307678,69.5394073215467,0.));
#104259=CARTESIAN_POINT('Ctrl Pts',(23.1231838380452,69.565568840605,0.));
#104260=CARTESIAN_POINT('Ctrl Pts',(23.1212222021049,69.5917660572255,0.));
#104261=CARTESIAN_POINT('Ctrl Pts',(23.1192333798437,69.617998872135,0.));
#104262=CARTESIAN_POINT('Ctrl Pts',(23.1172173283855,69.6442671863751,0.));
#104263=CARTESIAN_POINT('Ctrl Pts',(23.1151740050678,69.6705709012842,0.));
#104264=CARTESIAN_POINT('Ctrl Pts',(23.1131033674301,69.6969099184766,0.));
#104265=CARTESIAN_POINT('Ctrl Pts',(23.1110053732049,69.7232841398207,0.));
#104266=CARTESIAN_POINT('Ctrl Pts',(23.1088799803093,69.7496934674083,0.));
#104267=CARTESIAN_POINT('Ctrl Pts',(23.1067271468614,69.7761378035979,0.));
#104268=CARTESIAN_POINT('Ctrl Pts',(23.1045468311994,69.8026170510582,0.));
#104269=CARTESIAN_POINT('Ctrl Pts',(23.1023389919052,69.8291311128121,0.));
#104270=CARTESIAN_POINT('Ctrl Pts',(23.100103587824,69.8556798922688,0.));
#104271=CARTESIAN_POINT('Ctrl Pts',(23.0978405781018,69.882263293276,0.));
#104272=CARTESIAN_POINT('Ctrl Pts',(23.0955499221555,69.9088812200704,0.));
#104273=CARTESIAN_POINT('Ctrl Pts',(23.0932315796066,69.9355335771722,0.));
#104274=CARTESIAN_POINT('Ctrl Pts',(23.090885510225,69.9622202692871,0.));
#104275=CARTESIAN_POINT('Ctrl Pts',(23.0885116738798,69.9889412012143,0.));
#104276=CARTESIAN_POINT('Ctrl Pts',(23.0861100304731,70.0156962777173,0.));
#104277=CARTESIAN_POINT('Ctrl Pts',(23.0836805399377,70.0424854035125,0.));
#104278=CARTESIAN_POINT('Ctrl Pts',(23.081223162377,70.0693084835388,0.));
#104279=CARTESIAN_POINT('Ctrl Pts',(23.0787378581778,70.096165423165,0.));
#104280=CARTESIAN_POINT('Ctrl Pts',(23.076224588139,70.1230561284222,0.));
#104281=CARTESIAN_POINT('Ctrl Pts',(23.0736833135934,70.1499805062159,0.));
#104282=CARTESIAN_POINT('Ctrl Pts',(23.0711139965432,70.176938464556,0.));
#104283=CARTESIAN_POINT('Ctrl Pts',(23.0685165993681,70.2039299120456,0.));
#104284=CARTESIAN_POINT('Ctrl Pts',(23.0658910845425,70.2309547573789,0.));
#104285=CARTESIAN_POINT('Ctrl Pts',(23.0632374143276,70.2580129087878,0.));
#104286=CARTESIAN_POINT('Ctrl Pts',(23.0605555505326,70.2851042736081,0.));
#104287=CARTESIAN_POINT('Ctrl Pts',(23.0578454541116,70.3122287575374,0.));
#104288=CARTESIAN_POINT('Ctrl Pts',(23.0551070854942,70.3393862652353,0.));
#104289=CARTESIAN_POINT('Ctrl Pts',(23.0523404053188,70.3665767016596,0.));
#104290=CARTESIAN_POINT('Ctrl Pts',(23.0495453750773,70.39379997323,0.));
#104291=CARTESIAN_POINT('Ctrl Pts',(23.0467219577288,70.421055988934,0.));
#104292=CARTESIAN_POINT('Ctrl Pts',(23.0438701184995,70.4483446617553,0.));
#104293=CARTESIAN_POINT('Ctrl Pts',(23.0409898250726,70.4756659090104,0.));
#104294=CARTESIAN_POINT('Ctrl Pts',(23.038496437601,70.4991133648755,0.));
#104295=CARTESIAN_POINT('Ctrl Pts',(23.0365694096158,70.5171075702494,0.));
#104296=CARTESIAN_POINT('Ctrl Pts',(23.0352213647764,70.529634153525,0.));
#104297=CARTESIAN_POINT('Ctrl Pts',(23.034460662331,70.5366836381296,0.));
#104298=CARTESIAN_POINT('Ctrl Pts',(23.0342913834094,70.5382514078485,0.));
#104299=CARTESIAN_POINT('',(23.1372951448024,66.0656156664138,12.));
#104300=CARTESIAN_POINT('',(23.1372951448024,66.0656156664138,0.));
#104301=CARTESIAN_POINT('Ctrl Pts',(23.0342913834094,70.5382514078485,12.));
#104302=CARTESIAN_POINT('Ctrl Pts',(23.034460662331,70.5366836381296,12.));
#104303=CARTESIAN_POINT('Ctrl Pts',(23.0352213647764,70.529634153525,12.));
#104304=CARTESIAN_POINT('Ctrl Pts',(23.0365694096158,70.5171075702494,12.));
#104305=CARTESIAN_POINT('Ctrl Pts',(23.038496437601,70.4991133648755,12.));
#104306=CARTESIAN_POINT('Ctrl Pts',(23.0409898250726,70.4756659090104,12.));
#104307=CARTESIAN_POINT('Ctrl Pts',(23.0438701184995,70.4483446617553,12.));
#104308=CARTESIAN_POINT('Ctrl Pts',(23.0467219577288,70.421055988934,12.));
#104309=CARTESIAN_POINT('Ctrl Pts',(23.0495453750773,70.39379997323,12.));
#104310=CARTESIAN_POINT('Ctrl Pts',(23.0523404053188,70.3665767016596,12.));
#104311=CARTESIAN_POINT('Ctrl Pts',(23.0551070854942,70.3393862652353,12.));
#104312=CARTESIAN_POINT('Ctrl Pts',(23.0578454541116,70.3122287575374,12.));
#104313=CARTESIAN_POINT('Ctrl Pts',(23.0605555505326,70.2851042736081,12.));
#104314=CARTESIAN_POINT('Ctrl Pts',(23.0632374143276,70.2580129087878,12.));
#104315=CARTESIAN_POINT('Ctrl Pts',(23.0658910845425,70.2309547573789,12.));
#104316=CARTESIAN_POINT('Ctrl Pts',(23.0685165993681,70.2039299120456,12.));
#104317=CARTESIAN_POINT('Ctrl Pts',(23.0711139965432,70.176938464556,12.));
#104318=CARTESIAN_POINT('Ctrl Pts',(23.0736833135934,70.1499805062159,12.));
#104319=CARTESIAN_POINT('Ctrl Pts',(23.076224588139,70.1230561284222,12.));
#104320=CARTESIAN_POINT('Ctrl Pts',(23.0787378581778,70.096165423165,12.));
#104321=CARTESIAN_POINT('Ctrl Pts',(23.081223162377,70.0693084835388,12.));
#104322=CARTESIAN_POINT('Ctrl Pts',(23.0836805399377,70.0424854035125,12.));
#104323=CARTESIAN_POINT('Ctrl Pts',(23.0861100304731,70.0156962777173,12.));
#104324=CARTESIAN_POINT('Ctrl Pts',(23.0885116738798,69.9889412012143,12.));
#104325=CARTESIAN_POINT('Ctrl Pts',(23.090885510225,69.9622202692871,12.));
#104326=CARTESIAN_POINT('Ctrl Pts',(23.0932315796066,69.9355335771722,12.));
#104327=CARTESIAN_POINT('Ctrl Pts',(23.0955499221555,69.9088812200704,12.));
#104328=CARTESIAN_POINT('Ctrl Pts',(23.0978405781018,69.882263293276,12.));
#104329=CARTESIAN_POINT('Ctrl Pts',(23.100103587824,69.8556798922688,12.));
#104330=CARTESIAN_POINT('Ctrl Pts',(23.1023389919052,69.8291311128121,12.));
#104331=CARTESIAN_POINT('Ctrl Pts',(23.1045468311994,69.8026170510582,12.));
#104332=CARTESIAN_POINT('Ctrl Pts',(23.1067271468614,69.7761378035979,12.));
#104333=CARTESIAN_POINT('Ctrl Pts',(23.1088799803093,69.7496934674083,12.));
#104334=CARTESIAN_POINT('Ctrl Pts',(23.1110053732049,69.7232841398207,12.));
#104335=CARTESIAN_POINT('Ctrl Pts',(23.1131033674301,69.6969099184766,12.));
#104336=CARTESIAN_POINT('Ctrl Pts',(23.1151740050678,69.6705709012842,12.));
#104337=CARTESIAN_POINT('Ctrl Pts',(23.1172173283855,69.6442671863751,12.));
#104338=CARTESIAN_POINT('Ctrl Pts',(23.1192333798437,69.617998872135,12.));
#104339=CARTESIAN_POINT('Ctrl Pts',(23.1212222021049,69.5917660572255,12.));
#104340=CARTESIAN_POINT('Ctrl Pts',(23.1231838380452,69.565568840605,12.));
#104341=CARTESIAN_POINT('Ctrl Pts',(23.1251183307678,69.5394073215467,12.));
#104342=CARTESIAN_POINT('Ctrl Pts',(23.1270257236207,69.5132815996548,12.));
#104343=CARTESIAN_POINT('Ctrl Pts',(23.1289060601927,69.4871917748665,12.));
#104344=CARTESIAN_POINT('Ctrl Pts',(23.1307593843063,69.4611379474492,12.));
#104345=CARTESIAN_POINT('Ctrl Pts',(23.1325857400145,69.4351202179948,12.));
#104346=CARTESIAN_POINT('Ctrl Pts',(23.1343851715988,69.4091386874129,12.));
#104347=CARTESIAN_POINT('Ctrl Pts',(23.1361577235708,69.3831934569176,12.));
#104348=CARTESIAN_POINT('Ctrl Pts',(23.1379034406717,69.3572846280289,12.));
#104349=CARTESIAN_POINT('Ctrl Pts',(23.1396223678725,69.3314123025863,12.));
#104350=CARTESIAN_POINT('Ctrl Pts',(23.1413145503762,69.3055765827544,12.));
#104351=CARTESIAN_POINT('Ctrl Pts',(23.142980033622,69.2797775710275,12.));
#104352=CARTESIAN_POINT('Ctrl Pts',(23.1446188632931,69.2540153702311,12.));
#104353=CARTESIAN_POINT('Ctrl Pts',(23.1462310853205,69.2282900835234,12.));
#104354=CARTESIAN_POINT('Ctrl Pts',(23.1478167458787,69.2026018144023,12.));
#104355=CARTESIAN_POINT('Ctrl Pts',(23.1493758913857,69.176950666708,12.));
#104356=CARTESIAN_POINT('Ctrl Pts',(23.1509085685032,69.1513367446231,12.));
#104357=CARTESIAN_POINT('Ctrl Pts',(23.1524148241413,69.1257601526693,12.));
#104358=CARTESIAN_POINT('Ctrl Pts',(23.1538947054619,69.1002209957037,12.));
#104359=CARTESIAN_POINT('Ctrl Pts',(23.1553482598767,69.0747193789292,12.));
#104360=CARTESIAN_POINT('Ctrl Pts',(23.1567755350472,69.0492554078999,12.));
#104361=CARTESIAN_POINT('Ctrl Pts',(23.1581765788869,69.0238291885245,12.));
#104362=CARTESIAN_POINT('Ctrl Pts',(23.1595514395654,68.9984408270653,12.));
#104363=CARTESIAN_POINT('Ctrl Pts',(23.1609001655153,68.9730904301363,12.));
#104364=CARTESIAN_POINT('Ctrl Pts',(23.162222805429,68.9477781047103,12.));
#104365=CARTESIAN_POINT('Ctrl Pts',(23.1635194082581,68.9225039581249,12.));
#104366=CARTESIAN_POINT('Ctrl Pts',(23.1647900232151,68.8972680980844,12.));
#104367=CARTESIAN_POINT('Ctrl Pts',(23.1660346997762,68.8720706326606,12.));
#104368=CARTESIAN_POINT('Ctrl Pts',(23.1672534876885,68.8469116702885,12.));
#104369=CARTESIAN_POINT('Ctrl Pts',(23.1684464369681,68.8217913197735,12.));
#104370=CARTESIAN_POINT('Ctrl Pts',(23.1696135978992,68.7967096902981,12.));
#104371=CARTESIAN_POINT('Ctrl Pts',(23.1707550210359,68.7716668914246,12.));
#104372=CARTESIAN_POINT('Ctrl Pts',(23.1718707572046,68.7466630330968,12.));
#104373=CARTESIAN_POINT('Ctrl Pts',(23.1729608575115,68.7216982256357,12.));
#104374=CARTESIAN_POINT('Ctrl Pts',(23.1740253733423,68.6967725797458,12.));
#104375=CARTESIAN_POINT('Ctrl Pts',(23.1750643563605,68.6718862065227,12.));
#104376=CARTESIAN_POINT('Ctrl Pts',(23.1760778585093,68.6470392174567,12.));
#104377=CARTESIAN_POINT('Ctrl Pts',(23.1770659320136,68.6222317244337,12.));
#104378=CARTESIAN_POINT('Ctrl Pts',(23.1780286293873,68.5974638397322,12.));
#104379=CARTESIAN_POINT('Ctrl Pts',(23.1789660034339,68.572735676027,12.));
#104380=CARTESIAN_POINT('Ctrl Pts',(23.1798781072449,68.548047346398,12.));
#104381=CARTESIAN_POINT('Ctrl Pts',(23.180764994201,68.5233989643344,12.));
#104382=CARTESIAN_POINT('Ctrl Pts',(23.1816267179751,68.4987906437357,12.));
#104383=CARTESIAN_POINT('Ctrl Pts',(23.1824633325384,68.4742224989099,12.));
#104384=CARTESIAN_POINT('Ctrl Pts',(23.1832748921629,68.4496946445756,12.));
#104385=CARTESIAN_POINT('Ctrl Pts',(23.184061451419,68.4252071958725,12.));
#104386=CARTESIAN_POINT('Ctrl Pts',(23.1848230651775,68.4007602683649,12.));
#104387=CARTESIAN_POINT('Ctrl Pts',(23.1855597886117,68.3763539780442,12.));
#104388=CARTESIAN_POINT('Ctrl Pts',(23.1862716772034,68.3519884413253,12.));
#104389=CARTESIAN_POINT('Ctrl Pts',(23.1869587867463,68.3276637750494,12.));
#104390=CARTESIAN_POINT('Ctrl Pts',(23.1876211733439,68.3033800964946,12.));
#104391=CARTESIAN_POINT('Ctrl Pts',(23.1882588934108,68.2791375233798,12.));
#104392=CARTESIAN_POINT('Ctrl Pts',(23.1888720036756,68.2549361738679,12.));
#104393=CARTESIAN_POINT('Ctrl Pts',(23.1894605611869,68.2307761665629,12.));
#104394=CARTESIAN_POINT('Ctrl Pts',(23.1900246233164,68.2066576205113,12.));
#104395=CARTESIAN_POINT('Ctrl Pts',(23.1905642477571,68.182580655213,12.));
#104396=CARTESIAN_POINT('Ctrl Pts',(23.1910794925252,68.1585453906259,12.));
#104397=CARTESIAN_POINT('Ctrl Pts',(23.1915704159623,68.1345519471695,12.));
#104398=CARTESIAN_POINT('Ctrl Pts',(23.1920370767423,68.1106004457223,12.));
#104399=CARTESIAN_POINT('Ctrl Pts',(23.1924795338745,68.086691007624,12.));
#104400=CARTESIAN_POINT('Ctrl Pts',(23.1928978467017,68.0628237546853,12.));
#104401=CARTESIAN_POINT('Ctrl Pts',(23.1932920749021,68.0389988091926,12.));
#104402=CARTESIAN_POINT('Ctrl Pts',(23.193662278492,68.0152162939123,12.));
#104403=CARTESIAN_POINT('Ctrl Pts',(23.1940085178319,67.9914763320878,12.));
#104404=CARTESIAN_POINT('Ctrl Pts',(23.1943308536307,67.9677790474414,12.));
#104405=CARTESIAN_POINT('Ctrl Pts',(23.1946293469436,67.9441245641871,12.));
#104406=CARTESIAN_POINT('Ctrl Pts',(23.1949040591748,67.9205130070337,12.));
#104407=CARTESIAN_POINT('Ctrl Pts',(23.19515505208,67.8969445011908,12.));
#104408=CARTESIAN_POINT('Ctrl Pts',(23.1953823877726,67.8734191723639,12.));
#104409=CARTESIAN_POINT('Ctrl Pts',(23.1955861287275,67.8499371467578,12.));
#104410=CARTESIAN_POINT('Ctrl Pts',(23.1957663377797,67.8264985510884,12.));
#104411=CARTESIAN_POINT('Ctrl Pts',(23.1959230781265,67.8031035125873,12.));
#104412=CARTESIAN_POINT('Ctrl Pts',(23.1960564133308,67.7797521590056,12.));
#104413=CARTESIAN_POINT('Ctrl Pts',(23.1961664073273,67.7564446186115,12.));
#104414=CARTESIAN_POINT('Ctrl Pts',(23.1962531244261,67.7331810201931,12.));
#104415=CARTESIAN_POINT('Ctrl Pts',(23.1963166293116,67.7099614930712,12.));
#104416=CARTESIAN_POINT('Ctrl Pts',(23.1963569870456,67.6867861671045,12.));
#104417=CARTESIAN_POINT('Ctrl Pts',(23.1963742630709,67.6636551726948,12.));
#104418=CARTESIAN_POINT('Ctrl Pts',(23.1963685232176,67.6405686407828,12.));
#104419=CARTESIAN_POINT('Ctrl Pts',(23.1963398337055,67.6175267028517,12.));
#104420=CARTESIAN_POINT('Ctrl Pts',(23.1962882611443,67.5945294909398,12.));
#104421=CARTESIAN_POINT('Ctrl Pts',(23.1962138725358,67.5715771376454,12.));
#104422=CARTESIAN_POINT('Ctrl Pts',(23.1961167352776,67.5486697761301,12.));
#104423=CARTESIAN_POINT('Ctrl Pts',(23.1959969171709,67.525807540117,12.));
#104424=CARTESIAN_POINT('Ctrl Pts',(23.1958544864224,67.5029905638974,12.));
#104425=CARTESIAN_POINT('Ctrl Pts',(23.1956895116446,67.4802189823424,12.));
#104426=CARTESIAN_POINT('Ctrl Pts',(23.1955020618591,67.4574929309079,12.));
#104427=CARTESIAN_POINT('Ctrl Pts',(23.1952922065009,67.4348125456389,12.));
#104428=CARTESIAN_POINT('Ctrl Pts',(23.1950600154259,67.4121779631666,12.));
#104429=CARTESIAN_POINT('Ctrl Pts',(23.1948055589123,67.3895893207168,12.));
#104430=CARTESIAN_POINT('Ctrl Pts',(23.1945289076608,67.3670467561205,12.));
#104431=CARTESIAN_POINT('Ctrl Pts',(23.1942301327978,67.3445504078178,12.));
#104432=CARTESIAN_POINT('Ctrl Pts',(23.1939093058802,67.3221004148604,12.));
#104433=CARTESIAN_POINT('Ctrl Pts',(23.193566498902,67.2996969169099,12.));
#104434=CARTESIAN_POINT('Ctrl Pts',(23.1932017842954,67.2773400542477,12.));
#104435=CARTESIAN_POINT('Ctrl Pts',(23.1928152349343,67.2550299677888,12.));
#104436=CARTESIAN_POINT('Ctrl Pts',(23.1924069241385,67.232766799088,12.));
#104437=CARTESIAN_POINT('Ctrl Pts',(23.1919769256803,67.2105506903448,12.));
#104438=CARTESIAN_POINT('Ctrl Pts',(23.1915253137923,67.1883817844039,12.));
#104439=CARTESIAN_POINT('Ctrl Pts',(23.1910521631658,67.1662602247641,12.));
#104440=CARTESIAN_POINT('Ctrl Pts',(23.1905575489505,67.1441861555819,12.));
#104441=CARTESIAN_POINT('Ctrl Pts',(23.1900415467574,67.122159721674,12.));
#104442=CARTESIAN_POINT('Ctrl Pts',(23.1895042326625,67.1001810685138,12.));
#104443=CARTESIAN_POINT('Ctrl Pts',(23.1889456832115,67.0782503422293,12.));
#104444=CARTESIAN_POINT('Ctrl Pts',(23.1883659754267,67.0563676896312,12.));
#104445=CARTESIAN_POINT('Ctrl Pts',(23.1877651868155,67.0345332582297,12.));
#104446=CARTESIAN_POINT('Ctrl Pts',(23.1871433953795,67.0127471962507,12.));
#104447=CARTESIAN_POINT('Ctrl Pts',(23.1865006796291,66.9910096526483,12.));
#104448=CARTESIAN_POINT('Ctrl Pts',(23.1858371185852,66.9693207771059,12.));
#104449=CARTESIAN_POINT('Ctrl Pts',(23.1851527917665,66.9476807200225,12.));
#104450=CARTESIAN_POINT('Ctrl Pts',(23.1844477791816,66.9260896324955,12.));
#104451=CARTESIAN_POINT('Ctrl Pts',(23.1837221613231,66.904547666305,12.));
#104452=CARTESIAN_POINT('Ctrl Pts',(23.1829760191582,66.8830549738768,12.));
#104453=CARTESIAN_POINT('Ctrl Pts',(23.1822094341508,66.8616117083304,12.));
#104454=CARTESIAN_POINT('Ctrl Pts',(23.1814224882948,66.840218023555,12.));
#104455=CARTESIAN_POINT('Ctrl Pts',(23.1806152641475,66.8188740742727,12.));
#104456=CARTESIAN_POINT('Ctrl Pts',(23.1797878448645,66.7975800161014,12.));
#104457=CARTESIAN_POINT('Ctrl Pts',(23.1789403142375,66.7763360056146,12.));
#104458=CARTESIAN_POINT('Ctrl Pts',(23.1780727566309,66.7551422002229,12.));
#104459=CARTESIAN_POINT('Ctrl Pts',(23.1771852569136,66.7339987580441,12.));
#104460=CARTESIAN_POINT('Ctrl Pts',(23.1762779004043,66.712905837789,12.));
#104461=CARTESIAN_POINT('Ctrl Pts',(23.1753507727931,66.691863598595,12.));
#104462=CARTESIAN_POINT('Ctrl Pts',(23.174403960137,66.6708722000046,12.));
#104463=CARTESIAN_POINT('Ctrl Pts',(23.1734375490421,66.6499318023445,12.));
#104464=CARTESIAN_POINT('Ctrl Pts',(23.1724516268299,66.6290425670538,12.));
#104465=CARTESIAN_POINT('Ctrl Pts',(23.1714462816794,66.6082046569657,12.));
#104466=CARTESIAN_POINT('Ctrl Pts',(23.1704216028626,66.5874182367597,12.));
#104467=CARTESIAN_POINT('Ctrl Pts',(23.169377680588,66.5666834726495,12.));
#104468=CARTESIAN_POINT('Ctrl Pts',(23.1683146055736,66.5460005315406,12.));
#104469=CARTESIAN_POINT('Ctrl Pts',(23.1672324686927,66.5253695803209,12.));
#104470=CARTESIAN_POINT('Ctrl Pts',(23.1661313606123,66.5047907851319,12.));
#104471=CARTESIAN_POINT('Ctrl Pts',(23.1650113713792,66.4842643105263,12.));
#104472=CARTESIAN_POINT('Ctrl Pts',(23.163872591218,66.4637903210682,12.));
#104473=CARTESIAN_POINT('Ctrl Pts',(23.1627151114875,66.4433689832454,12.));
#104474=CARTESIAN_POINT('Ctrl Pts',(23.1615390254635,66.4230004670288,12.));
#104475=CARTESIAN_POINT('Ctrl Pts',(23.1603444294754,66.402684948127,12.));
#104476=CARTESIAN_POINT('Ctrl Pts',(23.15913142301,66.382422608185,12.));
#104477=CARTESIAN_POINT('Ctrl Pts',(23.1579001063438,66.3622136300692,12.));
#104478=CARTESIAN_POINT('Ctrl Pts',(23.1566505784626,66.3420581937159,12.));
#104479=CARTESIAN_POINT('Ctrl Pts',(23.1553829352531,66.3219564725161,12.));
#104480=CARTESIAN_POINT('Ctrl Pts',(23.154097266617,66.301908627539,12.));
#104481=CARTESIAN_POINT('Ctrl Pts',(23.1527936592625,66.2819148131072,12.));
#104482=CARTESIAN_POINT('Ctrl Pts',(23.1514722022483,66.2619751878741,12.));
#104483=CARTESIAN_POINT('Ctrl Pts',(23.1501329914487,66.2420899237317,12.));
#104484=CARTESIAN_POINT('Ctrl Pts',(23.1487761349328,66.2222592165473,12.));
#104485=CARTESIAN_POINT('Ctrl Pts',(23.1474017566484,66.2024832934866,12.));
#104486=CARTESIAN_POINT('Ctrl Pts',(23.1460099850763,66.18276239029,12.));
#104487=CARTESIAN_POINT('Ctrl Pts',(23.1446009424903,66.1630967296747,12.));
#104488=CARTESIAN_POINT('Ctrl Pts',(23.1431747350098,66.1434865015027,12.));
#104489=CARTESIAN_POINT('Ctrl Pts',(23.1417314398398,66.1239318368548,12.));
#104490=CARTESIAN_POINT('Ctrl Pts',(23.1402711039425,66.1044328067355,12.));
#104491=CARTESIAN_POINT('Ctrl Pts',(23.1390892229778,66.0888781152421,12.));
#104492=CARTESIAN_POINT('Ctrl Pts',(23.1381951597399,66.0772371487248,12.));
#104493=CARTESIAN_POINT('Ctrl Pts',(23.1375957166104,66.0694876382127,12.));
#104494=CARTESIAN_POINT('Ctrl Pts',(23.1372951448024,66.0656156664138,12.));
#104495=CARTESIAN_POINT('Ctrl Pts',(21.5904919935065,70.993479606912,-5.55111512312578E-16));
#104496=CARTESIAN_POINT('Ctrl Pts',(21.5904919935065,70.993479606912,4.));
#104497=CARTESIAN_POINT('Ctrl Pts',(21.5904919935065,70.993479606912,8.));
#104498=CARTESIAN_POINT('Ctrl Pts',(21.5904919935065,70.993479606912,12.));
#104499=CARTESIAN_POINT('Ctrl Pts',(21.6628164325804,71.0762040404458,-5.55111512312578E-16));
#104500=CARTESIAN_POINT('Ctrl Pts',(21.6628164325804,71.0762040404458,3.99999999999999));
#104501=CARTESIAN_POINT('Ctrl Pts',(21.6628164325804,71.0762040404458,8.));
#104502=CARTESIAN_POINT('Ctrl Pts',(21.6628164325804,71.0762040404458,12.));
#104503=CARTESIAN_POINT('Ctrl Pts',(21.8385342042358,71.1771795679078,-5.55111512312578E-16));
#104504=CARTESIAN_POINT('Ctrl Pts',(21.8385342042358,71.1771795679078,4.00000000000001));
#104505=CARTESIAN_POINT('Ctrl Pts',(21.8385342042358,71.1771795679079,7.99999999999999));
#104506=CARTESIAN_POINT('Ctrl Pts',(21.8385342042358,71.1771795679079,12.));
#104507=CARTESIAN_POINT('Ctrl Pts',(22.0366423876805,71.1663065220502,-5.55111512312578E-16));
#104508=CARTESIAN_POINT('Ctrl Pts',(22.0366423876805,71.1663065220502,3.99999999999999));
#104509=CARTESIAN_POINT('Ctrl Pts',(22.0366423876805,71.1663065220503,8.00000000000001));
#104510=CARTESIAN_POINT('Ctrl Pts',(22.0366423876805,71.1663065220503,12.));
#104511=CARTESIAN_POINT('Ctrl Pts',(22.1153394458685,71.1418425484888,-5.55111512312578E-16));
#104512=CARTESIAN_POINT('Ctrl Pts',(22.1153394458685,71.1418425484888,4.));
#104513=CARTESIAN_POINT('Ctrl Pts',(22.1153394458685,71.1418425484888,8.));
#104514=CARTESIAN_POINT('Ctrl Pts',(22.1153394458685,71.1418425484888,12.));
#104515=CARTESIAN_POINT('',(21.5904919935065,70.993479606912,0.));
#104516=CARTESIAN_POINT('',(22.1153394458686,71.1418425484891,0.));
#104517=CARTESIAN_POINT('Ctrl Pts',(21.5904919935065,70.993479606912,0.));
#104518=CARTESIAN_POINT('Ctrl Pts',(21.6628164325804,71.0762040404458,-6.93334779979405E-31));
#104519=CARTESIAN_POINT('Ctrl Pts',(21.7632265878121,71.1339043418527,3.85185988877447E-31));
#104520=CARTESIAN_POINT('Ctrl Pts',(21.8709478979137,71.1550826601348,1.54074395550979E-31));
#104521=CARTESIAN_POINT('Ctrl Pts',(21.9517388804899,71.1709663988463,-3.08148791101957E-32));
#104522=CARTESIAN_POINT('Ctrl Pts',(22.0366423876805,71.1663065220502,-9.55261252416069E-31));
#104523=CARTESIAN_POINT('Ctrl Pts',(22.1153394458685,71.1418425484888,4.62223186652938E-32));
#104524=CARTESIAN_POINT('',(22.1153394458686,71.1418425484891,12.));
#104525=CARTESIAN_POINT('Ctrl Pts',(22.1153394458685,71.1418425484888,-5.55111512312578E-16));
#104526=CARTESIAN_POINT('Ctrl Pts',(22.1153394458685,71.1418425484888,4.));
#104527=CARTESIAN_POINT('Ctrl Pts',(22.1153394458685,71.1418425484888,8.));
#104528=CARTESIAN_POINT('Ctrl Pts',(22.1153394458685,71.1418425484888,12.));
#104529=CARTESIAN_POINT('',(21.5904919935065,70.993479606912,12.));
#104530=CARTESIAN_POINT('Ctrl Pts',(22.1153394458685,71.1418425484888,12.));
#104531=CARTESIAN_POINT('Ctrl Pts',(22.0366423876805,71.1663065220503,12.));
#104532=CARTESIAN_POINT('Ctrl Pts',(21.9517388804899,71.1709663988464,12.));
#104533=CARTESIAN_POINT('Ctrl Pts',(21.8709478979137,71.1550826601348,12.));
#104534=CARTESIAN_POINT('Ctrl Pts',(21.7632265878121,71.1339043418527,12.));
#104535=CARTESIAN_POINT('Ctrl Pts',(21.6628164325804,71.0762040404458,12.));
#104536=CARTESIAN_POINT('Ctrl Pts',(21.5904919935065,70.993479606912,12.));
#104537=CARTESIAN_POINT('Ctrl Pts',(21.5904919935065,70.993479606912,12.));
#104538=CARTESIAN_POINT('Ctrl Pts',(21.5904919935065,70.993479606912,8.));
#104539=CARTESIAN_POINT('Ctrl Pts',(21.5904919935065,70.993479606912,4.));
#104540=CARTESIAN_POINT('Ctrl Pts',(21.5904919935065,70.993479606912,-5.55111512312578E-16));
#104541=CARTESIAN_POINT('Origin',(1.12623029467293E-10,3.57524700084383E-10,
0.));
#104542=CARTESIAN_POINT('Origin',(1.12623029467293E-10,3.57524700084383E-10,
12.));
#104543=CARTESIAN_POINT('Origin',(1.12623029467293E-10,3.57524700084383E-10,
0.));
#104544=CARTESIAN_POINT('Ctrl Pts',(28.787762030239,68.7132793373328,0.));
#104545=CARTESIAN_POINT('Ctrl Pts',(28.787762030239,68.7132793373328,4.));
#104546=CARTESIAN_POINT('Ctrl Pts',(28.787762030239,68.7132793373328,8.));
#104547=CARTESIAN_POINT('Ctrl Pts',(28.787762030239,68.7132793373328,12.));
#104548=CARTESIAN_POINT('Ctrl Pts',(28.8891094745185,68.670819333438,0.));
#104549=CARTESIAN_POINT('Ctrl Pts',(28.8891094745185,68.670819333438,4.));
#104550=CARTESIAN_POINT('Ctrl Pts',(28.8891094745185,68.670819333438,8.));
#104551=CARTESIAN_POINT('Ctrl Pts',(28.8891094745185,68.670819333438,12.));
#104552=CARTESIAN_POINT('Ctrl Pts',(29.0404604348956,68.5360395709812,0.));
#104553=CARTESIAN_POINT('Ctrl Pts',(29.0404604348956,68.5360395709812,4.));
#104554=CARTESIAN_POINT('Ctrl Pts',(29.0404604348956,68.5360395709812,7.99999999999999));
#104555=CARTESIAN_POINT('Ctrl Pts',(29.0404604348956,68.5360395709812,12.));
#104556=CARTESIAN_POINT('Ctrl Pts',(29.0927805237117,68.3446561754308,0.));
#104557=CARTESIAN_POINT('Ctrl Pts',(29.0927805237117,68.3446561754308,4.));
#104558=CARTESIAN_POINT('Ctrl Pts',(29.0927805237117,68.3446561754308,8.00000000000001));
#104559=CARTESIAN_POINT('Ctrl Pts',(29.0927805237117,68.3446561754308,12.));
#104560=CARTESIAN_POINT('Ctrl Pts',(29.0944526440247,68.2622612909745,0.));
#104561=CARTESIAN_POINT('Ctrl Pts',(29.0944526440247,68.2622612909745,4.));
#104562=CARTESIAN_POINT('Ctrl Pts',(29.0944526440247,68.2622612909745,8.));
#104563=CARTESIAN_POINT('Ctrl Pts',(29.0944526440247,68.2622612909745,12.));
#104564=CARTESIAN_POINT('',(28.787762030239,68.7132793373328,0.));
#104565=CARTESIAN_POINT('',(29.0944526440248,68.2622612909745,0.));
#104566=CARTESIAN_POINT('Ctrl Pts',(28.787762030239,68.7132793373328,0.));
#104567=CARTESIAN_POINT('Ctrl Pts',(28.8891094745185,68.670819333438,0.));
#104568=CARTESIAN_POINT('Ctrl Pts',(28.9755957375911,68.5938023263198,0.));
#104569=CARTESIAN_POINT('Ctrl Pts',(29.0297453895418,68.4983025002323,0.));
#104570=CARTESIAN_POINT('Ctrl Pts',(29.0703576285048,68.4266776306667,0.));
#104571=CARTESIAN_POINT('Ctrl Pts',(29.0927805237117,68.3446561754308,0.));
#104572=CARTESIAN_POINT('Ctrl Pts',(29.0944526440247,68.2622612909745,0.));
#104573=CARTESIAN_POINT('',(29.0944526440248,68.2622612909745,12.));
#104574=CARTESIAN_POINT('Ctrl Pts',(29.0944526440247,68.2622612909745,0.));
#104575=CARTESIAN_POINT('Ctrl Pts',(29.0944526440247,68.2622612909745,4.));
#104576=CARTESIAN_POINT('Ctrl Pts',(29.0944526440247,68.2622612909745,8.));
#104577=CARTESIAN_POINT('Ctrl Pts',(29.0944526440247,68.2622612909745,12.));
#104578=CARTESIAN_POINT('',(28.787762030239,68.7132793373328,12.));
#104579=CARTESIAN_POINT('Ctrl Pts',(29.0944526440247,68.2622612909745,12.));
#104580=CARTESIAN_POINT('Ctrl Pts',(29.0927805237117,68.3446561754308,12.));
#104581=CARTESIAN_POINT('Ctrl Pts',(29.0703576285048,68.4266776306667,12.));
#104582=CARTESIAN_POINT('Ctrl Pts',(29.0297453895418,68.4983025002323,12.));
#104583=CARTESIAN_POINT('Ctrl Pts',(28.9755957375911,68.5938023263198,12.));
#104584=CARTESIAN_POINT('Ctrl Pts',(28.8891094745185,68.670819333438,12.));
#104585=CARTESIAN_POINT('Ctrl Pts',(28.787762030239,68.7132793373328,12.));
#104586=CARTESIAN_POINT('Ctrl Pts',(28.787762030239,68.7132793373328,12.));
#104587=CARTESIAN_POINT('Ctrl Pts',(28.787762030239,68.7132793373328,8.));
#104588=CARTESIAN_POINT('Ctrl Pts',(28.787762030239,68.7132793373328,4.));
#104589=CARTESIAN_POINT('Ctrl Pts',(28.787762030239,68.7132793373328,0.));
#104590=CARTESIAN_POINT('Ctrl Pts',(28.8072485549236,63.7976679095314,0.));
#104591=CARTESIAN_POINT('Ctrl Pts',(28.8072485549236,63.7976679095314,12.));
#104592=CARTESIAN_POINT('Ctrl Pts',(28.8078854475432,63.8014989507494,0.));
#104593=CARTESIAN_POINT('Ctrl Pts',(28.8078854475432,63.8014989507494,12.));
#104594=CARTESIAN_POINT('Ctrl Pts',(28.8091580239553,63.8091667271232,0.));
#104595=CARTESIAN_POINT('Ctrl Pts',(28.8091580239553,63.8091667271232,12.));
#104596=CARTESIAN_POINT('Ctrl Pts',(28.8110632620957,63.8206854735028,0.));
#104597=CARTESIAN_POINT('Ctrl Pts',(28.8110632620957,63.8206854735028,12.));
#104598=CARTESIAN_POINT('Ctrl Pts',(28.8135963263368,63.8360779669856,0.));
#104599=CARTESIAN_POINT('Ctrl Pts',(28.8135963263368,63.8360779669856,12.));
#104600=CARTESIAN_POINT('Ctrl Pts',(28.8167505576681,63.8553755207487,0.));
#104601=CARTESIAN_POINT('Ctrl Pts',(28.8167505576681,63.8553755207487,12.));
#104602=CARTESIAN_POINT('Ctrl Pts',(28.8198926619857,63.8747299825313,0.));
#104603=CARTESIAN_POINT('Ctrl Pts',(28.8198926619857,63.8747299825313,12.));
#104604=CARTESIAN_POINT('Ctrl Pts',(28.823022586318,63.8941412856924,0.));
#104605=CARTESIAN_POINT('Ctrl Pts',(28.823022586318,63.8941412856924,12.));
#104606=CARTESIAN_POINT('Ctrl Pts',(28.8261402423291,63.9136093063786,0.));
#104607=CARTESIAN_POINT('Ctrl Pts',(28.8261402423291,63.9136093063786,12.));
#104608=CARTESIAN_POINT('Ctrl Pts',(28.8292455077559,63.9331338646996,0.));
#104609=CARTESIAN_POINT('Ctrl Pts',(28.8292455077559,63.9331338646996,12.));
#104610=CARTESIAN_POINT('Ctrl Pts',(28.8323382413789,63.9527147494423,0.));
#104611=CARTESIAN_POINT('Ctrl Pts',(28.8323382413789,63.9527147494423,12.));
#104612=CARTESIAN_POINT('Ctrl Pts',(28.83541829466,63.9723517369614,0.));
#104613=CARTESIAN_POINT('Ctrl Pts',(28.83541829466,63.9723517369614,12.));
#104614=CARTESIAN_POINT('Ctrl Pts',(28.8384855243242,63.9920446117582,0.));
#104615=CARTESIAN_POINT('Ctrl Pts',(28.8384855243242,63.9920446117582,12.));
#104616=CARTESIAN_POINT('Ctrl Pts',(28.8415398056428,64.0117931881298,0.));
#104617=CARTESIAN_POINT('Ctrl Pts',(28.8415398056428,64.0117931881298,12.));
#104618=CARTESIAN_POINT('Ctrl Pts',(28.844581028125,64.0315973031942,0.));
#104619=CARTESIAN_POINT('Ctrl Pts',(28.844581028125,64.0315973031942,12.));
#104620=CARTESIAN_POINT('Ctrl Pts',(28.8476090892232,64.0514568066637,0.));
#104621=CARTESIAN_POINT('Ctrl Pts',(28.8476090892232,64.0514568066637,12.));
#104622=CARTESIAN_POINT('Ctrl Pts',(28.8506238891092,64.0713715523599,0.));
#104623=CARTESIAN_POINT('Ctrl Pts',(28.8506238891092,64.0713715523599,12.));
#104624=CARTESIAN_POINT('Ctrl Pts',(28.8536253241853,64.0913413876622,0.));
#104625=CARTESIAN_POINT('Ctrl Pts',(28.8536253241853,64.0913413876622,12.));
#104626=CARTESIAN_POINT('Ctrl Pts',(28.8566132838178,64.1113661481965,0.));
#104627=CARTESIAN_POINT('Ctrl Pts',(28.8566132838178,64.1113661481965,12.));
#104628=CARTESIAN_POINT('Ctrl Pts',(28.8595876537148,64.1314456633381,0.));
#104629=CARTESIAN_POINT('Ctrl Pts',(28.8595876537148,64.1314456633381,12.));
#104630=CARTESIAN_POINT('Ctrl Pts',(28.8625483180437,64.1515797596564,0.));
#104631=CARTESIAN_POINT('Ctrl Pts',(28.8625483180437,64.1515797596564,12.));
#104632=CARTESIAN_POINT('Ctrl Pts',(28.8654951618649,64.1717682648685,0.));
#104633=CARTESIAN_POINT('Ctrl Pts',(28.8654951618649,64.1717682648685,12.));
#104634=CARTESIAN_POINT('Ctrl Pts',(28.8684280739014,64.1920110123299,0.));
#104635=CARTESIAN_POINT('Ctrl Pts',(28.8684280739014,64.1920110123299,12.));
#104636=CARTESIAN_POINT('Ctrl Pts',(28.8713469464185,64.2123078408461,0.));
#104637=CARTESIAN_POINT('Ctrl Pts',(28.8713469464185,64.2123078408461,12.));
#104638=CARTESIAN_POINT('Ctrl Pts',(28.8742516738946,64.2326585925252,0.));
#104639=CARTESIAN_POINT('Ctrl Pts',(28.8742516738946,64.2326585925252,12.));
#104640=CARTESIAN_POINT('Ctrl Pts',(28.877142152106,64.2530631112929,0.));
#104641=CARTESIAN_POINT('Ctrl Pts',(28.877142152106,64.2530631112929,12.));
#104642=CARTESIAN_POINT('Ctrl Pts',(28.8800182770064,64.2735212410711,0.));
#104643=CARTESIAN_POINT('Ctrl Pts',(28.8800182770064,64.2735212410711,12.));
#104644=CARTESIAN_POINT('Ctrl Pts',(28.882879943794,64.2940328242521,0.));
#104645=CARTESIAN_POINT('Ctrl Pts',(28.882879943794,64.2940328242521,12.));
#104646=CARTESIAN_POINT('Ctrl Pts',(28.8857270473959,64.3145977025037,0.));
#104647=CARTESIAN_POINT('Ctrl Pts',(28.8857270473959,64.3145977025037,12.));
#104648=CARTESIAN_POINT('Ctrl Pts',(28.8885594828926,64.3352157174619,0.));
#104649=CARTESIAN_POINT('Ctrl Pts',(28.8885594828926,64.3352157174619,12.));
#104650=CARTESIAN_POINT('Ctrl Pts',(28.8913771459323,64.3558867114076,0.));
#104651=CARTESIAN_POINT('Ctrl Pts',(28.8913771459323,64.3558867114076,12.));
#104652=CARTESIAN_POINT('Ctrl Pts',(28.89417993323,64.3766105280688,0.));
#104653=CARTESIAN_POINT('Ctrl Pts',(28.89417993323,64.3766105280688,12.));
#104654=CARTESIAN_POINT('Ctrl Pts',(28.8969677427504,64.397387012917,0.));
#104655=CARTESIAN_POINT('Ctrl Pts',(28.8969677427504,64.397387012917,12.));
#104656=CARTESIAN_POINT('Ctrl Pts',(28.899740473434,64.4182160127379,0.));
#104657=CARTESIAN_POINT('Ctrl Pts',(28.899740473434,64.4182160127379,12.));
#104658=CARTESIAN_POINT('Ctrl Pts',(28.9024980250307,64.4390973753634,0.));
#104659=CARTESIAN_POINT('Ctrl Pts',(28.9024980250307,64.4390973753634,12.));
#104660=CARTESIAN_POINT('Ctrl Pts',(28.9052402979062,64.4600309493583,0.));
#104661=CARTESIAN_POINT('Ctrl Pts',(28.9052402979062,64.4600309493583,12.));
#104662=CARTESIAN_POINT('Ctrl Pts',(28.9079671928264,64.4810165836592,0.));
#104663=CARTESIAN_POINT('Ctrl Pts',(28.9079671928264,64.4810165836592,12.));
#104664=CARTESIAN_POINT('Ctrl Pts',(28.910678610965,64.5020541275951,0.));
#104665=CARTESIAN_POINT('Ctrl Pts',(28.910678610965,64.5020541275951,12.));
#104666=CARTESIAN_POINT('Ctrl Pts',(28.9133744539949,64.523143431047,0.));
#104667=CARTESIAN_POINT('Ctrl Pts',(28.9133744539949,64.523143431047,12.));
#104668=CARTESIAN_POINT('Ctrl Pts',(28.9160546241538,64.5442843445559,0.));
#104669=CARTESIAN_POINT('Ctrl Pts',(28.9160546241538,64.5442843445559,12.));
#104670=CARTESIAN_POINT('Ctrl Pts',(28.9187190243224,64.5654767194472,0.));
#104671=CARTESIAN_POINT('Ctrl Pts',(28.9187190243224,64.5654767194472,12.));
#104672=CARTESIAN_POINT('Ctrl Pts',(28.9213675580985,64.5867204079426,0.));
#104673=CARTESIAN_POINT('Ctrl Pts',(28.9213675580985,64.5867204079426,12.));
#104674=CARTESIAN_POINT('Ctrl Pts',(28.9240001297542,64.6080152631039,0.));
#104675=CARTESIAN_POINT('Ctrl Pts',(28.9240001297542,64.6080152631039,12.));
#104676=CARTESIAN_POINT('Ctrl Pts',(28.926616644195,64.629361138774,0.));
#104677=CARTESIAN_POINT('Ctrl Pts',(28.926616644195,64.629361138774,12.));
#104678=CARTESIAN_POINT('Ctrl Pts',(28.9292170069221,64.6507578895161,0.));
#104679=CARTESIAN_POINT('Ctrl Pts',(28.9292170069221,64.6507578895161,12.));
#104680=CARTESIAN_POINT('Ctrl Pts',(28.9318011239915,64.672205370541,0.));
#104681=CARTESIAN_POINT('Ctrl Pts',(28.9318011239915,64.672205370541,12.));
#104682=CARTESIAN_POINT('Ctrl Pts',(28.9343689019882,64.6937034376617,0.));
#104683=CARTESIAN_POINT('Ctrl Pts',(28.9343689019882,64.6937034376617,12.));
#104684=CARTESIAN_POINT('Ctrl Pts',(28.9369202480392,64.715251947329,0.));
#104685=CARTESIAN_POINT('Ctrl Pts',(28.9369202480392,64.715251947329,12.));
#104686=CARTESIAN_POINT('Ctrl Pts',(28.9394550698204,64.7368507566467,0.));
#104687=CARTESIAN_POINT('Ctrl Pts',(28.9394550698204,64.7368507566467,12.));
#104688=CARTESIAN_POINT('Ctrl Pts',(28.9419732755655,64.758499723388,0.));
#104689=CARTESIAN_POINT('Ctrl Pts',(28.9419732755655,64.758499723388,12.));
#104690=CARTESIAN_POINT('Ctrl Pts',(28.944474774081,64.7801987060084,0.));
#104691=CARTESIAN_POINT('Ctrl Pts',(28.944474774081,64.7801987060084,12.));
#104692=CARTESIAN_POINT('Ctrl Pts',(28.9469594747431,64.8019475636442,0.));
#104693=CARTESIAN_POINT('Ctrl Pts',(28.9469594747431,64.8019475636442,12.));
#104694=CARTESIAN_POINT('Ctrl Pts',(28.9494272874831,64.8237461561019,0.));
#104695=CARTESIAN_POINT('Ctrl Pts',(28.9494272874831,64.8237461561019,12.));
#104696=CARTESIAN_POINT('Ctrl Pts',(28.9518781227765,64.8455943438423,0.));
#104697=CARTESIAN_POINT('Ctrl Pts',(28.9518781227765,64.8455943438423,12.));
#104698=CARTESIAN_POINT('Ctrl Pts',(28.9543118916328,64.8674919879648,0.));
#104699=CARTESIAN_POINT('Ctrl Pts',(28.9543118916328,64.8674919879648,12.));
#104700=CARTESIAN_POINT('Ctrl Pts',(28.9567285055866,64.8894389501801,0.));
#104701=CARTESIAN_POINT('Ctrl Pts',(28.9567285055866,64.8894389501801,12.));
#104702=CARTESIAN_POINT('Ctrl Pts',(28.9591278766934,64.9114350928125,0.));
#104703=CARTESIAN_POINT('Ctrl Pts',(28.9591278766934,64.9114350928125,12.));
#104704=CARTESIAN_POINT('Ctrl Pts',(28.9615099175249,64.9334802788038,0.));
#104705=CARTESIAN_POINT('Ctrl Pts',(28.9615099175249,64.9334802788038,12.));
#104706=CARTESIAN_POINT('Ctrl Pts',(28.9638745411677,64.955574371711,0.));
#104707=CARTESIAN_POINT('Ctrl Pts',(28.9638745411677,64.955574371711,12.));
#104708=CARTESIAN_POINT('Ctrl Pts',(28.9662216612217,64.9777172357027,0.));
#104709=CARTESIAN_POINT('Ctrl Pts',(28.9662216612217,64.9777172357027,12.));
#104710=CARTESIAN_POINT('Ctrl Pts',(28.9685511918018,64.9999087355504,0.));
#104711=CARTESIAN_POINT('Ctrl Pts',(28.9685511918018,64.9999087355504,12.));
#104712=CARTESIAN_POINT('Ctrl Pts',(28.97086304753,65.022148736628,0.));
#104713=CARTESIAN_POINT('Ctrl Pts',(28.97086304753,65.022148736628,12.));
#104714=CARTESIAN_POINT('Ctrl Pts',(28.9731571435282,65.0444371049082,0.));
#104715=CARTESIAN_POINT('Ctrl Pts',(28.9731571435282,65.0444371049082,12.));
#104716=CARTESIAN_POINT('Ctrl Pts',(28.9754333954135,65.0667737069563,0.));
#104717=CARTESIAN_POINT('Ctrl Pts',(28.9754333954135,65.0667737069563,12.));
#104718=CARTESIAN_POINT('Ctrl Pts',(28.9776917192933,65.0891584099168,0.));
#104719=CARTESIAN_POINT('Ctrl Pts',(28.9776917192933,65.0891584099168,12.));
#104720=CARTESIAN_POINT('Ctrl Pts',(28.9799320317641,65.1115910815037,0.));
#104721=CARTESIAN_POINT('Ctrl Pts',(28.9799320317641,65.1115910815037,12.));
#104722=CARTESIAN_POINT('Ctrl Pts',(28.9821542499042,65.1340715900028,0.));
#104723=CARTESIAN_POINT('Ctrl Pts',(28.9821542499042,65.1340715900028,12.));
#104724=CARTESIAN_POINT('Ctrl Pts',(28.9843582912692,65.1565998042697,0.));
#104725=CARTESIAN_POINT('Ctrl Pts',(28.9843582912692,65.1565998042697,12.));
#104726=CARTESIAN_POINT('Ctrl Pts',(28.9865440738883,65.1791755937256,0.));
#104727=CARTESIAN_POINT('Ctrl Pts',(28.9865440738883,65.1791755937256,12.));
#104728=CARTESIAN_POINT('Ctrl Pts',(28.9887115162633,65.2017988283479,0.));
#104729=CARTESIAN_POINT('Ctrl Pts',(28.9887115162633,65.2017988283479,12.));
#104730=CARTESIAN_POINT('Ctrl Pts',(28.9908605373663,65.2244693786609,0.));
#104731=CARTESIAN_POINT('Ctrl Pts',(28.9908605373663,65.2244693786609,12.));
#104732=CARTESIAN_POINT('Ctrl Pts',(28.9929910566325,65.2471871157397,0.));
#104733=CARTESIAN_POINT('Ctrl Pts',(28.9929910566325,65.2471871157397,12.));
#104734=CARTESIAN_POINT('Ctrl Pts',(28.9951029939557,65.2699519112064,0.));
#104735=CARTESIAN_POINT('Ctrl Pts',(28.9951029939557,65.2699519112064,12.));
#104736=CARTESIAN_POINT('Ctrl Pts',(28.9971962696845,65.2927636372254,0.));
#104737=CARTESIAN_POINT('Ctrl Pts',(28.9971962696845,65.2927636372254,12.));
#104738=CARTESIAN_POINT('Ctrl Pts',(28.9992708046211,65.3156221664916,0.));
#104739=CARTESIAN_POINT('Ctrl Pts',(28.9992708046211,65.3156221664916,12.));
#104740=CARTESIAN_POINT('Ctrl Pts',(29.0013265200185,65.3385273722241,0.));
#104741=CARTESIAN_POINT('Ctrl Pts',(29.0013265200185,65.3385273722241,12.));
#104742=CARTESIAN_POINT('Ctrl Pts',(29.003363337573,65.3614791281692,0.));
#104743=CARTESIAN_POINT('Ctrl Pts',(29.003363337573,65.3614791281692,12.));
#104744=CARTESIAN_POINT('Ctrl Pts',(29.0053811794207,65.3844773085961,0.));
#104745=CARTESIAN_POINT('Ctrl Pts',(29.0053811794207,65.3844773085961,12.));
#104746=CARTESIAN_POINT('Ctrl Pts',(29.0073799681342,65.4075217882934,0.));
#104747=CARTESIAN_POINT('Ctrl Pts',(29.0073799681342,65.4075217882934,12.));
#104748=CARTESIAN_POINT('Ctrl Pts',(29.0093596267215,65.4306124425562,0.));
#104749=CARTESIAN_POINT('Ctrl Pts',(29.0093596267215,65.4306124425562,12.));
#104750=CARTESIAN_POINT('Ctrl Pts',(29.0113200786239,65.4537491471828,0.));
#104751=CARTESIAN_POINT('Ctrl Pts',(29.0113200786239,65.4537491471828,12.));
#104752=CARTESIAN_POINT('Ctrl Pts',(29.013261247709,65.4769317784789,0.));
#104753=CARTESIAN_POINT('Ctrl Pts',(29.013261247709,65.4769317784789,12.));
#104754=CARTESIAN_POINT('Ctrl Pts',(29.0151830582675,65.5001602132535,0.));
#104755=CARTESIAN_POINT('Ctrl Pts',(29.0151830582675,65.5001602132535,12.));
#104756=CARTESIAN_POINT('Ctrl Pts',(29.0170854350095,65.5234343288136,0.));
#104757=CARTESIAN_POINT('Ctrl Pts',(29.0170854350095,65.5234343288136,12.));
#104758=CARTESIAN_POINT('Ctrl Pts',(29.0189683030642,65.5467540029514,0.));
#104759=CARTESIAN_POINT('Ctrl Pts',(29.0189683030642,65.5467540029514,12.));
#104760=CARTESIAN_POINT('Ctrl Pts',(29.0208315879764,65.5701191139418,0.));
#104761=CARTESIAN_POINT('Ctrl Pts',(29.0208315879764,65.5701191139418,12.));
#104762=CARTESIAN_POINT('Ctrl Pts',(29.0226752157003,65.5935295405453,0.));
#104763=CARTESIAN_POINT('Ctrl Pts',(29.0226752157003,65.5935295405453,12.));
#104764=CARTESIAN_POINT('Ctrl Pts',(29.0244991125958,65.6169851620046,0.));
#104765=CARTESIAN_POINT('Ctrl Pts',(29.0244991125958,65.6169851620046,12.));
#104766=CARTESIAN_POINT('Ctrl Pts',(29.0263032054266,65.6404858580403,0.));
#104767=CARTESIAN_POINT('Ctrl Pts',(29.0263032054266,65.6404858580403,12.));
#104768=CARTESIAN_POINT('Ctrl Pts',(29.0280874213596,65.6640315088388,0.));
#104769=CARTESIAN_POINT('Ctrl Pts',(29.0280874213596,65.6640315088388,12.));
#104770=CARTESIAN_POINT('Ctrl Pts',(29.0298516879611,65.6876219950493,0.));
#104771=CARTESIAN_POINT('Ctrl Pts',(29.0298516879611,65.6876219950493,12.));
#104772=CARTESIAN_POINT('Ctrl Pts',(29.0315959331919,65.7112571977891,0.));
#104773=CARTESIAN_POINT('Ctrl Pts',(29.0315959331919,65.7112571977891,12.));
#104774=CARTESIAN_POINT('Ctrl Pts',(29.0333200854027,65.7349369986384,0.));
#104775=CARTESIAN_POINT('Ctrl Pts',(29.0333200854027,65.7349369986384,12.));
#104776=CARTESIAN_POINT('Ctrl Pts',(29.035024073333,65.7586612796368,0.));
#104777=CARTESIAN_POINT('Ctrl Pts',(29.035024073333,65.7586612796368,12.));
#104778=CARTESIAN_POINT('Ctrl Pts',(29.0367078261102,65.7824299232705,0.));
#104779=CARTESIAN_POINT('Ctrl Pts',(29.0367078261102,65.7824299232705,12.));
#104780=CARTESIAN_POINT('Ctrl Pts',(29.0383712732469,65.8062428124713,0.));
#104781=CARTESIAN_POINT('Ctrl Pts',(29.0383712732469,65.8062428124713,12.));
#104782=CARTESIAN_POINT('Ctrl Pts',(29.0400143446338,65.8300998306191,0.));
#104783=CARTESIAN_POINT('Ctrl Pts',(29.0400143446338,65.8300998306191,12.));
#104784=CARTESIAN_POINT('Ctrl Pts',(29.0416369705375,65.854000861539,0.));
#104785=CARTESIAN_POINT('Ctrl Pts',(29.0416369705375,65.854000861539,12.));
#104786=CARTESIAN_POINT('Ctrl Pts',(29.0432390815977,65.8779457894961,0.));
#104787=CARTESIAN_POINT('Ctrl Pts',(29.0432390815977,65.8779457894961,12.));
#104788=CARTESIAN_POINT('Ctrl Pts',(29.0448206088288,65.9019344991854,0.));
#104789=CARTESIAN_POINT('Ctrl Pts',(29.0448206088288,65.9019344991854,12.));
#104790=CARTESIAN_POINT('Ctrl Pts',(29.0463814836157,65.9259668757307,0.));
#104791=CARTESIAN_POINT('Ctrl Pts',(29.0463814836157,65.9259668757307,12.));
#104792=CARTESIAN_POINT('Ctrl Pts',(29.0479216377081,65.9500428046868,0.));
#104793=CARTESIAN_POINT('Ctrl Pts',(29.0479216377081,65.9500428046868,12.));
#104794=CARTESIAN_POINT('Ctrl Pts',(29.0494410032172,65.974162172037,0.));
#104795=CARTESIAN_POINT('Ctrl Pts',(29.0494410032172,65.974162172037,12.));
#104796=CARTESIAN_POINT('Ctrl Pts',(29.0509395126142,65.9983248641879,0.));
#104797=CARTESIAN_POINT('Ctrl Pts',(29.0509395126142,65.9983248641879,12.));
#104798=CARTESIAN_POINT('Ctrl Pts',(29.0524170987307,66.0225307679591,0.));
#104799=CARTESIAN_POINT('Ctrl Pts',(29.0524170987307,66.0225307679591,12.));
#104800=CARTESIAN_POINT('Ctrl Pts',(29.0538736947552,66.0467797705815,0.));
#104801=CARTESIAN_POINT('Ctrl Pts',(29.0538736947552,66.0467797705815,12.));
#104802=CARTESIAN_POINT('Ctrl Pts',(29.0553092342278,66.0710717597009,0.));
#104803=CARTESIAN_POINT('Ctrl Pts',(29.0553092342278,66.0710717597009,12.));
#104804=CARTESIAN_POINT('Ctrl Pts',(29.0567236510373,66.0954066233754,0.));
#104805=CARTESIAN_POINT('Ctrl Pts',(29.0567236510373,66.0954066233754,12.));
#104806=CARTESIAN_POINT('Ctrl Pts',(29.0581168794189,66.1197842500711,0.));
#104807=CARTESIAN_POINT('Ctrl Pts',(29.0581168794189,66.1197842500711,12.));
#104808=CARTESIAN_POINT('Ctrl Pts',(29.0594888539555,66.1442045286516,0.));
#104809=CARTESIAN_POINT('Ctrl Pts',(29.0594888539555,66.1442045286516,12.));
#104810=CARTESIAN_POINT('Ctrl Pts',(29.0608395095745,66.1686673483755,0.));
#104811=CARTESIAN_POINT('Ctrl Pts',(29.0608395095745,66.1686673483755,12.));
#104812=CARTESIAN_POINT('Ctrl Pts',(29.062168781542,66.1931725989008,0.));
#104813=CARTESIAN_POINT('Ctrl Pts',(29.062168781542,66.1931725989008,12.));
#104814=CARTESIAN_POINT('Ctrl Pts',(29.0634766054599,66.2177201702819,0.));
#104815=CARTESIAN_POINT('Ctrl Pts',(29.0634766054599,66.2177201702819,12.));
#104816=CARTESIAN_POINT('Ctrl Pts',(29.0647629172645,66.2423099529668,0.));
#104817=CARTESIAN_POINT('Ctrl Pts',(29.0647629172645,66.2423099529668,12.));
#104818=CARTESIAN_POINT('Ctrl Pts',(29.0660276532272,66.2669418377866,0.));
#104819=CARTESIAN_POINT('Ctrl Pts',(29.0660276532272,66.2669418377866,12.));
#104820=CARTESIAN_POINT('Ctrl Pts',(29.0672707499527,66.2916157159528,0.));
#104821=CARTESIAN_POINT('Ctrl Pts',(29.0672707499527,66.2916157159528,12.));
#104822=CARTESIAN_POINT('Ctrl Pts',(29.0684921443718,66.3163314790607,0.));
#104823=CARTESIAN_POINT('Ctrl Pts',(29.0684921443718,66.3163314790607,12.));
#104824=CARTESIAN_POINT('Ctrl Pts',(29.0696917737397,66.3410890190879,0.));
#104825=CARTESIAN_POINT('Ctrl Pts',(29.0696917737397,66.3410890190879,12.));
#104826=CARTESIAN_POINT('Ctrl Pts',(29.0708695756335,66.3658882283906,0.));
#104827=CARTESIAN_POINT('Ctrl Pts',(29.0708695756335,66.3658882283906,12.));
#104828=CARTESIAN_POINT('Ctrl Pts',(29.0720254879535,66.3907289996942,0.));
#104829=CARTESIAN_POINT('Ctrl Pts',(29.0720254879535,66.3907289996942,12.));
#104830=CARTESIAN_POINT('Ctrl Pts',(29.0731594489218,66.4156112260904,0.));
#104831=CARTESIAN_POINT('Ctrl Pts',(29.0731594489218,66.4156112260904,12.));
#104832=CARTESIAN_POINT('Ctrl Pts',(29.0742713970762,66.4405348010404,0.));
#104833=CARTESIAN_POINT('Ctrl Pts',(29.0742713970762,66.4405348010404,12.));
#104834=CARTESIAN_POINT('Ctrl Pts',(29.0753612712669,66.4654996183739,0.));
#104835=CARTESIAN_POINT('Ctrl Pts',(29.0753612712669,66.4654996183739,12.));
#104836=CARTESIAN_POINT('Ctrl Pts',(29.0764290106553,66.4905055722864,0.));
#104837=CARTESIAN_POINT('Ctrl Pts',(29.0764290106553,66.4905055722864,12.));
#104838=CARTESIAN_POINT('Ctrl Pts',(29.0774745547146,66.5155525573308,0.));
#104839=CARTESIAN_POINT('Ctrl Pts',(29.0774745547146,66.5155525573308,12.));
#104840=CARTESIAN_POINT('Ctrl Pts',(29.0784978432294,66.5406404684116,0.));
#104841=CARTESIAN_POINT('Ctrl Pts',(29.0784978432294,66.5406404684116,12.));
#104842=CARTESIAN_POINT('Ctrl Pts',(29.0794988162892,66.5657692007894,0.));
#104843=CARTESIAN_POINT('Ctrl Pts',(29.0794988162892,66.5657692007894,12.));
#104844=CARTESIAN_POINT('Ctrl Pts',(29.0804774142852,66.5909386500796,0.));
#104845=CARTESIAN_POINT('Ctrl Pts',(29.0804774142852,66.5909386500796,12.));
#104846=CARTESIAN_POINT('Ctrl Pts',(29.0814335779085,66.6161487122504,0.));
#104847=CARTESIAN_POINT('Ctrl Pts',(29.0814335779085,66.6161487122504,12.));
#104848=CARTESIAN_POINT('Ctrl Pts',(29.0823672481508,66.6413992836148,0.));
#104849=CARTESIAN_POINT('Ctrl Pts',(29.0823672481508,66.6413992836148,12.));
#104850=CARTESIAN_POINT('Ctrl Pts',(29.0832783663048,66.6666902608246,0.));
#104851=CARTESIAN_POINT('Ctrl Pts',(29.0832783663048,66.6666902608246,12.));
#104852=CARTESIAN_POINT('Ctrl Pts',(29.0841668739585,66.6920215408744,0.));
#104853=CARTESIAN_POINT('Ctrl Pts',(29.0841668739585,66.6920215408744,12.));
#104854=CARTESIAN_POINT('Ctrl Pts',(29.0850327129913,66.7173930211015,0.));
#104855=CARTESIAN_POINT('Ctrl Pts',(29.0850327129913,66.7173930211015,12.));
#104856=CARTESIAN_POINT('Ctrl Pts',(29.0858758255729,66.7428045991841,0.));
#104857=CARTESIAN_POINT('Ctrl Pts',(29.0858758255729,66.7428045991841,12.));
#104858=CARTESIAN_POINT('Ctrl Pts',(29.0866961541629,66.7682561731349,0.));
#104859=CARTESIAN_POINT('Ctrl Pts',(29.0866961541629,66.7682561731349,12.));
#104860=CARTESIAN_POINT('Ctrl Pts',(29.0874936415137,66.7937476412941,0.));
#104861=CARTESIAN_POINT('Ctrl Pts',(29.0874936415137,66.7937476412941,12.));
#104862=CARTESIAN_POINT('Ctrl Pts',(29.0882682306636,66.8192789023323,0.));
#104863=CARTESIAN_POINT('Ctrl Pts',(29.0882682306636,66.8192789023323,12.));
#104864=CARTESIAN_POINT('Ctrl Pts',(29.0890198649327,66.8448498552508,0.));
#104865=CARTESIAN_POINT('Ctrl Pts',(29.0890198649327,66.8448498552508,12.));
#104866=CARTESIAN_POINT('Ctrl Pts',(29.0897484879207,66.8704603993794,0.));
#104867=CARTESIAN_POINT('Ctrl Pts',(29.0897484879207,66.8704603993794,12.));
#104868=CARTESIAN_POINT('Ctrl Pts',(29.0904540435063,66.8961104343703,0.));
#104869=CARTESIAN_POINT('Ctrl Pts',(29.0904540435063,66.8961104343703,12.));
#104870=CARTESIAN_POINT('Ctrl Pts',(29.0911364758484,66.9217998601881,0.));
#104871=CARTESIAN_POINT('Ctrl Pts',(29.0911364758484,66.9217998601881,12.));
#104872=CARTESIAN_POINT('Ctrl Pts',(29.0917957293824,66.9475285771133,0.));
#104873=CARTESIAN_POINT('Ctrl Pts',(29.0917957293824,66.9475285771133,12.));
#104874=CARTESIAN_POINT('Ctrl Pts',(29.092431748817,66.9732964857467,0.));
#104875=CARTESIAN_POINT('Ctrl Pts',(29.092431748817,66.9732964857467,12.));
#104876=CARTESIAN_POINT('Ctrl Pts',(29.0930444791328,66.9991034870084,0.));
#104877=CARTESIAN_POINT('Ctrl Pts',(29.0930444791328,66.9991034870084,12.));
#104878=CARTESIAN_POINT('Ctrl Pts',(29.0936338655828,67.0249494821361,0.));
#104879=CARTESIAN_POINT('Ctrl Pts',(29.0936338655828,67.0249494821361,12.));
#104880=CARTESIAN_POINT('Ctrl Pts',(29.0941998536957,67.0508343726771,0.));
#104881=CARTESIAN_POINT('Ctrl Pts',(29.0941998536957,67.0508343726771,12.));
#104882=CARTESIAN_POINT('Ctrl Pts',(29.0947423892725,67.0767580604872,0.));
#104883=CARTESIAN_POINT('Ctrl Pts',(29.0947423892725,67.0767580604872,12.));
#104884=CARTESIAN_POINT('Ctrl Pts',(29.0952614183777,67.1027204477304,0.));
#104885=CARTESIAN_POINT('Ctrl Pts',(29.0952614183777,67.1027204477304,12.));
#104886=CARTESIAN_POINT('Ctrl Pts',(29.0957568873357,67.1287214368743,0.));
#104887=CARTESIAN_POINT('Ctrl Pts',(29.0957568873357,67.1287214368743,12.));
#104888=CARTESIAN_POINT('Ctrl Pts',(29.0962287427274,67.1547609306845,0.));
#104889=CARTESIAN_POINT('Ctrl Pts',(29.0962287427274,67.1547609306845,12.));
#104890=CARTESIAN_POINT('Ctrl Pts',(29.0966769313893,67.1808388322116,0.));
#104891=CARTESIAN_POINT('Ctrl Pts',(29.0966769313893,67.1808388322116,12.));
#104892=CARTESIAN_POINT('Ctrl Pts',(29.0971014004134,67.2069550447895,0.));
#104893=CARTESIAN_POINT('Ctrl Pts',(29.0971014004134,67.2069550447895,12.));
#104894=CARTESIAN_POINT('Ctrl Pts',(29.0975020971473,67.2331094720482,0.));
#104895=CARTESIAN_POINT('Ctrl Pts',(29.0975020971473,67.2331094720482,12.));
#104896=CARTESIAN_POINT('Ctrl Pts',(29.0978789691964,67.2593020179216,0.));
#104897=CARTESIAN_POINT('Ctrl Pts',(29.0978789691964,67.2593020179216,12.));
#104898=CARTESIAN_POINT('Ctrl Pts',(29.0982319644276,67.2855325866516,0.));
#104899=CARTESIAN_POINT('Ctrl Pts',(29.0982319644276,67.2855325866516,12.));
#104900=CARTESIAN_POINT('Ctrl Pts',(29.0985610309768,67.311801082791,0.));
#104901=CARTESIAN_POINT('Ctrl Pts',(29.0985610309768,67.311801082791,12.));
#104902=CARTESIAN_POINT('Ctrl Pts',(29.0988661172526,67.3381074112013,0.));
#104903=CARTESIAN_POINT('Ctrl Pts',(29.0988661172526,67.3381074112013,12.));
#104904=CARTESIAN_POINT('Ctrl Pts',(29.0991471719172,67.3644514770373,0.));
#104905=CARTESIAN_POINT('Ctrl Pts',(29.0991471719172,67.3644514770373,12.));
#104906=CARTESIAN_POINT('Ctrl Pts',(29.0994041438715,67.3908331857313,0.));
#104907=CARTESIAN_POINT('Ctrl Pts',(29.0994041438715,67.3908331857313,12.));
#104908=CARTESIAN_POINT('Ctrl Pts',(29.0996369822418,67.4172524429726,0.));
#104909=CARTESIAN_POINT('Ctrl Pts',(29.0996369822418,67.4172524429726,12.));
#104910=CARTESIAN_POINT('Ctrl Pts',(29.0998456363687,67.4437091546869,0.));
#104911=CARTESIAN_POINT('Ctrl Pts',(29.0998456363687,67.4437091546869,12.));
#104912=CARTESIAN_POINT('Ctrl Pts',(29.1000300557961,67.4702032270063,0.));
#104913=CARTESIAN_POINT('Ctrl Pts',(29.1000300557961,67.4702032270063,12.));
#104914=CARTESIAN_POINT('Ctrl Pts',(29.1001901902914,67.496734566311,0.));
#104915=CARTESIAN_POINT('Ctrl Pts',(29.1001901902914,67.496734566311,12.));
#104916=CARTESIAN_POINT('Ctrl Pts',(29.1003259898686,67.5233030792714,0.));
#104917=CARTESIAN_POINT('Ctrl Pts',(29.1003259898686,67.5233030792714,12.));
#104918=CARTESIAN_POINT('Ctrl Pts',(29.1004374048149,67.5499086728891,0.));
#104919=CARTESIAN_POINT('Ctrl Pts',(29.1004374048149,67.5499086728891,12.));
#104920=CARTESIAN_POINT('Ctrl Pts',(29.1005243857137,67.5765512545276,0.));
#104921=CARTESIAN_POINT('Ctrl Pts',(29.1005243857137,67.5765512545276,12.));
#104922=CARTESIAN_POINT('Ctrl Pts',(29.1005868834863,67.6032307319614,0.));
#104923=CARTESIAN_POINT('Ctrl Pts',(29.1005868834863,67.6032307319614,12.));
#104924=CARTESIAN_POINT('Ctrl Pts',(29.1006248493576,67.6299470133286,0.));
#104925=CARTESIAN_POINT('Ctrl Pts',(29.1006248493576,67.6299470133286,12.));
#104926=CARTESIAN_POINT('Ctrl Pts',(29.1006382347811,67.6567000070319,0.));
#104927=CARTESIAN_POINT('Ctrl Pts',(29.1006382347811,67.6567000070319,12.));
#104928=CARTESIAN_POINT('Ctrl Pts',(29.1006269913746,67.6834896216458,0.));
#104929=CARTESIAN_POINT('Ctrl Pts',(29.1006269913746,67.6834896216458,12.));
#104930=CARTESIAN_POINT('Ctrl Pts',(29.1005910708624,67.7103157658297,0.));
#104931=CARTESIAN_POINT('Ctrl Pts',(29.1005910708624,67.7103157658297,12.));
#104932=CARTESIAN_POINT('Ctrl Pts',(29.1005304249988,67.7371783482039,0.));
#104933=CARTESIAN_POINT('Ctrl Pts',(29.1005304249988,67.7371783482039,12.));
#104934=CARTESIAN_POINT('Ctrl Pts',(29.1004450055647,67.7640772773397,0.));
#104935=CARTESIAN_POINT('Ctrl Pts',(29.1004450055647,67.7640772773397,12.));
#104936=CARTESIAN_POINT('Ctrl Pts',(29.1003347645299,67.7910124620148,0.));
#104937=CARTESIAN_POINT('Ctrl Pts',(29.1003347645299,67.7910124620148,12.));
#104938=CARTESIAN_POINT('Ctrl Pts',(29.1001996541846,67.8179838114109,0.));
#104939=CARTESIAN_POINT('Ctrl Pts',(29.1001996541846,67.8179838114109,12.));
#104940=CARTESIAN_POINT('Ctrl Pts',(29.1000396272868,67.844991235333,0.));
#104941=CARTESIAN_POINT('Ctrl Pts',(29.1000396272868,67.844991235333,12.));
#104942=CARTESIAN_POINT('Ctrl Pts',(29.0998546372027,67.8720346444111,0.));
#104943=CARTESIAN_POINT('Ctrl Pts',(29.0998546372027,67.8720346444111,12.));
#104944=CARTESIAN_POINT('Ctrl Pts',(29.0996446380617,67.8991139503168,0.));
#104945=CARTESIAN_POINT('Ctrl Pts',(29.0996446380617,67.8991139503168,12.));
#104946=CARTESIAN_POINT('Ctrl Pts',(29.0994095844208,67.9262290652797,0.));
#104947=CARTESIAN_POINT('Ctrl Pts',(29.0994095844208,67.9262290652797,12.));
#104948=CARTESIAN_POINT('Ctrl Pts',(29.0991494309394,67.9533799016122,0.));
#104949=CARTESIAN_POINT('Ctrl Pts',(29.0991494309394,67.9533799016122,12.));
#104950=CARTESIAN_POINT('Ctrl Pts',(29.0988641320243,67.9805663711845,0.));
#104951=CARTESIAN_POINT('Ctrl Pts',(29.0988641320243,67.9805663711845,12.));
#104952=CARTESIAN_POINT('Ctrl Pts',(29.0985536415537,68.0077883850136,0.));
#104953=CARTESIAN_POINT('Ctrl Pts',(29.0985536415537,68.0077883850136,12.));
#104954=CARTESIAN_POINT('Ctrl Pts',(29.0982179124112,68.0350458525589,0.));
#104955=CARTESIAN_POINT('Ctrl Pts',(29.0982179124112,68.0350458525589,12.));
#104956=CARTESIAN_POINT('Ctrl Pts',(29.0978568968677,68.0623386822917,0.));
#104957=CARTESIAN_POINT('Ctrl Pts',(29.0978568968677,68.0623386822917,12.));
#104958=CARTESIAN_POINT('Ctrl Pts',(29.0974705474279,68.089666782962,0.));
#104959=CARTESIAN_POINT('Ctrl Pts',(29.0974705474279,68.089666782962,12.));
#104960=CARTESIAN_POINT('Ctrl Pts',(29.097058817574,68.1170300647019,0.));
#104961=CARTESIAN_POINT('Ctrl Pts',(29.097058817574,68.1170300647019,12.));
#104962=CARTESIAN_POINT('Ctrl Pts',(29.096621662474,68.1444284400734,0.));
#104963=CARTESIAN_POINT('Ctrl Pts',(29.096621662474,68.1444284400734,12.));
#104964=CARTESIAN_POINT('Ctrl Pts',(29.0961590399023,68.1718618254221,0.));
#104965=CARTESIAN_POINT('Ctrl Pts',(29.0961590399023,68.1718618254221,12.));
#104966=CARTESIAN_POINT('Ctrl Pts',(29.0956709104588,68.1993301411959,0.));
#104967=CARTESIAN_POINT('Ctrl Pts',(29.0956709104588,68.1993301411959,12.));
#104968=CARTESIAN_POINT('Ctrl Pts',(29.0951572355352,68.22683330895,0.));
#104969=CARTESIAN_POINT('Ctrl Pts',(29.0951572355352,68.22683330895,12.));
#104970=CARTESIAN_POINT('Ctrl Pts',(29.0946179757132,68.2543712489815,0.));
#104971=CARTESIAN_POINT('Ctrl Pts',(29.0946179757132,68.2543712489815,12.));
#104972=CARTESIAN_POINT('Ctrl Pts',(29.0940530889141,68.2819438775932,0.));
#104973=CARTESIAN_POINT('Ctrl Pts',(29.0940530889141,68.2819438775932,12.));
#104974=CARTESIAN_POINT('Ctrl Pts',(29.0934625288442,68.3095511047852,0.));
#104975=CARTESIAN_POINT('Ctrl Pts',(29.0934625288442,68.3095511047852,12.));
#104976=CARTESIAN_POINT('Ctrl Pts',(29.0928462428218,68.3371928310351,0.));
#104977=CARTESIAN_POINT('Ctrl Pts',(29.0928462428218,68.3371928310351,12.));
#104978=CARTESIAN_POINT('Ctrl Pts',(29.0922041749393,68.3648689519188,0.));
#104979=CARTESIAN_POINT('Ctrl Pts',(29.0922041749393,68.3648689519188,12.));
#104980=CARTESIAN_POINT('Ctrl Pts',(29.0915362699549,68.3925793638241,0.));
#104981=CARTESIAN_POINT('Ctrl Pts',(29.0915362699549,68.3925793638241,12.));
#104982=CARTESIAN_POINT('Ctrl Pts',(29.0908424770941,68.4203239694742,0.));
#104983=CARTESIAN_POINT('Ctrl Pts',(29.0908424770941,68.4203239694742,12.));
#104984=CARTESIAN_POINT('Ctrl Pts',(29.0901227535274,68.4481026830845,0.));
#104985=CARTESIAN_POINT('Ctrl Pts',(29.0901227535274,68.4481026830845,12.));
#104986=CARTESIAN_POINT('Ctrl Pts',(29.0893770688807,68.4759154367582,0.));
#104987=CARTESIAN_POINT('Ctrl Pts',(29.0893770688807,68.4759154367582,12.));
#104988=CARTESIAN_POINT('Ctrl Pts',(29.0886054060334,68.5037621823575,0.));
#104989=CARTESIAN_POINT('Ctrl Pts',(29.0886054060334,68.5037621823575,12.));
#104990=CARTESIAN_POINT('Ctrl Pts',(29.0878077570819,68.5316428874729,0.));
#104991=CARTESIAN_POINT('Ctrl Pts',(29.0878077570819,68.5316428874729,12.));
#104992=CARTESIAN_POINT('Ctrl Pts',(29.0871488478365,68.5539746037961,0.));
#104993=CARTESIAN_POINT('Ctrl Pts',(29.0871488478365,68.5539746037961,12.));
#104994=CARTESIAN_POINT('Ctrl Pts',(29.0866429721958,68.5707386600286,0.));
#104995=CARTESIAN_POINT('Ctrl Pts',(29.0866429721958,68.5707386600286,12.));
#104996=CARTESIAN_POINT('Ctrl Pts',(29.0863005247789,68.5819214834609,0.));
#104997=CARTESIAN_POINT('Ctrl Pts',(29.0863005247789,68.5819214834609,12.));
#104998=CARTESIAN_POINT('Ctrl Pts',(29.0861280018229,68.5875145916629,0.));
#104999=CARTESIAN_POINT('Ctrl Pts',(29.0861280018229,68.5875145916629,12.));
#105000=CARTESIAN_POINT('',(28.8072485549236,63.7976679095314,0.));
#105001=CARTESIAN_POINT('Ctrl Pts',(28.8072485549236,63.7976679095314,0.));
#105002=CARTESIAN_POINT('Ctrl Pts',(28.8078854475432,63.8014989507494,0.));
#105003=CARTESIAN_POINT('Ctrl Pts',(28.8091580239553,63.8091667271232,0.));
#105004=CARTESIAN_POINT('Ctrl Pts',(28.8110632620957,63.8206854735028,0.));
#105005=CARTESIAN_POINT('Ctrl Pts',(28.8135963263368,63.8360779669856,0.));
#105006=CARTESIAN_POINT('Ctrl Pts',(28.8167505576681,63.8553755207487,0.));
#105007=CARTESIAN_POINT('Ctrl Pts',(28.8198926619857,63.8747299825313,0.));
#105008=CARTESIAN_POINT('Ctrl Pts',(28.823022586318,63.8941412856924,0.));
#105009=CARTESIAN_POINT('Ctrl Pts',(28.8261402423291,63.9136093063786,0.));
#105010=CARTESIAN_POINT('Ctrl Pts',(28.8292455077559,63.9331338646996,0.));
#105011=CARTESIAN_POINT('Ctrl Pts',(28.8323382413789,63.9527147494423,0.));
#105012=CARTESIAN_POINT('Ctrl Pts',(28.83541829466,63.9723517369614,0.));
#105013=CARTESIAN_POINT('Ctrl Pts',(28.8384855243242,63.9920446117582,0.));
#105014=CARTESIAN_POINT('Ctrl Pts',(28.8415398056428,64.0117931881298,0.));
#105015=CARTESIAN_POINT('Ctrl Pts',(28.844581028125,64.0315973031942,0.));
#105016=CARTESIAN_POINT('Ctrl Pts',(28.8476090892232,64.0514568066637,0.));
#105017=CARTESIAN_POINT('Ctrl Pts',(28.8506238891092,64.0713715523599,0.));
#105018=CARTESIAN_POINT('Ctrl Pts',(28.8536253241853,64.0913413876622,0.));
#105019=CARTESIAN_POINT('Ctrl Pts',(28.8566132838178,64.1113661481965,0.));
#105020=CARTESIAN_POINT('Ctrl Pts',(28.8595876537148,64.1314456633381,0.));
#105021=CARTESIAN_POINT('Ctrl Pts',(28.8625483180437,64.1515797596564,0.));
#105022=CARTESIAN_POINT('Ctrl Pts',(28.8654951618649,64.1717682648685,0.));
#105023=CARTESIAN_POINT('Ctrl Pts',(28.8684280739014,64.1920110123299,0.));
#105024=CARTESIAN_POINT('Ctrl Pts',(28.8713469464185,64.2123078408461,0.));
#105025=CARTESIAN_POINT('Ctrl Pts',(28.8742516738946,64.2326585925252,0.));
#105026=CARTESIAN_POINT('Ctrl Pts',(28.877142152106,64.2530631112929,0.));
#105027=CARTESIAN_POINT('Ctrl Pts',(28.8800182770064,64.2735212410711,0.));
#105028=CARTESIAN_POINT('Ctrl Pts',(28.882879943794,64.2940328242521,0.));
#105029=CARTESIAN_POINT('Ctrl Pts',(28.8857270473959,64.3145977025037,0.));
#105030=CARTESIAN_POINT('Ctrl Pts',(28.8885594828926,64.3352157174619,0.));
#105031=CARTESIAN_POINT('Ctrl Pts',(28.8913771459323,64.3558867114076,0.));
#105032=CARTESIAN_POINT('Ctrl Pts',(28.89417993323,64.3766105280688,0.));
#105033=CARTESIAN_POINT('Ctrl Pts',(28.8969677427504,64.397387012917,0.));
#105034=CARTESIAN_POINT('Ctrl Pts',(28.899740473434,64.4182160127379,0.));
#105035=CARTESIAN_POINT('Ctrl Pts',(28.9024980250307,64.4390973753634,0.));
#105036=CARTESIAN_POINT('Ctrl Pts',(28.9052402979062,64.4600309493583,0.));
#105037=CARTESIAN_POINT('Ctrl Pts',(28.9079671928264,64.4810165836592,0.));
#105038=CARTESIAN_POINT('Ctrl Pts',(28.910678610965,64.5020541275951,0.));
#105039=CARTESIAN_POINT('Ctrl Pts',(28.9133744539949,64.523143431047,0.));
#105040=CARTESIAN_POINT('Ctrl Pts',(28.9160546241538,64.5442843445559,0.));
#105041=CARTESIAN_POINT('Ctrl Pts',(28.9187190243224,64.5654767194472,0.));
#105042=CARTESIAN_POINT('Ctrl Pts',(28.9213675580985,64.5867204079426,0.));
#105043=CARTESIAN_POINT('Ctrl Pts',(28.9240001297542,64.6080152631039,0.));
#105044=CARTESIAN_POINT('Ctrl Pts',(28.926616644195,64.629361138774,0.));
#105045=CARTESIAN_POINT('Ctrl Pts',(28.9292170069221,64.6507578895161,0.));
#105046=CARTESIAN_POINT('Ctrl Pts',(28.9318011239915,64.672205370541,0.));
#105047=CARTESIAN_POINT('Ctrl Pts',(28.9343689019882,64.6937034376617,0.));
#105048=CARTESIAN_POINT('Ctrl Pts',(28.9369202480392,64.715251947329,0.));
#105049=CARTESIAN_POINT('Ctrl Pts',(28.9394550698204,64.7368507566467,0.));
#105050=CARTESIAN_POINT('Ctrl Pts',(28.9419732755655,64.758499723388,0.));
#105051=CARTESIAN_POINT('Ctrl Pts',(28.944474774081,64.7801987060084,0.));
#105052=CARTESIAN_POINT('Ctrl Pts',(28.9469594747431,64.8019475636442,0.));
#105053=CARTESIAN_POINT('Ctrl Pts',(28.9494272874831,64.8237461561019,0.));
#105054=CARTESIAN_POINT('Ctrl Pts',(28.9518781227765,64.8455943438423,0.));
#105055=CARTESIAN_POINT('Ctrl Pts',(28.9543118916328,64.8674919879648,0.));
#105056=CARTESIAN_POINT('Ctrl Pts',(28.9567285055866,64.8894389501801,0.));
#105057=CARTESIAN_POINT('Ctrl Pts',(28.9591278766934,64.9114350928125,0.));
#105058=CARTESIAN_POINT('Ctrl Pts',(28.9615099175249,64.9334802788038,0.));
#105059=CARTESIAN_POINT('Ctrl Pts',(28.9638745411677,64.955574371711,0.));
#105060=CARTESIAN_POINT('Ctrl Pts',(28.9662216612217,64.9777172357027,0.));
#105061=CARTESIAN_POINT('Ctrl Pts',(28.9685511918018,64.9999087355504,0.));
#105062=CARTESIAN_POINT('Ctrl Pts',(28.97086304753,65.022148736628,0.));
#105063=CARTESIAN_POINT('Ctrl Pts',(28.9731571435282,65.0444371049082,0.));
#105064=CARTESIAN_POINT('Ctrl Pts',(28.9754333954135,65.0667737069563,0.));
#105065=CARTESIAN_POINT('Ctrl Pts',(28.9776917192933,65.0891584099168,0.));
#105066=CARTESIAN_POINT('Ctrl Pts',(28.9799320317641,65.1115910815037,0.));
#105067=CARTESIAN_POINT('Ctrl Pts',(28.9821542499042,65.1340715900028,0.));
#105068=CARTESIAN_POINT('Ctrl Pts',(28.9843582912692,65.1565998042697,0.));
#105069=CARTESIAN_POINT('Ctrl Pts',(28.9865440738883,65.1791755937256,0.));
#105070=CARTESIAN_POINT('Ctrl Pts',(28.9887115162633,65.2017988283479,0.));
#105071=CARTESIAN_POINT('Ctrl Pts',(28.9908605373663,65.2244693786609,0.));
#105072=CARTESIAN_POINT('Ctrl Pts',(28.9929910566325,65.2471871157397,0.));
#105073=CARTESIAN_POINT('Ctrl Pts',(28.9951029939557,65.2699519112064,0.));
#105074=CARTESIAN_POINT('Ctrl Pts',(28.9971962696845,65.2927636372254,0.));
#105075=CARTESIAN_POINT('Ctrl Pts',(28.9992708046211,65.3156221664916,0.));
#105076=CARTESIAN_POINT('Ctrl Pts',(29.0013265200185,65.3385273722241,0.));
#105077=CARTESIAN_POINT('Ctrl Pts',(29.003363337573,65.3614791281692,0.));
#105078=CARTESIAN_POINT('Ctrl Pts',(29.0053811794207,65.3844773085961,0.));
#105079=CARTESIAN_POINT('Ctrl Pts',(29.0073799681342,65.4075217882934,0.));
#105080=CARTESIAN_POINT('Ctrl Pts',(29.0093596267215,65.4306124425562,0.));
#105081=CARTESIAN_POINT('Ctrl Pts',(29.0113200786239,65.4537491471828,0.));
#105082=CARTESIAN_POINT('Ctrl Pts',(29.013261247709,65.4769317784789,0.));
#105083=CARTESIAN_POINT('Ctrl Pts',(29.0151830582675,65.5001602132535,0.));
#105084=CARTESIAN_POINT('Ctrl Pts',(29.0170854350095,65.5234343288136,0.));
#105085=CARTESIAN_POINT('Ctrl Pts',(29.0189683030642,65.5467540029514,0.));
#105086=CARTESIAN_POINT('Ctrl Pts',(29.0208315879764,65.5701191139418,0.));
#105087=CARTESIAN_POINT('Ctrl Pts',(29.0226752157003,65.5935295405453,0.));
#105088=CARTESIAN_POINT('Ctrl Pts',(29.0244991125958,65.6169851620046,0.));
#105089=CARTESIAN_POINT('Ctrl Pts',(29.0263032054266,65.6404858580403,0.));
#105090=CARTESIAN_POINT('Ctrl Pts',(29.0280874213596,65.6640315088388,0.));
#105091=CARTESIAN_POINT('Ctrl Pts',(29.0298516879611,65.6876219950493,0.));
#105092=CARTESIAN_POINT('Ctrl Pts',(29.0315959331919,65.7112571977891,0.));
#105093=CARTESIAN_POINT('Ctrl Pts',(29.0333200854027,65.7349369986384,0.));
#105094=CARTESIAN_POINT('Ctrl Pts',(29.035024073333,65.7586612796368,0.));
#105095=CARTESIAN_POINT('Ctrl Pts',(29.0367078261102,65.7824299232705,0.));
#105096=CARTESIAN_POINT('Ctrl Pts',(29.0383712732469,65.8062428124713,0.));
#105097=CARTESIAN_POINT('Ctrl Pts',(29.0400143446338,65.8300998306191,0.));
#105098=CARTESIAN_POINT('Ctrl Pts',(29.0416369705375,65.854000861539,0.));
#105099=CARTESIAN_POINT('Ctrl Pts',(29.0432390815977,65.8779457894961,0.));
#105100=CARTESIAN_POINT('Ctrl Pts',(29.0448206088288,65.9019344991854,0.));
#105101=CARTESIAN_POINT('Ctrl Pts',(29.0463814836157,65.9259668757307,0.));
#105102=CARTESIAN_POINT('Ctrl Pts',(29.0479216377081,65.9500428046868,0.));
#105103=CARTESIAN_POINT('Ctrl Pts',(29.0494410032172,65.974162172037,0.));
#105104=CARTESIAN_POINT('Ctrl Pts',(29.0509395126142,65.9983248641879,0.));
#105105=CARTESIAN_POINT('Ctrl Pts',(29.0524170987307,66.0225307679591,0.));
#105106=CARTESIAN_POINT('Ctrl Pts',(29.0538736947552,66.0467797705815,0.));
#105107=CARTESIAN_POINT('Ctrl Pts',(29.0553092342278,66.0710717597009,0.));
#105108=CARTESIAN_POINT('Ctrl Pts',(29.0567236510373,66.0954066233754,0.));
#105109=CARTESIAN_POINT('Ctrl Pts',(29.0581168794189,66.1197842500711,0.));
#105110=CARTESIAN_POINT('Ctrl Pts',(29.0594888539555,66.1442045286516,0.));
#105111=CARTESIAN_POINT('Ctrl Pts',(29.0608395095745,66.1686673483755,0.));
#105112=CARTESIAN_POINT('Ctrl Pts',(29.062168781542,66.1931725989008,0.));
#105113=CARTESIAN_POINT('Ctrl Pts',(29.0634766054599,66.2177201702819,0.));
#105114=CARTESIAN_POINT('Ctrl Pts',(29.0647629172645,66.2423099529668,0.));
#105115=CARTESIAN_POINT('Ctrl Pts',(29.0660276532272,66.2669418377866,0.));
#105116=CARTESIAN_POINT('Ctrl Pts',(29.0672707499527,66.2916157159528,0.));
#105117=CARTESIAN_POINT('Ctrl Pts',(29.0684921443718,66.3163314790607,0.));
#105118=CARTESIAN_POINT('Ctrl Pts',(29.0696917737397,66.3410890190879,0.));
#105119=CARTESIAN_POINT('Ctrl Pts',(29.0708695756335,66.3658882283906,0.));
#105120=CARTESIAN_POINT('Ctrl Pts',(29.0720254879535,66.3907289996942,0.));
#105121=CARTESIAN_POINT('Ctrl Pts',(29.0731594489218,66.4156112260904,0.));
#105122=CARTESIAN_POINT('Ctrl Pts',(29.0742713970762,66.4405348010404,0.));
#105123=CARTESIAN_POINT('Ctrl Pts',(29.0753612712669,66.4654996183739,0.));
#105124=CARTESIAN_POINT('Ctrl Pts',(29.0764290106553,66.4905055722864,0.));
#105125=CARTESIAN_POINT('Ctrl Pts',(29.0774745547146,66.5155525573308,0.));
#105126=CARTESIAN_POINT('Ctrl Pts',(29.0784978432294,66.5406404684116,0.));
#105127=CARTESIAN_POINT('Ctrl Pts',(29.0794988162892,66.5657692007894,0.));
#105128=CARTESIAN_POINT('Ctrl Pts',(29.0804774142852,66.5909386500796,0.));
#105129=CARTESIAN_POINT('Ctrl Pts',(29.0814335779085,66.6161487122504,0.));
#105130=CARTESIAN_POINT('Ctrl Pts',(29.0823672481508,66.6413992836148,0.));
#105131=CARTESIAN_POINT('Ctrl Pts',(29.0832783663048,66.6666902608246,0.));
#105132=CARTESIAN_POINT('Ctrl Pts',(29.0841668739585,66.6920215408744,0.));
#105133=CARTESIAN_POINT('Ctrl Pts',(29.0850327129913,66.7173930211015,0.));
#105134=CARTESIAN_POINT('Ctrl Pts',(29.0858758255729,66.7428045991841,0.));
#105135=CARTESIAN_POINT('Ctrl Pts',(29.0866961541629,66.7682561731349,0.));
#105136=CARTESIAN_POINT('Ctrl Pts',(29.0874936415137,66.7937476412941,0.));
#105137=CARTESIAN_POINT('Ctrl Pts',(29.0882682306636,66.8192789023323,0.));
#105138=CARTESIAN_POINT('Ctrl Pts',(29.0890198649327,66.8448498552508,0.));
#105139=CARTESIAN_POINT('Ctrl Pts',(29.0897484879207,66.8704603993794,0.));
#105140=CARTESIAN_POINT('Ctrl Pts',(29.0904540435063,66.8961104343703,0.));
#105141=CARTESIAN_POINT('Ctrl Pts',(29.0911364758484,66.9217998601881,0.));
#105142=CARTESIAN_POINT('Ctrl Pts',(29.0917957293824,66.9475285771133,0.));
#105143=CARTESIAN_POINT('Ctrl Pts',(29.092431748817,66.9732964857467,0.));
#105144=CARTESIAN_POINT('Ctrl Pts',(29.0930444791328,66.9991034870084,0.));
#105145=CARTESIAN_POINT('Ctrl Pts',(29.0936338655828,67.0249494821361,0.));
#105146=CARTESIAN_POINT('Ctrl Pts',(29.0941998536957,67.0508343726771,0.));
#105147=CARTESIAN_POINT('Ctrl Pts',(29.0947423892725,67.0767580604872,0.));
#105148=CARTESIAN_POINT('Ctrl Pts',(29.0952614183777,67.1027204477304,0.));
#105149=CARTESIAN_POINT('Ctrl Pts',(29.0957568873357,67.1287214368743,0.));
#105150=CARTESIAN_POINT('Ctrl Pts',(29.0962287427274,67.1547609306845,0.));
#105151=CARTESIAN_POINT('Ctrl Pts',(29.0966769313893,67.1808388322116,0.));
#105152=CARTESIAN_POINT('Ctrl Pts',(29.0971014004134,67.2069550447895,0.));
#105153=CARTESIAN_POINT('Ctrl Pts',(29.0975020971473,67.2331094720482,0.));
#105154=CARTESIAN_POINT('Ctrl Pts',(29.0978789691964,67.2593020179216,0.));
#105155=CARTESIAN_POINT('Ctrl Pts',(29.0982319644276,67.2855325866516,0.));
#105156=CARTESIAN_POINT('Ctrl Pts',(29.0985610309768,67.311801082791,0.));
#105157=CARTESIAN_POINT('Ctrl Pts',(29.0988661172526,67.3381074112013,0.));
#105158=CARTESIAN_POINT('Ctrl Pts',(29.0991471719172,67.3644514770373,0.));
#105159=CARTESIAN_POINT('Ctrl Pts',(29.0994041438715,67.3908331857313,0.));
#105160=CARTESIAN_POINT('Ctrl Pts',(29.0996369822418,67.4172524429726,0.));
#105161=CARTESIAN_POINT('Ctrl Pts',(29.0998456363687,67.4437091546869,0.));
#105162=CARTESIAN_POINT('Ctrl Pts',(29.1000300557961,67.4702032270063,0.));
#105163=CARTESIAN_POINT('Ctrl Pts',(29.1001901902914,67.496734566311,0.));
#105164=CARTESIAN_POINT('Ctrl Pts',(29.1003259898686,67.5233030792714,0.));
#105165=CARTESIAN_POINT('Ctrl Pts',(29.1004374048149,67.5499086728891,0.));
#105166=CARTESIAN_POINT('Ctrl Pts',(29.1005243857137,67.5765512545276,0.));
#105167=CARTESIAN_POINT('Ctrl Pts',(29.1005868834863,67.6032307319614,0.));
#105168=CARTESIAN_POINT('Ctrl Pts',(29.1006248493576,67.6299470133286,0.));
#105169=CARTESIAN_POINT('Ctrl Pts',(29.1006382347811,67.6567000070319,0.));
#105170=CARTESIAN_POINT('Ctrl Pts',(29.1006269913746,67.6834896216458,0.));
#105171=CARTESIAN_POINT('Ctrl Pts',(29.1005910708624,67.7103157658297,0.));
#105172=CARTESIAN_POINT('Ctrl Pts',(29.1005304249988,67.7371783482039,0.));
#105173=CARTESIAN_POINT('Ctrl Pts',(29.1004450055647,67.7640772773397,0.));
#105174=CARTESIAN_POINT('Ctrl Pts',(29.1003347645299,67.7910124620148,0.));
#105175=CARTESIAN_POINT('Ctrl Pts',(29.1001996541846,67.8179838114109,0.));
#105176=CARTESIAN_POINT('Ctrl Pts',(29.1000396272868,67.844991235333,0.));
#105177=CARTESIAN_POINT('Ctrl Pts',(29.0998546372027,67.8720346444111,0.));
#105178=CARTESIAN_POINT('Ctrl Pts',(29.0996446380617,67.8991139503168,0.));
#105179=CARTESIAN_POINT('Ctrl Pts',(29.0994095844208,67.9262290652797,0.));
#105180=CARTESIAN_POINT('Ctrl Pts',(29.0991494309394,67.9533799016122,0.));
#105181=CARTESIAN_POINT('Ctrl Pts',(29.0988641320243,67.9805663711845,0.));
#105182=CARTESIAN_POINT('Ctrl Pts',(29.0985536415537,68.0077883850136,0.));
#105183=CARTESIAN_POINT('Ctrl Pts',(29.0982179124112,68.0350458525589,0.));
#105184=CARTESIAN_POINT('Ctrl Pts',(29.0978568968677,68.0623386822917,0.));
#105185=CARTESIAN_POINT('Ctrl Pts',(29.0974705474279,68.089666782962,0.));
#105186=CARTESIAN_POINT('Ctrl Pts',(29.097058817574,68.1170300647019,0.));
#105187=CARTESIAN_POINT('Ctrl Pts',(29.096621662474,68.1444284400734,0.));
#105188=CARTESIAN_POINT('Ctrl Pts',(29.0961590399023,68.1718618254221,0.));
#105189=CARTESIAN_POINT('Ctrl Pts',(29.0956709104588,68.1993301411959,0.));
#105190=CARTESIAN_POINT('Ctrl Pts',(29.0952305915108,68.2229056854495,0.));
#105191=CARTESIAN_POINT('Ctrl Pts',(29.0948791947834,68.2409993689947,0.));
#105192=CARTESIAN_POINT('Ctrl Pts',(29.094628043331,68.2535957746884,0.));
#105193=CARTESIAN_POINT('Ctrl Pts',(29.0944846386548,68.2606847334625,0.));
#105194=CARTESIAN_POINT('Ctrl Pts',(29.0944526440248,68.2622612909745,0.));
#105195=CARTESIAN_POINT('',(28.8072485549236,63.7976679095314,12.));
#105196=CARTESIAN_POINT('',(28.8072485549236,63.7976679095314,0.));
#105197=CARTESIAN_POINT('Ctrl Pts',(29.0944526440248,68.2622612909745,12.));
#105198=CARTESIAN_POINT('Ctrl Pts',(29.0944846386548,68.2606847334625,12.));
#105199=CARTESIAN_POINT('Ctrl Pts',(29.094628043331,68.2535957746884,12.));
#105200=CARTESIAN_POINT('Ctrl Pts',(29.0948791947834,68.2409993689947,12.));
#105201=CARTESIAN_POINT('Ctrl Pts',(29.0952305915108,68.2229056854495,12.));
#105202=CARTESIAN_POINT('Ctrl Pts',(29.0956709104588,68.1993301411959,12.));
#105203=CARTESIAN_POINT('Ctrl Pts',(29.0961590399023,68.1718618254221,12.));
#105204=CARTESIAN_POINT('Ctrl Pts',(29.096621662474,68.1444284400734,12.));
#105205=CARTESIAN_POINT('Ctrl Pts',(29.097058817574,68.1170300647019,12.));
#105206=CARTESIAN_POINT('Ctrl Pts',(29.0974705474279,68.089666782962,12.));
#105207=CARTESIAN_POINT('Ctrl Pts',(29.0978568968677,68.0623386822917,12.));
#105208=CARTESIAN_POINT('Ctrl Pts',(29.0982179124112,68.0350458525589,12.));
#105209=CARTESIAN_POINT('Ctrl Pts',(29.0985536415537,68.0077883850136,12.));
#105210=CARTESIAN_POINT('Ctrl Pts',(29.0988641320243,67.9805663711845,12.));
#105211=CARTESIAN_POINT('Ctrl Pts',(29.0991494309394,67.9533799016122,12.));
#105212=CARTESIAN_POINT('Ctrl Pts',(29.0994095844208,67.9262290652797,12.));
#105213=CARTESIAN_POINT('Ctrl Pts',(29.0996446380617,67.8991139503168,12.));
#105214=CARTESIAN_POINT('Ctrl Pts',(29.0998546372027,67.8720346444111,12.));
#105215=CARTESIAN_POINT('Ctrl Pts',(29.1000396272868,67.844991235333,12.));
#105216=CARTESIAN_POINT('Ctrl Pts',(29.1001996541846,67.8179838114109,12.));
#105217=CARTESIAN_POINT('Ctrl Pts',(29.1003347645299,67.7910124620148,12.));
#105218=CARTESIAN_POINT('Ctrl Pts',(29.1004450055647,67.7640772773397,12.));
#105219=CARTESIAN_POINT('Ctrl Pts',(29.1005304249988,67.7371783482039,12.));
#105220=CARTESIAN_POINT('Ctrl Pts',(29.1005910708624,67.7103157658297,12.));
#105221=CARTESIAN_POINT('Ctrl Pts',(29.1006269913746,67.6834896216458,12.));
#105222=CARTESIAN_POINT('Ctrl Pts',(29.1006382347811,67.6567000070319,12.));
#105223=CARTESIAN_POINT('Ctrl Pts',(29.1006248493576,67.6299470133286,12.));
#105224=CARTESIAN_POINT('Ctrl Pts',(29.1005868834863,67.6032307319614,12.));
#105225=CARTESIAN_POINT('Ctrl Pts',(29.1005243857137,67.5765512545276,12.));
#105226=CARTESIAN_POINT('Ctrl Pts',(29.1004374048149,67.5499086728891,12.));
#105227=CARTESIAN_POINT('Ctrl Pts',(29.1003259898686,67.5233030792714,12.));
#105228=CARTESIAN_POINT('Ctrl Pts',(29.1001901902914,67.496734566311,12.));
#105229=CARTESIAN_POINT('Ctrl Pts',(29.1000300557961,67.4702032270063,12.));
#105230=CARTESIAN_POINT('Ctrl Pts',(29.0998456363687,67.4437091546869,12.));
#105231=CARTESIAN_POINT('Ctrl Pts',(29.0996369822418,67.4172524429726,12.));
#105232=CARTESIAN_POINT('Ctrl Pts',(29.0994041438715,67.3908331857313,12.));
#105233=CARTESIAN_POINT('Ctrl Pts',(29.0991471719172,67.3644514770373,12.));
#105234=CARTESIAN_POINT('Ctrl Pts',(29.0988661172526,67.3381074112013,12.));
#105235=CARTESIAN_POINT('Ctrl Pts',(29.0985610309768,67.311801082791,12.));
#105236=CARTESIAN_POINT('Ctrl Pts',(29.0982319644276,67.2855325866516,12.));
#105237=CARTESIAN_POINT('Ctrl Pts',(29.0978789691964,67.2593020179216,12.));
#105238=CARTESIAN_POINT('Ctrl Pts',(29.0975020971473,67.2331094720482,12.));
#105239=CARTESIAN_POINT('Ctrl Pts',(29.0971014004134,67.2069550447895,12.));
#105240=CARTESIAN_POINT('Ctrl Pts',(29.0966769313893,67.1808388322116,12.));
#105241=CARTESIAN_POINT('Ctrl Pts',(29.0962287427274,67.1547609306845,12.));
#105242=CARTESIAN_POINT('Ctrl Pts',(29.0957568873357,67.1287214368743,12.));
#105243=CARTESIAN_POINT('Ctrl Pts',(29.0952614183777,67.1027204477304,12.));
#105244=CARTESIAN_POINT('Ctrl Pts',(29.0947423892725,67.0767580604872,12.));
#105245=CARTESIAN_POINT('Ctrl Pts',(29.0941998536957,67.0508343726771,12.));
#105246=CARTESIAN_POINT('Ctrl Pts',(29.0936338655828,67.0249494821361,12.));
#105247=CARTESIAN_POINT('Ctrl Pts',(29.0930444791328,66.9991034870084,12.));
#105248=CARTESIAN_POINT('Ctrl Pts',(29.092431748817,66.9732964857467,12.));
#105249=CARTESIAN_POINT('Ctrl Pts',(29.0917957293824,66.9475285771133,12.));
#105250=CARTESIAN_POINT('Ctrl Pts',(29.0911364758484,66.9217998601881,12.));
#105251=CARTESIAN_POINT('Ctrl Pts',(29.0904540435063,66.8961104343703,12.));
#105252=CARTESIAN_POINT('Ctrl Pts',(29.0897484879207,66.8704603993794,12.));
#105253=CARTESIAN_POINT('Ctrl Pts',(29.0890198649327,66.8448498552508,12.));
#105254=CARTESIAN_POINT('Ctrl Pts',(29.0882682306636,66.8192789023323,12.));
#105255=CARTESIAN_POINT('Ctrl Pts',(29.0874936415137,66.7937476412941,12.));
#105256=CARTESIAN_POINT('Ctrl Pts',(29.0866961541629,66.7682561731349,12.));
#105257=CARTESIAN_POINT('Ctrl Pts',(29.0858758255729,66.7428045991841,12.));
#105258=CARTESIAN_POINT('Ctrl Pts',(29.0850327129913,66.7173930211015,12.));
#105259=CARTESIAN_POINT('Ctrl Pts',(29.0841668739585,66.6920215408744,12.));
#105260=CARTESIAN_POINT('Ctrl Pts',(29.0832783663048,66.6666902608246,12.));
#105261=CARTESIAN_POINT('Ctrl Pts',(29.0823672481508,66.6413992836148,12.));
#105262=CARTESIAN_POINT('Ctrl Pts',(29.0814335779085,66.6161487122504,12.));
#105263=CARTESIAN_POINT('Ctrl Pts',(29.0804774142852,66.5909386500796,12.));
#105264=CARTESIAN_POINT('Ctrl Pts',(29.0794988162892,66.5657692007894,12.));
#105265=CARTESIAN_POINT('Ctrl Pts',(29.0784978432294,66.5406404684116,12.));
#105266=CARTESIAN_POINT('Ctrl Pts',(29.0774745547146,66.5155525573308,12.));
#105267=CARTESIAN_POINT('Ctrl Pts',(29.0764290106553,66.4905055722864,12.));
#105268=CARTESIAN_POINT('Ctrl Pts',(29.0753612712669,66.4654996183739,12.));
#105269=CARTESIAN_POINT('Ctrl Pts',(29.0742713970762,66.4405348010404,12.));
#105270=CARTESIAN_POINT('Ctrl Pts',(29.0731594489218,66.4156112260904,12.));
#105271=CARTESIAN_POINT('Ctrl Pts',(29.0720254879535,66.3907289996942,12.));
#105272=CARTESIAN_POINT('Ctrl Pts',(29.0708695756335,66.3658882283906,12.));
#105273=CARTESIAN_POINT('Ctrl Pts',(29.0696917737397,66.3410890190879,12.));
#105274=CARTESIAN_POINT('Ctrl Pts',(29.0684921443718,66.3163314790607,12.));
#105275=CARTESIAN_POINT('Ctrl Pts',(29.0672707499527,66.2916157159528,12.));
#105276=CARTESIAN_POINT('Ctrl Pts',(29.0660276532272,66.2669418377866,12.));
#105277=CARTESIAN_POINT('Ctrl Pts',(29.0647629172645,66.2423099529668,12.));
#105278=CARTESIAN_POINT('Ctrl Pts',(29.0634766054599,66.2177201702819,12.));
#105279=CARTESIAN_POINT('Ctrl Pts',(29.062168781542,66.1931725989008,12.));
#105280=CARTESIAN_POINT('Ctrl Pts',(29.0608395095745,66.1686673483755,12.));
#105281=CARTESIAN_POINT('Ctrl Pts',(29.0594888539555,66.1442045286516,12.));
#105282=CARTESIAN_POINT('Ctrl Pts',(29.0581168794189,66.1197842500711,12.));
#105283=CARTESIAN_POINT('Ctrl Pts',(29.0567236510373,66.0954066233754,12.));
#105284=CARTESIAN_POINT('Ctrl Pts',(29.0553092342278,66.0710717597009,12.));
#105285=CARTESIAN_POINT('Ctrl Pts',(29.0538736947552,66.0467797705815,12.));
#105286=CARTESIAN_POINT('Ctrl Pts',(29.0524170987307,66.0225307679591,12.));
#105287=CARTESIAN_POINT('Ctrl Pts',(29.0509395126142,65.9983248641879,12.));
#105288=CARTESIAN_POINT('Ctrl Pts',(29.0494410032172,65.974162172037,12.));
#105289=CARTESIAN_POINT('Ctrl Pts',(29.0479216377081,65.9500428046868,12.));
#105290=CARTESIAN_POINT('Ctrl Pts',(29.0463814836157,65.9259668757307,12.));
#105291=CARTESIAN_POINT('Ctrl Pts',(29.0448206088288,65.9019344991854,12.));
#105292=CARTESIAN_POINT('Ctrl Pts',(29.0432390815977,65.8779457894961,12.));
#105293=CARTESIAN_POINT('Ctrl Pts',(29.0416369705375,65.854000861539,12.));
#105294=CARTESIAN_POINT('Ctrl Pts',(29.0400143446338,65.8300998306191,12.));
#105295=CARTESIAN_POINT('Ctrl Pts',(29.0383712732469,65.8062428124713,12.));
#105296=CARTESIAN_POINT('Ctrl Pts',(29.0367078261102,65.7824299232705,12.));
#105297=CARTESIAN_POINT('Ctrl Pts',(29.035024073333,65.7586612796368,12.));
#105298=CARTESIAN_POINT('Ctrl Pts',(29.0333200854027,65.7349369986384,12.));
#105299=CARTESIAN_POINT('Ctrl Pts',(29.0315959331919,65.7112571977891,12.));
#105300=CARTESIAN_POINT('Ctrl Pts',(29.0298516879611,65.6876219950493,12.));
#105301=CARTESIAN_POINT('Ctrl Pts',(29.0280874213596,65.6640315088388,12.));
#105302=CARTESIAN_POINT('Ctrl Pts',(29.0263032054266,65.6404858580403,12.));
#105303=CARTESIAN_POINT('Ctrl Pts',(29.0244991125958,65.6169851620046,12.));
#105304=CARTESIAN_POINT('Ctrl Pts',(29.0226752157003,65.5935295405453,12.));
#105305=CARTESIAN_POINT('Ctrl Pts',(29.0208315879764,65.5701191139418,12.));
#105306=CARTESIAN_POINT('Ctrl Pts',(29.0189683030642,65.5467540029514,12.));
#105307=CARTESIAN_POINT('Ctrl Pts',(29.0170854350095,65.5234343288136,12.));
#105308=CARTESIAN_POINT('Ctrl Pts',(29.0151830582675,65.5001602132535,12.));
#105309=CARTESIAN_POINT('Ctrl Pts',(29.013261247709,65.4769317784789,12.));
#105310=CARTESIAN_POINT('Ctrl Pts',(29.0113200786239,65.4537491471828,12.));
#105311=CARTESIAN_POINT('Ctrl Pts',(29.0093596267215,65.4306124425562,12.));
#105312=CARTESIAN_POINT('Ctrl Pts',(29.0073799681342,65.4075217882934,12.));
#105313=CARTESIAN_POINT('Ctrl Pts',(29.0053811794207,65.3844773085961,12.));
#105314=CARTESIAN_POINT('Ctrl Pts',(29.003363337573,65.3614791281692,12.));
#105315=CARTESIAN_POINT('Ctrl Pts',(29.0013265200185,65.3385273722241,12.));
#105316=CARTESIAN_POINT('Ctrl Pts',(28.9992708046211,65.3156221664916,12.));
#105317=CARTESIAN_POINT('Ctrl Pts',(28.9971962696845,65.2927636372254,12.));
#105318=CARTESIAN_POINT('Ctrl Pts',(28.9951029939557,65.2699519112064,12.));
#105319=CARTESIAN_POINT('Ctrl Pts',(28.9929910566325,65.2471871157397,12.));
#105320=CARTESIAN_POINT('Ctrl Pts',(28.9908605373663,65.2244693786609,12.));
#105321=CARTESIAN_POINT('Ctrl Pts',(28.9887115162633,65.2017988283479,12.));
#105322=CARTESIAN_POINT('Ctrl Pts',(28.9865440738883,65.1791755937256,12.));
#105323=CARTESIAN_POINT('Ctrl Pts',(28.9843582912692,65.1565998042697,12.));
#105324=CARTESIAN_POINT('Ctrl Pts',(28.9821542499042,65.1340715900028,12.));
#105325=CARTESIAN_POINT('Ctrl Pts',(28.9799320317641,65.1115910815037,12.));
#105326=CARTESIAN_POINT('Ctrl Pts',(28.9776917192933,65.0891584099168,12.));
#105327=CARTESIAN_POINT('Ctrl Pts',(28.9754333954135,65.0667737069563,12.));
#105328=CARTESIAN_POINT('Ctrl Pts',(28.9731571435282,65.0444371049082,12.));
#105329=CARTESIAN_POINT('Ctrl Pts',(28.97086304753,65.022148736628,12.));
#105330=CARTESIAN_POINT('Ctrl Pts',(28.9685511918018,64.9999087355504,12.));
#105331=CARTESIAN_POINT('Ctrl Pts',(28.9662216612217,64.9777172357027,12.));
#105332=CARTESIAN_POINT('Ctrl Pts',(28.9638745411677,64.955574371711,12.));
#105333=CARTESIAN_POINT('Ctrl Pts',(28.9615099175249,64.9334802788038,12.));
#105334=CARTESIAN_POINT('Ctrl Pts',(28.9591278766934,64.9114350928125,12.));
#105335=CARTESIAN_POINT('Ctrl Pts',(28.9567285055866,64.8894389501801,12.));
#105336=CARTESIAN_POINT('Ctrl Pts',(28.9543118916328,64.8674919879648,12.));
#105337=CARTESIAN_POINT('Ctrl Pts',(28.9518781227765,64.8455943438423,12.));
#105338=CARTESIAN_POINT('Ctrl Pts',(28.9494272874831,64.8237461561019,12.));
#105339=CARTESIAN_POINT('Ctrl Pts',(28.9469594747431,64.8019475636442,12.));
#105340=CARTESIAN_POINT('Ctrl Pts',(28.944474774081,64.7801987060084,12.));
#105341=CARTESIAN_POINT('Ctrl Pts',(28.9419732755655,64.758499723388,12.));
#105342=CARTESIAN_POINT('Ctrl Pts',(28.9394550698204,64.7368507566467,12.));
#105343=CARTESIAN_POINT('Ctrl Pts',(28.9369202480392,64.715251947329,12.));
#105344=CARTESIAN_POINT('Ctrl Pts',(28.9343689019882,64.6937034376617,12.));
#105345=CARTESIAN_POINT('Ctrl Pts',(28.9318011239915,64.672205370541,12.));
#105346=CARTESIAN_POINT('Ctrl Pts',(28.9292170069221,64.6507578895161,12.));
#105347=CARTESIAN_POINT('Ctrl Pts',(28.926616644195,64.629361138774,12.));
#105348=CARTESIAN_POINT('Ctrl Pts',(28.9240001297542,64.6080152631039,12.));
#105349=CARTESIAN_POINT('Ctrl Pts',(28.9213675580985,64.5867204079426,12.));
#105350=CARTESIAN_POINT('Ctrl Pts',(28.9187190243224,64.5654767194472,12.));
#105351=CARTESIAN_POINT('Ctrl Pts',(28.9160546241538,64.5442843445559,12.));
#105352=CARTESIAN_POINT('Ctrl Pts',(28.9133744539949,64.523143431047,12.));
#105353=CARTESIAN_POINT('Ctrl Pts',(28.910678610965,64.5020541275951,12.));
#105354=CARTESIAN_POINT('Ctrl Pts',(28.9079671928264,64.4810165836592,12.));
#105355=CARTESIAN_POINT('Ctrl Pts',(28.9052402979062,64.4600309493583,12.));
#105356=CARTESIAN_POINT('Ctrl Pts',(28.9024980250307,64.4390973753634,12.));
#105357=CARTESIAN_POINT('Ctrl Pts',(28.899740473434,64.4182160127379,12.));
#105358=CARTESIAN_POINT('Ctrl Pts',(28.8969677427504,64.397387012917,12.));
#105359=CARTESIAN_POINT('Ctrl Pts',(28.89417993323,64.3766105280688,12.));
#105360=CARTESIAN_POINT('Ctrl Pts',(28.8913771459323,64.3558867114076,12.));
#105361=CARTESIAN_POINT('Ctrl Pts',(28.8885594828926,64.3352157174619,12.));
#105362=CARTESIAN_POINT('Ctrl Pts',(28.8857270473959,64.3145977025037,12.));
#105363=CARTESIAN_POINT('Ctrl Pts',(28.882879943794,64.2940328242521,12.));
#105364=CARTESIAN_POINT('Ctrl Pts',(28.8800182770064,64.2735212410711,12.));
#105365=CARTESIAN_POINT('Ctrl Pts',(28.877142152106,64.2530631112929,12.));
#105366=CARTESIAN_POINT('Ctrl Pts',(28.8742516738946,64.2326585925252,12.));
#105367=CARTESIAN_POINT('Ctrl Pts',(28.8713469464185,64.2123078408461,12.));
#105368=CARTESIAN_POINT('Ctrl Pts',(28.8684280739014,64.1920110123299,12.));
#105369=CARTESIAN_POINT('Ctrl Pts',(28.8654951618649,64.1717682648685,12.));
#105370=CARTESIAN_POINT('Ctrl Pts',(28.8625483180437,64.1515797596564,12.));
#105371=CARTESIAN_POINT('Ctrl Pts',(28.8595876537148,64.1314456633381,12.));
#105372=CARTESIAN_POINT('Ctrl Pts',(28.8566132838178,64.1113661481965,12.));
#105373=CARTESIAN_POINT('Ctrl Pts',(28.8536253241853,64.0913413876622,12.));
#105374=CARTESIAN_POINT('Ctrl Pts',(28.8506238891092,64.0713715523599,12.));
#105375=CARTESIAN_POINT('Ctrl Pts',(28.8476090892232,64.0514568066637,12.));
#105376=CARTESIAN_POINT('Ctrl Pts',(28.844581028125,64.0315973031942,12.));
#105377=CARTESIAN_POINT('Ctrl Pts',(28.8415398056428,64.0117931881298,12.));
#105378=CARTESIAN_POINT('Ctrl Pts',(28.8384855243242,63.9920446117582,12.));
#105379=CARTESIAN_POINT('Ctrl Pts',(28.83541829466,63.9723517369614,12.));
#105380=CARTESIAN_POINT('Ctrl Pts',(28.8323382413789,63.9527147494423,12.));
#105381=CARTESIAN_POINT('Ctrl Pts',(28.8292455077559,63.9331338646996,12.));
#105382=CARTESIAN_POINT('Ctrl Pts',(28.8261402423291,63.9136093063786,12.));
#105383=CARTESIAN_POINT('Ctrl Pts',(28.823022586318,63.8941412856924,12.));
#105384=CARTESIAN_POINT('Ctrl Pts',(28.8198926619857,63.8747299825313,12.));
#105385=CARTESIAN_POINT('Ctrl Pts',(28.8167505576681,63.8553755207487,12.));
#105386=CARTESIAN_POINT('Ctrl Pts',(28.8135963263368,63.8360779669856,12.));
#105387=CARTESIAN_POINT('Ctrl Pts',(28.8110632620957,63.8206854735028,12.));
#105388=CARTESIAN_POINT('Ctrl Pts',(28.8091580239553,63.8091667271232,12.));
#105389=CARTESIAN_POINT('Ctrl Pts',(28.8078854475432,63.8014989507494,12.));
#105390=CARTESIAN_POINT('Ctrl Pts',(28.8072485549236,63.7976679095314,12.));
#105391=CARTESIAN_POINT('Ctrl Pts',(27.6958230985043,68.8415926175085,-2.22044604925031E-15));
#105392=CARTESIAN_POINT('Ctrl Pts',(27.6958230985043,68.8415926175085,4.));
#105393=CARTESIAN_POINT('Ctrl Pts',(27.6958230985043,68.8415926175085,8.));
#105394=CARTESIAN_POINT('Ctrl Pts',(27.6958230985043,68.8415926175085,12.));
#105395=CARTESIAN_POINT('Ctrl Pts',(27.7750822307002,68.9176987693915,-2.22044604925031E-15));
#105396=CARTESIAN_POINT('Ctrl Pts',(27.7750822307002,68.9176987693915,4.));
#105397=CARTESIAN_POINT('Ctrl Pts',(27.7750822307002,68.9176987693915,8.));
#105398=CARTESIAN_POINT('Ctrl Pts',(27.7750822307002,68.9176987693915,12.));
#105399=CARTESIAN_POINT('Ctrl Pts',(27.9589320265197,69.002974546758,-2.00119860333522E-15));
#105400=CARTESIAN_POINT('Ctrl Pts',(27.9589320265197,69.002974546758,4.));
#105401=CARTESIAN_POINT('Ctrl Pts',(27.9589320265197,69.002974546758,7.99999999999999));
#105402=CARTESIAN_POINT('Ctrl Pts',(27.9589320265197,69.002974546758,12.));
#105403=CARTESIAN_POINT('Ctrl Pts',(28.1553386138881,68.9748773050759,-1.48061250865807E-15));
#105404=CARTESIAN_POINT('Ctrl Pts',(28.1553386138881,68.9748773050759,4.));
#105405=CARTESIAN_POINT('Ctrl Pts',(28.1553386138881,68.9748773050759,8.00000000000001));
#105406=CARTESIAN_POINT('Ctrl Pts',(28.1553386138881,68.9748773050759,12.));
#105407=CARTESIAN_POINT('Ctrl Pts',(28.2316040302242,68.9436475237613,-1.22965056797476E-15));
#105408=CARTESIAN_POINT('Ctrl Pts',(28.2316040302242,68.9436475237613,4.));
#105409=CARTESIAN_POINT('Ctrl Pts',(28.2316040302242,68.9436475237612,8.));
#105410=CARTESIAN_POINT('Ctrl Pts',(28.2316040302242,68.9436475237612,12.));
#105411=CARTESIAN_POINT('',(27.6958230985043,68.8415926175085,2.77555756156289E-16));
#105412=CARTESIAN_POINT('',(28.2316040302242,68.9436475237612,2.77555756156289E-16));
#105413=CARTESIAN_POINT('Ctrl Pts',(27.6958230985043,68.8415926175085,-1.12534929619454E-16));
#105414=CARTESIAN_POINT('Ctrl Pts',(27.7750822307002,68.9176987693915,-1.12534929619455E-16));
#105415=CARTESIAN_POINT('Ctrl Pts',(27.8801392568828,68.9664277850295,1.27493251891736E-17));
#105416=CARTESIAN_POINT('Ctrl Pts',(27.9892964598977,68.9781370393455,2.36429873471121E-16));
#105417=CARTESIAN_POINT('Ctrl Pts',(28.0711643621588,68.9869189800825,4.04190284682582E-16));
#105418=CARTESIAN_POINT('Ctrl Pts',(28.1553386138881,68.9748773050759,6.27298610972785E-16));
#105419=CARTESIAN_POINT('Ctrl Pts',(28.2316040302242,68.9436475237613,8.78260551656101E-16));
#105420=CARTESIAN_POINT('',(28.2316040302242,68.9436475237612,12.));
#105421=CARTESIAN_POINT('Ctrl Pts',(28.2316040302242,68.9436475237613,-1.22965056797476E-15));
#105422=CARTESIAN_POINT('Ctrl Pts',(28.2316040302242,68.9436475237613,4.));
#105423=CARTESIAN_POINT('Ctrl Pts',(28.2316040302242,68.9436475237612,8.));
#105424=CARTESIAN_POINT('Ctrl Pts',(28.2316040302242,68.9436475237612,12.));
#105425=CARTESIAN_POINT('',(27.6958230985043,68.8415926175085,12.));
#105426=CARTESIAN_POINT('Ctrl Pts',(28.2316040302242,68.9436475237612,12.));
#105427=CARTESIAN_POINT('Ctrl Pts',(28.1553386138881,68.9748773050759,12.));
#105428=CARTESIAN_POINT('Ctrl Pts',(28.0711643621588,68.9869189800825,12.));
#105429=CARTESIAN_POINT('Ctrl Pts',(27.9892964598977,68.9781370393455,12.));
#105430=CARTESIAN_POINT('Ctrl Pts',(27.8801392568828,68.9664277850295,12.));
#105431=CARTESIAN_POINT('Ctrl Pts',(27.7750822307002,68.9176987693915,12.));
#105432=CARTESIAN_POINT('Ctrl Pts',(27.6958230985043,68.8415926175085,12.));
#105433=CARTESIAN_POINT('Ctrl Pts',(27.6958230985043,68.8415926175085,12.));
#105434=CARTESIAN_POINT('Ctrl Pts',(27.6958230985043,68.8415926175085,8.));
#105435=CARTESIAN_POINT('Ctrl Pts',(27.6958230985043,68.8415926175085,4.));
#105436=CARTESIAN_POINT('Ctrl Pts',(27.6958230985043,68.8415926175085,-2.22044604925031E-15));
#105437=CARTESIAN_POINT('Origin',(1.43354795624835E-10,3.4634846687719E-10,
0.));
#105438=CARTESIAN_POINT('Origin',(1.43354795624835E-10,3.4634846687719E-10,
12.));
#105439=CARTESIAN_POINT('Origin',(1.43354795624835E-10,3.4634846687719E-10,
0.));
#105440=CARTESIAN_POINT('Ctrl Pts',(34.6669728017236,65.9427857825597,0.));
#105441=CARTESIAN_POINT('Ctrl Pts',(34.6669728017236,65.9427857825597,4.));
#105442=CARTESIAN_POINT('Ctrl Pts',(34.6669728017236,65.9427857825597,8.));
#105443=CARTESIAN_POINT('Ctrl Pts',(34.6669728017236,65.9427857825597,12.));
#105444=CARTESIAN_POINT('Ctrl Pts',(34.7642339552035,65.8916543400169,0.));
#105445=CARTESIAN_POINT('Ctrl Pts',(34.7642339552035,65.8916543400169,4.));
#105446=CARTESIAN_POINT('Ctrl Pts',(34.7642339552035,65.8916543400169,8.));
#105447=CARTESIAN_POINT('Ctrl Pts',(34.7642339552035,65.8916543400169,12.));
#105448=CARTESIAN_POINT('Ctrl Pts',(34.9032616822024,65.7441961270804,0.));
#105449=CARTESIAN_POINT('Ctrl Pts',(34.9032616822024,65.7441961270804,4.));
#105450=CARTESIAN_POINT('Ctrl Pts',(34.9032616822024,65.7441961270803,7.99999999999999));
#105451=CARTESIAN_POINT('Ctrl Pts',(34.9032616822024,65.7441961270803,12.));
#105452=CARTESIAN_POINT('Ctrl Pts',(34.9387029822715,65.5489812297285,0.));
#105453=CARTESIAN_POINT('Ctrl Pts',(34.9387029822715,65.5489812297285,4.));
#105454=CARTESIAN_POINT('Ctrl Pts',(34.9387029822716,65.5489812297284,8.00000000000001));
#105455=CARTESIAN_POINT('Ctrl Pts',(34.9387029822716,65.5489812297284,12.));
#105456=CARTESIAN_POINT('Ctrl Pts',(34.9331875523085,65.4667541477953,0.));
#105457=CARTESIAN_POINT('Ctrl Pts',(34.9331875523085,65.4667541477953,4.));
#105458=CARTESIAN_POINT('Ctrl Pts',(34.9331875523085,65.4667541477952,8.));
#105459=CARTESIAN_POINT('Ctrl Pts',(34.9331875523085,65.4667541477952,12.));
#105460=CARTESIAN_POINT('',(34.6669728017236,65.9427857825597,0.));
#105461=CARTESIAN_POINT('',(34.9331875523085,65.4667541477953,0.));
#105462=CARTESIAN_POINT('Ctrl Pts',(34.6669728017236,65.9427857825597,2.77555756156289E-16));
#105463=CARTESIAN_POINT('Ctrl Pts',(34.7642339552035,65.8916543400169,2.77555756156289E-16));
#105464=CARTESIAN_POINT('Ctrl Pts',(34.8436783706314,65.8073925040532,2.77555756156289E-16));
#105465=CARTESIAN_POINT('Ctrl Pts',(34.8892986466537,65.7075366486885,2.77555756156289E-16));
#105466=CARTESIAN_POINT('Ctrl Pts',(34.9235138536705,65.632644757165,2.77555756156289E-16));
#105467=CARTESIAN_POINT('Ctrl Pts',(34.9387029822715,65.5489812297285,2.77555756156289E-16));
#105468=CARTESIAN_POINT('Ctrl Pts',(34.9331875523085,65.4667541477953,2.77555756156289E-16));
#105469=CARTESIAN_POINT('',(34.9331875523085,65.4667541477952,12.));
#105470=CARTESIAN_POINT('Ctrl Pts',(34.9331875523085,65.4667541477953,0.));
#105471=CARTESIAN_POINT('Ctrl Pts',(34.9331875523085,65.4667541477953,4.));
#105472=CARTESIAN_POINT('Ctrl Pts',(34.9331875523085,65.4667541477952,8.));
#105473=CARTESIAN_POINT('Ctrl Pts',(34.9331875523085,65.4667541477952,12.));
#105474=CARTESIAN_POINT('',(34.6669728017236,65.9427857825597,12.));
#105475=CARTESIAN_POINT('Ctrl Pts',(34.9331875523085,65.4667541477952,12.));
#105476=CARTESIAN_POINT('Ctrl Pts',(34.9387029822716,65.5489812297284,12.));
#105477=CARTESIAN_POINT('Ctrl Pts',(34.9235138536705,65.6326447571649,12.));
#105478=CARTESIAN_POINT('Ctrl Pts',(34.8892986466538,65.7075366486884,12.));
#105479=CARTESIAN_POINT('Ctrl Pts',(34.8436783706315,65.8073925040531,12.));
#105480=CARTESIAN_POINT('Ctrl Pts',(34.7642339552035,65.8916543400169,12.));
#105481=CARTESIAN_POINT('Ctrl Pts',(34.6669728017236,65.9427857825597,12.));
#105482=CARTESIAN_POINT('Ctrl Pts',(34.6669728017236,65.9427857825597,12.));
#105483=CARTESIAN_POINT('Ctrl Pts',(34.6669728017236,65.9427857825597,8.));
#105484=CARTESIAN_POINT('Ctrl Pts',(34.6669728017236,65.9427857825597,4.));
#105485=CARTESIAN_POINT('Ctrl Pts',(34.6669728017236,65.9427857825597,0.));
#105486=CARTESIAN_POINT('Ctrl Pts',(34.2579614092497,61.0441813777723,0.));
#105487=CARTESIAN_POINT('Ctrl Pts',(34.2579614092497,61.0441813777723,12.));
#105488=CARTESIAN_POINT('Ctrl Pts',(34.2589297755434,61.0479423318725,0.));
#105489=CARTESIAN_POINT('Ctrl Pts',(34.2589297755434,61.0479423318725,12.));
#105490=CARTESIAN_POINT('Ctrl Pts',(34.2608658001631,61.0554700176998,0.));
#105491=CARTESIAN_POINT('Ctrl Pts',(34.2608658001631,61.0554700176998,12.));
#105492=CARTESIAN_POINT('Ctrl Pts',(34.2637677131934,61.0667788793266,0.));
#105493=CARTESIAN_POINT('Ctrl Pts',(34.2637677131934,61.0667788793266,12.));
#105494=CARTESIAN_POINT('Ctrl Pts',(34.2676326825626,61.0818920286293,0.));
#105495=CARTESIAN_POINT('Ctrl Pts',(34.2676326825626,61.0818920286293,12.));
#105496=CARTESIAN_POINT('Ctrl Pts',(34.2724568037227,61.1008412399997,0.));
#105497=CARTESIAN_POINT('Ctrl Pts',(34.2724568037227,61.1008412399997,12.));
#105498=CARTESIAN_POINT('Ctrl Pts',(34.277273803877,61.1198481997764,0.));
#105499=CARTESIAN_POINT('Ctrl Pts',(34.277273803877,61.1198481997764,12.));
#105500=CARTESIAN_POINT('Ctrl Pts',(34.2820836244469,61.1389128461886,0.));
#105501=CARTESIAN_POINT('Ctrl Pts',(34.2820836244469,61.1389128461886,12.));
#105502=CARTESIAN_POINT('Ctrl Pts',(34.2868861666384,61.1580350635533,0.));
#105503=CARTESIAN_POINT('Ctrl Pts',(34.2868861666384,61.1580350635533,12.));
#105504=CARTESIAN_POINT('Ctrl Pts',(34.2916812929751,61.1772146833205,0.));
#105505=CARTESIAN_POINT('Ctrl Pts',(34.2916812929751,61.1772146833205,12.));
#105506=CARTESIAN_POINT('Ctrl Pts',(34.2964688443663,61.1964515073891,0.));
#105507=CARTESIAN_POINT('Ctrl Pts',(34.2964688443663,61.1964515073891,12.));
#105508=CARTESIAN_POINT('Ctrl Pts',(34.3012486533474,61.2157453259107,0.));
#105509=CARTESIAN_POINT('Ctrl Pts',(34.3012486533474,61.2157453259107,12.));
#105510=CARTESIAN_POINT('Ctrl Pts',(34.3060205584064,61.2350959366939,0.));
#105511=CARTESIAN_POINT('Ctrl Pts',(34.3060205584064,61.2350959366939,12.));
#105512=CARTESIAN_POINT('Ctrl Pts',(34.3107844191043,61.2545031656133,0.));
#105513=CARTESIAN_POINT('Ctrl Pts',(34.3107844191043,61.2545031656133,12.));
#105514=CARTESIAN_POINT('Ctrl Pts',(34.3155401111747,61.2739668600365,0.));
#105515=CARTESIAN_POINT('Ctrl Pts',(34.3155401111747,61.2739668600365,12.));
#105516=CARTESIAN_POINT('Ctrl Pts',(34.3202875193617,61.2934868791855,0.));
#105517=CARTESIAN_POINT('Ctrl Pts',(34.3202875193617,61.2934868791855,12.));
#105518=CARTESIAN_POINT('Ctrl Pts',(34.3250265314768,61.3130630861386,0.));
#105519=CARTESIAN_POINT('Ctrl Pts',(34.3250265314768,61.3130630861386,12.));
#105520=CARTESIAN_POINT('Ctrl Pts',(34.3297570310146,61.3326953378851,0.));
#105521=CARTESIAN_POINT('Ctrl Pts',(34.3297570310146,61.3326953378851,12.));
#105522=CARTESIAN_POINT('Ctrl Pts',(34.3344788934363,61.3523834803188,0.));
#105523=CARTESIAN_POINT('Ctrl Pts',(34.3344788934363,61.3523834803188,12.));
#105524=CARTESIAN_POINT('Ctrl Pts',(34.339191990014,61.3721273534257,0.));
#105525=CARTESIAN_POINT('Ctrl Pts',(34.339191990014,61.3721273534257,12.));
#105526=CARTESIAN_POINT('Ctrl Pts',(34.3438961902405,61.3919267945302,0.));
#105527=CARTESIAN_POINT('Ctrl Pts',(34.3438961902405,61.3919267945302,12.));
#105528=CARTESIAN_POINT('Ctrl Pts',(34.3485913645979,61.4117816420229,0.));
#105529=CARTESIAN_POINT('Ctrl Pts',(34.3485913645979,61.4117816420229,12.));
#105530=CARTESIAN_POINT('Ctrl Pts',(34.3532773877089,61.4316917395918,0.));
#105531=CARTESIAN_POINT('Ctrl Pts',(34.3532773877089,61.4316917395918,12.));
#105532=CARTESIAN_POINT('Ctrl Pts',(34.3579541381996,61.4516569360454,0.));
#105533=CARTESIAN_POINT('Ctrl Pts',(34.3579541381996,61.4516569360454,12.));
#105534=CARTESIAN_POINT('Ctrl Pts',(34.3626214971888,61.4716770832897,0.));
#105535=CARTESIAN_POINT('Ctrl Pts',(34.3626214971888,61.4716770832897,12.));
#105536=CARTESIAN_POINT('Ctrl Pts',(34.3672793472465,61.4917520349278,0.));
#105537=CARTESIAN_POINT('Ctrl Pts',(34.3672793472465,61.4917520349278,12.));
#105538=CARTESIAN_POINT('Ctrl Pts',(34.3719275711195,61.5118816445437,0.));
#105539=CARTESIAN_POINT('Ctrl Pts',(34.3719275711195,61.5118816445437,12.));
#105540=CARTESIAN_POINT('Ctrl Pts',(34.376566050668,61.5320657642638,0.));
#105541=CARTESIAN_POINT('Ctrl Pts',(34.376566050668,61.5320657642638,12.));
#105542=CARTESIAN_POINT('Ctrl Pts',(34.3811946674197,61.5523042455158,0.));
#105543=CARTESIAN_POINT('Ctrl Pts',(34.3811946674197,61.5523042455158,12.));
#105544=CARTESIAN_POINT('Ctrl Pts',(34.3858133030518,61.5725969396829,0.));
#105545=CARTESIAN_POINT('Ctrl Pts',(34.3858133030518,61.5725969396829,12.));
#105546=CARTESIAN_POINT('Ctrl Pts',(34.3904218398636,61.5929436987409,0.));
#105547=CARTESIAN_POINT('Ctrl Pts',(34.3904218398636,61.5929436987409,12.));
#105548=CARTESIAN_POINT('Ctrl Pts',(34.3950201613432,61.6133443760142,0.));
#105549=CARTESIAN_POINT('Ctrl Pts',(34.3950201613432,61.6133443760142,12.));
#105550=CARTESIAN_POINT('Ctrl Pts',(34.3996081523753,61.6337988264556,0.));
#105551=CARTESIAN_POINT('Ctrl Pts',(34.3996081523753,61.6337988264556,12.));
#105552=CARTESIAN_POINT('Ctrl Pts',(34.4041856989316,61.6543069062416,0.));
#105553=CARTESIAN_POINT('Ctrl Pts',(34.4041856989316,61.6543069062416,12.));
#105554=CARTESIAN_POINT('Ctrl Pts',(34.4087526878812,61.6748684725205,0.));
#105555=CARTESIAN_POINT('Ctrl Pts',(34.4087526878812,61.6748684725205,12.));
#105556=CARTESIAN_POINT('Ctrl Pts',(34.4133090067703,61.695483383117,0.));
#105557=CARTESIAN_POINT('Ctrl Pts',(34.4133090067703,61.695483383117,12.));
#105558=CARTESIAN_POINT('Ctrl Pts',(34.4178545435766,61.7161514961915,0.));
#105559=CARTESIAN_POINT('Ctrl Pts',(34.4178545435766,61.7161514961915,12.));
#105560=CARTESIAN_POINT('Ctrl Pts',(34.4223891867179,61.7368726702596,0.));
#105561=CARTESIAN_POINT('Ctrl Pts',(34.4223891867179,61.7368726702596,12.));
#105562=CARTESIAN_POINT('Ctrl Pts',(34.4269128251576,61.7576467643432,0.));
#105563=CARTESIAN_POINT('Ctrl Pts',(34.4269128251576,61.7576467643432,12.));
#105564=CARTESIAN_POINT('Ctrl Pts',(34.4314253484791,61.7784736380727,0.));
#105565=CARTESIAN_POINT('Ctrl Pts',(34.4314253484791,61.7784736380727,12.));
#105566=CARTESIAN_POINT('Ctrl Pts',(34.4359266469749,61.7993531518037,0.));
#105567=CARTESIAN_POINT('Ctrl Pts',(34.4359266469749,61.7993531518037,12.));
#105568=CARTESIAN_POINT('Ctrl Pts',(34.4404166117299,61.8202851667222,0.));
#105569=CARTESIAN_POINT('Ctrl Pts',(34.4404166117299,61.8202851667222,12.));
#105570=CARTESIAN_POINT('Ctrl Pts',(34.4448951345739,61.8412695447926,0.));
#105571=CARTESIAN_POINT('Ctrl Pts',(34.4448951345739,61.8412695447926,12.));
#105572=CARTESIAN_POINT('Ctrl Pts',(34.449362108036,61.8623061487018,0.));
#105573=CARTESIAN_POINT('Ctrl Pts',(34.449362108036,61.8623061487018,12.));
#105574=CARTESIAN_POINT('Ctrl Pts',(34.4538174253012,61.8833948418025,0.));
#105575=CARTESIAN_POINT('Ctrl Pts',(34.4538174253012,61.8833948418025,12.));
#105576=CARTESIAN_POINT('Ctrl Pts',(34.4582609801637,61.9045354880445,0.));
#105577=CARTESIAN_POINT('Ctrl Pts',(34.4582609801637,61.9045354880445,12.));
#105578=CARTESIAN_POINT('Ctrl Pts',(34.4626926669974,61.9257279519308,0.));
#105579=CARTESIAN_POINT('Ctrl Pts',(34.4626926669974,61.9257279519308,12.));
#105580=CARTESIAN_POINT('Ctrl Pts',(34.4671123807717,61.9469720985531,0.));
#105581=CARTESIAN_POINT('Ctrl Pts',(34.4671123807717,61.9469720985531,12.));
#105582=CARTESIAN_POINT('Ctrl Pts',(34.4715200170592,61.9682677936054,0.));
#105583=CARTESIAN_POINT('Ctrl Pts',(34.4715200170592,61.9682677936054,12.));
#105584=CARTESIAN_POINT('Ctrl Pts',(34.4759154720473,61.9896149034001,0.));
#105585=CARTESIAN_POINT('Ctrl Pts',(34.4759154720473,61.9896149034001,12.));
#105586=CARTESIAN_POINT('Ctrl Pts',(34.4802986425528,62.0110132948794,0.));
#105587=CARTESIAN_POINT('Ctrl Pts',(34.4802986425528,62.0110132948794,12.));
#105588=CARTESIAN_POINT('Ctrl Pts',(34.4846694260199,62.0324628356141,0.));
#105589=CARTESIAN_POINT('Ctrl Pts',(34.4846694260199,62.0324628356141,12.));
#105590=CARTESIAN_POINT('Ctrl Pts',(34.4890277205039,62.0539633937939,0.));
#105591=CARTESIAN_POINT('Ctrl Pts',(34.4890277205039,62.0539633937939,12.));
#105592=CARTESIAN_POINT('Ctrl Pts',(34.4933734246592,62.0755148382135,0.));
#105593=CARTESIAN_POINT('Ctrl Pts',(34.4933734246592,62.0755148382135,12.));
#105594=CARTESIAN_POINT('Ctrl Pts',(34.4977064377282,62.0971170382567,0.));
#105595=CARTESIAN_POINT('Ctrl Pts',(34.4977064377282,62.0971170382567,12.));
#105596=CARTESIAN_POINT('Ctrl Pts',(34.5020266595293,62.1187698638707,0.));
#105597=CARTESIAN_POINT('Ctrl Pts',(34.5020266595293,62.1187698638707,12.));
#105598=CARTESIAN_POINT('Ctrl Pts',(34.5063339904533,62.1404731855687,0.));
#105599=CARTESIAN_POINT('Ctrl Pts',(34.5063339904533,62.1404731855687,12.));
#105600=CARTESIAN_POINT('Ctrl Pts',(34.5106283314594,62.1622268744337,0.));
#105601=CARTESIAN_POINT('Ctrl Pts',(34.5106283314594,62.1622268744337,12.));
#105602=CARTESIAN_POINT('Ctrl Pts',(34.5149095840729,62.1840308021171,0.));
#105603=CARTESIAN_POINT('Ctrl Pts',(34.5149095840729,62.1840308021171,12.));
#105604=CARTESIAN_POINT('Ctrl Pts',(34.5191776503843,62.2058848408346,0.));
#105605=CARTESIAN_POINT('Ctrl Pts',(34.5191776503843,62.2058848408346,12.));
#105606=CARTESIAN_POINT('Ctrl Pts',(34.5234324330492,62.2277888633576,0.));
#105607=CARTESIAN_POINT('Ctrl Pts',(34.5234324330492,62.2277888633576,12.));
#105608=CARTESIAN_POINT('Ctrl Pts',(34.527673835281,62.2497427430136,0.));
#105609=CARTESIAN_POINT('Ctrl Pts',(34.527673835281,62.2497427430136,12.));
#105610=CARTESIAN_POINT('Ctrl Pts',(34.5319017608434,62.2717463536828,0.));
#105611=CARTESIAN_POINT('Ctrl Pts',(34.5319017608434,62.2717463536828,12.));
#105612=CARTESIAN_POINT('Ctrl Pts',(34.536116114045,62.2937995697927,0.));
#105613=CARTESIAN_POINT('Ctrl Pts',(34.536116114045,62.2937995697927,12.));
#105614=CARTESIAN_POINT('Ctrl Pts',(34.5403167997333,62.3159022663052,0.));
#105615=CARTESIAN_POINT('Ctrl Pts',(34.5403167997333,62.3159022663052,12.));
#105616=CARTESIAN_POINT('Ctrl Pts',(34.5445037232928,62.3380543187067,0.));
#105617=CARTESIAN_POINT('Ctrl Pts',(34.5445037232928,62.3380543187067,12.));
#105618=CARTESIAN_POINT('Ctrl Pts',(34.5486767906376,62.3602556030114,0.));
#105619=CARTESIAN_POINT('Ctrl Pts',(34.5486767906376,62.3602556030114,12.));
#105620=CARTESIAN_POINT('Ctrl Pts',(34.552835908207,62.3825059957593,0.));
#105621=CARTESIAN_POINT('Ctrl Pts',(34.552835908207,62.3825059957593,12.));
#105622=CARTESIAN_POINT('Ctrl Pts',(34.5569809829615,62.4048053740129,0.));
#105623=CARTESIAN_POINT('Ctrl Pts',(34.5569809829615,62.4048053740129,12.));
#105624=CARTESIAN_POINT('Ctrl Pts',(34.5611119223807,62.4271536153473,0.));
#105625=CARTESIAN_POINT('Ctrl Pts',(34.5611119223807,62.4271536153473,12.));
#105626=CARTESIAN_POINT('Ctrl Pts',(34.5652286344606,62.4495505978415,0.));
#105627=CARTESIAN_POINT('Ctrl Pts',(34.5652286344606,62.4495505978415,12.));
#105628=CARTESIAN_POINT('Ctrl Pts',(34.5693310277064,62.471996200083,0.));
#105629=CARTESIAN_POINT('Ctrl Pts',(34.5693310277064,62.471996200083,12.));
#105630=CARTESIAN_POINT('Ctrl Pts',(34.5734190111279,62.494490301164,0.));
#105631=CARTESIAN_POINT('Ctrl Pts',(34.5734190111279,62.494490301164,12.));
#105632=CARTESIAN_POINT('Ctrl Pts',(34.5774924942351,62.5170327806774,0.));
#105633=CARTESIAN_POINT('Ctrl Pts',(34.5774924942351,62.5170327806774,12.));
#105634=CARTESIAN_POINT('Ctrl Pts',(34.5815513870363,62.5396235187053,0.));
#105635=CARTESIAN_POINT('Ctrl Pts',(34.5815513870363,62.5396235187053,12.));
#105636=CARTESIAN_POINT('Ctrl Pts',(34.5855956000343,62.5622623958125,0.));
#105637=CARTESIAN_POINT('Ctrl Pts',(34.5855956000343,62.5622623958125,12.));
#105638=CARTESIAN_POINT('Ctrl Pts',(34.5896250442199,62.5849492930501,0.));
#105639=CARTESIAN_POINT('Ctrl Pts',(34.5896250442199,62.5849492930501,12.));
#105640=CARTESIAN_POINT('Ctrl Pts',(34.5936396310671,62.6076840919521,0.));
#105641=CARTESIAN_POINT('Ctrl Pts',(34.5936396310671,62.6076840919521,12.));
#105642=CARTESIAN_POINT('Ctrl Pts',(34.5976392725303,62.6304666745319,0.));
#105643=CARTESIAN_POINT('Ctrl Pts',(34.5976392725303,62.6304666745319,12.));
#105644=CARTESIAN_POINT('Ctrl Pts',(34.6016238810419,62.6532969232695,0.));
#105645=CARTESIAN_POINT('Ctrl Pts',(34.6016238810419,62.6532969232695,12.));
#105646=CARTESIAN_POINT('Ctrl Pts',(34.6055933695093,62.6761747211081,0.));
#105647=CARTESIAN_POINT('Ctrl Pts',(34.6055933695093,62.6761747211081,12.));
#105648=CARTESIAN_POINT('Ctrl Pts',(34.6095476513095,62.6990999514597,0.));
#105649=CARTESIAN_POINT('Ctrl Pts',(34.6095476513095,62.6990999514597,12.));
#105650=CARTESIAN_POINT('Ctrl Pts',(34.6134866402842,62.7220724982005,0.));
#105651=CARTESIAN_POINT('Ctrl Pts',(34.6134866402842,62.7220724982005,12.));
#105652=CARTESIAN_POINT('Ctrl Pts',(34.6174102507368,62.7450922456662,0.));
#105653=CARTESIAN_POINT('Ctrl Pts',(34.6174102507368,62.7450922456662,12.));
#105654=CARTESIAN_POINT('Ctrl Pts',(34.6213183974302,62.7681590786398,0.));
#105655=CARTESIAN_POINT('Ctrl Pts',(34.6213183974302,62.7681590786398,12.));
#105656=CARTESIAN_POINT('Ctrl Pts',(34.6252109955836,62.7912728823483,0.));
#105657=CARTESIAN_POINT('Ctrl Pts',(34.6252109955836,62.7912728823483,12.));
#105658=CARTESIAN_POINT('Ctrl Pts',(34.629087960866,62.8144335424671,0.));
#105659=CARTESIAN_POINT('Ctrl Pts',(34.629087960866,62.8144335424671,12.));
#105660=CARTESIAN_POINT('Ctrl Pts',(34.6329492093931,62.8376409451167,0.));
#105661=CARTESIAN_POINT('Ctrl Pts',(34.6329492093931,62.8376409451167,12.));
#105662=CARTESIAN_POINT('Ctrl Pts',(34.6367946577241,62.8608949768583,0.));
#105663=CARTESIAN_POINT('Ctrl Pts',(34.6367946577241,62.8608949768583,12.));
#105664=CARTESIAN_POINT('Ctrl Pts',(34.6406242228606,62.8841955246819,0.));
#105665=CARTESIAN_POINT('Ctrl Pts',(34.6406242228606,62.8841955246819,12.));
#105666=CARTESIAN_POINT('Ctrl Pts',(34.6444378222425,62.9075424760042,0.));
#105667=CARTESIAN_POINT('Ctrl Pts',(34.6444378222425,62.9075424760042,12.));
#105668=CARTESIAN_POINT('Ctrl Pts',(34.6482353737433,62.9309357186733,0.));
#105669=CARTESIAN_POINT('Ctrl Pts',(34.6482353737433,62.9309357186733,12.));
#105670=CARTESIAN_POINT('Ctrl Pts',(34.6520167956656,62.9543751409648,0.));
#105671=CARTESIAN_POINT('Ctrl Pts',(34.6520167956656,62.9543751409648,12.));
#105672=CARTESIAN_POINT('Ctrl Pts',(34.6557820067389,62.9778606315777,0.));
#105673=CARTESIAN_POINT('Ctrl Pts',(34.6557820067389,62.9778606315777,12.));
#105674=CARTESIAN_POINT('Ctrl Pts',(34.6595309261185,63.0013920796225,0.));
#105675=CARTESIAN_POINT('Ctrl Pts',(34.6595309261185,63.0013920796225,12.));
#105676=CARTESIAN_POINT('Ctrl Pts',(34.6632634733819,63.0249693746198,0.));
#105677=CARTESIAN_POINT('Ctrl Pts',(34.6632634733819,63.0249693746198,12.));
#105678=CARTESIAN_POINT('Ctrl Pts',(34.6669795685225,63.0485924065039,0.));
#105679=CARTESIAN_POINT('Ctrl Pts',(34.6669795685225,63.0485924065039,12.));
#105680=CARTESIAN_POINT('Ctrl Pts',(34.670679131947,63.0722610656194,0.));
#105681=CARTESIAN_POINT('Ctrl Pts',(34.670679131947,63.0722610656194,12.));
#105682=CARTESIAN_POINT('Ctrl Pts',(34.6743620844721,63.0959752427169,0.));
#105683=CARTESIAN_POINT('Ctrl Pts',(34.6743620844721,63.0959752427169,12.));
#105684=CARTESIAN_POINT('Ctrl Pts',(34.6780283473252,63.119734828943,0.));
#105685=CARTESIAN_POINT('Ctrl Pts',(34.6780283473252,63.119734828943,12.));
#105686=CARTESIAN_POINT('Ctrl Pts',(34.68167784214,63.1435397158385,0.));
#105687=CARTESIAN_POINT('Ctrl Pts',(34.68167784214,63.1435397158385,12.));
#105688=CARTESIAN_POINT('Ctrl Pts',(34.6853104909516,63.1673897953425,0.));
#105689=CARTESIAN_POINT('Ctrl Pts',(34.6853104909516,63.1673897953425,12.));
#105690=CARTESIAN_POINT('Ctrl Pts',(34.6889262161923,63.1912849597885,0.));
#105691=CARTESIAN_POINT('Ctrl Pts',(34.6889262161923,63.1912849597885,12.));
#105692=CARTESIAN_POINT('Ctrl Pts',(34.6925249406898,63.2152251019014,0.));
#105693=CARTESIAN_POINT('Ctrl Pts',(34.6925249406898,63.2152251019014,12.));
#105694=CARTESIAN_POINT('Ctrl Pts',(34.696106587667,63.2392101147854,0.));
#105695=CARTESIAN_POINT('Ctrl Pts',(34.696106587667,63.2392101147854,12.));
#105696=CARTESIAN_POINT('Ctrl Pts',(34.6996710807384,63.2632398919234,0.));
#105697=CARTESIAN_POINT('Ctrl Pts',(34.6996710807384,63.2632398919234,12.));
#105698=CARTESIAN_POINT('Ctrl Pts',(34.7032183439045,63.2873143271813,0.));
#105699=CARTESIAN_POINT('Ctrl Pts',(34.7032183439045,63.2873143271813,12.));
#105700=CARTESIAN_POINT('Ctrl Pts',(34.7067483015492,63.311433314805,0.));
#105701=CARTESIAN_POINT('Ctrl Pts',(34.7067483015492,63.311433314805,12.));
#105702=CARTESIAN_POINT('Ctrl Pts',(34.7102608784372,63.3355967494169,0.));
#105703=CARTESIAN_POINT('Ctrl Pts',(34.7102608784372,63.3355967494169,12.));
#105704=CARTESIAN_POINT('Ctrl Pts',(34.7137559997143,63.359804526005,0.));
#105705=CARTESIAN_POINT('Ctrl Pts',(34.7137559997143,63.359804526005,12.));
#105706=CARTESIAN_POINT('Ctrl Pts',(34.7172335909037,63.3840565399207,0.));
#105707=CARTESIAN_POINT('Ctrl Pts',(34.7172335909037,63.3840565399207,12.));
#105708=CARTESIAN_POINT('Ctrl Pts',(34.7206935779007,63.4083526868837,0.));
#105709=CARTESIAN_POINT('Ctrl Pts',(34.7206935779007,63.4083526868837,12.));
#105710=CARTESIAN_POINT('Ctrl Pts',(34.7241358869702,63.4326928629797,0.));
#105711=CARTESIAN_POINT('Ctrl Pts',(34.7241358869702,63.4326928629797,12.));
#105712=CARTESIAN_POINT('Ctrl Pts',(34.7275604447438,63.4570769646568,0.));
#105713=CARTESIAN_POINT('Ctrl Pts',(34.7275604447438,63.4570769646568,12.));
#105714=CARTESIAN_POINT('Ctrl Pts',(34.7309671782212,63.481504888716,0.));
#105715=CARTESIAN_POINT('Ctrl Pts',(34.7309671782212,63.481504888716,12.));
#105716=CARTESIAN_POINT('Ctrl Pts',(34.7343560147663,63.5059765323082,0.));
#105717=CARTESIAN_POINT('Ctrl Pts',(34.7343560147663,63.5059765323082,12.));
#105718=CARTESIAN_POINT('Ctrl Pts',(34.7377268821022,63.5304917929378,0.));
#105719=CARTESIAN_POINT('Ctrl Pts',(34.7377268821022,63.5304917929378,12.));
#105720=CARTESIAN_POINT('Ctrl Pts',(34.7410797083079,63.5550505684621,0.));
#105721=CARTESIAN_POINT('Ctrl Pts',(34.7410797083079,63.5550505684621,12.));
#105722=CARTESIAN_POINT('Ctrl Pts',(34.7444144218162,63.5796527570874,0.));
#105723=CARTESIAN_POINT('Ctrl Pts',(34.7444144218162,63.5796527570874,12.));
#105724=CARTESIAN_POINT('Ctrl Pts',(34.7477309514142,63.6042982573599,0.));
#105725=CARTESIAN_POINT('Ctrl Pts',(34.7477309514142,63.6042982573599,12.));
#105726=CARTESIAN_POINT('Ctrl Pts',(34.7510292262415,63.628986968162,0.));
#105727=CARTESIAN_POINT('Ctrl Pts',(34.7510292262415,63.628986968162,12.));
#105728=CARTESIAN_POINT('Ctrl Pts',(34.7543091757841,63.6537187887174,0.));
#105729=CARTESIAN_POINT('Ctrl Pts',(34.7543091757841,63.6537187887174,12.));
#105730=CARTESIAN_POINT('Ctrl Pts',(34.7575707298718,63.6784936185893,0.));
#105731=CARTESIAN_POINT('Ctrl Pts',(34.7575707298718,63.6784936185893,12.));
#105732=CARTESIAN_POINT('Ctrl Pts',(34.7608138186757,63.7033113576782,0.));
#105733=CARTESIAN_POINT('Ctrl Pts',(34.7608138186757,63.7033113576782,12.));
#105734=CARTESIAN_POINT('Ctrl Pts',(34.7640383727094,63.7281719062135,0.));
#105735=CARTESIAN_POINT('Ctrl Pts',(34.7640383727094,63.7281719062135,12.));
#105736=CARTESIAN_POINT('Ctrl Pts',(34.7672443228266,63.7530751647479,0.));
#105737=CARTESIAN_POINT('Ctrl Pts',(34.7672443228266,63.7530751647479,12.));
#105738=CARTESIAN_POINT('Ctrl Pts',(34.7704316002165,63.7780210341619,0.));
#105739=CARTESIAN_POINT('Ctrl Pts',(34.7704316002165,63.7780210341619,12.));
#105740=CARTESIAN_POINT('Ctrl Pts',(34.7736001363991,63.8030094156635,0.));
#105741=CARTESIAN_POINT('Ctrl Pts',(34.7736001363991,63.8030094156635,12.));
#105742=CARTESIAN_POINT('Ctrl Pts',(34.7767498632244,63.8280402107858,0.));
#105743=CARTESIAN_POINT('Ctrl Pts',(34.7767498632244,63.8280402107858,12.));
#105744=CARTESIAN_POINT('Ctrl Pts',(34.7798807128716,63.8531133213794,0.));
#105745=CARTESIAN_POINT('Ctrl Pts',(34.7798807128716,63.8531133213794,12.));
#105746=CARTESIAN_POINT('Ctrl Pts',(34.7829926178495,63.8782286496059,0.));
#105747=CARTESIAN_POINT('Ctrl Pts',(34.7829926178495,63.8782286496059,12.));
#105748=CARTESIAN_POINT('Ctrl Pts',(34.7860855109908,63.9033860979429,0.));
#105749=CARTESIAN_POINT('Ctrl Pts',(34.7860855109908,63.9033860979429,12.));
#105750=CARTESIAN_POINT('Ctrl Pts',(34.7891593254485,63.9285855691839,0.));
#105751=CARTESIAN_POINT('Ctrl Pts',(34.7891593254485,63.9285855691839,12.));
#105752=CARTESIAN_POINT('Ctrl Pts',(34.7922139946943,63.9538269664366,0.));
#105753=CARTESIAN_POINT('Ctrl Pts',(34.7922139946943,63.9538269664366,12.));
#105754=CARTESIAN_POINT('Ctrl Pts',(34.7952494525182,63.9791101931169,0.));
#105755=CARTESIAN_POINT('Ctrl Pts',(34.7952494525182,63.9791101931169,12.));
#105756=CARTESIAN_POINT('Ctrl Pts',(34.79826563303,64.0044351529413,0.));
#105757=CARTESIAN_POINT('Ctrl Pts',(34.79826563303,64.0044351529413,12.));
#105758=CARTESIAN_POINT('Ctrl Pts',(34.8012624706533,64.0298017499305,0.));
#105759=CARTESIAN_POINT('Ctrl Pts',(34.8012624706533,64.0298017499305,12.));
#105760=CARTESIAN_POINT('Ctrl Pts',(34.8042399001214,64.0552098884101,0.));
#105761=CARTESIAN_POINT('Ctrl Pts',(34.8042399001214,64.0552098884101,12.));
#105762=CARTESIAN_POINT('Ctrl Pts',(34.8071978564748,64.0806594730085,0.));
#105763=CARTESIAN_POINT('Ctrl Pts',(34.8071978564748,64.0806594730085,12.));
#105764=CARTESIAN_POINT('Ctrl Pts',(34.8101362750595,64.1061504086512,0.));
#105765=CARTESIAN_POINT('Ctrl Pts',(34.8101362750595,64.1061504086512,12.));
#105766=CARTESIAN_POINT('Ctrl Pts',(34.8130550915284,64.1316826005502,0.));
#105767=CARTESIAN_POINT('Ctrl Pts',(34.8130550915284,64.1316826005502,12.));
#105768=CARTESIAN_POINT('Ctrl Pts',(34.8159542418372,64.1572559542085,0.));
#105769=CARTESIAN_POINT('Ctrl Pts',(34.8159542418372,64.1572559542085,12.));
#105770=CARTESIAN_POINT('Ctrl Pts',(34.8188336622418,64.1828703754237,0.));
#105771=CARTESIAN_POINT('Ctrl Pts',(34.8188336622418,64.1828703754237,12.));
#105772=CARTESIAN_POINT('Ctrl Pts',(34.8216932892969,64.2085257702885,0.));
#105773=CARTESIAN_POINT('Ctrl Pts',(34.8216932892969,64.2085257702885,12.));
#105774=CARTESIAN_POINT('Ctrl Pts',(34.8245330598559,64.2342220451878,0.));
#105775=CARTESIAN_POINT('Ctrl Pts',(34.8245330598559,64.2342220451878,12.));
#105776=CARTESIAN_POINT('Ctrl Pts',(34.8273529110742,64.259959106791,0.));
#105777=CARTESIAN_POINT('Ctrl Pts',(34.8273529110742,64.259959106791,12.));
#105778=CARTESIAN_POINT('Ctrl Pts',(34.8301527804052,64.2857368620513,0.));
#105779=CARTESIAN_POINT('Ctrl Pts',(34.8301527804052,64.2857368620513,12.));
#105780=CARTESIAN_POINT('Ctrl Pts',(34.8329326055916,64.3115552182056,0.));
#105781=CARTESIAN_POINT('Ctrl Pts',(34.8329326055916,64.3115552182056,12.));
#105782=CARTESIAN_POINT('Ctrl Pts',(34.8356923246617,64.3374140827708,0.));
#105783=CARTESIAN_POINT('Ctrl Pts',(34.8356923246617,64.3374140827708,12.));
#105784=CARTESIAN_POINT('Ctrl Pts',(34.8384318759249,64.3633133635385,0.));
#105785=CARTESIAN_POINT('Ctrl Pts',(34.8384318759249,64.3633133635385,12.));
#105786=CARTESIAN_POINT('Ctrl Pts',(34.8411511979705,64.3892529685614,0.));
#105787=CARTESIAN_POINT('Ctrl Pts',(34.8411511979705,64.3892529685614,12.));
#105788=CARTESIAN_POINT('Ctrl Pts',(34.8438502296669,64.4152328061526,0.));
#105789=CARTESIAN_POINT('Ctrl Pts',(34.8438502296669,64.4152328061526,12.));
#105790=CARTESIAN_POINT('Ctrl Pts',(34.8465289101626,64.4412527848979,0.));
#105791=CARTESIAN_POINT('Ctrl Pts',(34.8465289101626,64.4412527848979,12.));
#105792=CARTESIAN_POINT('Ctrl Pts',(34.8491871788898,64.4673128136631,0.));
#105793=CARTESIAN_POINT('Ctrl Pts',(34.8491871788898,64.4673128136631,12.));
#105794=CARTESIAN_POINT('Ctrl Pts',(34.851824975568,64.4934128015983,0.));
#105795=CARTESIAN_POINT('Ctrl Pts',(34.851824975568,64.4934128015983,12.));
#105796=CARTESIAN_POINT('Ctrl Pts',(34.8544422402114,64.5195526581398,0.));
#105797=CARTESIAN_POINT('Ctrl Pts',(34.8544422402114,64.5195526581398,12.));
#105798=CARTESIAN_POINT('Ctrl Pts',(34.8570389131334,64.5457322930074,0.));
#105799=CARTESIAN_POINT('Ctrl Pts',(34.8570389131334,64.5457322930074,12.));
#105800=CARTESIAN_POINT('Ctrl Pts',(34.859614934925,64.5719516161914,0.));
#105801=CARTESIAN_POINT('Ctrl Pts',(34.859614934925,64.5719516161914,12.));
#105802=CARTESIAN_POINT('Ctrl Pts',(34.8621702464397,64.5982105379374,0.));
#105803=CARTESIAN_POINT('Ctrl Pts',(34.8621702464397,64.5982105379374,12.));
#105804=CARTESIAN_POINT('Ctrl Pts',(34.8647047887774,64.6245089687276,0.));
#105805=CARTESIAN_POINT('Ctrl Pts',(34.8647047887774,64.6245089687276,12.));
#105806=CARTESIAN_POINT('Ctrl Pts',(34.8672185032724,64.6508468192609,0.));
#105807=CARTESIAN_POINT('Ctrl Pts',(34.8672185032724,64.6508468192609,12.));
#105808=CARTESIAN_POINT('Ctrl Pts',(34.8697113314797,64.6772240004241,0.));
#105809=CARTESIAN_POINT('Ctrl Pts',(34.8697113314797,64.6772240004241,12.));
#105810=CARTESIAN_POINT('Ctrl Pts',(34.8721832151981,64.7036404233319,0.));
#105811=CARTESIAN_POINT('Ctrl Pts',(34.8721832151981,64.7036404233319,12.));
#105812=CARTESIAN_POINT('Ctrl Pts',(34.8746340964976,64.7300959993662,0.));
#105813=CARTESIAN_POINT('Ctrl Pts',(34.8746340964976,64.7300959993662,12.));
#105814=CARTESIAN_POINT('Ctrl Pts',(34.8770639177494,64.7565906402154,0.));
#105815=CARTESIAN_POINT('Ctrl Pts',(34.8770639177494,64.7565906402154,12.));
#105816=CARTESIAN_POINT('Ctrl Pts',(34.8794726216511,64.7831242579023,0.));
#105817=CARTESIAN_POINT('Ctrl Pts',(34.8794726216511,64.7831242579023,12.));
#105818=CARTESIAN_POINT('Ctrl Pts',(34.8818601512726,64.8096967648299,0.));
#105819=CARTESIAN_POINT('Ctrl Pts',(34.8818601512726,64.8096967648299,12.));
#105820=CARTESIAN_POINT('Ctrl Pts',(34.8842264500184,64.8363080737369,0.));
#105821=CARTESIAN_POINT('Ctrl Pts',(34.8842264500184,64.8363080737369,12.));
#105822=CARTESIAN_POINT('Ctrl Pts',(34.8865714615433,64.8629580976057,0.));
#105823=CARTESIAN_POINT('Ctrl Pts',(34.8865714615433,64.8629580976057,12.));
#105824=CARTESIAN_POINT('Ctrl Pts',(34.8888951296809,64.8896467495755,0.));
#105825=CARTESIAN_POINT('Ctrl Pts',(34.8888951296809,64.8896467495755,12.));
#105826=CARTESIAN_POINT('Ctrl Pts',(34.8911973983785,64.9163739428606,0.));
#105827=CARTESIAN_POINT('Ctrl Pts',(34.8911973983785,64.9163739428606,12.));
#105828=CARTESIAN_POINT('Ctrl Pts',(34.8934782116097,64.9431395906341,0.));
#105829=CARTESIAN_POINT('Ctrl Pts',(34.8934782116097,64.9431395906341,12.));
#105830=CARTESIAN_POINT('Ctrl Pts',(34.8957375133702,64.9699436060178,0.));
#105831=CARTESIAN_POINT('Ctrl Pts',(34.8957375133702,64.9699436060178,12.));
#105832=CARTESIAN_POINT('Ctrl Pts',(34.8979752478623,64.9967859023225,0.));
#105833=CARTESIAN_POINT('Ctrl Pts',(34.8979752478623,64.9967859023225,12.));
#105834=CARTESIAN_POINT('Ctrl Pts',(34.9001913596422,65.0236663932338,0.));
#105835=CARTESIAN_POINT('Ctrl Pts',(34.9001913596422,65.0236663932338,12.));
#105836=CARTESIAN_POINT('Ctrl Pts',(34.9023857937866,65.0505849930173,0.));
#105837=CARTESIAN_POINT('Ctrl Pts',(34.9023857937866,65.0505849930173,12.));
#105838=CARTESIAN_POINT('Ctrl Pts',(34.9045584960503,65.0775416167073,0.));
#105839=CARTESIAN_POINT('Ctrl Pts',(34.9045584960503,65.0775416167073,12.));
#105840=CARTESIAN_POINT('Ctrl Pts',(34.9067094130387,65.1045361803097,0.));
#105841=CARTESIAN_POINT('Ctrl Pts',(34.9067094130387,65.1045361803097,12.));
#105842=CARTESIAN_POINT('Ctrl Pts',(34.9088384918321,65.1315686003485,0.));
#105843=CARTESIAN_POINT('Ctrl Pts',(34.9088384918321,65.1315686003485,12.));
#105844=CARTESIAN_POINT('Ctrl Pts',(34.9109456796201,65.1586387934216,0.));
#105845=CARTESIAN_POINT('Ctrl Pts',(34.9109456796201,65.1586387934216,12.));
#105846=CARTESIAN_POINT('Ctrl Pts',(34.9130309233017,65.1857466757082,0.));
#105847=CARTESIAN_POINT('Ctrl Pts',(34.9130309233017,65.1857466757082,12.));
#105848=CARTESIAN_POINT('Ctrl Pts',(34.9150941691754,65.2128921625838,0.));
#105849=CARTESIAN_POINT('Ctrl Pts',(34.9150941691754,65.2128921625838,12.));
#105850=CARTESIAN_POINT('Ctrl Pts',(34.9171353624131,65.2400751679586,0.));
#105851=CARTESIAN_POINT('Ctrl Pts',(34.9171353624131,65.2400751679586,12.));
#105852=CARTESIAN_POINT('Ctrl Pts',(34.9191544474898,65.2672956048121,0.));
#105853=CARTESIAN_POINT('Ctrl Pts',(34.9191544474898,65.2672956048121,12.));
#105854=CARTESIAN_POINT('Ctrl Pts',(34.921151369138,65.2945533863812,0.));
#105855=CARTESIAN_POINT('Ctrl Pts',(34.921151369138,65.2945533863812,12.));
#105856=CARTESIAN_POINT('Ctrl Pts',(34.9231260731846,65.3218484271941,0.));
#105857=CARTESIAN_POINT('Ctrl Pts',(34.9231260731846,65.3218484271941,12.));
#105858=CARTESIAN_POINT('Ctrl Pts',(34.9250785073473,65.3491806440529,0.));
#105859=CARTESIAN_POINT('Ctrl Pts',(34.9250785073473,65.3491806440529,12.));
#105860=CARTESIAN_POINT('Ctrl Pts',(34.9270086222703,65.3765499573019,0.));
#105861=CARTESIAN_POINT('Ctrl Pts',(34.9270086222703,65.3765499573019,12.));
#105862=CARTESIAN_POINT('Ctrl Pts',(34.92891637177,65.4039562911255,0.));
#105863=CARTESIAN_POINT('Ctrl Pts',(34.92891637177,65.4039562911255,12.));
#105864=CARTESIAN_POINT('Ctrl Pts',(34.9308017105481,65.4313995707423,0.));
#105865=CARTESIAN_POINT('Ctrl Pts',(34.9308017105481,65.4313995707423,12.));
#105866=CARTESIAN_POINT('Ctrl Pts',(34.9326645923897,65.4588797201884,0.));
#105867=CARTESIAN_POINT('Ctrl Pts',(34.9326645923897,65.4588797201884,12.));
#105868=CARTESIAN_POINT('Ctrl Pts',(34.9345049680816,65.4863966597524,0.));
#105869=CARTESIAN_POINT('Ctrl Pts',(34.9345049680816,65.4863966597524,12.));
#105870=CARTESIAN_POINT('Ctrl Pts',(34.9363227836621,65.5139503038116,0.));
#105871=CARTESIAN_POINT('Ctrl Pts',(34.9363227836621,65.5139503038116,12.));
#105872=CARTESIAN_POINT('Ctrl Pts',(34.9381179779763,65.5415405578138,0.));
#105873=CARTESIAN_POINT('Ctrl Pts',(34.9381179779763,65.5415405578138,12.));
#105874=CARTESIAN_POINT('Ctrl Pts',(34.9398904862278,65.5691673226051,0.));
#105875=CARTESIAN_POINT('Ctrl Pts',(34.9398904862278,65.5691673226051,12.));
#105876=CARTESIAN_POINT('Ctrl Pts',(34.9416402443551,65.5968304997821,0.));
#105877=CARTESIAN_POINT('Ctrl Pts',(34.9416402443551,65.5968304997821,12.));
#105878=CARTESIAN_POINT('Ctrl Pts',(34.9433671932982,65.6245299968635,0.));
#105879=CARTESIAN_POINT('Ctrl Pts',(34.9433671932982,65.6245299968635,12.));
#105880=CARTESIAN_POINT('Ctrl Pts',(34.9450712829142,65.652265732124,0.));
#105881=CARTESIAN_POINT('Ctrl Pts',(34.9450712829142,65.652265732124,12.));
#105882=CARTESIAN_POINT('Ctrl Pts',(34.9467524770271,65.6800376405722,0.));
#105883=CARTESIAN_POINT('Ctrl Pts',(34.9467524770271,65.6800376405722,12.));
#105884=CARTESIAN_POINT('Ctrl Pts',(34.9484107543857,65.707845675746,0.));
#105885=CARTESIAN_POINT('Ctrl Pts',(34.9484107543857,65.707845675746,12.));
#105886=CARTESIAN_POINT('Ctrl Pts',(34.9500461042919,65.7356898060478,0.));
#105887=CARTESIAN_POINT('Ctrl Pts',(34.9500461042919,65.7356898060478,12.));
#105888=CARTESIAN_POINT('Ctrl Pts',(34.9513360397181,65.757993971173,0.));
#105889=CARTESIAN_POINT('Ctrl Pts',(34.9513360397181,65.757993971173,12.));
#105890=CARTESIAN_POINT('Ctrl Pts',(34.9522931728594,65.7747383250775,0.));
#105891=CARTESIAN_POINT('Ctrl Pts',(34.9522931728594,65.7747383250775,12.));
#105892=CARTESIAN_POINT('Ctrl Pts',(34.9529266758405,65.7859084407494,0.));
#105893=CARTESIAN_POINT('Ctrl Pts',(34.9529266758405,65.7859084407494,12.));
#105894=CARTESIAN_POINT('Ctrl Pts',(34.9532422808861,65.7914953018525,0.));
#105895=CARTESIAN_POINT('Ctrl Pts',(34.9532422808861,65.7914953018525,12.));
#105896=CARTESIAN_POINT('',(34.2579614092497,61.0441813777723,0.));
#105897=CARTESIAN_POINT('Ctrl Pts',(34.2579614092497,61.0441813777723,0.));
#105898=CARTESIAN_POINT('Ctrl Pts',(34.2589297755434,61.0479423318725,0.));
#105899=CARTESIAN_POINT('Ctrl Pts',(34.2608658001631,61.0554700176998,0.));
#105900=CARTESIAN_POINT('Ctrl Pts',(34.2637677131934,61.0667788793266,0.));
#105901=CARTESIAN_POINT('Ctrl Pts',(34.2676326825626,61.0818920286293,0.));
#105902=CARTESIAN_POINT('Ctrl Pts',(34.2724568037227,61.1008412399997,0.));
#105903=CARTESIAN_POINT('Ctrl Pts',(34.277273803877,61.1198481997764,0.));
#105904=CARTESIAN_POINT('Ctrl Pts',(34.2820836244469,61.1389128461886,0.));
#105905=CARTESIAN_POINT('Ctrl Pts',(34.2868861666384,61.1580350635533,0.));
#105906=CARTESIAN_POINT('Ctrl Pts',(34.2916812929751,61.1772146833205,0.));
#105907=CARTESIAN_POINT('Ctrl Pts',(34.2964688443663,61.1964515073891,0.));
#105908=CARTESIAN_POINT('Ctrl Pts',(34.3012486533474,61.2157453259107,0.));
#105909=CARTESIAN_POINT('Ctrl Pts',(34.3060205584064,61.2350959366939,0.));
#105910=CARTESIAN_POINT('Ctrl Pts',(34.3107844191043,61.2545031656133,0.));
#105911=CARTESIAN_POINT('Ctrl Pts',(34.3155401111747,61.2739668600365,0.));
#105912=CARTESIAN_POINT('Ctrl Pts',(34.3202875193617,61.2934868791855,0.));
#105913=CARTESIAN_POINT('Ctrl Pts',(34.3250265314768,61.3130630861386,0.));
#105914=CARTESIAN_POINT('Ctrl Pts',(34.3297570310146,61.3326953378851,0.));
#105915=CARTESIAN_POINT('Ctrl Pts',(34.3344788934363,61.3523834803188,0.));
#105916=CARTESIAN_POINT('Ctrl Pts',(34.339191990014,61.3721273534257,0.));
#105917=CARTESIAN_POINT('Ctrl Pts',(34.3438961902405,61.3919267945302,0.));
#105918=CARTESIAN_POINT('Ctrl Pts',(34.3485913645979,61.4117816420229,0.));
#105919=CARTESIAN_POINT('Ctrl Pts',(34.3532773877089,61.4316917395918,0.));
#105920=CARTESIAN_POINT('Ctrl Pts',(34.3579541381996,61.4516569360454,0.));
#105921=CARTESIAN_POINT('Ctrl Pts',(34.3626214971888,61.4716770832897,0.));
#105922=CARTESIAN_POINT('Ctrl Pts',(34.3672793472465,61.4917520349278,0.));
#105923=CARTESIAN_POINT('Ctrl Pts',(34.3719275711195,61.5118816445437,0.));
#105924=CARTESIAN_POINT('Ctrl Pts',(34.376566050668,61.5320657642638,0.));
#105925=CARTESIAN_POINT('Ctrl Pts',(34.3811946674197,61.5523042455158,0.));
#105926=CARTESIAN_POINT('Ctrl Pts',(34.3858133030518,61.5725969396829,0.));
#105927=CARTESIAN_POINT('Ctrl Pts',(34.3904218398636,61.5929436987409,0.));
#105928=CARTESIAN_POINT('Ctrl Pts',(34.3950201613432,61.6133443760142,0.));
#105929=CARTESIAN_POINT('Ctrl Pts',(34.3996081523753,61.6337988264556,0.));
#105930=CARTESIAN_POINT('Ctrl Pts',(34.4041856989316,61.6543069062416,0.));
#105931=CARTESIAN_POINT('Ctrl Pts',(34.4087526878812,61.6748684725205,0.));
#105932=CARTESIAN_POINT('Ctrl Pts',(34.4133090067703,61.695483383117,0.));
#105933=CARTESIAN_POINT('Ctrl Pts',(34.4178545435766,61.7161514961915,0.));
#105934=CARTESIAN_POINT('Ctrl Pts',(34.4223891867179,61.7368726702596,0.));
#105935=CARTESIAN_POINT('Ctrl Pts',(34.4269128251576,61.7576467643432,0.));
#105936=CARTESIAN_POINT('Ctrl Pts',(34.4314253484791,61.7784736380727,0.));
#105937=CARTESIAN_POINT('Ctrl Pts',(34.4359266469749,61.7993531518037,0.));
#105938=CARTESIAN_POINT('Ctrl Pts',(34.4404166117299,61.8202851667222,0.));
#105939=CARTESIAN_POINT('Ctrl Pts',(34.4448951345739,61.8412695447926,0.));
#105940=CARTESIAN_POINT('Ctrl Pts',(34.449362108036,61.8623061487018,0.));
#105941=CARTESIAN_POINT('Ctrl Pts',(34.4538174253012,61.8833948418025,0.));
#105942=CARTESIAN_POINT('Ctrl Pts',(34.4582609801637,61.9045354880445,0.));
#105943=CARTESIAN_POINT('Ctrl Pts',(34.4626926669974,61.9257279519308,0.));
#105944=CARTESIAN_POINT('Ctrl Pts',(34.4671123807717,61.9469720985531,0.));
#105945=CARTESIAN_POINT('Ctrl Pts',(34.4715200170592,61.9682677936054,0.));
#105946=CARTESIAN_POINT('Ctrl Pts',(34.4759154720473,61.9896149034001,0.));
#105947=CARTESIAN_POINT('Ctrl Pts',(34.4802986425528,62.0110132948794,0.));
#105948=CARTESIAN_POINT('Ctrl Pts',(34.4846694260199,62.0324628356141,0.));
#105949=CARTESIAN_POINT('Ctrl Pts',(34.4890277205039,62.0539633937939,0.));
#105950=CARTESIAN_POINT('Ctrl Pts',(34.4933734246592,62.0755148382135,0.));
#105951=CARTESIAN_POINT('Ctrl Pts',(34.4977064377282,62.0971170382567,0.));
#105952=CARTESIAN_POINT('Ctrl Pts',(34.5020266595293,62.1187698638707,0.));
#105953=CARTESIAN_POINT('Ctrl Pts',(34.5063339904533,62.1404731855687,0.));
#105954=CARTESIAN_POINT('Ctrl Pts',(34.5106283314594,62.1622268744337,0.));
#105955=CARTESIAN_POINT('Ctrl Pts',(34.5149095840729,62.1840308021171,0.));
#105956=CARTESIAN_POINT('Ctrl Pts',(34.5191776503843,62.2058848408346,0.));
#105957=CARTESIAN_POINT('Ctrl Pts',(34.5234324330492,62.2277888633576,0.));
#105958=CARTESIAN_POINT('Ctrl Pts',(34.527673835281,62.2497427430136,0.));
#105959=CARTESIAN_POINT('Ctrl Pts',(34.5319017608434,62.2717463536828,0.));
#105960=CARTESIAN_POINT('Ctrl Pts',(34.536116114045,62.2937995697927,0.));
#105961=CARTESIAN_POINT('Ctrl Pts',(34.5403167997333,62.3159022663052,0.));
#105962=CARTESIAN_POINT('Ctrl Pts',(34.5445037232928,62.3380543187067,0.));
#105963=CARTESIAN_POINT('Ctrl Pts',(34.5486767906376,62.3602556030114,0.));
#105964=CARTESIAN_POINT('Ctrl Pts',(34.552835908207,62.3825059957593,0.));
#105965=CARTESIAN_POINT('Ctrl Pts',(34.5569809829615,62.4048053740129,0.));
#105966=CARTESIAN_POINT('Ctrl Pts',(34.5611119223807,62.4271536153473,0.));
#105967=CARTESIAN_POINT('Ctrl Pts',(34.5652286344606,62.4495505978415,0.));
#105968=CARTESIAN_POINT('Ctrl Pts',(34.5693310277064,62.471996200083,0.));
#105969=CARTESIAN_POINT('Ctrl Pts',(34.5734190111279,62.494490301164,0.));
#105970=CARTESIAN_POINT('Ctrl Pts',(34.5774924942351,62.5170327806774,0.));
#105971=CARTESIAN_POINT('Ctrl Pts',(34.5815513870363,62.5396235187053,0.));
#105972=CARTESIAN_POINT('Ctrl Pts',(34.5855956000343,62.5622623958125,0.));
#105973=CARTESIAN_POINT('Ctrl Pts',(34.5896250442199,62.5849492930501,0.));
#105974=CARTESIAN_POINT('Ctrl Pts',(34.5936396310671,62.6076840919521,0.));
#105975=CARTESIAN_POINT('Ctrl Pts',(34.5976392725303,62.6304666745319,0.));
#105976=CARTESIAN_POINT('Ctrl Pts',(34.6016238810419,62.6532969232695,0.));
#105977=CARTESIAN_POINT('Ctrl Pts',(34.6055933695093,62.6761747211081,0.));
#105978=CARTESIAN_POINT('Ctrl Pts',(34.6095476513095,62.6990999514597,0.));
#105979=CARTESIAN_POINT('Ctrl Pts',(34.6134866402842,62.7220724982005,0.));
#105980=CARTESIAN_POINT('Ctrl Pts',(34.6174102507368,62.7450922456662,0.));
#105981=CARTESIAN_POINT('Ctrl Pts',(34.6213183974302,62.7681590786398,0.));
#105982=CARTESIAN_POINT('Ctrl Pts',(34.6252109955836,62.7912728823483,0.));
#105983=CARTESIAN_POINT('Ctrl Pts',(34.629087960866,62.8144335424671,0.));
#105984=CARTESIAN_POINT('Ctrl Pts',(34.6329492093931,62.8376409451167,0.));
#105985=CARTESIAN_POINT('Ctrl Pts',(34.6367946577241,62.8608949768583,0.));
#105986=CARTESIAN_POINT('Ctrl Pts',(34.6406242228606,62.8841955246819,0.));
#105987=CARTESIAN_POINT('Ctrl Pts',(34.6444378222425,62.9075424760042,0.));
#105988=CARTESIAN_POINT('Ctrl Pts',(34.6482353737433,62.9309357186733,0.));
#105989=CARTESIAN_POINT('Ctrl Pts',(34.6520167956656,62.9543751409648,0.));
#105990=CARTESIAN_POINT('Ctrl Pts',(34.6557820067389,62.9778606315777,0.));
#105991=CARTESIAN_POINT('Ctrl Pts',(34.6595309261185,63.0013920796225,0.));
#105992=CARTESIAN_POINT('Ctrl Pts',(34.6632634733819,63.0249693746198,0.));
#105993=CARTESIAN_POINT('Ctrl Pts',(34.6669795685225,63.0485924065039,0.));
#105994=CARTESIAN_POINT('Ctrl Pts',(34.670679131947,63.0722610656194,0.));
#105995=CARTESIAN_POINT('Ctrl Pts',(34.6743620844721,63.0959752427169,0.));
#105996=CARTESIAN_POINT('Ctrl Pts',(34.6780283473252,63.119734828943,0.));
#105997=CARTESIAN_POINT('Ctrl Pts',(34.68167784214,63.1435397158385,0.));
#105998=CARTESIAN_POINT('Ctrl Pts',(34.6853104909516,63.1673897953425,0.));
#105999=CARTESIAN_POINT('Ctrl Pts',(34.6889262161923,63.1912849597885,0.));
#106000=CARTESIAN_POINT('Ctrl Pts',(34.6925249406898,63.2152251019014,0.));
#106001=CARTESIAN_POINT('Ctrl Pts',(34.696106587667,63.2392101147854,0.));
#106002=CARTESIAN_POINT('Ctrl Pts',(34.6996710807384,63.2632398919234,0.));
#106003=CARTESIAN_POINT('Ctrl Pts',(34.7032183439045,63.2873143271813,0.));
#106004=CARTESIAN_POINT('Ctrl Pts',(34.7067483015492,63.311433314805,0.));
#106005=CARTESIAN_POINT('Ctrl Pts',(34.7102608784372,63.3355967494169,0.));
#106006=CARTESIAN_POINT('Ctrl Pts',(34.7137559997143,63.359804526005,0.));
#106007=CARTESIAN_POINT('Ctrl Pts',(34.7172335909037,63.3840565399207,0.));
#106008=CARTESIAN_POINT('Ctrl Pts',(34.7206935779007,63.4083526868837,0.));
#106009=CARTESIAN_POINT('Ctrl Pts',(34.7241358869702,63.4326928629797,0.));
#106010=CARTESIAN_POINT('Ctrl Pts',(34.7275604447438,63.4570769646568,0.));
#106011=CARTESIAN_POINT('Ctrl Pts',(34.7309671782212,63.481504888716,0.));
#106012=CARTESIAN_POINT('Ctrl Pts',(34.7343560147663,63.5059765323082,0.));
#106013=CARTESIAN_POINT('Ctrl Pts',(34.7377268821022,63.5304917929378,0.));
#106014=CARTESIAN_POINT('Ctrl Pts',(34.7410797083079,63.5550505684621,0.));
#106015=CARTESIAN_POINT('Ctrl Pts',(34.7444144218162,63.5796527570874,0.));
#106016=CARTESIAN_POINT('Ctrl Pts',(34.7477309514142,63.6042982573599,0.));
#106017=CARTESIAN_POINT('Ctrl Pts',(34.7510292262415,63.628986968162,0.));
#106018=CARTESIAN_POINT('Ctrl Pts',(34.7543091757841,63.6537187887174,0.));
#106019=CARTESIAN_POINT('Ctrl Pts',(34.7575707298718,63.6784936185893,0.));
#106020=CARTESIAN_POINT('Ctrl Pts',(34.7608138186757,63.7033113576782,0.));
#106021=CARTESIAN_POINT('Ctrl Pts',(34.7640383727094,63.7281719062135,0.));
#106022=CARTESIAN_POINT('Ctrl Pts',(34.7672443228266,63.7530751647479,0.));
#106023=CARTESIAN_POINT('Ctrl Pts',(34.7704316002165,63.7780210341619,0.));
#106024=CARTESIAN_POINT('Ctrl Pts',(34.7736001363991,63.8030094156635,0.));
#106025=CARTESIAN_POINT('Ctrl Pts',(34.7767498632244,63.8280402107858,0.));
#106026=CARTESIAN_POINT('Ctrl Pts',(34.7798807128716,63.8531133213794,0.));
#106027=CARTESIAN_POINT('Ctrl Pts',(34.7829926178495,63.8782286496059,0.));
#106028=CARTESIAN_POINT('Ctrl Pts',(34.7860855109908,63.9033860979429,0.));
#106029=CARTESIAN_POINT('Ctrl Pts',(34.7891593254485,63.9285855691839,0.));
#106030=CARTESIAN_POINT('Ctrl Pts',(34.7922139946943,63.9538269664366,0.));
#106031=CARTESIAN_POINT('Ctrl Pts',(34.7952494525182,63.9791101931169,0.));
#106032=CARTESIAN_POINT('Ctrl Pts',(34.79826563303,64.0044351529413,0.));
#106033=CARTESIAN_POINT('Ctrl Pts',(34.8012624706533,64.0298017499305,0.));
#106034=CARTESIAN_POINT('Ctrl Pts',(34.8042399001214,64.0552098884101,0.));
#106035=CARTESIAN_POINT('Ctrl Pts',(34.8071978564748,64.0806594730085,0.));
#106036=CARTESIAN_POINT('Ctrl Pts',(34.8101362750595,64.1061504086512,0.));
#106037=CARTESIAN_POINT('Ctrl Pts',(34.8130550915284,64.1316826005502,0.));
#106038=CARTESIAN_POINT('Ctrl Pts',(34.8159542418372,64.1572559542085,0.));
#106039=CARTESIAN_POINT('Ctrl Pts',(34.8188336622418,64.1828703754237,0.));
#106040=CARTESIAN_POINT('Ctrl Pts',(34.8216932892969,64.2085257702885,0.));
#106041=CARTESIAN_POINT('Ctrl Pts',(34.8245330598559,64.2342220451878,0.));
#106042=CARTESIAN_POINT('Ctrl Pts',(34.8273529110742,64.259959106791,0.));
#106043=CARTESIAN_POINT('Ctrl Pts',(34.8301527804052,64.2857368620513,0.));
#106044=CARTESIAN_POINT('Ctrl Pts',(34.8329326055916,64.3115552182056,0.));
#106045=CARTESIAN_POINT('Ctrl Pts',(34.8356923246617,64.3374140827708,0.));
#106046=CARTESIAN_POINT('Ctrl Pts',(34.8384318759249,64.3633133635385,0.));
#106047=CARTESIAN_POINT('Ctrl Pts',(34.8411511979705,64.3892529685614,0.));
#106048=CARTESIAN_POINT('Ctrl Pts',(34.8438502296669,64.4152328061526,0.));
#106049=CARTESIAN_POINT('Ctrl Pts',(34.8465289101626,64.4412527848979,0.));
#106050=CARTESIAN_POINT('Ctrl Pts',(34.8491871788898,64.4673128136631,0.));
#106051=CARTESIAN_POINT('Ctrl Pts',(34.851824975568,64.4934128015983,0.));
#106052=CARTESIAN_POINT('Ctrl Pts',(34.8544422402114,64.5195526581398,0.));
#106053=CARTESIAN_POINT('Ctrl Pts',(34.8570389131334,64.5457322930074,0.));
#106054=CARTESIAN_POINT('Ctrl Pts',(34.859614934925,64.5719516161914,0.));
#106055=CARTESIAN_POINT('Ctrl Pts',(34.8621702464397,64.5982105379374,0.));
#106056=CARTESIAN_POINT('Ctrl Pts',(34.8647047887774,64.6245089687276,0.));
#106057=CARTESIAN_POINT('Ctrl Pts',(34.8672185032724,64.6508468192609,0.));
#106058=CARTESIAN_POINT('Ctrl Pts',(34.8697113314797,64.6772240004241,0.));
#106059=CARTESIAN_POINT('Ctrl Pts',(34.8721832151981,64.7036404233319,0.));
#106060=CARTESIAN_POINT('Ctrl Pts',(34.8746340964976,64.7300959993662,0.));
#106061=CARTESIAN_POINT('Ctrl Pts',(34.8770639177494,64.7565906402154,0.));
#106062=CARTESIAN_POINT('Ctrl Pts',(34.8794726216511,64.7831242579023,0.));
#106063=CARTESIAN_POINT('Ctrl Pts',(34.8818601512726,64.8096967648299,0.));
#106064=CARTESIAN_POINT('Ctrl Pts',(34.8842264500184,64.8363080737369,0.));
#106065=CARTESIAN_POINT('Ctrl Pts',(34.8865714615433,64.8629580976057,0.));
#106066=CARTESIAN_POINT('Ctrl Pts',(34.8888951296809,64.8896467495755,0.));
#106067=CARTESIAN_POINT('Ctrl Pts',(34.8911973983785,64.9163739428606,0.));
#106068=CARTESIAN_POINT('Ctrl Pts',(34.8934782116097,64.9431395906341,0.));
#106069=CARTESIAN_POINT('Ctrl Pts',(34.8957375133702,64.9699436060178,0.));
#106070=CARTESIAN_POINT('Ctrl Pts',(34.8979752478623,64.9967859023225,0.));
#106071=CARTESIAN_POINT('Ctrl Pts',(34.9001913596422,65.0236663932338,0.));
#106072=CARTESIAN_POINT('Ctrl Pts',(34.9023857937866,65.0505849930173,0.));
#106073=CARTESIAN_POINT('Ctrl Pts',(34.9045584960503,65.0775416167073,0.));
#106074=CARTESIAN_POINT('Ctrl Pts',(34.9067094130387,65.1045361803097,0.));
#106075=CARTESIAN_POINT('Ctrl Pts',(34.9088384918321,65.1315686003485,0.));
#106076=CARTESIAN_POINT('Ctrl Pts',(34.9109456796201,65.1586387934216,0.));
#106077=CARTESIAN_POINT('Ctrl Pts',(34.9130309233017,65.1857466757082,0.));
#106078=CARTESIAN_POINT('Ctrl Pts',(34.9150941691754,65.2128921625838,0.));
#106079=CARTESIAN_POINT('Ctrl Pts',(34.9171353624131,65.2400751679586,0.));
#106080=CARTESIAN_POINT('Ctrl Pts',(34.9191544474898,65.2672956048121,0.));
#106081=CARTESIAN_POINT('Ctrl Pts',(34.921151369138,65.2945533863812,0.));
#106082=CARTESIAN_POINT('Ctrl Pts',(34.9231260731846,65.3218484271941,0.));
#106083=CARTESIAN_POINT('Ctrl Pts',(34.9250785073473,65.3491806440529,0.));
#106084=CARTESIAN_POINT('Ctrl Pts',(34.9270086222703,65.3765499573019,0.));
#106085=CARTESIAN_POINT('Ctrl Pts',(34.92891637177,65.4039562911255,0.));
#106086=CARTESIAN_POINT('Ctrl Pts',(34.9305324724386,65.4274804996405,0.));
#106087=CARTESIAN_POINT('Ctrl Pts',(34.9317593813102,65.4455359574998,0.));
#106088=CARTESIAN_POINT('Ctrl Pts',(34.9326070346591,65.4581063193582,0.));
#106089=CARTESIAN_POINT('Ctrl Pts',(34.9330820191483,65.4651808010449,0.));
#106090=CARTESIAN_POINT('Ctrl Pts',(34.9331875523085,65.4667541477953,0.));
#106091=CARTESIAN_POINT('',(34.2579614092497,61.0441813777723,12.));
#106092=CARTESIAN_POINT('',(34.2579614092497,61.0441813777723,0.));
#106093=CARTESIAN_POINT('Ctrl Pts',(34.9331875523085,65.4667541477952,12.));
#106094=CARTESIAN_POINT('Ctrl Pts',(34.9330820191483,65.4651808010449,12.));
#106095=CARTESIAN_POINT('Ctrl Pts',(34.9326070346591,65.4581063193582,12.));
#106096=CARTESIAN_POINT('Ctrl Pts',(34.9317593813102,65.4455359574998,12.));
#106097=CARTESIAN_POINT('Ctrl Pts',(34.9305324724386,65.4274804996405,12.));
#106098=CARTESIAN_POINT('Ctrl Pts',(34.92891637177,65.4039562911255,12.));
#106099=CARTESIAN_POINT('Ctrl Pts',(34.9270086222703,65.3765499573019,12.));
#106100=CARTESIAN_POINT('Ctrl Pts',(34.9250785073473,65.3491806440529,12.));
#106101=CARTESIAN_POINT('Ctrl Pts',(34.9231260731846,65.3218484271941,12.));
#106102=CARTESIAN_POINT('Ctrl Pts',(34.921151369138,65.2945533863812,12.));
#106103=CARTESIAN_POINT('Ctrl Pts',(34.9191544474898,65.2672956048121,12.));
#106104=CARTESIAN_POINT('Ctrl Pts',(34.9171353624131,65.2400751679586,12.));
#106105=CARTESIAN_POINT('Ctrl Pts',(34.9150941691754,65.2128921625838,12.));
#106106=CARTESIAN_POINT('Ctrl Pts',(34.9130309233017,65.1857466757082,12.));
#106107=CARTESIAN_POINT('Ctrl Pts',(34.9109456796201,65.1586387934216,12.));
#106108=CARTESIAN_POINT('Ctrl Pts',(34.9088384918321,65.1315686003485,12.));
#106109=CARTESIAN_POINT('Ctrl Pts',(34.9067094130387,65.1045361803097,12.));
#106110=CARTESIAN_POINT('Ctrl Pts',(34.9045584960503,65.0775416167073,12.));
#106111=CARTESIAN_POINT('Ctrl Pts',(34.9023857937866,65.0505849930173,12.));
#106112=CARTESIAN_POINT('Ctrl Pts',(34.9001913596422,65.0236663932338,12.));
#106113=CARTESIAN_POINT('Ctrl Pts',(34.8979752478623,64.9967859023225,12.));
#106114=CARTESIAN_POINT('Ctrl Pts',(34.8957375133702,64.9699436060178,12.));
#106115=CARTESIAN_POINT('Ctrl Pts',(34.8934782116097,64.9431395906341,12.));
#106116=CARTESIAN_POINT('Ctrl Pts',(34.8911973983785,64.9163739428606,12.));
#106117=CARTESIAN_POINT('Ctrl Pts',(34.8888951296809,64.8896467495755,12.));
#106118=CARTESIAN_POINT('Ctrl Pts',(34.8865714615433,64.8629580976057,12.));
#106119=CARTESIAN_POINT('Ctrl Pts',(34.8842264500184,64.8363080737369,12.));
#106120=CARTESIAN_POINT('Ctrl Pts',(34.8818601512726,64.8096967648299,12.));
#106121=CARTESIAN_POINT('Ctrl Pts',(34.8794726216511,64.7831242579023,12.));
#106122=CARTESIAN_POINT('Ctrl Pts',(34.8770639177494,64.7565906402154,12.));
#106123=CARTESIAN_POINT('Ctrl Pts',(34.8746340964976,64.7300959993662,12.));
#106124=CARTESIAN_POINT('Ctrl Pts',(34.8721832151981,64.7036404233319,12.));
#106125=CARTESIAN_POINT('Ctrl Pts',(34.8697113314797,64.6772240004241,12.));
#106126=CARTESIAN_POINT('Ctrl Pts',(34.8672185032724,64.6508468192609,12.));
#106127=CARTESIAN_POINT('Ctrl Pts',(34.8647047887774,64.6245089687276,12.));
#106128=CARTESIAN_POINT('Ctrl Pts',(34.8621702464397,64.5982105379374,12.));
#106129=CARTESIAN_POINT('Ctrl Pts',(34.859614934925,64.5719516161914,12.));
#106130=CARTESIAN_POINT('Ctrl Pts',(34.8570389131334,64.5457322930074,12.));
#106131=CARTESIAN_POINT('Ctrl Pts',(34.8544422402114,64.5195526581398,12.));
#106132=CARTESIAN_POINT('Ctrl Pts',(34.851824975568,64.4934128015983,12.));
#106133=CARTESIAN_POINT('Ctrl Pts',(34.8491871788898,64.4673128136631,12.));
#106134=CARTESIAN_POINT('Ctrl Pts',(34.8465289101626,64.4412527848979,12.));
#106135=CARTESIAN_POINT('Ctrl Pts',(34.8438502296669,64.4152328061526,12.));
#106136=CARTESIAN_POINT('Ctrl Pts',(34.8411511979705,64.3892529685614,12.));
#106137=CARTESIAN_POINT('Ctrl Pts',(34.8384318759249,64.3633133635385,12.));
#106138=CARTESIAN_POINT('Ctrl Pts',(34.8356923246617,64.3374140827708,12.));
#106139=CARTESIAN_POINT('Ctrl Pts',(34.8329326055916,64.3115552182056,12.));
#106140=CARTESIAN_POINT('Ctrl Pts',(34.8301527804052,64.2857368620513,12.));
#106141=CARTESIAN_POINT('Ctrl Pts',(34.8273529110742,64.259959106791,12.));
#106142=CARTESIAN_POINT('Ctrl Pts',(34.8245330598559,64.2342220451878,12.));
#106143=CARTESIAN_POINT('Ctrl Pts',(34.8216932892969,64.2085257702885,12.));
#106144=CARTESIAN_POINT('Ctrl Pts',(34.8188336622418,64.1828703754237,12.));
#106145=CARTESIAN_POINT('Ctrl Pts',(34.8159542418372,64.1572559542085,12.));
#106146=CARTESIAN_POINT('Ctrl Pts',(34.8130550915284,64.1316826005502,12.));
#106147=CARTESIAN_POINT('Ctrl Pts',(34.8101362750595,64.1061504086512,12.));
#106148=CARTESIAN_POINT('Ctrl Pts',(34.8071978564748,64.0806594730085,12.));
#106149=CARTESIAN_POINT('Ctrl Pts',(34.8042399001214,64.0552098884101,12.));
#106150=CARTESIAN_POINT('Ctrl Pts',(34.8012624706533,64.0298017499305,12.));
#106151=CARTESIAN_POINT('Ctrl Pts',(34.79826563303,64.0044351529413,12.));
#106152=CARTESIAN_POINT('Ctrl Pts',(34.7952494525182,63.9791101931169,12.));
#106153=CARTESIAN_POINT('Ctrl Pts',(34.7922139946943,63.9538269664366,12.));
#106154=CARTESIAN_POINT('Ctrl Pts',(34.7891593254485,63.9285855691839,12.));
#106155=CARTESIAN_POINT('Ctrl Pts',(34.7860855109908,63.9033860979429,12.));
#106156=CARTESIAN_POINT('Ctrl Pts',(34.7829926178495,63.8782286496059,12.));
#106157=CARTESIAN_POINT('Ctrl Pts',(34.7798807128716,63.8531133213794,12.));
#106158=CARTESIAN_POINT('Ctrl Pts',(34.7767498632244,63.8280402107858,12.));
#106159=CARTESIAN_POINT('Ctrl Pts',(34.7736001363991,63.8030094156635,12.));
#106160=CARTESIAN_POINT('Ctrl Pts',(34.7704316002165,63.7780210341619,12.));
#106161=CARTESIAN_POINT('Ctrl Pts',(34.7672443228266,63.7530751647479,12.));
#106162=CARTESIAN_POINT('Ctrl Pts',(34.7640383727094,63.7281719062135,12.));
#106163=CARTESIAN_POINT('Ctrl Pts',(34.7608138186757,63.7033113576782,12.));
#106164=CARTESIAN_POINT('Ctrl Pts',(34.7575707298718,63.6784936185893,12.));
#106165=CARTESIAN_POINT('Ctrl Pts',(34.7543091757841,63.6537187887174,12.));
#106166=CARTESIAN_POINT('Ctrl Pts',(34.7510292262415,63.628986968162,12.));
#106167=CARTESIAN_POINT('Ctrl Pts',(34.7477309514142,63.6042982573599,12.));
#106168=CARTESIAN_POINT('Ctrl Pts',(34.7444144218162,63.5796527570874,12.));
#106169=CARTESIAN_POINT('Ctrl Pts',(34.7410797083079,63.5550505684621,12.));
#106170=CARTESIAN_POINT('Ctrl Pts',(34.7377268821022,63.5304917929378,12.));
#106171=CARTESIAN_POINT('Ctrl Pts',(34.7343560147663,63.5059765323082,12.));
#106172=CARTESIAN_POINT('Ctrl Pts',(34.7309671782212,63.481504888716,12.));
#106173=CARTESIAN_POINT('Ctrl Pts',(34.7275604447438,63.4570769646568,12.));
#106174=CARTESIAN_POINT('Ctrl Pts',(34.7241358869702,63.4326928629797,12.));
#106175=CARTESIAN_POINT('Ctrl Pts',(34.7206935779007,63.4083526868837,12.));
#106176=CARTESIAN_POINT('Ctrl Pts',(34.7172335909037,63.3840565399207,12.));
#106177=CARTESIAN_POINT('Ctrl Pts',(34.7137559997143,63.359804526005,12.));
#106178=CARTESIAN_POINT('Ctrl Pts',(34.7102608784372,63.3355967494169,12.));
#106179=CARTESIAN_POINT('Ctrl Pts',(34.7067483015492,63.311433314805,12.));
#106180=CARTESIAN_POINT('Ctrl Pts',(34.7032183439045,63.2873143271813,12.));
#106181=CARTESIAN_POINT('Ctrl Pts',(34.6996710807384,63.2632398919234,12.));
#106182=CARTESIAN_POINT('Ctrl Pts',(34.696106587667,63.2392101147854,12.));
#106183=CARTESIAN_POINT('Ctrl Pts',(34.6925249406898,63.2152251019014,12.));
#106184=CARTESIAN_POINT('Ctrl Pts',(34.6889262161923,63.1912849597885,12.));
#106185=CARTESIAN_POINT('Ctrl Pts',(34.6853104909516,63.1673897953425,12.));
#106186=CARTESIAN_POINT('Ctrl Pts',(34.68167784214,63.1435397158385,12.));
#106187=CARTESIAN_POINT('Ctrl Pts',(34.6780283473252,63.119734828943,12.));
#106188=CARTESIAN_POINT('Ctrl Pts',(34.6743620844721,63.0959752427169,12.));
#106189=CARTESIAN_POINT('Ctrl Pts',(34.670679131947,63.0722610656194,12.));
#106190=CARTESIAN_POINT('Ctrl Pts',(34.6669795685225,63.0485924065039,12.));
#106191=CARTESIAN_POINT('Ctrl Pts',(34.6632634733819,63.0249693746198,12.));
#106192=CARTESIAN_POINT('Ctrl Pts',(34.6595309261185,63.0013920796225,12.));
#106193=CARTESIAN_POINT('Ctrl Pts',(34.6557820067389,62.9778606315777,12.));
#106194=CARTESIAN_POINT('Ctrl Pts',(34.6520167956656,62.9543751409648,12.));
#106195=CARTESIAN_POINT('Ctrl Pts',(34.6482353737433,62.9309357186733,12.));
#106196=CARTESIAN_POINT('Ctrl Pts',(34.6444378222425,62.9075424760042,12.));
#106197=CARTESIAN_POINT('Ctrl Pts',(34.6406242228606,62.8841955246819,12.));
#106198=CARTESIAN_POINT('Ctrl Pts',(34.6367946577241,62.8608949768583,12.));
#106199=CARTESIAN_POINT('Ctrl Pts',(34.6329492093931,62.8376409451167,12.));
#106200=CARTESIAN_POINT('Ctrl Pts',(34.629087960866,62.8144335424671,12.));
#106201=CARTESIAN_POINT('Ctrl Pts',(34.6252109955836,62.7912728823483,12.));
#106202=CARTESIAN_POINT('Ctrl Pts',(34.6213183974302,62.7681590786398,12.));
#106203=CARTESIAN_POINT('Ctrl Pts',(34.6174102507368,62.7450922456662,12.));
#106204=CARTESIAN_POINT('Ctrl Pts',(34.6134866402842,62.7220724982005,12.));
#106205=CARTESIAN_POINT('Ctrl Pts',(34.6095476513095,62.6990999514597,12.));
#106206=CARTESIAN_POINT('Ctrl Pts',(34.6055933695093,62.6761747211081,12.));
#106207=CARTESIAN_POINT('Ctrl Pts',(34.6016238810419,62.6532969232695,12.));
#106208=CARTESIAN_POINT('Ctrl Pts',(34.5976392725303,62.6304666745319,12.));
#106209=CARTESIAN_POINT('Ctrl Pts',(34.5936396310671,62.6076840919521,12.));
#106210=CARTESIAN_POINT('Ctrl Pts',(34.5896250442199,62.5849492930501,12.));
#106211=CARTESIAN_POINT('Ctrl Pts',(34.5855956000343,62.5622623958125,12.));
#106212=CARTESIAN_POINT('Ctrl Pts',(34.5815513870363,62.5396235187053,12.));
#106213=CARTESIAN_POINT('Ctrl Pts',(34.5774924942351,62.5170327806774,12.));
#106214=CARTESIAN_POINT('Ctrl Pts',(34.5734190111279,62.494490301164,12.));
#106215=CARTESIAN_POINT('Ctrl Pts',(34.5693310277064,62.471996200083,12.));
#106216=CARTESIAN_POINT('Ctrl Pts',(34.5652286344606,62.4495505978415,12.));
#106217=CARTESIAN_POINT('Ctrl Pts',(34.5611119223807,62.4271536153473,12.));
#106218=CARTESIAN_POINT('Ctrl Pts',(34.5569809829615,62.4048053740129,12.));
#106219=CARTESIAN_POINT('Ctrl Pts',(34.552835908207,62.3825059957593,12.));
#106220=CARTESIAN_POINT('Ctrl Pts',(34.5486767906376,62.3602556030114,12.));
#106221=CARTESIAN_POINT('Ctrl Pts',(34.5445037232928,62.3380543187067,12.));
#106222=CARTESIAN_POINT('Ctrl Pts',(34.5403167997333,62.3159022663052,12.));
#106223=CARTESIAN_POINT('Ctrl Pts',(34.536116114045,62.2937995697927,12.));
#106224=CARTESIAN_POINT('Ctrl Pts',(34.5319017608434,62.2717463536828,12.));
#106225=CARTESIAN_POINT('Ctrl Pts',(34.527673835281,62.2497427430136,12.));
#106226=CARTESIAN_POINT('Ctrl Pts',(34.5234324330492,62.2277888633576,12.));
#106227=CARTESIAN_POINT('Ctrl Pts',(34.5191776503843,62.2058848408346,12.));
#106228=CARTESIAN_POINT('Ctrl Pts',(34.5149095840729,62.1840308021171,12.));
#106229=CARTESIAN_POINT('Ctrl Pts',(34.5106283314594,62.1622268744337,12.));
#106230=CARTESIAN_POINT('Ctrl Pts',(34.5063339904533,62.1404731855687,12.));
#106231=CARTESIAN_POINT('Ctrl Pts',(34.5020266595293,62.1187698638707,12.));
#106232=CARTESIAN_POINT('Ctrl Pts',(34.4977064377282,62.0971170382567,12.));
#106233=CARTESIAN_POINT('Ctrl Pts',(34.4933734246592,62.0755148382135,12.));
#106234=CARTESIAN_POINT('Ctrl Pts',(34.4890277205039,62.0539633937939,12.));
#106235=CARTESIAN_POINT('Ctrl Pts',(34.4846694260199,62.0324628356141,12.));
#106236=CARTESIAN_POINT('Ctrl Pts',(34.4802986425528,62.0110132948794,12.));
#106237=CARTESIAN_POINT('Ctrl Pts',(34.4759154720473,61.9896149034001,12.));
#106238=CARTESIAN_POINT('Ctrl Pts',(34.4715200170592,61.9682677936054,12.));
#106239=CARTESIAN_POINT('Ctrl Pts',(34.4671123807717,61.9469720985531,12.));
#106240=CARTESIAN_POINT('Ctrl Pts',(34.4626926669974,61.9257279519308,12.));
#106241=CARTESIAN_POINT('Ctrl Pts',(34.4582609801637,61.9045354880445,12.));
#106242=CARTESIAN_POINT('Ctrl Pts',(34.4538174253012,61.8833948418025,12.));
#106243=CARTESIAN_POINT('Ctrl Pts',(34.449362108036,61.8623061487018,12.));
#106244=CARTESIAN_POINT('Ctrl Pts',(34.4448951345739,61.8412695447926,12.));
#106245=CARTESIAN_POINT('Ctrl Pts',(34.4404166117299,61.8202851667222,12.));
#106246=CARTESIAN_POINT('Ctrl Pts',(34.4359266469749,61.7993531518037,12.));
#106247=CARTESIAN_POINT('Ctrl Pts',(34.4314253484791,61.7784736380727,12.));
#106248=CARTESIAN_POINT('Ctrl Pts',(34.4269128251576,61.7576467643432,12.));
#106249=CARTESIAN_POINT('Ctrl Pts',(34.4223891867179,61.7368726702596,12.));
#106250=CARTESIAN_POINT('Ctrl Pts',(34.4178545435766,61.7161514961915,12.));
#106251=CARTESIAN_POINT('Ctrl Pts',(34.4133090067703,61.695483383117,12.));
#106252=CARTESIAN_POINT('Ctrl Pts',(34.4087526878812,61.6748684725205,12.));
#106253=CARTESIAN_POINT('Ctrl Pts',(34.4041856989316,61.6543069062416,12.));
#106254=CARTESIAN_POINT('Ctrl Pts',(34.3996081523753,61.6337988264556,12.));
#106255=CARTESIAN_POINT('Ctrl Pts',(34.3950201613432,61.6133443760142,12.));
#106256=CARTESIAN_POINT('Ctrl Pts',(34.3904218398636,61.5929436987409,12.));
#106257=CARTESIAN_POINT('Ctrl Pts',(34.3858133030518,61.5725969396829,12.));
#106258=CARTESIAN_POINT('Ctrl Pts',(34.3811946674197,61.5523042455158,12.));
#106259=CARTESIAN_POINT('Ctrl Pts',(34.376566050668,61.5320657642638,12.));
#106260=CARTESIAN_POINT('Ctrl Pts',(34.3719275711195,61.5118816445437,12.));
#106261=CARTESIAN_POINT('Ctrl Pts',(34.3672793472465,61.4917520349278,12.));
#106262=CARTESIAN_POINT('Ctrl Pts',(34.3626214971888,61.4716770832897,12.));
#106263=CARTESIAN_POINT('Ctrl Pts',(34.3579541381996,61.4516569360454,12.));
#106264=CARTESIAN_POINT('Ctrl Pts',(34.3532773877089,61.4316917395918,12.));
#106265=CARTESIAN_POINT('Ctrl Pts',(34.3485913645979,61.4117816420229,12.));
#106266=CARTESIAN_POINT('Ctrl Pts',(34.3438961902405,61.3919267945302,12.));
#106267=CARTESIAN_POINT('Ctrl Pts',(34.339191990014,61.3721273534257,12.));
#106268=CARTESIAN_POINT('Ctrl Pts',(34.3344788934363,61.3523834803188,12.));
#106269=CARTESIAN_POINT('Ctrl Pts',(34.3297570310146,61.3326953378851,12.));
#106270=CARTESIAN_POINT('Ctrl Pts',(34.3250265314768,61.3130630861386,12.));
#106271=CARTESIAN_POINT('Ctrl Pts',(34.3202875193617,61.2934868791855,12.));
#106272=CARTESIAN_POINT('Ctrl Pts',(34.3155401111747,61.2739668600365,12.));
#106273=CARTESIAN_POINT('Ctrl Pts',(34.3107844191043,61.2545031656133,12.));
#106274=CARTESIAN_POINT('Ctrl Pts',(34.3060205584064,61.2350959366939,12.));
#106275=CARTESIAN_POINT('Ctrl Pts',(34.3012486533474,61.2157453259107,12.));
#106276=CARTESIAN_POINT('Ctrl Pts',(34.2964688443663,61.1964515073891,12.));
#106277=CARTESIAN_POINT('Ctrl Pts',(34.2916812929751,61.1772146833205,12.));
#106278=CARTESIAN_POINT('Ctrl Pts',(34.2868861666384,61.1580350635533,12.));
#106279=CARTESIAN_POINT('Ctrl Pts',(34.2820836244469,61.1389128461886,12.));
#106280=CARTESIAN_POINT('Ctrl Pts',(34.277273803877,61.1198481997764,12.));
#106281=CARTESIAN_POINT('Ctrl Pts',(34.2724568037227,61.1008412399997,12.));
#106282=CARTESIAN_POINT('Ctrl Pts',(34.2676326825626,61.0818920286293,12.));
#106283=CARTESIAN_POINT('Ctrl Pts',(34.2637677131934,61.0667788793266,12.));
#106284=CARTESIAN_POINT('Ctrl Pts',(34.2608658001631,61.0554700176998,12.));
#106285=CARTESIAN_POINT('Ctrl Pts',(34.2589297755434,61.0479423318725,12.));
#106286=CARTESIAN_POINT('Ctrl Pts',(34.2579614092497,61.0441813777723,12.));
#106287=CARTESIAN_POINT('Ctrl Pts',(33.5903722665274,66.1657795405958,-1.11022302462516E-15));
#106288=CARTESIAN_POINT('Ctrl Pts',(33.5903722665274,66.1657795405958,4.));
#106289=CARTESIAN_POINT('Ctrl Pts',(33.5903722665274,66.1657795405958,8.));
#106290=CARTESIAN_POINT('Ctrl Pts',(33.5903722665274,66.1657795405958,12.));
#106291=CARTESIAN_POINT('Ctrl Pts',(33.6759628819914,66.2346881970577,-1.11022302462516E-15));
#106292=CARTESIAN_POINT('Ctrl Pts',(33.6759628819914,66.2346881970577,4.));
#106293=CARTESIAN_POINT('Ctrl Pts',(33.6759628819914,66.2346881970577,8.));
#106294=CARTESIAN_POINT('Ctrl Pts',(33.6759628819914,66.2346881970577,12.));
#106295=CARTESIAN_POINT('Ctrl Pts',(33.8665453669327,66.3036153738441,-1.11022302462516E-15));
#106296=CARTESIAN_POINT('Ctrl Pts',(33.8665453669327,66.3036153738441,4.00000000000001));
#106297=CARTESIAN_POINT('Ctrl Pts',(33.8665453669327,66.3036153738441,7.99999999999999));
#106298=CARTESIAN_POINT('Ctrl Pts',(33.8665453669327,66.3036153738441,12.));
#106299=CARTESIAN_POINT('Ctrl Pts',(34.0597557125855,66.2585076236399,-1.11022302462516E-15));
#106300=CARTESIAN_POINT('Ctrl Pts',(34.0597557125855,66.2585076236399,4.));
#106301=CARTESIAN_POINT('Ctrl Pts',(34.0597557125855,66.2585076236399,8.00000000000001));
#106302=CARTESIAN_POINT('Ctrl Pts',(34.0597557125855,66.2585076236399,12.));
#106303=CARTESIAN_POINT('Ctrl Pts',(34.1330090612009,66.220749712065,-1.11022302462516E-15));
#106304=CARTESIAN_POINT('Ctrl Pts',(34.1330090612009,66.220749712065,4.));
#106305=CARTESIAN_POINT('Ctrl Pts',(34.1330090612009,66.220749712065,8.));
#106306=CARTESIAN_POINT('Ctrl Pts',(34.1330090612009,66.220749712065,12.));
#106307=CARTESIAN_POINT('',(33.5903722665274,66.1657795405958,0.));
#106308=CARTESIAN_POINT('',(34.133009061201,66.2207497120651,0.));
#106309=CARTESIAN_POINT('Ctrl Pts',(33.5903722665274,66.1657795405958,0.));
#106310=CARTESIAN_POINT('Ctrl Pts',(33.6759628819914,66.2346881970577,-7.70371977754894E-31));
#106311=CARTESIAN_POINT('Ctrl Pts',(33.7848671591007,66.2740751552214,6.16297582203915E-31));
#106312=CARTESIAN_POINT('Ctrl Pts',(33.894629513177,66.2762262188575,3.08148791101958E-31));
#106313=CARTESIAN_POINT('Ctrl Pts',(33.9769512787343,66.2778395165845,-6.16297582203913E-32));
#106314=CARTESIAN_POINT('Ctrl Pts',(34.0597557125855,66.2585076236399,-1.4482993181792E-30));
#106315=CARTESIAN_POINT('Ctrl Pts',(34.1330090612009,66.220749712065,-6.16297582203914E-32));
#106316=CARTESIAN_POINT('',(34.133009061201,66.2207497120651,12.));
#106317=CARTESIAN_POINT('Ctrl Pts',(34.1330090612009,66.220749712065,-1.11022302462516E-15));
#106318=CARTESIAN_POINT('Ctrl Pts',(34.1330090612009,66.220749712065,4.));
#106319=CARTESIAN_POINT('Ctrl Pts',(34.1330090612009,66.220749712065,8.));
#106320=CARTESIAN_POINT('Ctrl Pts',(34.1330090612009,66.220749712065,12.));
#106321=CARTESIAN_POINT('',(33.5903722665274,66.1657795405958,12.));
#106322=CARTESIAN_POINT('Ctrl Pts',(34.1330090612009,66.220749712065,12.));
#106323=CARTESIAN_POINT('Ctrl Pts',(34.0597557125855,66.2585076236399,12.));
#106324=CARTESIAN_POINT('Ctrl Pts',(33.9769512787343,66.2778395165845,12.));
#106325=CARTESIAN_POINT('Ctrl Pts',(33.894629513177,66.2762262188575,12.));
#106326=CARTESIAN_POINT('Ctrl Pts',(33.7848671591007,66.2740751552214,12.));
#106327=CARTESIAN_POINT('Ctrl Pts',(33.6759628819914,66.2346881970577,12.));
#106328=CARTESIAN_POINT('Ctrl Pts',(33.5903722665274,66.1657795405958,12.));
#106329=CARTESIAN_POINT('Ctrl Pts',(33.5903722665274,66.1657795405958,12.));
#106330=CARTESIAN_POINT('Ctrl Pts',(33.5903722665274,66.1657795405958,8.));
#106331=CARTESIAN_POINT('Ctrl Pts',(33.5903722665274,66.1657795405958,4.));
#106332=CARTESIAN_POINT('Ctrl Pts',(33.5903722665274,66.1657795405958,-1.11022302462516E-15));
#106333=CARTESIAN_POINT('Origin',(1.72995545227681E-10,3.3253631270614E-10,
0.));
#106334=CARTESIAN_POINT('Origin',(1.72995545227681E-10,3.3253631270614E-10,
12.));
#106335=CARTESIAN_POINT('Origin',(1.72995545227681E-10,3.3253631270614E-10,
0.));
#106336=CARTESIAN_POINT('Ctrl Pts',(40.2823469776964,62.6704278106387,-5.55111512312578E-16));
#106337=CARTESIAN_POINT('Ctrl Pts',(40.2823469776964,62.6704278106387,4.));
#106338=CARTESIAN_POINT('Ctrl Pts',(40.2823469776964,62.6704278106387,8.));
#106339=CARTESIAN_POINT('Ctrl Pts',(40.2823469776964,62.6704278106387,12.));
#106340=CARTESIAN_POINT('Ctrl Pts',(40.3747816242709,62.6110140705997,-5.55111512312578E-16));
#106341=CARTESIAN_POINT('Ctrl Pts',(40.3747816242709,62.6110140705997,4.));
#106342=CARTESIAN_POINT('Ctrl Pts',(40.3747816242709,62.6110140705997,8.00000000000001));
#106343=CARTESIAN_POINT('Ctrl Pts',(40.3747816242709,62.6110140705997,12.));
#106344=CARTESIAN_POINT('Ctrl Pts',(40.5004281293558,62.4519997852059,-5.55111512312578E-16));
#106345=CARTESIAN_POINT('Ctrl Pts',(40.5004281293558,62.4519997852059,4.));
#106346=CARTESIAN_POINT('Ctrl Pts',(40.5004281293558,62.4519997852059,7.99999999999999));
#106347=CARTESIAN_POINT('Ctrl Pts',(40.5004281293558,62.4519997852059,12.));
#106348=CARTESIAN_POINT('Ctrl Pts',(40.5187208145704,62.2544389573108,-5.55111512312578E-16));
#106349=CARTESIAN_POINT('Ctrl Pts',(40.5187208145704,62.2544389573108,4.));
#106350=CARTESIAN_POINT('Ctrl Pts',(40.5187208145704,62.2544389573108,8.00000000000001));
#106351=CARTESIAN_POINT('Ctrl Pts',(40.5187208145704,62.2544389573108,12.));
#106352=CARTESIAN_POINT('Ctrl Pts',(40.5060598100835,62.1730054756444,-5.55111512312578E-16));
#106353=CARTESIAN_POINT('Ctrl Pts',(40.5060598100835,62.1730054756444,4.));
#106354=CARTESIAN_POINT('Ctrl Pts',(40.5060598100835,62.1730054756444,8.));
#106355=CARTESIAN_POINT('Ctrl Pts',(40.5060598100835,62.1730054756444,12.));
#106356=CARTESIAN_POINT('',(40.2823469776964,62.6704278106387,0.));
#106357=CARTESIAN_POINT('',(40.5060598100837,62.1730054756444,2.77555756156289E-16));
#106358=CARTESIAN_POINT('Ctrl Pts',(40.2823469776964,62.6704278106387,-1.38777878078145E-16));
#106359=CARTESIAN_POINT('Ctrl Pts',(40.3747816242709,62.6110140705997,-1.38777878078145E-16));
#106360=CARTESIAN_POINT('Ctrl Pts',(40.4465796271766,62.5201487646603,-1.38777878078144E-16));
#106361=CARTESIAN_POINT('Ctrl Pts',(40.4833233215531,62.4166968325982,-1.38777878078145E-16));
#106362=CARTESIAN_POINT('Ctrl Pts',(40.5108810923356,62.3391078835515,-1.38777878078145E-16));
#106363=CARTESIAN_POINT('Ctrl Pts',(40.5187208145704,62.2544389573108,-1.38777878078145E-16));
#106364=CARTESIAN_POINT('Ctrl Pts',(40.5060598100835,62.1730054756444,-1.38777878078145E-16));
#106365=CARTESIAN_POINT('',(40.5060598100837,62.1730054756444,12.));
#106366=CARTESIAN_POINT('Ctrl Pts',(40.5060598100835,62.1730054756444,-5.55111512312578E-16));
#106367=CARTESIAN_POINT('Ctrl Pts',(40.5060598100835,62.1730054756444,4.));
#106368=CARTESIAN_POINT('Ctrl Pts',(40.5060598100835,62.1730054756444,8.));
#106369=CARTESIAN_POINT('Ctrl Pts',(40.5060598100835,62.1730054756444,12.));
#106370=CARTESIAN_POINT('',(40.2823469776964,62.6704278106387,12.));
#106371=CARTESIAN_POINT('Ctrl Pts',(40.5060598100835,62.1730054756444,12.));
#106372=CARTESIAN_POINT('Ctrl Pts',(40.5187208145704,62.2544389573108,12.));
#106373=CARTESIAN_POINT('Ctrl Pts',(40.5108810923356,62.3391078835515,12.));
#106374=CARTESIAN_POINT('Ctrl Pts',(40.4833233215531,62.4166968325982,12.));
#106375=CARTESIAN_POINT('Ctrl Pts',(40.4465796271766,62.5201487646603,12.));
#106376=CARTESIAN_POINT('Ctrl Pts',(40.3747816242709,62.6110140705997,12.));
#106377=CARTESIAN_POINT('Ctrl Pts',(40.2823469776964,62.6704278106387,12.));
#106378=CARTESIAN_POINT('Ctrl Pts',(40.2823469776964,62.6704278106387,12.));
#106379=CARTESIAN_POINT('Ctrl Pts',(40.2823469776964,62.6704278106387,8.));
#106380=CARTESIAN_POINT('Ctrl Pts',(40.2823469776964,62.6704278106387,4.));
#106381=CARTESIAN_POINT('Ctrl Pts',(40.2823469776964,62.6704278106387,-5.55111512312578E-16));
#106382=CARTESIAN_POINT('Ctrl Pts',(39.4479504917287,57.8261117662439,0.));
#106383=CARTESIAN_POINT('Ctrl Pts',(39.4479504917287,57.8261117662439,12.));
#106384=CARTESIAN_POINT('Ctrl Pts',(39.4492429618443,57.8297740100947,0.));
#106385=CARTESIAN_POINT('Ctrl Pts',(39.4492429618443,57.8297740100947,12.));
#106386=CARTESIAN_POINT('Ctrl Pts',(39.4518277003553,57.8371043151411,0.));
#106387=CARTESIAN_POINT('Ctrl Pts',(39.4518277003553,57.8371043151411,12.));
#106388=CARTESIAN_POINT('Ctrl Pts',(39.4557042029652,57.8481172247496,0.));
#106389=CARTESIAN_POINT('Ctrl Pts',(39.4557042029652,57.8481172247496,12.));
#106390=CARTESIAN_POINT('Ctrl Pts',(39.4608716627117,57.8628360096803,0.));
#106391=CARTESIAN_POINT('Ctrl Pts',(39.4608716627117,57.8628360096803,12.));
#106392=CARTESIAN_POINT('Ctrl Pts',(39.4673289592259,57.8812926637177,0.));
#106393=CARTESIAN_POINT('Ctrl Pts',(39.4673289592259,57.8812926637177,12.));
#106394=CARTESIAN_POINT('Ctrl Pts',(39.473784194937,57.8998074670478,0.));
#106395=CARTESIAN_POINT('Ctrl Pts',(39.473784194937,57.8998074670478,12.));
#106396=CARTESIAN_POINT('Ctrl Pts',(39.4802373061058,57.9183803632404,0.));
#106397=CARTESIAN_POINT('Ctrl Pts',(39.4802373061058,57.9183803632404,12.));
#106398=CARTESIAN_POINT('Ctrl Pts',(39.4866881842317,57.9370112456631,0.));
#106399=CARTESIAN_POINT('Ctrl Pts',(39.4866881842317,57.9370112456631,12.));
#106400=CARTESIAN_POINT('Ctrl Pts',(39.4931366776714,57.9556999583892,0.));
#106401=CARTESIAN_POINT('Ctrl Pts',(39.4931366776714,57.9556999583892,12.));
#106402=CARTESIAN_POINT('Ctrl Pts',(39.499582610674,57.974446317937,0.));
#106403=CARTESIAN_POINT('Ctrl Pts',(39.499582610674,57.974446317937,12.));
#106404=CARTESIAN_POINT('Ctrl Pts',(39.5060257981225,57.9932501298522,0.));
#106405=CARTESIAN_POINT('Ctrl Pts',(39.5060257981225,57.9932501298522,12.));
#106406=CARTESIAN_POINT('Ctrl Pts',(39.5124660614976,58.0121112067896,0.));
#106407=CARTESIAN_POINT('Ctrl Pts',(39.5124660614976,58.0121112067896,12.));
#106408=CARTESIAN_POINT('Ctrl Pts',(39.5189032457184,58.0310293875262,0.));
#106409=CARTESIAN_POINT('Ctrl Pts',(39.5189032457184,58.0310293875262,12.));
#106410=CARTESIAN_POINT('Ctrl Pts',(39.5253372136887,58.0500045308412,0.));
#106411=CARTESIAN_POINT('Ctrl Pts',(39.5253372136887,58.0500045308412,12.));
#106412=CARTESIAN_POINT('Ctrl Pts',(39.5317678383217,58.0690365065374,0.));
#106413=CARTESIAN_POINT('Ctrl Pts',(39.5317678383217,58.0690365065374,12.));
#106414=CARTESIAN_POINT('Ctrl Pts',(39.5381949959221,58.0881251879921,0.));
#106415=CARTESIAN_POINT('Ctrl Pts',(39.5381949959221,58.0881251879921,12.));
#106416=CARTESIAN_POINT('Ctrl Pts',(39.5446185579638,58.1072704428928,0.));
#106417=CARTESIAN_POINT('Ctrl Pts',(39.5446185579638,58.1072704428928,12.));
#106418=CARTESIAN_POINT('Ctrl Pts',(39.5510383869505,58.126472128574,0.));
#106419=CARTESIAN_POINT('Ctrl Pts',(39.5510383869505,58.126472128574,12.));
#106420=CARTESIAN_POINT('Ctrl Pts',(39.5574543406981,58.1457300968499,0.));
#106421=CARTESIAN_POINT('Ctrl Pts',(39.5574543406981,58.1457300968499,12.));
#106422=CARTESIAN_POINT('Ctrl Pts',(39.563866275018,58.1650441970387,0.));
#106423=CARTESIAN_POINT('Ctrl Pts',(39.563866275018,58.1650441970387,12.));
#106424=CARTESIAN_POINT('Ctrl Pts',(39.5702740467999,58.1844142794338,0.));
#106425=CARTESIAN_POINT('Ctrl Pts',(39.5702740467999,58.1844142794338,12.));
#106426=CARTESIAN_POINT('Ctrl Pts',(39.57667751752,58.2038401992457,0.));
#106427=CARTESIAN_POINT('Ctrl Pts',(39.57667751752,58.2038401992457,12.));
#106428=CARTESIAN_POINT('Ctrl Pts',(39.5830765530891,58.2233218164366,0.));
#106429=CARTESIAN_POINT('Ctrl Pts',(39.5830765530891,58.2233218164366,12.));
#106430=CARTESIAN_POINT('Ctrl Pts',(39.5894710221713,58.2428589938369,0.));
#106431=CARTESIAN_POINT('Ctrl Pts',(39.5894710221713,58.2428589938369,12.));
#106432=CARTESIAN_POINT('Ctrl Pts',(39.5958607950239,58.2624515958419,0.));
#106433=CARTESIAN_POINT('Ctrl Pts',(39.5958607950239,58.2624515958419,12.));
#106434=CARTESIAN_POINT('Ctrl Pts',(39.6022457420789,58.2820994868118,0.));
#106435=CARTESIAN_POINT('Ctrl Pts',(39.6022457420789,58.2820994868118,12.));
#106436=CARTESIAN_POINT('Ctrl Pts',(39.6086257327583,58.3018025297324,0.));
#106437=CARTESIAN_POINT('Ctrl Pts',(39.6086257327583,58.3018025297324,12.));
#106438=CARTESIAN_POINT('Ctrl Pts',(39.6150006360914,58.3215605869221,0.));
#106439=CARTESIAN_POINT('Ctrl Pts',(39.6150006360914,58.3215605869221,12.));
#106440=CARTESIAN_POINT('Ctrl Pts',(39.6213703212531,58.3413735206424,0.));
#106441=CARTESIAN_POINT('Ctrl Pts',(39.6213703212531,58.3413735206424,12.));
#106442=CARTESIAN_POINT('Ctrl Pts',(39.6277346580892,58.3612411936905,0.));
#106443=CARTESIAN_POINT('Ctrl Pts',(39.6277346580892,58.3612411936905,12.));
#106444=CARTESIAN_POINT('Ctrl Pts',(39.6340935177476,58.3811634701037,0.));
#106445=CARTESIAN_POINT('Ctrl Pts',(39.6340935177476,58.3811634701037,12.));
#106446=CARTESIAN_POINT('Ctrl Pts',(39.6404467729094,58.4011402154196,0.));
#106447=CARTESIAN_POINT('Ctrl Pts',(39.6404467729094,58.4011402154196,12.));
#106448=CARTESIAN_POINT('Ctrl Pts',(39.6467942974451,58.4211712963004,0.));
#106449=CARTESIAN_POINT('Ctrl Pts',(39.6467942974451,58.4211712963004,12.));
#106450=CARTESIAN_POINT('Ctrl Pts',(39.653135966204,58.4412565802979,0.));
#106451=CARTESIAN_POINT('Ctrl Pts',(39.653135966204,58.4412565802979,12.));
#106452=CARTESIAN_POINT('Ctrl Pts',(39.6594716547689,58.4613959355788,0.));
#106453=CARTESIAN_POINT('Ctrl Pts',(39.6594716547689,58.4613959355788,12.));
#106454=CARTESIAN_POINT('Ctrl Pts',(39.6658012391815,58.4815892306066,0.));
#106455=CARTESIAN_POINT('Ctrl Pts',(39.6658012391815,58.4815892306066,12.));
#106456=CARTESIAN_POINT('Ctrl Pts',(39.6721245959531,58.5018363341604,0.));
#106457=CARTESIAN_POINT('Ctrl Pts',(39.6721245959531,58.5018363341604,12.));
#106458=CARTESIAN_POINT('Ctrl Pts',(39.6784416021826,58.5221371154761,0.));
#106459=CARTESIAN_POINT('Ctrl Pts',(39.6784416021826,58.5221371154761,12.));
#106460=CARTESIAN_POINT('Ctrl Pts',(39.6847521356395,58.5424914443415,0.));
#106461=CARTESIAN_POINT('Ctrl Pts',(39.6847521356395,58.5424914443415,12.));
#106462=CARTESIAN_POINT('Ctrl Pts',(39.6910560748629,58.5628991912052,0.));
#106463=CARTESIAN_POINT('Ctrl Pts',(39.6910560748629,58.5628991912052,12.));
#106464=CARTESIAN_POINT('Ctrl Pts',(39.6973532992539,58.5833602272744,0.));
#106465=CARTESIAN_POINT('Ctrl Pts',(39.6973532992539,58.5833602272744,12.));
#106466=CARTESIAN_POINT('Ctrl Pts',(39.7036436890232,58.6038744244659,0.));
#106467=CARTESIAN_POINT('Ctrl Pts',(39.7036436890232,58.6038744244659,12.));
#106468=CARTESIAN_POINT('Ctrl Pts',(39.7099271251413,58.6244416553562,0.));
#106469=CARTESIAN_POINT('Ctrl Pts',(39.7099271251413,58.6244416553562,12.));
#106470=CARTESIAN_POINT('Ctrl Pts',(39.7162034892899,58.6450617931274,0.));
#106471=CARTESIAN_POINT('Ctrl Pts',(39.7162034892899,58.6450617931274,12.));
#106472=CARTESIAN_POINT('Ctrl Pts',(39.72247266381,58.6657347115034,0.));
#106473=CARTESIAN_POINT('Ctrl Pts',(39.72247266381,58.6657347115034,12.));
#106474=CARTESIAN_POINT('Ctrl Pts',(39.7287345316681,58.6864602847088,0.));
#106475=CARTESIAN_POINT('Ctrl Pts',(39.7287345316681,58.6864602847088,12.));
#106476=CARTESIAN_POINT('Ctrl Pts',(39.7349889764749,58.7072383875027,0.));
#106477=CARTESIAN_POINT('Ctrl Pts',(39.7349889764749,58.7072383875027,12.));
#106478=CARTESIAN_POINT('Ctrl Pts',(39.7412358824953,58.7280688951916,0.));
#106479=CARTESIAN_POINT('Ctrl Pts',(39.7412358824953,58.7280688951916,12.));
#106480=CARTESIAN_POINT('Ctrl Pts',(39.7474751346598,58.7489516836445,0.));
#106481=CARTESIAN_POINT('Ctrl Pts',(39.7474751346598,58.7489516836445,12.));
#106482=CARTESIAN_POINT('Ctrl Pts',(39.7537066185812,58.7698866293029,0.));
#106483=CARTESIAN_POINT('Ctrl Pts',(39.7537066185812,58.7698866293029,12.));
#106484=CARTESIAN_POINT('Ctrl Pts',(39.759930220552,58.7908736091798,0.));
#106485=CARTESIAN_POINT('Ctrl Pts',(39.759930220552,58.7908736091798,12.));
#106486=CARTESIAN_POINT('Ctrl Pts',(39.7661458275274,58.8119125008517,0.));
#106487=CARTESIAN_POINT('Ctrl Pts',(39.7661458275274,58.8119125008517,12.));
#106488=CARTESIAN_POINT('Ctrl Pts',(39.772353327112,58.8330031824453,0.));
#106489=CARTESIAN_POINT('Ctrl Pts',(39.772353327112,58.8330031824453,12.));
#106490=CARTESIAN_POINT('Ctrl Pts',(39.7785526075478,58.8541455326231,0.));
#106491=CARTESIAN_POINT('Ctrl Pts',(39.7785526075478,58.8541455326231,12.));
#106492=CARTESIAN_POINT('Ctrl Pts',(39.7847435576996,58.8753394305586,0.));
#106493=CARTESIAN_POINT('Ctrl Pts',(39.7847435576996,58.8753394305586,12.));
#106494=CARTESIAN_POINT('Ctrl Pts',(39.7909260670517,58.8965847559391,0.));
#106495=CARTESIAN_POINT('Ctrl Pts',(39.7909260670517,58.8965847559391,12.));
#106496=CARTESIAN_POINT('Ctrl Pts',(39.7971000257044,58.9178813889704,0.));
#106497=CARTESIAN_POINT('Ctrl Pts',(39.7971000257044,58.9178813889704,12.));
#106498=CARTESIAN_POINT('Ctrl Pts',(39.8032653243712,58.9392292103747,0.));
#106499=CARTESIAN_POINT('Ctrl Pts',(39.8032653243712,58.9392292103747,12.));
#106500=CARTESIAN_POINT('Ctrl Pts',(39.8094218543782,58.9606281013875,0.));
#106501=CARTESIAN_POINT('Ctrl Pts',(39.8094218543782,58.9606281013875,12.));
#106502=CARTESIAN_POINT('Ctrl Pts',(39.8155695076626,58.9820779437485,0.));
#106503=CARTESIAN_POINT('Ctrl Pts',(39.8155695076626,58.9820779437485,12.));
#106504=CARTESIAN_POINT('Ctrl Pts',(39.821708176766,59.0035786197024,0.));
#106505=CARTESIAN_POINT('Ctrl Pts',(39.821708176766,59.0035786197024,12.));
#106506=CARTESIAN_POINT('Ctrl Pts',(39.8278377548262,59.0251300119973,0.));
#106507=CARTESIAN_POINT('Ctrl Pts',(39.8278377548262,59.0251300119973,12.));
#106508=CARTESIAN_POINT('Ctrl Pts',(39.8339581355715,59.0467320038784,0.));
#106509=CARTESIAN_POINT('Ctrl Pts',(39.8339581355715,59.0467320038784,12.));
#106510=CARTESIAN_POINT('Ctrl Pts',(39.8400692133139,59.0683844790764,0.));
#106511=CARTESIAN_POINT('Ctrl Pts',(39.8400692133139,59.0683844790764,12.));
#106512=CARTESIAN_POINT('Ctrl Pts',(39.8461708829456,59.0900873217981,0.));
#106513=CARTESIAN_POINT('Ctrl Pts',(39.8461708829456,59.0900873217981,12.));
#106514=CARTESIAN_POINT('Ctrl Pts',(39.8522630399328,59.1118404167292,0.));
#106515=CARTESIAN_POINT('Ctrl Pts',(39.8522630399328,59.1118404167292,12.));
#106516=CARTESIAN_POINT('Ctrl Pts',(39.8583455803105,59.1336436490342,0.));
#106517=CARTESIAN_POINT('Ctrl Pts',(39.8583455803105,59.1336436490342,12.));
#106518=CARTESIAN_POINT('Ctrl Pts',(39.8644184006786,59.1554969043522,0.));
#106519=CARTESIAN_POINT('Ctrl Pts',(39.8644184006786,59.1554969043522,12.));
#106520=CARTESIAN_POINT('Ctrl Pts',(39.8704813981988,59.1774000687879,0.));
#106521=CARTESIAN_POINT('Ctrl Pts',(39.8704813981988,59.1774000687879,12.));
#106522=CARTESIAN_POINT('Ctrl Pts',(39.8765344705909,59.1993530289029,0.));
#106523=CARTESIAN_POINT('Ctrl Pts',(39.8765344705909,59.1993530289029,12.));
#106524=CARTESIAN_POINT('Ctrl Pts',(39.8825775161267,59.2213556717209,0.));
#106525=CARTESIAN_POINT('Ctrl Pts',(39.8825775161267,59.2213556717209,12.));
#106526=CARTESIAN_POINT('Ctrl Pts',(39.8886104336242,59.2434078847247,0.));
#106527=CARTESIAN_POINT('Ctrl Pts',(39.8886104336242,59.2434078847247,12.));
#106528=CARTESIAN_POINT('Ctrl Pts',(39.8946331224438,59.2655095558521,0.));
#106529=CARTESIAN_POINT('Ctrl Pts',(39.8946331224438,59.2655095558521,12.));
#106530=CARTESIAN_POINT('Ctrl Pts',(39.9006454824845,59.2876605734847,0.));
#106531=CARTESIAN_POINT('Ctrl Pts',(39.9006454824845,59.2876605734847,12.));
#106532=CARTESIAN_POINT('Ctrl Pts',(39.9066474141803,59.3098608264419,0.));
#106533=CARTESIAN_POINT('Ctrl Pts',(39.9066474141803,59.3098608264419,12.));
#106534=CARTESIAN_POINT('Ctrl Pts',(39.9126388184936,59.3321102039852,0.));
#106535=CARTESIAN_POINT('Ctrl Pts',(39.9126388184936,59.3321102039852,12.));
#106536=CARTESIAN_POINT('Ctrl Pts',(39.9186195969104,59.3544085958151,0.));
#106537=CARTESIAN_POINT('Ctrl Pts',(39.9186195969104,59.3544085958151,12.));
#106538=CARTESIAN_POINT('Ctrl Pts',(39.9245896514367,59.3767558920675,0.));
#106539=CARTESIAN_POINT('Ctrl Pts',(39.9245896514367,59.3767558920675,12.));
#106540=CARTESIAN_POINT('Ctrl Pts',(39.9305488845958,59.3991519833016,0.));
#106541=CARTESIAN_POINT('Ctrl Pts',(39.9305488845958,59.3991519833016,12.));
#106542=CARTESIAN_POINT('Ctrl Pts',(39.9364971994242,59.4215967604968,0.));
#106543=CARTESIAN_POINT('Ctrl Pts',(39.9364971994242,59.4215967604968,12.));
#106544=CARTESIAN_POINT('Ctrl Pts',(39.9424344994672,59.4440901150582,0.));
#106545=CARTESIAN_POINT('Ctrl Pts',(39.9424344994672,59.4440901150582,12.));
#106546=CARTESIAN_POINT('Ctrl Pts',(39.9483606887737,59.4666319388133,0.));
#106547=CARTESIAN_POINT('Ctrl Pts',(39.9483606887737,59.4666319388133,12.));
#106548=CARTESIAN_POINT('Ctrl Pts',(39.9542756718922,59.4892221240069,0.));
#106549=CARTESIAN_POINT('Ctrl Pts',(39.9542756718922,59.4892221240069,12.));
#106550=CARTESIAN_POINT('Ctrl Pts',(39.9601793538682,59.5118605632891,0.));
#106551=CARTESIAN_POINT('Ctrl Pts',(39.9601793538682,59.5118605632891,12.));
#106552=CARTESIAN_POINT('Ctrl Pts',(39.9660716402403,59.5345471497129,0.));
#106553=CARTESIAN_POINT('Ctrl Pts',(39.9660716402403,59.5345471497129,12.));
#106554=CARTESIAN_POINT('Ctrl Pts',(39.9719524370345,59.5572817767388,0.));
#106555=CARTESIAN_POINT('Ctrl Pts',(39.9719524370345,59.5572817767388,12.));
#106556=CARTESIAN_POINT('Ctrl Pts',(39.9778216507605,59.5800643382315,0.));
#106557=CARTESIAN_POINT('Ctrl Pts',(39.9778216507605,59.5800643382315,12.));
#106558=CARTESIAN_POINT('Ctrl Pts',(39.9836791884079,59.6028947284562,0.));
#106559=CARTESIAN_POINT('Ctrl Pts',(39.9836791884079,59.6028947284562,12.));
#106560=CARTESIAN_POINT('Ctrl Pts',(39.9895249574448,59.6257728420669,0.));
#106561=CARTESIAN_POINT('Ctrl Pts',(39.9895249574448,59.6257728420669,12.));
#106562=CARTESIAN_POINT('Ctrl Pts',(39.9953588658131,59.6486985741041,0.));
#106563=CARTESIAN_POINT('Ctrl Pts',(39.9953588658131,59.6486985741041,12.));
#106564=CARTESIAN_POINT('Ctrl Pts',(40.0011808219241,59.6716718200005,0.));
#106565=CARTESIAN_POINT('Ctrl Pts',(40.0011808219241,59.6716718200005,12.));
#106566=CARTESIAN_POINT('Ctrl Pts',(40.0069907346537,59.6946924755773,0.));
#106567=CARTESIAN_POINT('Ctrl Pts',(40.0069907346537,59.6946924755773,12.));
#106568=CARTESIAN_POINT('Ctrl Pts',(40.0127885133403,59.7177604370403,0.));
#106569=CARTESIAN_POINT('Ctrl Pts',(40.0127885133403,59.7177604370403,12.));
#106570=CARTESIAN_POINT('Ctrl Pts',(40.0185740677821,59.7408756009679,0.));
#106571=CARTESIAN_POINT('Ctrl Pts',(40.0185740677821,59.7408756009679,12.));
#106572=CARTESIAN_POINT('Ctrl Pts',(40.0243473082337,59.7640378643106,0.));
#106573=CARTESIAN_POINT('Ctrl Pts',(40.0243473082337,59.7640378643106,12.));
#106574=CARTESIAN_POINT('Ctrl Pts',(40.0301081454002,59.7872471243942,0.));
#106575=CARTESIAN_POINT('Ctrl Pts',(40.0301081454002,59.7872471243942,12.));
#106576=CARTESIAN_POINT('Ctrl Pts',(40.035856490434,59.8105032789179,0.));
#106577=CARTESIAN_POINT('Ctrl Pts',(40.035856490434,59.8105032789179,12.));
#106578=CARTESIAN_POINT('Ctrl Pts',(40.0415922549314,59.8338062259493,0.));
#106579=CARTESIAN_POINT('Ctrl Pts',(40.0415922549314,59.8338062259493,12.));
#106580=CARTESIAN_POINT('Ctrl Pts',(40.0473153509324,59.8571558639145,0.));
#106581=CARTESIAN_POINT('Ctrl Pts',(40.0473153509324,59.8571558639145,12.));
#106582=CARTESIAN_POINT('Ctrl Pts',(40.053025690916,59.8805520915972,0.));
#106583=CARTESIAN_POINT('Ctrl Pts',(40.053025690916,59.8805520915972,12.));
#106584=CARTESIAN_POINT('Ctrl Pts',(40.0587231877959,59.9039948081428,0.));
#106585=CARTESIAN_POINT('Ctrl Pts',(40.0587231877959,59.9039948081428,12.));
#106586=CARTESIAN_POINT('Ctrl Pts',(40.0644077549158,59.927483913055,0.));
#106587=CARTESIAN_POINT('Ctrl Pts',(40.0644077549158,59.927483913055,12.));
#106588=CARTESIAN_POINT('Ctrl Pts',(40.0700793060475,59.9510193061929,0.));
#106589=CARTESIAN_POINT('Ctrl Pts',(40.0700793060475,59.9510193061929,12.));
#106590=CARTESIAN_POINT('Ctrl Pts',(40.0757377553893,59.974600887759,0.));
#106591=CARTESIAN_POINT('Ctrl Pts',(40.0757377553893,59.974600887759,12.));
#106592=CARTESIAN_POINT('Ctrl Pts',(40.0813830175629,59.9982285582991,0.));
#106593=CARTESIAN_POINT('Ctrl Pts',(40.0813830175629,59.9982285582991,12.));
#106594=CARTESIAN_POINT('Ctrl Pts',(40.0870150076078,60.0219022187066,0.));
#106595=CARTESIAN_POINT('Ctrl Pts',(40.0870150076078,60.0219022187066,12.));
#106596=CARTESIAN_POINT('Ctrl Pts',(40.0926336409787,60.0456217702203,0.));
#106597=CARTESIAN_POINT('Ctrl Pts',(40.0926336409787,60.0456217702203,12.));
#106598=CARTESIAN_POINT('Ctrl Pts',(40.0982388335421,60.0693871144207,0.));
#106599=CARTESIAN_POINT('Ctrl Pts',(40.0982388335421,60.0693871144207,12.));
#106600=CARTESIAN_POINT('Ctrl Pts',(40.1038305015763,60.0931981532194,0.));
#106601=CARTESIAN_POINT('Ctrl Pts',(40.1038305015763,60.0931981532194,12.));
#106602=CARTESIAN_POINT('Ctrl Pts',(40.1094085617672,60.1170547888572,0.));
#106603=CARTESIAN_POINT('Ctrl Pts',(40.1094085617672,60.1170547888572,12.));
#106604=CARTESIAN_POINT('Ctrl Pts',(40.1149729312036,60.1409569239093,0.));
#106605=CARTESIAN_POINT('Ctrl Pts',(40.1149729312036,60.1409569239093,12.));
#106606=CARTESIAN_POINT('Ctrl Pts',(40.120523527374,60.164904461283,0.));
#106607=CARTESIAN_POINT('Ctrl Pts',(40.120523527374,60.164904461283,12.));
#106608=CARTESIAN_POINT('Ctrl Pts',(40.1260602681644,60.1888973042151,0.));
#106609=CARTESIAN_POINT('Ctrl Pts',(40.1260602681644,60.1888973042151,12.));
#106610=CARTESIAN_POINT('Ctrl Pts',(40.1315830718575,60.2129353562618,0.));
#106611=CARTESIAN_POINT('Ctrl Pts',(40.1315830718575,60.2129353562618,12.));
#106612=CARTESIAN_POINT('Ctrl Pts',(40.13709185713,60.2370185212957,0.));
#106613=CARTESIAN_POINT('Ctrl Pts',(40.13709185713,60.2370185212957,12.));
#106614=CARTESIAN_POINT('Ctrl Pts',(40.1425865430468,60.2611467035109,0.));
#106615=CARTESIAN_POINT('Ctrl Pts',(40.1425865430468,60.2611467035109,12.));
#106616=CARTESIAN_POINT('Ctrl Pts',(40.1480670490583,60.2853198074216,0.));
#106617=CARTESIAN_POINT('Ctrl Pts',(40.1480670490583,60.2853198074216,12.));
#106618=CARTESIAN_POINT('Ctrl Pts',(40.1535332949978,60.3095377378589,0.));
#106619=CARTESIAN_POINT('Ctrl Pts',(40.1535332949978,60.3095377378589,12.));
#106620=CARTESIAN_POINT('Ctrl Pts',(40.158985201081,60.3338003999616,0.));
#106621=CARTESIAN_POINT('Ctrl Pts',(40.158985201081,60.3338003999616,12.));
#106622=CARTESIAN_POINT('Ctrl Pts',(40.1644226879043,60.3581076991731,0.));
#106623=CARTESIAN_POINT('Ctrl Pts',(40.1644226879043,60.3581076991731,12.));
#106624=CARTESIAN_POINT('Ctrl Pts',(40.1698456764387,60.382459541246,0.));
#106625=CARTESIAN_POINT('Ctrl Pts',(40.1698456764387,60.382459541246,12.));
#106626=CARTESIAN_POINT('Ctrl Pts',(40.1752540880273,60.4068558322415,0.));
#106627=CARTESIAN_POINT('Ctrl Pts',(40.1752540880273,60.4068558322415,12.));
#106628=CARTESIAN_POINT('Ctrl Pts',(40.1806478443828,60.4312964785269,0.));
#106629=CARTESIAN_POINT('Ctrl Pts',(40.1806478443828,60.4312964785269,12.));
#106630=CARTESIAN_POINT('Ctrl Pts',(40.1860268675875,60.4557813867677,0.));
#106631=CARTESIAN_POINT('Ctrl Pts',(40.1860268675875,60.4557813867677,12.));
#106632=CARTESIAN_POINT('Ctrl Pts',(40.1913910800911,60.4803104639211,0.));
#106633=CARTESIAN_POINT('Ctrl Pts',(40.1913910800911,60.4803104639211,12.));
#106634=CARTESIAN_POINT('Ctrl Pts',(40.1967404047055,60.5048836172424,0.));
#106635=CARTESIAN_POINT('Ctrl Pts',(40.1967404047055,60.5048836172424,12.));
#106636=CARTESIAN_POINT('Ctrl Pts',(40.2020747646012,60.5295007542838,0.));
#106637=CARTESIAN_POINT('Ctrl Pts',(40.2020747646012,60.5295007542838,12.));
#106638=CARTESIAN_POINT('Ctrl Pts',(40.2073940833054,60.5541617828927,0.));
#106639=CARTESIAN_POINT('Ctrl Pts',(40.2073940833054,60.5541617828927,12.));
#106640=CARTESIAN_POINT('Ctrl Pts',(40.2126982847012,60.5788666112043,0.));
#106641=CARTESIAN_POINT('Ctrl Pts',(40.2126982847012,60.5788666112043,12.));
#106642=CARTESIAN_POINT('Ctrl Pts',(40.2179872930271,60.6036151476347,0.));
#106643=CARTESIAN_POINT('Ctrl Pts',(40.2179872930271,60.6036151476347,12.));
#106644=CARTESIAN_POINT('Ctrl Pts',(40.2232610328717,60.6284073008865,0.));
#106645=CARTESIAN_POINT('Ctrl Pts',(40.2232610328717,60.6284073008865,12.));
#106646=CARTESIAN_POINT('Ctrl Pts',(40.2285194291702,60.6532429799494,0.));
#106647=CARTESIAN_POINT('Ctrl Pts',(40.2285194291702,60.6532429799494,12.));
#106648=CARTESIAN_POINT('Ctrl Pts',(40.2337624072029,60.678122094098,0.));
#106649=CARTESIAN_POINT('Ctrl Pts',(40.2337624072029,60.678122094098,12.));
#106650=CARTESIAN_POINT('Ctrl Pts',(40.2389898925937,60.7030445528863,0.));
#106651=CARTESIAN_POINT('Ctrl Pts',(40.2389898925937,60.7030445528863,12.));
#106652=CARTESIAN_POINT('Ctrl Pts',(40.2442018113116,60.7280102661401,0.));
#106653=CARTESIAN_POINT('Ctrl Pts',(40.2442018113116,60.7280102661401,12.));
#106654=CARTESIAN_POINT('Ctrl Pts',(40.2493980896646,60.7530191439603,0.));
#106655=CARTESIAN_POINT('Ctrl Pts',(40.2493980896646,60.7530191439603,12.));
#106656=CARTESIAN_POINT('Ctrl Pts',(40.2545786542957,60.7780710967253,0.));
#106657=CARTESIAN_POINT('Ctrl Pts',(40.2545786542957,60.7780710967253,12.));
#106658=CARTESIAN_POINT('Ctrl Pts',(40.2597434321803,60.8031660350879,0.));
#106659=CARTESIAN_POINT('Ctrl Pts',(40.2597434321803,60.8031660350879,12.));
#106660=CARTESIAN_POINT('Ctrl Pts',(40.2648923506245,60.8283038699703,0.));
#106661=CARTESIAN_POINT('Ctrl Pts',(40.2648923506245,60.8283038699703,12.));
#106662=CARTESIAN_POINT('Ctrl Pts',(40.2700253372644,60.8534845125535,0.));
#106663=CARTESIAN_POINT('Ctrl Pts',(40.2700253372644,60.8534845125535,12.));
#106664=CARTESIAN_POINT('Ctrl Pts',(40.2751423200637,60.8787078742817,0.));
#106665=CARTESIAN_POINT('Ctrl Pts',(40.2751423200637,60.8787078742817,12.));
#106666=CARTESIAN_POINT('Ctrl Pts',(40.2802432273104,60.903973866867,0.));
#106667=CARTESIAN_POINT('Ctrl Pts',(40.2802432273104,60.903973866867,12.));
#106668=CARTESIAN_POINT('Ctrl Pts',(40.2853279876161,60.9292824022888,0.));
#106669=CARTESIAN_POINT('Ctrl Pts',(40.2853279876161,60.9292824022888,12.));
#106670=CARTESIAN_POINT('Ctrl Pts',(40.2903965299155,60.9546333927919,0.));
#106671=CARTESIAN_POINT('Ctrl Pts',(40.2903965299155,60.9546333927919,12.));
#106672=CARTESIAN_POINT('Ctrl Pts',(40.2954487834688,60.9800267508781,0.));
#106673=CARTESIAN_POINT('Ctrl Pts',(40.2954487834688,60.9800267508781,12.));
#106674=CARTESIAN_POINT('Ctrl Pts',(40.3004846778577,61.005462389306,0.));
#106675=CARTESIAN_POINT('Ctrl Pts',(40.3004846778577,61.005462389306,12.));
#106676=CARTESIAN_POINT('Ctrl Pts',(40.3055041429772,61.0309402210915,0.));
#106677=CARTESIAN_POINT('Ctrl Pts',(40.3055041429772,61.0309402210915,12.));
#106678=CARTESIAN_POINT('Ctrl Pts',(40.3105071090308,61.0564601595047,0.));
#106679=CARTESIAN_POINT('Ctrl Pts',(40.3105071090308,61.0564601595047,12.));
#106680=CARTESIAN_POINT('Ctrl Pts',(40.3154935065263,61.0820221180647,0.));
#106681=CARTESIAN_POINT('Ctrl Pts',(40.3154935065263,61.0820221180647,12.));
#106682=CARTESIAN_POINT('Ctrl Pts',(40.3204632662729,61.1076260105265,0.));
#106683=CARTESIAN_POINT('Ctrl Pts',(40.3204632662729,61.1076260105265,12.));
#106684=CARTESIAN_POINT('Ctrl Pts',(40.3254163193805,61.1332717508799,0.));
#106685=CARTESIAN_POINT('Ctrl Pts',(40.3254163193805,61.1332717508799,12.));
#106686=CARTESIAN_POINT('Ctrl Pts',(40.3303525972621,61.1589592533623,0.));
#106687=CARTESIAN_POINT('Ctrl Pts',(40.3303525972621,61.1589592533623,12.));
#106688=CARTESIAN_POINT('Ctrl Pts',(40.3352720316373,61.184688432465,0.));
#106689=CARTESIAN_POINT('Ctrl Pts',(40.3352720316373,61.184688432465,12.));
#106690=CARTESIAN_POINT('Ctrl Pts',(40.3401745545369,61.2104592029376,0.));
#106691=CARTESIAN_POINT('Ctrl Pts',(40.3401745545369,61.2104592029376,12.));
#106692=CARTESIAN_POINT('Ctrl Pts',(40.3450600983104,61.2362714797891,0.));
#106693=CARTESIAN_POINT('Ctrl Pts',(40.3450600983104,61.2362714797891,12.));
#106694=CARTESIAN_POINT('Ctrl Pts',(40.3499285956297,61.262125178285,0.));
#106695=CARTESIAN_POINT('Ctrl Pts',(40.3499285956297,61.262125178285,12.));
#106696=CARTESIAN_POINT('Ctrl Pts',(40.3547799794672,61.2880202139358,0.));
#106697=CARTESIAN_POINT('Ctrl Pts',(40.3547799794672,61.2880202139358,12.));
#106698=CARTESIAN_POINT('Ctrl Pts',(40.3596141830786,61.3139565024838,0.));
#106699=CARTESIAN_POINT('Ctrl Pts',(40.3596141830786,61.3139565024838,12.));
#106700=CARTESIAN_POINT('Ctrl Pts',(40.364431139986,61.3399339598852,0.));
#106701=CARTESIAN_POINT('Ctrl Pts',(40.364431139986,61.3399339598852,12.));
#106702=CARTESIAN_POINT('Ctrl Pts',(40.3692307839642,61.3659525022917,0.));
#106703=CARTESIAN_POINT('Ctrl Pts',(40.3692307839642,61.3659525022917,12.));
#106704=CARTESIAN_POINT('Ctrl Pts',(40.3740130490233,61.3920120460232,0.));
#106705=CARTESIAN_POINT('Ctrl Pts',(40.3740130490233,61.3920120460232,12.));
#106706=CARTESIAN_POINT('Ctrl Pts',(40.3787778694372,61.418112507605,0.));
#106707=CARTESIAN_POINT('Ctrl Pts',(40.3787778694372,61.418112507605,12.));
#106708=CARTESIAN_POINT('Ctrl Pts',(40.3835251797725,61.4442538038053,0.));
#106709=CARTESIAN_POINT('Ctrl Pts',(40.3835251797725,61.4442538038053,12.));
#106710=CARTESIAN_POINT('Ctrl Pts',(40.3882549149229,61.4704358516711,0.));
#106711=CARTESIAN_POINT('Ctrl Pts',(40.3882549149229,61.4704358516711,12.));
#106712=CARTESIAN_POINT('Ctrl Pts',(40.3929670101363,61.4966585685545,0.));
#106713=CARTESIAN_POINT('Ctrl Pts',(40.3929670101363,61.4966585685545,12.));
#106714=CARTESIAN_POINT('Ctrl Pts',(40.3976614010648,61.5229218721532,0.));
#106715=CARTESIAN_POINT('Ctrl Pts',(40.3976614010648,61.5229218721532,12.));
#106716=CARTESIAN_POINT('Ctrl Pts',(40.4023380237227,61.5492256804709,0.));
#106717=CARTESIAN_POINT('Ctrl Pts',(40.4023380237227,61.5492256804709,12.));
#106718=CARTESIAN_POINT('Ctrl Pts',(40.4069968143953,61.5755699117318,0.));
#106719=CARTESIAN_POINT('Ctrl Pts',(40.4069968143953,61.5755699117318,12.));
#106720=CARTESIAN_POINT('Ctrl Pts',(40.4116377095595,61.6019544843009,0.));
#106721=CARTESIAN_POINT('Ctrl Pts',(40.4116377095595,61.6019544843009,12.));
#106722=CARTESIAN_POINT('Ctrl Pts',(40.4162606458119,61.628379316608,0.));
#106723=CARTESIAN_POINT('Ctrl Pts',(40.4162606458119,61.628379316608,12.));
#106724=CARTESIAN_POINT('Ctrl Pts',(40.420865559772,61.6548443270397,0.));
#106725=CARTESIAN_POINT('Ctrl Pts',(40.420865559772,61.6548443270397,12.));
#106726=CARTESIAN_POINT('Ctrl Pts',(40.4254523880766,61.6813494339295,0.));
#106727=CARTESIAN_POINT('Ctrl Pts',(40.4254523880766,61.6813494339295,12.));
#106728=CARTESIAN_POINT('Ctrl Pts',(40.4300210675848,61.7078945557812,0.));
#106729=CARTESIAN_POINT('Ctrl Pts',(40.4300210675848,61.7078945557812,12.));
#106730=CARTESIAN_POINT('Ctrl Pts',(40.4345715355411,61.7344796114409,0.));
#106731=CARTESIAN_POINT('Ctrl Pts',(40.4345715355411,61.7344796114409,12.));
#106732=CARTESIAN_POINT('Ctrl Pts',(40.4391037297589,61.7611045202875,0.));
#106733=CARTESIAN_POINT('Ctrl Pts',(40.4391037297589,61.7611045202875,12.));
#106734=CARTESIAN_POINT('Ctrl Pts',(40.4436175887942,61.7877692024064,0.));
#106735=CARTESIAN_POINT('Ctrl Pts',(40.4436175887942,61.7877692024064,12.));
#106736=CARTESIAN_POINT('Ctrl Pts',(40.448113052135,61.8144735787767,0.));
#106737=CARTESIAN_POINT('Ctrl Pts',(40.448113052135,61.8144735787767,12.));
#106738=CARTESIAN_POINT('Ctrl Pts',(40.4525900597877,61.8412175708524,0.));
#106739=CARTESIAN_POINT('Ctrl Pts',(40.4525900597877,61.8412175708524,12.));
#106740=CARTESIAN_POINT('Ctrl Pts',(40.4570485518735,61.8680011001513,0.));
#106741=CARTESIAN_POINT('Ctrl Pts',(40.4570485518735,61.8680011001513,12.));
#106742=CARTESIAN_POINT('Ctrl Pts',(40.4614884681884,61.8948240877998,0.));
#106743=CARTESIAN_POINT('Ctrl Pts',(40.4614884681884,61.8948240877998,12.));
#106744=CARTESIAN_POINT('Ctrl Pts',(40.4659097478595,61.9216864541758,0.));
#106745=CARTESIAN_POINT('Ctrl Pts',(40.4659097478595,61.9216864541758,12.));
#106746=CARTESIAN_POINT('Ctrl Pts',(40.4703123287642,61.9485881182957,0.));
#106747=CARTESIAN_POINT('Ctrl Pts',(40.4703123287642,61.9485881182957,12.));
#106748=CARTESIAN_POINT('Ctrl Pts',(40.4746961480045,61.9755289983094,0.));
#106749=CARTESIAN_POINT('Ctrl Pts',(40.4746961480045,61.9755289983094,12.));
#106750=CARTESIAN_POINT('Ctrl Pts',(40.4790611429613,62.0025090126008,0.));
#106751=CARTESIAN_POINT('Ctrl Pts',(40.4790611429613,62.0025090126008,12.));
#106752=CARTESIAN_POINT('Ctrl Pts',(40.4834072522181,62.0295280807449,0.));
#106753=CARTESIAN_POINT('Ctrl Pts',(40.4834072522181,62.0295280807449,12.));
#106754=CARTESIAN_POINT('Ctrl Pts',(40.4877344164407,62.0565861244171,0.));
#106755=CARTESIAN_POINT('Ctrl Pts',(40.4877344164407,62.0565861244171,12.));
#106756=CARTESIAN_POINT('Ctrl Pts',(40.4920425795184,62.0836830685665,0.));
#106757=CARTESIAN_POINT('Ctrl Pts',(40.4920425795184,62.0836830685665,12.));
#106758=CARTESIAN_POINT('Ctrl Pts',(40.4963316888356,62.110818841691,0.));
#106759=CARTESIAN_POINT('Ctrl Pts',(40.4963316888356,62.110818841691,12.));
#106760=CARTESIAN_POINT('Ctrl Pts',(40.5006016927489,62.137993373242,0.));
#106761=CARTESIAN_POINT('Ctrl Pts',(40.5006016927489,62.137993373242,12.));
#106762=CARTESIAN_POINT('Ctrl Pts',(40.5048525385985,62.1652065915724,0.));
#106763=CARTESIAN_POINT('Ctrl Pts',(40.5048525385985,62.1652065915724,12.));
#106764=CARTESIAN_POINT('Ctrl Pts',(40.5090841704111,62.1924584215634,0.));
#106765=CARTESIAN_POINT('Ctrl Pts',(40.5090841704111,62.1924584215634,12.));
#106766=CARTESIAN_POINT('Ctrl Pts',(40.5132965269679,62.2197487826212,0.));
#106767=CARTESIAN_POINT('Ctrl Pts',(40.5132965269679,62.2197487826212,12.));
#106768=CARTESIAN_POINT('Ctrl Pts',(40.5174895391059,62.2470775858834,0.));
#106769=CARTESIAN_POINT('Ctrl Pts',(40.5174895391059,62.2470775858834,12.));
#106770=CARTESIAN_POINT('Ctrl Pts',(40.5216631336335,62.2744447382207,0.));
#106771=CARTESIAN_POINT('Ctrl Pts',(40.5216631336335,62.2744447382207,12.));
#106772=CARTESIAN_POINT('Ctrl Pts',(40.5258172381564,62.3018501471877,0.));
#106773=CARTESIAN_POINT('Ctrl Pts',(40.5258172381564,62.3018501471877,12.));
#106774=CARTESIAN_POINT('Ctrl Pts',(40.5299517857793,62.3292937258021,0.));
#106775=CARTESIAN_POINT('Ctrl Pts',(40.5299517857793,62.3292937258021,12.));
#106776=CARTESIAN_POINT('Ctrl Pts',(40.5340667194272,62.35677539702,0.));
#106777=CARTESIAN_POINT('Ctrl Pts',(40.5340667194272,62.35677539702,12.));
#106778=CARTESIAN_POINT('Ctrl Pts',(40.5381619973972,62.3842950992505,0.));
#106779=CARTESIAN_POINT('Ctrl Pts',(40.5381619973972,62.3842950992505,12.));
#106780=CARTESIAN_POINT('Ctrl Pts',(40.5422375944697,62.4118527880601,0.));
#106781=CARTESIAN_POINT('Ctrl Pts',(40.5422375944697,62.4118527880601,12.));
#106782=CARTESIAN_POINT('Ctrl Pts',(40.5462934972334,62.439448432904,0.));
#106783=CARTESIAN_POINT('Ctrl Pts',(40.5462934972334,62.439448432904,12.));
#106784=CARTESIAN_POINT('Ctrl Pts',(40.5495224601437,62.4615552986669,0.));
#106785=CARTESIAN_POINT('Ctrl Pts',(40.5495224601437,62.4615552986669,12.));
#106786=CARTESIAN_POINT('Ctrl Pts',(40.5519353177058,62.4781525155997,0.));
#106787=CARTESIAN_POINT('Ctrl Pts',(40.5519353177058,62.4781525155997,12.));
#106788=CARTESIAN_POINT('Ctrl Pts',(40.5535399497448,62.4892249121863,0.));
#106789=CARTESIAN_POINT('Ctrl Pts',(40.5535399497448,62.4892249121863,12.));
#106790=CARTESIAN_POINT('Ctrl Pts',(40.554341280847,62.494763006804,0.));
#106791=CARTESIAN_POINT('Ctrl Pts',(40.554341280847,62.494763006804,12.));
#106792=CARTESIAN_POINT('',(39.4479504917287,57.8261117662439,0.));
#106793=CARTESIAN_POINT('Ctrl Pts',(39.4479504917287,57.8261117662439,0.));
#106794=CARTESIAN_POINT('Ctrl Pts',(39.4492429618443,57.8297740100947,0.));
#106795=CARTESIAN_POINT('Ctrl Pts',(39.4518277003553,57.8371043151411,0.));
#106796=CARTESIAN_POINT('Ctrl Pts',(39.4557042029652,57.8481172247496,0.));
#106797=CARTESIAN_POINT('Ctrl Pts',(39.4608716627117,57.8628360096803,0.));
#106798=CARTESIAN_POINT('Ctrl Pts',(39.4673289592259,57.8812926637177,0.));
#106799=CARTESIAN_POINT('Ctrl Pts',(39.473784194937,57.8998074670478,0.));
#106800=CARTESIAN_POINT('Ctrl Pts',(39.4802373061058,57.9183803632404,0.));
#106801=CARTESIAN_POINT('Ctrl Pts',(39.4866881842317,57.9370112456631,0.));
#106802=CARTESIAN_POINT('Ctrl Pts',(39.4931366776714,57.9556999583892,0.));
#106803=CARTESIAN_POINT('Ctrl Pts',(39.499582610674,57.974446317937,0.));
#106804=CARTESIAN_POINT('Ctrl Pts',(39.5060257981225,57.9932501298522,0.));
#106805=CARTESIAN_POINT('Ctrl Pts',(39.5124660614976,58.0121112067896,0.));
#106806=CARTESIAN_POINT('Ctrl Pts',(39.5189032457184,58.0310293875262,0.));
#106807=CARTESIAN_POINT('Ctrl Pts',(39.5253372136887,58.0500045308412,0.));
#106808=CARTESIAN_POINT('Ctrl Pts',(39.5317678383217,58.0690365065374,0.));
#106809=CARTESIAN_POINT('Ctrl Pts',(39.5381949959221,58.0881251879921,0.));
#106810=CARTESIAN_POINT('Ctrl Pts',(39.5446185579638,58.1072704428928,0.));
#106811=CARTESIAN_POINT('Ctrl Pts',(39.5510383869505,58.126472128574,0.));
#106812=CARTESIAN_POINT('Ctrl Pts',(39.5574543406981,58.1457300968499,0.));
#106813=CARTESIAN_POINT('Ctrl Pts',(39.563866275018,58.1650441970387,0.));
#106814=CARTESIAN_POINT('Ctrl Pts',(39.5702740467999,58.1844142794338,0.));
#106815=CARTESIAN_POINT('Ctrl Pts',(39.57667751752,58.2038401992457,0.));
#106816=CARTESIAN_POINT('Ctrl Pts',(39.5830765530891,58.2233218164366,0.));
#106817=CARTESIAN_POINT('Ctrl Pts',(39.5894710221713,58.2428589938369,0.));
#106818=CARTESIAN_POINT('Ctrl Pts',(39.5958607950239,58.2624515958419,0.));
#106819=CARTESIAN_POINT('Ctrl Pts',(39.6022457420789,58.2820994868118,0.));
#106820=CARTESIAN_POINT('Ctrl Pts',(39.6086257327583,58.3018025297324,0.));
#106821=CARTESIAN_POINT('Ctrl Pts',(39.6150006360914,58.3215605869221,0.));
#106822=CARTESIAN_POINT('Ctrl Pts',(39.6213703212531,58.3413735206424,0.));
#106823=CARTESIAN_POINT('Ctrl Pts',(39.6277346580892,58.3612411936905,0.));
#106824=CARTESIAN_POINT('Ctrl Pts',(39.6340935177476,58.3811634701037,0.));
#106825=CARTESIAN_POINT('Ctrl Pts',(39.6404467729094,58.4011402154196,0.));
#106826=CARTESIAN_POINT('Ctrl Pts',(39.6467942974451,58.4211712963004,0.));
#106827=CARTESIAN_POINT('Ctrl Pts',(39.653135966204,58.4412565802979,0.));
#106828=CARTESIAN_POINT('Ctrl Pts',(39.6594716547689,58.4613959355788,0.));
#106829=CARTESIAN_POINT('Ctrl Pts',(39.6658012391815,58.4815892306066,0.));
#106830=CARTESIAN_POINT('Ctrl Pts',(39.6721245959531,58.5018363341604,0.));
#106831=CARTESIAN_POINT('Ctrl Pts',(39.6784416021826,58.5221371154761,0.));
#106832=CARTESIAN_POINT('Ctrl Pts',(39.6847521356395,58.5424914443415,0.));
#106833=CARTESIAN_POINT('Ctrl Pts',(39.6910560748629,58.5628991912052,0.));
#106834=CARTESIAN_POINT('Ctrl Pts',(39.6973532992539,58.5833602272744,0.));
#106835=CARTESIAN_POINT('Ctrl Pts',(39.7036436890232,58.6038744244659,0.));
#106836=CARTESIAN_POINT('Ctrl Pts',(39.7099271251413,58.6244416553562,0.));
#106837=CARTESIAN_POINT('Ctrl Pts',(39.7162034892899,58.6450617931274,0.));
#106838=CARTESIAN_POINT('Ctrl Pts',(39.72247266381,58.6657347115034,0.));
#106839=CARTESIAN_POINT('Ctrl Pts',(39.7287345316681,58.6864602847088,0.));
#106840=CARTESIAN_POINT('Ctrl Pts',(39.7349889764749,58.7072383875027,0.));
#106841=CARTESIAN_POINT('Ctrl Pts',(39.7412358824953,58.7280688951916,0.));
#106842=CARTESIAN_POINT('Ctrl Pts',(39.7474751346598,58.7489516836445,0.));
#106843=CARTESIAN_POINT('Ctrl Pts',(39.7537066185812,58.7698866293029,0.));
#106844=CARTESIAN_POINT('Ctrl Pts',(39.759930220552,58.7908736091798,0.));
#106845=CARTESIAN_POINT('Ctrl Pts',(39.7661458275274,58.8119125008517,0.));
#106846=CARTESIAN_POINT('Ctrl Pts',(39.772353327112,58.8330031824453,0.));
#106847=CARTESIAN_POINT('Ctrl Pts',(39.7785526075478,58.8541455326231,0.));
#106848=CARTESIAN_POINT('Ctrl Pts',(39.7847435576996,58.8753394305586,0.));
#106849=CARTESIAN_POINT('Ctrl Pts',(39.7909260670517,58.8965847559391,0.));
#106850=CARTESIAN_POINT('Ctrl Pts',(39.7971000257044,58.9178813889704,0.));
#106851=CARTESIAN_POINT('Ctrl Pts',(39.8032653243712,58.9392292103747,0.));
#106852=CARTESIAN_POINT('Ctrl Pts',(39.8094218543782,58.9606281013875,0.));
#106853=CARTESIAN_POINT('Ctrl Pts',(39.8155695076626,58.9820779437485,0.));
#106854=CARTESIAN_POINT('Ctrl Pts',(39.821708176766,59.0035786197024,0.));
#106855=CARTESIAN_POINT('Ctrl Pts',(39.8278377548262,59.0251300119973,0.));
#106856=CARTESIAN_POINT('Ctrl Pts',(39.8339581355715,59.0467320038784,0.));
#106857=CARTESIAN_POINT('Ctrl Pts',(39.8400692133139,59.0683844790764,0.));
#106858=CARTESIAN_POINT('Ctrl Pts',(39.8461708829456,59.0900873217981,0.));
#106859=CARTESIAN_POINT('Ctrl Pts',(39.8522630399328,59.1118404167292,0.));
#106860=CARTESIAN_POINT('Ctrl Pts',(39.8583455803105,59.1336436490342,0.));
#106861=CARTESIAN_POINT('Ctrl Pts',(39.8644184006786,59.1554969043522,0.));
#106862=CARTESIAN_POINT('Ctrl Pts',(39.8704813981988,59.1774000687879,0.));
#106863=CARTESIAN_POINT('Ctrl Pts',(39.8765344705909,59.1993530289029,0.));
#106864=CARTESIAN_POINT('Ctrl Pts',(39.8825775161267,59.2213556717209,0.));
#106865=CARTESIAN_POINT('Ctrl Pts',(39.8886104336242,59.2434078847247,0.));
#106866=CARTESIAN_POINT('Ctrl Pts',(39.8946331224438,59.2655095558521,0.));
#106867=CARTESIAN_POINT('Ctrl Pts',(39.9006454824845,59.2876605734847,0.));
#106868=CARTESIAN_POINT('Ctrl Pts',(39.9066474141803,59.3098608264419,0.));
#106869=CARTESIAN_POINT('Ctrl Pts',(39.9126388184936,59.3321102039852,0.));
#106870=CARTESIAN_POINT('Ctrl Pts',(39.9186195969104,59.3544085958151,0.));
#106871=CARTESIAN_POINT('Ctrl Pts',(39.9245896514367,59.3767558920675,0.));
#106872=CARTESIAN_POINT('Ctrl Pts',(39.9305488845958,59.3991519833016,0.));
#106873=CARTESIAN_POINT('Ctrl Pts',(39.9364971994242,59.4215967604968,0.));
#106874=CARTESIAN_POINT('Ctrl Pts',(39.9424344994672,59.4440901150582,0.));
#106875=CARTESIAN_POINT('Ctrl Pts',(39.9483606887737,59.4666319388133,0.));
#106876=CARTESIAN_POINT('Ctrl Pts',(39.9542756718922,59.4892221240069,0.));
#106877=CARTESIAN_POINT('Ctrl Pts',(39.9601793538682,59.5118605632891,0.));
#106878=CARTESIAN_POINT('Ctrl Pts',(39.9660716402403,59.5345471497129,0.));
#106879=CARTESIAN_POINT('Ctrl Pts',(39.9719524370345,59.5572817767388,0.));
#106880=CARTESIAN_POINT('Ctrl Pts',(39.9778216507605,59.5800643382315,0.));
#106881=CARTESIAN_POINT('Ctrl Pts',(39.9836791884079,59.6028947284562,0.));
#106882=CARTESIAN_POINT('Ctrl Pts',(39.9895249574448,59.6257728420669,0.));
#106883=CARTESIAN_POINT('Ctrl Pts',(39.9953588658131,59.6486985741041,0.));
#106884=CARTESIAN_POINT('Ctrl Pts',(40.0011808219241,59.6716718200005,0.));
#106885=CARTESIAN_POINT('Ctrl Pts',(40.0069907346537,59.6946924755773,0.));
#106886=CARTESIAN_POINT('Ctrl Pts',(40.0127885133403,59.7177604370403,0.));
#106887=CARTESIAN_POINT('Ctrl Pts',(40.0185740677821,59.7408756009679,0.));
#106888=CARTESIAN_POINT('Ctrl Pts',(40.0243473082337,59.7640378643106,0.));
#106889=CARTESIAN_POINT('Ctrl Pts',(40.0301081454002,59.7872471243942,0.));
#106890=CARTESIAN_POINT('Ctrl Pts',(40.035856490434,59.8105032789179,0.));
#106891=CARTESIAN_POINT('Ctrl Pts',(40.0415922549314,59.8338062259493,0.));
#106892=CARTESIAN_POINT('Ctrl Pts',(40.0473153509324,59.8571558639145,0.));
#106893=CARTESIAN_POINT('Ctrl Pts',(40.053025690916,59.8805520915972,0.));
#106894=CARTESIAN_POINT('Ctrl Pts',(40.0587231877959,59.9039948081428,0.));
#106895=CARTESIAN_POINT('Ctrl Pts',(40.0644077549158,59.927483913055,0.));
#106896=CARTESIAN_POINT('Ctrl Pts',(40.0700793060475,59.9510193061929,0.));
#106897=CARTESIAN_POINT('Ctrl Pts',(40.0757377553893,59.974600887759,0.));
#106898=CARTESIAN_POINT('Ctrl Pts',(40.0813830175629,59.9982285582991,0.));
#106899=CARTESIAN_POINT('Ctrl Pts',(40.0870150076078,60.0219022187066,0.));
#106900=CARTESIAN_POINT('Ctrl Pts',(40.0926336409787,60.0456217702203,0.));
#106901=CARTESIAN_POINT('Ctrl Pts',(40.0982388335421,60.0693871144207,0.));
#106902=CARTESIAN_POINT('Ctrl Pts',(40.1038305015763,60.0931981532194,0.));
#106903=CARTESIAN_POINT('Ctrl Pts',(40.1094085617672,60.1170547888572,0.));
#106904=CARTESIAN_POINT('Ctrl Pts',(40.1149729312036,60.1409569239093,0.));
#106905=CARTESIAN_POINT('Ctrl Pts',(40.120523527374,60.164904461283,0.));
#106906=CARTESIAN_POINT('Ctrl Pts',(40.1260602681644,60.1888973042151,0.));
#106907=CARTESIAN_POINT('Ctrl Pts',(40.1315830718575,60.2129353562618,0.));
#106908=CARTESIAN_POINT('Ctrl Pts',(40.13709185713,60.2370185212957,0.));
#106909=CARTESIAN_POINT('Ctrl Pts',(40.1425865430468,60.2611467035109,0.));
#106910=CARTESIAN_POINT('Ctrl Pts',(40.1480670490583,60.2853198074216,0.));
#106911=CARTESIAN_POINT('Ctrl Pts',(40.1535332949978,60.3095377378589,0.));
#106912=CARTESIAN_POINT('Ctrl Pts',(40.158985201081,60.3338003999616,0.));
#106913=CARTESIAN_POINT('Ctrl Pts',(40.1644226879043,60.3581076991731,0.));
#106914=CARTESIAN_POINT('Ctrl Pts',(40.1698456764387,60.382459541246,0.));
#106915=CARTESIAN_POINT('Ctrl Pts',(40.1752540880273,60.4068558322415,0.));
#106916=CARTESIAN_POINT('Ctrl Pts',(40.1806478443828,60.4312964785269,0.));
#106917=CARTESIAN_POINT('Ctrl Pts',(40.1860268675875,60.4557813867677,0.));
#106918=CARTESIAN_POINT('Ctrl Pts',(40.1913910800911,60.4803104639211,0.));
#106919=CARTESIAN_POINT('Ctrl Pts',(40.1967404047055,60.5048836172424,0.));
#106920=CARTESIAN_POINT('Ctrl Pts',(40.2020747646012,60.5295007542838,0.));
#106921=CARTESIAN_POINT('Ctrl Pts',(40.2073940833054,60.5541617828927,0.));
#106922=CARTESIAN_POINT('Ctrl Pts',(40.2126982847012,60.5788666112043,0.));
#106923=CARTESIAN_POINT('Ctrl Pts',(40.2179872930271,60.6036151476347,0.));
#106924=CARTESIAN_POINT('Ctrl Pts',(40.2232610328717,60.6284073008865,0.));
#106925=CARTESIAN_POINT('Ctrl Pts',(40.2285194291702,60.6532429799494,0.));
#106926=CARTESIAN_POINT('Ctrl Pts',(40.2337624072029,60.678122094098,0.));
#106927=CARTESIAN_POINT('Ctrl Pts',(40.2389898925937,60.7030445528863,0.));
#106928=CARTESIAN_POINT('Ctrl Pts',(40.2442018113116,60.7280102661401,0.));
#106929=CARTESIAN_POINT('Ctrl Pts',(40.2493980896646,60.7530191439603,0.));
#106930=CARTESIAN_POINT('Ctrl Pts',(40.2545786542957,60.7780710967253,0.));
#106931=CARTESIAN_POINT('Ctrl Pts',(40.2597434321803,60.8031660350879,0.));
#106932=CARTESIAN_POINT('Ctrl Pts',(40.2648923506245,60.8283038699703,0.));
#106933=CARTESIAN_POINT('Ctrl Pts',(40.2700253372644,60.8534845125535,0.));
#106934=CARTESIAN_POINT('Ctrl Pts',(40.2751423200637,60.8787078742817,0.));
#106935=CARTESIAN_POINT('Ctrl Pts',(40.2802432273104,60.903973866867,0.));
#106936=CARTESIAN_POINT('Ctrl Pts',(40.2853279876161,60.9292824022888,0.));
#106937=CARTESIAN_POINT('Ctrl Pts',(40.2903965299155,60.9546333927919,0.));
#106938=CARTESIAN_POINT('Ctrl Pts',(40.2954487834688,60.9800267508781,0.));
#106939=CARTESIAN_POINT('Ctrl Pts',(40.3004846778577,61.005462389306,0.));
#106940=CARTESIAN_POINT('Ctrl Pts',(40.3055041429772,61.0309402210915,0.));
#106941=CARTESIAN_POINT('Ctrl Pts',(40.3105071090308,61.0564601595047,0.));
#106942=CARTESIAN_POINT('Ctrl Pts',(40.3154935065263,61.0820221180647,0.));
#106943=CARTESIAN_POINT('Ctrl Pts',(40.3204632662729,61.1076260105265,0.));
#106944=CARTESIAN_POINT('Ctrl Pts',(40.3254163193805,61.1332717508799,0.));
#106945=CARTESIAN_POINT('Ctrl Pts',(40.3303525972621,61.1589592533623,0.));
#106946=CARTESIAN_POINT('Ctrl Pts',(40.3352720316373,61.184688432465,0.));
#106947=CARTESIAN_POINT('Ctrl Pts',(40.3401745545369,61.2104592029376,0.));
#106948=CARTESIAN_POINT('Ctrl Pts',(40.3450600983104,61.2362714797891,0.));
#106949=CARTESIAN_POINT('Ctrl Pts',(40.3499285956297,61.262125178285,0.));
#106950=CARTESIAN_POINT('Ctrl Pts',(40.3547799794672,61.2880202139358,0.));
#106951=CARTESIAN_POINT('Ctrl Pts',(40.3596141830786,61.3139565024838,0.));
#106952=CARTESIAN_POINT('Ctrl Pts',(40.364431139986,61.3399339598852,0.));
#106953=CARTESIAN_POINT('Ctrl Pts',(40.3692307839642,61.3659525022917,0.));
#106954=CARTESIAN_POINT('Ctrl Pts',(40.3740130490233,61.3920120460232,0.));
#106955=CARTESIAN_POINT('Ctrl Pts',(40.3787778694372,61.418112507605,0.));
#106956=CARTESIAN_POINT('Ctrl Pts',(40.3835251797725,61.4442538038053,0.));
#106957=CARTESIAN_POINT('Ctrl Pts',(40.3882549149229,61.4704358516711,0.));
#106958=CARTESIAN_POINT('Ctrl Pts',(40.3929670101363,61.4966585685545,0.));
#106959=CARTESIAN_POINT('Ctrl Pts',(40.3976614010648,61.5229218721532,0.));
#106960=CARTESIAN_POINT('Ctrl Pts',(40.4023380237227,61.5492256804709,0.));
#106961=CARTESIAN_POINT('Ctrl Pts',(40.4069968143953,61.5755699117318,0.));
#106962=CARTESIAN_POINT('Ctrl Pts',(40.4116377095595,61.6019544843009,0.));
#106963=CARTESIAN_POINT('Ctrl Pts',(40.4162606458119,61.628379316608,0.));
#106964=CARTESIAN_POINT('Ctrl Pts',(40.420865559772,61.6548443270397,0.));
#106965=CARTESIAN_POINT('Ctrl Pts',(40.4254523880766,61.6813494339295,0.));
#106966=CARTESIAN_POINT('Ctrl Pts',(40.4300210675848,61.7078945557812,0.));
#106967=CARTESIAN_POINT('Ctrl Pts',(40.4345715355411,61.7344796114409,0.));
#106968=CARTESIAN_POINT('Ctrl Pts',(40.4391037297589,61.7611045202875,0.));
#106969=CARTESIAN_POINT('Ctrl Pts',(40.4436175887942,61.7877692024064,0.));
#106970=CARTESIAN_POINT('Ctrl Pts',(40.448113052135,61.8144735787767,0.));
#106971=CARTESIAN_POINT('Ctrl Pts',(40.4525900597877,61.8412175708524,0.));
#106972=CARTESIAN_POINT('Ctrl Pts',(40.4570485518735,61.8680011001513,0.));
#106973=CARTESIAN_POINT('Ctrl Pts',(40.4614884681884,61.8948240877998,0.));
#106974=CARTESIAN_POINT('Ctrl Pts',(40.4659097478595,61.9216864541758,0.));
#106975=CARTESIAN_POINT('Ctrl Pts',(40.4703123287642,61.9485881182957,0.));
#106976=CARTESIAN_POINT('Ctrl Pts',(40.4746961480045,61.9755289983094,0.));
#106977=CARTESIAN_POINT('Ctrl Pts',(40.4790611429613,62.0025090126008,0.));
#106978=CARTESIAN_POINT('Ctrl Pts',(40.4834072522181,62.0295280807449,0.));
#106979=CARTESIAN_POINT('Ctrl Pts',(40.4877344164407,62.0565861244171,0.));
#106980=CARTESIAN_POINT('Ctrl Pts',(40.4920425795184,62.0836830685665,0.));
#106981=CARTESIAN_POINT('Ctrl Pts',(40.4963316888356,62.110818841691,0.));
#106982=CARTESIAN_POINT('Ctrl Pts',(40.4999919096189,62.1341126810362,0.));
#106983=CARTESIAN_POINT('Ctrl Pts',(40.5027877865723,62.1519925002733,0.));
#106984=CARTESIAN_POINT('Ctrl Pts',(40.5047277935687,62.1644411502524,0.));
#106985=CARTESIAN_POINT('Ctrl Pts',(40.5058175523044,62.1714473137745,0.));
#106986=CARTESIAN_POINT('Ctrl Pts',(40.5060598100837,62.1730054756444,0.));
#106987=CARTESIAN_POINT('',(39.4479504917287,57.8261117662439,12.));
#106988=CARTESIAN_POINT('',(39.4479504917287,57.8261117662439,0.));
#106989=CARTESIAN_POINT('Ctrl Pts',(40.5060598100837,62.1730054756444,12.));
#106990=CARTESIAN_POINT('Ctrl Pts',(40.5058175523044,62.1714473137745,12.));
#106991=CARTESIAN_POINT('Ctrl Pts',(40.5047277935687,62.1644411502524,12.));
#106992=CARTESIAN_POINT('Ctrl Pts',(40.5027877865723,62.1519925002733,12.));
#106993=CARTESIAN_POINT('Ctrl Pts',(40.4999919096189,62.1341126810362,12.));
#106994=CARTESIAN_POINT('Ctrl Pts',(40.4963316888356,62.110818841691,12.));
#106995=CARTESIAN_POINT('Ctrl Pts',(40.4920425795184,62.0836830685665,12.));
#106996=CARTESIAN_POINT('Ctrl Pts',(40.4877344164407,62.0565861244171,12.));
#106997=CARTESIAN_POINT('Ctrl Pts',(40.4834072522181,62.0295280807449,12.));
#106998=CARTESIAN_POINT('Ctrl Pts',(40.4790611429613,62.0025090126008,12.));
#106999=CARTESIAN_POINT('Ctrl Pts',(40.4746961480045,61.9755289983094,12.));
#107000=CARTESIAN_POINT('Ctrl Pts',(40.4703123287642,61.9485881182957,12.));
#107001=CARTESIAN_POINT('Ctrl Pts',(40.4659097478595,61.9216864541758,12.));
#107002=CARTESIAN_POINT('Ctrl Pts',(40.4614884681884,61.8948240877998,12.));
#107003=CARTESIAN_POINT('Ctrl Pts',(40.4570485518735,61.8680011001513,12.));
#107004=CARTESIAN_POINT('Ctrl Pts',(40.4525900597877,61.8412175708524,12.));
#107005=CARTESIAN_POINT('Ctrl Pts',(40.448113052135,61.8144735787767,12.));
#107006=CARTESIAN_POINT('Ctrl Pts',(40.4436175887942,61.7877692024064,12.));
#107007=CARTESIAN_POINT('Ctrl Pts',(40.4391037297589,61.7611045202875,12.));
#107008=CARTESIAN_POINT('Ctrl Pts',(40.4345715355411,61.7344796114409,12.));
#107009=CARTESIAN_POINT('Ctrl Pts',(40.4300210675848,61.7078945557812,12.));
#107010=CARTESIAN_POINT('Ctrl Pts',(40.4254523880766,61.6813494339295,12.));
#107011=CARTESIAN_POINT('Ctrl Pts',(40.420865559772,61.6548443270397,12.));
#107012=CARTESIAN_POINT('Ctrl Pts',(40.4162606458119,61.628379316608,12.));
#107013=CARTESIAN_POINT('Ctrl Pts',(40.4116377095595,61.6019544843009,12.));
#107014=CARTESIAN_POINT('Ctrl Pts',(40.4069968143953,61.5755699117318,12.));
#107015=CARTESIAN_POINT('Ctrl Pts',(40.4023380237227,61.5492256804709,12.));
#107016=CARTESIAN_POINT('Ctrl Pts',(40.3976614010648,61.5229218721532,12.));
#107017=CARTESIAN_POINT('Ctrl Pts',(40.3929670101363,61.4966585685545,12.));
#107018=CARTESIAN_POINT('Ctrl Pts',(40.3882549149229,61.4704358516711,12.));
#107019=CARTESIAN_POINT('Ctrl Pts',(40.3835251797725,61.4442538038053,12.));
#107020=CARTESIAN_POINT('Ctrl Pts',(40.3787778694372,61.418112507605,12.));
#107021=CARTESIAN_POINT('Ctrl Pts',(40.3740130490233,61.3920120460232,12.));
#107022=CARTESIAN_POINT('Ctrl Pts',(40.3692307839642,61.3659525022917,12.));
#107023=CARTESIAN_POINT('Ctrl Pts',(40.364431139986,61.3399339598852,12.));
#107024=CARTESIAN_POINT('Ctrl Pts',(40.3596141830786,61.3139565024838,12.));
#107025=CARTESIAN_POINT('Ctrl Pts',(40.3547799794672,61.2880202139358,12.));
#107026=CARTESIAN_POINT('Ctrl Pts',(40.3499285956297,61.262125178285,12.));
#107027=CARTESIAN_POINT('Ctrl Pts',(40.3450600983104,61.2362714797891,12.));
#107028=CARTESIAN_POINT('Ctrl Pts',(40.3401745545369,61.2104592029376,12.));
#107029=CARTESIAN_POINT('Ctrl Pts',(40.3352720316373,61.184688432465,12.));
#107030=CARTESIAN_POINT('Ctrl Pts',(40.3303525972621,61.1589592533623,12.));
#107031=CARTESIAN_POINT('Ctrl Pts',(40.3254163193805,61.1332717508799,12.));
#107032=CARTESIAN_POINT('Ctrl Pts',(40.3204632662729,61.1076260105265,12.));
#107033=CARTESIAN_POINT('Ctrl Pts',(40.3154935065263,61.0820221180647,12.));
#107034=CARTESIAN_POINT('Ctrl Pts',(40.3105071090308,61.0564601595047,12.));
#107035=CARTESIAN_POINT('Ctrl Pts',(40.3055041429772,61.0309402210915,12.));
#107036=CARTESIAN_POINT('Ctrl Pts',(40.3004846778577,61.005462389306,12.));
#107037=CARTESIAN_POINT('Ctrl Pts',(40.2954487834688,60.9800267508781,12.));
#107038=CARTESIAN_POINT('Ctrl Pts',(40.2903965299155,60.9546333927919,12.));
#107039=CARTESIAN_POINT('Ctrl Pts',(40.2853279876161,60.9292824022888,12.));
#107040=CARTESIAN_POINT('Ctrl Pts',(40.2802432273104,60.903973866867,12.));
#107041=CARTESIAN_POINT('Ctrl Pts',(40.2751423200637,60.8787078742817,12.));
#107042=CARTESIAN_POINT('Ctrl Pts',(40.2700253372644,60.8534845125535,12.));
#107043=CARTESIAN_POINT('Ctrl Pts',(40.2648923506245,60.8283038699703,12.));
#107044=CARTESIAN_POINT('Ctrl Pts',(40.2597434321803,60.8031660350879,12.));
#107045=CARTESIAN_POINT('Ctrl Pts',(40.2545786542957,60.7780710967253,12.));
#107046=CARTESIAN_POINT('Ctrl Pts',(40.2493980896646,60.7530191439603,12.));
#107047=CARTESIAN_POINT('Ctrl Pts',(40.2442018113116,60.7280102661401,12.));
#107048=CARTESIAN_POINT('Ctrl Pts',(40.2389898925937,60.7030445528863,12.));
#107049=CARTESIAN_POINT('Ctrl Pts',(40.2337624072029,60.678122094098,12.));
#107050=CARTESIAN_POINT('Ctrl Pts',(40.2285194291702,60.6532429799494,12.));
#107051=CARTESIAN_POINT('Ctrl Pts',(40.2232610328717,60.6284073008865,12.));
#107052=CARTESIAN_POINT('Ctrl Pts',(40.2179872930271,60.6036151476347,12.));
#107053=CARTESIAN_POINT('Ctrl Pts',(40.2126982847012,60.5788666112043,12.));
#107054=CARTESIAN_POINT('Ctrl Pts',(40.2073940833054,60.5541617828927,12.));
#107055=CARTESIAN_POINT('Ctrl Pts',(40.2020747646012,60.5295007542838,12.));
#107056=CARTESIAN_POINT('Ctrl Pts',(40.1967404047055,60.5048836172424,12.));
#107057=CARTESIAN_POINT('Ctrl Pts',(40.1913910800911,60.4803104639211,12.));
#107058=CARTESIAN_POINT('Ctrl Pts',(40.1860268675875,60.4557813867677,12.));
#107059=CARTESIAN_POINT('Ctrl Pts',(40.1806478443828,60.4312964785269,12.));
#107060=CARTESIAN_POINT('Ctrl Pts',(40.1752540880273,60.4068558322415,12.));
#107061=CARTESIAN_POINT('Ctrl Pts',(40.1698456764387,60.382459541246,12.));
#107062=CARTESIAN_POINT('Ctrl Pts',(40.1644226879043,60.3581076991731,12.));
#107063=CARTESIAN_POINT('Ctrl Pts',(40.158985201081,60.3338003999616,12.));
#107064=CARTESIAN_POINT('Ctrl Pts',(40.1535332949978,60.3095377378589,12.));
#107065=CARTESIAN_POINT('Ctrl Pts',(40.1480670490583,60.2853198074216,12.));
#107066=CARTESIAN_POINT('Ctrl Pts',(40.1425865430468,60.2611467035109,12.));
#107067=CARTESIAN_POINT('Ctrl Pts',(40.13709185713,60.2370185212957,12.));
#107068=CARTESIAN_POINT('Ctrl Pts',(40.1315830718575,60.2129353562618,12.));
#107069=CARTESIAN_POINT('Ctrl Pts',(40.1260602681644,60.1888973042151,12.));
#107070=CARTESIAN_POINT('Ctrl Pts',(40.120523527374,60.164904461283,12.));
#107071=CARTESIAN_POINT('Ctrl Pts',(40.1149729312036,60.1409569239093,12.));
#107072=CARTESIAN_POINT('Ctrl Pts',(40.1094085617672,60.1170547888572,12.));
#107073=CARTESIAN_POINT('Ctrl Pts',(40.1038305015763,60.0931981532194,12.));
#107074=CARTESIAN_POINT('Ctrl Pts',(40.0982388335421,60.0693871144207,12.));
#107075=CARTESIAN_POINT('Ctrl Pts',(40.0926336409787,60.0456217702203,12.));
#107076=CARTESIAN_POINT('Ctrl Pts',(40.0870150076078,60.0219022187066,12.));
#107077=CARTESIAN_POINT('Ctrl Pts',(40.0813830175629,59.9982285582991,12.));
#107078=CARTESIAN_POINT('Ctrl Pts',(40.0757377553893,59.974600887759,12.));
#107079=CARTESIAN_POINT('Ctrl Pts',(40.0700793060475,59.9510193061929,12.));
#107080=CARTESIAN_POINT('Ctrl Pts',(40.0644077549158,59.927483913055,12.));
#107081=CARTESIAN_POINT('Ctrl Pts',(40.0587231877959,59.9039948081428,12.));
#107082=CARTESIAN_POINT('Ctrl Pts',(40.053025690916,59.8805520915972,12.));
#107083=CARTESIAN_POINT('Ctrl Pts',(40.0473153509324,59.8571558639145,12.));
#107084=CARTESIAN_POINT('Ctrl Pts',(40.0415922549314,59.8338062259493,12.));
#107085=CARTESIAN_POINT('Ctrl Pts',(40.035856490434,59.8105032789179,12.));
#107086=CARTESIAN_POINT('Ctrl Pts',(40.0301081454002,59.7872471243942,12.));
#107087=CARTESIAN_POINT('Ctrl Pts',(40.0243473082337,59.7640378643106,12.));
#107088=CARTESIAN_POINT('Ctrl Pts',(40.0185740677821,59.7408756009679,12.));
#107089=CARTESIAN_POINT('Ctrl Pts',(40.0127885133403,59.7177604370403,12.));
#107090=CARTESIAN_POINT('Ctrl Pts',(40.0069907346537,59.6946924755773,12.));
#107091=CARTESIAN_POINT('Ctrl Pts',(40.0011808219241,59.6716718200005,12.));
#107092=CARTESIAN_POINT('Ctrl Pts',(39.9953588658131,59.6486985741041,12.));
#107093=CARTESIAN_POINT('Ctrl Pts',(39.9895249574448,59.6257728420669,12.));
#107094=CARTESIAN_POINT('Ctrl Pts',(39.9836791884079,59.6028947284562,12.));
#107095=CARTESIAN_POINT('Ctrl Pts',(39.9778216507605,59.5800643382315,12.));
#107096=CARTESIAN_POINT('Ctrl Pts',(39.9719524370345,59.5572817767388,12.));
#107097=CARTESIAN_POINT('Ctrl Pts',(39.9660716402403,59.5345471497129,12.));
#107098=CARTESIAN_POINT('Ctrl Pts',(39.9601793538682,59.5118605632891,12.));
#107099=CARTESIAN_POINT('Ctrl Pts',(39.9542756718922,59.4892221240069,12.));
#107100=CARTESIAN_POINT('Ctrl Pts',(39.9483606887737,59.4666319388133,12.));
#107101=CARTESIAN_POINT('Ctrl Pts',(39.9424344994672,59.4440901150582,12.));
#107102=CARTESIAN_POINT('Ctrl Pts',(39.9364971994242,59.4215967604968,12.));
#107103=CARTESIAN_POINT('Ctrl Pts',(39.9305488845958,59.3991519833016,12.));
#107104=CARTESIAN_POINT('Ctrl Pts',(39.9245896514367,59.3767558920675,12.));
#107105=CARTESIAN_POINT('Ctrl Pts',(39.9186195969104,59.3544085958151,12.));
#107106=CARTESIAN_POINT('Ctrl Pts',(39.9126388184936,59.3321102039852,12.));
#107107=CARTESIAN_POINT('Ctrl Pts',(39.9066474141803,59.3098608264419,12.));
#107108=CARTESIAN_POINT('Ctrl Pts',(39.9006454824845,59.2876605734847,12.));
#107109=CARTESIAN_POINT('Ctrl Pts',(39.8946331224438,59.2655095558521,12.));
#107110=CARTESIAN_POINT('Ctrl Pts',(39.8886104336242,59.2434078847247,12.));
#107111=CARTESIAN_POINT('Ctrl Pts',(39.8825775161267,59.2213556717209,12.));
#107112=CARTESIAN_POINT('Ctrl Pts',(39.8765344705909,59.1993530289029,12.));
#107113=CARTESIAN_POINT('Ctrl Pts',(39.8704813981988,59.1774000687879,12.));
#107114=CARTESIAN_POINT('Ctrl Pts',(39.8644184006786,59.1554969043522,12.));
#107115=CARTESIAN_POINT('Ctrl Pts',(39.8583455803105,59.1336436490342,12.));
#107116=CARTESIAN_POINT('Ctrl Pts',(39.8522630399328,59.1118404167292,12.));
#107117=CARTESIAN_POINT('Ctrl Pts',(39.8461708829456,59.0900873217981,12.));
#107118=CARTESIAN_POINT('Ctrl Pts',(39.8400692133139,59.0683844790764,12.));
#107119=CARTESIAN_POINT('Ctrl Pts',(39.8339581355715,59.0467320038784,12.));
#107120=CARTESIAN_POINT('Ctrl Pts',(39.8278377548262,59.0251300119973,12.));
#107121=CARTESIAN_POINT('Ctrl Pts',(39.821708176766,59.0035786197024,12.));
#107122=CARTESIAN_POINT('Ctrl Pts',(39.8155695076626,58.9820779437485,12.));
#107123=CARTESIAN_POINT('Ctrl Pts',(39.8094218543782,58.9606281013875,12.));
#107124=CARTESIAN_POINT('Ctrl Pts',(39.8032653243712,58.9392292103747,12.));
#107125=CARTESIAN_POINT('Ctrl Pts',(39.7971000257044,58.9178813889704,12.));
#107126=CARTESIAN_POINT('Ctrl Pts',(39.7909260670517,58.8965847559391,12.));
#107127=CARTESIAN_POINT('Ctrl Pts',(39.7847435576996,58.8753394305586,12.));
#107128=CARTESIAN_POINT('Ctrl Pts',(39.7785526075478,58.8541455326231,12.));
#107129=CARTESIAN_POINT('Ctrl Pts',(39.772353327112,58.8330031824453,12.));
#107130=CARTESIAN_POINT('Ctrl Pts',(39.7661458275274,58.8119125008517,12.));
#107131=CARTESIAN_POINT('Ctrl Pts',(39.759930220552,58.7908736091798,12.));
#107132=CARTESIAN_POINT('Ctrl Pts',(39.7537066185812,58.7698866293029,12.));
#107133=CARTESIAN_POINT('Ctrl Pts',(39.7474751346598,58.7489516836445,12.));
#107134=CARTESIAN_POINT('Ctrl Pts',(39.7412358824953,58.7280688951916,12.));
#107135=CARTESIAN_POINT('Ctrl Pts',(39.7349889764749,58.7072383875027,12.));
#107136=CARTESIAN_POINT('Ctrl Pts',(39.7287345316681,58.6864602847088,12.));
#107137=CARTESIAN_POINT('Ctrl Pts',(39.72247266381,58.6657347115034,12.));
#107138=CARTESIAN_POINT('Ctrl Pts',(39.7162034892899,58.6450617931274,12.));
#107139=CARTESIAN_POINT('Ctrl Pts',(39.7099271251413,58.6244416553562,12.));
#107140=CARTESIAN_POINT('Ctrl Pts',(39.7036436890232,58.6038744244659,12.));
#107141=CARTESIAN_POINT('Ctrl Pts',(39.6973532992539,58.5833602272744,12.));
#107142=CARTESIAN_POINT('Ctrl Pts',(39.6910560748629,58.5628991912052,12.));
#107143=CARTESIAN_POINT('Ctrl Pts',(39.6847521356395,58.5424914443415,12.));
#107144=CARTESIAN_POINT('Ctrl Pts',(39.6784416021826,58.5221371154761,12.));
#107145=CARTESIAN_POINT('Ctrl Pts',(39.6721245959531,58.5018363341604,12.));
#107146=CARTESIAN_POINT('Ctrl Pts',(39.6658012391815,58.4815892306066,12.));
#107147=CARTESIAN_POINT('Ctrl Pts',(39.6594716547689,58.4613959355788,12.));
#107148=CARTESIAN_POINT('Ctrl Pts',(39.653135966204,58.4412565802979,12.));
#107149=CARTESIAN_POINT('Ctrl Pts',(39.6467942974451,58.4211712963004,12.));
#107150=CARTESIAN_POINT('Ctrl Pts',(39.6404467729094,58.4011402154196,12.));
#107151=CARTESIAN_POINT('Ctrl Pts',(39.6340935177476,58.3811634701037,12.));
#107152=CARTESIAN_POINT('Ctrl Pts',(39.6277346580892,58.3612411936905,12.));
#107153=CARTESIAN_POINT('Ctrl Pts',(39.6213703212531,58.3413735206424,12.));
#107154=CARTESIAN_POINT('Ctrl Pts',(39.6150006360914,58.3215605869221,12.));
#107155=CARTESIAN_POINT('Ctrl Pts',(39.6086257327583,58.3018025297324,12.));
#107156=CARTESIAN_POINT('Ctrl Pts',(39.6022457420789,58.2820994868118,12.));
#107157=CARTESIAN_POINT('Ctrl Pts',(39.5958607950239,58.2624515958419,12.));
#107158=CARTESIAN_POINT('Ctrl Pts',(39.5894710221713,58.2428589938369,12.));
#107159=CARTESIAN_POINT('Ctrl Pts',(39.5830765530891,58.2233218164366,12.));
#107160=CARTESIAN_POINT('Ctrl Pts',(39.57667751752,58.2038401992457,12.));
#107161=CARTESIAN_POINT('Ctrl Pts',(39.5702740467999,58.1844142794338,12.));
#107162=CARTESIAN_POINT('Ctrl Pts',(39.563866275018,58.1650441970387,12.));
#107163=CARTESIAN_POINT('Ctrl Pts',(39.5574543406981,58.1457300968499,12.));
#107164=CARTESIAN_POINT('Ctrl Pts',(39.5510383869505,58.126472128574,12.));
#107165=CARTESIAN_POINT('Ctrl Pts',(39.5446185579638,58.1072704428928,12.));
#107166=CARTESIAN_POINT('Ctrl Pts',(39.5381949959221,58.0881251879921,12.));
#107167=CARTESIAN_POINT('Ctrl Pts',(39.5317678383217,58.0690365065374,12.));
#107168=CARTESIAN_POINT('Ctrl Pts',(39.5253372136887,58.0500045308412,12.));
#107169=CARTESIAN_POINT('Ctrl Pts',(39.5189032457184,58.0310293875262,12.));
#107170=CARTESIAN_POINT('Ctrl Pts',(39.5124660614976,58.0121112067896,12.));
#107171=CARTESIAN_POINT('Ctrl Pts',(39.5060257981225,57.9932501298522,12.));
#107172=CARTESIAN_POINT('Ctrl Pts',(39.499582610674,57.974446317937,12.));
#107173=CARTESIAN_POINT('Ctrl Pts',(39.4931366776714,57.9556999583892,12.));
#107174=CARTESIAN_POINT('Ctrl Pts',(39.4866881842317,57.9370112456631,12.));
#107175=CARTESIAN_POINT('Ctrl Pts',(39.4802373061058,57.9183803632404,12.));
#107176=CARTESIAN_POINT('Ctrl Pts',(39.473784194937,57.8998074670478,12.));
#107177=CARTESIAN_POINT('Ctrl Pts',(39.4673289592259,57.8812926637177,12.));
#107178=CARTESIAN_POINT('Ctrl Pts',(39.4608716627117,57.8628360096803,12.));
#107179=CARTESIAN_POINT('Ctrl Pts',(39.4557042029652,57.8481172247496,12.));
#107180=CARTESIAN_POINT('Ctrl Pts',(39.4518277003553,57.8371043151411,12.));
#107181=CARTESIAN_POINT('Ctrl Pts',(39.4492429618443,57.8297740100947,12.));
#107182=CARTESIAN_POINT('Ctrl Pts',(39.4479504917287,57.8261117662439,12.));
#107183=CARTESIAN_POINT('Ctrl Pts',(39.2292784191814,62.9864049293895,-5.55111512312578E-16));
#107184=CARTESIAN_POINT('Ctrl Pts',(39.2292784191814,62.9864049293895,4.));
#107185=CARTESIAN_POINT('Ctrl Pts',(39.2292784191814,62.9864049293895,8.));
#107186=CARTESIAN_POINT('Ctrl Pts',(39.2292784191814,62.9864049293895,12.));
#107187=CARTESIAN_POINT('Ctrl Pts',(39.3205491216487,63.0475916539466,-5.55111512312578E-16));
#107188=CARTESIAN_POINT('Ctrl Pts',(39.3205491216487,63.0475916539466,4.));
#107189=CARTESIAN_POINT('Ctrl Pts',(39.3205491216487,63.0475916539466,8.));
#107190=CARTESIAN_POINT('Ctrl Pts',(39.3205491216487,63.0475916539466,12.));
#107191=CARTESIAN_POINT('Ctrl Pts',(39.5164137621552,63.0996457958587,-5.55111512312578E-16));
#107192=CARTESIAN_POINT('Ctrl Pts',(39.5164137621552,63.0996457958587,4.00000000000001));
#107193=CARTESIAN_POINT('Ctrl Pts',(39.5164137621552,63.0996457958587,8.));
#107194=CARTESIAN_POINT('Ctrl Pts',(39.5164137621552,63.0996457958587,12.));
#107195=CARTESIAN_POINT('Ctrl Pts',(39.704957504468,63.0378706912078,-5.55111512312578E-16));
#107196=CARTESIAN_POINT('Ctrl Pts',(39.704957504468,63.0378706912078,4.));
#107197=CARTESIAN_POINT('Ctrl Pts',(39.704957504468,63.0378706912078,8.00000000000001));
#107198=CARTESIAN_POINT('Ctrl Pts',(39.704957504468,63.0378706912078,12.));
#107199=CARTESIAN_POINT('Ctrl Pts',(39.7746412831482,62.9938720098785,-5.55111512312578E-16));
#107200=CARTESIAN_POINT('Ctrl Pts',(39.7746412831482,62.9938720098785,4.));
#107201=CARTESIAN_POINT('Ctrl Pts',(39.7746412831482,62.9938720098785,8.));
#107202=CARTESIAN_POINT('Ctrl Pts',(39.7746412831482,62.9938720098785,12.));
#107203=CARTESIAN_POINT('',(39.2292784191814,62.9864049293895,2.77555756156289E-16));
#107204=CARTESIAN_POINT('',(39.774641283148,62.9938720098781,0.));
#107205=CARTESIAN_POINT('Ctrl Pts',(39.2292784191814,62.9864049293895,-1.38777878078145E-16));
#107206=CARTESIAN_POINT('Ctrl Pts',(39.3205491216487,63.0475916539466,-1.38777878078145E-16));
#107207=CARTESIAN_POINT('Ctrl Pts',(39.4324717733667,63.0773368778964,-1.38777878078144E-16));
#107208=CARTESIAN_POINT('Ctrl Pts',(39.5420039277153,63.0699133682745,-1.38777878078145E-16));
#107209=CARTESIAN_POINT('Ctrl Pts',(39.6241530434768,63.0643457360582,-1.38777878078145E-16));
#107210=CARTESIAN_POINT('Ctrl Pts',(39.704957504468,63.0378706912078,-1.38777878078145E-16));
#107211=CARTESIAN_POINT('Ctrl Pts',(39.7746412831482,62.9938720098785,-1.38777878078145E-16));
#107212=CARTESIAN_POINT('',(39.774641283148,62.9938720098781,12.));
#107213=CARTESIAN_POINT('Ctrl Pts',(39.7746412831482,62.9938720098785,-5.55111512312578E-16));
#107214=CARTESIAN_POINT('Ctrl Pts',(39.7746412831482,62.9938720098785,4.));
#107215=CARTESIAN_POINT('Ctrl Pts',(39.7746412831482,62.9938720098785,8.));
#107216=CARTESIAN_POINT('Ctrl Pts',(39.7746412831482,62.9938720098785,12.));
#107217=CARTESIAN_POINT('',(39.2292784191814,62.9864049293895,12.));
#107218=CARTESIAN_POINT('Ctrl Pts',(39.7746412831482,62.9938720098785,12.));
#107219=CARTESIAN_POINT('Ctrl Pts',(39.704957504468,63.0378706912078,12.));
#107220=CARTESIAN_POINT('Ctrl Pts',(39.6241530434768,63.0643457360582,12.));
#107221=CARTESIAN_POINT('Ctrl Pts',(39.5420039277153,63.0699133682745,12.));
#107222=CARTESIAN_POINT('Ctrl Pts',(39.4324717733667,63.0773368778964,12.));
#107223=CARTESIAN_POINT('Ctrl Pts',(39.3205491216487,63.0475916539466,12.));
#107224=CARTESIAN_POINT('Ctrl Pts',(39.2292784191814,62.9864049293895,12.));
#107225=CARTESIAN_POINT('Ctrl Pts',(39.2292784191814,62.9864049293895,12.));
#107226=CARTESIAN_POINT('Ctrl Pts',(39.2292784191814,62.9864049293895,8.));
#107227=CARTESIAN_POINT('Ctrl Pts',(39.2292784191814,62.9864049293895,4.));
#107228=CARTESIAN_POINT('Ctrl Pts',(39.2292784191814,62.9864049293895,-5.55111512312578E-16));
#107229=CARTESIAN_POINT('Origin',(2.01319694273778E-10,3.16193356404481E-10,
0.));
#107230=CARTESIAN_POINT('Origin',(2.01319694273778E-10,3.16193356404481E-10,
12.));
#107231=CARTESIAN_POINT('Origin',(2.01319694273778E-10,3.16193356404481E-10,
0.));
#107232=CARTESIAN_POINT('Ctrl Pts',(45.5911481700231,58.9211100416396,0.));
#107233=CARTESIAN_POINT('Ctrl Pts',(45.5911481700231,58.9211100416396,4.));
#107234=CARTESIAN_POINT('Ctrl Pts',(45.591148170023,58.9211100416396,8.));
#107235=CARTESIAN_POINT('Ctrl Pts',(45.591148170023,58.9211100416396,12.));
#107236=CARTESIAN_POINT('Ctrl Pts',(45.6780528262179,58.8538661785412,0.));
#107237=CARTESIAN_POINT('Ctrl Pts',(45.6780528262179,58.8538661785412,4.));
#107238=CARTESIAN_POINT('Ctrl Pts',(45.6780528262179,58.8538661785413,8.00000000000001));
#107239=CARTESIAN_POINT('Ctrl Pts',(45.6780528262179,58.8538661785413,12.));
#107240=CARTESIAN_POINT('Ctrl Pts',(45.7893619681938,58.6845061116498,0.));
#107241=CARTESIAN_POINT('Ctrl Pts',(45.7893619681938,58.6845061116498,4.));
#107242=CARTESIAN_POINT('Ctrl Pts',(45.7893619681937,58.6845061116498,7.99999999999999));
#107243=CARTESIAN_POINT('Ctrl Pts',(45.7893619681937,58.6845061116498,12.));
#107244=CARTESIAN_POINT('Ctrl Pts',(45.7903667155981,58.4861028141708,0.));
#107245=CARTESIAN_POINT('Ctrl Pts',(45.7903667155981,58.4861028141708,4.));
#107246=CARTESIAN_POINT('Ctrl Pts',(45.790366715598,58.486102814171,8.00000000000001));
#107247=CARTESIAN_POINT('Ctrl Pts',(45.790366715598,58.486102814171,12.));
#107248=CARTESIAN_POINT('Ctrl Pts',(45.7706564944768,58.4060826907376,0.));
#107249=CARTESIAN_POINT('Ctrl Pts',(45.7706564944768,58.4060826907376,4.));
#107250=CARTESIAN_POINT('Ctrl Pts',(45.7706564944767,58.4060826907378,8.));
#107251=CARTESIAN_POINT('Ctrl Pts',(45.7706564944767,58.4060826907378,12.));
#107252=CARTESIAN_POINT('',(45.5911481700231,58.9211100416396,0.));
#107253=CARTESIAN_POINT('',(45.7706564944766,58.4060826907377,0.));
#107254=CARTESIAN_POINT('Ctrl Pts',(45.5911481700231,58.9211100416396,2.77555756156289E-16));
#107255=CARTESIAN_POINT('Ctrl Pts',(45.6780528262179,58.8538661785412,2.77555756156289E-16));
#107256=CARTESIAN_POINT('Ctrl Pts',(45.7416580502041,58.7570889974604,2.77555756156289E-16));
#107257=CARTESIAN_POINT('Ctrl Pts',(45.7692455126976,58.6508283125143,2.77555756156289E-16));
#107258=CARTESIAN_POINT('Ctrl Pts',(45.7899361095677,58.5711327988047,2.77555756156289E-16));
#107259=CARTESIAN_POINT('Ctrl Pts',(45.7903667155981,58.4861028141708,2.77555756156289E-16));
#107260=CARTESIAN_POINT('Ctrl Pts',(45.7706564944768,58.4060826907376,2.77555756156289E-16));
#107261=CARTESIAN_POINT('',(45.7706564944766,58.4060826907378,12.));
#107262=CARTESIAN_POINT('Ctrl Pts',(45.7706564944768,58.4060826907376,0.));
#107263=CARTESIAN_POINT('Ctrl Pts',(45.7706564944768,58.4060826907376,4.));
#107264=CARTESIAN_POINT('Ctrl Pts',(45.7706564944767,58.4060826907378,8.));
#107265=CARTESIAN_POINT('Ctrl Pts',(45.7706564944767,58.4060826907378,12.));
#107266=CARTESIAN_POINT('',(45.591148170023,58.9211100416396,12.));
#107267=CARTESIAN_POINT('Ctrl Pts',(45.7706564944767,58.4060826907378,12.));
#107268=CARTESIAN_POINT('Ctrl Pts',(45.790366715598,58.486102814171,12.));
#107269=CARTESIAN_POINT('Ctrl Pts',(45.7899361095676,58.5711327988048,12.));
#107270=CARTESIAN_POINT('Ctrl Pts',(45.7692455126975,58.6508283125143,12.));
#107271=CARTESIAN_POINT('Ctrl Pts',(45.7416580502041,58.7570889974605,12.));
#107272=CARTESIAN_POINT('Ctrl Pts',(45.6780528262179,58.8538661785413,12.));
#107273=CARTESIAN_POINT('Ctrl Pts',(45.591148170023,58.9211100416396,12.));
#107274=CARTESIAN_POINT('Ctrl Pts',(45.591148170023,58.9211100416396,12.));
#107275=CARTESIAN_POINT('Ctrl Pts',(45.591148170023,58.9211100416396,8.));
#107276=CARTESIAN_POINT('Ctrl Pts',(45.5911481700231,58.9211100416396,4.));
#107277=CARTESIAN_POINT('Ctrl Pts',(45.5911481700231,58.9211100416396,0.));
#107278=CARTESIAN_POINT('Ctrl Pts',(44.3377168516418,54.1679505278134,0.));
#107279=CARTESIAN_POINT('Ctrl Pts',(44.3377168516418,54.1679505278134,12.));
#107280=CARTESIAN_POINT('Ctrl Pts',(44.3393235891014,54.1714861895278,0.));
#107281=CARTESIAN_POINT('Ctrl Pts',(44.3393235891014,54.1714861895278,12.));
#107282=CARTESIAN_POINT('Ctrl Pts',(44.3425373700829,54.1785633257456,0.));
#107283=CARTESIAN_POINT('Ctrl Pts',(44.3425373700829,54.1785633257456,12.));
#107284=CARTESIAN_POINT('Ctrl Pts',(44.3473589597467,54.189196468444,0.));
#107285=CARTESIAN_POINT('Ctrl Pts',(44.3473589597467,54.189196468444,12.));
#107286=CARTESIAN_POINT('Ctrl Pts',(44.3537895823819,54.203408870162,0.));
#107287=CARTESIAN_POINT('Ctrl Pts',(44.3537895823819,54.203408870162,12.));
#107288=CARTESIAN_POINT('Ctrl Pts',(44.3618309103245,54.2212325005847,0.));
#107289=CARTESIAN_POINT('Ctrl Pts',(44.3618309103245,54.2212325005847,12.));
#107290=CARTESIAN_POINT('Ctrl Pts',(44.3698752533509,54.2391142386354,0.));
#107291=CARTESIAN_POINT('Ctrl Pts',(44.3698752533509,54.2391142386354,12.));
#107292=CARTESIAN_POINT('Ctrl Pts',(44.3779225430461,54.2570540336536,0.));
#107293=CARTESIAN_POINT('Ctrl Pts',(44.3779225430461,54.2570540336536,12.));
#107294=CARTESIAN_POINT('Ctrl Pts',(44.3859726620288,54.2750517888695,0.));
#107295=CARTESIAN_POINT('Ctrl Pts',(44.3859726620288,54.2750517888695,12.));
#107296=CARTESIAN_POINT('Ctrl Pts',(44.3940254456427,54.2931073621661,0.));
#107297=CARTESIAN_POINT('Ctrl Pts',(44.3940254456427,54.2931073621661,12.));
#107298=CARTESIAN_POINT('Ctrl Pts',(44.4020807028143,54.3112205860776,0.));
#107299=CARTESIAN_POINT('Ctrl Pts',(44.4020807028143,54.3112205860776,12.));
#107300=CARTESIAN_POINT('Ctrl Pts',(44.4101382321834,54.3293912830237,0.));
#107301=CARTESIAN_POINT('Ctrl Pts',(44.4101382321834,54.3293912830237,12.));
#107302=CARTESIAN_POINT('Ctrl Pts',(44.4181978395814,54.347619281931,0.));
#107303=CARTESIAN_POINT('Ctrl Pts',(44.4181978395814,54.347619281931,12.));
#107304=CARTESIAN_POINT('Ctrl Pts',(44.4262593564664,54.3659044357064,0.));
#107305=CARTESIAN_POINT('Ctrl Pts',(44.4262593564664,54.3659044357064,12.));
#107306=CARTESIAN_POINT('Ctrl Pts',(44.4343226339554,54.3842466156151,0.));
#107307=CARTESIAN_POINT('Ctrl Pts',(44.4343226339554,54.3842466156151,12.));
#107308=CARTESIAN_POINT('Ctrl Pts',(44.442387534098,54.4026457030316,0.));
#107309=CARTESIAN_POINT('Ctrl Pts',(44.442387534098,54.4026457030316,12.));
#107310=CARTESIAN_POINT('Ctrl Pts',(44.4504539226336,54.4211015825959,0.));
#107311=CARTESIAN_POINT('Ctrl Pts',(44.4504539226336,54.4211015825959,12.));
#107312=CARTESIAN_POINT('Ctrl Pts',(44.4585216599933,54.4396141337008,0.));
#107313=CARTESIAN_POINT('Ctrl Pts',(44.4585216599933,54.4396141337008,12.));
#107314=CARTESIAN_POINT('Ctrl Pts',(44.4665905967701,54.4581832262072,0.));
#107315=CARTESIAN_POINT('Ctrl Pts',(44.4665905967701,54.4581832262072,12.));
#107316=CARTESIAN_POINT('Ctrl Pts',(44.4746605784056,54.4768087248854,0.));
#107317=CARTESIAN_POINT('Ctrl Pts',(44.4746605784056,54.4768087248854,12.));
#107318=CARTESIAN_POINT('Ctrl Pts',(44.482731448127,54.4954904921938,0.));
#107319=CARTESIAN_POINT('Ctrl Pts',(44.482731448127,54.4954904921938,12.));
#107320=CARTESIAN_POINT('Ctrl Pts',(44.4908030503209,54.5142283914684,0.));
#107321=CARTESIAN_POINT('Ctrl Pts',(44.4908030503209,54.5142283914684,12.));
#107322=CARTESIAN_POINT('Ctrl Pts',(44.4988752343714,54.5330222905438,0.));
#107323=CARTESIAN_POINT('Ctrl Pts',(44.4988752343714,54.5330222905438,12.));
#107324=CARTESIAN_POINT('Ctrl Pts',(44.5069478544945,54.5518720616016,0.));
#107325=CARTESIAN_POINT('Ctrl Pts',(44.5069478544945,54.5518720616016,12.));
#107326=CARTESIAN_POINT('Ctrl Pts',(44.5150207678988,54.5707775794412,0.));
#107327=CARTESIAN_POINT('Ctrl Pts',(44.5150207678988,54.5707775794412,12.));
#107328=CARTESIAN_POINT('Ctrl Pts',(44.5230938335167,54.5897387202815,0.));
#107329=CARTESIAN_POINT('Ctrl Pts',(44.5230938335167,54.5897387202815,12.));
#107330=CARTESIAN_POINT('Ctrl Pts',(44.5311669104514,54.6087553602914,0.));
#107331=CARTESIAN_POINT('Ctrl Pts',(44.5311669104514,54.6087553602914,12.));
#107332=CARTESIAN_POINT('Ctrl Pts',(44.5392398566802,54.6278273743587,0.));
#107333=CARTESIAN_POINT('Ctrl Pts',(44.5392398566802,54.6278273743587,12.));
#107334=CARTESIAN_POINT('Ctrl Pts',(44.5473125297311,54.6469546367408,0.));
#107335=CARTESIAN_POINT('Ctrl Pts',(44.5473125297311,54.6469546367408,12.));
#107336=CARTESIAN_POINT('Ctrl Pts',(44.5553847872721,54.6661370216252,0.));
#107337=CARTESIAN_POINT('Ctrl Pts',(44.5553847872721,54.6661370216252,12.));
#107338=CARTESIAN_POINT('Ctrl Pts',(44.5634564876863,54.6853744036751,0.));
#107339=CARTESIAN_POINT('Ctrl Pts',(44.5634564876863,54.6853744036751,12.));
#107340=CARTESIAN_POINT('Ctrl Pts',(44.5715274907619,54.7046666586754,0.));
#107341=CARTESIAN_POINT('Ctrl Pts',(44.5715274907619,54.7046666586754,12.));
#107342=CARTESIAN_POINT('Ctrl Pts',(44.5795976579454,54.7240136637717,0.));
#107343=CARTESIAN_POINT('Ctrl Pts',(44.5795976579454,54.7240136637717,12.));
#107344=CARTESIAN_POINT('Ctrl Pts',(44.5876668519661,54.7434152971267,0.));
#107345=CARTESIAN_POINT('Ctrl Pts',(44.5876668519661,54.7434152971267,12.));
#107346=CARTESIAN_POINT('Ctrl Pts',(44.5957349366058,54.7628714377037,0.));
#107347=CARTESIAN_POINT('Ctrl Pts',(44.5957349366058,54.7628714377037,12.));
#107348=CARTESIAN_POINT('Ctrl Pts',(44.6038017764309,54.7823819650149,0.));
#107349=CARTESIAN_POINT('Ctrl Pts',(44.6038017764309,54.7823819650149,12.));
#107350=CARTESIAN_POINT('Ctrl Pts',(44.6118672364906,54.8019467588278,0.));
#107351=CARTESIAN_POINT('Ctrl Pts',(44.6118672364906,54.8019467588278,12.));
#107352=CARTESIAN_POINT('Ctrl Pts',(44.6199311823293,54.8215656991837,0.));
#107353=CARTESIAN_POINT('Ctrl Pts',(44.6199311823293,54.8215656991837,12.));
#107354=CARTESIAN_POINT('Ctrl Pts',(44.6279934801168,54.8412386665276,0.));
#107355=CARTESIAN_POINT('Ctrl Pts',(44.6279934801168,54.8412386665276,12.));
#107356=CARTESIAN_POINT('Ctrl Pts',(44.6360539967392,54.860965541796,0.));
#107357=CARTESIAN_POINT('Ctrl Pts',(44.6360539967392,54.860965541796,12.));
#107358=CARTESIAN_POINT('Ctrl Pts',(44.6441125999063,54.8807462065164,0.));
#107359=CARTESIAN_POINT('Ctrl Pts',(44.6441125999063,54.8807462065164,12.));
#107360=CARTESIAN_POINT('Ctrl Pts',(44.6521691582533,54.9005805428969,0.));
#107361=CARTESIAN_POINT('Ctrl Pts',(44.6521691582533,54.9005805428969,12.));
#107362=CARTESIAN_POINT('Ctrl Pts',(44.6602235412836,54.9204684337822,0.));
#107363=CARTESIAN_POINT('Ctrl Pts',(44.6602235412836,54.9204684337822,12.));
#107364=CARTESIAN_POINT('Ctrl Pts',(44.6682756193147,54.9404097626077,0.));
#107365=CARTESIAN_POINT('Ctrl Pts',(44.6682756193147,54.9404097626077,12.));
#107366=CARTESIAN_POINT('Ctrl Pts',(44.6763252634258,54.9604044133501,0.));
#107367=CARTESIAN_POINT('Ctrl Pts',(44.6763252634258,54.9604044133501,12.));
#107368=CARTESIAN_POINT('Ctrl Pts',(44.6843723454,54.9804522704686,0.));
#107369=CARTESIAN_POINT('Ctrl Pts',(44.6843723454,54.9804522704686,12.));
#107370=CARTESIAN_POINT('Ctrl Pts',(44.6924167376869,55.0005532188667,0.));
#107371=CARTESIAN_POINT('Ctrl Pts',(44.6924167376869,55.0005532188667,12.));
#107372=CARTESIAN_POINT('Ctrl Pts',(44.7004583134249,55.0207071439237,0.));
#107373=CARTESIAN_POINT('Ctrl Pts',(44.7004583134249,55.0207071439237,12.));
#107374=CARTESIAN_POINT('Ctrl Pts',(44.7084969464513,55.0409139315078,0.));
#107375=CARTESIAN_POINT('Ctrl Pts',(44.7084969464513,55.0409139315078,12.));
#107376=CARTESIAN_POINT('Ctrl Pts',(44.7165325113159,55.0611734679894,0.));
#107377=CARTESIAN_POINT('Ctrl Pts',(44.7165325113159,55.0611734679894,12.));
#107378=CARTESIAN_POINT('Ctrl Pts',(44.7245648832979,55.0814856402496,0.));
#107379=CARTESIAN_POINT('Ctrl Pts',(44.7245648832979,55.0814856402496,12.));
#107380=CARTESIAN_POINT('Ctrl Pts',(44.7325939384035,55.1018503356796,0.));
#107381=CARTESIAN_POINT('Ctrl Pts',(44.7325939384035,55.1018503356796,12.));
#107382=CARTESIAN_POINT('Ctrl Pts',(44.7406195533479,55.1222674421743,0.));
#107383=CARTESIAN_POINT('Ctrl Pts',(44.7406195533479,55.1222674421743,12.));
#107384=CARTESIAN_POINT('Ctrl Pts',(44.7486416055419,55.14273684812,0.));
#107385=CARTESIAN_POINT('Ctrl Pts',(44.7486416055419,55.14273684812,12.));
#107386=CARTESIAN_POINT('Ctrl Pts',(44.7566599730773,55.1632584423815,0.));
#107387=CARTESIAN_POINT('Ctrl Pts',(44.7566599730773,55.1632584423815,12.));
#107388=CARTESIAN_POINT('Ctrl Pts',(44.7646745347109,55.1838321142779,0.));
#107389=CARTESIAN_POINT('Ctrl Pts',(44.7646745347109,55.1838321142779,12.));
#107390=CARTESIAN_POINT('Ctrl Pts',(44.7726851698618,55.2044577535866,0.));
#107391=CARTESIAN_POINT('Ctrl Pts',(44.7726851698618,55.2044577535866,12.));
#107392=CARTESIAN_POINT('Ctrl Pts',(44.7806917586077,55.2251352505475,0.));
#107393=CARTESIAN_POINT('Ctrl Pts',(44.7806917586077,55.2251352505475,12.));
#107394=CARTESIAN_POINT('Ctrl Pts',(44.7886941816823,55.2458644958617,0.));
#107395=CARTESIAN_POINT('Ctrl Pts',(44.7886941816823,55.2458644958617,12.));
#107396=CARTESIAN_POINT('Ctrl Pts',(44.7966923204741,55.2666453806883,0.));
#107397=CARTESIAN_POINT('Ctrl Pts',(44.7966923204741,55.2666453806883,12.));
#107398=CARTESIAN_POINT('Ctrl Pts',(44.8046860570245,55.287477796635,0.));
#107399=CARTESIAN_POINT('Ctrl Pts',(44.8046860570245,55.287477796635,12.));
#107400=CARTESIAN_POINT('Ctrl Pts',(44.812675274021,55.3083616357605,0.));
#107401=CARTESIAN_POINT('Ctrl Pts',(44.812675274021,55.3083616357605,12.));
#107402=CARTESIAN_POINT('Ctrl Pts',(44.8206598547888,55.3292967905726,0.));
#107403=CARTESIAN_POINT('Ctrl Pts',(44.8206598547888,55.3292967905726,12.));
#107404=CARTESIAN_POINT('Ctrl Pts',(44.8286396832849,55.350283154023,0.));
#107405=CARTESIAN_POINT('Ctrl Pts',(44.8286396832849,55.350283154023,12.));
#107406=CARTESIAN_POINT('Ctrl Pts',(44.8366146440896,55.3713206194962,0.));
#107407=CARTESIAN_POINT('Ctrl Pts',(44.8366146440896,55.3713206194962,12.));
#107408=CARTESIAN_POINT('Ctrl Pts',(44.8445846224033,55.3924090808002,0.));
#107409=CARTESIAN_POINT('Ctrl Pts',(44.8445846224033,55.3924090808002,12.));
#107410=CARTESIAN_POINT('Ctrl Pts',(44.8525495040397,55.4135484321706,0.));
#107411=CARTESIAN_POINT('Ctrl Pts',(44.8525495040397,55.4135484321706,12.));
#107412=CARTESIAN_POINT('Ctrl Pts',(44.8605091754208,55.4347385682697,0.));
#107413=CARTESIAN_POINT('Ctrl Pts',(44.8605091754208,55.4347385682697,12.));
#107414=CARTESIAN_POINT('Ctrl Pts',(44.8684635235727,55.4559793841838,0.));
#107415=CARTESIAN_POINT('Ctrl Pts',(44.8684635235727,55.4559793841838,12.));
#107416=CARTESIAN_POINT('Ctrl Pts',(44.8764124361218,55.4772707754139,0.));
#107417=CARTESIAN_POINT('Ctrl Pts',(44.8764124361218,55.4772707754139,12.));
#107418=CARTESIAN_POINT('Ctrl Pts',(44.8843558012903,55.4986126378676,0.));
#107419=CARTESIAN_POINT('Ctrl Pts',(44.8843558012903,55.4986126378676,12.));
#107420=CARTESIAN_POINT('Ctrl Pts',(44.8922935078905,55.5200048678648,0.));
#107421=CARTESIAN_POINT('Ctrl Pts',(44.8922935078905,55.5200048678648,12.));
#107422=CARTESIAN_POINT('Ctrl Pts',(44.9002254453192,55.541447362135,0.));
#107423=CARTESIAN_POINT('Ctrl Pts',(44.9002254453192,55.541447362135,12.));
#107424=CARTESIAN_POINT('Ctrl Pts',(44.9081515035525,55.5629400178136,0.));
#107425=CARTESIAN_POINT('Ctrl Pts',(44.9081515035525,55.5629400178136,12.));
#107426=CARTESIAN_POINT('Ctrl Pts',(44.9160715731425,55.5844827324315,0.));
#107427=CARTESIAN_POINT('Ctrl Pts',(44.9160715731425,55.5844827324315,12.));
#107428=CARTESIAN_POINT('Ctrl Pts',(44.9239855452119,55.6060754039089,0.));
#107429=CARTESIAN_POINT('Ctrl Pts',(44.9239855452119,55.6060754039089,12.));
#107430=CARTESIAN_POINT('Ctrl Pts',(44.9318933114483,55.6277179305604,0.));
#107431=CARTESIAN_POINT('Ctrl Pts',(44.9318933114483,55.6277179305604,12.));
#107432=CARTESIAN_POINT('Ctrl Pts',(44.9397947640996,55.6494102110922,0.));
#107433=CARTESIAN_POINT('Ctrl Pts',(44.9397947640996,55.6494102110922,12.));
#107434=CARTESIAN_POINT('Ctrl Pts',(44.9476897959694,55.671152144599,0.));
#107435=CARTESIAN_POINT('Ctrl Pts',(44.9476897959694,55.671152144599,12.));
#107436=CARTESIAN_POINT('Ctrl Pts',(44.9555783004133,55.6929436305522,0.));
#107437=CARTESIAN_POINT('Ctrl Pts',(44.9555783004133,55.6929436305522,12.));
#107438=CARTESIAN_POINT('Ctrl Pts',(44.9634601713352,55.7147845687969,0.));
#107439=CARTESIAN_POINT('Ctrl Pts',(44.9634601713352,55.7147845687969,12.));
#107440=CARTESIAN_POINT('Ctrl Pts',(44.9713353031827,55.7366748595582,0.));
#107441=CARTESIAN_POINT('Ctrl Pts',(44.9713353031827,55.7366748595582,12.));
#107442=CARTESIAN_POINT('Ctrl Pts',(44.979203590942,55.7586144034376,0.));
#107443=CARTESIAN_POINT('Ctrl Pts',(44.979203590942,55.7586144034376,12.));
#107444=CARTESIAN_POINT('Ctrl Pts',(44.9870649301333,55.7806031014093,0.));
#107445=CARTESIAN_POINT('Ctrl Pts',(44.9870649301333,55.7806031014093,12.));
#107446=CARTESIAN_POINT('Ctrl Pts',(44.9949192168073,55.8026408548078,0.));
#107447=CARTESIAN_POINT('Ctrl Pts',(44.9949192168073,55.8026408548078,12.));
#107448=CARTESIAN_POINT('Ctrl Pts',(45.002766347541,55.8247275653257,0.));
#107449=CARTESIAN_POINT('Ctrl Pts',(45.002766347541,55.8247275653257,12.));
#107450=CARTESIAN_POINT('Ctrl Pts',(45.0106062194325,55.8468631350195,0.));
#107451=CARTESIAN_POINT('Ctrl Pts',(45.0106062194325,55.8468631350195,12.));
#107452=CARTESIAN_POINT('Ctrl Pts',(45.0184387300968,55.8690474663058,0.));
#107453=CARTESIAN_POINT('Ctrl Pts',(45.0184387300968,55.8690474663058,12.));
#107454=CARTESIAN_POINT('Ctrl Pts',(45.0262637776623,55.8912804619588,0.));
#107455=CARTESIAN_POINT('Ctrl Pts',(45.0262637776623,55.8912804619588,12.));
#107456=CARTESIAN_POINT('Ctrl Pts',(45.0340812607675,55.9135620250977,0.));
#107457=CARTESIAN_POINT('Ctrl Pts',(45.0340812607675,55.9135620250977,12.));
#107458=CARTESIAN_POINT('Ctrl Pts',(45.041891078557,55.9358920591861,0.));
#107459=CARTESIAN_POINT('Ctrl Pts',(45.041891078557,55.9358920591861,12.));
#107460=CARTESIAN_POINT('Ctrl Pts',(45.0496931306766,55.958270468037,0.));
#107461=CARTESIAN_POINT('Ctrl Pts',(45.0496931306766,55.958270468037,12.));
#107462=CARTESIAN_POINT('Ctrl Pts',(45.0574873172696,55.9806971558099,0.));
#107463=CARTESIAN_POINT('Ctrl Pts',(45.0574873172696,55.9806971558099,12.));
#107464=CARTESIAN_POINT('Ctrl Pts',(45.0652735389728,56.0031720270074,0.));
#107465=CARTESIAN_POINT('Ctrl Pts',(45.0652735389728,56.0031720270074,12.));
#107466=CARTESIAN_POINT('Ctrl Pts',(45.0730516969142,56.025694986463,0.));
#107467=CARTESIAN_POINT('Ctrl Pts',(45.0730516969142,56.025694986463,12.));
#107468=CARTESIAN_POINT('Ctrl Pts',(45.0808216927082,56.0482659393412,0.));
#107469=CARTESIAN_POINT('Ctrl Pts',(45.0808216927082,56.0482659393412,12.));
#107470=CARTESIAN_POINT('Ctrl Pts',(45.0885834284513,56.070884791141,0.));
#107471=CARTESIAN_POINT('Ctrl Pts',(45.0885834284513,56.070884791141,12.));
#107472=CARTESIAN_POINT('Ctrl Pts',(45.0963368067177,56.0935514476946,0.));
#107473=CARTESIAN_POINT('Ctrl Pts',(45.0963368067177,56.0935514476946,12.));
#107474=CARTESIAN_POINT('Ctrl Pts',(45.1040817305563,56.1162658151621,0.));
#107475=CARTESIAN_POINT('Ctrl Pts',(45.1040817305563,56.1162658151621,12.));
#107476=CARTESIAN_POINT('Ctrl Pts',(45.1118181034888,56.1390278000226,0.));
#107477=CARTESIAN_POINT('Ctrl Pts',(45.1118181034888,56.1390278000226,12.));
#107478=CARTESIAN_POINT('Ctrl Pts',(45.119545829506,56.1618373090729,0.));
#107479=CARTESIAN_POINT('Ctrl Pts',(45.119545829506,56.1618373090729,12.));
#107480=CARTESIAN_POINT('Ctrl Pts',(45.1272648130627,56.1846942494321,0.));
#107481=CARTESIAN_POINT('Ctrl Pts',(45.1272648130627,56.1846942494321,12.));
#107482=CARTESIAN_POINT('Ctrl Pts',(45.1349749590736,56.2075985285391,0.));
#107483=CARTESIAN_POINT('Ctrl Pts',(45.1349749590736,56.2075985285391,12.));
#107484=CARTESIAN_POINT('Ctrl Pts',(45.1426761729107,56.2305500541491,0.));
#107485=CARTESIAN_POINT('Ctrl Pts',(45.1426761729107,56.2305500541491,12.));
#107486=CARTESIAN_POINT('Ctrl Pts',(45.150368360401,56.2535487343227,0.));
#107487=CARTESIAN_POINT('Ctrl Pts',(45.150368360401,56.2535487343227,12.));
#107488=CARTESIAN_POINT('Ctrl Pts',(45.158051427823,56.2765944774252,0.));
#107489=CARTESIAN_POINT('Ctrl Pts',(45.158051427823,56.2765944774252,12.));
#107490=CARTESIAN_POINT('Ctrl Pts',(45.1657252819018,56.2996871921321,0.));
#107491=CARTESIAN_POINT('Ctrl Pts',(45.1657252819018,56.2996871921321,12.));
#107492=CARTESIAN_POINT('Ctrl Pts',(45.1733898298062,56.3228267874265,0.));
#107493=CARTESIAN_POINT('Ctrl Pts',(45.1733898298062,56.3228267874265,12.));
#107494=CARTESIAN_POINT('Ctrl Pts',(45.1810449791451,56.3460131725962,0.));
#107495=CARTESIAN_POINT('Ctrl Pts',(45.1810449791451,56.3460131725962,12.));
#107496=CARTESIAN_POINT('Ctrl Pts',(45.1886906379664,56.3692462572228,0.));
#107497=CARTESIAN_POINT('Ctrl Pts',(45.1886906379664,56.3692462572228,12.));
#107498=CARTESIAN_POINT('Ctrl Pts',(45.1963267147527,56.3925259511804,0.));
#107499=CARTESIAN_POINT('Ctrl Pts',(45.1963267147527,56.3925259511804,12.));
#107500=CARTESIAN_POINT('Ctrl Pts',(45.2039531184172,56.4158521646412,0.));
#107501=CARTESIAN_POINT('Ctrl Pts',(45.2039531184172,56.4158521646412,12.));
#107502=CARTESIAN_POINT('Ctrl Pts',(45.2115697583002,56.4392248080733,0.));
#107503=CARTESIAN_POINT('Ctrl Pts',(45.2115697583002,56.4392248080733,12.));
#107504=CARTESIAN_POINT('Ctrl Pts',(45.2191765441666,56.4626437922385,0.));
#107505=CARTESIAN_POINT('Ctrl Pts',(45.2191765441666,56.4626437922385,12.));
#107506=CARTESIAN_POINT('Ctrl Pts',(45.2267733862046,56.4861090281819,0.));
#107507=CARTESIAN_POINT('Ctrl Pts',(45.2267733862046,56.4861090281819,12.));
#107508=CARTESIAN_POINT('Ctrl Pts',(45.2343601950222,56.5096204272299,0.));
#107509=CARTESIAN_POINT('Ctrl Pts',(45.2343601950222,56.5096204272299,12.));
#107510=CARTESIAN_POINT('Ctrl Pts',(45.2419368816423,56.533177900995,0.));
#107511=CARTESIAN_POINT('Ctrl Pts',(45.2419368816423,56.533177900995,12.));
#107512=CARTESIAN_POINT('Ctrl Pts',(45.2495033574997,56.5567813613752,0.));
#107513=CARTESIAN_POINT('Ctrl Pts',(45.2495033574997,56.5567813613752,12.));
#107514=CARTESIAN_POINT('Ctrl Pts',(45.2570595344382,56.5804307205507,0.));
#107515=CARTESIAN_POINT('Ctrl Pts',(45.2570595344382,56.5804307205507,12.));
#107516=CARTESIAN_POINT('Ctrl Pts',(45.2646053247094,56.604125890975,0.));
#107517=CARTESIAN_POINT('Ctrl Pts',(45.2646053247094,56.604125890975,12.));
#107518=CARTESIAN_POINT('Ctrl Pts',(45.2721406409706,56.6278667853716,0.));
#107519=CARTESIAN_POINT('Ctrl Pts',(45.2721406409706,56.6278667853716,12.));
#107520=CARTESIAN_POINT('Ctrl Pts',(45.2796653962795,56.6516533167398,0.));
#107521=CARTESIAN_POINT('Ctrl Pts',(45.2796653962795,56.6516533167398,12.));
#107522=CARTESIAN_POINT('Ctrl Pts',(45.2871795040912,56.6754853983535,0.));
#107523=CARTESIAN_POINT('Ctrl Pts',(45.2871795040912,56.6754853983535,12.));
#107524=CARTESIAN_POINT('Ctrl Pts',(45.2946828782557,56.6993629437597,0.));
#107525=CARTESIAN_POINT('Ctrl Pts',(45.2946828782557,56.6993629437597,12.));
#107526=CARTESIAN_POINT('Ctrl Pts',(45.3021754330169,56.7232858667697,0.));
#107527=CARTESIAN_POINT('Ctrl Pts',(45.3021754330169,56.7232858667697,12.));
#107528=CARTESIAN_POINT('Ctrl Pts',(45.3096570830107,56.747254081454,0.));
#107529=CARTESIAN_POINT('Ctrl Pts',(45.3096570830107,56.747254081454,12.));
#107530=CARTESIAN_POINT('Ctrl Pts',(45.3171277432592,56.771267502148,0.));
#107531=CARTESIAN_POINT('Ctrl Pts',(45.3171277432592,56.771267502148,12.));
#107532=CARTESIAN_POINT('Ctrl Pts',(45.3245873291682,56.7953260434521,0.));
#107533=CARTESIAN_POINT('Ctrl Pts',(45.3245873291682,56.7953260434521,12.));
#107534=CARTESIAN_POINT('Ctrl Pts',(45.3320357565241,56.8194296202293,0.));
#107535=CARTESIAN_POINT('Ctrl Pts',(45.3320357565241,56.8194296202293,12.));
#107536=CARTESIAN_POINT('Ctrl Pts',(45.3394729414932,56.8435781475982,0.));
#107537=CARTESIAN_POINT('Ctrl Pts',(45.3394729414932,56.8435781475982,12.));
#107538=CARTESIAN_POINT('Ctrl Pts',(45.3468988006201,56.8677715409266,0.));
#107539=CARTESIAN_POINT('Ctrl Pts',(45.3468988006201,56.8677715409266,12.));
#107540=CARTESIAN_POINT('Ctrl Pts',(45.3543132508234,56.8920097158371,0.));
#107541=CARTESIAN_POINT('Ctrl Pts',(45.3543132508234,56.8920097158371,12.));
#107542=CARTESIAN_POINT('Ctrl Pts',(45.3617162093918,56.916292588208,0.));
#107543=CARTESIAN_POINT('Ctrl Pts',(45.3617162093918,56.916292588208,12.));
#107544=CARTESIAN_POINT('Ctrl Pts',(45.3691075939827,56.9406200741714,0.));
#107545=CARTESIAN_POINT('Ctrl Pts',(45.3691075939827,56.9406200741714,12.));
#107546=CARTESIAN_POINT('Ctrl Pts',(45.3764873226202,56.9649920901079,0.));
#107547=CARTESIAN_POINT('Ctrl Pts',(45.3764873226202,56.9649920901079,12.));
#107548=CARTESIAN_POINT('Ctrl Pts',(45.3838553136957,56.9894085526383,0.));
#107549=CARTESIAN_POINT('Ctrl Pts',(45.3838553136957,56.9894085526383,12.));
#107550=CARTESIAN_POINT('Ctrl Pts',(45.3912114859624,57.0138693786287,0.));
#107551=CARTESIAN_POINT('Ctrl Pts',(45.3912114859624,57.0138693786287,12.));
#107552=CARTESIAN_POINT('Ctrl Pts',(45.3985557585316,57.0383744851917,0.));
#107553=CARTESIAN_POINT('Ctrl Pts',(45.3985557585316,57.0383744851917,12.));
#107554=CARTESIAN_POINT('Ctrl Pts',(45.4058880508693,57.0629237896848,0.));
#107555=CARTESIAN_POINT('Ctrl Pts',(45.4058880508693,57.0629237896848,12.));
#107556=CARTESIAN_POINT('Ctrl Pts',(45.4132082827945,57.0875172097048,0.));
#107557=CARTESIAN_POINT('Ctrl Pts',(45.4132082827945,57.0875172097048,12.));
#107558=CARTESIAN_POINT('Ctrl Pts',(45.4205163744778,57.1121546630776,0.));
#107559=CARTESIAN_POINT('Ctrl Pts',(45.4205163744778,57.1121546630776,12.));
#107560=CARTESIAN_POINT('Ctrl Pts',(45.4278122464387,57.1368360678629,0.));
#107561=CARTESIAN_POINT('Ctrl Pts',(45.4278122464387,57.1368360678629,12.));
#107562=CARTESIAN_POINT('Ctrl Pts',(45.4350958195434,57.1615613423586,0.));
#107563=CARTESIAN_POINT('Ctrl Pts',(45.4350958195434,57.1615613423586,12.));
#107564=CARTESIAN_POINT('Ctrl Pts',(45.4423670150035,57.1863304051011,0.));
#107565=CARTESIAN_POINT('Ctrl Pts',(45.4423670150035,57.1863304051011,12.));
#107566=CARTESIAN_POINT('Ctrl Pts',(45.4496257543758,57.2111431748629,0.));
#107567=CARTESIAN_POINT('Ctrl Pts',(45.4496257543758,57.2111431748629,12.));
#107568=CARTESIAN_POINT('Ctrl Pts',(45.4568719595639,57.2359995706441,0.));
#107569=CARTESIAN_POINT('Ctrl Pts',(45.4568719595639,57.2359995706441,12.));
#107570=CARTESIAN_POINT('Ctrl Pts',(45.4641055528137,57.2608995116727,0.));
#107571=CARTESIAN_POINT('Ctrl Pts',(45.4641055528137,57.2608995116727,12.));
#107572=CARTESIAN_POINT('Ctrl Pts',(45.4713264567059,57.2858429174056,0.));
#107573=CARTESIAN_POINT('Ctrl Pts',(45.4713264567059,57.2858429174056,12.));
#107574=CARTESIAN_POINT('Ctrl Pts',(45.4785345941505,57.3108297075262,0.));
#107575=CARTESIAN_POINT('Ctrl Pts',(45.4785345941505,57.3108297075262,12.));
#107576=CARTESIAN_POINT('Ctrl Pts',(45.4857298883826,57.3358598019391,0.));
#107577=CARTESIAN_POINT('Ctrl Pts',(45.4857298883826,57.3358598019391,12.));
#107578=CARTESIAN_POINT('Ctrl Pts',(45.4929122629576,57.360933120758,0.));
#107579=CARTESIAN_POINT('Ctrl Pts',(45.4929122629576,57.360933120758,12.));
#107580=CARTESIAN_POINT('Ctrl Pts',(45.5000816417516,57.3860495843043,0.));
#107581=CARTESIAN_POINT('Ctrl Pts',(45.5000816417516,57.3860495843043,12.));
#107582=CARTESIAN_POINT('Ctrl Pts',(45.5072379489637,57.4112091131193,0.));
#107583=CARTESIAN_POINT('Ctrl Pts',(45.5072379489637,57.4112091131193,12.));
#107584=CARTESIAN_POINT('Ctrl Pts',(45.5143811091209,57.4364116279708,0.));
#107585=CARTESIAN_POINT('Ctrl Pts',(45.5143811091209,57.4364116279708,12.));
#107586=CARTESIAN_POINT('Ctrl Pts',(45.5215110470824,57.4616570498566,0.));
#107587=CARTESIAN_POINT('Ctrl Pts',(45.5215110470824,57.4616570498566,12.));
#107588=CARTESIAN_POINT('Ctrl Pts',(45.5286276880479,57.4869453000055,0.));
#107589=CARTESIAN_POINT('Ctrl Pts',(45.5286276880479,57.4869453000055,12.));
#107590=CARTESIAN_POINT('Ctrl Pts',(45.5357309575603,57.5122762998732,0.));
#107591=CARTESIAN_POINT('Ctrl Pts',(45.5357309575603,57.5122762998732,12.));
#107592=CARTESIAN_POINT('Ctrl Pts',(45.5428207814832,57.5376499711338,0.));
#107593=CARTESIAN_POINT('Ctrl Pts',(45.5428207814832,57.5376499711338,12.));
#107594=CARTESIAN_POINT('Ctrl Pts',(45.5498970859829,57.5630662356671,0.));
#107595=CARTESIAN_POINT('Ctrl Pts',(45.5498970859829,57.5630662356671,12.));
#107596=CARTESIAN_POINT('Ctrl Pts',(45.5569597975095,57.5885250155432,0.));
#107597=CARTESIAN_POINT('Ctrl Pts',(45.5569597975095,57.5885250155432,12.));
#107598=CARTESIAN_POINT('Ctrl Pts',(45.5640088427819,57.6140262330048,0.));
#107599=CARTESIAN_POINT('Ctrl Pts',(45.5640088427819,57.6140262330048,12.));
#107600=CARTESIAN_POINT('Ctrl Pts',(45.5710441487683,57.6395698104416,0.));
#107601=CARTESIAN_POINT('Ctrl Pts',(45.5710441487683,57.6395698104416,12.));
#107602=CARTESIAN_POINT('Ctrl Pts',(45.5780656427172,57.6651556704249,0.));
#107603=CARTESIAN_POINT('Ctrl Pts',(45.5780656427172,57.6651556704249,12.));
#107604=CARTESIAN_POINT('Ctrl Pts',(45.5850732521902,57.6907837357426,0.));
#107605=CARTESIAN_POINT('Ctrl Pts',(45.5850732521902,57.6907837357426,12.));
#107606=CARTESIAN_POINT('Ctrl Pts',(45.5920669050987,57.7164539294316,0.));
#107607=CARTESIAN_POINT('Ctrl Pts',(45.5920669050987,57.7164539294316,12.));
#107608=CARTESIAN_POINT('Ctrl Pts',(45.5990465297341,57.7421661748022,0.));
#107609=CARTESIAN_POINT('Ctrl Pts',(45.5990465297341,57.7421661748022,12.));
#107610=CARTESIAN_POINT('Ctrl Pts',(45.6060120548199,57.7679203954735,0.));
#107611=CARTESIAN_POINT('Ctrl Pts',(45.6060120548199,57.7679203954735,12.));
#107612=CARTESIAN_POINT('Ctrl Pts',(45.6129634094677,57.7937165153379,0.));
#107613=CARTESIAN_POINT('Ctrl Pts',(45.6129634094677,57.7937165153379,12.));
#107614=CARTESIAN_POINT('Ctrl Pts',(45.619900523078,57.819554458484,0.));
#107615=CARTESIAN_POINT('Ctrl Pts',(45.619900523078,57.819554458484,12.));
#107616=CARTESIAN_POINT('Ctrl Pts',(45.6268233252543,57.8454341491236,0.));
#107617=CARTESIAN_POINT('Ctrl Pts',(45.6268233252543,57.8454341491236,12.));
#107618=CARTESIAN_POINT('Ctrl Pts',(45.6337317457253,57.8713555115232,0.));
#107619=CARTESIAN_POINT('Ctrl Pts',(45.6337317457253,57.8713555115232,12.));
#107620=CARTESIAN_POINT('Ctrl Pts',(45.6406257142384,57.8973184699038,0.));
#107621=CARTESIAN_POINT('Ctrl Pts',(45.6406257142384,57.8973184699038,12.));
#107622=CARTESIAN_POINT('Ctrl Pts',(45.6475051605542,57.923322948432,0.));
#107623=CARTESIAN_POINT('Ctrl Pts',(45.6475051605542,57.923322948432,12.));
#107624=CARTESIAN_POINT('Ctrl Pts',(45.6543700146688,57.9493688714249,0.));
#107625=CARTESIAN_POINT('Ctrl Pts',(45.6543700146688,57.9493688714249,12.));
#107626=CARTESIAN_POINT('Ctrl Pts',(45.6612202069927,57.975456163507,0.));
#107627=CARTESIAN_POINT('Ctrl Pts',(45.6612202069927,57.975456163507,12.));
#107628=CARTESIAN_POINT('Ctrl Pts',(45.6680556685494,58.0015847497838,0.));
#107629=CARTESIAN_POINT('Ctrl Pts',(45.6680556685494,58.0015847497838,12.));
#107630=CARTESIAN_POINT('Ctrl Pts',(45.6748763311635,58.0277545560001,0.));
#107631=CARTESIAN_POINT('Ctrl Pts',(45.6748763311635,58.0277545560001,12.));
#107632=CARTESIAN_POINT('Ctrl Pts',(45.6816821276662,58.0539655087095,0.));
#107633=CARTESIAN_POINT('Ctrl Pts',(45.6816821276662,58.0539655087095,12.));
#107634=CARTESIAN_POINT('Ctrl Pts',(45.6884729914465,58.0802175348939,0.));
#107635=CARTESIAN_POINT('Ctrl Pts',(45.6884729914465,58.0802175348939,12.));
#107636=CARTESIAN_POINT('Ctrl Pts',(45.6952488560133,58.1065105615884,0.));
#107637=CARTESIAN_POINT('Ctrl Pts',(45.6952488560133,58.1065105615884,12.));
#107638=CARTESIAN_POINT('Ctrl Pts',(45.7020096545174,58.1328445154667,0.));
#107639=CARTESIAN_POINT('Ctrl Pts',(45.7020096545174,58.1328445154667,12.));
#107640=CARTESIAN_POINT('Ctrl Pts',(45.708755319378,58.159219322515,0.));
#107641=CARTESIAN_POINT('Ctrl Pts',(45.708755319378,58.159219322515,12.));
#107642=CARTESIAN_POINT('Ctrl Pts',(45.7154857816507,58.1856349074723,0.));
#107643=CARTESIAN_POINT('Ctrl Pts',(45.7154857816507,58.1856349074723,12.));
#107644=CARTESIAN_POINT('Ctrl Pts',(45.7222009715431,58.2120911942819,0.));
#107645=CARTESIAN_POINT('Ctrl Pts',(45.7222009715431,58.2120911942819,12.));
#107646=CARTESIAN_POINT('Ctrl Pts',(45.7289008195612,58.2385881070959,0.));
#107647=CARTESIAN_POINT('Ctrl Pts',(45.7289008195612,58.2385881070959,12.));
#107648=CARTESIAN_POINT('Ctrl Pts',(45.7355852575127,58.2651255711481,0.));
#107649=CARTESIAN_POINT('Ctrl Pts',(45.7355852575127,58.2651255711481,12.));
#107650=CARTESIAN_POINT('Ctrl Pts',(45.7422542194625,58.2917035135833,0.));
#107651=CARTESIAN_POINT('Ctrl Pts',(45.7422542194625,58.2917035135833,12.));
#107652=CARTESIAN_POINT('Ctrl Pts',(45.7489076429725,58.3183218645265,0.));
#107653=CARTESIAN_POINT('Ctrl Pts',(45.7489076429725,58.3183218645265,12.));
#107654=CARTESIAN_POINT('Ctrl Pts',(45.7555454693956,58.3449805573335,0.));
#107655=CARTESIAN_POINT('Ctrl Pts',(45.7555454693956,58.3449805573335,12.));
#107656=CARTESIAN_POINT('Ctrl Pts',(45.762167641136,58.3716795262252,0.));
#107657=CARTESIAN_POINT('Ctrl Pts',(45.762167641136,58.3716795262252,12.));
#107658=CARTESIAN_POINT('Ctrl Pts',(45.7687740994899,58.3984187044166,0.));
#107659=CARTESIAN_POINT('Ctrl Pts',(45.7687740994899,58.3984187044166,12.));
#107660=CARTESIAN_POINT('Ctrl Pts',(45.77536478215,58.4251980219532,0.));
#107661=CARTESIAN_POINT('Ctrl Pts',(45.77536478215,58.4251980219532,12.));
#107662=CARTESIAN_POINT('Ctrl Pts',(45.7819396211062,58.4520174038836,0.));
#107663=CARTESIAN_POINT('Ctrl Pts',(45.7819396211062,58.4520174038836,12.));
#107664=CARTESIAN_POINT('Ctrl Pts',(45.7884985397138,58.4788767677114,0.));
#107665=CARTESIAN_POINT('Ctrl Pts',(45.7884985397138,58.4788767677114,12.));
#107666=CARTESIAN_POINT('Ctrl Pts',(45.7950414569431,58.5057760270407,0.));
#107667=CARTESIAN_POINT('Ctrl Pts',(45.7950414569431,58.5057760270407,12.));
#107668=CARTESIAN_POINT('Ctrl Pts',(45.801568292618,58.5327150960874,0.));
#107669=CARTESIAN_POINT('Ctrl Pts',(45.801568292618,58.5327150960874,12.));
#107670=CARTESIAN_POINT('Ctrl Pts',(45.8080789725167,58.5596938940308,0.));
#107671=CARTESIAN_POINT('Ctrl Pts',(45.8080789725167,58.5596938940308,12.));
#107672=CARTESIAN_POINT('Ctrl Pts',(45.8145734330666,58.5867123490943,0.));
#107673=CARTESIAN_POINT('Ctrl Pts',(45.8145734330666,58.5867123490943,12.));
#107674=CARTESIAN_POINT('Ctrl Pts',(45.8210516273556,58.6137704035561,0.));
#107675=CARTESIAN_POINT('Ctrl Pts',(45.8210516273556,58.6137704035561,12.));
#107676=CARTESIAN_POINT('Ctrl Pts',(45.8275135263874,58.64086801535,0.));
#107677=CARTESIAN_POINT('Ctrl Pts',(45.8275135263874,58.64086801535,12.));
#107678=CARTESIAN_POINT('Ctrl Pts',(45.8339591141396,58.668005155216,0.));
#107679=CARTESIAN_POINT('Ctrl Pts',(45.8339591141396,58.668005155216,12.));
#107680=CARTESIAN_POINT('Ctrl Pts',(45.8391025301766,58.6897464750196,0.));
#107681=CARTESIAN_POINT('Ctrl Pts',(45.8391025301766,58.6897464750196,12.));
#107682=CARTESIAN_POINT('Ctrl Pts',(45.8429527488565,58.7060702401382,0.));
#107683=CARTESIAN_POINT('Ctrl Pts',(45.8429527488565,58.7060702401382,12.));
#107684=CARTESIAN_POINT('Ctrl Pts',(45.8455162977347,58.7169606500157,0.));
#107685=CARTESIAN_POINT('Ctrl Pts',(45.8455162977347,58.7169606500157,12.));
#107686=CARTESIAN_POINT('Ctrl Pts',(45.8467972562798,58.722407829904,0.));
#107687=CARTESIAN_POINT('Ctrl Pts',(45.8467972562798,58.722407829904,12.));
#107688=CARTESIAN_POINT('',(44.3377168516418,54.1679505278134,0.));
#107689=CARTESIAN_POINT('Ctrl Pts',(44.3377168516418,54.1679505278134,0.));
#107690=CARTESIAN_POINT('Ctrl Pts',(44.3393235891014,54.1714861895278,0.));
#107691=CARTESIAN_POINT('Ctrl Pts',(44.3425373700829,54.1785633257456,0.));
#107692=CARTESIAN_POINT('Ctrl Pts',(44.3473589597467,54.189196468444,0.));
#107693=CARTESIAN_POINT('Ctrl Pts',(44.3537895823819,54.203408870162,0.));
#107694=CARTESIAN_POINT('Ctrl Pts',(44.3618309103245,54.2212325005847,0.));
#107695=CARTESIAN_POINT('Ctrl Pts',(44.3698752533509,54.2391142386354,0.));
#107696=CARTESIAN_POINT('Ctrl Pts',(44.3779225430461,54.2570540336536,0.));
#107697=CARTESIAN_POINT('Ctrl Pts',(44.3859726620288,54.2750517888695,0.));
#107698=CARTESIAN_POINT('Ctrl Pts',(44.3940254456427,54.2931073621661,0.));
#107699=CARTESIAN_POINT('Ctrl Pts',(44.4020807028143,54.3112205860776,0.));
#107700=CARTESIAN_POINT('Ctrl Pts',(44.4101382321834,54.3293912830237,0.));
#107701=CARTESIAN_POINT('Ctrl Pts',(44.4181978395814,54.347619281931,0.));
#107702=CARTESIAN_POINT('Ctrl Pts',(44.4262593564664,54.3659044357064,0.));
#107703=CARTESIAN_POINT('Ctrl Pts',(44.4343226339554,54.3842466156151,0.));
#107704=CARTESIAN_POINT('Ctrl Pts',(44.442387534098,54.4026457030316,0.));
#107705=CARTESIAN_POINT('Ctrl Pts',(44.4504539226336,54.4211015825959,0.));
#107706=CARTESIAN_POINT('Ctrl Pts',(44.4585216599933,54.4396141337008,0.));
#107707=CARTESIAN_POINT('Ctrl Pts',(44.4665905967701,54.4581832262072,0.));
#107708=CARTESIAN_POINT('Ctrl Pts',(44.4746605784056,54.4768087248854,0.));
#107709=CARTESIAN_POINT('Ctrl Pts',(44.482731448127,54.4954904921938,0.));
#107710=CARTESIAN_POINT('Ctrl Pts',(44.4908030503209,54.5142283914684,0.));
#107711=CARTESIAN_POINT('Ctrl Pts',(44.4988752343714,54.5330222905438,0.));
#107712=CARTESIAN_POINT('Ctrl Pts',(44.5069478544945,54.5518720616016,0.));
#107713=CARTESIAN_POINT('Ctrl Pts',(44.5150207678988,54.5707775794412,0.));
#107714=CARTESIAN_POINT('Ctrl Pts',(44.5230938335167,54.5897387202815,0.));
#107715=CARTESIAN_POINT('Ctrl Pts',(44.5311669104514,54.6087553602914,0.));
#107716=CARTESIAN_POINT('Ctrl Pts',(44.5392398566802,54.6278273743587,0.));
#107717=CARTESIAN_POINT('Ctrl Pts',(44.5473125297311,54.6469546367408,0.));
#107718=CARTESIAN_POINT('Ctrl Pts',(44.5553847872721,54.6661370216252,0.));
#107719=CARTESIAN_POINT('Ctrl Pts',(44.5634564876863,54.6853744036751,0.));
#107720=CARTESIAN_POINT('Ctrl Pts',(44.5715274907619,54.7046666586754,0.));
#107721=CARTESIAN_POINT('Ctrl Pts',(44.5795976579454,54.7240136637717,0.));
#107722=CARTESIAN_POINT('Ctrl Pts',(44.5876668519661,54.7434152971267,0.));
#107723=CARTESIAN_POINT('Ctrl Pts',(44.5957349366058,54.7628714377037,0.));
#107724=CARTESIAN_POINT('Ctrl Pts',(44.6038017764309,54.7823819650149,0.));
#107725=CARTESIAN_POINT('Ctrl Pts',(44.6118672364906,54.8019467588278,0.));
#107726=CARTESIAN_POINT('Ctrl Pts',(44.6199311823293,54.8215656991837,0.));
#107727=CARTESIAN_POINT('Ctrl Pts',(44.6279934801168,54.8412386665276,0.));
#107728=CARTESIAN_POINT('Ctrl Pts',(44.6360539967392,54.860965541796,0.));
#107729=CARTESIAN_POINT('Ctrl Pts',(44.6441125999063,54.8807462065164,0.));
#107730=CARTESIAN_POINT('Ctrl Pts',(44.6521691582533,54.9005805428969,0.));
#107731=CARTESIAN_POINT('Ctrl Pts',(44.6602235412836,54.9204684337822,0.));
#107732=CARTESIAN_POINT('Ctrl Pts',(44.6682756193147,54.9404097626077,0.));
#107733=CARTESIAN_POINT('Ctrl Pts',(44.6763252634258,54.9604044133501,0.));
#107734=CARTESIAN_POINT('Ctrl Pts',(44.6843723454,54.9804522704686,0.));
#107735=CARTESIAN_POINT('Ctrl Pts',(44.6924167376869,55.0005532188667,0.));
#107736=CARTESIAN_POINT('Ctrl Pts',(44.7004583134249,55.0207071439237,0.));
#107737=CARTESIAN_POINT('Ctrl Pts',(44.7084969464513,55.0409139315078,0.));
#107738=CARTESIAN_POINT('Ctrl Pts',(44.7165325113159,55.0611734679894,0.));
#107739=CARTESIAN_POINT('Ctrl Pts',(44.7245648832979,55.0814856402496,0.));
#107740=CARTESIAN_POINT('Ctrl Pts',(44.7325939384035,55.1018503356796,0.));
#107741=CARTESIAN_POINT('Ctrl Pts',(44.7406195533479,55.1222674421743,0.));
#107742=CARTESIAN_POINT('Ctrl Pts',(44.7486416055419,55.14273684812,0.));
#107743=CARTESIAN_POINT('Ctrl Pts',(44.7566599730773,55.1632584423815,0.));
#107744=CARTESIAN_POINT('Ctrl Pts',(44.7646745347109,55.1838321142779,0.));
#107745=CARTESIAN_POINT('Ctrl Pts',(44.7726851698618,55.2044577535866,0.));
#107746=CARTESIAN_POINT('Ctrl Pts',(44.7806917586077,55.2251352505475,0.));
#107747=CARTESIAN_POINT('Ctrl Pts',(44.7886941816823,55.2458644958617,0.));
#107748=CARTESIAN_POINT('Ctrl Pts',(44.7966923204741,55.2666453806883,0.));
#107749=CARTESIAN_POINT('Ctrl Pts',(44.8046860570245,55.287477796635,0.));
#107750=CARTESIAN_POINT('Ctrl Pts',(44.812675274021,55.3083616357605,0.));
#107751=CARTESIAN_POINT('Ctrl Pts',(44.8206598547888,55.3292967905726,0.));
#107752=CARTESIAN_POINT('Ctrl Pts',(44.8286396832849,55.350283154023,0.));
#107753=CARTESIAN_POINT('Ctrl Pts',(44.8366146440896,55.3713206194962,0.));
#107754=CARTESIAN_POINT('Ctrl Pts',(44.8445846224033,55.3924090808002,0.));
#107755=CARTESIAN_POINT('Ctrl Pts',(44.8525495040397,55.4135484321706,0.));
#107756=CARTESIAN_POINT('Ctrl Pts',(44.8605091754208,55.4347385682697,0.));
#107757=CARTESIAN_POINT('Ctrl Pts',(44.8684635235727,55.4559793841838,0.));
#107758=CARTESIAN_POINT('Ctrl Pts',(44.8764124361218,55.4772707754139,0.));
#107759=CARTESIAN_POINT('Ctrl Pts',(44.8843558012903,55.4986126378676,0.));
#107760=CARTESIAN_POINT('Ctrl Pts',(44.8922935078905,55.5200048678648,0.));
#107761=CARTESIAN_POINT('Ctrl Pts',(44.9002254453192,55.541447362135,0.));
#107762=CARTESIAN_POINT('Ctrl Pts',(44.9081515035525,55.5629400178136,0.));
#107763=CARTESIAN_POINT('Ctrl Pts',(44.9160715731425,55.5844827324315,0.));
#107764=CARTESIAN_POINT('Ctrl Pts',(44.9239855452119,55.6060754039089,0.));
#107765=CARTESIAN_POINT('Ctrl Pts',(44.9318933114483,55.6277179305604,0.));
#107766=CARTESIAN_POINT('Ctrl Pts',(44.9397947640996,55.6494102110922,0.));
#107767=CARTESIAN_POINT('Ctrl Pts',(44.9476897959694,55.671152144599,0.));
#107768=CARTESIAN_POINT('Ctrl Pts',(44.9555783004133,55.6929436305522,0.));
#107769=CARTESIAN_POINT('Ctrl Pts',(44.9634601713352,55.7147845687969,0.));
#107770=CARTESIAN_POINT('Ctrl Pts',(44.9713353031827,55.7366748595582,0.));
#107771=CARTESIAN_POINT('Ctrl Pts',(44.979203590942,55.7586144034376,0.));
#107772=CARTESIAN_POINT('Ctrl Pts',(44.9870649301333,55.7806031014093,0.));
#107773=CARTESIAN_POINT('Ctrl Pts',(44.9949192168073,55.8026408548078,0.));
#107774=CARTESIAN_POINT('Ctrl Pts',(45.002766347541,55.8247275653257,0.));
#107775=CARTESIAN_POINT('Ctrl Pts',(45.0106062194325,55.8468631350195,0.));
#107776=CARTESIAN_POINT('Ctrl Pts',(45.0184387300968,55.8690474663058,0.));
#107777=CARTESIAN_POINT('Ctrl Pts',(45.0262637776623,55.8912804619588,0.));
#107778=CARTESIAN_POINT('Ctrl Pts',(45.0340812607675,55.9135620250977,0.));
#107779=CARTESIAN_POINT('Ctrl Pts',(45.041891078557,55.9358920591861,0.));
#107780=CARTESIAN_POINT('Ctrl Pts',(45.0496931306766,55.958270468037,0.));
#107781=CARTESIAN_POINT('Ctrl Pts',(45.0574873172696,55.9806971558099,0.));
#107782=CARTESIAN_POINT('Ctrl Pts',(45.0652735389728,56.0031720270074,0.));
#107783=CARTESIAN_POINT('Ctrl Pts',(45.0730516969142,56.025694986463,0.));
#107784=CARTESIAN_POINT('Ctrl Pts',(45.0808216927082,56.0482659393412,0.));
#107785=CARTESIAN_POINT('Ctrl Pts',(45.0885834284513,56.070884791141,0.));
#107786=CARTESIAN_POINT('Ctrl Pts',(45.0963368067177,56.0935514476946,0.));
#107787=CARTESIAN_POINT('Ctrl Pts',(45.1040817305563,56.1162658151621,0.));
#107788=CARTESIAN_POINT('Ctrl Pts',(45.1118181034888,56.1390278000226,0.));
#107789=CARTESIAN_POINT('Ctrl Pts',(45.119545829506,56.1618373090729,0.));
#107790=CARTESIAN_POINT('Ctrl Pts',(45.1272648130627,56.1846942494321,0.));
#107791=CARTESIAN_POINT('Ctrl Pts',(45.1349749590736,56.2075985285391,0.));
#107792=CARTESIAN_POINT('Ctrl Pts',(45.1426761729107,56.2305500541491,0.));
#107793=CARTESIAN_POINT('Ctrl Pts',(45.150368360401,56.2535487343227,0.));
#107794=CARTESIAN_POINT('Ctrl Pts',(45.158051427823,56.2765944774252,0.));
#107795=CARTESIAN_POINT('Ctrl Pts',(45.1657252819018,56.2996871921321,0.));
#107796=CARTESIAN_POINT('Ctrl Pts',(45.1733898298062,56.3228267874265,0.));
#107797=CARTESIAN_POINT('Ctrl Pts',(45.1810449791451,56.3460131725962,0.));
#107798=CARTESIAN_POINT('Ctrl Pts',(45.1886906379664,56.3692462572228,0.));
#107799=CARTESIAN_POINT('Ctrl Pts',(45.1963267147527,56.3925259511804,0.));
#107800=CARTESIAN_POINT('Ctrl Pts',(45.2039531184172,56.4158521646412,0.));
#107801=CARTESIAN_POINT('Ctrl Pts',(45.2115697583002,56.4392248080733,0.));
#107802=CARTESIAN_POINT('Ctrl Pts',(45.2191765441666,56.4626437922385,0.));
#107803=CARTESIAN_POINT('Ctrl Pts',(45.2267733862046,56.4861090281819,0.));
#107804=CARTESIAN_POINT('Ctrl Pts',(45.2343601950222,56.5096204272299,0.));
#107805=CARTESIAN_POINT('Ctrl Pts',(45.2419368816423,56.533177900995,0.));
#107806=CARTESIAN_POINT('Ctrl Pts',(45.2495033574997,56.5567813613752,0.));
#107807=CARTESIAN_POINT('Ctrl Pts',(45.2570595344382,56.5804307205507,0.));
#107808=CARTESIAN_POINT('Ctrl Pts',(45.2646053247094,56.604125890975,0.));
#107809=CARTESIAN_POINT('Ctrl Pts',(45.2721406409706,56.6278667853716,0.));
#107810=CARTESIAN_POINT('Ctrl Pts',(45.2796653962795,56.6516533167398,0.));
#107811=CARTESIAN_POINT('Ctrl Pts',(45.2871795040912,56.6754853983535,0.));
#107812=CARTESIAN_POINT('Ctrl Pts',(45.2946828782557,56.6993629437597,0.));
#107813=CARTESIAN_POINT('Ctrl Pts',(45.3021754330169,56.7232858667697,0.));
#107814=CARTESIAN_POINT('Ctrl Pts',(45.3096570830107,56.747254081454,0.));
#107815=CARTESIAN_POINT('Ctrl Pts',(45.3171277432592,56.771267502148,0.));
#107816=CARTESIAN_POINT('Ctrl Pts',(45.3245873291682,56.7953260434521,0.));
#107817=CARTESIAN_POINT('Ctrl Pts',(45.3320357565241,56.8194296202293,0.));
#107818=CARTESIAN_POINT('Ctrl Pts',(45.3394729414932,56.8435781475982,0.));
#107819=CARTESIAN_POINT('Ctrl Pts',(45.3468988006201,56.8677715409266,0.));
#107820=CARTESIAN_POINT('Ctrl Pts',(45.3543132508234,56.8920097158371,0.));
#107821=CARTESIAN_POINT('Ctrl Pts',(45.3617162093918,56.916292588208,0.));
#107822=CARTESIAN_POINT('Ctrl Pts',(45.3691075939827,56.9406200741714,0.));
#107823=CARTESIAN_POINT('Ctrl Pts',(45.3764873226202,56.9649920901079,0.));
#107824=CARTESIAN_POINT('Ctrl Pts',(45.3838553136957,56.9894085526383,0.));
#107825=CARTESIAN_POINT('Ctrl Pts',(45.3912114859624,57.0138693786287,0.));
#107826=CARTESIAN_POINT('Ctrl Pts',(45.3985557585316,57.0383744851917,0.));
#107827=CARTESIAN_POINT('Ctrl Pts',(45.4058880508693,57.0629237896848,0.));
#107828=CARTESIAN_POINT('Ctrl Pts',(45.4132082827945,57.0875172097048,0.));
#107829=CARTESIAN_POINT('Ctrl Pts',(45.4205163744778,57.1121546630776,0.));
#107830=CARTESIAN_POINT('Ctrl Pts',(45.4278122464387,57.1368360678629,0.));
#107831=CARTESIAN_POINT('Ctrl Pts',(45.4350958195434,57.1615613423586,0.));
#107832=CARTESIAN_POINT('Ctrl Pts',(45.4423670150035,57.1863304051011,0.));
#107833=CARTESIAN_POINT('Ctrl Pts',(45.4496257543758,57.2111431748629,0.));
#107834=CARTESIAN_POINT('Ctrl Pts',(45.4568719595639,57.2359995706441,0.));
#107835=CARTESIAN_POINT('Ctrl Pts',(45.4641055528137,57.2608995116727,0.));
#107836=CARTESIAN_POINT('Ctrl Pts',(45.4713264567059,57.2858429174056,0.));
#107837=CARTESIAN_POINT('Ctrl Pts',(45.4785345941505,57.3108297075262,0.));
#107838=CARTESIAN_POINT('Ctrl Pts',(45.4857298883826,57.3358598019391,0.));
#107839=CARTESIAN_POINT('Ctrl Pts',(45.4929122629576,57.360933120758,0.));
#107840=CARTESIAN_POINT('Ctrl Pts',(45.5000816417516,57.3860495843043,0.));
#107841=CARTESIAN_POINT('Ctrl Pts',(45.5072379489637,57.4112091131193,0.));
#107842=CARTESIAN_POINT('Ctrl Pts',(45.5143811091209,57.4364116279708,0.));
#107843=CARTESIAN_POINT('Ctrl Pts',(45.5215110470824,57.4616570498566,0.));
#107844=CARTESIAN_POINT('Ctrl Pts',(45.5286276880479,57.4869453000055,0.));
#107845=CARTESIAN_POINT('Ctrl Pts',(45.5357309575603,57.5122762998732,0.));
#107846=CARTESIAN_POINT('Ctrl Pts',(45.5428207814832,57.5376499711338,0.));
#107847=CARTESIAN_POINT('Ctrl Pts',(45.5498970859829,57.5630662356671,0.));
#107848=CARTESIAN_POINT('Ctrl Pts',(45.5569597975095,57.5885250155432,0.));
#107849=CARTESIAN_POINT('Ctrl Pts',(45.5640088427819,57.6140262330048,0.));
#107850=CARTESIAN_POINT('Ctrl Pts',(45.5710441487683,57.6395698104416,0.));
#107851=CARTESIAN_POINT('Ctrl Pts',(45.5780656427172,57.6651556704249,0.));
#107852=CARTESIAN_POINT('Ctrl Pts',(45.5850732521902,57.6907837357426,0.));
#107853=CARTESIAN_POINT('Ctrl Pts',(45.5920669050987,57.7164539294316,0.));
#107854=CARTESIAN_POINT('Ctrl Pts',(45.5990465297341,57.7421661748022,0.));
#107855=CARTESIAN_POINT('Ctrl Pts',(45.6060120548199,57.7679203954735,0.));
#107856=CARTESIAN_POINT('Ctrl Pts',(45.6129634094677,57.7937165153379,0.));
#107857=CARTESIAN_POINT('Ctrl Pts',(45.619900523078,57.819554458484,0.));
#107858=CARTESIAN_POINT('Ctrl Pts',(45.6268233252543,57.8454341491236,0.));
#107859=CARTESIAN_POINT('Ctrl Pts',(45.6337317457253,57.8713555115232,0.));
#107860=CARTESIAN_POINT('Ctrl Pts',(45.6406257142384,57.8973184699038,0.));
#107861=CARTESIAN_POINT('Ctrl Pts',(45.6475051605542,57.923322948432,0.));
#107862=CARTESIAN_POINT('Ctrl Pts',(45.6543700146688,57.9493688714249,0.));
#107863=CARTESIAN_POINT('Ctrl Pts',(45.6612202069927,57.975456163507,0.));
#107864=CARTESIAN_POINT('Ctrl Pts',(45.6680556685494,58.0015847497838,0.));
#107865=CARTESIAN_POINT('Ctrl Pts',(45.6748763311635,58.0277545560001,0.));
#107866=CARTESIAN_POINT('Ctrl Pts',(45.6816821276662,58.0539655087095,0.));
#107867=CARTESIAN_POINT('Ctrl Pts',(45.6884729914465,58.0802175348939,0.));
#107868=CARTESIAN_POINT('Ctrl Pts',(45.6952488560133,58.1065105615884,0.));
#107869=CARTESIAN_POINT('Ctrl Pts',(45.7020096545174,58.1328445154667,0.));
#107870=CARTESIAN_POINT('Ctrl Pts',(45.708755319378,58.159219322515,0.));
#107871=CARTESIAN_POINT('Ctrl Pts',(45.7154857816507,58.1856349074723,0.));
#107872=CARTESIAN_POINT('Ctrl Pts',(45.7222009715431,58.2120911942819,0.));
#107873=CARTESIAN_POINT('Ctrl Pts',(45.7289008195612,58.2385881070959,0.));
#107874=CARTESIAN_POINT('Ctrl Pts',(45.7355852575127,58.2651255711481,0.));
#107875=CARTESIAN_POINT('Ctrl Pts',(45.7422542194625,58.2917035135833,0.));
#107876=CARTESIAN_POINT('Ctrl Pts',(45.7489076429725,58.3183218645265,0.));
#107877=CARTESIAN_POINT('Ctrl Pts',(45.7555454693956,58.3449805573335,0.));
#107878=CARTESIAN_POINT('Ctrl Pts',(45.7612219538034,58.3678667473265,0.));
#107879=CARTESIAN_POINT('Ctrl Pts',(45.7655655205267,58.385434851721,0.));
#107880=CARTESIAN_POINT('Ctrl Pts',(45.7685831165459,58.3976670480779,0.));
#107881=CARTESIAN_POINT('Ctrl Pts',(45.7702793558062,58.4045515723007,0.));
#107882=CARTESIAN_POINT('Ctrl Pts',(45.7706564944766,58.4060826907377,0.));
#107883=CARTESIAN_POINT('',(44.3377168516418,54.1679505278134,12.));
#107884=CARTESIAN_POINT('',(44.3377168516418,54.1679505278134,0.));
#107885=CARTESIAN_POINT('Ctrl Pts',(45.7706564944766,58.4060826907378,12.));
#107886=CARTESIAN_POINT('Ctrl Pts',(45.7702793558062,58.4045515723008,12.));
#107887=CARTESIAN_POINT('Ctrl Pts',(45.7685831165459,58.397667048078,12.));
#107888=CARTESIAN_POINT('Ctrl Pts',(45.7655655205267,58.385434851721,12.));
#107889=CARTESIAN_POINT('Ctrl Pts',(45.7612219538034,58.3678667473266,12.));
#107890=CARTESIAN_POINT('Ctrl Pts',(45.7555454693956,58.3449805573335,12.));
#107891=CARTESIAN_POINT('Ctrl Pts',(45.7489076429725,58.3183218645265,12.));
#107892=CARTESIAN_POINT('Ctrl Pts',(45.7422542194625,58.2917035135833,12.));
#107893=CARTESIAN_POINT('Ctrl Pts',(45.7355852575127,58.2651255711481,12.));
#107894=CARTESIAN_POINT('Ctrl Pts',(45.7289008195612,58.2385881070959,12.));
#107895=CARTESIAN_POINT('Ctrl Pts',(45.7222009715431,58.2120911942819,12.));
#107896=CARTESIAN_POINT('Ctrl Pts',(45.7154857816507,58.1856349074723,12.));
#107897=CARTESIAN_POINT('Ctrl Pts',(45.708755319378,58.159219322515,12.));
#107898=CARTESIAN_POINT('Ctrl Pts',(45.7020096545174,58.1328445154667,12.));
#107899=CARTESIAN_POINT('Ctrl Pts',(45.6952488560133,58.1065105615884,12.));
#107900=CARTESIAN_POINT('Ctrl Pts',(45.6884729914465,58.0802175348939,12.));
#107901=CARTESIAN_POINT('Ctrl Pts',(45.6816821276662,58.0539655087095,12.));
#107902=CARTESIAN_POINT('Ctrl Pts',(45.6748763311635,58.0277545560001,12.));
#107903=CARTESIAN_POINT('Ctrl Pts',(45.6680556685494,58.0015847497838,12.));
#107904=CARTESIAN_POINT('Ctrl Pts',(45.6612202069927,57.975456163507,12.));
#107905=CARTESIAN_POINT('Ctrl Pts',(45.6543700146688,57.9493688714249,12.));
#107906=CARTESIAN_POINT('Ctrl Pts',(45.6475051605542,57.923322948432,12.));
#107907=CARTESIAN_POINT('Ctrl Pts',(45.6406257142384,57.8973184699038,12.));
#107908=CARTESIAN_POINT('Ctrl Pts',(45.6337317457253,57.8713555115232,12.));
#107909=CARTESIAN_POINT('Ctrl Pts',(45.6268233252543,57.8454341491236,12.));
#107910=CARTESIAN_POINT('Ctrl Pts',(45.619900523078,57.819554458484,12.));
#107911=CARTESIAN_POINT('Ctrl Pts',(45.6129634094677,57.7937165153379,12.));
#107912=CARTESIAN_POINT('Ctrl Pts',(45.6060120548199,57.7679203954735,12.));
#107913=CARTESIAN_POINT('Ctrl Pts',(45.5990465297341,57.7421661748022,12.));
#107914=CARTESIAN_POINT('Ctrl Pts',(45.5920669050987,57.7164539294316,12.));
#107915=CARTESIAN_POINT('Ctrl Pts',(45.5850732521902,57.6907837357426,12.));
#107916=CARTESIAN_POINT('Ctrl Pts',(45.5780656427172,57.6651556704249,12.));
#107917=CARTESIAN_POINT('Ctrl Pts',(45.5710441487683,57.6395698104416,12.));
#107918=CARTESIAN_POINT('Ctrl Pts',(45.5640088427819,57.6140262330048,12.));
#107919=CARTESIAN_POINT('Ctrl Pts',(45.5569597975095,57.5885250155432,12.));
#107920=CARTESIAN_POINT('Ctrl Pts',(45.5498970859829,57.5630662356671,12.));
#107921=CARTESIAN_POINT('Ctrl Pts',(45.5428207814832,57.5376499711338,12.));
#107922=CARTESIAN_POINT('Ctrl Pts',(45.5357309575603,57.5122762998732,12.));
#107923=CARTESIAN_POINT('Ctrl Pts',(45.5286276880479,57.4869453000055,12.));
#107924=CARTESIAN_POINT('Ctrl Pts',(45.5215110470824,57.4616570498566,12.));
#107925=CARTESIAN_POINT('Ctrl Pts',(45.5143811091209,57.4364116279708,12.));
#107926=CARTESIAN_POINT('Ctrl Pts',(45.5072379489637,57.4112091131193,12.));
#107927=CARTESIAN_POINT('Ctrl Pts',(45.5000816417516,57.3860495843043,12.));
#107928=CARTESIAN_POINT('Ctrl Pts',(45.4929122629576,57.360933120758,12.));
#107929=CARTESIAN_POINT('Ctrl Pts',(45.4857298883826,57.3358598019391,12.));
#107930=CARTESIAN_POINT('Ctrl Pts',(45.4785345941505,57.3108297075262,12.));
#107931=CARTESIAN_POINT('Ctrl Pts',(45.4713264567059,57.2858429174056,12.));
#107932=CARTESIAN_POINT('Ctrl Pts',(45.4641055528137,57.2608995116727,12.));
#107933=CARTESIAN_POINT('Ctrl Pts',(45.4568719595639,57.2359995706441,12.));
#107934=CARTESIAN_POINT('Ctrl Pts',(45.4496257543758,57.2111431748629,12.));
#107935=CARTESIAN_POINT('Ctrl Pts',(45.4423670150035,57.1863304051011,12.));
#107936=CARTESIAN_POINT('Ctrl Pts',(45.4350958195434,57.1615613423586,12.));
#107937=CARTESIAN_POINT('Ctrl Pts',(45.4278122464387,57.1368360678629,12.));
#107938=CARTESIAN_POINT('Ctrl Pts',(45.4205163744778,57.1121546630776,12.));
#107939=CARTESIAN_POINT('Ctrl Pts',(45.4132082827945,57.0875172097048,12.));
#107940=CARTESIAN_POINT('Ctrl Pts',(45.4058880508693,57.0629237896848,12.));
#107941=CARTESIAN_POINT('Ctrl Pts',(45.3985557585316,57.0383744851917,12.));
#107942=CARTESIAN_POINT('Ctrl Pts',(45.3912114859624,57.0138693786287,12.));
#107943=CARTESIAN_POINT('Ctrl Pts',(45.3838553136957,56.9894085526383,12.));
#107944=CARTESIAN_POINT('Ctrl Pts',(45.3764873226202,56.9649920901079,12.));
#107945=CARTESIAN_POINT('Ctrl Pts',(45.3691075939827,56.9406200741714,12.));
#107946=CARTESIAN_POINT('Ctrl Pts',(45.3617162093918,56.916292588208,12.));
#107947=CARTESIAN_POINT('Ctrl Pts',(45.3543132508234,56.8920097158371,12.));
#107948=CARTESIAN_POINT('Ctrl Pts',(45.3468988006201,56.8677715409266,12.));
#107949=CARTESIAN_POINT('Ctrl Pts',(45.3394729414932,56.8435781475982,12.));
#107950=CARTESIAN_POINT('Ctrl Pts',(45.3320357565241,56.8194296202293,12.));
#107951=CARTESIAN_POINT('Ctrl Pts',(45.3245873291682,56.7953260434521,12.));
#107952=CARTESIAN_POINT('Ctrl Pts',(45.3171277432592,56.771267502148,12.));
#107953=CARTESIAN_POINT('Ctrl Pts',(45.3096570830107,56.747254081454,12.));
#107954=CARTESIAN_POINT('Ctrl Pts',(45.3021754330169,56.7232858667697,12.));
#107955=CARTESIAN_POINT('Ctrl Pts',(45.2946828782557,56.6993629437597,12.));
#107956=CARTESIAN_POINT('Ctrl Pts',(45.2871795040912,56.6754853983535,12.));
#107957=CARTESIAN_POINT('Ctrl Pts',(45.2796653962795,56.6516533167398,12.));
#107958=CARTESIAN_POINT('Ctrl Pts',(45.2721406409706,56.6278667853716,12.));
#107959=CARTESIAN_POINT('Ctrl Pts',(45.2646053247094,56.604125890975,12.));
#107960=CARTESIAN_POINT('Ctrl Pts',(45.2570595344382,56.5804307205507,12.));
#107961=CARTESIAN_POINT('Ctrl Pts',(45.2495033574997,56.5567813613752,12.));
#107962=CARTESIAN_POINT('Ctrl Pts',(45.2419368816423,56.533177900995,12.));
#107963=CARTESIAN_POINT('Ctrl Pts',(45.2343601950222,56.5096204272299,12.));
#107964=CARTESIAN_POINT('Ctrl Pts',(45.2267733862046,56.4861090281819,12.));
#107965=CARTESIAN_POINT('Ctrl Pts',(45.2191765441666,56.4626437922385,12.));
#107966=CARTESIAN_POINT('Ctrl Pts',(45.2115697583002,56.4392248080733,12.));
#107967=CARTESIAN_POINT('Ctrl Pts',(45.2039531184172,56.4158521646412,12.));
#107968=CARTESIAN_POINT('Ctrl Pts',(45.1963267147527,56.3925259511804,12.));
#107969=CARTESIAN_POINT('Ctrl Pts',(45.1886906379664,56.3692462572228,12.));
#107970=CARTESIAN_POINT('Ctrl Pts',(45.1810449791451,56.3460131725962,12.));
#107971=CARTESIAN_POINT('Ctrl Pts',(45.1733898298062,56.3228267874265,12.));
#107972=CARTESIAN_POINT('Ctrl Pts',(45.1657252819018,56.2996871921321,12.));
#107973=CARTESIAN_POINT('Ctrl Pts',(45.158051427823,56.2765944774252,12.));
#107974=CARTESIAN_POINT('Ctrl Pts',(45.150368360401,56.2535487343227,12.));
#107975=CARTESIAN_POINT('Ctrl Pts',(45.1426761729107,56.2305500541491,12.));
#107976=CARTESIAN_POINT('Ctrl Pts',(45.1349749590736,56.2075985285391,12.));
#107977=CARTESIAN_POINT('Ctrl Pts',(45.1272648130627,56.1846942494321,12.));
#107978=CARTESIAN_POINT('Ctrl Pts',(45.119545829506,56.1618373090729,12.));
#107979=CARTESIAN_POINT('Ctrl Pts',(45.1118181034888,56.1390278000226,12.));
#107980=CARTESIAN_POINT('Ctrl Pts',(45.1040817305563,56.1162658151621,12.));
#107981=CARTESIAN_POINT('Ctrl Pts',(45.0963368067177,56.0935514476946,12.));
#107982=CARTESIAN_POINT('Ctrl Pts',(45.0885834284513,56.070884791141,12.));
#107983=CARTESIAN_POINT('Ctrl Pts',(45.0808216927082,56.0482659393412,12.));
#107984=CARTESIAN_POINT('Ctrl Pts',(45.0730516969142,56.025694986463,12.));
#107985=CARTESIAN_POINT('Ctrl Pts',(45.0652735389728,56.0031720270074,12.));
#107986=CARTESIAN_POINT('Ctrl Pts',(45.0574873172696,55.9806971558099,12.));
#107987=CARTESIAN_POINT('Ctrl Pts',(45.0496931306766,55.958270468037,12.));
#107988=CARTESIAN_POINT('Ctrl Pts',(45.041891078557,55.9358920591861,12.));
#107989=CARTESIAN_POINT('Ctrl Pts',(45.0340812607675,55.9135620250977,12.));
#107990=CARTESIAN_POINT('Ctrl Pts',(45.0262637776623,55.8912804619588,12.));
#107991=CARTESIAN_POINT('Ctrl Pts',(45.0184387300968,55.8690474663058,12.));
#107992=CARTESIAN_POINT('Ctrl Pts',(45.0106062194325,55.8468631350195,12.));
#107993=CARTESIAN_POINT('Ctrl Pts',(45.002766347541,55.8247275653257,12.));
#107994=CARTESIAN_POINT('Ctrl Pts',(44.9949192168073,55.8026408548078,12.));
#107995=CARTESIAN_POINT('Ctrl Pts',(44.9870649301333,55.7806031014093,12.));
#107996=CARTESIAN_POINT('Ctrl Pts',(44.979203590942,55.7586144034376,12.));
#107997=CARTESIAN_POINT('Ctrl Pts',(44.9713353031827,55.7366748595582,12.));
#107998=CARTESIAN_POINT('Ctrl Pts',(44.9634601713352,55.7147845687969,12.));
#107999=CARTESIAN_POINT('Ctrl Pts',(44.9555783004133,55.6929436305522,12.));
#108000=CARTESIAN_POINT('Ctrl Pts',(44.9476897959694,55.671152144599,12.));
#108001=CARTESIAN_POINT('Ctrl Pts',(44.9397947640996,55.6494102110922,12.));
#108002=CARTESIAN_POINT('Ctrl Pts',(44.9318933114483,55.6277179305604,12.));
#108003=CARTESIAN_POINT('Ctrl Pts',(44.9239855452119,55.6060754039089,12.));
#108004=CARTESIAN_POINT('Ctrl Pts',(44.9160715731425,55.5844827324315,12.));
#108005=CARTESIAN_POINT('Ctrl Pts',(44.9081515035525,55.5629400178136,12.));
#108006=CARTESIAN_POINT('Ctrl Pts',(44.9002254453192,55.541447362135,12.));
#108007=CARTESIAN_POINT('Ctrl Pts',(44.8922935078905,55.5200048678648,12.));
#108008=CARTESIAN_POINT('Ctrl Pts',(44.8843558012903,55.4986126378676,12.));
#108009=CARTESIAN_POINT('Ctrl Pts',(44.8764124361218,55.4772707754139,12.));
#108010=CARTESIAN_POINT('Ctrl Pts',(44.8684635235727,55.4559793841838,12.));
#108011=CARTESIAN_POINT('Ctrl Pts',(44.8605091754208,55.4347385682697,12.));
#108012=CARTESIAN_POINT('Ctrl Pts',(44.8525495040397,55.4135484321706,12.));
#108013=CARTESIAN_POINT('Ctrl Pts',(44.8445846224033,55.3924090808002,12.));
#108014=CARTESIAN_POINT('Ctrl Pts',(44.8366146440896,55.3713206194962,12.));
#108015=CARTESIAN_POINT('Ctrl Pts',(44.8286396832849,55.350283154023,12.));
#108016=CARTESIAN_POINT('Ctrl Pts',(44.8206598547888,55.3292967905726,12.));
#108017=CARTESIAN_POINT('Ctrl Pts',(44.812675274021,55.3083616357605,12.));
#108018=CARTESIAN_POINT('Ctrl Pts',(44.8046860570245,55.287477796635,12.));
#108019=CARTESIAN_POINT('Ctrl Pts',(44.7966923204741,55.2666453806883,12.));
#108020=CARTESIAN_POINT('Ctrl Pts',(44.7886941816823,55.2458644958617,12.));
#108021=CARTESIAN_POINT('Ctrl Pts',(44.7806917586077,55.2251352505475,12.));
#108022=CARTESIAN_POINT('Ctrl Pts',(44.7726851698618,55.2044577535866,12.));
#108023=CARTESIAN_POINT('Ctrl Pts',(44.7646745347109,55.1838321142779,12.));
#108024=CARTESIAN_POINT('Ctrl Pts',(44.7566599730773,55.1632584423815,12.));
#108025=CARTESIAN_POINT('Ctrl Pts',(44.7486416055419,55.14273684812,12.));
#108026=CARTESIAN_POINT('Ctrl Pts',(44.7406195533479,55.1222674421743,12.));
#108027=CARTESIAN_POINT('Ctrl Pts',(44.7325939384035,55.1018503356796,12.));
#108028=CARTESIAN_POINT('Ctrl Pts',(44.7245648832979,55.0814856402496,12.));
#108029=CARTESIAN_POINT('Ctrl Pts',(44.7165325113159,55.0611734679894,12.));
#108030=CARTESIAN_POINT('Ctrl Pts',(44.7084969464513,55.0409139315078,12.));
#108031=CARTESIAN_POINT('Ctrl Pts',(44.7004583134249,55.0207071439237,12.));
#108032=CARTESIAN_POINT('Ctrl Pts',(44.6924167376869,55.0005532188667,12.));
#108033=CARTESIAN_POINT('Ctrl Pts',(44.6843723454,54.9804522704686,12.));
#108034=CARTESIAN_POINT('Ctrl Pts',(44.6763252634258,54.9604044133501,12.));
#108035=CARTESIAN_POINT('Ctrl Pts',(44.6682756193147,54.9404097626077,12.));
#108036=CARTESIAN_POINT('Ctrl Pts',(44.6602235412836,54.9204684337822,12.));
#108037=CARTESIAN_POINT('Ctrl Pts',(44.6521691582533,54.9005805428969,12.));
#108038=CARTESIAN_POINT('Ctrl Pts',(44.6441125999063,54.8807462065164,12.));
#108039=CARTESIAN_POINT('Ctrl Pts',(44.6360539967392,54.860965541796,12.));
#108040=CARTESIAN_POINT('Ctrl Pts',(44.6279934801168,54.8412386665276,12.));
#108041=CARTESIAN_POINT('Ctrl Pts',(44.6199311823293,54.8215656991837,12.));
#108042=CARTESIAN_POINT('Ctrl Pts',(44.6118672364906,54.8019467588278,12.));
#108043=CARTESIAN_POINT('Ctrl Pts',(44.6038017764309,54.7823819650149,12.));
#108044=CARTESIAN_POINT('Ctrl Pts',(44.5957349366058,54.7628714377037,12.));
#108045=CARTESIAN_POINT('Ctrl Pts',(44.5876668519661,54.7434152971267,12.));
#108046=CARTESIAN_POINT('Ctrl Pts',(44.5795976579454,54.7240136637717,12.));
#108047=CARTESIAN_POINT('Ctrl Pts',(44.5715274907619,54.7046666586754,12.));
#108048=CARTESIAN_POINT('Ctrl Pts',(44.5634564876863,54.6853744036751,12.));
#108049=CARTESIAN_POINT('Ctrl Pts',(44.5553847872721,54.6661370216252,12.));
#108050=CARTESIAN_POINT('Ctrl Pts',(44.5473125297311,54.6469546367408,12.));
#108051=CARTESIAN_POINT('Ctrl Pts',(44.5392398566802,54.6278273743587,12.));
#108052=CARTESIAN_POINT('Ctrl Pts',(44.5311669104514,54.6087553602914,12.));
#108053=CARTESIAN_POINT('Ctrl Pts',(44.5230938335167,54.5897387202815,12.));
#108054=CARTESIAN_POINT('Ctrl Pts',(44.5150207678988,54.5707775794412,12.));
#108055=CARTESIAN_POINT('Ctrl Pts',(44.5069478544945,54.5518720616016,12.));
#108056=CARTESIAN_POINT('Ctrl Pts',(44.4988752343714,54.5330222905438,12.));
#108057=CARTESIAN_POINT('Ctrl Pts',(44.4908030503209,54.5142283914684,12.));
#108058=CARTESIAN_POINT('Ctrl Pts',(44.482731448127,54.4954904921938,12.));
#108059=CARTESIAN_POINT('Ctrl Pts',(44.4746605784056,54.4768087248854,12.));
#108060=CARTESIAN_POINT('Ctrl Pts',(44.4665905967701,54.4581832262072,12.));
#108061=CARTESIAN_POINT('Ctrl Pts',(44.4585216599933,54.4396141337008,12.));
#108062=CARTESIAN_POINT('Ctrl Pts',(44.4504539226336,54.4211015825959,12.));
#108063=CARTESIAN_POINT('Ctrl Pts',(44.442387534098,54.4026457030316,12.));
#108064=CARTESIAN_POINT('Ctrl Pts',(44.4343226339554,54.3842466156151,12.));
#108065=CARTESIAN_POINT('Ctrl Pts',(44.4262593564664,54.3659044357064,12.));
#108066=CARTESIAN_POINT('Ctrl Pts',(44.4181978395814,54.347619281931,12.));
#108067=CARTESIAN_POINT('Ctrl Pts',(44.4101382321834,54.3293912830237,12.));
#108068=CARTESIAN_POINT('Ctrl Pts',(44.4020807028143,54.3112205860776,12.));
#108069=CARTESIAN_POINT('Ctrl Pts',(44.3940254456427,54.2931073621661,12.));
#108070=CARTESIAN_POINT('Ctrl Pts',(44.3859726620288,54.2750517888695,12.));
#108071=CARTESIAN_POINT('Ctrl Pts',(44.3779225430461,54.2570540336536,12.));
#108072=CARTESIAN_POINT('Ctrl Pts',(44.3698752533509,54.2391142386354,12.));
#108073=CARTESIAN_POINT('Ctrl Pts',(44.3618309103245,54.2212325005847,12.));
#108074=CARTESIAN_POINT('Ctrl Pts',(44.3537895823819,54.203408870162,12.));
#108075=CARTESIAN_POINT('Ctrl Pts',(44.3473589597467,54.189196468444,12.));
#108076=CARTESIAN_POINT('Ctrl Pts',(44.3425373700829,54.1785633257456,12.));
#108077=CARTESIAN_POINT('Ctrl Pts',(44.3393235891014,54.1714861895278,12.));
#108078=CARTESIAN_POINT('Ctrl Pts',(44.3377168516418,54.1679505278134,12.));
#108079=CARTESIAN_POINT('Ctrl Pts',(44.5696260757798,59.3276657444395,-5.55111512312578E-16));
#108080=CARTESIAN_POINT('Ctrl Pts',(44.5696260757798,59.3276657444395,4.));
#108081=CARTESIAN_POINT('Ctrl Pts',(44.5696260757798,59.3276657444395,8.));
#108082=CARTESIAN_POINT('Ctrl Pts',(44.5696260757798,59.3276657444395,12.));
#108083=CARTESIAN_POINT('Ctrl Pts',(44.6658822400938,59.380664869172,-5.55111512312578E-16));
#108084=CARTESIAN_POINT('Ctrl Pts',(44.6658822400938,59.380664869172,4.));
#108085=CARTESIAN_POINT('Ctrl Pts',(44.6658822400938,59.3806648691719,8.));
#108086=CARTESIAN_POINT('Ctrl Pts',(44.6658822400938,59.3806648691719,12.));
#108087=CARTESIAN_POINT('Ctrl Pts',(44.8655383388343,59.4154499491516,-5.55111512312578E-16));
#108088=CARTESIAN_POINT('Ctrl Pts',(44.8655383388343,59.4154499491516,4.));
#108089=CARTESIAN_POINT('Ctrl Pts',(44.8655383388343,59.4154499491515,8.));
#108090=CARTESIAN_POINT('Ctrl Pts',(44.8655383388343,59.4154499491515,12.));
#108091=CARTESIAN_POINT('Ctrl Pts',(45.0479805952319,59.3374774995079,-5.55111512312578E-16));
#108092=CARTESIAN_POINT('Ctrl Pts',(45.0479805952319,59.3374774995079,4.));
#108093=CARTESIAN_POINT('Ctrl Pts',(45.0479805952318,59.3374774995078,8.));
#108094=CARTESIAN_POINT('Ctrl Pts',(45.0479805952318,59.3374774995078,12.));
#108095=CARTESIAN_POINT('Ctrl Pts',(45.1135644683449,59.2875729049564,-5.55111512312578E-16));
#108096=CARTESIAN_POINT('Ctrl Pts',(45.1135644683449,59.2875729049564,4.));
#108097=CARTESIAN_POINT('Ctrl Pts',(45.1135644683448,59.2875729049563,8.));
#108098=CARTESIAN_POINT('Ctrl Pts',(45.1135644683448,59.2875729049563,12.));
#108099=CARTESIAN_POINT('',(44.5696260757798,59.3276657444395,2.77555756156289E-16));
#108100=CARTESIAN_POINT('',(45.1135644683448,59.2875729049562,0.));
#108101=CARTESIAN_POINT('Ctrl Pts',(44.5696260757798,59.3276657444395,-4.16333634234434E-16));
#108102=CARTESIAN_POINT('Ctrl Pts',(44.6658822400938,59.380664869172,-4.16333634234434E-16));
#108103=CARTESIAN_POINT('Ctrl Pts',(44.7799714393741,59.4005420577317,-4.16333634234434E-16));
#108104=CARTESIAN_POINT('Ctrl Pts',(44.888439792175,59.3836004611084,-4.16333634234434E-16));
#108105=CARTESIAN_POINT('Ctrl Pts',(44.9697910567758,59.3708942636409,-4.16333634234434E-16));
#108106=CARTESIAN_POINT('Ctrl Pts',(45.0479805952319,59.3374774995079,-4.16333634234434E-16));
#108107=CARTESIAN_POINT('Ctrl Pts',(45.1135644683449,59.2875729049564,-4.16333634234434E-16));
#108108=CARTESIAN_POINT('',(45.1135644683447,59.2875729049563,12.));
#108109=CARTESIAN_POINT('Ctrl Pts',(45.1135644683449,59.2875729049564,-5.55111512312578E-16));
#108110=CARTESIAN_POINT('Ctrl Pts',(45.1135644683449,59.2875729049564,4.));
#108111=CARTESIAN_POINT('Ctrl Pts',(45.1135644683448,59.2875729049563,8.));
#108112=CARTESIAN_POINT('Ctrl Pts',(45.1135644683448,59.2875729049563,12.));
#108113=CARTESIAN_POINT('',(44.5696260757798,59.3276657444395,12.));
#108114=CARTESIAN_POINT('Ctrl Pts',(45.1135644683448,59.2875729049563,12.));
#108115=CARTESIAN_POINT('Ctrl Pts',(45.0479805952318,59.3374774995078,12.));
#108116=CARTESIAN_POINT('Ctrl Pts',(44.9697910567757,59.3708942636408,12.));
#108117=CARTESIAN_POINT('Ctrl Pts',(44.888439792175,59.3836004611083,12.));
#108118=CARTESIAN_POINT('Ctrl Pts',(44.7799714393741,59.4005420577317,12.));
#108119=CARTESIAN_POINT('Ctrl Pts',(44.6658822400938,59.3806648691719,12.));
#108120=CARTESIAN_POINT('Ctrl Pts',(44.5696260757798,59.3276657444395,12.));
#108121=CARTESIAN_POINT('Ctrl Pts',(44.5696260757798,59.3276657444395,12.));
#108122=CARTESIAN_POINT('Ctrl Pts',(44.5696260757798,59.3276657444395,8.));
#108123=CARTESIAN_POINT('Ctrl Pts',(44.5696260757798,59.3276657444395,4.));
#108124=CARTESIAN_POINT('Ctrl Pts',(44.5696260757798,59.3276657444395,-5.55111512312578E-16));
#108125=CARTESIAN_POINT('Origin',(2.28111678886296E-10,2.97443977737815E-10,
0.));
#108126=CARTESIAN_POINT('Origin',(2.28111678886296E-10,2.97443977737815E-10,
12.));
#108127=CARTESIAN_POINT('Origin',(2.28111678886296E-10,2.97443977737815E-10,
0.));
#108128=CARTESIAN_POINT('Ctrl Pts',(50.5529731960876,54.7233670476849,0.));
#108129=CARTESIAN_POINT('Ctrl Pts',(50.5529731960876,54.7233670476849,4.));
#108130=CARTESIAN_POINT('Ctrl Pts',(50.5529731960876,54.7233670476849,8.));
#108131=CARTESIAN_POINT('Ctrl Pts',(50.5529731960876,54.7233670476849,12.));
#108132=CARTESIAN_POINT('Ctrl Pts',(50.6336864649947,54.6488048279283,0.));
#108133=CARTESIAN_POINT('Ctrl Pts',(50.6336864649947,54.6488048279283,4.));
#108134=CARTESIAN_POINT('Ctrl Pts',(50.6336864649947,54.6488048279283,8.));
#108135=CARTESIAN_POINT('Ctrl Pts',(50.6336864649947,54.6488048279283,12.));
#108136=CARTESIAN_POINT('Ctrl Pts',(50.7298112257545,54.4703879751555,0.));
#108137=CARTESIAN_POINT('Ctrl Pts',(50.7298112257545,54.4703879751555,4.00000000000001));
#108138=CARTESIAN_POINT('Ctrl Pts',(50.7298112257545,54.4703879751555,8.));
#108139=CARTESIAN_POINT('Ctrl Pts',(50.7298112257545,54.4703879751555,12.));
#108140=CARTESIAN_POINT('Ctrl Pts',(50.7135202769403,54.2726521137411,0.));
#108141=CARTESIAN_POINT('Ctrl Pts',(50.7135202769403,54.2726521137411,4.));
#108142=CARTESIAN_POINT('Ctrl Pts',(50.7135202769403,54.2726521137411,8.));
#108143=CARTESIAN_POINT('Ctrl Pts',(50.7135202769403,54.2726521137411,12.));
#108144=CARTESIAN_POINT('Ctrl Pts',(50.6869108458687,54.1946543499979,0.));
#108145=CARTESIAN_POINT('Ctrl Pts',(50.6869108458687,54.1946543499979,4.));
#108146=CARTESIAN_POINT('Ctrl Pts',(50.6869108458687,54.1946543499979,8.));
#108147=CARTESIAN_POINT('Ctrl Pts',(50.6869108458687,54.1946543499979,12.));
#108148=CARTESIAN_POINT('',(50.5529731960876,54.7233670476849,0.));
#108149=CARTESIAN_POINT('',(50.6869108458688,54.1946543499978,0.));
#108150=CARTESIAN_POINT('Ctrl Pts',(50.5529731960876,54.7233670476849,1.38777878078145E-16));
#108151=CARTESIAN_POINT('Ctrl Pts',(50.6336864649947,54.6488048279283,1.38777878078144E-16));
#108152=CARTESIAN_POINT('Ctrl Pts',(50.6886148997146,54.5468523406296,1.38777878078145E-16));
#108153=CARTESIAN_POINT('Ctrl Pts',(50.7068361639613,54.4385916056111,1.38777878078145E-16));
#108154=CARTESIAN_POINT('Ctrl Pts',(50.7205021121464,54.3573960543472,1.38777878078145E-16));
#108155=CARTESIAN_POINT('Ctrl Pts',(50.7135202769403,54.2726521137411,1.38777878078144E-16));
#108156=CARTESIAN_POINT('Ctrl Pts',(50.6869108458687,54.1946543499979,1.38777878078145E-16));
#108157=CARTESIAN_POINT('',(50.6869108458688,54.1946543499978,12.));
#108158=CARTESIAN_POINT('Ctrl Pts',(50.6869108458687,54.1946543499979,0.));
#108159=CARTESIAN_POINT('Ctrl Pts',(50.6869108458687,54.1946543499979,4.));
#108160=CARTESIAN_POINT('Ctrl Pts',(50.6869108458687,54.1946543499979,8.));
#108161=CARTESIAN_POINT('Ctrl Pts',(50.6869108458687,54.1946543499979,12.));
#108162=CARTESIAN_POINT('',(50.5529731960876,54.7233670476849,12.));
#108163=CARTESIAN_POINT('Ctrl Pts',(50.6869108458687,54.1946543499979,12.));
#108164=CARTESIAN_POINT('Ctrl Pts',(50.7135202769403,54.2726521137411,12.));
#108165=CARTESIAN_POINT('Ctrl Pts',(50.7205021121464,54.3573960543472,12.));
#108166=CARTESIAN_POINT('Ctrl Pts',(50.7068361639613,54.4385916056111,12.));
#108167=CARTESIAN_POINT('Ctrl Pts',(50.6886148997146,54.5468523406296,12.));
#108168=CARTESIAN_POINT('Ctrl Pts',(50.6336864649947,54.6488048279283,12.));
#108169=CARTESIAN_POINT('Ctrl Pts',(50.5529731960876,54.7233670476849,12.));
#108170=CARTESIAN_POINT('Ctrl Pts',(50.5529731960876,54.7233670476849,12.));
#108171=CARTESIAN_POINT('Ctrl Pts',(50.5529731960876,54.7233670476849,8.));
#108172=CARTESIAN_POINT('Ctrl Pts',(50.5529731960876,54.7233670476849,4.));
#108173=CARTESIAN_POINT('Ctrl Pts',(50.5529731960876,54.7233670476849,0.));
#108174=CARTESIAN_POINT('Ctrl Pts',(48.8900464144686,50.0975384783634,0.));
#108175=CARTESIAN_POINT('Ctrl Pts',(48.8900464144686,50.0975384783634,12.));
#108176=CARTESIAN_POINT('Ctrl Pts',(48.8919551910299,50.1009206494209,0.));
#108177=CARTESIAN_POINT('Ctrl Pts',(48.8919551910299,50.1009206494209,12.));
#108178=CARTESIAN_POINT('Ctrl Pts',(48.8957735556681,50.1076907555303,0.));
#108179=CARTESIAN_POINT('Ctrl Pts',(48.8957735556681,50.1076907555303,12.));
#108180=CARTESIAN_POINT('Ctrl Pts',(48.9015035371772,50.1178632066821,0.));
#108181=CARTESIAN_POINT('Ctrl Pts',(48.9015035371772,50.1178632066821,12.));
#108182=CARTESIAN_POINT('Ctrl Pts',(48.9091483817797,50.1314610602286,0.));
#108183=CARTESIAN_POINT('Ctrl Pts',(48.9091483817797,50.1314610602286,12.));
#108184=CARTESIAN_POINT('Ctrl Pts',(48.9187125417897,50.148516018447,0.));
#108185=CARTESIAN_POINT('Ctrl Pts',(48.9187125417897,50.148516018447,12.));
#108186=CARTESIAN_POINT('Ctrl Pts',(48.9282847698237,50.1656286003943,0.));
#108187=CARTESIAN_POINT('Ctrl Pts',(48.9282847698237,50.1656286003943,12.));
#108188=CARTESIAN_POINT('Ctrl Pts',(48.9378649933116,50.1827987615659,0.));
#108189=CARTESIAN_POINT('Ctrl Pts',(48.9378649933116,50.1827987615659,12.));
#108190=CARTESIAN_POINT('Ctrl Pts',(48.9474530868847,50.2000264157903,0.));
#108191=CARTESIAN_POINT('Ctrl Pts',(48.9474530868847,50.2000264157903,12.));
#108192=CARTESIAN_POINT('Ctrl Pts',(48.9570488741273,50.2173114358423,0.));
#108193=CARTESIAN_POINT('Ctrl Pts',(48.9570488741273,50.2173114358423,12.));
#108194=CARTESIAN_POINT('Ctrl Pts',(48.9666521500969,50.2346536715465,0.));
#108195=CARTESIAN_POINT('Ctrl Pts',(48.9666521500969,50.2346536715465,12.));
#108196=CARTESIAN_POINT('Ctrl Pts',(48.9762626987227,50.252052963548,0.));
#108197=CARTESIAN_POINT('Ctrl Pts',(48.9762626987227,50.252052963548,12.));
#108198=CARTESIAN_POINT('Ctrl Pts',(48.9858803116649,50.2695091583473,0.));
#108199=CARTESIAN_POINT('Ctrl Pts',(48.9858803116649,50.2695091583473,12.));
#108200=CARTESIAN_POINT('Ctrl Pts',(48.9955048082028,50.2870221241003,0.));
#108201=CARTESIAN_POINT('Ctrl Pts',(48.9955048082028,50.2870221241003,12.));
#108202=CARTESIAN_POINT('Ctrl Pts',(49.0051360288002,50.3045917455383,0.));
#108203=CARTESIAN_POINT('Ctrl Pts',(49.0051360288002,50.3045917455383,12.));
#108204=CARTESIAN_POINT('Ctrl Pts',(49.0147738256925,50.3222179165102,0.));
#108205=CARTESIAN_POINT('Ctrl Pts',(49.0147738256925,50.3222179165102,12.));
#108206=CARTESIAN_POINT('Ctrl Pts',(49.0244180550759,50.3399005337967,0.));
#108207=CARTESIAN_POINT('Ctrl Pts',(49.0244180550759,50.3399005337967,12.));
#108208=CARTESIAN_POINT('Ctrl Pts',(49.034068567401,50.3576394894136,0.));
#108209=CARTESIAN_POINT('Ctrl Pts',(49.034068567401,50.3576394894136,12.));
#108210=CARTESIAN_POINT('Ctrl Pts',(49.0437252024868,50.3754346667389,0.));
#108211=CARTESIAN_POINT('Ctrl Pts',(49.0437252024868,50.3754346667389,12.));
#108212=CARTESIAN_POINT('Ctrl Pts',(49.0533877945771,50.393285944528,0.));
#108213=CARTESIAN_POINT('Ctrl Pts',(49.0533877945771,50.393285944528,12.));
#108214=CARTESIAN_POINT('Ctrl Pts',(49.0630561755082,50.4111931994264,0.));
#108215=CARTESIAN_POINT('Ctrl Pts',(49.0630561755082,50.4111931994264,12.));
#108216=CARTESIAN_POINT('Ctrl Pts',(49.0727301783477,50.4291563088528,0.));
#108217=CARTESIAN_POINT('Ctrl Pts',(49.0727301783477,50.4291563088528,12.));
#108218=CARTESIAN_POINT('Ctrl Pts',(49.0824096415339,50.4471751542717,0.));
#108219=CARTESIAN_POINT('Ctrl Pts',(49.0824096415339,50.4471751542717,12.));
#108220=CARTESIAN_POINT('Ctrl Pts',(49.0920944086973,50.465249621057,0.));
#108221=CARTESIAN_POINT('Ctrl Pts',(49.0920944086973,50.465249621057,12.));
#108222=CARTESIAN_POINT('Ctrl Pts',(49.1017843266782,50.4833795969296,0.));
#108223=CARTESIAN_POINT('Ctrl Pts',(49.1017843266782,50.4833795969296,12.));
#108224=CARTESIAN_POINT('Ctrl Pts',(49.1114792441573,50.5015649708742,0.));
#108225=CARTESIAN_POINT('Ctrl Pts',(49.1114792441573,50.5015649708742,12.));
#108226=CARTESIAN_POINT('Ctrl Pts',(49.1211790099817,50.5198056318111,0.));
#108227=CARTESIAN_POINT('Ctrl Pts',(49.1211790099817,50.5198056318111,12.));
#108228=CARTESIAN_POINT('Ctrl Pts',(49.1308834717645,50.5381014674822,0.));
#108229=CARTESIAN_POINT('Ctrl Pts',(49.1308834717645,50.5381014674822,12.));
#108230=CARTESIAN_POINT('Ctrl Pts',(49.1405924766169,50.5564523650406,0.));
#108231=CARTESIAN_POINT('Ctrl Pts',(49.1405924766169,50.5564523650406,12.));
#108232=CARTESIAN_POINT('Ctrl Pts',(49.1503058717831,50.5748582115575,0.));
#108233=CARTESIAN_POINT('Ctrl Pts',(49.1503058717831,50.5748582115575,12.));
#108234=CARTESIAN_POINT('Ctrl Pts',(49.1600235052613,50.593318894516,0.));
#108235=CARTESIAN_POINT('Ctrl Pts',(49.1600235052613,50.593318894516,12.));
#108236=CARTESIAN_POINT('Ctrl Pts',(49.1697452265473,50.6118343023937,0.));
#108237=CARTESIAN_POINT('Ctrl Pts',(49.1697452265473,50.6118343023937,12.));
#108238=CARTESIAN_POINT('Ctrl Pts',(49.1794708869074,50.6304043248796,0.));
#108239=CARTESIAN_POINT('Ctrl Pts',(49.1794708869074,50.6304043248796,12.));
#108240=CARTESIAN_POINT('Ctrl Pts',(49.1892003389743,50.6490288525639,0.));
#108241=CARTESIAN_POINT('Ctrl Pts',(49.1892003389743,50.6490288525639,12.));
#108242=CARTESIAN_POINT('Ctrl Pts',(49.1989334364991,50.6677077767427,0.));
#108243=CARTESIAN_POINT('Ctrl Pts',(49.1989334364991,50.6677077767427,12.));
#108244=CARTESIAN_POINT('Ctrl Pts',(49.2086700340625,50.6864409891905,0.));
#108245=CARTESIAN_POINT('Ctrl Pts',(49.2086700340625,50.6864409891905,12.));
#108246=CARTESIAN_POINT('Ctrl Pts',(49.218409986748,50.7052283818941,0.));
#108247=CARTESIAN_POINT('Ctrl Pts',(49.218409986748,50.7052283818941,12.));
#108248=CARTESIAN_POINT('Ctrl Pts',(49.2281531501569,50.7240698470698,0.));
#108249=CARTESIAN_POINT('Ctrl Pts',(49.2281531501569,50.7240698470698,12.));
#108250=CARTESIAN_POINT('Ctrl Pts',(49.2378993805482,50.7429652772816,0.));
#108251=CARTESIAN_POINT('Ctrl Pts',(49.2378993805482,50.7429652772816,12.));
#108252=CARTESIAN_POINT('Ctrl Pts',(49.2476485349373,50.7619145655207,0.));
#108253=CARTESIAN_POINT('Ctrl Pts',(49.2476485349373,50.7619145655207,12.));
#108254=CARTESIAN_POINT('Ctrl Pts',(49.2574004712122,50.7809176052954,0.));
#108255=CARTESIAN_POINT('Ctrl Pts',(49.2574004712122,50.7809176052954,12.));
#108256=CARTESIAN_POINT('Ctrl Pts',(49.2671550482415,50.7999742907111,0.));
#108257=CARTESIAN_POINT('Ctrl Pts',(49.2671550482415,50.7999742907111,12.));
#108258=CARTESIAN_POINT('Ctrl Pts',(49.2769121258144,50.8190845164319,0.));
#108259=CARTESIAN_POINT('Ctrl Pts',(49.2769121258144,50.8190845164319,12.));
#108260=CARTESIAN_POINT('Ctrl Pts',(49.2866715645828,50.8382481776392,0.));
#108261=CARTESIAN_POINT('Ctrl Pts',(49.2866715645828,50.8382481776392,12.));
#108262=CARTESIAN_POINT('Ctrl Pts',(49.2964332260043,50.8574651699877,0.));
#108263=CARTESIAN_POINT('Ctrl Pts',(49.2964332260043,50.8574651699877,12.));
#108264=CARTESIAN_POINT('Ctrl Pts',(49.3061969722798,50.8767353895509,0.));
#108265=CARTESIAN_POINT('Ctrl Pts',(49.3061969722798,50.8767353895509,12.));
#108266=CARTESIAN_POINT('Ctrl Pts',(49.3159626663129,50.8960587327869,0.));
#108267=CARTESIAN_POINT('Ctrl Pts',(49.3159626663129,50.8960587327869,12.));
#108268=CARTESIAN_POINT('Ctrl Pts',(49.325730171735,50.9154350965681,0.));
#108269=CARTESIAN_POINT('Ctrl Pts',(49.325730171735,50.9154350965681,12.));
#108270=CARTESIAN_POINT('Ctrl Pts',(49.3354993529163,50.9348643781928,0.));
#108271=CARTESIAN_POINT('Ctrl Pts',(49.3354993529163,50.9348643781928,12.));
#108272=CARTESIAN_POINT('Ctrl Pts',(49.3452700749804,50.9543464753974,0.));
#108273=CARTESIAN_POINT('Ctrl Pts',(49.3452700749804,50.9543464753974,12.));
#108274=CARTESIAN_POINT('Ctrl Pts',(49.3550422038221,50.9738812863636,0.));
#108275=CARTESIAN_POINT('Ctrl Pts',(49.3550422038221,50.9738812863636,12.));
#108276=CARTESIAN_POINT('Ctrl Pts',(49.3648156061049,50.9934687097179,0.));
#108277=CARTESIAN_POINT('Ctrl Pts',(49.3648156061049,50.9934687097179,12.));
#108278=CARTESIAN_POINT('Ctrl Pts',(49.3745901492428,51.0131086445268,0.));
#108279=CARTESIAN_POINT('Ctrl Pts',(49.3745901492428,51.0131086445268,12.));
#108280=CARTESIAN_POINT('Ctrl Pts',(49.3843657013851,51.0328009902857,0.));
#108281=CARTESIAN_POINT('Ctrl Pts',(49.3843657013851,51.0328009902857,12.));
#108282=CARTESIAN_POINT('Ctrl Pts',(49.3941421314014,51.0525456469072,0.));
#108283=CARTESIAN_POINT('Ctrl Pts',(49.3941421314014,51.0525456469072,12.));
#108284=CARTESIAN_POINT('Ctrl Pts',(49.4039193088635,51.0723425146987,0.));
#108285=CARTESIAN_POINT('Ctrl Pts',(49.4039193088635,51.0723425146987,12.));
#108286=CARTESIAN_POINT('Ctrl Pts',(49.4136971040428,51.0921914943663,0.));
#108287=CARTESIAN_POINT('Ctrl Pts',(49.4136971040428,51.0921914943663,12.));
#108288=CARTESIAN_POINT('Ctrl Pts',(49.4234753879071,51.1120924870196,0.));
#108289=CARTESIAN_POINT('Ctrl Pts',(49.4234753879071,51.1120924870196,12.));
#108290=CARTESIAN_POINT('Ctrl Pts',(49.4332540321178,51.1320453941702,0.));
#108291=CARTESIAN_POINT('Ctrl Pts',(49.4332540321178,51.1320453941702,12.));
#108292=CARTESIAN_POINT('Ctrl Pts',(49.4430329090288,51.1520501177291,0.));
#108293=CARTESIAN_POINT('Ctrl Pts',(49.4430329090288,51.1520501177291,12.));
#108294=CARTESIAN_POINT('Ctrl Pts',(49.4528118916833,51.1721065599972,0.));
#108295=CARTESIAN_POINT('Ctrl Pts',(49.4528118916833,51.1721065599972,12.));
#108296=CARTESIAN_POINT('Ctrl Pts',(49.4625908538076,51.1922146236686,0.));
#108297=CARTESIAN_POINT('Ctrl Pts',(49.4625908538076,51.1922146236686,12.));
#108298=CARTESIAN_POINT('Ctrl Pts',(49.4723696698022,51.2123742118288,0.));
#108299=CARTESIAN_POINT('Ctrl Pts',(49.4723696698022,51.2123742118288,12.));
#108300=CARTESIAN_POINT('Ctrl Pts',(49.4821482147357,51.2325852279507,0.));
#108301=CARTESIAN_POINT('Ctrl Pts',(49.4821482147357,51.2325852279507,12.));
#108302=CARTESIAN_POINT('Ctrl Pts',(49.4919263643357,51.2528475758841,0.));
#108303=CARTESIAN_POINT('Ctrl Pts',(49.4919263643357,51.2528475758841,12.));
#108304=CARTESIAN_POINT('Ctrl Pts',(49.5017039949841,51.2731611598465,0.));
#108305=CARTESIAN_POINT('Ctrl Pts',(49.5017039949841,51.2731611598465,12.));
#108306=CARTESIAN_POINT('Ctrl Pts',(49.5114809837111,51.2935258844278,0.));
#108307=CARTESIAN_POINT('Ctrl Pts',(49.5114809837111,51.2935258844278,12.));
#108308=CARTESIAN_POINT('Ctrl Pts',(49.5212572081901,51.3139416545903,0.));
#108309=CARTESIAN_POINT('Ctrl Pts',(49.5212572081901,51.3139416545903,12.));
#108310=CARTESIAN_POINT('Ctrl Pts',(49.5310325467334,51.3344083756659,0.));
#108311=CARTESIAN_POINT('Ctrl Pts',(49.5310325467334,51.3344083756659,12.));
#108312=CARTESIAN_POINT('Ctrl Pts',(49.5408068782871,51.354925953347,0.));
#108313=CARTESIAN_POINT('Ctrl Pts',(49.5408068782871,51.354925953347,12.));
#108314=CARTESIAN_POINT('Ctrl Pts',(49.5505800824268,51.3754942936796,0.));
#108315=CARTESIAN_POINT('Ctrl Pts',(49.5505800824268,51.3754942936796,12.));
#108316=CARTESIAN_POINT('Ctrl Pts',(49.5603520393514,51.3961133030688,0.));
#108317=CARTESIAN_POINT('Ctrl Pts',(49.5603520393514,51.3961133030688,12.));
#108318=CARTESIAN_POINT('Ctrl Pts',(49.5701226298779,51.4167828882765,0.));
#108319=CARTESIAN_POINT('Ctrl Pts',(49.5701226298779,51.4167828882765,12.));
#108320=CARTESIAN_POINT('Ctrl Pts',(49.579891735436,51.4375029564191,0.));
#108321=CARTESIAN_POINT('Ctrl Pts',(49.579891735436,51.4375029564191,12.));
#108322=CARTESIAN_POINT('Ctrl Pts',(49.5896592380634,51.4582734149562,0.));
#108323=CARTESIAN_POINT('Ctrl Pts',(49.5896592380634,51.4582734149562,12.));
#108324=CARTESIAN_POINT('Ctrl Pts',(49.5994250204003,51.4790941716859,0.));
#108325=CARTESIAN_POINT('Ctrl Pts',(49.5994250204003,51.4790941716859,12.));
#108326=CARTESIAN_POINT('Ctrl Pts',(49.609188965684,51.4999651347496,0.));
#108327=CARTESIAN_POINT('Ctrl Pts',(49.609188965684,51.4999651347496,12.));
#108328=CARTESIAN_POINT('Ctrl Pts',(49.6189509577441,51.5208862126303,0.));
#108329=CARTESIAN_POINT('Ctrl Pts',(49.6189509577441,51.5208862126303,12.));
#108330=CARTESIAN_POINT('Ctrl Pts',(49.6287108809975,51.5418573141494,0.));
#108331=CARTESIAN_POINT('Ctrl Pts',(49.6287108809975,51.5418573141494,12.));
#108332=CARTESIAN_POINT('Ctrl Pts',(49.6384686204443,51.5628783484556,0.));
#108333=CARTESIAN_POINT('Ctrl Pts',(49.6384686204443,51.5628783484556,12.));
#108334=CARTESIAN_POINT('Ctrl Pts',(49.6482240616627,51.5839492250218,0.));
#108335=CARTESIAN_POINT('Ctrl Pts',(49.6482240616627,51.5839492250218,12.));
#108336=CARTESIAN_POINT('Ctrl Pts',(49.6579770908063,51.6050698536525,0.));
#108337=CARTESIAN_POINT('Ctrl Pts',(49.6579770908063,51.6050698536525,12.));
#108338=CARTESIAN_POINT('Ctrl Pts',(49.6677275945975,51.6262401444799,0.));
#108339=CARTESIAN_POINT('Ctrl Pts',(49.6677275945975,51.6262401444799,12.));
#108340=CARTESIAN_POINT('Ctrl Pts',(49.6774754603235,51.6474600079611,0.));
#108341=CARTESIAN_POINT('Ctrl Pts',(49.6774754603235,51.6474600079611,12.));
#108342=CARTESIAN_POINT('Ctrl Pts',(49.6872205758314,51.6687293548656,0.));
#108343=CARTESIAN_POINT('Ctrl Pts',(49.6872205758314,51.6687293548656,12.));
#108344=CARTESIAN_POINT('Ctrl Pts',(49.6969628295236,51.6900480962744,0.));
#108345=CARTESIAN_POINT('Ctrl Pts',(49.6969628295236,51.6900480962744,12.));
#108346=CARTESIAN_POINT('Ctrl Pts',(49.7067021103534,51.7114161435848,0.));
#108347=CARTESIAN_POINT('Ctrl Pts',(49.7067021103534,51.7114161435848,12.));
#108348=CARTESIAN_POINT('Ctrl Pts',(49.7164383078206,51.7328334085084,0.));
#108349=CARTESIAN_POINT('Ctrl Pts',(49.7164383078206,51.7328334085084,12.));
#108350=CARTESIAN_POINT('Ctrl Pts',(49.7261713119672,51.754299803068,0.));
#108351=CARTESIAN_POINT('Ctrl Pts',(49.7261713119672,51.754299803068,12.));
#108352=CARTESIAN_POINT('Ctrl Pts',(49.7359010133741,51.7758152395857,0.));
#108353=CARTESIAN_POINT('Ctrl Pts',(49.7359010133741,51.7758152395857,12.));
#108354=CARTESIAN_POINT('Ctrl Pts',(49.7456273031555,51.7973796306826,0.));
#108355=CARTESIAN_POINT('Ctrl Pts',(49.7456273031555,51.7973796306826,12.));
#108356=CARTESIAN_POINT('Ctrl Pts',(49.7553500729563,51.8189928892841,0.));
#108357=CARTESIAN_POINT('Ctrl Pts',(49.7553500729563,51.8189928892841,12.));
#108358=CARTESIAN_POINT('Ctrl Pts',(49.7650692149464,51.8406549286177,0.));
#108359=CARTESIAN_POINT('Ctrl Pts',(49.7650692149464,51.8406549286177,12.));
#108360=CARTESIAN_POINT('Ctrl Pts',(49.7747846218177,51.8623656622092,0.));
#108361=CARTESIAN_POINT('Ctrl Pts',(49.7747846218177,51.8623656622092,12.));
#108362=CARTESIAN_POINT('Ctrl Pts',(49.78449618678,51.8841250038716,0.));
#108363=CARTESIAN_POINT('Ctrl Pts',(49.78449618678,51.8841250038716,12.));
#108364=CARTESIAN_POINT('Ctrl Pts',(49.7942038035568,51.9059328677051,0.));
#108365=CARTESIAN_POINT('Ctrl Pts',(49.7942038035568,51.9059328677051,12.));
#108366=CARTESIAN_POINT('Ctrl Pts',(49.8039073663808,51.9277891681014,0.));
#108367=CARTESIAN_POINT('Ctrl Pts',(49.8039073663808,51.9277891681014,12.));
#108368=CARTESIAN_POINT('Ctrl Pts',(49.8136067699896,51.9496938197418,0.));
#108369=CARTESIAN_POINT('Ctrl Pts',(49.8136067699896,51.9496938197418,12.));
#108370=CARTESIAN_POINT('Ctrl Pts',(49.8233019096224,51.9716467375938,0.));
#108371=CARTESIAN_POINT('Ctrl Pts',(49.8233019096224,51.9716467375938,12.));
#108372=CARTESIAN_POINT('Ctrl Pts',(49.8329926810172,51.9936478369008,0.));
#108373=CARTESIAN_POINT('Ctrl Pts',(49.8329926810172,51.9936478369008,12.));
#108374=CARTESIAN_POINT('Ctrl Pts',(49.8426789804068,52.015697033182,0.));
#108375=CARTESIAN_POINT('Ctrl Pts',(49.8426789804068,52.015697033182,12.));
#108376=CARTESIAN_POINT('Ctrl Pts',(49.8523607045146,52.0377942422373,0.));
#108377=CARTESIAN_POINT('Ctrl Pts',(49.8523607045146,52.0377942422373,12.));
#108378=CARTESIAN_POINT('Ctrl Pts',(49.8620377505498,52.059939380145,0.));
#108379=CARTESIAN_POINT('Ctrl Pts',(49.8620377505498,52.059939380145,12.));
#108380=CARTESIAN_POINT('Ctrl Pts',(49.871710016205,52.0821323632588,0.));
#108381=CARTESIAN_POINT('Ctrl Pts',(49.871710016205,52.0821323632588,12.));
#108382=CARTESIAN_POINT('Ctrl Pts',(49.8813773996523,52.1043731081968,0.));
#108383=CARTESIAN_POINT('Ctrl Pts',(49.8813773996523,52.1043731081968,12.));
#108384=CARTESIAN_POINT('Ctrl Pts',(49.8910397995404,52.1266615318414,0.));
#108385=CARTESIAN_POINT('Ctrl Pts',(49.8910397995404,52.1266615318414,12.));
#108386=CARTESIAN_POINT('Ctrl Pts',(49.90069711499,52.1489975513449,0.));
#108387=CARTESIAN_POINT('Ctrl Pts',(49.90069711499,52.1489975513449,12.));
#108388=CARTESIAN_POINT('Ctrl Pts',(49.9103492455904,52.1713810841277,0.));
#108389=CARTESIAN_POINT('Ctrl Pts',(49.9103492455904,52.1713810841277,12.));
#108390=CARTESIAN_POINT('Ctrl Pts',(49.919996091396,52.1938120478752,0.));
#108391=CARTESIAN_POINT('Ctrl Pts',(49.919996091396,52.1938120478752,12.));
#108392=CARTESIAN_POINT('Ctrl Pts',(49.9296375529241,52.2162903605272,0.));
#108393=CARTESIAN_POINT('Ctrl Pts',(49.9296375529241,52.2162903605272,12.));
#108394=CARTESIAN_POINT('Ctrl Pts',(49.9392735311507,52.238815940277,0.));
#108395=CARTESIAN_POINT('Ctrl Pts',(49.9392735311507,52.238815940277,12.));
#108396=CARTESIAN_POINT('Ctrl Pts',(49.9489039275064,52.2613887055773,0.));
#108397=CARTESIAN_POINT('Ctrl Pts',(49.9489039275064,52.2613887055773,12.));
#108398=CARTESIAN_POINT('Ctrl Pts',(49.9585286438734,52.2840085751385,0.));
#108399=CARTESIAN_POINT('Ctrl Pts',(49.9585286438734,52.2840085751385,12.));
#108400=CARTESIAN_POINT('Ctrl Pts',(49.9681475825824,52.3066754679265,0.));
#108401=CARTESIAN_POINT('Ctrl Pts',(49.9681475825824,52.3066754679265,12.));
#108402=CARTESIAN_POINT('Ctrl Pts',(49.9777606464103,52.3293893031524,0.));
#108403=CARTESIAN_POINT('Ctrl Pts',(49.9777606464103,52.3293893031524,12.));
#108404=CARTESIAN_POINT('Ctrl Pts',(49.9873677385769,52.3521500002711,0.));
#108405=CARTESIAN_POINT('Ctrl Pts',(49.9873677385769,52.3521500002711,12.));
#108406=CARTESIAN_POINT('Ctrl Pts',(49.9969687627402,52.3749574789865,0.));
#108407=CARTESIAN_POINT('Ctrl Pts',(49.9969687627402,52.3749574789865,12.));
#108408=CARTESIAN_POINT('Ctrl Pts',(50.0065636229934,52.3978116592505,0.));
#108409=CARTESIAN_POINT('Ctrl Pts',(50.0065636229934,52.3978116592505,12.));
#108410=CARTESIAN_POINT('Ctrl Pts',(50.0161522238619,52.420712461261,0.));
#108411=CARTESIAN_POINT('Ctrl Pts',(50.0161522238619,52.420712461261,12.));
#108412=CARTESIAN_POINT('Ctrl Pts',(50.0257344703008,52.4436598054523,0.));
#108413=CARTESIAN_POINT('Ctrl Pts',(50.0257344703008,52.4436598054523,12.));
#108414=CARTESIAN_POINT('Ctrl Pts',(50.0353102676933,52.4666536124926,0.));
#108415=CARTESIAN_POINT('Ctrl Pts',(50.0353102676933,52.4666536124926,12.));
#108416=CARTESIAN_POINT('Ctrl Pts',(50.0448795218453,52.4896938032896,0.));
#108417=CARTESIAN_POINT('Ctrl Pts',(50.0448795218453,52.4896938032896,12.));
#108418=CARTESIAN_POINT('Ctrl Pts',(50.0544421389824,52.5127802989903,0.));
#108419=CARTESIAN_POINT('Ctrl Pts',(50.0544421389824,52.5127802989903,12.));
#108420=CARTESIAN_POINT('Ctrl Pts',(50.0639980257477,52.5359130209789,0.));
#108421=CARTESIAN_POINT('Ctrl Pts',(50.0639980257477,52.5359130209789,12.));
#108422=CARTESIAN_POINT('Ctrl Pts',(50.0735470891996,52.5590918908691,0.));
#108423=CARTESIAN_POINT('Ctrl Pts',(50.0735470891996,52.5590918908691,12.));
#108424=CARTESIAN_POINT('Ctrl Pts',(50.0830892368095,52.5823168304981,0.));
#108425=CARTESIAN_POINT('Ctrl Pts',(50.0830892368095,52.5823168304981,12.));
#108426=CARTESIAN_POINT('Ctrl Pts',(50.0926243764569,52.6055877619338,0.));
#108427=CARTESIAN_POINT('Ctrl Pts',(50.0926243764569,52.6055877619338,12.));
#108428=CARTESIAN_POINT('Ctrl Pts',(50.1021524164261,52.6289046074743,0.));
#108429=CARTESIAN_POINT('Ctrl Pts',(50.1021524164261,52.6289046074743,12.));
#108430=CARTESIAN_POINT('Ctrl Pts',(50.1116732654041,52.6522672896462,0.));
#108431=CARTESIAN_POINT('Ctrl Pts',(50.1116732654041,52.6522672896462,12.));
#108432=CARTESIAN_POINT('Ctrl Pts',(50.1211868324781,52.6756757311979,0.));
#108433=CARTESIAN_POINT('Ctrl Pts',(50.1211868324781,52.6756757311979,12.));
#108434=CARTESIAN_POINT('Ctrl Pts',(50.1306930271343,52.6991298550928,0.));
#108435=CARTESIAN_POINT('Ctrl Pts',(50.1306930271343,52.6991298550928,12.));
#108436=CARTESIAN_POINT('Ctrl Pts',(50.1401917592532,52.7226295845156,0.));
#108437=CARTESIAN_POINT('Ctrl Pts',(50.1401917592532,52.7226295845156,12.));
#108438=CARTESIAN_POINT('Ctrl Pts',(50.1496829391068,52.7461748428733,0.));
#108439=CARTESIAN_POINT('Ctrl Pts',(50.1496829391068,52.7461748428733,12.));
#108440=CARTESIAN_POINT('Ctrl Pts',(50.1591664773561,52.769765553794,0.));
#108441=CARTESIAN_POINT('Ctrl Pts',(50.1591664773561,52.769765553794,12.));
#108442=CARTESIAN_POINT('Ctrl Pts',(50.1686422850493,52.793401641121,0.));
#108443=CARTESIAN_POINT('Ctrl Pts',(50.1686422850493,52.793401641121,12.));
#108444=CARTESIAN_POINT('Ctrl Pts',(50.1781102736215,52.8170830289052,0.));
#108445=CARTESIAN_POINT('Ctrl Pts',(50.1781102736215,52.8170830289052,12.));
#108446=CARTESIAN_POINT('Ctrl Pts',(50.1875703548893,52.8408096414101,0.));
#108447=CARTESIAN_POINT('Ctrl Pts',(50.1875703548893,52.8408096414101,12.));
#108448=CARTESIAN_POINT('Ctrl Pts',(50.1970224410476,52.8645814031137,0.));
#108449=CARTESIAN_POINT('Ctrl Pts',(50.1970224410476,52.8645814031137,12.));
#108450=CARTESIAN_POINT('Ctrl Pts',(50.2064664446663,52.8883982387068,0.));
#108451=CARTESIAN_POINT('Ctrl Pts',(50.2064664446663,52.8883982387068,12.));
#108452=CARTESIAN_POINT('Ctrl Pts',(50.2159022786876,52.9122600730882,0.));
#108453=CARTESIAN_POINT('Ctrl Pts',(50.2159022786876,52.9122600730882,12.));
#108454=CARTESIAN_POINT('Ctrl Pts',(50.2253298564237,52.9361668313539,0.));
#108455=CARTESIAN_POINT('Ctrl Pts',(50.2253298564237,52.9361668313539,12.));
#108456=CARTESIAN_POINT('Ctrl Pts',(50.2347490915553,52.9601184388027,0.));
#108457=CARTESIAN_POINT('Ctrl Pts',(50.2347490915553,52.9601184388027,12.));
#108458=CARTESIAN_POINT('Ctrl Pts',(50.2441598981286,52.9841148209404,0.));
#108459=CARTESIAN_POINT('Ctrl Pts',(50.2441598981286,52.9841148209404,12.));
#108460=CARTESIAN_POINT('Ctrl Pts',(50.2535621905553,53.0081559034802,0.));
#108461=CARTESIAN_POINT('Ctrl Pts',(50.2535621905553,53.0081559034802,12.));
#108462=CARTESIAN_POINT('Ctrl Pts',(50.262955883611,53.0322416123404,0.));
#108463=CARTESIAN_POINT('Ctrl Pts',(50.262955883611,53.0322416123404,12.));
#108464=CARTESIAN_POINT('Ctrl Pts',(50.272340892437,53.0563718736361,0.));
#108465=CARTESIAN_POINT('Ctrl Pts',(50.272340892437,53.0563718736361,12.));
#108466=CARTESIAN_POINT('Ctrl Pts',(50.2817171325354,53.0805466136791,0.));
#108467=CARTESIAN_POINT('Ctrl Pts',(50.2817171325354,53.0805466136791,12.));
#108468=CARTESIAN_POINT('Ctrl Pts',(50.2910845197615,53.1047657589806,0.));
#108469=CARTESIAN_POINT('Ctrl Pts',(50.2910845197615,53.1047657589806,12.));
#108470=CARTESIAN_POINT('Ctrl Pts',(50.3004429703188,53.1290292362482,0.));
#108471=CARTESIAN_POINT('Ctrl Pts',(50.3004429703188,53.1290292362482,12.));
#108472=CARTESIAN_POINT('Ctrl Pts',(50.3097924007535,53.153336972382,0.));
#108473=CARTESIAN_POINT('Ctrl Pts',(50.3097924007535,53.153336972382,12.));
#108474=CARTESIAN_POINT('Ctrl Pts',(50.3191327279497,53.1776888944622,0.));
#108475=CARTESIAN_POINT('Ctrl Pts',(50.3191327279497,53.1776888944622,12.));
#108476=CARTESIAN_POINT('Ctrl Pts',(50.3284638691285,53.202084929748,0.));
#108477=CARTESIAN_POINT('Ctrl Pts',(50.3284638691285,53.202084929748,12.));
#108478=CARTESIAN_POINT('Ctrl Pts',(50.3377857418522,53.2265250056896,0.));
#108479=CARTESIAN_POINT('Ctrl Pts',(50.3377857418522,53.2265250056896,12.));
#108480=CARTESIAN_POINT('Ctrl Pts',(50.3470982640293,53.2510090499341,0.));
#108481=CARTESIAN_POINT('Ctrl Pts',(50.3470982640293,53.2510090499341,12.));
#108482=CARTESIAN_POINT('Ctrl Pts',(50.3564013539198,53.2755369903291,0.));
#108483=CARTESIAN_POINT('Ctrl Pts',(50.3564013539198,53.2755369903291,12.));
#108484=CARTESIAN_POINT('Ctrl Pts',(50.3656949301423,53.3001087549222,0.));
#108485=CARTESIAN_POINT('Ctrl Pts',(50.3656949301423,53.3001087549222,12.));
#108486=CARTESIAN_POINT('Ctrl Pts',(50.3749789116777,53.3247242719575,0.));
#108487=CARTESIAN_POINT('Ctrl Pts',(50.3749789116777,53.3247242719575,12.));
#108488=CARTESIAN_POINT('Ctrl Pts',(50.384253217845,53.3493834698685,0.));
#108489=CARTESIAN_POINT('Ctrl Pts',(50.384253217845,53.3493834698685,12.));
#108490=CARTESIAN_POINT('Ctrl Pts',(50.393517768283,53.3740862772673,0.));
#108491=CARTESIAN_POINT('Ctrl Pts',(50.393517768283,53.3740862772673,12.));
#108492=CARTESIAN_POINT('Ctrl Pts',(50.4027724829296,53.3988326229308,0.));
#108493=CARTESIAN_POINT('Ctrl Pts',(50.4027724829296,53.3988326229308,12.));
#108494=CARTESIAN_POINT('Ctrl Pts',(50.4120172820054,53.4236224357846,0.));
#108495=CARTESIAN_POINT('Ctrl Pts',(50.4120172820054,53.4236224357846,12.));
#108496=CARTESIAN_POINT('Ctrl Pts',(50.4212520859924,53.4484556448787,0.));
#108497=CARTESIAN_POINT('Ctrl Pts',(50.4212520859924,53.4484556448787,12.));
#108498=CARTESIAN_POINT('Ctrl Pts',(50.4304768156677,53.4733321794199,0.));
#108499=CARTESIAN_POINT('Ctrl Pts',(50.4304768156677,53.4733321794199,12.));
#108500=CARTESIAN_POINT('Ctrl Pts',(50.4396913921389,53.4982519688032,0.));
#108501=CARTESIAN_POINT('Ctrl Pts',(50.4396913921389,53.4982519688032,12.));
#108502=CARTESIAN_POINT('Ctrl Pts',(50.4488957368841,53.5232149426415,0.));
#108503=CARTESIAN_POINT('Ctrl Pts',(50.4488957368841,53.5232149426415,12.));
#108504=CARTESIAN_POINT('Ctrl Pts',(50.4580897717835,53.5482210307864,0.));
#108505=CARTESIAN_POINT('Ctrl Pts',(50.4580897717835,53.5482210307864,12.));
#108506=CARTESIAN_POINT('Ctrl Pts',(50.4672734191749,53.5732701633603,0.));
#108507=CARTESIAN_POINT('Ctrl Pts',(50.4672734191749,53.5732701633603,12.));
#108508=CARTESIAN_POINT('Ctrl Pts',(50.4764466018064,53.5983622707231,0.));
#108509=CARTESIAN_POINT('Ctrl Pts',(50.4764466018064,53.5983622707231,12.));
#108510=CARTESIAN_POINT('Ctrl Pts',(50.4856092427309,53.6234972834055,0.));
#108511=CARTESIAN_POINT('Ctrl Pts',(50.4856092427309,53.6234972834055,12.));
#108512=CARTESIAN_POINT('Ctrl Pts',(50.4947612652147,53.6486751320434,0.));
#108513=CARTESIAN_POINT('Ctrl Pts',(50.4947612652147,53.6486751320434,12.));
#108514=CARTESIAN_POINT('Ctrl Pts',(50.5039025926531,53.6738957473158,0.));
#108515=CARTESIAN_POINT('Ctrl Pts',(50.5039025926531,53.6738957473158,12.));
#108516=CARTESIAN_POINT('Ctrl Pts',(50.5130331484563,53.6991590598551,0.));
#108517=CARTESIAN_POINT('Ctrl Pts',(50.5130331484563,53.6991590598551,12.));
#108518=CARTESIAN_POINT('Ctrl Pts',(50.5221528560427,53.7244650002382,0.));
#108519=CARTESIAN_POINT('Ctrl Pts',(50.5221528560427,53.7244650002382,12.));
#108520=CARTESIAN_POINT('Ctrl Pts',(50.5312616390789,53.7498134991714,0.));
#108521=CARTESIAN_POINT('Ctrl Pts',(50.5312616390789,53.7498134991714,12.));
#108522=CARTESIAN_POINT('Ctrl Pts',(50.5403594216706,53.7752044876313,0.));
#108523=CARTESIAN_POINT('Ctrl Pts',(50.5403594216706,53.7752044876313,12.));
#108524=CARTESIAN_POINT('Ctrl Pts',(50.5494461285762,53.8006378970198,0.));
#108525=CARTESIAN_POINT('Ctrl Pts',(50.5494461285762,53.8006378970198,12.));
#108526=CARTESIAN_POINT('Ctrl Pts',(50.5585216854082,53.8261136593064,0.));
#108527=CARTESIAN_POINT('Ctrl Pts',(50.5585216854082,53.8261136593064,12.));
#108528=CARTESIAN_POINT('Ctrl Pts',(50.567586018852,53.8516317071783,0.));
#108529=CARTESIAN_POINT('Ctrl Pts',(50.567586018852,53.8516317071783,12.));
#108530=CARTESIAN_POINT('Ctrl Pts',(50.5766390561861,53.8771919737007,0.));
#108531=CARTESIAN_POINT('Ctrl Pts',(50.5766390561861,53.8771919737007,12.));
#108532=CARTESIAN_POINT('Ctrl Pts',(50.5856807248133,53.9027943919814,0.));
#108533=CARTESIAN_POINT('Ctrl Pts',(50.5856807248133,53.9027943919814,12.));
#108534=CARTESIAN_POINT('Ctrl Pts',(50.5947109517476,53.9284388947996,0.));
#108535=CARTESIAN_POINT('Ctrl Pts',(50.5947109517476,53.9284388947996,12.));
#108536=CARTESIAN_POINT('Ctrl Pts',(50.603729663215,53.9541254143131,0.));
#108537=CARTESIAN_POINT('Ctrl Pts',(50.603729663215,53.9541254143131,12.));
#108538=CARTESIAN_POINT('Ctrl Pts',(50.6127367839738,53.9798538815561,0.));
#108539=CARTESIAN_POINT('Ctrl Pts',(50.6127367839738,53.9798538815561,12.));
#108540=CARTESIAN_POINT('Ctrl Pts',(50.6217322378686,54.0056242268443,0.));
#108541=CARTESIAN_POINT('Ctrl Pts',(50.6217322378686,54.0056242268443,12.));
#108542=CARTESIAN_POINT('Ctrl Pts',(50.630715949059,54.0314363806751,0.));
#108543=CARTESIAN_POINT('Ctrl Pts',(50.630715949059,54.0314363806751,12.));
#108544=CARTESIAN_POINT('Ctrl Pts',(50.6396878430961,54.0572902745101,0.));
#108545=CARTESIAN_POINT('Ctrl Pts',(50.6396878430961,54.0572902745101,12.));
#108546=CARTESIAN_POINT('Ctrl Pts',(50.6486478479459,54.0831858415182,0.));
#108547=CARTESIAN_POINT('Ctrl Pts',(50.6486478479459,54.0831858415182,12.));
#108548=CARTESIAN_POINT('Ctrl Pts',(50.657595895318,54.1091230175319,0.));
#108549=CARTESIAN_POINT('Ctrl Pts',(50.657595895318,54.1091230175319,12.));
#108550=CARTESIAN_POINT('Ctrl Pts',(50.6665319209798,54.1351017412722,0.));
#108551=CARTESIAN_POINT('Ctrl Pts',(50.6665319209798,54.1351017412722,12.));
#108552=CARTESIAN_POINT('Ctrl Pts',(50.6754558618218,54.1611219522299,0.));
#108553=CARTESIAN_POINT('Ctrl Pts',(50.6754558618218,54.1611219522299,12.));
#108554=CARTESIAN_POINT('Ctrl Pts',(50.6843676535428,54.1871835889908,0.));
#108555=CARTESIAN_POINT('Ctrl Pts',(50.6843676535428,54.1871835889908,12.));
#108556=CARTESIAN_POINT('Ctrl Pts',(50.6932672279758,54.2132865872968,0.));
#108557=CARTESIAN_POINT('Ctrl Pts',(50.6932672279758,54.2132865872968,12.));
#108558=CARTESIAN_POINT('Ctrl Pts',(50.7021545108369,54.2394308784093,0.));
#108559=CARTESIAN_POINT('Ctrl Pts',(50.7021545108369,54.2394308784093,12.));
#108560=CARTESIAN_POINT('Ctrl Pts',(50.7110294185832,54.2656163868258,0.));
#108561=CARTESIAN_POINT('Ctrl Pts',(50.7110294185832,54.2656163868258,12.));
#108562=CARTESIAN_POINT('Ctrl Pts',(50.7198918629632,54.2918430335414,0.));
#108563=CARTESIAN_POINT('Ctrl Pts',(50.7198918629632,54.2918430335414,12.));
#108564=CARTESIAN_POINT('Ctrl Pts',(50.7287417566296,54.3181107400862,0.));
#108565=CARTESIAN_POINT('Ctrl Pts',(50.7287417566296,54.3181107400862,12.));
#108566=CARTESIAN_POINT('Ctrl Pts',(50.7375790185988,54.344419432416,0.));
#108567=CARTESIAN_POINT('Ctrl Pts',(50.7375790185988,54.344419432416,12.));
#108568=CARTESIAN_POINT('Ctrl Pts',(50.7464035792846,54.3707690445679,0.));
#108569=CARTESIAN_POINT('Ctrl Pts',(50.7464035792846,54.3707690445679,12.));
#108570=CARTESIAN_POINT('Ctrl Pts',(50.7552153869224,54.3971595231285,0.));
#108571=CARTESIAN_POINT('Ctrl Pts',(50.7552153869224,54.3971595231285,12.));
#108572=CARTESIAN_POINT('Ctrl Pts',(50.7640144089601,54.4235908287188,0.));
#108573=CARTESIAN_POINT('Ctrl Pts',(50.7640144089601,54.4235908287188,12.));
#108574=CARTESIAN_POINT('Ctrl Pts',(50.772800626886,54.4500629335867,0.));
#108575=CARTESIAN_POINT('Ctrl Pts',(50.772800626886,54.4500629335867,12.));
#108576=CARTESIAN_POINT('Ctrl Pts',(50.7798193515479,54.4712732428597,0.));
#108577=CARTESIAN_POINT('Ctrl Pts',(50.7798193515479,54.4712732428597,12.));
#108578=CARTESIAN_POINT('Ctrl Pts',(50.7850776288567,54.4871993224549,0.));
#108579=CARTESIAN_POINT('Ctrl Pts',(50.7850776288567,54.4871993224549,12.));
#108580=CARTESIAN_POINT('Ctrl Pts',(50.7885805844191,54.4978248630284,0.));
#108581=CARTESIAN_POINT('Ctrl Pts',(50.7885805844191,54.4978248630284,12.));
#108582=CARTESIAN_POINT('Ctrl Pts',(50.7903314215393,54.5031396718592,0.));
#108583=CARTESIAN_POINT('Ctrl Pts',(50.7903314215393,54.5031396718592,12.));
#108584=CARTESIAN_POINT('',(48.8900464144686,50.0975384783634,0.));
#108585=CARTESIAN_POINT('Ctrl Pts',(48.8900464144686,50.0975384783634,0.));
#108586=CARTESIAN_POINT('Ctrl Pts',(48.8919551910299,50.1009206494209,0.));
#108587=CARTESIAN_POINT('Ctrl Pts',(48.8957735556681,50.1076907555303,0.));
#108588=CARTESIAN_POINT('Ctrl Pts',(48.9015035371772,50.1178632066821,0.));
#108589=CARTESIAN_POINT('Ctrl Pts',(48.9091483817797,50.1314610602286,0.));
#108590=CARTESIAN_POINT('Ctrl Pts',(48.9187125417897,50.148516018447,0.));
#108591=CARTESIAN_POINT('Ctrl Pts',(48.9282847698237,50.1656286003943,0.));
#108592=CARTESIAN_POINT('Ctrl Pts',(48.9378649933116,50.1827987615659,0.));
#108593=CARTESIAN_POINT('Ctrl Pts',(48.9474530868847,50.2000264157903,0.));
#108594=CARTESIAN_POINT('Ctrl Pts',(48.9570488741273,50.2173114358423,0.));
#108595=CARTESIAN_POINT('Ctrl Pts',(48.9666521500969,50.2346536715465,0.));
#108596=CARTESIAN_POINT('Ctrl Pts',(48.9762626987227,50.252052963548,0.));
#108597=CARTESIAN_POINT('Ctrl Pts',(48.9858803116649,50.2695091583473,0.));
#108598=CARTESIAN_POINT('Ctrl Pts',(48.9955048082028,50.2870221241003,0.));
#108599=CARTESIAN_POINT('Ctrl Pts',(49.0051360288002,50.3045917455383,0.));
#108600=CARTESIAN_POINT('Ctrl Pts',(49.0147738256925,50.3222179165102,0.));
#108601=CARTESIAN_POINT('Ctrl Pts',(49.0244180550759,50.3399005337967,0.));
#108602=CARTESIAN_POINT('Ctrl Pts',(49.034068567401,50.3576394894136,0.));
#108603=CARTESIAN_POINT('Ctrl Pts',(49.0437252024868,50.3754346667389,0.));
#108604=CARTESIAN_POINT('Ctrl Pts',(49.0533877945771,50.393285944528,0.));
#108605=CARTESIAN_POINT('Ctrl Pts',(49.0630561755082,50.4111931994264,0.));
#108606=CARTESIAN_POINT('Ctrl Pts',(49.0727301783477,50.4291563088528,0.));
#108607=CARTESIAN_POINT('Ctrl Pts',(49.0824096415339,50.4471751542717,0.));
#108608=CARTESIAN_POINT('Ctrl Pts',(49.0920944086973,50.465249621057,0.));
#108609=CARTESIAN_POINT('Ctrl Pts',(49.1017843266782,50.4833795969296,0.));
#108610=CARTESIAN_POINT('Ctrl Pts',(49.1114792441573,50.5015649708742,0.));
#108611=CARTESIAN_POINT('Ctrl Pts',(49.1211790099817,50.5198056318111,0.));
#108612=CARTESIAN_POINT('Ctrl Pts',(49.1308834717645,50.5381014674822,0.));
#108613=CARTESIAN_POINT('Ctrl Pts',(49.1405924766169,50.5564523650406,0.));
#108614=CARTESIAN_POINT('Ctrl Pts',(49.1503058717831,50.5748582115575,0.));
#108615=CARTESIAN_POINT('Ctrl Pts',(49.1600235052613,50.593318894516,0.));
#108616=CARTESIAN_POINT('Ctrl Pts',(49.1697452265473,50.6118343023937,0.));
#108617=CARTESIAN_POINT('Ctrl Pts',(49.1794708869074,50.6304043248796,0.));
#108618=CARTESIAN_POINT('Ctrl Pts',(49.1892003389743,50.6490288525639,0.));
#108619=CARTESIAN_POINT('Ctrl Pts',(49.1989334364991,50.6677077767427,0.));
#108620=CARTESIAN_POINT('Ctrl Pts',(49.2086700340625,50.6864409891905,0.));
#108621=CARTESIAN_POINT('Ctrl Pts',(49.218409986748,50.7052283818941,0.));
#108622=CARTESIAN_POINT('Ctrl Pts',(49.2281531501569,50.7240698470698,0.));
#108623=CARTESIAN_POINT('Ctrl Pts',(49.2378993805482,50.7429652772816,0.));
#108624=CARTESIAN_POINT('Ctrl Pts',(49.2476485349373,50.7619145655207,0.));
#108625=CARTESIAN_POINT('Ctrl Pts',(49.2574004712122,50.7809176052954,0.));
#108626=CARTESIAN_POINT('Ctrl Pts',(49.2671550482415,50.7999742907111,0.));
#108627=CARTESIAN_POINT('Ctrl Pts',(49.2769121258144,50.8190845164319,0.));
#108628=CARTESIAN_POINT('Ctrl Pts',(49.2866715645828,50.8382481776392,0.));
#108629=CARTESIAN_POINT('Ctrl Pts',(49.2964332260043,50.8574651699877,0.));
#108630=CARTESIAN_POINT('Ctrl Pts',(49.3061969722798,50.8767353895509,0.));
#108631=CARTESIAN_POINT('Ctrl Pts',(49.3159626663129,50.8960587327869,0.));
#108632=CARTESIAN_POINT('Ctrl Pts',(49.325730171735,50.9154350965681,0.));
#108633=CARTESIAN_POINT('Ctrl Pts',(49.3354993529163,50.9348643781928,0.));
#108634=CARTESIAN_POINT('Ctrl Pts',(49.3452700749804,50.9543464753974,0.));
#108635=CARTESIAN_POINT('Ctrl Pts',(49.3550422038221,50.9738812863636,0.));
#108636=CARTESIAN_POINT('Ctrl Pts',(49.3648156061049,50.9934687097179,0.));
#108637=CARTESIAN_POINT('Ctrl Pts',(49.3745901492428,51.0131086445268,0.));
#108638=CARTESIAN_POINT('Ctrl Pts',(49.3843657013851,51.0328009902857,0.));
#108639=CARTESIAN_POINT('Ctrl Pts',(49.3941421314014,51.0525456469072,0.));
#108640=CARTESIAN_POINT('Ctrl Pts',(49.4039193088635,51.0723425146987,0.));
#108641=CARTESIAN_POINT('Ctrl Pts',(49.4136971040428,51.0921914943663,0.));
#108642=CARTESIAN_POINT('Ctrl Pts',(49.4234753879071,51.1120924870196,0.));
#108643=CARTESIAN_POINT('Ctrl Pts',(49.4332540321178,51.1320453941702,0.));
#108644=CARTESIAN_POINT('Ctrl Pts',(49.4430329090288,51.1520501177291,0.));
#108645=CARTESIAN_POINT('Ctrl Pts',(49.4528118916833,51.1721065599972,0.));
#108646=CARTESIAN_POINT('Ctrl Pts',(49.4625908538076,51.1922146236686,0.));
#108647=CARTESIAN_POINT('Ctrl Pts',(49.4723696698022,51.2123742118288,0.));
#108648=CARTESIAN_POINT('Ctrl Pts',(49.4821482147357,51.2325852279507,0.));
#108649=CARTESIAN_POINT('Ctrl Pts',(49.4919263643357,51.2528475758841,0.));
#108650=CARTESIAN_POINT('Ctrl Pts',(49.5017039949841,51.2731611598465,0.));
#108651=CARTESIAN_POINT('Ctrl Pts',(49.5114809837111,51.2935258844278,0.));
#108652=CARTESIAN_POINT('Ctrl Pts',(49.5212572081901,51.3139416545903,0.));
#108653=CARTESIAN_POINT('Ctrl Pts',(49.5310325467334,51.3344083756659,0.));
#108654=CARTESIAN_POINT('Ctrl Pts',(49.5408068782871,51.354925953347,0.));
#108655=CARTESIAN_POINT('Ctrl Pts',(49.5505800824268,51.3754942936796,0.));
#108656=CARTESIAN_POINT('Ctrl Pts',(49.5603520393514,51.3961133030688,0.));
#108657=CARTESIAN_POINT('Ctrl Pts',(49.5701226298779,51.4167828882765,0.));
#108658=CARTESIAN_POINT('Ctrl Pts',(49.579891735436,51.4375029564191,0.));
#108659=CARTESIAN_POINT('Ctrl Pts',(49.5896592380634,51.4582734149562,0.));
#108660=CARTESIAN_POINT('Ctrl Pts',(49.5994250204003,51.4790941716859,0.));
#108661=CARTESIAN_POINT('Ctrl Pts',(49.609188965684,51.4999651347496,0.));
#108662=CARTESIAN_POINT('Ctrl Pts',(49.6189509577441,51.5208862126303,0.));
#108663=CARTESIAN_POINT('Ctrl Pts',(49.6287108809975,51.5418573141494,0.));
#108664=CARTESIAN_POINT('Ctrl Pts',(49.6384686204443,51.5628783484556,0.));
#108665=CARTESIAN_POINT('Ctrl Pts',(49.6482240616627,51.5839492250218,0.));
#108666=CARTESIAN_POINT('Ctrl Pts',(49.6579770908063,51.6050698536525,0.));
#108667=CARTESIAN_POINT('Ctrl Pts',(49.6677275945975,51.6262401444799,0.));
#108668=CARTESIAN_POINT('Ctrl Pts',(49.6774754603235,51.6474600079611,0.));
#108669=CARTESIAN_POINT('Ctrl Pts',(49.6872205758314,51.6687293548656,0.));
#108670=CARTESIAN_POINT('Ctrl Pts',(49.6969628295236,51.6900480962744,0.));
#108671=CARTESIAN_POINT('Ctrl Pts',(49.7067021103534,51.7114161435848,0.));
#108672=CARTESIAN_POINT('Ctrl Pts',(49.7164383078206,51.7328334085084,0.));
#108673=CARTESIAN_POINT('Ctrl Pts',(49.7261713119672,51.754299803068,0.));
#108674=CARTESIAN_POINT('Ctrl Pts',(49.7359010133741,51.7758152395857,0.));
#108675=CARTESIAN_POINT('Ctrl Pts',(49.7456273031555,51.7973796306826,0.));
#108676=CARTESIAN_POINT('Ctrl Pts',(49.7553500729563,51.8189928892841,0.));
#108677=CARTESIAN_POINT('Ctrl Pts',(49.7650692149464,51.8406549286177,0.));
#108678=CARTESIAN_POINT('Ctrl Pts',(49.7747846218177,51.8623656622092,0.));
#108679=CARTESIAN_POINT('Ctrl Pts',(49.78449618678,51.8841250038716,0.));
#108680=CARTESIAN_POINT('Ctrl Pts',(49.7942038035568,51.9059328677051,0.));
#108681=CARTESIAN_POINT('Ctrl Pts',(49.8039073663808,51.9277891681014,0.));
#108682=CARTESIAN_POINT('Ctrl Pts',(49.8136067699896,51.9496938197418,0.));
#108683=CARTESIAN_POINT('Ctrl Pts',(49.8233019096224,51.9716467375938,0.));
#108684=CARTESIAN_POINT('Ctrl Pts',(49.8329926810172,51.9936478369008,0.));
#108685=CARTESIAN_POINT('Ctrl Pts',(49.8426789804068,52.015697033182,0.));
#108686=CARTESIAN_POINT('Ctrl Pts',(49.8523607045146,52.0377942422373,0.));
#108687=CARTESIAN_POINT('Ctrl Pts',(49.8620377505498,52.059939380145,0.));
#108688=CARTESIAN_POINT('Ctrl Pts',(49.871710016205,52.0821323632588,0.));
#108689=CARTESIAN_POINT('Ctrl Pts',(49.8813773996523,52.1043731081968,0.));
#108690=CARTESIAN_POINT('Ctrl Pts',(49.8910397995404,52.1266615318414,0.));
#108691=CARTESIAN_POINT('Ctrl Pts',(49.90069711499,52.1489975513449,0.));
#108692=CARTESIAN_POINT('Ctrl Pts',(49.9103492455904,52.1713810841277,0.));
#108693=CARTESIAN_POINT('Ctrl Pts',(49.919996091396,52.1938120478752,0.));
#108694=CARTESIAN_POINT('Ctrl Pts',(49.9296375529241,52.2162903605272,0.));
#108695=CARTESIAN_POINT('Ctrl Pts',(49.9392735311507,52.238815940277,0.));
#108696=CARTESIAN_POINT('Ctrl Pts',(49.9489039275064,52.2613887055773,0.));
#108697=CARTESIAN_POINT('Ctrl Pts',(49.9585286438734,52.2840085751385,0.));
#108698=CARTESIAN_POINT('Ctrl Pts',(49.9681475825824,52.3066754679265,0.));
#108699=CARTESIAN_POINT('Ctrl Pts',(49.9777606464103,52.3293893031524,0.));
#108700=CARTESIAN_POINT('Ctrl Pts',(49.9873677385769,52.3521500002711,0.));
#108701=CARTESIAN_POINT('Ctrl Pts',(49.9969687627402,52.3749574789865,0.));
#108702=CARTESIAN_POINT('Ctrl Pts',(50.0065636229934,52.3978116592505,0.));
#108703=CARTESIAN_POINT('Ctrl Pts',(50.0161522238619,52.420712461261,0.));
#108704=CARTESIAN_POINT('Ctrl Pts',(50.0257344703008,52.4436598054523,0.));
#108705=CARTESIAN_POINT('Ctrl Pts',(50.0353102676933,52.4666536124926,0.));
#108706=CARTESIAN_POINT('Ctrl Pts',(50.0448795218453,52.4896938032896,0.));
#108707=CARTESIAN_POINT('Ctrl Pts',(50.0544421389824,52.5127802989903,0.));
#108708=CARTESIAN_POINT('Ctrl Pts',(50.0639980257477,52.5359130209789,0.));
#108709=CARTESIAN_POINT('Ctrl Pts',(50.0735470891996,52.5590918908691,0.));
#108710=CARTESIAN_POINT('Ctrl Pts',(50.0830892368095,52.5823168304981,0.));
#108711=CARTESIAN_POINT('Ctrl Pts',(50.0926243764569,52.6055877619338,0.));
#108712=CARTESIAN_POINT('Ctrl Pts',(50.1021524164261,52.6289046074743,0.));
#108713=CARTESIAN_POINT('Ctrl Pts',(50.1116732654041,52.6522672896462,0.));
#108714=CARTESIAN_POINT('Ctrl Pts',(50.1211868324781,52.6756757311979,0.));
#108715=CARTESIAN_POINT('Ctrl Pts',(50.1306930271343,52.6991298550928,0.));
#108716=CARTESIAN_POINT('Ctrl Pts',(50.1401917592532,52.7226295845156,0.));
#108717=CARTESIAN_POINT('Ctrl Pts',(50.1496829391068,52.7461748428733,0.));
#108718=CARTESIAN_POINT('Ctrl Pts',(50.1591664773561,52.769765553794,0.));
#108719=CARTESIAN_POINT('Ctrl Pts',(50.1686422850493,52.793401641121,0.));
#108720=CARTESIAN_POINT('Ctrl Pts',(50.1781102736215,52.8170830289052,0.));
#108721=CARTESIAN_POINT('Ctrl Pts',(50.1875703548893,52.8408096414101,0.));
#108722=CARTESIAN_POINT('Ctrl Pts',(50.1970224410476,52.8645814031137,0.));
#108723=CARTESIAN_POINT('Ctrl Pts',(50.2064664446663,52.8883982387068,0.));
#108724=CARTESIAN_POINT('Ctrl Pts',(50.2159022786876,52.9122600730882,0.));
#108725=CARTESIAN_POINT('Ctrl Pts',(50.2253298564237,52.9361668313539,0.));
#108726=CARTESIAN_POINT('Ctrl Pts',(50.2347490915553,52.9601184388027,0.));
#108727=CARTESIAN_POINT('Ctrl Pts',(50.2441598981286,52.9841148209404,0.));
#108728=CARTESIAN_POINT('Ctrl Pts',(50.2535621905553,53.0081559034802,0.));
#108729=CARTESIAN_POINT('Ctrl Pts',(50.262955883611,53.0322416123404,0.));
#108730=CARTESIAN_POINT('Ctrl Pts',(50.272340892437,53.0563718736361,0.));
#108731=CARTESIAN_POINT('Ctrl Pts',(50.2817171325354,53.0805466136791,0.));
#108732=CARTESIAN_POINT('Ctrl Pts',(50.2910845197615,53.1047657589806,0.));
#108733=CARTESIAN_POINT('Ctrl Pts',(50.3004429703188,53.1290292362482,0.));
#108734=CARTESIAN_POINT('Ctrl Pts',(50.3097924007535,53.153336972382,0.));
#108735=CARTESIAN_POINT('Ctrl Pts',(50.3191327279497,53.1776888944622,0.));
#108736=CARTESIAN_POINT('Ctrl Pts',(50.3284638691285,53.202084929748,0.));
#108737=CARTESIAN_POINT('Ctrl Pts',(50.3377857418522,53.2265250056896,0.));
#108738=CARTESIAN_POINT('Ctrl Pts',(50.3470982640293,53.2510090499341,0.));
#108739=CARTESIAN_POINT('Ctrl Pts',(50.3564013539198,53.2755369903291,0.));
#108740=CARTESIAN_POINT('Ctrl Pts',(50.3656949301423,53.3001087549222,0.));
#108741=CARTESIAN_POINT('Ctrl Pts',(50.3749789116777,53.3247242719575,0.));
#108742=CARTESIAN_POINT('Ctrl Pts',(50.384253217845,53.3493834698685,0.));
#108743=CARTESIAN_POINT('Ctrl Pts',(50.393517768283,53.3740862772673,0.));
#108744=CARTESIAN_POINT('Ctrl Pts',(50.4027724829296,53.3988326229308,0.));
#108745=CARTESIAN_POINT('Ctrl Pts',(50.4120172820054,53.4236224357846,0.));
#108746=CARTESIAN_POINT('Ctrl Pts',(50.4212520859924,53.4484556448787,0.));
#108747=CARTESIAN_POINT('Ctrl Pts',(50.4304768156677,53.4733321794199,0.));
#108748=CARTESIAN_POINT('Ctrl Pts',(50.4396913921389,53.4982519688032,0.));
#108749=CARTESIAN_POINT('Ctrl Pts',(50.4488957368841,53.5232149426415,0.));
#108750=CARTESIAN_POINT('Ctrl Pts',(50.4580897717835,53.5482210307864,0.));
#108751=CARTESIAN_POINT('Ctrl Pts',(50.4672734191749,53.5732701633603,0.));
#108752=CARTESIAN_POINT('Ctrl Pts',(50.4764466018064,53.5983622707231,0.));
#108753=CARTESIAN_POINT('Ctrl Pts',(50.4856092427309,53.6234972834055,0.));
#108754=CARTESIAN_POINT('Ctrl Pts',(50.4947612652147,53.6486751320434,0.));
#108755=CARTESIAN_POINT('Ctrl Pts',(50.5039025926531,53.6738957473158,0.));
#108756=CARTESIAN_POINT('Ctrl Pts',(50.5130331484563,53.6991590598551,0.));
#108757=CARTESIAN_POINT('Ctrl Pts',(50.5221528560427,53.7244650002382,0.));
#108758=CARTESIAN_POINT('Ctrl Pts',(50.5312616390789,53.7498134991714,0.));
#108759=CARTESIAN_POINT('Ctrl Pts',(50.5403594216706,53.7752044876313,0.));
#108760=CARTESIAN_POINT('Ctrl Pts',(50.5494461285762,53.8006378970198,0.));
#108761=CARTESIAN_POINT('Ctrl Pts',(50.5585216854082,53.8261136593064,0.));
#108762=CARTESIAN_POINT('Ctrl Pts',(50.567586018852,53.8516317071783,0.));
#108763=CARTESIAN_POINT('Ctrl Pts',(50.5766390561861,53.8771919737007,0.));
#108764=CARTESIAN_POINT('Ctrl Pts',(50.5856807248133,53.9027943919814,0.));
#108765=CARTESIAN_POINT('Ctrl Pts',(50.5947109517476,53.9284388947996,0.));
#108766=CARTESIAN_POINT('Ctrl Pts',(50.603729663215,53.9541254143131,0.));
#108767=CARTESIAN_POINT('Ctrl Pts',(50.6127367839738,53.9798538815561,0.));
#108768=CARTESIAN_POINT('Ctrl Pts',(50.6217322378686,54.0056242268443,0.));
#108769=CARTESIAN_POINT('Ctrl Pts',(50.630715949059,54.0314363806751,0.));
#108770=CARTESIAN_POINT('Ctrl Pts',(50.6396878430961,54.0572902745101,0.));
#108771=CARTESIAN_POINT('Ctrl Pts',(50.6486478479459,54.0831858415182,0.));
#108772=CARTESIAN_POINT('Ctrl Pts',(50.657595895318,54.1091230175319,0.));
#108773=CARTESIAN_POINT('Ctrl Pts',(50.6665319209798,54.1351017412722,0.));
#108774=CARTESIAN_POINT('Ctrl Pts',(50.6741814675382,54.1574061041882,0.));
#108775=CARTESIAN_POINT('Ctrl Pts',(50.6800396668659,54.1745287898577,0.));
#108776=CARTESIAN_POINT('Ctrl Pts',(50.6841118861803,54.1864514381924,0.));
#108777=CARTESIAN_POINT('Ctrl Pts',(50.6864016965603,54.1931619277295,0.));
#108778=CARTESIAN_POINT('Ctrl Pts',(50.6869108458688,54.1946543499978,0.));
#108779=CARTESIAN_POINT('',(48.8900464144686,50.0975384783634,12.));
#108780=CARTESIAN_POINT('',(48.8900464144686,50.0975384783634,0.));
#108781=CARTESIAN_POINT('Ctrl Pts',(50.6869108458688,54.1946543499978,12.));
#108782=CARTESIAN_POINT('Ctrl Pts',(50.6864016965603,54.1931619277295,12.));
#108783=CARTESIAN_POINT('Ctrl Pts',(50.6841118861803,54.1864514381924,12.));
#108784=CARTESIAN_POINT('Ctrl Pts',(50.6800396668659,54.1745287898577,12.));
#108785=CARTESIAN_POINT('Ctrl Pts',(50.6741814675382,54.1574061041882,12.));
#108786=CARTESIAN_POINT('Ctrl Pts',(50.6665319209798,54.1351017412722,12.));
#108787=CARTESIAN_POINT('Ctrl Pts',(50.657595895318,54.1091230175319,12.));
#108788=CARTESIAN_POINT('Ctrl Pts',(50.6486478479459,54.0831858415182,12.));
#108789=CARTESIAN_POINT('Ctrl Pts',(50.6396878430961,54.0572902745101,12.));
#108790=CARTESIAN_POINT('Ctrl Pts',(50.630715949059,54.0314363806751,12.));
#108791=CARTESIAN_POINT('Ctrl Pts',(50.6217322378686,54.0056242268443,12.));
#108792=CARTESIAN_POINT('Ctrl Pts',(50.6127367839738,53.9798538815561,12.));
#108793=CARTESIAN_POINT('Ctrl Pts',(50.603729663215,53.9541254143131,12.));
#108794=CARTESIAN_POINT('Ctrl Pts',(50.5947109517476,53.9284388947996,12.));
#108795=CARTESIAN_POINT('Ctrl Pts',(50.5856807248133,53.9027943919814,12.));
#108796=CARTESIAN_POINT('Ctrl Pts',(50.5766390561861,53.8771919737007,12.));
#108797=CARTESIAN_POINT('Ctrl Pts',(50.567586018852,53.8516317071783,12.));
#108798=CARTESIAN_POINT('Ctrl Pts',(50.5585216854082,53.8261136593064,12.));
#108799=CARTESIAN_POINT('Ctrl Pts',(50.5494461285762,53.8006378970198,12.));
#108800=CARTESIAN_POINT('Ctrl Pts',(50.5403594216706,53.7752044876313,12.));
#108801=CARTESIAN_POINT('Ctrl Pts',(50.5312616390789,53.7498134991714,12.));
#108802=CARTESIAN_POINT('Ctrl Pts',(50.5221528560427,53.7244650002382,12.));
#108803=CARTESIAN_POINT('Ctrl Pts',(50.5130331484563,53.6991590598551,12.));
#108804=CARTESIAN_POINT('Ctrl Pts',(50.5039025926531,53.6738957473158,12.));
#108805=CARTESIAN_POINT('Ctrl Pts',(50.4947612652147,53.6486751320434,12.));
#108806=CARTESIAN_POINT('Ctrl Pts',(50.4856092427309,53.6234972834055,12.));
#108807=CARTESIAN_POINT('Ctrl Pts',(50.4764466018064,53.5983622707231,12.));
#108808=CARTESIAN_POINT('Ctrl Pts',(50.4672734191749,53.5732701633603,12.));
#108809=CARTESIAN_POINT('Ctrl Pts',(50.4580897717835,53.5482210307864,12.));
#108810=CARTESIAN_POINT('Ctrl Pts',(50.4488957368841,53.5232149426415,12.));
#108811=CARTESIAN_POINT('Ctrl Pts',(50.4396913921389,53.4982519688032,12.));
#108812=CARTESIAN_POINT('Ctrl Pts',(50.4304768156677,53.4733321794199,12.));
#108813=CARTESIAN_POINT('Ctrl Pts',(50.4212520859924,53.4484556448787,12.));
#108814=CARTESIAN_POINT('Ctrl Pts',(50.4120172820054,53.4236224357846,12.));
#108815=CARTESIAN_POINT('Ctrl Pts',(50.4027724829296,53.3988326229308,12.));
#108816=CARTESIAN_POINT('Ctrl Pts',(50.393517768283,53.3740862772673,12.));
#108817=CARTESIAN_POINT('Ctrl Pts',(50.384253217845,53.3493834698685,12.));
#108818=CARTESIAN_POINT('Ctrl Pts',(50.3749789116777,53.3247242719575,12.));
#108819=CARTESIAN_POINT('Ctrl Pts',(50.3656949301423,53.3001087549222,12.));
#108820=CARTESIAN_POINT('Ctrl Pts',(50.3564013539198,53.2755369903291,12.));
#108821=CARTESIAN_POINT('Ctrl Pts',(50.3470982640293,53.2510090499341,12.));
#108822=CARTESIAN_POINT('Ctrl Pts',(50.3377857418522,53.2265250056896,12.));
#108823=CARTESIAN_POINT('Ctrl Pts',(50.3284638691285,53.202084929748,12.));
#108824=CARTESIAN_POINT('Ctrl Pts',(50.3191327279497,53.1776888944622,12.));
#108825=CARTESIAN_POINT('Ctrl Pts',(50.3097924007535,53.153336972382,12.));
#108826=CARTESIAN_POINT('Ctrl Pts',(50.3004429703188,53.1290292362482,12.));
#108827=CARTESIAN_POINT('Ctrl Pts',(50.2910845197615,53.1047657589806,12.));
#108828=CARTESIAN_POINT('Ctrl Pts',(50.2817171325354,53.0805466136791,12.));
#108829=CARTESIAN_POINT('Ctrl Pts',(50.272340892437,53.0563718736361,12.));
#108830=CARTESIAN_POINT('Ctrl Pts',(50.262955883611,53.0322416123404,12.));
#108831=CARTESIAN_POINT('Ctrl Pts',(50.2535621905553,53.0081559034802,12.));
#108832=CARTESIAN_POINT('Ctrl Pts',(50.2441598981286,52.9841148209404,12.));
#108833=CARTESIAN_POINT('Ctrl Pts',(50.2347490915553,52.9601184388027,12.));
#108834=CARTESIAN_POINT('Ctrl Pts',(50.2253298564237,52.9361668313539,12.));
#108835=CARTESIAN_POINT('Ctrl Pts',(50.2159022786876,52.9122600730882,12.));
#108836=CARTESIAN_POINT('Ctrl Pts',(50.2064664446663,52.8883982387068,12.));
#108837=CARTESIAN_POINT('Ctrl Pts',(50.1970224410476,52.8645814031137,12.));
#108838=CARTESIAN_POINT('Ctrl Pts',(50.1875703548893,52.8408096414101,12.));
#108839=CARTESIAN_POINT('Ctrl Pts',(50.1781102736215,52.8170830289052,12.));
#108840=CARTESIAN_POINT('Ctrl Pts',(50.1686422850493,52.793401641121,12.));
#108841=CARTESIAN_POINT('Ctrl Pts',(50.1591664773561,52.769765553794,12.));
#108842=CARTESIAN_POINT('Ctrl Pts',(50.1496829391068,52.7461748428733,12.));
#108843=CARTESIAN_POINT('Ctrl Pts',(50.1401917592532,52.7226295845156,12.));
#108844=CARTESIAN_POINT('Ctrl Pts',(50.1306930271343,52.6991298550928,12.));
#108845=CARTESIAN_POINT('Ctrl Pts',(50.1211868324781,52.6756757311979,12.));
#108846=CARTESIAN_POINT('Ctrl Pts',(50.1116732654041,52.6522672896462,12.));
#108847=CARTESIAN_POINT('Ctrl Pts',(50.1021524164261,52.6289046074743,12.));
#108848=CARTESIAN_POINT('Ctrl Pts',(50.0926243764569,52.6055877619338,12.));
#108849=CARTESIAN_POINT('Ctrl Pts',(50.0830892368095,52.5823168304981,12.));
#108850=CARTESIAN_POINT('Ctrl Pts',(50.0735470891996,52.5590918908691,12.));
#108851=CARTESIAN_POINT('Ctrl Pts',(50.0639980257477,52.5359130209789,12.));
#108852=CARTESIAN_POINT('Ctrl Pts',(50.0544421389824,52.5127802989903,12.));
#108853=CARTESIAN_POINT('Ctrl Pts',(50.0448795218453,52.4896938032896,12.));
#108854=CARTESIAN_POINT('Ctrl Pts',(50.0353102676933,52.4666536124926,12.));
#108855=CARTESIAN_POINT('Ctrl Pts',(50.0257344703008,52.4436598054523,12.));
#108856=CARTESIAN_POINT('Ctrl Pts',(50.0161522238619,52.420712461261,12.));
#108857=CARTESIAN_POINT('Ctrl Pts',(50.0065636229934,52.3978116592505,12.));
#108858=CARTESIAN_POINT('Ctrl Pts',(49.9969687627402,52.3749574789865,12.));
#108859=CARTESIAN_POINT('Ctrl Pts',(49.9873677385769,52.3521500002711,12.));
#108860=CARTESIAN_POINT('Ctrl Pts',(49.9777606464103,52.3293893031524,12.));
#108861=CARTESIAN_POINT('Ctrl Pts',(49.9681475825824,52.3066754679265,12.));
#108862=CARTESIAN_POINT('Ctrl Pts',(49.9585286438734,52.2840085751385,12.));
#108863=CARTESIAN_POINT('Ctrl Pts',(49.9489039275064,52.2613887055773,12.));
#108864=CARTESIAN_POINT('Ctrl Pts',(49.9392735311507,52.238815940277,12.));
#108865=CARTESIAN_POINT('Ctrl Pts',(49.9296375529241,52.2162903605272,12.));
#108866=CARTESIAN_POINT('Ctrl Pts',(49.919996091396,52.1938120478752,12.));
#108867=CARTESIAN_POINT('Ctrl Pts',(49.9103492455904,52.1713810841277,12.));
#108868=CARTESIAN_POINT('Ctrl Pts',(49.90069711499,52.1489975513449,12.));
#108869=CARTESIAN_POINT('Ctrl Pts',(49.8910397995404,52.1266615318414,12.));
#108870=CARTESIAN_POINT('Ctrl Pts',(49.8813773996523,52.1043731081968,12.));
#108871=CARTESIAN_POINT('Ctrl Pts',(49.871710016205,52.0821323632588,12.));
#108872=CARTESIAN_POINT('Ctrl Pts',(49.8620377505498,52.059939380145,12.));
#108873=CARTESIAN_POINT('Ctrl Pts',(49.8523607045146,52.0377942422373,12.));
#108874=CARTESIAN_POINT('Ctrl Pts',(49.8426789804068,52.015697033182,12.));
#108875=CARTESIAN_POINT('Ctrl Pts',(49.8329926810172,51.9936478369008,12.));
#108876=CARTESIAN_POINT('Ctrl Pts',(49.8233019096224,51.9716467375938,12.));
#108877=CARTESIAN_POINT('Ctrl Pts',(49.8136067699896,51.9496938197418,12.));
#108878=CARTESIAN_POINT('Ctrl Pts',(49.8039073663808,51.9277891681014,12.));
#108879=CARTESIAN_POINT('Ctrl Pts',(49.7942038035568,51.9059328677051,12.));
#108880=CARTESIAN_POINT('Ctrl Pts',(49.78449618678,51.8841250038716,12.));
#108881=CARTESIAN_POINT('Ctrl Pts',(49.7747846218177,51.8623656622092,12.));
#108882=CARTESIAN_POINT('Ctrl Pts',(49.7650692149464,51.8406549286177,12.));
#108883=CARTESIAN_POINT('Ctrl Pts',(49.7553500729563,51.8189928892841,12.));
#108884=CARTESIAN_POINT('Ctrl Pts',(49.7456273031555,51.7973796306826,12.));
#108885=CARTESIAN_POINT('Ctrl Pts',(49.7359010133741,51.7758152395857,12.));
#108886=CARTESIAN_POINT('Ctrl Pts',(49.7261713119672,51.754299803068,12.));
#108887=CARTESIAN_POINT('Ctrl Pts',(49.7164383078206,51.7328334085084,12.));
#108888=CARTESIAN_POINT('Ctrl Pts',(49.7067021103534,51.7114161435848,12.));
#108889=CARTESIAN_POINT('Ctrl Pts',(49.6969628295236,51.6900480962744,12.));
#108890=CARTESIAN_POINT('Ctrl Pts',(49.6872205758314,51.6687293548656,12.));
#108891=CARTESIAN_POINT('Ctrl Pts',(49.6774754603235,51.6474600079611,12.));
#108892=CARTESIAN_POINT('Ctrl Pts',(49.6677275945975,51.6262401444799,12.));
#108893=CARTESIAN_POINT('Ctrl Pts',(49.6579770908063,51.6050698536525,12.));
#108894=CARTESIAN_POINT('Ctrl Pts',(49.6482240616627,51.5839492250218,12.));
#108895=CARTESIAN_POINT('Ctrl Pts',(49.6384686204443,51.5628783484556,12.));
#108896=CARTESIAN_POINT('Ctrl Pts',(49.6287108809975,51.5418573141494,12.));
#108897=CARTESIAN_POINT('Ctrl Pts',(49.6189509577441,51.5208862126303,12.));
#108898=CARTESIAN_POINT('Ctrl Pts',(49.609188965684,51.4999651347496,12.));
#108899=CARTESIAN_POINT('Ctrl Pts',(49.5994250204003,51.4790941716859,12.));
#108900=CARTESIAN_POINT('Ctrl Pts',(49.5896592380634,51.4582734149562,12.));
#108901=CARTESIAN_POINT('Ctrl Pts',(49.579891735436,51.4375029564191,12.));
#108902=CARTESIAN_POINT('Ctrl Pts',(49.5701226298779,51.4167828882765,12.));
#108903=CARTESIAN_POINT('Ctrl Pts',(49.5603520393514,51.3961133030688,12.));
#108904=CARTESIAN_POINT('Ctrl Pts',(49.5505800824268,51.3754942936796,12.));
#108905=CARTESIAN_POINT('Ctrl Pts',(49.5408068782871,51.354925953347,12.));
#108906=CARTESIAN_POINT('Ctrl Pts',(49.5310325467334,51.3344083756659,12.));
#108907=CARTESIAN_POINT('Ctrl Pts',(49.5212572081901,51.3139416545903,12.));
#108908=CARTESIAN_POINT('Ctrl Pts',(49.5114809837111,51.2935258844278,12.));
#108909=CARTESIAN_POINT('Ctrl Pts',(49.5017039949841,51.2731611598465,12.));
#108910=CARTESIAN_POINT('Ctrl Pts',(49.4919263643357,51.2528475758841,12.));
#108911=CARTESIAN_POINT('Ctrl Pts',(49.4821482147357,51.2325852279507,12.));
#108912=CARTESIAN_POINT('Ctrl Pts',(49.4723696698022,51.2123742118288,12.));
#108913=CARTESIAN_POINT('Ctrl Pts',(49.4625908538076,51.1922146236686,12.));
#108914=CARTESIAN_POINT('Ctrl Pts',(49.4528118916833,51.1721065599972,12.));
#108915=CARTESIAN_POINT('Ctrl Pts',(49.4430329090288,51.1520501177291,12.));
#108916=CARTESIAN_POINT('Ctrl Pts',(49.4332540321178,51.1320453941702,12.));
#108917=CARTESIAN_POINT('Ctrl Pts',(49.4234753879071,51.1120924870196,12.));
#108918=CARTESIAN_POINT('Ctrl Pts',(49.4136971040428,51.0921914943663,12.));
#108919=CARTESIAN_POINT('Ctrl Pts',(49.4039193088635,51.0723425146987,12.));
#108920=CARTESIAN_POINT('Ctrl Pts',(49.3941421314014,51.0525456469072,12.));
#108921=CARTESIAN_POINT('Ctrl Pts',(49.3843657013851,51.0328009902857,12.));
#108922=CARTESIAN_POINT('Ctrl Pts',(49.3745901492428,51.0131086445268,12.));
#108923=CARTESIAN_POINT('Ctrl Pts',(49.3648156061049,50.9934687097179,12.));
#108924=CARTESIAN_POINT('Ctrl Pts',(49.3550422038221,50.9738812863636,12.));
#108925=CARTESIAN_POINT('Ctrl Pts',(49.3452700749804,50.9543464753974,12.));
#108926=CARTESIAN_POINT('Ctrl Pts',(49.3354993529163,50.9348643781928,12.));
#108927=CARTESIAN_POINT('Ctrl Pts',(49.325730171735,50.9154350965681,12.));
#108928=CARTESIAN_POINT('Ctrl Pts',(49.3159626663129,50.8960587327869,12.));
#108929=CARTESIAN_POINT('Ctrl Pts',(49.3061969722798,50.8767353895509,12.));
#108930=CARTESIAN_POINT('Ctrl Pts',(49.2964332260043,50.8574651699877,12.));
#108931=CARTESIAN_POINT('Ctrl Pts',(49.2866715645828,50.8382481776392,12.));
#108932=CARTESIAN_POINT('Ctrl Pts',(49.2769121258144,50.8190845164319,12.));
#108933=CARTESIAN_POINT('Ctrl Pts',(49.2671550482415,50.7999742907111,12.));
#108934=CARTESIAN_POINT('Ctrl Pts',(49.2574004712122,50.7809176052954,12.));
#108935=CARTESIAN_POINT('Ctrl Pts',(49.2476485349373,50.7619145655207,12.));
#108936=CARTESIAN_POINT('Ctrl Pts',(49.2378993805482,50.7429652772816,12.));
#108937=CARTESIAN_POINT('Ctrl Pts',(49.2281531501569,50.7240698470698,12.));
#108938=CARTESIAN_POINT('Ctrl Pts',(49.218409986748,50.7052283818941,12.));
#108939=CARTESIAN_POINT('Ctrl Pts',(49.2086700340625,50.6864409891905,12.));
#108940=CARTESIAN_POINT('Ctrl Pts',(49.1989334364991,50.6677077767427,12.));
#108941=CARTESIAN_POINT('Ctrl Pts',(49.1892003389743,50.6490288525639,12.));
#108942=CARTESIAN_POINT('Ctrl Pts',(49.1794708869074,50.6304043248796,12.));
#108943=CARTESIAN_POINT('Ctrl Pts',(49.1697452265473,50.6118343023937,12.));
#108944=CARTESIAN_POINT('Ctrl Pts',(49.1600235052613,50.593318894516,12.));
#108945=CARTESIAN_POINT('Ctrl Pts',(49.1503058717831,50.5748582115575,12.));
#108946=CARTESIAN_POINT('Ctrl Pts',(49.1405924766169,50.5564523650406,12.));
#108947=CARTESIAN_POINT('Ctrl Pts',(49.1308834717645,50.5381014674822,12.));
#108948=CARTESIAN_POINT('Ctrl Pts',(49.1211790099817,50.5198056318111,12.));
#108949=CARTESIAN_POINT('Ctrl Pts',(49.1114792441573,50.5015649708742,12.));
#108950=CARTESIAN_POINT('Ctrl Pts',(49.1017843266782,50.4833795969296,12.));
#108951=CARTESIAN_POINT('Ctrl Pts',(49.0920944086973,50.465249621057,12.));
#108952=CARTESIAN_POINT('Ctrl Pts',(49.0824096415339,50.4471751542717,12.));
#108953=CARTESIAN_POINT('Ctrl Pts',(49.0727301783477,50.4291563088528,12.));
#108954=CARTESIAN_POINT('Ctrl Pts',(49.0630561755082,50.4111931994264,12.));
#108955=CARTESIAN_POINT('Ctrl Pts',(49.0533877945771,50.393285944528,12.));
#108956=CARTESIAN_POINT('Ctrl Pts',(49.0437252024868,50.3754346667389,12.));
#108957=CARTESIAN_POINT('Ctrl Pts',(49.034068567401,50.3576394894136,12.));
#108958=CARTESIAN_POINT('Ctrl Pts',(49.0244180550759,50.3399005337967,12.));
#108959=CARTESIAN_POINT('Ctrl Pts',(49.0147738256925,50.3222179165102,12.));
#108960=CARTESIAN_POINT('Ctrl Pts',(49.0051360288002,50.3045917455383,12.));
#108961=CARTESIAN_POINT('Ctrl Pts',(48.9955048082028,50.2870221241003,12.));
#108962=CARTESIAN_POINT('Ctrl Pts',(48.9858803116649,50.2695091583473,12.));
#108963=CARTESIAN_POINT('Ctrl Pts',(48.9762626987227,50.252052963548,12.));
#108964=CARTESIAN_POINT('Ctrl Pts',(48.9666521500969,50.2346536715465,12.));
#108965=CARTESIAN_POINT('Ctrl Pts',(48.9570488741273,50.2173114358423,12.));
#108966=CARTESIAN_POINT('Ctrl Pts',(48.9474530868847,50.2000264157903,12.));
#108967=CARTESIAN_POINT('Ctrl Pts',(48.9378649933116,50.1827987615659,12.));
#108968=CARTESIAN_POINT('Ctrl Pts',(48.9282847698237,50.1656286003943,12.));
#108969=CARTESIAN_POINT('Ctrl Pts',(48.9187125417897,50.148516018447,12.));
#108970=CARTESIAN_POINT('Ctrl Pts',(48.9091483817797,50.1314610602286,12.));
#108971=CARTESIAN_POINT('Ctrl Pts',(48.9015035371772,50.1178632066821,12.));
#108972=CARTESIAN_POINT('Ctrl Pts',(48.8957735556681,50.1076907555303,12.));
#108973=CARTESIAN_POINT('Ctrl Pts',(48.8919551910299,50.1009206494209,12.));
#108974=CARTESIAN_POINT('Ctrl Pts',(48.8900464144686,50.0975384783634,12.));
#108975=CARTESIAN_POINT('Ctrl Pts',(49.5707719660639,55.2174072001495,-5.55111512312578E-16));
#108976=CARTESIAN_POINT('Ctrl Pts',(49.5707719660639,55.2174072001495,4.));
#108977=CARTESIAN_POINT('Ctrl Pts',(49.5707719660639,55.2174072001495,8.));
#108978=CARTESIAN_POINT('Ctrl Pts',(49.5707719660639,55.2174072001495,12.));
#108979=CARTESIAN_POINT('Ctrl Pts',(49.6712810246933,55.2618153697169,-5.55111512312578E-16));
#108980=CARTESIAN_POINT('Ctrl Pts',(49.6712810246933,55.2618153697169,4.));
#108981=CARTESIAN_POINT('Ctrl Pts',(49.6712810246933,55.2618153697169,8.));
#108982=CARTESIAN_POINT('Ctrl Pts',(49.6712810246933,55.2618153697169,12.));
#108983=CARTESIAN_POINT('Ctrl Pts',(49.8732090625342,55.2790667815473,-5.55111512312578E-16));
#108984=CARTESIAN_POINT('Ctrl Pts',(49.8732090625342,55.2790667815473,4.));
#108985=CARTESIAN_POINT('Ctrl Pts',(49.8732090625342,55.2790667815473,7.99999999999999));
#108986=CARTESIAN_POINT('Ctrl Pts',(49.8732090625342,55.2790667815473,12.));
#108987=CARTESIAN_POINT('Ctrl Pts',(50.0481613529516,55.1854902750885,-5.55111512312578E-16));
#108988=CARTESIAN_POINT('Ctrl Pts',(50.0481613529516,55.1854902750885,4.));
#108989=CARTESIAN_POINT('Ctrl Pts',(50.0481613529516,55.1854902750885,8.00000000000001));
#108990=CARTESIAN_POINT('Ctrl Pts',(50.0481613529516,55.1854902750885,12.));
#108991=CARTESIAN_POINT('Ctrl Pts',(50.1091461876225,55.1300595714123,-5.55111512312578E-16));
#108992=CARTESIAN_POINT('Ctrl Pts',(50.1091461876225,55.1300595714123,4.));
#108993=CARTESIAN_POINT('Ctrl Pts',(50.1091461876225,55.1300595714123,8.));
#108994=CARTESIAN_POINT('Ctrl Pts',(50.1091461876225,55.1300595714123,12.));
#108995=CARTESIAN_POINT('',(49.5707719660639,55.2174072001495,-2.77555756156289E-16));
#108996=CARTESIAN_POINT('',(50.1091461876225,55.1300595714124,2.77555756156289E-16));
#108997=CARTESIAN_POINT('Ctrl Pts',(49.5707719660639,55.2174072001495,-5.55111512312578E-16));
#108998=CARTESIAN_POINT('Ctrl Pts',(49.6712810246933,55.2618153697169,-5.55111512312578E-16));
#108999=CARTESIAN_POINT('Ctrl Pts',(49.7866684748881,55.2716733193343,-5.55111512312578E-16));
#109000=CARTESIAN_POINT('Ctrl Pts',(49.8932475177609,55.2453425609388,-5.55111512312578E-16));
#109001=CARTESIAN_POINT('Ctrl Pts',(49.9731817999155,55.2255944921423,-5.55111512312578E-16));
#109002=CARTESIAN_POINT('Ctrl Pts',(50.0481613529516,55.1854902750885,-5.55111512312578E-16));
#109003=CARTESIAN_POINT('Ctrl Pts',(50.1091461876225,55.1300595714123,-5.55111512312578E-16));
#109004=CARTESIAN_POINT('',(50.1091461876225,55.1300595714124,12.));
#109005=CARTESIAN_POINT('Ctrl Pts',(50.1091461876225,55.1300595714123,-5.55111512312578E-16));
#109006=CARTESIAN_POINT('Ctrl Pts',(50.1091461876225,55.1300595714123,4.));
#109007=CARTESIAN_POINT('Ctrl Pts',(50.1091461876225,55.1300595714123,8.));
#109008=CARTESIAN_POINT('Ctrl Pts',(50.1091461876225,55.1300595714123,12.));
#109009=CARTESIAN_POINT('',(49.5707719660639,55.2174072001495,12.));
#109010=CARTESIAN_POINT('Ctrl Pts',(50.1091461876225,55.1300595714123,12.));
#109011=CARTESIAN_POINT('Ctrl Pts',(50.0481613529516,55.1854902750885,12.));
#109012=CARTESIAN_POINT('Ctrl Pts',(49.9731817999155,55.2255944921423,12.));
#109013=CARTESIAN_POINT('Ctrl Pts',(49.8932475177609,55.2453425609388,12.));
#109014=CARTESIAN_POINT('Ctrl Pts',(49.7866684748881,55.2716733193343,12.));
#109015=CARTESIAN_POINT('Ctrl Pts',(49.6712810246933,55.2618153697169,12.));
#109016=CARTESIAN_POINT('Ctrl Pts',(49.5707719660639,55.2174072001495,12.));
#109017=CARTESIAN_POINT('Ctrl Pts',(49.5707719660639,55.2174072001495,12.));
#109018=CARTESIAN_POINT('Ctrl Pts',(49.5707719660639,55.2174072001495,8.));
#109019=CARTESIAN_POINT('Ctrl Pts',(49.5707719660639,55.2174072001495,4.));
#109020=CARTESIAN_POINT('Ctrl Pts',(49.5707719660639,55.2174072001495,-5.55111512312578E-16));
#109021=CARTESIAN_POINT('Origin',(2.53167595884892E-10,2.7643087079898E-10,
0.));
#109022=CARTESIAN_POINT('Origin',(2.53167595884892E-10,2.7643087079898E-10,
12.));
#109023=CARTESIAN_POINT('Origin',(2.53167595884892E-10,2.7643087079898E-10,
0.));
#109024=CARTESIAN_POINT('Ctrl Pts',(55.1300595714105,50.1091461876246,0.));
#109025=CARTESIAN_POINT('Ctrl Pts',(55.1300595714105,50.1091461876246,4.));
#109026=CARTESIAN_POINT('Ctrl Pts',(55.1300595714105,50.1091461876246,8.));
#109027=CARTESIAN_POINT('Ctrl Pts',(55.1300595714105,50.1091461876246,12.));
#109028=CARTESIAN_POINT('Ctrl Pts',(55.2039671763178,50.0278330747237,0.));
#109029=CARTESIAN_POINT('Ctrl Pts',(55.2039671763178,50.0278330747237,4.));
#109030=CARTESIAN_POINT('Ctrl Pts',(55.2039671763178,50.0278330747237,8.));
#109031=CARTESIAN_POINT('Ctrl Pts',(55.2039671763178,50.0278330747237,12.));
#109032=CARTESIAN_POINT('Ctrl Pts',(55.2841761056306,49.8417173275612,0.));
#109033=CARTESIAN_POINT('Ctrl Pts',(55.2841761056306,49.8417173275612,4.));
#109034=CARTESIAN_POINT('Ctrl Pts',(55.2841761056306,49.8417173275612,7.99999999999999));
#109035=CARTESIAN_POINT('Ctrl Pts',(55.2841761056306,49.8417173275612,12.));
#109036=CARTESIAN_POINT('Ctrl Pts',(55.2507133273147,49.6461537600002,0.));
#109037=CARTESIAN_POINT('Ctrl Pts',(55.2507133273147,49.6461537600002,4.));
#109038=CARTESIAN_POINT('Ctrl Pts',(55.2507133273147,49.6461537600002,8.00000000000001));
#109039=CARTESIAN_POINT('Ctrl Pts',(55.2507133273147,49.6461537600002,12.));
#109040=CARTESIAN_POINT('Ctrl Pts',(55.21740720013,49.5707719660253,0.));
#109041=CARTESIAN_POINT('Ctrl Pts',(55.21740720013,49.5707719660253,4.));
#109042=CARTESIAN_POINT('Ctrl Pts',(55.21740720013,49.5707719660253,8.));
#109043=CARTESIAN_POINT('Ctrl Pts',(55.21740720013,49.5707719660253,12.));
#109044=CARTESIAN_POINT('',(55.1300595714105,50.1091461876246,0.));
#109045=CARTESIAN_POINT('',(55.2174072001297,49.5707719660254,0.));
#109046=CARTESIAN_POINT('Ctrl Pts',(55.1300595714105,50.1091461876246,1.38777878078145E-16));
#109047=CARTESIAN_POINT('Ctrl Pts',(55.2039671763178,50.0278330747237,1.38777878078145E-16));
#109048=CARTESIAN_POINT('Ctrl Pts',(55.2498008502108,49.9214812192023,1.38777878078145E-16));
#109049=CARTESIAN_POINT('Ctrl Pts',(55.2585172318169,49.8120443611017,1.38777878078145E-16));
#109050=CARTESIAN_POINT('Ctrl Pts',(55.2650545180215,49.7299667175263,1.38777878078145E-16));
#109051=CARTESIAN_POINT('Ctrl Pts',(55.2507133273147,49.6461537600002,1.38777878078144E-16));
#109052=CARTESIAN_POINT('Ctrl Pts',(55.21740720013,49.5707719660253,1.38777878078145E-16));
#109053=CARTESIAN_POINT('',(55.2174072001297,49.5707719660254,12.));
#109054=CARTESIAN_POINT('Ctrl Pts',(55.21740720013,49.5707719660253,0.));
#109055=CARTESIAN_POINT('Ctrl Pts',(55.21740720013,49.5707719660253,4.));
#109056=CARTESIAN_POINT('Ctrl Pts',(55.21740720013,49.5707719660253,8.));
#109057=CARTESIAN_POINT('Ctrl Pts',(55.21740720013,49.5707719660253,12.));
#109058=CARTESIAN_POINT('',(55.1300595714105,50.1091461876246,12.));
#109059=CARTESIAN_POINT('Ctrl Pts',(55.21740720013,49.5707719660253,12.));
#109060=CARTESIAN_POINT('Ctrl Pts',(55.2507133273147,49.6461537600002,12.));
#109061=CARTESIAN_POINT('Ctrl Pts',(55.2650545180215,49.7299667175263,12.));
#109062=CARTESIAN_POINT('Ctrl Pts',(55.2585172318169,49.8120443611017,12.));
#109063=CARTESIAN_POINT('Ctrl Pts',(55.2498008502108,49.9214812192023,12.));
#109064=CARTESIAN_POINT('Ctrl Pts',(55.2039671763178,50.0278330747237,12.));
#109065=CARTESIAN_POINT('Ctrl Pts',(55.1300595714105,50.1091461876246,12.));
#109066=CARTESIAN_POINT('Ctrl Pts',(55.1300595714105,50.1091461876246,12.));
#109067=CARTESIAN_POINT('Ctrl Pts',(55.1300595714105,50.1091461876246,8.));
#109068=CARTESIAN_POINT('Ctrl Pts',(55.1300595714105,50.1091461876246,4.));
#109069=CARTESIAN_POINT('Ctrl Pts',(55.1300595714105,50.1091461876246,0.));
#109070=CARTESIAN_POINT('Ctrl Pts',(53.0702932034641,45.6458539113724,0.));
#109071=CARTESIAN_POINT('Ctrl Pts',(53.0702932034641,45.6458539113724,12.));
#109072=CARTESIAN_POINT('Ctrl Pts',(53.0724894921849,45.6490568514089,0.));
#109073=CARTESIAN_POINT('Ctrl Pts',(53.0724894921849,45.6490568514089,12.));
#109074=CARTESIAN_POINT('Ctrl Pts',(53.0768833804193,45.6554684028145,0.));
#109075=CARTESIAN_POINT('Ctrl Pts',(53.0768833804193,45.6554684028145,12.));
#109076=CARTESIAN_POINT('Ctrl Pts',(53.0834781451546,45.6651027439241,0.));
#109077=CARTESIAN_POINT('Ctrl Pts',(53.0834781451546,45.6651027439241,12.));
#109078=CARTESIAN_POINT('Ctrl Pts',(53.0922790298409,45.6779825614231,0.));
#109079=CARTESIAN_POINT('Ctrl Pts',(53.0922790298409,45.6779825614231,12.));
#109080=CARTESIAN_POINT('Ctrl Pts',(53.1032932328857,45.694139048907,0.));
#109081=CARTESIAN_POINT('Ctrl Pts',(53.1032932328857,45.694139048907,12.));
#109082=CARTESIAN_POINT('Ctrl Pts',(53.114320495492,45.7103522376696,0.));
#109083=CARTESIAN_POINT('Ctrl Pts',(53.114320495492,45.7103522376696,12.));
#109084=CARTESIAN_POINT('Ctrl Pts',(53.1253607414872,45.7266220897003,0.));
#109085=CARTESIAN_POINT('Ctrl Pts',(53.1253607414872,45.7266220897003,12.));
#109086=CARTESIAN_POINT('Ctrl Pts',(53.1364138384693,45.7429485300823,0.));
#109087=CARTESIAN_POINT('Ctrl Pts',(53.1364138384693,45.7429485300823,12.));
#109088=CARTESIAN_POINT('Ctrl Pts',(53.1474795996053,45.7593314474501,0.));
#109089=CARTESIAN_POINT('Ctrl Pts',(53.1474795996053,45.7593314474501,12.));
#109090=CARTESIAN_POINT('Ctrl Pts',(53.1585578076444,45.7757707100618,0.));
#109091=CARTESIAN_POINT('Ctrl Pts',(53.1585578076444,45.7757707100618,12.));
#109092=CARTESIAN_POINT('Ctrl Pts',(53.1696482334487,45.7922661780005,0.));
#109093=CARTESIAN_POINT('Ctrl Pts',(53.1696482334487,45.7922661780005,12.));
#109094=CARTESIAN_POINT('Ctrl Pts',(53.1807506560933,45.808817716509,0.));
#109095=CARTESIAN_POINT('Ctrl Pts',(53.1807506560933,45.808817716509,12.));
#109096=CARTESIAN_POINT('Ctrl Pts',(53.1918648840541,45.8254252099957,0.));
#109097=CARTESIAN_POINT('Ctrl Pts',(53.1918648840541,45.8254252099957,12.));
#109098=CARTESIAN_POINT('Ctrl Pts',(53.2029907483557,45.8420885575349,0.));
#109099=CARTESIAN_POINT('Ctrl Pts',(53.2029907483557,45.8420885575349,12.));
#109100=CARTESIAN_POINT('Ctrl Pts',(53.2141280925439,45.8588076662582,0.));
#109101=CARTESIAN_POINT('Ctrl Pts',(53.2141280925439,45.8588076662582,12.));
#109102=CARTESIAN_POINT('Ctrl Pts',(53.2252767643662,45.8755824458723,0.));
#109103=CARTESIAN_POINT('Ctrl Pts',(53.2252767643662,45.8755824458723,12.));
#109104=CARTESIAN_POINT('Ctrl Pts',(53.2364366054306,45.892412801838,0.));
#109105=CARTESIAN_POINT('Ctrl Pts',(53.2364366054306,45.892412801838,12.));
#109106=CARTESIAN_POINT('Ctrl Pts',(53.2476074460017,45.9092986319377,0.));
#109107=CARTESIAN_POINT('Ctrl Pts',(53.2476074460017,45.9092986319377,12.));
#109108=CARTESIAN_POINT('Ctrl Pts',(53.2587891103866,45.9262398298349,0.));
#109109=CARTESIAN_POINT('Ctrl Pts',(53.2587891103866,45.9262398298349,12.));
#109110=CARTESIAN_POINT('Ctrl Pts',(53.2699814203105,45.9432362873008,0.));
#109111=CARTESIAN_POINT('Ctrl Pts',(53.2699814203105,45.9432362873008,12.));
#109112=CARTESIAN_POINT('Ctrl Pts',(53.2811841987926,45.9602878967698,0.));
#109113=CARTESIAN_POINT('Ctrl Pts',(53.2811841987926,45.9602878967698,12.));
#109114=CARTESIAN_POINT('Ctrl Pts',(53.292397274555,45.9773945542384,0.));
#109115=CARTESIAN_POINT('Ctrl Pts',(53.292397274555,45.9773945542384,12.));
#109116=CARTESIAN_POINT('Ctrl Pts',(53.3036204818329,45.9945561591453,0.));
#109117=CARTESIAN_POINT('Ctrl Pts',(53.3036204818329,45.9945561591453,12.));
#109118=CARTESIAN_POINT('Ctrl Pts',(53.3148536582635,46.0117726129873,0.));
#109119=CARTESIAN_POINT('Ctrl Pts',(53.3148536582635,46.0117726129873,12.));
#109120=CARTESIAN_POINT('Ctrl Pts',(53.326096643428,46.02904381836,0.));
#109121=CARTESIAN_POINT('Ctrl Pts',(53.326096643428,46.02904381836,12.));
#109122=CARTESIAN_POINT('Ctrl Pts',(53.3373492770671,46.0463696777801,0.));
#109123=CARTESIAN_POINT('Ctrl Pts',(53.3373492770671,46.0463696777801,12.));
#109124=CARTESIAN_POINT('Ctrl Pts',(53.3486113975901,46.0637500926982,0.));
#109125=CARTESIAN_POINT('Ctrl Pts',(53.3486113975901,46.0637500926982,12.));
#109126=CARTESIAN_POINT('Ctrl Pts',(53.3598828428546,46.0811849640218,0.));
#109127=CARTESIAN_POINT('Ctrl Pts',(53.3598828428546,46.0811849640218,12.));
#109128=CARTESIAN_POINT('Ctrl Pts',(53.3711634508437,46.0986741925656,0.));
#109129=CARTESIAN_POINT('Ctrl Pts',(53.3711634508437,46.0986741925656,12.));
#109130=CARTESIAN_POINT('Ctrl Pts',(53.3824530603276,46.1162176794884,0.));
#109131=CARTESIAN_POINT('Ctrl Pts',(53.3824530603276,46.1162176794884,12.));
#109132=CARTESIAN_POINT('Ctrl Pts',(53.3937515116549,46.1338153268097,0.));
#109133=CARTESIAN_POINT('Ctrl Pts',(53.3937515116549,46.1338153268097,12.));
#109134=CARTESIAN_POINT('Ctrl Pts',(53.4050586470436,46.1514670376012,0.));
#109135=CARTESIAN_POINT('Ctrl Pts',(53.4050586470436,46.1514670376012,12.));
#109136=CARTESIAN_POINT('Ctrl Pts',(53.4163743101517,46.1691727157134,0.));
#109137=CARTESIAN_POINT('Ctrl Pts',(53.4163743101517,46.1691727157134,12.));
#109138=CARTESIAN_POINT('Ctrl Pts',(53.4276983458125,46.1869322656024,0.));
#109139=CARTESIAN_POINT('Ctrl Pts',(53.4276983458125,46.1869322656024,12.));
#109140=CARTESIAN_POINT('Ctrl Pts',(53.4390305997274,46.2047455921286,0.));
#109141=CARTESIAN_POINT('Ctrl Pts',(53.4390305997274,46.2047455921286,12.));
#109142=CARTESIAN_POINT('Ctrl Pts',(53.4503709181178,46.2226126003202,0.));
#109143=CARTESIAN_POINT('Ctrl Pts',(53.4503709181178,46.2226126003202,12.));
#109144=CARTESIAN_POINT('Ctrl Pts',(53.4617191477402,46.2405331953889,0.));
#109145=CARTESIAN_POINT('Ctrl Pts',(53.4617191477402,46.2405331953889,12.));
#109146=CARTESIAN_POINT('Ctrl Pts',(53.4730751360371,46.2585072828353,0.));
#109147=CARTESIAN_POINT('Ctrl Pts',(53.4730751360371,46.2585072828353,12.));
#109148=CARTESIAN_POINT('Ctrl Pts',(53.4844387312414,46.2765347685198,0.));
#109149=CARTESIAN_POINT('Ctrl Pts',(53.4844387312414,46.2765347685198,12.));
#109150=CARTESIAN_POINT('Ctrl Pts',(53.4958097825006,46.2946155587417,0.));
#109151=CARTESIAN_POINT('Ctrl Pts',(53.4958097825006,46.2946155587417,12.));
#109152=CARTESIAN_POINT('Ctrl Pts',(53.5071881399911,46.3127495603098,0.));
#109153=CARTESIAN_POINT('Ctrl Pts',(53.5071881399911,46.3127495603098,12.));
#109154=CARTESIAN_POINT('Ctrl Pts',(53.5185736548548,46.3309366805093,0.));
#109155=CARTESIAN_POINT('Ctrl Pts',(53.5185736548548,46.3309366805093,12.));
#109156=CARTESIAN_POINT('Ctrl Pts',(53.5299661791385,46.3491768270655,0.));
#109157=CARTESIAN_POINT('Ctrl Pts',(53.5299661791385,46.3491768270655,12.));
#109158=CARTESIAN_POINT('Ctrl Pts',(53.5413655657327,46.3674699081046,0.));
#109159=CARTESIAN_POINT('Ctrl Pts',(53.5413655657327,46.3674699081046,12.));
#109160=CARTESIAN_POINT('Ctrl Pts',(53.5527716683048,46.3858158321059,0.));
#109161=CARTESIAN_POINT('Ctrl Pts',(53.5527716683048,46.3858158321059,12.));
#109162=CARTESIAN_POINT('Ctrl Pts',(53.5641843412559,46.4042145078701,0.));
#109163=CARTESIAN_POINT('Ctrl Pts',(53.5641843412559,46.4042145078701,12.));
#109164=CARTESIAN_POINT('Ctrl Pts',(53.5756034397481,46.4226658445474,0.));
#109165=CARTESIAN_POINT('Ctrl Pts',(53.5756034397481,46.4226658445474,12.));
#109166=CARTESIAN_POINT('Ctrl Pts',(53.5870288197166,46.4411697516478,0.));
#109167=CARTESIAN_POINT('Ctrl Pts',(53.5870288197166,46.4411697516478,12.));
#109168=CARTESIAN_POINT('Ctrl Pts',(53.5984603378855,46.459726139052,0.));
#109169=CARTESIAN_POINT('Ctrl Pts',(53.5984603378855,46.459726139052,12.));
#109170=CARTESIAN_POINT('Ctrl Pts',(53.6098978517859,46.4783349170173,0.));
#109171=CARTESIAN_POINT('Ctrl Pts',(53.6098978517859,46.4783349170173,12.));
#109172=CARTESIAN_POINT('Ctrl Pts',(53.6213412197533,46.496995996177,0.));
#109173=CARTESIAN_POINT('Ctrl Pts',(53.6213412197533,46.496995996177,12.));
#109174=CARTESIAN_POINT('Ctrl Pts',(53.6327903009094,46.5157092875373,0.));
#109175=CARTESIAN_POINT('Ctrl Pts',(53.6327903009094,46.5157092875373,12.));
#109176=CARTESIAN_POINT('Ctrl Pts',(53.6442449551455,46.5344747024676,0.));
#109177=CARTESIAN_POINT('Ctrl Pts',(53.6442449551455,46.5344747024676,12.));
#109178=CARTESIAN_POINT('Ctrl Pts',(53.6557050431071,46.5532921526901,0.));
#109179=CARTESIAN_POINT('Ctrl Pts',(53.6557050431071,46.5532921526901,12.));
#109180=CARTESIAN_POINT('Ctrl Pts',(53.6671704261737,46.5721615502591,0.));
#109181=CARTESIAN_POINT('Ctrl Pts',(53.6671704261737,46.5721615502591,12.));
#109182=CARTESIAN_POINT('Ctrl Pts',(53.678640966456,46.5910828075653,0.));
#109183=CARTESIAN_POINT('Ctrl Pts',(53.678640966456,46.5910828075653,12.));
#109184=CARTESIAN_POINT('Ctrl Pts',(53.6901165267941,46.6100558373402,0.));
#109185=CARTESIAN_POINT('Ctrl Pts',(53.6901165267941,46.6100558373402,12.));
#109186=CARTESIAN_POINT('Ctrl Pts',(53.701596970754,46.6290805526559,0.));
#109187=CARTESIAN_POINT('Ctrl Pts',(53.701596970754,46.6290805526559,12.));
#109188=CARTESIAN_POINT('Ctrl Pts',(53.7130821626263,46.6481568669216,0.));
#109189=CARTESIAN_POINT('Ctrl Pts',(53.7130821626263,46.6481568669216,12.));
#109190=CARTESIAN_POINT('Ctrl Pts',(53.7245719674222,46.6672846938752,0.));
#109191=CARTESIAN_POINT('Ctrl Pts',(53.7245719674222,46.6672846938752,12.));
#109192=CARTESIAN_POINT('Ctrl Pts',(53.7360662508677,46.6864639475863,0.));
#109193=CARTESIAN_POINT('Ctrl Pts',(53.7360662508677,46.6864639475863,12.));
#109194=CARTESIAN_POINT('Ctrl Pts',(53.7475648793948,46.7056945424559,0.));
#109195=CARTESIAN_POINT('Ctrl Pts',(53.7475648793948,46.7056945424559,12.));
#109196=CARTESIAN_POINT('Ctrl Pts',(53.7590677201344,46.724976393213,0.));
#109197=CARTESIAN_POINT('Ctrl Pts',(53.7590677201344,46.724976393213,12.));
#109198=CARTESIAN_POINT('Ctrl Pts',(53.770574640907,46.7443094149041,0.));
#109199=CARTESIAN_POINT('Ctrl Pts',(53.770574640907,46.7443094149041,12.));
#109200=CARTESIAN_POINT('Ctrl Pts',(53.782085510217,46.7636935228851,0.));
#109201=CARTESIAN_POINT('Ctrl Pts',(53.782085510217,46.7636935228851,12.));
#109202=CARTESIAN_POINT('Ctrl Pts',(53.7936001972468,46.7831286328268,0.));
#109203=CARTESIAN_POINT('Ctrl Pts',(53.7936001972468,46.7831286328268,12.));
#109204=CARTESIAN_POINT('Ctrl Pts',(53.8051185718525,46.8026146607144,0.));
#109205=CARTESIAN_POINT('Ctrl Pts',(53.8051185718525,46.8026146607144,12.));
#109206=CARTESIAN_POINT('Ctrl Pts',(53.8166405045582,46.8221515228459,0.));
#109207=CARTESIAN_POINT('Ctrl Pts',(53.8166405045582,46.8221515228459,12.));
#109208=CARTESIAN_POINT('Ctrl Pts',(53.8281658665517,46.8417391358231,0.));
#109209=CARTESIAN_POINT('Ctrl Pts',(53.8281658665517,46.8417391358231,12.));
#109210=CARTESIAN_POINT('Ctrl Pts',(53.8396945296777,46.8613774165452,0.));
#109211=CARTESIAN_POINT('Ctrl Pts',(53.8396945296777,46.8613774165452,12.));
#109212=CARTESIAN_POINT('Ctrl Pts',(53.851226366434,46.8810662822147,0.));
#109213=CARTESIAN_POINT('Ctrl Pts',(53.851226366434,46.8810662822147,12.));
#109214=CARTESIAN_POINT('Ctrl Pts',(53.8627612499648,46.900805650336,0.));
#109215=CARTESIAN_POINT('Ctrl Pts',(53.8627612499648,46.900805650336,12.));
#109216=CARTESIAN_POINT('Ctrl Pts',(53.8742990540557,46.9205954387128,0.));
#109217=CARTESIAN_POINT('Ctrl Pts',(53.8742990540557,46.9205954387128,12.));
#109218=CARTESIAN_POINT('Ctrl Pts',(53.8858396531277,46.9404355654381,0.));
#109219=CARTESIAN_POINT('Ctrl Pts',(53.8858396531277,46.9404355654381,12.));
#109220=CARTESIAN_POINT('Ctrl Pts',(53.8973829222317,46.9603259488894,0.));
#109221=CARTESIAN_POINT('Ctrl Pts',(53.8973829222317,46.9603259488894,12.));
#109222=CARTESIAN_POINT('Ctrl Pts',(53.9089287370436,46.9802665077342,0.));
#109223=CARTESIAN_POINT('Ctrl Pts',(53.9089287370436,46.9802665077342,12.));
#109224=CARTESIAN_POINT('Ctrl Pts',(53.9204769738584,47.0002571609286,0.));
#109225=CARTESIAN_POINT('Ctrl Pts',(53.9204769738584,47.0002571609286,12.));
#109226=CARTESIAN_POINT('Ctrl Pts',(53.9320275095864,47.0202978277148,0.));
#109227=CARTESIAN_POINT('Ctrl Pts',(53.9320275095864,47.0202978277148,12.));
#109228=CARTESIAN_POINT('Ctrl Pts',(53.9435802217468,47.04038842761,0.));
#109229=CARTESIAN_POINT('Ctrl Pts',(53.9435802217468,47.04038842761,12.));
#109230=CARTESIAN_POINT('Ctrl Pts',(53.9551349884637,47.0605288804042,0.));
#109231=CARTESIAN_POINT('Ctrl Pts',(53.9551349884637,47.0605288804042,12.));
#109232=CARTESIAN_POINT('Ctrl Pts',(53.9666916884624,47.0807191061674,0.));
#109233=CARTESIAN_POINT('Ctrl Pts',(53.9666916884624,47.0807191061674,12.));
#109234=CARTESIAN_POINT('Ctrl Pts',(53.9782502010642,47.1009590252466,0.));
#109235=CARTESIAN_POINT('Ctrl Pts',(53.9782502010642,47.1009590252466,12.));
#109236=CARTESIAN_POINT('Ctrl Pts',(53.9898104061809,47.1212485582632,0.));
#109237=CARTESIAN_POINT('Ctrl Pts',(53.9898104061809,47.1212485582632,12.));
#109238=CARTESIAN_POINT('Ctrl Pts',(54.0013721843094,47.1415876261012,0.));
#109239=CARTESIAN_POINT('Ctrl Pts',(54.0013721843094,47.1415876261012,12.));
#109240=CARTESIAN_POINT('Ctrl Pts',(54.0129354165269,47.161976149906,0.));
#109241=CARTESIAN_POINT('Ctrl Pts',(54.0129354165269,47.161976149906,12.));
#109242=CARTESIAN_POINT('Ctrl Pts',(54.0244999844872,47.1824140510906,0.));
#109243=CARTESIAN_POINT('Ctrl Pts',(54.0244999844872,47.1824140510906,12.));
#109244=CARTESIAN_POINT('Ctrl Pts',(54.0360657704156,47.2029012513334,0.));
#109245=CARTESIAN_POINT('Ctrl Pts',(54.0360657704156,47.2029012513334,12.));
#109246=CARTESIAN_POINT('Ctrl Pts',(54.047632657105,47.2234376725752,0.));
#109247=CARTESIAN_POINT('Ctrl Pts',(54.047632657105,47.2234376725752,12.));
#109248=CARTESIAN_POINT('Ctrl Pts',(54.0592005279108,47.2440232370085,0.));
#109249=CARTESIAN_POINT('Ctrl Pts',(54.0592005279108,47.2440232370085,12.));
#109250=CARTESIAN_POINT('Ctrl Pts',(54.0707692667461,47.2646578670767,0.));
#109251=CARTESIAN_POINT('Ctrl Pts',(54.0707692667461,47.2646578670767,12.));
#109252=CARTESIAN_POINT('Ctrl Pts',(54.082338758079,47.2853414854805,0.));
#109253=CARTESIAN_POINT('Ctrl Pts',(54.082338758079,47.2853414854805,12.));
#109254=CARTESIAN_POINT('Ctrl Pts',(54.0939088869271,47.3060740151754,0.));
#109255=CARTESIAN_POINT('Ctrl Pts',(54.0939088869271,47.3060740151754,12.));
#109256=CARTESIAN_POINT('Ctrl Pts',(54.1054795388538,47.326855379369,0.));
#109257=CARTESIAN_POINT('Ctrl Pts',(54.1054795388538,47.326855379369,12.));
#109258=CARTESIAN_POINT('Ctrl Pts',(54.1170505999637,47.3476855015095,0.));
#109259=CARTESIAN_POINT('Ctrl Pts',(54.1170505999637,47.3476855015095,12.));
#109260=CARTESIAN_POINT('Ctrl Pts',(54.1286219568981,47.3685643052867,0.));
#109261=CARTESIAN_POINT('Ctrl Pts',(54.1286219568981,47.3685643052867,12.));
#109262=CARTESIAN_POINT('Ctrl Pts',(54.1401934968306,47.3894917146361,0.));
#109263=CARTESIAN_POINT('Ctrl Pts',(54.1401934968306,47.3894917146361,12.));
#109264=CARTESIAN_POINT('Ctrl Pts',(54.1517651074638,47.4104676537381,0.));
#109265=CARTESIAN_POINT('Ctrl Pts',(54.1517651074638,47.4104676537381,12.));
#109266=CARTESIAN_POINT('Ctrl Pts',(54.163336677024,47.4314920470142,0.));
#109267=CARTESIAN_POINT('Ctrl Pts',(54.163336677024,47.4314920470142,12.));
#109268=CARTESIAN_POINT('Ctrl Pts',(54.1749080942593,47.4525648191173,0.));
#109269=CARTESIAN_POINT('Ctrl Pts',(54.1749080942593,47.4525648191173,12.));
#109270=CARTESIAN_POINT('Ctrl Pts',(54.1864792484343,47.473685894932,0.));
#109271=CARTESIAN_POINT('Ctrl Pts',(54.1864792484343,47.473685894932,12.));
#109272=CARTESIAN_POINT('Ctrl Pts',(54.1980500293267,47.4948551995799,0.));
#109273=CARTESIAN_POINT('Ctrl Pts',(54.1980500293267,47.4948551995799,12.));
#109274=CARTESIAN_POINT('Ctrl Pts',(54.2096203272228,47.5160726584172,0.));
#109275=CARTESIAN_POINT('Ctrl Pts',(54.2096203272228,47.5160726584172,12.));
#109276=CARTESIAN_POINT('Ctrl Pts',(54.2211900329141,47.5373381970328,0.));
#109277=CARTESIAN_POINT('Ctrl Pts',(54.2211900329141,47.5373381970328,12.));
#109278=CARTESIAN_POINT('Ctrl Pts',(54.232759037693,47.5586517412368,0.));
#109279=CARTESIAN_POINT('Ctrl Pts',(54.232759037693,47.5586517412368,12.));
#109280=CARTESIAN_POINT('Ctrl Pts',(54.2443272333498,47.5800132170614,0.));
#109281=CARTESIAN_POINT('Ctrl Pts',(54.2443272333498,47.5800132170614,12.));
#109282=CARTESIAN_POINT('Ctrl Pts',(54.2558945121684,47.6014225507664,0.));
#109283=CARTESIAN_POINT('Ctrl Pts',(54.2558945121684,47.6014225507664,12.));
#109284=CARTESIAN_POINT('Ctrl Pts',(54.2674607669228,47.6228796688376,0.));
#109285=CARTESIAN_POINT('Ctrl Pts',(54.2674607669228,47.6228796688376,12.));
#109286=CARTESIAN_POINT('Ctrl Pts',(54.2790258908736,47.6443844979846,0.));
#109287=CARTESIAN_POINT('Ctrl Pts',(54.2790258908736,47.6443844979846,12.));
#109288=CARTESIAN_POINT('Ctrl Pts',(54.2905897777647,47.6659369651299,0.));
#109289=CARTESIAN_POINT('Ctrl Pts',(54.2905897777647,47.6659369651299,12.));
#109290=CARTESIAN_POINT('Ctrl Pts',(54.3021523218188,47.6875369974086,0.));
#109291=CARTESIAN_POINT('Ctrl Pts',(54.3021523218188,47.6875369974086,12.));
#109292=CARTESIAN_POINT('Ctrl Pts',(54.3137134177345,47.7091845221748,0.));
#109293=CARTESIAN_POINT('Ctrl Pts',(54.3137134177345,47.7091845221748,12.));
#109294=CARTESIAN_POINT('Ctrl Pts',(54.3252729606824,47.7308794669994,0.));
#109295=CARTESIAN_POINT('Ctrl Pts',(54.3252729606824,47.7308794669994,12.));
#109296=CARTESIAN_POINT('Ctrl Pts',(54.3368308463023,47.7526217596694,0.));
#109297=CARTESIAN_POINT('Ctrl Pts',(54.3368308463023,47.7526217596694,12.));
#109298=CARTESIAN_POINT('Ctrl Pts',(54.3483869706998,47.7744113281768,0.));
#109299=CARTESIAN_POINT('Ctrl Pts',(54.3483869706998,47.7744113281768,12.));
#109300=CARTESIAN_POINT('Ctrl Pts',(54.3599412304431,47.7962481007179,0.));
#109301=CARTESIAN_POINT('Ctrl Pts',(54.3599412304431,47.7962481007179,12.));
#109302=CARTESIAN_POINT('Ctrl Pts',(54.3714935225585,47.8181320056988,0.));
#109303=CARTESIAN_POINT('Ctrl Pts',(54.3714935225585,47.8181320056988,12.));
#109304=CARTESIAN_POINT('Ctrl Pts',(54.3830437445275,47.8400629717352,0.));
#109305=CARTESIAN_POINT('Ctrl Pts',(54.3830437445275,47.8400629717352,12.));
#109306=CARTESIAN_POINT('Ctrl Pts',(54.3945917942835,47.8620409276495,0.));
#109307=CARTESIAN_POINT('Ctrl Pts',(54.3945917942835,47.8620409276495,12.));
#109308=CARTESIAN_POINT('Ctrl Pts',(54.4061375702088,47.8840658024626,0.));
#109309=CARTESIAN_POINT('Ctrl Pts',(54.4061375702088,47.8840658024626,12.));
#109310=CARTESIAN_POINT('Ctrl Pts',(54.4176809711324,47.9061375253909,0.));
#109311=CARTESIAN_POINT('Ctrl Pts',(54.4176809711324,47.9061375253909,12.));
#109312=CARTESIAN_POINT('Ctrl Pts',(54.4292218963253,47.9282560258528,0.));
#109313=CARTESIAN_POINT('Ctrl Pts',(54.4292218963253,47.9282560258528,12.));
#109314=CARTESIAN_POINT('Ctrl Pts',(54.4407602454974,47.9504212334681,0.));
#109315=CARTESIAN_POINT('Ctrl Pts',(54.4407602454974,47.9504212334681,12.));
#109316=CARTESIAN_POINT('Ctrl Pts',(54.4522959187952,47.972633078057,0.));
#109317=CARTESIAN_POINT('Ctrl Pts',(54.4522959187952,47.972633078057,12.));
#109318=CARTESIAN_POINT('Ctrl Pts',(54.4638288167991,47.9948914896316,0.));
#109319=CARTESIAN_POINT('Ctrl Pts',(54.4638288167991,47.9948914896316,12.));
#109320=CARTESIAN_POINT('Ctrl Pts',(54.4753588405202,48.0171963983912,0.));
#109321=CARTESIAN_POINT('Ctrl Pts',(54.4753588405202,48.0171963983912,12.));
#109322=CARTESIAN_POINT('Ctrl Pts',(54.4868858913961,48.039547734729,0.));
#109323=CARTESIAN_POINT('Ctrl Pts',(54.4868858913961,48.039547734729,12.));
#109324=CARTESIAN_POINT('Ctrl Pts',(54.4984098712883,48.0619454292321,0.));
#109325=CARTESIAN_POINT('Ctrl Pts',(54.4984098712883,48.0619454292321,12.));
#109326=CARTESIAN_POINT('Ctrl Pts',(54.5099306824788,48.0843894126807,0.));
#109327=CARTESIAN_POINT('Ctrl Pts',(54.5099306824788,48.0843894126807,12.));
#109328=CARTESIAN_POINT('Ctrl Pts',(54.5214482276679,48.1068796160406,0.));
#109329=CARTESIAN_POINT('Ctrl Pts',(54.5214482276679,48.1068796160406,12.));
#109330=CARTESIAN_POINT('Ctrl Pts',(54.5329624099719,48.1294159704571,0.));
#109331=CARTESIAN_POINT('Ctrl Pts',(54.5329624099719,48.1294159704571,12.));
#109332=CARTESIAN_POINT('Ctrl Pts',(54.5444731329196,48.1519984072617,0.));
#109333=CARTESIAN_POINT('Ctrl Pts',(54.5444731329196,48.1519984072617,12.));
#109334=CARTESIAN_POINT('Ctrl Pts',(54.5559803004487,48.1746268579732,0.));
#109335=CARTESIAN_POINT('Ctrl Pts',(54.5559803004487,48.1746268579732,12.));
#109336=CARTESIAN_POINT('Ctrl Pts',(54.5674838169041,48.1973012542966,0.));
#109337=CARTESIAN_POINT('Ctrl Pts',(54.5674838169041,48.1973012542966,12.));
#109338=CARTESIAN_POINT('Ctrl Pts',(54.5789835870348,48.2200215281178,0.));
#109339=CARTESIAN_POINT('Ctrl Pts',(54.5789835870348,48.2200215281178,12.));
#109340=CARTESIAN_POINT('Ctrl Pts',(54.5904795159936,48.2427876114956,0.));
#109341=CARTESIAN_POINT('Ctrl Pts',(54.5904795159936,48.2427876114956,12.));
#109342=CARTESIAN_POINT('Ctrl Pts',(54.6019715093319,48.2655994366672,0.));
#109343=CARTESIAN_POINT('Ctrl Pts',(54.6019715093319,48.2655994366672,12.));
#109344=CARTESIAN_POINT('Ctrl Pts',(54.6134594729964,48.288456936051,0.));
#109345=CARTESIAN_POINT('Ctrl Pts',(54.6134594729964,48.288456936051,12.));
#109346=CARTESIAN_POINT('Ctrl Pts',(54.6249433133262,48.3113600422443,0.));
#109347=CARTESIAN_POINT('Ctrl Pts',(54.6249433133262,48.3113600422443,12.));
#109348=CARTESIAN_POINT('Ctrl Pts',(54.636422937049,48.3343086880192,0.));
#109349=CARTESIAN_POINT('Ctrl Pts',(54.636422937049,48.3343086880192,12.));
#109350=CARTESIAN_POINT('Ctrl Pts',(54.647898251279,48.3573028063122,0.));
#109351=CARTESIAN_POINT('Ctrl Pts',(54.647898251279,48.3573028063122,12.));
#109352=CARTESIAN_POINT('Ctrl Pts',(54.6593691635143,48.3803423302294,0.));
#109353=CARTESIAN_POINT('Ctrl Pts',(54.6593691635143,48.3803423302294,12.));
#109354=CARTESIAN_POINT('Ctrl Pts',(54.6708355816359,48.4034271930516,0.));
#109355=CARTESIAN_POINT('Ctrl Pts',(54.6708355816359,48.4034271930516,12.));
#109356=CARTESIAN_POINT('Ctrl Pts',(54.6822974139065,48.4265573282342,0.));
#109357=CARTESIAN_POINT('Ctrl Pts',(54.6822974139065,48.4265573282342,12.));
#109358=CARTESIAN_POINT('Ctrl Pts',(54.6937545689694,48.4497326694051,0.));
#109359=CARTESIAN_POINT('Ctrl Pts',(54.6937545689694,48.4497326694051,12.));
#109360=CARTESIAN_POINT('Ctrl Pts',(54.7052069558493,48.4729531503565,0.));
#109361=CARTESIAN_POINT('Ctrl Pts',(54.7052069558493,48.4729531503565,12.));
#109362=CARTESIAN_POINT('Ctrl Pts',(54.7166544839475,48.4962187050452,0.));
#109363=CARTESIAN_POINT('Ctrl Pts',(54.7166544839475,48.4962187050452,12.));
#109364=CARTESIAN_POINT('Ctrl Pts',(54.7280970630346,48.5195292675955,0.));
#109365=CARTESIAN_POINT('Ctrl Pts',(54.7280970630346,48.5195292675955,12.));
#109366=CARTESIAN_POINT('Ctrl Pts',(54.7395346032451,48.5428847722975,0.));
#109367=CARTESIAN_POINT('Ctrl Pts',(54.7395346032451,48.5428847722975,12.));
#109368=CARTESIAN_POINT('Ctrl Pts',(54.7509670150716,48.5662851536027,0.));
#109369=CARTESIAN_POINT('Ctrl Pts',(54.7509670150716,48.5662851536027,12.));
#109370=CARTESIAN_POINT('Ctrl Pts',(54.7623942093591,48.5897303461131,0.));
#109371=CARTESIAN_POINT('Ctrl Pts',(54.7623942093591,48.5897303461131,12.));
#109372=CARTESIAN_POINT('Ctrl Pts',(54.773816097304,48.6132202845792,0.));
#109373=CARTESIAN_POINT('Ctrl Pts',(54.773816097304,48.6132202845792,12.));
#109374=CARTESIAN_POINT('Ctrl Pts',(54.7852325904591,48.6367549039121,0.));
#109375=CARTESIAN_POINT('Ctrl Pts',(54.7852325904591,48.6367549039121,12.));
#109376=CARTESIAN_POINT('Ctrl Pts',(54.7966436007395,48.6603341391891,0.));
#109377=CARTESIAN_POINT('Ctrl Pts',(54.7966436007395,48.6603341391891,12.));
#109378=CARTESIAN_POINT('Ctrl Pts',(54.8080490404274,48.6839579256565,0.));
#109379=CARTESIAN_POINT('Ctrl Pts',(54.8080490404274,48.6839579256565,12.));
#109380=CARTESIAN_POINT('Ctrl Pts',(54.8194488221803,48.7076261987284,0.));
#109381=CARTESIAN_POINT('Ctrl Pts',(54.8194488221803,48.7076261987284,12.));
#109382=CARTESIAN_POINT('Ctrl Pts',(54.8308428590334,48.7313388939834,0.));
#109383=CARTESIAN_POINT('Ctrl Pts',(54.8308428590334,48.7313388939834,12.));
#109384=CARTESIAN_POINT('Ctrl Pts',(54.8422310643752,48.755095947159,0.));
#109385=CARTESIAN_POINT('Ctrl Pts',(54.8422310643752,48.755095947159,12.));
#109386=CARTESIAN_POINT('Ctrl Pts',(54.8536133519285,48.7788972941431,0.));
#109387=CARTESIAN_POINT('Ctrl Pts',(54.8536133519285,48.7788972941431,12.));
#109388=CARTESIAN_POINT('Ctrl Pts',(54.8649896357284,48.8027428709613,0.));
#109389=CARTESIAN_POINT('Ctrl Pts',(54.8649896357284,48.8027428709613,12.));
#109390=CARTESIAN_POINT('Ctrl Pts',(54.8763598301045,48.8266326137629,0.));
#109391=CARTESIAN_POINT('Ctrl Pts',(54.8763598301045,48.8266326137629,12.));
#109392=CARTESIAN_POINT('Ctrl Pts',(54.8877238496577,48.8505664587985,0.));
#109393=CARTESIAN_POINT('Ctrl Pts',(54.8877238496577,48.8505664587985,12.));
#109394=CARTESIAN_POINT('Ctrl Pts',(54.8990816092964,48.8745443424488,0.));
#109395=CARTESIAN_POINT('Ctrl Pts',(54.8990816092964,48.8745443424488,12.));
#109396=CARTESIAN_POINT('Ctrl Pts',(54.910433024275,48.8985662012535,0.));
#109397=CARTESIAN_POINT('Ctrl Pts',(54.910433024275,48.8985662012535,12.));
#109398=CARTESIAN_POINT('Ctrl Pts',(54.9217780102357,48.922631971937,0.));
#109399=CARTESIAN_POINT('Ctrl Pts',(54.9217780102357,48.922631971937,12.));
#109400=CARTESIAN_POINT('Ctrl Pts',(54.933116483242,48.9467415914266,0.));
#109401=CARTESIAN_POINT('Ctrl Pts',(54.933116483242,48.9467415914266,12.));
#109402=CARTESIAN_POINT('Ctrl Pts',(54.9444483598372,48.9708949968789,0.));
#109403=CARTESIAN_POINT('Ctrl Pts',(54.9444483598372,48.9708949968789,12.));
#109404=CARTESIAN_POINT('Ctrl Pts',(54.9557735569936,48.995092125652,0.));
#109405=CARTESIAN_POINT('Ctrl Pts',(54.9557735569936,48.995092125652,12.));
#109406=CARTESIAN_POINT('Ctrl Pts',(54.9670919920024,49.0193329152475,0.));
#109407=CARTESIAN_POINT('Ctrl Pts',(54.9670919920024,49.0193329152475,12.));
#109408=CARTESIAN_POINT('Ctrl Pts',(54.9784035823764,49.0436173032527,0.));
#109409=CARTESIAN_POINT('Ctrl Pts',(54.9784035823764,49.0436173032527,12.));
#109410=CARTESIAN_POINT('Ctrl Pts',(54.9897082457606,49.0679452272871,0.));
#109411=CARTESIAN_POINT('Ctrl Pts',(54.9897082457606,49.0679452272871,12.));
#109412=CARTESIAN_POINT('Ctrl Pts',(55.0010058998111,49.0923166249222,0.));
#109413=CARTESIAN_POINT('Ctrl Pts',(55.0010058998111,49.0923166249222,12.));
#109414=CARTESIAN_POINT('Ctrl Pts',(55.0122964621868,49.1167314336737,0.));
#109415=CARTESIAN_POINT('Ctrl Pts',(55.0122964621868,49.1167314336737,12.));
#109416=CARTESIAN_POINT('Ctrl Pts',(55.0235798508056,49.1411895911646,0.));
#109417=CARTESIAN_POINT('Ctrl Pts',(55.0235798508056,49.1411895911646,12.));
#109418=CARTESIAN_POINT('Ctrl Pts',(55.0348559840462,49.1656910352484,0.));
#109419=CARTESIAN_POINT('Ctrl Pts',(55.0348559840462,49.1656910352484,12.));
#109420=CARTESIAN_POINT('Ctrl Pts',(55.0461247809745,49.1902357041462,0.));
#109421=CARTESIAN_POINT('Ctrl Pts',(55.0461247809745,49.1902357041462,12.));
#109422=CARTESIAN_POINT('Ctrl Pts',(55.0573861615569,49.2148235365694,0.));
#109423=CARTESIAN_POINT('Ctrl Pts',(55.0573861615569,49.2148235365694,12.));
#109424=CARTESIAN_POINT('Ctrl Pts',(55.0686400468911,49.2394544718513,0.));
#109425=CARTESIAN_POINT('Ctrl Pts',(55.0686400468911,49.2394544718513,12.));
#109426=CARTESIAN_POINT('Ctrl Pts',(55.0798863586986,49.2641284496496,0.));
#109427=CARTESIAN_POINT('Ctrl Pts',(55.0798863586986,49.2641284496496,12.));
#109428=CARTESIAN_POINT('Ctrl Pts',(55.0911250188282,49.2888454096544,0.));
#109429=CARTESIAN_POINT('Ctrl Pts',(55.0911250188282,49.2888454096544,12.));
#109430=CARTESIAN_POINT('Ctrl Pts',(55.1023559487133,49.3136052912614,0.));
#109431=CARTESIAN_POINT('Ctrl Pts',(55.1023559487133,49.3136052912614,12.));
#109432=CARTESIAN_POINT('Ctrl Pts',(55.1135790689475,49.3384080333166,0.));
#109433=CARTESIAN_POINT('Ctrl Pts',(55.1135790689475,49.3384080333166,12.));
#109434=CARTESIAN_POINT('Ctrl Pts',(55.1247942985649,49.3632535736744,0.));
#109435=CARTESIAN_POINT('Ctrl Pts',(55.1247942985649,49.3632535736744,12.));
#109436=CARTESIAN_POINT('Ctrl Pts',(55.1360015556262,49.3881418495529,0.));
#109437=CARTESIAN_POINT('Ctrl Pts',(55.1360015556262,49.3881418495529,12.));
#109438=CARTESIAN_POINT('Ctrl Pts',(55.1472007585224,49.413072798324,0.));
#109439=CARTESIAN_POINT('Ctrl Pts',(55.1472007585224,49.413072798324,12.));
#109440=CARTESIAN_POINT('Ctrl Pts',(55.158391827114,49.4380463581989,0.));
#109441=CARTESIAN_POINT('Ctrl Pts',(55.158391827114,49.4380463581989,12.));
#109442=CARTESIAN_POINT('Ctrl Pts',(55.1695746838168,49.4630624688787,0.));
#109443=CARTESIAN_POINT('Ctrl Pts',(55.1695746838168,49.4630624688787,12.));
#109444=CARTESIAN_POINT('Ctrl Pts',(55.1807492550073,49.4881210723921,0.));
#109445=CARTESIAN_POINT('Ctrl Pts',(55.1807492550073,49.4881210723921,12.));
#109446=CARTESIAN_POINT('Ctrl Pts',(55.1919154713569,49.5132221132916,0.));
#109447=CARTESIAN_POINT('Ctrl Pts',(55.1919154713569,49.5132221132916,12.));
#109448=CARTESIAN_POINT('Ctrl Pts',(55.2030732647222,49.5383655367987,0.));
#109449=CARTESIAN_POINT('Ctrl Pts',(55.2030732647222,49.5383655367987,12.));
#109450=CARTESIAN_POINT('Ctrl Pts',(55.2142225656943,49.5635512873368,0.));
#109451=CARTESIAN_POINT('Ctrl Pts',(55.2142225656943,49.5635512873368,12.));
#109452=CARTESIAN_POINT('Ctrl Pts',(55.225363300765,49.5887793068337,0.));
#109453=CARTESIAN_POINT('Ctrl Pts',(55.225363300765,49.5887793068337,12.));
#109454=CARTESIAN_POINT('Ctrl Pts',(55.2364953899423,49.6140495332865,0.));
#109455=CARTESIAN_POINT('Ctrl Pts',(55.2364953899423,49.6140495332865,12.));
#109456=CARTESIAN_POINT('Ctrl Pts',(55.2476187434204,49.6393618987614,0.));
#109457=CARTESIAN_POINT('Ctrl Pts',(55.2476187434204,49.6393618987614,12.));
#109458=CARTESIAN_POINT('Ctrl Pts',(55.2587332663982,49.6647163322457,0.));
#109459=CARTESIAN_POINT('Ctrl Pts',(55.2587332663982,49.6647163322457,12.));
#109460=CARTESIAN_POINT('Ctrl Pts',(55.2698388650215,49.690112763181,0.));
#109461=CARTESIAN_POINT('Ctrl Pts',(55.2698388650215,49.690112763181,12.));
#109462=CARTESIAN_POINT('Ctrl Pts',(55.2809354521616,49.7155511248629,0.));
#109463=CARTESIAN_POINT('Ctrl Pts',(55.2809354521616,49.7155511248629,12.));
#109464=CARTESIAN_POINT('Ctrl Pts',(55.292022952748,49.7410313576444,0.));
#109465=CARTESIAN_POINT('Ctrl Pts',(55.292022952748,49.7410313576444,12.));
#109466=CARTESIAN_POINT('Ctrl Pts',(55.3031013105578,49.7665534128269,0.));
#109467=CARTESIAN_POINT('Ctrl Pts',(55.3031013105578,49.7665534128269,12.));
#109468=CARTESIAN_POINT('Ctrl Pts',(55.3141704897307,49.7921172540185,0.));
#109469=CARTESIAN_POINT('Ctrl Pts',(55.3141704897307,49.7921172540185,12.));
#109470=CARTESIAN_POINT('Ctrl Pts',(55.3252304694066,49.817722855186,0.));
#109471=CARTESIAN_POINT('Ctrl Pts',(55.3252304694066,49.817722855186,12.));
#109472=CARTESIAN_POINT('Ctrl Pts',(55.3340710859607,49.8382407306675,0.));
#109473=CARTESIAN_POINT('Ctrl Pts',(55.3340710859607,49.8382407306675,12.));
#109474=CARTESIAN_POINT('Ctrl Pts',(55.340697403233,49.8536479176573,0.));
#109475=CARTESIAN_POINT('Ctrl Pts',(55.340697403233,49.8536479176573,12.));
#109476=CARTESIAN_POINT('Ctrl Pts',(55.3451131058727,49.8639277221471,0.));
#109477=CARTESIAN_POINT('Ctrl Pts',(55.3451131058727,49.8639277221471,12.));
#109478=CARTESIAN_POINT('Ctrl Pts',(55.3473204966403,49.8690697110161,0.));
#109479=CARTESIAN_POINT('Ctrl Pts',(55.3473204966403,49.8690697110161,12.));
#109480=CARTESIAN_POINT('',(53.0702932034641,45.6458539113724,0.));
#109481=CARTESIAN_POINT('Ctrl Pts',(53.0702932034641,45.6458539113724,0.));
#109482=CARTESIAN_POINT('Ctrl Pts',(53.0724894921849,45.6490568514089,0.));
#109483=CARTESIAN_POINT('Ctrl Pts',(53.0768833804193,45.6554684028145,0.));
#109484=CARTESIAN_POINT('Ctrl Pts',(53.0834781451546,45.6651027439241,0.));
#109485=CARTESIAN_POINT('Ctrl Pts',(53.0922790298409,45.6779825614231,0.));
#109486=CARTESIAN_POINT('Ctrl Pts',(53.1032932328857,45.694139048907,0.));
#109487=CARTESIAN_POINT('Ctrl Pts',(53.114320495492,45.7103522376696,0.));
#109488=CARTESIAN_POINT('Ctrl Pts',(53.1253607414872,45.7266220897003,0.));
#109489=CARTESIAN_POINT('Ctrl Pts',(53.1364138384693,45.7429485300823,0.));
#109490=CARTESIAN_POINT('Ctrl Pts',(53.1474795996053,45.7593314474501,0.));
#109491=CARTESIAN_POINT('Ctrl Pts',(53.1585578076444,45.7757707100618,0.));
#109492=CARTESIAN_POINT('Ctrl Pts',(53.1696482334487,45.7922661780005,0.));
#109493=CARTESIAN_POINT('Ctrl Pts',(53.1807506560933,45.808817716509,0.));
#109494=CARTESIAN_POINT('Ctrl Pts',(53.1918648840541,45.8254252099957,0.));
#109495=CARTESIAN_POINT('Ctrl Pts',(53.2029907483557,45.8420885575349,0.));
#109496=CARTESIAN_POINT('Ctrl Pts',(53.2141280925439,45.8588076662582,0.));
#109497=CARTESIAN_POINT('Ctrl Pts',(53.2252767643662,45.8755824458723,0.));
#109498=CARTESIAN_POINT('Ctrl Pts',(53.2364366054306,45.892412801838,0.));
#109499=CARTESIAN_POINT('Ctrl Pts',(53.2476074460017,45.9092986319377,0.));
#109500=CARTESIAN_POINT('Ctrl Pts',(53.2587891103866,45.9262398298349,0.));
#109501=CARTESIAN_POINT('Ctrl Pts',(53.2699814203105,45.9432362873008,0.));
#109502=CARTESIAN_POINT('Ctrl Pts',(53.2811841987926,45.9602878967698,0.));
#109503=CARTESIAN_POINT('Ctrl Pts',(53.292397274555,45.9773945542384,0.));
#109504=CARTESIAN_POINT('Ctrl Pts',(53.3036204818329,45.9945561591453,0.));
#109505=CARTESIAN_POINT('Ctrl Pts',(53.3148536582635,46.0117726129873,0.));
#109506=CARTESIAN_POINT('Ctrl Pts',(53.326096643428,46.02904381836,0.));
#109507=CARTESIAN_POINT('Ctrl Pts',(53.3373492770671,46.0463696777801,0.));
#109508=CARTESIAN_POINT('Ctrl Pts',(53.3486113975901,46.0637500926982,0.));
#109509=CARTESIAN_POINT('Ctrl Pts',(53.3598828428546,46.0811849640218,0.));
#109510=CARTESIAN_POINT('Ctrl Pts',(53.3711634508437,46.0986741925656,0.));
#109511=CARTESIAN_POINT('Ctrl Pts',(53.3824530603276,46.1162176794884,0.));
#109512=CARTESIAN_POINT('Ctrl Pts',(53.3937515116549,46.1338153268097,0.));
#109513=CARTESIAN_POINT('Ctrl Pts',(53.4050586470436,46.1514670376012,0.));
#109514=CARTESIAN_POINT('Ctrl Pts',(53.4163743101517,46.1691727157134,0.));
#109515=CARTESIAN_POINT('Ctrl Pts',(53.4276983458125,46.1869322656024,0.));
#109516=CARTESIAN_POINT('Ctrl Pts',(53.4390305997274,46.2047455921286,0.));
#109517=CARTESIAN_POINT('Ctrl Pts',(53.4503709181178,46.2226126003202,0.));
#109518=CARTESIAN_POINT('Ctrl Pts',(53.4617191477402,46.2405331953889,0.));
#109519=CARTESIAN_POINT('Ctrl Pts',(53.4730751360371,46.2585072828353,0.));
#109520=CARTESIAN_POINT('Ctrl Pts',(53.4844387312414,46.2765347685198,0.));
#109521=CARTESIAN_POINT('Ctrl Pts',(53.4958097825006,46.2946155587417,0.));
#109522=CARTESIAN_POINT('Ctrl Pts',(53.5071881399911,46.3127495603098,0.));
#109523=CARTESIAN_POINT('Ctrl Pts',(53.5185736548548,46.3309366805093,0.));
#109524=CARTESIAN_POINT('Ctrl Pts',(53.5299661791385,46.3491768270655,0.));
#109525=CARTESIAN_POINT('Ctrl Pts',(53.5413655657327,46.3674699081046,0.));
#109526=CARTESIAN_POINT('Ctrl Pts',(53.5527716683048,46.3858158321059,0.));
#109527=CARTESIAN_POINT('Ctrl Pts',(53.5641843412559,46.4042145078701,0.));
#109528=CARTESIAN_POINT('Ctrl Pts',(53.5756034397481,46.4226658445474,0.));
#109529=CARTESIAN_POINT('Ctrl Pts',(53.5870288197166,46.4411697516478,0.));
#109530=CARTESIAN_POINT('Ctrl Pts',(53.5984603378855,46.459726139052,0.));
#109531=CARTESIAN_POINT('Ctrl Pts',(53.6098978517859,46.4783349170173,0.));
#109532=CARTESIAN_POINT('Ctrl Pts',(53.6213412197533,46.496995996177,0.));
#109533=CARTESIAN_POINT('Ctrl Pts',(53.6327903009094,46.5157092875373,0.));
#109534=CARTESIAN_POINT('Ctrl Pts',(53.6442449551455,46.5344747024676,0.));
#109535=CARTESIAN_POINT('Ctrl Pts',(53.6557050431071,46.5532921526901,0.));
#109536=CARTESIAN_POINT('Ctrl Pts',(53.6671704261737,46.5721615502591,0.));
#109537=CARTESIAN_POINT('Ctrl Pts',(53.678640966456,46.5910828075653,0.));
#109538=CARTESIAN_POINT('Ctrl Pts',(53.6901165267941,46.6100558373402,0.));
#109539=CARTESIAN_POINT('Ctrl Pts',(53.701596970754,46.6290805526559,0.));
#109540=CARTESIAN_POINT('Ctrl Pts',(53.7130821626263,46.6481568669216,0.));
#109541=CARTESIAN_POINT('Ctrl Pts',(53.7245719674222,46.6672846938752,0.));
#109542=CARTESIAN_POINT('Ctrl Pts',(53.7360662508677,46.6864639475863,0.));
#109543=CARTESIAN_POINT('Ctrl Pts',(53.7475648793948,46.7056945424559,0.));
#109544=CARTESIAN_POINT('Ctrl Pts',(53.7590677201344,46.724976393213,0.));
#109545=CARTESIAN_POINT('Ctrl Pts',(53.770574640907,46.7443094149041,0.));
#109546=CARTESIAN_POINT('Ctrl Pts',(53.782085510217,46.7636935228851,0.));
#109547=CARTESIAN_POINT('Ctrl Pts',(53.7936001972468,46.7831286328268,0.));
#109548=CARTESIAN_POINT('Ctrl Pts',(53.8051185718525,46.8026146607144,0.));
#109549=CARTESIAN_POINT('Ctrl Pts',(53.8166405045582,46.8221515228459,0.));
#109550=CARTESIAN_POINT('Ctrl Pts',(53.8281658665517,46.8417391358231,0.));
#109551=CARTESIAN_POINT('Ctrl Pts',(53.8396945296777,46.8613774165452,0.));
#109552=CARTESIAN_POINT('Ctrl Pts',(53.851226366434,46.8810662822147,0.));
#109553=CARTESIAN_POINT('Ctrl Pts',(53.8627612499648,46.900805650336,0.));
#109554=CARTESIAN_POINT('Ctrl Pts',(53.8742990540557,46.9205954387128,0.));
#109555=CARTESIAN_POINT('Ctrl Pts',(53.8858396531277,46.9404355654381,0.));
#109556=CARTESIAN_POINT('Ctrl Pts',(53.8973829222317,46.9603259488894,0.));
#109557=CARTESIAN_POINT('Ctrl Pts',(53.9089287370436,46.9802665077342,0.));
#109558=CARTESIAN_POINT('Ctrl Pts',(53.9204769738584,47.0002571609286,0.));
#109559=CARTESIAN_POINT('Ctrl Pts',(53.9320275095864,47.0202978277148,0.));
#109560=CARTESIAN_POINT('Ctrl Pts',(53.9435802217468,47.04038842761,0.));
#109561=CARTESIAN_POINT('Ctrl Pts',(53.9551349884637,47.0605288804042,0.));
#109562=CARTESIAN_POINT('Ctrl Pts',(53.9666916884624,47.0807191061674,0.));
#109563=CARTESIAN_POINT('Ctrl Pts',(53.9782502010642,47.1009590252466,0.));
#109564=CARTESIAN_POINT('Ctrl Pts',(53.9898104061809,47.1212485582632,0.));
#109565=CARTESIAN_POINT('Ctrl Pts',(54.0013721843094,47.1415876261012,0.));
#109566=CARTESIAN_POINT('Ctrl Pts',(54.0129354165269,47.161976149906,0.));
#109567=CARTESIAN_POINT('Ctrl Pts',(54.0244999844872,47.1824140510906,0.));
#109568=CARTESIAN_POINT('Ctrl Pts',(54.0360657704156,47.2029012513334,0.));
#109569=CARTESIAN_POINT('Ctrl Pts',(54.047632657105,47.2234376725752,0.));
#109570=CARTESIAN_POINT('Ctrl Pts',(54.0592005279108,47.2440232370085,0.));
#109571=CARTESIAN_POINT('Ctrl Pts',(54.0707692667461,47.2646578670767,0.));
#109572=CARTESIAN_POINT('Ctrl Pts',(54.082338758079,47.2853414854805,0.));
#109573=CARTESIAN_POINT('Ctrl Pts',(54.0939088869271,47.3060740151754,0.));
#109574=CARTESIAN_POINT('Ctrl Pts',(54.1054795388538,47.326855379369,0.));
#109575=CARTESIAN_POINT('Ctrl Pts',(54.1170505999637,47.3476855015095,0.));
#109576=CARTESIAN_POINT('Ctrl Pts',(54.1286219568981,47.3685643052867,0.));
#109577=CARTESIAN_POINT('Ctrl Pts',(54.1401934968306,47.3894917146361,0.));
#109578=CARTESIAN_POINT('Ctrl Pts',(54.1517651074638,47.4104676537381,0.));
#109579=CARTESIAN_POINT('Ctrl Pts',(54.163336677024,47.4314920470142,0.));
#109580=CARTESIAN_POINT('Ctrl Pts',(54.1749080942593,47.4525648191173,0.));
#109581=CARTESIAN_POINT('Ctrl Pts',(54.1864792484343,47.473685894932,0.));
#109582=CARTESIAN_POINT('Ctrl Pts',(54.1980500293267,47.4948551995799,0.));
#109583=CARTESIAN_POINT('Ctrl Pts',(54.2096203272228,47.5160726584172,0.));
#109584=CARTESIAN_POINT('Ctrl Pts',(54.2211900329141,47.5373381970328,0.));
#109585=CARTESIAN_POINT('Ctrl Pts',(54.232759037693,47.5586517412368,0.));
#109586=CARTESIAN_POINT('Ctrl Pts',(54.2443272333498,47.5800132170614,0.));
#109587=CARTESIAN_POINT('Ctrl Pts',(54.2558945121684,47.6014225507664,0.));
#109588=CARTESIAN_POINT('Ctrl Pts',(54.2674607669228,47.6228796688376,0.));
#109589=CARTESIAN_POINT('Ctrl Pts',(54.2790258908736,47.6443844979846,0.));
#109590=CARTESIAN_POINT('Ctrl Pts',(54.2905897777647,47.6659369651299,0.));
#109591=CARTESIAN_POINT('Ctrl Pts',(54.3021523218188,47.6875369974086,0.));
#109592=CARTESIAN_POINT('Ctrl Pts',(54.3137134177345,47.7091845221748,0.));
#109593=CARTESIAN_POINT('Ctrl Pts',(54.3252729606824,47.7308794669994,0.));
#109594=CARTESIAN_POINT('Ctrl Pts',(54.3368308463023,47.7526217596694,0.));
#109595=CARTESIAN_POINT('Ctrl Pts',(54.3483869706998,47.7744113281768,0.));
#109596=CARTESIAN_POINT('Ctrl Pts',(54.3599412304431,47.7962481007179,0.));
#109597=CARTESIAN_POINT('Ctrl Pts',(54.3714935225585,47.8181320056988,0.));
#109598=CARTESIAN_POINT('Ctrl Pts',(54.3830437445275,47.8400629717352,0.));
#109599=CARTESIAN_POINT('Ctrl Pts',(54.3945917942835,47.8620409276495,0.));
#109600=CARTESIAN_POINT('Ctrl Pts',(54.4061375702088,47.8840658024626,0.));
#109601=CARTESIAN_POINT('Ctrl Pts',(54.4176809711324,47.9061375253909,0.));
#109602=CARTESIAN_POINT('Ctrl Pts',(54.4292218963253,47.9282560258528,0.));
#109603=CARTESIAN_POINT('Ctrl Pts',(54.4407602454974,47.9504212334681,0.));
#109604=CARTESIAN_POINT('Ctrl Pts',(54.4522959187952,47.972633078057,0.));
#109605=CARTESIAN_POINT('Ctrl Pts',(54.4638288167991,47.9948914896316,0.));
#109606=CARTESIAN_POINT('Ctrl Pts',(54.4753588405202,48.0171963983912,0.));
#109607=CARTESIAN_POINT('Ctrl Pts',(54.4868858913961,48.039547734729,0.));
#109608=CARTESIAN_POINT('Ctrl Pts',(54.4984098712883,48.0619454292321,0.));
#109609=CARTESIAN_POINT('Ctrl Pts',(54.5099306824788,48.0843894126807,0.));
#109610=CARTESIAN_POINT('Ctrl Pts',(54.5214482276679,48.1068796160406,0.));
#109611=CARTESIAN_POINT('Ctrl Pts',(54.5329624099719,48.1294159704571,0.));
#109612=CARTESIAN_POINT('Ctrl Pts',(54.5444731329196,48.1519984072617,0.));
#109613=CARTESIAN_POINT('Ctrl Pts',(54.5559803004487,48.1746268579732,0.));
#109614=CARTESIAN_POINT('Ctrl Pts',(54.5674838169041,48.1973012542966,0.));
#109615=CARTESIAN_POINT('Ctrl Pts',(54.5789835870348,48.2200215281178,0.));
#109616=CARTESIAN_POINT('Ctrl Pts',(54.5904795159936,48.2427876114956,0.));
#109617=CARTESIAN_POINT('Ctrl Pts',(54.6019715093319,48.2655994366672,0.));
#109618=CARTESIAN_POINT('Ctrl Pts',(54.6134594729964,48.288456936051,0.));
#109619=CARTESIAN_POINT('Ctrl Pts',(54.6249433133262,48.3113600422443,0.));
#109620=CARTESIAN_POINT('Ctrl Pts',(54.636422937049,48.3343086880192,0.));
#109621=CARTESIAN_POINT('Ctrl Pts',(54.647898251279,48.3573028063122,0.));
#109622=CARTESIAN_POINT('Ctrl Pts',(54.6593691635143,48.3803423302294,0.));
#109623=CARTESIAN_POINT('Ctrl Pts',(54.6708355816359,48.4034271930516,0.));
#109624=CARTESIAN_POINT('Ctrl Pts',(54.6822974139065,48.4265573282342,0.));
#109625=CARTESIAN_POINT('Ctrl Pts',(54.6937545689694,48.4497326694051,0.));
#109626=CARTESIAN_POINT('Ctrl Pts',(54.7052069558493,48.4729531503565,0.));
#109627=CARTESIAN_POINT('Ctrl Pts',(54.7166544839475,48.4962187050452,0.));
#109628=CARTESIAN_POINT('Ctrl Pts',(54.7280970630346,48.5195292675955,0.));
#109629=CARTESIAN_POINT('Ctrl Pts',(54.7395346032451,48.5428847722975,0.));
#109630=CARTESIAN_POINT('Ctrl Pts',(54.7509670150716,48.5662851536027,0.));
#109631=CARTESIAN_POINT('Ctrl Pts',(54.7623942093591,48.5897303461131,0.));
#109632=CARTESIAN_POINT('Ctrl Pts',(54.773816097304,48.6132202845792,0.));
#109633=CARTESIAN_POINT('Ctrl Pts',(54.7852325904591,48.6367549039121,0.));
#109634=CARTESIAN_POINT('Ctrl Pts',(54.7966436007395,48.6603341391891,0.));
#109635=CARTESIAN_POINT('Ctrl Pts',(54.8080490404274,48.6839579256565,0.));
#109636=CARTESIAN_POINT('Ctrl Pts',(54.8194488221803,48.7076261987284,0.));
#109637=CARTESIAN_POINT('Ctrl Pts',(54.8308428590334,48.7313388939834,0.));
#109638=CARTESIAN_POINT('Ctrl Pts',(54.8422310643752,48.755095947159,0.));
#109639=CARTESIAN_POINT('Ctrl Pts',(54.8536133519285,48.7788972941431,0.));
#109640=CARTESIAN_POINT('Ctrl Pts',(54.8649896357284,48.8027428709613,0.));
#109641=CARTESIAN_POINT('Ctrl Pts',(54.8763598301045,48.8266326137629,0.));
#109642=CARTESIAN_POINT('Ctrl Pts',(54.8877238496577,48.8505664587985,0.));
#109643=CARTESIAN_POINT('Ctrl Pts',(54.8990816092964,48.8745443424488,0.));
#109644=CARTESIAN_POINT('Ctrl Pts',(54.910433024275,48.8985662012535,0.));
#109645=CARTESIAN_POINT('Ctrl Pts',(54.9217780102357,48.922631971937,0.));
#109646=CARTESIAN_POINT('Ctrl Pts',(54.933116483242,48.9467415914266,0.));
#109647=CARTESIAN_POINT('Ctrl Pts',(54.9444483598372,48.9708949968789,0.));
#109648=CARTESIAN_POINT('Ctrl Pts',(54.9557735569936,48.995092125652,0.));
#109649=CARTESIAN_POINT('Ctrl Pts',(54.9670919920024,49.0193329152475,0.));
#109650=CARTESIAN_POINT('Ctrl Pts',(54.9784035823764,49.0436173032527,0.));
#109651=CARTESIAN_POINT('Ctrl Pts',(54.9897082457606,49.0679452272871,0.));
#109652=CARTESIAN_POINT('Ctrl Pts',(55.0010058998111,49.0923166249222,0.));
#109653=CARTESIAN_POINT('Ctrl Pts',(55.0122964621868,49.1167314336737,0.));
#109654=CARTESIAN_POINT('Ctrl Pts',(55.0235798508056,49.1411895911646,0.));
#109655=CARTESIAN_POINT('Ctrl Pts',(55.0348559840462,49.1656910352484,0.));
#109656=CARTESIAN_POINT('Ctrl Pts',(55.0461247809745,49.1902357041462,0.));
#109657=CARTESIAN_POINT('Ctrl Pts',(55.0573861615569,49.2148235365694,0.));
#109658=CARTESIAN_POINT('Ctrl Pts',(55.0686400468911,49.2394544718513,0.));
#109659=CARTESIAN_POINT('Ctrl Pts',(55.0798863586986,49.2641284496496,0.));
#109660=CARTESIAN_POINT('Ctrl Pts',(55.0911250188282,49.2888454096544,0.));
#109661=CARTESIAN_POINT('Ctrl Pts',(55.1023559487133,49.3136052912614,0.));
#109662=CARTESIAN_POINT('Ctrl Pts',(55.1135790689475,49.3384080333166,0.));
#109663=CARTESIAN_POINT('Ctrl Pts',(55.1247942985649,49.3632535736744,0.));
#109664=CARTESIAN_POINT('Ctrl Pts',(55.1360015556262,49.3881418495529,0.));
#109665=CARTESIAN_POINT('Ctrl Pts',(55.1472007585224,49.413072798324,0.));
#109666=CARTESIAN_POINT('Ctrl Pts',(55.158391827114,49.4380463581989,0.));
#109667=CARTESIAN_POINT('Ctrl Pts',(55.1695746838168,49.4630624688787,0.));
#109668=CARTESIAN_POINT('Ctrl Pts',(55.1807492550073,49.4881210723921,0.));
#109669=CARTESIAN_POINT('Ctrl Pts',(55.1919154713569,49.5132221132916,0.));
#109670=CARTESIAN_POINT('Ctrl Pts',(55.2014798623975,49.5347748994607,0.));
#109671=CARTESIAN_POINT('Ctrl Pts',(55.2088081098955,49.5513218524279,0.));
#109672=CARTESIAN_POINT('Ctrl Pts',(55.2139039604569,49.5628442141869,0.));
#109673=CARTESIAN_POINT('Ctrl Pts',(55.2167699151168,49.5693295981608,0.));
#109674=CARTESIAN_POINT('Ctrl Pts',(55.2174072001297,49.5707719660254,0.));
#109675=CARTESIAN_POINT('',(53.0702932034641,45.6458539113724,12.));
#109676=CARTESIAN_POINT('',(53.0702932034641,45.6458539113724,0.));
#109677=CARTESIAN_POINT('Ctrl Pts',(55.2174072001297,49.5707719660254,12.));
#109678=CARTESIAN_POINT('Ctrl Pts',(55.2167699151168,49.5693295981608,12.));
#109679=CARTESIAN_POINT('Ctrl Pts',(55.2139039604569,49.5628442141869,12.));
#109680=CARTESIAN_POINT('Ctrl Pts',(55.2088081098955,49.5513218524279,12.));
#109681=CARTESIAN_POINT('Ctrl Pts',(55.2014798623975,49.5347748994607,12.));
#109682=CARTESIAN_POINT('Ctrl Pts',(55.1919154713569,49.5132221132916,12.));
#109683=CARTESIAN_POINT('Ctrl Pts',(55.1807492550073,49.4881210723921,12.));
#109684=CARTESIAN_POINT('Ctrl Pts',(55.1695746838168,49.4630624688787,12.));
#109685=CARTESIAN_POINT('Ctrl Pts',(55.158391827114,49.4380463581989,12.));
#109686=CARTESIAN_POINT('Ctrl Pts',(55.1472007585224,49.413072798324,12.));
#109687=CARTESIAN_POINT('Ctrl Pts',(55.1360015556262,49.3881418495529,12.));
#109688=CARTESIAN_POINT('Ctrl Pts',(55.1247942985649,49.3632535736744,12.));
#109689=CARTESIAN_POINT('Ctrl Pts',(55.1135790689475,49.3384080333166,12.));
#109690=CARTESIAN_POINT('Ctrl Pts',(55.1023559487133,49.3136052912614,12.));
#109691=CARTESIAN_POINT('Ctrl Pts',(55.0911250188282,49.2888454096544,12.));
#109692=CARTESIAN_POINT('Ctrl Pts',(55.0798863586986,49.2641284496496,12.));
#109693=CARTESIAN_POINT('Ctrl Pts',(55.0686400468911,49.2394544718513,12.));
#109694=CARTESIAN_POINT('Ctrl Pts',(55.0573861615569,49.2148235365694,12.));
#109695=CARTESIAN_POINT('Ctrl Pts',(55.0461247809745,49.1902357041462,12.));
#109696=CARTESIAN_POINT('Ctrl Pts',(55.0348559840462,49.1656910352484,12.));
#109697=CARTESIAN_POINT('Ctrl Pts',(55.0235798508056,49.1411895911646,12.));
#109698=CARTESIAN_POINT('Ctrl Pts',(55.0122964621868,49.1167314336737,12.));
#109699=CARTESIAN_POINT('Ctrl Pts',(55.0010058998111,49.0923166249222,12.));
#109700=CARTESIAN_POINT('Ctrl Pts',(54.9897082457606,49.0679452272871,12.));
#109701=CARTESIAN_POINT('Ctrl Pts',(54.9784035823764,49.0436173032527,12.));
#109702=CARTESIAN_POINT('Ctrl Pts',(54.9670919920024,49.0193329152475,12.));
#109703=CARTESIAN_POINT('Ctrl Pts',(54.9557735569936,48.995092125652,12.));
#109704=CARTESIAN_POINT('Ctrl Pts',(54.9444483598372,48.9708949968789,12.));
#109705=CARTESIAN_POINT('Ctrl Pts',(54.933116483242,48.9467415914266,12.));
#109706=CARTESIAN_POINT('Ctrl Pts',(54.9217780102357,48.922631971937,12.));
#109707=CARTESIAN_POINT('Ctrl Pts',(54.910433024275,48.8985662012535,12.));
#109708=CARTESIAN_POINT('Ctrl Pts',(54.8990816092964,48.8745443424488,12.));
#109709=CARTESIAN_POINT('Ctrl Pts',(54.8877238496577,48.8505664587985,12.));
#109710=CARTESIAN_POINT('Ctrl Pts',(54.8763598301045,48.8266326137629,12.));
#109711=CARTESIAN_POINT('Ctrl Pts',(54.8649896357284,48.8027428709613,12.));
#109712=CARTESIAN_POINT('Ctrl Pts',(54.8536133519285,48.7788972941431,12.));
#109713=CARTESIAN_POINT('Ctrl Pts',(54.8422310643752,48.755095947159,12.));
#109714=CARTESIAN_POINT('Ctrl Pts',(54.8308428590334,48.7313388939834,12.));
#109715=CARTESIAN_POINT('Ctrl Pts',(54.8194488221803,48.7076261987284,12.));
#109716=CARTESIAN_POINT('Ctrl Pts',(54.8080490404274,48.6839579256565,12.));
#109717=CARTESIAN_POINT('Ctrl Pts',(54.7966436007395,48.6603341391891,12.));
#109718=CARTESIAN_POINT('Ctrl Pts',(54.7852325904591,48.6367549039121,12.));
#109719=CARTESIAN_POINT('Ctrl Pts',(54.773816097304,48.6132202845792,12.));
#109720=CARTESIAN_POINT('Ctrl Pts',(54.7623942093591,48.5897303461131,12.));
#109721=CARTESIAN_POINT('Ctrl Pts',(54.7509670150716,48.5662851536027,12.));
#109722=CARTESIAN_POINT('Ctrl Pts',(54.7395346032451,48.5428847722975,12.));
#109723=CARTESIAN_POINT('Ctrl Pts',(54.7280970630346,48.5195292675955,12.));
#109724=CARTESIAN_POINT('Ctrl Pts',(54.7166544839475,48.4962187050452,12.));
#109725=CARTESIAN_POINT('Ctrl Pts',(54.7052069558493,48.4729531503565,12.));
#109726=CARTESIAN_POINT('Ctrl Pts',(54.6937545689694,48.4497326694051,12.));
#109727=CARTESIAN_POINT('Ctrl Pts',(54.6822974139065,48.4265573282342,12.));
#109728=CARTESIAN_POINT('Ctrl Pts',(54.6708355816359,48.4034271930516,12.));
#109729=CARTESIAN_POINT('Ctrl Pts',(54.6593691635143,48.3803423302294,12.));
#109730=CARTESIAN_POINT('Ctrl Pts',(54.647898251279,48.3573028063122,12.));
#109731=CARTESIAN_POINT('Ctrl Pts',(54.636422937049,48.3343086880192,12.));
#109732=CARTESIAN_POINT('Ctrl Pts',(54.6249433133262,48.3113600422443,12.));
#109733=CARTESIAN_POINT('Ctrl Pts',(54.6134594729964,48.288456936051,12.));
#109734=CARTESIAN_POINT('Ctrl Pts',(54.6019715093319,48.2655994366672,12.));
#109735=CARTESIAN_POINT('Ctrl Pts',(54.5904795159936,48.2427876114956,12.));
#109736=CARTESIAN_POINT('Ctrl Pts',(54.5789835870348,48.2200215281178,12.));
#109737=CARTESIAN_POINT('Ctrl Pts',(54.5674838169041,48.1973012542966,12.));
#109738=CARTESIAN_POINT('Ctrl Pts',(54.5559803004487,48.1746268579732,12.));
#109739=CARTESIAN_POINT('Ctrl Pts',(54.5444731329196,48.1519984072617,12.));
#109740=CARTESIAN_POINT('Ctrl Pts',(54.5329624099719,48.1294159704571,12.));
#109741=CARTESIAN_POINT('Ctrl Pts',(54.5214482276679,48.1068796160406,12.));
#109742=CARTESIAN_POINT('Ctrl Pts',(54.5099306824788,48.0843894126807,12.));
#109743=CARTESIAN_POINT('Ctrl Pts',(54.4984098712883,48.0619454292321,12.));
#109744=CARTESIAN_POINT('Ctrl Pts',(54.4868858913961,48.039547734729,12.));
#109745=CARTESIAN_POINT('Ctrl Pts',(54.4753588405202,48.0171963983912,12.));
#109746=CARTESIAN_POINT('Ctrl Pts',(54.4638288167991,47.9948914896316,12.));
#109747=CARTESIAN_POINT('Ctrl Pts',(54.4522959187952,47.972633078057,12.));
#109748=CARTESIAN_POINT('Ctrl Pts',(54.4407602454974,47.9504212334681,12.));
#109749=CARTESIAN_POINT('Ctrl Pts',(54.4292218963253,47.9282560258528,12.));
#109750=CARTESIAN_POINT('Ctrl Pts',(54.4176809711324,47.9061375253909,12.));
#109751=CARTESIAN_POINT('Ctrl Pts',(54.4061375702088,47.8840658024626,12.));
#109752=CARTESIAN_POINT('Ctrl Pts',(54.3945917942835,47.8620409276495,12.));
#109753=CARTESIAN_POINT('Ctrl Pts',(54.3830437445275,47.8400629717352,12.));
#109754=CARTESIAN_POINT('Ctrl Pts',(54.3714935225585,47.8181320056988,12.));
#109755=CARTESIAN_POINT('Ctrl Pts',(54.3599412304431,47.7962481007179,12.));
#109756=CARTESIAN_POINT('Ctrl Pts',(54.3483869706998,47.7744113281768,12.));
#109757=CARTESIAN_POINT('Ctrl Pts',(54.3368308463023,47.7526217596694,12.));
#109758=CARTESIAN_POINT('Ctrl Pts',(54.3252729606824,47.7308794669994,12.));
#109759=CARTESIAN_POINT('Ctrl Pts',(54.3137134177345,47.7091845221748,12.));
#109760=CARTESIAN_POINT('Ctrl Pts',(54.3021523218188,47.6875369974086,12.));
#109761=CARTESIAN_POINT('Ctrl Pts',(54.2905897777647,47.6659369651299,12.));
#109762=CARTESIAN_POINT('Ctrl Pts',(54.2790258908736,47.6443844979846,12.));
#109763=CARTESIAN_POINT('Ctrl Pts',(54.2674607669228,47.6228796688376,12.));
#109764=CARTESIAN_POINT('Ctrl Pts',(54.2558945121684,47.6014225507664,12.));
#109765=CARTESIAN_POINT('Ctrl Pts',(54.2443272333498,47.5800132170614,12.));
#109766=CARTESIAN_POINT('Ctrl Pts',(54.232759037693,47.5586517412368,12.));
#109767=CARTESIAN_POINT('Ctrl Pts',(54.2211900329141,47.5373381970328,12.));
#109768=CARTESIAN_POINT('Ctrl Pts',(54.2096203272228,47.5160726584172,12.));
#109769=CARTESIAN_POINT('Ctrl Pts',(54.1980500293267,47.4948551995799,12.));
#109770=CARTESIAN_POINT('Ctrl Pts',(54.1864792484343,47.473685894932,12.));
#109771=CARTESIAN_POINT('Ctrl Pts',(54.1749080942593,47.4525648191173,12.));
#109772=CARTESIAN_POINT('Ctrl Pts',(54.163336677024,47.4314920470142,12.));
#109773=CARTESIAN_POINT('Ctrl Pts',(54.1517651074638,47.4104676537381,12.));
#109774=CARTESIAN_POINT('Ctrl Pts',(54.1401934968306,47.3894917146361,12.));
#109775=CARTESIAN_POINT('Ctrl Pts',(54.1286219568981,47.3685643052867,12.));
#109776=CARTESIAN_POINT('Ctrl Pts',(54.1170505999637,47.3476855015095,12.));
#109777=CARTESIAN_POINT('Ctrl Pts',(54.1054795388538,47.326855379369,12.));
#109778=CARTESIAN_POINT('Ctrl Pts',(54.0939088869271,47.3060740151754,12.));
#109779=CARTESIAN_POINT('Ctrl Pts',(54.082338758079,47.2853414854805,12.));
#109780=CARTESIAN_POINT('Ctrl Pts',(54.0707692667461,47.2646578670767,12.));
#109781=CARTESIAN_POINT('Ctrl Pts',(54.0592005279108,47.2440232370085,12.));
#109782=CARTESIAN_POINT('Ctrl Pts',(54.047632657105,47.2234376725752,12.));
#109783=CARTESIAN_POINT('Ctrl Pts',(54.0360657704156,47.2029012513334,12.));
#109784=CARTESIAN_POINT('Ctrl Pts',(54.0244999844872,47.1824140510906,12.));
#109785=CARTESIAN_POINT('Ctrl Pts',(54.0129354165269,47.161976149906,12.));
#109786=CARTESIAN_POINT('Ctrl Pts',(54.0013721843094,47.1415876261012,12.));
#109787=CARTESIAN_POINT('Ctrl Pts',(53.9898104061809,47.1212485582632,12.));
#109788=CARTESIAN_POINT('Ctrl Pts',(53.9782502010642,47.1009590252466,12.));
#109789=CARTESIAN_POINT('Ctrl Pts',(53.9666916884624,47.0807191061674,12.));
#109790=CARTESIAN_POINT('Ctrl Pts',(53.9551349884637,47.0605288804042,12.));
#109791=CARTESIAN_POINT('Ctrl Pts',(53.9435802217468,47.04038842761,12.));
#109792=CARTESIAN_POINT('Ctrl Pts',(53.9320275095864,47.0202978277148,12.));
#109793=CARTESIAN_POINT('Ctrl Pts',(53.9204769738584,47.0002571609286,12.));
#109794=CARTESIAN_POINT('Ctrl Pts',(53.9089287370436,46.9802665077342,12.));
#109795=CARTESIAN_POINT('Ctrl Pts',(53.8973829222317,46.9603259488894,12.));
#109796=CARTESIAN_POINT('Ctrl Pts',(53.8858396531277,46.9404355654381,12.));
#109797=CARTESIAN_POINT('Ctrl Pts',(53.8742990540557,46.9205954387128,12.));
#109798=CARTESIAN_POINT('Ctrl Pts',(53.8627612499648,46.900805650336,12.));
#109799=CARTESIAN_POINT('Ctrl Pts',(53.851226366434,46.8810662822147,12.));
#109800=CARTESIAN_POINT('Ctrl Pts',(53.8396945296777,46.8613774165452,12.));
#109801=CARTESIAN_POINT('Ctrl Pts',(53.8281658665517,46.8417391358231,12.));
#109802=CARTESIAN_POINT('Ctrl Pts',(53.8166405045582,46.8221515228459,12.));
#109803=CARTESIAN_POINT('Ctrl Pts',(53.8051185718525,46.8026146607144,12.));
#109804=CARTESIAN_POINT('Ctrl Pts',(53.7936001972468,46.7831286328268,12.));
#109805=CARTESIAN_POINT('Ctrl Pts',(53.782085510217,46.7636935228851,12.));
#109806=CARTESIAN_POINT('Ctrl Pts',(53.770574640907,46.7443094149041,12.));
#109807=CARTESIAN_POINT('Ctrl Pts',(53.7590677201344,46.724976393213,12.));
#109808=CARTESIAN_POINT('Ctrl Pts',(53.7475648793948,46.7056945424559,12.));
#109809=CARTESIAN_POINT('Ctrl Pts',(53.7360662508677,46.6864639475863,12.));
#109810=CARTESIAN_POINT('Ctrl Pts',(53.7245719674222,46.6672846938752,12.));
#109811=CARTESIAN_POINT('Ctrl Pts',(53.7130821626263,46.6481568669216,12.));
#109812=CARTESIAN_POINT('Ctrl Pts',(53.701596970754,46.6290805526559,12.));
#109813=CARTESIAN_POINT('Ctrl Pts',(53.6901165267941,46.6100558373402,12.));
#109814=CARTESIAN_POINT('Ctrl Pts',(53.678640966456,46.5910828075653,12.));
#109815=CARTESIAN_POINT('Ctrl Pts',(53.6671704261737,46.5721615502591,12.));
#109816=CARTESIAN_POINT('Ctrl Pts',(53.6557050431071,46.5532921526901,12.));
#109817=CARTESIAN_POINT('Ctrl Pts',(53.6442449551455,46.5344747024676,12.));
#109818=CARTESIAN_POINT('Ctrl Pts',(53.6327903009094,46.5157092875373,12.));
#109819=CARTESIAN_POINT('Ctrl Pts',(53.6213412197533,46.496995996177,12.));
#109820=CARTESIAN_POINT('Ctrl Pts',(53.6098978517859,46.4783349170173,12.));
#109821=CARTESIAN_POINT('Ctrl Pts',(53.5984603378855,46.459726139052,12.));
#109822=CARTESIAN_POINT('Ctrl Pts',(53.5870288197166,46.4411697516478,12.));
#109823=CARTESIAN_POINT('Ctrl Pts',(53.5756034397481,46.4226658445474,12.));
#109824=CARTESIAN_POINT('Ctrl Pts',(53.5641843412559,46.4042145078701,12.));
#109825=CARTESIAN_POINT('Ctrl Pts',(53.5527716683048,46.3858158321059,12.));
#109826=CARTESIAN_POINT('Ctrl Pts',(53.5413655657327,46.3674699081046,12.));
#109827=CARTESIAN_POINT('Ctrl Pts',(53.5299661791385,46.3491768270655,12.));
#109828=CARTESIAN_POINT('Ctrl Pts',(53.5185736548548,46.3309366805093,12.));
#109829=CARTESIAN_POINT('Ctrl Pts',(53.5071881399911,46.3127495603098,12.));
#109830=CARTESIAN_POINT('Ctrl Pts',(53.4958097825006,46.2946155587417,12.));
#109831=CARTESIAN_POINT('Ctrl Pts',(53.4844387312414,46.2765347685198,12.));
#109832=CARTESIAN_POINT('Ctrl Pts',(53.4730751360371,46.2585072828353,12.));
#109833=CARTESIAN_POINT('Ctrl Pts',(53.4617191477402,46.2405331953889,12.));
#109834=CARTESIAN_POINT('Ctrl Pts',(53.4503709181178,46.2226126003202,12.));
#109835=CARTESIAN_POINT('Ctrl Pts',(53.4390305997274,46.2047455921286,12.));
#109836=CARTESIAN_POINT('Ctrl Pts',(53.4276983458125,46.1869322656024,12.));
#109837=CARTESIAN_POINT('Ctrl Pts',(53.4163743101517,46.1691727157134,12.));
#109838=CARTESIAN_POINT('Ctrl Pts',(53.4050586470436,46.1514670376012,12.));
#109839=CARTESIAN_POINT('Ctrl Pts',(53.3937515116549,46.1338153268097,12.));
#109840=CARTESIAN_POINT('Ctrl Pts',(53.3824530603276,46.1162176794884,12.));
#109841=CARTESIAN_POINT('Ctrl Pts',(53.3711634508437,46.0986741925656,12.));
#109842=CARTESIAN_POINT('Ctrl Pts',(53.3598828428546,46.0811849640218,12.));
#109843=CARTESIAN_POINT('Ctrl Pts',(53.3486113975901,46.0637500926982,12.));
#109844=CARTESIAN_POINT('Ctrl Pts',(53.3373492770671,46.0463696777801,12.));
#109845=CARTESIAN_POINT('Ctrl Pts',(53.326096643428,46.02904381836,12.));
#109846=CARTESIAN_POINT('Ctrl Pts',(53.3148536582635,46.0117726129873,12.));
#109847=CARTESIAN_POINT('Ctrl Pts',(53.3036204818329,45.9945561591453,12.));
#109848=CARTESIAN_POINT('Ctrl Pts',(53.292397274555,45.9773945542384,12.));
#109849=CARTESIAN_POINT('Ctrl Pts',(53.2811841987926,45.9602878967698,12.));
#109850=CARTESIAN_POINT('Ctrl Pts',(53.2699814203105,45.9432362873008,12.));
#109851=CARTESIAN_POINT('Ctrl Pts',(53.2587891103866,45.9262398298349,12.));
#109852=CARTESIAN_POINT('Ctrl Pts',(53.2476074460017,45.9092986319377,12.));
#109853=CARTESIAN_POINT('Ctrl Pts',(53.2364366054306,45.892412801838,12.));
#109854=CARTESIAN_POINT('Ctrl Pts',(53.2252767643662,45.8755824458723,12.));
#109855=CARTESIAN_POINT('Ctrl Pts',(53.2141280925439,45.8588076662582,12.));
#109856=CARTESIAN_POINT('Ctrl Pts',(53.2029907483557,45.8420885575349,12.));
#109857=CARTESIAN_POINT('Ctrl Pts',(53.1918648840541,45.8254252099957,12.));
#109858=CARTESIAN_POINT('Ctrl Pts',(53.1807506560933,45.808817716509,12.));
#109859=CARTESIAN_POINT('Ctrl Pts',(53.1696482334487,45.7922661780005,12.));
#109860=CARTESIAN_POINT('Ctrl Pts',(53.1585578076444,45.7757707100618,12.));
#109861=CARTESIAN_POINT('Ctrl Pts',(53.1474795996053,45.7593314474501,12.));
#109862=CARTESIAN_POINT('Ctrl Pts',(53.1364138384693,45.7429485300823,12.));
#109863=CARTESIAN_POINT('Ctrl Pts',(53.1253607414872,45.7266220897003,12.));
#109864=CARTESIAN_POINT('Ctrl Pts',(53.114320495492,45.7103522376696,12.));
#109865=CARTESIAN_POINT('Ctrl Pts',(53.1032932328857,45.694139048907,12.));
#109866=CARTESIAN_POINT('Ctrl Pts',(53.0922790298409,45.6779825614231,12.));
#109867=CARTESIAN_POINT('Ctrl Pts',(53.0834781451546,45.6651027439241,12.));
#109868=CARTESIAN_POINT('Ctrl Pts',(53.0768833804193,45.6554684028145,12.));
#109869=CARTESIAN_POINT('Ctrl Pts',(53.0724894921849,45.6490568514089,12.));
#109870=CARTESIAN_POINT('Ctrl Pts',(53.0702932034641,45.6458539113724,12.));
#109871=CARTESIAN_POINT('Ctrl Pts',(54.1946543500373,50.6869108458851,-1.11022302462516E-15));
#109872=CARTESIAN_POINT('Ctrl Pts',(54.1946543500373,50.6869108458851,4.));
#109873=CARTESIAN_POINT('Ctrl Pts',(54.1946543500373,50.6869108458851,8.));
#109874=CARTESIAN_POINT('Ctrl Pts',(54.1946543500373,50.6869108458851,12.));
#109875=CARTESIAN_POINT('Ctrl Pts',(54.2986513683568,50.7223900873023,-1.11022302462516E-15));
#109876=CARTESIAN_POINT('Ctrl Pts',(54.2986513683568,50.7223900873023,4.));
#109877=CARTESIAN_POINT('Ctrl Pts',(54.2986513683568,50.7223900873023,8.));
#109878=CARTESIAN_POINT('Ctrl Pts',(54.2986513683568,50.7223900873023,12.));
#109879=CARTESIAN_POINT('Ctrl Pts',(54.5013145669267,50.7219766588197,-1.03713937562159E-15));
#109880=CARTESIAN_POINT('Ctrl Pts',(54.5013145669267,50.7219766588197,4.));
#109881=CARTESIAN_POINT('Ctrl Pts',(54.5013145669267,50.7219766588197,7.99999999999999));
#109882=CARTESIAN_POINT('Ctrl Pts',(54.5013145669267,50.7219766588197,12.));
#109883=CARTESIAN_POINT('Ctrl Pts',(54.6674453828701,50.6135081477658,-8.63611844427818E-16));
#109884=CARTESIAN_POINT('Ctrl Pts',(54.6674453828701,50.6135081477658,4.));
#109885=CARTESIAN_POINT('Ctrl Pts',(54.6674453828701,50.6135081477658,8.));
#109886=CARTESIAN_POINT('Ctrl Pts',(54.6674453828701,50.6135081477658,12.));
#109887=CARTESIAN_POINT('Ctrl Pts',(54.7233670476834,50.55297319609,-7.79957864200068E-16));
#109888=CARTESIAN_POINT('Ctrl Pts',(54.7233670476834,50.55297319609,4.));
#109889=CARTESIAN_POINT('Ctrl Pts',(54.7233670476834,50.55297319609,8.));
#109890=CARTESIAN_POINT('Ctrl Pts',(54.7233670476834,50.55297319609,12.));
#109891=CARTESIAN_POINT('',(54.1946543500373,50.6869108458851,0.));
#109892=CARTESIAN_POINT('',(54.723367047683,50.5529731960897,0.));
#109893=CARTESIAN_POINT('Ctrl Pts',(54.1946543500373,50.6869108458851,8.74764948622162E-18));
#109894=CARTESIAN_POINT('Ctrl Pts',(54.2986513683568,50.7223900873023,8.74764948622131E-18));
#109895=CARTESIAN_POINT('Ctrl Pts',(54.4144589103968,50.7221538424551,5.05097346311187E-17));
#109896=CARTESIAN_POINT('Ctrl Pts',(54.5183375111709,50.6866343053397,1.25069822123835E-16));
#109897=CARTESIAN_POINT('Ctrl Pts',(54.5962464617515,50.6599946525032,1.80989887743373E-16));
#109898=CARTESIAN_POINT('Ctrl Pts',(54.6674453828701,50.6135081477658,2.55358829683559E-16));
#109899=CARTESIAN_POINT('Ctrl Pts',(54.7233670476834,50.55297319609,3.3901280991131E-16));
#109900=CARTESIAN_POINT('',(54.723367047683,50.5529731960897,12.));
#109901=CARTESIAN_POINT('Ctrl Pts',(54.7233670476834,50.55297319609,-7.79957864200068E-16));
#109902=CARTESIAN_POINT('Ctrl Pts',(54.7233670476834,50.55297319609,4.));
#109903=CARTESIAN_POINT('Ctrl Pts',(54.7233670476834,50.55297319609,8.));
#109904=CARTESIAN_POINT('Ctrl Pts',(54.7233670476834,50.55297319609,12.));
#109905=CARTESIAN_POINT('',(54.1946543500373,50.6869108458851,12.));
#109906=CARTESIAN_POINT('Ctrl Pts',(54.7233670476834,50.55297319609,12.));
#109907=CARTESIAN_POINT('Ctrl Pts',(54.6674453828701,50.6135081477658,12.));
#109908=CARTESIAN_POINT('Ctrl Pts',(54.5962464617515,50.6599946525032,12.));
#109909=CARTESIAN_POINT('Ctrl Pts',(54.5183375111709,50.6866343053397,12.));
#109910=CARTESIAN_POINT('Ctrl Pts',(54.4144589103968,50.7221538424551,12.));
#109911=CARTESIAN_POINT('Ctrl Pts',(54.2986513683568,50.7223900873023,12.));
#109912=CARTESIAN_POINT('Ctrl Pts',(54.1946543500373,50.6869108458851,12.));
#109913=CARTESIAN_POINT('Ctrl Pts',(54.1946543500373,50.6869108458851,12.));
#109914=CARTESIAN_POINT('Ctrl Pts',(54.1946543500373,50.6869108458851,8.));
#109915=CARTESIAN_POINT('Ctrl Pts',(54.1946543500373,50.6869108458851,4.));
#109916=CARTESIAN_POINT('Ctrl Pts',(54.1946543500373,50.6869108458851,-1.11022302462516E-15));
#109917=CARTESIAN_POINT('Origin',(2.7629675461203E-10,2.53313958019842E-10,
0.));
#109918=CARTESIAN_POINT('Origin',(2.7629675461203E-10,2.53313958019842E-10,
12.));
#109919=CARTESIAN_POINT('Origin',(2.7629675461203E-10,2.53313958019842E-10,
0.));
#109920=CARTESIAN_POINT('Ctrl Pts',(59.2875729049545,45.1135644683471,0.));
#109921=CARTESIAN_POINT('Ctrl Pts',(59.2875729049545,45.1135644683471,4.));
#109922=CARTESIAN_POINT('Ctrl Pts',(59.2875729049545,45.1135644683471,8.));
#109923=CARTESIAN_POINT('Ctrl Pts',(59.2875729049545,45.1135644683471,12.));
#109924=CARTESIAN_POINT('Ctrl Pts',(59.3541123643618,45.0261193041895,0.));
#109925=CARTESIAN_POINT('Ctrl Pts',(59.3541123643618,45.0261193041895,4.));
#109926=CARTESIAN_POINT('Ctrl Pts',(59.3541123643618,45.0261193041895,8.));
#109927=CARTESIAN_POINT('Ctrl Pts',(59.3541123643618,45.0261193041895,12.));
#109928=CARTESIAN_POINT('Ctrl Pts',(59.4177951463802,44.8337211159575,0.));
#109929=CARTESIAN_POINT('Ctrl Pts',(59.4177951463802,44.8337211159575,4.00000000000001));
#109930=CARTESIAN_POINT('Ctrl Pts',(59.4177951463802,44.8337211159575,8.));
#109931=CARTESIAN_POINT('Ctrl Pts',(59.4177951463802,44.8337211159575,12.));
#109932=CARTESIAN_POINT('Ctrl Pts',(59.3674150879748,44.6418181989799,0.));
#109933=CARTESIAN_POINT('Ctrl Pts',(59.3674150879748,44.6418181989799,4.));
#109934=CARTESIAN_POINT('Ctrl Pts',(59.3674150879747,44.6418181989798,8.00000000000001));
#109935=CARTESIAN_POINT('Ctrl Pts',(59.3674150879747,44.6418181989798,12.));
#109936=CARTESIAN_POINT('Ctrl Pts',(59.3276657444157,44.5696260757423,0.));
#109937=CARTESIAN_POINT('Ctrl Pts',(59.3276657444157,44.5696260757423,4.));
#109938=CARTESIAN_POINT('Ctrl Pts',(59.3276657444157,44.5696260757423,8.));
#109939=CARTESIAN_POINT('Ctrl Pts',(59.3276657444157,44.5696260757423,12.));
#109940=CARTESIAN_POINT('',(59.2875729049545,45.1135644683471,0.));
#109941=CARTESIAN_POINT('',(59.3276657444159,44.5696260757422,0.));
#109942=CARTESIAN_POINT('Ctrl Pts',(59.2875729049545,45.1135644683471,0.));
#109943=CARTESIAN_POINT('Ctrl Pts',(59.3541123643618,45.0261193041895,0.));
#109944=CARTESIAN_POINT('Ctrl Pts',(59.3905025255151,44.9161774823427,0.));
#109945=CARTESIAN_POINT('Ctrl Pts',(59.3896476775505,44.8063973817217,0.));
#109946=CARTESIAN_POINT('Ctrl Pts',(59.3890065415771,44.724062306256,0.));
#109947=CARTESIAN_POINT('Ctrl Pts',(59.3674150879748,44.6418181989799,0.));
#109948=CARTESIAN_POINT('Ctrl Pts',(59.3276657444157,44.5696260757423,0.));
#109949=CARTESIAN_POINT('',(59.3276657444159,44.5696260757422,12.));
#109950=CARTESIAN_POINT('Ctrl Pts',(59.3276657444157,44.5696260757423,0.));
#109951=CARTESIAN_POINT('Ctrl Pts',(59.3276657444157,44.5696260757423,4.));
#109952=CARTESIAN_POINT('Ctrl Pts',(59.3276657444157,44.5696260757423,8.));
#109953=CARTESIAN_POINT('Ctrl Pts',(59.3276657444157,44.5696260757423,12.));
#109954=CARTESIAN_POINT('',(59.2875729049545,45.1135644683471,12.));
#109955=CARTESIAN_POINT('Ctrl Pts',(59.3276657444157,44.5696260757423,12.));
#109956=CARTESIAN_POINT('Ctrl Pts',(59.3674150879747,44.6418181989798,12.));
#109957=CARTESIAN_POINT('Ctrl Pts',(59.3890065415771,44.724062306256,12.));
#109958=CARTESIAN_POINT('Ctrl Pts',(59.3896476775505,44.8063973817217,12.));
#109959=CARTESIAN_POINT('Ctrl Pts',(59.3905025255151,44.9161774823427,12.));
#109960=CARTESIAN_POINT('Ctrl Pts',(59.3541123643618,45.0261193041895,12.));
#109961=CARTESIAN_POINT('Ctrl Pts',(59.2875729049545,45.1135644683471,12.));
#109962=CARTESIAN_POINT('Ctrl Pts',(59.2875729049545,45.1135644683471,12.));
#109963=CARTESIAN_POINT('Ctrl Pts',(59.2875729049545,45.1135644683471,8.));
#109964=CARTESIAN_POINT('Ctrl Pts',(59.2875729049545,45.1135644683471,4.));
#109965=CARTESIAN_POINT('Ctrl Pts',(59.2875729049545,45.1135644683471,0.));
#109966=CARTESIAN_POINT('Ctrl Pts',(56.8466430164621,40.8467768343956,0.));
#109967=CARTESIAN_POINT('Ctrl Pts',(56.8466430164621,40.8467768343956,12.));
#109968=CARTESIAN_POINT('Ctrl Pts',(56.8491101022591,40.8497761671036,0.));
#109969=CARTESIAN_POINT('Ctrl Pts',(56.8491101022591,40.8497761671036,12.));
#109970=CARTESIAN_POINT('Ctrl Pts',(56.8540460739472,40.8557803680278,0.));
#109971=CARTESIAN_POINT('Ctrl Pts',(56.8540460739472,40.8557803680278,12.));
#109972=CARTESIAN_POINT('Ctrl Pts',(56.8614554317668,40.864803275942,0.));
#109973=CARTESIAN_POINT('Ctrl Pts',(56.8614554317668,40.864803275942,12.));
#109974=CARTESIAN_POINT('Ctrl Pts',(56.8713453764905,40.8768670342052,0.));
#109975=CARTESIAN_POINT('Ctrl Pts',(56.8713453764905,40.8768670342052,12.));
#109976=CARTESIAN_POINT('Ctrl Pts',(56.8837257978343,40.8920020903293,0.));
#109977=CARTESIAN_POINT('Ctrl Pts',(56.8837257978343,40.8920020903293,12.));
#109978=CARTESIAN_POINT('Ctrl Pts',(56.8961241708861,40.9071924937508,0.));
#109979=CARTESIAN_POINT('Ctrl Pts',(56.8961241708861,40.9071924937508,12.));
#109980=CARTESIAN_POINT('Ctrl Pts',(56.9085404164502,40.9224382132427,0.));
#109981=CARTESIAN_POINT('Ctrl Pts',(56.9085404164502,40.9224382132427,12.));
#109982=CARTESIAN_POINT('Ctrl Pts',(56.9209743960992,40.9377391857129,0.));
#109983=CARTESIAN_POINT('Ctrl Pts',(56.9209743960992,40.9377391857129,12.));
#109984=CARTESIAN_POINT('Ctrl Pts',(56.9334259140049,40.9530953165031,0.));
#109985=CARTESIAN_POINT('Ctrl Pts',(56.9334259140049,40.9530953165031,12.));
#109986=CARTESIAN_POINT('Ctrl Pts',(56.9458947422608,40.9685064933074,0.));
#109987=CARTESIAN_POINT('Ctrl Pts',(56.9458947422608,40.9685064933074,12.));
#109988=CARTESIAN_POINT('Ctrl Pts',(56.9583806404069,40.9839725967121,0.));
#109989=CARTESIAN_POINT('Ctrl Pts',(56.9583806404069,40.9839725967121,12.));
#109990=CARTESIAN_POINT('Ctrl Pts',(56.9708833766137,40.9994935117276,0.));
#109991=CARTESIAN_POINT('Ctrl Pts',(56.9708833766137,40.9994935117276,12.));
#109992=CARTESIAN_POINT('Ctrl Pts',(56.9834027500117,41.0150691398947,0.));
#109993=CARTESIAN_POINT('Ctrl Pts',(56.9834027500117,41.0150691398947,12.));
#109994=CARTESIAN_POINT('Ctrl Pts',(56.995938583472,41.0306993953989,0.));
#109995=CARTESIAN_POINT('Ctrl Pts',(56.995938583472,41.0306993953989,12.));
#109996=CARTESIAN_POINT('Ctrl Pts',(57.008490713042,41.0463841993608,0.));
#109997=CARTESIAN_POINT('Ctrl Pts',(57.008490713042,41.0463841993608,12.));
#109998=CARTESIAN_POINT('Ctrl Pts',(57.0210589791788,41.0621234751007,0.));
#109999=CARTESIAN_POINT('Ctrl Pts',(57.0210589791788,41.0621234751007,12.));
#110000=CARTESIAN_POINT('Ctrl Pts',(57.0336432158536,41.0779171422438,0.));
#110001=CARTESIAN_POINT('Ctrl Pts',(57.0336432158536,41.0779171422438,12.));
#110002=CARTESIAN_POINT('Ctrl Pts',(57.046243245068,41.0937651137549,0.));
#110003=CARTESIAN_POINT('Ctrl Pts',(57.046243245068,41.0937651137549,12.));
#110004=CARTESIAN_POINT('Ctrl Pts',(57.0588588825298,41.1096672990148,0.));
#110005=CARTESIAN_POINT('Ctrl Pts',(57.0588588825298,41.1096672990148,12.));
#110006=CARTESIAN_POINT('Ctrl Pts',(57.0714899412099,41.1256236057443,0.));
#110007=CARTESIAN_POINT('Ctrl Pts',(57.0714899412099,41.1256236057443,12.));
#110008=CARTESIAN_POINT('Ctrl Pts',(57.084136235426,41.1416339422117,0.));
#110009=CARTESIAN_POINT('Ctrl Pts',(57.084136235426,41.1416339422117,12.));
#110010=CARTESIAN_POINT('Ctrl Pts',(57.0967975854874,41.1576982197375,0.));
#110011=CARTESIAN_POINT('Ctrl Pts',(57.0967975854874,41.1576982197375,12.));
#110012=CARTESIAN_POINT('Ctrl Pts',(57.1094738174957,41.1738163525902,0.));
#110013=CARTESIAN_POINT('Ctrl Pts',(57.1094738174957,41.1738163525902,12.));
#110014=CARTESIAN_POINT('Ctrl Pts',(57.1221647611207,41.1899882567923,0.));
#110015=CARTESIAN_POINT('Ctrl Pts',(57.1221647611207,41.1899882567923,12.));
#110016=CARTESIAN_POINT('Ctrl Pts',(57.1348702480647,41.2062138492915,0.));
#110017=CARTESIAN_POINT('Ctrl Pts',(57.1348702480647,41.2062138492915,12.));
#110018=CARTESIAN_POINT('Ctrl Pts',(57.147590110182,41.222493046943,0.));
#110019=CARTESIAN_POINT('Ctrl Pts',(57.147590110182,41.222493046943,12.));
#110020=CARTESIAN_POINT('Ctrl Pts',(57.1603241779077,41.2388257656559,0.));
#110021=CARTESIAN_POINT('Ctrl Pts',(57.1603241779077,41.2388257656559,12.));
#110022=CARTESIAN_POINT('Ctrl Pts',(57.17307228108,41.2552119208466,0.));
#110023=CARTESIAN_POINT('Ctrl Pts',(57.17307228108,41.2552119208466,12.));
#110024=CARTESIAN_POINT('Ctrl Pts',(57.1858342496538,41.2716514278276,0.));
#110025=CARTESIAN_POINT('Ctrl Pts',(57.1858342496538,41.2716514278276,12.));
#110026=CARTESIAN_POINT('Ctrl Pts',(57.1986099143983,41.2881442021863,0.));
#110027=CARTESIAN_POINT('Ctrl Pts',(57.1986099143983,41.2881442021863,12.));
#110028=CARTESIAN_POINT('Ctrl Pts',(57.2113991077302,41.3046901602293,0.));
#110029=CARTESIAN_POINT('Ctrl Pts',(57.2113991077302,41.3046901602293,12.));
#110030=CARTESIAN_POINT('Ctrl Pts',(57.2242016640198,41.321289219149,0.));
#110031=CARTESIAN_POINT('Ctrl Pts',(57.2242016640198,41.321289219149,12.));
#110032=CARTESIAN_POINT('Ctrl Pts',(57.2370174191401,41.3379412967875,0.));
#110033=CARTESIAN_POINT('Ctrl Pts',(57.2370174191401,41.3379412967875,12.));
#110034=CARTESIAN_POINT('Ctrl Pts',(57.2498462101879,41.3546463114885,0.));
#110035=CARTESIAN_POINT('Ctrl Pts',(57.2498462101879,41.3546463114885,12.));
#110036=CARTESIAN_POINT('Ctrl Pts',(57.2626878751596,41.3714041819224,0.));
#110037=CARTESIAN_POINT('Ctrl Pts',(57.2626878751596,41.3714041819224,12.));
#110038=CARTESIAN_POINT('Ctrl Pts',(57.2755422525844,41.3882148268814,0.));
#110039=CARTESIAN_POINT('Ctrl Pts',(57.2755422525844,41.3882148268814,12.));
#110040=CARTESIAN_POINT('Ctrl Pts',(57.2884091815406,41.4050781652938,0.));
#110041=CARTESIAN_POINT('Ctrl Pts',(57.2884091815406,41.4050781652938,12.));
#110042=CARTESIAN_POINT('Ctrl Pts',(57.3012885018151,41.4219941163163,0.));
#110043=CARTESIAN_POINT('Ctrl Pts',(57.3012885018151,41.4219941163163,12.));
#110044=CARTESIAN_POINT('Ctrl Pts',(57.3141800540137,41.4389625993948,0.));
#110045=CARTESIAN_POINT('Ctrl Pts',(57.3141800540137,41.4389625993948,12.));
#110046=CARTESIAN_POINT('Ctrl Pts',(57.3270836796911,41.4559835343328,0.));
#110047=CARTESIAN_POINT('Ctrl Pts',(57.3270836796911,41.4559835343328,12.));
#110048=CARTESIAN_POINT('Ctrl Pts',(57.3399992214717,41.4730568413518,0.));
#110049=CARTESIAN_POINT('Ctrl Pts',(57.3399992214717,41.4730568413518,12.));
#110050=CARTESIAN_POINT('Ctrl Pts',(57.3529265229835,41.4901824410637,0.));
#110051=CARTESIAN_POINT('Ctrl Pts',(57.3529265229835,41.4901824410637,12.));
#110052=CARTESIAN_POINT('Ctrl Pts',(57.3658654287937,41.5073602544396,0.));
#110053=CARTESIAN_POINT('Ctrl Pts',(57.3658654287937,41.5073602544396,12.));
#110054=CARTESIAN_POINT('Ctrl Pts',(57.3788157843454,41.5245902027771,0.));
#110055=CARTESIAN_POINT('Ctrl Pts',(57.3788157843454,41.5245902027771,12.));
#110056=CARTESIAN_POINT('Ctrl Pts',(57.3917774358863,41.5418722076572,0.));
#110057=CARTESIAN_POINT('Ctrl Pts',(57.3917774358863,41.5418722076572,12.));
#110058=CARTESIAN_POINT('Ctrl Pts',(57.4047502304231,41.5592061909176,0.));
#110059=CARTESIAN_POINT('Ctrl Pts',(57.4047502304231,41.5592061909176,12.));
#110060=CARTESIAN_POINT('Ctrl Pts',(57.4177340157508,41.5765920746777,0.));
#110061=CARTESIAN_POINT('Ctrl Pts',(57.4177340157508,41.5765920746777,12.));
#110062=CARTESIAN_POINT('Ctrl Pts',(57.4307286404662,41.5940297813477,0.));
#110063=CARTESIAN_POINT('Ctrl Pts',(57.4307286404662,41.5940297813477,12.));
#110064=CARTESIAN_POINT('Ctrl Pts',(57.4437339539841,41.6115192336388,0.));
#110065=CARTESIAN_POINT('Ctrl Pts',(57.4437339539841,41.6115192336388,12.));
#110066=CARTESIAN_POINT('Ctrl Pts',(57.4567498065562,41.6290603545666,0.));
#110067=CARTESIAN_POINT('Ctrl Pts',(57.4567498065562,41.6290603545666,12.));
#110068=CARTESIAN_POINT('Ctrl Pts',(57.4697760492683,41.6466530674515,0.));
#110069=CARTESIAN_POINT('Ctrl Pts',(57.4697760492683,41.6466530674515,12.));
#110070=CARTESIAN_POINT('Ctrl Pts',(57.4828125340218,41.6642972959165,0.));
#110071=CARTESIAN_POINT('Ctrl Pts',(57.4828125340218,41.6642972959165,12.));
#110072=CARTESIAN_POINT('Ctrl Pts',(57.4958591135165,41.6819929638797,0.));
#110073=CARTESIAN_POINT('Ctrl Pts',(57.4958591135165,41.6819929638797,12.));
#110074=CARTESIAN_POINT('Ctrl Pts',(57.5089156412343,41.6997399955447,0.));
#110075=CARTESIAN_POINT('Ctrl Pts',(57.5089156412343,41.6997399955447,12.));
#110076=CARTESIAN_POINT('Ctrl Pts',(57.5219819714171,41.7175383153821,0.));
#110077=CARTESIAN_POINT('Ctrl Pts',(57.5219819714171,41.7175383153821,12.));
#110078=CARTESIAN_POINT('Ctrl Pts',(57.5350579590649,41.7353878481337,0.));
#110079=CARTESIAN_POINT('Ctrl Pts',(57.5350579590649,41.7353878481337,12.));
#110080=CARTESIAN_POINT('Ctrl Pts',(57.5481434599335,41.7532885188175,0.));
#110081=CARTESIAN_POINT('Ctrl Pts',(57.5481434599335,41.7532885188175,12.));
#110082=CARTESIAN_POINT('Ctrl Pts',(57.561238330532,41.7712402527273,0.));
#110083=CARTESIAN_POINT('Ctrl Pts',(57.561238330532,41.7712402527273,12.));
#110084=CARTESIAN_POINT('Ctrl Pts',(57.5743424281204,41.7892429754297,0.));
#110085=CARTESIAN_POINT('Ctrl Pts',(57.5743424281204,41.7892429754297,12.));
#110086=CARTESIAN_POINT('Ctrl Pts',(57.5874556107056,41.8072966127558,0.));
#110087=CARTESIAN_POINT('Ctrl Pts',(57.5874556107056,41.8072966127558,12.));
#110088=CARTESIAN_POINT('Ctrl Pts',(57.6005777370349,41.8254010908051,0.));
#110089=CARTESIAN_POINT('Ctrl Pts',(57.6005777370349,41.8254010908051,12.));
#110090=CARTESIAN_POINT('Ctrl Pts',(57.6137086665882,41.8435563359456,0.));
#110091=CARTESIAN_POINT('Ctrl Pts',(57.6137086665882,41.8435563359456,12.));
#110092=CARTESIAN_POINT('Ctrl Pts',(57.6268482595702,41.8617622748108,0.));
#110093=CARTESIAN_POINT('Ctrl Pts',(57.6268482595702,41.8617622748108,12.));
#110094=CARTESIAN_POINT('Ctrl Pts',(57.6399963769003,41.8800188342909,0.));
#110095=CARTESIAN_POINT('Ctrl Pts',(57.6399963769003,41.8800188342909,12.));
#110096=CARTESIAN_POINT('Ctrl Pts',(57.6531528802059,41.8983259415245,0.));
#110097=CARTESIAN_POINT('Ctrl Pts',(57.6531528802059,41.8983259415245,12.));
#110098=CARTESIAN_POINT('Ctrl Pts',(57.6663176318176,41.9166835239046,0.));
#110099=CARTESIAN_POINT('Ctrl Pts',(57.6663176318176,41.9166835239046,12.));
#110100=CARTESIAN_POINT('Ctrl Pts',(57.6794904947641,41.9350915090791,0.));
#110101=CARTESIAN_POINT('Ctrl Pts',(57.6794904947641,41.9350915090791,12.));
#110102=CARTESIAN_POINT('Ctrl Pts',(57.6926713327674,41.9535498249489,0.));
#110103=CARTESIAN_POINT('Ctrl Pts',(57.6926713327674,41.9535498249489,12.));
#110104=CARTESIAN_POINT('Ctrl Pts',(57.7058600102365,41.9720583996601,0.));
#110105=CARTESIAN_POINT('Ctrl Pts',(57.7058600102365,41.9720583996601,12.));
#110106=CARTESIAN_POINT('Ctrl Pts',(57.7190563922614,41.9906171615975,0.));
#110107=CARTESIAN_POINT('Ctrl Pts',(57.7190563922614,41.9906171615975,12.));
#110108=CARTESIAN_POINT('Ctrl Pts',(57.7322603446086,42.0092260393911,0.));
#110109=CARTESIAN_POINT('Ctrl Pts',(57.7322603446086,42.0092260393911,12.));
#110110=CARTESIAN_POINT('Ctrl Pts',(57.7454717337151,42.0278849619156,0.));
#110111=CARTESIAN_POINT('Ctrl Pts',(57.7454717337151,42.0278849619156,12.));
#110112=CARTESIAN_POINT('Ctrl Pts',(57.7586904266828,42.0465938582878,0.));
#110113=CARTESIAN_POINT('Ctrl Pts',(57.7586904266828,42.0465938582878,12.));
#110114=CARTESIAN_POINT('Ctrl Pts',(57.7719162912721,42.0653526578571,0.));
#110115=CARTESIAN_POINT('Ctrl Pts',(57.7719162912721,42.0653526578571,12.));
#110116=CARTESIAN_POINT('Ctrl Pts',(57.7851491958954,42.0841612902018,0.));
#110117=CARTESIAN_POINT('Ctrl Pts',(57.7851491958954,42.0841612902018,12.));
#110118=CARTESIAN_POINT('Ctrl Pts',(57.798389009613,42.1030196851344,0.));
#110119=CARTESIAN_POINT('Ctrl Pts',(57.798389009613,42.1030196851344,12.));
#110120=CARTESIAN_POINT('Ctrl Pts',(57.8116356021274,42.121927772701,0.));
#110121=CARTESIAN_POINT('Ctrl Pts',(57.8116356021274,42.121927772701,12.));
#110122=CARTESIAN_POINT('Ctrl Pts',(57.8248888437787,42.1408854831792,0.));
#110123=CARTESIAN_POINT('Ctrl Pts',(57.8248888437787,42.1408854831792,12.));
#110124=CARTESIAN_POINT('Ctrl Pts',(57.8381486055376,42.1598927470671,0.));
#110125=CARTESIAN_POINT('Ctrl Pts',(57.8381486055376,42.1598927470671,12.));
#110126=CARTESIAN_POINT('Ctrl Pts',(57.8514147590012,42.1789494950824,0.));
#110127=CARTESIAN_POINT('Ctrl Pts',(57.8514147590012,42.1789494950824,12.));
#110128=CARTESIAN_POINT('Ctrl Pts',(57.86468717639,42.1980556581689,0.));
#110129=CARTESIAN_POINT('Ctrl Pts',(57.86468717639,42.1980556581689,12.));
#110130=CARTESIAN_POINT('Ctrl Pts',(57.8779657305422,42.2172111674946,0.));
#110131=CARTESIAN_POINT('Ctrl Pts',(57.8779657305422,42.2172111674946,12.));
#110132=CARTESIAN_POINT('Ctrl Pts',(57.8912502949084,42.2364159544492,0.));
#110133=CARTESIAN_POINT('Ctrl Pts',(57.8912502949084,42.2364159544492,12.));
#110134=CARTESIAN_POINT('Ctrl Pts',(57.9045407435447,42.2556699506332,0.));
#110135=CARTESIAN_POINT('Ctrl Pts',(57.9045407435447,42.2556699506332,12.));
#110136=CARTESIAN_POINT('Ctrl Pts',(57.9178369511084,42.274973087857,0.));
#110137=CARTESIAN_POINT('Ctrl Pts',(57.9178369511084,42.274973087857,12.));
#110138=CARTESIAN_POINT('Ctrl Pts',(57.9311387928541,42.2943252981471,0.));
#110139=CARTESIAN_POINT('Ctrl Pts',(57.9311387928541,42.2943252981471,12.));
#110140=CARTESIAN_POINT('Ctrl Pts',(57.9444461446292,42.3137265137446,0.));
#110141=CARTESIAN_POINT('Ctrl Pts',(57.9444461446292,42.3137265137446,12.));
#110142=CARTESIAN_POINT('Ctrl Pts',(57.9577588828693,42.3331766671028,0.));
#110143=CARTESIAN_POINT('Ctrl Pts',(57.9577588828693,42.3331766671028,12.));
#110144=CARTESIAN_POINT('Ctrl Pts',(57.9710768845923,42.3526756908764,0.));
#110145=CARTESIAN_POINT('Ctrl Pts',(57.9710768845923,42.3526756908764,12.));
#110146=CARTESIAN_POINT('Ctrl Pts',(57.9844000273936,42.3722235179216,0.));
#110147=CARTESIAN_POINT('Ctrl Pts',(57.9844000273936,42.3722235179216,12.));
#110148=CARTESIAN_POINT('Ctrl Pts',(57.9977281894437,42.3918200813025,0.));
#110149=CARTESIAN_POINT('Ctrl Pts',(57.9977281894437,42.3918200813025,12.));
#110150=CARTESIAN_POINT('Ctrl Pts',(58.011061249483,42.4114653142891,0.));
#110151=CARTESIAN_POINT('Ctrl Pts',(58.011061249483,42.4114653142891,12.));
#110152=CARTESIAN_POINT('Ctrl Pts',(58.0243990868175,42.4311591503551,0.));
#110153=CARTESIAN_POINT('Ctrl Pts',(58.0243990868175,42.4311591503551,12.));
#110154=CARTESIAN_POINT('Ctrl Pts',(58.0377415813132,42.4509015231668,0.));
#110155=CARTESIAN_POINT('Ctrl Pts',(58.0377415813132,42.4509015231668,12.));
#110156=CARTESIAN_POINT('Ctrl Pts',(58.0510886133917,42.4706923665838,0.));
#110157=CARTESIAN_POINT('Ctrl Pts',(58.0510886133917,42.4706923665838,12.));
#110158=CARTESIAN_POINT('Ctrl Pts',(58.064440064027,42.490531614665,0.));
#110159=CARTESIAN_POINT('Ctrl Pts',(58.064440064027,42.490531614665,12.));
#110160=CARTESIAN_POINT('Ctrl Pts',(58.0777958147404,42.5104192016664,0.));
#110161=CARTESIAN_POINT('Ctrl Pts',(58.0777958147404,42.5104192016664,12.));
#110162=CARTESIAN_POINT('Ctrl Pts',(58.0911557475967,42.5303550620388,0.));
#110163=CARTESIAN_POINT('Ctrl Pts',(58.0911557475967,42.5303550620388,12.));
#110164=CARTESIAN_POINT('Ctrl Pts',(58.1045197452003,42.5503391304183,0.));
#110165=CARTESIAN_POINT('Ctrl Pts',(58.1045197452003,42.5503391304183,12.));
#110166=CARTESIAN_POINT('Ctrl Pts',(58.1178876906905,42.5703713416263,0.));
#110167=CARTESIAN_POINT('Ctrl Pts',(58.1178876906905,42.5703713416263,12.));
#110168=CARTESIAN_POINT('Ctrl Pts',(58.1312594677383,42.5904516306759,0.));
#110169=CARTESIAN_POINT('Ctrl Pts',(58.1312594677383,42.5904516306759,12.));
#110170=CARTESIAN_POINT('Ctrl Pts',(58.1446349605419,42.6105799327697,0.));
#110171=CARTESIAN_POINT('Ctrl Pts',(58.1446349605419,42.6105799327697,12.));
#110172=CARTESIAN_POINT('Ctrl Pts',(58.158014053823,42.6307561832978,0.));
#110173=CARTESIAN_POINT('Ctrl Pts',(58.158014053823,42.6307561832978,12.));
#110174=CARTESIAN_POINT('Ctrl Pts',(58.1713966328217,42.650980317827,0.));
#110175=CARTESIAN_POINT('Ctrl Pts',(58.1713966328217,42.650980317827,12.));
#110176=CARTESIAN_POINT('Ctrl Pts',(58.1847825832932,42.6712522721021,0.));
#110177=CARTESIAN_POINT('Ctrl Pts',(58.1847825832932,42.6712522721021,12.));
#110178=CARTESIAN_POINT('Ctrl Pts',(58.1981717915043,42.6915719820517,0.));
#110179=CARTESIAN_POINT('Ctrl Pts',(58.1981717915043,42.6915719820517,12.));
#110180=CARTESIAN_POINT('Ctrl Pts',(58.2115641442302,42.7119393837867,0.));
#110181=CARTESIAN_POINT('Ctrl Pts',(58.2115641442302,42.7119393837867,12.));
#110182=CARTESIAN_POINT('Ctrl Pts',(58.2249595287497,42.7323544135983,0.));
#110183=CARTESIAN_POINT('Ctrl Pts',(58.2249595287497,42.7323544135983,12.));
#110184=CARTESIAN_POINT('Ctrl Pts',(58.238357832842,42.7528170079482,0.));
#110185=CARTESIAN_POINT('Ctrl Pts',(58.238357832842,42.7528170079482,12.));
#110186=CARTESIAN_POINT('Ctrl Pts',(58.2517589447818,42.7733271034679,0.));
#110187=CARTESIAN_POINT('Ctrl Pts',(58.2517589447818,42.7733271034679,12.));
#110188=CARTESIAN_POINT('Ctrl Pts',(58.2651627533368,42.7938846369651,0.));
#110189=CARTESIAN_POINT('Ctrl Pts',(58.2651627533368,42.7938846369651,12.));
#110190=CARTESIAN_POINT('Ctrl Pts',(58.278569147764,42.8144895454234,0.));
#110191=CARTESIAN_POINT('Ctrl Pts',(58.278569147764,42.8144895454234,12.));
#110192=CARTESIAN_POINT('Ctrl Pts',(58.2919780178063,42.8351417659998,0.));
#110193=CARTESIAN_POINT('Ctrl Pts',(58.2919780178063,42.8351417659998,12.));
#110194=CARTESIAN_POINT('Ctrl Pts',(58.305389253689,42.8558412360154,0.));
#110195=CARTESIAN_POINT('Ctrl Pts',(58.305389253689,42.8558412360154,12.));
#110196=CARTESIAN_POINT('Ctrl Pts',(58.3188027461157,42.8765878929545,0.));
#110197=CARTESIAN_POINT('Ctrl Pts',(58.3188027461157,42.8765878929545,12.));
#110198=CARTESIAN_POINT('Ctrl Pts',(58.3322183862647,42.8973816744703,0.));
#110199=CARTESIAN_POINT('Ctrl Pts',(58.3322183862647,42.8973816744703,12.));
#110200=CARTESIAN_POINT('Ctrl Pts',(58.3456360657861,42.9182225183851,0.));
#110201=CARTESIAN_POINT('Ctrl Pts',(58.3456360657861,42.9182225183851,12.));
#110202=CARTESIAN_POINT('Ctrl Pts',(58.3590556767981,42.9391103626881,0.));
#110203=CARTESIAN_POINT('Ctrl Pts',(58.3590556767981,42.9391103626881,12.));
#110204=CARTESIAN_POINT('Ctrl Pts',(58.3724771118835,42.9600451455267,0.));
#110205=CARTESIAN_POINT('Ctrl Pts',(58.3724771118835,42.9600451455267,12.));
#110206=CARTESIAN_POINT('Ctrl Pts',(58.3859002640871,42.9810268052043,0.));
#110207=CARTESIAN_POINT('Ctrl Pts',(58.3859002640871,42.9810268052043,12.));
#110208=CARTESIAN_POINT('Ctrl Pts',(58.3993250269115,43.002055280187,0.));
#110209=CARTESIAN_POINT('Ctrl Pts',(58.3993250269115,43.002055280187,12.));
#110210=CARTESIAN_POINT('Ctrl Pts',(58.4127512943144,43.0231305091033,0.));
#110211=CARTESIAN_POINT('Ctrl Pts',(58.4127512943144,43.0231305091033,12.));
#110212=CARTESIAN_POINT('Ctrl Pts',(58.4261789607055,43.0442524307432,0.));
#110213=CARTESIAN_POINT('Ctrl Pts',(58.4261789607055,43.0442524307432,12.));
#110214=CARTESIAN_POINT('Ctrl Pts',(58.4396079209438,43.0654209840502,0.));
#110215=CARTESIAN_POINT('Ctrl Pts',(58.4396079209438,43.0654209840502,12.));
#110216=CARTESIAN_POINT('Ctrl Pts',(58.4530380703335,43.0866361081166,0.));
#110217=CARTESIAN_POINT('Ctrl Pts',(58.4530380703335,43.0866361081166,12.));
#110218=CARTESIAN_POINT('Ctrl Pts',(58.4664693046206,43.1078977421908,0.));
#110219=CARTESIAN_POINT('Ctrl Pts',(58.4664693046206,43.1078977421908,12.));
#110220=CARTESIAN_POINT('Ctrl Pts',(58.4799015199904,43.1292058256774,0.));
#110221=CARTESIAN_POINT('Ctrl Pts',(58.4799015199904,43.1292058256774,12.));
#110222=CARTESIAN_POINT('Ctrl Pts',(58.4933346130638,43.1505602981366,0.));
#110223=CARTESIAN_POINT('Ctrl Pts',(58.4933346130638,43.1505602981366,12.));
#110224=CARTESIAN_POINT('Ctrl Pts',(58.5067684808946,43.1719610992772,0.));
#110225=CARTESIAN_POINT('Ctrl Pts',(58.5067684808946,43.1719610992772,12.));
#110226=CARTESIAN_POINT('Ctrl Pts',(58.5202030209667,43.1934081689504,0.));
#110227=CARTESIAN_POINT('Ctrl Pts',(58.5202030209667,43.1934081689504,12.));
#110228=CARTESIAN_POINT('Ctrl Pts',(58.5336381311911,43.214901447157,0.));
#110229=CARTESIAN_POINT('Ctrl Pts',(58.5336381311911,43.214901447157,12.));
#110230=CARTESIAN_POINT('Ctrl Pts',(58.5470737099027,43.2364408740489,0.));
#110231=CARTESIAN_POINT('Ctrl Pts',(58.5470737099027,43.2364408740489,12.));
#110232=CARTESIAN_POINT('Ctrl Pts',(58.5605096558578,43.2580263899278,0.));
#110233=CARTESIAN_POINT('Ctrl Pts',(58.5605096558578,43.2580263899278,12.));
#110234=CARTESIAN_POINT('Ctrl Pts',(58.5739458682317,43.2796579352405,0.));
#110235=CARTESIAN_POINT('Ctrl Pts',(58.5739458682317,43.2796579352405,12.));
#110236=CARTESIAN_POINT('Ctrl Pts',(58.5873822466163,43.3013354505708,0.));
#110237=CARTESIAN_POINT('Ctrl Pts',(58.5873822466163,43.3013354505708,12.));
#110238=CARTESIAN_POINT('Ctrl Pts',(58.6008186910166,43.3230588766456,0.));
#110239=CARTESIAN_POINT('Ctrl Pts',(58.6008186910166,43.3230588766456,12.));
#110240=CARTESIAN_POINT('Ctrl Pts',(58.6142551018473,43.3448281543375,0.));
#110241=CARTESIAN_POINT('Ctrl Pts',(58.6142551018473,43.3448281543375,12.));
#110242=CARTESIAN_POINT('Ctrl Pts',(58.627691379929,43.3666432246635,0.));
#110243=CARTESIAN_POINT('Ctrl Pts',(58.627691379929,43.3666432246635,12.));
#110244=CARTESIAN_POINT('Ctrl Pts',(58.6411274264854,43.3885040287808,0.));
#110245=CARTESIAN_POINT('Ctrl Pts',(58.6411274264854,43.3885040287808,12.));
#110246=CARTESIAN_POINT('Ctrl Pts',(58.6545631431388,43.4104105079766,0.));
#110247=CARTESIAN_POINT('Ctrl Pts',(58.6545631431388,43.4104105079766,12.));
#110248=CARTESIAN_POINT('Ctrl Pts',(58.6679984319095,43.4323626036736,0.));
#110249=CARTESIAN_POINT('Ctrl Pts',(58.6679984319095,43.4323626036736,12.));
#110250=CARTESIAN_POINT('Ctrl Pts',(58.6814331952138,43.4543602574352,0.));
#110251=CARTESIAN_POINT('Ctrl Pts',(58.6814331952138,43.4543602574352,12.));
#110252=CARTESIAN_POINT('Ctrl Pts',(58.6948673358639,43.4764034109655,0.));
#110253=CARTESIAN_POINT('Ctrl Pts',(58.6948673358639,43.4764034109655,12.));
#110254=CARTESIAN_POINT('Ctrl Pts',(58.708300757066,43.4984920061071,0.));
#110255=CARTESIAN_POINT('Ctrl Pts',(58.708300757066,43.4984920061071,12.));
#110256=CARTESIAN_POINT('Ctrl Pts',(58.7217333624206,43.5206259848333,0.));
#110257=CARTESIAN_POINT('Ctrl Pts',(58.7217333624206,43.5206259848333,12.));
#110258=CARTESIAN_POINT('Ctrl Pts',(58.7351650559176,43.5428052892483,0.));
#110259=CARTESIAN_POINT('Ctrl Pts',(58.7351650559176,43.5428052892483,12.));
#110260=CARTESIAN_POINT('Ctrl Pts',(58.7485957419296,43.5650298615912,0.));
#110261=CARTESIAN_POINT('Ctrl Pts',(58.7485957419296,43.5650298615912,12.));
#110262=CARTESIAN_POINT('Ctrl Pts',(58.7620253252059,43.5872996442343,0.));
#110263=CARTESIAN_POINT('Ctrl Pts',(58.7620253252059,43.5872996442343,12.));
#110264=CARTESIAN_POINT('Ctrl Pts',(58.7754537108672,43.6096145796798,0.));
#110265=CARTESIAN_POINT('Ctrl Pts',(58.7754537108672,43.6096145796798,12.));
#110266=CARTESIAN_POINT('Ctrl Pts',(58.7888808043976,43.6319746105488,0.));
#110267=CARTESIAN_POINT('Ctrl Pts',(58.7888808043976,43.6319746105488,12.));
#110268=CARTESIAN_POINT('Ctrl Pts',(58.8023065116446,43.6543796795797,0.));
#110269=CARTESIAN_POINT('Ctrl Pts',(58.8023065116446,43.6543796795797,12.));
#110270=CARTESIAN_POINT('Ctrl Pts',(58.8157307388247,43.6768297296403,0.));
#110271=CARTESIAN_POINT('Ctrl Pts',(58.8157307388247,43.6768297296403,12.));
#110272=CARTESIAN_POINT('Ctrl Pts',(58.8291533925299,43.6993247037318,0.));
#110273=CARTESIAN_POINT('Ctrl Pts',(58.8291533925299,43.6993247037318,12.));
#110274=CARTESIAN_POINT('Ctrl Pts',(58.8425743797325,43.7218645449921,0.));
#110275=CARTESIAN_POINT('Ctrl Pts',(58.8425743797325,43.7218645449921,12.));
#110276=CARTESIAN_POINT('Ctrl Pts',(58.8559936077933,43.7444491966935,0.));
#110277=CARTESIAN_POINT('Ctrl Pts',(58.8559936077933,43.7444491966935,12.));
#110278=CARTESIAN_POINT('Ctrl Pts',(58.8694109844636,43.7670786022392,0.));
#110279=CARTESIAN_POINT('Ctrl Pts',(58.8694109844636,43.7670786022392,12.));
#110280=CARTESIAN_POINT('Ctrl Pts',(58.882826417861,43.7897527051599,0.));
#110281=CARTESIAN_POINT('Ctrl Pts',(58.882826417861,43.7897527051599,12.));
#110282=CARTESIAN_POINT('Ctrl Pts',(58.8962398164486,43.812471449107,0.));
#110283=CARTESIAN_POINT('Ctrl Pts',(58.8962398164486,43.812471449107,12.));
#110284=CARTESIAN_POINT('Ctrl Pts',(58.9096510890128,43.8352347778419,0.));
#110285=CARTESIAN_POINT('Ctrl Pts',(58.9096510890128,43.8352347778419,12.));
#110286=CARTESIAN_POINT('Ctrl Pts',(58.9230601446445,43.8580426352236,0.));
#110287=CARTESIAN_POINT('Ctrl Pts',(58.9230601446445,43.8580426352236,12.));
#110288=CARTESIAN_POINT('Ctrl Pts',(58.9364668927132,43.8808949651882,0.));
#110289=CARTESIAN_POINT('Ctrl Pts',(58.9364668927132,43.8808949651882,12.));
#110290=CARTESIAN_POINT('Ctrl Pts',(58.9498712429066,43.9037917117749,0.));
#110291=CARTESIAN_POINT('Ctrl Pts',(58.9498712429066,43.9037917117749,12.));
#110292=CARTESIAN_POINT('Ctrl Pts',(58.9632731052704,43.9267328191508,0.));
#110293=CARTESIAN_POINT('Ctrl Pts',(58.9632731052704,43.9267328191508,12.));
#110294=CARTESIAN_POINT('Ctrl Pts',(58.9766723902531,43.9497182316333,0.));
#110295=CARTESIAN_POINT('Ctrl Pts',(58.9766723902531,43.9497182316333,12.));
#110296=CARTESIAN_POINT('Ctrl Pts',(58.9900690087404,43.9727478937053,0.));
#110297=CARTESIAN_POINT('Ctrl Pts',(58.9900690087404,43.9727478937053,12.));
#110298=CARTESIAN_POINT('Ctrl Pts',(59.0034628721161,43.9958217500364,0.));
#110299=CARTESIAN_POINT('Ctrl Pts',(59.0034628721161,43.9958217500364,12.));
#110300=CARTESIAN_POINT('Ctrl Pts',(59.0168538922087,44.0189397454593,0.));
#110301=CARTESIAN_POINT('Ctrl Pts',(59.0168538922087,44.0189397454593,12.));
#110302=CARTESIAN_POINT('Ctrl Pts',(59.0302419811772,44.0421018249219,0.));
#110303=CARTESIAN_POINT('Ctrl Pts',(59.0302419811772,44.0421018249219,12.));
#110304=CARTESIAN_POINT('Ctrl Pts',(59.0436270514085,44.0653079334384,0.));
#110305=CARTESIAN_POINT('Ctrl Pts',(59.0436270514085,44.0653079334384,12.));
#110306=CARTESIAN_POINT('Ctrl Pts',(59.0570090154243,44.0885580160433,0.));
#110307=CARTESIAN_POINT('Ctrl Pts',(59.0570090154243,44.0885580160433,12.));
#110308=CARTESIAN_POINT('Ctrl Pts',(59.0703877857529,44.1118520177224,0.));
#110309=CARTESIAN_POINT('Ctrl Pts',(59.0703877857529,44.1118520177224,12.));
#110310=CARTESIAN_POINT('Ctrl Pts',(59.0837632749209,44.1351898834057,0.));
#110311=CARTESIAN_POINT('Ctrl Pts',(59.0837632749209,44.1351898834057,12.));
#110312=CARTESIAN_POINT('Ctrl Pts',(59.0971353957218,44.1585715581074,0.));
#110313=CARTESIAN_POINT('Ctrl Pts',(59.0971353957218,44.1585715581074,12.));
#110314=CARTESIAN_POINT('Ctrl Pts',(59.1105040614285,44.1819969870314,0.));
#110315=CARTESIAN_POINT('Ctrl Pts',(59.1105040614285,44.1819969870314,12.));
#110316=CARTESIAN_POINT('Ctrl Pts',(59.1238691860307,44.2054661156876,0.));
#110317=CARTESIAN_POINT('Ctrl Pts',(59.1238691860307,44.2054661156876,12.));
#110318=CARTESIAN_POINT('Ctrl Pts',(59.1372306844575,44.2289788899962,0.));
#110319=CARTESIAN_POINT('Ctrl Pts',(59.1372306844575,44.2289788899962,12.));
#110320=CARTESIAN_POINT('Ctrl Pts',(59.1505884728194,44.2525352563979,0.));
#110321=CARTESIAN_POINT('Ctrl Pts',(59.1505884728194,44.2525352563979,12.));
#110322=CARTESIAN_POINT('Ctrl Pts',(59.1639424678766,44.2761351616027,0.));
#110323=CARTESIAN_POINT('Ctrl Pts',(59.1639424678766,44.2761351616027,12.));
#110324=CARTESIAN_POINT('Ctrl Pts',(59.1772925865191,44.2997785523413,0.));
#110325=CARTESIAN_POINT('Ctrl Pts',(59.1772925865191,44.2997785523413,12.));
#110326=CARTESIAN_POINT('Ctrl Pts',(59.1906387451971,44.3234653750877,0.));
#110327=CARTESIAN_POINT('Ctrl Pts',(59.1906387451971,44.3234653750877,12.));
#110328=CARTESIAN_POINT('Ctrl Pts',(59.2039808594765,44.3471955758412,0.));
#110329=CARTESIAN_POINT('Ctrl Pts',(59.2039808594765,44.3471955758412,12.));
#110330=CARTESIAN_POINT('Ctrl Pts',(59.217318843283,44.3709690997495,0.));
#110331=CARTESIAN_POINT('Ctrl Pts',(59.217318843283,44.3709690997495,12.));
#110332=CARTESIAN_POINT('Ctrl Pts',(59.2306526095175,44.394785891411,0.));
#110333=CARTESIAN_POINT('Ctrl Pts',(59.2306526095175,44.394785891411,12.));
#110334=CARTESIAN_POINT('Ctrl Pts',(59.2439820714231,44.4186458955486,0.));
#110335=CARTESIAN_POINT('Ctrl Pts',(59.2439820714231,44.4186458955486,12.));
#110336=CARTESIAN_POINT('Ctrl Pts',(59.2573071437801,44.4425490575932,0.));
#110337=CARTESIAN_POINT('Ctrl Pts',(59.2573071437801,44.4425490575932,12.));
#110338=CARTESIAN_POINT('Ctrl Pts',(59.2706277440438,44.4664953242373,0.));
#110339=CARTESIAN_POINT('Ctrl Pts',(59.2706277440438,44.4664953242373,12.));
#110340=CARTESIAN_POINT('Ctrl Pts',(59.2839437938187,44.490484644147,0.));
#110341=CARTESIAN_POINT('Ctrl Pts',(59.2839437938187,44.490484644147,12.));
#110342=CARTESIAN_POINT('Ctrl Pts',(59.2972552192072,44.514516968128,0.));
#110343=CARTESIAN_POINT('Ctrl Pts',(59.2972552192072,44.514516968128,12.));
#110344=CARTESIAN_POINT('Ctrl Pts',(59.3105619475512,44.5385922475494,0.));
#110345=CARTESIAN_POINT('Ctrl Pts',(59.3105619475512,44.5385922475494,12.));
#110346=CARTESIAN_POINT('Ctrl Pts',(59.3238639048618,44.5627104330956,0.));
#110347=CARTESIAN_POINT('Ctrl Pts',(59.3238639048618,44.5627104330956,12.));
#110348=CARTESIAN_POINT('Ctrl Pts',(59.3371610128494,44.586871473322,0.));
#110349=CARTESIAN_POINT('Ctrl Pts',(59.3371610128494,44.586871473322,12.));
#110350=CARTESIAN_POINT('Ctrl Pts',(59.3504531864223,44.6110753134333,0.));
#110351=CARTESIAN_POINT('Ctrl Pts',(59.3504531864223,44.6110753134333,12.));
#110352=CARTESIAN_POINT('Ctrl Pts',(59.3637403301959,44.6353218935813,0.));
#110353=CARTESIAN_POINT('Ctrl Pts',(59.3637403301959,44.6353218935813,12.));
#110354=CARTESIAN_POINT('Ctrl Pts',(59.3770223435405,44.6596111512861,0.));
#110355=CARTESIAN_POINT('Ctrl Pts',(59.3770223435405,44.6596111512861,12.));
#110356=CARTESIAN_POINT('Ctrl Pts',(59.3902991268094,44.6839430244376,0.));
#110357=CARTESIAN_POINT('Ctrl Pts',(59.3902991268094,44.6839430244376,12.));
#110358=CARTESIAN_POINT('Ctrl Pts',(59.403570587392,44.708317454179,0.));
#110359=CARTESIAN_POINT('Ctrl Pts',(59.403570587392,44.708317454179,12.));
#110360=CARTESIAN_POINT('Ctrl Pts',(59.4168366453047,44.7327343876333,0.));
#110361=CARTESIAN_POINT('Ctrl Pts',(59.4168366453047,44.7327343876333,12.));
#110362=CARTESIAN_POINT('Ctrl Pts',(59.4300972402943,44.7571937811872,0.));
#110363=CARTESIAN_POINT('Ctrl Pts',(59.4300972402943,44.7571937811872,12.));
#110364=CARTESIAN_POINT('Ctrl Pts',(59.4433523334651,44.7816956017127,0.));
#110365=CARTESIAN_POINT('Ctrl Pts',(59.4433523334651,44.7816956017127,12.));
#110366=CARTESIAN_POINT('Ctrl Pts',(59.4566019017674,44.8062398250937,0.));
#110367=CARTESIAN_POINT('Ctrl Pts',(59.4566019017674,44.8062398250937,12.));
#110368=CARTESIAN_POINT('Ctrl Pts',(59.4671971277837,44.8259091133624,0.));
#110369=CARTESIAN_POINT('Ctrl Pts',(59.4671971277837,44.8259091133624,12.));
#110370=CARTESIAN_POINT('Ctrl Pts',(59.475141054744,44.8406801497506,0.));
#110371=CARTESIAN_POINT('Ctrl Pts',(59.475141054744,44.8406801497506,12.));
#110372=CARTESIAN_POINT('Ctrl Pts',(59.4804358982977,44.8505359826374,0.));
#110373=CARTESIAN_POINT('Ctrl Pts',(59.4804358982977,44.8505359826374,12.));
#110374=CARTESIAN_POINT('Ctrl Pts',(59.483083043136,44.8554660179045,0.));
#110375=CARTESIAN_POINT('Ctrl Pts',(59.483083043136,44.8554660179045,12.));
#110376=CARTESIAN_POINT('',(56.8466430164621,40.8467768343956,0.));
#110377=CARTESIAN_POINT('Ctrl Pts',(56.8466430164621,40.8467768343956,0.));
#110378=CARTESIAN_POINT('Ctrl Pts',(56.8491101022591,40.8497761671036,0.));
#110379=CARTESIAN_POINT('Ctrl Pts',(56.8540460739472,40.8557803680278,0.));
#110380=CARTESIAN_POINT('Ctrl Pts',(56.8614554317668,40.864803275942,0.));
#110381=CARTESIAN_POINT('Ctrl Pts',(56.8713453764905,40.8768670342052,0.));
#110382=CARTESIAN_POINT('Ctrl Pts',(56.8837257978343,40.8920020903293,0.));
#110383=CARTESIAN_POINT('Ctrl Pts',(56.8961241708861,40.9071924937508,0.));
#110384=CARTESIAN_POINT('Ctrl Pts',(56.9085404164502,40.9224382132427,0.));
#110385=CARTESIAN_POINT('Ctrl Pts',(56.9209743960992,40.9377391857129,0.));
#110386=CARTESIAN_POINT('Ctrl Pts',(56.9334259140049,40.9530953165031,0.));
#110387=CARTESIAN_POINT('Ctrl Pts',(56.9458947422608,40.9685064933074,0.));
#110388=CARTESIAN_POINT('Ctrl Pts',(56.9583806404069,40.9839725967121,0.));
#110389=CARTESIAN_POINT('Ctrl Pts',(56.9708833766137,40.9994935117276,0.));
#110390=CARTESIAN_POINT('Ctrl Pts',(56.9834027500117,41.0150691398947,0.));
#110391=CARTESIAN_POINT('Ctrl Pts',(56.995938583472,41.0306993953989,0.));
#110392=CARTESIAN_POINT('Ctrl Pts',(57.008490713042,41.0463841993608,0.));
#110393=CARTESIAN_POINT('Ctrl Pts',(57.0210589791788,41.0621234751007,0.));
#110394=CARTESIAN_POINT('Ctrl Pts',(57.0336432158536,41.0779171422438,0.));
#110395=CARTESIAN_POINT('Ctrl Pts',(57.046243245068,41.0937651137549,0.));
#110396=CARTESIAN_POINT('Ctrl Pts',(57.0588588825298,41.1096672990148,0.));
#110397=CARTESIAN_POINT('Ctrl Pts',(57.0714899412099,41.1256236057443,0.));
#110398=CARTESIAN_POINT('Ctrl Pts',(57.084136235426,41.1416339422117,0.));
#110399=CARTESIAN_POINT('Ctrl Pts',(57.0967975854874,41.1576982197375,0.));
#110400=CARTESIAN_POINT('Ctrl Pts',(57.1094738174957,41.1738163525902,0.));
#110401=CARTESIAN_POINT('Ctrl Pts',(57.1221647611207,41.1899882567923,0.));
#110402=CARTESIAN_POINT('Ctrl Pts',(57.1348702480647,41.2062138492915,0.));
#110403=CARTESIAN_POINT('Ctrl Pts',(57.147590110182,41.222493046943,0.));
#110404=CARTESIAN_POINT('Ctrl Pts',(57.1603241779077,41.2388257656559,0.));
#110405=CARTESIAN_POINT('Ctrl Pts',(57.17307228108,41.2552119208466,0.));
#110406=CARTESIAN_POINT('Ctrl Pts',(57.1858342496538,41.2716514278276,0.));
#110407=CARTESIAN_POINT('Ctrl Pts',(57.1986099143983,41.2881442021863,0.));
#110408=CARTESIAN_POINT('Ctrl Pts',(57.2113991077302,41.3046901602293,0.));
#110409=CARTESIAN_POINT('Ctrl Pts',(57.2242016640198,41.321289219149,0.));
#110410=CARTESIAN_POINT('Ctrl Pts',(57.2370174191401,41.3379412967875,0.));
#110411=CARTESIAN_POINT('Ctrl Pts',(57.2498462101879,41.3546463114885,0.));
#110412=CARTESIAN_POINT('Ctrl Pts',(57.2626878751596,41.3714041819224,0.));
#110413=CARTESIAN_POINT('Ctrl Pts',(57.2755422525844,41.3882148268814,0.));
#110414=CARTESIAN_POINT('Ctrl Pts',(57.2884091815406,41.4050781652938,0.));
#110415=CARTESIAN_POINT('Ctrl Pts',(57.3012885018151,41.4219941163163,0.));
#110416=CARTESIAN_POINT('Ctrl Pts',(57.3141800540137,41.4389625993948,0.));
#110417=CARTESIAN_POINT('Ctrl Pts',(57.3270836796911,41.4559835343328,0.));
#110418=CARTESIAN_POINT('Ctrl Pts',(57.3399992214717,41.4730568413518,0.));
#110419=CARTESIAN_POINT('Ctrl Pts',(57.3529265229835,41.4901824410637,0.));
#110420=CARTESIAN_POINT('Ctrl Pts',(57.3658654287937,41.5073602544396,0.));
#110421=CARTESIAN_POINT('Ctrl Pts',(57.3788157843454,41.5245902027771,0.));
#110422=CARTESIAN_POINT('Ctrl Pts',(57.3917774358863,41.5418722076572,0.));
#110423=CARTESIAN_POINT('Ctrl Pts',(57.4047502304231,41.5592061909176,0.));
#110424=CARTESIAN_POINT('Ctrl Pts',(57.4177340157508,41.5765920746777,0.));
#110425=CARTESIAN_POINT('Ctrl Pts',(57.4307286404662,41.5940297813477,0.));
#110426=CARTESIAN_POINT('Ctrl Pts',(57.4437339539841,41.6115192336388,0.));
#110427=CARTESIAN_POINT('Ctrl Pts',(57.4567498065562,41.6290603545666,0.));
#110428=CARTESIAN_POINT('Ctrl Pts',(57.4697760492683,41.6466530674515,0.));
#110429=CARTESIAN_POINT('Ctrl Pts',(57.4828125340218,41.6642972959165,0.));
#110430=CARTESIAN_POINT('Ctrl Pts',(57.4958591135165,41.6819929638797,0.));
#110431=CARTESIAN_POINT('Ctrl Pts',(57.5089156412343,41.6997399955447,0.));
#110432=CARTESIAN_POINT('Ctrl Pts',(57.5219819714171,41.7175383153821,0.));
#110433=CARTESIAN_POINT('Ctrl Pts',(57.5350579590649,41.7353878481337,0.));
#110434=CARTESIAN_POINT('Ctrl Pts',(57.5481434599335,41.7532885188175,0.));
#110435=CARTESIAN_POINT('Ctrl Pts',(57.561238330532,41.7712402527273,0.));
#110436=CARTESIAN_POINT('Ctrl Pts',(57.5743424281204,41.7892429754297,0.));
#110437=CARTESIAN_POINT('Ctrl Pts',(57.5874556107056,41.8072966127558,0.));
#110438=CARTESIAN_POINT('Ctrl Pts',(57.6005777370349,41.8254010908051,0.));
#110439=CARTESIAN_POINT('Ctrl Pts',(57.6137086665882,41.8435563359456,0.));
#110440=CARTESIAN_POINT('Ctrl Pts',(57.6268482595702,41.8617622748108,0.));
#110441=CARTESIAN_POINT('Ctrl Pts',(57.6399963769003,41.8800188342909,0.));
#110442=CARTESIAN_POINT('Ctrl Pts',(57.6531528802059,41.8983259415245,0.));
#110443=CARTESIAN_POINT('Ctrl Pts',(57.6663176318176,41.9166835239046,0.));
#110444=CARTESIAN_POINT('Ctrl Pts',(57.6794904947641,41.9350915090791,0.));
#110445=CARTESIAN_POINT('Ctrl Pts',(57.6926713327674,41.9535498249489,0.));
#110446=CARTESIAN_POINT('Ctrl Pts',(57.7058600102365,41.9720583996601,0.));
#110447=CARTESIAN_POINT('Ctrl Pts',(57.7190563922614,41.9906171615975,0.));
#110448=CARTESIAN_POINT('Ctrl Pts',(57.7322603446086,42.0092260393911,0.));
#110449=CARTESIAN_POINT('Ctrl Pts',(57.7454717337151,42.0278849619156,0.));
#110450=CARTESIAN_POINT('Ctrl Pts',(57.7586904266828,42.0465938582878,0.));
#110451=CARTESIAN_POINT('Ctrl Pts',(57.7719162912721,42.0653526578571,0.));
#110452=CARTESIAN_POINT('Ctrl Pts',(57.7851491958954,42.0841612902018,0.));
#110453=CARTESIAN_POINT('Ctrl Pts',(57.798389009613,42.1030196851344,0.));
#110454=CARTESIAN_POINT('Ctrl Pts',(57.8116356021274,42.121927772701,0.));
#110455=CARTESIAN_POINT('Ctrl Pts',(57.8248888437787,42.1408854831792,0.));
#110456=CARTESIAN_POINT('Ctrl Pts',(57.8381486055376,42.1598927470671,0.));
#110457=CARTESIAN_POINT('Ctrl Pts',(57.8514147590012,42.1789494950824,0.));
#110458=CARTESIAN_POINT('Ctrl Pts',(57.86468717639,42.1980556581689,0.));
#110459=CARTESIAN_POINT('Ctrl Pts',(57.8779657305422,42.2172111674946,0.));
#110460=CARTESIAN_POINT('Ctrl Pts',(57.8912502949084,42.2364159544492,0.));
#110461=CARTESIAN_POINT('Ctrl Pts',(57.9045407435447,42.2556699506332,0.));
#110462=CARTESIAN_POINT('Ctrl Pts',(57.9178369511084,42.274973087857,0.));
#110463=CARTESIAN_POINT('Ctrl Pts',(57.9311387928541,42.2943252981471,0.));
#110464=CARTESIAN_POINT('Ctrl Pts',(57.9444461446292,42.3137265137446,0.));
#110465=CARTESIAN_POINT('Ctrl Pts',(57.9577588828693,42.3331766671028,0.));
#110466=CARTESIAN_POINT('Ctrl Pts',(57.9710768845923,42.3526756908764,0.));
#110467=CARTESIAN_POINT('Ctrl Pts',(57.9844000273936,42.3722235179216,0.));
#110468=CARTESIAN_POINT('Ctrl Pts',(57.9977281894437,42.3918200813025,0.));
#110469=CARTESIAN_POINT('Ctrl Pts',(58.011061249483,42.4114653142891,0.));
#110470=CARTESIAN_POINT('Ctrl Pts',(58.0243990868175,42.4311591503551,0.));
#110471=CARTESIAN_POINT('Ctrl Pts',(58.0377415813132,42.4509015231668,0.));
#110472=CARTESIAN_POINT('Ctrl Pts',(58.0510886133917,42.4706923665838,0.));
#110473=CARTESIAN_POINT('Ctrl Pts',(58.064440064027,42.490531614665,0.));
#110474=CARTESIAN_POINT('Ctrl Pts',(58.0777958147404,42.5104192016664,0.));
#110475=CARTESIAN_POINT('Ctrl Pts',(58.0911557475967,42.5303550620388,0.));
#110476=CARTESIAN_POINT('Ctrl Pts',(58.1045197452003,42.5503391304183,0.));
#110477=CARTESIAN_POINT('Ctrl Pts',(58.1178876906905,42.5703713416263,0.));
#110478=CARTESIAN_POINT('Ctrl Pts',(58.1312594677383,42.5904516306759,0.));
#110479=CARTESIAN_POINT('Ctrl Pts',(58.1446349605419,42.6105799327697,0.));
#110480=CARTESIAN_POINT('Ctrl Pts',(58.158014053823,42.6307561832978,0.));
#110481=CARTESIAN_POINT('Ctrl Pts',(58.1713966328217,42.650980317827,0.));
#110482=CARTESIAN_POINT('Ctrl Pts',(58.1847825832932,42.6712522721021,0.));
#110483=CARTESIAN_POINT('Ctrl Pts',(58.1981717915043,42.6915719820517,0.));
#110484=CARTESIAN_POINT('Ctrl Pts',(58.2115641442302,42.7119393837867,0.));
#110485=CARTESIAN_POINT('Ctrl Pts',(58.2249595287497,42.7323544135983,0.));
#110486=CARTESIAN_POINT('Ctrl Pts',(58.238357832842,42.7528170079482,0.));
#110487=CARTESIAN_POINT('Ctrl Pts',(58.2517589447818,42.7733271034679,0.));
#110488=CARTESIAN_POINT('Ctrl Pts',(58.2651627533368,42.7938846369651,0.));
#110489=CARTESIAN_POINT('Ctrl Pts',(58.278569147764,42.8144895454234,0.));
#110490=CARTESIAN_POINT('Ctrl Pts',(58.2919780178063,42.8351417659998,0.));
#110491=CARTESIAN_POINT('Ctrl Pts',(58.305389253689,42.8558412360154,0.));
#110492=CARTESIAN_POINT('Ctrl Pts',(58.3188027461157,42.8765878929545,0.));
#110493=CARTESIAN_POINT('Ctrl Pts',(58.3322183862647,42.8973816744703,0.));
#110494=CARTESIAN_POINT('Ctrl Pts',(58.3456360657861,42.9182225183851,0.));
#110495=CARTESIAN_POINT('Ctrl Pts',(58.3590556767981,42.9391103626881,0.));
#110496=CARTESIAN_POINT('Ctrl Pts',(58.3724771118835,42.9600451455267,0.));
#110497=CARTESIAN_POINT('Ctrl Pts',(58.3859002640871,42.9810268052043,0.));
#110498=CARTESIAN_POINT('Ctrl Pts',(58.3993250269115,43.002055280187,0.));
#110499=CARTESIAN_POINT('Ctrl Pts',(58.4127512943144,43.0231305091033,0.));
#110500=CARTESIAN_POINT('Ctrl Pts',(58.4261789607055,43.0442524307432,0.));
#110501=CARTESIAN_POINT('Ctrl Pts',(58.4396079209438,43.0654209840502,0.));
#110502=CARTESIAN_POINT('Ctrl Pts',(58.4530380703335,43.0866361081166,0.));
#110503=CARTESIAN_POINT('Ctrl Pts',(58.4664693046206,43.1078977421908,0.));
#110504=CARTESIAN_POINT('Ctrl Pts',(58.4799015199904,43.1292058256774,0.));
#110505=CARTESIAN_POINT('Ctrl Pts',(58.4933346130638,43.1505602981366,0.));
#110506=CARTESIAN_POINT('Ctrl Pts',(58.5067684808946,43.1719610992772,0.));
#110507=CARTESIAN_POINT('Ctrl Pts',(58.5202030209667,43.1934081689504,0.));
#110508=CARTESIAN_POINT('Ctrl Pts',(58.5336381311911,43.214901447157,0.));
#110509=CARTESIAN_POINT('Ctrl Pts',(58.5470737099027,43.2364408740489,0.));
#110510=CARTESIAN_POINT('Ctrl Pts',(58.5605096558578,43.2580263899278,0.));
#110511=CARTESIAN_POINT('Ctrl Pts',(58.5739458682317,43.2796579352405,0.));
#110512=CARTESIAN_POINT('Ctrl Pts',(58.5873822466163,43.3013354505708,0.));
#110513=CARTESIAN_POINT('Ctrl Pts',(58.6008186910166,43.3230588766456,0.));
#110514=CARTESIAN_POINT('Ctrl Pts',(58.6142551018473,43.3448281543375,0.));
#110515=CARTESIAN_POINT('Ctrl Pts',(58.627691379929,43.3666432246635,0.));
#110516=CARTESIAN_POINT('Ctrl Pts',(58.6411274264854,43.3885040287808,0.));
#110517=CARTESIAN_POINT('Ctrl Pts',(58.6545631431388,43.4104105079766,0.));
#110518=CARTESIAN_POINT('Ctrl Pts',(58.6679984319095,43.4323626036736,0.));
#110519=CARTESIAN_POINT('Ctrl Pts',(58.6814331952138,43.4543602574352,0.));
#110520=CARTESIAN_POINT('Ctrl Pts',(58.6948673358639,43.4764034109655,0.));
#110521=CARTESIAN_POINT('Ctrl Pts',(58.708300757066,43.4984920061071,0.));
#110522=CARTESIAN_POINT('Ctrl Pts',(58.7217333624206,43.5206259848333,0.));
#110523=CARTESIAN_POINT('Ctrl Pts',(58.7351650559176,43.5428052892483,0.));
#110524=CARTESIAN_POINT('Ctrl Pts',(58.7485957419296,43.5650298615912,0.));
#110525=CARTESIAN_POINT('Ctrl Pts',(58.7620253252059,43.5872996442343,0.));
#110526=CARTESIAN_POINT('Ctrl Pts',(58.7754537108672,43.6096145796798,0.));
#110527=CARTESIAN_POINT('Ctrl Pts',(58.7888808043976,43.6319746105488,0.));
#110528=CARTESIAN_POINT('Ctrl Pts',(58.8023065116446,43.6543796795797,0.));
#110529=CARTESIAN_POINT('Ctrl Pts',(58.8157307388247,43.6768297296403,0.));
#110530=CARTESIAN_POINT('Ctrl Pts',(58.8291533925299,43.6993247037318,0.));
#110531=CARTESIAN_POINT('Ctrl Pts',(58.8425743797325,43.7218645449921,0.));
#110532=CARTESIAN_POINT('Ctrl Pts',(58.8559936077933,43.7444491966935,0.));
#110533=CARTESIAN_POINT('Ctrl Pts',(58.8694109844636,43.7670786022392,0.));
#110534=CARTESIAN_POINT('Ctrl Pts',(58.882826417861,43.7897527051599,0.));
#110535=CARTESIAN_POINT('Ctrl Pts',(58.8962398164486,43.812471449107,0.));
#110536=CARTESIAN_POINT('Ctrl Pts',(58.9096510890128,43.8352347778419,0.));
#110537=CARTESIAN_POINT('Ctrl Pts',(58.9230601446445,43.8580426352236,0.));
#110538=CARTESIAN_POINT('Ctrl Pts',(58.9364668927132,43.8808949651882,0.));
#110539=CARTESIAN_POINT('Ctrl Pts',(58.9498712429066,43.9037917117749,0.));
#110540=CARTESIAN_POINT('Ctrl Pts',(58.9632731052704,43.9267328191508,0.));
#110541=CARTESIAN_POINT('Ctrl Pts',(58.9766723902531,43.9497182316333,0.));
#110542=CARTESIAN_POINT('Ctrl Pts',(58.9900690087404,43.9727478937053,0.));
#110543=CARTESIAN_POINT('Ctrl Pts',(59.0034628721161,43.9958217500364,0.));
#110544=CARTESIAN_POINT('Ctrl Pts',(59.0168538922087,44.0189397454593,0.));
#110545=CARTESIAN_POINT('Ctrl Pts',(59.0302419811772,44.0421018249219,0.));
#110546=CARTESIAN_POINT('Ctrl Pts',(59.0436270514085,44.0653079334384,0.));
#110547=CARTESIAN_POINT('Ctrl Pts',(59.0570090154243,44.0885580160433,0.));
#110548=CARTESIAN_POINT('Ctrl Pts',(59.0703877857529,44.1118520177224,0.));
#110549=CARTESIAN_POINT('Ctrl Pts',(59.0837632749209,44.1351898834057,0.));
#110550=CARTESIAN_POINT('Ctrl Pts',(59.0971353957218,44.1585715581074,0.));
#110551=CARTESIAN_POINT('Ctrl Pts',(59.1105040614285,44.1819969870314,0.));
#110552=CARTESIAN_POINT('Ctrl Pts',(59.1238691860307,44.2054661156876,0.));
#110553=CARTESIAN_POINT('Ctrl Pts',(59.1372306844575,44.2289788899962,0.));
#110554=CARTESIAN_POINT('Ctrl Pts',(59.1505884728194,44.2525352563979,0.));
#110555=CARTESIAN_POINT('Ctrl Pts',(59.1639424678766,44.2761351616027,0.));
#110556=CARTESIAN_POINT('Ctrl Pts',(59.1772925865191,44.2997785523413,0.));
#110557=CARTESIAN_POINT('Ctrl Pts',(59.1906387451971,44.3234653750877,0.));
#110558=CARTESIAN_POINT('Ctrl Pts',(59.2039808594765,44.3471955758412,0.));
#110559=CARTESIAN_POINT('Ctrl Pts',(59.217318843283,44.3709690997495,0.));
#110560=CARTESIAN_POINT('Ctrl Pts',(59.2306526095175,44.394785891411,0.));
#110561=CARTESIAN_POINT('Ctrl Pts',(59.2439820714231,44.4186458955486,0.));
#110562=CARTESIAN_POINT('Ctrl Pts',(59.2573071437801,44.4425490575932,0.));
#110563=CARTESIAN_POINT('Ctrl Pts',(59.2706277440438,44.4664953242373,0.));
#110564=CARTESIAN_POINT('Ctrl Pts',(59.2839437938187,44.490484644147,0.));
#110565=CARTESIAN_POINT('Ctrl Pts',(59.2972552192072,44.514516968128,0.));
#110566=CARTESIAN_POINT('Ctrl Pts',(59.3086616639392,44.5351541478336,0.));
#110567=CARTESIAN_POINT('Ctrl Pts',(59.317404187219,44.5509994357954,0.));
#110568=CARTESIAN_POINT('Ctrl Pts',(59.3234848865279,44.5620338188487,0.));
#110569=CARTESIAN_POINT('Ctrl Pts',(59.3269051738223,44.5682447395714,0.));
#110570=CARTESIAN_POINT('Ctrl Pts',(59.3276657444159,44.5696260757422,0.));
#110571=CARTESIAN_POINT('',(56.8466430164621,40.8467768343956,12.));
#110572=CARTESIAN_POINT('',(56.8466430164621,40.8467768343956,0.));
#110573=CARTESIAN_POINT('Ctrl Pts',(59.3276657444159,44.5696260757422,12.));
#110574=CARTESIAN_POINT('Ctrl Pts',(59.3269051738223,44.5682447395714,12.));
#110575=CARTESIAN_POINT('Ctrl Pts',(59.3234848865279,44.5620338188486,12.));
#110576=CARTESIAN_POINT('Ctrl Pts',(59.317404187219,44.5509994357954,12.));
#110577=CARTESIAN_POINT('Ctrl Pts',(59.3086616639392,44.5351541478336,12.));
#110578=CARTESIAN_POINT('Ctrl Pts',(59.2972552192072,44.514516968128,12.));
#110579=CARTESIAN_POINT('Ctrl Pts',(59.2839437938187,44.490484644147,12.));
#110580=CARTESIAN_POINT('Ctrl Pts',(59.2706277440438,44.4664953242373,12.));
#110581=CARTESIAN_POINT('Ctrl Pts',(59.2573071437801,44.4425490575932,12.));
#110582=CARTESIAN_POINT('Ctrl Pts',(59.2439820714231,44.4186458955486,12.));
#110583=CARTESIAN_POINT('Ctrl Pts',(59.2306526095175,44.394785891411,12.));
#110584=CARTESIAN_POINT('Ctrl Pts',(59.217318843283,44.3709690997495,12.));
#110585=CARTESIAN_POINT('Ctrl Pts',(59.2039808594765,44.3471955758412,12.));
#110586=CARTESIAN_POINT('Ctrl Pts',(59.1906387451971,44.3234653750877,12.));
#110587=CARTESIAN_POINT('Ctrl Pts',(59.1772925865191,44.2997785523413,12.));
#110588=CARTESIAN_POINT('Ctrl Pts',(59.1639424678766,44.2761351616027,12.));
#110589=CARTESIAN_POINT('Ctrl Pts',(59.1505884728194,44.2525352563979,12.));
#110590=CARTESIAN_POINT('Ctrl Pts',(59.1372306844575,44.2289788899962,12.));
#110591=CARTESIAN_POINT('Ctrl Pts',(59.1238691860307,44.2054661156876,12.));
#110592=CARTESIAN_POINT('Ctrl Pts',(59.1105040614285,44.1819969870314,12.));
#110593=CARTESIAN_POINT('Ctrl Pts',(59.0971353957218,44.1585715581074,12.));
#110594=CARTESIAN_POINT('Ctrl Pts',(59.0837632749209,44.1351898834057,12.));
#110595=CARTESIAN_POINT('Ctrl Pts',(59.0703877857529,44.1118520177224,12.));
#110596=CARTESIAN_POINT('Ctrl Pts',(59.0570090154243,44.0885580160433,12.));
#110597=CARTESIAN_POINT('Ctrl Pts',(59.0436270514085,44.0653079334384,12.));
#110598=CARTESIAN_POINT('Ctrl Pts',(59.0302419811772,44.0421018249219,12.));
#110599=CARTESIAN_POINT('Ctrl Pts',(59.0168538922087,44.0189397454593,12.));
#110600=CARTESIAN_POINT('Ctrl Pts',(59.0034628721161,43.9958217500364,12.));
#110601=CARTESIAN_POINT('Ctrl Pts',(58.9900690087404,43.9727478937053,12.));
#110602=CARTESIAN_POINT('Ctrl Pts',(58.9766723902531,43.9497182316333,12.));
#110603=CARTESIAN_POINT('Ctrl Pts',(58.9632731052704,43.9267328191508,12.));
#110604=CARTESIAN_POINT('Ctrl Pts',(58.9498712429066,43.9037917117749,12.));
#110605=CARTESIAN_POINT('Ctrl Pts',(58.9364668927132,43.8808949651882,12.));
#110606=CARTESIAN_POINT('Ctrl Pts',(58.9230601446445,43.8580426352236,12.));
#110607=CARTESIAN_POINT('Ctrl Pts',(58.9096510890128,43.8352347778419,12.));
#110608=CARTESIAN_POINT('Ctrl Pts',(58.8962398164486,43.812471449107,12.));
#110609=CARTESIAN_POINT('Ctrl Pts',(58.882826417861,43.7897527051599,12.));
#110610=CARTESIAN_POINT('Ctrl Pts',(58.8694109844636,43.7670786022392,12.));
#110611=CARTESIAN_POINT('Ctrl Pts',(58.8559936077933,43.7444491966935,12.));
#110612=CARTESIAN_POINT('Ctrl Pts',(58.8425743797325,43.7218645449921,12.));
#110613=CARTESIAN_POINT('Ctrl Pts',(58.8291533925299,43.6993247037318,12.));
#110614=CARTESIAN_POINT('Ctrl Pts',(58.8157307388247,43.6768297296403,12.));
#110615=CARTESIAN_POINT('Ctrl Pts',(58.8023065116446,43.6543796795797,12.));
#110616=CARTESIAN_POINT('Ctrl Pts',(58.7888808043976,43.6319746105488,12.));
#110617=CARTESIAN_POINT('Ctrl Pts',(58.7754537108672,43.6096145796798,12.));
#110618=CARTESIAN_POINT('Ctrl Pts',(58.7620253252059,43.5872996442343,12.));
#110619=CARTESIAN_POINT('Ctrl Pts',(58.7485957419296,43.5650298615912,12.));
#110620=CARTESIAN_POINT('Ctrl Pts',(58.7351650559176,43.5428052892483,12.));
#110621=CARTESIAN_POINT('Ctrl Pts',(58.7217333624206,43.5206259848333,12.));
#110622=CARTESIAN_POINT('Ctrl Pts',(58.708300757066,43.4984920061071,12.));
#110623=CARTESIAN_POINT('Ctrl Pts',(58.6948673358639,43.4764034109655,12.));
#110624=CARTESIAN_POINT('Ctrl Pts',(58.6814331952138,43.4543602574352,12.));
#110625=CARTESIAN_POINT('Ctrl Pts',(58.6679984319095,43.4323626036736,12.));
#110626=CARTESIAN_POINT('Ctrl Pts',(58.6545631431388,43.4104105079766,12.));
#110627=CARTESIAN_POINT('Ctrl Pts',(58.6411274264854,43.3885040287808,12.));
#110628=CARTESIAN_POINT('Ctrl Pts',(58.627691379929,43.3666432246635,12.));
#110629=CARTESIAN_POINT('Ctrl Pts',(58.6142551018473,43.3448281543375,12.));
#110630=CARTESIAN_POINT('Ctrl Pts',(58.6008186910166,43.3230588766456,12.));
#110631=CARTESIAN_POINT('Ctrl Pts',(58.5873822466163,43.3013354505708,12.));
#110632=CARTESIAN_POINT('Ctrl Pts',(58.5739458682317,43.2796579352405,12.));
#110633=CARTESIAN_POINT('Ctrl Pts',(58.5605096558578,43.2580263899278,12.));
#110634=CARTESIAN_POINT('Ctrl Pts',(58.5470737099027,43.2364408740489,12.));
#110635=CARTESIAN_POINT('Ctrl Pts',(58.5336381311911,43.214901447157,12.));
#110636=CARTESIAN_POINT('Ctrl Pts',(58.5202030209667,43.1934081689504,12.));
#110637=CARTESIAN_POINT('Ctrl Pts',(58.5067684808946,43.1719610992772,12.));
#110638=CARTESIAN_POINT('Ctrl Pts',(58.4933346130638,43.1505602981366,12.));
#110639=CARTESIAN_POINT('Ctrl Pts',(58.4799015199904,43.1292058256774,12.));
#110640=CARTESIAN_POINT('Ctrl Pts',(58.4664693046206,43.1078977421908,12.));
#110641=CARTESIAN_POINT('Ctrl Pts',(58.4530380703335,43.0866361081166,12.));
#110642=CARTESIAN_POINT('Ctrl Pts',(58.4396079209438,43.0654209840502,12.));
#110643=CARTESIAN_POINT('Ctrl Pts',(58.4261789607055,43.0442524307432,12.));
#110644=CARTESIAN_POINT('Ctrl Pts',(58.4127512943144,43.0231305091033,12.));
#110645=CARTESIAN_POINT('Ctrl Pts',(58.3993250269115,43.002055280187,12.));
#110646=CARTESIAN_POINT('Ctrl Pts',(58.3859002640871,42.9810268052043,12.));
#110647=CARTESIAN_POINT('Ctrl Pts',(58.3724771118835,42.9600451455267,12.));
#110648=CARTESIAN_POINT('Ctrl Pts',(58.3590556767981,42.9391103626881,12.));
#110649=CARTESIAN_POINT('Ctrl Pts',(58.3456360657861,42.9182225183851,12.));
#110650=CARTESIAN_POINT('Ctrl Pts',(58.3322183862647,42.8973816744703,12.));
#110651=CARTESIAN_POINT('Ctrl Pts',(58.3188027461157,42.8765878929545,12.));
#110652=CARTESIAN_POINT('Ctrl Pts',(58.305389253689,42.8558412360154,12.));
#110653=CARTESIAN_POINT('Ctrl Pts',(58.2919780178063,42.8351417659998,12.));
#110654=CARTESIAN_POINT('Ctrl Pts',(58.278569147764,42.8144895454234,12.));
#110655=CARTESIAN_POINT('Ctrl Pts',(58.2651627533368,42.7938846369651,12.));
#110656=CARTESIAN_POINT('Ctrl Pts',(58.2517589447818,42.7733271034679,12.));
#110657=CARTESIAN_POINT('Ctrl Pts',(58.238357832842,42.7528170079482,12.));
#110658=CARTESIAN_POINT('Ctrl Pts',(58.2249595287497,42.7323544135983,12.));
#110659=CARTESIAN_POINT('Ctrl Pts',(58.2115641442302,42.7119393837867,12.));
#110660=CARTESIAN_POINT('Ctrl Pts',(58.1981717915043,42.6915719820517,12.));
#110661=CARTESIAN_POINT('Ctrl Pts',(58.1847825832932,42.6712522721021,12.));
#110662=CARTESIAN_POINT('Ctrl Pts',(58.1713966328217,42.650980317827,12.));
#110663=CARTESIAN_POINT('Ctrl Pts',(58.158014053823,42.6307561832978,12.));
#110664=CARTESIAN_POINT('Ctrl Pts',(58.1446349605419,42.6105799327697,12.));
#110665=CARTESIAN_POINT('Ctrl Pts',(58.1312594677383,42.5904516306759,12.));
#110666=CARTESIAN_POINT('Ctrl Pts',(58.1178876906905,42.5703713416263,12.));
#110667=CARTESIAN_POINT('Ctrl Pts',(58.1045197452003,42.5503391304183,12.));
#110668=CARTESIAN_POINT('Ctrl Pts',(58.0911557475967,42.5303550620388,12.));
#110669=CARTESIAN_POINT('Ctrl Pts',(58.0777958147404,42.5104192016664,12.));
#110670=CARTESIAN_POINT('Ctrl Pts',(58.064440064027,42.490531614665,12.));
#110671=CARTESIAN_POINT('Ctrl Pts',(58.0510886133917,42.4706923665838,12.));
#110672=CARTESIAN_POINT('Ctrl Pts',(58.0377415813132,42.4509015231668,12.));
#110673=CARTESIAN_POINT('Ctrl Pts',(58.0243990868175,42.4311591503551,12.));
#110674=CARTESIAN_POINT('Ctrl Pts',(58.011061249483,42.4114653142891,12.));
#110675=CARTESIAN_POINT('Ctrl Pts',(57.9977281894437,42.3918200813025,12.));
#110676=CARTESIAN_POINT('Ctrl Pts',(57.9844000273936,42.3722235179216,12.));
#110677=CARTESIAN_POINT('Ctrl Pts',(57.9710768845923,42.3526756908764,12.));
#110678=CARTESIAN_POINT('Ctrl Pts',(57.9577588828693,42.3331766671028,12.));
#110679=CARTESIAN_POINT('Ctrl Pts',(57.9444461446292,42.3137265137446,12.));
#110680=CARTESIAN_POINT('Ctrl Pts',(57.9311387928541,42.2943252981471,12.));
#110681=CARTESIAN_POINT('Ctrl Pts',(57.9178369511084,42.274973087857,12.));
#110682=CARTESIAN_POINT('Ctrl Pts',(57.9045407435447,42.2556699506332,12.));
#110683=CARTESIAN_POINT('Ctrl Pts',(57.8912502949084,42.2364159544492,12.));
#110684=CARTESIAN_POINT('Ctrl Pts',(57.8779657305422,42.2172111674946,12.));
#110685=CARTESIAN_POINT('Ctrl Pts',(57.86468717639,42.1980556581689,12.));
#110686=CARTESIAN_POINT('Ctrl Pts',(57.8514147590012,42.1789494950824,12.));
#110687=CARTESIAN_POINT('Ctrl Pts',(57.8381486055376,42.1598927470671,12.));
#110688=CARTESIAN_POINT('Ctrl Pts',(57.8248888437787,42.1408854831792,12.));
#110689=CARTESIAN_POINT('Ctrl Pts',(57.8116356021274,42.121927772701,12.));
#110690=CARTESIAN_POINT('Ctrl Pts',(57.798389009613,42.1030196851344,12.));
#110691=CARTESIAN_POINT('Ctrl Pts',(57.7851491958954,42.0841612902018,12.));
#110692=CARTESIAN_POINT('Ctrl Pts',(57.7719162912721,42.0653526578571,12.));
#110693=CARTESIAN_POINT('Ctrl Pts',(57.7586904266828,42.0465938582878,12.));
#110694=CARTESIAN_POINT('Ctrl Pts',(57.7454717337151,42.0278849619156,12.));
#110695=CARTESIAN_POINT('Ctrl Pts',(57.7322603446086,42.0092260393911,12.));
#110696=CARTESIAN_POINT('Ctrl Pts',(57.7190563922614,41.9906171615975,12.));
#110697=CARTESIAN_POINT('Ctrl Pts',(57.7058600102365,41.9720583996601,12.));
#110698=CARTESIAN_POINT('Ctrl Pts',(57.6926713327674,41.9535498249489,12.));
#110699=CARTESIAN_POINT('Ctrl Pts',(57.6794904947641,41.9350915090791,12.));
#110700=CARTESIAN_POINT('Ctrl Pts',(57.6663176318176,41.9166835239046,12.));
#110701=CARTESIAN_POINT('Ctrl Pts',(57.6531528802059,41.8983259415245,12.));
#110702=CARTESIAN_POINT('Ctrl Pts',(57.6399963769003,41.8800188342909,12.));
#110703=CARTESIAN_POINT('Ctrl Pts',(57.6268482595702,41.8617622748108,12.));
#110704=CARTESIAN_POINT('Ctrl Pts',(57.6137086665882,41.8435563359456,12.));
#110705=CARTESIAN_POINT('Ctrl Pts',(57.6005777370349,41.8254010908051,12.));
#110706=CARTESIAN_POINT('Ctrl Pts',(57.5874556107056,41.8072966127558,12.));
#110707=CARTESIAN_POINT('Ctrl Pts',(57.5743424281204,41.7892429754297,12.));
#110708=CARTESIAN_POINT('Ctrl Pts',(57.561238330532,41.7712402527273,12.));
#110709=CARTESIAN_POINT('Ctrl Pts',(57.5481434599335,41.7532885188175,12.));
#110710=CARTESIAN_POINT('Ctrl Pts',(57.5350579590649,41.7353878481337,12.));
#110711=CARTESIAN_POINT('Ctrl Pts',(57.5219819714171,41.7175383153821,12.));
#110712=CARTESIAN_POINT('Ctrl Pts',(57.5089156412343,41.6997399955447,12.));
#110713=CARTESIAN_POINT('Ctrl Pts',(57.4958591135165,41.6819929638797,12.));
#110714=CARTESIAN_POINT('Ctrl Pts',(57.4828125340218,41.6642972959165,12.));
#110715=CARTESIAN_POINT('Ctrl Pts',(57.4697760492683,41.6466530674515,12.));
#110716=CARTESIAN_POINT('Ctrl Pts',(57.4567498065562,41.6290603545666,12.));
#110717=CARTESIAN_POINT('Ctrl Pts',(57.4437339539841,41.6115192336388,12.));
#110718=CARTESIAN_POINT('Ctrl Pts',(57.4307286404662,41.5940297813477,12.));
#110719=CARTESIAN_POINT('Ctrl Pts',(57.4177340157508,41.5765920746777,12.));
#110720=CARTESIAN_POINT('Ctrl Pts',(57.4047502304231,41.5592061909176,12.));
#110721=CARTESIAN_POINT('Ctrl Pts',(57.3917774358863,41.5418722076572,12.));
#110722=CARTESIAN_POINT('Ctrl Pts',(57.3788157843454,41.5245902027771,12.));
#110723=CARTESIAN_POINT('Ctrl Pts',(57.3658654287937,41.5073602544396,12.));
#110724=CARTESIAN_POINT('Ctrl Pts',(57.3529265229835,41.4901824410637,12.));
#110725=CARTESIAN_POINT('Ctrl Pts',(57.3399992214717,41.4730568413518,12.));
#110726=CARTESIAN_POINT('Ctrl Pts',(57.3270836796911,41.4559835343328,12.));
#110727=CARTESIAN_POINT('Ctrl Pts',(57.3141800540137,41.4389625993948,12.));
#110728=CARTESIAN_POINT('Ctrl Pts',(57.3012885018151,41.4219941163163,12.));
#110729=CARTESIAN_POINT('Ctrl Pts',(57.2884091815406,41.4050781652938,12.));
#110730=CARTESIAN_POINT('Ctrl Pts',(57.2755422525844,41.3882148268814,12.));
#110731=CARTESIAN_POINT('Ctrl Pts',(57.2626878751596,41.3714041819224,12.));
#110732=CARTESIAN_POINT('Ctrl Pts',(57.2498462101879,41.3546463114885,12.));
#110733=CARTESIAN_POINT('Ctrl Pts',(57.2370174191401,41.3379412967875,12.));
#110734=CARTESIAN_POINT('Ctrl Pts',(57.2242016640198,41.321289219149,12.));
#110735=CARTESIAN_POINT('Ctrl Pts',(57.2113991077302,41.3046901602293,12.));
#110736=CARTESIAN_POINT('Ctrl Pts',(57.1986099143983,41.2881442021863,12.));
#110737=CARTESIAN_POINT('Ctrl Pts',(57.1858342496538,41.2716514278276,12.));
#110738=CARTESIAN_POINT('Ctrl Pts',(57.17307228108,41.2552119208466,12.));
#110739=CARTESIAN_POINT('Ctrl Pts',(57.1603241779077,41.2388257656559,12.));
#110740=CARTESIAN_POINT('Ctrl Pts',(57.147590110182,41.222493046943,12.));
#110741=CARTESIAN_POINT('Ctrl Pts',(57.1348702480647,41.2062138492915,12.));
#110742=CARTESIAN_POINT('Ctrl Pts',(57.1221647611207,41.1899882567923,12.));
#110743=CARTESIAN_POINT('Ctrl Pts',(57.1094738174957,41.1738163525902,12.));
#110744=CARTESIAN_POINT('Ctrl Pts',(57.0967975854874,41.1576982197375,12.));
#110745=CARTESIAN_POINT('Ctrl Pts',(57.084136235426,41.1416339422117,12.));
#110746=CARTESIAN_POINT('Ctrl Pts',(57.0714899412099,41.1256236057443,12.));
#110747=CARTESIAN_POINT('Ctrl Pts',(57.0588588825298,41.1096672990148,12.));
#110748=CARTESIAN_POINT('Ctrl Pts',(57.046243245068,41.0937651137549,12.));
#110749=CARTESIAN_POINT('Ctrl Pts',(57.0336432158536,41.0779171422438,12.));
#110750=CARTESIAN_POINT('Ctrl Pts',(57.0210589791788,41.0621234751007,12.));
#110751=CARTESIAN_POINT('Ctrl Pts',(57.008490713042,41.0463841993608,12.));
#110752=CARTESIAN_POINT('Ctrl Pts',(56.995938583472,41.0306993953989,12.));
#110753=CARTESIAN_POINT('Ctrl Pts',(56.9834027500117,41.0150691398947,12.));
#110754=CARTESIAN_POINT('Ctrl Pts',(56.9708833766137,40.9994935117276,12.));
#110755=CARTESIAN_POINT('Ctrl Pts',(56.9583806404069,40.9839725967121,12.));
#110756=CARTESIAN_POINT('Ctrl Pts',(56.9458947422608,40.9685064933074,12.));
#110757=CARTESIAN_POINT('Ctrl Pts',(56.9334259140049,40.9530953165031,12.));
#110758=CARTESIAN_POINT('Ctrl Pts',(56.9209743960992,40.9377391857129,12.));
#110759=CARTESIAN_POINT('Ctrl Pts',(56.9085404164502,40.9224382132427,12.));
#110760=CARTESIAN_POINT('Ctrl Pts',(56.8961241708861,40.9071924937508,12.));
#110761=CARTESIAN_POINT('Ctrl Pts',(56.8837257978343,40.8920020903293,12.));
#110762=CARTESIAN_POINT('Ctrl Pts',(56.8713453764905,40.8768670342052,12.));
#110763=CARTESIAN_POINT('Ctrl Pts',(56.8614554317668,40.864803275942,12.));
#110764=CARTESIAN_POINT('Ctrl Pts',(56.8540460739472,40.8557803680278,12.));
#110765=CARTESIAN_POINT('Ctrl Pts',(56.8491101022591,40.8497761671036,12.));
#110766=CARTESIAN_POINT('Ctrl Pts',(56.8466430164621,40.8467768343956,12.));
#110767=CARTESIAN_POINT('Ctrl Pts',(58.4060826907792,45.7706564944895,-5.55111512312578E-16));
#110768=CARTESIAN_POINT('Ctrl Pts',(58.4060826907792,45.7706564944895,4.));
#110769=CARTESIAN_POINT('Ctrl Pts',(58.4060826907792,45.7706564944895,8.));
#110770=CARTESIAN_POINT('Ctrl Pts',(58.4060826907792,45.7706564944895,12.));
#110771=CARTESIAN_POINT('Ctrl Pts',(58.5127761886842,45.7969367893064,-5.55111512312578E-16));
#110772=CARTESIAN_POINT('Ctrl Pts',(58.5127761886842,45.7969367893064,4.));
#110773=CARTESIAN_POINT('Ctrl Pts',(58.5127761886843,45.7969367893065,8.00000000000001));
#110774=CARTESIAN_POINT('Ctrl Pts',(58.5127761886843,45.7969367893065,12.));
#110775=CARTESIAN_POINT('Ctrl Pts',(58.7146322050558,45.7788617791412,-5.55111512312578E-16));
#110776=CARTESIAN_POINT('Ctrl Pts',(58.7146322050558,45.7788617791412,4.));
#110777=CARTESIAN_POINT('Ctrl Pts',(58.7146322050559,45.7788617791413,7.99999999999999));
#110778=CARTESIAN_POINT('Ctrl Pts',(58.7146322050559,45.7788617791413,12.));
#110779=CARTESIAN_POINT('Ctrl Pts',(58.870677144318,45.6563266621664,-5.55111512312578E-16));
#110780=CARTESIAN_POINT('Ctrl Pts',(58.870677144318,45.6563266621664,4.));
#110781=CARTESIAN_POINT('Ctrl Pts',(58.870677144318,45.6563266621664,8.00000000000001));
#110782=CARTESIAN_POINT('Ctrl Pts',(58.870677144318,45.6563266621664,12.));
#110783=CARTESIAN_POINT('Ctrl Pts',(58.9211100416379,45.5911481700253,-5.55111512312578E-16));
#110784=CARTESIAN_POINT('Ctrl Pts',(58.9211100416379,45.5911481700253,4.));
#110785=CARTESIAN_POINT('Ctrl Pts',(58.9211100416379,45.5911481700253,8.));
#110786=CARTESIAN_POINT('Ctrl Pts',(58.9211100416379,45.5911481700253,12.));
#110787=CARTESIAN_POINT('',(58.4060826907792,45.7706564944895,2.77555756156289E-16));
#110788=CARTESIAN_POINT('',(58.9211100416379,45.5911481700253,0.));
#110789=CARTESIAN_POINT('Ctrl Pts',(58.4060826907792,45.7706564944895,-1.38777878078145E-16));
#110790=CARTESIAN_POINT('Ctrl Pts',(58.5127761886842,45.7969367893064,-1.38777878078145E-16));
#110791=CARTESIAN_POINT('Ctrl Pts',(58.6281224837537,45.7866082120692,-1.38777878078144E-16));
#110792=CARTESIAN_POINT('Ctrl Pts',(58.7285100597671,45.7421702122002,-1.38777878078145E-16));
#110793=CARTESIAN_POINT('Ctrl Pts',(58.8038007417771,45.7088417122985,-1.38777878078145E-16));
#110794=CARTESIAN_POINT('Ctrl Pts',(58.870677144318,45.6563266621664,-1.38777878078145E-16));
#110795=CARTESIAN_POINT('Ctrl Pts',(58.9211100416379,45.5911481700253,-1.38777878078145E-16));
#110796=CARTESIAN_POINT('',(58.9211100416379,45.5911481700253,12.));
#110797=CARTESIAN_POINT('Ctrl Pts',(58.9211100416379,45.5911481700253,-5.55111512312578E-16));
#110798=CARTESIAN_POINT('Ctrl Pts',(58.9211100416379,45.5911481700253,4.));
#110799=CARTESIAN_POINT('Ctrl Pts',(58.9211100416379,45.5911481700253,8.));
#110800=CARTESIAN_POINT('Ctrl Pts',(58.9211100416379,45.5911481700253,12.));
#110801=CARTESIAN_POINT('',(58.4060826907792,45.7706564944895,12.));
#110802=CARTESIAN_POINT('Ctrl Pts',(58.9211100416379,45.5911481700253,12.));
#110803=CARTESIAN_POINT('Ctrl Pts',(58.870677144318,45.6563266621664,12.));
#110804=CARTESIAN_POINT('Ctrl Pts',(58.8038007417771,45.7088417122985,12.));
#110805=CARTESIAN_POINT('Ctrl Pts',(58.7285100597671,45.7421702122002,12.));
#110806=CARTESIAN_POINT('Ctrl Pts',(58.6281224837538,45.7866082120692,12.));
#110807=CARTESIAN_POINT('Ctrl Pts',(58.5127761886843,45.7969367893065,12.));
#110808=CARTESIAN_POINT('Ctrl Pts',(58.4060826907792,45.7706564944895,12.));
#110809=CARTESIAN_POINT('Ctrl Pts',(58.4060826907792,45.7706564944895,12.));
#110810=CARTESIAN_POINT('Ctrl Pts',(58.4060826907792,45.7706564944895,8.));
#110811=CARTESIAN_POINT('Ctrl Pts',(58.4060826907792,45.7706564944895,4.));
#110812=CARTESIAN_POINT('Ctrl Pts',(58.4060826907792,45.7706564944895,-5.55111512312578E-16));
#110813=CARTESIAN_POINT('Origin',(2.97323128204029E-10,2.28269173065022E-10,
0.));
#110814=CARTESIAN_POINT('Origin',(2.97323128204029E-10,2.28269173065022E-10,
12.));
#110815=CARTESIAN_POINT('Origin',(2.97323128204029E-10,2.28269173065022E-10,
0.));
#110816=CARTESIAN_POINT('Ctrl Pts',(62.9938720098768,39.77464128315,0.));
#110817=CARTESIAN_POINT('Ctrl Pts',(62.9938720098768,39.77464128315,4.));
#110818=CARTESIAN_POINT('Ctrl Pts',(62.9938720098768,39.77464128315,8.));
#110819=CARTESIAN_POINT('Ctrl Pts',(62.9938720098768,39.77464128315,12.));
#110820=CARTESIAN_POINT('Ctrl Pts',(63.0525369183203,39.681729578236,0.));
#110821=CARTESIAN_POINT('Ctrl Pts',(63.0525369183203,39.681729578236,4.));
#110822=CARTESIAN_POINT('Ctrl Pts',(63.0525369183204,39.6817295782359,8.00000000000001));
#110823=CARTESIAN_POINT('Ctrl Pts',(63.0525369183204,39.6817295782359,12.));
#110824=CARTESIAN_POINT('Ctrl Pts',(63.099209014761,39.484513183097,0.));
#110825=CARTESIAN_POINT('Ctrl Pts',(63.099209014761,39.484513183097,4.));
#110826=CARTESIAN_POINT('Ctrl Pts',(63.099209014761,39.484513183097,7.99999999999999));
#110827=CARTESIAN_POINT('Ctrl Pts',(63.099209014761,39.484513183097,12.));
#110828=CARTESIAN_POINT('Ctrl Pts',(63.032294972791,39.2977314459986,0.));
#110829=CARTESIAN_POINT('Ctrl Pts',(63.032294972791,39.2977314459986,4.));
#110830=CARTESIAN_POINT('Ctrl Pts',(63.0322949727911,39.2977314459985,8.00000000000001));
#110831=CARTESIAN_POINT('Ctrl Pts',(63.0322949727911,39.2977314459985,12.));
#110832=CARTESIAN_POINT('Ctrl Pts',(62.9864049293638,39.2292784191469,0.));
#110833=CARTESIAN_POINT('Ctrl Pts',(62.9864049293638,39.2292784191469,4.));
#110834=CARTESIAN_POINT('Ctrl Pts',(62.986404929364,39.2292784191468,8.));
#110835=CARTESIAN_POINT('Ctrl Pts',(62.986404929364,39.2292784191468,12.));
#110836=CARTESIAN_POINT('',(62.9938720098768,39.77464128315,0.));
#110837=CARTESIAN_POINT('',(62.9864049293634,39.2292784191472,0.));
#110838=CARTESIAN_POINT('Ctrl Pts',(62.9938720098768,39.77464128315,2.77555756156289E-16));
#110839=CARTESIAN_POINT('Ctrl Pts',(63.0525369183203,39.681729578236,2.77555756156289E-16));
#110840=CARTESIAN_POINT('Ctrl Pts',(63.079206687715,39.5690344952994,2.77555756156289E-16));
#110841=CARTESIAN_POINT('Ctrl Pts',(63.0687871057919,39.4597466476414,2.77555756156289E-16));
#110842=CARTESIAN_POINT('Ctrl Pts',(63.0609724193496,39.3777807618979,2.77555756156289E-16));
#110843=CARTESIAN_POINT('Ctrl Pts',(63.032294972791,39.2977314459986,2.77555756156289E-16));
#110844=CARTESIAN_POINT('Ctrl Pts',(62.9864049293638,39.2292784191469,2.77555756156289E-16));
#110845=CARTESIAN_POINT('',(62.9864049293634,39.2292784191472,12.));
#110846=CARTESIAN_POINT('Ctrl Pts',(62.9864049293638,39.2292784191469,0.));
#110847=CARTESIAN_POINT('Ctrl Pts',(62.9864049293638,39.2292784191469,4.));
#110848=CARTESIAN_POINT('Ctrl Pts',(62.986404929364,39.2292784191468,8.));
#110849=CARTESIAN_POINT('Ctrl Pts',(62.986404929364,39.2292784191468,12.));
#110850=CARTESIAN_POINT('',(62.9938720098768,39.77464128315,12.));
#110851=CARTESIAN_POINT('Ctrl Pts',(62.986404929364,39.2292784191468,12.));
#110852=CARTESIAN_POINT('Ctrl Pts',(63.0322949727911,39.2977314459985,12.));
#110853=CARTESIAN_POINT('Ctrl Pts',(63.0609724193497,39.3777807618979,12.));
#110854=CARTESIAN_POINT('Ctrl Pts',(63.068787105792,39.4597466476414,12.));
#110855=CARTESIAN_POINT('Ctrl Pts',(63.079206687715,39.5690344952994,12.));
#110856=CARTESIAN_POINT('Ctrl Pts',(63.0525369183204,39.6817295782359,12.));
#110857=CARTESIAN_POINT('Ctrl Pts',(62.9938720098768,39.77464128315,12.));
#110858=CARTESIAN_POINT('Ctrl Pts',(62.9938720098768,39.77464128315,12.));
#110859=CARTESIAN_POINT('Ctrl Pts',(62.9938720098768,39.77464128315,8.));
#110860=CARTESIAN_POINT('Ctrl Pts',(62.9938720098768,39.77464128315,4.));
#110861=CARTESIAN_POINT('Ctrl Pts',(62.9938720098768,39.77464128315,0.));
#110862=CARTESIAN_POINT('Ctrl Pts',(60.1903555511633,35.7368311217509,0.));
#110863=CARTESIAN_POINT('Ctrl Pts',(60.1903555511633,35.7368311217509,12.));
#110864=CARTESIAN_POINT('Ctrl Pts',(60.1930746580239,35.7396040203973,0.));
#110865=CARTESIAN_POINT('Ctrl Pts',(60.1930746580239,35.7396040203973,12.));
#110866=CARTESIAN_POINT('Ctrl Pts',(60.1985151474406,35.7451551752456,0.));
#110867=CARTESIAN_POINT('Ctrl Pts',(60.1985151474406,35.7451551752456,12.));
#110868=CARTESIAN_POINT('Ctrl Pts',(60.2066827086579,35.7534979801871,0.));
#110869=CARTESIAN_POINT('Ctrl Pts',(60.2066827086579,35.7534979801871,12.));
#110870=CARTESIAN_POINT('Ctrl Pts',(60.2175864449678,35.7646538667299,0.));
#110871=CARTESIAN_POINT('Ctrl Pts',(60.2175864449678,35.7646538667299,12.));
#110872=CARTESIAN_POINT('Ctrl Pts',(60.2312388621286,35.7786523045782,0.));
#110873=CARTESIAN_POINT('Ctrl Pts',(60.2312388621286,35.7786523045782,12.));
#110874=CARTESIAN_POINT('Ctrl Pts',(60.2449139865206,35.7927043145165,0.));
#110875=CARTESIAN_POINT('Ctrl Pts',(60.2449139865206,35.7927043145165,12.));
#110876=CARTESIAN_POINT('Ctrl Pts',(60.2586117365278,35.8068098723386,0.));
#110877=CARTESIAN_POINT('Ctrl Pts',(60.2586117365278,35.8068098723386,12.));
#110878=CARTESIAN_POINT('Ctrl Pts',(60.2723319687507,35.8209689272574,0.));
#110879=CARTESIAN_POINT('Ctrl Pts',(60.2723319687507,35.8209689272574,12.));
#110880=CARTESIAN_POINT('Ctrl Pts',(60.2860744798563,35.8351814020424,0.));
#110881=CARTESIAN_POINT('Ctrl Pts',(60.2860744798563,35.8351814020424,12.));
#110882=CARTESIAN_POINT('Ctrl Pts',(60.2998390330173,35.8494472046784,0.));
#110883=CARTESIAN_POINT('Ctrl Pts',(60.2998390330173,35.8494472046784,12.));
#110884=CARTESIAN_POINT('Ctrl Pts',(60.313625378281,35.8637662371635,0.));
#110885=CARTESIAN_POINT('Ctrl Pts',(60.313625378281,35.8637662371635,12.));
#110886=CARTESIAN_POINT('Ctrl Pts',(60.3274332746782,35.878138405151,0.));
#110887=CARTESIAN_POINT('Ctrl Pts',(60.3274332746782,35.878138405151,12.));
#110888=CARTESIAN_POINT('Ctrl Pts',(60.3412625135223,35.8925636280632,0.));
#110889=CARTESIAN_POINT('Ctrl Pts',(60.3412625135223,35.8925636280632,12.));
#110890=CARTESIAN_POINT('Ctrl Pts',(60.3551129108794,35.9070418358501,0.));
#110891=CARTESIAN_POINT('Ctrl Pts',(60.3551129108794,35.9070418358501,12.));
#110892=CARTESIAN_POINT('Ctrl Pts',(60.368984296546,35.9215729642219,0.));
#110893=CARTESIAN_POINT('Ctrl Pts',(60.368984296546,35.9215729642219,12.));
#110894=CARTESIAN_POINT('Ctrl Pts',(60.3828765049031,35.9361569506955,0.));
#110895=CARTESIAN_POINT('Ctrl Pts',(60.3828765049031,35.9361569506955,12.));
#110896=CARTESIAN_POINT('Ctrl Pts',(60.3967893635487,35.9507937296726,0.));
#110897=CARTESIAN_POINT('Ctrl Pts',(60.3967893635487,35.9507937296726,12.));
#110898=CARTESIAN_POINT('Ctrl Pts',(60.4107226875759,35.9654832299627,0.));
#110899=CARTESIAN_POINT('Ctrl Pts',(60.4107226875759,35.9654832299627,12.));
#110900=CARTESIAN_POINT('Ctrl Pts',(60.4246762854961,35.9802253773534,0.));
#110901=CARTESIAN_POINT('Ctrl Pts',(60.4246762854961,35.9802253773534,12.));
#110902=CARTESIAN_POINT('Ctrl Pts',(60.438649962949,35.9950200962175,0.));
#110903=CARTESIAN_POINT('Ctrl Pts',(60.438649962949,35.9950200962175,12.));
#110904=CARTESIAN_POINT('Ctrl Pts',(60.452643526964,36.0098673113557,0.));
#110905=CARTESIAN_POINT('Ctrl Pts',(60.452643526964,36.0098673113557,12.));
#110906=CARTESIAN_POINT('Ctrl Pts',(60.4666567908053,36.0247669500867,0.));
#110907=CARTESIAN_POINT('Ctrl Pts',(60.4666567908053,36.0247669500867,12.));
#110908=CARTESIAN_POINT('Ctrl Pts',(60.4806895737643,36.0397189421617,0.));
#110909=CARTESIAN_POINT('Ctrl Pts',(60.4806895737643,36.0397189421617,12.));
#110910=CARTESIAN_POINT('Ctrl Pts',(60.4947416988396,36.0547232187681,0.));
#110911=CARTESIAN_POINT('Ctrl Pts',(60.4947416988396,36.0547232187681,12.));
#110912=CARTESIAN_POINT('Ctrl Pts',(60.5088129911357,36.0697797118377,0.));
#110913=CARTESIAN_POINT('Ctrl Pts',(60.5088129911357,36.0697797118377,12.));
#110914=CARTESIAN_POINT('Ctrl Pts',(60.5229032759001,36.0848883531969,0.));
#110915=CARTESIAN_POINT('Ctrl Pts',(60.5229032759001,36.0848883531969,12.));
#110916=CARTESIAN_POINT('Ctrl Pts',(60.5370123768841,36.1000490738532,0.));
#110917=CARTESIAN_POINT('Ctrl Pts',(60.5370123768841,36.1000490738532,12.));
#110918=CARTESIAN_POINT('Ctrl Pts',(60.5511401172014,36.1152618043756,0.));
#110919=CARTESIAN_POINT('Ctrl Pts',(60.5511401172014,36.1152618043756,12.));
#110920=CARTESIAN_POINT('Ctrl Pts',(60.5652863200732,36.1305264752195,0.));
#110921=CARTESIAN_POINT('Ctrl Pts',(60.5652863200732,36.1305264752195,12.));
#110922=CARTESIAN_POINT('Ctrl Pts',(60.5794508095555,36.1458430170425,0.));
#110923=CARTESIAN_POINT('Ctrl Pts',(60.5794508095555,36.1458430170425,12.));
#110924=CARTESIAN_POINT('Ctrl Pts',(60.5936334114082,36.1612113610758,0.));
#110925=CARTESIAN_POINT('Ctrl Pts',(60.5936334114082,36.1612113610758,12.));
#110926=CARTESIAN_POINT('Ctrl Pts',(60.6078339534151,36.1766314392624,0.));
#110927=CARTESIAN_POINT('Ctrl Pts',(60.6078339534151,36.1766314392624,12.));
#110928=CARTESIAN_POINT('Ctrl Pts',(60.6220522649129,36.1921031840618,0.));
#110929=CARTESIAN_POINT('Ctrl Pts',(60.6220522649129,36.1921031840618,12.));
#110930=CARTESIAN_POINT('Ctrl Pts',(60.6362881765014,36.2076265283261,0.));
#110931=CARTESIAN_POINT('Ctrl Pts',(60.6362881765014,36.2076265283261,12.));
#110932=CARTESIAN_POINT('Ctrl Pts',(60.6505415197055,36.2232014051549,0.));
#110933=CARTESIAN_POINT('Ctrl Pts',(60.6505415197055,36.2232014051549,12.));
#110934=CARTESIAN_POINT('Ctrl Pts',(60.6648121265908,36.2388277477225,0.));
#110935=CARTESIAN_POINT('Ctrl Pts',(60.6648121265908,36.2388277477225,12.));
#110936=CARTESIAN_POINT('Ctrl Pts',(60.6790998297823,36.2545054892911,0.));
#110937=CARTESIAN_POINT('Ctrl Pts',(60.6790998297823,36.2545054892911,12.));
#110938=CARTESIAN_POINT('Ctrl Pts',(60.6934044626304,36.2702345632883,0.));
#110939=CARTESIAN_POINT('Ctrl Pts',(60.6934044626304,36.2702345632883,12.));
#110940=CARTESIAN_POINT('Ctrl Pts',(60.7077258593268,36.2860149033586,0.));
#110941=CARTESIAN_POINT('Ctrl Pts',(60.7077258593268,36.2860149033586,12.));
#110942=CARTESIAN_POINT('Ctrl Pts',(60.7220638550396,36.3018464434204,0.));
#110943=CARTESIAN_POINT('Ctrl Pts',(60.7220638550396,36.3018464434204,12.));
#110944=CARTESIAN_POINT('Ctrl Pts',(60.7364182860388,36.3177291177148,0.));
#110945=CARTESIAN_POINT('Ctrl Pts',(60.7364182860388,36.3177291177148,12.));
#110946=CARTESIAN_POINT('Ctrl Pts',(60.7507889896283,36.3336628607844,0.));
#110947=CARTESIAN_POINT('Ctrl Pts',(60.7507889896283,36.3336628607844,12.));
#110948=CARTESIAN_POINT('Ctrl Pts',(60.7651758040791,36.349647607448,0.));
#110949=CARTESIAN_POINT('Ctrl Pts',(60.7651758040791,36.349647607448,12.));
#110950=CARTESIAN_POINT('Ctrl Pts',(60.779578568563,36.3656832927733,0.));
#110951=CARTESIAN_POINT('Ctrl Pts',(60.779578568563,36.3656832927733,12.));
#110952=CARTESIAN_POINT('Ctrl Pts',(60.7939971230781,36.38176985204,0.));
#110953=CARTESIAN_POINT('Ctrl Pts',(60.7939971230781,36.38176985204,12.));
#110954=CARTESIAN_POINT('Ctrl Pts',(60.8084313084009,36.3979072207174,0.));
#110955=CARTESIAN_POINT('Ctrl Pts',(60.8084313084009,36.3979072207174,12.));
#110956=CARTESIAN_POINT('Ctrl Pts',(60.8228809661179,36.414095334487,0.));
#110957=CARTESIAN_POINT('Ctrl Pts',(60.8228809661179,36.414095334487,12.));
#110958=CARTESIAN_POINT('Ctrl Pts',(60.8373459386397,36.4303341292497,0.));
#110959=CARTESIAN_POINT('Ctrl Pts',(60.8373459386397,36.4303341292497,12.));
#110960=CARTESIAN_POINT('Ctrl Pts',(60.851826069218,36.4466235411353,0.));
#110961=CARTESIAN_POINT('Ctrl Pts',(60.851826069218,36.4466235411353,12.));
#110962=CARTESIAN_POINT('Ctrl Pts',(60.8663212019646,36.4629635065037,0.));
#110963=CARTESIAN_POINT('Ctrl Pts',(60.8663212019646,36.4629635065037,12.));
#110964=CARTESIAN_POINT('Ctrl Pts',(60.8808311818489,36.4793539619459,0.));
#110965=CARTESIAN_POINT('Ctrl Pts',(60.8808311818489,36.4793539619459,12.));
#110966=CARTESIAN_POINT('Ctrl Pts',(60.8953558546791,36.4957948442832,0.));
#110967=CARTESIAN_POINT('Ctrl Pts',(60.8953558546791,36.4957948442832,12.));
#110968=CARTESIAN_POINT('Ctrl Pts',(60.9098950670847,36.5122860905611,0.));
#110969=CARTESIAN_POINT('Ctrl Pts',(60.9098950670847,36.5122860905611,12.));
#110970=CARTESIAN_POINT('Ctrl Pts',(60.924448666499,36.5288276380417,0.));
#110971=CARTESIAN_POINT('Ctrl Pts',(60.924448666499,36.5288276380417,12.));
#110972=CARTESIAN_POINT('Ctrl Pts',(60.9390165011357,36.5454194241866,0.));
#110973=CARTESIAN_POINT('Ctrl Pts',(60.9390165011357,36.5454194241866,12.));
#110974=CARTESIAN_POINT('Ctrl Pts',(60.9535984199874,36.5620613866616,0.));
#110975=CARTESIAN_POINT('Ctrl Pts',(60.9535984199874,36.5620613866616,12.));
#110976=CARTESIAN_POINT('Ctrl Pts',(60.9681942728237,36.5787534633416,0.));
#110977=CARTESIAN_POINT('Ctrl Pts',(60.9681942728237,36.5787534633416,12.));
#110978=CARTESIAN_POINT('Ctrl Pts',(60.9828039101887,36.5954955923109,0.));
#110979=CARTESIAN_POINT('Ctrl Pts',(60.9828039101887,36.5954955923109,12.));
#110980=CARTESIAN_POINT('Ctrl Pts',(60.9974271833982,36.6122877118599,0.));
#110981=CARTESIAN_POINT('Ctrl Pts',(60.9974271833982,36.6122877118599,12.));
#110982=CARTESIAN_POINT('Ctrl Pts',(61.012063944535,36.6291297604775,0.));
#110983=CARTESIAN_POINT('Ctrl Pts',(61.012063944535,36.6291297604775,12.));
#110984=CARTESIAN_POINT('Ctrl Pts',(61.0267140464434,36.6460216768553,0.));
#110985=CARTESIAN_POINT('Ctrl Pts',(61.0267140464434,36.6460216768553,12.));
#110986=CARTESIAN_POINT('Ctrl Pts',(61.0413773427204,36.6629633998886,0.));
#110987=CARTESIAN_POINT('Ctrl Pts',(61.0413773427204,36.6629633998886,12.));
#110988=CARTESIAN_POINT('Ctrl Pts',(61.0560536877084,36.6799548686741,0.));
#110989=CARTESIAN_POINT('Ctrl Pts',(61.0560536877084,36.6799548686741,12.));
#110990=CARTESIAN_POINT('Ctrl Pts',(61.0707429364841,36.6969960225019,0.));
#110991=CARTESIAN_POINT('Ctrl Pts',(61.0707429364841,36.6969960225019,12.));
#110992=CARTESIAN_POINT('Ctrl Pts',(61.085444944851,36.7140868008479,0.));
#110993=CARTESIAN_POINT('Ctrl Pts',(61.085444944851,36.7140868008479,12.));
#110994=CARTESIAN_POINT('Ctrl Pts',(61.1001595693357,36.7312271433799,0.));
#110995=CARTESIAN_POINT('Ctrl Pts',(61.1001595693357,36.7312271433799,12.));
#110996=CARTESIAN_POINT('Ctrl Pts',(61.1148866671821,36.7484169899591,0.));
#110997=CARTESIAN_POINT('Ctrl Pts',(61.1148866671821,36.7484169899591,12.));
#110998=CARTESIAN_POINT('Ctrl Pts',(61.1296260963468,36.7656562806381,0.));
#110999=CARTESIAN_POINT('Ctrl Pts',(61.1296260963468,36.7656562806381,12.));
#111000=CARTESIAN_POINT('Ctrl Pts',(61.1443777154926,36.782944955654,0.));
#111001=CARTESIAN_POINT('Ctrl Pts',(61.1443777154926,36.782944955654,12.));
#111002=CARTESIAN_POINT('Ctrl Pts',(61.1591413839809,36.8002829554221,0.));
#111003=CARTESIAN_POINT('Ctrl Pts',(61.1591413839809,36.8002829554221,12.));
#111004=CARTESIAN_POINT('Ctrl Pts',(61.1739169618688,36.8176702205436,0.));
#111005=CARTESIAN_POINT('Ctrl Pts',(61.1739169618688,36.8176702205436,12.));
#111006=CARTESIAN_POINT('Ctrl Pts',(61.1887043099026,36.8351066918043,0.));
#111007=CARTESIAN_POINT('Ctrl Pts',(61.1887043099026,36.8351066918043,12.));
#111008=CARTESIAN_POINT('Ctrl Pts',(61.2035032895121,36.8525923101736,0.));
#111009=CARTESIAN_POINT('Ctrl Pts',(61.2035032895121,36.8525923101736,12.));
#111010=CARTESIAN_POINT('Ctrl Pts',(61.2183137628031,36.8701270167954,0.));
#111011=CARTESIAN_POINT('Ctrl Pts',(61.2183137628031,36.8701270167954,12.));
#111012=CARTESIAN_POINT('Ctrl Pts',(61.2331355925513,36.8877107529844,0.));
#111013=CARTESIAN_POINT('Ctrl Pts',(61.2331355925513,36.8877107529844,12.));
#111014=CARTESIAN_POINT('Ctrl Pts',(61.2479686421979,36.9053434602324,0.));
#111015=CARTESIAN_POINT('Ctrl Pts',(61.2479686421979,36.9053434602324,12.));
#111016=CARTESIAN_POINT('Ctrl Pts',(61.2628127758443,36.9230250802079,0.));
#111017=CARTESIAN_POINT('Ctrl Pts',(61.2628127758443,36.9230250802079,12.));
#111018=CARTESIAN_POINT('Ctrl Pts',(61.2776678582474,36.9407555547542,0.));
#111019=CARTESIAN_POINT('Ctrl Pts',(61.2776678582474,36.9407555547542,12.));
#111020=CARTESIAN_POINT('Ctrl Pts',(61.2925337548113,36.9585348258798,0.));
#111021=CARTESIAN_POINT('Ctrl Pts',(61.2925337548113,36.9585348258798,12.));
#111022=CARTESIAN_POINT('Ctrl Pts',(61.3074103315834,36.976362835757,0.));
#111023=CARTESIAN_POINT('Ctrl Pts',(61.3074103315834,36.976362835757,12.));
#111024=CARTESIAN_POINT('Ctrl Pts',(61.3222974552519,36.994239526729,0.));
#111025=CARTESIAN_POINT('Ctrl Pts',(61.3222974552519,36.994239526729,12.));
#111026=CARTESIAN_POINT('Ctrl Pts',(61.3371949931396,37.0121648413088,0.));
#111027=CARTESIAN_POINT('Ctrl Pts',(61.3371949931396,37.0121648413088,12.));
#111028=CARTESIAN_POINT('Ctrl Pts',(61.352102813199,37.0301387221766,0.));
#111029=CARTESIAN_POINT('Ctrl Pts',(61.352102813199,37.0301387221766,12.));
#111030=CARTESIAN_POINT('Ctrl Pts',(61.3670207840041,37.0481611121698,0.));
#111031=CARTESIAN_POINT('Ctrl Pts',(61.3670207840041,37.0481611121698,12.));
#111032=CARTESIAN_POINT('Ctrl Pts',(61.3819487747458,37.0662319542827,0.));
#111033=CARTESIAN_POINT('Ctrl Pts',(61.3819487747458,37.0662319542827,12.));
#111034=CARTESIAN_POINT('Ctrl Pts',(61.3968866552294,37.0843511916729,0.));
#111035=CARTESIAN_POINT('Ctrl Pts',(61.3968866552294,37.0843511916729,12.));
#111036=CARTESIAN_POINT('Ctrl Pts',(61.411834295869,37.1025187676597,0.));
#111037=CARTESIAN_POINT('Ctrl Pts',(61.411834295869,37.1025187676597,12.));
#111038=CARTESIAN_POINT('Ctrl Pts',(61.4267915676834,37.1207346257229,0.));
#111039=CARTESIAN_POINT('Ctrl Pts',(61.4267915676834,37.1207346257229,12.));
#111040=CARTESIAN_POINT('Ctrl Pts',(61.4417583422888,37.138998709492,0.));
#111041=CARTESIAN_POINT('Ctrl Pts',(61.4417583422888,37.138998709492,12.));
#111042=CARTESIAN_POINT('Ctrl Pts',(61.4567344918946,37.157310962747,0.));
#111043=CARTESIAN_POINT('Ctrl Pts',(61.4567344918946,37.157310962747,12.));
#111044=CARTESIAN_POINT('Ctrl Pts',(61.471719889301,37.1756713294249,0.));
#111045=CARTESIAN_POINT('Ctrl Pts',(61.471719889301,37.1756713294249,12.));
#111046=CARTESIAN_POINT('Ctrl Pts',(61.4867144078939,37.1940797536182,0.));
#111047=CARTESIAN_POINT('Ctrl Pts',(61.4867144078939,37.1940797536182,12.));
#111048=CARTESIAN_POINT('Ctrl Pts',(61.5017179216404,37.2125361795727,0.));
#111049=CARTESIAN_POINT('Ctrl Pts',(61.5017179216404,37.2125361795727,12.));
#111050=CARTESIAN_POINT('Ctrl Pts',(61.5167303050823,37.2310405516775,0.));
#111051=CARTESIAN_POINT('Ctrl Pts',(61.5167303050823,37.2310405516775,12.));
#111052=CARTESIAN_POINT('Ctrl Pts',(61.5317514333319,37.2495928144661,0.));
#111053=CARTESIAN_POINT('Ctrl Pts',(61.5317514333319,37.2495928144661,12.));
#111054=CARTESIAN_POINT('Ctrl Pts',(61.5467811820686,37.2681929126218,0.));
#111055=CARTESIAN_POINT('Ctrl Pts',(61.5467811820686,37.2681929126218,12.));
#111056=CARTESIAN_POINT('Ctrl Pts',(61.5618194275349,37.286840790977,0.));
#111057=CARTESIAN_POINT('Ctrl Pts',(61.5618194275349,37.286840790977,12.));
#111058=CARTESIAN_POINT('Ctrl Pts',(61.5768660465313,37.3055363945108,0.));
#111059=CARTESIAN_POINT('Ctrl Pts',(61.5768660465313,37.3055363945108,12.));
#111060=CARTESIAN_POINT('Ctrl Pts',(61.591920916412,37.3242796683395,0.));
#111061=CARTESIAN_POINT('Ctrl Pts',(61.591920916412,37.3242796683395,12.));
#111062=CARTESIAN_POINT('Ctrl Pts',(61.6069839150804,37.3430705577178,0.));
#111063=CARTESIAN_POINT('Ctrl Pts',(61.6069839150804,37.3430705577178,12.));
#111064=CARTESIAN_POINT('Ctrl Pts',(61.6220549209862,37.3619090080447,0.));
#111065=CARTESIAN_POINT('Ctrl Pts',(61.6220549209862,37.3619090080447,12.));
#111066=CARTESIAN_POINT('Ctrl Pts',(61.6371338131208,37.3807949648622,0.));
#111067=CARTESIAN_POINT('Ctrl Pts',(61.6371338131208,37.3807949648622,12.));
#111068=CARTESIAN_POINT('Ctrl Pts',(61.6522204710133,37.3997283738534,0.));
#111069=CARTESIAN_POINT('Ctrl Pts',(61.6522204710133,37.3997283738534,12.));
#111070=CARTESIAN_POINT('Ctrl Pts',(61.6673147747249,37.4187091808324,0.));
#111071=CARTESIAN_POINT('Ctrl Pts',(61.6673147747249,37.4187091808324,12.));
#111072=CARTESIAN_POINT('Ctrl Pts',(61.6824166048453,37.4377373317456,0.));
#111073=CARTESIAN_POINT('Ctrl Pts',(61.6824166048453,37.4377373317456,12.));
#111074=CARTESIAN_POINT('Ctrl Pts',(61.69752584249,37.4568127726776,0.));
#111075=CARTESIAN_POINT('Ctrl Pts',(61.69752584249,37.4568127726776,12.));
#111076=CARTESIAN_POINT('Ctrl Pts',(61.7126423692965,37.4759354498509,0.));
#111077=CARTESIAN_POINT('Ctrl Pts',(61.7126423692965,37.4759354498509,12.));
#111078=CARTESIAN_POINT('Ctrl Pts',(61.7277660674203,37.4951053096235,0.));
#111079=CARTESIAN_POINT('Ctrl Pts',(61.7277660674203,37.4951053096235,12.));
#111080=CARTESIAN_POINT('Ctrl Pts',(61.7428968195296,37.5143222984794,0.));
#111081=CARTESIAN_POINT('Ctrl Pts',(61.7428968195296,37.5143222984794,12.));
#111082=CARTESIAN_POINT('Ctrl Pts',(61.7580345088014,37.5335863630286,0.));
#111083=CARTESIAN_POINT('Ctrl Pts',(61.7580345088014,37.5335863630286,12.));
#111084=CARTESIAN_POINT('Ctrl Pts',(61.7731790189191,37.5528974500142,0.));
#111085=CARTESIAN_POINT('Ctrl Pts',(61.7731790189191,37.5528974500142,12.));
#111086=CARTESIAN_POINT('Ctrl Pts',(61.7883302340689,37.5722555063112,0.));
#111087=CARTESIAN_POINT('Ctrl Pts',(61.7883302340689,37.5722555063112,12.));
#111088=CARTESIAN_POINT('Ctrl Pts',(61.8034880389362,37.5916604789252,0.));
#111089=CARTESIAN_POINT('Ctrl Pts',(61.8034880389362,37.5916604789252,12.));
#111090=CARTESIAN_POINT('Ctrl Pts',(61.8186523187011,37.6111123149836,0.));
#111091=CARTESIAN_POINT('Ctrl Pts',(61.8186523187011,37.6111123149836,12.));
#111092=CARTESIAN_POINT('Ctrl Pts',(61.8338229590345,37.6306109617341,0.));
#111093=CARTESIAN_POINT('Ctrl Pts',(61.8338229590345,37.6306109617341,12.));
#111094=CARTESIAN_POINT('Ctrl Pts',(61.848999846095,37.6501563665518,0.));
#111095=CARTESIAN_POINT('Ctrl Pts',(61.848999846095,37.6501563665518,12.));
#111096=CARTESIAN_POINT('Ctrl Pts',(61.8641828665257,37.6697484769389,0.));
#111097=CARTESIAN_POINT('Ctrl Pts',(61.8641828665257,37.6697484769389,12.));
#111098=CARTESIAN_POINT('Ctrl Pts',(61.879371907451,37.689387240523,0.));
#111099=CARTESIAN_POINT('Ctrl Pts',(61.879371907451,37.689387240523,12.));
#111100=CARTESIAN_POINT('Ctrl Pts',(61.8945668564714,37.7090726050488,0.));
#111101=CARTESIAN_POINT('Ctrl Pts',(61.8945668564714,37.7090726050488,12.));
#111102=CARTESIAN_POINT('Ctrl Pts',(61.9097676016616,37.7288045183765,0.));
#111103=CARTESIAN_POINT('Ctrl Pts',(61.9097676016616,37.7288045183765,12.));
#111104=CARTESIAN_POINT('Ctrl Pts',(61.9249740315664,37.748582928488,0.));
#111105=CARTESIAN_POINT('Ctrl Pts',(61.9249740315664,37.748582928488,12.));
#111106=CARTESIAN_POINT('Ctrl Pts',(61.940186035198,37.7684077834877,0.));
#111107=CARTESIAN_POINT('Ctrl Pts',(61.940186035198,37.7684077834877,12.));
#111108=CARTESIAN_POINT('Ctrl Pts',(61.9554035020335,37.7882790316012,0.));
#111109=CARTESIAN_POINT('Ctrl Pts',(61.9554035020335,37.7882790316012,12.));
#111110=CARTESIAN_POINT('Ctrl Pts',(61.9706263220101,37.808196621168,0.));
#111111=CARTESIAN_POINT('Ctrl Pts',(61.9706263220101,37.808196621168,12.));
#111112=CARTESIAN_POINT('Ctrl Pts',(61.9858543855221,37.8281605006371,0.));
#111113=CARTESIAN_POINT('Ctrl Pts',(61.9858543855221,37.8281605006371,12.));
#111114=CARTESIAN_POINT('Ctrl Pts',(62.0010875834176,37.8481706185742,0.));
#111115=CARTESIAN_POINT('Ctrl Pts',(62.0010875834176,37.8481706185742,12.));
#111116=CARTESIAN_POINT('Ctrl Pts',(62.0163258069954,37.8682269236628,0.));
#111117=CARTESIAN_POINT('Ctrl Pts',(62.0163258069954,37.8682269236628,12.));
#111118=CARTESIAN_POINT('Ctrl Pts',(62.0315689480022,37.888329364703,0.));
#111119=CARTESIAN_POINT('Ctrl Pts',(62.0315689480022,37.888329364703,12.));
#111120=CARTESIAN_POINT('Ctrl Pts',(62.0468168986289,37.9084778906053,0.));
#111121=CARTESIAN_POINT('Ctrl Pts',(62.0468168986289,37.9084778906053,12.));
#111122=CARTESIAN_POINT('Ctrl Pts',(62.0620695515072,37.9286724503849,0.));
#111123=CARTESIAN_POINT('Ctrl Pts',(62.0620695515072,37.9286724503849,12.));
#111124=CARTESIAN_POINT('Ctrl Pts',(62.0773267997072,37.9489129931685,0.));
#111125=CARTESIAN_POINT('Ctrl Pts',(62.0773267997072,37.9489129931685,12.));
#111126=CARTESIAN_POINT('Ctrl Pts',(62.0925885367346,37.9691994681962,0.));
#111127=CARTESIAN_POINT('Ctrl Pts',(62.0925885367346,37.9691994681962,12.));
#111128=CARTESIAN_POINT('Ctrl Pts',(62.107854656528,37.9895318248212,0.));
#111129=CARTESIAN_POINT('Ctrl Pts',(62.107854656528,37.9895318248212,12.));
#111130=CARTESIAN_POINT('Ctrl Pts',(62.1231250534558,38.0099100125041,0.));
#111131=CARTESIAN_POINT('Ctrl Pts',(62.1231250534558,38.0099100125041,12.));
#111132=CARTESIAN_POINT('Ctrl Pts',(62.1383996223136,38.0303339808059,0.));
#111133=CARTESIAN_POINT('Ctrl Pts',(62.1383996223136,38.0303339808059,12.));
#111134=CARTESIAN_POINT('Ctrl Pts',(62.153678258321,38.0508036793944,0.));
#111135=CARTESIAN_POINT('Ctrl Pts',(62.153678258321,38.0508036793944,12.));
#111136=CARTESIAN_POINT('Ctrl Pts',(62.1689608571182,38.0713190580466,0.));
#111137=CARTESIAN_POINT('Ctrl Pts',(62.1689608571182,38.0713190580466,12.));
#111138=CARTESIAN_POINT('Ctrl Pts',(62.1842473147627,38.0918800666479,0.));
#111139=CARTESIAN_POINT('Ctrl Pts',(62.1842473147627,38.0918800666479,12.));
#111140=CARTESIAN_POINT('Ctrl Pts',(62.1995375277253,38.1124866551884,0.));
#111141=CARTESIAN_POINT('Ctrl Pts',(62.1995375277253,38.1124866551884,12.));
#111142=CARTESIAN_POINT('Ctrl Pts',(62.2148313928859,38.1331387737528,0.));
#111143=CARTESIAN_POINT('Ctrl Pts',(62.2148313928859,38.1331387737528,12.));
#111144=CARTESIAN_POINT('Ctrl Pts',(62.2301288075319,38.1538363725263,0.));
#111145=CARTESIAN_POINT('Ctrl Pts',(62.2301288075319,38.1538363725263,12.));
#111146=CARTESIAN_POINT('Ctrl Pts',(62.2454296693581,38.1745794017997,0.));
#111147=CARTESIAN_POINT('Ctrl Pts',(62.2454296693581,38.1745794017997,12.));
#111148=CARTESIAN_POINT('Ctrl Pts',(62.2607338764655,38.1953678119692,0.));
#111149=CARTESIAN_POINT('Ctrl Pts',(62.2607338764655,38.1953678119692,12.));
#111150=CARTESIAN_POINT('Ctrl Pts',(62.2760413273601,38.2162015535351,0.));
#111151=CARTESIAN_POINT('Ctrl Pts',(62.2760413273601,38.2162015535351,12.));
#111152=CARTESIAN_POINT('Ctrl Pts',(62.2913519209517,38.2370805770931,0.));
#111153=CARTESIAN_POINT('Ctrl Pts',(62.2913519209517,38.2370805770931,12.));
#111154=CARTESIAN_POINT('Ctrl Pts',(62.3066655565497,38.2580048333356,0.));
#111155=CARTESIAN_POINT('Ctrl Pts',(62.3066655565497,38.2580048333356,12.));
#111156=CARTESIAN_POINT('Ctrl Pts',(62.3219821338564,38.2789742730559,0.));
#111157=CARTESIAN_POINT('Ctrl Pts',(62.3219821338564,38.2789742730559,12.));
#111158=CARTESIAN_POINT('Ctrl Pts',(62.337301552961,38.2999888471474,0.));
#111159=CARTESIAN_POINT('Ctrl Pts',(62.337301552961,38.2999888471474,12.));
#111160=CARTESIAN_POINT('Ctrl Pts',(62.3526237143338,38.3210485066003,0.));
#111161=CARTESIAN_POINT('Ctrl Pts',(62.3526237143338,38.3210485066003,12.));
#111162=CARTESIAN_POINT('Ctrl Pts',(62.3679485188178,38.3421532024915,0.));
#111163=CARTESIAN_POINT('Ctrl Pts',(62.3679485188178,38.3421532024915,12.));
#111164=CARTESIAN_POINT('Ctrl Pts',(62.3832758676281,38.3633028859835,0.));
#111165=CARTESIAN_POINT('Ctrl Pts',(62.3832758676281,38.3633028859835,12.));
#111166=CARTESIAN_POINT('Ctrl Pts',(62.3986056623587,38.384497508335,0.));
#111167=CARTESIAN_POINT('Ctrl Pts',(62.3986056623587,38.384497508335,12.));
#111168=CARTESIAN_POINT('Ctrl Pts',(62.4139378049891,38.4057370209054,0.));
#111169=CARTESIAN_POINT('Ctrl Pts',(62.4139378049891,38.4057370209054,12.));
#111170=CARTESIAN_POINT('Ctrl Pts',(62.42927219789,38.4270213751567,0.));
#111171=CARTESIAN_POINT('Ctrl Pts',(62.42927219789,38.4270213751567,12.));
#111172=CARTESIAN_POINT('Ctrl Pts',(62.4446087438304,38.4483505226511,0.));
#111173=CARTESIAN_POINT('Ctrl Pts',(62.4446087438304,38.4483505226511,12.));
#111174=CARTESIAN_POINT('Ctrl Pts',(62.4599473459799,38.4697244150473,0.));
#111175=CARTESIAN_POINT('Ctrl Pts',(62.4599473459799,38.4697244150473,12.));
#111176=CARTESIAN_POINT('Ctrl Pts',(62.4752879078842,38.4911430040988,0.));
#111177=CARTESIAN_POINT('Ctrl Pts',(62.4752879078842,38.4911430040988,12.));
#111178=CARTESIAN_POINT('Ctrl Pts',(62.4906303334435,38.5126062416496,0.));
#111179=CARTESIAN_POINT('Ctrl Pts',(62.4906303334435,38.5126062416496,12.));
#111180=CARTESIAN_POINT('Ctrl Pts',(62.50597452689,38.5341140796247,0.));
#111181=CARTESIAN_POINT('Ctrl Pts',(62.50597452689,38.5341140796247,12.));
#111182=CARTESIAN_POINT('Ctrl Pts',(62.5213203927672,38.5556664700201,0.));
#111183=CARTESIAN_POINT('Ctrl Pts',(62.5213203927672,38.5556664700201,12.));
#111184=CARTESIAN_POINT('Ctrl Pts',(62.5366678359036,38.5772633648841,0.));
#111185=CARTESIAN_POINT('Ctrl Pts',(62.5366678359036,38.5772633648841,12.));
#111186=CARTESIAN_POINT('Ctrl Pts',(62.5520167614529,38.5989047163401,0.));
#111187=CARTESIAN_POINT('Ctrl Pts',(62.5520167614529,38.5989047163401,12.));
#111188=CARTESIAN_POINT('Ctrl Pts',(62.567367074937,38.6205904766078,0.));
#111189=CARTESIAN_POINT('Ctrl Pts',(62.567367074937,38.6205904766078,12.));
#111190=CARTESIAN_POINT('Ctrl Pts',(62.5827186822923,38.6423205980214,0.));
#111191=CARTESIAN_POINT('Ctrl Pts',(62.5827186822923,38.6423205980214,12.));
#111192=CARTESIAN_POINT('Ctrl Pts',(62.5980714899048,38.6640950330418,0.));
#111193=CARTESIAN_POINT('Ctrl Pts',(62.5980714899048,38.6640950330418,12.));
#111194=CARTESIAN_POINT('Ctrl Pts',(62.6134254046732,38.6859137342726,0.));
#111195=CARTESIAN_POINT('Ctrl Pts',(62.6134254046732,38.6859137342726,12.));
#111196=CARTESIAN_POINT('Ctrl Pts',(62.6287803339534,38.7077766544411,0.));
#111197=CARTESIAN_POINT('Ctrl Pts',(62.6287803339534,38.7077766544411,12.));
#111198=CARTESIAN_POINT('Ctrl Pts',(62.6441361854406,38.7296837463605,0.));
#111199=CARTESIAN_POINT('Ctrl Pts',(62.6441361854406,38.7296837463605,12.));
#111200=CARTESIAN_POINT('Ctrl Pts',(62.6594928670626,38.7516349628902,0.));
#111201=CARTESIAN_POINT('Ctrl Pts',(62.6594928670626,38.7516349628902,12.));
#111202=CARTESIAN_POINT('Ctrl Pts',(62.6748502868836,38.7736302568982,0.));
#111203=CARTESIAN_POINT('Ctrl Pts',(62.6748502868836,38.7736302568982,12.));
#111204=CARTESIAN_POINT('Ctrl Pts',(62.6902083529698,38.7956695812032,0.));
#111205=CARTESIAN_POINT('Ctrl Pts',(62.6902083529698,38.7956695812032,12.));
#111206=CARTESIAN_POINT('Ctrl Pts',(62.7055669733811,38.8177528885687,0.));
#111207=CARTESIAN_POINT('Ctrl Pts',(62.7055669733811,38.8177528885687,12.));
#111208=CARTESIAN_POINT('Ctrl Pts',(62.7209260564506,38.8398801318184,0.));
#111209=CARTESIAN_POINT('Ctrl Pts',(62.7209260564506,38.8398801318184,12.));
#111210=CARTESIAN_POINT('Ctrl Pts',(62.7362855110052,38.8620512639239,0.));
#111211=CARTESIAN_POINT('Ctrl Pts',(62.7362855110052,38.8620512639239,12.));
#111212=CARTESIAN_POINT('Ctrl Pts',(62.7516452466129,38.8842662380984,0.));
#111213=CARTESIAN_POINT('Ctrl Pts',(62.7516452466129,38.8842662380984,12.));
#111214=CARTESIAN_POINT('Ctrl Pts',(62.7670051738132,38.9065250078824,0.));
#111215=CARTESIAN_POINT('Ctrl Pts',(62.7670051738132,38.9065250078824,12.));
#111216=CARTESIAN_POINT('Ctrl Pts',(62.7823652043677,38.928827527232,0.));
#111217=CARTESIAN_POINT('Ctrl Pts',(62.7823652043677,38.928827527232,12.));
#111218=CARTESIAN_POINT('Ctrl Pts',(62.797725250709,38.9511737503146,0.));
#111219=CARTESIAN_POINT('Ctrl Pts',(62.797725250709,38.9511737503146,12.));
#111220=CARTESIAN_POINT('Ctrl Pts',(62.8130852254004,38.9735636313073,0.));
#111221=CARTESIAN_POINT('Ctrl Pts',(62.8130852254004,38.9735636313073,12.));
#111222=CARTESIAN_POINT('Ctrl Pts',(62.8284450405451,38.9959971241695,0.));
#111223=CARTESIAN_POINT('Ctrl Pts',(62.8284450405451,38.9959971241695,12.));
#111224=CARTESIAN_POINT('Ctrl Pts',(62.8438046073237,39.0184741824649,0.));
#111225=CARTESIAN_POINT('Ctrl Pts',(62.8438046073237,39.0184741824649,12.));
#111226=CARTESIAN_POINT('Ctrl Pts',(62.859163835209,39.0409947590519,0.));
#111227=CARTESIAN_POINT('Ctrl Pts',(62.859163835209,39.0409947590519,12.));
#111228=CARTESIAN_POINT('Ctrl Pts',(62.8745226326046,39.0635588063309,0.));
#111229=CARTESIAN_POINT('Ctrl Pts',(62.8745226326046,39.0635588063309,12.));
#111230=CARTESIAN_POINT('Ctrl Pts',(62.8898809082659,39.0861662767964,0.));
#111231=CARTESIAN_POINT('Ctrl Pts',(62.8898809082659,39.0861662767964,12.));
#111232=CARTESIAN_POINT('Ctrl Pts',(62.9052385725416,39.1088171235144,0.));
#111233=CARTESIAN_POINT('Ctrl Pts',(62.9052385725416,39.1088171235144,12.));
#111234=CARTESIAN_POINT('Ctrl Pts',(62.9205955385551,39.1315113005745,0.));
#111235=CARTESIAN_POINT('Ctrl Pts',(62.9205955385551,39.1315113005745,12.));
#111236=CARTESIAN_POINT('Ctrl Pts',(62.9359517237352,39.1542487636708,0.));
#111237=CARTESIAN_POINT('Ctrl Pts',(62.9359517237352,39.1542487636708,12.));
#111238=CARTESIAN_POINT('Ctrl Pts',(62.9513070501777,39.1770294702367,0.));
#111239=CARTESIAN_POINT('Ctrl Pts',(62.9513070501777,39.1770294702367,12.));
#111240=CARTESIAN_POINT('Ctrl Pts',(62.9666614412627,39.199853378159,0.));
#111241=CARTESIAN_POINT('Ctrl Pts',(62.9666614412627,39.199853378159,12.));
#111242=CARTESIAN_POINT('Ctrl Pts',(62.9820148189849,39.2227204447583,0.));
#111243=CARTESIAN_POINT('Ctrl Pts',(62.9820148189849,39.2227204447583,12.));
#111244=CARTESIAN_POINT('Ctrl Pts',(62.9973671008685,39.2456306256092,0.));
#111245=CARTESIAN_POINT('Ctrl Pts',(62.9973671008685,39.2456306256092,12.));
#111246=CARTESIAN_POINT('Ctrl Pts',(63.0127181973702,39.268583873541,0.));
#111247=CARTESIAN_POINT('Ctrl Pts',(63.0127181973702,39.268583873541,12.));
#111248=CARTESIAN_POINT('Ctrl Pts',(63.0280680082522,39.2915801372468,0.));
#111249=CARTESIAN_POINT('Ctrl Pts',(63.0280680082522,39.2915801372468,12.));
#111250=CARTESIAN_POINT('Ctrl Pts',(63.0434164278221,39.3146193632546,0.));
#111251=CARTESIAN_POINT('Ctrl Pts',(63.0434164278221,39.3146193632546,12.));
#111252=CARTESIAN_POINT('Ctrl Pts',(63.0587633513993,39.3377014983757,0.));
#111253=CARTESIAN_POINT('Ctrl Pts',(63.0587633513993,39.3377014983757,12.));
#111254=CARTESIAN_POINT('Ctrl Pts',(63.0741086815957,39.3608264920487,0.));
#111255=CARTESIAN_POINT('Ctrl Pts',(63.0741086815957,39.3608264920487,12.));
#111256=CARTESIAN_POINT('Ctrl Pts',(63.0894523341238,39.3839942985688,0.));
#111257=CARTESIAN_POINT('Ctrl Pts',(63.0894523341238,39.3839942985688,12.));
#111258=CARTESIAN_POINT('Ctrl Pts',(63.1047942451583,39.4072048797401,0.));
#111259=CARTESIAN_POINT('Ctrl Pts',(63.1047942451583,39.4072048797401,12.));
#111260=CARTESIAN_POINT('Ctrl Pts',(63.1201343730643,39.4304582059507,0.));
#111261=CARTESIAN_POINT('Ctrl Pts',(63.1201343730643,39.4304582059507,12.));
#111262=CARTESIAN_POINT('Ctrl Pts',(63.1354726927781,39.4537542551852,0.));
#111263=CARTESIAN_POINT('Ctrl Pts',(63.1354726927781,39.4537542551852,12.));
#111264=CARTESIAN_POINT('Ctrl Pts',(63.147741892189,39.4724252610807,0.));
#111265=CARTESIAN_POINT('Ctrl Pts',(63.147741892189,39.4724252610807,12.));
#111266=CARTESIAN_POINT('Ctrl Pts',(63.1569429707564,39.4864477303613,0.));
#111267=CARTESIAN_POINT('Ctrl Pts',(63.1569429707564,39.4864477303613,12.));
#111268=CARTESIAN_POINT('Ctrl Pts',(63.1630766582674,39.4958045828059,0.));
#111269=CARTESIAN_POINT('Ctrl Pts',(63.1630766582674,39.4958045828059,12.));
#111270=CARTESIAN_POINT('Ctrl Pts',(63.1661434108059,39.5004851439258,0.));
#111271=CARTESIAN_POINT('Ctrl Pts',(63.1661434108059,39.5004851439258,12.));
#111272=CARTESIAN_POINT('',(60.1903555511633,35.7368311217509,0.));
#111273=CARTESIAN_POINT('Ctrl Pts',(60.1903555511633,35.7368311217509,0.));
#111274=CARTESIAN_POINT('Ctrl Pts',(60.1930746580239,35.7396040203973,0.));
#111275=CARTESIAN_POINT('Ctrl Pts',(60.1985151474406,35.7451551752456,0.));
#111276=CARTESIAN_POINT('Ctrl Pts',(60.2066827086579,35.7534979801871,0.));
#111277=CARTESIAN_POINT('Ctrl Pts',(60.2175864449678,35.7646538667299,0.));
#111278=CARTESIAN_POINT('Ctrl Pts',(60.2312388621286,35.7786523045782,0.));
#111279=CARTESIAN_POINT('Ctrl Pts',(60.2449139865206,35.7927043145165,0.));
#111280=CARTESIAN_POINT('Ctrl Pts',(60.2586117365278,35.8068098723386,0.));
#111281=CARTESIAN_POINT('Ctrl Pts',(60.2723319687507,35.8209689272574,0.));
#111282=CARTESIAN_POINT('Ctrl Pts',(60.2860744798563,35.8351814020424,0.));
#111283=CARTESIAN_POINT('Ctrl Pts',(60.2998390330173,35.8494472046784,0.));
#111284=CARTESIAN_POINT('Ctrl Pts',(60.313625378281,35.8637662371635,0.));
#111285=CARTESIAN_POINT('Ctrl Pts',(60.3274332746782,35.878138405151,0.));
#111286=CARTESIAN_POINT('Ctrl Pts',(60.3412625135223,35.8925636280632,0.));
#111287=CARTESIAN_POINT('Ctrl Pts',(60.3551129108794,35.9070418358501,0.));
#111288=CARTESIAN_POINT('Ctrl Pts',(60.368984296546,35.9215729642219,0.));
#111289=CARTESIAN_POINT('Ctrl Pts',(60.3828765049031,35.9361569506955,0.));
#111290=CARTESIAN_POINT('Ctrl Pts',(60.3967893635487,35.9507937296726,0.));
#111291=CARTESIAN_POINT('Ctrl Pts',(60.4107226875759,35.9654832299627,0.));
#111292=CARTESIAN_POINT('Ctrl Pts',(60.4246762854961,35.9802253773534,0.));
#111293=CARTESIAN_POINT('Ctrl Pts',(60.438649962949,35.9950200962175,0.));
#111294=CARTESIAN_POINT('Ctrl Pts',(60.452643526964,36.0098673113557,0.));
#111295=CARTESIAN_POINT('Ctrl Pts',(60.4666567908053,36.0247669500867,0.));
#111296=CARTESIAN_POINT('Ctrl Pts',(60.4806895737643,36.0397189421617,0.));
#111297=CARTESIAN_POINT('Ctrl Pts',(60.4947416988396,36.0547232187681,0.));
#111298=CARTESIAN_POINT('Ctrl Pts',(60.5088129911357,36.0697797118377,0.));
#111299=CARTESIAN_POINT('Ctrl Pts',(60.5229032759001,36.0848883531969,0.));
#111300=CARTESIAN_POINT('Ctrl Pts',(60.5370123768841,36.1000490738532,0.));
#111301=CARTESIAN_POINT('Ctrl Pts',(60.5511401172014,36.1152618043756,0.));
#111302=CARTESIAN_POINT('Ctrl Pts',(60.5652863200732,36.1305264752195,0.));
#111303=CARTESIAN_POINT('Ctrl Pts',(60.5794508095555,36.1458430170425,0.));
#111304=CARTESIAN_POINT('Ctrl Pts',(60.5936334114082,36.1612113610758,0.));
#111305=CARTESIAN_POINT('Ctrl Pts',(60.6078339534151,36.1766314392624,0.));
#111306=CARTESIAN_POINT('Ctrl Pts',(60.6220522649129,36.1921031840618,0.));
#111307=CARTESIAN_POINT('Ctrl Pts',(60.6362881765014,36.2076265283261,0.));
#111308=CARTESIAN_POINT('Ctrl Pts',(60.6505415197055,36.2232014051549,0.));
#111309=CARTESIAN_POINT('Ctrl Pts',(60.6648121265908,36.2388277477225,0.));
#111310=CARTESIAN_POINT('Ctrl Pts',(60.6790998297823,36.2545054892911,0.));
#111311=CARTESIAN_POINT('Ctrl Pts',(60.6934044626304,36.2702345632883,0.));
#111312=CARTESIAN_POINT('Ctrl Pts',(60.7077258593268,36.2860149033586,0.));
#111313=CARTESIAN_POINT('Ctrl Pts',(60.7220638550396,36.3018464434204,0.));
#111314=CARTESIAN_POINT('Ctrl Pts',(60.7364182860388,36.3177291177148,0.));
#111315=CARTESIAN_POINT('Ctrl Pts',(60.7507889896283,36.3336628607844,0.));
#111316=CARTESIAN_POINT('Ctrl Pts',(60.7651758040791,36.349647607448,0.));
#111317=CARTESIAN_POINT('Ctrl Pts',(60.779578568563,36.3656832927733,0.));
#111318=CARTESIAN_POINT('Ctrl Pts',(60.7939971230781,36.38176985204,0.));
#111319=CARTESIAN_POINT('Ctrl Pts',(60.8084313084009,36.3979072207174,0.));
#111320=CARTESIAN_POINT('Ctrl Pts',(60.8228809661179,36.414095334487,0.));
#111321=CARTESIAN_POINT('Ctrl Pts',(60.8373459386397,36.4303341292497,0.));
#111322=CARTESIAN_POINT('Ctrl Pts',(60.851826069218,36.4466235411353,0.));
#111323=CARTESIAN_POINT('Ctrl Pts',(60.8663212019646,36.4629635065037,0.));
#111324=CARTESIAN_POINT('Ctrl Pts',(60.8808311818489,36.4793539619459,0.));
#111325=CARTESIAN_POINT('Ctrl Pts',(60.8953558546791,36.4957948442832,0.));
#111326=CARTESIAN_POINT('Ctrl Pts',(60.9098950670847,36.5122860905611,0.));
#111327=CARTESIAN_POINT('Ctrl Pts',(60.924448666499,36.5288276380417,0.));
#111328=CARTESIAN_POINT('Ctrl Pts',(60.9390165011357,36.5454194241866,0.));
#111329=CARTESIAN_POINT('Ctrl Pts',(60.9535984199874,36.5620613866616,0.));
#111330=CARTESIAN_POINT('Ctrl Pts',(60.9681942728237,36.5787534633416,0.));
#111331=CARTESIAN_POINT('Ctrl Pts',(60.9828039101887,36.5954955923109,0.));
#111332=CARTESIAN_POINT('Ctrl Pts',(60.9974271833982,36.6122877118599,0.));
#111333=CARTESIAN_POINT('Ctrl Pts',(61.012063944535,36.6291297604775,0.));
#111334=CARTESIAN_POINT('Ctrl Pts',(61.0267140464434,36.6460216768553,0.));
#111335=CARTESIAN_POINT('Ctrl Pts',(61.0413773427204,36.6629633998886,0.));
#111336=CARTESIAN_POINT('Ctrl Pts',(61.0560536877084,36.6799548686741,0.));
#111337=CARTESIAN_POINT('Ctrl Pts',(61.0707429364841,36.6969960225019,0.));
#111338=CARTESIAN_POINT('Ctrl Pts',(61.085444944851,36.7140868008479,0.));
#111339=CARTESIAN_POINT('Ctrl Pts',(61.1001595693357,36.7312271433799,0.));
#111340=CARTESIAN_POINT('Ctrl Pts',(61.1148866671821,36.7484169899591,0.));
#111341=CARTESIAN_POINT('Ctrl Pts',(61.1296260963468,36.7656562806381,0.));
#111342=CARTESIAN_POINT('Ctrl Pts',(61.1443777154926,36.782944955654,0.));
#111343=CARTESIAN_POINT('Ctrl Pts',(61.1591413839809,36.8002829554221,0.));
#111344=CARTESIAN_POINT('Ctrl Pts',(61.1739169618688,36.8176702205436,0.));
#111345=CARTESIAN_POINT('Ctrl Pts',(61.1887043099026,36.8351066918043,0.));
#111346=CARTESIAN_POINT('Ctrl Pts',(61.2035032895121,36.8525923101736,0.));
#111347=CARTESIAN_POINT('Ctrl Pts',(61.2183137628031,36.8701270167954,0.));
#111348=CARTESIAN_POINT('Ctrl Pts',(61.2331355925513,36.8877107529844,0.));
#111349=CARTESIAN_POINT('Ctrl Pts',(61.2479686421979,36.9053434602324,0.));
#111350=CARTESIAN_POINT('Ctrl Pts',(61.2628127758443,36.9230250802079,0.));
#111351=CARTESIAN_POINT('Ctrl Pts',(61.2776678582474,36.9407555547542,0.));
#111352=CARTESIAN_POINT('Ctrl Pts',(61.2925337548113,36.9585348258798,0.));
#111353=CARTESIAN_POINT('Ctrl Pts',(61.3074103315834,36.976362835757,0.));
#111354=CARTESIAN_POINT('Ctrl Pts',(61.3222974552519,36.994239526729,0.));
#111355=CARTESIAN_POINT('Ctrl Pts',(61.3371949931396,37.0121648413088,0.));
#111356=CARTESIAN_POINT('Ctrl Pts',(61.352102813199,37.0301387221766,0.));
#111357=CARTESIAN_POINT('Ctrl Pts',(61.3670207840041,37.0481611121698,0.));
#111358=CARTESIAN_POINT('Ctrl Pts',(61.3819487747458,37.0662319542827,0.));
#111359=CARTESIAN_POINT('Ctrl Pts',(61.3968866552294,37.0843511916729,0.));
#111360=CARTESIAN_POINT('Ctrl Pts',(61.411834295869,37.1025187676597,0.));
#111361=CARTESIAN_POINT('Ctrl Pts',(61.4267915676834,37.1207346257229,0.));
#111362=CARTESIAN_POINT('Ctrl Pts',(61.4417583422888,37.138998709492,0.));
#111363=CARTESIAN_POINT('Ctrl Pts',(61.4567344918946,37.157310962747,0.));
#111364=CARTESIAN_POINT('Ctrl Pts',(61.471719889301,37.1756713294249,0.));
#111365=CARTESIAN_POINT('Ctrl Pts',(61.4867144078939,37.1940797536182,0.));
#111366=CARTESIAN_POINT('Ctrl Pts',(61.5017179216404,37.2125361795727,0.));
#111367=CARTESIAN_POINT('Ctrl Pts',(61.5167303050823,37.2310405516775,0.));
#111368=CARTESIAN_POINT('Ctrl Pts',(61.5317514333319,37.2495928144661,0.));
#111369=CARTESIAN_POINT('Ctrl Pts',(61.5467811820686,37.2681929126218,0.));
#111370=CARTESIAN_POINT('Ctrl Pts',(61.5618194275349,37.286840790977,0.));
#111371=CARTESIAN_POINT('Ctrl Pts',(61.5768660465313,37.3055363945108,0.));
#111372=CARTESIAN_POINT('Ctrl Pts',(61.591920916412,37.3242796683395,0.));
#111373=CARTESIAN_POINT('Ctrl Pts',(61.6069839150804,37.3430705577178,0.));
#111374=CARTESIAN_POINT('Ctrl Pts',(61.6220549209862,37.3619090080447,0.));
#111375=CARTESIAN_POINT('Ctrl Pts',(61.6371338131208,37.3807949648622,0.));
#111376=CARTESIAN_POINT('Ctrl Pts',(61.6522204710133,37.3997283738534,0.));
#111377=CARTESIAN_POINT('Ctrl Pts',(61.6673147747249,37.4187091808324,0.));
#111378=CARTESIAN_POINT('Ctrl Pts',(61.6824166048453,37.4377373317456,0.));
#111379=CARTESIAN_POINT('Ctrl Pts',(61.69752584249,37.4568127726776,0.));
#111380=CARTESIAN_POINT('Ctrl Pts',(61.7126423692965,37.4759354498509,0.));
#111381=CARTESIAN_POINT('Ctrl Pts',(61.7277660674203,37.4951053096235,0.));
#111382=CARTESIAN_POINT('Ctrl Pts',(61.7428968195296,37.5143222984794,0.));
#111383=CARTESIAN_POINT('Ctrl Pts',(61.7580345088014,37.5335863630286,0.));
#111384=CARTESIAN_POINT('Ctrl Pts',(61.7731790189191,37.5528974500142,0.));
#111385=CARTESIAN_POINT('Ctrl Pts',(61.7883302340689,37.5722555063112,0.));
#111386=CARTESIAN_POINT('Ctrl Pts',(61.8034880389362,37.5916604789252,0.));
#111387=CARTESIAN_POINT('Ctrl Pts',(61.8186523187011,37.6111123149836,0.));
#111388=CARTESIAN_POINT('Ctrl Pts',(61.8338229590345,37.6306109617341,0.));
#111389=CARTESIAN_POINT('Ctrl Pts',(61.848999846095,37.6501563665518,0.));
#111390=CARTESIAN_POINT('Ctrl Pts',(61.8641828665257,37.6697484769389,0.));
#111391=CARTESIAN_POINT('Ctrl Pts',(61.879371907451,37.689387240523,0.));
#111392=CARTESIAN_POINT('Ctrl Pts',(61.8945668564714,37.7090726050488,0.));
#111393=CARTESIAN_POINT('Ctrl Pts',(61.9097676016616,37.7288045183765,0.));
#111394=CARTESIAN_POINT('Ctrl Pts',(61.9249740315664,37.748582928488,0.));
#111395=CARTESIAN_POINT('Ctrl Pts',(61.940186035198,37.7684077834877,0.));
#111396=CARTESIAN_POINT('Ctrl Pts',(61.9554035020335,37.7882790316012,0.));
#111397=CARTESIAN_POINT('Ctrl Pts',(61.9706263220101,37.808196621168,0.));
#111398=CARTESIAN_POINT('Ctrl Pts',(61.9858543855221,37.8281605006371,0.));
#111399=CARTESIAN_POINT('Ctrl Pts',(62.0010875834176,37.8481706185742,0.));
#111400=CARTESIAN_POINT('Ctrl Pts',(62.0163258069954,37.8682269236628,0.));
#111401=CARTESIAN_POINT('Ctrl Pts',(62.0315689480022,37.888329364703,0.));
#111402=CARTESIAN_POINT('Ctrl Pts',(62.0468168986289,37.9084778906053,0.));
#111403=CARTESIAN_POINT('Ctrl Pts',(62.0620695515072,37.9286724503849,0.));
#111404=CARTESIAN_POINT('Ctrl Pts',(62.0773267997072,37.9489129931685,0.));
#111405=CARTESIAN_POINT('Ctrl Pts',(62.0925885367346,37.9691994681962,0.));
#111406=CARTESIAN_POINT('Ctrl Pts',(62.107854656528,37.9895318248212,0.));
#111407=CARTESIAN_POINT('Ctrl Pts',(62.1231250534558,38.0099100125041,0.));
#111408=CARTESIAN_POINT('Ctrl Pts',(62.1383996223136,38.0303339808059,0.));
#111409=CARTESIAN_POINT('Ctrl Pts',(62.153678258321,38.0508036793944,0.));
#111410=CARTESIAN_POINT('Ctrl Pts',(62.1689608571182,38.0713190580466,0.));
#111411=CARTESIAN_POINT('Ctrl Pts',(62.1842473147627,38.0918800666479,0.));
#111412=CARTESIAN_POINT('Ctrl Pts',(62.1995375277253,38.1124866551884,0.));
#111413=CARTESIAN_POINT('Ctrl Pts',(62.2148313928859,38.1331387737528,0.));
#111414=CARTESIAN_POINT('Ctrl Pts',(62.2301288075319,38.1538363725263,0.));
#111415=CARTESIAN_POINT('Ctrl Pts',(62.2454296693581,38.1745794017997,0.));
#111416=CARTESIAN_POINT('Ctrl Pts',(62.2607338764655,38.1953678119692,0.));
#111417=CARTESIAN_POINT('Ctrl Pts',(62.2760413273601,38.2162015535351,0.));
#111418=CARTESIAN_POINT('Ctrl Pts',(62.2913519209517,38.2370805770931,0.));
#111419=CARTESIAN_POINT('Ctrl Pts',(62.3066655565497,38.2580048333356,0.));
#111420=CARTESIAN_POINT('Ctrl Pts',(62.3219821338564,38.2789742730559,0.));
#111421=CARTESIAN_POINT('Ctrl Pts',(62.337301552961,38.2999888471474,0.));
#111422=CARTESIAN_POINT('Ctrl Pts',(62.3526237143338,38.3210485066003,0.));
#111423=CARTESIAN_POINT('Ctrl Pts',(62.3679485188178,38.3421532024915,0.));
#111424=CARTESIAN_POINT('Ctrl Pts',(62.3832758676281,38.3633028859835,0.));
#111425=CARTESIAN_POINT('Ctrl Pts',(62.3986056623587,38.384497508335,0.));
#111426=CARTESIAN_POINT('Ctrl Pts',(62.4139378049891,38.4057370209054,0.));
#111427=CARTESIAN_POINT('Ctrl Pts',(62.42927219789,38.4270213751567,0.));
#111428=CARTESIAN_POINT('Ctrl Pts',(62.4446087438304,38.4483505226511,0.));
#111429=CARTESIAN_POINT('Ctrl Pts',(62.4599473459799,38.4697244150473,0.));
#111430=CARTESIAN_POINT('Ctrl Pts',(62.4752879078842,38.4911430040988,0.));
#111431=CARTESIAN_POINT('Ctrl Pts',(62.4906303334435,38.5126062416496,0.));
#111432=CARTESIAN_POINT('Ctrl Pts',(62.50597452689,38.5341140796247,0.));
#111433=CARTESIAN_POINT('Ctrl Pts',(62.5213203927672,38.5556664700201,0.));
#111434=CARTESIAN_POINT('Ctrl Pts',(62.5366678359036,38.5772633648841,0.));
#111435=CARTESIAN_POINT('Ctrl Pts',(62.5520167614529,38.5989047163401,0.));
#111436=CARTESIAN_POINT('Ctrl Pts',(62.567367074937,38.6205904766078,0.));
#111437=CARTESIAN_POINT('Ctrl Pts',(62.5827186822923,38.6423205980214,0.));
#111438=CARTESIAN_POINT('Ctrl Pts',(62.5980714899048,38.6640950330418,0.));
#111439=CARTESIAN_POINT('Ctrl Pts',(62.6134254046732,38.6859137342726,0.));
#111440=CARTESIAN_POINT('Ctrl Pts',(62.6287803339534,38.7077766544411,0.));
#111441=CARTESIAN_POINT('Ctrl Pts',(62.6441361854406,38.7296837463605,0.));
#111442=CARTESIAN_POINT('Ctrl Pts',(62.6594928670626,38.7516349628902,0.));
#111443=CARTESIAN_POINT('Ctrl Pts',(62.6748502868836,38.7736302568982,0.));
#111444=CARTESIAN_POINT('Ctrl Pts',(62.6902083529698,38.7956695812032,0.));
#111445=CARTESIAN_POINT('Ctrl Pts',(62.7055669733811,38.8177528885687,0.));
#111446=CARTESIAN_POINT('Ctrl Pts',(62.7209260564506,38.8398801318184,0.));
#111447=CARTESIAN_POINT('Ctrl Pts',(62.7362855110052,38.8620512639239,0.));
#111448=CARTESIAN_POINT('Ctrl Pts',(62.7516452466129,38.8842662380984,0.));
#111449=CARTESIAN_POINT('Ctrl Pts',(62.7670051738132,38.9065250078824,0.));
#111450=CARTESIAN_POINT('Ctrl Pts',(62.7823652043677,38.928827527232,0.));
#111451=CARTESIAN_POINT('Ctrl Pts',(62.797725250709,38.9511737503146,0.));
#111452=CARTESIAN_POINT('Ctrl Pts',(62.8130852254004,38.9735636313073,0.));
#111453=CARTESIAN_POINT('Ctrl Pts',(62.8284450405451,38.9959971241695,0.));
#111454=CARTESIAN_POINT('Ctrl Pts',(62.8438046073237,39.0184741824649,0.));
#111455=CARTESIAN_POINT('Ctrl Pts',(62.859163835209,39.0409947590519,0.));
#111456=CARTESIAN_POINT('Ctrl Pts',(62.8745226326046,39.0635588063309,0.));
#111457=CARTESIAN_POINT('Ctrl Pts',(62.8898809082659,39.0861662767964,0.));
#111458=CARTESIAN_POINT('Ctrl Pts',(62.9052385725416,39.1088171235144,0.));
#111459=CARTESIAN_POINT('Ctrl Pts',(62.9205955385551,39.1315113005745,0.));
#111460=CARTESIAN_POINT('Ctrl Pts',(62.9359517237352,39.1542487636708,0.));
#111461=CARTESIAN_POINT('Ctrl Pts',(62.9513070501777,39.1770294702367,0.));
#111462=CARTESIAN_POINT('Ctrl Pts',(62.9644687386694,39.1965939820804,0.));
#111463=CARTESIAN_POINT('Ctrl Pts',(62.9745590018501,39.2116170128279,0.));
#111464=CARTESIAN_POINT('Ctrl Pts',(62.9815782721131,39.2220794388576,0.));
#111465=CARTESIAN_POINT('Ctrl Pts',(62.9855268615905,39.2279686274724,0.));
#111466=CARTESIAN_POINT('Ctrl Pts',(62.9864049293634,39.2292784191472,0.));
#111467=CARTESIAN_POINT('',(60.1903555511633,35.7368311217509,12.));
#111468=CARTESIAN_POINT('',(60.1903555511633,35.7368311217509,0.));
#111469=CARTESIAN_POINT('Ctrl Pts',(62.9864049293634,39.2292784191472,12.));
#111470=CARTESIAN_POINT('Ctrl Pts',(62.9855268615905,39.2279686274724,12.));
#111471=CARTESIAN_POINT('Ctrl Pts',(62.9815782721131,39.2220794388576,12.));
#111472=CARTESIAN_POINT('Ctrl Pts',(62.9745590018501,39.2116170128279,12.));
#111473=CARTESIAN_POINT('Ctrl Pts',(62.9644687386694,39.1965939820804,12.));
#111474=CARTESIAN_POINT('Ctrl Pts',(62.9513070501777,39.1770294702367,12.));
#111475=CARTESIAN_POINT('Ctrl Pts',(62.9359517237352,39.1542487636708,12.));
#111476=CARTESIAN_POINT('Ctrl Pts',(62.9205955385551,39.1315113005745,12.));
#111477=CARTESIAN_POINT('Ctrl Pts',(62.9052385725416,39.1088171235144,12.));
#111478=CARTESIAN_POINT('Ctrl Pts',(62.8898809082659,39.0861662767964,12.));
#111479=CARTESIAN_POINT('Ctrl Pts',(62.8745226326046,39.0635588063309,12.));
#111480=CARTESIAN_POINT('Ctrl Pts',(62.859163835209,39.0409947590519,12.));
#111481=CARTESIAN_POINT('Ctrl Pts',(62.8438046073237,39.0184741824649,12.));
#111482=CARTESIAN_POINT('Ctrl Pts',(62.8284450405451,38.9959971241695,12.));
#111483=CARTESIAN_POINT('Ctrl Pts',(62.8130852254004,38.9735636313073,12.));
#111484=CARTESIAN_POINT('Ctrl Pts',(62.797725250709,38.9511737503146,12.));
#111485=CARTESIAN_POINT('Ctrl Pts',(62.7823652043677,38.928827527232,12.));
#111486=CARTESIAN_POINT('Ctrl Pts',(62.7670051738132,38.9065250078824,12.));
#111487=CARTESIAN_POINT('Ctrl Pts',(62.7516452466129,38.8842662380984,12.));
#111488=CARTESIAN_POINT('Ctrl Pts',(62.7362855110052,38.8620512639239,12.));
#111489=CARTESIAN_POINT('Ctrl Pts',(62.7209260564506,38.8398801318184,12.));
#111490=CARTESIAN_POINT('Ctrl Pts',(62.7055669733811,38.8177528885687,12.));
#111491=CARTESIAN_POINT('Ctrl Pts',(62.6902083529698,38.7956695812032,12.));
#111492=CARTESIAN_POINT('Ctrl Pts',(62.6748502868836,38.7736302568982,12.));
#111493=CARTESIAN_POINT('Ctrl Pts',(62.6594928670626,38.7516349628902,12.));
#111494=CARTESIAN_POINT('Ctrl Pts',(62.6441361854406,38.7296837463605,12.));
#111495=CARTESIAN_POINT('Ctrl Pts',(62.6287803339534,38.7077766544411,12.));
#111496=CARTESIAN_POINT('Ctrl Pts',(62.6134254046732,38.6859137342726,12.));
#111497=CARTESIAN_POINT('Ctrl Pts',(62.5980714899048,38.6640950330418,12.));
#111498=CARTESIAN_POINT('Ctrl Pts',(62.5827186822923,38.6423205980214,12.));
#111499=CARTESIAN_POINT('Ctrl Pts',(62.567367074937,38.6205904766078,12.));
#111500=CARTESIAN_POINT('Ctrl Pts',(62.5520167614529,38.5989047163401,12.));
#111501=CARTESIAN_POINT('Ctrl Pts',(62.5366678359036,38.5772633648841,12.));
#111502=CARTESIAN_POINT('Ctrl Pts',(62.5213203927672,38.5556664700201,12.));
#111503=CARTESIAN_POINT('Ctrl Pts',(62.50597452689,38.5341140796247,12.));
#111504=CARTESIAN_POINT('Ctrl Pts',(62.4906303334435,38.5126062416496,12.));
#111505=CARTESIAN_POINT('Ctrl Pts',(62.4752879078842,38.4911430040988,12.));
#111506=CARTESIAN_POINT('Ctrl Pts',(62.4599473459799,38.4697244150473,12.));
#111507=CARTESIAN_POINT('Ctrl Pts',(62.4446087438304,38.4483505226511,12.));
#111508=CARTESIAN_POINT('Ctrl Pts',(62.42927219789,38.4270213751567,12.));
#111509=CARTESIAN_POINT('Ctrl Pts',(62.4139378049891,38.4057370209054,12.));
#111510=CARTESIAN_POINT('Ctrl Pts',(62.3986056623587,38.384497508335,12.));
#111511=CARTESIAN_POINT('Ctrl Pts',(62.3832758676281,38.3633028859835,12.));
#111512=CARTESIAN_POINT('Ctrl Pts',(62.3679485188178,38.3421532024915,12.));
#111513=CARTESIAN_POINT('Ctrl Pts',(62.3526237143338,38.3210485066003,12.));
#111514=CARTESIAN_POINT('Ctrl Pts',(62.337301552961,38.2999888471474,12.));
#111515=CARTESIAN_POINT('Ctrl Pts',(62.3219821338564,38.2789742730559,12.));
#111516=CARTESIAN_POINT('Ctrl Pts',(62.3066655565497,38.2580048333356,12.));
#111517=CARTESIAN_POINT('Ctrl Pts',(62.2913519209517,38.2370805770931,12.));
#111518=CARTESIAN_POINT('Ctrl Pts',(62.2760413273601,38.2162015535351,12.));
#111519=CARTESIAN_POINT('Ctrl Pts',(62.2607338764655,38.1953678119692,12.));
#111520=CARTESIAN_POINT('Ctrl Pts',(62.2454296693581,38.1745794017997,12.));
#111521=CARTESIAN_POINT('Ctrl Pts',(62.2301288075319,38.1538363725263,12.));
#111522=CARTESIAN_POINT('Ctrl Pts',(62.2148313928859,38.1331387737528,12.));
#111523=CARTESIAN_POINT('Ctrl Pts',(62.1995375277253,38.1124866551884,12.));
#111524=CARTESIAN_POINT('Ctrl Pts',(62.1842473147627,38.0918800666479,12.));
#111525=CARTESIAN_POINT('Ctrl Pts',(62.1689608571182,38.0713190580466,12.));
#111526=CARTESIAN_POINT('Ctrl Pts',(62.153678258321,38.0508036793944,12.));
#111527=CARTESIAN_POINT('Ctrl Pts',(62.1383996223136,38.0303339808059,12.));
#111528=CARTESIAN_POINT('Ctrl Pts',(62.1231250534558,38.0099100125041,12.));
#111529=CARTESIAN_POINT('Ctrl Pts',(62.107854656528,37.9895318248212,12.));
#111530=CARTESIAN_POINT('Ctrl Pts',(62.0925885367346,37.9691994681962,12.));
#111531=CARTESIAN_POINT('Ctrl Pts',(62.0773267997072,37.9489129931685,12.));
#111532=CARTESIAN_POINT('Ctrl Pts',(62.0620695515072,37.9286724503849,12.));
#111533=CARTESIAN_POINT('Ctrl Pts',(62.0468168986289,37.9084778906053,12.));
#111534=CARTESIAN_POINT('Ctrl Pts',(62.0315689480022,37.888329364703,12.));
#111535=CARTESIAN_POINT('Ctrl Pts',(62.0163258069954,37.8682269236628,12.));
#111536=CARTESIAN_POINT('Ctrl Pts',(62.0010875834176,37.8481706185742,12.));
#111537=CARTESIAN_POINT('Ctrl Pts',(61.9858543855221,37.8281605006371,12.));
#111538=CARTESIAN_POINT('Ctrl Pts',(61.9706263220101,37.808196621168,12.));
#111539=CARTESIAN_POINT('Ctrl Pts',(61.9554035020335,37.7882790316012,12.));
#111540=CARTESIAN_POINT('Ctrl Pts',(61.940186035198,37.7684077834877,12.));
#111541=CARTESIAN_POINT('Ctrl Pts',(61.9249740315664,37.748582928488,12.));
#111542=CARTESIAN_POINT('Ctrl Pts',(61.9097676016616,37.7288045183765,12.));
#111543=CARTESIAN_POINT('Ctrl Pts',(61.8945668564714,37.7090726050488,12.));
#111544=CARTESIAN_POINT('Ctrl Pts',(61.879371907451,37.689387240523,12.));
#111545=CARTESIAN_POINT('Ctrl Pts',(61.8641828665257,37.6697484769389,12.));
#111546=CARTESIAN_POINT('Ctrl Pts',(61.848999846095,37.6501563665518,12.));
#111547=CARTESIAN_POINT('Ctrl Pts',(61.8338229590345,37.6306109617341,12.));
#111548=CARTESIAN_POINT('Ctrl Pts',(61.8186523187011,37.6111123149836,12.));
#111549=CARTESIAN_POINT('Ctrl Pts',(61.8034880389362,37.5916604789252,12.));
#111550=CARTESIAN_POINT('Ctrl Pts',(61.7883302340689,37.5722555063112,12.));
#111551=CARTESIAN_POINT('Ctrl Pts',(61.7731790189191,37.5528974500142,12.));
#111552=CARTESIAN_POINT('Ctrl Pts',(61.7580345088014,37.5335863630286,12.));
#111553=CARTESIAN_POINT('Ctrl Pts',(61.7428968195296,37.5143222984794,12.));
#111554=CARTESIAN_POINT('Ctrl Pts',(61.7277660674203,37.4951053096235,12.));
#111555=CARTESIAN_POINT('Ctrl Pts',(61.7126423692965,37.4759354498509,12.));
#111556=CARTESIAN_POINT('Ctrl Pts',(61.69752584249,37.4568127726776,12.));
#111557=CARTESIAN_POINT('Ctrl Pts',(61.6824166048453,37.4377373317456,12.));
#111558=CARTESIAN_POINT('Ctrl Pts',(61.6673147747249,37.4187091808324,12.));
#111559=CARTESIAN_POINT('Ctrl Pts',(61.6522204710133,37.3997283738534,12.));
#111560=CARTESIAN_POINT('Ctrl Pts',(61.6371338131208,37.3807949648622,12.));
#111561=CARTESIAN_POINT('Ctrl Pts',(61.6220549209862,37.3619090080447,12.));
#111562=CARTESIAN_POINT('Ctrl Pts',(61.6069839150804,37.3430705577178,12.));
#111563=CARTESIAN_POINT('Ctrl Pts',(61.591920916412,37.3242796683395,12.));
#111564=CARTESIAN_POINT('Ctrl Pts',(61.5768660465313,37.3055363945108,12.));
#111565=CARTESIAN_POINT('Ctrl Pts',(61.5618194275349,37.286840790977,12.));
#111566=CARTESIAN_POINT('Ctrl Pts',(61.5467811820686,37.2681929126218,12.));
#111567=CARTESIAN_POINT('Ctrl Pts',(61.5317514333319,37.2495928144661,12.));
#111568=CARTESIAN_POINT('Ctrl Pts',(61.5167303050823,37.2310405516775,12.));
#111569=CARTESIAN_POINT('Ctrl Pts',(61.5017179216404,37.2125361795727,12.));
#111570=CARTESIAN_POINT('Ctrl Pts',(61.4867144078939,37.1940797536182,12.));
#111571=CARTESIAN_POINT('Ctrl Pts',(61.471719889301,37.1756713294249,12.));
#111572=CARTESIAN_POINT('Ctrl Pts',(61.4567344918946,37.157310962747,12.));
#111573=CARTESIAN_POINT('Ctrl Pts',(61.4417583422888,37.138998709492,12.));
#111574=CARTESIAN_POINT('Ctrl Pts',(61.4267915676834,37.1207346257229,12.));
#111575=CARTESIAN_POINT('Ctrl Pts',(61.411834295869,37.1025187676597,12.));
#111576=CARTESIAN_POINT('Ctrl Pts',(61.3968866552294,37.0843511916729,12.));
#111577=CARTESIAN_POINT('Ctrl Pts',(61.3819487747458,37.0662319542827,12.));
#111578=CARTESIAN_POINT('Ctrl Pts',(61.3670207840041,37.0481611121698,12.));
#111579=CARTESIAN_POINT('Ctrl Pts',(61.352102813199,37.0301387221766,12.));
#111580=CARTESIAN_POINT('Ctrl Pts',(61.3371949931396,37.0121648413088,12.));
#111581=CARTESIAN_POINT('Ctrl Pts',(61.3222974552519,36.994239526729,12.));
#111582=CARTESIAN_POINT('Ctrl Pts',(61.3074103315834,36.976362835757,12.));
#111583=CARTESIAN_POINT('Ctrl Pts',(61.2925337548113,36.9585348258798,12.));
#111584=CARTESIAN_POINT('Ctrl Pts',(61.2776678582474,36.9407555547542,12.));
#111585=CARTESIAN_POINT('Ctrl Pts',(61.2628127758443,36.9230250802079,12.));
#111586=CARTESIAN_POINT('Ctrl Pts',(61.2479686421979,36.9053434602324,12.));
#111587=CARTESIAN_POINT('Ctrl Pts',(61.2331355925513,36.8877107529844,12.));
#111588=CARTESIAN_POINT('Ctrl Pts',(61.2183137628031,36.8701270167954,12.));
#111589=CARTESIAN_POINT('Ctrl Pts',(61.2035032895121,36.8525923101736,12.));
#111590=CARTESIAN_POINT('Ctrl Pts',(61.1887043099026,36.8351066918043,12.));
#111591=CARTESIAN_POINT('Ctrl Pts',(61.1739169618688,36.8176702205436,12.));
#111592=CARTESIAN_POINT('Ctrl Pts',(61.1591413839809,36.8002829554221,12.));
#111593=CARTESIAN_POINT('Ctrl Pts',(61.1443777154926,36.782944955654,12.));
#111594=CARTESIAN_POINT('Ctrl Pts',(61.1296260963468,36.7656562806381,12.));
#111595=CARTESIAN_POINT('Ctrl Pts',(61.1148866671821,36.7484169899591,12.));
#111596=CARTESIAN_POINT('Ctrl Pts',(61.1001595693357,36.7312271433799,12.));
#111597=CARTESIAN_POINT('Ctrl Pts',(61.085444944851,36.7140868008479,12.));
#111598=CARTESIAN_POINT('Ctrl Pts',(61.0707429364841,36.6969960225019,12.));
#111599=CARTESIAN_POINT('Ctrl Pts',(61.0560536877084,36.6799548686741,12.));
#111600=CARTESIAN_POINT('Ctrl Pts',(61.0413773427204,36.6629633998886,12.));
#111601=CARTESIAN_POINT('Ctrl Pts',(61.0267140464434,36.6460216768553,12.));
#111602=CARTESIAN_POINT('Ctrl Pts',(61.012063944535,36.6291297604775,12.));
#111603=CARTESIAN_POINT('Ctrl Pts',(60.9974271833982,36.6122877118599,12.));
#111604=CARTESIAN_POINT('Ctrl Pts',(60.9828039101887,36.5954955923109,12.));
#111605=CARTESIAN_POINT('Ctrl Pts',(60.9681942728237,36.5787534633416,12.));
#111606=CARTESIAN_POINT('Ctrl Pts',(60.9535984199874,36.5620613866616,12.));
#111607=CARTESIAN_POINT('Ctrl Pts',(60.9390165011357,36.5454194241866,12.));
#111608=CARTESIAN_POINT('Ctrl Pts',(60.924448666499,36.5288276380417,12.));
#111609=CARTESIAN_POINT('Ctrl Pts',(60.9098950670847,36.5122860905611,12.));
#111610=CARTESIAN_POINT('Ctrl Pts',(60.8953558546791,36.4957948442832,12.));
#111611=CARTESIAN_POINT('Ctrl Pts',(60.8808311818489,36.4793539619459,12.));
#111612=CARTESIAN_POINT('Ctrl Pts',(60.8663212019646,36.4629635065037,12.));
#111613=CARTESIAN_POINT('Ctrl Pts',(60.851826069218,36.4466235411353,12.));
#111614=CARTESIAN_POINT('Ctrl Pts',(60.8373459386397,36.4303341292497,12.));
#111615=CARTESIAN_POINT('Ctrl Pts',(60.8228809661179,36.414095334487,12.));
#111616=CARTESIAN_POINT('Ctrl Pts',(60.8084313084009,36.3979072207174,12.));
#111617=CARTESIAN_POINT('Ctrl Pts',(60.7939971230781,36.38176985204,12.));
#111618=CARTESIAN_POINT('Ctrl Pts',(60.779578568563,36.3656832927733,12.));
#111619=CARTESIAN_POINT('Ctrl Pts',(60.7651758040791,36.349647607448,12.));
#111620=CARTESIAN_POINT('Ctrl Pts',(60.7507889896283,36.3336628607844,12.));
#111621=CARTESIAN_POINT('Ctrl Pts',(60.7364182860388,36.3177291177148,12.));
#111622=CARTESIAN_POINT('Ctrl Pts',(60.7220638550396,36.3018464434204,12.));
#111623=CARTESIAN_POINT('Ctrl Pts',(60.7077258593268,36.2860149033586,12.));
#111624=CARTESIAN_POINT('Ctrl Pts',(60.6934044626304,36.2702345632883,12.));
#111625=CARTESIAN_POINT('Ctrl Pts',(60.6790998297823,36.2545054892911,12.));
#111626=CARTESIAN_POINT('Ctrl Pts',(60.6648121265908,36.2388277477225,12.));
#111627=CARTESIAN_POINT('Ctrl Pts',(60.6505415197055,36.2232014051549,12.));
#111628=CARTESIAN_POINT('Ctrl Pts',(60.6362881765014,36.2076265283261,12.));
#111629=CARTESIAN_POINT('Ctrl Pts',(60.6220522649129,36.1921031840618,12.));
#111630=CARTESIAN_POINT('Ctrl Pts',(60.6078339534151,36.1766314392624,12.));
#111631=CARTESIAN_POINT('Ctrl Pts',(60.5936334114082,36.1612113610758,12.));
#111632=CARTESIAN_POINT('Ctrl Pts',(60.5794508095555,36.1458430170425,12.));
#111633=CARTESIAN_POINT('Ctrl Pts',(60.5652863200732,36.1305264752195,12.));
#111634=CARTESIAN_POINT('Ctrl Pts',(60.5511401172014,36.1152618043756,12.));
#111635=CARTESIAN_POINT('Ctrl Pts',(60.5370123768841,36.1000490738532,12.));
#111636=CARTESIAN_POINT('Ctrl Pts',(60.5229032759001,36.0848883531969,12.));
#111637=CARTESIAN_POINT('Ctrl Pts',(60.5088129911357,36.0697797118377,12.));
#111638=CARTESIAN_POINT('Ctrl Pts',(60.4947416988396,36.0547232187681,12.));
#111639=CARTESIAN_POINT('Ctrl Pts',(60.4806895737643,36.0397189421617,12.));
#111640=CARTESIAN_POINT('Ctrl Pts',(60.4666567908053,36.0247669500867,12.));
#111641=CARTESIAN_POINT('Ctrl Pts',(60.452643526964,36.0098673113557,12.));
#111642=CARTESIAN_POINT('Ctrl Pts',(60.438649962949,35.9950200962175,12.));
#111643=CARTESIAN_POINT('Ctrl Pts',(60.4246762854961,35.9802253773534,12.));
#111644=CARTESIAN_POINT('Ctrl Pts',(60.4107226875759,35.9654832299627,12.));
#111645=CARTESIAN_POINT('Ctrl Pts',(60.3967893635487,35.9507937296726,12.));
#111646=CARTESIAN_POINT('Ctrl Pts',(60.3828765049031,35.9361569506955,12.));
#111647=CARTESIAN_POINT('Ctrl Pts',(60.368984296546,35.9215729642219,12.));
#111648=CARTESIAN_POINT('Ctrl Pts',(60.3551129108794,35.9070418358501,12.));
#111649=CARTESIAN_POINT('Ctrl Pts',(60.3412625135223,35.8925636280632,12.));
#111650=CARTESIAN_POINT('Ctrl Pts',(60.3274332746782,35.878138405151,12.));
#111651=CARTESIAN_POINT('Ctrl Pts',(60.313625378281,35.8637662371635,12.));
#111652=CARTESIAN_POINT('Ctrl Pts',(60.2998390330173,35.8494472046784,12.));
#111653=CARTESIAN_POINT('Ctrl Pts',(60.2860744798563,35.8351814020424,12.));
#111654=CARTESIAN_POINT('Ctrl Pts',(60.2723319687507,35.8209689272574,12.));
#111655=CARTESIAN_POINT('Ctrl Pts',(60.2586117365278,35.8068098723386,12.));
#111656=CARTESIAN_POINT('Ctrl Pts',(60.2449139865206,35.7927043145165,12.));
#111657=CARTESIAN_POINT('Ctrl Pts',(60.2312388621286,35.7786523045782,12.));
#111658=CARTESIAN_POINT('Ctrl Pts',(60.2175864449678,35.7646538667299,12.));
#111659=CARTESIAN_POINT('Ctrl Pts',(60.2066827086579,35.7534979801871,12.));
#111660=CARTESIAN_POINT('Ctrl Pts',(60.1985151474406,35.7451551752456,12.));
#111661=CARTESIAN_POINT('Ctrl Pts',(60.1930746580239,35.7396040203973,12.));
#111662=CARTESIAN_POINT('Ctrl Pts',(60.1903555511633,35.7368311217509,12.));
#111663=CARTESIAN_POINT('Ctrl Pts',(62.1730054756871,40.5060598100929,-1.11022302462516E-15));
#111664=CARTESIAN_POINT('Ctrl Pts',(62.1730054756871,40.5060598100929,4.));
#111665=CARTESIAN_POINT('Ctrl Pts',(62.1730054756872,40.5060598100929,8.));
#111666=CARTESIAN_POINT('Ctrl Pts',(62.1730054756872,40.5060598100929,12.));
#111667=CARTESIAN_POINT('Ctrl Pts',(62.2815834512355,40.5229411493977,-1.11022302462516E-15));
#111668=CARTESIAN_POINT('Ctrl Pts',(62.2815834512355,40.5229411493977,4.));
#111669=CARTESIAN_POINT('Ctrl Pts',(62.2815834512355,40.5229411493977,8.00000000000001));
#111670=CARTESIAN_POINT('Ctrl Pts',(62.2815834512355,40.5229411493977,12.));
#111671=CARTESIAN_POINT('Ctrl Pts',(62.4810961163745,40.4873422218648,-1.11022302462516E-15));
#111672=CARTESIAN_POINT('Ctrl Pts',(62.4810961163745,40.4873422218648,4.));
#111673=CARTESIAN_POINT('Ctrl Pts',(62.4810961163746,40.4873422218649,7.99999999999999));
#111674=CARTESIAN_POINT('Ctrl Pts',(62.4810961163746,40.4873422218649,12.));
#111675=CARTESIAN_POINT('Ctrl Pts',(62.6258675056116,40.3516729626244,-1.11022302462516E-15));
#111676=CARTESIAN_POINT('Ctrl Pts',(62.6258675056116,40.3516729626244,4.));
#111677=CARTESIAN_POINT('Ctrl Pts',(62.6258675056117,40.3516729626244,8.00000000000001));
#111678=CARTESIAN_POINT('Ctrl Pts',(62.6258675056117,40.3516729626244,12.));
#111679=CARTESIAN_POINT('Ctrl Pts',(62.6704278106374,40.282346977699,-1.11022302462516E-15));
#111680=CARTESIAN_POINT('Ctrl Pts',(62.6704278106374,40.282346977699,4.));
#111681=CARTESIAN_POINT('Ctrl Pts',(62.6704278106375,40.282346977699,8.));
#111682=CARTESIAN_POINT('Ctrl Pts',(62.6704278106375,40.282346977699,12.));
#111683=CARTESIAN_POINT('',(62.1730054756871,40.5060598100929,0.));
#111684=CARTESIAN_POINT('',(62.6704278106372,40.2823469776988,0.));
#111685=CARTESIAN_POINT('Ctrl Pts',(62.1730054756871,40.5060598100929,-2.77555756156289E-16));
#111686=CARTESIAN_POINT('Ctrl Pts',(62.2815834512355,40.5229411493977,-2.77555756156289E-16));
#111687=CARTESIAN_POINT('Ctrl Pts',(62.3955906884578,40.5025989050932,-2.77555756156289E-16));
#111688=CARTESIAN_POINT('Ctrl Pts',(62.4917232233448,40.4495806341087,-2.77555756156289E-16));
#111689=CARTESIAN_POINT('Ctrl Pts',(62.56382262451,40.4098169308703,-2.77555756156289E-16));
#111690=CARTESIAN_POINT('Ctrl Pts',(62.6258675056116,40.3516729626244,-2.7755575615629E-16));
#111691=CARTESIAN_POINT('Ctrl Pts',(62.6704278106374,40.282346977699,-2.77555756156289E-16));
#111692=CARTESIAN_POINT('',(62.6704278106372,40.2823469776988,12.));
#111693=CARTESIAN_POINT('Ctrl Pts',(62.6704278106374,40.282346977699,-1.11022302462516E-15));
#111694=CARTESIAN_POINT('Ctrl Pts',(62.6704278106374,40.282346977699,4.));
#111695=CARTESIAN_POINT('Ctrl Pts',(62.6704278106375,40.282346977699,8.));
#111696=CARTESIAN_POINT('Ctrl Pts',(62.6704278106375,40.282346977699,12.));
#111697=CARTESIAN_POINT('',(62.1730054756872,40.5060598100929,12.));
#111698=CARTESIAN_POINT('Ctrl Pts',(62.6704278106375,40.282346977699,12.));
#111699=CARTESIAN_POINT('Ctrl Pts',(62.6258675056117,40.3516729626244,12.));
#111700=CARTESIAN_POINT('Ctrl Pts',(62.5638226245101,40.4098169308703,12.));
#111701=CARTESIAN_POINT('Ctrl Pts',(62.4917232233448,40.4495806341087,12.));
#111702=CARTESIAN_POINT('Ctrl Pts',(62.3955906884578,40.5025989050932,12.));
#111703=CARTESIAN_POINT('Ctrl Pts',(62.2815834512355,40.5229411493977,12.));
#111704=CARTESIAN_POINT('Ctrl Pts',(62.1730054756872,40.5060598100929,12.));
#111705=CARTESIAN_POINT('Ctrl Pts',(62.1730054756872,40.5060598100929,12.));
#111706=CARTESIAN_POINT('Ctrl Pts',(62.1730054756872,40.5060598100929,8.));
#111707=CARTESIAN_POINT('Ctrl Pts',(62.1730054756871,40.5060598100929,4.));
#111708=CARTESIAN_POINT('Ctrl Pts',(62.1730054756871,40.5060598100929,-1.11022302462516E-15));
#111709=CARTESIAN_POINT('Origin',(3.16086693261782E-10,2.01487121870483E-10,
0.));
#111710=CARTESIAN_POINT('Origin',(3.16086693261782E-10,2.01487121870483E-10,
12.));
#111711=CARTESIAN_POINT('Origin',(3.16086693261782E-10,2.01487121870483E-10,
0.));
#111712=CARTESIAN_POINT('Ctrl Pts',(66.2207497120638,34.1330090612036,-1.11022302462516E-15));
#111713=CARTESIAN_POINT('Ctrl Pts',(66.2207497120638,34.1330090612036,4.));
#111714=CARTESIAN_POINT('Ctrl Pts',(66.2207497120638,34.1330090612036,8.));
#111715=CARTESIAN_POINT('Ctrl Pts',(66.2207497120638,34.1330090612036,12.));
#111716=CARTESIAN_POINT('Ctrl Pts',(66.2710935941675,34.035337929709,-1.11022302462516E-15));
#111717=CARTESIAN_POINT('Ctrl Pts',(66.2710935941675,34.035337929709,3.99999999999999));
#111718=CARTESIAN_POINT('Ctrl Pts',(66.2710935941675,34.035337929709,8.));
#111719=CARTESIAN_POINT('Ctrl Pts',(66.2710935941675,34.035337929709,12.));
#111720=CARTESIAN_POINT('Ctrl Pts',(66.3003999311009,33.8348041971636,-1.03714006649092E-15));
#111721=CARTESIAN_POINT('Ctrl Pts',(66.3003999311009,33.8348041971636,4.00000000000001));
#111722=CARTESIAN_POINT('Ctrl Pts',(66.3003999311009,33.8348041971637,8.));
#111723=CARTESIAN_POINT('Ctrl Pts',(66.3003999311009,33.8348041971637,12.));
#111724=CARTESIAN_POINT('Ctrl Pts',(66.2174610329232,33.6545652280944,-8.63611844392939E-16));
#111725=CARTESIAN_POINT('Ctrl Pts',(66.2174610329232,33.6545652280944,3.99999999999999));
#111726=CARTESIAN_POINT('Ctrl Pts',(66.2174610329232,33.6545652280945,8.));
#111727=CARTESIAN_POINT('Ctrl Pts',(66.2174610329232,33.6545652280945,12.));
#111728=CARTESIAN_POINT('Ctrl Pts',(66.1657795405672,33.5903722664961,-7.79957864155586E-16));
#111729=CARTESIAN_POINT('Ctrl Pts',(66.1657795405672,33.5903722664961,4.));
#111730=CARTESIAN_POINT('Ctrl Pts',(66.1657795405672,33.5903722664962,8.));
#111731=CARTESIAN_POINT('Ctrl Pts',(66.1657795405672,33.5903722664962,12.));
#111732=CARTESIAN_POINT('',(66.2207497120638,34.1330090612036,0.));
#111733=CARTESIAN_POINT('',(66.1657795405672,33.5903722664961,0.));
#111734=CARTESIAN_POINT('Ctrl Pts',(66.2207497120638,34.1330090612036,1.47525527571556E-16));
#111735=CARTESIAN_POINT('Ctrl Pts',(66.2710935941675,34.035337929709,1.47525527571554E-16));
#111736=CARTESIAN_POINT('Ctrl Pts',(66.2878400724152,33.9207472253973,1.8928721793398E-16));
#111737=CARTESIAN_POINT('Ctrl Pts',(66.2679350453204,33.8127833826289,2.63847361835582E-16));
#111738=CARTESIAN_POINT('Ctrl Pts',(66.2530062749993,33.7318105005526,3.19767469761783E-16));
#111739=CARTESIAN_POINT('Ctrl Pts',(66.2174610329232,33.6545652280944,3.94136707803771E-16));
#111740=CARTESIAN_POINT('Ctrl Pts',(66.1657795405672,33.5903722664961,4.77790688041126E-16));
#111741=CARTESIAN_POINT('',(66.1657795405673,33.5903722664962,12.));
#111742=CARTESIAN_POINT('Ctrl Pts',(66.1657795405672,33.5903722664961,-7.79957864155586E-16));
#111743=CARTESIAN_POINT('Ctrl Pts',(66.1657795405672,33.5903722664961,4.));
#111744=CARTESIAN_POINT('Ctrl Pts',(66.1657795405672,33.5903722664962,8.));
#111745=CARTESIAN_POINT('Ctrl Pts',(66.1657795405672,33.5903722664962,12.));
#111746=CARTESIAN_POINT('',(66.2207497120638,34.1330090612036,12.));
#111747=CARTESIAN_POINT('Ctrl Pts',(66.1657795405672,33.5903722664962,12.));
#111748=CARTESIAN_POINT('Ctrl Pts',(66.2174610329232,33.6545652280945,12.));
#111749=CARTESIAN_POINT('Ctrl Pts',(66.2530062749993,33.7318105005527,12.));
#111750=CARTESIAN_POINT('Ctrl Pts',(66.2679350453204,33.812783382629,12.));
#111751=CARTESIAN_POINT('Ctrl Pts',(66.2878400724151,33.9207472253974,12.));
#111752=CARTESIAN_POINT('Ctrl Pts',(66.2710935941675,34.035337929709,12.));
#111753=CARTESIAN_POINT('Ctrl Pts',(66.2207497120638,34.1330090612036,12.));
#111754=CARTESIAN_POINT('Ctrl Pts',(66.2207497120638,34.1330090612036,12.));
#111755=CARTESIAN_POINT('Ctrl Pts',(66.2207497120638,34.1330090612036,8.));
#111756=CARTESIAN_POINT('Ctrl Pts',(66.2207497120638,34.1330090612036,4.));
#111757=CARTESIAN_POINT('Ctrl Pts',(66.2207497120638,34.1330090612036,-1.11022302462516E-15));
#111758=CARTESIAN_POINT('Ctrl Pts',(63.0759831361898,30.3549065457811,0.));
#111759=CARTESIAN_POINT('Ctrl Pts',(63.0759831361898,30.3549065457811,12.));
#111760=CARTESIAN_POINT('Ctrl Pts',(63.078933570069,30.357431906933,0.));
#111761=CARTESIAN_POINT('Ctrl Pts',(63.078933570069,30.357431906933,12.));
#111762=CARTESIAN_POINT('Ctrl Pts',(63.0848371718048,30.3624877680651,0.));
#111763=CARTESIAN_POINT('Ctrl Pts',(63.0848371718048,30.3624877680651,12.));
#111764=CARTESIAN_POINT('Ctrl Pts',(63.0937007763471,30.3700869762507,0.));
#111765=CARTESIAN_POINT('Ctrl Pts',(63.0937007763471,30.3700869762507,12.));
#111766=CARTESIAN_POINT('Ctrl Pts',(63.105535320226,30.3802500880403,0.));
#111767=CARTESIAN_POINT('Ctrl Pts',(63.105535320226,30.3802500880403,12.));
#111768=CARTESIAN_POINT('Ctrl Pts',(63.1203558300657,30.3930053710484,0.));
#111769=CARTESIAN_POINT('Ctrl Pts',(63.1203558300657,30.3930053710484,12.));
#111770=CARTESIAN_POINT('Ctrl Pts',(63.135203629844,30.4058120432229,0.));
#111771=CARTESIAN_POINT('Ctrl Pts',(63.135203629844,30.4058120432229,12.));
#111772=CARTESIAN_POINT('Ctrl Pts',(63.1500786361459,30.418670087563,0.));
#111773=CARTESIAN_POINT('Ctrl Pts',(63.1500786361459,30.418670087563,12.));
#111774=CARTESIAN_POINT('Ctrl Pts',(63.164980701691,30.4315794659731,0.));
#111775=CARTESIAN_POINT('Ctrl Pts',(63.164980701691,30.4315794659731,12.));
#111776=CARTESIAN_POINT('Ctrl Pts',(63.179909617189,30.4445401192381,0.));
#111777=CARTESIAN_POINT('Ctrl Pts',(63.179909617189,30.4445401192381,12.));
#111778=CARTESIAN_POINT('Ctrl Pts',(63.1948651386942,30.4575519763337,0.));
#111779=CARTESIAN_POINT('Ctrl Pts',(63.1948651386942,30.4575519763337,12.));
#111780=CARTESIAN_POINT('Ctrl Pts',(63.2098470086636,30.470614961416,0.));
#111781=CARTESIAN_POINT('Ctrl Pts',(63.2098470086636,30.470614961416,12.));
#111782=CARTESIAN_POINT('Ctrl Pts',(63.2248549788221,30.4837290014989,0.));
#111783=CARTESIAN_POINT('Ctrl Pts',(63.2248549788221,30.4837290014989,12.));
#111784=CARTESIAN_POINT('Ctrl Pts',(63.2398888342545,30.4968940344998,0.));
#111785=CARTESIAN_POINT('Ctrl Pts',(63.2398888342545,30.4968940344998,12.));
#111786=CARTESIAN_POINT('Ctrl Pts',(63.2549483856215,30.5101100066659,0.));
#111787=CARTESIAN_POINT('Ctrl Pts',(63.2549483856215,30.5101100066659,12.));
#111788=CARTESIAN_POINT('Ctrl Pts',(63.2700334577639,30.5233768687865,0.));
#111789=CARTESIAN_POINT('Ctrl Pts',(63.2700334577639,30.5233768687865,12.));
#111790=CARTESIAN_POINT('Ctrl Pts',(63.2851438802473,30.5366945730508,0.));
#111791=CARTESIAN_POINT('Ctrl Pts',(63.2851438802473,30.5366945730508,12.));
#111792=CARTESIAN_POINT('Ctrl Pts',(63.3002794756086,30.5500630691359,0.));
#111793=CARTESIAN_POINT('Ctrl Pts',(63.3002794756086,30.5500630691359,12.));
#111794=CARTESIAN_POINT('Ctrl Pts',(63.3154400534397,30.563482302238,0.));
#111795=CARTESIAN_POINT('Ctrl Pts',(63.3154400534397,30.563482302238,12.));
#111796=CARTESIAN_POINT('Ctrl Pts',(63.3306254165126,30.5769522151164,0.));
#111797=CARTESIAN_POINT('Ctrl Pts',(63.3306254165126,30.5769522151164,12.));
#111798=CARTESIAN_POINT('Ctrl Pts',(63.3458353646154,30.5904727493712,0.));
#111799=CARTESIAN_POINT('Ctrl Pts',(63.3458353646154,30.5904727493712,12.));
#111800=CARTESIAN_POINT('Ctrl Pts',(63.3610696989577,30.6040438469078,0.));
#111801=CARTESIAN_POINT('Ctrl Pts',(63.3610696989577,30.6040438469078,12.));
#111802=CARTESIAN_POINT('Ctrl Pts',(63.3763282271796,30.6176654515967,0.));
#111803=CARTESIAN_POINT('Ctrl Pts',(63.3763282271796,30.6176654515967,12.));
#111804=CARTESIAN_POINT('Ctrl Pts',(63.3916107631376,30.6313375092062,0.));
#111805=CARTESIAN_POINT('Ctrl Pts',(63.3916107631376,30.6313375092062,12.));
#111806=CARTESIAN_POINT('Ctrl Pts',(63.4069171245066,30.6450599666121,0.));
#111807=CARTESIAN_POINT('Ctrl Pts',(63.4069171245066,30.6450599666121,12.));
#111808=CARTESIAN_POINT('Ctrl Pts',(63.4222471311239,30.6588327712484,0.));
#111809=CARTESIAN_POINT('Ctrl Pts',(63.4222471311239,30.6588327712484,12.));
#111810=CARTESIAN_POINT('Ctrl Pts',(63.4376006029604,30.6726558704315,0.));
#111811=CARTESIAN_POINT('Ctrl Pts',(63.4376006029604,30.6726558704315,12.));
#111812=CARTESIAN_POINT('Ctrl Pts',(63.4529773584249,30.6865292107929,0.));
#111813=CARTESIAN_POINT('Ctrl Pts',(63.4529773584249,30.6865292107929,12.));
#111814=CARTESIAN_POINT('Ctrl Pts',(63.4683772152529,30.7004527385821,0.));
#111815=CARTESIAN_POINT('Ctrl Pts',(63.4683772152529,30.7004527385821,12.));
#111816=CARTESIAN_POINT('Ctrl Pts',(63.4837999912771,30.7144263999265,0.));
#111817=CARTESIAN_POINT('Ctrl Pts',(63.4837999912771,30.7144263999265,12.));
#111818=CARTESIAN_POINT('Ctrl Pts',(63.4992455051795,30.7284501410822,0.));
#111819=CARTESIAN_POINT('Ctrl Pts',(63.4992455051795,30.7284501410822,12.));
#111820=CARTESIAN_POINT('Ctrl Pts',(63.5147135773894,30.7425239087281,0.));
#111821=CARTESIAN_POINT('Ctrl Pts',(63.5147135773894,30.7425239087281,12.));
#111822=CARTESIAN_POINT('Ctrl Pts',(63.5302040304142,30.7566476500757,0.));
#111823=CARTESIAN_POINT('Ctrl Pts',(63.5302040304142,30.7566476500757,12.));
#111824=CARTESIAN_POINT('Ctrl Pts',(63.5457166883537,30.7708213127159,0.));
#111825=CARTESIAN_POINT('Ctrl Pts',(63.5457166883537,30.7708213127159,12.));
#111826=CARTESIAN_POINT('Ctrl Pts',(63.5612513766,30.7850448445205,0.));
#111827=CARTESIAN_POINT('Ctrl Pts',(63.5612513766,30.7850448445205,12.));
#111828=CARTESIAN_POINT('Ctrl Pts',(63.5768079214881,30.7993181935271,0.));
#111829=CARTESIAN_POINT('Ctrl Pts',(63.5768079214881,30.7993181935271,12.));
#111830=CARTESIAN_POINT('Ctrl Pts',(63.5923861498987,30.813641307801,0.));
#111831=CARTESIAN_POINT('Ctrl Pts',(63.5923861498987,30.813641307801,12.));
#111832=CARTESIAN_POINT('Ctrl Pts',(63.6079858892771,30.8280141354459,0.));
#111833=CARTESIAN_POINT('Ctrl Pts',(63.6079858892771,30.8280141354459,12.));
#111834=CARTESIAN_POINT('Ctrl Pts',(63.6236069678055,30.8424366246672,0.));
#111835=CARTESIAN_POINT('Ctrl Pts',(63.6236069678055,30.8424366246672,12.));
#111836=CARTESIAN_POINT('Ctrl Pts',(63.6392492145233,30.8569087238131,0.));
#111837=CARTESIAN_POINT('Ctrl Pts',(63.6392492145233,30.8569087238131,12.));
#111838=CARTESIAN_POINT('Ctrl Pts',(63.6549124594666,30.8714303814194,0.));
#111839=CARTESIAN_POINT('Ctrl Pts',(63.6549124594666,30.8714303814194,12.));
#111840=CARTESIAN_POINT('Ctrl Pts',(63.6705965337971,30.8860015462475,0.));
#111841=CARTESIAN_POINT('Ctrl Pts',(63.6705965337971,30.8860015462475,12.));
#111842=CARTESIAN_POINT('Ctrl Pts',(63.6863012697328,30.900622167269,0.));
#111843=CARTESIAN_POINT('Ctrl Pts',(63.6863012697328,30.900622167269,12.));
#111844=CARTESIAN_POINT('Ctrl Pts',(63.7020265004792,30.9152921936465,0.));
#111845=CARTESIAN_POINT('Ctrl Pts',(63.7020265004792,30.9152921936465,12.));
#111846=CARTESIAN_POINT('Ctrl Pts',(63.7177720601609,30.9300115747116,0.));
#111847=CARTESIAN_POINT('Ctrl Pts',(63.7177720601609,30.9300115747116,12.));
#111848=CARTESIAN_POINT('Ctrl Pts',(63.7335377837441,30.9447802599355,0.));
#111849=CARTESIAN_POINT('Ctrl Pts',(63.7335377837441,30.9447802599355,12.));
#111850=CARTESIAN_POINT('Ctrl Pts',(63.749323506987,30.9595981989104,0.));
#111851=CARTESIAN_POINT('Ctrl Pts',(63.749323506987,30.9595981989104,12.));
#111852=CARTESIAN_POINT('Ctrl Pts',(63.7651290664733,30.9744653413689,0.));
#111853=CARTESIAN_POINT('Ctrl Pts',(63.7651290664733,30.9744653413689,12.));
#111854=CARTESIAN_POINT('Ctrl Pts',(63.7809542996264,30.989381637191,0.));
#111855=CARTESIAN_POINT('Ctrl Pts',(63.7809542996264,30.989381637191,12.));
#111856=CARTESIAN_POINT('Ctrl Pts',(63.796799044728,31.0043470364108,0.));
#111857=CARTESIAN_POINT('Ctrl Pts',(63.796799044728,31.0043470364108,12.));
#111858=CARTESIAN_POINT('Ctrl Pts',(63.8126631409364,31.0193614892171,0.));
#111859=CARTESIAN_POINT('Ctrl Pts',(63.8126631409364,31.0193614892171,12.));
#111860=CARTESIAN_POINT('Ctrl Pts',(63.8285464282846,31.0344249459538,0.));
#111861=CARTESIAN_POINT('Ctrl Pts',(63.8285464282846,31.0344249459538,12.));
#111862=CARTESIAN_POINT('Ctrl Pts',(63.8444487476611,31.0495373571215,0.));
#111863=CARTESIAN_POINT('Ctrl Pts',(63.8444487476611,31.0495373571215,12.));
#111864=CARTESIAN_POINT('Ctrl Pts',(63.8603699407922,31.0646986733723,0.));
#111865=CARTESIAN_POINT('Ctrl Pts',(63.8603699407922,31.0646986733723,12.));
#111866=CARTESIAN_POINT('Ctrl Pts',(63.8763098502237,31.0799088455041,0.));
#111867=CARTESIAN_POINT('Ctrl Pts',(63.8763098502237,31.0799088455041,12.));
#111868=CARTESIAN_POINT('Ctrl Pts',(63.8922683192964,31.0951678244455,0.));
#111869=CARTESIAN_POINT('Ctrl Pts',(63.8922683192964,31.0951678244455,12.));
#111870=CARTESIAN_POINT('Ctrl Pts',(63.9082451921448,31.1104755612607,0.));
#111871=CARTESIAN_POINT('Ctrl Pts',(63.9082451921448,31.1104755612607,12.));
#111872=CARTESIAN_POINT('Ctrl Pts',(63.9242403136955,31.1258320071545,0.));
#111873=CARTESIAN_POINT('Ctrl Pts',(63.9242403136955,31.1258320071545,12.));
#111874=CARTESIAN_POINT('Ctrl Pts',(63.940253529665,31.1412371134727,0.));
#111875=CARTESIAN_POINT('Ctrl Pts',(63.940253529665,31.1412371134727,12.));
#111876=CARTESIAN_POINT('Ctrl Pts',(63.9562846865567,31.1566908316992,0.));
#111877=CARTESIAN_POINT('Ctrl Pts',(63.9562846865567,31.1566908316992,12.));
#111878=CARTESIAN_POINT('Ctrl Pts',(63.9723336316551,31.1721931134487,0.));
#111879=CARTESIAN_POINT('Ctrl Pts',(63.9723336316551,31.1721931134487,12.));
#111880=CARTESIAN_POINT('Ctrl Pts',(63.9884002130211,31.1877439104717,0.));
#111881=CARTESIAN_POINT('Ctrl Pts',(63.9884002130211,31.1877439104717,12.));
#111882=CARTESIAN_POINT('Ctrl Pts',(64.0044842794831,31.2033431746558,0.));
#111883=CARTESIAN_POINT('Ctrl Pts',(64.0044842794831,31.2033431746558,12.));
#111884=CARTESIAN_POINT('Ctrl Pts',(64.02058568063,31.2189908580245,0.));
#111885=CARTESIAN_POINT('Ctrl Pts',(64.02058568063,31.2189908580245,12.));
#111886=CARTESIAN_POINT('Ctrl Pts',(64.0367042667984,31.2346869127297,0.));
#111887=CARTESIAN_POINT('Ctrl Pts',(64.0367042667984,31.2346869127297,12.));
#111888=CARTESIAN_POINT('Ctrl Pts',(64.0528398890657,31.2504312910451,0.));
#111889=CARTESIAN_POINT('Ctrl Pts',(64.0528398890657,31.2504312910451,12.));
#111890=CARTESIAN_POINT('Ctrl Pts',(64.0689923992461,31.2662239453728,0.));
#111891=CARTESIAN_POINT('Ctrl Pts',(64.0689923992461,31.2662239453728,12.));
#111892=CARTESIAN_POINT('Ctrl Pts',(64.0851616498852,31.2820648282447,0.));
#111893=CARTESIAN_POINT('Ctrl Pts',(64.0851616498852,31.2820648282447,12.));
#111894=CARTESIAN_POINT('Ctrl Pts',(64.1013474942556,31.2979538923214,0.));
#111895=CARTESIAN_POINT('Ctrl Pts',(64.1013474942556,31.2979538923214,12.));
#111896=CARTESIAN_POINT('Ctrl Pts',(64.117549786349,31.3138910903859,0.));
#111897=CARTESIAN_POINT('Ctrl Pts',(64.117549786349,31.3138910903859,12.));
#111898=CARTESIAN_POINT('Ctrl Pts',(64.133768380869,31.3298763753377,0.));
#111899=CARTESIAN_POINT('Ctrl Pts',(64.133768380869,31.3298763753377,12.));
#111900=CARTESIAN_POINT('Ctrl Pts',(64.1500031332282,31.3459097002006,0.));
#111901=CARTESIAN_POINT('Ctrl Pts',(64.1500031332282,31.3459097002006,12.));
#111902=CARTESIAN_POINT('Ctrl Pts',(64.166253899542,31.3619910181228,0.));
#111903=CARTESIAN_POINT('Ctrl Pts',(64.166253899542,31.3619910181228,12.));
#111904=CARTESIAN_POINT('Ctrl Pts',(64.1825205366224,31.3781202823754,0.));
#111905=CARTESIAN_POINT('Ctrl Pts',(64.1825205366224,31.3781202823754,12.));
#111906=CARTESIAN_POINT('Ctrl Pts',(64.1988029019707,31.3942974463446,0.));
#111907=CARTESIAN_POINT('Ctrl Pts',(64.1988029019707,31.3942974463446,12.));
#111908=CARTESIAN_POINT('Ctrl Pts',(64.2151008537697,31.410522463528,0.));
#111909=CARTESIAN_POINT('Ctrl Pts',(64.2151008537697,31.410522463528,12.));
#111910=CARTESIAN_POINT('Ctrl Pts',(64.231414250881,31.4267952875423,0.));
#111911=CARTESIAN_POINT('Ctrl Pts',(64.231414250881,31.4267952875423,12.));
#111912=CARTESIAN_POINT('Ctrl Pts',(64.2477429528393,31.4431158721222,0.));
#111913=CARTESIAN_POINT('Ctrl Pts',(64.2477429528393,31.4431158721222,12.));
#111914=CARTESIAN_POINT('Ctrl Pts',(64.2640868198473,31.4594841711195,0.));
#111915=CARTESIAN_POINT('Ctrl Pts',(64.2640868198473,31.4594841711195,12.));
#111916=CARTESIAN_POINT('Ctrl Pts',(64.2804457127671,31.4759001384941,0.));
#111917=CARTESIAN_POINT('Ctrl Pts',(64.2804457127671,31.4759001384941,12.));
#111918=CARTESIAN_POINT('Ctrl Pts',(64.2968194931158,31.4923637283132,0.));
#111919=CARTESIAN_POINT('Ctrl Pts',(64.2968194931158,31.4923637283132,12.));
#111920=CARTESIAN_POINT('Ctrl Pts',(64.3132080230637,31.5088748947582,0.));
#111921=CARTESIAN_POINT('Ctrl Pts',(64.3132080230637,31.5088748947582,12.));
#111922=CARTESIAN_POINT('Ctrl Pts',(64.3296111654283,31.5254335921245,0.));
#111923=CARTESIAN_POINT('Ctrl Pts',(64.3296111654283,31.5254335921245,12.));
#111924=CARTESIAN_POINT('Ctrl Pts',(64.3460287836687,31.5420397748191,0.));
#111925=CARTESIAN_POINT('Ctrl Pts',(64.3460287836687,31.5420397748191,12.));
#111926=CARTESIAN_POINT('Ctrl Pts',(64.3624607418768,31.5586933973515,0.));
#111927=CARTESIAN_POINT('Ctrl Pts',(64.3624607418768,31.5586933973515,12.));
#111928=CARTESIAN_POINT('Ctrl Pts',(64.3789069047733,31.5753944143336,0.));
#111929=CARTESIAN_POINT('Ctrl Pts',(64.3789069047733,31.5753944143336,12.));
#111930=CARTESIAN_POINT('Ctrl Pts',(64.3953671377046,31.5921427804865,0.));
#111931=CARTESIAN_POINT('Ctrl Pts',(64.3953671377046,31.5921427804865,12.));
#111932=CARTESIAN_POINT('Ctrl Pts',(64.4118413066378,31.6089384506395,0.));
#111933=CARTESIAN_POINT('Ctrl Pts',(64.4118413066378,31.6089384506395,12.));
#111934=CARTESIAN_POINT('Ctrl Pts',(64.4283292781565,31.6257813797288,0.));
#111935=CARTESIAN_POINT('Ctrl Pts',(64.4283292781565,31.6257813797288,12.));
#111936=CARTESIAN_POINT('Ctrl Pts',(64.4448309194525,31.6426715227878,0.));
#111937=CARTESIAN_POINT('Ctrl Pts',(64.4448309194525,31.6426715227878,12.));
#111938=CARTESIAN_POINT('Ctrl Pts',(64.4613460983214,31.6596088349482,0.));
#111939=CARTESIAN_POINT('Ctrl Pts',(64.4613460983214,31.6596088349482,12.));
#111940=CARTESIAN_POINT('Ctrl Pts',(64.4778746831614,31.6765932714464,0.));
#111941=CARTESIAN_POINT('Ctrl Pts',(64.4778746831614,31.6765932714464,12.));
#111942=CARTESIAN_POINT('Ctrl Pts',(64.4944165429674,31.6936247876229,0.));
#111943=CARTESIAN_POINT('Ctrl Pts',(64.4944165429674,31.6936247876229,12.));
#111944=CARTESIAN_POINT('Ctrl Pts',(64.510971547327,31.7107033389201,0.));
#111945=CARTESIAN_POINT('Ctrl Pts',(64.510971547327,31.7107033389201,12.));
#111946=CARTESIAN_POINT('Ctrl Pts',(64.5275395664124,31.7278288808731,0.));
#111947=CARTESIAN_POINT('Ctrl Pts',(64.5275395664124,31.7278288808731,12.));
#111948=CARTESIAN_POINT('Ctrl Pts',(64.544120470977,31.7450013691112,0.));
#111949=CARTESIAN_POINT('Ctrl Pts',(64.544120470977,31.7450013691112,12.));
#111950=CARTESIAN_POINT('Ctrl Pts',(64.5607141323521,31.7622207593634,0.));
#111951=CARTESIAN_POINT('Ctrl Pts',(64.5607141323521,31.7622207593634,12.));
#111952=CARTESIAN_POINT('Ctrl Pts',(64.5773204224429,31.7794870074583,0.));
#111953=CARTESIAN_POINT('Ctrl Pts',(64.5773204224429,31.7794870074583,12.));
#111954=CARTESIAN_POINT('Ctrl Pts',(64.5939392137235,31.7968000693218,0.));
#111955=CARTESIAN_POINT('Ctrl Pts',(64.5939392137235,31.7968000693218,12.));
#111956=CARTESIAN_POINT('Ctrl Pts',(64.6105703792312,31.8141599009684,0.));
#111957=CARTESIAN_POINT('Ctrl Pts',(64.6105703792312,31.8141599009684,12.));
#111958=CARTESIAN_POINT('Ctrl Pts',(64.6272137925627,31.8315664585026,0.));
#111959=CARTESIAN_POINT('Ctrl Pts',(64.6272137925627,31.8315664585026,12.));
#111960=CARTESIAN_POINT('Ctrl Pts',(64.6438693278714,31.8490196981248,0.));
#111961=CARTESIAN_POINT('Ctrl Pts',(64.6438693278714,31.8490196981248,12.));
#111962=CARTESIAN_POINT('Ctrl Pts',(64.6605368598629,31.8665195761311,0.));
#111963=CARTESIAN_POINT('Ctrl Pts',(64.6605368598629,31.8665195761311,12.));
#111964=CARTESIAN_POINT('Ctrl Pts',(64.6772162637907,31.8840660489107,0.));
#111965=CARTESIAN_POINT('Ctrl Pts',(64.6772162637907,31.8840660489107,12.));
#111966=CARTESIAN_POINT('Ctrl Pts',(64.6939074154498,31.9016590729374,0.));
#111967=CARTESIAN_POINT('Ctrl Pts',(64.6939074154498,31.9016590729374,12.));
#111968=CARTESIAN_POINT('Ctrl Pts',(64.7106101911732,31.9192986047706,0.));
#111969=CARTESIAN_POINT('Ctrl Pts',(64.7106101911732,31.9192986047706,12.));
#111970=CARTESIAN_POINT('Ctrl Pts',(64.7273244678297,31.9369846010616,0.));
#111971=CARTESIAN_POINT('Ctrl Pts',(64.7273244678297,31.9369846010616,12.));
#111972=CARTESIAN_POINT('Ctrl Pts',(64.7440501228202,31.9547170185534,0.));
#111973=CARTESIAN_POINT('Ctrl Pts',(64.7440501228202,31.9547170185534,12.));
#111974=CARTESIAN_POINT('Ctrl Pts',(64.7607870340735,31.9724958140789,0.));
#111975=CARTESIAN_POINT('Ctrl Pts',(64.7607870340735,31.9724958140789,12.));
#111976=CARTESIAN_POINT('Ctrl Pts',(64.77753508004,31.990320944552,0.));
#111977=CARTESIAN_POINT('Ctrl Pts',(64.77753508004,31.990320944552,12.));
#111978=CARTESIAN_POINT('Ctrl Pts',(64.7942941396881,32.0081923669677,0.));
#111979=CARTESIAN_POINT('Ctrl Pts',(64.7942941396881,32.0081923669677,12.));
#111980=CARTESIAN_POINT('Ctrl Pts',(64.8110640925021,32.0261100384092,0.));
#111981=CARTESIAN_POINT('Ctrl Pts',(64.8110640925021,32.0261100384092,12.));
#111982=CARTESIAN_POINT('Ctrl Pts',(64.8278448184786,32.0440739160477,0.));
#111983=CARTESIAN_POINT('Ctrl Pts',(64.8278448184786,32.0440739160477,12.));
#111984=CARTESIAN_POINT('Ctrl Pts',(64.8446361981234,32.0620839571408,0.));
#111985=CARTESIAN_POINT('Ctrl Pts',(64.8446361981234,32.0620839571408,12.));
#111986=CARTESIAN_POINT('Ctrl Pts',(64.861438112445,32.0801401190241,0.));
#111987=CARTESIAN_POINT('Ctrl Pts',(64.861438112445,32.0801401190241,12.));
#111988=CARTESIAN_POINT('Ctrl Pts',(64.878250442952,32.0982423591108,0.));
#111989=CARTESIAN_POINT('Ctrl Pts',(64.878250442952,32.0982423591108,12.));
#111990=CARTESIAN_POINT('Ctrl Pts',(64.8950730716493,32.1163906348979,0.));
#111991=CARTESIAN_POINT('Ctrl Pts',(64.8950730716493,32.1163906348979,12.));
#111992=CARTESIAN_POINT('Ctrl Pts',(64.9119058810362,32.1345849039671,0.));
#111993=CARTESIAN_POINT('Ctrl Pts',(64.9119058810362,32.1345849039671,12.));
#111994=CARTESIAN_POINT('Ctrl Pts',(64.9287487541018,32.1528251239832,0.));
#111995=CARTESIAN_POINT('Ctrl Pts',(64.9287487541018,32.1528251239832,12.));
#111996=CARTESIAN_POINT('Ctrl Pts',(64.9456015743203,32.171111252686,0.));
#111997=CARTESIAN_POINT('Ctrl Pts',(64.9456015743203,32.171111252686,12.));
#111998=CARTESIAN_POINT('Ctrl Pts',(64.9624642256477,32.1894432478889,0.));
#111999=CARTESIAN_POINT('Ctrl Pts',(64.9624642256477,32.1894432478889,12.));
#112000=CARTESIAN_POINT('Ctrl Pts',(64.9793365925194,32.2078210674858,0.));
#112001=CARTESIAN_POINT('Ctrl Pts',(64.9793365925194,32.2078210674858,12.));
#112002=CARTESIAN_POINT('Ctrl Pts',(64.996218559847,32.2262446694516,0.));
#112003=CARTESIAN_POINT('Ctrl Pts',(64.996218559847,32.2262446694516,12.));
#112004=CARTESIAN_POINT('Ctrl Pts',(65.0131100130155,32.244714011842,0.));
#112005=CARTESIAN_POINT('Ctrl Pts',(65.0131100130155,32.244714011842,12.));
#112006=CARTESIAN_POINT('Ctrl Pts',(65.0300108378786,32.2632290527855,0.));
#112007=CARTESIAN_POINT('Ctrl Pts',(65.0300108378786,32.2632290527855,12.));
#112008=CARTESIAN_POINT('Ctrl Pts',(65.0469209207548,32.2817897504799,0.));
#112009=CARTESIAN_POINT('Ctrl Pts',(65.0469209207548,32.2817897504799,12.));
#112010=CARTESIAN_POINT('Ctrl Pts',(65.0638401484245,32.3003960632001,0.));
#112011=CARTESIAN_POINT('Ctrl Pts',(65.0638401484245,32.3003960632001,12.));
#112012=CARTESIAN_POINT('Ctrl Pts',(65.0807684081278,32.3190479492985,0.));
#112013=CARTESIAN_POINT('Ctrl Pts',(65.0807684081278,32.3190479492985,12.));
#112014=CARTESIAN_POINT('Ctrl Pts',(65.097705587561,32.3377453672052,0.));
#112015=CARTESIAN_POINT('Ctrl Pts',(65.097705587561,32.3377453672052,12.));
#112016=CARTESIAN_POINT('Ctrl Pts',(65.1146515748723,32.3564882754213,0.));
#112017=CARTESIAN_POINT('Ctrl Pts',(65.1146515748723,32.3564882754213,12.));
#112018=CARTESIAN_POINT('Ctrl Pts',(65.1316062586586,32.3752766325135,0.));
#112019=CARTESIAN_POINT('Ctrl Pts',(65.1316062586586,32.3752766325135,12.));
#112020=CARTESIAN_POINT('Ctrl Pts',(65.1485695279628,32.3941103971218,0.));
#112021=CARTESIAN_POINT('Ctrl Pts',(65.1485695279628,32.3941103971218,12.));
#112022=CARTESIAN_POINT('Ctrl Pts',(65.165541272272,32.4129895279612,0.));
#112023=CARTESIAN_POINT('Ctrl Pts',(65.165541272272,32.4129895279612,12.));
#112024=CARTESIAN_POINT('Ctrl Pts',(65.182521381514,32.4319139838212,0.));
#112025=CARTESIAN_POINT('Ctrl Pts',(65.182521381514,32.4319139838212,12.));
#112026=CARTESIAN_POINT('Ctrl Pts',(65.1995097460545,32.4508837235613,0.));
#112027=CARTESIAN_POINT('Ctrl Pts',(65.1995097460545,32.4508837235613,12.));
#112028=CARTESIAN_POINT('Ctrl Pts',(65.2165062566936,32.4698987061037,0.));
#112029=CARTESIAN_POINT('Ctrl Pts',(65.2165062566936,32.4698987061037,12.));
#112030=CARTESIAN_POINT('Ctrl Pts',(65.2335108046625,32.4889588904397,0.));
#112031=CARTESIAN_POINT('Ctrl Pts',(65.2335108046625,32.4889588904397,12.));
#112032=CARTESIAN_POINT('Ctrl Pts',(65.2505232816215,32.508064235633,0.));
#112033=CARTESIAN_POINT('Ctrl Pts',(65.2505232816215,32.508064235633,12.));
#112034=CARTESIAN_POINT('Ctrl Pts',(65.2675435796558,32.5272147008191,0.));
#112035=CARTESIAN_POINT('Ctrl Pts',(65.2675435796558,32.5272147008191,12.));
#112036=CARTESIAN_POINT('Ctrl Pts',(65.2845715912717,32.5464102452013,0.));
#112037=CARTESIAN_POINT('Ctrl Pts',(65.2845715912717,32.5464102452013,12.));
#112038=CARTESIAN_POINT('Ctrl Pts',(65.3016072093907,32.565650828042,0.));
#112039=CARTESIAN_POINT('Ctrl Pts',(65.3016072093907,32.565650828042,12.));
#112040=CARTESIAN_POINT('Ctrl Pts',(65.3186503273498,32.5849364086679,0.));
#112041=CARTESIAN_POINT('Ctrl Pts',(65.3186503273498,32.5849364086679,12.));
#112042=CARTESIAN_POINT('Ctrl Pts',(65.3357008389004,32.6042669464752,0.));
#112043=CARTESIAN_POINT('Ctrl Pts',(65.3357008389004,32.6042669464752,12.));
#112044=CARTESIAN_POINT('Ctrl Pts',(65.3527586382082,32.6236424009302,0.));
#112045=CARTESIAN_POINT('Ctrl Pts',(65.3527586382082,32.6236424009302,12.));
#112046=CARTESIAN_POINT('Ctrl Pts',(65.3698236198511,32.6430627315673,0.));
#112047=CARTESIAN_POINT('Ctrl Pts',(65.3698236198511,32.6430627315673,12.));
#112048=CARTESIAN_POINT('Ctrl Pts',(65.3868956788178,32.6625278979807,0.));
#112049=CARTESIAN_POINT('Ctrl Pts',(65.3868956788178,32.6625278979807,12.));
#112050=CARTESIAN_POINT('Ctrl Pts',(65.4039747105033,32.6820378598263,0.));
#112051=CARTESIAN_POINT('Ctrl Pts',(65.4039747105033,32.6820378598263,12.));
#112052=CARTESIAN_POINT('Ctrl Pts',(65.4210606107029,32.7015925768261,0.));
#112053=CARTESIAN_POINT('Ctrl Pts',(65.4210606107029,32.7015925768261,12.));
#112054=CARTESIAN_POINT('Ctrl Pts',(65.4381532756062,32.7211920087682,0.));
#112055=CARTESIAN_POINT('Ctrl Pts',(65.4381532756062,32.7211920087682,12.));
#112056=CARTESIAN_POINT('Ctrl Pts',(65.4552526017907,32.7408361155038,0.));
#112057=CARTESIAN_POINT('Ctrl Pts',(65.4552526017907,32.7408361155038,12.));
#112058=CARTESIAN_POINT('Ctrl Pts',(65.4723584862129,32.7605248569382,0.));
#112059=CARTESIAN_POINT('Ctrl Pts',(65.4723584862129,32.7605248569382,12.));
#112060=CARTESIAN_POINT('Ctrl Pts',(65.4894708262071,32.7802581930294,0.));
#112061=CARTESIAN_POINT('Ctrl Pts',(65.4894708262071,32.7802581930294,12.));
#112062=CARTESIAN_POINT('Ctrl Pts',(65.5065895194938,32.8000360837981,0.));
#112063=CARTESIAN_POINT('Ctrl Pts',(65.5065895194938,32.8000360837981,12.));
#112064=CARTESIAN_POINT('Ctrl Pts',(65.5237144641864,32.8198584893319,0.));
#112065=CARTESIAN_POINT('Ctrl Pts',(65.5237144641864,32.8198584893319,12.));
#112066=CARTESIAN_POINT('Ctrl Pts',(65.5408455587963,32.8397253697865,0.));
#112067=CARTESIAN_POINT('Ctrl Pts',(65.5408455587963,32.8397253697865,12.));
#112068=CARTESIAN_POINT('Ctrl Pts',(65.5579827022412,32.8596366853826,0.));
#112069=CARTESIAN_POINT('Ctrl Pts',(65.5579827022412,32.8596366853826,12.));
#112070=CARTESIAN_POINT('Ctrl Pts',(65.575125793846,32.8795923964022,0.));
#112071=CARTESIAN_POINT('Ctrl Pts',(65.575125793846,32.8795923964022,12.));
#112072=CARTESIAN_POINT('Ctrl Pts',(65.5922747333181,32.899592463189,0.));
#112073=CARTESIAN_POINT('Ctrl Pts',(65.5922747333181,32.899592463189,12.));
#112074=CARTESIAN_POINT('Ctrl Pts',(65.6094294207267,32.9196368461457,0.));
#112075=CARTESIAN_POINT('Ctrl Pts',(65.6094294207267,32.9196368461457,12.));
#112076=CARTESIAN_POINT('Ctrl Pts',(65.6265897564782,32.9397255057273,0.));
#112077=CARTESIAN_POINT('Ctrl Pts',(65.6265897564782,32.9397255057273,12.));
#112078=CARTESIAN_POINT('Ctrl Pts',(65.6437556412956,32.9598584024318,0.));
#112079=CARTESIAN_POINT('Ctrl Pts',(65.6437556412956,32.9598584024318,12.));
#112080=CARTESIAN_POINT('Ctrl Pts',(65.6609269761902,32.9800354967847,0.));
#112081=CARTESIAN_POINT('Ctrl Pts',(65.6609269761902,32.9800354967847,12.));
#112082=CARTESIAN_POINT('Ctrl Pts',(65.6781036625041,33.0002567493581,0.));
#112083=CARTESIAN_POINT('Ctrl Pts',(65.6781036625041,33.0002567493581,12.));
#112084=CARTESIAN_POINT('Ctrl Pts',(65.6952856019542,33.0205221207877,0.));
#112085=CARTESIAN_POINT('Ctrl Pts',(65.6952856019542,33.0205221207877,12.));
#112086=CARTESIAN_POINT('Ctrl Pts',(65.7124726966805,33.0408315717874,0.));
#112087=CARTESIAN_POINT('Ctrl Pts',(65.7124726966805,33.0408315717874,12.));
#112088=CARTESIAN_POINT('Ctrl Pts',(65.729664849282,33.061185063158,0.));
#112089=CARTESIAN_POINT('Ctrl Pts',(65.729664849282,33.061185063158,12.));
#112090=CARTESIAN_POINT('Ctrl Pts',(65.7468619628808,33.0815825557976,0.));
#112091=CARTESIAN_POINT('Ctrl Pts',(65.7468619628808,33.0815825557976,12.));
#112092=CARTESIAN_POINT('Ctrl Pts',(65.7640639410653,33.102024010688,0.));
#112093=CARTESIAN_POINT('Ctrl Pts',(65.7640639410653,33.102024010688,12.));
#112094=CARTESIAN_POINT('Ctrl Pts',(65.7812706877691,33.1225093888669,0.));
#112095=CARTESIAN_POINT('Ctrl Pts',(65.7812706877691,33.1225093888669,12.));
#112096=CARTESIAN_POINT('Ctrl Pts',(65.7984821071621,33.1430386513975,0.));
#112097=CARTESIAN_POINT('Ctrl Pts',(65.7984821071621,33.1430386513975,12.));
#112098=CARTESIAN_POINT('Ctrl Pts',(65.8156981035504,33.16361175934,0.));
#112099=CARTESIAN_POINT('Ctrl Pts',(65.8156981035504,33.16361175934,12.));
#112100=CARTESIAN_POINT('Ctrl Pts',(65.8329185812379,33.1842286737053,0.));
#112101=CARTESIAN_POINT('Ctrl Pts',(65.8329185812379,33.1842286737053,12.));
#112102=CARTESIAN_POINT('Ctrl Pts',(65.8501434445174,33.2048893554496,0.));
#112103=CARTESIAN_POINT('Ctrl Pts',(65.8501434445174,33.2048893554496,12.));
#112104=CARTESIAN_POINT('Ctrl Pts',(65.8673725979591,33.2255937655656,0.));
#112105=CARTESIAN_POINT('Ctrl Pts',(65.8673725979591,33.2255937655656,12.));
#112106=CARTESIAN_POINT('Ctrl Pts',(65.8846059466382,33.2463418651498,0.));
#112107=CARTESIAN_POINT('Ctrl Pts',(65.8846059466382,33.2463418651498,12.));
#112108=CARTESIAN_POINT('Ctrl Pts',(65.901843396389,33.2671336154754,0.));
#112109=CARTESIAN_POINT('Ctrl Pts',(65.901843396389,33.2671336154754,12.));
#112110=CARTESIAN_POINT('Ctrl Pts',(65.9190848540422,33.2879689780566,0.));
#112111=CARTESIAN_POINT('Ctrl Pts',(65.9190848540422,33.2879689780566,12.));
#112112=CARTESIAN_POINT('Ctrl Pts',(65.9363302276822,33.3088479147151,0.));
#112113=CARTESIAN_POINT('Ctrl Pts',(65.9363302276822,33.3088479147151,12.));
#112114=CARTESIAN_POINT('Ctrl Pts',(65.9535794260802,33.3297703874249,0.));
#112115=CARTESIAN_POINT('Ctrl Pts',(65.9535794260802,33.3297703874249,12.));
#112116=CARTESIAN_POINT('Ctrl Pts',(65.9708323581385,33.3507363581579,0.));
#112117=CARTESIAN_POINT('Ctrl Pts',(65.9708323581385,33.3507363581579,12.));
#112118=CARTESIAN_POINT('Ctrl Pts',(65.9880889322822,33.3717457887095,0.));
#112119=CARTESIAN_POINT('Ctrl Pts',(65.9880889322822,33.3717457887095,12.));
#112120=CARTESIAN_POINT('Ctrl Pts',(66.0053490559826,33.3927986405612,0.));
#112121=CARTESIAN_POINT('Ctrl Pts',(66.0053490559826,33.3927986405612,12.));
#112122=CARTESIAN_POINT('Ctrl Pts',(66.0226126349482,33.4138948746408,0.));
#112123=CARTESIAN_POINT('Ctrl Pts',(66.0226126349482,33.4138948746408,12.));
#112124=CARTESIAN_POINT('Ctrl Pts',(66.0398795737827,33.4350344515128,0.));
#112125=CARTESIAN_POINT('Ctrl Pts',(66.0398795737827,33.4350344515128,12.));
#112126=CARTESIAN_POINT('Ctrl Pts',(66.0571497774484,33.4562173318053,0.));
#112127=CARTESIAN_POINT('Ctrl Pts',(66.0571497774484,33.4562173318053,12.));
#112128=CARTESIAN_POINT('Ctrl Pts',(66.0744231525445,33.4774434765762,0.));
#112129=CARTESIAN_POINT('Ctrl Pts',(66.0744231525445,33.4774434765762,12.));
#112130=CARTESIAN_POINT('Ctrl Pts',(66.0916996085237,33.4987128476618,0.));
#112131=CARTESIAN_POINT('Ctrl Pts',(66.0916996085237,33.4987128476618,12.));
#112132=CARTESIAN_POINT('Ctrl Pts',(66.1089790592673,33.5200254081212,0.));
#112133=CARTESIAN_POINT('Ctrl Pts',(66.1089790592673,33.5200254081212,12.));
#112134=CARTESIAN_POINT('Ctrl Pts',(66.1262614234579,33.5413811223398,0.));
#112135=CARTESIAN_POINT('Ctrl Pts',(66.1262614234579,33.5413811223398,12.));
#112136=CARTESIAN_POINT('Ctrl Pts',(66.1435466210966,33.5627799550423,0.));
#112137=CARTESIAN_POINT('Ctrl Pts',(66.1435466210966,33.5627799550423,12.));
#112138=CARTESIAN_POINT('Ctrl Pts',(66.1608345707551,33.5842218705103,0.));
#112139=CARTESIAN_POINT('Ctrl Pts',(66.1608345707551,33.5842218705103,12.));
#112140=CARTESIAN_POINT('Ctrl Pts',(66.1781251863998,33.6057068316758,0.));
#112141=CARTESIAN_POINT('Ctrl Pts',(66.1781251863998,33.6057068316758,12.));
#112142=CARTESIAN_POINT('Ctrl Pts',(66.1954183747167,33.6272347993519,0.));
#112143=CARTESIAN_POINT('Ctrl Pts',(66.1954183747167,33.6272347993519,12.));
#112144=CARTESIAN_POINT('Ctrl Pts',(66.2127140313777,33.648805731163,0.));
#112145=CARTESIAN_POINT('Ctrl Pts',(66.2127140313777,33.648805731163,12.));
#112146=CARTESIAN_POINT('Ctrl Pts',(66.2300120464323,33.6704195830526,0.));
#112147=CARTESIAN_POINT('Ctrl Pts',(66.2300120464323,33.6704195830526,12.));
#112148=CARTESIAN_POINT('Ctrl Pts',(66.2473123109626,33.6920763111575,0.));
#112149=CARTESIAN_POINT('Ctrl Pts',(66.2473123109626,33.6920763111575,12.));
#112150=CARTESIAN_POINT('Ctrl Pts',(66.2646147235444,33.713775873597,0.));
#112151=CARTESIAN_POINT('Ctrl Pts',(66.2646147235444,33.713775873597,12.));
#112152=CARTESIAN_POINT('Ctrl Pts',(66.2819191962273,33.7355182321862,0.));
#112153=CARTESIAN_POINT('Ctrl Pts',(66.2819191962273,33.7355182321862,12.));
#112154=CARTESIAN_POINT('Ctrl Pts',(66.2992256621001,33.7573033544374,0.));
#112155=CARTESIAN_POINT('Ctrl Pts',(66.2992256621001,33.7573033544374,12.));
#112156=CARTESIAN_POINT('Ctrl Pts',(66.3165340771053,33.7791312144798,0.));
#112157=CARTESIAN_POINT('Ctrl Pts',(66.3165340771053,33.7791312144798,12.));
#112158=CARTESIAN_POINT('Ctrl Pts',(66.3338444143559,33.8010017925666,0.));
#112159=CARTESIAN_POINT('Ctrl Pts',(66.3338444143559,33.8010017925666,12.));
#112160=CARTESIAN_POINT('Ctrl Pts',(66.3476942111456,33.8185324184602,0.));
#112161=CARTESIAN_POINT('Ctrl Pts',(66.3476942111456,33.8185324184602,12.));
#112162=CARTESIAN_POINT('Ctrl Pts',(66.3580824155565,33.8316996011751,0.));
#112163=CARTESIAN_POINT('Ctrl Pts',(66.3580824155565,33.8316996011751,12.));
#112164=CARTESIAN_POINT('Ctrl Pts',(66.3650082659593,33.8404862618803,0.));
#112165=CARTESIAN_POINT('Ctrl Pts',(66.3650082659593,33.8404862618803,12.));
#112166=CARTESIAN_POINT('Ctrl Pts',(66.3684712863594,33.8448817269567,0.));
#112167=CARTESIAN_POINT('Ctrl Pts',(66.3684712863594,33.8448817269567,12.));
#112168=CARTESIAN_POINT('',(63.0759831361898,30.3549065457811,0.));
#112169=CARTESIAN_POINT('Ctrl Pts',(63.0759831361898,30.3549065457811,0.));
#112170=CARTESIAN_POINT('Ctrl Pts',(63.078933570069,30.357431906933,0.));
#112171=CARTESIAN_POINT('Ctrl Pts',(63.0848371718048,30.3624877680651,0.));
#112172=CARTESIAN_POINT('Ctrl Pts',(63.0937007763471,30.3700869762507,0.));
#112173=CARTESIAN_POINT('Ctrl Pts',(63.105535320226,30.3802500880403,0.));
#112174=CARTESIAN_POINT('Ctrl Pts',(63.1203558300657,30.3930053710484,0.));
#112175=CARTESIAN_POINT('Ctrl Pts',(63.135203629844,30.4058120432229,0.));
#112176=CARTESIAN_POINT('Ctrl Pts',(63.1500786361459,30.418670087563,0.));
#112177=CARTESIAN_POINT('Ctrl Pts',(63.164980701691,30.4315794659731,0.));
#112178=CARTESIAN_POINT('Ctrl Pts',(63.179909617189,30.4445401192381,0.));
#112179=CARTESIAN_POINT('Ctrl Pts',(63.1948651386942,30.4575519763337,0.));
#112180=CARTESIAN_POINT('Ctrl Pts',(63.2098470086636,30.470614961416,0.));
#112181=CARTESIAN_POINT('Ctrl Pts',(63.2248549788221,30.4837290014989,0.));
#112182=CARTESIAN_POINT('Ctrl Pts',(63.2398888342545,30.4968940344998,0.));
#112183=CARTESIAN_POINT('Ctrl Pts',(63.2549483856215,30.5101100066659,0.));
#112184=CARTESIAN_POINT('Ctrl Pts',(63.2700334577639,30.5233768687865,0.));
#112185=CARTESIAN_POINT('Ctrl Pts',(63.2851438802473,30.5366945730508,0.));
#112186=CARTESIAN_POINT('Ctrl Pts',(63.3002794756086,30.5500630691359,0.));
#112187=CARTESIAN_POINT('Ctrl Pts',(63.3154400534397,30.563482302238,0.));
#112188=CARTESIAN_POINT('Ctrl Pts',(63.3306254165126,30.5769522151164,0.));
#112189=CARTESIAN_POINT('Ctrl Pts',(63.3458353646154,30.5904727493712,0.));
#112190=CARTESIAN_POINT('Ctrl Pts',(63.3610696989577,30.6040438469078,0.));
#112191=CARTESIAN_POINT('Ctrl Pts',(63.3763282271796,30.6176654515967,0.));
#112192=CARTESIAN_POINT('Ctrl Pts',(63.3916107631376,30.6313375092062,0.));
#112193=CARTESIAN_POINT('Ctrl Pts',(63.4069171245066,30.6450599666121,0.));
#112194=CARTESIAN_POINT('Ctrl Pts',(63.4222471311239,30.6588327712484,0.));
#112195=CARTESIAN_POINT('Ctrl Pts',(63.4376006029604,30.6726558704315,0.));
#112196=CARTESIAN_POINT('Ctrl Pts',(63.4529773584249,30.6865292107929,0.));
#112197=CARTESIAN_POINT('Ctrl Pts',(63.4683772152529,30.7004527385821,0.));
#112198=CARTESIAN_POINT('Ctrl Pts',(63.4837999912771,30.7144263999265,0.));
#112199=CARTESIAN_POINT('Ctrl Pts',(63.4992455051795,30.7284501410822,0.));
#112200=CARTESIAN_POINT('Ctrl Pts',(63.5147135773894,30.7425239087281,0.));
#112201=CARTESIAN_POINT('Ctrl Pts',(63.5302040304142,30.7566476500757,0.));
#112202=CARTESIAN_POINT('Ctrl Pts',(63.5457166883537,30.7708213127159,0.));
#112203=CARTESIAN_POINT('Ctrl Pts',(63.5612513766,30.7850448445205,0.));
#112204=CARTESIAN_POINT('Ctrl Pts',(63.5768079214881,30.7993181935271,0.));
#112205=CARTESIAN_POINT('Ctrl Pts',(63.5923861498987,30.813641307801,0.));
#112206=CARTESIAN_POINT('Ctrl Pts',(63.6079858892771,30.8280141354459,0.));
#112207=CARTESIAN_POINT('Ctrl Pts',(63.6236069678055,30.8424366246672,0.));
#112208=CARTESIAN_POINT('Ctrl Pts',(63.6392492145233,30.8569087238131,0.));
#112209=CARTESIAN_POINT('Ctrl Pts',(63.6549124594666,30.8714303814194,0.));
#112210=CARTESIAN_POINT('Ctrl Pts',(63.6705965337971,30.8860015462475,0.));
#112211=CARTESIAN_POINT('Ctrl Pts',(63.6863012697328,30.900622167269,0.));
#112212=CARTESIAN_POINT('Ctrl Pts',(63.7020265004792,30.9152921936465,0.));
#112213=CARTESIAN_POINT('Ctrl Pts',(63.7177720601609,30.9300115747116,0.));
#112214=CARTESIAN_POINT('Ctrl Pts',(63.7335377837441,30.9447802599355,0.));
#112215=CARTESIAN_POINT('Ctrl Pts',(63.749323506987,30.9595981989104,0.));
#112216=CARTESIAN_POINT('Ctrl Pts',(63.7651290664733,30.9744653413689,0.));
#112217=CARTESIAN_POINT('Ctrl Pts',(63.7809542996264,30.989381637191,0.));
#112218=CARTESIAN_POINT('Ctrl Pts',(63.796799044728,31.0043470364108,0.));
#112219=CARTESIAN_POINT('Ctrl Pts',(63.8126631409364,31.0193614892171,0.));
#112220=CARTESIAN_POINT('Ctrl Pts',(63.8285464282846,31.0344249459538,0.));
#112221=CARTESIAN_POINT('Ctrl Pts',(63.8444487476611,31.0495373571215,0.));
#112222=CARTESIAN_POINT('Ctrl Pts',(63.8603699407922,31.0646986733723,0.));
#112223=CARTESIAN_POINT('Ctrl Pts',(63.8763098502237,31.0799088455041,0.));
#112224=CARTESIAN_POINT('Ctrl Pts',(63.8922683192964,31.0951678244455,0.));
#112225=CARTESIAN_POINT('Ctrl Pts',(63.9082451921448,31.1104755612607,0.));
#112226=CARTESIAN_POINT('Ctrl Pts',(63.9242403136955,31.1258320071545,0.));
#112227=CARTESIAN_POINT('Ctrl Pts',(63.940253529665,31.1412371134727,0.));
#112228=CARTESIAN_POINT('Ctrl Pts',(63.9562846865567,31.1566908316992,0.));
#112229=CARTESIAN_POINT('Ctrl Pts',(63.9723336316551,31.1721931134487,0.));
#112230=CARTESIAN_POINT('Ctrl Pts',(63.9884002130211,31.1877439104717,0.));
#112231=CARTESIAN_POINT('Ctrl Pts',(64.0044842794831,31.2033431746558,0.));
#112232=CARTESIAN_POINT('Ctrl Pts',(64.02058568063,31.2189908580245,0.));
#112233=CARTESIAN_POINT('Ctrl Pts',(64.0367042667984,31.2346869127297,0.));
#112234=CARTESIAN_POINT('Ctrl Pts',(64.0528398890657,31.2504312910451,0.));
#112235=CARTESIAN_POINT('Ctrl Pts',(64.0689923992461,31.2662239453728,0.));
#112236=CARTESIAN_POINT('Ctrl Pts',(64.0851616498852,31.2820648282447,0.));
#112237=CARTESIAN_POINT('Ctrl Pts',(64.1013474942556,31.2979538923214,0.));
#112238=CARTESIAN_POINT('Ctrl Pts',(64.117549786349,31.3138910903859,0.));
#112239=CARTESIAN_POINT('Ctrl Pts',(64.133768380869,31.3298763753377,0.));
#112240=CARTESIAN_POINT('Ctrl Pts',(64.1500031332282,31.3459097002006,0.));
#112241=CARTESIAN_POINT('Ctrl Pts',(64.166253899542,31.3619910181228,0.));
#112242=CARTESIAN_POINT('Ctrl Pts',(64.1825205366224,31.3781202823754,0.));
#112243=CARTESIAN_POINT('Ctrl Pts',(64.1988029019707,31.3942974463446,0.));
#112244=CARTESIAN_POINT('Ctrl Pts',(64.2151008537697,31.410522463528,0.));
#112245=CARTESIAN_POINT('Ctrl Pts',(64.231414250881,31.4267952875423,0.));
#112246=CARTESIAN_POINT('Ctrl Pts',(64.2477429528393,31.4431158721222,0.));
#112247=CARTESIAN_POINT('Ctrl Pts',(64.2640868198473,31.4594841711195,0.));
#112248=CARTESIAN_POINT('Ctrl Pts',(64.2804457127671,31.4759001384941,0.));
#112249=CARTESIAN_POINT('Ctrl Pts',(64.2968194931158,31.4923637283132,0.));
#112250=CARTESIAN_POINT('Ctrl Pts',(64.3132080230637,31.5088748947582,0.));
#112251=CARTESIAN_POINT('Ctrl Pts',(64.3296111654283,31.5254335921245,0.));
#112252=CARTESIAN_POINT('Ctrl Pts',(64.3460287836687,31.5420397748191,0.));
#112253=CARTESIAN_POINT('Ctrl Pts',(64.3624607418768,31.5586933973515,0.));
#112254=CARTESIAN_POINT('Ctrl Pts',(64.3789069047733,31.5753944143336,0.));
#112255=CARTESIAN_POINT('Ctrl Pts',(64.3953671377046,31.5921427804865,0.));
#112256=CARTESIAN_POINT('Ctrl Pts',(64.4118413066378,31.6089384506395,0.));
#112257=CARTESIAN_POINT('Ctrl Pts',(64.4283292781565,31.6257813797288,0.));
#112258=CARTESIAN_POINT('Ctrl Pts',(64.4448309194525,31.6426715227878,0.));
#112259=CARTESIAN_POINT('Ctrl Pts',(64.4613460983214,31.6596088349482,0.));
#112260=CARTESIAN_POINT('Ctrl Pts',(64.4778746831614,31.6765932714464,0.));
#112261=CARTESIAN_POINT('Ctrl Pts',(64.4944165429674,31.6936247876229,0.));
#112262=CARTESIAN_POINT('Ctrl Pts',(64.510971547327,31.7107033389201,0.));
#112263=CARTESIAN_POINT('Ctrl Pts',(64.5275395664124,31.7278288808731,0.));
#112264=CARTESIAN_POINT('Ctrl Pts',(64.544120470977,31.7450013691112,0.));
#112265=CARTESIAN_POINT('Ctrl Pts',(64.5607141323521,31.7622207593634,0.));
#112266=CARTESIAN_POINT('Ctrl Pts',(64.5773204224429,31.7794870074583,0.));
#112267=CARTESIAN_POINT('Ctrl Pts',(64.5939392137235,31.7968000693218,0.));
#112268=CARTESIAN_POINT('Ctrl Pts',(64.6105703792312,31.8141599009684,0.));
#112269=CARTESIAN_POINT('Ctrl Pts',(64.6272137925627,31.8315664585026,0.));
#112270=CARTESIAN_POINT('Ctrl Pts',(64.6438693278714,31.8490196981248,0.));
#112271=CARTESIAN_POINT('Ctrl Pts',(64.6605368598629,31.8665195761311,0.));
#112272=CARTESIAN_POINT('Ctrl Pts',(64.6772162637907,31.8840660489107,0.));
#112273=CARTESIAN_POINT('Ctrl Pts',(64.6939074154498,31.9016590729374,0.));
#112274=CARTESIAN_POINT('Ctrl Pts',(64.7106101911732,31.9192986047706,0.));
#112275=CARTESIAN_POINT('Ctrl Pts',(64.7273244678297,31.9369846010616,0.));
#112276=CARTESIAN_POINT('Ctrl Pts',(64.7440501228202,31.9547170185534,0.));
#112277=CARTESIAN_POINT('Ctrl Pts',(64.7607870340735,31.9724958140789,0.));
#112278=CARTESIAN_POINT('Ctrl Pts',(64.77753508004,31.990320944552,0.));
#112279=CARTESIAN_POINT('Ctrl Pts',(64.7942941396881,32.0081923669677,0.));
#112280=CARTESIAN_POINT('Ctrl Pts',(64.8110640925021,32.0261100384092,0.));
#112281=CARTESIAN_POINT('Ctrl Pts',(64.8278448184786,32.0440739160477,0.));
#112282=CARTESIAN_POINT('Ctrl Pts',(64.8446361981234,32.0620839571408,0.));
#112283=CARTESIAN_POINT('Ctrl Pts',(64.861438112445,32.0801401190241,0.));
#112284=CARTESIAN_POINT('Ctrl Pts',(64.878250442952,32.0982423591108,0.));
#112285=CARTESIAN_POINT('Ctrl Pts',(64.8950730716493,32.1163906348979,0.));
#112286=CARTESIAN_POINT('Ctrl Pts',(64.9119058810362,32.1345849039671,0.));
#112287=CARTESIAN_POINT('Ctrl Pts',(64.9287487541018,32.1528251239832,0.));
#112288=CARTESIAN_POINT('Ctrl Pts',(64.9456015743203,32.171111252686,0.));
#112289=CARTESIAN_POINT('Ctrl Pts',(64.9624642256477,32.1894432478889,0.));
#112290=CARTESIAN_POINT('Ctrl Pts',(64.9793365925194,32.2078210674858,0.));
#112291=CARTESIAN_POINT('Ctrl Pts',(64.996218559847,32.2262446694516,0.));
#112292=CARTESIAN_POINT('Ctrl Pts',(65.0131100130155,32.244714011842,0.));
#112293=CARTESIAN_POINT('Ctrl Pts',(65.0300108378786,32.2632290527855,0.));
#112294=CARTESIAN_POINT('Ctrl Pts',(65.0469209207548,32.2817897504799,0.));
#112295=CARTESIAN_POINT('Ctrl Pts',(65.0638401484245,32.3003960632001,0.));
#112296=CARTESIAN_POINT('Ctrl Pts',(65.0807684081278,32.3190479492985,0.));
#112297=CARTESIAN_POINT('Ctrl Pts',(65.097705587561,32.3377453672052,0.));
#112298=CARTESIAN_POINT('Ctrl Pts',(65.1146515748723,32.3564882754213,0.));
#112299=CARTESIAN_POINT('Ctrl Pts',(65.1316062586586,32.3752766325135,0.));
#112300=CARTESIAN_POINT('Ctrl Pts',(65.1485695279628,32.3941103971218,0.));
#112301=CARTESIAN_POINT('Ctrl Pts',(65.165541272272,32.4129895279612,0.));
#112302=CARTESIAN_POINT('Ctrl Pts',(65.182521381514,32.4319139838212,0.));
#112303=CARTESIAN_POINT('Ctrl Pts',(65.1995097460545,32.4508837235613,0.));
#112304=CARTESIAN_POINT('Ctrl Pts',(65.2165062566936,32.4698987061037,0.));
#112305=CARTESIAN_POINT('Ctrl Pts',(65.2335108046625,32.4889588904397,0.));
#112306=CARTESIAN_POINT('Ctrl Pts',(65.2505232816215,32.508064235633,0.));
#112307=CARTESIAN_POINT('Ctrl Pts',(65.2675435796558,32.5272147008191,0.));
#112308=CARTESIAN_POINT('Ctrl Pts',(65.2845715912717,32.5464102452013,0.));
#112309=CARTESIAN_POINT('Ctrl Pts',(65.3016072093907,32.565650828042,0.));
#112310=CARTESIAN_POINT('Ctrl Pts',(65.3186503273498,32.5849364086679,0.));
#112311=CARTESIAN_POINT('Ctrl Pts',(65.3357008389004,32.6042669464752,0.));
#112312=CARTESIAN_POINT('Ctrl Pts',(65.3527586382082,32.6236424009302,0.));
#112313=CARTESIAN_POINT('Ctrl Pts',(65.3698236198511,32.6430627315673,0.));
#112314=CARTESIAN_POINT('Ctrl Pts',(65.3868956788178,32.6625278979807,0.));
#112315=CARTESIAN_POINT('Ctrl Pts',(65.4039747105033,32.6820378598263,0.));
#112316=CARTESIAN_POINT('Ctrl Pts',(65.4210606107029,32.7015925768261,0.));
#112317=CARTESIAN_POINT('Ctrl Pts',(65.4381532756062,32.7211920087682,0.));
#112318=CARTESIAN_POINT('Ctrl Pts',(65.4552526017907,32.7408361155038,0.));
#112319=CARTESIAN_POINT('Ctrl Pts',(65.4723584862129,32.7605248569382,0.));
#112320=CARTESIAN_POINT('Ctrl Pts',(65.4894708262071,32.7802581930294,0.));
#112321=CARTESIAN_POINT('Ctrl Pts',(65.5065895194938,32.8000360837981,0.));
#112322=CARTESIAN_POINT('Ctrl Pts',(65.5237144641864,32.8198584893319,0.));
#112323=CARTESIAN_POINT('Ctrl Pts',(65.5408455587963,32.8397253697865,0.));
#112324=CARTESIAN_POINT('Ctrl Pts',(65.5579827022412,32.8596366853826,0.));
#112325=CARTESIAN_POINT('Ctrl Pts',(65.575125793846,32.8795923964022,0.));
#112326=CARTESIAN_POINT('Ctrl Pts',(65.5922747333181,32.899592463189,0.));
#112327=CARTESIAN_POINT('Ctrl Pts',(65.6094294207267,32.9196368461457,0.));
#112328=CARTESIAN_POINT('Ctrl Pts',(65.6265897564782,32.9397255057273,0.));
#112329=CARTESIAN_POINT('Ctrl Pts',(65.6437556412956,32.9598584024318,0.));
#112330=CARTESIAN_POINT('Ctrl Pts',(65.6609269761902,32.9800354967847,0.));
#112331=CARTESIAN_POINT('Ctrl Pts',(65.6781036625041,33.0002567493581,0.));
#112332=CARTESIAN_POINT('Ctrl Pts',(65.6952856019542,33.0205221207877,0.));
#112333=CARTESIAN_POINT('Ctrl Pts',(65.7124726966805,33.0408315717874,0.));
#112334=CARTESIAN_POINT('Ctrl Pts',(65.729664849282,33.061185063158,0.));
#112335=CARTESIAN_POINT('Ctrl Pts',(65.7468619628808,33.0815825557976,0.));
#112336=CARTESIAN_POINT('Ctrl Pts',(65.7640639410653,33.102024010688,0.));
#112337=CARTESIAN_POINT('Ctrl Pts',(65.7812706877691,33.1225093888669,0.));
#112338=CARTESIAN_POINT('Ctrl Pts',(65.7984821071621,33.1430386513975,0.));
#112339=CARTESIAN_POINT('Ctrl Pts',(65.8156981035504,33.16361175934,0.));
#112340=CARTESIAN_POINT('Ctrl Pts',(65.8329185812379,33.1842286737053,0.));
#112341=CARTESIAN_POINT('Ctrl Pts',(65.8501434445174,33.2048893554496,0.));
#112342=CARTESIAN_POINT('Ctrl Pts',(65.8673725979591,33.2255937655656,0.));
#112343=CARTESIAN_POINT('Ctrl Pts',(65.8846059466382,33.2463418651498,0.));
#112344=CARTESIAN_POINT('Ctrl Pts',(65.901843396389,33.2671336154754,0.));
#112345=CARTESIAN_POINT('Ctrl Pts',(65.9190848540422,33.2879689780566,0.));
#112346=CARTESIAN_POINT('Ctrl Pts',(65.9363302276822,33.3088479147151,0.));
#112347=CARTESIAN_POINT('Ctrl Pts',(65.9535794260802,33.3297703874249,0.));
#112348=CARTESIAN_POINT('Ctrl Pts',(65.9708323581385,33.3507363581579,0.));
#112349=CARTESIAN_POINT('Ctrl Pts',(65.9880889322822,33.3717457887095,0.));
#112350=CARTESIAN_POINT('Ctrl Pts',(66.0053490559826,33.3927986405612,0.));
#112351=CARTESIAN_POINT('Ctrl Pts',(66.0226126349482,33.4138948746408,0.));
#112352=CARTESIAN_POINT('Ctrl Pts',(66.0398795737827,33.4350344515128,0.));
#112353=CARTESIAN_POINT('Ctrl Pts',(66.0571497774484,33.4562173318053,0.));
#112354=CARTESIAN_POINT('Ctrl Pts',(66.0744231525445,33.4774434765762,0.));
#112355=CARTESIAN_POINT('Ctrl Pts',(66.0916996085237,33.4987128476618,0.));
#112356=CARTESIAN_POINT('Ctrl Pts',(66.1089790592673,33.5200254081212,0.));
#112357=CARTESIAN_POINT('Ctrl Pts',(66.1262614234579,33.5413811223398,0.));
#112358=CARTESIAN_POINT('Ctrl Pts',(66.1410781873125,33.5597240685729,0.));
#112359=CARTESIAN_POINT('Ctrl Pts',(66.1524393973986,33.5738105077708,0.));
#112360=CARTESIAN_POINT('Ctrl Pts',(66.1603438177307,33.5836213513975,0.));
#112361=CARTESIAN_POINT('Ctrl Pts',(66.164790658241,33.589143987623,0.));
#112362=CARTESIAN_POINT('Ctrl Pts',(66.1657795405672,33.590372266496,0.));
#112363=CARTESIAN_POINT('',(63.0759831361898,30.3549065457811,12.));
#112364=CARTESIAN_POINT('',(63.0759831361898,30.3549065457811,0.));
#112365=CARTESIAN_POINT('Ctrl Pts',(66.1657795405673,33.5903722664962,12.));
#112366=CARTESIAN_POINT('Ctrl Pts',(66.1647906582411,33.5891439876231,12.));
#112367=CARTESIAN_POINT('Ctrl Pts',(66.1603438177307,33.5836213513976,12.));
#112368=CARTESIAN_POINT('Ctrl Pts',(66.1524393973986,33.5738105077708,12.));
#112369=CARTESIAN_POINT('Ctrl Pts',(66.1410781873125,33.5597240685729,12.));
#112370=CARTESIAN_POINT('Ctrl Pts',(66.1262614234579,33.5413811223398,12.));
#112371=CARTESIAN_POINT('Ctrl Pts',(66.1089790592673,33.5200254081212,12.));
#112372=CARTESIAN_POINT('Ctrl Pts',(66.0916996085237,33.4987128476618,12.));
#112373=CARTESIAN_POINT('Ctrl Pts',(66.0744231525445,33.4774434765762,12.));
#112374=CARTESIAN_POINT('Ctrl Pts',(66.0571497774484,33.4562173318053,12.));
#112375=CARTESIAN_POINT('Ctrl Pts',(66.0398795737827,33.4350344515128,12.));
#112376=CARTESIAN_POINT('Ctrl Pts',(66.0226126349482,33.4138948746408,12.));
#112377=CARTESIAN_POINT('Ctrl Pts',(66.0053490559826,33.3927986405612,12.));
#112378=CARTESIAN_POINT('Ctrl Pts',(65.9880889322822,33.3717457887095,12.));
#112379=CARTESIAN_POINT('Ctrl Pts',(65.9708323581385,33.3507363581579,12.));
#112380=CARTESIAN_POINT('Ctrl Pts',(65.9535794260802,33.3297703874249,12.));
#112381=CARTESIAN_POINT('Ctrl Pts',(65.9363302276822,33.3088479147151,12.));
#112382=CARTESIAN_POINT('Ctrl Pts',(65.9190848540422,33.2879689780566,12.));
#112383=CARTESIAN_POINT('Ctrl Pts',(65.901843396389,33.2671336154754,12.));
#112384=CARTESIAN_POINT('Ctrl Pts',(65.8846059466382,33.2463418651498,12.));
#112385=CARTESIAN_POINT('Ctrl Pts',(65.8673725979591,33.2255937655656,12.));
#112386=CARTESIAN_POINT('Ctrl Pts',(65.8501434445174,33.2048893554496,12.));
#112387=CARTESIAN_POINT('Ctrl Pts',(65.8329185812379,33.1842286737053,12.));
#112388=CARTESIAN_POINT('Ctrl Pts',(65.8156981035504,33.16361175934,12.));
#112389=CARTESIAN_POINT('Ctrl Pts',(65.7984821071621,33.1430386513975,12.));
#112390=CARTESIAN_POINT('Ctrl Pts',(65.7812706877691,33.1225093888669,12.));
#112391=CARTESIAN_POINT('Ctrl Pts',(65.7640639410653,33.102024010688,12.));
#112392=CARTESIAN_POINT('Ctrl Pts',(65.7468619628808,33.0815825557976,12.));
#112393=CARTESIAN_POINT('Ctrl Pts',(65.729664849282,33.061185063158,12.));
#112394=CARTESIAN_POINT('Ctrl Pts',(65.7124726966805,33.0408315717874,12.));
#112395=CARTESIAN_POINT('Ctrl Pts',(65.6952856019542,33.0205221207877,12.));
#112396=CARTESIAN_POINT('Ctrl Pts',(65.6781036625041,33.0002567493581,12.));
#112397=CARTESIAN_POINT('Ctrl Pts',(65.6609269761902,32.9800354967847,12.));
#112398=CARTESIAN_POINT('Ctrl Pts',(65.6437556412956,32.9598584024318,12.));
#112399=CARTESIAN_POINT('Ctrl Pts',(65.6265897564782,32.9397255057273,12.));
#112400=CARTESIAN_POINT('Ctrl Pts',(65.6094294207267,32.9196368461457,12.));
#112401=CARTESIAN_POINT('Ctrl Pts',(65.5922747333181,32.899592463189,12.));
#112402=CARTESIAN_POINT('Ctrl Pts',(65.575125793846,32.8795923964022,12.));
#112403=CARTESIAN_POINT('Ctrl Pts',(65.5579827022412,32.8596366853826,12.));
#112404=CARTESIAN_POINT('Ctrl Pts',(65.5408455587963,32.8397253697865,12.));
#112405=CARTESIAN_POINT('Ctrl Pts',(65.5237144641864,32.8198584893319,12.));
#112406=CARTESIAN_POINT('Ctrl Pts',(65.5065895194938,32.8000360837981,12.));
#112407=CARTESIAN_POINT('Ctrl Pts',(65.4894708262071,32.7802581930294,12.));
#112408=CARTESIAN_POINT('Ctrl Pts',(65.4723584862129,32.7605248569382,12.));
#112409=CARTESIAN_POINT('Ctrl Pts',(65.4552526017907,32.7408361155038,12.));
#112410=CARTESIAN_POINT('Ctrl Pts',(65.4381532756062,32.7211920087682,12.));
#112411=CARTESIAN_POINT('Ctrl Pts',(65.4210606107029,32.7015925768261,12.));
#112412=CARTESIAN_POINT('Ctrl Pts',(65.4039747105033,32.6820378598263,12.));
#112413=CARTESIAN_POINT('Ctrl Pts',(65.3868956788178,32.6625278979807,12.));
#112414=CARTESIAN_POINT('Ctrl Pts',(65.3698236198511,32.6430627315673,12.));
#112415=CARTESIAN_POINT('Ctrl Pts',(65.3527586382082,32.6236424009302,12.));
#112416=CARTESIAN_POINT('Ctrl Pts',(65.3357008389004,32.6042669464752,12.));
#112417=CARTESIAN_POINT('Ctrl Pts',(65.3186503273498,32.5849364086679,12.));
#112418=CARTESIAN_POINT('Ctrl Pts',(65.3016072093907,32.565650828042,12.));
#112419=CARTESIAN_POINT('Ctrl Pts',(65.2845715912717,32.5464102452013,12.));
#112420=CARTESIAN_POINT('Ctrl Pts',(65.2675435796558,32.5272147008191,12.));
#112421=CARTESIAN_POINT('Ctrl Pts',(65.2505232816215,32.508064235633,12.));
#112422=CARTESIAN_POINT('Ctrl Pts',(65.2335108046625,32.4889588904397,12.));
#112423=CARTESIAN_POINT('Ctrl Pts',(65.2165062566936,32.4698987061037,12.));
#112424=CARTESIAN_POINT('Ctrl Pts',(65.1995097460545,32.4508837235613,12.));
#112425=CARTESIAN_POINT('Ctrl Pts',(65.182521381514,32.4319139838212,12.));
#112426=CARTESIAN_POINT('Ctrl Pts',(65.165541272272,32.4129895279612,12.));
#112427=CARTESIAN_POINT('Ctrl Pts',(65.1485695279628,32.3941103971218,12.));
#112428=CARTESIAN_POINT('Ctrl Pts',(65.1316062586586,32.3752766325135,12.));
#112429=CARTESIAN_POINT('Ctrl Pts',(65.1146515748723,32.3564882754213,12.));
#112430=CARTESIAN_POINT('Ctrl Pts',(65.097705587561,32.3377453672052,12.));
#112431=CARTESIAN_POINT('Ctrl Pts',(65.0807684081278,32.3190479492985,12.));
#112432=CARTESIAN_POINT('Ctrl Pts',(65.0638401484245,32.3003960632001,12.));
#112433=CARTESIAN_POINT('Ctrl Pts',(65.0469209207548,32.2817897504799,12.));
#112434=CARTESIAN_POINT('Ctrl Pts',(65.0300108378786,32.2632290527855,12.));
#112435=CARTESIAN_POINT('Ctrl Pts',(65.0131100130155,32.244714011842,12.));
#112436=CARTESIAN_POINT('Ctrl Pts',(64.996218559847,32.2262446694516,12.));
#112437=CARTESIAN_POINT('Ctrl Pts',(64.9793365925194,32.2078210674858,12.));
#112438=CARTESIAN_POINT('Ctrl Pts',(64.9624642256477,32.1894432478889,12.));
#112439=CARTESIAN_POINT('Ctrl Pts',(64.9456015743203,32.171111252686,12.));
#112440=CARTESIAN_POINT('Ctrl Pts',(64.9287487541018,32.1528251239832,12.));
#112441=CARTESIAN_POINT('Ctrl Pts',(64.9119058810362,32.1345849039671,12.));
#112442=CARTESIAN_POINT('Ctrl Pts',(64.8950730716493,32.1163906348979,12.));
#112443=CARTESIAN_POINT('Ctrl Pts',(64.878250442952,32.0982423591108,12.));
#112444=CARTESIAN_POINT('Ctrl Pts',(64.861438112445,32.0801401190241,12.));
#112445=CARTESIAN_POINT('Ctrl Pts',(64.8446361981234,32.0620839571408,12.));
#112446=CARTESIAN_POINT('Ctrl Pts',(64.8278448184786,32.0440739160477,12.));
#112447=CARTESIAN_POINT('Ctrl Pts',(64.8110640925021,32.0261100384092,12.));
#112448=CARTESIAN_POINT('Ctrl Pts',(64.7942941396881,32.0081923669677,12.));
#112449=CARTESIAN_POINT('Ctrl Pts',(64.77753508004,31.990320944552,12.));
#112450=CARTESIAN_POINT('Ctrl Pts',(64.7607870340735,31.9724958140789,12.));
#112451=CARTESIAN_POINT('Ctrl Pts',(64.7440501228202,31.9547170185534,12.));
#112452=CARTESIAN_POINT('Ctrl Pts',(64.7273244678297,31.9369846010616,12.));
#112453=CARTESIAN_POINT('Ctrl Pts',(64.7106101911732,31.9192986047706,12.));
#112454=CARTESIAN_POINT('Ctrl Pts',(64.6939074154498,31.9016590729374,12.));
#112455=CARTESIAN_POINT('Ctrl Pts',(64.6772162637907,31.8840660489107,12.));
#112456=CARTESIAN_POINT('Ctrl Pts',(64.6605368598629,31.8665195761311,12.));
#112457=CARTESIAN_POINT('Ctrl Pts',(64.6438693278714,31.8490196981248,12.));
#112458=CARTESIAN_POINT('Ctrl Pts',(64.6272137925627,31.8315664585026,12.));
#112459=CARTESIAN_POINT('Ctrl Pts',(64.6105703792312,31.8141599009684,12.));
#112460=CARTESIAN_POINT('Ctrl Pts',(64.5939392137235,31.7968000693218,12.));
#112461=CARTESIAN_POINT('Ctrl Pts',(64.5773204224429,31.7794870074583,12.));
#112462=CARTESIAN_POINT('Ctrl Pts',(64.5607141323521,31.7622207593634,12.));
#112463=CARTESIAN_POINT('Ctrl Pts',(64.544120470977,31.7450013691112,12.));
#112464=CARTESIAN_POINT('Ctrl Pts',(64.5275395664124,31.7278288808731,12.));
#112465=CARTESIAN_POINT('Ctrl Pts',(64.510971547327,31.7107033389201,12.));
#112466=CARTESIAN_POINT('Ctrl Pts',(64.4944165429674,31.6936247876229,12.));
#112467=CARTESIAN_POINT('Ctrl Pts',(64.4778746831614,31.6765932714464,12.));
#112468=CARTESIAN_POINT('Ctrl Pts',(64.4613460983214,31.6596088349482,12.));
#112469=CARTESIAN_POINT('Ctrl Pts',(64.4448309194525,31.6426715227878,12.));
#112470=CARTESIAN_POINT('Ctrl Pts',(64.4283292781565,31.6257813797288,12.));
#112471=CARTESIAN_POINT('Ctrl Pts',(64.4118413066378,31.6089384506395,12.));
#112472=CARTESIAN_POINT('Ctrl Pts',(64.3953671377046,31.5921427804865,12.));
#112473=CARTESIAN_POINT('Ctrl Pts',(64.3789069047733,31.5753944143336,12.));
#112474=CARTESIAN_POINT('Ctrl Pts',(64.3624607418768,31.5586933973515,12.));
#112475=CARTESIAN_POINT('Ctrl Pts',(64.3460287836687,31.5420397748191,12.));
#112476=CARTESIAN_POINT('Ctrl Pts',(64.3296111654283,31.5254335921245,12.));
#112477=CARTESIAN_POINT('Ctrl Pts',(64.3132080230637,31.5088748947582,12.));
#112478=CARTESIAN_POINT('Ctrl Pts',(64.2968194931158,31.4923637283132,12.));
#112479=CARTESIAN_POINT('Ctrl Pts',(64.2804457127671,31.4759001384941,12.));
#112480=CARTESIAN_POINT('Ctrl Pts',(64.2640868198473,31.4594841711195,12.));
#112481=CARTESIAN_POINT('Ctrl Pts',(64.2477429528393,31.4431158721222,12.));
#112482=CARTESIAN_POINT('Ctrl Pts',(64.231414250881,31.4267952875423,12.));
#112483=CARTESIAN_POINT('Ctrl Pts',(64.2151008537697,31.410522463528,12.));
#112484=CARTESIAN_POINT('Ctrl Pts',(64.1988029019707,31.3942974463446,12.));
#112485=CARTESIAN_POINT('Ctrl Pts',(64.1825205366224,31.3781202823754,12.));
#112486=CARTESIAN_POINT('Ctrl Pts',(64.166253899542,31.3619910181228,12.));
#112487=CARTESIAN_POINT('Ctrl Pts',(64.1500031332282,31.3459097002006,12.));
#112488=CARTESIAN_POINT('Ctrl Pts',(64.133768380869,31.3298763753377,12.));
#112489=CARTESIAN_POINT('Ctrl Pts',(64.117549786349,31.3138910903859,12.));
#112490=CARTESIAN_POINT('Ctrl Pts',(64.1013474942556,31.2979538923214,12.));
#112491=CARTESIAN_POINT('Ctrl Pts',(64.0851616498852,31.2820648282447,12.));
#112492=CARTESIAN_POINT('Ctrl Pts',(64.0689923992461,31.2662239453728,12.));
#112493=CARTESIAN_POINT('Ctrl Pts',(64.0528398890657,31.2504312910451,12.));
#112494=CARTESIAN_POINT('Ctrl Pts',(64.0367042667984,31.2346869127297,12.));
#112495=CARTESIAN_POINT('Ctrl Pts',(64.02058568063,31.2189908580245,12.));
#112496=CARTESIAN_POINT('Ctrl Pts',(64.0044842794831,31.2033431746558,12.));
#112497=CARTESIAN_POINT('Ctrl Pts',(63.9884002130211,31.1877439104717,12.));
#112498=CARTESIAN_POINT('Ctrl Pts',(63.9723336316551,31.1721931134487,12.));
#112499=CARTESIAN_POINT('Ctrl Pts',(63.9562846865567,31.1566908316992,12.));
#112500=CARTESIAN_POINT('Ctrl Pts',(63.940253529665,31.1412371134727,12.));
#112501=CARTESIAN_POINT('Ctrl Pts',(63.9242403136955,31.1258320071545,12.));
#112502=CARTESIAN_POINT('Ctrl Pts',(63.9082451921448,31.1104755612607,12.));
#112503=CARTESIAN_POINT('Ctrl Pts',(63.8922683192964,31.0951678244455,12.));
#112504=CARTESIAN_POINT('Ctrl Pts',(63.8763098502237,31.0799088455041,12.));
#112505=CARTESIAN_POINT('Ctrl Pts',(63.8603699407922,31.0646986733723,12.));
#112506=CARTESIAN_POINT('Ctrl Pts',(63.8444487476611,31.0495373571215,12.));
#112507=CARTESIAN_POINT('Ctrl Pts',(63.8285464282846,31.0344249459538,12.));
#112508=CARTESIAN_POINT('Ctrl Pts',(63.8126631409364,31.0193614892171,12.));
#112509=CARTESIAN_POINT('Ctrl Pts',(63.796799044728,31.0043470364108,12.));
#112510=CARTESIAN_POINT('Ctrl Pts',(63.7809542996264,30.989381637191,12.));
#112511=CARTESIAN_POINT('Ctrl Pts',(63.7651290664733,30.9744653413689,12.));
#112512=CARTESIAN_POINT('Ctrl Pts',(63.749323506987,30.9595981989104,12.));
#112513=CARTESIAN_POINT('Ctrl Pts',(63.7335377837441,30.9447802599355,12.));
#112514=CARTESIAN_POINT('Ctrl Pts',(63.7177720601609,30.9300115747116,12.));
#112515=CARTESIAN_POINT('Ctrl Pts',(63.7020265004792,30.9152921936465,12.));
#112516=CARTESIAN_POINT('Ctrl Pts',(63.6863012697328,30.900622167269,12.));
#112517=CARTESIAN_POINT('Ctrl Pts',(63.6705965337971,30.8860015462475,12.));
#112518=CARTESIAN_POINT('Ctrl Pts',(63.6549124594666,30.8714303814194,12.));
#112519=CARTESIAN_POINT('Ctrl Pts',(63.6392492145233,30.8569087238131,12.));
#112520=CARTESIAN_POINT('Ctrl Pts',(63.6236069678055,30.8424366246672,12.));
#112521=CARTESIAN_POINT('Ctrl Pts',(63.6079858892771,30.8280141354459,12.));
#112522=CARTESIAN_POINT('Ctrl Pts',(63.5923861498987,30.813641307801,12.));
#112523=CARTESIAN_POINT('Ctrl Pts',(63.5768079214881,30.7993181935271,12.));
#112524=CARTESIAN_POINT('Ctrl Pts',(63.5612513766,30.7850448445205,12.));
#112525=CARTESIAN_POINT('Ctrl Pts',(63.5457166883537,30.7708213127159,12.));
#112526=CARTESIAN_POINT('Ctrl Pts',(63.5302040304142,30.7566476500757,12.));
#112527=CARTESIAN_POINT('Ctrl Pts',(63.5147135773894,30.7425239087281,12.));
#112528=CARTESIAN_POINT('Ctrl Pts',(63.4992455051795,30.7284501410822,12.));
#112529=CARTESIAN_POINT('Ctrl Pts',(63.4837999912771,30.7144263999265,12.));
#112530=CARTESIAN_POINT('Ctrl Pts',(63.4683772152529,30.7004527385821,12.));
#112531=CARTESIAN_POINT('Ctrl Pts',(63.4529773584249,30.6865292107929,12.));
#112532=CARTESIAN_POINT('Ctrl Pts',(63.4376006029604,30.6726558704315,12.));
#112533=CARTESIAN_POINT('Ctrl Pts',(63.4222471311239,30.6588327712484,12.));
#112534=CARTESIAN_POINT('Ctrl Pts',(63.4069171245066,30.6450599666121,12.));
#112535=CARTESIAN_POINT('Ctrl Pts',(63.3916107631376,30.6313375092062,12.));
#112536=CARTESIAN_POINT('Ctrl Pts',(63.3763282271796,30.6176654515967,12.));
#112537=CARTESIAN_POINT('Ctrl Pts',(63.3610696989577,30.6040438469078,12.));
#112538=CARTESIAN_POINT('Ctrl Pts',(63.3458353646154,30.5904727493712,12.));
#112539=CARTESIAN_POINT('Ctrl Pts',(63.3306254165126,30.5769522151164,12.));
#112540=CARTESIAN_POINT('Ctrl Pts',(63.3154400534397,30.563482302238,12.));
#112541=CARTESIAN_POINT('Ctrl Pts',(63.3002794756086,30.5500630691359,12.));
#112542=CARTESIAN_POINT('Ctrl Pts',(63.2851438802473,30.5366945730508,12.));
#112543=CARTESIAN_POINT('Ctrl Pts',(63.2700334577639,30.5233768687865,12.));
#112544=CARTESIAN_POINT('Ctrl Pts',(63.2549483856215,30.5101100066659,12.));
#112545=CARTESIAN_POINT('Ctrl Pts',(63.2398888342545,30.4968940344998,12.));
#112546=CARTESIAN_POINT('Ctrl Pts',(63.2248549788221,30.4837290014989,12.));
#112547=CARTESIAN_POINT('Ctrl Pts',(63.2098470086636,30.470614961416,12.));
#112548=CARTESIAN_POINT('Ctrl Pts',(63.1948651386942,30.4575519763337,12.));
#112549=CARTESIAN_POINT('Ctrl Pts',(63.179909617189,30.4445401192381,12.));
#112550=CARTESIAN_POINT('Ctrl Pts',(63.164980701691,30.4315794659731,12.));
#112551=CARTESIAN_POINT('Ctrl Pts',(63.1500786361459,30.418670087563,12.));
#112552=CARTESIAN_POINT('Ctrl Pts',(63.135203629844,30.4058120432229,12.));
#112553=CARTESIAN_POINT('Ctrl Pts',(63.1203558300657,30.3930053710484,12.));
#112554=CARTESIAN_POINT('Ctrl Pts',(63.105535320226,30.3802500880403,12.));
#112555=CARTESIAN_POINT('Ctrl Pts',(63.0937007763471,30.3700869762507,12.));
#112556=CARTESIAN_POINT('Ctrl Pts',(63.0848371718048,30.3624877680651,12.));
#112557=CARTESIAN_POINT('Ctrl Pts',(63.078933570069,30.357431906933,12.));
#112558=CARTESIAN_POINT('Ctrl Pts',(63.0759831361898,30.3549065457811,12.));
#112559=CARTESIAN_POINT('Ctrl Pts',(65.4667541478388,34.933187552314,0.));
#112560=CARTESIAN_POINT('Ctrl Pts',(65.4667541478388,34.933187552314,4.));
#112561=CARTESIAN_POINT('Ctrl Pts',(65.4667541478387,34.933187552314,8.));
#112562=CARTESIAN_POINT('Ctrl Pts',(65.4667541478387,34.933187552314,12.));
#112563=CARTESIAN_POINT('Ctrl Pts',(65.5763902570752,34.940541458921,0.));
#112564=CARTESIAN_POINT('Ctrl Pts',(65.5763902570752,34.940541458921,4.));
#112565=CARTESIAN_POINT('Ctrl Pts',(65.576390257075,34.940541458921,8.));
#112566=CARTESIAN_POINT('Ctrl Pts',(65.576390257075,34.940541458921,12.));
#112567=CARTESIAN_POINT('Ctrl Pts',(65.772041268059,34.8876896346299,0.));
#112568=CARTESIAN_POINT('Ctrl Pts',(65.772041268059,34.8876896346299,4.));
#112569=CARTESIAN_POINT('Ctrl Pts',(65.7720412680589,34.8876896346299,7.99999999999999));
#112570=CARTESIAN_POINT('Ctrl Pts',(65.7720412680589,34.8876896346299,12.));
#112571=CARTESIAN_POINT('Ctrl Pts',(65.9044372006544,34.7399186668304,0.));
#112572=CARTESIAN_POINT('Ctrl Pts',(65.9044372006544,34.7399186668304,4.));
#112573=CARTESIAN_POINT('Ctrl Pts',(65.9044372006543,34.7399186668304,8.00000000000001));
#112574=CARTESIAN_POINT('Ctrl Pts',(65.9044372006543,34.7399186668304,12.));
#112575=CARTESIAN_POINT('Ctrl Pts',(65.9427857825585,34.6669728017261,0.));
#112576=CARTESIAN_POINT('Ctrl Pts',(65.9427857825585,34.6669728017261,4.));
#112577=CARTESIAN_POINT('Ctrl Pts',(65.9427857825584,34.6669728017261,8.));
#112578=CARTESIAN_POINT('Ctrl Pts',(65.9427857825584,34.6669728017261,12.));
#112579=CARTESIAN_POINT('',(65.4667541478388,34.933187552314,0.));
#112580=CARTESIAN_POINT('',(65.9427857825584,34.6669728017261,0.));
#112581=CARTESIAN_POINT('Ctrl Pts',(65.4667541478388,34.933187552314,3.76195697576961E-35));
#112582=CARTESIAN_POINT('Ctrl Pts',(65.5763902570752,34.940541458921,3.76195697576961E-35));
#112583=CARTESIAN_POINT('Ctrl Pts',(65.6881908347802,34.9103404164689,3.76195697576962E-35));
#112584=CARTESIAN_POINT('Ctrl Pts',(65.7793366930115,34.8491453679733,3.76195697576961E-35));
#112585=CARTESIAN_POINT('Ctrl Pts',(65.8476960866849,34.8032490816016,3.76195697576961E-35));
#112586=CARTESIAN_POINT('Ctrl Pts',(65.9044372006544,34.7399186668304,3.76195697576961E-35));
#112587=CARTESIAN_POINT('Ctrl Pts',(65.9427857825585,34.6669728017261,3.76195697576961E-35));
#112588=CARTESIAN_POINT('',(65.9427857825584,34.6669728017261,12.));
#112589=CARTESIAN_POINT('Ctrl Pts',(65.9427857825585,34.6669728017261,0.));
#112590=CARTESIAN_POINT('Ctrl Pts',(65.9427857825585,34.6669728017261,4.));
#112591=CARTESIAN_POINT('Ctrl Pts',(65.9427857825584,34.6669728017261,8.));
#112592=CARTESIAN_POINT('Ctrl Pts',(65.9427857825584,34.6669728017261,12.));
#112593=CARTESIAN_POINT('',(65.4667541478387,34.933187552314,12.));
#112594=CARTESIAN_POINT('Ctrl Pts',(65.9427857825584,34.6669728017261,12.));
#112595=CARTESIAN_POINT('Ctrl Pts',(65.9044372006543,34.7399186668304,12.));
#112596=CARTESIAN_POINT('Ctrl Pts',(65.8476960866848,34.8032490816016,12.));
#112597=CARTESIAN_POINT('Ctrl Pts',(65.7793366930113,34.8491453679733,12.));
#112598=CARTESIAN_POINT('Ctrl Pts',(65.6881908347801,34.9103404164689,12.));
#112599=CARTESIAN_POINT('Ctrl Pts',(65.576390257075,34.940541458921,12.));
#112600=CARTESIAN_POINT('Ctrl Pts',(65.4667541478387,34.933187552314,12.));
#112601=CARTESIAN_POINT('Ctrl Pts',(65.4667541478387,34.933187552314,12.));
#112602=CARTESIAN_POINT('Ctrl Pts',(65.4667541478387,34.933187552314,8.));
#112603=CARTESIAN_POINT('Ctrl Pts',(65.4667541478388,34.933187552314,4.));
#112604=CARTESIAN_POINT('Ctrl Pts',(65.4667541478388,34.933187552314,0.));
#112605=CARTESIAN_POINT('Origin',(3.32444647725448E-10,1.73171632017259E-10,
0.));
#112606=CARTESIAN_POINT('Origin',(3.32444647725448E-10,1.73171632017259E-10,
12.));
#112607=CARTESIAN_POINT('Origin',(3.32444647725448E-10,1.73171632017259E-10,
0.));
#112608=CARTESIAN_POINT('Ctrl Pts',(68.9436475237602,28.2316040302268,-5.55111512312578E-16));
#112609=CARTESIAN_POINT('Ctrl Pts',(68.9436475237602,28.2316040302268,4.));
#112610=CARTESIAN_POINT('Ctrl Pts',(68.9436475237602,28.2316040302269,8.));
#112611=CARTESIAN_POINT('Ctrl Pts',(68.9436475237602,28.2316040302269,12.));
#112612=CARTESIAN_POINT('Ctrl Pts',(68.9852872321828,28.1299168084378,-5.55111512312578E-16));
#112613=CARTESIAN_POINT('Ctrl Pts',(68.9852872321828,28.1299168084378,4.));
#112614=CARTESIAN_POINT('Ctrl Pts',(68.9852872321828,28.1299168084378,8.00000000000001));
#112615=CARTESIAN_POINT('Ctrl Pts',(68.9852872321828,28.1299168084378,12.));
#112616=CARTESIAN_POINT('Ctrl Pts',(68.9970049015576,27.9275918177432,-5.55111512312578E-16));
#112617=CARTESIAN_POINT('Ctrl Pts',(68.9970049015576,27.9275918177432,4.));
#112618=CARTESIAN_POINT('Ctrl Pts',(68.9970049015576,27.9275918177433,7.99999999999999));
#112619=CARTESIAN_POINT('Ctrl Pts',(68.9970049015576,27.9275918177433,12.));
#112620=CARTESIAN_POINT('Ctrl Pts',(68.8986722313991,27.7552674476222,-5.55111512312578E-16));
#112621=CARTESIAN_POINT('Ctrl Pts',(68.8986722313991,27.7552674476222,4.));
#112622=CARTESIAN_POINT('Ctrl Pts',(68.8986722313991,27.7552674476223,8.00000000000001));
#112623=CARTESIAN_POINT('Ctrl Pts',(68.8986722313991,27.7552674476223,12.));
#112624=CARTESIAN_POINT('Ctrl Pts',(68.8415926174774,27.6958230984758,-5.55111512312578E-16));
#112625=CARTESIAN_POINT('Ctrl Pts',(68.8415926174774,27.6958230984758,4.));
#112626=CARTESIAN_POINT('Ctrl Pts',(68.8415926174774,27.6958230984758,8.));
#112627=CARTESIAN_POINT('Ctrl Pts',(68.8415926174774,27.6958230984758,12.));
#112628=CARTESIAN_POINT('',(68.9436475237602,28.2316040302268,0.));
#112629=CARTESIAN_POINT('',(68.8415926174774,27.6958230984757,2.77555756156289E-16));
#112630=CARTESIAN_POINT('Ctrl Pts',(68.9436475237602,28.2316040302268,-5.55111512312578E-16));
#112631=CARTESIAN_POINT('Ctrl Pts',(68.9852872321828,28.1299168084378,-5.55111512312578E-16));
#112632=CARTESIAN_POINT('Ctrl Pts',(68.9919830432541,28.0143025280409,-5.55111512312578E-16));
#112633=CARTESIAN_POINT('Ctrl Pts',(68.9627440495799,27.9084843686476,-5.55111512312578E-16));
#112634=CARTESIAN_POINT('Ctrl Pts',(68.9408148043242,27.8291207491026,-5.55111512312578E-16));
#112635=CARTESIAN_POINT('Ctrl Pts',(68.8986722313991,27.7552674476222,-5.55111512312578E-16));
#112636=CARTESIAN_POINT('Ctrl Pts',(68.8415926174774,27.6958230984758,-5.55111512312578E-16));
#112637=CARTESIAN_POINT('',(68.8415926174774,27.6958230984758,12.));
#112638=CARTESIAN_POINT('Ctrl Pts',(68.8415926174774,27.6958230984758,-5.55111512312578E-16));
#112639=CARTESIAN_POINT('Ctrl Pts',(68.8415926174774,27.6958230984758,4.));
#112640=CARTESIAN_POINT('Ctrl Pts',(68.8415926174774,27.6958230984758,8.));
#112641=CARTESIAN_POINT('Ctrl Pts',(68.8415926174774,27.6958230984758,12.));
#112642=CARTESIAN_POINT('',(68.9436475237602,28.2316040302269,12.));
#112643=CARTESIAN_POINT('Ctrl Pts',(68.8415926174774,27.6958230984758,12.));
#112644=CARTESIAN_POINT('Ctrl Pts',(68.8986722313991,27.7552674476223,12.));
#112645=CARTESIAN_POINT('Ctrl Pts',(68.9408148043242,27.8291207491027,12.));
#112646=CARTESIAN_POINT('Ctrl Pts',(68.9627440495799,27.9084843686477,12.));
#112647=CARTESIAN_POINT('Ctrl Pts',(68.9919830432541,28.0143025280409,12.));
#112648=CARTESIAN_POINT('Ctrl Pts',(68.9852872321828,28.1299168084378,12.));
#112649=CARTESIAN_POINT('Ctrl Pts',(68.9436475237602,28.2316040302269,12.));
#112650=CARTESIAN_POINT('Ctrl Pts',(68.9436475237602,28.2316040302269,12.));
#112651=CARTESIAN_POINT('Ctrl Pts',(68.9436475237602,28.2316040302269,8.));
#112652=CARTESIAN_POINT('Ctrl Pts',(68.9436475237602,28.2316040302268,4.));
#112653=CARTESIAN_POINT('Ctrl Pts',(68.9436475237602,28.2316040302268,-5.55111512312578E-16));
#112654=CARTESIAN_POINT('Ctrl Pts',(65.4815644032299,24.7419628022042,0.));
#112655=CARTESIAN_POINT('Ctrl Pts',(65.4815644032299,24.7419628022042,12.));
#112656=CARTESIAN_POINT('Ctrl Pts',(65.4847237095443,24.7442214063382,0.));
#112657=CARTESIAN_POINT('Ctrl Pts',(65.4847237095443,24.7442214063382,12.));
#112658=CARTESIAN_POINT('Ctrl Pts',(65.4910454936254,24.7487434955982,0.));
#112659=CARTESIAN_POINT('Ctrl Pts',(65.4910454936254,24.7487434955982,12.));
#112660=CARTESIAN_POINT('Ctrl Pts',(65.5005376841101,24.7555412724651,0.));
#112661=CARTESIAN_POINT('Ctrl Pts',(65.5005376841101,24.7555412724651,12.));
#112662=CARTESIAN_POINT('Ctrl Pts',(65.5132129675333,24.7646342620841,0.));
#112663=CARTESIAN_POINT('Ctrl Pts',(65.5132129675333,24.7646342620841,12.));
#112664=CARTESIAN_POINT('Ctrl Pts',(65.5290887770232,24.7760493148465,0.));
#112665=CARTESIAN_POINT('Ctrl Pts',(65.5290887770232,24.7760493148465,12.));
#112666=CARTESIAN_POINT('Ctrl Pts',(65.5449962514661,24.7875131827491,0.));
#112667=CARTESIAN_POINT('Ctrl Pts',(65.5449962514661,24.7875131827491,12.));
#112668=CARTESIAN_POINT('Ctrl Pts',(65.5609353062829,24.799025856126,0.));
#112669=CARTESIAN_POINT('Ctrl Pts',(65.5609353062829,24.799025856126,12.));
#112670=CARTESIAN_POINT('Ctrl Pts',(65.5769057914333,24.8105873098626,0.));
#112671=CARTESIAN_POINT('Ctrl Pts',(65.5769057914333,24.8105873098626,12.));
#112672=CARTESIAN_POINT('Ctrl Pts',(65.5929074932624,24.8221975032104,0.));
#112673=CARTESIAN_POINT('Ctrl Pts',(65.5929074932624,24.8221975032104,12.));
#112674=CARTESIAN_POINT('Ctrl Pts',(65.6089401625628,24.8338563866764,0.));
#112675=CARTESIAN_POINT('Ctrl Pts',(65.6089401625628,24.8338563866764,12.));
#112676=CARTESIAN_POINT('Ctrl Pts',(65.6250035361612,24.8455639071517,0.));
#112677=CARTESIAN_POINT('Ctrl Pts',(65.6250035361612,24.8455639071517,12.));
#112678=CARTESIAN_POINT('Ctrl Pts',(65.6410973603661,24.8573200135666,0.));
#112679=CARTESIAN_POINT('Ctrl Pts',(65.6410973603661,24.8573200135666,12.));
#112680=CARTESIAN_POINT('Ctrl Pts',(65.6572214156692,24.8691246628057,0.));
#112681=CARTESIAN_POINT('Ctrl Pts',(65.6572214156692,24.8691246628057,12.));
#112682=CARTESIAN_POINT('Ctrl Pts',(65.6733755087669,24.8809778178229,0.));
#112683=CARTESIAN_POINT('Ctrl Pts',(65.6733755087669,24.8809778178229,12.));
#112684=CARTESIAN_POINT('Ctrl Pts',(65.6895594608775,24.8928794448607,0.));
#112685=CARTESIAN_POINT('Ctrl Pts',(65.6895594608775,24.8928794448607,12.));
#112686=CARTESIAN_POINT('Ctrl Pts',(65.7057730980483,24.9048295111448,0.));
#112687=CARTESIAN_POINT('Ctrl Pts',(65.7057730980483,24.9048295111448,12.));
#112688=CARTESIAN_POINT('Ctrl Pts',(65.7220162391053,24.9168279820106,0.));
#112689=CARTESIAN_POINT('Ctrl Pts',(65.7220162391053,24.9168279820106,12.));
#112690=CARTESIAN_POINT('Ctrl Pts',(65.7382886895888,24.928874819458,0.));
#112691=CARTESIAN_POINT('Ctrl Pts',(65.7382886895888,24.928874819458,12.));
#112692=CARTESIAN_POINT('Ctrl Pts',(65.7545902480323,24.9409699836537,0.));
#112693=CARTESIAN_POINT('Ctrl Pts',(65.7545902480323,24.9409699836537,12.));
#112694=CARTESIAN_POINT('Ctrl Pts',(65.7709207098959,24.9531134338696,0.));
#112695=CARTESIAN_POINT('Ctrl Pts',(65.7709207098959,24.9531134338696,12.));
#112696=CARTESIAN_POINT('Ctrl Pts',(65.7872798720823,24.9653051295581,0.));
#112697=CARTESIAN_POINT('Ctrl Pts',(65.7872798720823,24.9653051295581,12.));
#112698=CARTESIAN_POINT('Ctrl Pts',(65.8036675380718,24.9775450315683,0.));
#112699=CARTESIAN_POINT('Ctrl Pts',(65.8036675380718,24.9775450315683,12.));
#112700=CARTESIAN_POINT('Ctrl Pts',(65.8200835177024,24.9898331020983,0.));
#112701=CARTESIAN_POINT('Ctrl Pts',(65.8200835177024,24.9898331020983,12.));
#112702=CARTESIAN_POINT('Ctrl Pts',(65.8365276247128,25.002169304117,0.));
#112703=CARTESIAN_POINT('Ctrl Pts',(65.8365276247128,25.002169304117,12.));
#112704=CARTESIAN_POINT('Ctrl Pts',(65.8529996750445,25.0145536009604,0.));
#112705=CARTESIAN_POINT('Ctrl Pts',(65.8529996750445,25.0145536009604,12.));
#112706=CARTESIAN_POINT('Ctrl Pts',(65.8694994847616,25.0269859558363,0.));
#112707=CARTESIAN_POINT('Ctrl Pts',(65.8694994847616,25.0269859558363,12.));
#112708=CARTESIAN_POINT('Ctrl Pts',(65.8860268683128,25.0394663314055,0.));
#112709=CARTESIAN_POINT('Ctrl Pts',(65.8860268683128,25.0394663314055,12.));
#112710=CARTESIAN_POINT('Ctrl Pts',(65.9025816394424,25.0519946900078,0.));
#112711=CARTESIAN_POINT('Ctrl Pts',(65.9025816394424,25.0519946900078,12.));
#112712=CARTESIAN_POINT('Ctrl Pts',(65.919163611981,25.0645709938524,0.));
#112713=CARTESIAN_POINT('Ctrl Pts',(65.919163611981,25.0645709938524,12.));
#112714=CARTESIAN_POINT('Ctrl Pts',(65.9357726006163,25.0771952052028,0.));
#112715=CARTESIAN_POINT('Ctrl Pts',(65.9357726006163,25.0771952052028,12.));
#112716=CARTESIAN_POINT('Ctrl Pts',(65.9524084218139,25.0898672865915,0.));
#112717=CARTESIAN_POINT('Ctrl Pts',(65.9524084218139,25.0898672865915,12.));
#112718=CARTESIAN_POINT('Ctrl Pts',(65.9690708941558,25.1025872009004,0.));
#112719=CARTESIAN_POINT('Ctrl Pts',(65.9690708941558,25.1025872009004,12.));
#112720=CARTESIAN_POINT('Ctrl Pts',(65.9857598378433,25.1153549112503,0.));
#112721=CARTESIAN_POINT('Ctrl Pts',(65.9857598378433,25.1153549112503,12.));
#112722=CARTESIAN_POINT('Ctrl Pts',(66.0024750743897,25.1281703809297,0.));
#112723=CARTESIAN_POINT('Ctrl Pts',(66.0024750743897,25.1281703809297,12.));
#112724=CARTESIAN_POINT('Ctrl Pts',(66.0192164262621,25.1410335733099,0.));
#112725=CARTESIAN_POINT('Ctrl Pts',(66.0192164262621,25.1410335733099,12.));
#112726=CARTESIAN_POINT('Ctrl Pts',(66.0359837164734,25.1539444517419,0.));
#112727=CARTESIAN_POINT('Ctrl Pts',(66.0359837164734,25.1539444517419,12.));
#112728=CARTESIAN_POINT('Ctrl Pts',(66.0527767686025,25.1669029795661,0.));
#112729=CARTESIAN_POINT('Ctrl Pts',(66.0527767686025,25.1669029795661,12.));
#112730=CARTESIAN_POINT('Ctrl Pts',(66.0695954069713,25.1799091201599,0.));
#112731=CARTESIAN_POINT('Ctrl Pts',(66.0695954069713,25.1799091201599,12.));
#112732=CARTESIAN_POINT('Ctrl Pts',(66.086439456768,25.1929628369685,0.));
#112733=CARTESIAN_POINT('Ctrl Pts',(66.086439456768,25.1929628369685,12.));
#112734=CARTESIAN_POINT('Ctrl Pts',(66.10330874419,25.2060640935365,0.));
#112735=CARTESIAN_POINT('Ctrl Pts',(66.10330874419,25.2060640935365,12.));
#112736=CARTESIAN_POINT('Ctrl Pts',(66.1202030965758,25.2192128535357,0.));
#112737=CARTESIAN_POINT('Ctrl Pts',(66.1202030965758,25.2192128535357,12.));
#112738=CARTESIAN_POINT('Ctrl Pts',(66.1371223423345,25.232409080755,0.));
#112739=CARTESIAN_POINT('Ctrl Pts',(66.1371223423345,25.232409080755,12.));
#112740=CARTESIAN_POINT('Ctrl Pts',(66.1540663108754,25.2456527390875,0.));
#112741=CARTESIAN_POINT('Ctrl Pts',(66.1540663108754,25.2456527390875,12.));
#112742=CARTESIAN_POINT('Ctrl Pts',(66.1710348325384,25.2589437925147,0.));
#112743=CARTESIAN_POINT('Ctrl Pts',(66.1710348325384,25.2589437925147,12.));
#112744=CARTESIAN_POINT('Ctrl Pts',(66.1880277385136,25.2722822050837,0.));
#112745=CARTESIAN_POINT('Ctrl Pts',(66.1880277385136,25.2722822050837,12.));
#112746=CARTESIAN_POINT('Ctrl Pts',(66.2050448607911,25.285667940893,0.));
#112747=CARTESIAN_POINT('Ctrl Pts',(66.2050448607911,25.285667940893,12.));
#112748=CARTESIAN_POINT('Ctrl Pts',(66.2220860321952,25.2991009641094,0.));
#112749=CARTESIAN_POINT('Ctrl Pts',(66.2220860321952,25.2991009641094,12.));
#112750=CARTESIAN_POINT('Ctrl Pts',(66.2391510863998,25.312581238973,0.));
#112751=CARTESIAN_POINT('Ctrl Pts',(66.2391510863998,25.312581238973,12.));
#112752=CARTESIAN_POINT('Ctrl Pts',(66.2562398579471,25.3261087298026,0.));
#112753=CARTESIAN_POINT('Ctrl Pts',(66.2562398579471,25.3261087298026,12.));
#112754=CARTESIAN_POINT('Ctrl Pts',(66.2733521822662,25.3396834009949,0.));
#112755=CARTESIAN_POINT('Ctrl Pts',(66.2733521822662,25.3396834009949,12.));
#112756=CARTESIAN_POINT('Ctrl Pts',(66.290487895671,25.3533052170249,0.));
#112757=CARTESIAN_POINT('Ctrl Pts',(66.290487895671,25.3533052170249,12.));
#112758=CARTESIAN_POINT('Ctrl Pts',(66.3076468353412,25.3669741424488,0.));
#112759=CARTESIAN_POINT('Ctrl Pts',(66.3076468353412,25.3669741424488,12.));
#112760=CARTESIAN_POINT('Ctrl Pts',(66.3248288393046,25.3806901419012,0.));
#112761=CARTESIAN_POINT('Ctrl Pts',(66.3248288393046,25.3806901419012,12.));
#112762=CARTESIAN_POINT('Ctrl Pts',(66.3420337464178,25.3944531800901,0.));
#112763=CARTESIAN_POINT('Ctrl Pts',(66.3420337464178,25.3944531800901,12.));
#112764=CARTESIAN_POINT('Ctrl Pts',(66.359261396341,25.4082632217847,0.));
#112765=CARTESIAN_POINT('Ctrl Pts',(66.359261396341,25.4082632217847,12.));
#112766=CARTESIAN_POINT('Ctrl Pts',(66.3765116295364,25.4221202318199,0.));
#112767=CARTESIAN_POINT('Ctrl Pts',(66.3765116295364,25.4221202318199,12.));
#112768=CARTESIAN_POINT('Ctrl Pts',(66.3937842872685,25.4360241751018,0.));
#112769=CARTESIAN_POINT('Ctrl Pts',(66.3937842872685,25.4360241751018,12.));
#112770=CARTESIAN_POINT('Ctrl Pts',(66.4110792116,25.4499750166079,0.));
#112771=CARTESIAN_POINT('Ctrl Pts',(66.4110792116,25.4499750166079,12.));
#112772=CARTESIAN_POINT('Ctrl Pts',(66.4283962453899,25.4639727213849,0.));
#112773=CARTESIAN_POINT('Ctrl Pts',(66.4283962453899,25.4639727213849,12.));
#112774=CARTESIAN_POINT('Ctrl Pts',(66.4457352322871,25.4780172545417,0.));
#112775=CARTESIAN_POINT('Ctrl Pts',(66.4457352322871,25.4780172545417,12.));
#112776=CARTESIAN_POINT('Ctrl Pts',(66.4630960167252,25.4921085812548,0.));
#112777=CARTESIAN_POINT('Ctrl Pts',(66.4630960167252,25.4921085812548,12.));
#112778=CARTESIAN_POINT('Ctrl Pts',(66.4804784439148,25.5062466667702,0.));
#112779=CARTESIAN_POINT('Ctrl Pts',(66.4804784439148,25.5062466667702,12.));
#112780=CARTESIAN_POINT('Ctrl Pts',(66.4978823598354,25.5204314764033,0.));
#112781=CARTESIAN_POINT('Ctrl Pts',(66.4978823598354,25.5204314764033,12.));
#112782=CARTESIAN_POINT('Ctrl Pts',(66.5153076112231,25.534662975532,0.));
#112783=CARTESIAN_POINT('Ctrl Pts',(66.5153076112231,25.534662975532,12.));
#112784=CARTESIAN_POINT('Ctrl Pts',(66.5327540455624,25.5489411295912,0.));
#112785=CARTESIAN_POINT('Ctrl Pts',(66.5327540455624,25.5489411295912,12.));
#112786=CARTESIAN_POINT('Ctrl Pts',(66.5502215110829,25.5632659040792,0.));
#112787=CARTESIAN_POINT('Ctrl Pts',(66.5502215110829,25.5632659040792,12.));
#112788=CARTESIAN_POINT('Ctrl Pts',(66.5677098567542,25.5776372645601,0.));
#112789=CARTESIAN_POINT('Ctrl Pts',(66.5677098567542,25.5776372645601,12.));
#112790=CARTESIAN_POINT('Ctrl Pts',(66.5852189322813,25.5920551766629,0.));
#112791=CARTESIAN_POINT('Ctrl Pts',(66.5852189322813,25.5920551766629,12.));
#112792=CARTESIAN_POINT('Ctrl Pts',(66.6027485880963,25.6065196060756,0.));
#112793=CARTESIAN_POINT('Ctrl Pts',(66.6027485880963,25.6065196060756,12.));
#112794=CARTESIAN_POINT('Ctrl Pts',(66.6202986753506,25.6210305185403,0.));
#112795=CARTESIAN_POINT('Ctrl Pts',(66.6202986753506,25.6210305185403,12.));
#112796=CARTESIAN_POINT('Ctrl Pts',(66.6378690459129,25.6355878798614,0.));
#112797=CARTESIAN_POINT('Ctrl Pts',(66.6378690459129,25.6355878798614,12.));
#112798=CARTESIAN_POINT('Ctrl Pts',(66.6554595523624,25.6501916559055,0.));
#112799=CARTESIAN_POINT('Ctrl Pts',(66.6554595523624,25.6501916559055,12.));
#112800=CARTESIAN_POINT('Ctrl Pts',(66.6730700479837,25.6648418126013,0.));
#112801=CARTESIAN_POINT('Ctrl Pts',(66.6730700479837,25.6648418126013,12.));
#112802=CARTESIAN_POINT('Ctrl Pts',(66.6907003867572,25.6795383159319,0.));
#112803=CARTESIAN_POINT('Ctrl Pts',(66.6907003867572,25.6795383159319,12.));
#112804=CARTESIAN_POINT('Ctrl Pts',(66.7083504233529,25.6942811319322,0.));
#112805=CARTESIAN_POINT('Ctrl Pts',(66.7083504233529,25.6942811319322,12.));
#112806=CARTESIAN_POINT('Ctrl Pts',(66.7260200131266,25.7090702266963,0.));
#112807=CARTESIAN_POINT('Ctrl Pts',(66.7260200131266,25.7090702266963,12.));
#112808=CARTESIAN_POINT('Ctrl Pts',(66.7437090121153,25.7239055663772,0.));
#112809=CARTESIAN_POINT('Ctrl Pts',(66.7437090121153,25.7239055663772,12.));
#112810=CARTESIAN_POINT('Ctrl Pts',(66.7614172770316,25.7387871171866,0.));
#112811=CARTESIAN_POINT('Ctrl Pts',(66.7614172770316,25.7387871171866,12.));
#112812=CARTESIAN_POINT('Ctrl Pts',(66.7791446652545,25.7537148453864,0.));
#112813=CARTESIAN_POINT('Ctrl Pts',(66.7791446652545,25.7537148453864,12.));
#112814=CARTESIAN_POINT('Ctrl Pts',(66.7968910348245,25.7686887172878,0.));
#112815=CARTESIAN_POINT('Ctrl Pts',(66.7968910348245,25.7686887172878,12.));
#112816=CARTESIAN_POINT('Ctrl Pts',(66.8146562444433,25.7837086992595,0.));
#112817=CARTESIAN_POINT('Ctrl Pts',(66.8146562444433,25.7837086992595,12.));
#112818=CARTESIAN_POINT('Ctrl Pts',(66.8324401534668,25.7987747577269,0.));
#112819=CARTESIAN_POINT('Ctrl Pts',(66.8324401534668,25.7987747577269,12.));
#112820=CARTESIAN_POINT('Ctrl Pts',(66.8502426219001,25.8138868591709,0.));
#112821=CARTESIAN_POINT('Ctrl Pts',(66.8502426219001,25.8138868591709,12.));
#112822=CARTESIAN_POINT('Ctrl Pts',(66.8680635103876,25.8290449701193,0.));
#112823=CARTESIAN_POINT('Ctrl Pts',(66.8680635103876,25.8290449701193,12.));
#112824=CARTESIAN_POINT('Ctrl Pts',(66.8859026802088,25.844249057147,0.));
#112825=CARTESIAN_POINT('Ctrl Pts',(66.8859026802088,25.844249057147,12.));
#112826=CARTESIAN_POINT('Ctrl Pts',(66.9037599932761,25.8594990868833,0.));
#112827=CARTESIAN_POINT('Ctrl Pts',(66.9037599932761,25.8594990868833,12.));
#112828=CARTESIAN_POINT('Ctrl Pts',(66.92163531213,25.8747950260111,0.));
#112829=CARTESIAN_POINT('Ctrl Pts',(66.92163531213,25.8747950260111,12.));
#112830=CARTESIAN_POINT('Ctrl Pts',(66.939528499934,25.890136841266,0.));
#112831=CARTESIAN_POINT('Ctrl Pts',(66.939528499934,25.890136841266,12.));
#112832=CARTESIAN_POINT('Ctrl Pts',(66.9574394204663,25.9055244994277,0.));
#112833=CARTESIAN_POINT('Ctrl Pts',(66.9574394204663,25.9055244994277,12.));
#112834=CARTESIAN_POINT('Ctrl Pts',(66.975367938115,25.9209579673209,0.));
#112835=CARTESIAN_POINT('Ctrl Pts',(66.975367938115,25.9209579673209,12.));
#112836=CARTESIAN_POINT('Ctrl Pts',(66.9933139178778,25.9364372118222,0.));
#112837=CARTESIAN_POINT('Ctrl Pts',(66.9933139178778,25.9364372118222,12.));
#112838=CARTESIAN_POINT('Ctrl Pts',(67.0112772253556,25.9519621998598,0.));
#112839=CARTESIAN_POINT('Ctrl Pts',(67.0112772253556,25.9519621998598,12.));
#112840=CARTESIAN_POINT('Ctrl Pts',(67.0292577267489,25.9675328984121,0.));
#112841=CARTESIAN_POINT('Ctrl Pts',(67.0292577267489,25.9675328984121,12.));
#112842=CARTESIAN_POINT('Ctrl Pts',(67.0472552888485,25.9831492744984,0.));
#112843=CARTESIAN_POINT('Ctrl Pts',(67.0472552888485,25.9831492744984,12.));
#112844=CARTESIAN_POINT('Ctrl Pts',(67.0652697790325,25.9988112951814,0.));
#112845=CARTESIAN_POINT('Ctrl Pts',(67.0652697790325,25.9988112951814,12.));
#112846=CARTESIAN_POINT('Ctrl Pts',(67.0833010652634,26.014518927573,0.));
#112847=CARTESIAN_POINT('Ctrl Pts',(67.0833010652634,26.014518927573,12.));
#112848=CARTESIAN_POINT('Ctrl Pts',(67.101349016084,26.030272138834,0.));
#112849=CARTESIAN_POINT('Ctrl Pts',(67.101349016084,26.030272138834,12.));
#112850=CARTESIAN_POINT('Ctrl Pts',(67.1194135006124,26.0460708961725,0.));
#112851=CARTESIAN_POINT('Ctrl Pts',(67.1194135006124,26.0460708961725,12.));
#112852=CARTESIAN_POINT('Ctrl Pts',(67.1374943885354,26.061915166836,0.));
#112853=CARTESIAN_POINT('Ctrl Pts',(67.1374943885354,26.061915166836,12.));
#112854=CARTESIAN_POINT('Ctrl Pts',(67.1555915501049,26.0778049181128,0.));
#112855=CARTESIAN_POINT('Ctrl Pts',(67.1555915501049,26.0778049181128,12.));
#112856=CARTESIAN_POINT('Ctrl Pts',(67.173704856136,26.0937401173383,0.));
#112857=CARTESIAN_POINT('Ctrl Pts',(67.173704856136,26.0937401173383,12.));
#112858=CARTESIAN_POINT('Ctrl Pts',(67.1918341780018,26.1097207318949,0.));
#112859=CARTESIAN_POINT('Ctrl Pts',(67.1918341780018,26.1097207318949,12.));
#112860=CARTESIAN_POINT('Ctrl Pts',(67.2099793876297,26.1257467292102,0.));
#112861=CARTESIAN_POINT('Ctrl Pts',(67.2099793876297,26.1257467292102,12.));
#112862=CARTESIAN_POINT('Ctrl Pts',(67.2281403574938,26.1418180767489,0.));
#112863=CARTESIAN_POINT('Ctrl Pts',(67.2281403574938,26.1418180767489,12.));
#112864=CARTESIAN_POINT('Ctrl Pts',(67.2463169606115,26.1579347420138,0.));
#112865=CARTESIAN_POINT('Ctrl Pts',(67.2463169606115,26.1579347420138,12.));
#112866=CARTESIAN_POINT('Ctrl Pts',(67.2645090705421,26.1740966925529,0.));
#112867=CARTESIAN_POINT('Ctrl Pts',(67.2645090705421,26.1740966925529,12.));
#112868=CARTESIAN_POINT('Ctrl Pts',(67.282716561383,26.1903038959589,0.));
#112869=CARTESIAN_POINT('Ctrl Pts',(67.282716561383,26.1903038959589,12.));
#112870=CARTESIAN_POINT('Ctrl Pts',(67.3009393077651,26.2065563198683,0.));
#112871=CARTESIAN_POINT('Ctrl Pts',(67.3009393077651,26.2065563198683,12.));
#112872=CARTESIAN_POINT('Ctrl Pts',(67.3191771848463,26.2228539319526,0.));
#112873=CARTESIAN_POINT('Ctrl Pts',(67.3191771848463,26.2228539319526,12.));
#112874=CARTESIAN_POINT('Ctrl Pts',(67.3374300683073,26.2391966999191,0.));
#112875=CARTESIAN_POINT('Ctrl Pts',(67.3374300683073,26.2391966999191,12.));
#112876=CARTESIAN_POINT('Ctrl Pts',(67.3556978343507,26.255584591518,0.));
#112877=CARTESIAN_POINT('Ctrl Pts',(67.3556978343507,26.255584591518,12.));
#112878=CARTESIAN_POINT('Ctrl Pts',(67.3739803596969,26.2720175745423,0.));
#112879=CARTESIAN_POINT('Ctrl Pts',(67.3739803596969,26.2720175745423,12.));
#112880=CARTESIAN_POINT('Ctrl Pts',(67.392277521581,26.288495616827,0.));
#112881=CARTESIAN_POINT('Ctrl Pts',(67.392277521581,26.288495616827,12.));
#112882=CARTESIAN_POINT('Ctrl Pts',(67.4105891977461,26.3050186862407,0.));
#112883=CARTESIAN_POINT('Ctrl Pts',(67.4105891977461,26.3050186862407,12.));
#112884=CARTESIAN_POINT('Ctrl Pts',(67.4289152664398,26.321586750686,0.));
#112885=CARTESIAN_POINT('Ctrl Pts',(67.4289152664398,26.321586750686,12.));
#112886=CARTESIAN_POINT('Ctrl Pts',(67.4472556064119,26.3381997781055,0.));
#112887=CARTESIAN_POINT('Ctrl Pts',(67.4472556064119,26.3381997781055,12.));
#112888=CARTESIAN_POINT('Ctrl Pts',(67.4656100969116,26.3548577364833,0.));
#112889=CARTESIAN_POINT('Ctrl Pts',(67.4656100969116,26.3548577364833,12.));
#112890=CARTESIAN_POINT('Ctrl Pts',(67.4839786176836,26.3715605938433,0.));
#112891=CARTESIAN_POINT('Ctrl Pts',(67.4839786176836,26.3715605938433,12.));
#112892=CARTESIAN_POINT('Ctrl Pts',(67.5023610489622,26.3883083182421,0.));
#112893=CARTESIAN_POINT('Ctrl Pts',(67.5023610489622,26.3883083182421,12.));
#112894=CARTESIAN_POINT('Ctrl Pts',(67.5207572714683,26.4051008777675,0.));
#112895=CARTESIAN_POINT('Ctrl Pts',(67.5207572714683,26.4051008777675,12.));
#112896=CARTESIAN_POINT('Ctrl Pts',(67.5391671664072,26.4219382405458,0.));
#112897=CARTESIAN_POINT('Ctrl Pts',(67.5391671664072,26.4219382405458,12.));
#112898=CARTESIAN_POINT('Ctrl Pts',(67.5575906154657,26.4388203747425,0.));
#112899=CARTESIAN_POINT('Ctrl Pts',(67.5575906154657,26.4388203747425,12.));
#112900=CARTESIAN_POINT('Ctrl Pts',(67.5760275008093,26.4557472485621,0.));
#112901=CARTESIAN_POINT('Ctrl Pts',(67.5760275008093,26.4557472485621,12.));
#112902=CARTESIAN_POINT('Ctrl Pts',(67.5944777050768,26.4727188302409,0.));
#112903=CARTESIAN_POINT('Ctrl Pts',(67.5944777050768,26.4727188302409,12.));
#112904=CARTESIAN_POINT('Ctrl Pts',(67.6129411113757,26.489735088044,0.));
#112905=CARTESIAN_POINT('Ctrl Pts',(67.6129411113757,26.489735088044,12.));
#112906=CARTESIAN_POINT('Ctrl Pts',(67.6314176032811,26.5067959902725,0.));
#112907=CARTESIAN_POINT('Ctrl Pts',(67.6314176032811,26.5067959902725,12.));
#112908=CARTESIAN_POINT('Ctrl Pts',(67.649907064832,26.5239015052654,0.));
#112909=CARTESIAN_POINT('Ctrl Pts',(67.649907064832,26.5239015052654,12.));
#112910=CARTESIAN_POINT('Ctrl Pts',(67.6684093805291,26.5410516013985,0.));
#112911=CARTESIAN_POINT('Ctrl Pts',(67.6684093805291,26.5410516013985,12.));
#112912=CARTESIAN_POINT('Ctrl Pts',(67.6869244353294,26.5582462470794,0.));
#112913=CARTESIAN_POINT('Ctrl Pts',(67.6869244353294,26.5582462470794,12.));
#112914=CARTESIAN_POINT('Ctrl Pts',(67.7054521146424,26.5754854107421,0.));
#112915=CARTESIAN_POINT('Ctrl Pts',(67.7054521146424,26.5754854107421,12.));
#112916=CARTESIAN_POINT('Ctrl Pts',(67.7239923043288,26.5927690608544,0.));
#112917=CARTESIAN_POINT('Ctrl Pts',(67.7239923043288,26.5927690608544,12.));
#112918=CARTESIAN_POINT('Ctrl Pts',(67.7425448906977,26.6100971659202,0.));
#112919=CARTESIAN_POINT('Ctrl Pts',(67.7425448906977,26.6100971659202,12.));
#112920=CARTESIAN_POINT('Ctrl Pts',(67.7611097605042,26.6274696944793,0.));
#112921=CARTESIAN_POINT('Ctrl Pts',(67.7611097605042,26.6274696944793,12.));
#112922=CARTESIAN_POINT('Ctrl Pts',(67.7796868009455,26.6448866151029,0.));
#112923=CARTESIAN_POINT('Ctrl Pts',(67.7796868009455,26.6448866151029,12.));
#112924=CARTESIAN_POINT('Ctrl Pts',(67.798275899657,26.6623478963871,0.));
#112925=CARTESIAN_POINT('Ctrl Pts',(67.798275899657,26.6623478963871,12.));
#112926=CARTESIAN_POINT('Ctrl Pts',(67.8168769447098,26.6798535069589,0.));
#112927=CARTESIAN_POINT('Ctrl Pts',(67.8168769447098,26.6798535069589,12.));
#112928=CARTESIAN_POINT('Ctrl Pts',(67.8354898246086,26.6974034154804,0.));
#112929=CARTESIAN_POINT('Ctrl Pts',(67.8354898246086,26.6974034154804,12.));
#112930=CARTESIAN_POINT('Ctrl Pts',(67.8541144282875,26.7149975906478,0.));
#112931=CARTESIAN_POINT('Ctrl Pts',(67.8541144282875,26.7149975906478,12.));
#112932=CARTESIAN_POINT('Ctrl Pts',(67.8727506451063,26.7326360011885,0.));
#112933=CARTESIAN_POINT('Ctrl Pts',(67.8727506451063,26.7326360011885,12.));
#112934=CARTESIAN_POINT('Ctrl Pts',(67.8913983648436,26.7503186158522,0.));
#112935=CARTESIAN_POINT('Ctrl Pts',(67.8913983648436,26.7503186158522,12.));
#112936=CARTESIAN_POINT('Ctrl Pts',(67.9100574776972,26.7680454034169,0.));
#112937=CARTESIAN_POINT('Ctrl Pts',(67.9100574776972,26.7680454034169,12.));
#112938=CARTESIAN_POINT('Ctrl Pts',(67.928727874284,26.7858163326934,0.));
#112939=CARTESIAN_POINT('Ctrl Pts',(67.928727874284,26.7858163326934,12.));
#112940=CARTESIAN_POINT('Ctrl Pts',(67.9474094456396,26.8036313725262,0.));
#112941=CARTESIAN_POINT('Ctrl Pts',(67.9474094456396,26.8036313725262,12.));
#112942=CARTESIAN_POINT('Ctrl Pts',(67.9661020832164,26.821490491792,0.));
#112943=CARTESIAN_POINT('Ctrl Pts',(67.9661020832164,26.821490491792,12.));
#112944=CARTESIAN_POINT('Ctrl Pts',(67.9848056788809,26.8393936593911,0.));
#112945=CARTESIAN_POINT('Ctrl Pts',(67.9848056788809,26.8393936593911,12.));
#112946=CARTESIAN_POINT('Ctrl Pts',(68.0035201249102,26.8573408442496,0.));
#112947=CARTESIAN_POINT('Ctrl Pts',(68.0035201249102,26.8573408442496,12.));
#112948=CARTESIAN_POINT('Ctrl Pts',(68.0222453139856,26.8753320153252,0.));
#112949=CARTESIAN_POINT('Ctrl Pts',(68.0222453139856,26.8753320153252,12.));
#112950=CARTESIAN_POINT('Ctrl Pts',(68.0409811391869,26.8933671416063,0.));
#112951=CARTESIAN_POINT('Ctrl Pts',(68.0409811391869,26.8933671416063,12.));
#112952=CARTESIAN_POINT('Ctrl Pts',(68.0597274939859,26.911446192111,0.));
#112953=CARTESIAN_POINT('Ctrl Pts',(68.0597274939859,26.911446192111,12.));
#112954=CARTESIAN_POINT('Ctrl Pts',(68.0784842722369,26.9295691358779,0.));
#112955=CARTESIAN_POINT('Ctrl Pts',(68.0784842722369,26.9295691358779,12.));
#112956=CARTESIAN_POINT('Ctrl Pts',(68.0972513681751,26.9477359419652,0.));
#112957=CARTESIAN_POINT('Ctrl Pts',(68.0972513681751,26.9477359419652,12.));
#112958=CARTESIAN_POINT('Ctrl Pts',(68.1160286764255,26.9659465794601,0.));
#112959=CARTESIAN_POINT('Ctrl Pts',(68.1160286764255,26.9659465794601,12.));
#112960=CARTESIAN_POINT('Ctrl Pts',(68.1348160920106,26.9842010174822,0.));
#112961=CARTESIAN_POINT('Ctrl Pts',(68.1348160920106,26.9842010174822,12.));
#112962=CARTESIAN_POINT('Ctrl Pts',(68.1536135103557,27.0024992251838,0.));
#112963=CARTESIAN_POINT('Ctrl Pts',(68.1536135103557,27.0024992251838,12.));
#112964=CARTESIAN_POINT('Ctrl Pts',(68.1724208272958,27.0208411717472,0.));
#112965=CARTESIAN_POINT('Ctrl Pts',(68.1724208272958,27.0208411717472,12.));
#112966=CARTESIAN_POINT('Ctrl Pts',(68.1912379390773,27.0392268263798,0.));
#112967=CARTESIAN_POINT('Ctrl Pts',(68.1912379390773,27.0392268263798,12.));
#112968=CARTESIAN_POINT('Ctrl Pts',(68.2100647423332,27.0576561583172,0.));
#112969=CARTESIAN_POINT('Ctrl Pts',(68.2100647423332,27.0576561583172,12.));
#112970=CARTESIAN_POINT('Ctrl Pts',(68.2289011340615,27.0761291368226,0.));
#112971=CARTESIAN_POINT('Ctrl Pts',(68.2289011340615,27.0761291368226,12.));
#112972=CARTESIAN_POINT('Ctrl Pts',(68.2477470116012,27.0946457311813,0.));
#112973=CARTESIAN_POINT('Ctrl Pts',(68.2477470116012,27.0946457311813,12.));
#112974=CARTESIAN_POINT('Ctrl Pts',(68.2666022726104,27.1132059106943,0.));
#112975=CARTESIAN_POINT('Ctrl Pts',(68.2666022726104,27.1132059106943,12.));
#112976=CARTESIAN_POINT('Ctrl Pts',(68.2854668150364,27.1318096446649,0.));
#112977=CARTESIAN_POINT('Ctrl Pts',(68.2854668150364,27.1318096446649,12.));
#112978=CARTESIAN_POINT('Ctrl Pts',(68.3043405371603,27.1504569024136,0.));
#112979=CARTESIAN_POINT('Ctrl Pts',(68.3043405371603,27.1504569024136,12.));
#112980=CARTESIAN_POINT('Ctrl Pts',(68.3232233376425,27.1691476532921,0.));
#112981=CARTESIAN_POINT('Ctrl Pts',(68.3232233376425,27.1691476532921,12.));
#112982=CARTESIAN_POINT('Ctrl Pts',(68.3421151155711,27.1878818666926,0.));
#112983=CARTESIAN_POINT('Ctrl Pts',(68.3421151155711,27.1878818666926,12.));
#112984=CARTESIAN_POINT('Ctrl Pts',(68.3610157704994,27.2066595120542,0.));
#112985=CARTESIAN_POINT('Ctrl Pts',(68.3610157704994,27.2066595120542,12.));
#112986=CARTESIAN_POINT('Ctrl Pts',(68.3799252025102,27.2254805588673,0.));
#112987=CARTESIAN_POINT('Ctrl Pts',(68.3799252025102,27.2254805588673,12.));
#112988=CARTESIAN_POINT('Ctrl Pts',(68.3988433121581,27.244344976665,0.));
#112989=CARTESIAN_POINT('Ctrl Pts',(68.3988433121581,27.244344976665,12.));
#112990=CARTESIAN_POINT('Ctrl Pts',(68.4177700003465,27.263252735006,0.));
#112991=CARTESIAN_POINT('Ctrl Pts',(68.4177700003465,27.263252735006,12.));
#112992=CARTESIAN_POINT('Ctrl Pts',(68.4367051682164,27.2822038034538,0.));
#112993=CARTESIAN_POINT('Ctrl Pts',(68.4367051682164,27.2822038034538,12.));
#112994=CARTESIAN_POINT('Ctrl Pts',(68.4556487170441,27.301198151557,0.));
#112995=CARTESIAN_POINT('Ctrl Pts',(68.4556487170441,27.301198151557,12.));
#112996=CARTESIAN_POINT('Ctrl Pts',(68.4746005480997,27.3202357488154,0.));
#112997=CARTESIAN_POINT('Ctrl Pts',(68.4746005480997,27.3202357488154,12.));
#112998=CARTESIAN_POINT('Ctrl Pts',(68.4935605626372,27.3393165646752,0.));
#112999=CARTESIAN_POINT('Ctrl Pts',(68.4935605626372,27.3393165646752,12.));
#113000=CARTESIAN_POINT('Ctrl Pts',(68.5125286621902,27.3584405685947,0.));
#113001=CARTESIAN_POINT('Ctrl Pts',(68.5125286621902,27.3584405685947,12.));
#113002=CARTESIAN_POINT('Ctrl Pts',(68.5315047488046,27.3776077300918,0.));
#113003=CARTESIAN_POINT('Ctrl Pts',(68.5315047488046,27.3776077300918,12.));
#113004=CARTESIAN_POINT('Ctrl Pts',(68.5504887252976,27.3968180187941,0.));
#113005=CARTESIAN_POINT('Ctrl Pts',(68.5504887252976,27.3968180187941,12.));
#113006=CARTESIAN_POINT('Ctrl Pts',(68.5694804955002,27.4160714044825,0.));
#113007=CARTESIAN_POINT('Ctrl Pts',(68.5694804955002,27.4160714044825,12.));
#113008=CARTESIAN_POINT('Ctrl Pts',(68.5884799645193,27.4353678571349,0.));
#113009=CARTESIAN_POINT('Ctrl Pts',(68.5884799645193,27.4353678571349,12.));
#113010=CARTESIAN_POINT('Ctrl Pts',(68.6074870381588,27.4547073468213,0.));
#113011=CARTESIAN_POINT('Ctrl Pts',(68.6074870381588,27.4547073468213,12.));
#113012=CARTESIAN_POINT('Ctrl Pts',(68.6265016223536,27.4740898435977,0.));
#113013=CARTESIAN_POINT('Ctrl Pts',(68.6265016223536,27.4740898435977,12.));
#113014=CARTESIAN_POINT('Ctrl Pts',(68.6455236225471,27.4935153173863,0.));
#113015=CARTESIAN_POINT('Ctrl Pts',(68.6455236225471,27.4935153173863,12.));
#113016=CARTESIAN_POINT('Ctrl Pts',(68.6645529432059,27.5129837378798,0.));
#113017=CARTESIAN_POINT('Ctrl Pts',(68.6645529432059,27.5129837378798,12.));
#113018=CARTESIAN_POINT('Ctrl Pts',(68.683589486992,27.5324950743723,0.));
#113019=CARTESIAN_POINT('Ctrl Pts',(68.683589486992,27.5324950743723,12.));
#113020=CARTESIAN_POINT('Ctrl Pts',(68.7026331554348,27.552049295893,0.));
#113021=CARTESIAN_POINT('Ctrl Pts',(68.7026331554348,27.552049295893,12.));
#113022=CARTESIAN_POINT('Ctrl Pts',(68.721683850427,27.5716463715027,0.));
#113023=CARTESIAN_POINT('Ctrl Pts',(68.721683850427,27.5716463715027,12.));
#113024=CARTESIAN_POINT('Ctrl Pts',(68.7407414755291,27.5912862705482,0.));
#113025=CARTESIAN_POINT('Ctrl Pts',(68.7407414755291,27.5912862705482,12.));
#113026=CARTESIAN_POINT('Ctrl Pts',(68.7598059372121,27.6109689629025,0.));
#113027=CARTESIAN_POINT('Ctrl Pts',(68.7598059372121,27.6109689629025,12.));
#113028=CARTESIAN_POINT('Ctrl Pts',(68.7788771464655,27.6306944192711,0.));
#113029=CARTESIAN_POINT('Ctrl Pts',(68.7788771464655,27.6306944192711,12.));
#113030=CARTESIAN_POINT('Ctrl Pts',(68.7979550191773,27.6504626112621,0.));
#113031=CARTESIAN_POINT('Ctrl Pts',(68.7979550191773,27.6504626112621,12.));
#113032=CARTESIAN_POINT('Ctrl Pts',(68.8170394725786,27.670273510707,0.));
#113033=CARTESIAN_POINT('Ctrl Pts',(68.8170394725786,27.670273510707,12.));
#113034=CARTESIAN_POINT('Ctrl Pts',(68.8361304224378,27.6901270891201,0.));
#113035=CARTESIAN_POINT('Ctrl Pts',(68.8361304224378,27.6901270891201,12.));
#113036=CARTESIAN_POINT('Ctrl Pts',(68.855227779818,27.7100233170728,0.));
#113037=CARTESIAN_POINT('Ctrl Pts',(68.855227779818,27.7100233170728,12.));
#113038=CARTESIAN_POINT('Ctrl Pts',(68.8743314483451,27.7299621636602,0.));
#113039=CARTESIAN_POINT('Ctrl Pts',(68.8743314483451,27.7299621636602,12.));
#113040=CARTESIAN_POINT('Ctrl Pts',(68.8934413203945,27.7499435957608,0.));
#113041=CARTESIAN_POINT('Ctrl Pts',(68.8934413203945,27.7499435957608,12.));
#113042=CARTESIAN_POINT('Ctrl Pts',(68.9125572825946,27.7699675790683,0.));
#113043=CARTESIAN_POINT('Ctrl Pts',(68.9125572825946,27.7699675790683,12.));
#113044=CARTESIAN_POINT('Ctrl Pts',(68.9316792226187,27.7900340793796,0.));
#113045=CARTESIAN_POINT('Ctrl Pts',(68.9316792226187,27.7900340793796,12.));
#113046=CARTESIAN_POINT('Ctrl Pts',(68.9508070357786,27.8101430638128,0.));
#113047=CARTESIAN_POINT('Ctrl Pts',(68.9508070357786,27.8101430638128,12.));
#113048=CARTESIAN_POINT('Ctrl Pts',(68.9699406311305,27.8302945019939,0.));
#113049=CARTESIAN_POINT('Ctrl Pts',(68.9699406311305,27.8302945019939,12.));
#113050=CARTESIAN_POINT('Ctrl Pts',(68.9890799391863,27.8504883673903,0.));
#113051=CARTESIAN_POINT('Ctrl Pts',(68.9890799391863,27.8504883673903,12.));
#113052=CARTESIAN_POINT('Ctrl Pts',(69.0082249138015,27.8707246380697,0.));
#113053=CARTESIAN_POINT('Ctrl Pts',(69.0082249138015,27.8707246380697,12.));
#113054=CARTESIAN_POINT('Ctrl Pts',(69.0273755264702,27.8910032967037,0.));
#113055=CARTESIAN_POINT('Ctrl Pts',(69.0273755264702,27.8910032967037,12.));
#113056=CARTESIAN_POINT('Ctrl Pts',(69.0427005153223,27.9072601239469,0.));
#113057=CARTESIAN_POINT('Ctrl Pts',(69.0427005153223,27.9072601239469,12.));
#113058=CARTESIAN_POINT('Ctrl Pts',(69.0541967850685,27.9194718098851,0.));
#113059=CARTESIAN_POINT('Ctrl Pts',(69.0541967850685,27.9194718098851,12.));
#113060=CARTESIAN_POINT('Ctrl Pts',(69.0618620884596,27.9276214070576,0.));
#113061=CARTESIAN_POINT('Ctrl Pts',(69.0618620884596,27.9276214070576,12.));
#113062=CARTESIAN_POINT('Ctrl Pts',(69.065695021045,27.9316983239472,0.));
#113063=CARTESIAN_POINT('Ctrl Pts',(69.065695021045,27.9316983239472,12.));
#113064=CARTESIAN_POINT('',(65.4815644032299,24.7419628022042,0.));
#113065=CARTESIAN_POINT('Ctrl Pts',(65.4815644032299,24.7419628022042,0.));
#113066=CARTESIAN_POINT('Ctrl Pts',(65.4847237095443,24.7442214063382,0.));
#113067=CARTESIAN_POINT('Ctrl Pts',(65.4910454936254,24.7487434955982,0.));
#113068=CARTESIAN_POINT('Ctrl Pts',(65.5005376841101,24.7555412724651,0.));
#113069=CARTESIAN_POINT('Ctrl Pts',(65.5132129675333,24.7646342620841,0.));
#113070=CARTESIAN_POINT('Ctrl Pts',(65.5290887770232,24.7760493148465,0.));
#113071=CARTESIAN_POINT('Ctrl Pts',(65.5449962514661,24.7875131827491,0.));
#113072=CARTESIAN_POINT('Ctrl Pts',(65.5609353062829,24.799025856126,0.));
#113073=CARTESIAN_POINT('Ctrl Pts',(65.5769057914333,24.8105873098626,0.));
#113074=CARTESIAN_POINT('Ctrl Pts',(65.5929074932624,24.8221975032104,0.));
#113075=CARTESIAN_POINT('Ctrl Pts',(65.6089401625628,24.8338563866764,0.));
#113076=CARTESIAN_POINT('Ctrl Pts',(65.6250035361612,24.8455639071517,0.));
#113077=CARTESIAN_POINT('Ctrl Pts',(65.6410973603661,24.8573200135666,0.));
#113078=CARTESIAN_POINT('Ctrl Pts',(65.6572214156692,24.8691246628057,0.));
#113079=CARTESIAN_POINT('Ctrl Pts',(65.6733755087669,24.8809778178229,0.));
#113080=CARTESIAN_POINT('Ctrl Pts',(65.6895594608775,24.8928794448607,0.));
#113081=CARTESIAN_POINT('Ctrl Pts',(65.7057730980483,24.9048295111448,0.));
#113082=CARTESIAN_POINT('Ctrl Pts',(65.7220162391053,24.9168279820106,0.));
#113083=CARTESIAN_POINT('Ctrl Pts',(65.7382886895888,24.928874819458,0.));
#113084=CARTESIAN_POINT('Ctrl Pts',(65.7545902480323,24.9409699836537,0.));
#113085=CARTESIAN_POINT('Ctrl Pts',(65.7709207098959,24.9531134338696,0.));
#113086=CARTESIAN_POINT('Ctrl Pts',(65.7872798720823,24.9653051295581,0.));
#113087=CARTESIAN_POINT('Ctrl Pts',(65.8036675380718,24.9775450315683,0.));
#113088=CARTESIAN_POINT('Ctrl Pts',(65.8200835177024,24.9898331020983,0.));
#113089=CARTESIAN_POINT('Ctrl Pts',(65.8365276247128,25.002169304117,0.));
#113090=CARTESIAN_POINT('Ctrl Pts',(65.8529996750445,25.0145536009604,0.));
#113091=CARTESIAN_POINT('Ctrl Pts',(65.8694994847616,25.0269859558363,0.));
#113092=CARTESIAN_POINT('Ctrl Pts',(65.8860268683128,25.0394663314055,0.));
#113093=CARTESIAN_POINT('Ctrl Pts',(65.9025816394424,25.0519946900078,0.));
#113094=CARTESIAN_POINT('Ctrl Pts',(65.919163611981,25.0645709938524,0.));
#113095=CARTESIAN_POINT('Ctrl Pts',(65.9357726006163,25.0771952052028,0.));
#113096=CARTESIAN_POINT('Ctrl Pts',(65.9524084218139,25.0898672865915,0.));
#113097=CARTESIAN_POINT('Ctrl Pts',(65.9690708941558,25.1025872009004,0.));
#113098=CARTESIAN_POINT('Ctrl Pts',(65.9857598378433,25.1153549112503,0.));
#113099=CARTESIAN_POINT('Ctrl Pts',(66.0024750743897,25.1281703809297,0.));
#113100=CARTESIAN_POINT('Ctrl Pts',(66.0192164262621,25.1410335733099,0.));
#113101=CARTESIAN_POINT('Ctrl Pts',(66.0359837164734,25.1539444517419,0.));
#113102=CARTESIAN_POINT('Ctrl Pts',(66.0527767686025,25.1669029795661,0.));
#113103=CARTESIAN_POINT('Ctrl Pts',(66.0695954069713,25.1799091201599,0.));
#113104=CARTESIAN_POINT('Ctrl Pts',(66.086439456768,25.1929628369685,0.));
#113105=CARTESIAN_POINT('Ctrl Pts',(66.10330874419,25.2060640935365,0.));
#113106=CARTESIAN_POINT('Ctrl Pts',(66.1202030965758,25.2192128535357,0.));
#113107=CARTESIAN_POINT('Ctrl Pts',(66.1371223423345,25.232409080755,0.));
#113108=CARTESIAN_POINT('Ctrl Pts',(66.1540663108754,25.2456527390875,0.));
#113109=CARTESIAN_POINT('Ctrl Pts',(66.1710348325384,25.2589437925147,0.));
#113110=CARTESIAN_POINT('Ctrl Pts',(66.1880277385136,25.2722822050837,0.));
#113111=CARTESIAN_POINT('Ctrl Pts',(66.2050448607911,25.285667940893,0.));
#113112=CARTESIAN_POINT('Ctrl Pts',(66.2220860321952,25.2991009641094,0.));
#113113=CARTESIAN_POINT('Ctrl Pts',(66.2391510863998,25.312581238973,0.));
#113114=CARTESIAN_POINT('Ctrl Pts',(66.2562398579471,25.3261087298026,0.));
#113115=CARTESIAN_POINT('Ctrl Pts',(66.2733521822662,25.3396834009949,0.));
#113116=CARTESIAN_POINT('Ctrl Pts',(66.290487895671,25.3533052170249,0.));
#113117=CARTESIAN_POINT('Ctrl Pts',(66.3076468353412,25.3669741424488,0.));
#113118=CARTESIAN_POINT('Ctrl Pts',(66.3248288393046,25.3806901419012,0.));
#113119=CARTESIAN_POINT('Ctrl Pts',(66.3420337464178,25.3944531800901,0.));
#113120=CARTESIAN_POINT('Ctrl Pts',(66.359261396341,25.4082632217847,0.));
#113121=CARTESIAN_POINT('Ctrl Pts',(66.3765116295364,25.4221202318199,0.));
#113122=CARTESIAN_POINT('Ctrl Pts',(66.3937842872685,25.4360241751018,0.));
#113123=CARTESIAN_POINT('Ctrl Pts',(66.4110792116,25.4499750166079,0.));
#113124=CARTESIAN_POINT('Ctrl Pts',(66.4283962453899,25.4639727213849,0.));
#113125=CARTESIAN_POINT('Ctrl Pts',(66.4457352322871,25.4780172545417,0.));
#113126=CARTESIAN_POINT('Ctrl Pts',(66.4630960167252,25.4921085812548,0.));
#113127=CARTESIAN_POINT('Ctrl Pts',(66.4804784439148,25.5062466667702,0.));
#113128=CARTESIAN_POINT('Ctrl Pts',(66.4978823598354,25.5204314764033,0.));
#113129=CARTESIAN_POINT('Ctrl Pts',(66.5153076112231,25.534662975532,0.));
#113130=CARTESIAN_POINT('Ctrl Pts',(66.5327540455624,25.5489411295912,0.));
#113131=CARTESIAN_POINT('Ctrl Pts',(66.5502215110829,25.5632659040792,0.));
#113132=CARTESIAN_POINT('Ctrl Pts',(66.5677098567542,25.5776372645601,0.));
#113133=CARTESIAN_POINT('Ctrl Pts',(66.5852189322813,25.5920551766629,0.));
#113134=CARTESIAN_POINT('Ctrl Pts',(66.6027485880963,25.6065196060756,0.));
#113135=CARTESIAN_POINT('Ctrl Pts',(66.6202986753506,25.6210305185403,0.));
#113136=CARTESIAN_POINT('Ctrl Pts',(66.6378690459129,25.6355878798614,0.));
#113137=CARTESIAN_POINT('Ctrl Pts',(66.6554595523624,25.6501916559055,0.));
#113138=CARTESIAN_POINT('Ctrl Pts',(66.6730700479837,25.6648418126013,0.));
#113139=CARTESIAN_POINT('Ctrl Pts',(66.6907003867572,25.6795383159319,0.));
#113140=CARTESIAN_POINT('Ctrl Pts',(66.7083504233529,25.6942811319322,0.));
#113141=CARTESIAN_POINT('Ctrl Pts',(66.7260200131266,25.7090702266963,0.));
#113142=CARTESIAN_POINT('Ctrl Pts',(66.7437090121153,25.7239055663772,0.));
#113143=CARTESIAN_POINT('Ctrl Pts',(66.7614172770316,25.7387871171866,0.));
#113144=CARTESIAN_POINT('Ctrl Pts',(66.7791446652545,25.7537148453864,0.));
#113145=CARTESIAN_POINT('Ctrl Pts',(66.7968910348245,25.7686887172878,0.));
#113146=CARTESIAN_POINT('Ctrl Pts',(66.8146562444433,25.7837086992595,0.));
#113147=CARTESIAN_POINT('Ctrl Pts',(66.8324401534668,25.7987747577269,0.));
#113148=CARTESIAN_POINT('Ctrl Pts',(66.8502426219001,25.8138868591709,0.));
#113149=CARTESIAN_POINT('Ctrl Pts',(66.8680635103876,25.8290449701193,0.));
#113150=CARTESIAN_POINT('Ctrl Pts',(66.8859026802088,25.844249057147,0.));
#113151=CARTESIAN_POINT('Ctrl Pts',(66.9037599932761,25.8594990868833,0.));
#113152=CARTESIAN_POINT('Ctrl Pts',(66.92163531213,25.8747950260111,0.));
#113153=CARTESIAN_POINT('Ctrl Pts',(66.939528499934,25.890136841266,0.));
#113154=CARTESIAN_POINT('Ctrl Pts',(66.9574394204663,25.9055244994277,0.));
#113155=CARTESIAN_POINT('Ctrl Pts',(66.975367938115,25.9209579673209,0.));
#113156=CARTESIAN_POINT('Ctrl Pts',(66.9933139178778,25.9364372118222,0.));
#113157=CARTESIAN_POINT('Ctrl Pts',(67.0112772253556,25.9519621998598,0.));
#113158=CARTESIAN_POINT('Ctrl Pts',(67.0292577267489,25.9675328984121,0.));
#113159=CARTESIAN_POINT('Ctrl Pts',(67.0472552888485,25.9831492744984,0.));
#113160=CARTESIAN_POINT('Ctrl Pts',(67.0652697790325,25.9988112951814,0.));
#113161=CARTESIAN_POINT('Ctrl Pts',(67.0833010652634,26.014518927573,0.));
#113162=CARTESIAN_POINT('Ctrl Pts',(67.101349016084,26.030272138834,0.));
#113163=CARTESIAN_POINT('Ctrl Pts',(67.1194135006124,26.0460708961725,0.));
#113164=CARTESIAN_POINT('Ctrl Pts',(67.1374943885354,26.061915166836,0.));
#113165=CARTESIAN_POINT('Ctrl Pts',(67.1555915501049,26.0778049181128,0.));
#113166=CARTESIAN_POINT('Ctrl Pts',(67.173704856136,26.0937401173383,0.));
#113167=CARTESIAN_POINT('Ctrl Pts',(67.1918341780018,26.1097207318949,0.));
#113168=CARTESIAN_POINT('Ctrl Pts',(67.2099793876297,26.1257467292102,0.));
#113169=CARTESIAN_POINT('Ctrl Pts',(67.2281403574938,26.1418180767489,0.));
#113170=CARTESIAN_POINT('Ctrl Pts',(67.2463169606115,26.1579347420138,0.));
#113171=CARTESIAN_POINT('Ctrl Pts',(67.2645090705421,26.1740966925529,0.));
#113172=CARTESIAN_POINT('Ctrl Pts',(67.282716561383,26.1903038959589,0.));
#113173=CARTESIAN_POINT('Ctrl Pts',(67.3009393077651,26.2065563198683,0.));
#113174=CARTESIAN_POINT('Ctrl Pts',(67.3191771848463,26.2228539319526,0.));
#113175=CARTESIAN_POINT('Ctrl Pts',(67.3374300683073,26.2391966999191,0.));
#113176=CARTESIAN_POINT('Ctrl Pts',(67.3556978343507,26.255584591518,0.));
#113177=CARTESIAN_POINT('Ctrl Pts',(67.3739803596969,26.2720175745423,0.));
#113178=CARTESIAN_POINT('Ctrl Pts',(67.392277521581,26.288495616827,0.));
#113179=CARTESIAN_POINT('Ctrl Pts',(67.4105891977461,26.3050186862407,0.));
#113180=CARTESIAN_POINT('Ctrl Pts',(67.4289152664398,26.321586750686,0.));
#113181=CARTESIAN_POINT('Ctrl Pts',(67.4472556064119,26.3381997781055,0.));
#113182=CARTESIAN_POINT('Ctrl Pts',(67.4656100969116,26.3548577364833,0.));
#113183=CARTESIAN_POINT('Ctrl Pts',(67.4839786176836,26.3715605938433,0.));
#113184=CARTESIAN_POINT('Ctrl Pts',(67.5023610489622,26.3883083182421,0.));
#113185=CARTESIAN_POINT('Ctrl Pts',(67.5207572714683,26.4051008777675,0.));
#113186=CARTESIAN_POINT('Ctrl Pts',(67.5391671664072,26.4219382405458,0.));
#113187=CARTESIAN_POINT('Ctrl Pts',(67.5575906154657,26.4388203747425,0.));
#113188=CARTESIAN_POINT('Ctrl Pts',(67.5760275008093,26.4557472485621,0.));
#113189=CARTESIAN_POINT('Ctrl Pts',(67.5944777050768,26.4727188302409,0.));
#113190=CARTESIAN_POINT('Ctrl Pts',(67.6129411113757,26.489735088044,0.));
#113191=CARTESIAN_POINT('Ctrl Pts',(67.6314176032811,26.5067959902725,0.));
#113192=CARTESIAN_POINT('Ctrl Pts',(67.649907064832,26.5239015052654,0.));
#113193=CARTESIAN_POINT('Ctrl Pts',(67.6684093805291,26.5410516013985,0.));
#113194=CARTESIAN_POINT('Ctrl Pts',(67.6869244353294,26.5582462470794,0.));
#113195=CARTESIAN_POINT('Ctrl Pts',(67.7054521146424,26.5754854107421,0.));
#113196=CARTESIAN_POINT('Ctrl Pts',(67.7239923043288,26.5927690608544,0.));
#113197=CARTESIAN_POINT('Ctrl Pts',(67.7425448906977,26.6100971659202,0.));
#113198=CARTESIAN_POINT('Ctrl Pts',(67.7611097605042,26.6274696944793,0.));
#113199=CARTESIAN_POINT('Ctrl Pts',(67.7796868009455,26.6448866151029,0.));
#113200=CARTESIAN_POINT('Ctrl Pts',(67.798275899657,26.6623478963871,0.));
#113201=CARTESIAN_POINT('Ctrl Pts',(67.8168769447098,26.6798535069589,0.));
#113202=CARTESIAN_POINT('Ctrl Pts',(67.8354898246086,26.6974034154804,0.));
#113203=CARTESIAN_POINT('Ctrl Pts',(67.8541144282875,26.7149975906478,0.));
#113204=CARTESIAN_POINT('Ctrl Pts',(67.8727506451063,26.7326360011885,0.));
#113205=CARTESIAN_POINT('Ctrl Pts',(67.8913983648436,26.7503186158522,0.));
#113206=CARTESIAN_POINT('Ctrl Pts',(67.9100574776972,26.7680454034169,0.));
#113207=CARTESIAN_POINT('Ctrl Pts',(67.928727874284,26.7858163326934,0.));
#113208=CARTESIAN_POINT('Ctrl Pts',(67.9474094456396,26.8036313725262,0.));
#113209=CARTESIAN_POINT('Ctrl Pts',(67.9661020832164,26.821490491792,0.));
#113210=CARTESIAN_POINT('Ctrl Pts',(67.9848056788809,26.8393936593911,0.));
#113211=CARTESIAN_POINT('Ctrl Pts',(68.0035201249102,26.8573408442496,0.));
#113212=CARTESIAN_POINT('Ctrl Pts',(68.0222453139856,26.8753320153252,0.));
#113213=CARTESIAN_POINT('Ctrl Pts',(68.0409811391869,26.8933671416063,0.));
#113214=CARTESIAN_POINT('Ctrl Pts',(68.0597274939859,26.911446192111,0.));
#113215=CARTESIAN_POINT('Ctrl Pts',(68.0784842722369,26.9295691358779,0.));
#113216=CARTESIAN_POINT('Ctrl Pts',(68.0972513681751,26.9477359419652,0.));
#113217=CARTESIAN_POINT('Ctrl Pts',(68.1160286764255,26.9659465794601,0.));
#113218=CARTESIAN_POINT('Ctrl Pts',(68.1348160920106,26.9842010174822,0.));
#113219=CARTESIAN_POINT('Ctrl Pts',(68.1536135103557,27.0024992251838,0.));
#113220=CARTESIAN_POINT('Ctrl Pts',(68.1724208272958,27.0208411717472,0.));
#113221=CARTESIAN_POINT('Ctrl Pts',(68.1912379390773,27.0392268263798,0.));
#113222=CARTESIAN_POINT('Ctrl Pts',(68.2100647423332,27.0576561583172,0.));
#113223=CARTESIAN_POINT('Ctrl Pts',(68.2289011340615,27.0761291368226,0.));
#113224=CARTESIAN_POINT('Ctrl Pts',(68.2477470116012,27.0946457311813,0.));
#113225=CARTESIAN_POINT('Ctrl Pts',(68.2666022726104,27.1132059106943,0.));
#113226=CARTESIAN_POINT('Ctrl Pts',(68.2854668150364,27.1318096446649,0.));
#113227=CARTESIAN_POINT('Ctrl Pts',(68.3043405371603,27.1504569024136,0.));
#113228=CARTESIAN_POINT('Ctrl Pts',(68.3232233376425,27.1691476532921,0.));
#113229=CARTESIAN_POINT('Ctrl Pts',(68.3421151155711,27.1878818666926,0.));
#113230=CARTESIAN_POINT('Ctrl Pts',(68.3610157704994,27.2066595120542,0.));
#113231=CARTESIAN_POINT('Ctrl Pts',(68.3799252025102,27.2254805588673,0.));
#113232=CARTESIAN_POINT('Ctrl Pts',(68.3988433121581,27.244344976665,0.));
#113233=CARTESIAN_POINT('Ctrl Pts',(68.4177700003465,27.263252735006,0.));
#113234=CARTESIAN_POINT('Ctrl Pts',(68.4367051682164,27.2822038034538,0.));
#113235=CARTESIAN_POINT('Ctrl Pts',(68.4556487170441,27.301198151557,0.));
#113236=CARTESIAN_POINT('Ctrl Pts',(68.4746005480997,27.3202357488154,0.));
#113237=CARTESIAN_POINT('Ctrl Pts',(68.4935605626372,27.3393165646752,0.));
#113238=CARTESIAN_POINT('Ctrl Pts',(68.5125286621902,27.3584405685947,0.));
#113239=CARTESIAN_POINT('Ctrl Pts',(68.5315047488046,27.3776077300918,0.));
#113240=CARTESIAN_POINT('Ctrl Pts',(68.5504887252976,27.3968180187941,0.));
#113241=CARTESIAN_POINT('Ctrl Pts',(68.5694804955002,27.4160714044825,0.));
#113242=CARTESIAN_POINT('Ctrl Pts',(68.5884799645193,27.4353678571349,0.));
#113243=CARTESIAN_POINT('Ctrl Pts',(68.6074870381588,27.4547073468213,0.));
#113244=CARTESIAN_POINT('Ctrl Pts',(68.6265016223536,27.4740898435977,0.));
#113245=CARTESIAN_POINT('Ctrl Pts',(68.6455236225471,27.4935153173863,0.));
#113246=CARTESIAN_POINT('Ctrl Pts',(68.6645529432059,27.5129837378798,0.));
#113247=CARTESIAN_POINT('Ctrl Pts',(68.683589486992,27.5324950743723,0.));
#113248=CARTESIAN_POINT('Ctrl Pts',(68.7026331554348,27.552049295893,0.));
#113249=CARTESIAN_POINT('Ctrl Pts',(68.721683850427,27.5716463715027,0.));
#113250=CARTESIAN_POINT('Ctrl Pts',(68.7407414755291,27.5912862705482,0.));
#113251=CARTESIAN_POINT('Ctrl Pts',(68.7598059372121,27.6109689629025,0.));
#113252=CARTESIAN_POINT('Ctrl Pts',(68.7788771464655,27.6306944192711,0.));
#113253=CARTESIAN_POINT('Ctrl Pts',(68.7979550191773,27.6504626112621,0.));
#113254=CARTESIAN_POINT('Ctrl Pts',(68.8143140938753,27.6674443909882,0.));
#113255=CARTESIAN_POINT('Ctrl Pts',(68.826859785198,27.6804870323286,0.));
#113256=CARTESIAN_POINT('Ctrl Pts',(68.8355891981877,27.6895716271084,0.));
#113257=CARTESIAN_POINT('Ctrl Pts',(68.8405004465895,27.6946856803482,0.));
#113258=CARTESIAN_POINT('Ctrl Pts',(68.8415926174774,27.6958230984757,0.));
#113259=CARTESIAN_POINT('',(65.4815644032299,24.7419628022042,12.));
#113260=CARTESIAN_POINT('',(65.4815644032299,24.7419628022042,0.));
#113261=CARTESIAN_POINT('Ctrl Pts',(68.8415926174774,27.6958230984758,12.));
#113262=CARTESIAN_POINT('Ctrl Pts',(68.8405004465895,27.6946856803482,12.));
#113263=CARTESIAN_POINT('Ctrl Pts',(68.8355891981877,27.6895716271084,12.));
#113264=CARTESIAN_POINT('Ctrl Pts',(68.826859785198,27.6804870323286,12.));
#113265=CARTESIAN_POINT('Ctrl Pts',(68.8143140938753,27.6674443909882,12.));
#113266=CARTESIAN_POINT('Ctrl Pts',(68.7979550191773,27.6504626112621,12.));
#113267=CARTESIAN_POINT('Ctrl Pts',(68.7788771464655,27.6306944192711,12.));
#113268=CARTESIAN_POINT('Ctrl Pts',(68.7598059372121,27.6109689629025,12.));
#113269=CARTESIAN_POINT('Ctrl Pts',(68.7407414755291,27.5912862705482,12.));
#113270=CARTESIAN_POINT('Ctrl Pts',(68.721683850427,27.5716463715027,12.));
#113271=CARTESIAN_POINT('Ctrl Pts',(68.7026331554348,27.552049295893,12.));
#113272=CARTESIAN_POINT('Ctrl Pts',(68.683589486992,27.5324950743723,12.));
#113273=CARTESIAN_POINT('Ctrl Pts',(68.6645529432059,27.5129837378798,12.));
#113274=CARTESIAN_POINT('Ctrl Pts',(68.6455236225471,27.4935153173863,12.));
#113275=CARTESIAN_POINT('Ctrl Pts',(68.6265016223536,27.4740898435977,12.));
#113276=CARTESIAN_POINT('Ctrl Pts',(68.6074870381588,27.4547073468213,12.));
#113277=CARTESIAN_POINT('Ctrl Pts',(68.5884799645193,27.4353678571349,12.));
#113278=CARTESIAN_POINT('Ctrl Pts',(68.5694804955002,27.4160714044825,12.));
#113279=CARTESIAN_POINT('Ctrl Pts',(68.5504887252976,27.3968180187941,12.));
#113280=CARTESIAN_POINT('Ctrl Pts',(68.5315047488046,27.3776077300918,12.));
#113281=CARTESIAN_POINT('Ctrl Pts',(68.5125286621902,27.3584405685947,12.));
#113282=CARTESIAN_POINT('Ctrl Pts',(68.4935605626372,27.3393165646752,12.));
#113283=CARTESIAN_POINT('Ctrl Pts',(68.4746005480997,27.3202357488154,12.));
#113284=CARTESIAN_POINT('Ctrl Pts',(68.4556487170441,27.301198151557,12.));
#113285=CARTESIAN_POINT('Ctrl Pts',(68.4367051682164,27.2822038034538,12.));
#113286=CARTESIAN_POINT('Ctrl Pts',(68.4177700003465,27.263252735006,12.));
#113287=CARTESIAN_POINT('Ctrl Pts',(68.3988433121581,27.244344976665,12.));
#113288=CARTESIAN_POINT('Ctrl Pts',(68.3799252025102,27.2254805588673,12.));
#113289=CARTESIAN_POINT('Ctrl Pts',(68.3610157704994,27.2066595120542,12.));
#113290=CARTESIAN_POINT('Ctrl Pts',(68.3421151155711,27.1878818666926,12.));
#113291=CARTESIAN_POINT('Ctrl Pts',(68.3232233376425,27.1691476532921,12.));
#113292=CARTESIAN_POINT('Ctrl Pts',(68.3043405371603,27.1504569024136,12.));
#113293=CARTESIAN_POINT('Ctrl Pts',(68.2854668150364,27.1318096446649,12.));
#113294=CARTESIAN_POINT('Ctrl Pts',(68.2666022726104,27.1132059106943,12.));
#113295=CARTESIAN_POINT('Ctrl Pts',(68.2477470116012,27.0946457311813,12.));
#113296=CARTESIAN_POINT('Ctrl Pts',(68.2289011340615,27.0761291368226,12.));
#113297=CARTESIAN_POINT('Ctrl Pts',(68.2100647423332,27.0576561583172,12.));
#113298=CARTESIAN_POINT('Ctrl Pts',(68.1912379390773,27.0392268263798,12.));
#113299=CARTESIAN_POINT('Ctrl Pts',(68.1724208272958,27.0208411717472,12.));
#113300=CARTESIAN_POINT('Ctrl Pts',(68.1536135103557,27.0024992251838,12.));
#113301=CARTESIAN_POINT('Ctrl Pts',(68.1348160920106,26.9842010174822,12.));
#113302=CARTESIAN_POINT('Ctrl Pts',(68.1160286764255,26.9659465794601,12.));
#113303=CARTESIAN_POINT('Ctrl Pts',(68.0972513681751,26.9477359419652,12.));
#113304=CARTESIAN_POINT('Ctrl Pts',(68.0784842722369,26.9295691358779,12.));
#113305=CARTESIAN_POINT('Ctrl Pts',(68.0597274939859,26.911446192111,12.));
#113306=CARTESIAN_POINT('Ctrl Pts',(68.0409811391869,26.8933671416063,12.));
#113307=CARTESIAN_POINT('Ctrl Pts',(68.0222453139856,26.8753320153252,12.));
#113308=CARTESIAN_POINT('Ctrl Pts',(68.0035201249102,26.8573408442496,12.));
#113309=CARTESIAN_POINT('Ctrl Pts',(67.9848056788809,26.8393936593911,12.));
#113310=CARTESIAN_POINT('Ctrl Pts',(67.9661020832164,26.821490491792,12.));
#113311=CARTESIAN_POINT('Ctrl Pts',(67.9474094456396,26.8036313725262,12.));
#113312=CARTESIAN_POINT('Ctrl Pts',(67.928727874284,26.7858163326934,12.));
#113313=CARTESIAN_POINT('Ctrl Pts',(67.9100574776972,26.7680454034169,12.));
#113314=CARTESIAN_POINT('Ctrl Pts',(67.8913983648436,26.7503186158522,12.));
#113315=CARTESIAN_POINT('Ctrl Pts',(67.8727506451063,26.7326360011885,12.));
#113316=CARTESIAN_POINT('Ctrl Pts',(67.8541144282875,26.7149975906478,12.));
#113317=CARTESIAN_POINT('Ctrl Pts',(67.8354898246086,26.6974034154804,12.));
#113318=CARTESIAN_POINT('Ctrl Pts',(67.8168769447098,26.6798535069589,12.));
#113319=CARTESIAN_POINT('Ctrl Pts',(67.798275899657,26.6623478963871,12.));
#113320=CARTESIAN_POINT('Ctrl Pts',(67.7796868009455,26.6448866151029,12.));
#113321=CARTESIAN_POINT('Ctrl Pts',(67.7611097605042,26.6274696944793,12.));
#113322=CARTESIAN_POINT('Ctrl Pts',(67.7425448906977,26.6100971659202,12.));
#113323=CARTESIAN_POINT('Ctrl Pts',(67.7239923043288,26.5927690608544,12.));
#113324=CARTESIAN_POINT('Ctrl Pts',(67.7054521146424,26.5754854107421,12.));
#113325=CARTESIAN_POINT('Ctrl Pts',(67.6869244353294,26.5582462470794,12.));
#113326=CARTESIAN_POINT('Ctrl Pts',(67.6684093805291,26.5410516013985,12.));
#113327=CARTESIAN_POINT('Ctrl Pts',(67.649907064832,26.5239015052654,12.));
#113328=CARTESIAN_POINT('Ctrl Pts',(67.6314176032811,26.5067959902725,12.));
#113329=CARTESIAN_POINT('Ctrl Pts',(67.6129411113757,26.489735088044,12.));
#113330=CARTESIAN_POINT('Ctrl Pts',(67.5944777050768,26.4727188302409,12.));
#113331=CARTESIAN_POINT('Ctrl Pts',(67.5760275008093,26.4557472485621,12.));
#113332=CARTESIAN_POINT('Ctrl Pts',(67.5575906154657,26.4388203747425,12.));
#113333=CARTESIAN_POINT('Ctrl Pts',(67.5391671664072,26.4219382405458,12.));
#113334=CARTESIAN_POINT('Ctrl Pts',(67.5207572714683,26.4051008777675,12.));
#113335=CARTESIAN_POINT('Ctrl Pts',(67.5023610489622,26.3883083182421,12.));
#113336=CARTESIAN_POINT('Ctrl Pts',(67.4839786176836,26.3715605938433,12.));
#113337=CARTESIAN_POINT('Ctrl Pts',(67.4656100969116,26.3548577364833,12.));
#113338=CARTESIAN_POINT('Ctrl Pts',(67.4472556064119,26.3381997781055,12.));
#113339=CARTESIAN_POINT('Ctrl Pts',(67.4289152664398,26.321586750686,12.));
#113340=CARTESIAN_POINT('Ctrl Pts',(67.4105891977461,26.3050186862407,12.));
#113341=CARTESIAN_POINT('Ctrl Pts',(67.392277521581,26.288495616827,12.));
#113342=CARTESIAN_POINT('Ctrl Pts',(67.3739803596969,26.2720175745423,12.));
#113343=CARTESIAN_POINT('Ctrl Pts',(67.3556978343507,26.255584591518,12.));
#113344=CARTESIAN_POINT('Ctrl Pts',(67.3374300683073,26.2391966999191,12.));
#113345=CARTESIAN_POINT('Ctrl Pts',(67.3191771848463,26.2228539319526,12.));
#113346=CARTESIAN_POINT('Ctrl Pts',(67.3009393077651,26.2065563198683,12.));
#113347=CARTESIAN_POINT('Ctrl Pts',(67.282716561383,26.1903038959589,12.));
#113348=CARTESIAN_POINT('Ctrl Pts',(67.2645090705421,26.1740966925529,12.));
#113349=CARTESIAN_POINT('Ctrl Pts',(67.2463169606115,26.1579347420138,12.));
#113350=CARTESIAN_POINT('Ctrl Pts',(67.2281403574938,26.1418180767489,12.));
#113351=CARTESIAN_POINT('Ctrl Pts',(67.2099793876297,26.1257467292102,12.));
#113352=CARTESIAN_POINT('Ctrl Pts',(67.1918341780018,26.1097207318949,12.));
#113353=CARTESIAN_POINT('Ctrl Pts',(67.173704856136,26.0937401173383,12.));
#113354=CARTESIAN_POINT('Ctrl Pts',(67.1555915501049,26.0778049181128,12.));
#113355=CARTESIAN_POINT('Ctrl Pts',(67.1374943885354,26.061915166836,12.));
#113356=CARTESIAN_POINT('Ctrl Pts',(67.1194135006124,26.0460708961725,12.));
#113357=CARTESIAN_POINT('Ctrl Pts',(67.101349016084,26.030272138834,12.));
#113358=CARTESIAN_POINT('Ctrl Pts',(67.0833010652634,26.014518927573,12.));
#113359=CARTESIAN_POINT('Ctrl Pts',(67.0652697790325,25.9988112951814,12.));
#113360=CARTESIAN_POINT('Ctrl Pts',(67.0472552888485,25.9831492744984,12.));
#113361=CARTESIAN_POINT('Ctrl Pts',(67.0292577267489,25.9675328984121,12.));
#113362=CARTESIAN_POINT('Ctrl Pts',(67.0112772253556,25.9519621998598,12.));
#113363=CARTESIAN_POINT('Ctrl Pts',(66.9933139178778,25.9364372118222,12.));
#113364=CARTESIAN_POINT('Ctrl Pts',(66.975367938115,25.9209579673209,12.));
#113365=CARTESIAN_POINT('Ctrl Pts',(66.9574394204663,25.9055244994277,12.));
#113366=CARTESIAN_POINT('Ctrl Pts',(66.939528499934,25.890136841266,12.));
#113367=CARTESIAN_POINT('Ctrl Pts',(66.92163531213,25.8747950260111,12.));
#113368=CARTESIAN_POINT('Ctrl Pts',(66.9037599932761,25.8594990868833,12.));
#113369=CARTESIAN_POINT('Ctrl Pts',(66.8859026802088,25.844249057147,12.));
#113370=CARTESIAN_POINT('Ctrl Pts',(66.8680635103876,25.8290449701193,12.));
#113371=CARTESIAN_POINT('Ctrl Pts',(66.8502426219001,25.8138868591709,12.));
#113372=CARTESIAN_POINT('Ctrl Pts',(66.8324401534668,25.7987747577269,12.));
#113373=CARTESIAN_POINT('Ctrl Pts',(66.8146562444433,25.7837086992595,12.));
#113374=CARTESIAN_POINT('Ctrl Pts',(66.7968910348245,25.7686887172878,12.));
#113375=CARTESIAN_POINT('Ctrl Pts',(66.7791446652545,25.7537148453864,12.));
#113376=CARTESIAN_POINT('Ctrl Pts',(66.7614172770316,25.7387871171866,12.));
#113377=CARTESIAN_POINT('Ctrl Pts',(66.7437090121153,25.7239055663772,12.));
#113378=CARTESIAN_POINT('Ctrl Pts',(66.7260200131266,25.7090702266963,12.));
#113379=CARTESIAN_POINT('Ctrl Pts',(66.7083504233529,25.6942811319322,12.));
#113380=CARTESIAN_POINT('Ctrl Pts',(66.6907003867572,25.6795383159319,12.));
#113381=CARTESIAN_POINT('Ctrl Pts',(66.6730700479837,25.6648418126013,12.));
#113382=CARTESIAN_POINT('Ctrl Pts',(66.6554595523624,25.6501916559055,12.));
#113383=CARTESIAN_POINT('Ctrl Pts',(66.6378690459129,25.6355878798614,12.));
#113384=CARTESIAN_POINT('Ctrl Pts',(66.6202986753506,25.6210305185403,12.));
#113385=CARTESIAN_POINT('Ctrl Pts',(66.6027485880963,25.6065196060756,12.));
#113386=CARTESIAN_POINT('Ctrl Pts',(66.5852189322813,25.5920551766629,12.));
#113387=CARTESIAN_POINT('Ctrl Pts',(66.5677098567542,25.5776372645601,12.));
#113388=CARTESIAN_POINT('Ctrl Pts',(66.5502215110829,25.5632659040792,12.));
#113389=CARTESIAN_POINT('Ctrl Pts',(66.5327540455624,25.5489411295912,12.));
#113390=CARTESIAN_POINT('Ctrl Pts',(66.5153076112231,25.534662975532,12.));
#113391=CARTESIAN_POINT('Ctrl Pts',(66.4978823598354,25.5204314764033,12.));
#113392=CARTESIAN_POINT('Ctrl Pts',(66.4804784439148,25.5062466667702,12.));
#113393=CARTESIAN_POINT('Ctrl Pts',(66.4630960167252,25.4921085812548,12.));
#113394=CARTESIAN_POINT('Ctrl Pts',(66.4457352322871,25.4780172545417,12.));
#113395=CARTESIAN_POINT('Ctrl Pts',(66.4283962453899,25.4639727213849,12.));
#113396=CARTESIAN_POINT('Ctrl Pts',(66.4110792116,25.4499750166079,12.));
#113397=CARTESIAN_POINT('Ctrl Pts',(66.3937842872685,25.4360241751018,12.));
#113398=CARTESIAN_POINT('Ctrl Pts',(66.3765116295364,25.4221202318199,12.));
#113399=CARTESIAN_POINT('Ctrl Pts',(66.359261396341,25.4082632217847,12.));
#113400=CARTESIAN_POINT('Ctrl Pts',(66.3420337464178,25.3944531800901,12.));
#113401=CARTESIAN_POINT('Ctrl Pts',(66.3248288393046,25.3806901419012,12.));
#113402=CARTESIAN_POINT('Ctrl Pts',(66.3076468353412,25.3669741424488,12.));
#113403=CARTESIAN_POINT('Ctrl Pts',(66.290487895671,25.3533052170249,12.));
#113404=CARTESIAN_POINT('Ctrl Pts',(66.2733521822662,25.3396834009949,12.));
#113405=CARTESIAN_POINT('Ctrl Pts',(66.2562398579471,25.3261087298026,12.));
#113406=CARTESIAN_POINT('Ctrl Pts',(66.2391510863998,25.312581238973,12.));
#113407=CARTESIAN_POINT('Ctrl Pts',(66.2220860321952,25.2991009641094,12.));
#113408=CARTESIAN_POINT('Ctrl Pts',(66.2050448607911,25.285667940893,12.));
#113409=CARTESIAN_POINT('Ctrl Pts',(66.1880277385136,25.2722822050837,12.));
#113410=CARTESIAN_POINT('Ctrl Pts',(66.1710348325384,25.2589437925147,12.));
#113411=CARTESIAN_POINT('Ctrl Pts',(66.1540663108754,25.2456527390875,12.));
#113412=CARTESIAN_POINT('Ctrl Pts',(66.1371223423345,25.232409080755,12.));
#113413=CARTESIAN_POINT('Ctrl Pts',(66.1202030965758,25.2192128535357,12.));
#113414=CARTESIAN_POINT('Ctrl Pts',(66.10330874419,25.2060640935365,12.));
#113415=CARTESIAN_POINT('Ctrl Pts',(66.086439456768,25.1929628369685,12.));
#113416=CARTESIAN_POINT('Ctrl Pts',(66.0695954069713,25.1799091201599,12.));
#113417=CARTESIAN_POINT('Ctrl Pts',(66.0527767686025,25.1669029795661,12.));
#113418=CARTESIAN_POINT('Ctrl Pts',(66.0359837164734,25.1539444517419,12.));
#113419=CARTESIAN_POINT('Ctrl Pts',(66.0192164262621,25.1410335733099,12.));
#113420=CARTESIAN_POINT('Ctrl Pts',(66.0024750743897,25.1281703809297,12.));
#113421=CARTESIAN_POINT('Ctrl Pts',(65.9857598378433,25.1153549112503,12.));
#113422=CARTESIAN_POINT('Ctrl Pts',(65.9690708941558,25.1025872009004,12.));
#113423=CARTESIAN_POINT('Ctrl Pts',(65.9524084218139,25.0898672865915,12.));
#113424=CARTESIAN_POINT('Ctrl Pts',(65.9357726006163,25.0771952052028,12.));
#113425=CARTESIAN_POINT('Ctrl Pts',(65.919163611981,25.0645709938524,12.));
#113426=CARTESIAN_POINT('Ctrl Pts',(65.9025816394424,25.0519946900078,12.));
#113427=CARTESIAN_POINT('Ctrl Pts',(65.8860268683128,25.0394663314055,12.));
#113428=CARTESIAN_POINT('Ctrl Pts',(65.8694994847616,25.0269859558363,12.));
#113429=CARTESIAN_POINT('Ctrl Pts',(65.8529996750445,25.0145536009604,12.));
#113430=CARTESIAN_POINT('Ctrl Pts',(65.8365276247128,25.002169304117,12.));
#113431=CARTESIAN_POINT('Ctrl Pts',(65.8200835177024,24.9898331020983,12.));
#113432=CARTESIAN_POINT('Ctrl Pts',(65.8036675380718,24.9775450315683,12.));
#113433=CARTESIAN_POINT('Ctrl Pts',(65.7872798720823,24.9653051295581,12.));
#113434=CARTESIAN_POINT('Ctrl Pts',(65.7709207098959,24.9531134338696,12.));
#113435=CARTESIAN_POINT('Ctrl Pts',(65.7545902480323,24.9409699836537,12.));
#113436=CARTESIAN_POINT('Ctrl Pts',(65.7382886895888,24.928874819458,12.));
#113437=CARTESIAN_POINT('Ctrl Pts',(65.7220162391053,24.9168279820106,12.));
#113438=CARTESIAN_POINT('Ctrl Pts',(65.7057730980483,24.9048295111448,12.));
#113439=CARTESIAN_POINT('Ctrl Pts',(65.6895594608775,24.8928794448607,12.));
#113440=CARTESIAN_POINT('Ctrl Pts',(65.6733755087669,24.8809778178229,12.));
#113441=CARTESIAN_POINT('Ctrl Pts',(65.6572214156692,24.8691246628057,12.));
#113442=CARTESIAN_POINT('Ctrl Pts',(65.6410973603661,24.8573200135666,12.));
#113443=CARTESIAN_POINT('Ctrl Pts',(65.6250035361612,24.8455639071517,12.));
#113444=CARTESIAN_POINT('Ctrl Pts',(65.6089401625628,24.8338563866764,12.));
#113445=CARTESIAN_POINT('Ctrl Pts',(65.5929074932624,24.8221975032104,12.));
#113446=CARTESIAN_POINT('Ctrl Pts',(65.5769057914333,24.8105873098626,12.));
#113447=CARTESIAN_POINT('Ctrl Pts',(65.5609353062829,24.799025856126,12.));
#113448=CARTESIAN_POINT('Ctrl Pts',(65.5449962514661,24.7875131827491,12.));
#113449=CARTESIAN_POINT('Ctrl Pts',(65.5290887770232,24.7760493148465,12.));
#113450=CARTESIAN_POINT('Ctrl Pts',(65.5132129675333,24.7646342620841,12.));
#113451=CARTESIAN_POINT('Ctrl Pts',(65.5005376841101,24.7555412724651,12.));
#113452=CARTESIAN_POINT('Ctrl Pts',(65.4910454936254,24.7487434955982,12.));
#113453=CARTESIAN_POINT('Ctrl Pts',(65.4847237095443,24.7442214063382,12.));
#113454=CARTESIAN_POINT('Ctrl Pts',(65.4815644032299,24.7419628022042,12.));
#113455=CARTESIAN_POINT('Ctrl Pts',(68.2622612910177,29.0944526440266,0.));
#113456=CARTESIAN_POINT('Ctrl Pts',(68.2622612910177,29.0944526440266,4.));
#113457=CARTESIAN_POINT('Ctrl Pts',(68.2622612910177,29.0944526440266,8.));
#113458=CARTESIAN_POINT('Ctrl Pts',(68.2622612910177,29.0944526440266,12.));
#113459=CARTESIAN_POINT('Ctrl Pts',(68.3721211369508,29.0922231502663,0.));
#113460=CARTESIAN_POINT('Ctrl Pts',(68.3721211369508,29.0922231502663,4.));
#113461=CARTESIAN_POINT('Ctrl Pts',(68.3721211369509,29.0922231502664,8.00000000000001));
#113462=CARTESIAN_POINT('Ctrl Pts',(68.3721211369509,29.0922231502664,12.));
#113463=CARTESIAN_POINT('Ctrl Pts',(68.5624216146675,29.0225207419381,0.));
#113464=CARTESIAN_POINT('Ctrl Pts',(68.5624216146675,29.0225207419381,4.00000000000001));
#113465=CARTESIAN_POINT('Ctrl Pts',(68.5624216146676,29.0225207419382,7.99999999999999));
#113466=CARTESIAN_POINT('Ctrl Pts',(68.5624216146676,29.0225207419382,12.));
#113467=CARTESIAN_POINT('Ctrl Pts',(68.6814343344131,28.8637726134455,0.));
#113468=CARTESIAN_POINT('Ctrl Pts',(68.6814343344131,28.8637726134455,3.99999999999999));
#113469=CARTESIAN_POINT('Ctrl Pts',(68.6814343344132,28.8637726134455,8.00000000000001));
#113470=CARTESIAN_POINT('Ctrl Pts',(68.6814343344132,28.8637726134455,12.));
#113471=CARTESIAN_POINT('Ctrl Pts',(68.7132793373318,28.7877620302417,0.));
#113472=CARTESIAN_POINT('Ctrl Pts',(68.7132793373318,28.7877620302417,4.));
#113473=CARTESIAN_POINT('Ctrl Pts',(68.7132793373319,28.7877620302417,8.));
#113474=CARTESIAN_POINT('Ctrl Pts',(68.7132793373319,28.7877620302417,12.));
#113475=CARTESIAN_POINT('',(68.2622612910177,29.0944526440266,0.));
#113476=CARTESIAN_POINT('',(68.7132793373317,28.7877620302417,0.));
#113477=CARTESIAN_POINT('Ctrl Pts',(68.2622612910177,29.0944526440266,0.));
#113478=CARTESIAN_POINT('Ctrl Pts',(68.3721211369508,29.0922231502663,0.));
#113479=CARTESIAN_POINT('Ctrl Pts',(68.4808642670747,29.0523932026502,0.));
#113480=CARTESIAN_POINT('Ctrl Pts',(68.5663297619426,28.983487101511,0.));
#113481=CARTESIAN_POINT('Ctrl Pts',(68.6304288830936,28.9318075256566,0.));
#113482=CARTESIAN_POINT('Ctrl Pts',(68.6814343344131,28.8637726134455,0.));
#113483=CARTESIAN_POINT('Ctrl Pts',(68.7132793373318,28.7877620302417,0.));
#113484=CARTESIAN_POINT('',(68.7132793373317,28.7877620302417,12.));
#113485=CARTESIAN_POINT('Ctrl Pts',(68.7132793373318,28.7877620302417,0.));
#113486=CARTESIAN_POINT('Ctrl Pts',(68.7132793373318,28.7877620302417,4.));
#113487=CARTESIAN_POINT('Ctrl Pts',(68.7132793373319,28.7877620302417,8.));
#113488=CARTESIAN_POINT('Ctrl Pts',(68.7132793373319,28.7877620302417,12.));
#113489=CARTESIAN_POINT('',(68.2622612910177,29.0944526440266,12.));
#113490=CARTESIAN_POINT('Ctrl Pts',(68.7132793373319,28.7877620302417,12.));
#113491=CARTESIAN_POINT('Ctrl Pts',(68.6814343344132,28.8637726134455,12.));
#113492=CARTESIAN_POINT('Ctrl Pts',(68.6304288830936,28.9318075256567,12.));
#113493=CARTESIAN_POINT('Ctrl Pts',(68.5663297619426,28.9834871015111,12.));
#113494=CARTESIAN_POINT('Ctrl Pts',(68.4808642670747,29.0523932026503,12.));
#113495=CARTESIAN_POINT('Ctrl Pts',(68.3721211369509,29.0922231502664,12.));
#113496=CARTESIAN_POINT('Ctrl Pts',(68.2622612910177,29.0944526440266,12.));
#113497=CARTESIAN_POINT('Ctrl Pts',(68.2622612910177,29.0944526440266,12.));
#113498=CARTESIAN_POINT('Ctrl Pts',(68.2622612910177,29.0944526440266,8.));
#113499=CARTESIAN_POINT('Ctrl Pts',(68.2622612910177,29.0944526440266,4.));
#113500=CARTESIAN_POINT('Ctrl Pts',(68.2622612910177,29.0944526440266,0.));
#113501=CARTESIAN_POINT('Origin',(3.46272497684358E-10,1.43538201480493E-10,
0.));
#113502=CARTESIAN_POINT('Origin',(3.46272497684358E-10,1.43538201480493E-10,
12.));
#113503=CARTESIAN_POINT('Origin',(3.46272497684358E-10,1.43538201480493E-10,
0.));
#113504=CARTESIAN_POINT('Ctrl Pts',(71.1418425484881,22.1153394458717,0.));
#113505=CARTESIAN_POINT('Ctrl Pts',(71.1418425484881,22.1153394458717,4.));
#113506=CARTESIAN_POINT('Ctrl Pts',(71.1418425484881,22.1153394458717,8.));
#113507=CARTESIAN_POINT('Ctrl Pts',(71.1418425484881,22.1153394458717,12.));
#113508=CARTESIAN_POINT('Ctrl Pts',(71.1744611799059,22.0104100349462,0.));
#113509=CARTESIAN_POINT('Ctrl Pts',(71.1744611799059,22.0104100349462,4.));
#113510=CARTESIAN_POINT('Ctrl Pts',(71.1744611799059,22.0104100349462,8.));
#113511=CARTESIAN_POINT('Ctrl Pts',(71.1744611799059,22.0104100349462,12.));
#113512=CARTESIAN_POINT('Ctrl Pts',(71.1685011351939,21.8078334561031,0.));
#113513=CARTESIAN_POINT('Ctrl Pts',(71.1685011351939,21.8078334561031,4.));
#113514=CARTESIAN_POINT('Ctrl Pts',(71.168501135194,21.8078334561031,8.));
#113515=CARTESIAN_POINT('Ctrl Pts',(71.168501135194,21.8078334561031,12.));
#113516=CARTESIAN_POINT('Ctrl Pts',(71.0555229320375,21.6447353227844,0.));
#113517=CARTESIAN_POINT('Ctrl Pts',(71.0555229320375,21.6447353227844,4.));
#113518=CARTESIAN_POINT('Ctrl Pts',(71.0555229320376,21.6447353227844,8.00000000000001));
#113519=CARTESIAN_POINT('Ctrl Pts',(71.0555229320376,21.6447353227844,12.));
#113520=CARTESIAN_POINT('Ctrl Pts',(70.9934796068774,21.5904919934804,0.));
#113521=CARTESIAN_POINT('Ctrl Pts',(70.9934796068774,21.5904919934804,4.));
#113522=CARTESIAN_POINT('Ctrl Pts',(70.9934796068774,21.5904919934804,8.));
#113523=CARTESIAN_POINT('Ctrl Pts',(70.9934796068774,21.5904919934804,12.));
#113524=CARTESIAN_POINT('',(71.1418425484881,22.1153394458717,0.));
#113525=CARTESIAN_POINT('',(70.9934796068777,21.59049199348,0.));
#113526=CARTESIAN_POINT('Ctrl Pts',(71.1418425484881,22.1153394458717,0.));
#113527=CARTESIAN_POINT('Ctrl Pts',(71.1744611799059,22.0104100349462,0.));
#113528=CARTESIAN_POINT('Ctrl Pts',(71.1710554400705,21.894651989893,0.));
#113529=CARTESIAN_POINT('Ctrl Pts',(71.1327049954369,21.7917848658274,0.));
#113530=CARTESIAN_POINT('Ctrl Pts',(71.1039421619617,21.7146345227781,0.));
#113531=CARTESIAN_POINT('Ctrl Pts',(71.0555229320375,21.6447353227844,0.));
#113532=CARTESIAN_POINT('Ctrl Pts',(70.9934796068774,21.5904919934804,0.));
#113533=CARTESIAN_POINT('',(70.9934796068777,21.5904919934801,12.));
#113534=CARTESIAN_POINT('Ctrl Pts',(70.9934796068774,21.5904919934804,0.));
#113535=CARTESIAN_POINT('Ctrl Pts',(70.9934796068774,21.5904919934804,4.));
#113536=CARTESIAN_POINT('Ctrl Pts',(70.9934796068774,21.5904919934804,8.));
#113537=CARTESIAN_POINT('Ctrl Pts',(70.9934796068774,21.5904919934804,12.));
#113538=CARTESIAN_POINT('',(71.1418425484881,22.1153394458717,12.));
#113539=CARTESIAN_POINT('Ctrl Pts',(70.9934796068774,21.5904919934804,12.));
#113540=CARTESIAN_POINT('Ctrl Pts',(71.0555229320376,21.6447353227844,12.));
#113541=CARTESIAN_POINT('Ctrl Pts',(71.1039421619617,21.7146345227781,12.));
#113542=CARTESIAN_POINT('Ctrl Pts',(71.1327049954369,21.7917848658274,12.));
#113543=CARTESIAN_POINT('Ctrl Pts',(71.1710554400705,21.894651989893,12.));
#113544=CARTESIAN_POINT('Ctrl Pts',(71.1744611799059,22.0104100349462,12.));
#113545=CARTESIAN_POINT('Ctrl Pts',(71.1418425484881,22.1153394458717,12.));
#113546=CARTESIAN_POINT('Ctrl Pts',(71.1418425484881,22.1153394458717,12.));
#113547=CARTESIAN_POINT('Ctrl Pts',(71.1418425484881,22.1153394458717,8.));
#113548=CARTESIAN_POINT('Ctrl Pts',(71.1418425484881,22.1153394458717,4.));
#113549=CARTESIAN_POINT('Ctrl Pts',(71.1418425484881,22.1153394458717,0.));
#113550=CARTESIAN_POINT('Ctrl Pts',(67.3887914263118,18.9407177820969,0.));
#113551=CARTESIAN_POINT('Ctrl Pts',(67.3887914263118,18.9407177820969,12.));
#113552=CARTESIAN_POINT('Ctrl Pts',(67.3921355608328,18.9426924398719,0.));
#113553=CARTESIAN_POINT('Ctrl Pts',(67.3921355608328,18.9426924398719,12.));
#113554=CARTESIAN_POINT('Ctrl Pts',(67.3988274146651,18.9466463414299,0.));
#113555=CARTESIAN_POINT('Ctrl Pts',(67.3988274146651,18.9466463414299,12.));
#113556=CARTESIAN_POINT('Ctrl Pts',(67.4088759497911,18.9525909517915,0.));
#113557=CARTESIAN_POINT('Ctrl Pts',(67.4088759497911,18.9525909517915,12.));
#113558=CARTESIAN_POINT('Ctrl Pts',(67.4222955061981,18.9605446160985,0.));
#113559=CARTESIAN_POINT('Ctrl Pts',(67.4222955061981,18.9605446160985,12.));
#113560=CARTESIAN_POINT('Ctrl Pts',(67.4391057908418,18.9705325631711,0.));
#113561=CARTESIAN_POINT('Ctrl Pts',(67.4391057908418,18.9705325631711,12.));
#113562=CARTESIAN_POINT('Ctrl Pts',(67.4559518744638,18.9805663798449,0.));
#113563=CARTESIAN_POINT('Ctrl Pts',(67.4559518744638,18.9805663798449,12.));
#113564=CARTESIAN_POINT('Ctrl Pts',(67.472833671964,18.9906460638625,0.));
#113565=CARTESIAN_POINT('Ctrl Pts',(67.472833671964,18.9906460638625,12.));
#113566=CARTESIAN_POINT('Ctrl Pts',(67.4897510316844,19.0007716032819,0.));
#113567=CARTESIAN_POINT('Ctrl Pts',(67.4897510316844,19.0007716032819,12.));
#113568=CARTESIAN_POINT('Ctrl Pts',(67.5067037372317,19.0109429761306,0.));
#113569=CARTESIAN_POINT('Ctrl Pts',(67.5067037372317,19.0109429761306,12.));
#113570=CARTESIAN_POINT('Ctrl Pts',(67.5236915360331,19.021160154824,0.));
#113571=CARTESIAN_POINT('Ctrl Pts',(67.5236915360331,19.021160154824,12.));
#113572=CARTESIAN_POINT('Ctrl Pts',(67.540714161288,19.0314231093923,0.));
#113573=CARTESIAN_POINT('Ctrl Pts',(67.540714161288,19.0314231093923,12.));
#113574=CARTESIAN_POINT('Ctrl Pts',(67.5577713558194,19.0417318110708,0.));
#113575=CARTESIAN_POINT('Ctrl Pts',(67.5577713558194,19.0417318110708,12.));
#113576=CARTESIAN_POINT('Ctrl Pts',(67.5748628971964,19.0520862360396,0.));
#113577=CARTESIAN_POINT('Ctrl Pts',(67.5748628971964,19.0520862360396,12.));
#113578=CARTESIAN_POINT('Ctrl Pts',(67.5919885896222,19.062486364241,0.));
#113579=CARTESIAN_POINT('Ctrl Pts',(67.5919885896222,19.062486364241,12.));
#113580=CARTESIAN_POINT('Ctrl Pts',(67.6091482520534,19.072932177628,0.));
#113581=CARTESIAN_POINT('Ctrl Pts',(67.6091482520534,19.072932177628,12.));
#113582=CARTESIAN_POINT('Ctrl Pts',(67.6263417083426,19.0834236587118,0.));
#113583=CARTESIAN_POINT('Ctrl Pts',(67.6263417083426,19.0834236587118,12.));
#113584=CARTESIAN_POINT('Ctrl Pts',(67.6435687749841,19.0939607887502,0.));
#113585=CARTESIAN_POINT('Ctrl Pts',(67.6435687749841,19.0939607887502,12.));
#113586=CARTESIAN_POINT('Ctrl Pts',(67.6608292549462,19.1045435468358,0.));
#113587=CARTESIAN_POINT('Ctrl Pts',(67.6608292549462,19.1045435468358,12.));
#113588=CARTESIAN_POINT('Ctrl Pts',(67.6781229440573,19.115171910846,0.));
#113589=CARTESIAN_POINT('Ctrl Pts',(67.6781229440573,19.115171910846,12.));
#113590=CARTESIAN_POINT('Ctrl Pts',(67.6954496350063,19.1258458580345,0.));
#113591=CARTESIAN_POINT('Ctrl Pts',(67.6954496350063,19.1258458580345,12.));
#113592=CARTESIAN_POINT('Ctrl Pts',(67.7128091219348,19.136565365709,0.));
#113593=CARTESIAN_POINT('Ctrl Pts',(67.7128091219348,19.136565365709,12.));
#113594=CARTESIAN_POINT('Ctrl Pts',(67.7302012056584,19.1473304119955,0.));
#113595=CARTESIAN_POINT('Ctrl Pts',(67.7302012056584,19.1473304119955,12.));
#113596=CARTESIAN_POINT('Ctrl Pts',(67.7476256934444,19.1581409758097,0.));
#113597=CARTESIAN_POINT('Ctrl Pts',(67.7476256934444,19.1581409758097,12.));
#113598=CARTESIAN_POINT('Ctrl Pts',(67.7650823965127,19.168997036495,0.));
#113599=CARTESIAN_POINT('Ctrl Pts',(67.7650823965127,19.168997036495,12.));
#113600=CARTESIAN_POINT('Ctrl Pts',(67.7825711283096,19.1798985735688,0.));
#113601=CARTESIAN_POINT('Ctrl Pts',(67.7825711283096,19.1798985735688,12.));
#113602=CARTESIAN_POINT('Ctrl Pts',(67.8000917023926,19.1908455664098,0.));
#113603=CARTESIAN_POINT('Ctrl Pts',(67.8000917023926,19.1908455664098,12.));
#113604=CARTESIAN_POINT('Ctrl Pts',(67.8176439306621,19.201837993993,0.));
#113605=CARTESIAN_POINT('Ctrl Pts',(67.8176439306621,19.201837993993,12.));
#113606=CARTESIAN_POINT('Ctrl Pts',(67.835227624289,19.2128758350346,0.));
#113607=CARTESIAN_POINT('Ctrl Pts',(67.835227624289,19.2128758350346,12.));
#113608=CARTESIAN_POINT('Ctrl Pts',(67.8528425945184,19.2239590681133,0.));
#113609=CARTESIAN_POINT('Ctrl Pts',(67.8528425945184,19.2239590681133,12.));
#113610=CARTESIAN_POINT('Ctrl Pts',(67.8704886534544,19.2350876717874,0.));
#113611=CARTESIAN_POINT('Ctrl Pts',(67.8704886534544,19.2350876717874,12.));
#113612=CARTESIAN_POINT('Ctrl Pts',(67.8881656149955,19.2462616247279,0.));
#113613=CARTESIAN_POINT('Ctrl Pts',(67.8881656149955,19.2462616247279,12.));
#113614=CARTESIAN_POINT('Ctrl Pts',(67.9058732951788,19.2574809057696,0.));
#113615=CARTESIAN_POINT('Ctrl Pts',(67.9058732951788,19.2574809057696,12.));
#113616=CARTESIAN_POINT('Ctrl Pts',(67.9236115116758,19.2687454938442,0.));
#113617=CARTESIAN_POINT('Ctrl Pts',(67.9236115116758,19.2687454938442,12.));
#113618=CARTESIAN_POINT('Ctrl Pts',(67.9413800834793,19.280055367936,0.));
#113619=CARTESIAN_POINT('Ctrl Pts',(67.9413800834793,19.280055367936,12.));
#113620=CARTESIAN_POINT('Ctrl Pts',(67.9591788305394,19.2914105070286,0.));
#113621=CARTESIAN_POINT('Ctrl Pts',(67.9591788305394,19.2914105070286,12.));
#113622=CARTESIAN_POINT('Ctrl Pts',(67.9770075733485,19.302810890038,0.));
#113623=CARTESIAN_POINT('Ctrl Pts',(67.9770075733485,19.302810890038,12.));
#113624=CARTESIAN_POINT('Ctrl Pts',(67.9948661329617,19.3142564958203,0.));
#113625=CARTESIAN_POINT('Ctrl Pts',(67.9948661329617,19.3142564958203,12.));
#113626=CARTESIAN_POINT('Ctrl Pts',(68.0127543311776,19.3257473032035,0.));
#113627=CARTESIAN_POINT('Ctrl Pts',(68.0127543311776,19.3257473032035,12.));
#113628=CARTESIAN_POINT('Ctrl Pts',(68.0306719906636,19.3372832910076,0.));
#113629=CARTESIAN_POINT('Ctrl Pts',(68.0306719906636,19.3372832910076,12.));
#113630=CARTESIAN_POINT('Ctrl Pts',(68.0486189351011,19.3488644380641,0.));
#113631=CARTESIAN_POINT('Ctrl Pts',(68.0486189351011,19.3488644380641,12.));
#113632=CARTESIAN_POINT('Ctrl Pts',(68.0665949893195,19.3604907232314,0.));
#113633=CARTESIAN_POINT('Ctrl Pts',(68.0665949893195,19.3604907232314,12.));
#113634=CARTESIAN_POINT('Ctrl Pts',(68.0845999792247,19.3721621253912,0.));
#113635=CARTESIAN_POINT('Ctrl Pts',(68.0845999792247,19.3721621253912,12.));
#113636=CARTESIAN_POINT('Ctrl Pts',(68.1026337317285,19.3838786234421,0.));
#113637=CARTESIAN_POINT('Ctrl Pts',(68.1026337317285,19.3838786234421,12.));
#113638=CARTESIAN_POINT('Ctrl Pts',(68.1206960746769,19.3956401962895,0.));
#113639=CARTESIAN_POINT('Ctrl Pts',(68.1206960746769,19.3956401962895,12.));
#113640=CARTESIAN_POINT('Ctrl Pts',(68.1387868367691,19.40744682283,0.));
#113641=CARTESIAN_POINT('Ctrl Pts',(68.1387868367691,19.40744682283,12.));
#113642=CARTESIAN_POINT('Ctrl Pts',(68.1569058475054,19.4192984819418,0.));
#113643=CARTESIAN_POINT('Ctrl Pts',(68.1569058475054,19.4192984819418,12.));
#113644=CARTESIAN_POINT('Ctrl Pts',(68.1750529372232,19.4311951524983,0.));
#113645=CARTESIAN_POINT('Ctrl Pts',(68.1750529372232,19.4311951524983,12.));
#113646=CARTESIAN_POINT('Ctrl Pts',(68.1932279371127,19.4431368133719,0.));
#113647=CARTESIAN_POINT('Ctrl Pts',(68.1932279371127,19.4431368133719,12.));
#113648=CARTESIAN_POINT('Ctrl Pts',(68.2114306792358,19.4551234434381,0.));
#113649=CARTESIAN_POINT('Ctrl Pts',(68.2114306792358,19.4551234434381,12.));
#113650=CARTESIAN_POINT('Ctrl Pts',(68.2296609965448,19.467155021572,0.));
#113651=CARTESIAN_POINT('Ctrl Pts',(68.2296609965448,19.467155021572,12.));
#113652=CARTESIAN_POINT('Ctrl Pts',(68.2479187228803,19.4792315266501,0.));
#113653=CARTESIAN_POINT('Ctrl Pts',(68.2479187228803,19.4792315266501,12.));
#113654=CARTESIAN_POINT('Ctrl Pts',(68.2662036929526,19.4913529375543,0.));
#113655=CARTESIAN_POINT('Ctrl Pts',(68.2662036929526,19.4913529375543,12.));
#113656=CARTESIAN_POINT('Ctrl Pts',(68.2845157423233,19.5035192331705,0.));
#113657=CARTESIAN_POINT('Ctrl Pts',(68.2845157423233,19.5035192331705,12.));
#113658=CARTESIAN_POINT('Ctrl Pts',(68.3028547073864,19.5157303923856,0.));
#113659=CARTESIAN_POINT('Ctrl Pts',(68.3028547073864,19.5157303923856,12.));
#113660=CARTESIAN_POINT('Ctrl Pts',(68.3212204253417,19.5279863940773,0.));
#113661=CARTESIAN_POINT('Ctrl Pts',(68.3212204253417,19.5279863940773,12.));
#113662=CARTESIAN_POINT('Ctrl Pts',(68.3396127341938,19.5402872171191,0.));
#113663=CARTESIAN_POINT('Ctrl Pts',(68.3396127341938,19.5402872171191,12.));
#113664=CARTESIAN_POINT('Ctrl Pts',(68.3580314727523,19.5526328403852,0.));
#113665=CARTESIAN_POINT('Ctrl Pts',(68.3580314727523,19.5526328403852,12.));
#113666=CARTESIAN_POINT('Ctrl Pts',(68.3764764806287,19.5650232427516,0.));
#113667=CARTESIAN_POINT('Ctrl Pts',(68.3764764806287,19.5650232427516,12.));
#113668=CARTESIAN_POINT('Ctrl Pts',(68.3949475982335,19.5774584030938,0.));
#113669=CARTESIAN_POINT('Ctrl Pts',(68.3949475982335,19.5774584030938,12.));
#113670=CARTESIAN_POINT('Ctrl Pts',(68.4134446667696,19.5899383002803,0.));
#113671=CARTESIAN_POINT('Ctrl Pts',(68.4134446667696,19.5899383002803,12.));
#113672=CARTESIAN_POINT('Ctrl Pts',(68.4319675282275,19.6024629131785,0.));
#113673=CARTESIAN_POINT('Ctrl Pts',(68.4319675282275,19.6024629131785,12.));
#113674=CARTESIAN_POINT('Ctrl Pts',(68.4505160253778,19.6150322206577,0.));
#113675=CARTESIAN_POINT('Ctrl Pts',(68.4505160253778,19.6150322206577,12.));
#113676=CARTESIAN_POINT('Ctrl Pts',(68.4690900017632,19.6276462015888,0.));
#113677=CARTESIAN_POINT('Ctrl Pts',(68.4690900017632,19.6276462015888,12.));
#113678=CARTESIAN_POINT('Ctrl Pts',(68.4876893016856,19.6403048348395,0.));
#113679=CARTESIAN_POINT('Ctrl Pts',(68.4876893016856,19.6403048348395,12.));
#113680=CARTESIAN_POINT('Ctrl Pts',(68.5063137701971,19.6530080992686,0.));
#113681=CARTESIAN_POINT('Ctrl Pts',(68.5063137701971,19.6530080992686,12.));
#113682=CARTESIAN_POINT('Ctrl Pts',(68.5249632530979,19.6657559737336,0.));
#113683=CARTESIAN_POINT('Ctrl Pts',(68.5249632530979,19.6657559737336,12.));
#113684=CARTESIAN_POINT('Ctrl Pts',(68.5436375969311,19.6785484370927,0.));
#113685=CARTESIAN_POINT('Ctrl Pts',(68.5436375969311,19.6785484370927,12.));
#113686=CARTESIAN_POINT('Ctrl Pts',(68.5623366489779,19.6913854682046,0.));
#113687=CARTESIAN_POINT('Ctrl Pts',(68.5623366489779,19.6913854682046,12.));
#113688=CARTESIAN_POINT('Ctrl Pts',(68.581060257249,19.7042670459237,0.));
#113689=CARTESIAN_POINT('Ctrl Pts',(68.581060257249,19.7042670459237,12.));
#113690=CARTESIAN_POINT('Ctrl Pts',(68.5998082704766,19.7171931490956,0.));
#113691=CARTESIAN_POINT('Ctrl Pts',(68.5998082704766,19.7171931490956,12.));
#113692=CARTESIAN_POINT('Ctrl Pts',(68.6185805381126,19.7301637565652,0.));
#113693=CARTESIAN_POINT('Ctrl Pts',(68.6185805381126,19.7301637565652,12.));
#113694=CARTESIAN_POINT('Ctrl Pts',(68.6373769103224,19.7431788471776,0.));
#113695=CARTESIAN_POINT('Ctrl Pts',(68.6373769103224,19.7431788471776,12.));
#113696=CARTESIAN_POINT('Ctrl Pts',(68.6561972379793,19.7562383997781,0.));
#113697=CARTESIAN_POINT('Ctrl Pts',(68.6561972379793,19.7562383997781,12.));
#113698=CARTESIAN_POINT('Ctrl Pts',(68.6750413726547,19.7693423932058,0.));
#113699=CARTESIAN_POINT('Ctrl Pts',(68.6750413726547,19.7693423932058,12.));
#113700=CARTESIAN_POINT('Ctrl Pts',(68.6939091666111,19.7824908062913,0.));
#113701=CARTESIAN_POINT('Ctrl Pts',(68.6939091666111,19.7824908062913,12.));
#113702=CARTESIAN_POINT('Ctrl Pts',(68.7128004727998,19.795683617864,0.));
#113703=CARTESIAN_POINT('Ctrl Pts',(68.7128004727998,19.795683617864,12.));
#113704=CARTESIAN_POINT('Ctrl Pts',(68.7317151448557,19.8089208067532,0.));
#113705=CARTESIAN_POINT('Ctrl Pts',(68.7317151448557,19.8089208067532,12.));
#113706=CARTESIAN_POINT('Ctrl Pts',(68.7506530370918,19.8222023517874,0.));
#113707=CARTESIAN_POINT('Ctrl Pts',(68.7506530370918,19.8222023517874,12.));
#113708=CARTESIAN_POINT('Ctrl Pts',(68.7696140044892,19.835528231787,0.));
#113709=CARTESIAN_POINT('Ctrl Pts',(68.7696140044892,19.835528231787,12.));
#113710=CARTESIAN_POINT('Ctrl Pts',(68.7885979026927,19.8488984255641,0.));
#113711=CARTESIAN_POINT('Ctrl Pts',(68.7885979026927,19.8488984255641,12.));
#113712=CARTESIAN_POINT('Ctrl Pts',(68.8076045880102,19.8623129119304,0.));
#113713=CARTESIAN_POINT('Ctrl Pts',(68.8076045880102,19.8623129119304,12.));
#113714=CARTESIAN_POINT('Ctrl Pts',(68.8266339174068,19.8757716696969,0.));
#113715=CARTESIAN_POINT('Ctrl Pts',(68.8266339174068,19.8757716696969,12.));
#113716=CARTESIAN_POINT('Ctrl Pts',(68.8456857484988,19.8892746776734,0.));
#113717=CARTESIAN_POINT('Ctrl Pts',(68.8456857484988,19.8892746776734,12.));
#113718=CARTESIAN_POINT('Ctrl Pts',(68.8647599395437,19.9028219146607,0.));
#113719=CARTESIAN_POINT('Ctrl Pts',(68.8647599395437,19.9028219146607,12.));
#113720=CARTESIAN_POINT('Ctrl Pts',(68.8838563494356,19.9164133594513,0.));
#113721=CARTESIAN_POINT('Ctrl Pts',(68.8838563494356,19.9164133594513,12.));
#113722=CARTESIAN_POINT('Ctrl Pts',(68.902974837704,19.9300489908364,0.));
#113723=CARTESIAN_POINT('Ctrl Pts',(68.902974837704,19.9300489908364,12.));
#113724=CARTESIAN_POINT('Ctrl Pts',(68.9221152645086,19.9437287876063,0.));
#113725=CARTESIAN_POINT('Ctrl Pts',(68.9221152645086,19.9437287876063,12.));
#113726=CARTESIAN_POINT('Ctrl Pts',(68.9412774906346,19.9574527285492,0.));
#113727=CARTESIAN_POINT('Ctrl Pts',(68.9412774906346,19.9574527285492,12.));
#113728=CARTESIAN_POINT('Ctrl Pts',(68.960461377483,19.9712207924437,0.));
#113729=CARTESIAN_POINT('Ctrl Pts',(68.960461377483,19.9712207924437,12.));
#113730=CARTESIAN_POINT('Ctrl Pts',(68.9796667870667,19.98503295806,0.));
#113731=CARTESIAN_POINT('Ctrl Pts',(68.9796667870667,19.98503295806,12.));
#113732=CARTESIAN_POINT('Ctrl Pts',(68.9988935820101,19.9988892041671,0.));
#113733=CARTESIAN_POINT('Ctrl Pts',(68.9988935820101,19.9988892041671,12.));
#113734=CARTESIAN_POINT('Ctrl Pts',(69.0181416255433,20.0127895095327,0.));
#113735=CARTESIAN_POINT('Ctrl Pts',(69.0181416255433,20.0127895095327,12.));
#113736=CARTESIAN_POINT('Ctrl Pts',(69.0374107814977,20.0267338529221,0.));
#113737=CARTESIAN_POINT('Ctrl Pts',(69.0374107814977,20.0267338529221,12.));
#113738=CARTESIAN_POINT('Ctrl Pts',(69.0567009142968,20.0407222130902,0.));
#113739=CARTESIAN_POINT('Ctrl Pts',(69.0567009142968,20.0407222130902,12.));
#113740=CARTESIAN_POINT('Ctrl Pts',(69.0760118889525,20.0547545687839,0.));
#113741=CARTESIAN_POINT('Ctrl Pts',(69.0760118889525,20.0547545687839,12.));
#113742=CARTESIAN_POINT('Ctrl Pts',(69.0953435710634,20.0688308987478,0.));
#113743=CARTESIAN_POINT('Ctrl Pts',(69.0953435710634,20.0688308987478,12.));
#113744=CARTESIAN_POINT('Ctrl Pts',(69.1146958268104,20.0829511817251,0.));
#113745=CARTESIAN_POINT('Ctrl Pts',(69.1146958268104,20.0829511817251,12.));
#113746=CARTESIAN_POINT('Ctrl Pts',(69.1340685229516,20.0971153964557,0.));
#113747=CARTESIAN_POINT('Ctrl Pts',(69.1340685229516,20.0971153964557,12.));
#113748=CARTESIAN_POINT('Ctrl Pts',(69.1534615268153,20.1113235216694,0.));
#113749=CARTESIAN_POINT('Ctrl Pts',(69.1534615268153,20.1113235216694,12.));
#113750=CARTESIAN_POINT('Ctrl Pts',(69.172874706296,20.1255755360871,0.));
#113751=CARTESIAN_POINT('Ctrl Pts',(69.172874706296,20.1255755360871,12.));
#113752=CARTESIAN_POINT('Ctrl Pts',(69.1923079298534,20.1398714184278,0.));
#113753=CARTESIAN_POINT('Ctrl Pts',(69.1923079298534,20.1398714184278,12.));
#113754=CARTESIAN_POINT('Ctrl Pts',(69.2117610665073,20.1542111474086,0.));
#113755=CARTESIAN_POINT('Ctrl Pts',(69.2117610665073,20.1542111474086,12.));
#113756=CARTESIAN_POINT('Ctrl Pts',(69.2312339858337,20.1685947017433,0.));
#113757=CARTESIAN_POINT('Ctrl Pts',(69.2312339858337,20.1685947017433,12.));
#113758=CARTESIAN_POINT('Ctrl Pts',(69.2507265579562,20.183022060135,0.));
#113759=CARTESIAN_POINT('Ctrl Pts',(69.2507265579562,20.183022060135,12.));
#113760=CARTESIAN_POINT('Ctrl Pts',(69.2702386535432,20.1974932012775,0.));
#113761=CARTESIAN_POINT('Ctrl Pts',(69.2702386535432,20.1974932012775,12.));
#113762=CARTESIAN_POINT('Ctrl Pts',(69.2897701438066,20.2120081038622,0.));
#113763=CARTESIAN_POINT('Ctrl Pts',(69.2897701438066,20.2120081038622,12.));
#113764=CARTESIAN_POINT('Ctrl Pts',(69.3093209004986,20.2265667465784,0.));
#113765=CARTESIAN_POINT('Ctrl Pts',(69.3093209004986,20.2265667465784,12.));
#113766=CARTESIAN_POINT('Ctrl Pts',(69.3288907959065,20.2411691081122,0.));
#113767=CARTESIAN_POINT('Ctrl Pts',(69.3288907959065,20.2411691081122,12.));
#113768=CARTESIAN_POINT('Ctrl Pts',(69.3484797028454,20.255815167139,0.));
#113769=CARTESIAN_POINT('Ctrl Pts',(69.3484797028454,20.255815167139,12.));
#113770=CARTESIAN_POINT('Ctrl Pts',(69.3680874946548,20.2705049023241,0.));
#113771=CARTESIAN_POINT('Ctrl Pts',(69.3680874946548,20.2705049023241,12.));
#113772=CARTESIAN_POINT('Ctrl Pts',(69.3877140451975,20.2852382923299,0.));
#113773=CARTESIAN_POINT('Ctrl Pts',(69.3877140451975,20.2852382923299,12.));
#113774=CARTESIAN_POINT('Ctrl Pts',(69.4073592288562,20.3000153158167,0.));
#113775=CARTESIAN_POINT('Ctrl Pts',(69.4073592288562,20.3000153158167,12.));
#113776=CARTESIAN_POINT('Ctrl Pts',(69.4270229205296,20.3148359514414,0.));
#113777=CARTESIAN_POINT('Ctrl Pts',(69.4270229205296,20.3148359514414,12.));
#113778=CARTESIAN_POINT('Ctrl Pts',(69.4467049956257,20.3297001778505,0.));
#113779=CARTESIAN_POINT('Ctrl Pts',(69.4467049956257,20.3297001778505,12.));
#113780=CARTESIAN_POINT('Ctrl Pts',(69.4664053300579,20.3446079736799,0.));
#113781=CARTESIAN_POINT('Ctrl Pts',(69.4664053300579,20.3446079736799,12.));
#113782=CARTESIAN_POINT('Ctrl Pts',(69.4861238002433,20.359559317562,0.));
#113783=CARTESIAN_POINT('Ctrl Pts',(69.4861238002433,20.359559317562,12.));
#113784=CARTESIAN_POINT('Ctrl Pts',(69.5058602831004,20.3745541881267,0.));
#113785=CARTESIAN_POINT('Ctrl Pts',(69.5058602831004,20.3745541881267,12.));
#113786=CARTESIAN_POINT('Ctrl Pts',(69.5256146560444,20.3895925640006,0.));
#113787=CARTESIAN_POINT('Ctrl Pts',(69.5256146560444,20.3895925640006,12.));
#113788=CARTESIAN_POINT('Ctrl Pts',(69.5453867969815,20.4046744238002,0.));
#113789=CARTESIAN_POINT('Ctrl Pts',(69.5453867969815,20.4046744238002,12.));
#113790=CARTESIAN_POINT('Ctrl Pts',(69.565176584305,20.4197997461306,0.));
#113791=CARTESIAN_POINT('Ctrl Pts',(69.565176584305,20.4197997461306,12.));
#113792=CARTESIAN_POINT('Ctrl Pts',(69.5849838968944,20.4349685095928,0.));
#113793=CARTESIAN_POINT('Ctrl Pts',(69.5849838968944,20.4349685095928,12.));
#113794=CARTESIAN_POINT('Ctrl Pts',(69.6048086141122,20.4501806927854,0.));
#113795=CARTESIAN_POINT('Ctrl Pts',(69.6048086141122,20.4501806927854,12.));
#113796=CARTESIAN_POINT('Ctrl Pts',(69.6246506158009,20.4654362743036,0.));
#113797=CARTESIAN_POINT('Ctrl Pts',(69.6246506158009,20.4654362743036,12.));
#113798=CARTESIAN_POINT('Ctrl Pts',(69.6445097822778,20.4807352327335,0.));
#113799=CARTESIAN_POINT('Ctrl Pts',(69.6445097822778,20.4807352327335,12.));
#113800=CARTESIAN_POINT('Ctrl Pts',(69.6643859943291,20.4960775466487,0.));
#113801=CARTESIAN_POINT('Ctrl Pts',(69.6643859943291,20.4960775466487,12.));
#113802=CARTESIAN_POINT('Ctrl Pts',(69.6842791332102,20.511463194618,0.));
#113803=CARTESIAN_POINT('Ctrl Pts',(69.6842791332102,20.511463194618,12.));
#113804=CARTESIAN_POINT('Ctrl Pts',(69.7041890806421,20.5268921552076,0.));
#113805=CARTESIAN_POINT('Ctrl Pts',(69.7041890806421,20.5268921552076,12.));
#113806=CARTESIAN_POINT('Ctrl Pts',(69.7241157188086,20.54236440698,0.));
#113807=CARTESIAN_POINT('Ctrl Pts',(69.7241157188086,20.54236440698,12.));
#113808=CARTESIAN_POINT('Ctrl Pts',(69.7440589303511,20.5578799284898,0.));
#113809=CARTESIAN_POINT('Ctrl Pts',(69.7440589303511,20.5578799284898,12.));
#113810=CARTESIAN_POINT('Ctrl Pts',(69.7640185983641,20.5734386982782,0.));
#113811=CARTESIAN_POINT('Ctrl Pts',(69.7640185983641,20.5734386982782,12.));
#113812=CARTESIAN_POINT('Ctrl Pts',(69.7839946063942,20.5890406948809,0.));
#113813=CARTESIAN_POINT('Ctrl Pts',(69.7839946063942,20.5890406948809,12.));
#113814=CARTESIAN_POINT('Ctrl Pts',(69.8039868384382,20.6046858968305,0.));
#113815=CARTESIAN_POINT('Ctrl Pts',(69.8039868384382,20.6046858968305,12.));
#113816=CARTESIAN_POINT('Ctrl Pts',(69.8239951789402,20.6203742826566,0.));
#113817=CARTESIAN_POINT('Ctrl Pts',(69.8239951789402,20.6203742826566,12.));
#113818=CARTESIAN_POINT('Ctrl Pts',(69.8440195127874,20.6361058308812,0.));
#113819=CARTESIAN_POINT('Ctrl Pts',(69.8440195127874,20.6361058308812,12.));
#113820=CARTESIAN_POINT('Ctrl Pts',(69.8640597253058,20.6518805200132,0.));
#113821=CARTESIAN_POINT('Ctrl Pts',(69.8640597253058,20.6518805200132,12.));
#113822=CARTESIAN_POINT('Ctrl Pts',(69.884115702258,20.6676983285542,0.));
#113823=CARTESIAN_POINT('Ctrl Pts',(69.884115702258,20.6676983285542,12.));
#113824=CARTESIAN_POINT('Ctrl Pts',(69.9041873298416,20.6835592350031,0.));
#113825=CARTESIAN_POINT('Ctrl Pts',(69.9041873298416,20.6835592350031,12.));
#113826=CARTESIAN_POINT('Ctrl Pts',(69.9242744946854,20.6994632178551,0.));
#113827=CARTESIAN_POINT('Ctrl Pts',(69.9242744946854,20.6994632178551,12.));
#113828=CARTESIAN_POINT('Ctrl Pts',(69.9443770838444,20.7154102555996,0.));
#113829=CARTESIAN_POINT('Ctrl Pts',(69.9443770838444,20.7154102555996,12.));
#113830=CARTESIAN_POINT('Ctrl Pts',(69.9644949847929,20.7314003267118,0.));
#113831=CARTESIAN_POINT('Ctrl Pts',(69.9644949847929,20.7314003267118,12.));
#113832=CARTESIAN_POINT('Ctrl Pts',(69.9846280854254,20.7474334096582,0.));
#113833=CARTESIAN_POINT('Ctrl Pts',(69.9846280854254,20.7474334096582,12.));
#113834=CARTESIAN_POINT('Ctrl Pts',(70.0047762740569,20.7635094829016,0.));
#113835=CARTESIAN_POINT('Ctrl Pts',(70.0047762740569,20.7635094829016,12.));
#113836=CARTESIAN_POINT('Ctrl Pts',(70.0249394394221,20.7796285249023,0.));
#113837=CARTESIAN_POINT('Ctrl Pts',(70.0249394394221,20.7796285249023,12.));
#113838=CARTESIAN_POINT('Ctrl Pts',(70.0451174706739,20.7957905141155,0.));
#113839=CARTESIAN_POINT('Ctrl Pts',(70.0451174706739,20.7957905141155,12.));
#113840=CARTESIAN_POINT('Ctrl Pts',(70.0653102573798,20.8119954289846,0.));
#113841=CARTESIAN_POINT('Ctrl Pts',(70.0653102573798,20.8119954289846,12.));
#113842=CARTESIAN_POINT('Ctrl Pts',(70.0855176895185,20.8282432479425,0.));
#113843=CARTESIAN_POINT('Ctrl Pts',(70.0855176895185,20.8282432479425,12.));
#113844=CARTESIAN_POINT('Ctrl Pts',(70.1057396574741,20.8445339494184,0.));
#113845=CARTESIAN_POINT('Ctrl Pts',(70.1057396574741,20.8445339494184,12.));
#113846=CARTESIAN_POINT('Ctrl Pts',(70.1259760520306,20.8608675118377,0.));
#113847=CARTESIAN_POINT('Ctrl Pts',(70.1259760520306,20.8608675118377,12.));
#113848=CARTESIAN_POINT('Ctrl Pts',(70.1462267643649,20.8772439136207,0.));
#113849=CARTESIAN_POINT('Ctrl Pts',(70.1462267643649,20.8772439136207,12.));
#113850=CARTESIAN_POINT('Ctrl Pts',(70.1664916860366,20.8936631331751,0.));
#113851=CARTESIAN_POINT('Ctrl Pts',(70.1664916860366,20.8936631331751,12.));
#113852=CARTESIAN_POINT('Ctrl Pts',(70.1867707089866,20.9101251488948,0.));
#113853=CARTESIAN_POINT('Ctrl Pts',(70.1867707089866,20.9101251488948,12.));
#113854=CARTESIAN_POINT('Ctrl Pts',(70.2070637255469,20.9266299391688,0.));
#113855=CARTESIAN_POINT('Ctrl Pts',(70.2070637255469,20.9266299391688,12.));
#113856=CARTESIAN_POINT('Ctrl Pts',(70.2273706284479,20.9431774823833,0.));
#113857=CARTESIAN_POINT('Ctrl Pts',(70.2273706284479,20.9431774823833,12.));
#113858=CARTESIAN_POINT('Ctrl Pts',(70.2476913108242,20.9597677569227,0.));
#113859=CARTESIAN_POINT('Ctrl Pts',(70.2476913108242,20.9597677569227,12.));
#113860=CARTESIAN_POINT('Ctrl Pts',(70.2680256662215,20.9764007411649,0.));
#113861=CARTESIAN_POINT('Ctrl Pts',(70.2680256662215,20.9764007411649,12.));
#113862=CARTESIAN_POINT('Ctrl Pts',(70.288373588597,20.993076413477,0.));
#113863=CARTESIAN_POINT('Ctrl Pts',(70.288373588597,20.993076413477,12.));
#113864=CARTESIAN_POINT('Ctrl Pts',(70.3087349722959,21.0097947522212,0.));
#113865=CARTESIAN_POINT('Ctrl Pts',(70.3087349722959,21.0097947522212,12.));
#113866=CARTESIAN_POINT('Ctrl Pts',(70.3291097120293,21.0265557357544,0.));
#113867=CARTESIAN_POINT('Ctrl Pts',(70.3291097120293,21.0265557357544,12.));
#113868=CARTESIAN_POINT('Ctrl Pts',(70.3494977028497,21.0433593424266,0.));
#113869=CARTESIAN_POINT('Ctrl Pts',(70.3494977028497,21.0433593424266,12.));
#113870=CARTESIAN_POINT('Ctrl Pts',(70.3698988401291,21.0602055505751,0.));
#113871=CARTESIAN_POINT('Ctrl Pts',(70.3698988401291,21.0602055505751,12.));
#113872=CARTESIAN_POINT('Ctrl Pts',(70.3903130195279,21.0770943385146,0.));
#113873=CARTESIAN_POINT('Ctrl Pts',(70.3903130195279,21.0770943385146,12.));
#113874=CARTESIAN_POINT('Ctrl Pts',(70.4107401370403,21.0940256845477,0.));
#113875=CARTESIAN_POINT('Ctrl Pts',(70.4107401370403,21.0940256845477,12.));
#113876=CARTESIAN_POINT('Ctrl Pts',(70.4311800890411,21.110999566975,0.));
#113877=CARTESIAN_POINT('Ctrl Pts',(70.4311800890411,21.110999566975,12.));
#113878=CARTESIAN_POINT('Ctrl Pts',(70.4516327723349,21.1280159641003,0.));
#113879=CARTESIAN_POINT('Ctrl Pts',(70.4516327723349,21.1280159641003,12.));
#113880=CARTESIAN_POINT('Ctrl Pts',(70.4720980841934,21.1450748542335,0.));
#113881=CARTESIAN_POINT('Ctrl Pts',(70.4720980841934,21.1450748542335,12.));
#113882=CARTESIAN_POINT('Ctrl Pts',(70.4925759224208,21.1621762156894,0.));
#113883=CARTESIAN_POINT('Ctrl Pts',(70.4925759224208,21.1621762156894,12.));
#113884=CARTESIAN_POINT('Ctrl Pts',(70.5130661852946,21.1793200267843,0.));
#113885=CARTESIAN_POINT('Ctrl Pts',(70.5130661852946,21.1793200267843,12.));
#113886=CARTESIAN_POINT('Ctrl Pts',(70.5335687714422,21.1965062658296,0.));
#113887=CARTESIAN_POINT('Ctrl Pts',(70.5335687714422,21.1965062658296,12.));
#113888=CARTESIAN_POINT('Ctrl Pts',(70.5540835797281,21.2137349111207,0.));
#113889=CARTESIAN_POINT('Ctrl Pts',(70.5540835797281,21.2137349111207,12.));
#113890=CARTESIAN_POINT('Ctrl Pts',(70.5746105091503,21.2310059409265,0.));
#113891=CARTESIAN_POINT('Ctrl Pts',(70.5746105091503,21.2310059409265,12.));
#113892=CARTESIAN_POINT('Ctrl Pts',(70.5951494586961,21.2483193334677,0.));
#113893=CARTESIAN_POINT('Ctrl Pts',(70.5951494586961,21.2483193334677,12.));
#113894=CARTESIAN_POINT('Ctrl Pts',(70.6157003273326,21.2656750669129,0.));
#113895=CARTESIAN_POINT('Ctrl Pts',(70.6157003273326,21.2656750669129,12.));
#113896=CARTESIAN_POINT('Ctrl Pts',(70.6362630143062,21.2830731194188,0.));
#113897=CARTESIAN_POINT('Ctrl Pts',(70.6362630143062,21.2830731194188,12.));
#113898=CARTESIAN_POINT('Ctrl Pts',(70.6568374193786,21.3005134691563,0.));
#113899=CARTESIAN_POINT('Ctrl Pts',(70.6568374193786,21.3005134691563,12.));
#113900=CARTESIAN_POINT('Ctrl Pts',(70.6774234430899,21.3179960943389,0.));
#113901=CARTESIAN_POINT('Ctrl Pts',(70.6774234430899,21.3179960943389,12.));
#113902=CARTESIAN_POINT('Ctrl Pts',(70.6980209870032,21.3355209732438,0.));
#113903=CARTESIAN_POINT('Ctrl Pts',(70.6980209870032,21.3355209732438,12.));
#113904=CARTESIAN_POINT('Ctrl Pts',(70.7186299539698,21.353088084234,0.));
#113905=CARTESIAN_POINT('Ctrl Pts',(70.7186299539698,21.353088084234,12.));
#113906=CARTESIAN_POINT('Ctrl Pts',(70.7392502475437,21.3706974057028,0.));
#113907=CARTESIAN_POINT('Ctrl Pts',(70.7392502475437,21.3706974057028,12.));
#113908=CARTESIAN_POINT('Ctrl Pts',(70.7598817714078,21.3883489160187,0.));
#113909=CARTESIAN_POINT('Ctrl Pts',(70.7598817714078,21.3883489160187,12.));
#113910=CARTESIAN_POINT('Ctrl Pts',(70.780524428744,21.4060425934595,0.));
#113911=CARTESIAN_POINT('Ctrl Pts',(70.780524428744,21.4060425934595,12.));
#113912=CARTESIAN_POINT('Ctrl Pts',(70.8011781217409,21.4237784161592,0.));
#113913=CARTESIAN_POINT('Ctrl Pts',(70.8011781217409,21.4237784161592,12.));
#113914=CARTESIAN_POINT('Ctrl Pts',(70.8218427507545,21.4415563620127,0.));
#113915=CARTESIAN_POINT('Ctrl Pts',(70.8218427507545,21.4415563620127,12.));
#113916=CARTESIAN_POINT('Ctrl Pts',(70.84251821499,21.4593764087492,0.));
#113917=CARTESIAN_POINT('Ctrl Pts',(70.84251821499,21.4593764087492,12.));
#113918=CARTESIAN_POINT('Ctrl Pts',(70.8632044140166,21.4772385340978,0.));
#113919=CARTESIAN_POINT('Ctrl Pts',(70.8632044140166,21.4772385340978,12.));
#113920=CARTESIAN_POINT('Ctrl Pts',(70.8839012490903,21.4951427159272,0.));
#113921=CARTESIAN_POINT('Ctrl Pts',(70.8839012490903,21.4951427159272,12.));
#113922=CARTESIAN_POINT('Ctrl Pts',(70.9046086244123,21.5130889323767,0.));
#113923=CARTESIAN_POINT('Ctrl Pts',(70.9046086244123,21.5130889323767,12.));
#113924=CARTESIAN_POINT('Ctrl Pts',(70.9253264487576,21.5310771620209,0.));
#113925=CARTESIAN_POINT('Ctrl Pts',(70.9253264487576,21.5310771620209,12.));
#113926=CARTESIAN_POINT('Ctrl Pts',(70.9460546358597,21.549107383907,0.));
#113927=CARTESIAN_POINT('Ctrl Pts',(70.9460546358597,21.549107383907,12.));
#113928=CARTESIAN_POINT('Ctrl Pts',(70.9667931008097,21.5671795771873,0.));
#113929=CARTESIAN_POINT('Ctrl Pts',(70.9667931008097,21.5671795771873,12.));
#113930=CARTESIAN_POINT('Ctrl Pts',(70.9875417572138,21.5852937208258,0.));
#113931=CARTESIAN_POINT('Ctrl Pts',(70.9875417572138,21.5852937208258,12.));
#113932=CARTESIAN_POINT('Ctrl Pts',(71.0083005139086,21.6034497932574,0.));
#113933=CARTESIAN_POINT('Ctrl Pts',(71.0083005139086,21.6034497932574,12.));
#113934=CARTESIAN_POINT('Ctrl Pts',(71.0290692721932,21.6216477720941,0.));
#113935=CARTESIAN_POINT('Ctrl Pts',(71.0290692721932,21.6216477720941,12.));
#113936=CARTESIAN_POINT('Ctrl Pts',(71.0498479219659,21.6398876337207,0.));
#113937=CARTESIAN_POINT('Ctrl Pts',(71.0498479219659,21.6398876337207,12.));
#113938=CARTESIAN_POINT('Ctrl Pts',(71.0706363472965,21.6581693538424,0.));
#113939=CARTESIAN_POINT('Ctrl Pts',(71.0706363472965,21.6581693538424,12.));
#113940=CARTESIAN_POINT('Ctrl Pts',(71.0914344333048,21.6764929081762,0.));
#113941=CARTESIAN_POINT('Ctrl Pts',(71.0914344333048,21.6764929081762,12.));
#113942=CARTESIAN_POINT('Ctrl Pts',(71.1122420728349,21.6948582730895,0.));
#113943=CARTESIAN_POINT('Ctrl Pts',(71.1122420728349,21.6948582730895,12.));
#113944=CARTESIAN_POINT('Ctrl Pts',(71.133059172642,21.7132654262501,0.));
#113945=CARTESIAN_POINT('Ctrl Pts',(71.133059172642,21.7132654262501,12.));
#113946=CARTESIAN_POINT('Ctrl Pts',(71.1538856611899,21.7317143472827,0.));
#113947=CARTESIAN_POINT('Ctrl Pts',(71.1538856611899,21.7317143472827,12.));
#113948=CARTESIAN_POINT('Ctrl Pts',(71.1747214905981,21.7502050183602,0.));
#113949=CARTESIAN_POINT('Ctrl Pts',(71.1747214905981,21.7502050183602,12.));
#113950=CARTESIAN_POINT('Ctrl Pts',(71.1955666309591,21.7687374247046,0.));
#113951=CARTESIAN_POINT('Ctrl Pts',(71.1955666309591,21.7687374247046,12.));
#113952=CARTESIAN_POINT('Ctrl Pts',(71.212250179455,21.7835967290261,0.));
#113953=CARTESIAN_POINT('Ctrl Pts',(71.212250179455,21.7835967290261,12.));
#113954=CARTESIAN_POINT('Ctrl Pts',(71.2247670209821,21.7947599798839,0.));
#113955=CARTESIAN_POINT('Ctrl Pts',(71.2247670209821,21.7947599798839,12.));
#113956=CARTESIAN_POINT('Ctrl Pts',(71.2331134397743,21.8022104901682,0.));
#113957=CARTESIAN_POINT('Ctrl Pts',(71.2331134397743,21.8022104901682,12.));
#113958=CARTESIAN_POINT('Ctrl Pts',(71.2372871136137,21.8059378310719,0.));
#113959=CARTESIAN_POINT('Ctrl Pts',(71.2372871136137,21.8059378310719,12.));
#113960=CARTESIAN_POINT('',(67.3887914263118,18.9407177820969,0.));
#113961=CARTESIAN_POINT('Ctrl Pts',(67.3887914263118,18.9407177820969,0.));
#113962=CARTESIAN_POINT('Ctrl Pts',(67.3921355608328,18.9426924398719,0.));
#113963=CARTESIAN_POINT('Ctrl Pts',(67.3988274146651,18.9466463414299,0.));
#113964=CARTESIAN_POINT('Ctrl Pts',(67.4088759497911,18.9525909517915,0.));
#113965=CARTESIAN_POINT('Ctrl Pts',(67.4222955061981,18.9605446160985,0.));
#113966=CARTESIAN_POINT('Ctrl Pts',(67.4391057908418,18.9705325631711,0.));
#113967=CARTESIAN_POINT('Ctrl Pts',(67.4559518744638,18.9805663798449,0.));
#113968=CARTESIAN_POINT('Ctrl Pts',(67.472833671964,18.9906460638625,0.));
#113969=CARTESIAN_POINT('Ctrl Pts',(67.4897510316844,19.0007716032819,0.));
#113970=CARTESIAN_POINT('Ctrl Pts',(67.5067037372317,19.0109429761306,0.));
#113971=CARTESIAN_POINT('Ctrl Pts',(67.5236915360331,19.021160154824,0.));
#113972=CARTESIAN_POINT('Ctrl Pts',(67.540714161288,19.0314231093923,0.));
#113973=CARTESIAN_POINT('Ctrl Pts',(67.5577713558194,19.0417318110708,0.));
#113974=CARTESIAN_POINT('Ctrl Pts',(67.5748628971964,19.0520862360396,0.));
#113975=CARTESIAN_POINT('Ctrl Pts',(67.5919885896222,19.062486364241,0.));
#113976=CARTESIAN_POINT('Ctrl Pts',(67.6091482520534,19.072932177628,0.));
#113977=CARTESIAN_POINT('Ctrl Pts',(67.6263417083426,19.0834236587118,0.));
#113978=CARTESIAN_POINT('Ctrl Pts',(67.6435687749841,19.0939607887502,0.));
#113979=CARTESIAN_POINT('Ctrl Pts',(67.6608292549462,19.1045435468358,0.));
#113980=CARTESIAN_POINT('Ctrl Pts',(67.6781229440573,19.115171910846,0.));
#113981=CARTESIAN_POINT('Ctrl Pts',(67.6954496350063,19.1258458580345,0.));
#113982=CARTESIAN_POINT('Ctrl Pts',(67.7128091219348,19.136565365709,0.));
#113983=CARTESIAN_POINT('Ctrl Pts',(67.7302012056584,19.1473304119955,0.));
#113984=CARTESIAN_POINT('Ctrl Pts',(67.7476256934444,19.1581409758097,0.));
#113985=CARTESIAN_POINT('Ctrl Pts',(67.7650823965127,19.168997036495,0.));
#113986=CARTESIAN_POINT('Ctrl Pts',(67.7825711283096,19.1798985735688,0.));
#113987=CARTESIAN_POINT('Ctrl Pts',(67.8000917023926,19.1908455664098,0.));
#113988=CARTESIAN_POINT('Ctrl Pts',(67.8176439306621,19.201837993993,0.));
#113989=CARTESIAN_POINT('Ctrl Pts',(67.835227624289,19.2128758350346,0.));
#113990=CARTESIAN_POINT('Ctrl Pts',(67.8528425945184,19.2239590681133,0.));
#113991=CARTESIAN_POINT('Ctrl Pts',(67.8704886534544,19.2350876717874,0.));
#113992=CARTESIAN_POINT('Ctrl Pts',(67.8881656149955,19.2462616247279,0.));
#113993=CARTESIAN_POINT('Ctrl Pts',(67.9058732951788,19.2574809057696,0.));
#113994=CARTESIAN_POINT('Ctrl Pts',(67.9236115116758,19.2687454938442,0.));
#113995=CARTESIAN_POINT('Ctrl Pts',(67.9413800834793,19.280055367936,0.));
#113996=CARTESIAN_POINT('Ctrl Pts',(67.9591788305394,19.2914105070286,0.));
#113997=CARTESIAN_POINT('Ctrl Pts',(67.9770075733485,19.302810890038,0.));
#113998=CARTESIAN_POINT('Ctrl Pts',(67.9948661329617,19.3142564958203,0.));
#113999=CARTESIAN_POINT('Ctrl Pts',(68.0127543311776,19.3257473032035,0.));
#114000=CARTESIAN_POINT('Ctrl Pts',(68.0306719906636,19.3372832910076,0.));
#114001=CARTESIAN_POINT('Ctrl Pts',(68.0486189351011,19.3488644380641,0.));
#114002=CARTESIAN_POINT('Ctrl Pts',(68.0665949893195,19.3604907232314,0.));
#114003=CARTESIAN_POINT('Ctrl Pts',(68.0845999792247,19.3721621253912,0.));
#114004=CARTESIAN_POINT('Ctrl Pts',(68.1026337317285,19.3838786234421,0.));
#114005=CARTESIAN_POINT('Ctrl Pts',(68.1206960746769,19.3956401962895,0.));
#114006=CARTESIAN_POINT('Ctrl Pts',(68.1387868367691,19.40744682283,0.));
#114007=CARTESIAN_POINT('Ctrl Pts',(68.1569058475054,19.4192984819418,0.));
#114008=CARTESIAN_POINT('Ctrl Pts',(68.1750529372232,19.4311951524983,0.));
#114009=CARTESIAN_POINT('Ctrl Pts',(68.1932279371127,19.4431368133719,0.));
#114010=CARTESIAN_POINT('Ctrl Pts',(68.2114306792358,19.4551234434381,0.));
#114011=CARTESIAN_POINT('Ctrl Pts',(68.2296609965448,19.467155021572,0.));
#114012=CARTESIAN_POINT('Ctrl Pts',(68.2479187228803,19.4792315266501,0.));
#114013=CARTESIAN_POINT('Ctrl Pts',(68.2662036929526,19.4913529375543,0.));
#114014=CARTESIAN_POINT('Ctrl Pts',(68.2845157423233,19.5035192331705,0.));
#114015=CARTESIAN_POINT('Ctrl Pts',(68.3028547073864,19.5157303923856,0.));
#114016=CARTESIAN_POINT('Ctrl Pts',(68.3212204253417,19.5279863940773,0.));
#114017=CARTESIAN_POINT('Ctrl Pts',(68.3396127341938,19.5402872171191,0.));
#114018=CARTESIAN_POINT('Ctrl Pts',(68.3580314727523,19.5526328403852,0.));
#114019=CARTESIAN_POINT('Ctrl Pts',(68.3764764806287,19.5650232427516,0.));
#114020=CARTESIAN_POINT('Ctrl Pts',(68.3949475982335,19.5774584030938,0.));
#114021=CARTESIAN_POINT('Ctrl Pts',(68.4134446667696,19.5899383002803,0.));
#114022=CARTESIAN_POINT('Ctrl Pts',(68.4319675282275,19.6024629131785,0.));
#114023=CARTESIAN_POINT('Ctrl Pts',(68.4505160253778,19.6150322206577,0.));
#114024=CARTESIAN_POINT('Ctrl Pts',(68.4690900017632,19.6276462015888,0.));
#114025=CARTESIAN_POINT('Ctrl Pts',(68.4876893016856,19.6403048348395,0.));
#114026=CARTESIAN_POINT('Ctrl Pts',(68.5063137701971,19.6530080992686,0.));
#114027=CARTESIAN_POINT('Ctrl Pts',(68.5249632530979,19.6657559737336,0.));
#114028=CARTESIAN_POINT('Ctrl Pts',(68.5436375969311,19.6785484370927,0.));
#114029=CARTESIAN_POINT('Ctrl Pts',(68.5623366489779,19.6913854682046,0.));
#114030=CARTESIAN_POINT('Ctrl Pts',(68.581060257249,19.7042670459237,0.));
#114031=CARTESIAN_POINT('Ctrl Pts',(68.5998082704766,19.7171931490956,0.));
#114032=CARTESIAN_POINT('Ctrl Pts',(68.6185805381126,19.7301637565652,0.));
#114033=CARTESIAN_POINT('Ctrl Pts',(68.6373769103224,19.7431788471776,0.));
#114034=CARTESIAN_POINT('Ctrl Pts',(68.6561972379793,19.7562383997781,0.));
#114035=CARTESIAN_POINT('Ctrl Pts',(68.6750413726547,19.7693423932058,0.));
#114036=CARTESIAN_POINT('Ctrl Pts',(68.6939091666111,19.7824908062913,0.));
#114037=CARTESIAN_POINT('Ctrl Pts',(68.7128004727998,19.795683617864,0.));
#114038=CARTESIAN_POINT('Ctrl Pts',(68.7317151448557,19.8089208067532,0.));
#114039=CARTESIAN_POINT('Ctrl Pts',(68.7506530370918,19.8222023517874,0.));
#114040=CARTESIAN_POINT('Ctrl Pts',(68.7696140044892,19.835528231787,0.));
#114041=CARTESIAN_POINT('Ctrl Pts',(68.7885979026927,19.8488984255641,0.));
#114042=CARTESIAN_POINT('Ctrl Pts',(68.8076045880102,19.8623129119304,0.));
#114043=CARTESIAN_POINT('Ctrl Pts',(68.8266339174068,19.8757716696969,0.));
#114044=CARTESIAN_POINT('Ctrl Pts',(68.8456857484988,19.8892746776734,0.));
#114045=CARTESIAN_POINT('Ctrl Pts',(68.8647599395437,19.9028219146607,0.));
#114046=CARTESIAN_POINT('Ctrl Pts',(68.8838563494356,19.9164133594513,0.));
#114047=CARTESIAN_POINT('Ctrl Pts',(68.902974837704,19.9300489908364,0.));
#114048=CARTESIAN_POINT('Ctrl Pts',(68.9221152645086,19.9437287876063,0.));
#114049=CARTESIAN_POINT('Ctrl Pts',(68.9412774906346,19.9574527285492,0.));
#114050=CARTESIAN_POINT('Ctrl Pts',(68.960461377483,19.9712207924437,0.));
#114051=CARTESIAN_POINT('Ctrl Pts',(68.9796667870667,19.98503295806,0.));
#114052=CARTESIAN_POINT('Ctrl Pts',(68.9988935820101,19.9988892041671,0.));
#114053=CARTESIAN_POINT('Ctrl Pts',(69.0181416255433,20.0127895095327,0.));
#114054=CARTESIAN_POINT('Ctrl Pts',(69.0374107814977,20.0267338529221,0.));
#114055=CARTESIAN_POINT('Ctrl Pts',(69.0567009142968,20.0407222130902,0.));
#114056=CARTESIAN_POINT('Ctrl Pts',(69.0760118889525,20.0547545687839,0.));
#114057=CARTESIAN_POINT('Ctrl Pts',(69.0953435710634,20.0688308987478,0.));
#114058=CARTESIAN_POINT('Ctrl Pts',(69.1146958268104,20.0829511817251,0.));
#114059=CARTESIAN_POINT('Ctrl Pts',(69.1340685229516,20.0971153964557,0.));
#114060=CARTESIAN_POINT('Ctrl Pts',(69.1534615268153,20.1113235216694,0.));
#114061=CARTESIAN_POINT('Ctrl Pts',(69.172874706296,20.1255755360871,0.));
#114062=CARTESIAN_POINT('Ctrl Pts',(69.1923079298534,20.1398714184278,0.));
#114063=CARTESIAN_POINT('Ctrl Pts',(69.2117610665073,20.1542111474086,0.));
#114064=CARTESIAN_POINT('Ctrl Pts',(69.2312339858337,20.1685947017433,0.));
#114065=CARTESIAN_POINT('Ctrl Pts',(69.2507265579562,20.183022060135,0.));
#114066=CARTESIAN_POINT('Ctrl Pts',(69.2702386535432,20.1974932012775,0.));
#114067=CARTESIAN_POINT('Ctrl Pts',(69.2897701438066,20.2120081038622,0.));
#114068=CARTESIAN_POINT('Ctrl Pts',(69.3093209004986,20.2265667465784,0.));
#114069=CARTESIAN_POINT('Ctrl Pts',(69.3288907959065,20.2411691081122,0.));
#114070=CARTESIAN_POINT('Ctrl Pts',(69.3484797028454,20.255815167139,0.));
#114071=CARTESIAN_POINT('Ctrl Pts',(69.3680874946548,20.2705049023241,0.));
#114072=CARTESIAN_POINT('Ctrl Pts',(69.3877140451975,20.2852382923299,0.));
#114073=CARTESIAN_POINT('Ctrl Pts',(69.4073592288562,20.3000153158167,0.));
#114074=CARTESIAN_POINT('Ctrl Pts',(69.4270229205296,20.3148359514414,0.));
#114075=CARTESIAN_POINT('Ctrl Pts',(69.4467049956257,20.3297001778505,0.));
#114076=CARTESIAN_POINT('Ctrl Pts',(69.4664053300579,20.3446079736799,0.));
#114077=CARTESIAN_POINT('Ctrl Pts',(69.4861238002433,20.359559317562,0.));
#114078=CARTESIAN_POINT('Ctrl Pts',(69.5058602831004,20.3745541881267,0.));
#114079=CARTESIAN_POINT('Ctrl Pts',(69.5256146560444,20.3895925640006,0.));
#114080=CARTESIAN_POINT('Ctrl Pts',(69.5453867969815,20.4046744238002,0.));
#114081=CARTESIAN_POINT('Ctrl Pts',(69.565176584305,20.4197997461306,0.));
#114082=CARTESIAN_POINT('Ctrl Pts',(69.5849838968944,20.4349685095928,0.));
#114083=CARTESIAN_POINT('Ctrl Pts',(69.6048086141122,20.4501806927854,0.));
#114084=CARTESIAN_POINT('Ctrl Pts',(69.6246506158009,20.4654362743036,0.));
#114085=CARTESIAN_POINT('Ctrl Pts',(69.6445097822778,20.4807352327335,0.));
#114086=CARTESIAN_POINT('Ctrl Pts',(69.6643859943291,20.4960775466487,0.));
#114087=CARTESIAN_POINT('Ctrl Pts',(69.6842791332102,20.511463194618,0.));
#114088=CARTESIAN_POINT('Ctrl Pts',(69.7041890806421,20.5268921552076,0.));
#114089=CARTESIAN_POINT('Ctrl Pts',(69.7241157188086,20.54236440698,0.));
#114090=CARTESIAN_POINT('Ctrl Pts',(69.7440589303511,20.5578799284898,0.));
#114091=CARTESIAN_POINT('Ctrl Pts',(69.7640185983641,20.5734386982782,0.));
#114092=CARTESIAN_POINT('Ctrl Pts',(69.7839946063942,20.5890406948809,0.));
#114093=CARTESIAN_POINT('Ctrl Pts',(69.8039868384382,20.6046858968305,0.));
#114094=CARTESIAN_POINT('Ctrl Pts',(69.8239951789402,20.6203742826566,0.));
#114095=CARTESIAN_POINT('Ctrl Pts',(69.8440195127874,20.6361058308812,0.));
#114096=CARTESIAN_POINT('Ctrl Pts',(69.8640597253058,20.6518805200132,0.));
#114097=CARTESIAN_POINT('Ctrl Pts',(69.884115702258,20.6676983285542,0.));
#114098=CARTESIAN_POINT('Ctrl Pts',(69.9041873298416,20.6835592350031,0.));
#114099=CARTESIAN_POINT('Ctrl Pts',(69.9242744946854,20.6994632178551,0.));
#114100=CARTESIAN_POINT('Ctrl Pts',(69.9443770838444,20.7154102555996,0.));
#114101=CARTESIAN_POINT('Ctrl Pts',(69.9644949847929,20.7314003267118,0.));
#114102=CARTESIAN_POINT('Ctrl Pts',(69.9846280854254,20.7474334096582,0.));
#114103=CARTESIAN_POINT('Ctrl Pts',(70.0047762740569,20.7635094829016,0.));
#114104=CARTESIAN_POINT('Ctrl Pts',(70.0249394394221,20.7796285249023,0.));
#114105=CARTESIAN_POINT('Ctrl Pts',(70.0451174706739,20.7957905141155,0.));
#114106=CARTESIAN_POINT('Ctrl Pts',(70.0653102573798,20.8119954289846,0.));
#114107=CARTESIAN_POINT('Ctrl Pts',(70.0855176895185,20.8282432479425,0.));
#114108=CARTESIAN_POINT('Ctrl Pts',(70.1057396574741,20.8445339494184,0.));
#114109=CARTESIAN_POINT('Ctrl Pts',(70.1259760520306,20.8608675118377,0.));
#114110=CARTESIAN_POINT('Ctrl Pts',(70.1462267643649,20.8772439136207,0.));
#114111=CARTESIAN_POINT('Ctrl Pts',(70.1664916860366,20.8936631331751,0.));
#114112=CARTESIAN_POINT('Ctrl Pts',(70.1867707089866,20.9101251488948,0.));
#114113=CARTESIAN_POINT('Ctrl Pts',(70.2070637255469,20.9266299391688,0.));
#114114=CARTESIAN_POINT('Ctrl Pts',(70.2273706284479,20.9431774823833,0.));
#114115=CARTESIAN_POINT('Ctrl Pts',(70.2476913108242,20.9597677569227,0.));
#114116=CARTESIAN_POINT('Ctrl Pts',(70.2680256662215,20.9764007411649,0.));
#114117=CARTESIAN_POINT('Ctrl Pts',(70.288373588597,20.993076413477,0.));
#114118=CARTESIAN_POINT('Ctrl Pts',(70.3087349722959,21.0097947522212,0.));
#114119=CARTESIAN_POINT('Ctrl Pts',(70.3291097120293,21.0265557357544,0.));
#114120=CARTESIAN_POINT('Ctrl Pts',(70.3494977028497,21.0433593424266,0.));
#114121=CARTESIAN_POINT('Ctrl Pts',(70.3698988401291,21.0602055505751,0.));
#114122=CARTESIAN_POINT('Ctrl Pts',(70.3903130195279,21.0770943385146,0.));
#114123=CARTESIAN_POINT('Ctrl Pts',(70.4107401370403,21.0940256845477,0.));
#114124=CARTESIAN_POINT('Ctrl Pts',(70.4311800890411,21.110999566975,0.));
#114125=CARTESIAN_POINT('Ctrl Pts',(70.4516327723349,21.1280159641003,0.));
#114126=CARTESIAN_POINT('Ctrl Pts',(70.4720980841934,21.1450748542335,0.));
#114127=CARTESIAN_POINT('Ctrl Pts',(70.4925759224208,21.1621762156894,0.));
#114128=CARTESIAN_POINT('Ctrl Pts',(70.5130661852946,21.1793200267843,0.));
#114129=CARTESIAN_POINT('Ctrl Pts',(70.5335687714422,21.1965062658296,0.));
#114130=CARTESIAN_POINT('Ctrl Pts',(70.5540835797281,21.2137349111207,0.));
#114131=CARTESIAN_POINT('Ctrl Pts',(70.5746105091503,21.2310059409265,0.));
#114132=CARTESIAN_POINT('Ctrl Pts',(70.5951494586961,21.2483193334677,0.));
#114133=CARTESIAN_POINT('Ctrl Pts',(70.6157003273326,21.2656750669129,0.));
#114134=CARTESIAN_POINT('Ctrl Pts',(70.6362630143062,21.2830731194188,0.));
#114135=CARTESIAN_POINT('Ctrl Pts',(70.6568374193786,21.3005134691563,0.));
#114136=CARTESIAN_POINT('Ctrl Pts',(70.6774234430899,21.3179960943389,0.));
#114137=CARTESIAN_POINT('Ctrl Pts',(70.6980209870032,21.3355209732438,0.));
#114138=CARTESIAN_POINT('Ctrl Pts',(70.7186299539698,21.353088084234,0.));
#114139=CARTESIAN_POINT('Ctrl Pts',(70.7392502475437,21.3706974057028,0.));
#114140=CARTESIAN_POINT('Ctrl Pts',(70.7598817714078,21.3883489160187,0.));
#114141=CARTESIAN_POINT('Ctrl Pts',(70.780524428744,21.4060425934595,0.));
#114142=CARTESIAN_POINT('Ctrl Pts',(70.8011781217409,21.4237784161592,0.));
#114143=CARTESIAN_POINT('Ctrl Pts',(70.8218427507545,21.4415563620127,0.));
#114144=CARTESIAN_POINT('Ctrl Pts',(70.84251821499,21.4593764087492,0.));
#114145=CARTESIAN_POINT('Ctrl Pts',(70.8632044140166,21.4772385340978,0.));
#114146=CARTESIAN_POINT('Ctrl Pts',(70.8839012490903,21.4951427159272,0.));
#114147=CARTESIAN_POINT('Ctrl Pts',(70.9046086244123,21.5130889323767,0.));
#114148=CARTESIAN_POINT('Ctrl Pts',(70.9253264487576,21.5310771620209,0.));
#114149=CARTESIAN_POINT('Ctrl Pts',(70.9460546358597,21.549107383907,0.));
#114150=CARTESIAN_POINT('Ctrl Pts',(70.9638315189647,21.5645987555282,0.));
#114151=CARTESIAN_POINT('Ctrl Pts',(70.9774662112376,21.576498336635,0.));
#114152=CARTESIAN_POINT('Ctrl Pts',(70.9869541807808,21.584787543316,0.));
#114153=CARTESIAN_POINT('Ctrl Pts',(70.9922924595081,21.5894540925369,0.));
#114154=CARTESIAN_POINT('Ctrl Pts',(70.9934796068777,21.59049199348,0.));
#114155=CARTESIAN_POINT('',(67.3887914263118,18.9407177820969,12.));
#114156=CARTESIAN_POINT('',(67.3887914263118,18.9407177820969,0.));
#114157=CARTESIAN_POINT('Ctrl Pts',(70.9934796068777,21.59049199348,12.));
#114158=CARTESIAN_POINT('Ctrl Pts',(70.9922924595081,21.5894540925369,12.));
#114159=CARTESIAN_POINT('Ctrl Pts',(70.9869541807808,21.584787543316,12.));
#114160=CARTESIAN_POINT('Ctrl Pts',(70.9774662112376,21.576498336635,12.));
#114161=CARTESIAN_POINT('Ctrl Pts',(70.9638315189647,21.5645987555282,12.));
#114162=CARTESIAN_POINT('Ctrl Pts',(70.9460546358597,21.549107383907,12.));
#114163=CARTESIAN_POINT('Ctrl Pts',(70.9253264487576,21.5310771620209,12.));
#114164=CARTESIAN_POINT('Ctrl Pts',(70.9046086244123,21.5130889323767,12.));
#114165=CARTESIAN_POINT('Ctrl Pts',(70.8839012490903,21.4951427159272,12.));
#114166=CARTESIAN_POINT('Ctrl Pts',(70.8632044140166,21.4772385340978,12.));
#114167=CARTESIAN_POINT('Ctrl Pts',(70.84251821499,21.4593764087492,12.));
#114168=CARTESIAN_POINT('Ctrl Pts',(70.8218427507545,21.4415563620127,12.));
#114169=CARTESIAN_POINT('Ctrl Pts',(70.8011781217409,21.4237784161592,12.));
#114170=CARTESIAN_POINT('Ctrl Pts',(70.780524428744,21.4060425934595,12.));
#114171=CARTESIAN_POINT('Ctrl Pts',(70.7598817714078,21.3883489160187,12.));
#114172=CARTESIAN_POINT('Ctrl Pts',(70.7392502475437,21.3706974057028,12.));
#114173=CARTESIAN_POINT('Ctrl Pts',(70.7186299539698,21.353088084234,12.));
#114174=CARTESIAN_POINT('Ctrl Pts',(70.6980209870032,21.3355209732438,12.));
#114175=CARTESIAN_POINT('Ctrl Pts',(70.6774234430899,21.3179960943389,12.));
#114176=CARTESIAN_POINT('Ctrl Pts',(70.6568374193786,21.3005134691563,12.));
#114177=CARTESIAN_POINT('Ctrl Pts',(70.6362630143062,21.2830731194188,12.));
#114178=CARTESIAN_POINT('Ctrl Pts',(70.6157003273326,21.2656750669129,12.));
#114179=CARTESIAN_POINT('Ctrl Pts',(70.5951494586961,21.2483193334677,12.));
#114180=CARTESIAN_POINT('Ctrl Pts',(70.5746105091503,21.2310059409265,12.));
#114181=CARTESIAN_POINT('Ctrl Pts',(70.5540835797281,21.2137349111207,12.));
#114182=CARTESIAN_POINT('Ctrl Pts',(70.5335687714422,21.1965062658296,12.));
#114183=CARTESIAN_POINT('Ctrl Pts',(70.5130661852946,21.1793200267843,12.));
#114184=CARTESIAN_POINT('Ctrl Pts',(70.4925759224208,21.1621762156894,12.));
#114185=CARTESIAN_POINT('Ctrl Pts',(70.4720980841934,21.1450748542335,12.));
#114186=CARTESIAN_POINT('Ctrl Pts',(70.4516327723349,21.1280159641003,12.));
#114187=CARTESIAN_POINT('Ctrl Pts',(70.4311800890411,21.110999566975,12.));
#114188=CARTESIAN_POINT('Ctrl Pts',(70.4107401370403,21.0940256845477,12.));
#114189=CARTESIAN_POINT('Ctrl Pts',(70.3903130195279,21.0770943385146,12.));
#114190=CARTESIAN_POINT('Ctrl Pts',(70.3698988401291,21.0602055505751,12.));
#114191=CARTESIAN_POINT('Ctrl Pts',(70.3494977028497,21.0433593424266,12.));
#114192=CARTESIAN_POINT('Ctrl Pts',(70.3291097120293,21.0265557357544,12.));
#114193=CARTESIAN_POINT('Ctrl Pts',(70.3087349722959,21.0097947522212,12.));
#114194=CARTESIAN_POINT('Ctrl Pts',(70.288373588597,20.993076413477,12.));
#114195=CARTESIAN_POINT('Ctrl Pts',(70.2680256662215,20.9764007411649,12.));
#114196=CARTESIAN_POINT('Ctrl Pts',(70.2476913108242,20.9597677569227,12.));
#114197=CARTESIAN_POINT('Ctrl Pts',(70.2273706284479,20.9431774823833,12.));
#114198=CARTESIAN_POINT('Ctrl Pts',(70.2070637255469,20.9266299391688,12.));
#114199=CARTESIAN_POINT('Ctrl Pts',(70.1867707089866,20.9101251488948,12.));
#114200=CARTESIAN_POINT('Ctrl Pts',(70.1664916860366,20.8936631331751,12.));
#114201=CARTESIAN_POINT('Ctrl Pts',(70.1462267643649,20.8772439136207,12.));
#114202=CARTESIAN_POINT('Ctrl Pts',(70.1259760520306,20.8608675118377,12.));
#114203=CARTESIAN_POINT('Ctrl Pts',(70.1057396574741,20.8445339494184,12.));
#114204=CARTESIAN_POINT('Ctrl Pts',(70.0855176895185,20.8282432479425,12.));
#114205=CARTESIAN_POINT('Ctrl Pts',(70.0653102573798,20.8119954289846,12.));
#114206=CARTESIAN_POINT('Ctrl Pts',(70.0451174706739,20.7957905141155,12.));
#114207=CARTESIAN_POINT('Ctrl Pts',(70.0249394394221,20.7796285249023,12.));
#114208=CARTESIAN_POINT('Ctrl Pts',(70.0047762740569,20.7635094829016,12.));
#114209=CARTESIAN_POINT('Ctrl Pts',(69.9846280854254,20.7474334096582,12.));
#114210=CARTESIAN_POINT('Ctrl Pts',(69.9644949847929,20.7314003267118,12.));
#114211=CARTESIAN_POINT('Ctrl Pts',(69.9443770838444,20.7154102555996,12.));
#114212=CARTESIAN_POINT('Ctrl Pts',(69.9242744946854,20.6994632178551,12.));
#114213=CARTESIAN_POINT('Ctrl Pts',(69.9041873298416,20.6835592350031,12.));
#114214=CARTESIAN_POINT('Ctrl Pts',(69.884115702258,20.6676983285542,12.));
#114215=CARTESIAN_POINT('Ctrl Pts',(69.8640597253058,20.6518805200132,12.));
#114216=CARTESIAN_POINT('Ctrl Pts',(69.8440195127874,20.6361058308812,12.));
#114217=CARTESIAN_POINT('Ctrl Pts',(69.8239951789402,20.6203742826566,12.));
#114218=CARTESIAN_POINT('Ctrl Pts',(69.8039868384382,20.6046858968305,12.));
#114219=CARTESIAN_POINT('Ctrl Pts',(69.7839946063942,20.5890406948809,12.));
#114220=CARTESIAN_POINT('Ctrl Pts',(69.7640185983641,20.5734386982782,12.));
#114221=CARTESIAN_POINT('Ctrl Pts',(69.7440589303511,20.5578799284898,12.));
#114222=CARTESIAN_POINT('Ctrl Pts',(69.7241157188086,20.54236440698,12.));
#114223=CARTESIAN_POINT('Ctrl Pts',(69.7041890806421,20.5268921552076,12.));
#114224=CARTESIAN_POINT('Ctrl Pts',(69.6842791332102,20.511463194618,12.));
#114225=CARTESIAN_POINT('Ctrl Pts',(69.6643859943291,20.4960775466487,12.));
#114226=CARTESIAN_POINT('Ctrl Pts',(69.6445097822778,20.4807352327335,12.));
#114227=CARTESIAN_POINT('Ctrl Pts',(69.6246506158009,20.4654362743036,12.));
#114228=CARTESIAN_POINT('Ctrl Pts',(69.6048086141122,20.4501806927854,12.));
#114229=CARTESIAN_POINT('Ctrl Pts',(69.5849838968944,20.4349685095928,12.));
#114230=CARTESIAN_POINT('Ctrl Pts',(69.565176584305,20.4197997461306,12.));
#114231=CARTESIAN_POINT('Ctrl Pts',(69.5453867969815,20.4046744238002,12.));
#114232=CARTESIAN_POINT('Ctrl Pts',(69.5256146560444,20.3895925640006,12.));
#114233=CARTESIAN_POINT('Ctrl Pts',(69.5058602831004,20.3745541881267,12.));
#114234=CARTESIAN_POINT('Ctrl Pts',(69.4861238002433,20.359559317562,12.));
#114235=CARTESIAN_POINT('Ctrl Pts',(69.4664053300579,20.3446079736799,12.));
#114236=CARTESIAN_POINT('Ctrl Pts',(69.4467049956257,20.3297001778505,12.));
#114237=CARTESIAN_POINT('Ctrl Pts',(69.4270229205296,20.3148359514414,12.));
#114238=CARTESIAN_POINT('Ctrl Pts',(69.4073592288562,20.3000153158167,12.));
#114239=CARTESIAN_POINT('Ctrl Pts',(69.3877140451975,20.2852382923299,12.));
#114240=CARTESIAN_POINT('Ctrl Pts',(69.3680874946548,20.2705049023241,12.));
#114241=CARTESIAN_POINT('Ctrl Pts',(69.3484797028454,20.255815167139,12.));
#114242=CARTESIAN_POINT('Ctrl Pts',(69.3288907959065,20.2411691081122,12.));
#114243=CARTESIAN_POINT('Ctrl Pts',(69.3093209004986,20.2265667465784,12.));
#114244=CARTESIAN_POINT('Ctrl Pts',(69.2897701438066,20.2120081038622,12.));
#114245=CARTESIAN_POINT('Ctrl Pts',(69.2702386535432,20.1974932012775,12.));
#114246=CARTESIAN_POINT('Ctrl Pts',(69.2507265579562,20.183022060135,12.));
#114247=CARTESIAN_POINT('Ctrl Pts',(69.2312339858337,20.1685947017433,12.));
#114248=CARTESIAN_POINT('Ctrl Pts',(69.2117610665073,20.1542111474086,12.));
#114249=CARTESIAN_POINT('Ctrl Pts',(69.1923079298534,20.1398714184278,12.));
#114250=CARTESIAN_POINT('Ctrl Pts',(69.172874706296,20.1255755360871,12.));
#114251=CARTESIAN_POINT('Ctrl Pts',(69.1534615268153,20.1113235216694,12.));
#114252=CARTESIAN_POINT('Ctrl Pts',(69.1340685229516,20.0971153964557,12.));
#114253=CARTESIAN_POINT('Ctrl Pts',(69.1146958268104,20.0829511817251,12.));
#114254=CARTESIAN_POINT('Ctrl Pts',(69.0953435710634,20.0688308987478,12.));
#114255=CARTESIAN_POINT('Ctrl Pts',(69.0760118889525,20.0547545687839,12.));
#114256=CARTESIAN_POINT('Ctrl Pts',(69.0567009142968,20.0407222130902,12.));
#114257=CARTESIAN_POINT('Ctrl Pts',(69.0374107814977,20.0267338529221,12.));
#114258=CARTESIAN_POINT('Ctrl Pts',(69.0181416255433,20.0127895095327,12.));
#114259=CARTESIAN_POINT('Ctrl Pts',(68.9988935820101,19.9988892041671,12.));
#114260=CARTESIAN_POINT('Ctrl Pts',(68.9796667870667,19.98503295806,12.));
#114261=CARTESIAN_POINT('Ctrl Pts',(68.960461377483,19.9712207924437,12.));
#114262=CARTESIAN_POINT('Ctrl Pts',(68.9412774906346,19.9574527285492,12.));
#114263=CARTESIAN_POINT('Ctrl Pts',(68.9221152645086,19.9437287876063,12.));
#114264=CARTESIAN_POINT('Ctrl Pts',(68.902974837704,19.9300489908364,12.));
#114265=CARTESIAN_POINT('Ctrl Pts',(68.8838563494356,19.9164133594513,12.));
#114266=CARTESIAN_POINT('Ctrl Pts',(68.8647599395437,19.9028219146607,12.));
#114267=CARTESIAN_POINT('Ctrl Pts',(68.8456857484988,19.8892746776734,12.));
#114268=CARTESIAN_POINT('Ctrl Pts',(68.8266339174068,19.8757716696969,12.));
#114269=CARTESIAN_POINT('Ctrl Pts',(68.8076045880102,19.8623129119304,12.));
#114270=CARTESIAN_POINT('Ctrl Pts',(68.7885979026927,19.8488984255641,12.));
#114271=CARTESIAN_POINT('Ctrl Pts',(68.7696140044892,19.835528231787,12.));
#114272=CARTESIAN_POINT('Ctrl Pts',(68.7506530370918,19.8222023517874,12.));
#114273=CARTESIAN_POINT('Ctrl Pts',(68.7317151448557,19.8089208067532,12.));
#114274=CARTESIAN_POINT('Ctrl Pts',(68.7128004727998,19.795683617864,12.));
#114275=CARTESIAN_POINT('Ctrl Pts',(68.6939091666111,19.7824908062913,12.));
#114276=CARTESIAN_POINT('Ctrl Pts',(68.6750413726547,19.7693423932058,12.));
#114277=CARTESIAN_POINT('Ctrl Pts',(68.6561972379793,19.7562383997781,12.));
#114278=CARTESIAN_POINT('Ctrl Pts',(68.6373769103224,19.7431788471776,12.));
#114279=CARTESIAN_POINT('Ctrl Pts',(68.6185805381126,19.7301637565652,12.));
#114280=CARTESIAN_POINT('Ctrl Pts',(68.5998082704766,19.7171931490956,12.));
#114281=CARTESIAN_POINT('Ctrl Pts',(68.581060257249,19.7042670459237,12.));
#114282=CARTESIAN_POINT('Ctrl Pts',(68.5623366489779,19.6913854682046,12.));
#114283=CARTESIAN_POINT('Ctrl Pts',(68.5436375969311,19.6785484370927,12.));
#114284=CARTESIAN_POINT('Ctrl Pts',(68.5249632530979,19.6657559737336,12.));
#114285=CARTESIAN_POINT('Ctrl Pts',(68.5063137701971,19.6530080992686,12.));
#114286=CARTESIAN_POINT('Ctrl Pts',(68.4876893016856,19.6403048348395,12.));
#114287=CARTESIAN_POINT('Ctrl Pts',(68.4690900017632,19.6276462015888,12.));
#114288=CARTESIAN_POINT('Ctrl Pts',(68.4505160253778,19.6150322206577,12.));
#114289=CARTESIAN_POINT('Ctrl Pts',(68.4319675282275,19.6024629131785,12.));
#114290=CARTESIAN_POINT('Ctrl Pts',(68.4134446667696,19.5899383002803,12.));
#114291=CARTESIAN_POINT('Ctrl Pts',(68.3949475982335,19.5774584030938,12.));
#114292=CARTESIAN_POINT('Ctrl Pts',(68.3764764806287,19.5650232427516,12.));
#114293=CARTESIAN_POINT('Ctrl Pts',(68.3580314727523,19.5526328403852,12.));
#114294=CARTESIAN_POINT('Ctrl Pts',(68.3396127341938,19.5402872171191,12.));
#114295=CARTESIAN_POINT('Ctrl Pts',(68.3212204253417,19.5279863940773,12.));
#114296=CARTESIAN_POINT('Ctrl Pts',(68.3028547073864,19.5157303923856,12.));
#114297=CARTESIAN_POINT('Ctrl Pts',(68.2845157423233,19.5035192331705,12.));
#114298=CARTESIAN_POINT('Ctrl Pts',(68.2662036929526,19.4913529375543,12.));
#114299=CARTESIAN_POINT('Ctrl Pts',(68.2479187228803,19.4792315266501,12.));
#114300=CARTESIAN_POINT('Ctrl Pts',(68.2296609965448,19.467155021572,12.));
#114301=CARTESIAN_POINT('Ctrl Pts',(68.2114306792358,19.4551234434381,12.));
#114302=CARTESIAN_POINT('Ctrl Pts',(68.1932279371127,19.4431368133719,12.));
#114303=CARTESIAN_POINT('Ctrl Pts',(68.1750529372232,19.4311951524983,12.));
#114304=CARTESIAN_POINT('Ctrl Pts',(68.1569058475054,19.4192984819418,12.));
#114305=CARTESIAN_POINT('Ctrl Pts',(68.1387868367691,19.40744682283,12.));
#114306=CARTESIAN_POINT('Ctrl Pts',(68.1206960746769,19.3956401962895,12.));
#114307=CARTESIAN_POINT('Ctrl Pts',(68.1026337317285,19.3838786234421,12.));
#114308=CARTESIAN_POINT('Ctrl Pts',(68.0845999792247,19.3721621253912,12.));
#114309=CARTESIAN_POINT('Ctrl Pts',(68.0665949893195,19.3604907232314,12.));
#114310=CARTESIAN_POINT('Ctrl Pts',(68.0486189351011,19.3488644380641,12.));
#114311=CARTESIAN_POINT('Ctrl Pts',(68.0306719906636,19.3372832910076,12.));
#114312=CARTESIAN_POINT('Ctrl Pts',(68.0127543311776,19.3257473032035,12.));
#114313=CARTESIAN_POINT('Ctrl Pts',(67.9948661329617,19.3142564958203,12.));
#114314=CARTESIAN_POINT('Ctrl Pts',(67.9770075733485,19.302810890038,12.));
#114315=CARTESIAN_POINT('Ctrl Pts',(67.9591788305394,19.2914105070286,12.));
#114316=CARTESIAN_POINT('Ctrl Pts',(67.9413800834793,19.280055367936,12.));
#114317=CARTESIAN_POINT('Ctrl Pts',(67.9236115116758,19.2687454938442,12.));
#114318=CARTESIAN_POINT('Ctrl Pts',(67.9058732951788,19.2574809057696,12.));
#114319=CARTESIAN_POINT('Ctrl Pts',(67.8881656149955,19.2462616247279,12.));
#114320=CARTESIAN_POINT('Ctrl Pts',(67.8704886534544,19.2350876717874,12.));
#114321=CARTESIAN_POINT('Ctrl Pts',(67.8528425945184,19.2239590681133,12.));
#114322=CARTESIAN_POINT('Ctrl Pts',(67.835227624289,19.2128758350346,12.));
#114323=CARTESIAN_POINT('Ctrl Pts',(67.8176439306621,19.201837993993,12.));
#114324=CARTESIAN_POINT('Ctrl Pts',(67.8000917023926,19.1908455664098,12.));
#114325=CARTESIAN_POINT('Ctrl Pts',(67.7825711283096,19.1798985735688,12.));
#114326=CARTESIAN_POINT('Ctrl Pts',(67.7650823965127,19.168997036495,12.));
#114327=CARTESIAN_POINT('Ctrl Pts',(67.7476256934444,19.1581409758097,12.));
#114328=CARTESIAN_POINT('Ctrl Pts',(67.7302012056584,19.1473304119955,12.));
#114329=CARTESIAN_POINT('Ctrl Pts',(67.7128091219348,19.136565365709,12.));
#114330=CARTESIAN_POINT('Ctrl Pts',(67.6954496350063,19.1258458580345,12.));
#114331=CARTESIAN_POINT('Ctrl Pts',(67.6781229440573,19.115171910846,12.));
#114332=CARTESIAN_POINT('Ctrl Pts',(67.6608292549462,19.1045435468358,12.));
#114333=CARTESIAN_POINT('Ctrl Pts',(67.6435687749841,19.0939607887502,12.));
#114334=CARTESIAN_POINT('Ctrl Pts',(67.6263417083426,19.0834236587118,12.));
#114335=CARTESIAN_POINT('Ctrl Pts',(67.6091482520534,19.072932177628,12.));
#114336=CARTESIAN_POINT('Ctrl Pts',(67.5919885896222,19.062486364241,12.));
#114337=CARTESIAN_POINT('Ctrl Pts',(67.5748628971964,19.0520862360396,12.));
#114338=CARTESIAN_POINT('Ctrl Pts',(67.5577713558194,19.0417318110708,12.));
#114339=CARTESIAN_POINT('Ctrl Pts',(67.540714161288,19.0314231093923,12.));
#114340=CARTESIAN_POINT('Ctrl Pts',(67.5236915360331,19.021160154824,12.));
#114341=CARTESIAN_POINT('Ctrl Pts',(67.5067037372317,19.0109429761306,12.));
#114342=CARTESIAN_POINT('Ctrl Pts',(67.4897510316844,19.0007716032819,12.));
#114343=CARTESIAN_POINT('Ctrl Pts',(67.472833671964,18.9906460638625,12.));
#114344=CARTESIAN_POINT('Ctrl Pts',(67.4559518744638,18.9805663798449,12.));
#114345=CARTESIAN_POINT('Ctrl Pts',(67.4391057908418,18.9705325631711,12.));
#114346=CARTESIAN_POINT('Ctrl Pts',(67.4222955061981,18.9605446160985,12.));
#114347=CARTESIAN_POINT('Ctrl Pts',(67.4088759497911,18.9525909517915,12.));
#114348=CARTESIAN_POINT('Ctrl Pts',(67.3988274146651,18.9466463414299,12.));
#114349=CARTESIAN_POINT('Ctrl Pts',(67.3921355608328,18.9426924398719,12.));
#114350=CARTESIAN_POINT('Ctrl Pts',(67.3887914263118,18.9407177820969,12.));
#114351=CARTESIAN_POINT('Ctrl Pts',(70.538251407892,23.0342913834073,0.));
#114352=CARTESIAN_POINT('Ctrl Pts',(70.538251407892,23.0342913834073,4.));
#114353=CARTESIAN_POINT('Ctrl Pts',(70.538251407892,23.0342913834073,8.));
#114354=CARTESIAN_POINT('Ctrl Pts',(70.538251407892,23.0342913834073,12.));
#114355=CARTESIAN_POINT('Ctrl Pts',(70.6474988907591,23.0224954570734,0.));
#114356=CARTESIAN_POINT('Ctrl Pts',(70.6474988907591,23.0224954570734,4.));
#114357=CARTESIAN_POINT('Ctrl Pts',(70.6474988907591,23.0224954570734,8.));
#114358=CARTESIAN_POINT('Ctrl Pts',(70.6474988907591,23.0224954570734,12.));
#114359=CARTESIAN_POINT('Ctrl Pts',(70.83100071469,22.9364730048789,7.30819363922311E-17));
#114360=CARTESIAN_POINT('Ctrl Pts',(70.83100071469,22.9364730048789,4.00000000000001));
#114361=CARTESIAN_POINT('Ctrl Pts',(70.83100071469,22.9364730048789,7.99999999999999));
#114362=CARTESIAN_POINT('Ctrl Pts',(70.83100071469,22.9364730048789,12.));
#114363=CARTESIAN_POINT('Ctrl Pts',(70.9357242819029,22.7679558220498,2.46611180197085E-16));
#114364=CARTESIAN_POINT('Ctrl Pts',(70.9357242819029,22.7679558220498,4.));
#114365=CARTESIAN_POINT('Ctrl Pts',(70.9357242819029,22.7679558220498,8.00000000000001));
#114366=CARTESIAN_POINT('Ctrl Pts',(70.9357242819029,22.7679558220498,12.));
#114367=CARTESIAN_POINT('Ctrl Pts',(70.9608233461354,22.6894590071812,3.30265160424765E-16));
#114368=CARTESIAN_POINT('Ctrl Pts',(70.9608233461354,22.6894590071812,4.));
#114369=CARTESIAN_POINT('Ctrl Pts',(70.9608233461354,22.6894590071812,8.));
#114370=CARTESIAN_POINT('Ctrl Pts',(70.9608233461354,22.6894590071812,12.));
#114371=CARTESIAN_POINT('',(70.538251407892,23.0342913834073,0.));
#114372=CARTESIAN_POINT('',(70.9608233461355,22.6894590071812,0.));
#114373=CARTESIAN_POINT('Ctrl Pts',(70.538251407892,23.0342913834073,1.8765334327149E-16));
#114374=CARTESIAN_POINT('Ctrl Pts',(70.6474988907591,23.0224954570734,1.8765334327149E-16));
#114375=CARTESIAN_POINT('Ctrl Pts',(70.7523570758625,22.9733397701051,2.29414449781337E-16));
#114376=CARTESIAN_POINT('Ctrl Pts',(70.8314917485681,22.8972470282358,3.03974677078978E-16));
#114377=CARTESIAN_POINT('Ctrl Pts',(70.8908427530974,22.8401774718338,3.59894847552209E-16));
#114378=CARTESIAN_POINT('Ctrl Pts',(70.9357242819029,22.7679558220498,4.34264523468575E-16));
#114379=CARTESIAN_POINT('Ctrl Pts',(70.9608233461354,22.6894590071812,5.17918503696256E-16));
#114380=CARTESIAN_POINT('',(70.9608233461355,22.6894590071812,12.));
#114381=CARTESIAN_POINT('Ctrl Pts',(70.9608233461354,22.6894590071812,3.30265160424765E-16));
#114382=CARTESIAN_POINT('Ctrl Pts',(70.9608233461354,22.6894590071812,4.));
#114383=CARTESIAN_POINT('Ctrl Pts',(70.9608233461354,22.6894590071812,8.));
#114384=CARTESIAN_POINT('Ctrl Pts',(70.9608233461354,22.6894590071812,12.));
#114385=CARTESIAN_POINT('',(70.538251407892,23.0342913834073,12.));
#114386=CARTESIAN_POINT('Ctrl Pts',(70.9608233461354,22.6894590071812,12.));
#114387=CARTESIAN_POINT('Ctrl Pts',(70.9357242819029,22.7679558220498,12.));
#114388=CARTESIAN_POINT('Ctrl Pts',(70.8908427530974,22.8401774718337,12.));
#114389=CARTESIAN_POINT('Ctrl Pts',(70.8314917485681,22.8972470282358,12.));
#114390=CARTESIAN_POINT('Ctrl Pts',(70.7523570758625,22.9733397701051,12.));
#114391=CARTESIAN_POINT('Ctrl Pts',(70.6474988907591,23.0224954570734,12.));
#114392=CARTESIAN_POINT('Ctrl Pts',(70.538251407892,23.0342913834073,12.));
#114393=CARTESIAN_POINT('Ctrl Pts',(70.538251407892,23.0342913834073,12.));
#114394=CARTESIAN_POINT('Ctrl Pts',(70.538251407892,23.0342913834073,8.));
#114395=CARTESIAN_POINT('Ctrl Pts',(70.538251407892,23.0342913834073,4.));
#114396=CARTESIAN_POINT('Ctrl Pts',(70.538251407892,23.0342913834073,0.));
#114397=CARTESIAN_POINT('Origin',(3.57465004850839E-10,1.12812358559725E-10,
0.));
#114398=CARTESIAN_POINT('Origin',(3.57465004850839E-10,1.12812358559725E-10,
12.));
#114399=CARTESIAN_POINT('Origin',(3.57465004850839E-10,1.12812358559725E-10,
0.));
#114400=CARTESIAN_POINT('Ctrl Pts',(72.7986051948032,15.830763774726,-5.55111512312578E-16));
#114401=CARTESIAN_POINT('Ctrl Pts',(72.7986051948032,15.830763774726,4.));
#114402=CARTESIAN_POINT('Ctrl Pts',(72.7986051948032,15.830763774726,8.));
#114403=CARTESIAN_POINT('Ctrl Pts',(72.7986051948032,15.830763774726,12.));
#114404=CARTESIAN_POINT('Ctrl Pts',(72.8219545017353,15.7233907508395,-5.55111512312578E-16));
#114405=CARTESIAN_POINT('Ctrl Pts',(72.8219545017353,15.7233907508395,4.));
#114406=CARTESIAN_POINT('Ctrl Pts',(72.8219545017353,15.7233907508395,8.));
#114407=CARTESIAN_POINT('Ctrl Pts',(72.8219545017353,15.7233907508395,12.));
#114408=CARTESIAN_POINT('Ctrl Pts',(72.7983622347336,15.522104120072,-5.55111512312578E-16));
#114409=CARTESIAN_POINT('Ctrl Pts',(72.7983622347336,15.522104120072,4.00000000000001));
#114410=CARTESIAN_POINT('Ctrl Pts',(72.7983622347336,15.522104120072,8.));
#114411=CARTESIAN_POINT('Ctrl Pts',(72.7983622347336,15.522104120072,12.));
#114412=CARTESIAN_POINT('Ctrl Pts',(72.6715981986661,15.3694736926917,-5.55111512312578E-16));
#114413=CARTESIAN_POINT('Ctrl Pts',(72.6715981986661,15.3694736926917,4.));
#114414=CARTESIAN_POINT('Ctrl Pts',(72.6715981986661,15.3694736926917,8.));
#114415=CARTESIAN_POINT('Ctrl Pts',(72.6715981986661,15.3694736926917,12.));
#114416=CARTESIAN_POINT('Ctrl Pts',(72.605063349435,15.320844207719,-5.55111512312578E-16));
#114417=CARTESIAN_POINT('Ctrl Pts',(72.605063349435,15.320844207719,4.));
#114418=CARTESIAN_POINT('Ctrl Pts',(72.6050633494351,15.3208442077189,8.));
#114419=CARTESIAN_POINT('Ctrl Pts',(72.6050633494351,15.3208442077189,12.));
#114420=CARTESIAN_POINT('',(72.7986051948032,15.830763774726,0.));
#114421=CARTESIAN_POINT('',(72.6050633494351,15.3208442077189,0.));
#114422=CARTESIAN_POINT('Ctrl Pts',(72.7986051948032,15.830763774726,1.38777878078144E-16));
#114423=CARTESIAN_POINT('Ctrl Pts',(72.8219545017353,15.7233907508395,1.38777878078144E-16));
#114424=CARTESIAN_POINT('Ctrl Pts',(72.8084732063058,15.6083698189724,1.38777878078145E-16));
#114425=CARTESIAN_POINT('Ctrl Pts',(72.7613031699568,15.5092366269867,1.38777878078145E-16));
#114426=CARTESIAN_POINT('Ctrl Pts',(72.725925642695,15.4348867329975,1.38777878078145E-16));
#114427=CARTESIAN_POINT('Ctrl Pts',(72.6715981986661,15.3694736926917,1.38777878078144E-16));
#114428=CARTESIAN_POINT('Ctrl Pts',(72.605063349435,15.320844207719,1.38777878078145E-16));
#114429=CARTESIAN_POINT('',(72.6050633494351,15.3208442077189,12.));
#114430=CARTESIAN_POINT('Ctrl Pts',(72.605063349435,15.320844207719,-5.55111512312578E-16));
#114431=CARTESIAN_POINT('Ctrl Pts',(72.605063349435,15.320844207719,4.));
#114432=CARTESIAN_POINT('Ctrl Pts',(72.6050633494351,15.3208442077189,8.));
#114433=CARTESIAN_POINT('Ctrl Pts',(72.6050633494351,15.3208442077189,12.));
#114434=CARTESIAN_POINT('',(72.7986051948032,15.830763774726,12.));
#114435=CARTESIAN_POINT('Ctrl Pts',(72.6050633494351,15.3208442077189,12.));
#114436=CARTESIAN_POINT('Ctrl Pts',(72.6715981986661,15.3694736926917,12.));
#114437=CARTESIAN_POINT('Ctrl Pts',(72.7259256426951,15.4348867329975,12.));
#114438=CARTESIAN_POINT('Ctrl Pts',(72.7613031699568,15.5092366269867,12.));
#114439=CARTESIAN_POINT('Ctrl Pts',(72.8084732063058,15.6083698189724,12.));
#114440=CARTESIAN_POINT('Ctrl Pts',(72.8219545017353,15.7233907508395,12.));
#114441=CARTESIAN_POINT('Ctrl Pts',(72.7986051948032,15.830763774726,12.));
#114442=CARTESIAN_POINT('Ctrl Pts',(72.7986051948032,15.830763774726,12.));
#114443=CARTESIAN_POINT('Ctrl Pts',(72.7986051948032,15.830763774726,8.));
#114444=CARTESIAN_POINT('Ctrl Pts',(72.7986051948032,15.830763774726,4.));
#114445=CARTESIAN_POINT('Ctrl Pts',(72.7986051948032,15.830763774726,-5.55111512312578E-16));
#114446=CARTESIAN_POINT('Ctrl Pts',(68.7831490561748,12.9953224629497,0.));
#114447=CARTESIAN_POINT('Ctrl Pts',(68.7831490561748,12.9953224629497,12.));
#114448=CARTESIAN_POINT('Ctrl Pts',(68.7866525680193,12.9969981460277,0.));
#114449=CARTESIAN_POINT('Ctrl Pts',(68.7866525680193,12.9969981460277,12.));
#114450=CARTESIAN_POINT('Ctrl Pts',(68.7936635625545,13.0003537683055,0.));
#114451=CARTESIAN_POINT('Ctrl Pts',(68.7936635625545,13.0003537683055,12.));
#114452=CARTESIAN_POINT('Ctrl Pts',(68.804191966902,13.0053999700875,0.));
#114453=CARTESIAN_POINT('Ctrl Pts',(68.804191966902,13.0053999700875,12.));
#114454=CARTESIAN_POINT('Ctrl Pts',(68.8182536653656,13.0121537768946,0.));
#114455=CARTESIAN_POINT('Ctrl Pts',(68.8182536653656,13.0121537768946,12.));
#114456=CARTESIAN_POINT('Ctrl Pts',(68.8358704887468,13.0206386039691,0.));
#114457=CARTESIAN_POINT('Ctrl Pts',(68.8358704887468,13.0206386039691,12.));
#114458=CARTESIAN_POINT('Ctrl Pts',(68.8535269726793,13.0291660060107,0.));
#114459=CARTESIAN_POINT('Ctrl Pts',(68.8535269726793,13.0291660060107,12.));
#114460=CARTESIAN_POINT('Ctrl Pts',(68.8712230321906,13.0377359881875,0.));
#114461=CARTESIAN_POINT('Ctrl Pts',(68.8712230321906,13.0377359881875,12.));
#114462=CARTESIAN_POINT('Ctrl Pts',(68.8889585151585,13.0463485518207,0.));
#114463=CARTESIAN_POINT('Ctrl Pts',(68.8889585151585,13.0463485518207,12.));
#114464=CARTESIAN_POINT('Ctrl Pts',(68.9067332040985,13.0550036938813,0.));
#114465=CARTESIAN_POINT('Ctrl Pts',(68.9067332040985,13.0550036938813,12.));
#114466=CARTESIAN_POINT('Ctrl Pts',(68.9245468449945,13.0637014089029,0.));
#114467=CARTESIAN_POINT('Ctrl Pts',(68.9245468449945,13.0637014089029,12.));
#114468=CARTESIAN_POINT('Ctrl Pts',(68.9423991694492,13.072441690283,0.));
#114469=CARTESIAN_POINT('Ctrl Pts',(68.9423991694492,13.072441690283,12.));
#114470=CARTESIAN_POINT('Ctrl Pts',(68.9602899187573,13.0812245317808,0.));
#114471=CARTESIAN_POINT('Ctrl Pts',(68.9602899187573,13.0812245317808,12.));
#114472=CARTESIAN_POINT('Ctrl Pts',(68.9782188692581,13.090049929053,0.));
#114473=CARTESIAN_POINT('Ctrl Pts',(68.9782188692581,13.090049929053,12.));
#114474=CARTESIAN_POINT('Ctrl Pts',(68.9961858241519,13.0989178791834,0.));
#114475=CARTESIAN_POINT('Ctrl Pts',(68.9961858241519,13.0989178791834,12.));
#114476=CARTESIAN_POINT('Ctrl Pts',(69.0141906015113,13.1078283799722,0.));
#114477=CARTESIAN_POINT('Ctrl Pts',(69.0141906015113,13.1078283799722,12.));
#114478=CARTESIAN_POINT('Ctrl Pts',(69.0322330243348,13.1167814293497,0.));
#114479=CARTESIAN_POINT('Ctrl Pts',(69.0322330243348,13.1167814293497,12.));
#114480=CARTESIAN_POINT('Ctrl Pts',(69.0503129081817,13.1257770246386,0.));
#114481=CARTESIAN_POINT('Ctrl Pts',(69.0503129081817,13.1257770246386,12.));
#114482=CARTESIAN_POINT('Ctrl Pts',(69.0684300549477,13.1348151621834,0.));
#114483=CARTESIAN_POINT('Ctrl Pts',(69.0684300549477,13.1348151621834,12.));
#114484=CARTESIAN_POINT('Ctrl Pts',(69.0865842593102,13.1438958377404,0.));
#114485=CARTESIAN_POINT('Ctrl Pts',(69.0865842593102,13.1438958377404,12.));
#114486=CARTESIAN_POINT('Ctrl Pts',(69.1047753127643,13.1530190467183,0.));
#114487=CARTESIAN_POINT('Ctrl Pts',(69.1047753127643,13.1530190467183,12.));
#114488=CARTESIAN_POINT('Ctrl Pts',(69.1230030082573,13.1621847844528,0.));
#114489=CARTESIAN_POINT('Ctrl Pts',(69.1230030082573,13.1621847844528,12.));
#114490=CARTESIAN_POINT('Ctrl Pts',(69.1412671454564,13.1713930465133,0.));
#114491=CARTESIAN_POINT('Ctrl Pts',(69.1412671454564,13.1713930465133,12.));
#114492=CARTESIAN_POINT('Ctrl Pts',(69.1595675305245,13.1806438286934,0.));
#114493=CARTESIAN_POINT('Ctrl Pts',(69.1595675305245,13.1806438286934,12.));
#114494=CARTESIAN_POINT('Ctrl Pts',(69.1779039735996,13.1899371268683,0.));
#114495=CARTESIAN_POINT('Ctrl Pts',(69.1779039735996,13.1899371268683,12.));
#114496=CARTESIAN_POINT('Ctrl Pts',(69.1962762870527,13.1992729368929,0.));
#114497=CARTESIAN_POINT('Ctrl Pts',(69.1962762870527,13.1992729368929,12.));
#114498=CARTESIAN_POINT('Ctrl Pts',(69.2146842833537,13.2086512544735,0.));
#114499=CARTESIAN_POINT('Ctrl Pts',(69.2146842833537,13.2086512544735,12.));
#114500=CARTESIAN_POINT('Ctrl Pts',(69.2331277732861,13.2180720750594,0.));
#114501=CARTESIAN_POINT('Ctrl Pts',(69.2331277732861,13.2180720750594,12.));
#114502=CARTESIAN_POINT('Ctrl Pts',(69.2516065668844,13.2275353939051,0.));
#114503=CARTESIAN_POINT('Ctrl Pts',(69.2516065668844,13.2275353939051,12.));
#114504=CARTESIAN_POINT('Ctrl Pts',(69.270120474245,13.237041206122,0.));
#114505=CARTESIAN_POINT('Ctrl Pts',(69.270120474245,13.237041206122,12.));
#114506=CARTESIAN_POINT('Ctrl Pts',(69.2886693063182,13.2465895067262,0.));
#114507=CARTESIAN_POINT('Ctrl Pts',(69.2886693063182,13.2465895067262,12.));
#114508=CARTESIAN_POINT('Ctrl Pts',(69.3072528758518,13.2561802906896,0.));
#114509=CARTESIAN_POINT('Ctrl Pts',(69.3072528758518,13.2561802906896,12.));
#114510=CARTESIAN_POINT('Ctrl Pts',(69.3258709977382,13.265813552961,0.));
#114511=CARTESIAN_POINT('Ctrl Pts',(69.3258709977382,13.265813552961,12.));
#114512=CARTESIAN_POINT('Ctrl Pts',(69.3445234885065,13.2754892884433,0.));
#114513=CARTESIAN_POINT('Ctrl Pts',(69.3445234885065,13.2754892884433,12.));
#114514=CARTESIAN_POINT('Ctrl Pts',(69.3632101660066,13.2852074919766,0.));
#114515=CARTESIAN_POINT('Ctrl Pts',(69.3632101660066,13.2852074919766,12.));
#114516=CARTESIAN_POINT('Ctrl Pts',(69.3819308490422,13.2949681583167,0.));
#114517=CARTESIAN_POINT('Ctrl Pts',(69.3819308490422,13.2949681583167,12.));
#114518=CARTESIAN_POINT('Ctrl Pts',(69.4006853569511,13.3047712821051,0.));
#114519=CARTESIAN_POINT('Ctrl Pts',(69.4006853569511,13.3047712821051,12.));
#114520=CARTESIAN_POINT('Ctrl Pts',(69.4194735096265,13.3146168578743,0.));
#114521=CARTESIAN_POINT('Ctrl Pts',(69.4194735096265,13.3146168578743,12.));
#114522=CARTESIAN_POINT('Ctrl Pts',(69.4382951276998,13.3245048800643,0.));
#114523=CARTESIAN_POINT('Ctrl Pts',(69.4382951276998,13.3245048800643,12.));
#114524=CARTESIAN_POINT('Ctrl Pts',(69.4571500326673,13.3344353430313,0.));
#114525=CARTESIAN_POINT('Ctrl Pts',(69.4571500326673,13.3344353430313,12.));
#114526=CARTESIAN_POINT('Ctrl Pts',(69.4760380470365,13.3444082410543,0.));
#114527=CARTESIAN_POINT('Ctrl Pts',(69.4760380470365,13.3444082410543,12.));
#114528=CARTESIAN_POINT('Ctrl Pts',(69.4949589944606,13.3544235683394,0.));
#114529=CARTESIAN_POINT('Ctrl Pts',(69.4949589944606,13.3544235683394,12.));
#114530=CARTESIAN_POINT('Ctrl Pts',(69.5139126996675,13.3644813190219,0.));
#114531=CARTESIAN_POINT('Ctrl Pts',(69.5139126996675,13.3644813190219,12.));
#114532=CARTESIAN_POINT('Ctrl Pts',(69.5328989883885,13.3745814871665,0.));
#114533=CARTESIAN_POINT('Ctrl Pts',(69.5328989883885,13.3745814871665,12.));
#114534=CARTESIAN_POINT('Ctrl Pts',(69.5519176872862,13.3847240667628,0.));
#114535=CARTESIAN_POINT('Ctrl Pts',(69.5519176872862,13.3847240667628,12.));
#114536=CARTESIAN_POINT('Ctrl Pts',(69.5709686238724,13.3949090517177,0.));
#114537=CARTESIAN_POINT('Ctrl Pts',(69.5709686238724,13.3949090517177,12.));
#114538=CARTESIAN_POINT('Ctrl Pts',(69.5900516264553,13.40513643585,0.));
#114539=CARTESIAN_POINT('Ctrl Pts',(69.5900516264553,13.40513643585,12.));
#114540=CARTESIAN_POINT('Ctrl Pts',(69.6091665241765,13.4154062129002,0.));
#114541=CARTESIAN_POINT('Ctrl Pts',(69.6091665241765,13.4154062129002,12.));
#114542=CARTESIAN_POINT('Ctrl Pts',(69.6283131470273,13.4257183765341,0.));
#114543=CARTESIAN_POINT('Ctrl Pts',(69.6283131470273,13.4257183765341,12.));
#114544=CARTESIAN_POINT('Ctrl Pts',(69.6474913258675,13.4360729203442,0.));
#114545=CARTESIAN_POINT('Ctrl Pts',(69.6474913258675,13.4360729203442,12.));
#114546=CARTESIAN_POINT('Ctrl Pts',(69.666700892444,13.4464698378453,0.));
#114547=CARTESIAN_POINT('Ctrl Pts',(69.666700892444,13.4464698378453,12.));
#114548=CARTESIAN_POINT('Ctrl Pts',(69.6859416793885,13.456909122476,0.));
#114549=CARTESIAN_POINT('Ctrl Pts',(69.6859416793885,13.456909122476,12.));
#114550=CARTESIAN_POINT('Ctrl Pts',(69.7052135201998,13.4673907676044,0.));
#114551=CARTESIAN_POINT('Ctrl Pts',(69.7052135201998,13.4673907676044,12.));
#114552=CARTESIAN_POINT('Ctrl Pts',(69.724516249225,13.4779147665285,0.));
#114553=CARTESIAN_POINT('Ctrl Pts',(69.724516249225,13.4779147665285,12.));
#114554=CARTESIAN_POINT('Ctrl Pts',(69.7438497016406,13.4884811124748,0.));
#114555=CARTESIAN_POINT('Ctrl Pts',(69.7438497016406,13.4884811124748,12.));
#114556=CARTESIAN_POINT('Ctrl Pts',(69.7632137134249,13.4990897985905,0.));
#114557=CARTESIAN_POINT('Ctrl Pts',(69.7632137134249,13.4990897985905,12.));
#114558=CARTESIAN_POINT('Ctrl Pts',(69.7826081213576,13.5097408179479,0.));
#114559=CARTESIAN_POINT('Ctrl Pts',(69.7826081213576,13.5097408179479,12.));
#114560=CARTESIAN_POINT('Ctrl Pts',(69.8020327630205,13.5204341635507,0.));
#114561=CARTESIAN_POINT('Ctrl Pts',(69.8020327630205,13.5204341635507,12.));
#114562=CARTESIAN_POINT('Ctrl Pts',(69.8214874767944,13.5311698283339,0.));
#114563=CARTESIAN_POINT('Ctrl Pts',(69.8214874767944,13.5311698283339,12.));
#114564=CARTESIAN_POINT('Ctrl Pts',(69.840972101856,13.5419478051625,0.));
#114565=CARTESIAN_POINT('Ctrl Pts',(69.840972101856,13.5419478051625,12.));
#114566=CARTESIAN_POINT('Ctrl Pts',(69.8604864781706,13.5527680868255,0.));
#114567=CARTESIAN_POINT('Ctrl Pts',(69.8604864781706,13.5527680868255,12.));
#114568=CARTESIAN_POINT('Ctrl Pts',(69.8800304464882,13.5636306660422,0.));
#114569=CARTESIAN_POINT('Ctrl Pts',(69.8800304464882,13.5636306660422,12.));
#114570=CARTESIAN_POINT('Ctrl Pts',(69.8996038483361,13.5745355354657,0.));
#114571=CARTESIAN_POINT('Ctrl Pts',(69.8996038483361,13.5745355354657,12.));
#114572=CARTESIAN_POINT('Ctrl Pts',(69.9192065260108,13.5854826876835,0.));
#114573=CARTESIAN_POINT('Ctrl Pts',(69.9192065260108,13.5854826876835,12.));
#114574=CARTESIAN_POINT('Ctrl Pts',(69.9388383225648,13.5964721152135,0.));
#114575=CARTESIAN_POINT('Ctrl Pts',(69.9388383225648,13.5964721152135,12.));
#114576=CARTESIAN_POINT('Ctrl Pts',(69.9584990817974,13.6075038104999,0.));
#114577=CARTESIAN_POINT('Ctrl Pts',(69.9584990817974,13.6075038104999,12.));
#114578=CARTESIAN_POINT('Ctrl Pts',(69.9781886482528,13.6185777659198,0.));
#114579=CARTESIAN_POINT('Ctrl Pts',(69.9781886482528,13.6185777659198,12.));
#114580=CARTESIAN_POINT('Ctrl Pts',(69.9979068672153,13.6296939737865,0.));
#114581=CARTESIAN_POINT('Ctrl Pts',(69.9979068672153,13.6296939737865,12.));
#114582=CARTESIAN_POINT('Ctrl Pts',(70.0176535847049,13.6408524263496,0.));
#114583=CARTESIAN_POINT('Ctrl Pts',(70.0176535847049,13.6408524263496,12.));
#114584=CARTESIAN_POINT('Ctrl Pts',(70.0374286474677,13.6520531157907,0.));
#114585=CARTESIAN_POINT('Ctrl Pts',(70.0374286474677,13.6520531157907,12.));
#114586=CARTESIAN_POINT('Ctrl Pts',(70.0572319029676,13.6632960342196,0.));
#114587=CARTESIAN_POINT('Ctrl Pts',(70.0572319029676,13.6632960342196,12.));
#114588=CARTESIAN_POINT('Ctrl Pts',(70.0770631993856,13.674581173683,0.));
#114589=CARTESIAN_POINT('Ctrl Pts',(70.0770631993856,13.674581173683,12.));
#114590=CARTESIAN_POINT('Ctrl Pts',(70.0969223856136,13.6859085261653,0.));
#114591=CARTESIAN_POINT('Ctrl Pts',(70.0969223856136,13.6859085261653,12.));
#114592=CARTESIAN_POINT('Ctrl Pts',(70.1168093112486,13.6972780835897,0.));
#114593=CARTESIAN_POINT('Ctrl Pts',(70.1168093112486,13.6972780835897,12.));
#114594=CARTESIAN_POINT('Ctrl Pts',(70.1367238265825,13.7086898378122,0.));
#114595=CARTESIAN_POINT('Ctrl Pts',(70.1367238265825,13.7086898378122,12.));
#114596=CARTESIAN_POINT('Ctrl Pts',(70.156665782595,13.7201437806199,0.));
#114597=CARTESIAN_POINT('Ctrl Pts',(70.156665782595,13.7201437806199,12.));
#114598=CARTESIAN_POINT('Ctrl Pts',(70.1766350309518,13.7316399037393,0.));
#114599=CARTESIAN_POINT('Ctrl Pts',(70.1766350309518,13.7316399037393,12.));
#114600=CARTESIAN_POINT('Ctrl Pts',(70.1966314239995,13.7431781988365,0.));
#114601=CARTESIAN_POINT('Ctrl Pts',(70.1966314239995,13.7431781988365,12.));
#114602=CARTESIAN_POINT('Ctrl Pts',(70.2166548147604,13.7547586575181,0.));
#114603=CARTESIAN_POINT('Ctrl Pts',(70.2166548147604,13.7547586575181,12.));
#114604=CARTESIAN_POINT('Ctrl Pts',(70.2367050569216,13.7663812713243,0.));
#114605=CARTESIAN_POINT('Ctrl Pts',(70.2367050569216,13.7663812713243,12.));
#114606=CARTESIAN_POINT('Ctrl Pts',(70.2567820048303,13.7780460317294,0.));
#114607=CARTESIAN_POINT('Ctrl Pts',(70.2567820048303,13.7780460317294,12.));
#114608=CARTESIAN_POINT('Ctrl Pts',(70.2768855134947,13.7897529301491,0.));
#114609=CARTESIAN_POINT('Ctrl Pts',(70.2768855134947,13.7897529301491,12.));
#114610=CARTESIAN_POINT('Ctrl Pts',(70.2970154385774,13.8015019579414,0.));
#114611=CARTESIAN_POINT('Ctrl Pts',(70.2970154385774,13.8015019579414,12.));
#114612=CARTESIAN_POINT('Ctrl Pts',(70.3171716363897,13.8132931064064,0.));
#114613=CARTESIAN_POINT('Ctrl Pts',(70.3171716363897,13.8132931064064,12.));
#114614=CARTESIAN_POINT('Ctrl Pts',(70.3373539638809,13.8251263667791,0.));
#114615=CARTESIAN_POINT('Ctrl Pts',(70.3373539638809,13.8251263667791,12.));
#114616=CARTESIAN_POINT('Ctrl Pts',(70.3575622786335,13.8370017302309,0.));
#114617=CARTESIAN_POINT('Ctrl Pts',(70.3575622786335,13.8370017302309,12.));
#114618=CARTESIAN_POINT('Ctrl Pts',(70.3777964388632,13.8489191878767,0.));
#114619=CARTESIAN_POINT('Ctrl Pts',(70.3777964388632,13.8489191878767,12.));
#114620=CARTESIAN_POINT('Ctrl Pts',(70.3980563034133,13.8608787307752,0.));
#114621=CARTESIAN_POINT('Ctrl Pts',(70.3980563034133,13.8608787307752,12.));
#114622=CARTESIAN_POINT('Ctrl Pts',(70.41834173175,13.8728803499287,0.));
#114623=CARTESIAN_POINT('Ctrl Pts',(70.41834173175,13.8728803499287,12.));
#114624=CARTESIAN_POINT('Ctrl Pts',(70.4386525839521,13.8849240362763,0.));
#114625=CARTESIAN_POINT('Ctrl Pts',(70.4386525839521,13.8849240362763,12.));
#114626=CARTESIAN_POINT('Ctrl Pts',(70.4589887207073,13.8970097806954,0.));
#114627=CARTESIAN_POINT('Ctrl Pts',(70.4589887207073,13.8970097806954,12.));
#114628=CARTESIAN_POINT('Ctrl Pts',(70.4793500033124,13.9091375740088,0.));
#114629=CARTESIAN_POINT('Ctrl Pts',(70.4793500033124,13.9091375740088,12.));
#114630=CARTESIAN_POINT('Ctrl Pts',(70.4997362936673,13.9213074069853,0.));
#114631=CARTESIAN_POINT('Ctrl Pts',(70.4997362936673,13.9213074069853,12.));
#114632=CARTESIAN_POINT('Ctrl Pts',(70.520147454271,13.9335192703388,0.));
#114633=CARTESIAN_POINT('Ctrl Pts',(70.520147454271,13.9335192703388,12.));
#114634=CARTESIAN_POINT('Ctrl Pts',(70.5405833482112,13.9457731547215,0.));
#114635=CARTESIAN_POINT('Ctrl Pts',(70.5405833482112,13.9457731547215,12.));
#114636=CARTESIAN_POINT('Ctrl Pts',(70.5610438391612,13.958069050726,0.));
#114637=CARTESIAN_POINT('Ctrl Pts',(70.5610438391612,13.958069050726,12.));
#114638=CARTESIAN_POINT('Ctrl Pts',(70.5815287913784,13.9704069488917,0.));
#114639=CARTESIAN_POINT('Ctrl Pts',(70.5815287913784,13.9704069488917,12.));
#114640=CARTESIAN_POINT('Ctrl Pts',(70.6020380697005,13.9827868397057,0.));
#114641=CARTESIAN_POINT('Ctrl Pts',(70.6020380697005,13.9827868397057,12.));
#114642=CARTESIAN_POINT('Ctrl Pts',(70.6225715395394,13.9952087136018,0.));
#114643=CARTESIAN_POINT('Ctrl Pts',(70.6225715395394,13.9952087136018,12.));
#114644=CARTESIAN_POINT('Ctrl Pts',(70.6431290668745,14.0076725609537,0.));
#114645=CARTESIAN_POINT('Ctrl Pts',(70.6431290668745,14.0076725609537,12.));
#114646=CARTESIAN_POINT('Ctrl Pts',(70.6637105182484,14.020178372077,0.));
#114647=CARTESIAN_POINT('Ctrl Pts',(70.6637105182484,14.020178372077,12.));
#114648=CARTESIAN_POINT('Ctrl Pts',(70.6843157607668,14.0327261372362,0.));
#114649=CARTESIAN_POINT('Ctrl Pts',(70.6843157607668,14.0327261372362,12.));
#114650=CARTESIAN_POINT('Ctrl Pts',(70.7049446620928,14.0453158466451,0.));
#114651=CARTESIAN_POINT('Ctrl Pts',(70.7049446620928,14.0453158466451,12.));
#114652=CARTESIAN_POINT('Ctrl Pts',(70.7255970904436,14.0579474904657,0.));
#114653=CARTESIAN_POINT('Ctrl Pts',(70.7255970904436,14.0579474904657,12.));
#114654=CARTESIAN_POINT('Ctrl Pts',(70.7462729145807,14.0706210588016,0.));
#114655=CARTESIAN_POINT('Ctrl Pts',(70.7462729145807,14.0706210588016,12.));
#114656=CARTESIAN_POINT('Ctrl Pts',(70.7669720038077,14.0833365416996,0.));
#114657=CARTESIAN_POINT('Ctrl Pts',(70.7669720038077,14.0833365416996,12.));
#114658=CARTESIAN_POINT('Ctrl Pts',(70.7876942279697,14.0960939291569,0.));
#114659=CARTESIAN_POINT('Ctrl Pts',(70.7876942279697,14.0960939291569,12.));
#114660=CARTESIAN_POINT('Ctrl Pts',(70.8084394574493,14.1088932111214,0.));
#114661=CARTESIAN_POINT('Ctrl Pts',(70.8084394574493,14.1088932111214,12.));
#114662=CARTESIAN_POINT('Ctrl Pts',(70.8292075631621,14.1217343774913,0.));
#114663=CARTESIAN_POINT('Ctrl Pts',(70.8292075631621,14.1217343774913,12.));
#114664=CARTESIAN_POINT('Ctrl Pts',(70.8499984165489,14.1346174181079,0.));
#114665=CARTESIAN_POINT('Ctrl Pts',(70.8499984165489,14.1346174181079,12.));
#114666=CARTESIAN_POINT('Ctrl Pts',(70.8708118895715,14.1475423227568,0.));
#114667=CARTESIAN_POINT('Ctrl Pts',(70.8708118895715,14.1475423227568,12.));
#114668=CARTESIAN_POINT('Ctrl Pts',(70.8916478547132,14.1605090811754,0.));
#114669=CARTESIAN_POINT('Ctrl Pts',(70.8916478547132,14.1605090811754,12.));
#114670=CARTESIAN_POINT('Ctrl Pts',(70.9125061849745,14.1735176830533,0.));
#114671=CARTESIAN_POINT('Ctrl Pts',(70.9125061849745,14.1735176830533,12.));
#114672=CARTESIAN_POINT('Ctrl Pts',(70.9333867538704,14.1865681180321,0.));
#114673=CARTESIAN_POINT('Ctrl Pts',(70.9333867538704,14.1865681180321,12.));
#114674=CARTESIAN_POINT('Ctrl Pts',(70.9542894354216,14.1996603756982,0.));
#114675=CARTESIAN_POINT('Ctrl Pts',(70.9542894354216,14.1996603756982,12.));
#114676=CARTESIAN_POINT('Ctrl Pts',(70.9752141041518,14.2127944455839,0.));
#114677=CARTESIAN_POINT('Ctrl Pts',(70.9752141041518,14.2127944455839,12.));
#114678=CARTESIAN_POINT('Ctrl Pts',(70.9961606350861,14.2259703171737,0.));
#114679=CARTESIAN_POINT('Ctrl Pts',(70.9961606350861,14.2259703171737,12.));
#114680=CARTESIAN_POINT('Ctrl Pts',(71.0171289037488,14.2391879799062,0.));
#114681=CARTESIAN_POINT('Ctrl Pts',(71.0171289037488,14.2391879799062,12.));
#114682=CARTESIAN_POINT('Ctrl Pts',(71.0381187861588,14.2524474231733,0.));
#114683=CARTESIAN_POINT('Ctrl Pts',(71.0381187861588,14.2524474231733,12.));
#114684=CARTESIAN_POINT('Ctrl Pts',(71.0591301588231,14.2657486363139,0.));
#114685=CARTESIAN_POINT('Ctrl Pts',(71.0591301588231,14.2657486363139,12.));
#114686=CARTESIAN_POINT('Ctrl Pts',(71.0801628987332,14.2790916086133,0.));
#114687=CARTESIAN_POINT('Ctrl Pts',(71.0801628987332,14.2790916086133,12.));
#114688=CARTESIAN_POINT('Ctrl Pts',(71.1012168833643,14.2924763293105,0.));
#114689=CARTESIAN_POINT('Ctrl Pts',(71.1012168833643,14.2924763293105,12.));
#114690=CARTESIAN_POINT('Ctrl Pts',(71.1222919906727,14.3059027875994,0.));
#114691=CARTESIAN_POINT('Ctrl Pts',(71.1222919906727,14.3059027875994,12.));
#114692=CARTESIAN_POINT('Ctrl Pts',(71.1433880990929,14.3193709726294,0.));
#114693=CARTESIAN_POINT('Ctrl Pts',(71.1433880990929,14.3193709726294,12.));
#114694=CARTESIAN_POINT('Ctrl Pts',(71.1645050875308,14.332880873499,0.));
#114695=CARTESIAN_POINT('Ctrl Pts',(71.1645050875308,14.332880873499,12.));
#114696=CARTESIAN_POINT('Ctrl Pts',(71.1856428353593,14.3464324792534,0.));
#114697=CARTESIAN_POINT('Ctrl Pts',(71.1856428353593,14.3464324792534,12.));
#114698=CARTESIAN_POINT('Ctrl Pts',(71.2068012224174,14.3600257788924,0.));
#114699=CARTESIAN_POINT('Ctrl Pts',(71.2068012224174,14.3600257788924,12.));
#114700=CARTESIAN_POINT('Ctrl Pts',(71.2279801290084,14.3736607613722,0.));
#114701=CARTESIAN_POINT('Ctrl Pts',(71.2279801290084,14.3736607613722,12.));
#114702=CARTESIAN_POINT('Ctrl Pts',(71.2491794358958,14.3873374156056,0.));
#114703=CARTESIAN_POINT('Ctrl Pts',(71.2491794358958,14.3873374156056,12.));
#114704=CARTESIAN_POINT('Ctrl Pts',(71.2703990242988,14.401055730457,0.));
#114705=CARTESIAN_POINT('Ctrl Pts',(71.2703990242988,14.401055730457,12.));
#114706=CARTESIAN_POINT('Ctrl Pts',(71.2916387758861,14.4148156947384,0.));
#114707=CARTESIAN_POINT('Ctrl Pts',(71.2916387758861,14.4148156947384,12.));
#114708=CARTESIAN_POINT('Ctrl Pts',(71.312898572777,14.4286172972167,0.));
#114709=CARTESIAN_POINT('Ctrl Pts',(71.312898572777,14.4286172972167,12.));
#114710=CARTESIAN_POINT('Ctrl Pts',(71.3341782975386,14.4424605266165,0.));
#114711=CARTESIAN_POINT('Ctrl Pts',(71.3341782975386,14.4424605266165,12.));
#114712=CARTESIAN_POINT('Ctrl Pts',(71.3554778331835,14.4563453716204,0.));
#114713=CARTESIAN_POINT('Ctrl Pts',(71.3554778331835,14.4563453716204,12.));
#114714=CARTESIAN_POINT('Ctrl Pts',(71.376797063165,14.4702718208651,0.));
#114715=CARTESIAN_POINT('Ctrl Pts',(71.376797063165,14.4702718208651,12.));
#114716=CARTESIAN_POINT('Ctrl Pts',(71.3981358713723,14.4842398629355,0.));
#114717=CARTESIAN_POINT('Ctrl Pts',(71.3981358713723,14.4842398629355,12.));
#114718=CARTESIAN_POINT('Ctrl Pts',(71.4194941421292,14.4982494863718,0.));
#114719=CARTESIAN_POINT('Ctrl Pts',(71.4194941421292,14.4982494863718,12.));
#114720=CARTESIAN_POINT('Ctrl Pts',(71.4408717601923,14.5123006796728,0.));
#114721=CARTESIAN_POINT('Ctrl Pts',(71.4408717601923,14.5123006796728,12.));
#114722=CARTESIAN_POINT('Ctrl Pts',(71.4622686107475,14.5263934312969,0.));
#114723=CARTESIAN_POINT('Ctrl Pts',(71.4622686107475,14.5263934312969,12.));
#114724=CARTESIAN_POINT('Ctrl Pts',(71.4836845794048,14.540527729659,0.));
#114725=CARTESIAN_POINT('Ctrl Pts',(71.4836845794048,14.540527729659,12.));
#114726=CARTESIAN_POINT('Ctrl Pts',(71.5051195521909,14.5547035631234,0.));
#114727=CARTESIAN_POINT('Ctrl Pts',(71.5051195521909,14.5547035631234,12.));
#114728=CARTESIAN_POINT('Ctrl Pts',(71.5265734155498,14.5689209200091,0.));
#114729=CARTESIAN_POINT('Ctrl Pts',(71.5265734155498,14.5689209200091,12.));
#114730=CARTESIAN_POINT('Ctrl Pts',(71.5480460563447,14.5831797885952,0.));
#114731=CARTESIAN_POINT('Ctrl Pts',(71.5480460563447,14.5831797885952,12.));
#114732=CARTESIAN_POINT('Ctrl Pts',(71.5695373618562,14.597480157121,0.));
#114733=CARTESIAN_POINT('Ctrl Pts',(71.5695373618562,14.597480157121,12.));
#114734=CARTESIAN_POINT('Ctrl Pts',(71.5910472197813,14.6118220137849,0.));
#114735=CARTESIAN_POINT('Ctrl Pts',(71.5910472197813,14.6118220137849,12.));
#114736=CARTESIAN_POINT('Ctrl Pts',(71.612575518229,14.626205346737,0.));
#114737=CARTESIAN_POINT('Ctrl Pts',(71.612575518229,14.626205346737,12.));
#114738=CARTESIAN_POINT('Ctrl Pts',(71.6341221457169,14.6406301440814,0.));
#114739=CARTESIAN_POINT('Ctrl Pts',(71.6341221457169,14.6406301440814,12.));
#114740=CARTESIAN_POINT('Ctrl Pts',(71.6556869911662,14.6550963938829,0.));
#114741=CARTESIAN_POINT('Ctrl Pts',(71.6556869911662,14.6550963938829,12.));
#114742=CARTESIAN_POINT('Ctrl Pts',(71.6772699438963,14.6696040841678,0.));
#114743=CARTESIAN_POINT('Ctrl Pts',(71.6772699438963,14.6696040841678,12.));
#114744=CARTESIAN_POINT('Ctrl Pts',(71.6988708936172,14.6841532029232,0.));
#114745=CARTESIAN_POINT('Ctrl Pts',(71.6988708936172,14.6841532029232,12.));
#114746=CARTESIAN_POINT('Ctrl Pts',(71.7204897304194,14.6987437380901,0.));
#114747=CARTESIAN_POINT('Ctrl Pts',(71.7204897304194,14.6987437380901,12.));
#114748=CARTESIAN_POINT('Ctrl Pts',(71.7421263447719,14.7133756775626,0.));
#114749=CARTESIAN_POINT('Ctrl Pts',(71.7421263447719,14.7133756775626,12.));
#114750=CARTESIAN_POINT('Ctrl Pts',(71.7637806275328,14.7280490091957,0.));
#114751=CARTESIAN_POINT('Ctrl Pts',(71.7637806275328,14.7280490091957,12.));
#114752=CARTESIAN_POINT('Ctrl Pts',(71.7854524699569,14.7427637208073,0.));
#114753=CARTESIAN_POINT('Ctrl Pts',(71.7854524699569,14.7427637208073,12.));
#114754=CARTESIAN_POINT('Ctrl Pts',(71.8071417637017,14.7575198001776,0.));
#114755=CARTESIAN_POINT('Ctrl Pts',(71.8071417637017,14.7575198001776,12.));
#114756=CARTESIAN_POINT('Ctrl Pts',(71.8288484008333,14.7723172350451,0.));
#114757=CARTESIAN_POINT('Ctrl Pts',(71.8288484008333,14.7723172350451,12.));
#114758=CARTESIAN_POINT('Ctrl Pts',(71.8505722738272,14.7871560131017,0.));
#114759=CARTESIAN_POINT('Ctrl Pts',(71.8505722738272,14.7871560131017,12.));
#114760=CARTESIAN_POINT('Ctrl Pts',(71.8723132755446,14.8020361219998,0.));
#114761=CARTESIAN_POINT('Ctrl Pts',(71.8723132755446,14.8020361219998,12.));
#114762=CARTESIAN_POINT('Ctrl Pts',(71.8940712992109,14.8169575493557,0.));
#114763=CARTESIAN_POINT('Ctrl Pts',(71.8940712992109,14.8169575493557,12.));
#114764=CARTESIAN_POINT('Ctrl Pts',(71.9158462383914,14.8319202827482,0.));
#114765=CARTESIAN_POINT('Ctrl Pts',(71.9158462383914,14.8319202827482,12.));
#114766=CARTESIAN_POINT('Ctrl Pts',(71.9376379869678,14.8469243097163,0.));
#114767=CARTESIAN_POINT('Ctrl Pts',(71.9376379869678,14.8469243097163,12.));
#114768=CARTESIAN_POINT('Ctrl Pts',(71.9594464391078,14.8619696177507,0.));
#114769=CARTESIAN_POINT('Ctrl Pts',(71.9594464391078,14.8619696177507,12.));
#114770=CARTESIAN_POINT('Ctrl Pts',(71.9812714893102,14.8770561943014,0.));
#114771=CARTESIAN_POINT('Ctrl Pts',(71.9812714893102,14.8770561943014,12.));
#114772=CARTESIAN_POINT('Ctrl Pts',(72.0031130324529,14.8921840267832,0.));
#114773=CARTESIAN_POINT('Ctrl Pts',(72.0031130324529,14.8921840267832,12.));
#114774=CARTESIAN_POINT('Ctrl Pts',(72.0249709638422,14.9073531025764,0.));
#114775=CARTESIAN_POINT('Ctrl Pts',(72.0249709638422,14.9073531025764,12.));
#114776=CARTESIAN_POINT('Ctrl Pts',(72.0468451792505,14.9225634090268,0.));
#114777=CARTESIAN_POINT('Ctrl Pts',(72.0468451792505,14.9225634090268,12.));
#114778=CARTESIAN_POINT('Ctrl Pts',(72.0687355749807,14.9378149334388,0.));
#114779=CARTESIAN_POINT('Ctrl Pts',(72.0687355749807,14.9378149334388,12.));
#114780=CARTESIAN_POINT('Ctrl Pts',(72.0906420478076,14.9531076630768,0.));
#114781=CARTESIAN_POINT('Ctrl Pts',(72.0906420478076,14.9531076630768,12.));
#114782=CARTESIAN_POINT('Ctrl Pts',(72.112564494854,14.9684415851698,0.));
#114783=CARTESIAN_POINT('Ctrl Pts',(72.112564494854,14.9684415851698,12.));
#114784=CARTESIAN_POINT('Ctrl Pts',(72.1345028134777,14.9838166869107,0.));
#114785=CARTESIAN_POINT('Ctrl Pts',(72.1345028134777,14.9838166869107,12.));
#114786=CARTESIAN_POINT('Ctrl Pts',(72.1564569011669,14.9992329554537,0.));
#114787=CARTESIAN_POINT('Ctrl Pts',(72.1564569011669,14.9992329554537,12.));
#114788=CARTESIAN_POINT('Ctrl Pts',(72.1784266553953,15.0146903779062,0.));
#114789=CARTESIAN_POINT('Ctrl Pts',(72.1784266553953,15.0146903779062,12.));
#114790=CARTESIAN_POINT('Ctrl Pts',(72.2004119736115,15.0301889413257,0.));
#114791=CARTESIAN_POINT('Ctrl Pts',(72.2004119736115,15.0301889413257,12.));
#114792=CARTESIAN_POINT('Ctrl Pts',(72.2224127535415,15.0457286327331,0.));
#114793=CARTESIAN_POINT('Ctrl Pts',(72.2224127535415,15.0457286327331,12.));
#114794=CARTESIAN_POINT('Ctrl Pts',(72.2444288934262,15.0613094391189,0.));
#114795=CARTESIAN_POINT('Ctrl Pts',(72.2444288934262,15.0613094391189,12.));
#114796=CARTESIAN_POINT('Ctrl Pts',(72.2664602922852,15.0769313474477,0.));
#114797=CARTESIAN_POINT('Ctrl Pts',(72.2664602922852,15.0769313474477,12.));
#114798=CARTESIAN_POINT('Ctrl Pts',(72.2885068501628,15.092594344659,0.));
#114799=CARTESIAN_POINT('Ctrl Pts',(72.2885068501628,15.092594344659,12.));
#114800=CARTESIAN_POINT('Ctrl Pts',(72.3105684683944,15.1082984176649,0.));
#114801=CARTESIAN_POINT('Ctrl Pts',(72.3105684683944,15.1082984176649,12.));
#114802=CARTESIAN_POINT('Ctrl Pts',(72.3326450490177,15.124043553347,0.));
#114803=CARTESIAN_POINT('Ctrl Pts',(72.3326450490177,15.124043553347,12.));
#114804=CARTESIAN_POINT('Ctrl Pts',(72.3547364941969,15.1398297385506,0.));
#114805=CARTESIAN_POINT('Ctrl Pts',(72.3547364941969,15.1398297385506,12.));
#114806=CARTESIAN_POINT('Ctrl Pts',(72.376842705589,15.1556569600745,0.));
#114807=CARTESIAN_POINT('Ctrl Pts',(72.376842705589,15.1556569600745,12.));
#114808=CARTESIAN_POINT('Ctrl Pts',(72.3989635838492,15.1715252046606,0.));
#114809=CARTESIAN_POINT('Ctrl Pts',(72.3989635838492,15.1715252046606,12.));
#114810=CARTESIAN_POINT('Ctrl Pts',(72.421099027786,15.1874344589726,0.));
#114811=CARTESIAN_POINT('Ctrl Pts',(72.421099027786,15.1874344589726,12.));
#114812=CARTESIAN_POINT('Ctrl Pts',(72.4432489350471,15.2033847096091,0.));
#114813=CARTESIAN_POINT('Ctrl Pts',(72.4432489350471,15.2033847096091,12.));
#114814=CARTESIAN_POINT('Ctrl Pts',(72.4654132036428,15.2193759431373,0.));
#114815=CARTESIAN_POINT('Ctrl Pts',(72.4654132036428,15.2193759431373,12.));
#114816=CARTESIAN_POINT('Ctrl Pts',(72.4875917332762,15.235408146116,0.));
#114817=CARTESIAN_POINT('Ctrl Pts',(72.4875917332762,15.235408146116,12.));
#114818=CARTESIAN_POINT('Ctrl Pts',(72.5097844266075,15.2514813051172,0.));
#114819=CARTESIAN_POINT('Ctrl Pts',(72.5097844266075,15.2514813051172,12.));
#114820=CARTESIAN_POINT('Ctrl Pts',(72.5319911908917,15.2675954067479,0.));
#114821=CARTESIAN_POINT('Ctrl Pts',(72.5319911908917,15.2675954067479,12.));
#114822=CARTESIAN_POINT('Ctrl Pts',(72.5542119383642,15.2837504376536,0.));
#114823=CARTESIAN_POINT('Ctrl Pts',(72.5542119383642,15.2837504376536,12.));
#114824=CARTESIAN_POINT('Ctrl Pts',(72.5764465826224,15.2999463844661,0.));
#114825=CARTESIAN_POINT('Ctrl Pts',(72.5764465826224,15.2999463844661,12.));
#114826=CARTESIAN_POINT('Ctrl Pts',(72.5986950357677,15.3161832337594,0.));
#114827=CARTESIAN_POINT('Ctrl Pts',(72.5986950357677,15.3161832337594,12.));
#114828=CARTESIAN_POINT('Ctrl Pts',(72.6209572051042,15.3324609719956,0.));
#114829=CARTESIAN_POINT('Ctrl Pts',(72.6209572051042,15.3324609719956,12.));
#114830=CARTESIAN_POINT('Ctrl Pts',(72.6432329903553,15.3487795854745,0.));
#114831=CARTESIAN_POINT('Ctrl Pts',(72.6432329903553,15.3487795854745,12.));
#114832=CARTESIAN_POINT('Ctrl Pts',(72.6655222797801,15.3651390602666,0.));
#114833=CARTESIAN_POINT('Ctrl Pts',(72.6655222797801,15.3651390602666,12.));
#114834=CARTESIAN_POINT('Ctrl Pts',(72.687824955772,15.3815393822736,0.));
#114835=CARTESIAN_POINT('Ctrl Pts',(72.687824955772,15.3815393822736,12.));
#114836=CARTESIAN_POINT('Ctrl Pts',(72.7101409017716,15.3979805373174,0.));
#114837=CARTESIAN_POINT('Ctrl Pts',(72.7101409017716,15.3979805373174,12.));
#114838=CARTESIAN_POINT('Ctrl Pts',(72.7324700089712,15.4144625111944,0.));
#114839=CARTESIAN_POINT('Ctrl Pts',(72.7324700089712,15.4144625111944,12.));
#114840=CARTESIAN_POINT('Ctrl Pts',(72.7548121825342,15.4309852897844,0.));
#114841=CARTESIAN_POINT('Ctrl Pts',(72.7548121825342,15.4309852897844,12.));
#114842=CARTESIAN_POINT('Ctrl Pts',(72.777167349421,15.4475488590244,0.));
#114843=CARTESIAN_POINT('Ctrl Pts',(72.777167349421,15.4475488590244,12.));
#114844=CARTESIAN_POINT('Ctrl Pts',(72.7995354603795,15.4641532053281,0.));
#114845=CARTESIAN_POINT('Ctrl Pts',(72.7995354603795,15.4641532053281,12.));
#114846=CARTESIAN_POINT('Ctrl Pts',(72.8219164843279,15.4807983165804,0.));
#114847=CARTESIAN_POINT('Ctrl Pts',(72.8219164843279,15.4807983165804,12.));
#114848=CARTESIAN_POINT('Ctrl Pts',(72.8398316205897,15.494147009702,0.));
#114849=CARTESIAN_POINT('Ctrl Pts',(72.8398316205897,15.494147009702,12.));
#114850=CARTESIAN_POINT('Ctrl Pts',(72.8532737731759,15.5041768663999,0.));
#114851=CARTESIAN_POINT('Ctrl Pts',(72.8532737731759,15.5041768663999,12.));
#114852=CARTESIAN_POINT('Ctrl Pts',(72.8622377860824,15.5108715869141,0.));
#114853=CARTESIAN_POINT('Ctrl Pts',(72.8622377860824,15.5108715869141,12.));
#114854=CARTESIAN_POINT('Ctrl Pts',(72.8667204369977,15.5142209845168,0.));
#114855=CARTESIAN_POINT('Ctrl Pts',(72.8667204369977,15.5142209845168,12.));
#114856=CARTESIAN_POINT('',(68.7831490561748,12.9953224629497,0.));
#114857=CARTESIAN_POINT('Ctrl Pts',(68.7831490561748,12.9953224629497,0.));
#114858=CARTESIAN_POINT('Ctrl Pts',(68.7866525680193,12.9969981460277,0.));
#114859=CARTESIAN_POINT('Ctrl Pts',(68.7936635625545,13.0003537683055,0.));
#114860=CARTESIAN_POINT('Ctrl Pts',(68.804191966902,13.0053999700875,0.));
#114861=CARTESIAN_POINT('Ctrl Pts',(68.8182536653656,13.0121537768946,0.));
#114862=CARTESIAN_POINT('Ctrl Pts',(68.8358704887468,13.0206386039691,0.));
#114863=CARTESIAN_POINT('Ctrl Pts',(68.8535269726793,13.0291660060107,0.));
#114864=CARTESIAN_POINT('Ctrl Pts',(68.8712230321906,13.0377359881875,0.));
#114865=CARTESIAN_POINT('Ctrl Pts',(68.8889585151585,13.0463485518207,0.));
#114866=CARTESIAN_POINT('Ctrl Pts',(68.9067332040985,13.0550036938813,0.));
#114867=CARTESIAN_POINT('Ctrl Pts',(68.9245468449945,13.0637014089029,0.));
#114868=CARTESIAN_POINT('Ctrl Pts',(68.9423991694492,13.072441690283,0.));
#114869=CARTESIAN_POINT('Ctrl Pts',(68.9602899187573,13.0812245317808,0.));
#114870=CARTESIAN_POINT('Ctrl Pts',(68.9782188692581,13.090049929053,0.));
#114871=CARTESIAN_POINT('Ctrl Pts',(68.9961858241519,13.0989178791834,0.));
#114872=CARTESIAN_POINT('Ctrl Pts',(69.0141906015113,13.1078283799722,0.));
#114873=CARTESIAN_POINT('Ctrl Pts',(69.0322330243348,13.1167814293497,0.));
#114874=CARTESIAN_POINT('Ctrl Pts',(69.0503129081817,13.1257770246386,0.));
#114875=CARTESIAN_POINT('Ctrl Pts',(69.0684300549477,13.1348151621834,0.));
#114876=CARTESIAN_POINT('Ctrl Pts',(69.0865842593102,13.1438958377404,0.));
#114877=CARTESIAN_POINT('Ctrl Pts',(69.1047753127643,13.1530190467183,0.));
#114878=CARTESIAN_POINT('Ctrl Pts',(69.1230030082573,13.1621847844528,0.));
#114879=CARTESIAN_POINT('Ctrl Pts',(69.1412671454564,13.1713930465133,0.));
#114880=CARTESIAN_POINT('Ctrl Pts',(69.1595675305245,13.1806438286934,0.));
#114881=CARTESIAN_POINT('Ctrl Pts',(69.1779039735996,13.1899371268683,0.));
#114882=CARTESIAN_POINT('Ctrl Pts',(69.1962762870527,13.1992729368929,0.));
#114883=CARTESIAN_POINT('Ctrl Pts',(69.2146842833537,13.2086512544735,0.));
#114884=CARTESIAN_POINT('Ctrl Pts',(69.2331277732861,13.2180720750594,0.));
#114885=CARTESIAN_POINT('Ctrl Pts',(69.2516065668844,13.2275353939051,0.));
#114886=CARTESIAN_POINT('Ctrl Pts',(69.270120474245,13.237041206122,0.));
#114887=CARTESIAN_POINT('Ctrl Pts',(69.2886693063182,13.2465895067262,0.));
#114888=CARTESIAN_POINT('Ctrl Pts',(69.3072528758518,13.2561802906896,0.));
#114889=CARTESIAN_POINT('Ctrl Pts',(69.3258709977382,13.265813552961,0.));
#114890=CARTESIAN_POINT('Ctrl Pts',(69.3445234885065,13.2754892884433,0.));
#114891=CARTESIAN_POINT('Ctrl Pts',(69.3632101660066,13.2852074919766,0.));
#114892=CARTESIAN_POINT('Ctrl Pts',(69.3819308490422,13.2949681583167,0.));
#114893=CARTESIAN_POINT('Ctrl Pts',(69.4006853569511,13.3047712821051,0.));
#114894=CARTESIAN_POINT('Ctrl Pts',(69.4194735096265,13.3146168578743,0.));
#114895=CARTESIAN_POINT('Ctrl Pts',(69.4382951276998,13.3245048800643,0.));
#114896=CARTESIAN_POINT('Ctrl Pts',(69.4571500326673,13.3344353430313,0.));
#114897=CARTESIAN_POINT('Ctrl Pts',(69.4760380470365,13.3444082410543,0.));
#114898=CARTESIAN_POINT('Ctrl Pts',(69.4949589944606,13.3544235683394,0.));
#114899=CARTESIAN_POINT('Ctrl Pts',(69.5139126996675,13.3644813190219,0.));
#114900=CARTESIAN_POINT('Ctrl Pts',(69.5328989883885,13.3745814871665,0.));
#114901=CARTESIAN_POINT('Ctrl Pts',(69.5519176872862,13.3847240667628,0.));
#114902=CARTESIAN_POINT('Ctrl Pts',(69.5709686238724,13.3949090517177,0.));
#114903=CARTESIAN_POINT('Ctrl Pts',(69.5900516264553,13.40513643585,0.));
#114904=CARTESIAN_POINT('Ctrl Pts',(69.6091665241765,13.4154062129002,0.));
#114905=CARTESIAN_POINT('Ctrl Pts',(69.6283131470273,13.4257183765341,0.));
#114906=CARTESIAN_POINT('Ctrl Pts',(69.6474913258675,13.4360729203442,0.));
#114907=CARTESIAN_POINT('Ctrl Pts',(69.666700892444,13.4464698378453,0.));
#114908=CARTESIAN_POINT('Ctrl Pts',(69.6859416793885,13.456909122476,0.));
#114909=CARTESIAN_POINT('Ctrl Pts',(69.7052135201998,13.4673907676044,0.));
#114910=CARTESIAN_POINT('Ctrl Pts',(69.724516249225,13.4779147665285,0.));
#114911=CARTESIAN_POINT('Ctrl Pts',(69.7438497016406,13.4884811124748,0.));
#114912=CARTESIAN_POINT('Ctrl Pts',(69.7632137134249,13.4990897985905,0.));
#114913=CARTESIAN_POINT('Ctrl Pts',(69.7826081213576,13.5097408179479,0.));
#114914=CARTESIAN_POINT('Ctrl Pts',(69.8020327630205,13.5204341635507,0.));
#114915=CARTESIAN_POINT('Ctrl Pts',(69.8214874767944,13.5311698283339,0.));
#114916=CARTESIAN_POINT('Ctrl Pts',(69.840972101856,13.5419478051625,0.));
#114917=CARTESIAN_POINT('Ctrl Pts',(69.8604864781706,13.5527680868255,0.));
#114918=CARTESIAN_POINT('Ctrl Pts',(69.8800304464882,13.5636306660422,0.));
#114919=CARTESIAN_POINT('Ctrl Pts',(69.8996038483361,13.5745355354657,0.));
#114920=CARTESIAN_POINT('Ctrl Pts',(69.9192065260108,13.5854826876835,0.));
#114921=CARTESIAN_POINT('Ctrl Pts',(69.9388383225648,13.5964721152135,0.));
#114922=CARTESIAN_POINT('Ctrl Pts',(69.9584990817974,13.6075038104999,0.));
#114923=CARTESIAN_POINT('Ctrl Pts',(69.9781886482528,13.6185777659198,0.));
#114924=CARTESIAN_POINT('Ctrl Pts',(69.9979068672153,13.6296939737865,0.));
#114925=CARTESIAN_POINT('Ctrl Pts',(70.0176535847049,13.6408524263496,0.));
#114926=CARTESIAN_POINT('Ctrl Pts',(70.0374286474677,13.6520531157907,0.));
#114927=CARTESIAN_POINT('Ctrl Pts',(70.0572319029676,13.6632960342196,0.));
#114928=CARTESIAN_POINT('Ctrl Pts',(70.0770631993856,13.674581173683,0.));
#114929=CARTESIAN_POINT('Ctrl Pts',(70.0969223856136,13.6859085261653,0.));
#114930=CARTESIAN_POINT('Ctrl Pts',(70.1168093112486,13.6972780835897,0.));
#114931=CARTESIAN_POINT('Ctrl Pts',(70.1367238265825,13.7086898378122,0.));
#114932=CARTESIAN_POINT('Ctrl Pts',(70.156665782595,13.7201437806199,0.));
#114933=CARTESIAN_POINT('Ctrl Pts',(70.1766350309518,13.7316399037393,0.));
#114934=CARTESIAN_POINT('Ctrl Pts',(70.1966314239995,13.7431781988365,0.));
#114935=CARTESIAN_POINT('Ctrl Pts',(70.2166548147604,13.7547586575181,0.));
#114936=CARTESIAN_POINT('Ctrl Pts',(70.2367050569216,13.7663812713243,0.));
#114937=CARTESIAN_POINT('Ctrl Pts',(70.2567820048303,13.7780460317294,0.));
#114938=CARTESIAN_POINT('Ctrl Pts',(70.2768855134947,13.7897529301491,0.));
#114939=CARTESIAN_POINT('Ctrl Pts',(70.2970154385774,13.8015019579414,0.));
#114940=CARTESIAN_POINT('Ctrl Pts',(70.3171716363897,13.8132931064064,0.));
#114941=CARTESIAN_POINT('Ctrl Pts',(70.3373539638809,13.8251263667791,0.));
#114942=CARTESIAN_POINT('Ctrl Pts',(70.3575622786335,13.8370017302309,0.));
#114943=CARTESIAN_POINT('Ctrl Pts',(70.3777964388632,13.8489191878767,0.));
#114944=CARTESIAN_POINT('Ctrl Pts',(70.3980563034133,13.8608787307752,0.));
#114945=CARTESIAN_POINT('Ctrl Pts',(70.41834173175,13.8728803499287,0.));
#114946=CARTESIAN_POINT('Ctrl Pts',(70.4386525839521,13.8849240362763,0.));
#114947=CARTESIAN_POINT('Ctrl Pts',(70.4589887207073,13.8970097806954,0.));
#114948=CARTESIAN_POINT('Ctrl Pts',(70.4793500033124,13.9091375740088,0.));
#114949=CARTESIAN_POINT('Ctrl Pts',(70.4997362936673,13.9213074069853,0.));
#114950=CARTESIAN_POINT('Ctrl Pts',(70.520147454271,13.9335192703388,0.));
#114951=CARTESIAN_POINT('Ctrl Pts',(70.5405833482112,13.9457731547215,0.));
#114952=CARTESIAN_POINT('Ctrl Pts',(70.5610438391612,13.958069050726,0.));
#114953=CARTESIAN_POINT('Ctrl Pts',(70.5815287913784,13.9704069488917,0.));
#114954=CARTESIAN_POINT('Ctrl Pts',(70.6020380697005,13.9827868397057,0.));
#114955=CARTESIAN_POINT('Ctrl Pts',(70.6225715395394,13.9952087136018,0.));
#114956=CARTESIAN_POINT('Ctrl Pts',(70.6431290668745,14.0076725609537,0.));
#114957=CARTESIAN_POINT('Ctrl Pts',(70.6637105182484,14.020178372077,0.));
#114958=CARTESIAN_POINT('Ctrl Pts',(70.6843157607668,14.0327261372362,0.));
#114959=CARTESIAN_POINT('Ctrl Pts',(70.7049446620928,14.0453158466451,0.));
#114960=CARTESIAN_POINT('Ctrl Pts',(70.7255970904436,14.0579474904657,0.));
#114961=CARTESIAN_POINT('Ctrl Pts',(70.7462729145807,14.0706210588016,0.));
#114962=CARTESIAN_POINT('Ctrl Pts',(70.7669720038077,14.0833365416996,0.));
#114963=CARTESIAN_POINT('Ctrl Pts',(70.7876942279697,14.0960939291569,0.));
#114964=CARTESIAN_POINT('Ctrl Pts',(70.8084394574493,14.1088932111214,0.));
#114965=CARTESIAN_POINT('Ctrl Pts',(70.8292075631621,14.1217343774913,0.));
#114966=CARTESIAN_POINT('Ctrl Pts',(70.8499984165489,14.1346174181079,0.));
#114967=CARTESIAN_POINT('Ctrl Pts',(70.8708118895715,14.1475423227568,0.));
#114968=CARTESIAN_POINT('Ctrl Pts',(70.8916478547132,14.1605090811754,0.));
#114969=CARTESIAN_POINT('Ctrl Pts',(70.9125061849745,14.1735176830533,0.));
#114970=CARTESIAN_POINT('Ctrl Pts',(70.9333867538704,14.1865681180321,0.));
#114971=CARTESIAN_POINT('Ctrl Pts',(70.9542894354216,14.1996603756982,0.));
#114972=CARTESIAN_POINT('Ctrl Pts',(70.9752141041518,14.2127944455839,0.));
#114973=CARTESIAN_POINT('Ctrl Pts',(70.9961606350861,14.2259703171737,0.));
#114974=CARTESIAN_POINT('Ctrl Pts',(71.0171289037488,14.2391879799062,0.));
#114975=CARTESIAN_POINT('Ctrl Pts',(71.0381187861588,14.2524474231733,0.));
#114976=CARTESIAN_POINT('Ctrl Pts',(71.0591301588231,14.2657486363139,0.));
#114977=CARTESIAN_POINT('Ctrl Pts',(71.0801628987332,14.2790916086133,0.));
#114978=CARTESIAN_POINT('Ctrl Pts',(71.1012168833643,14.2924763293105,0.));
#114979=CARTESIAN_POINT('Ctrl Pts',(71.1222919906727,14.3059027875994,0.));
#114980=CARTESIAN_POINT('Ctrl Pts',(71.1433880990929,14.3193709726294,0.));
#114981=CARTESIAN_POINT('Ctrl Pts',(71.1645050875308,14.332880873499,0.));
#114982=CARTESIAN_POINT('Ctrl Pts',(71.1856428353593,14.3464324792534,0.));
#114983=CARTESIAN_POINT('Ctrl Pts',(71.2068012224174,14.3600257788924,0.));
#114984=CARTESIAN_POINT('Ctrl Pts',(71.2279801290084,14.3736607613722,0.));
#114985=CARTESIAN_POINT('Ctrl Pts',(71.2491794358958,14.3873374156056,0.));
#114986=CARTESIAN_POINT('Ctrl Pts',(71.2703990242988,14.401055730457,0.));
#114987=CARTESIAN_POINT('Ctrl Pts',(71.2916387758861,14.4148156947384,0.));
#114988=CARTESIAN_POINT('Ctrl Pts',(71.312898572777,14.4286172972167,0.));
#114989=CARTESIAN_POINT('Ctrl Pts',(71.3341782975386,14.4424605266165,0.));
#114990=CARTESIAN_POINT('Ctrl Pts',(71.3554778331835,14.4563453716204,0.));
#114991=CARTESIAN_POINT('Ctrl Pts',(71.376797063165,14.4702718208651,0.));
#114992=CARTESIAN_POINT('Ctrl Pts',(71.3981358713723,14.4842398629355,0.));
#114993=CARTESIAN_POINT('Ctrl Pts',(71.4194941421292,14.4982494863718,0.));
#114994=CARTESIAN_POINT('Ctrl Pts',(71.4408717601923,14.5123006796728,0.));
#114995=CARTESIAN_POINT('Ctrl Pts',(71.4622686107475,14.5263934312969,0.));
#114996=CARTESIAN_POINT('Ctrl Pts',(71.4836845794048,14.540527729659,0.));
#114997=CARTESIAN_POINT('Ctrl Pts',(71.5051195521909,14.5547035631234,0.));
#114998=CARTESIAN_POINT('Ctrl Pts',(71.5265734155498,14.5689209200091,0.));
#114999=CARTESIAN_POINT('Ctrl Pts',(71.5480460563447,14.5831797885952,0.));
#115000=CARTESIAN_POINT('Ctrl Pts',(71.5695373618562,14.597480157121,0.));
#115001=CARTESIAN_POINT('Ctrl Pts',(71.5910472197813,14.6118220137849,0.));
#115002=CARTESIAN_POINT('Ctrl Pts',(71.612575518229,14.626205346737,0.));
#115003=CARTESIAN_POINT('Ctrl Pts',(71.6341221457169,14.6406301440814,0.));
#115004=CARTESIAN_POINT('Ctrl Pts',(71.6556869911662,14.6550963938829,0.));
#115005=CARTESIAN_POINT('Ctrl Pts',(71.6772699438963,14.6696040841678,0.));
#115006=CARTESIAN_POINT('Ctrl Pts',(71.6988708936172,14.6841532029232,0.));
#115007=CARTESIAN_POINT('Ctrl Pts',(71.7204897304194,14.6987437380901,0.));
#115008=CARTESIAN_POINT('Ctrl Pts',(71.7421263447719,14.7133756775626,0.));
#115009=CARTESIAN_POINT('Ctrl Pts',(71.7637806275328,14.7280490091957,0.));
#115010=CARTESIAN_POINT('Ctrl Pts',(71.7854524699569,14.7427637208073,0.));
#115011=CARTESIAN_POINT('Ctrl Pts',(71.8071417637017,14.7575198001776,0.));
#115012=CARTESIAN_POINT('Ctrl Pts',(71.8288484008333,14.7723172350451,0.));
#115013=CARTESIAN_POINT('Ctrl Pts',(71.8505722738272,14.7871560131017,0.));
#115014=CARTESIAN_POINT('Ctrl Pts',(71.8723132755446,14.8020361219998,0.));
#115015=CARTESIAN_POINT('Ctrl Pts',(71.8940712992109,14.8169575493557,0.));
#115016=CARTESIAN_POINT('Ctrl Pts',(71.9158462383914,14.8319202827482,0.));
#115017=CARTESIAN_POINT('Ctrl Pts',(71.9376379869678,14.8469243097163,0.));
#115018=CARTESIAN_POINT('Ctrl Pts',(71.9594464391078,14.8619696177507,0.));
#115019=CARTESIAN_POINT('Ctrl Pts',(71.9812714893102,14.8770561943014,0.));
#115020=CARTESIAN_POINT('Ctrl Pts',(72.0031130324529,14.8921840267832,0.));
#115021=CARTESIAN_POINT('Ctrl Pts',(72.0249709638422,14.9073531025764,0.));
#115022=CARTESIAN_POINT('Ctrl Pts',(72.0468451792505,14.9225634090268,0.));
#115023=CARTESIAN_POINT('Ctrl Pts',(72.0687355749807,14.9378149334388,0.));
#115024=CARTESIAN_POINT('Ctrl Pts',(72.0906420478076,14.9531076630768,0.));
#115025=CARTESIAN_POINT('Ctrl Pts',(72.112564494854,14.9684415851698,0.));
#115026=CARTESIAN_POINT('Ctrl Pts',(72.1345028134777,14.9838166869107,0.));
#115027=CARTESIAN_POINT('Ctrl Pts',(72.1564569011669,14.9992329554537,0.));
#115028=CARTESIAN_POINT('Ctrl Pts',(72.1784266553953,15.0146903779062,0.));
#115029=CARTESIAN_POINT('Ctrl Pts',(72.2004119736115,15.0301889413257,0.));
#115030=CARTESIAN_POINT('Ctrl Pts',(72.2224127535415,15.0457286327331,0.));
#115031=CARTESIAN_POINT('Ctrl Pts',(72.2444288934262,15.0613094391189,0.));
#115032=CARTESIAN_POINT('Ctrl Pts',(72.2664602922852,15.0769313474477,0.));
#115033=CARTESIAN_POINT('Ctrl Pts',(72.2885068501628,15.092594344659,0.));
#115034=CARTESIAN_POINT('Ctrl Pts',(72.3105684683944,15.1082984176649,0.));
#115035=CARTESIAN_POINT('Ctrl Pts',(72.3326450490177,15.124043553347,0.));
#115036=CARTESIAN_POINT('Ctrl Pts',(72.3547364941969,15.1398297385506,0.));
#115037=CARTESIAN_POINT('Ctrl Pts',(72.376842705589,15.1556569600745,0.));
#115038=CARTESIAN_POINT('Ctrl Pts',(72.3989635838492,15.1715252046606,0.));
#115039=CARTESIAN_POINT('Ctrl Pts',(72.421099027786,15.1874344589726,0.));
#115040=CARTESIAN_POINT('Ctrl Pts',(72.4432489350471,15.2033847096091,0.));
#115041=CARTESIAN_POINT('Ctrl Pts',(72.4654132036428,15.2193759431373,0.));
#115042=CARTESIAN_POINT('Ctrl Pts',(72.4875917332762,15.235408146116,0.));
#115043=CARTESIAN_POINT('Ctrl Pts',(72.5097844266075,15.2514813051172,0.));
#115044=CARTESIAN_POINT('Ctrl Pts',(72.5319911908917,15.2675954067479,0.));
#115045=CARTESIAN_POINT('Ctrl Pts',(72.5542119383642,15.2837504376536,0.));
#115046=CARTESIAN_POINT('Ctrl Pts',(72.5732713370618,15.297633502478,0.));
#115047=CARTESIAN_POINT('Ctrl Pts',(72.5878912620439,15.3082994603539,0.));
#115048=CARTESIAN_POINT('Ctrl Pts',(72.5980655789635,15.3157301930682,0.));
#115049=CARTESIAN_POINT('Ctrl Pts',(72.6037902604921,15.3199137230129,0.));
#115050=CARTESIAN_POINT('Ctrl Pts',(72.6050633494351,15.3208442077189,0.));
#115051=CARTESIAN_POINT('',(68.7831490561748,12.9953224629497,12.));
#115052=CARTESIAN_POINT('',(68.7831490561748,12.9953224629497,0.));
#115053=CARTESIAN_POINT('Ctrl Pts',(72.6050633494351,15.3208442077189,12.));
#115054=CARTESIAN_POINT('Ctrl Pts',(72.6037902604921,15.3199137230129,12.));
#115055=CARTESIAN_POINT('Ctrl Pts',(72.5980655789635,15.3157301930682,12.));
#115056=CARTESIAN_POINT('Ctrl Pts',(72.5878912620439,15.3082994603539,12.));
#115057=CARTESIAN_POINT('Ctrl Pts',(72.5732713370618,15.297633502478,12.));
#115058=CARTESIAN_POINT('Ctrl Pts',(72.5542119383642,15.2837504376536,12.));
#115059=CARTESIAN_POINT('Ctrl Pts',(72.5319911908917,15.2675954067479,12.));
#115060=CARTESIAN_POINT('Ctrl Pts',(72.5097844266075,15.2514813051172,12.));
#115061=CARTESIAN_POINT('Ctrl Pts',(72.4875917332762,15.235408146116,12.));
#115062=CARTESIAN_POINT('Ctrl Pts',(72.4654132036428,15.2193759431373,12.));
#115063=CARTESIAN_POINT('Ctrl Pts',(72.4432489350471,15.2033847096091,12.));
#115064=CARTESIAN_POINT('Ctrl Pts',(72.421099027786,15.1874344589726,12.));
#115065=CARTESIAN_POINT('Ctrl Pts',(72.3989635838492,15.1715252046606,12.));
#115066=CARTESIAN_POINT('Ctrl Pts',(72.376842705589,15.1556569600745,12.));
#115067=CARTESIAN_POINT('Ctrl Pts',(72.3547364941969,15.1398297385506,12.));
#115068=CARTESIAN_POINT('Ctrl Pts',(72.3326450490177,15.124043553347,12.));
#115069=CARTESIAN_POINT('Ctrl Pts',(72.3105684683944,15.1082984176649,12.));
#115070=CARTESIAN_POINT('Ctrl Pts',(72.2885068501628,15.092594344659,12.));
#115071=CARTESIAN_POINT('Ctrl Pts',(72.2664602922852,15.0769313474477,12.));
#115072=CARTESIAN_POINT('Ctrl Pts',(72.2444288934262,15.0613094391189,12.));
#115073=CARTESIAN_POINT('Ctrl Pts',(72.2224127535415,15.0457286327331,12.));
#115074=CARTESIAN_POINT('Ctrl Pts',(72.2004119736115,15.0301889413257,12.));
#115075=CARTESIAN_POINT('Ctrl Pts',(72.1784266553953,15.0146903779062,12.));
#115076=CARTESIAN_POINT('Ctrl Pts',(72.1564569011669,14.9992329554537,12.));
#115077=CARTESIAN_POINT('Ctrl Pts',(72.1345028134777,14.9838166869107,12.));
#115078=CARTESIAN_POINT('Ctrl Pts',(72.112564494854,14.9684415851698,12.));
#115079=CARTESIAN_POINT('Ctrl Pts',(72.0906420478076,14.9531076630768,12.));
#115080=CARTESIAN_POINT('Ctrl Pts',(72.0687355749807,14.9378149334388,12.));
#115081=CARTESIAN_POINT('Ctrl Pts',(72.0468451792505,14.9225634090268,12.));
#115082=CARTESIAN_POINT('Ctrl Pts',(72.0249709638422,14.9073531025764,12.));
#115083=CARTESIAN_POINT('Ctrl Pts',(72.0031130324529,14.8921840267832,12.));
#115084=CARTESIAN_POINT('Ctrl Pts',(71.9812714893102,14.8770561943014,12.));
#115085=CARTESIAN_POINT('Ctrl Pts',(71.9594464391078,14.8619696177507,12.));
#115086=CARTESIAN_POINT('Ctrl Pts',(71.9376379869678,14.8469243097163,12.));
#115087=CARTESIAN_POINT('Ctrl Pts',(71.9158462383914,14.8319202827482,12.));
#115088=CARTESIAN_POINT('Ctrl Pts',(71.8940712992109,14.8169575493557,12.));
#115089=CARTESIAN_POINT('Ctrl Pts',(71.8723132755446,14.8020361219998,12.));
#115090=CARTESIAN_POINT('Ctrl Pts',(71.8505722738272,14.7871560131017,12.));
#115091=CARTESIAN_POINT('Ctrl Pts',(71.8288484008333,14.7723172350451,12.));
#115092=CARTESIAN_POINT('Ctrl Pts',(71.8071417637017,14.7575198001776,12.));
#115093=CARTESIAN_POINT('Ctrl Pts',(71.7854524699569,14.7427637208073,12.));
#115094=CARTESIAN_POINT('Ctrl Pts',(71.7637806275328,14.7280490091957,12.));
#115095=CARTESIAN_POINT('Ctrl Pts',(71.7421263447719,14.7133756775626,12.));
#115096=CARTESIAN_POINT('Ctrl Pts',(71.7204897304194,14.6987437380901,12.));
#115097=CARTESIAN_POINT('Ctrl Pts',(71.6988708936172,14.6841532029232,12.));
#115098=CARTESIAN_POINT('Ctrl Pts',(71.6772699438963,14.6696040841678,12.));
#115099=CARTESIAN_POINT('Ctrl Pts',(71.6556869911662,14.6550963938829,12.));
#115100=CARTESIAN_POINT('Ctrl Pts',(71.6341221457169,14.6406301440814,12.));
#115101=CARTESIAN_POINT('Ctrl Pts',(71.612575518229,14.626205346737,12.));
#115102=CARTESIAN_POINT('Ctrl Pts',(71.5910472197813,14.6118220137849,12.));
#115103=CARTESIAN_POINT('Ctrl Pts',(71.5695373618562,14.597480157121,12.));
#115104=CARTESIAN_POINT('Ctrl Pts',(71.5480460563447,14.5831797885952,12.));
#115105=CARTESIAN_POINT('Ctrl Pts',(71.5265734155498,14.5689209200091,12.));
#115106=CARTESIAN_POINT('Ctrl Pts',(71.5051195521909,14.5547035631234,12.));
#115107=CARTESIAN_POINT('Ctrl Pts',(71.4836845794048,14.540527729659,12.));
#115108=CARTESIAN_POINT('Ctrl Pts',(71.4622686107475,14.5263934312969,12.));
#115109=CARTESIAN_POINT('Ctrl Pts',(71.4408717601923,14.5123006796728,12.));
#115110=CARTESIAN_POINT('Ctrl Pts',(71.4194941421292,14.4982494863718,12.));
#115111=CARTESIAN_POINT('Ctrl Pts',(71.3981358713723,14.4842398629355,12.));
#115112=CARTESIAN_POINT('Ctrl Pts',(71.376797063165,14.4702718208651,12.));
#115113=CARTESIAN_POINT('Ctrl Pts',(71.3554778331835,14.4563453716204,12.));
#115114=CARTESIAN_POINT('Ctrl Pts',(71.3341782975386,14.4424605266165,12.));
#115115=CARTESIAN_POINT('Ctrl Pts',(71.312898572777,14.4286172972167,12.));
#115116=CARTESIAN_POINT('Ctrl Pts',(71.2916387758861,14.4148156947384,12.));
#115117=CARTESIAN_POINT('Ctrl Pts',(71.2703990242988,14.401055730457,12.));
#115118=CARTESIAN_POINT('Ctrl Pts',(71.2491794358958,14.3873374156056,12.));
#115119=CARTESIAN_POINT('Ctrl Pts',(71.2279801290084,14.3736607613722,12.));
#115120=CARTESIAN_POINT('Ctrl Pts',(71.2068012224174,14.3600257788924,12.));
#115121=CARTESIAN_POINT('Ctrl Pts',(71.1856428353593,14.3464324792534,12.));
#115122=CARTESIAN_POINT('Ctrl Pts',(71.1645050875308,14.332880873499,12.));
#115123=CARTESIAN_POINT('Ctrl Pts',(71.1433880990929,14.3193709726294,12.));
#115124=CARTESIAN_POINT('Ctrl Pts',(71.1222919906727,14.3059027875994,12.));
#115125=CARTESIAN_POINT('Ctrl Pts',(71.1012168833643,14.2924763293105,12.));
#115126=CARTESIAN_POINT('Ctrl Pts',(71.0801628987332,14.2790916086133,12.));
#115127=CARTESIAN_POINT('Ctrl Pts',(71.0591301588231,14.2657486363139,12.));
#115128=CARTESIAN_POINT('Ctrl Pts',(71.0381187861588,14.2524474231733,12.));
#115129=CARTESIAN_POINT('Ctrl Pts',(71.0171289037488,14.2391879799062,12.));
#115130=CARTESIAN_POINT('Ctrl Pts',(70.9961606350861,14.2259703171737,12.));
#115131=CARTESIAN_POINT('Ctrl Pts',(70.9752141041518,14.2127944455839,12.));
#115132=CARTESIAN_POINT('Ctrl Pts',(70.9542894354216,14.1996603756982,12.));
#115133=CARTESIAN_POINT('Ctrl Pts',(70.9333867538704,14.1865681180321,12.));
#115134=CARTESIAN_POINT('Ctrl Pts',(70.9125061849745,14.1735176830533,12.));
#115135=CARTESIAN_POINT('Ctrl Pts',(70.8916478547132,14.1605090811754,12.));
#115136=CARTESIAN_POINT('Ctrl Pts',(70.8708118895715,14.1475423227568,12.));
#115137=CARTESIAN_POINT('Ctrl Pts',(70.8499984165489,14.1346174181079,12.));
#115138=CARTESIAN_POINT('Ctrl Pts',(70.8292075631621,14.1217343774913,12.));
#115139=CARTESIAN_POINT('Ctrl Pts',(70.8084394574493,14.1088932111214,12.));
#115140=CARTESIAN_POINT('Ctrl Pts',(70.7876942279697,14.0960939291569,12.));
#115141=CARTESIAN_POINT('Ctrl Pts',(70.7669720038077,14.0833365416996,12.));
#115142=CARTESIAN_POINT('Ctrl Pts',(70.7462729145807,14.0706210588016,12.));
#115143=CARTESIAN_POINT('Ctrl Pts',(70.7255970904436,14.0579474904657,12.));
#115144=CARTESIAN_POINT('Ctrl Pts',(70.7049446620928,14.0453158466451,12.));
#115145=CARTESIAN_POINT('Ctrl Pts',(70.6843157607668,14.0327261372362,12.));
#115146=CARTESIAN_POINT('Ctrl Pts',(70.6637105182484,14.020178372077,12.));
#115147=CARTESIAN_POINT('Ctrl Pts',(70.6431290668745,14.0076725609537,12.));
#115148=CARTESIAN_POINT('Ctrl Pts',(70.6225715395394,13.9952087136018,12.));
#115149=CARTESIAN_POINT('Ctrl Pts',(70.6020380697005,13.9827868397057,12.));
#115150=CARTESIAN_POINT('Ctrl Pts',(70.5815287913784,13.9704069488917,12.));
#115151=CARTESIAN_POINT('Ctrl Pts',(70.5610438391612,13.958069050726,12.));
#115152=CARTESIAN_POINT('Ctrl Pts',(70.5405833482112,13.9457731547215,12.));
#115153=CARTESIAN_POINT('Ctrl Pts',(70.520147454271,13.9335192703388,12.));
#115154=CARTESIAN_POINT('Ctrl Pts',(70.4997362936673,13.9213074069853,12.));
#115155=CARTESIAN_POINT('Ctrl Pts',(70.4793500033124,13.9091375740088,12.));
#115156=CARTESIAN_POINT('Ctrl Pts',(70.4589887207073,13.8970097806954,12.));
#115157=CARTESIAN_POINT('Ctrl Pts',(70.4386525839521,13.8849240362763,12.));
#115158=CARTESIAN_POINT('Ctrl Pts',(70.41834173175,13.8728803499287,12.));
#115159=CARTESIAN_POINT('Ctrl Pts',(70.3980563034133,13.8608787307752,12.));
#115160=CARTESIAN_POINT('Ctrl Pts',(70.3777964388632,13.8489191878767,12.));
#115161=CARTESIAN_POINT('Ctrl Pts',(70.3575622786335,13.8370017302309,12.));
#115162=CARTESIAN_POINT('Ctrl Pts',(70.3373539638809,13.8251263667791,12.));
#115163=CARTESIAN_POINT('Ctrl Pts',(70.3171716363897,13.8132931064064,12.));
#115164=CARTESIAN_POINT('Ctrl Pts',(70.2970154385774,13.8015019579414,12.));
#115165=CARTESIAN_POINT('Ctrl Pts',(70.2768855134947,13.7897529301491,12.));
#115166=CARTESIAN_POINT('Ctrl Pts',(70.2567820048303,13.7780460317294,12.));
#115167=CARTESIAN_POINT('Ctrl Pts',(70.2367050569216,13.7663812713243,12.));
#115168=CARTESIAN_POINT('Ctrl Pts',(70.2166548147604,13.7547586575181,12.));
#115169=CARTESIAN_POINT('Ctrl Pts',(70.1966314239995,13.7431781988365,12.));
#115170=CARTESIAN_POINT('Ctrl Pts',(70.1766350309518,13.7316399037393,12.));
#115171=CARTESIAN_POINT('Ctrl Pts',(70.156665782595,13.7201437806199,12.));
#115172=CARTESIAN_POINT('Ctrl Pts',(70.1367238265825,13.7086898378122,12.));
#115173=CARTESIAN_POINT('Ctrl Pts',(70.1168093112486,13.6972780835897,12.));
#115174=CARTESIAN_POINT('Ctrl Pts',(70.0969223856136,13.6859085261653,12.));
#115175=CARTESIAN_POINT('Ctrl Pts',(70.0770631993856,13.674581173683,12.));
#115176=CARTESIAN_POINT('Ctrl Pts',(70.0572319029676,13.6632960342196,12.));
#115177=CARTESIAN_POINT('Ctrl Pts',(70.0374286474677,13.6520531157907,12.));
#115178=CARTESIAN_POINT('Ctrl Pts',(70.0176535847049,13.6408524263496,12.));
#115179=CARTESIAN_POINT('Ctrl Pts',(69.9979068672153,13.6296939737865,12.));
#115180=CARTESIAN_POINT('Ctrl Pts',(69.9781886482528,13.6185777659198,12.));
#115181=CARTESIAN_POINT('Ctrl Pts',(69.9584990817974,13.6075038104999,12.));
#115182=CARTESIAN_POINT('Ctrl Pts',(69.9388383225648,13.5964721152135,12.));
#115183=CARTESIAN_POINT('Ctrl Pts',(69.9192065260108,13.5854826876835,12.));
#115184=CARTESIAN_POINT('Ctrl Pts',(69.8996038483361,13.5745355354657,12.));
#115185=CARTESIAN_POINT('Ctrl Pts',(69.8800304464882,13.5636306660422,12.));
#115186=CARTESIAN_POINT('Ctrl Pts',(69.8604864781706,13.5527680868255,12.));
#115187=CARTESIAN_POINT('Ctrl Pts',(69.840972101856,13.5419478051625,12.));
#115188=CARTESIAN_POINT('Ctrl Pts',(69.8214874767944,13.5311698283339,12.));
#115189=CARTESIAN_POINT('Ctrl Pts',(69.8020327630205,13.5204341635507,12.));
#115190=CARTESIAN_POINT('Ctrl Pts',(69.7826081213576,13.5097408179479,12.));
#115191=CARTESIAN_POINT('Ctrl Pts',(69.7632137134249,13.4990897985905,12.));
#115192=CARTESIAN_POINT('Ctrl Pts',(69.7438497016406,13.4884811124748,12.));
#115193=CARTESIAN_POINT('Ctrl Pts',(69.724516249225,13.4779147665285,12.));
#115194=CARTESIAN_POINT('Ctrl Pts',(69.7052135201998,13.4673907676044,12.));
#115195=CARTESIAN_POINT('Ctrl Pts',(69.6859416793885,13.456909122476,12.));
#115196=CARTESIAN_POINT('Ctrl Pts',(69.666700892444,13.4464698378453,12.));
#115197=CARTESIAN_POINT('Ctrl Pts',(69.6474913258675,13.4360729203442,12.));
#115198=CARTESIAN_POINT('Ctrl Pts',(69.6283131470273,13.4257183765341,12.));
#115199=CARTESIAN_POINT('Ctrl Pts',(69.6091665241765,13.4154062129002,12.));
#115200=CARTESIAN_POINT('Ctrl Pts',(69.5900516264553,13.40513643585,12.));
#115201=CARTESIAN_POINT('Ctrl Pts',(69.5709686238724,13.3949090517177,12.));
#115202=CARTESIAN_POINT('Ctrl Pts',(69.5519176872862,13.3847240667628,12.));
#115203=CARTESIAN_POINT('Ctrl Pts',(69.5328989883885,13.3745814871665,12.));
#115204=CARTESIAN_POINT('Ctrl Pts',(69.5139126996675,13.3644813190219,12.));
#115205=CARTESIAN_POINT('Ctrl Pts',(69.4949589944606,13.3544235683394,12.));
#115206=CARTESIAN_POINT('Ctrl Pts',(69.4760380470365,13.3444082410543,12.));
#115207=CARTESIAN_POINT('Ctrl Pts',(69.4571500326673,13.3344353430313,12.));
#115208=CARTESIAN_POINT('Ctrl Pts',(69.4382951276998,13.3245048800643,12.));
#115209=CARTESIAN_POINT('Ctrl Pts',(69.4194735096265,13.3146168578743,12.));
#115210=CARTESIAN_POINT('Ctrl Pts',(69.4006853569511,13.3047712821051,12.));
#115211=CARTESIAN_POINT('Ctrl Pts',(69.3819308490422,13.2949681583167,12.));
#115212=CARTESIAN_POINT('Ctrl Pts',(69.3632101660066,13.2852074919766,12.));
#115213=CARTESIAN_POINT('Ctrl Pts',(69.3445234885065,13.2754892884433,12.));
#115214=CARTESIAN_POINT('Ctrl Pts',(69.3258709977382,13.265813552961,12.));
#115215=CARTESIAN_POINT('Ctrl Pts',(69.3072528758518,13.2561802906896,12.));
#115216=CARTESIAN_POINT('Ctrl Pts',(69.2886693063182,13.2465895067262,12.));
#115217=CARTESIAN_POINT('Ctrl Pts',(69.270120474245,13.237041206122,12.));
#115218=CARTESIAN_POINT('Ctrl Pts',(69.2516065668844,13.2275353939051,12.));
#115219=CARTESIAN_POINT('Ctrl Pts',(69.2331277732861,13.2180720750594,12.));
#115220=CARTESIAN_POINT('Ctrl Pts',(69.2146842833537,13.2086512544735,12.));
#115221=CARTESIAN_POINT('Ctrl Pts',(69.1962762870527,13.1992729368929,12.));
#115222=CARTESIAN_POINT('Ctrl Pts',(69.1779039735996,13.1899371268683,12.));
#115223=CARTESIAN_POINT('Ctrl Pts',(69.1595675305245,13.1806438286934,12.));
#115224=CARTESIAN_POINT('Ctrl Pts',(69.1412671454564,13.1713930465133,12.));
#115225=CARTESIAN_POINT('Ctrl Pts',(69.1230030082573,13.1621847844528,12.));
#115226=CARTESIAN_POINT('Ctrl Pts',(69.1047753127643,13.1530190467183,12.));
#115227=CARTESIAN_POINT('Ctrl Pts',(69.0865842593102,13.1438958377404,12.));
#115228=CARTESIAN_POINT('Ctrl Pts',(69.0684300549477,13.1348151621834,12.));
#115229=CARTESIAN_POINT('Ctrl Pts',(69.0503129081817,13.1257770246386,12.));
#115230=CARTESIAN_POINT('Ctrl Pts',(69.0322330243348,13.1167814293497,12.));
#115231=CARTESIAN_POINT('Ctrl Pts',(69.0141906015113,13.1078283799722,12.));
#115232=CARTESIAN_POINT('Ctrl Pts',(68.9961858241519,13.0989178791834,12.));
#115233=CARTESIAN_POINT('Ctrl Pts',(68.9782188692581,13.090049929053,12.));
#115234=CARTESIAN_POINT('Ctrl Pts',(68.9602899187573,13.0812245317808,12.));
#115235=CARTESIAN_POINT('Ctrl Pts',(68.9423991694492,13.072441690283,12.));
#115236=CARTESIAN_POINT('Ctrl Pts',(68.9245468449945,13.0637014089029,12.));
#115237=CARTESIAN_POINT('Ctrl Pts',(68.9067332040985,13.0550036938813,12.));
#115238=CARTESIAN_POINT('Ctrl Pts',(68.8889585151585,13.0463485518207,12.));
#115239=CARTESIAN_POINT('Ctrl Pts',(68.8712230321906,13.0377359881875,12.));
#115240=CARTESIAN_POINT('Ctrl Pts',(68.8535269726793,13.0291660060107,12.));
#115241=CARTESIAN_POINT('Ctrl Pts',(68.8358704887468,13.0206386039691,12.));
#115242=CARTESIAN_POINT('Ctrl Pts',(68.8182536653656,13.0121537768946,12.));
#115243=CARTESIAN_POINT('Ctrl Pts',(68.804191966902,13.0053999700875,12.));
#115244=CARTESIAN_POINT('Ctrl Pts',(68.7936635625545,13.0003537683055,12.));
#115245=CARTESIAN_POINT('Ctrl Pts',(68.7866525680193,12.9969981460277,12.));
#115246=CARTESIAN_POINT('Ctrl Pts',(68.7831490561748,12.9953224629497,12.));
#115247=CARTESIAN_POINT('Ctrl Pts',(72.2774028393913,16.7988252568749,-5.55111512312578E-16));
#115248=CARTESIAN_POINT('Ctrl Pts',(72.2774028393913,16.7988252568749,4.));
#115249=CARTESIAN_POINT('Ctrl Pts',(72.2774028393913,16.7988252568749,8.));
#115250=CARTESIAN_POINT('Ctrl Pts',(72.2774028393913,16.7988252568749,12.));
#115251=CARTESIAN_POINT('Ctrl Pts',(72.3852065198824,16.7775526720894,-5.55111512312578E-16));
#115252=CARTESIAN_POINT('Ctrl Pts',(72.3852065198824,16.7775526720894,4.));
#115253=CARTESIAN_POINT('Ctrl Pts',(72.3852065198824,16.7775526720894,8.00000000000001));
#115254=CARTESIAN_POINT('Ctrl Pts',(72.3852065198824,16.7775526720894,12.));
#115255=CARTESIAN_POINT('Ctrl Pts',(72.560513354629,16.6758649025559,-5.55111512312578E-16));
#115256=CARTESIAN_POINT('Ctrl Pts',(72.560513354629,16.6758649025559,4.));
#115257=CARTESIAN_POINT('Ctrl Pts',(72.560513354629,16.6758649025559,7.99999999999999));
#115258=CARTESIAN_POINT('Ctrl Pts',(72.560513354629,16.6758649025559,12.));
#115259=CARTESIAN_POINT('Ctrl Pts',(72.6501505354463,16.4988611391808,-5.55111512312578E-16));
#115260=CARTESIAN_POINT('Ctrl Pts',(72.6501505354463,16.4988611391808,4.));
#115261=CARTESIAN_POINT('Ctrl Pts',(72.6501505354463,16.4988611391808,8.00000000000001));
#115262=CARTESIAN_POINT('Ctrl Pts',(72.6501505354463,16.4988611391808,12.));
#115263=CARTESIAN_POINT('Ctrl Pts',(72.6683126419586,16.4184755008061,-5.55111512312578E-16));
#115264=CARTESIAN_POINT('Ctrl Pts',(72.6683126419586,16.4184755008061,4.));
#115265=CARTESIAN_POINT('Ctrl Pts',(72.6683126419586,16.4184755008061,8.));
#115266=CARTESIAN_POINT('Ctrl Pts',(72.6683126419586,16.4184755008061,12.));
#115267=CARTESIAN_POINT('',(72.2774028393913,16.7988252568749,2.77555756156289E-16));
#115268=CARTESIAN_POINT('',(72.6683126419586,16.4184755008061,0.));
#115269=CARTESIAN_POINT('Ctrl Pts',(72.2774028393913,16.7988252568749,-1.38777878078145E-16));
#115270=CARTESIAN_POINT('Ctrl Pts',(72.3852065198824,16.7775526720894,-1.38777878078145E-16));
#115271=CARTESIAN_POINT('Ctrl Pts',(72.4853818540233,16.7194453752131,-1.38777878078144E-16));
#115272=CARTESIAN_POINT('Ctrl Pts',(72.5575834236159,16.6367451007559,-1.38777878078145E-16));
#115273=CARTESIAN_POINT('Ctrl Pts',(72.6117346008103,16.574719894913,-1.38777878078145E-16));
#115274=CARTESIAN_POINT('Ctrl Pts',(72.6501505354463,16.4988611391808,-1.38777878078145E-16));
#115275=CARTESIAN_POINT('Ctrl Pts',(72.6683126419586,16.4184755008061,-1.38777878078145E-16));
#115276=CARTESIAN_POINT('',(72.6683126419586,16.4184755008061,12.));
#115277=CARTESIAN_POINT('Ctrl Pts',(72.6683126419586,16.4184755008061,-5.55111512312578E-16));
#115278=CARTESIAN_POINT('Ctrl Pts',(72.6683126419586,16.4184755008061,4.));
#115279=CARTESIAN_POINT('Ctrl Pts',(72.6683126419586,16.4184755008061,8.));
#115280=CARTESIAN_POINT('Ctrl Pts',(72.6683126419586,16.4184755008061,12.));
#115281=CARTESIAN_POINT('',(72.2774028393913,16.7988252568749,12.));
#115282=CARTESIAN_POINT('Ctrl Pts',(72.6683126419586,16.4184755008061,12.));
#115283=CARTESIAN_POINT('Ctrl Pts',(72.6501505354463,16.4988611391808,12.));
#115284=CARTESIAN_POINT('Ctrl Pts',(72.6117346008103,16.574719894913,12.));
#115285=CARTESIAN_POINT('Ctrl Pts',(72.5575834236159,16.6367451007559,12.));
#115286=CARTESIAN_POINT('Ctrl Pts',(72.4853818540233,16.7194453752131,12.));
#115287=CARTESIAN_POINT('Ctrl Pts',(72.3852065198824,16.7775526720894,12.));
#115288=CARTESIAN_POINT('Ctrl Pts',(72.2774028393913,16.7988252568749,12.));
#115289=CARTESIAN_POINT('Ctrl Pts',(72.2774028393913,16.7988252568749,12.));
#115290=CARTESIAN_POINT('Ctrl Pts',(72.2774028393913,16.7988252568749,8.));
#115291=CARTESIAN_POINT('Ctrl Pts',(72.2774028393913,16.7988252568749,4.));
#115292=CARTESIAN_POINT('Ctrl Pts',(72.2774028393913,16.7988252568749,-5.55111512312578E-16));
#115293=CARTESIAN_POINT('Origin',(3.65936987487134E-10,8.12279454723526E-11,
0.));
#115294=CARTESIAN_POINT('Origin',(3.65936987487134E-10,8.12279454723526E-11,
12.));
#115295=CARTESIAN_POINT('Origin',(3.65936987487134E-10,8.12279454723526E-11,
0.));
#115296=CARTESIAN_POINT('Ctrl Pts',(73.9013264985861,9.42570643237831,0.));
#115297=CARTESIAN_POINT('Ctrl Pts',(73.9013264985861,9.42570643237831,4.));
#115298=CARTESIAN_POINT('Ctrl Pts',(73.9013264985861,9.42570643237828,8.));
#115299=CARTESIAN_POINT('Ctrl Pts',(73.9013264985861,9.42570643237828,12.));
#115300=CARTESIAN_POINT('Ctrl Pts',(73.9152287787081,9.31670696907632,0.));
#115301=CARTESIAN_POINT('Ctrl Pts',(73.9152287787081,9.31670696907632,4.));
#115302=CARTESIAN_POINT('Ctrl Pts',(73.9152287787081,9.31670696907632,8.));
#115303=CARTESIAN_POINT('Ctrl Pts',(73.9152287787081,9.31670696907632,12.));
#115304=CARTESIAN_POINT('Ctrl Pts',(73.8741839722668,9.11824194722592,0.));
#115305=CARTESIAN_POINT('Ctrl Pts',(73.8741839722668,9.11824194722592,4.));
#115306=CARTESIAN_POINT('Ctrl Pts',(73.8741839722668,9.11824194722597,7.99999999999999));
#115307=CARTESIAN_POINT('Ctrl Pts',(73.8741839722668,9.11824194722597,12.));
#115308=CARTESIAN_POINT('Ctrl Pts',(73.7345987226923,8.97724108745619,0.));
#115309=CARTESIAN_POINT('Ctrl Pts',(73.7345987226923,8.97724108745619,4.));
#115310=CARTESIAN_POINT('Ctrl Pts',(73.7345987226924,8.97724108745623,8.00000000000001));
#115311=CARTESIAN_POINT('Ctrl Pts',(73.7345987226924,8.97724108745623,12.));
#115312=CARTESIAN_POINT('Ctrl Pts',(73.6640787197678,8.93459554655875,0.));
#115313=CARTESIAN_POINT('Ctrl Pts',(73.6640787197678,8.93459554655875,4.));
#115314=CARTESIAN_POINT('Ctrl Pts',(73.664078719768,8.93459554655877,8.));
#115315=CARTESIAN_POINT('Ctrl Pts',(73.664078719768,8.93459554655877,12.));
#115316=CARTESIAN_POINT('',(73.9013264985861,9.42570643237831,0.));
#115317=CARTESIAN_POINT('',(73.6640787197679,8.93459554655866,0.));
#115318=CARTESIAN_POINT('Ctrl Pts',(73.9013264985861,9.42570643237831,2.77555756156289E-16));
#115319=CARTESIAN_POINT('Ctrl Pts',(73.9152287787081,9.31670696907632,2.77555756156289E-16));
#115320=CARTESIAN_POINT('Ctrl Pts',(73.8917746035988,9.20329838516181,2.77555756156289E-16));
#115321=CARTESIAN_POINT('Ctrl Pts',(73.8361439572623,9.10865360927363,2.77555756156289E-16));
#115322=CARTESIAN_POINT('Ctrl Pts',(73.7944209725099,9.0376700273575,2.77555756156289E-16));
#115323=CARTESIAN_POINT('Ctrl Pts',(73.7345987226923,8.97724108745619,2.77555756156289E-16));
#115324=CARTESIAN_POINT('Ctrl Pts',(73.6640787197678,8.93459554655875,2.77555756156289E-16));
#115325=CARTESIAN_POINT('',(73.664078719768,8.93459554655874,12.));
#115326=CARTESIAN_POINT('Ctrl Pts',(73.6640787197678,8.93459554655875,0.));
#115327=CARTESIAN_POINT('Ctrl Pts',(73.6640787197678,8.93459554655875,4.));
#115328=CARTESIAN_POINT('Ctrl Pts',(73.664078719768,8.93459554655877,8.));
#115329=CARTESIAN_POINT('Ctrl Pts',(73.664078719768,8.93459554655877,12.));
#115330=CARTESIAN_POINT('',(73.9013264985861,9.42570643237828,12.));
#115331=CARTESIAN_POINT('Ctrl Pts',(73.664078719768,8.93459554655877,12.));
#115332=CARTESIAN_POINT('Ctrl Pts',(73.7345987226924,8.97724108745623,12.));
#115333=CARTESIAN_POINT('Ctrl Pts',(73.79442097251,9.03767002735755,12.));
#115334=CARTESIAN_POINT('Ctrl Pts',(73.8361439572624,9.10865360927367,12.));
#115335=CARTESIAN_POINT('Ctrl Pts',(73.8917746035988,9.20329838516184,12.));
#115336=CARTESIAN_POINT('Ctrl Pts',(73.9152287787081,9.31670696907632,12.));
#115337=CARTESIAN_POINT('Ctrl Pts',(73.9013264985861,9.42570643237828,12.));
#115338=CARTESIAN_POINT('Ctrl Pts',(73.9013264985861,9.42570643237828,12.));
#115339=CARTESIAN_POINT('Ctrl Pts',(73.9013264985861,9.42570643237828,8.));
#115340=CARTESIAN_POINT('Ctrl Pts',(73.9013264985861,9.42570643237831,4.));
#115341=CARTESIAN_POINT('Ctrl Pts',(73.9013264985861,9.42570643237831,0.));
#115342=CARTESIAN_POINT('Ctrl Pts',(69.6540253893192,6.95102489306927,0.));
#115343=CARTESIAN_POINT('Ctrl Pts',(69.6540253893192,6.95102489306927,12.));
#115344=CARTESIAN_POINT('Ctrl Pts',(69.6576616146467,6.95238884849026,0.));
#115345=CARTESIAN_POINT('Ctrl Pts',(69.6576616146467,6.95238884849026,12.));
#115346=CARTESIAN_POINT('Ctrl Pts',(69.664938391983,6.95512065317601,0.));
#115347=CARTESIAN_POINT('Ctrl Pts',(69.664938391983,6.95512065317601,12.));
#115348=CARTESIAN_POINT('Ctrl Pts',(69.6758665380378,6.95923004173592,0.));
#115349=CARTESIAN_POINT('Ctrl Pts',(69.6758665380378,6.95923004173592,12.));
#115350=CARTESIAN_POINT('Ctrl Pts',(69.6904633605421,6.96473259049514,0.));
#115351=CARTESIAN_POINT('Ctrl Pts',(69.6904633605421,6.96473259049514,12.));
#115352=CARTESIAN_POINT('Ctrl Pts',(69.7087526479973,6.97164972291441,0.));
#115353=CARTESIAN_POINT('Ctrl Pts',(69.7087526479973,6.97164972291441,12.));
#115354=CARTESIAN_POINT('Ctrl Pts',(69.7270851557366,6.97860581164528,0.));
#115355=CARTESIAN_POINT('Ctrl Pts',(69.7270851557366,6.97860581164528,12.));
#115356=CARTESIAN_POINT('Ctrl Pts',(69.7454607995607,6.98560086924215,0.));
#115357=CARTESIAN_POINT('Ctrl Pts',(69.7454607995607,6.98560086924215,12.));
#115358=CARTESIAN_POINT('Ctrl Pts',(69.7638794280419,6.99263491027942,0.));
#115359=CARTESIAN_POINT('Ctrl Pts',(69.7638794280419,6.99263491027942,12.));
#115360=CARTESIAN_POINT('Ctrl Pts',(69.782340824259,6.99970795069477,0.));
#115361=CARTESIAN_POINT('Ctrl Pts',(69.782340824259,6.99970795069477,12.));
#115362=CARTESIAN_POINT('Ctrl Pts',(69.8008447346863,7.00682000718152,0.));
#115363=CARTESIAN_POINT('Ctrl Pts',(69.8008447346863,7.00682000718152,12.));
#115364=CARTESIAN_POINT('Ctrl Pts',(69.8193908913722,7.01397109655456,0.));
#115365=CARTESIAN_POINT('Ctrl Pts',(69.8193908913722,7.01397109655456,12.));
#115366=CARTESIAN_POINT('Ctrl Pts',(69.8379790360518,7.02116123514453,0.));
#115367=CARTESIAN_POINT('Ctrl Pts',(69.8379790360518,7.02116123514453,12.));
#115368=CARTESIAN_POINT('Ctrl Pts',(69.8566089455375,7.02839043811814,0.));
#115369=CARTESIAN_POINT('Ctrl Pts',(69.8566089455375,7.02839043811814,12.));
#115370=CARTESIAN_POINT('Ctrl Pts',(69.8752804235238,7.03565871972222,0.));
#115371=CARTESIAN_POINT('Ctrl Pts',(69.8752804235238,7.03565871972222,12.));
#115372=CARTESIAN_POINT('Ctrl Pts',(69.8939932885841,7.04296609362167,0.));
#115373=CARTESIAN_POINT('Ctrl Pts',(69.8939932885841,7.04296609362167,12.));
#115374=CARTESIAN_POINT('Ctrl Pts',(69.9127473642099,7.05031257318117,0.));
#115375=CARTESIAN_POINT('Ctrl Pts',(69.9127473642099,7.05031257318117,12.));
#115376=CARTESIAN_POINT('Ctrl Pts',(69.9315424664291,7.05769817180858,0.));
#115377=CARTESIAN_POINT('Ctrl Pts',(69.9315424664291,7.05769817180858,12.));
#115378=CARTESIAN_POINT('Ctrl Pts',(69.9503783975727,7.06512290312851,0.));
#115379=CARTESIAN_POINT('Ctrl Pts',(69.9503783975727,7.06512290312851,12.));
#115380=CARTESIAN_POINT('Ctrl Pts',(69.9692549527296,7.07258678080832,0.));
#115381=CARTESIAN_POINT('Ctrl Pts',(69.9692549527296,7.07258678080832,12.));
#115382=CARTESIAN_POINT('Ctrl Pts',(69.988171923788,7.08008981844653,0.));
#115383=CARTESIAN_POINT('Ctrl Pts',(69.988171923788,7.08008981844653,12.));
#115384=CARTESIAN_POINT('Ctrl Pts',(70.0071291040766,7.08763202944247,0.));
#115385=CARTESIAN_POINT('Ctrl Pts',(70.0071291040766,7.08763202944247,12.));
#115386=CARTESIAN_POINT('Ctrl Pts',(70.0261262936388,7.0952134268425,0.));
#115387=CARTESIAN_POINT('Ctrl Pts',(70.0261262936388,7.0952134268425,12.));
#115388=CARTESIAN_POINT('Ctrl Pts',(70.0451632990086,7.10283402335035,0.));
#115389=CARTESIAN_POINT('Ctrl Pts',(70.0451632990086,7.10283402335035,12.));
#115390=CARTESIAN_POINT('Ctrl Pts',(70.0642399306869,7.11049383140447,0.));
#115391=CARTESIAN_POINT('Ctrl Pts',(70.0642399306869,7.11049383140447,12.));
#115392=CARTESIAN_POINT('Ctrl Pts',(70.0833560013975,7.11819286322827,0.));
#115393=CARTESIAN_POINT('Ctrl Pts',(70.0833560013975,7.11819286322827,12.));
#115394=CARTESIAN_POINT('Ctrl Pts',(70.1025113239495,7.12593113088905,0.));
#115395=CARTESIAN_POINT('Ctrl Pts',(70.1025113239495,7.12593113088905,12.));
#115396=CARTESIAN_POINT('Ctrl Pts',(70.1217057094499,7.13370864634444,0.));
#115397=CARTESIAN_POINT('Ctrl Pts',(70.1217057094499,7.13370864634444,12.));
#115398=CARTESIAN_POINT('Ctrl Pts',(70.1409389682424,7.14152542142375,0.));
#115399=CARTESIAN_POINT('Ctrl Pts',(70.1409389682424,7.14152542142375,12.));
#115400=CARTESIAN_POINT('Ctrl Pts',(70.1602109107202,7.14938146780815,0.));
#115401=CARTESIAN_POINT('Ctrl Pts',(70.1602109107202,7.14938146780815,12.));
#115402=CARTESIAN_POINT('Ctrl Pts',(70.1795213481185,7.15727679700934,0.));
#115403=CARTESIAN_POINT('Ctrl Pts',(70.1795213481185,7.15727679700934,12.));
#115404=CARTESIAN_POINT('Ctrl Pts',(70.1988700934593,7.16521142033865,0.));
#115405=CARTESIAN_POINT('Ctrl Pts',(70.1988700934593,7.16521142033865,12.));
#115406=CARTESIAN_POINT('Ctrl Pts',(70.2182569618994,7.17318534889717,0.));
#115407=CARTESIAN_POINT('Ctrl Pts',(70.2182569618994,7.17318534889717,12.));
#115408=CARTESIAN_POINT('Ctrl Pts',(70.2376817702215,7.18119859359779,0.));
#115409=CARTESIAN_POINT('Ctrl Pts',(70.2376817702215,7.18119859359779,12.));
#115410=CARTESIAN_POINT('Ctrl Pts',(70.2571443365192,7.18925116517556,0.));
#115411=CARTESIAN_POINT('Ctrl Pts',(70.2571443365192,7.18925116517556,12.));
#115412=CARTESIAN_POINT('Ctrl Pts',(70.2766444798285,7.19734307419874,0.));
#115413=CARTESIAN_POINT('Ctrl Pts',(70.2766444798285,7.19734307419874,12.));
#115414=CARTESIAN_POINT('Ctrl Pts',(70.2961820197077,7.20547433107483,0.));
#115415=CARTESIAN_POINT('Ctrl Pts',(70.2961820197077,7.20547433107483,12.));
#115416=CARTESIAN_POINT('Ctrl Pts',(70.3157567762588,7.21364494605451,0.));
#115417=CARTESIAN_POINT('Ctrl Pts',(70.3157567762588,7.21364494605451,12.));
#115418=CARTESIAN_POINT('Ctrl Pts',(70.3353685703112,7.22185492923192,0.));
#115419=CARTESIAN_POINT('Ctrl Pts',(70.3353685703112,7.22185492923192,12.));
#115420=CARTESIAN_POINT('Ctrl Pts',(70.3550172235486,7.2301042905423,0.));
#115421=CARTESIAN_POINT('Ctrl Pts',(70.3550172235486,7.2301042905423,12.));
#115422=CARTESIAN_POINT('Ctrl Pts',(70.3747025586552,7.23839303975608,0.));
#115423=CARTESIAN_POINT('Ctrl Pts',(70.3747025586552,7.23839303975608,12.));
#115424=CARTESIAN_POINT('Ctrl Pts',(70.3944243994504,7.24672118647086,0.));
#115425=CARTESIAN_POINT('Ctrl Pts',(70.3944243994504,7.24672118647086,12.));
#115426=CARTESIAN_POINT('Ctrl Pts',(70.4141825708178,7.25508874012044,0.));
#115427=CARTESIAN_POINT('Ctrl Pts',(70.4141825708178,7.25508874012044,12.));
#115428=CARTESIAN_POINT('Ctrl Pts',(70.4339768986346,7.26349570998034,0.));
#115429=CARTESIAN_POINT('Ctrl Pts',(70.4339768986346,7.26349570998034,12.));
#115430=CARTESIAN_POINT('Ctrl Pts',(70.4538072096992,7.27194210517064,0.));
#115431=CARTESIAN_POINT('Ctrl Pts',(70.4538072096992,7.27194210517064,12.));
#115432=CARTESIAN_POINT('Ctrl Pts',(70.4736733316487,7.28042793465472,0.));
#115433=CARTESIAN_POINT('Ctrl Pts',(70.4736733316487,7.28042793465472,12.));
#115434=CARTESIAN_POINT('Ctrl Pts',(70.4935750929058,7.28895320723863,0.));
#115435=CARTESIAN_POINT('Ctrl Pts',(70.4935750929058,7.28895320723863,12.));
#115436=CARTESIAN_POINT('Ctrl Pts',(70.5135123227169,7.29751793157824,0.));
#115437=CARTESIAN_POINT('Ctrl Pts',(70.5135123227169,7.29751793157824,12.));
#115438=CARTESIAN_POINT('Ctrl Pts',(70.5334848511681,7.30612211618054,0.));
#115439=CARTESIAN_POINT('Ctrl Pts',(70.5334848511681,7.30612211618054,12.));
#115440=CARTESIAN_POINT('Ctrl Pts',(70.5534925092043,7.31476576940393,0.));
#115441=CARTESIAN_POINT('Ctrl Pts',(70.5534925092043,7.31476576940393,12.));
#115442=CARTESIAN_POINT('Ctrl Pts',(70.5735351286476,7.32344889945221,0.));
#115443=CARTESIAN_POINT('Ctrl Pts',(70.5735351286476,7.32344889945221,12.));
#115444=CARTESIAN_POINT('Ctrl Pts',(70.5936125421946,7.33217151437592,0.));
#115445=CARTESIAN_POINT('Ctrl Pts',(70.5936125421946,7.33217151437592,12.));
#115446=CARTESIAN_POINT('Ctrl Pts',(70.6137245833996,7.34093362208009,0.));
#115447=CARTESIAN_POINT('Ctrl Pts',(70.6137245833996,7.34093362208009,12.));
#115448=CARTESIAN_POINT('Ctrl Pts',(70.6338710866562,7.34973523032579,0.));
#115449=CARTESIAN_POINT('Ctrl Pts',(70.6338710866562,7.34973523032579,12.));
#115450=CARTESIAN_POINT('Ctrl Pts',(70.6540518871775,7.35857634673056,0.));
#115451=CARTESIAN_POINT('Ctrl Pts',(70.6540518871775,7.35857634673056,12.));
#115452=CARTESIAN_POINT('Ctrl Pts',(70.6742668209687,7.36745697876302,0.));
#115453=CARTESIAN_POINT('Ctrl Pts',(70.6742668209687,7.36745697876302,12.));
#115454=CARTESIAN_POINT('Ctrl Pts',(70.694515724827,7.37637713374769,0.));
#115455=CARTESIAN_POINT('Ctrl Pts',(70.694515724827,7.37637713374769,12.));
#115456=CARTESIAN_POINT('Ctrl Pts',(70.7147984363424,7.38533681887033,0.));
#115457=CARTESIAN_POINT('Ctrl Pts',(70.7147984363424,7.38533681887033,12.));
#115458=CARTESIAN_POINT('Ctrl Pts',(70.735114793895,7.39433604117892,0.));
#115459=CARTESIAN_POINT('Ctrl Pts',(70.735114793895,7.39433604117892,12.));
#115460=CARTESIAN_POINT('Ctrl Pts',(70.7554646366514,7.40337480758231,0.));
#115461=CARTESIAN_POINT('Ctrl Pts',(70.7554646366514,7.40337480758231,12.));
#115462=CARTESIAN_POINT('Ctrl Pts',(70.7758478045576,7.41245312484488,0.));
#115463=CARTESIAN_POINT('Ctrl Pts',(70.7758478045576,7.41245312484488,12.));
#115464=CARTESIAN_POINT('Ctrl Pts',(70.7962641383351,7.42157099959317,0.));
#115465=CARTESIAN_POINT('Ctrl Pts',(70.7962641383351,7.42157099959317,12.));
#115466=CARTESIAN_POINT('Ctrl Pts',(70.8167134794738,7.43072843832009,0.));
#115467=CARTESIAN_POINT('Ctrl Pts',(70.8167134794738,7.43072843832009,12.));
#115468=CARTESIAN_POINT('Ctrl Pts',(70.8371956702242,7.43992544738608,0.));
#115469=CARTESIAN_POINT('Ctrl Pts',(70.8371956702242,7.43992544738608,12.));
#115470=CARTESIAN_POINT('Ctrl Pts',(70.8577105535841,7.44916203301646,0.));
#115471=CARTESIAN_POINT('Ctrl Pts',(70.8577105535841,7.44916203301646,12.));
#115472=CARTESIAN_POINT('Ctrl Pts',(70.8782579732885,7.45843820129777,0.));
#115473=CARTESIAN_POINT('Ctrl Pts',(70.8782579732885,7.45843820129777,12.));
#115474=CARTESIAN_POINT('Ctrl Pts',(70.8988377738088,7.4677539581852,0.));
#115475=CARTESIAN_POINT('Ctrl Pts',(70.8988377738088,7.4677539581852,12.));
#115476=CARTESIAN_POINT('Ctrl Pts',(70.9194498003483,7.47710930950555,0.));
#115477=CARTESIAN_POINT('Ctrl Pts',(70.9194498003483,7.47710930950555,12.));
#115478=CARTESIAN_POINT('Ctrl Pts',(70.9400938988373,7.48650426095824,0.));
#115479=CARTESIAN_POINT('Ctrl Pts',(70.9400938988373,7.48650426095824,12.));
#115480=CARTESIAN_POINT('Ctrl Pts',(70.9607699159234,7.49593881811142,0.));
#115481=CARTESIAN_POINT('Ctrl Pts',(70.9607699159234,7.49593881811142,12.));
#115482=CARTESIAN_POINT('Ctrl Pts',(70.9814776989637,7.5054129863995,0.));
#115483=CARTESIAN_POINT('Ctrl Pts',(70.9814776989637,7.5054129863995,12.));
#115484=CARTESIAN_POINT('Ctrl Pts',(71.0022170960235,7.51492677113113,0.));
#115485=CARTESIAN_POINT('Ctrl Pts',(71.0022170960235,7.51492677113113,12.));
#115486=CARTESIAN_POINT('Ctrl Pts',(71.0229879558713,7.52448017749137,0.));
#115487=CARTESIAN_POINT('Ctrl Pts',(71.0229879558713,7.52448017749137,12.));
#115488=CARTESIAN_POINT('Ctrl Pts',(71.0437901279722,7.53407321054255,0.));
#115489=CARTESIAN_POINT('Ctrl Pts',(71.0437901279722,7.53407321054255,12.));
#115490=CARTESIAN_POINT('Ctrl Pts',(71.0646234624783,7.5437058752195,0.));
#115491=CARTESIAN_POINT('Ctrl Pts',(71.0646234624783,7.5437058752195,12.));
#115492=CARTESIAN_POINT('Ctrl Pts',(71.0854878102203,7.55337817632874,0.));
#115493=CARTESIAN_POINT('Ctrl Pts',(71.0854878102203,7.55337817632874,12.));
#115494=CARTESIAN_POINT('Ctrl Pts',(71.1063830227074,7.56309011855618,0.));
#115495=CARTESIAN_POINT('Ctrl Pts',(71.1063830227074,7.56309011855618,12.));
#115496=CARTESIAN_POINT('Ctrl Pts',(71.1273089521218,7.57284170646867,0.));
#115497=CARTESIAN_POINT('Ctrl Pts',(71.1273089521218,7.57284170646867,12.));
#115498=CARTESIAN_POINT('Ctrl Pts',(71.1482654513133,7.58263294451467,0.));
#115499=CARTESIAN_POINT('Ctrl Pts',(71.1482654513133,7.58263294451467,12.));
#115500=CARTESIAN_POINT('Ctrl Pts',(71.1692523737887,7.59246383701861,0.));
#115501=CARTESIAN_POINT('Ctrl Pts',(71.1692523737887,7.59246383701861,12.));
#115502=CARTESIAN_POINT('Ctrl Pts',(71.1902695737063,7.60233438818157,0.));
#115503=CARTESIAN_POINT('Ctrl Pts',(71.1902695737063,7.60233438818157,12.));
#115504=CARTESIAN_POINT('Ctrl Pts',(71.2113169058778,7.61224460208888,0.));
#115505=CARTESIAN_POINT('Ctrl Pts',(71.2113169058778,7.61224460208888,12.));
#115506=CARTESIAN_POINT('Ctrl Pts',(71.232394225762,7.62219448271126,0.));
#115507=CARTESIAN_POINT('Ctrl Pts',(71.232394225762,7.62219448271126,12.));
#115508=CARTESIAN_POINT('Ctrl Pts',(71.2535013894587,7.63218403390516,0.));
#115509=CARTESIAN_POINT('Ctrl Pts',(71.2535013894587,7.63218403390516,12.));
#115510=CARTESIAN_POINT('Ctrl Pts',(71.2746382536974,7.64221325940673,0.));
#115511=CARTESIAN_POINT('Ctrl Pts',(71.2746382536974,7.64221325940673,12.));
#115512=CARTESIAN_POINT('Ctrl Pts',(71.2958046758334,7.65228216283344,0.));
#115513=CARTESIAN_POINT('Ctrl Pts',(71.2958046758334,7.65228216283344,12.));
#115514=CARTESIAN_POINT('Ctrl Pts',(71.3170005138474,7.6623907476912,0.));
#115515=CARTESIAN_POINT('Ctrl Pts',(71.3170005138474,7.6623907476912,12.));
#115516=CARTESIAN_POINT('Ctrl Pts',(71.3382256263405,7.67253901737541,0.));
#115517=CARTESIAN_POINT('Ctrl Pts',(71.3382256263405,7.67253901737541,12.));
#115518=CARTESIAN_POINT('Ctrl Pts',(71.3594798725294,7.68272697517104,0.));
#115519=CARTESIAN_POINT('Ctrl Pts',(71.3594798725294,7.68272697517104,12.));
#115520=CARTESIAN_POINT('Ctrl Pts',(71.380763112236,7.69295462424648,0.));
#115521=CARTESIAN_POINT('Ctrl Pts',(71.380763112236,7.69295462424648,12.));
#115522=CARTESIAN_POINT('Ctrl Pts',(71.4020752058827,7.70322196765574,0.));
#115523=CARTESIAN_POINT('Ctrl Pts',(71.4020752058827,7.70322196765574,12.));
#115524=CARTESIAN_POINT('Ctrl Pts',(71.4234160144943,7.71352900834539,0.));
#115525=CARTESIAN_POINT('Ctrl Pts',(71.4234160144943,7.71352900834539,12.));
#115526=CARTESIAN_POINT('Ctrl Pts',(71.4447853996919,7.72387574915546,0.));
#115527=CARTESIAN_POINT('Ctrl Pts',(71.4447853996919,7.72387574915546,12.));
#115528=CARTESIAN_POINT('Ctrl Pts',(71.4661832236881,7.73426219281933,0.));
#115529=CARTESIAN_POINT('Ctrl Pts',(71.4661832236881,7.73426219281933,12.));
#115530=CARTESIAN_POINT('Ctrl Pts',(71.487609349277,7.74468834195735,0.));
#115531=CARTESIAN_POINT('Ctrl Pts',(71.487609349277,7.74468834195735,12.));
#115532=CARTESIAN_POINT('Ctrl Pts',(71.5090636398307,7.75515419907956,0.));
#115533=CARTESIAN_POINT('Ctrl Pts',(71.5090636398307,7.75515419907956,12.));
#115534=CARTESIAN_POINT('Ctrl Pts',(71.5305459592987,7.7656597665922,0.));
#115535=CARTESIAN_POINT('Ctrl Pts',(71.5305459592987,7.7656597665922,12.));
#115536=CARTESIAN_POINT('Ctrl Pts',(71.5520561722039,7.77620504679869,0.));
#115537=CARTESIAN_POINT('Ctrl Pts',(71.5520561722039,7.77620504679869,12.));
#115538=CARTESIAN_POINT('Ctrl Pts',(71.5735941436366,7.78679004189936,0.));
#115539=CARTESIAN_POINT('Ctrl Pts',(71.5735941436366,7.78679004189936,12.));
#115540=CARTESIAN_POINT('Ctrl Pts',(71.5951597392471,7.79741475398513,0.));
#115541=CARTESIAN_POINT('Ctrl Pts',(71.5951597392471,7.79741475398513,12.));
#115542=CARTESIAN_POINT('Ctrl Pts',(71.616752825242,7.80807918504018,0.));
#115543=CARTESIAN_POINT('Ctrl Pts',(71.616752825242,7.80807918504018,12.));
#115544=CARTESIAN_POINT('Ctrl Pts',(71.638373268384,7.81878333694857,0.));
#115545=CARTESIAN_POINT('Ctrl Pts',(71.638373268384,7.81878333694857,12.));
#115546=CARTESIAN_POINT('Ctrl Pts',(71.6600209359869,7.82952721149505,0.));
#115547=CARTESIAN_POINT('Ctrl Pts',(71.6600209359869,7.82952721149505,12.));
#115548=CARTESIAN_POINT('Ctrl Pts',(71.681695695912,7.8403108103649,0.));
#115549=CARTESIAN_POINT('Ctrl Pts',(71.681695695912,7.8403108103649,12.));
#115550=CARTESIAN_POINT('Ctrl Pts',(71.7033974165576,7.8511341351374,0.));
#115551=CARTESIAN_POINT('Ctrl Pts',(71.7033974165576,7.8511341351374,12.));
#115552=CARTESIAN_POINT('Ctrl Pts',(71.7251259668573,7.86199718728831,0.));
#115553=CARTESIAN_POINT('Ctrl Pts',(71.7251259668573,7.86199718728831,12.));
#115554=CARTESIAN_POINT('Ctrl Pts',(71.7468812162795,7.87289996819656,0.));
#115555=CARTESIAN_POINT('Ctrl Pts',(71.7468812162795,7.87289996819656,12.));
#115556=CARTESIAN_POINT('Ctrl Pts',(71.768663034824,7.88384247914523,0.));
#115557=CARTESIAN_POINT('Ctrl Pts',(71.768663034824,7.88384247914523,12.));
#115558=CARTESIAN_POINT('Ctrl Pts',(71.7904712930172,7.89482472132136,0.));
#115559=CARTESIAN_POINT('Ctrl Pts',(71.7904712930172,7.89482472132136,12.));
#115560=CARTESIAN_POINT('Ctrl Pts',(71.8123058619038,7.90584669580957,0.));
#115561=CARTESIAN_POINT('Ctrl Pts',(71.8123058619038,7.90584669580957,12.));
#115562=CARTESIAN_POINT('Ctrl Pts',(71.8341666130424,7.91690840359372,0.));
#115563=CARTESIAN_POINT('Ctrl Pts',(71.8341666130424,7.91690840359372,12.));
#115564=CARTESIAN_POINT('Ctrl Pts',(71.8560534185071,7.92800984556401,0.));
#115565=CARTESIAN_POINT('Ctrl Pts',(71.8560534185071,7.92800984556401,12.));
#115566=CARTESIAN_POINT('Ctrl Pts',(71.8779661508833,7.93915102251797,0.));
#115567=CARTESIAN_POINT('Ctrl Pts',(71.8779661508833,7.93915102251797,12.));
#115568=CARTESIAN_POINT('Ctrl Pts',(71.8999046832642,7.95033193516047,0.));
#115569=CARTESIAN_POINT('Ctrl Pts',(71.8999046832642,7.95033193516047,12.));
#115570=CARTESIAN_POINT('Ctrl Pts',(71.9218688892426,7.96155258409753,0.));
#115571=CARTESIAN_POINT('Ctrl Pts',(71.9218688892426,7.96155258409753,12.));
#115572=CARTESIAN_POINT('Ctrl Pts',(71.9438586429072,7.97281296983703,0.));
#115573=CARTESIAN_POINT('Ctrl Pts',(71.9438586429072,7.97281296983703,12.));
#115574=CARTESIAN_POINT('Ctrl Pts',(71.9658738188421,7.98411309279599,0.));
#115575=CARTESIAN_POINT('Ctrl Pts',(71.9658738188421,7.98411309279599,12.));
#115576=CARTESIAN_POINT('Ctrl Pts',(71.9879142921248,7.99545295330183,0.));
#115577=CARTESIAN_POINT('Ctrl Pts',(71.9879142921248,7.99545295330183,12.));
#115578=CARTESIAN_POINT('Ctrl Pts',(72.0099799383216,8.00683255159251,0.));
#115579=CARTESIAN_POINT('Ctrl Pts',(72.0099799383216,8.00683255159251,12.));
#115580=CARTESIAN_POINT('Ctrl Pts',(72.0320706334802,8.01825188781071,0.));
#115581=CARTESIAN_POINT('Ctrl Pts',(72.0320706334802,8.01825188781071,12.));
#115582=CARTESIAN_POINT('Ctrl Pts',(72.0541862541262,8.0297109620033,0.));
#115583=CARTESIAN_POINT('Ctrl Pts',(72.0541862541262,8.0297109620033,12.));
#115584=CARTESIAN_POINT('Ctrl Pts',(72.0763266772632,8.04120977412893,0.));
#115585=CARTESIAN_POINT('Ctrl Pts',(72.0763266772632,8.04120977412893,12.));
#115586=CARTESIAN_POINT('Ctrl Pts',(72.0984917803702,8.05274832405958,0.));
#115587=CARTESIAN_POINT('Ctrl Pts',(72.0984917803702,8.05274832405958,12.));
#115588=CARTESIAN_POINT('Ctrl Pts',(72.1206814413985,8.06432661158091,0.));
#115589=CARTESIAN_POINT('Ctrl Pts',(72.1206814413985,8.06432661158091,12.));
#115590=CARTESIAN_POINT('Ctrl Pts',(72.1428955387648,8.07594463638701,0.));
#115591=CARTESIAN_POINT('Ctrl Pts',(72.1428955387648,8.07594463638701,12.));
#115592=CARTESIAN_POINT('Ctrl Pts',(72.165133951346,8.08760239807816,0.));
#115593=CARTESIAN_POINT('Ctrl Pts',(72.165133951346,8.08760239807816,12.));
#115594=CARTESIAN_POINT('Ctrl Pts',(72.18739655848,8.09929989616875,0.));
#115595=CARTESIAN_POINT('Ctrl Pts',(72.18739655848,8.09929989616875,12.));
#115596=CARTESIAN_POINT('Ctrl Pts',(72.2096832399626,8.11103713008923,0.));
#115597=CARTESIAN_POINT('Ctrl Pts',(72.2096832399626,8.11103713008923,12.));
#115598=CARTESIAN_POINT('Ctrl Pts',(72.2319938760451,8.12281409918663,0.));
#115599=CARTESIAN_POINT('Ctrl Pts',(72.2319938760451,8.12281409918663,12.));
#115600=CARTESIAN_POINT('Ctrl Pts',(72.2543283474279,8.1346308027203,0.));
#115601=CARTESIAN_POINT('Ctrl Pts',(72.2543283474279,8.1346308027203,12.));
#115602=CARTESIAN_POINT('Ctrl Pts',(72.2766865352552,8.14648723985794,0.));
#115603=CARTESIAN_POINT('Ctrl Pts',(72.2766865352552,8.14648723985794,12.));
#115604=CARTESIAN_POINT('Ctrl Pts',(72.2990683211155,8.15838340968329,0.));
#115605=CARTESIAN_POINT('Ctrl Pts',(72.2990683211155,8.15838340968329,12.));
#115606=CARTESIAN_POINT('Ctrl Pts',(72.3214735870402,8.17031931119883,0.));
#115607=CARTESIAN_POINT('Ctrl Pts',(72.3214735870402,8.17031931119883,12.));
#115608=CARTESIAN_POINT('Ctrl Pts',(72.3439022155007,8.18229494332623,0.));
#115609=CARTESIAN_POINT('Ctrl Pts',(72.3439022155007,8.18229494332623,12.));
#115610=CARTESIAN_POINT('Ctrl Pts',(72.3663540894034,8.1943103049032,0.));
#115611=CARTESIAN_POINT('Ctrl Pts',(72.3663540894034,8.1943103049032,12.));
#115612=CARTESIAN_POINT('Ctrl Pts',(72.3888290920845,8.20636539467783,0.));
#115613=CARTESIAN_POINT('Ctrl Pts',(72.3888290920845,8.20636539467783,12.));
#115614=CARTESIAN_POINT('Ctrl Pts',(72.4113271073091,8.21846021131565,0.));
#115615=CARTESIAN_POINT('Ctrl Pts',(72.4113271073091,8.21846021131565,12.));
#115616=CARTESIAN_POINT('Ctrl Pts',(72.4338480192701,8.23059475340355,0.));
#115617=CARTESIAN_POINT('Ctrl Pts',(72.4338480192701,8.23059475340355,12.));
#115618=CARTESIAN_POINT('Ctrl Pts',(72.4563917125842,8.24276901945038,0.));
#115619=CARTESIAN_POINT('Ctrl Pts',(72.4563917125842,8.24276901945038,12.));
#115620=CARTESIAN_POINT('Ctrl Pts',(72.4789580722871,8.25498300788494,0.));
#115621=CARTESIAN_POINT('Ctrl Pts',(72.4789580722871,8.25498300788494,12.));
#115622=CARTESIAN_POINT('Ctrl Pts',(72.501546983825,8.26723671704925,0.));
#115623=CARTESIAN_POINT('Ctrl Pts',(72.501546983825,8.26723671704925,12.));
#115624=CARTESIAN_POINT('Ctrl Pts',(72.524158333056,8.27953014520386,0.));
#115625=CARTESIAN_POINT('Ctrl Pts',(72.524158333056,8.27953014520386,12.));
#115626=CARTESIAN_POINT('Ctrl Pts',(72.5467920062522,8.2918632905329,0.));
#115627=CARTESIAN_POINT('Ctrl Pts',(72.5467920062522,8.2918632905329,12.));
#115628=CARTESIAN_POINT('Ctrl Pts',(72.5694478900983,8.30423615114456,0.));
#115629=CARTESIAN_POINT('Ctrl Pts',(72.5694478900983,8.30423615114456,12.));
#115630=CARTESIAN_POINT('Ctrl Pts',(72.5921258716899,8.3166487250701,0.));
#115631=CARTESIAN_POINT('Ctrl Pts',(72.5921258716899,8.3166487250701,12.));
#115632=CARTESIAN_POINT('Ctrl Pts',(72.614825838529,8.32910101025654,0.));
#115633=CARTESIAN_POINT('Ctrl Pts',(72.614825838529,8.32910101025654,12.));
#115634=CARTESIAN_POINT('Ctrl Pts',(72.6375476785208,8.34159300456966,0.));
#115635=CARTESIAN_POINT('Ctrl Pts',(72.6375476785208,8.34159300456966,12.));
#115636=CARTESIAN_POINT('Ctrl Pts',(72.6602912799689,8.35412470580084,0.));
#115637=CARTESIAN_POINT('Ctrl Pts',(72.6602912799689,8.35412470580084,12.));
#115638=CARTESIAN_POINT('Ctrl Pts',(72.68305653157,8.36669611166835,0.));
#115639=CARTESIAN_POINT('Ctrl Pts',(72.68305653157,8.36669611166835,12.));
#115640=CARTESIAN_POINT('Ctrl Pts',(72.7058433224072,8.37930721981736,0.));
#115641=CARTESIAN_POINT('Ctrl Pts',(72.7058433224072,8.37930721981736,12.));
#115642=CARTESIAN_POINT('Ctrl Pts',(72.728651541938,8.39195802781408,0.));
#115643=CARTESIAN_POINT('Ctrl Pts',(72.728651541938,8.39195802781408,12.));
#115644=CARTESIAN_POINT('Ctrl Pts',(72.7514810799932,8.40464853314494,0.));
#115645=CARTESIAN_POINT('Ctrl Pts',(72.7514810799932,8.40464853314494,12.));
#115646=CARTESIAN_POINT('Ctrl Pts',(72.7743318267876,8.41737873322354,0.));
#115647=CARTESIAN_POINT('Ctrl Pts',(72.7743318267876,8.41737873322354,12.));
#115648=CARTESIAN_POINT('Ctrl Pts',(72.7972036729283,8.43014862539172,0.));
#115649=CARTESIAN_POINT('Ctrl Pts',(72.7972036729283,8.43014862539172,12.));
#115650=CARTESIAN_POINT('Ctrl Pts',(72.8200965094197,8.44295820691908,0.));
#115651=CARTESIAN_POINT('Ctrl Pts',(72.8200965094197,8.44295820691908,12.));
#115652=CARTESIAN_POINT('Ctrl Pts',(72.8430102276703,8.45580747499772,0.));
#115653=CARTESIAN_POINT('Ctrl Pts',(72.8430102276703,8.45580747499772,12.));
#115654=CARTESIAN_POINT('Ctrl Pts',(72.8659447194918,8.46869642673764,0.));
#115655=CARTESIAN_POINT('Ctrl Pts',(72.8659447194918,8.46869642673764,12.));
#115656=CARTESIAN_POINT('Ctrl Pts',(72.888899877077,8.48162505917629,0.));
#115657=CARTESIAN_POINT('Ctrl Pts',(72.888899877077,8.48162505917629,12.));
#115658=CARTESIAN_POINT('Ctrl Pts',(72.9118755929785,8.49459336928277,0.));
#115659=CARTESIAN_POINT('Ctrl Pts',(72.9118755929785,8.49459336928277,12.));
#115660=CARTESIAN_POINT('Ctrl Pts',(72.9348717600837,8.5076013539598,0.));
#115661=CARTESIAN_POINT('Ctrl Pts',(72.9348717600837,8.5076013539598,12.));
#115662=CARTESIAN_POINT('Ctrl Pts',(72.9578882715923,8.52064901004245,0.));
#115663=CARTESIAN_POINT('Ctrl Pts',(72.9578882715923,8.52064901004245,12.));
#115664=CARTESIAN_POINT('Ctrl Pts',(72.9809250209843,8.53373633429304,0.));
#115665=CARTESIAN_POINT('Ctrl Pts',(72.9809250209843,8.53373633429304,12.));
#115666=CARTESIAN_POINT('Ctrl Pts',(73.0039819020663,8.5468633234044,0.));
#115667=CARTESIAN_POINT('Ctrl Pts',(73.0039819020663,8.5468633234044,12.));
#115668=CARTESIAN_POINT('Ctrl Pts',(73.0270588090193,8.56002997400097,0.));
#115669=CARTESIAN_POINT('Ctrl Pts',(73.0270588090193,8.56002997400097,12.));
#115670=CARTESIAN_POINT('Ctrl Pts',(73.0501556364482,8.57323628263596,0.));
#115671=CARTESIAN_POINT('Ctrl Pts',(73.0501556364482,8.57323628263596,12.));
#115672=CARTESIAN_POINT('Ctrl Pts',(73.073272279419,8.58648224578724,0.));
#115673=CARTESIAN_POINT('Ctrl Pts',(73.073272279419,8.58648224578724,12.));
#115674=CARTESIAN_POINT('Ctrl Pts',(73.0964086335226,8.5997678598454,0.));
#115675=CARTESIAN_POINT('Ctrl Pts',(73.0964086335226,8.5997678598454,12.));
#115676=CARTESIAN_POINT('Ctrl Pts',(73.1195645948169,8.6130931211199,0.));
#115677=CARTESIAN_POINT('Ctrl Pts',(73.1195645948169,8.6130931211199,12.));
#115678=CARTESIAN_POINT('Ctrl Pts',(73.142740059703,8.62645802585476,0.));
#115679=CARTESIAN_POINT('Ctrl Pts',(73.142740059703,8.62645802585476,12.));
#115680=CARTESIAN_POINT('Ctrl Pts',(73.165934924813,8.63986257023736,0.));
#115681=CARTESIAN_POINT('Ctrl Pts',(73.165934924813,8.63986257023736,12.));
#115682=CARTESIAN_POINT('Ctrl Pts',(73.1891490869057,8.65330675040537,0.));
#115683=CARTESIAN_POINT('Ctrl Pts',(73.1891490869057,8.65330675040537,12.));
#115684=CARTESIAN_POINT('Ctrl Pts',(73.2123824427212,8.66679056245097,0.));
#115685=CARTESIAN_POINT('Ctrl Pts',(73.2123824427212,8.66679056245097,12.));
#115686=CARTESIAN_POINT('Ctrl Pts',(73.2356348889704,8.68031400241885,0.));
#115687=CARTESIAN_POINT('Ctrl Pts',(73.2356348889704,8.68031400241885,12.));
#115688=CARTESIAN_POINT('Ctrl Pts',(73.2589063226373,8.69387706629305,0.));
#115689=CARTESIAN_POINT('Ctrl Pts',(73.2589063226373,8.69387706629305,12.));
#115690=CARTESIAN_POINT('Ctrl Pts',(73.282196641216,8.70747974998246,0.));
#115691=CARTESIAN_POINT('Ctrl Pts',(73.282196641216,8.70747974998246,12.));
#115692=CARTESIAN_POINT('Ctrl Pts',(73.3055057429744,8.72112204930233,0.));
#115693=CARTESIAN_POINT('Ctrl Pts',(73.3055057429744,8.72112204930233,12.));
#115694=CARTESIAN_POINT('Ctrl Pts',(73.3288335271989,8.73480395995361,0.));
#115695=CARTESIAN_POINT('Ctrl Pts',(73.3288335271989,8.73480395995361,12.));
#115696=CARTESIAN_POINT('Ctrl Pts',(73.3521798944595,8.74852547749737,0.));
#115697=CARTESIAN_POINT('Ctrl Pts',(73.3521798944595,8.74852547749737,12.));
#115698=CARTESIAN_POINT('Ctrl Pts',(73.3755447460235,8.76228659740306,0.));
#115699=CARTESIAN_POINT('Ctrl Pts',(73.3755447460235,8.76228659740306,12.));
#115700=CARTESIAN_POINT('Ctrl Pts',(73.3989279832808,8.77608731509305,0.));
#115701=CARTESIAN_POINT('Ctrl Pts',(73.3989279832808,8.77608731509305,12.));
#115702=CARTESIAN_POINT('Ctrl Pts',(73.422329507112,8.78992762598739,0.));
#115703=CARTESIAN_POINT('Ctrl Pts',(73.422329507112,8.78992762598739,12.));
#115704=CARTESIAN_POINT('Ctrl Pts',(73.4457492173949,8.80380752553715,0.));
#115705=CARTESIAN_POINT('Ctrl Pts',(73.4457492173949,8.80380752553715,12.));
#115706=CARTESIAN_POINT('Ctrl Pts',(73.4691870121608,8.81772700927594,0.));
#115707=CARTESIAN_POINT('Ctrl Pts',(73.4691870121608,8.81772700927594,12.));
#115708=CARTESIAN_POINT('Ctrl Pts',(73.4926427882787,8.83168607277416,0.));
#115709=CARTESIAN_POINT('Ctrl Pts',(73.4926427882787,8.83168607277416,12.));
#115710=CARTESIAN_POINT('Ctrl Pts',(73.5161164429765,8.84568471153895,0.));
#115711=CARTESIAN_POINT('Ctrl Pts',(73.5161164429765,8.84568471153895,12.));
#115712=CARTESIAN_POINT('Ctrl Pts',(73.5396078751672,8.85972292092184,0.));
#115713=CARTESIAN_POINT('Ctrl Pts',(73.5396078751672,8.85972292092184,12.));
#115714=CARTESIAN_POINT('Ctrl Pts',(73.5631169867113,8.87380069602956,0.));
#115715=CARTESIAN_POINT('Ctrl Pts',(73.5631169867113,8.87380069602956,12.));
#115716=CARTESIAN_POINT('Ctrl Pts',(73.5866436840493,8.88791803160342,0.));
#115717=CARTESIAN_POINT('Ctrl Pts',(73.5866436840493,8.88791803160342,12.));
#115718=CARTESIAN_POINT('Ctrl Pts',(73.6101878785868,8.90207492198872,0.));
#115719=CARTESIAN_POINT('Ctrl Pts',(73.6101878785868,8.90207492198872,12.));
#115720=CARTESIAN_POINT('Ctrl Pts',(73.6337494830846,8.91627136139888,0.));
#115721=CARTESIAN_POINT('Ctrl Pts',(73.6337494830846,8.91627136139888,12.));
#115722=CARTESIAN_POINT('Ctrl Pts',(73.6573284088088,8.93050734411972,0.));
#115723=CARTESIAN_POINT('Ctrl Pts',(73.6573284088088,8.93050734411972,12.));
#115724=CARTESIAN_POINT('Ctrl Pts',(73.6809245622361,8.94478286474384,0.));
#115725=CARTESIAN_POINT('Ctrl Pts',(73.6809245622361,8.94478286474384,12.));
#115726=CARTESIAN_POINT('Ctrl Pts',(73.7045378422775,8.95909791836291,0.));
#115727=CARTESIAN_POINT('Ctrl Pts',(73.7045378422775,8.95909791836291,12.));
#115728=CARTESIAN_POINT('Ctrl Pts',(73.7281681364031,8.97345250083919,0.));
#115729=CARTESIAN_POINT('Ctrl Pts',(73.7281681364031,8.97345250083919,12.));
#115730=CARTESIAN_POINT('Ctrl Pts',(73.7518153262253,8.98784660837829,0.));
#115731=CARTESIAN_POINT('Ctrl Pts',(73.7518153262253,8.98784660837829,12.));
#115732=CARTESIAN_POINT('Ctrl Pts',(73.7754792943925,9.00228023701468,0.));
#115733=CARTESIAN_POINT('Ctrl Pts',(73.7754792943925,9.00228023701468,12.));
#115734=CARTESIAN_POINT('Ctrl Pts',(73.7991599312731,9.01675338208223,0.));
#115735=CARTESIAN_POINT('Ctrl Pts',(73.7991599312731,9.01675338208223,12.));
#115736=CARTESIAN_POINT('Ctrl Pts',(73.8228571411607,9.03126603777982,0.));
#115737=CARTESIAN_POINT('Ctrl Pts',(73.8228571411607,9.03126603777982,12.));
#115738=CARTESIAN_POINT('Ctrl Pts',(73.8465708500679,9.04581819646386,0.));
#115739=CARTESIAN_POINT('Ctrl Pts',(73.8465708500679,9.04581819646386,12.));
#115740=CARTESIAN_POINT('Ctrl Pts',(73.870301007746,9.06040984889251,0.));
#115741=CARTESIAN_POINT('Ctrl Pts',(73.870301007746,9.06040984889251,12.));
#115742=CARTESIAN_POINT('Ctrl Pts',(73.8940475821756,9.07504098570548,0.));
#115743=CARTESIAN_POINT('Ctrl Pts',(73.8940475821756,9.07504098570548,12.));
#115744=CARTESIAN_POINT('Ctrl Pts',(73.9130579611989,9.08677747601239,0.));
#115745=CARTESIAN_POINT('Ctrl Pts',(73.9130579611989,9.08677747601239,12.));
#115746=CARTESIAN_POINT('Ctrl Pts',(73.9273231219464,9.0955976052846,0.));
#115747=CARTESIAN_POINT('Ctrl Pts',(73.9273231219464,9.0955976052846,12.));
#115748=CARTESIAN_POINT('Ctrl Pts',(73.9368365074164,9.10148558516325,0.));
#115749=CARTESIAN_POINT('Ctrl Pts',(73.9368365074164,9.10148558516325,12.));
#115750=CARTESIAN_POINT('Ctrl Pts',(73.9415940197274,9.10443154852688,0.));
#115751=CARTESIAN_POINT('Ctrl Pts',(73.9415940197274,9.10443154852688,12.));
#115752=CARTESIAN_POINT('',(69.6540253893192,6.95102489306927,0.));
#115753=CARTESIAN_POINT('Ctrl Pts',(69.6540253893192,6.95102489306927,0.));
#115754=CARTESIAN_POINT('Ctrl Pts',(69.6576616146467,6.95238884849026,0.));
#115755=CARTESIAN_POINT('Ctrl Pts',(69.664938391983,6.95512065317601,0.));
#115756=CARTESIAN_POINT('Ctrl Pts',(69.6758665380378,6.95923004173592,0.));
#115757=CARTESIAN_POINT('Ctrl Pts',(69.6904633605421,6.96473259049514,0.));
#115758=CARTESIAN_POINT('Ctrl Pts',(69.7087526479973,6.97164972291441,0.));
#115759=CARTESIAN_POINT('Ctrl Pts',(69.7270851557366,6.97860581164528,0.));
#115760=CARTESIAN_POINT('Ctrl Pts',(69.7454607995607,6.98560086924215,0.));
#115761=CARTESIAN_POINT('Ctrl Pts',(69.7638794280419,6.99263491027942,0.));
#115762=CARTESIAN_POINT('Ctrl Pts',(69.782340824259,6.99970795069477,0.));
#115763=CARTESIAN_POINT('Ctrl Pts',(69.8008447346863,7.00682000718152,0.));
#115764=CARTESIAN_POINT('Ctrl Pts',(69.8193908913722,7.01397109655456,0.));
#115765=CARTESIAN_POINT('Ctrl Pts',(69.8379790360518,7.02116123514453,0.));
#115766=CARTESIAN_POINT('Ctrl Pts',(69.8566089455375,7.02839043811814,0.));
#115767=CARTESIAN_POINT('Ctrl Pts',(69.8752804235238,7.03565871972222,0.));
#115768=CARTESIAN_POINT('Ctrl Pts',(69.8939932885841,7.04296609362167,0.));
#115769=CARTESIAN_POINT('Ctrl Pts',(69.9127473642099,7.05031257318117,0.));
#115770=CARTESIAN_POINT('Ctrl Pts',(69.9315424664291,7.05769817180858,0.));
#115771=CARTESIAN_POINT('Ctrl Pts',(69.9503783975727,7.06512290312851,0.));
#115772=CARTESIAN_POINT('Ctrl Pts',(69.9692549527296,7.07258678080832,0.));
#115773=CARTESIAN_POINT('Ctrl Pts',(69.988171923788,7.08008981844653,0.));
#115774=CARTESIAN_POINT('Ctrl Pts',(70.0071291040766,7.08763202944247,0.));
#115775=CARTESIAN_POINT('Ctrl Pts',(70.0261262936388,7.0952134268425,0.));
#115776=CARTESIAN_POINT('Ctrl Pts',(70.0451632990086,7.10283402335035,0.));
#115777=CARTESIAN_POINT('Ctrl Pts',(70.0642399306869,7.11049383140447,0.));
#115778=CARTESIAN_POINT('Ctrl Pts',(70.0833560013975,7.11819286322827,0.));
#115779=CARTESIAN_POINT('Ctrl Pts',(70.1025113239495,7.12593113088905,0.));
#115780=CARTESIAN_POINT('Ctrl Pts',(70.1217057094499,7.13370864634444,0.));
#115781=CARTESIAN_POINT('Ctrl Pts',(70.1409389682424,7.14152542142375,0.));
#115782=CARTESIAN_POINT('Ctrl Pts',(70.1602109107202,7.14938146780815,0.));
#115783=CARTESIAN_POINT('Ctrl Pts',(70.1795213481185,7.15727679700934,0.));
#115784=CARTESIAN_POINT('Ctrl Pts',(70.1988700934593,7.16521142033865,0.));
#115785=CARTESIAN_POINT('Ctrl Pts',(70.2182569618994,7.17318534889717,0.));
#115786=CARTESIAN_POINT('Ctrl Pts',(70.2376817702215,7.18119859359779,0.));
#115787=CARTESIAN_POINT('Ctrl Pts',(70.2571443365192,7.18925116517556,0.));
#115788=CARTESIAN_POINT('Ctrl Pts',(70.2766444798285,7.19734307419874,0.));
#115789=CARTESIAN_POINT('Ctrl Pts',(70.2961820197077,7.20547433107483,0.));
#115790=CARTESIAN_POINT('Ctrl Pts',(70.3157567762588,7.21364494605451,0.));
#115791=CARTESIAN_POINT('Ctrl Pts',(70.3353685703112,7.22185492923192,0.));
#115792=CARTESIAN_POINT('Ctrl Pts',(70.3550172235486,7.2301042905423,0.));
#115793=CARTESIAN_POINT('Ctrl Pts',(70.3747025586552,7.23839303975608,0.));
#115794=CARTESIAN_POINT('Ctrl Pts',(70.3944243994504,7.24672118647086,0.));
#115795=CARTESIAN_POINT('Ctrl Pts',(70.4141825708178,7.25508874012044,0.));
#115796=CARTESIAN_POINT('Ctrl Pts',(70.4339768986346,7.26349570998034,0.));
#115797=CARTESIAN_POINT('Ctrl Pts',(70.4538072096992,7.27194210517064,0.));
#115798=CARTESIAN_POINT('Ctrl Pts',(70.4736733316487,7.28042793465472,0.));
#115799=CARTESIAN_POINT('Ctrl Pts',(70.4935750929058,7.28895320723863,0.));
#115800=CARTESIAN_POINT('Ctrl Pts',(70.5135123227169,7.29751793157824,0.));
#115801=CARTESIAN_POINT('Ctrl Pts',(70.5334848511681,7.30612211618054,0.));
#115802=CARTESIAN_POINT('Ctrl Pts',(70.5534925092043,7.31476576940393,0.));
#115803=CARTESIAN_POINT('Ctrl Pts',(70.5735351286476,7.32344889945221,0.));
#115804=CARTESIAN_POINT('Ctrl Pts',(70.5936125421946,7.33217151437592,0.));
#115805=CARTESIAN_POINT('Ctrl Pts',(70.6137245833996,7.34093362208009,0.));
#115806=CARTESIAN_POINT('Ctrl Pts',(70.6338710866562,7.34973523032579,0.));
#115807=CARTESIAN_POINT('Ctrl Pts',(70.6540518871775,7.35857634673056,0.));
#115808=CARTESIAN_POINT('Ctrl Pts',(70.6742668209687,7.36745697876302,0.));
#115809=CARTESIAN_POINT('Ctrl Pts',(70.694515724827,7.37637713374769,0.));
#115810=CARTESIAN_POINT('Ctrl Pts',(70.7147984363424,7.38533681887033,0.));
#115811=CARTESIAN_POINT('Ctrl Pts',(70.735114793895,7.39433604117892,0.));
#115812=CARTESIAN_POINT('Ctrl Pts',(70.7554646366514,7.40337480758231,0.));
#115813=CARTESIAN_POINT('Ctrl Pts',(70.7758478045576,7.41245312484488,0.));
#115814=CARTESIAN_POINT('Ctrl Pts',(70.7962641383351,7.42157099959317,0.));
#115815=CARTESIAN_POINT('Ctrl Pts',(70.8167134794738,7.43072843832009,0.));
#115816=CARTESIAN_POINT('Ctrl Pts',(70.8371956702242,7.43992544738608,0.));
#115817=CARTESIAN_POINT('Ctrl Pts',(70.8577105535841,7.44916203301646,0.));
#115818=CARTESIAN_POINT('Ctrl Pts',(70.8782579732885,7.45843820129777,0.));
#115819=CARTESIAN_POINT('Ctrl Pts',(70.8988377738088,7.4677539581852,0.));
#115820=CARTESIAN_POINT('Ctrl Pts',(70.9194498003483,7.47710930950555,0.));
#115821=CARTESIAN_POINT('Ctrl Pts',(70.9400938988373,7.48650426095824,0.));
#115822=CARTESIAN_POINT('Ctrl Pts',(70.9607699159234,7.49593881811142,0.));
#115823=CARTESIAN_POINT('Ctrl Pts',(70.9814776989637,7.5054129863995,0.));
#115824=CARTESIAN_POINT('Ctrl Pts',(71.0022170960235,7.51492677113113,0.));
#115825=CARTESIAN_POINT('Ctrl Pts',(71.0229879558713,7.52448017749137,0.));
#115826=CARTESIAN_POINT('Ctrl Pts',(71.0437901279722,7.53407321054255,0.));
#115827=CARTESIAN_POINT('Ctrl Pts',(71.0646234624783,7.5437058752195,0.));
#115828=CARTESIAN_POINT('Ctrl Pts',(71.0854878102203,7.55337817632874,0.));
#115829=CARTESIAN_POINT('Ctrl Pts',(71.1063830227074,7.56309011855618,0.));
#115830=CARTESIAN_POINT('Ctrl Pts',(71.1273089521218,7.57284170646867,0.));
#115831=CARTESIAN_POINT('Ctrl Pts',(71.1482654513133,7.58263294451467,0.));
#115832=CARTESIAN_POINT('Ctrl Pts',(71.1692523737887,7.59246383701861,0.));
#115833=CARTESIAN_POINT('Ctrl Pts',(71.1902695737063,7.60233438818157,0.));
#115834=CARTESIAN_POINT('Ctrl Pts',(71.2113169058778,7.61224460208888,0.));
#115835=CARTESIAN_POINT('Ctrl Pts',(71.232394225762,7.62219448271126,0.));
#115836=CARTESIAN_POINT('Ctrl Pts',(71.2535013894587,7.63218403390516,0.));
#115837=CARTESIAN_POINT('Ctrl Pts',(71.2746382536974,7.64221325940673,0.));
#115838=CARTESIAN_POINT('Ctrl Pts',(71.2958046758334,7.65228216283344,0.));
#115839=CARTESIAN_POINT('Ctrl Pts',(71.3170005138474,7.6623907476912,0.));
#115840=CARTESIAN_POINT('Ctrl Pts',(71.3382256263405,7.67253901737541,0.));
#115841=CARTESIAN_POINT('Ctrl Pts',(71.3594798725294,7.68272697517104,0.));
#115842=CARTESIAN_POINT('Ctrl Pts',(71.380763112236,7.69295462424648,0.));
#115843=CARTESIAN_POINT('Ctrl Pts',(71.4020752058827,7.70322196765574,0.));
#115844=CARTESIAN_POINT('Ctrl Pts',(71.4234160144943,7.71352900834539,0.));
#115845=CARTESIAN_POINT('Ctrl Pts',(71.4447853996919,7.72387574915546,0.));
#115846=CARTESIAN_POINT('Ctrl Pts',(71.4661832236881,7.73426219281933,0.));
#115847=CARTESIAN_POINT('Ctrl Pts',(71.487609349277,7.74468834195735,0.));
#115848=CARTESIAN_POINT('Ctrl Pts',(71.5090636398307,7.75515419907956,0.));
#115849=CARTESIAN_POINT('Ctrl Pts',(71.5305459592987,7.7656597665922,0.));
#115850=CARTESIAN_POINT('Ctrl Pts',(71.5520561722039,7.77620504679869,0.));
#115851=CARTESIAN_POINT('Ctrl Pts',(71.5735941436366,7.78679004189936,0.));
#115852=CARTESIAN_POINT('Ctrl Pts',(71.5951597392471,7.79741475398513,0.));
#115853=CARTESIAN_POINT('Ctrl Pts',(71.616752825242,7.80807918504018,0.));
#115854=CARTESIAN_POINT('Ctrl Pts',(71.638373268384,7.81878333694857,0.));
#115855=CARTESIAN_POINT('Ctrl Pts',(71.6600209359869,7.82952721149505,0.));
#115856=CARTESIAN_POINT('Ctrl Pts',(71.681695695912,7.8403108103649,0.));
#115857=CARTESIAN_POINT('Ctrl Pts',(71.7033974165576,7.8511341351374,0.));
#115858=CARTESIAN_POINT('Ctrl Pts',(71.7251259668573,7.86199718728831,0.));
#115859=CARTESIAN_POINT('Ctrl Pts',(71.7468812162795,7.87289996819656,0.));
#115860=CARTESIAN_POINT('Ctrl Pts',(71.768663034824,7.88384247914523,0.));
#115861=CARTESIAN_POINT('Ctrl Pts',(71.7904712930172,7.89482472132136,0.));
#115862=CARTESIAN_POINT('Ctrl Pts',(71.8123058619038,7.90584669580957,0.));
#115863=CARTESIAN_POINT('Ctrl Pts',(71.8341666130424,7.91690840359372,0.));
#115864=CARTESIAN_POINT('Ctrl Pts',(71.8560534185071,7.92800984556401,0.));
#115865=CARTESIAN_POINT('Ctrl Pts',(71.8779661508833,7.93915102251797,0.));
#115866=CARTESIAN_POINT('Ctrl Pts',(71.8999046832642,7.95033193516047,0.));
#115867=CARTESIAN_POINT('Ctrl Pts',(71.9218688892426,7.96155258409753,0.));
#115868=CARTESIAN_POINT('Ctrl Pts',(71.9438586429072,7.97281296983703,0.));
#115869=CARTESIAN_POINT('Ctrl Pts',(71.9658738188421,7.98411309279599,0.));
#115870=CARTESIAN_POINT('Ctrl Pts',(71.9879142921248,7.99545295330183,0.));
#115871=CARTESIAN_POINT('Ctrl Pts',(72.0099799383216,8.00683255159251,0.));
#115872=CARTESIAN_POINT('Ctrl Pts',(72.0320706334802,8.01825188781071,0.));
#115873=CARTESIAN_POINT('Ctrl Pts',(72.0541862541262,8.0297109620033,0.));
#115874=CARTESIAN_POINT('Ctrl Pts',(72.0763266772632,8.04120977412893,0.));
#115875=CARTESIAN_POINT('Ctrl Pts',(72.0984917803702,8.05274832405958,0.));
#115876=CARTESIAN_POINT('Ctrl Pts',(72.1206814413985,8.06432661158091,0.));
#115877=CARTESIAN_POINT('Ctrl Pts',(72.1428955387648,8.07594463638701,0.));
#115878=CARTESIAN_POINT('Ctrl Pts',(72.165133951346,8.08760239807816,0.));
#115879=CARTESIAN_POINT('Ctrl Pts',(72.18739655848,8.09929989616875,0.));
#115880=CARTESIAN_POINT('Ctrl Pts',(72.2096832399626,8.11103713008923,0.));
#115881=CARTESIAN_POINT('Ctrl Pts',(72.2319938760451,8.12281409918663,0.));
#115882=CARTESIAN_POINT('Ctrl Pts',(72.2543283474279,8.1346308027203,0.));
#115883=CARTESIAN_POINT('Ctrl Pts',(72.2766865352552,8.14648723985794,0.));
#115884=CARTESIAN_POINT('Ctrl Pts',(72.2990683211155,8.15838340968329,0.));
#115885=CARTESIAN_POINT('Ctrl Pts',(72.3214735870402,8.17031931119883,0.));
#115886=CARTESIAN_POINT('Ctrl Pts',(72.3439022155007,8.18229494332623,0.));
#115887=CARTESIAN_POINT('Ctrl Pts',(72.3663540894034,8.1943103049032,0.));
#115888=CARTESIAN_POINT('Ctrl Pts',(72.3888290920845,8.20636539467783,0.));
#115889=CARTESIAN_POINT('Ctrl Pts',(72.4113271073091,8.21846021131565,0.));
#115890=CARTESIAN_POINT('Ctrl Pts',(72.4338480192701,8.23059475340355,0.));
#115891=CARTESIAN_POINT('Ctrl Pts',(72.4563917125842,8.24276901945038,0.));
#115892=CARTESIAN_POINT('Ctrl Pts',(72.4789580722871,8.25498300788494,0.));
#115893=CARTESIAN_POINT('Ctrl Pts',(72.501546983825,8.26723671704925,0.));
#115894=CARTESIAN_POINT('Ctrl Pts',(72.524158333056,8.27953014520386,0.));
#115895=CARTESIAN_POINT('Ctrl Pts',(72.5467920062522,8.2918632905329,0.));
#115896=CARTESIAN_POINT('Ctrl Pts',(72.5694478900983,8.30423615114456,0.));
#115897=CARTESIAN_POINT('Ctrl Pts',(72.5921258716899,8.3166487250701,0.));
#115898=CARTESIAN_POINT('Ctrl Pts',(72.614825838529,8.32910101025654,0.));
#115899=CARTESIAN_POINT('Ctrl Pts',(72.6375476785208,8.34159300456966,0.));
#115900=CARTESIAN_POINT('Ctrl Pts',(72.6602912799689,8.35412470580084,0.));
#115901=CARTESIAN_POINT('Ctrl Pts',(72.68305653157,8.36669611166835,0.));
#115902=CARTESIAN_POINT('Ctrl Pts',(72.7058433224072,8.37930721981736,0.));
#115903=CARTESIAN_POINT('Ctrl Pts',(72.728651541938,8.39195802781408,0.));
#115904=CARTESIAN_POINT('Ctrl Pts',(72.7514810799932,8.40464853314494,0.));
#115905=CARTESIAN_POINT('Ctrl Pts',(72.7743318267876,8.41737873322354,0.));
#115906=CARTESIAN_POINT('Ctrl Pts',(72.7972036729283,8.43014862539172,0.));
#115907=CARTESIAN_POINT('Ctrl Pts',(72.8200965094197,8.44295820691908,0.));
#115908=CARTESIAN_POINT('Ctrl Pts',(72.8430102276703,8.45580747499772,0.));
#115909=CARTESIAN_POINT('Ctrl Pts',(72.8659447194918,8.46869642673764,0.));
#115910=CARTESIAN_POINT('Ctrl Pts',(72.888899877077,8.48162505917629,0.));
#115911=CARTESIAN_POINT('Ctrl Pts',(72.9118755929785,8.49459336928277,0.));
#115912=CARTESIAN_POINT('Ctrl Pts',(72.9348717600837,8.5076013539598,0.));
#115913=CARTESIAN_POINT('Ctrl Pts',(72.9578882715923,8.52064901004245,0.));
#115914=CARTESIAN_POINT('Ctrl Pts',(72.9809250209843,8.53373633429304,0.));
#115915=CARTESIAN_POINT('Ctrl Pts',(73.0039819020663,8.5468633234044,0.));
#115916=CARTESIAN_POINT('Ctrl Pts',(73.0270588090193,8.56002997400097,0.));
#115917=CARTESIAN_POINT('Ctrl Pts',(73.0501556364482,8.57323628263596,0.));
#115918=CARTESIAN_POINT('Ctrl Pts',(73.073272279419,8.58648224578724,0.));
#115919=CARTESIAN_POINT('Ctrl Pts',(73.0964086335226,8.5997678598454,0.));
#115920=CARTESIAN_POINT('Ctrl Pts',(73.1195645948169,8.6130931211199,0.));
#115921=CARTESIAN_POINT('Ctrl Pts',(73.142740059703,8.62645802585476,0.));
#115922=CARTESIAN_POINT('Ctrl Pts',(73.165934924813,8.63986257023736,0.));
#115923=CARTESIAN_POINT('Ctrl Pts',(73.1891490869057,8.65330675040537,0.));
#115924=CARTESIAN_POINT('Ctrl Pts',(73.2123824427212,8.66679056245097,0.));
#115925=CARTESIAN_POINT('Ctrl Pts',(73.2356348889704,8.68031400241885,0.));
#115926=CARTESIAN_POINT('Ctrl Pts',(73.2589063226373,8.69387706629305,0.));
#115927=CARTESIAN_POINT('Ctrl Pts',(73.282196641216,8.70747974998246,0.));
#115928=CARTESIAN_POINT('Ctrl Pts',(73.3055057429744,8.72112204930233,0.));
#115929=CARTESIAN_POINT('Ctrl Pts',(73.3288335271989,8.73480395995361,0.));
#115930=CARTESIAN_POINT('Ctrl Pts',(73.3521798944595,8.74852547749737,0.));
#115931=CARTESIAN_POINT('Ctrl Pts',(73.3755447460235,8.76228659740306,0.));
#115932=CARTESIAN_POINT('Ctrl Pts',(73.3989279832808,8.77608731509305,0.));
#115933=CARTESIAN_POINT('Ctrl Pts',(73.422329507112,8.78992762598739,0.));
#115934=CARTESIAN_POINT('Ctrl Pts',(73.4457492173949,8.80380752553715,0.));
#115935=CARTESIAN_POINT('Ctrl Pts',(73.4691870121608,8.81772700927594,0.));
#115936=CARTESIAN_POINT('Ctrl Pts',(73.4926427882787,8.83168607277416,0.));
#115937=CARTESIAN_POINT('Ctrl Pts',(73.5161164429765,8.84568471153895,0.));
#115938=CARTESIAN_POINT('Ctrl Pts',(73.5396078751672,8.85972292092184,0.));
#115939=CARTESIAN_POINT('Ctrl Pts',(73.5631169867113,8.87380069602956,0.));
#115940=CARTESIAN_POINT('Ctrl Pts',(73.5866436840493,8.88791803160342,0.));
#115941=CARTESIAN_POINT('Ctrl Pts',(73.6101878785868,8.90207492198872,0.));
#115942=CARTESIAN_POINT('Ctrl Pts',(73.6303847393446,8.91424402151035,0.));
#115943=CARTESIAN_POINT('Ctrl Pts',(73.6458786305791,8.92359518177574,0.));
#115944=CARTESIAN_POINT('Ctrl Pts',(73.6566618621802,8.93011088816058,0.));
#115945=CARTESIAN_POINT('Ctrl Pts',(73.6627293782269,8.93377955964027,0.));
#115946=CARTESIAN_POINT('Ctrl Pts',(73.6640787197679,8.93459554655865,0.));
#115947=CARTESIAN_POINT('',(69.6540253893192,6.95102489306927,12.));
#115948=CARTESIAN_POINT('',(69.6540253893192,6.95102489306927,0.));
#115949=CARTESIAN_POINT('Ctrl Pts',(73.664078719768,8.93459554655874,12.));
#115950=CARTESIAN_POINT('Ctrl Pts',(73.662729378227,8.93377955964033,12.));
#115951=CARTESIAN_POINT('Ctrl Pts',(73.6566618621802,8.93011088816063,12.));
#115952=CARTESIAN_POINT('Ctrl Pts',(73.6458786305792,8.92359518177578,12.));
#115953=CARTESIAN_POINT('Ctrl Pts',(73.6303847393446,8.91424402151036,12.));
#115954=CARTESIAN_POINT('Ctrl Pts',(73.6101878785868,8.90207492198872,12.));
#115955=CARTESIAN_POINT('Ctrl Pts',(73.5866436840493,8.88791803160342,12.));
#115956=CARTESIAN_POINT('Ctrl Pts',(73.5631169867113,8.87380069602956,12.));
#115957=CARTESIAN_POINT('Ctrl Pts',(73.5396078751672,8.85972292092184,12.));
#115958=CARTESIAN_POINT('Ctrl Pts',(73.5161164429765,8.84568471153895,12.));
#115959=CARTESIAN_POINT('Ctrl Pts',(73.4926427882787,8.83168607277416,12.));
#115960=CARTESIAN_POINT('Ctrl Pts',(73.4691870121608,8.81772700927594,12.));
#115961=CARTESIAN_POINT('Ctrl Pts',(73.4457492173949,8.80380752553715,12.));
#115962=CARTESIAN_POINT('Ctrl Pts',(73.422329507112,8.78992762598739,12.));
#115963=CARTESIAN_POINT('Ctrl Pts',(73.3989279832808,8.77608731509305,12.));
#115964=CARTESIAN_POINT('Ctrl Pts',(73.3755447460235,8.76228659740306,12.));
#115965=CARTESIAN_POINT('Ctrl Pts',(73.3521798944595,8.74852547749737,12.));
#115966=CARTESIAN_POINT('Ctrl Pts',(73.3288335271989,8.73480395995361,12.));
#115967=CARTESIAN_POINT('Ctrl Pts',(73.3055057429744,8.72112204930233,12.));
#115968=CARTESIAN_POINT('Ctrl Pts',(73.282196641216,8.70747974998246,12.));
#115969=CARTESIAN_POINT('Ctrl Pts',(73.2589063226373,8.69387706629305,12.));
#115970=CARTESIAN_POINT('Ctrl Pts',(73.2356348889704,8.68031400241885,12.));
#115971=CARTESIAN_POINT('Ctrl Pts',(73.2123824427212,8.66679056245097,12.));
#115972=CARTESIAN_POINT('Ctrl Pts',(73.1891490869057,8.65330675040537,12.));
#115973=CARTESIAN_POINT('Ctrl Pts',(73.165934924813,8.63986257023736,12.));
#115974=CARTESIAN_POINT('Ctrl Pts',(73.142740059703,8.62645802585476,12.));
#115975=CARTESIAN_POINT('Ctrl Pts',(73.1195645948169,8.6130931211199,12.));
#115976=CARTESIAN_POINT('Ctrl Pts',(73.0964086335226,8.5997678598454,12.));
#115977=CARTESIAN_POINT('Ctrl Pts',(73.073272279419,8.58648224578724,12.));
#115978=CARTESIAN_POINT('Ctrl Pts',(73.0501556364482,8.57323628263596,12.));
#115979=CARTESIAN_POINT('Ctrl Pts',(73.0270588090193,8.56002997400097,12.));
#115980=CARTESIAN_POINT('Ctrl Pts',(73.0039819020663,8.5468633234044,12.));
#115981=CARTESIAN_POINT('Ctrl Pts',(72.9809250209843,8.53373633429304,12.));
#115982=CARTESIAN_POINT('Ctrl Pts',(72.9578882715923,8.52064901004245,12.));
#115983=CARTESIAN_POINT('Ctrl Pts',(72.9348717600837,8.5076013539598,12.));
#115984=CARTESIAN_POINT('Ctrl Pts',(72.9118755929785,8.49459336928277,12.));
#115985=CARTESIAN_POINT('Ctrl Pts',(72.888899877077,8.48162505917629,12.));
#115986=CARTESIAN_POINT('Ctrl Pts',(72.8659447194918,8.46869642673764,12.));
#115987=CARTESIAN_POINT('Ctrl Pts',(72.8430102276703,8.45580747499772,12.));
#115988=CARTESIAN_POINT('Ctrl Pts',(72.8200965094197,8.44295820691908,12.));
#115989=CARTESIAN_POINT('Ctrl Pts',(72.7972036729283,8.43014862539172,12.));
#115990=CARTESIAN_POINT('Ctrl Pts',(72.7743318267876,8.41737873322354,12.));
#115991=CARTESIAN_POINT('Ctrl Pts',(72.7514810799932,8.40464853314494,12.));
#115992=CARTESIAN_POINT('Ctrl Pts',(72.728651541938,8.39195802781408,12.));
#115993=CARTESIAN_POINT('Ctrl Pts',(72.7058433224072,8.37930721981736,12.));
#115994=CARTESIAN_POINT('Ctrl Pts',(72.68305653157,8.36669611166835,12.));
#115995=CARTESIAN_POINT('Ctrl Pts',(72.6602912799689,8.35412470580084,12.));
#115996=CARTESIAN_POINT('Ctrl Pts',(72.6375476785208,8.34159300456966,12.));
#115997=CARTESIAN_POINT('Ctrl Pts',(72.614825838529,8.32910101025654,12.));
#115998=CARTESIAN_POINT('Ctrl Pts',(72.5921258716899,8.3166487250701,12.));
#115999=CARTESIAN_POINT('Ctrl Pts',(72.5694478900983,8.30423615114456,12.));
#116000=CARTESIAN_POINT('Ctrl Pts',(72.5467920062522,8.2918632905329,12.));
#116001=CARTESIAN_POINT('Ctrl Pts',(72.524158333056,8.27953014520386,12.));
#116002=CARTESIAN_POINT('Ctrl Pts',(72.501546983825,8.26723671704925,12.));
#116003=CARTESIAN_POINT('Ctrl Pts',(72.4789580722871,8.25498300788494,12.));
#116004=CARTESIAN_POINT('Ctrl Pts',(72.4563917125842,8.24276901945038,12.));
#116005=CARTESIAN_POINT('Ctrl Pts',(72.4338480192701,8.23059475340355,12.));
#116006=CARTESIAN_POINT('Ctrl Pts',(72.4113271073091,8.21846021131565,12.));
#116007=CARTESIAN_POINT('Ctrl Pts',(72.3888290920845,8.20636539467783,12.));
#116008=CARTESIAN_POINT('Ctrl Pts',(72.3663540894034,8.1943103049032,12.));
#116009=CARTESIAN_POINT('Ctrl Pts',(72.3439022155007,8.18229494332623,12.));
#116010=CARTESIAN_POINT('Ctrl Pts',(72.3214735870402,8.17031931119883,12.));
#116011=CARTESIAN_POINT('Ctrl Pts',(72.2990683211155,8.15838340968329,12.));
#116012=CARTESIAN_POINT('Ctrl Pts',(72.2766865352552,8.14648723985794,12.));
#116013=CARTESIAN_POINT('Ctrl Pts',(72.2543283474279,8.1346308027203,12.));
#116014=CARTESIAN_POINT('Ctrl Pts',(72.2319938760451,8.12281409918663,12.));
#116015=CARTESIAN_POINT('Ctrl Pts',(72.2096832399626,8.11103713008923,12.));
#116016=CARTESIAN_POINT('Ctrl Pts',(72.18739655848,8.09929989616875,12.));
#116017=CARTESIAN_POINT('Ctrl Pts',(72.165133951346,8.08760239807816,12.));
#116018=CARTESIAN_POINT('Ctrl Pts',(72.1428955387648,8.07594463638701,12.));
#116019=CARTESIAN_POINT('Ctrl Pts',(72.1206814413985,8.06432661158091,12.));
#116020=CARTESIAN_POINT('Ctrl Pts',(72.0984917803702,8.05274832405958,12.));
#116021=CARTESIAN_POINT('Ctrl Pts',(72.0763266772632,8.04120977412893,12.));
#116022=CARTESIAN_POINT('Ctrl Pts',(72.0541862541262,8.0297109620033,12.));
#116023=CARTESIAN_POINT('Ctrl Pts',(72.0320706334802,8.01825188781071,12.));
#116024=CARTESIAN_POINT('Ctrl Pts',(72.0099799383216,8.00683255159251,12.));
#116025=CARTESIAN_POINT('Ctrl Pts',(71.9879142921248,7.99545295330183,12.));
#116026=CARTESIAN_POINT('Ctrl Pts',(71.9658738188421,7.98411309279599,12.));
#116027=CARTESIAN_POINT('Ctrl Pts',(71.9438586429072,7.97281296983703,12.));
#116028=CARTESIAN_POINT('Ctrl Pts',(71.9218688892426,7.96155258409753,12.));
#116029=CARTESIAN_POINT('Ctrl Pts',(71.8999046832642,7.95033193516047,12.));
#116030=CARTESIAN_POINT('Ctrl Pts',(71.8779661508833,7.93915102251797,12.));
#116031=CARTESIAN_POINT('Ctrl Pts',(71.8560534185071,7.92800984556401,12.));
#116032=CARTESIAN_POINT('Ctrl Pts',(71.8341666130424,7.91690840359372,12.));
#116033=CARTESIAN_POINT('Ctrl Pts',(71.8123058619038,7.90584669580957,12.));
#116034=CARTESIAN_POINT('Ctrl Pts',(71.7904712930172,7.89482472132136,12.));
#116035=CARTESIAN_POINT('Ctrl Pts',(71.768663034824,7.88384247914523,12.));
#116036=CARTESIAN_POINT('Ctrl Pts',(71.7468812162795,7.87289996819656,12.));
#116037=CARTESIAN_POINT('Ctrl Pts',(71.7251259668573,7.86199718728831,12.));
#116038=CARTESIAN_POINT('Ctrl Pts',(71.7033974165576,7.8511341351374,12.));
#116039=CARTESIAN_POINT('Ctrl Pts',(71.681695695912,7.8403108103649,12.));
#116040=CARTESIAN_POINT('Ctrl Pts',(71.6600209359869,7.82952721149505,12.));
#116041=CARTESIAN_POINT('Ctrl Pts',(71.638373268384,7.81878333694857,12.));
#116042=CARTESIAN_POINT('Ctrl Pts',(71.616752825242,7.80807918504018,12.));
#116043=CARTESIAN_POINT('Ctrl Pts',(71.5951597392471,7.79741475398513,12.));
#116044=CARTESIAN_POINT('Ctrl Pts',(71.5735941436366,7.78679004189936,12.));
#116045=CARTESIAN_POINT('Ctrl Pts',(71.5520561722039,7.77620504679869,12.));
#116046=CARTESIAN_POINT('Ctrl Pts',(71.5305459592987,7.7656597665922,12.));
#116047=CARTESIAN_POINT('Ctrl Pts',(71.5090636398307,7.75515419907956,12.));
#116048=CARTESIAN_POINT('Ctrl Pts',(71.487609349277,7.74468834195735,12.));
#116049=CARTESIAN_POINT('Ctrl Pts',(71.4661832236881,7.73426219281933,12.));
#116050=CARTESIAN_POINT('Ctrl Pts',(71.4447853996919,7.72387574915546,12.));
#116051=CARTESIAN_POINT('Ctrl Pts',(71.4234160144943,7.71352900834539,12.));
#116052=CARTESIAN_POINT('Ctrl Pts',(71.4020752058827,7.70322196765574,12.));
#116053=CARTESIAN_POINT('Ctrl Pts',(71.380763112236,7.69295462424648,12.));
#116054=CARTESIAN_POINT('Ctrl Pts',(71.3594798725294,7.68272697517104,12.));
#116055=CARTESIAN_POINT('Ctrl Pts',(71.3382256263405,7.67253901737541,12.));
#116056=CARTESIAN_POINT('Ctrl Pts',(71.3170005138474,7.6623907476912,12.));
#116057=CARTESIAN_POINT('Ctrl Pts',(71.2958046758334,7.65228216283344,12.));
#116058=CARTESIAN_POINT('Ctrl Pts',(71.2746382536974,7.64221325940673,12.));
#116059=CARTESIAN_POINT('Ctrl Pts',(71.2535013894587,7.63218403390516,12.));
#116060=CARTESIAN_POINT('Ctrl Pts',(71.232394225762,7.62219448271126,12.));
#116061=CARTESIAN_POINT('Ctrl Pts',(71.2113169058778,7.61224460208888,12.));
#116062=CARTESIAN_POINT('Ctrl Pts',(71.1902695737063,7.60233438818157,12.));
#116063=CARTESIAN_POINT('Ctrl Pts',(71.1692523737887,7.59246383701861,12.));
#116064=CARTESIAN_POINT('Ctrl Pts',(71.1482654513133,7.58263294451467,12.));
#116065=CARTESIAN_POINT('Ctrl Pts',(71.1273089521218,7.57284170646867,12.));
#116066=CARTESIAN_POINT('Ctrl Pts',(71.1063830227074,7.56309011855618,12.));
#116067=CARTESIAN_POINT('Ctrl Pts',(71.0854878102203,7.55337817632874,12.));
#116068=CARTESIAN_POINT('Ctrl Pts',(71.0646234624783,7.5437058752195,12.));
#116069=CARTESIAN_POINT('Ctrl Pts',(71.0437901279722,7.53407321054255,12.));
#116070=CARTESIAN_POINT('Ctrl Pts',(71.0229879558713,7.52448017749137,12.));
#116071=CARTESIAN_POINT('Ctrl Pts',(71.0022170960235,7.51492677113113,12.));
#116072=CARTESIAN_POINT('Ctrl Pts',(70.9814776989637,7.5054129863995,12.));
#116073=CARTESIAN_POINT('Ctrl Pts',(70.9607699159234,7.49593881811142,12.));
#116074=CARTESIAN_POINT('Ctrl Pts',(70.9400938988373,7.48650426095824,12.));
#116075=CARTESIAN_POINT('Ctrl Pts',(70.9194498003483,7.47710930950555,12.));
#116076=CARTESIAN_POINT('Ctrl Pts',(70.8988377738088,7.4677539581852,12.));
#116077=CARTESIAN_POINT('Ctrl Pts',(70.8782579732885,7.45843820129777,12.));
#116078=CARTESIAN_POINT('Ctrl Pts',(70.8577105535841,7.44916203301646,12.));
#116079=CARTESIAN_POINT('Ctrl Pts',(70.8371956702242,7.43992544738608,12.));
#116080=CARTESIAN_POINT('Ctrl Pts',(70.8167134794738,7.43072843832009,12.));
#116081=CARTESIAN_POINT('Ctrl Pts',(70.7962641383351,7.42157099959317,12.));
#116082=CARTESIAN_POINT('Ctrl Pts',(70.7758478045576,7.41245312484488,12.));
#116083=CARTESIAN_POINT('Ctrl Pts',(70.7554646366514,7.40337480758231,12.));
#116084=CARTESIAN_POINT('Ctrl Pts',(70.735114793895,7.39433604117892,12.));
#116085=CARTESIAN_POINT('Ctrl Pts',(70.7147984363424,7.38533681887033,12.));
#116086=CARTESIAN_POINT('Ctrl Pts',(70.694515724827,7.37637713374769,12.));
#116087=CARTESIAN_POINT('Ctrl Pts',(70.6742668209687,7.36745697876302,12.));
#116088=CARTESIAN_POINT('Ctrl Pts',(70.6540518871775,7.35857634673056,12.));
#116089=CARTESIAN_POINT('Ctrl Pts',(70.6338710866562,7.34973523032579,12.));
#116090=CARTESIAN_POINT('Ctrl Pts',(70.6137245833996,7.34093362208009,12.));
#116091=CARTESIAN_POINT('Ctrl Pts',(70.5936125421946,7.33217151437592,12.));
#116092=CARTESIAN_POINT('Ctrl Pts',(70.5735351286476,7.32344889945221,12.));
#116093=CARTESIAN_POINT('Ctrl Pts',(70.5534925092043,7.31476576940393,12.));
#116094=CARTESIAN_POINT('Ctrl Pts',(70.5334848511681,7.30612211618054,12.));
#116095=CARTESIAN_POINT('Ctrl Pts',(70.5135123227169,7.29751793157824,12.));
#116096=CARTESIAN_POINT('Ctrl Pts',(70.4935750929058,7.28895320723863,12.));
#116097=CARTESIAN_POINT('Ctrl Pts',(70.4736733316487,7.28042793465472,12.));
#116098=CARTESIAN_POINT('Ctrl Pts',(70.4538072096992,7.27194210517064,12.));
#116099=CARTESIAN_POINT('Ctrl Pts',(70.4339768986346,7.26349570998034,12.));
#116100=CARTESIAN_POINT('Ctrl Pts',(70.4141825708178,7.25508874012044,12.));
#116101=CARTESIAN_POINT('Ctrl Pts',(70.3944243994504,7.24672118647086,12.));
#116102=CARTESIAN_POINT('Ctrl Pts',(70.3747025586552,7.23839303975608,12.));
#116103=CARTESIAN_POINT('Ctrl Pts',(70.3550172235486,7.2301042905423,12.));
#116104=CARTESIAN_POINT('Ctrl Pts',(70.3353685703112,7.22185492923192,12.));
#116105=CARTESIAN_POINT('Ctrl Pts',(70.3157567762588,7.21364494605451,12.));
#116106=CARTESIAN_POINT('Ctrl Pts',(70.2961820197077,7.20547433107483,12.));
#116107=CARTESIAN_POINT('Ctrl Pts',(70.2766444798285,7.19734307419874,12.));
#116108=CARTESIAN_POINT('Ctrl Pts',(70.2571443365192,7.18925116517556,12.));
#116109=CARTESIAN_POINT('Ctrl Pts',(70.2376817702215,7.18119859359779,12.));
#116110=CARTESIAN_POINT('Ctrl Pts',(70.2182569618994,7.17318534889717,12.));
#116111=CARTESIAN_POINT('Ctrl Pts',(70.1988700934593,7.16521142033865,12.));
#116112=CARTESIAN_POINT('Ctrl Pts',(70.1795213481185,7.15727679700934,12.));
#116113=CARTESIAN_POINT('Ctrl Pts',(70.1602109107202,7.14938146780815,12.));
#116114=CARTESIAN_POINT('Ctrl Pts',(70.1409389682424,7.14152542142375,12.));
#116115=CARTESIAN_POINT('Ctrl Pts',(70.1217057094499,7.13370864634444,12.));
#116116=CARTESIAN_POINT('Ctrl Pts',(70.1025113239495,7.12593113088905,12.));
#116117=CARTESIAN_POINT('Ctrl Pts',(70.0833560013975,7.11819286322827,12.));
#116118=CARTESIAN_POINT('Ctrl Pts',(70.0642399306869,7.11049383140447,12.));
#116119=CARTESIAN_POINT('Ctrl Pts',(70.0451632990086,7.10283402335035,12.));
#116120=CARTESIAN_POINT('Ctrl Pts',(70.0261262936388,7.0952134268425,12.));
#116121=CARTESIAN_POINT('Ctrl Pts',(70.0071291040766,7.08763202944247,12.));
#116122=CARTESIAN_POINT('Ctrl Pts',(69.988171923788,7.08008981844653,12.));
#116123=CARTESIAN_POINT('Ctrl Pts',(69.9692549527296,7.07258678080832,12.));
#116124=CARTESIAN_POINT('Ctrl Pts',(69.9503783975727,7.06512290312851,12.));
#116125=CARTESIAN_POINT('Ctrl Pts',(69.9315424664291,7.05769817180858,12.));
#116126=CARTESIAN_POINT('Ctrl Pts',(69.9127473642099,7.05031257318117,12.));
#116127=CARTESIAN_POINT('Ctrl Pts',(69.8939932885841,7.04296609362167,12.));
#116128=CARTESIAN_POINT('Ctrl Pts',(69.8752804235238,7.03565871972222,12.));
#116129=CARTESIAN_POINT('Ctrl Pts',(69.8566089455375,7.02839043811814,12.));
#116130=CARTESIAN_POINT('Ctrl Pts',(69.8379790360518,7.02116123514453,12.));
#116131=CARTESIAN_POINT('Ctrl Pts',(69.8193908913722,7.01397109655456,12.));
#116132=CARTESIAN_POINT('Ctrl Pts',(69.8008447346863,7.00682000718152,12.));
#116133=CARTESIAN_POINT('Ctrl Pts',(69.782340824259,6.99970795069477,12.));
#116134=CARTESIAN_POINT('Ctrl Pts',(69.7638794280419,6.99263491027942,12.));
#116135=CARTESIAN_POINT('Ctrl Pts',(69.7454607995607,6.98560086924215,12.));
#116136=CARTESIAN_POINT('Ctrl Pts',(69.7270851557366,6.97860581164528,12.));
#116137=CARTESIAN_POINT('Ctrl Pts',(69.7087526479973,6.97164972291441,12.));
#116138=CARTESIAN_POINT('Ctrl Pts',(69.6904633605421,6.96473259049514,12.));
#116139=CARTESIAN_POINT('Ctrl Pts',(69.6758665380378,6.95923004173592,12.));
#116140=CARTESIAN_POINT('Ctrl Pts',(69.664938391983,6.95512065317601,12.));
#116141=CARTESIAN_POINT('Ctrl Pts',(69.6576616146467,6.95238884849026,12.));
#116142=CARTESIAN_POINT('Ctrl Pts',(69.6540253893192,6.95102489306927,12.));
#116143=CARTESIAN_POINT('Ctrl Pts',(73.466479592994,10.4355099267296,-5.55111512312578E-16));
#116144=CARTESIAN_POINT('Ctrl Pts',(73.466479592994,10.4355099267296,4.));
#116145=CARTESIAN_POINT('Ctrl Pts',(73.466479592994,10.4355099267296,8.));
#116146=CARTESIAN_POINT('Ctrl Pts',(73.466479592994,10.4355099267296,12.));
#116147=CARTESIAN_POINT('Ctrl Pts',(73.5720190200069,10.4049225807075,-5.55111512312578E-16));
#116148=CARTESIAN_POINT('Ctrl Pts',(73.5720190200069,10.4049225807075,4.));
#116149=CARTESIAN_POINT('Ctrl Pts',(73.5720190200068,10.4049225807075,8.));
#116150=CARTESIAN_POINT('Ctrl Pts',(73.5720190200068,10.4049225807075,12.));
#116151=CARTESIAN_POINT('Ctrl Pts',(73.7377969500799,10.2883434191782,-5.55111512312578E-16));
#116152=CARTESIAN_POINT('Ctrl Pts',(73.7377969500799,10.2883434191782,4.));
#116153=CARTESIAN_POINT('Ctrl Pts',(73.7377969500798,10.2883434191783,7.99999999999999));
#116154=CARTESIAN_POINT('Ctrl Pts',(73.7377969500798,10.2883434191783,12.));
#116155=CARTESIAN_POINT('Ctrl Pts',(73.8116652760545,10.1042001607579,-5.55111512312578E-16));
#116156=CARTESIAN_POINT('Ctrl Pts',(73.8116652760545,10.1042001607579,4.));
#116157=CARTESIAN_POINT('Ctrl Pts',(73.8116652760545,10.1042001607579,8.00000000000001));
#116158=CARTESIAN_POINT('Ctrl Pts',(73.8116652760545,10.1042001607579,12.));
#116159=CARTESIAN_POINT('Ctrl Pts',(73.8227522002495,10.0225374821234,-5.55111512312578E-16));
#116160=CARTESIAN_POINT('Ctrl Pts',(73.8227522002495,10.0225374821234,4.));
#116161=CARTESIAN_POINT('Ctrl Pts',(73.8227522002494,10.0225374821234,8.));
#116162=CARTESIAN_POINT('Ctrl Pts',(73.8227522002494,10.0225374821234,12.));
#116163=CARTESIAN_POINT('',(73.466479592994,10.4355099267296,0.));
#116164=CARTESIAN_POINT('',(73.8227522002494,10.0225374821234,0.));
#116165=CARTESIAN_POINT('Ctrl Pts',(73.466479592994,10.4355099267296,2.77555756156289E-16));
#116166=CARTESIAN_POINT('Ctrl Pts',(73.5720190200069,10.4049225807075,2.77555756156289E-16));
#116167=CARTESIAN_POINT('Ctrl Pts',(73.6667492657629,10.3383059169765,2.7755575615629E-16));
#116168=CARTESIAN_POINT('Ctrl Pts',(73.7314682122214,10.2496275073218,2.77555756156289E-16));
#116169=CARTESIAN_POINT('Ctrl Pts',(73.7800074220654,10.1831187000809,2.77555756156289E-16));
#116170=CARTESIAN_POINT('Ctrl Pts',(73.8116652760545,10.1042001607579,2.77555756156288E-16));
#116171=CARTESIAN_POINT('Ctrl Pts',(73.8227522002495,10.0225374821234,2.77555756156289E-16));
#116172=CARTESIAN_POINT('',(73.8227522002494,10.0225374821234,12.));
#116173=CARTESIAN_POINT('Ctrl Pts',(73.8227522002495,10.0225374821234,-5.55111512312578E-16));
#116174=CARTESIAN_POINT('Ctrl Pts',(73.8227522002495,10.0225374821234,4.));
#116175=CARTESIAN_POINT('Ctrl Pts',(73.8227522002494,10.0225374821234,8.));
#116176=CARTESIAN_POINT('Ctrl Pts',(73.8227522002494,10.0225374821234,12.));
#116177=CARTESIAN_POINT('',(73.466479592994,10.4355099267296,12.));
#116178=CARTESIAN_POINT('Ctrl Pts',(73.8227522002494,10.0225374821234,12.));
#116179=CARTESIAN_POINT('Ctrl Pts',(73.8116652760545,10.1042001607579,12.));
#116180=CARTESIAN_POINT('Ctrl Pts',(73.7800074220654,10.1831187000809,12.));
#116181=CARTESIAN_POINT('Ctrl Pts',(73.7314682122214,10.2496275073219,12.));
#116182=CARTESIAN_POINT('Ctrl Pts',(73.6667492657628,10.3383059169765,12.));
#116183=CARTESIAN_POINT('Ctrl Pts',(73.5720190200068,10.4049225807075,12.));
#116184=CARTESIAN_POINT('Ctrl Pts',(73.466479592994,10.4355099267296,12.));
#116185=CARTESIAN_POINT('Ctrl Pts',(73.466479592994,10.4355099267296,12.));
#116186=CARTESIAN_POINT('Ctrl Pts',(73.466479592994,10.4355099267296,8.));
#116187=CARTESIAN_POINT('Ctrl Pts',(73.466479592994,10.4355099267296,4.));
#116188=CARTESIAN_POINT('Ctrl Pts',(73.466479592994,10.4355099267296,-5.55111512312578E-16));
#116189=CARTESIAN_POINT('Origin',(3.71623968689858E-10,4.90253386731614E-11,
0.));
#116190=CARTESIAN_POINT('Origin',(3.71623968689858E-10,4.90253386731614E-11,
12.));
#116191=CARTESIAN_POINT('Origin',(3.71623968689858E-10,4.90253386731614E-11,
0.));
#116192=CARTESIAN_POINT('Ctrl Pts',(74.4537274248118,-2.62535189104657,
0.));
#116193=CARTESIAN_POINT('Ctrl Pts',(74.4537274248118,-2.62535189104657,
12.));
#116194=CARTESIAN_POINT('Ctrl Pts',(74.4487312586601,-2.62283178248298,
0.));
#116195=CARTESIAN_POINT('Ctrl Pts',(74.4487312586601,-2.62283178248298,
12.));
#116196=CARTESIAN_POINT('Ctrl Pts',(74.4387409032582,-2.61779535432371,
0.));
#116197=CARTESIAN_POINT('Ctrl Pts',(74.4387409032582,-2.61779535432371,
12.));
#116198=CARTESIAN_POINT('Ctrl Pts',(74.4237613008609,-2.61025207898831,
0.));
#116199=CARTESIAN_POINT('Ctrl Pts',(74.4237613008609,-2.61025207898831,
12.));
#116200=CARTESIAN_POINT('Ctrl Pts',(74.4038003595514,-2.60021711327492,
0.));
#116201=CARTESIAN_POINT('Ctrl Pts',(74.4038003595514,-2.60021711327492,
12.));
#116202=CARTESIAN_POINT('Ctrl Pts',(74.3788689604,-2.58771130268619,0.));
#116203=CARTESIAN_POINT('Ctrl Pts',(74.3788689604,-2.58771130268619,12.));
#116204=CARTESIAN_POINT('Ctrl Pts',(74.3539573568054,-2.57524339541657,
0.));
#116205=CARTESIAN_POINT('Ctrl Pts',(74.3539573568054,-2.57524339541657,
12.));
#116206=CARTESIAN_POINT('Ctrl Pts',(74.3290655814922,-2.56281339800083,
0.));
#116207=CARTESIAN_POINT('Ctrl Pts',(74.3290655814922,-2.56281339800083,
12.));
#116208=CARTESIAN_POINT('Ctrl Pts',(74.3041936853329,-2.55042131526685,
0.));
#116209=CARTESIAN_POINT('Ctrl Pts',(74.3041936853329,-2.55042131526685,
12.));
#116210=CARTESIAN_POINT('Ctrl Pts',(74.2793417427044,-2.53806714838104,
0.));
#116211=CARTESIAN_POINT('Ctrl Pts',(74.2793417427044,-2.53806714838104,
12.));
#116212=CARTESIAN_POINT('Ctrl Pts',(74.2545098494549,-2.52575089478113,
0.));
#116213=CARTESIAN_POINT('Ctrl Pts',(74.2545098494549,-2.52575089478113,
12.));
#116214=CARTESIAN_POINT('Ctrl Pts',(74.2296981152027,-2.51347254956027,
0.));
#116215=CARTESIAN_POINT('Ctrl Pts',(74.2296981152027,-2.51347254956027,
12.));
#116216=CARTESIAN_POINT('Ctrl Pts',(74.2049066571942,-2.50123210644075,
0.));
#116217=CARTESIAN_POINT('Ctrl Pts',(74.2049066571942,-2.50123210644075,
12.));
#116218=CARTESIAN_POINT('Ctrl Pts',(74.180135593693,-2.48902955888402,0.));
#116219=CARTESIAN_POINT('Ctrl Pts',(74.180135593693,-2.48902955888402,12.));
#116220=CARTESIAN_POINT('Ctrl Pts',(74.1553850371577,-2.47686490120423,
0.));
#116221=CARTESIAN_POINT('Ctrl Pts',(74.1553850371577,-2.47686490120423,
12.));
#116222=CARTESIAN_POINT('Ctrl Pts',(74.1306550887196,-2.46473812948048,
0.));
#116223=CARTESIAN_POINT('Ctrl Pts',(74.1306550887196,-2.46473812948048,
12.));
#116224=CARTESIAN_POINT('Ctrl Pts',(74.1059458420175,-2.45264924094853,
0.));
#116225=CARTESIAN_POINT('Ctrl Pts',(74.1059458420175,-2.45264924094853,
12.));
#116226=CARTESIAN_POINT('Ctrl Pts',(74.0812573859474,-2.44059823356722,
0.));
#116227=CARTESIAN_POINT('Ctrl Pts',(74.0812573859474,-2.44059823356722,
12.));
#116228=CARTESIAN_POINT('Ctrl Pts',(74.0565898079227,-2.42858510549787,
0.));
#116229=CARTESIAN_POINT('Ctrl Pts',(74.0565898079227,-2.42858510549787,
12.));
#116230=CARTESIAN_POINT('Ctrl Pts',(74.0319431966956,-2.41660985465228,
0.));
#116231=CARTESIAN_POINT('Ctrl Pts',(74.0319431966956,-2.41660985465228,
12.));
#116232=CARTESIAN_POINT('Ctrl Pts',(74.0073176459287,-2.40467247811497,
0.));
#116233=CARTESIAN_POINT('Ctrl Pts',(74.0073176459287,-2.40467247811497,
12.));
#116234=CARTESIAN_POINT('Ctrl Pts',(73.9827132538149,-2.39277297220716,
0.));
#116235=CARTESIAN_POINT('Ctrl Pts',(73.9827132538149,-2.39277297220716,
12.));
#116236=CARTESIAN_POINT('Ctrl Pts',(73.9581301214609,-2.38091133274933,
0.));
#116237=CARTESIAN_POINT('Ctrl Pts',(73.9581301214609,-2.38091133274933,
12.));
#116238=CARTESIAN_POINT('Ctrl Pts',(73.9335683516388,-2.36908755525994,
0.));
#116239=CARTESIAN_POINT('Ctrl Pts',(73.9335683516388,-2.36908755525994,
12.));
#116240=CARTESIAN_POINT('Ctrl Pts',(73.9090280474723,-2.35730163516324,
0.));
#116241=CARTESIAN_POINT('Ctrl Pts',(73.9090280474723,-2.35730163516324,
12.));
#116242=CARTESIAN_POINT('Ctrl Pts',(73.8845093109302,-2.3455535680214,0.));
#116243=CARTESIAN_POINT('Ctrl Pts',(73.8845093109302,-2.3455535680214,12.));
#116244=CARTESIAN_POINT('Ctrl Pts',(73.8600122421502,-2.33384334963981,
0.));
#116245=CARTESIAN_POINT('Ctrl Pts',(73.8600122421502,-2.33384334963981,
12.));
#116246=CARTESIAN_POINT('Ctrl Pts',(73.8355369402733,-2.32217097594216,
0.));
#116247=CARTESIAN_POINT('Ctrl Pts',(73.8355369402733,-2.32217097594216,
12.));
#116248=CARTESIAN_POINT('Ctrl Pts',(73.8110835039341,-2.31053644289425,
0.));
#116249=CARTESIAN_POINT('Ctrl Pts',(73.8110835039341,-2.31053644289425,
12.));
#116250=CARTESIAN_POINT('Ctrl Pts',(73.7866520318849,-2.29893974640435,
0.));
#116251=CARTESIAN_POINT('Ctrl Pts',(73.7866520318849,-2.29893974640435,
12.));
#116252=CARTESIAN_POINT('Ctrl Pts',(73.7622426235648,-2.28738088222859,
0.));
#116253=CARTESIAN_POINT('Ctrl Pts',(73.7622426235648,-2.28738088222859,
12.));
#116254=CARTESIAN_POINT('Ctrl Pts',(73.7378553796792,-2.27585984587193,
0.));
#116255=CARTESIAN_POINT('Ctrl Pts',(73.7378553796792,-2.27585984587193,
12.));
#116256=CARTESIAN_POINT('Ctrl Pts',(73.7134904019378,-2.26437663263664,
0.));
#116257=CARTESIAN_POINT('Ctrl Pts',(73.7134904019378,-2.26437663263664,
12.));
#116258=CARTESIAN_POINT('Ctrl Pts',(73.6891477928124,-2.25293123766425,
0.));
#116259=CARTESIAN_POINT('Ctrl Pts',(73.6891477928124,-2.25293123766425,
12.));
#116260=CARTESIAN_POINT('Ctrl Pts',(73.6648276552766,-2.24152365597699,
0.));
#116261=CARTESIAN_POINT('Ctrl Pts',(73.6648276552766,-2.24152365597699,
12.));
#116262=CARTESIAN_POINT('Ctrl Pts',(73.6405300925714,-2.23015388251289,
0.));
#116263=CARTESIAN_POINT('Ctrl Pts',(73.6405300925714,-2.23015388251289,
12.));
#116264=CARTESIAN_POINT('Ctrl Pts',(73.6162552079044,-2.21882191216521,
0.));
#116265=CARTESIAN_POINT('Ctrl Pts',(73.6162552079044,-2.21882191216521,
12.));
#116266=CARTESIAN_POINT('Ctrl Pts',(73.5920031044604,-2.20752773978353,
0.));
#116267=CARTESIAN_POINT('Ctrl Pts',(73.5920031044604,-2.20752773978353,
12.));
#116268=CARTESIAN_POINT('Ctrl Pts',(73.5677738855461,-2.19627136015683,
0.));
#116269=CARTESIAN_POINT('Ctrl Pts',(73.5677738855461,-2.19627136015683,
12.));
#116270=CARTESIAN_POINT('Ctrl Pts',(73.5435676546934,-2.18505276799757,
0.));
#116271=CARTESIAN_POINT('Ctrl Pts',(73.5435676546934,-2.18505276799757,
12.));
#116272=CARTESIAN_POINT('Ctrl Pts',(73.5193845157705,-2.17387195792306,
0.));
#116273=CARTESIAN_POINT('Ctrl Pts',(73.5193845157705,-2.17387195792306,
12.));
#116274=CARTESIAN_POINT('Ctrl Pts',(73.4952245731044,-2.16272892442916,
0.));
#116275=CARTESIAN_POINT('Ctrl Pts',(73.4952245731044,-2.16272892442916,
12.));
#116276=CARTESIAN_POINT('Ctrl Pts',(73.4710879315367,-2.15162366187899,
0.));
#116277=CARTESIAN_POINT('Ctrl Pts',(73.4710879315367,-2.15162366187899,
12.));
#116278=CARTESIAN_POINT('Ctrl Pts',(73.4469746963622,-2.14055616452049,
0.));
#116279=CARTESIAN_POINT('Ctrl Pts',(73.4469746963622,-2.14055616452049,
12.));
#116280=CARTESIAN_POINT('Ctrl Pts',(73.4228849732914,-2.12952642649361,
0.));
#116281=CARTESIAN_POINT('Ctrl Pts',(73.4228849732914,-2.12952642649361,
12.));
#116282=CARTESIAN_POINT('Ctrl Pts',(73.3988188684022,-2.11853444183764,
0.));
#116283=CARTESIAN_POINT('Ctrl Pts',(73.3988188684022,-2.11853444183764,
12.));
#116284=CARTESIAN_POINT('Ctrl Pts',(73.3747764880903,-2.10758020449401,
0.));
#116285=CARTESIAN_POINT('Ctrl Pts',(73.3747764880903,-2.10758020449401,
12.));
#116286=CARTESIAN_POINT('Ctrl Pts',(73.3507579390254,-2.09666370830733,
0.));
#116287=CARTESIAN_POINT('Ctrl Pts',(73.3507579390254,-2.09666370830733,
12.));
#116288=CARTESIAN_POINT('Ctrl Pts',(73.3267633281822,-2.08578494702762,
0.));
#116289=CARTESIAN_POINT('Ctrl Pts',(73.3267633281822,-2.08578494702762,
12.));
#116290=CARTESIAN_POINT('Ctrl Pts',(73.3027927628636,-2.07494391430954,
0.));
#116291=CARTESIAN_POINT('Ctrl Pts',(73.3027927628636,-2.07494391430954,
12.));
#116292=CARTESIAN_POINT('Ctrl Pts',(73.2788463507248,-2.06414060370838,
0.));
#116293=CARTESIAN_POINT('Ctrl Pts',(73.2788463507248,-2.06414060370838,
12.));
#116294=CARTESIAN_POINT('Ctrl Pts',(73.2549241997946,-2.05337500867396,
0.));
#116295=CARTESIAN_POINT('Ctrl Pts',(73.2549241997946,-2.05337500867396,
12.));
#116296=CARTESIAN_POINT('Ctrl Pts',(73.2310264184965,-2.04264712253915,
0.));
#116297=CARTESIAN_POINT('Ctrl Pts',(73.2310264184965,-2.04264712253915,
12.));
#116298=CARTESIAN_POINT('Ctrl Pts',(73.2071531156492,-2.03195693852441,
0.));
#116299=CARTESIAN_POINT('Ctrl Pts',(73.2071531156492,-2.03195693852441,
12.));
#116300=CARTESIAN_POINT('Ctrl Pts',(73.1833044004612,-2.02130444974352,
0.));
#116301=CARTESIAN_POINT('Ctrl Pts',(73.1833044004612,-2.02130444974352,
12.));
#116302=CARTESIAN_POINT('Ctrl Pts',(73.159480382525,-2.01068964920465,0.));
#116303=CARTESIAN_POINT('Ctrl Pts',(73.159480382525,-2.01068964920465,12.));
#116304=CARTESIAN_POINT('Ctrl Pts',(73.1356811718094,-2.00011252980988,
0.));
#116305=CARTESIAN_POINT('Ctrl Pts',(73.1356811718094,-2.00011252980988,
12.));
#116306=CARTESIAN_POINT('Ctrl Pts',(73.1119068786482,-1.9895730843493,0.));
#116307=CARTESIAN_POINT('Ctrl Pts',(73.1119068786482,-1.9895730843493,12.));
#116308=CARTESIAN_POINT('Ctrl Pts',(73.0881576137415,-1.97907130550172,
0.));
#116309=CARTESIAN_POINT('Ctrl Pts',(73.0881576137415,-1.97907130550172,
12.));
#116310=CARTESIAN_POINT('Ctrl Pts',(73.0644334881679,-1.96860718583945,
0.));
#116311=CARTESIAN_POINT('Ctrl Pts',(73.0644334881679,-1.96860718583945,
12.));
#116312=CARTESIAN_POINT('Ctrl Pts',(73.0407346133912,-1.95818071782774,
0.));
#116313=CARTESIAN_POINT('Ctrl Pts',(73.0407346133912,-1.95818071782774,
12.));
#116314=CARTESIAN_POINT('Ctrl Pts',(73.0170611012659,-1.94779189382301,
0.));
#116315=CARTESIAN_POINT('Ctrl Pts',(73.0170611012659,-1.94779189382301,
12.));
#116316=CARTESIAN_POINT('Ctrl Pts',(72.9934130640414,-1.93744070606557,
0.));
#116317=CARTESIAN_POINT('Ctrl Pts',(72.9934130640414,-1.93744070606557,
12.));
#116318=CARTESIAN_POINT('Ctrl Pts',(72.9697906143638,-1.92712714667649,
0.));
#116319=CARTESIAN_POINT('Ctrl Pts',(72.9697906143638,-1.92712714667649,
12.));
#116320=CARTESIAN_POINT('Ctrl Pts',(72.9461938652816,-1.91685120766428,
0.));
#116321=CARTESIAN_POINT('Ctrl Pts',(72.9461938652816,-1.91685120766428,
12.));
#116322=CARTESIAN_POINT('Ctrl Pts',(72.9226229302483,-1.90661288092583,
0.));
#116323=CARTESIAN_POINT('Ctrl Pts',(72.9226229302483,-1.90661288092583,
12.));
#116324=CARTESIAN_POINT('Ctrl Pts',(72.8990779231226,-1.89641215824585,
0.));
#116325=CARTESIAN_POINT('Ctrl Pts',(72.8990779231226,-1.89641215824585,
12.));
#116326=CARTESIAN_POINT('Ctrl Pts',(72.8755589581674,-1.88624903129196,
0.));
#116327=CARTESIAN_POINT('Ctrl Pts',(72.8755589581674,-1.88624903129196,
12.));
#116328=CARTESIAN_POINT('Ctrl Pts',(72.8520661500465,-1.87612349160952,
0.));
#116329=CARTESIAN_POINT('Ctrl Pts',(72.8520661500465,-1.87612349160952,
12.));
#116330=CARTESIAN_POINT('Ctrl Pts',(72.8285996138346,-1.86603553062776,
0.));
#116331=CARTESIAN_POINT('Ctrl Pts',(72.8285996138346,-1.86603553062776,
12.));
#116332=CARTESIAN_POINT('Ctrl Pts',(72.8051594650214,-1.85598513966116,
0.));
#116333=CARTESIAN_POINT('Ctrl Pts',(72.8051594650214,-1.85598513966116,
12.));
#116334=CARTESIAN_POINT('Ctrl Pts',(72.7817458195155,-1.84597230990858,
0.));
#116335=CARTESIAN_POINT('Ctrl Pts',(72.7817458195155,-1.84597230990858,
12.));
#116336=CARTESIAN_POINT('Ctrl Pts',(72.7583587936454,-1.83599703244926,
0.));
#116337=CARTESIAN_POINT('Ctrl Pts',(72.7583587936454,-1.83599703244926,
12.));
#116338=CARTESIAN_POINT('Ctrl Pts',(72.73499850416,-1.82605929823566,0.));
#116339=CARTESIAN_POINT('Ctrl Pts',(72.73499850416,-1.82605929823566,12.));
#116340=CARTESIAN_POINT('Ctrl Pts',(72.7116650682347,-1.81615909809872,
0.));
#116341=CARTESIAN_POINT('Ctrl Pts',(72.7116650682347,-1.81615909809872,
12.));
#116342=CARTESIAN_POINT('Ctrl Pts',(72.6883586034768,-1.80629642275052,
0.));
#116343=CARTESIAN_POINT('Ctrl Pts',(72.6883586034768,-1.80629642275052,
12.));
#116344=CARTESIAN_POINT('Ctrl Pts',(72.6650792279271,-1.79647126278359,
0.));
#116345=CARTESIAN_POINT('Ctrl Pts',(72.6650792279271,-1.79647126278359,
12.));
#116346=CARTESIAN_POINT('Ctrl Pts',(72.6418270600623,-1.78668360866814,
0.));
#116347=CARTESIAN_POINT('Ctrl Pts',(72.6418270600623,-1.78668360866814,
12.));
#116348=CARTESIAN_POINT('Ctrl Pts',(72.618602218792,-1.77693345074431,0.));
#116349=CARTESIAN_POINT('Ctrl Pts',(72.618602218792,-1.77693345074431,12.));
#116350=CARTESIAN_POINT('Ctrl Pts',(72.5954048234655,-1.7672207792258,0.));
#116351=CARTESIAN_POINT('Ctrl Pts',(72.5954048234655,-1.7672207792258,12.));
#116352=CARTESIAN_POINT('Ctrl Pts',(72.5722349938789,-1.7575455842035,0.));
#116353=CARTESIAN_POINT('Ctrl Pts',(72.5722349938789,-1.7575455842035,12.));
#116354=CARTESIAN_POINT('Ctrl Pts',(72.5490928502773,-1.74790785564476,
0.));
#116355=CARTESIAN_POINT('Ctrl Pts',(72.5490928502773,-1.74790785564476,
12.));
#116356=CARTESIAN_POINT('Ctrl Pts',(72.5259785133586,-1.73830758339124,
0.));
#116357=CARTESIAN_POINT('Ctrl Pts',(72.5259785133586,-1.73830758339124,
12.));
#116358=CARTESIAN_POINT('Ctrl Pts',(72.5028921042704,-1.72874475715099,
0.));
#116359=CARTESIAN_POINT('Ctrl Pts',(72.5028921042704,-1.72874475715099,
12.));
#116360=CARTESIAN_POINT('Ctrl Pts',(72.4798337446162,-1.71921936650032,
0.));
#116361=CARTESIAN_POINT('Ctrl Pts',(72.4798337446162,-1.71921936650032,
12.));
#116362=CARTESIAN_POINT('Ctrl Pts',(72.4568035564618,-1.70973140088838,
0.));
#116363=CARTESIAN_POINT('Ctrl Pts',(72.4568035564618,-1.70973140088838,
12.));
#116364=CARTESIAN_POINT('Ctrl Pts',(72.4338016623388,-1.70028084963647,
0.));
#116365=CARTESIAN_POINT('Ctrl Pts',(72.4338016623388,-1.70028084963647,
12.));
#116366=CARTESIAN_POINT('Ctrl Pts',(72.4108281852473,-1.69086770193641,
0.));
#116367=CARTESIAN_POINT('Ctrl Pts',(72.4108281852473,-1.69086770193641,
12.));
#116368=CARTESIAN_POINT('Ctrl Pts',(72.3878832486549,-1.68149194684289,
0.));
#116369=CARTESIAN_POINT('Ctrl Pts',(72.3878832486549,-1.68149194684289,
12.));
#116370=CARTESIAN_POINT('Ctrl Pts',(72.3649669765013,-1.67215357327373,
0.));
#116371=CARTESIAN_POINT('Ctrl Pts',(72.3649669765013,-1.67215357327373,
12.));
#116372=CARTESIAN_POINT('Ctrl Pts',(72.3420794932052,-1.66285257001503,
0.));
#116373=CARTESIAN_POINT('Ctrl Pts',(72.3420794932052,-1.66285257001503,
12.));
#116374=CARTESIAN_POINT('Ctrl Pts',(72.3192209236691,-1.65358892572066,
0.));
#116375=CARTESIAN_POINT('Ctrl Pts',(72.3192209236691,-1.65358892572066,
12.));
#116376=CARTESIAN_POINT('Ctrl Pts',(72.2963913932811,-1.64436262891078,
0.));
#116377=CARTESIAN_POINT('Ctrl Pts',(72.2963913932811,-1.64436262891078,
12.));
#116378=CARTESIAN_POINT('Ctrl Pts',(72.2735910279149,-1.63517366796459,
0.));
#116379=CARTESIAN_POINT('Ctrl Pts',(72.2735910279149,-1.63517366796459,
12.));
#116380=CARTESIAN_POINT('Ctrl Pts',(72.2508199539325,-1.62602203111925,
0.));
#116381=CARTESIAN_POINT('Ctrl Pts',(72.2508199539325,-1.62602203111925,
12.));
#116382=CARTESIAN_POINT('Ctrl Pts',(72.2280782981941,-1.61690770647536,
0.));
#116383=CARTESIAN_POINT('Ctrl Pts',(72.2280782981941,-1.61690770647536,
12.));
#116384=CARTESIAN_POINT('Ctrl Pts',(72.2053661880611,-1.60783068199662,
0.));
#116385=CARTESIAN_POINT('Ctrl Pts',(72.2053661880611,-1.60783068199662,
12.));
#116386=CARTESIAN_POINT('Ctrl Pts',(72.1826837514,-1.5987909455085,0.));
#116387=CARTESIAN_POINT('Ctrl Pts',(72.1826837514,-1.5987909455085,12.));
#116388=CARTESIAN_POINT('Ctrl Pts',(72.1600311165813,-1.58978848469129,
0.));
#116389=CARTESIAN_POINT('Ctrl Pts',(72.1600311165813,-1.58978848469129,
12.));
#116390=CARTESIAN_POINT('Ctrl Pts',(72.1374084124829,-1.58082328707808,
0.));
#116391=CARTESIAN_POINT('Ctrl Pts',(72.1374084124829,-1.58082328707808,
12.));
#116392=CARTESIAN_POINT('Ctrl Pts',(72.1148157684987,-1.57189534006044,
0.));
#116393=CARTESIAN_POINT('Ctrl Pts',(72.1148157684987,-1.57189534006044,
12.));
#116394=CARTESIAN_POINT('Ctrl Pts',(72.092253314543,-1.56300463088811,0.));
#116395=CARTESIAN_POINT('Ctrl Pts',(72.092253314543,-1.56300463088811,12.));
#116396=CARTESIAN_POINT('Ctrl Pts',(72.0697211810548,-1.55415114666774,
0.));
#116397=CARTESIAN_POINT('Ctrl Pts',(72.0697211810548,-1.55415114666774,
12.));
#116398=CARTESIAN_POINT('Ctrl Pts',(72.0472194989968,-1.54533487435627,
0.));
#116399=CARTESIAN_POINT('Ctrl Pts',(72.0472194989968,-1.54533487435627,
12.));
#116400=CARTESIAN_POINT('Ctrl Pts',(72.0247483998582,-1.53655580075814,
0.));
#116401=CARTESIAN_POINT('Ctrl Pts',(72.0247483998582,-1.53655580075814,
12.));
#116402=CARTESIAN_POINT('Ctrl Pts',(72.0023080156647,-1.52781391253104,
0.));
#116403=CARTESIAN_POINT('Ctrl Pts',(72.0023080156647,-1.52781391253104,
12.));
#116404=CARTESIAN_POINT('Ctrl Pts',(71.9798984789828,-1.51910919618567,
0.));
#116405=CARTESIAN_POINT('Ctrl Pts',(71.9798984789828,-1.51910919618567,
12.));
#116406=CARTESIAN_POINT('Ctrl Pts',(71.9575199229241,-1.51044163808455,
0.));
#116407=CARTESIAN_POINT('Ctrl Pts',(71.9575199229241,-1.51044163808455,
12.));
#116408=CARTESIAN_POINT('Ctrl Pts',(71.935172481145,-1.50181122443536,0.));
#116409=CARTESIAN_POINT('Ctrl Pts',(71.935172481145,-1.50181122443536,12.));
#116410=CARTESIAN_POINT('Ctrl Pts',(71.9128562878491,-1.49321794128801,
0.));
#116411=CARTESIAN_POINT('Ctrl Pts',(71.9128562878491,-1.49321794128801,
12.));
#116412=CARTESIAN_POINT('Ctrl Pts',(71.8905714777972,-1.48466177454022,
0.));
#116413=CARTESIAN_POINT('Ctrl Pts',(71.8905714777972,-1.48466177454022,
12.));
#116414=CARTESIAN_POINT('Ctrl Pts',(71.8683181863123,-1.47614270993731,
0.));
#116415=CARTESIAN_POINT('Ctrl Pts',(71.8683181863123,-1.47614270993731,
12.));
#116416=CARTESIAN_POINT('Ctrl Pts',(71.8460965492836,-1.4676607330709,0.));
#116417=CARTESIAN_POINT('Ctrl Pts',(71.8460965492836,-1.4676607330709,12.));
#116418=CARTESIAN_POINT('Ctrl Pts',(71.8239067031664,-1.45921582937229,
0.));
#116419=CARTESIAN_POINT('Ctrl Pts',(71.8239067031664,-1.45921582937229,
12.));
#116420=CARTESIAN_POINT('Ctrl Pts',(71.8017487849865,-1.45080798410957,
0.));
#116421=CARTESIAN_POINT('Ctrl Pts',(71.8017487849865,-1.45080798410957,
12.));
#116422=CARTESIAN_POINT('Ctrl Pts',(71.7796229323496,-1.44243718239305,
0.));
#116423=CARTESIAN_POINT('Ctrl Pts',(71.7796229323496,-1.44243718239305,
12.));
#116424=CARTESIAN_POINT('Ctrl Pts',(71.7575292834456,-1.4341034091749,0.));
#116425=CARTESIAN_POINT('Ctrl Pts',(71.7575292834456,-1.4341034091749,12.));
#116426=CARTESIAN_POINT('Ctrl Pts',(71.7354679770537,-1.42580664924775,
0.));
#116427=CARTESIAN_POINT('Ctrl Pts',(71.7354679770537,-1.42580664924775,
12.));
#116428=CARTESIAN_POINT('Ctrl Pts',(71.7134391525417,-1.41754688723792,
0.));
#116429=CARTESIAN_POINT('Ctrl Pts',(71.7134391525417,-1.41754688723792,
12.));
#116430=CARTESIAN_POINT('Ctrl Pts',(71.6914429498702,-1.40932410760275,
0.));
#116431=CARTESIAN_POINT('Ctrl Pts',(71.6914429498702,-1.40932410760275,
12.));
#116432=CARTESIAN_POINT('Ctrl Pts',(71.6694795096034,-1.401138294636,0.));
#116433=CARTESIAN_POINT('Ctrl Pts',(71.6694795096034,-1.401138294636,12.));
#116434=CARTESIAN_POINT('Ctrl Pts',(71.6475489729149,-1.39298943246732,
0.));
#116435=CARTESIAN_POINT('Ctrl Pts',(71.6475489729149,-1.39298943246732,
12.));
#116436=CARTESIAN_POINT('Ctrl Pts',(71.6256514815918,-1.38487750506076,
0.));
#116437=CARTESIAN_POINT('Ctrl Pts',(71.6256514815918,-1.38487750506076,
12.));
#116438=CARTESIAN_POINT('Ctrl Pts',(71.6037871780347,-1.37680249620763,
0.));
#116439=CARTESIAN_POINT('Ctrl Pts',(71.6037871780347,-1.37680249620763,
12.));
#116440=CARTESIAN_POINT('Ctrl Pts',(71.5819562052613,-1.36876438952449,
0.));
#116441=CARTESIAN_POINT('Ctrl Pts',(71.5819562052613,-1.36876438952449,
12.));
#116442=CARTESIAN_POINT('Ctrl Pts',(71.5601587069175,-1.36076316845807,
0.));
#116443=CARTESIAN_POINT('Ctrl Pts',(71.5601587069175,-1.36076316845807,
12.));
#116444=CARTESIAN_POINT('Ctrl Pts',(71.538394827283,-1.35279881628454,0.));
#116445=CARTESIAN_POINT('Ctrl Pts',(71.538394827283,-1.35279881628454,12.));
#116446=CARTESIAN_POINT('Ctrl Pts',(71.5166647112766,-1.34487131610786,
0.));
#116447=CARTESIAN_POINT('Ctrl Pts',(71.5166647112766,-1.34487131610786,
12.));
#116448=CARTESIAN_POINT('Ctrl Pts',(71.4949685044559,-1.33698065085228,
0.));
#116449=CARTESIAN_POINT('Ctrl Pts',(71.4949685044559,-1.33698065085228,
12.));
#116450=CARTESIAN_POINT('Ctrl Pts',(71.4733063530227,-1.32912680326132,
0.));
#116451=CARTESIAN_POINT('Ctrl Pts',(71.4733063530227,-1.32912680326132,
12.));
#116452=CARTESIAN_POINT('Ctrl Pts',(71.4516784038346,-1.32130975590232,
0.));
#116453=CARTESIAN_POINT('Ctrl Pts',(71.4516784038346,-1.32130975590232,
12.));
#116454=CARTESIAN_POINT('Ctrl Pts',(71.4300848044095,-1.31352949116539,
0.));
#116455=CARTESIAN_POINT('Ctrl Pts',(71.4300848044095,-1.31352949116539,
12.));
#116456=CARTESIAN_POINT('Ctrl Pts',(71.4085257029308,-1.3057859912614,0.));
#116457=CARTESIAN_POINT('Ctrl Pts',(71.4085257029308,-1.3057859912614,12.));
#116458=CARTESIAN_POINT('Ctrl Pts',(71.3870012482474,-1.29807923821414,
0.));
#116459=CARTESIAN_POINT('Ctrl Pts',(71.3870012482474,-1.29807923821414,
12.));
#116460=CARTESIAN_POINT('Ctrl Pts',(71.3655115898801,-1.29040921386061,
0.));
#116461=CARTESIAN_POINT('Ctrl Pts',(71.3655115898801,-1.29040921386061,
12.));
#116462=CARTESIAN_POINT('Ctrl Pts',(71.344056878033,-1.28277589985475,0.));
#116463=CARTESIAN_POINT('Ctrl Pts',(71.344056878033,-1.28277589985475,12.));
#116464=CARTESIAN_POINT('Ctrl Pts',(71.3226372635993,-1.27517927766611,
0.));
#116465=CARTESIAN_POINT('Ctrl Pts',(71.3226372635993,-1.27517927766611,
12.));
#116466=CARTESIAN_POINT('Ctrl Pts',(71.301252898167,-1.26761932857724,0.));
#116467=CARTESIAN_POINT('Ctrl Pts',(71.301252898167,-1.26761932857724,12.));
#116468=CARTESIAN_POINT('Ctrl Pts',(71.2799039340191,-1.26009603367565,
0.));
#116469=CARTESIAN_POINT('Ctrl Pts',(71.2799039340191,-1.26009603367565,
12.));
#116470=CARTESIAN_POINT('Ctrl Pts',(71.2585905241422,-1.25260937385561,
0.));
#116471=CARTESIAN_POINT('Ctrl Pts',(71.2585905241422,-1.25260937385561,
12.));
#116472=CARTESIAN_POINT('Ctrl Pts',(71.2373128222359,-1.24515932982108,
0.));
#116473=CARTESIAN_POINT('Ctrl Pts',(71.2373128222359,-1.24515932982108,
12.));
#116474=CARTESIAN_POINT('Ctrl Pts',(71.2160709827189,-1.23774588208427,
0.));
#116475=CARTESIAN_POINT('Ctrl Pts',(71.2160709827189,-1.23774588208427,
12.));
#116476=CARTESIAN_POINT('Ctrl Pts',(71.1948651607319,-1.23036901096246,
0.));
#116477=CARTESIAN_POINT('Ctrl Pts',(71.1948651607319,-1.23036901096246,
12.));
#116478=CARTESIAN_POINT('Ctrl Pts',(71.1736955121361,-1.22302869657029,
0.));
#116479=CARTESIAN_POINT('Ctrl Pts',(71.1736955121361,-1.22302869657029,
12.));
#116480=CARTESIAN_POINT('Ctrl Pts',(71.1525621935266,-1.21572491882274,
0.));
#116481=CARTESIAN_POINT('Ctrl Pts',(71.1525621935266,-1.21572491882274,
12.));
#116482=CARTESIAN_POINT('Ctrl Pts',(71.1314653622442,-1.20845765743655,
0.));
#116483=CARTESIAN_POINT('Ctrl Pts',(71.1314653622442,-1.20845765743655,
12.));
#116484=CARTESIAN_POINT('Ctrl Pts',(71.1104051763839,-1.20122689192837,
0.));
#116485=CARTESIAN_POINT('Ctrl Pts',(71.1104051763839,-1.20122689192837,
12.));
#116486=CARTESIAN_POINT('Ctrl Pts',(71.089381794801,-1.19403260160998,0.));
#116487=CARTESIAN_POINT('Ctrl Pts',(71.089381794801,-1.19403260160998,12.));
#116488=CARTESIAN_POINT('Ctrl Pts',(71.0683953771147,-1.18687476558127,
0.));
#116489=CARTESIAN_POINT('Ctrl Pts',(71.0683953771147,-1.18687476558127,
12.));
#116490=CARTESIAN_POINT('Ctrl Pts',(71.0474460837157,-1.179753362735,0.));
#116491=CARTESIAN_POINT('Ctrl Pts',(71.0474460837157,-1.179753362735,12.));
#116492=CARTESIAN_POINT('Ctrl Pts',(71.0265340757697,-1.17266837175776,
0.));
#116493=CARTESIAN_POINT('Ctrl Pts',(71.0265340757697,-1.17266837175776,
12.));
#116494=CARTESIAN_POINT('Ctrl Pts',(71.0056595152204,-1.16561977112883,
0.));
#116495=CARTESIAN_POINT('Ctrl Pts',(71.0056595152204,-1.16561977112883,
12.));
#116496=CARTESIAN_POINT('Ctrl Pts',(70.9848225647876,-1.1586075391149,0.));
#116497=CARTESIAN_POINT('Ctrl Pts',(70.9848225647876,-1.1586075391149,12.));
#116498=CARTESIAN_POINT('Ctrl Pts',(70.9640233879671,-1.15163165376531,
0.));
#116499=CARTESIAN_POINT('Ctrl Pts',(70.9640233879671,-1.15163165376531,
12.));
#116500=CARTESIAN_POINT('Ctrl Pts',(70.943262149058,-1.14469209291494,0.));
#116501=CARTESIAN_POINT('Ctrl Pts',(70.943262149058,-1.14469209291494,12.));
#116502=CARTESIAN_POINT('Ctrl Pts',(70.9225390131835,-1.13778883418217,
0.));
#116503=CARTESIAN_POINT('Ctrl Pts',(70.9225390131835,-1.13778883418217,
12.));
#116504=CARTESIAN_POINT('Ctrl Pts',(70.9018541463083,-1.13092185496564,
0.));
#116505=CARTESIAN_POINT('Ctrl Pts',(70.9018541463083,-1.13092185496564,
12.));
#116506=CARTESIAN_POINT('Ctrl Pts',(70.8812077152564,-1.12409113243511,
0.));
#116507=CARTESIAN_POINT('Ctrl Pts',(70.8812077152564,-1.12409113243511,
12.));
#116508=CARTESIAN_POINT('Ctrl Pts',(70.860599887712,-1.11729664352991,0.));
#116509=CARTESIAN_POINT('Ctrl Pts',(70.860599887712,-1.11729664352991,12.));
#116510=CARTESIAN_POINT('Ctrl Pts',(70.8400308322013,-1.11053836496638,
0.));
#116511=CARTESIAN_POINT('Ctrl Pts',(70.8400308322013,-1.11053836496638,
12.));
#116512=CARTESIAN_POINT('Ctrl Pts',(70.8195007180739,-1.10381627323946,
0.));
#116513=CARTESIAN_POINT('Ctrl Pts',(70.8195007180739,-1.10381627323946,
12.));
#116514=CARTESIAN_POINT('Ctrl Pts',(70.7990097154855,-1.0971303446227,0.));
#116515=CARTESIAN_POINT('Ctrl Pts',(70.7990097154855,-1.0971303446227,12.));
#116516=CARTESIAN_POINT('Ctrl Pts',(70.7785579953611,-1.09048055516434,
0.));
#116517=CARTESIAN_POINT('Ctrl Pts',(70.7785579953611,-1.09048055516434,
12.));
#116518=CARTESIAN_POINT('Ctrl Pts',(70.7581457294475,-1.08386688068349,
0.));
#116519=CARTESIAN_POINT('Ctrl Pts',(70.7581457294475,-1.08386688068349,
12.));
#116520=CARTESIAN_POINT('Ctrl Pts',(70.737773090397,-1.07728929676412,0.));
#116521=CARTESIAN_POINT('Ctrl Pts',(70.737773090397,-1.07728929676412,12.));
#116522=CARTESIAN_POINT('Ctrl Pts',(70.7174402518378,-1.07074777874597,
0.));
#116523=CARTESIAN_POINT('Ctrl Pts',(70.7174402518378,-1.07074777874597,
12.));
#116524=CARTESIAN_POINT('Ctrl Pts',(70.6971473884443,-1.0642423017128,0.));
#116525=CARTESIAN_POINT('Ctrl Pts',(70.6971473884443,-1.0642423017128,12.));
#116526=CARTESIAN_POINT('Ctrl Pts',(70.6768946760063,-1.05777284047728,
0.));
#116527=CARTESIAN_POINT('Ctrl Pts',(70.6768946760063,-1.05777284047728,
12.));
#116528=CARTESIAN_POINT('Ctrl Pts',(70.6566822912965,-1.05133936960069,
0.));
#116529=CARTESIAN_POINT('Ctrl Pts',(70.6566822912965,-1.05133936960069,
12.));
#116530=CARTESIAN_POINT('Ctrl Pts',(70.6365104119238,-1.04494186341156,
0.));
#116531=CARTESIAN_POINT('Ctrl Pts',(70.6365104119238,-1.04494186341156,
12.));
#116532=CARTESIAN_POINT('Ctrl Pts',(70.6163792162079,-1.03858029601906,
0.));
#116533=CARTESIAN_POINT('Ctrl Pts',(70.6163792162079,-1.03858029601906,
12.));
#116534=CARTESIAN_POINT('Ctrl Pts',(70.5962888829958,-1.03225464132873,
0.));
#116535=CARTESIAN_POINT('Ctrl Pts',(70.5962888829958,-1.03225464132873,
12.));
#116536=CARTESIAN_POINT('Ctrl Pts',(70.5762395916412,-1.02596487304049,
0.));
#116537=CARTESIAN_POINT('Ctrl Pts',(70.5762395916412,-1.02596487304049,
12.));
#116538=CARTESIAN_POINT('Ctrl Pts',(70.5562315224219,-1.01971096460599,
0.));
#116539=CARTESIAN_POINT('Ctrl Pts',(70.5562315224219,-1.01971096460599,
12.));
#116540=CARTESIAN_POINT('Ctrl Pts',(70.5362648569072,-1.0134928891854,0.));
#116541=CARTESIAN_POINT('Ctrl Pts',(70.5362648569072,-1.0134928891854,12.));
#116542=CARTESIAN_POINT('Ctrl Pts',(70.5163397782699,-1.00731061960968,
0.));
#116543=CARTESIAN_POINT('Ctrl Pts',(70.5163397782699,-1.00731061960968,
12.));
#116544=CARTESIAN_POINT('Ctrl Pts',(70.4964564717917,-1.00116412831438,
0.));
#116545=CARTESIAN_POINT('Ctrl Pts',(70.4964564717917,-1.00116412831438,
12.));
#116546=CARTESIAN_POINT('Ctrl Pts',(70.476615124517,-0.995053387379685,
0.));
#116547=CARTESIAN_POINT('Ctrl Pts',(70.476615124517,-0.995053387379685,
12.));
#116548=CARTESIAN_POINT('Ctrl Pts',(70.4568159243131,-0.988978368643593,
0.));
#116549=CARTESIAN_POINT('Ctrl Pts',(70.4568159243131,-0.988978368643593,
12.));
#116550=CARTESIAN_POINT('Ctrl Pts',(70.4370590590839,-0.982939043792163,
0.));
#116551=CARTESIAN_POINT('Ctrl Pts',(70.4370590590839,-0.982939043792163,
12.));
#116552=CARTESIAN_POINT('Ctrl Pts',(70.41734471596,-0.976935384450131,0.));
#116553=CARTESIAN_POINT('Ctrl Pts',(70.41734471596,-0.976935384450131,12.));
#116554=CARTESIAN_POINT('Ctrl Pts',(70.3976730803664,-0.970967362281305,
0.));
#116555=CARTESIAN_POINT('Ctrl Pts',(70.3976730803664,-0.970967362281305,
12.));
#116556=CARTESIAN_POINT('Ctrl Pts',(70.3780443378003,-0.965034948786564,
0.));
#116557=CARTESIAN_POINT('Ctrl Pts',(70.3780443378003,-0.965034948786564,
12.));
#116558=CARTESIAN_POINT('Ctrl Pts',(70.3584586759561,-0.959138115058888,
0.));
#116559=CARTESIAN_POINT('Ctrl Pts',(70.3584586759561,-0.959138115058888,
12.));
#116560=CARTESIAN_POINT('Ctrl Pts',(70.338916286457,-0.953276831581237,
0.));
#116561=CARTESIAN_POINT('Ctrl Pts',(70.338916286457,-0.953276831581237,
12.));
#116562=CARTESIAN_POINT('Ctrl Pts',(70.3194173673635,-0.947451067929568,
0.));
#116563=CARTESIAN_POINT('Ctrl Pts',(70.3194173673635,-0.947451067929568,
12.));
#116564=CARTESIAN_POINT('Ctrl Pts',(70.2999621233938,-0.941660792742957,
0.));
#116565=CARTESIAN_POINT('Ctrl Pts',(70.2999621233938,-0.941660792742957,
12.));
#116566=CARTESIAN_POINT('Ctrl Pts',(70.2805507606832,-0.935905974336494,
0.));
#116567=CARTESIAN_POINT('Ctrl Pts',(70.2805507606832,-0.935905974336494,
12.));
#116568=CARTESIAN_POINT('Ctrl Pts',(70.2611834821711,-0.93018658123558,
0.));
#116569=CARTESIAN_POINT('Ctrl Pts',(70.2611834821711,-0.93018658123558,
12.));
#116570=CARTESIAN_POINT('Ctrl Pts',(70.241860483586,-0.924502582639455,
0.));
#116571=CARTESIAN_POINT('Ctrl Pts',(70.241860483586,-0.924502582639455,
12.));
#116572=CARTESIAN_POINT('Ctrl Pts',(70.2225819470306,-0.918853949157049,
0.));
#116573=CARTESIAN_POINT('Ctrl Pts',(70.2225819470306,-0.918853949157049,
12.));
#116574=CARTESIAN_POINT('Ctrl Pts',(70.2033480471749,-0.913240652090843,
0.));
#116575=CARTESIAN_POINT('Ctrl Pts',(70.2033480471749,-0.913240652090843,
12.));
#116576=CARTESIAN_POINT('Ctrl Pts',(70.184158963563,-0.907662662015655,
0.));
#116577=CARTESIAN_POINT('Ctrl Pts',(70.184158963563,-0.907662662015655,
12.));
#116578=CARTESIAN_POINT('Ctrl Pts',(70.1650148905109,-0.902119947629777,
0.));
#116579=CARTESIAN_POINT('Ctrl Pts',(70.1650148905109,-0.902119947629777,
12.));
#116580=CARTESIAN_POINT('Ctrl Pts',(70.1459160490366,-0.896612474372089,
0.));
#116581=CARTESIAN_POINT('Ctrl Pts',(70.1459160490366,-0.896612474372089,
12.));
#116582=CARTESIAN_POINT('Ctrl Pts',(70.1268626950031,-0.891140203464729,
0.));
#116583=CARTESIAN_POINT('Ctrl Pts',(70.1268626950031,-0.891140203464729,
12.));
#116584=CARTESIAN_POINT('Ctrl Pts',(70.1078550938801,-0.885703094803091,
0.));
#116585=CARTESIAN_POINT('Ctrl Pts',(70.1078550938801,-0.885703094803091,
12.));
#116586=CARTESIAN_POINT('Ctrl Pts',(70.0888934967772,-0.880301109661041,
0.));
#116587=CARTESIAN_POINT('Ctrl Pts',(70.0888934967772,-0.880301109661041,
12.));
#116588=CARTESIAN_POINT('Ctrl Pts',(70.0699781184013,-0.874934213255575,
0.));
#116589=CARTESIAN_POINT('Ctrl Pts',(70.0699781184013,-0.874934213255575,
12.));
#116590=CARTESIAN_POINT('Ctrl Pts',(70.0511091083285,-0.869602377870143,
0.));
#116591=CARTESIAN_POINT('Ctrl Pts',(70.0511091083285,-0.869602377870143,
12.));
#116592=CARTESIAN_POINT('Ctrl Pts',(70.0322865493339,-0.864305583660094,
0.));
#116593=CARTESIAN_POINT('Ctrl Pts',(70.0322865493339,-0.864305583660094,
12.));
#116594=CARTESIAN_POINT('Ctrl Pts',(70.0172656934192,-0.860096170667403,
0.));
#116595=CARTESIAN_POINT('Ctrl Pts',(70.0172656934192,-0.860096170667403,
12.));
#116596=CARTESIAN_POINT('Ctrl Pts',(70.0060209754332,-0.856954870258375,
0.));
#116597=CARTESIAN_POINT('Ctrl Pts',(70.0060209754332,-0.856954870258375,
12.));
#116598=CARTESIAN_POINT('Ctrl Pts',(69.9985337959499,-0.854867673848295,
0.));
#116599=CARTESIAN_POINT('Ctrl Pts',(69.9985337959499,-0.854867673848295,
12.));
#116600=CARTESIAN_POINT('Ctrl Pts',(69.9947925310006,-0.853825826608997,
0.));
#116601=CARTESIAN_POINT('Ctrl Pts',(69.9947925310006,-0.853825826608997,
12.));
#116602=CARTESIAN_POINT('',(69.9947925310006,-0.853825826608997,12.));
#116603=CARTESIAN_POINT('Ctrl Pts',(69.9947925310006,-0.853825826608997,
12.));
#116604=CARTESIAN_POINT('Ctrl Pts',(69.9985337959499,-0.854867673848295,
12.));
#116605=CARTESIAN_POINT('Ctrl Pts',(70.0060209754332,-0.856954870258375,
12.));
#116606=CARTESIAN_POINT('Ctrl Pts',(70.0172656934192,-0.860096170667403,
12.));
#116607=CARTESIAN_POINT('Ctrl Pts',(70.0322865493339,-0.864305583660094,
12.));
#116608=CARTESIAN_POINT('Ctrl Pts',(70.0511091083285,-0.869602377870143,
12.));
#116609=CARTESIAN_POINT('Ctrl Pts',(70.0699781184013,-0.874934213255575,
12.));
#116610=CARTESIAN_POINT('Ctrl Pts',(70.0888934967772,-0.880301109661041,
12.));
#116611=CARTESIAN_POINT('Ctrl Pts',(70.1078550938801,-0.885703094803091,
12.));
#116612=CARTESIAN_POINT('Ctrl Pts',(70.1268626950031,-0.891140203464729,
12.));
#116613=CARTESIAN_POINT('Ctrl Pts',(70.1459160490366,-0.896612474372089,
12.));
#116614=CARTESIAN_POINT('Ctrl Pts',(70.1650148905109,-0.902119947629777,
12.));
#116615=CARTESIAN_POINT('Ctrl Pts',(70.184158963563,-0.907662662015655,
12.));
#116616=CARTESIAN_POINT('Ctrl Pts',(70.2033480471749,-0.913240652090843,
12.));
#116617=CARTESIAN_POINT('Ctrl Pts',(70.2225819470306,-0.918853949157049,
12.));
#116618=CARTESIAN_POINT('Ctrl Pts',(70.241860483586,-0.924502582639455,
12.));
#116619=CARTESIAN_POINT('Ctrl Pts',(70.2611834821711,-0.93018658123558,
12.));
#116620=CARTESIAN_POINT('Ctrl Pts',(70.2805507606832,-0.935905974336494,
12.));
#116621=CARTESIAN_POINT('Ctrl Pts',(70.2999621233938,-0.941660792742957,
12.));
#116622=CARTESIAN_POINT('Ctrl Pts',(70.3194173673635,-0.947451067929568,
12.));
#116623=CARTESIAN_POINT('Ctrl Pts',(70.338916286457,-0.953276831581237,
12.));
#116624=CARTESIAN_POINT('Ctrl Pts',(70.3584586759561,-0.959138115058888,
12.));
#116625=CARTESIAN_POINT('Ctrl Pts',(70.3780443378003,-0.965034948786564,
12.));
#116626=CARTESIAN_POINT('Ctrl Pts',(70.3976730803664,-0.970967362281305,
12.));
#116627=CARTESIAN_POINT('Ctrl Pts',(70.41734471596,-0.976935384450131,12.));
#116628=CARTESIAN_POINT('Ctrl Pts',(70.4370590590839,-0.982939043792163,
12.));
#116629=CARTESIAN_POINT('Ctrl Pts',(70.4568159243131,-0.988978368643593,
12.));
#116630=CARTESIAN_POINT('Ctrl Pts',(70.476615124517,-0.995053387379685,
12.));
#116631=CARTESIAN_POINT('Ctrl Pts',(70.4964564717917,-1.00116412831438,
12.));
#116632=CARTESIAN_POINT('Ctrl Pts',(70.5163397782699,-1.00731061960968,
12.));
#116633=CARTESIAN_POINT('Ctrl Pts',(70.5362648569072,-1.0134928891854,12.));
#116634=CARTESIAN_POINT('Ctrl Pts',(70.5562315224219,-1.01971096460599,
12.));
#116635=CARTESIAN_POINT('Ctrl Pts',(70.5762395916412,-1.02596487304049,
12.));
#116636=CARTESIAN_POINT('Ctrl Pts',(70.5962888829958,-1.03225464132873,
12.));
#116637=CARTESIAN_POINT('Ctrl Pts',(70.6163792162079,-1.03858029601906,
12.));
#116638=CARTESIAN_POINT('Ctrl Pts',(70.6365104119238,-1.04494186341156,
12.));
#116639=CARTESIAN_POINT('Ctrl Pts',(70.6566822912965,-1.05133936960069,
12.));
#116640=CARTESIAN_POINT('Ctrl Pts',(70.6768946760063,-1.05777284047728,
12.));
#116641=CARTESIAN_POINT('Ctrl Pts',(70.6971473884443,-1.0642423017128,12.));
#116642=CARTESIAN_POINT('Ctrl Pts',(70.7174402518378,-1.07074777874597,
12.));
#116643=CARTESIAN_POINT('Ctrl Pts',(70.737773090397,-1.07728929676412,12.));
#116644=CARTESIAN_POINT('Ctrl Pts',(70.7581457294475,-1.08386688068349,
12.));
#116645=CARTESIAN_POINT('Ctrl Pts',(70.7785579953611,-1.09048055516434,
12.));
#116646=CARTESIAN_POINT('Ctrl Pts',(70.7990097154855,-1.0971303446227,12.));
#116647=CARTESIAN_POINT('Ctrl Pts',(70.8195007180739,-1.10381627323946,
12.));
#116648=CARTESIAN_POINT('Ctrl Pts',(70.8400308322013,-1.11053836496638,
12.));
#116649=CARTESIAN_POINT('Ctrl Pts',(70.860599887712,-1.11729664352991,12.));
#116650=CARTESIAN_POINT('Ctrl Pts',(70.8812077152564,-1.12409113243511,
12.));
#116651=CARTESIAN_POINT('Ctrl Pts',(70.9018541463083,-1.13092185496564,
12.));
#116652=CARTESIAN_POINT('Ctrl Pts',(70.9225390131835,-1.13778883418217,
12.));
#116653=CARTESIAN_POINT('Ctrl Pts',(70.943262149058,-1.14469209291494,12.));
#116654=CARTESIAN_POINT('Ctrl Pts',(70.9640233879671,-1.15163165376531,
12.));
#116655=CARTESIAN_POINT('Ctrl Pts',(70.9848225647876,-1.1586075391149,12.));
#116656=CARTESIAN_POINT('Ctrl Pts',(71.0056595152204,-1.16561977112883,
12.));
#116657=CARTESIAN_POINT('Ctrl Pts',(71.0265340757697,-1.17266837175776,
12.));
#116658=CARTESIAN_POINT('Ctrl Pts',(71.0474460837157,-1.179753362735,12.));
#116659=CARTESIAN_POINT('Ctrl Pts',(71.0683953771147,-1.18687476558127,
12.));
#116660=CARTESIAN_POINT('Ctrl Pts',(71.089381794801,-1.19403260160998,12.));
#116661=CARTESIAN_POINT('Ctrl Pts',(71.1104051763839,-1.20122689192837,
12.));
#116662=CARTESIAN_POINT('Ctrl Pts',(71.1314653622442,-1.20845765743655,
12.));
#116663=CARTESIAN_POINT('Ctrl Pts',(71.1525621935266,-1.21572491882274,
12.));
#116664=CARTESIAN_POINT('Ctrl Pts',(71.1736955121361,-1.22302869657029,
12.));
#116665=CARTESIAN_POINT('Ctrl Pts',(71.1948651607319,-1.23036901096246,
12.));
#116666=CARTESIAN_POINT('Ctrl Pts',(71.2160709827189,-1.23774588208427,
12.));
#116667=CARTESIAN_POINT('Ctrl Pts',(71.2373128222359,-1.24515932982108,
12.));
#116668=CARTESIAN_POINT('Ctrl Pts',(71.2585905241422,-1.25260937385561,
12.));
#116669=CARTESIAN_POINT('Ctrl Pts',(71.2799039340191,-1.26009603367565,
12.));
#116670=CARTESIAN_POINT('Ctrl Pts',(71.301252898167,-1.26761932857724,12.));
#116671=CARTESIAN_POINT('Ctrl Pts',(71.3226372635993,-1.27517927766611,
12.));
#116672=CARTESIAN_POINT('Ctrl Pts',(71.344056878033,-1.28277589985475,12.));
#116673=CARTESIAN_POINT('Ctrl Pts',(71.3655115898801,-1.29040921386061,
12.));
#116674=CARTESIAN_POINT('Ctrl Pts',(71.3870012482474,-1.29807923821414,
12.));
#116675=CARTESIAN_POINT('Ctrl Pts',(71.4085257029308,-1.3057859912614,12.));
#116676=CARTESIAN_POINT('Ctrl Pts',(71.4300848044095,-1.31352949116539,
12.));
#116677=CARTESIAN_POINT('Ctrl Pts',(71.4516784038346,-1.32130975590232,
12.));
#116678=CARTESIAN_POINT('Ctrl Pts',(71.4733063530227,-1.32912680326132,
12.));
#116679=CARTESIAN_POINT('Ctrl Pts',(71.4949685044559,-1.33698065085228,
12.));
#116680=CARTESIAN_POINT('Ctrl Pts',(71.5166647112766,-1.34487131610786,
12.));
#116681=CARTESIAN_POINT('Ctrl Pts',(71.538394827283,-1.35279881628454,12.));
#116682=CARTESIAN_POINT('Ctrl Pts',(71.5601587069175,-1.36076316845807,
12.));
#116683=CARTESIAN_POINT('Ctrl Pts',(71.5819562052613,-1.36876438952449,
12.));
#116684=CARTESIAN_POINT('Ctrl Pts',(71.6037871780347,-1.37680249620763,
12.));
#116685=CARTESIAN_POINT('Ctrl Pts',(71.6256514815918,-1.38487750506076,
12.));
#116686=CARTESIAN_POINT('Ctrl Pts',(71.6475489729149,-1.39298943246732,
12.));
#116687=CARTESIAN_POINT('Ctrl Pts',(71.6694795096034,-1.401138294636,12.));
#116688=CARTESIAN_POINT('Ctrl Pts',(71.6914429498702,-1.40932410760275,
12.));
#116689=CARTESIAN_POINT('Ctrl Pts',(71.7134391525417,-1.41754688723792,
12.));
#116690=CARTESIAN_POINT('Ctrl Pts',(71.7354679770537,-1.42580664924775,
12.));
#116691=CARTESIAN_POINT('Ctrl Pts',(71.7575292834456,-1.4341034091749,12.));
#116692=CARTESIAN_POINT('Ctrl Pts',(71.7796229323496,-1.44243718239305,
12.));
#116693=CARTESIAN_POINT('Ctrl Pts',(71.8017487849865,-1.45080798410957,
12.));
#116694=CARTESIAN_POINT('Ctrl Pts',(71.8239067031664,-1.45921582937229,
12.));
#116695=CARTESIAN_POINT('Ctrl Pts',(71.8460965492836,-1.4676607330709,12.));
#116696=CARTESIAN_POINT('Ctrl Pts',(71.8683181863123,-1.47614270993731,
12.));
#116697=CARTESIAN_POINT('Ctrl Pts',(71.8905714777972,-1.48466177454022,
12.));
#116698=CARTESIAN_POINT('Ctrl Pts',(71.9128562878491,-1.49321794128801,
12.));
#116699=CARTESIAN_POINT('Ctrl Pts',(71.935172481145,-1.50181122443536,12.));
#116700=CARTESIAN_POINT('Ctrl Pts',(71.9575199229241,-1.51044163808455,
12.));
#116701=CARTESIAN_POINT('Ctrl Pts',(71.9798984789828,-1.51910919618567,
12.));
#116702=CARTESIAN_POINT('Ctrl Pts',(72.0023080156647,-1.52781391253104,
12.));
#116703=CARTESIAN_POINT('Ctrl Pts',(72.0247483998582,-1.53655580075814,
12.));
#116704=CARTESIAN_POINT('Ctrl Pts',(72.0472194989968,-1.54533487435627,
12.));
#116705=CARTESIAN_POINT('Ctrl Pts',(72.0697211810548,-1.55415114666774,
12.));
#116706=CARTESIAN_POINT('Ctrl Pts',(72.092253314543,-1.56300463088811,12.));
#116707=CARTESIAN_POINT('Ctrl Pts',(72.1148157684987,-1.57189534006044,
12.));
#116708=CARTESIAN_POINT('Ctrl Pts',(72.1374084124829,-1.58082328707808,
12.));
#116709=CARTESIAN_POINT('Ctrl Pts',(72.1600311165813,-1.58978848469129,
12.));
#116710=CARTESIAN_POINT('Ctrl Pts',(72.1826837514,-1.5987909455085,12.));
#116711=CARTESIAN_POINT('Ctrl Pts',(72.2053661880611,-1.60783068199662,
12.));
#116712=CARTESIAN_POINT('Ctrl Pts',(72.2280782981941,-1.61690770647536,
12.));
#116713=CARTESIAN_POINT('Ctrl Pts',(72.2508199539325,-1.62602203111925,
12.));
#116714=CARTESIAN_POINT('Ctrl Pts',(72.2735910279149,-1.63517366796459,
12.));
#116715=CARTESIAN_POINT('Ctrl Pts',(72.2963913932811,-1.64436262891078,
12.));
#116716=CARTESIAN_POINT('Ctrl Pts',(72.3192209236691,-1.65358892572066,
12.));
#116717=CARTESIAN_POINT('Ctrl Pts',(72.3420794932052,-1.66285257001503,
12.));
#116718=CARTESIAN_POINT('Ctrl Pts',(72.3649669765013,-1.67215357327373,
12.));
#116719=CARTESIAN_POINT('Ctrl Pts',(72.3878832486549,-1.68149194684289,
12.));
#116720=CARTESIAN_POINT('Ctrl Pts',(72.4108281852473,-1.69086770193641,
12.));
#116721=CARTESIAN_POINT('Ctrl Pts',(72.4338016623388,-1.70028084963647,
12.));
#116722=CARTESIAN_POINT('Ctrl Pts',(72.4568035564618,-1.70973140088838,
12.));
#116723=CARTESIAN_POINT('Ctrl Pts',(72.4798337446162,-1.71921936650032,
12.));
#116724=CARTESIAN_POINT('Ctrl Pts',(72.5028921042704,-1.72874475715099,
12.));
#116725=CARTESIAN_POINT('Ctrl Pts',(72.5259785133586,-1.73830758339124,
12.));
#116726=CARTESIAN_POINT('Ctrl Pts',(72.5490928502773,-1.74790785564476,
12.));
#116727=CARTESIAN_POINT('Ctrl Pts',(72.5722349938789,-1.7575455842035,12.));
#116728=CARTESIAN_POINT('Ctrl Pts',(72.5954048234655,-1.7672207792258,12.));
#116729=CARTESIAN_POINT('Ctrl Pts',(72.618602218792,-1.77693345074431,12.));
#116730=CARTESIAN_POINT('Ctrl Pts',(72.6418270600623,-1.78668360866814,
12.));
#116731=CARTESIAN_POINT('Ctrl Pts',(72.6650792279271,-1.79647126278359,
12.));
#116732=CARTESIAN_POINT('Ctrl Pts',(72.6883586034768,-1.80629642275052,
12.));
#116733=CARTESIAN_POINT('Ctrl Pts',(72.7116650682347,-1.81615909809872,
12.));
#116734=CARTESIAN_POINT('Ctrl Pts',(72.73499850416,-1.82605929823566,12.));
#116735=CARTESIAN_POINT('Ctrl Pts',(72.7583587936454,-1.83599703244926,
12.));
#116736=CARTESIAN_POINT('Ctrl Pts',(72.7817458195155,-1.84597230990858,
12.));
#116737=CARTESIAN_POINT('Ctrl Pts',(72.8051594650214,-1.85598513966116,
12.));
#116738=CARTESIAN_POINT('Ctrl Pts',(72.8285996138346,-1.86603553062776,
12.));
#116739=CARTESIAN_POINT('Ctrl Pts',(72.8520661500465,-1.87612349160952,
12.));
#116740=CARTESIAN_POINT('Ctrl Pts',(72.8755589581674,-1.88624903129196,
12.));
#116741=CARTESIAN_POINT('Ctrl Pts',(72.8990779231226,-1.89641215824585,
12.));
#116742=CARTESIAN_POINT('Ctrl Pts',(72.9226229302483,-1.90661288092583,
12.));
#116743=CARTESIAN_POINT('Ctrl Pts',(72.9461938652816,-1.91685120766428,
12.));
#116744=CARTESIAN_POINT('Ctrl Pts',(72.9697906143638,-1.92712714667649,
12.));
#116745=CARTESIAN_POINT('Ctrl Pts',(72.9934130640414,-1.93744070606557,
12.));
#116746=CARTESIAN_POINT('Ctrl Pts',(73.0170611012659,-1.94779189382301,
12.));
#116747=CARTESIAN_POINT('Ctrl Pts',(73.0407346133912,-1.95818071782774,
12.));
#116748=CARTESIAN_POINT('Ctrl Pts',(73.0644334881679,-1.96860718583945,
12.));
#116749=CARTESIAN_POINT('Ctrl Pts',(73.0881576137415,-1.97907130550172,
12.));
#116750=CARTESIAN_POINT('Ctrl Pts',(73.1119068786482,-1.9895730843493,12.));
#116751=CARTESIAN_POINT('Ctrl Pts',(73.1356811718094,-2.00011252980988,
12.));
#116752=CARTESIAN_POINT('Ctrl Pts',(73.159480382525,-2.01068964920465,12.));
#116753=CARTESIAN_POINT('Ctrl Pts',(73.1833044004612,-2.02130444974352,
12.));
#116754=CARTESIAN_POINT('Ctrl Pts',(73.2071531156492,-2.03195693852441,
12.));
#116755=CARTESIAN_POINT('Ctrl Pts',(73.2310264184965,-2.04264712253915,
12.));
#116756=CARTESIAN_POINT('Ctrl Pts',(73.2549241997946,-2.05337500867396,
12.));
#116757=CARTESIAN_POINT('Ctrl Pts',(73.2788463507248,-2.06414060370838,
12.));
#116758=CARTESIAN_POINT('Ctrl Pts',(73.3027927628636,-2.07494391430954,
12.));
#116759=CARTESIAN_POINT('Ctrl Pts',(73.3267633281822,-2.08578494702762,
12.));
#116760=CARTESIAN_POINT('Ctrl Pts',(73.3507579390254,-2.09666370830733,
12.));
#116761=CARTESIAN_POINT('Ctrl Pts',(73.3747764880903,-2.10758020449401,
12.));
#116762=CARTESIAN_POINT('Ctrl Pts',(73.3988188684022,-2.11853444183764,
12.));
#116763=CARTESIAN_POINT('Ctrl Pts',(73.4228849732914,-2.12952642649361,
12.));
#116764=CARTESIAN_POINT('Ctrl Pts',(73.4469746963622,-2.14055616452049,
12.));
#116765=CARTESIAN_POINT('Ctrl Pts',(73.4710879315367,-2.15162366187899,
12.));
#116766=CARTESIAN_POINT('Ctrl Pts',(73.4952245731044,-2.16272892442916,
12.));
#116767=CARTESIAN_POINT('Ctrl Pts',(73.5193845157705,-2.17387195792306,
12.));
#116768=CARTESIAN_POINT('Ctrl Pts',(73.5435676546934,-2.18505276799757,
12.));
#116769=CARTESIAN_POINT('Ctrl Pts',(73.5677738855461,-2.19627136015683,
12.));
#116770=CARTESIAN_POINT('Ctrl Pts',(73.5920031044604,-2.20752773978353,
12.));
#116771=CARTESIAN_POINT('Ctrl Pts',(73.6162552079044,-2.21882191216521,
12.));
#116772=CARTESIAN_POINT('Ctrl Pts',(73.6405300925714,-2.23015388251289,
12.));
#116773=CARTESIAN_POINT('Ctrl Pts',(73.6648276552766,-2.24152365597699,
12.));
#116774=CARTESIAN_POINT('Ctrl Pts',(73.6891477928124,-2.25293123766425,
12.));
#116775=CARTESIAN_POINT('Ctrl Pts',(73.7134904019378,-2.26437663263664,
12.));
#116776=CARTESIAN_POINT('Ctrl Pts',(73.7378553796792,-2.27585984587193,
12.));
#116777=CARTESIAN_POINT('Ctrl Pts',(73.7622426235648,-2.28738088222859,
12.));
#116778=CARTESIAN_POINT('Ctrl Pts',(73.7866520318849,-2.29893974640435,
12.));
#116779=CARTESIAN_POINT('Ctrl Pts',(73.8110835039341,-2.31053644289425,
12.));
#116780=CARTESIAN_POINT('Ctrl Pts',(73.8355369402733,-2.32217097594216,
12.));
#116781=CARTESIAN_POINT('Ctrl Pts',(73.8600122421502,-2.33384334963981,
12.));
#116782=CARTESIAN_POINT('Ctrl Pts',(73.8845093109302,-2.3455535680214,12.));
#116783=CARTESIAN_POINT('Ctrl Pts',(73.9090280474723,-2.35730163516324,
12.));
#116784=CARTESIAN_POINT('Ctrl Pts',(73.9335683516388,-2.36908755525994,
12.));
#116785=CARTESIAN_POINT('Ctrl Pts',(73.9581301214609,-2.38091133274933,
12.));
#116786=CARTESIAN_POINT('Ctrl Pts',(73.9827132538149,-2.39277297220716,
12.));
#116787=CARTESIAN_POINT('Ctrl Pts',(74.0073176459287,-2.40467247811497,
12.));
#116788=CARTESIAN_POINT('Ctrl Pts',(74.0319431966956,-2.41660985465228,
12.));
#116789=CARTESIAN_POINT('Ctrl Pts',(74.0565898079227,-2.42858510549787,
12.));
#116790=CARTESIAN_POINT('Ctrl Pts',(74.0812573859474,-2.44059823356722,
12.));
#116791=CARTESIAN_POINT('Ctrl Pts',(74.1059458420175,-2.45264924094853,
12.));
#116792=CARTESIAN_POINT('Ctrl Pts',(74.1271264545378,-2.46301176097528,
12.));
#116793=CARTESIAN_POINT('Ctrl Pts',(74.1433763941622,-2.47097695565718,
12.));
#116794=CARTESIAN_POINT('Ctrl Pts',(74.1546864735453,-2.47652804725573,
12.));
#116795=CARTESIAN_POINT('Ctrl Pts',(74.1610506466543,-2.47965393946825,
12.));
#116796=CARTESIAN_POINT('Ctrl Pts',(74.1624659714955,-2.48034921844901,
12.));
#116797=CARTESIAN_POINT('',(69.9947925310006,-0.853825826608997,0.));
#116798=CARTESIAN_POINT('',(69.9947925310006,-0.853825826608997,0.));
#116799=CARTESIAN_POINT('Ctrl Pts',(74.1624659714955,-2.48034921844903,
0.));
#116800=CARTESIAN_POINT('Ctrl Pts',(74.1610506466543,-2.47965393946827,
0.));
#116801=CARTESIAN_POINT('Ctrl Pts',(74.1546864735453,-2.47652804725574,
0.));
#116802=CARTESIAN_POINT('Ctrl Pts',(74.1433763941622,-2.47097695565719,
0.));
#116803=CARTESIAN_POINT('Ctrl Pts',(74.1271264545378,-2.46301176097528,
0.));
#116804=CARTESIAN_POINT('Ctrl Pts',(74.1059458420175,-2.45264924094853,
0.));
#116805=CARTESIAN_POINT('Ctrl Pts',(74.0812573859474,-2.44059823356722,
0.));
#116806=CARTESIAN_POINT('Ctrl Pts',(74.0565898079227,-2.42858510549787,
0.));
#116807=CARTESIAN_POINT('Ctrl Pts',(74.0319431966956,-2.41660985465228,
0.));
#116808=CARTESIAN_POINT('Ctrl Pts',(74.0073176459287,-2.40467247811497,
0.));
#116809=CARTESIAN_POINT('Ctrl Pts',(73.9827132538149,-2.39277297220716,
0.));
#116810=CARTESIAN_POINT('Ctrl Pts',(73.9581301214609,-2.38091133274933,
0.));
#116811=CARTESIAN_POINT('Ctrl Pts',(73.9335683516388,-2.36908755525994,
0.));
#116812=CARTESIAN_POINT('Ctrl Pts',(73.9090280474723,-2.35730163516324,
0.));
#116813=CARTESIAN_POINT('Ctrl Pts',(73.8845093109302,-2.3455535680214,0.));
#116814=CARTESIAN_POINT('Ctrl Pts',(73.8600122421502,-2.33384334963981,
0.));
#116815=CARTESIAN_POINT('Ctrl Pts',(73.8355369402733,-2.32217097594216,
0.));
#116816=CARTESIAN_POINT('Ctrl Pts',(73.8110835039341,-2.31053644289425,
0.));
#116817=CARTESIAN_POINT('Ctrl Pts',(73.7866520318849,-2.29893974640435,
0.));
#116818=CARTESIAN_POINT('Ctrl Pts',(73.7622426235648,-2.28738088222859,
0.));
#116819=CARTESIAN_POINT('Ctrl Pts',(73.7378553796792,-2.27585984587193,
0.));
#116820=CARTESIAN_POINT('Ctrl Pts',(73.7134904019378,-2.26437663263664,
0.));
#116821=CARTESIAN_POINT('Ctrl Pts',(73.6891477928124,-2.25293123766425,
0.));
#116822=CARTESIAN_POINT('Ctrl Pts',(73.6648276552766,-2.24152365597699,
0.));
#116823=CARTESIAN_POINT('Ctrl Pts',(73.6405300925714,-2.23015388251289,
0.));
#116824=CARTESIAN_POINT('Ctrl Pts',(73.6162552079044,-2.21882191216521,
0.));
#116825=CARTESIAN_POINT('Ctrl Pts',(73.5920031044604,-2.20752773978353,
0.));
#116826=CARTESIAN_POINT('Ctrl Pts',(73.5677738855461,-2.19627136015683,
0.));
#116827=CARTESIAN_POINT('Ctrl Pts',(73.5435676546934,-2.18505276799757,
0.));
#116828=CARTESIAN_POINT('Ctrl Pts',(73.5193845157705,-2.17387195792306,
0.));
#116829=CARTESIAN_POINT('Ctrl Pts',(73.4952245731044,-2.16272892442916,
0.));
#116830=CARTESIAN_POINT('Ctrl Pts',(73.4710879315367,-2.15162366187899,
0.));
#116831=CARTESIAN_POINT('Ctrl Pts',(73.4469746963622,-2.14055616452049,
0.));
#116832=CARTESIAN_POINT('Ctrl Pts',(73.4228849732914,-2.12952642649361,
0.));
#116833=CARTESIAN_POINT('Ctrl Pts',(73.3988188684022,-2.11853444183764,
0.));
#116834=CARTESIAN_POINT('Ctrl Pts',(73.3747764880903,-2.10758020449401,
0.));
#116835=CARTESIAN_POINT('Ctrl Pts',(73.3507579390254,-2.09666370830733,
0.));
#116836=CARTESIAN_POINT('Ctrl Pts',(73.3267633281822,-2.08578494702762,
0.));
#116837=CARTESIAN_POINT('Ctrl Pts',(73.3027927628636,-2.07494391430954,
0.));
#116838=CARTESIAN_POINT('Ctrl Pts',(73.2788463507248,-2.06414060370838,
0.));
#116839=CARTESIAN_POINT('Ctrl Pts',(73.2549241997946,-2.05337500867396,
0.));
#116840=CARTESIAN_POINT('Ctrl Pts',(73.2310264184965,-2.04264712253915,
0.));
#116841=CARTESIAN_POINT('Ctrl Pts',(73.2071531156492,-2.03195693852441,
0.));
#116842=CARTESIAN_POINT('Ctrl Pts',(73.1833044004612,-2.02130444974352,
0.));
#116843=CARTESIAN_POINT('Ctrl Pts',(73.159480382525,-2.01068964920465,0.));
#116844=CARTESIAN_POINT('Ctrl Pts',(73.1356811718094,-2.00011252980988,
0.));
#116845=CARTESIAN_POINT('Ctrl Pts',(73.1119068786482,-1.9895730843493,0.));
#116846=CARTESIAN_POINT('Ctrl Pts',(73.0881576137415,-1.97907130550172,
0.));
#116847=CARTESIAN_POINT('Ctrl Pts',(73.0644334881679,-1.96860718583945,
0.));
#116848=CARTESIAN_POINT('Ctrl Pts',(73.0407346133912,-1.95818071782774,
0.));
#116849=CARTESIAN_POINT('Ctrl Pts',(73.0170611012659,-1.94779189382301,
0.));
#116850=CARTESIAN_POINT('Ctrl Pts',(72.9934130640414,-1.93744070606557,
0.));
#116851=CARTESIAN_POINT('Ctrl Pts',(72.9697906143638,-1.92712714667649,
0.));
#116852=CARTESIAN_POINT('Ctrl Pts',(72.9461938652816,-1.91685120766428,
0.));
#116853=CARTESIAN_POINT('Ctrl Pts',(72.9226229302483,-1.90661288092583,
0.));
#116854=CARTESIAN_POINT('Ctrl Pts',(72.8990779231226,-1.89641215824585,
0.));
#116855=CARTESIAN_POINT('Ctrl Pts',(72.8755589581674,-1.88624903129196,
0.));
#116856=CARTESIAN_POINT('Ctrl Pts',(72.8520661500465,-1.87612349160952,
0.));
#116857=CARTESIAN_POINT('Ctrl Pts',(72.8285996138346,-1.86603553062776,
0.));
#116858=CARTESIAN_POINT('Ctrl Pts',(72.8051594650214,-1.85598513966116,
0.));
#116859=CARTESIAN_POINT('Ctrl Pts',(72.7817458195155,-1.84597230990858,
0.));
#116860=CARTESIAN_POINT('Ctrl Pts',(72.7583587936454,-1.83599703244926,
0.));
#116861=CARTESIAN_POINT('Ctrl Pts',(72.73499850416,-1.82605929823566,0.));
#116862=CARTESIAN_POINT('Ctrl Pts',(72.7116650682347,-1.81615909809872,
0.));
#116863=CARTESIAN_POINT('Ctrl Pts',(72.6883586034768,-1.80629642275052,
0.));
#116864=CARTESIAN_POINT('Ctrl Pts',(72.6650792279271,-1.79647126278359,
0.));
#116865=CARTESIAN_POINT('Ctrl Pts',(72.6418270600623,-1.78668360866814,
0.));
#116866=CARTESIAN_POINT('Ctrl Pts',(72.618602218792,-1.77693345074431,0.));
#116867=CARTESIAN_POINT('Ctrl Pts',(72.5954048234655,-1.7672207792258,0.));
#116868=CARTESIAN_POINT('Ctrl Pts',(72.5722349938789,-1.7575455842035,0.));
#116869=CARTESIAN_POINT('Ctrl Pts',(72.5490928502773,-1.74790785564476,
0.));
#116870=CARTESIAN_POINT('Ctrl Pts',(72.5259785133586,-1.73830758339124,
0.));
#116871=CARTESIAN_POINT('Ctrl Pts',(72.5028921042704,-1.72874475715099,
0.));
#116872=CARTESIAN_POINT('Ctrl Pts',(72.4798337446162,-1.71921936650032,
0.));
#116873=CARTESIAN_POINT('Ctrl Pts',(72.4568035564618,-1.70973140088838,
0.));
#116874=CARTESIAN_POINT('Ctrl Pts',(72.4338016623388,-1.70028084963647,
0.));
#116875=CARTESIAN_POINT('Ctrl Pts',(72.4108281852473,-1.69086770193641,
0.));
#116876=CARTESIAN_POINT('Ctrl Pts',(72.3878832486549,-1.68149194684289,
0.));
#116877=CARTESIAN_POINT('Ctrl Pts',(72.3649669765013,-1.67215357327373,
0.));
#116878=CARTESIAN_POINT('Ctrl Pts',(72.3420794932052,-1.66285257001503,
0.));
#116879=CARTESIAN_POINT('Ctrl Pts',(72.3192209236691,-1.65358892572066,
0.));
#116880=CARTESIAN_POINT('Ctrl Pts',(72.2963913932811,-1.64436262891078,
0.));
#116881=CARTESIAN_POINT('Ctrl Pts',(72.2735910279149,-1.63517366796459,
0.));
#116882=CARTESIAN_POINT('Ctrl Pts',(72.2508199539325,-1.62602203111925,
0.));
#116883=CARTESIAN_POINT('Ctrl Pts',(72.2280782981941,-1.61690770647536,
0.));
#116884=CARTESIAN_POINT('Ctrl Pts',(72.2053661880611,-1.60783068199662,
0.));
#116885=CARTESIAN_POINT('Ctrl Pts',(72.1826837514,-1.5987909455085,0.));
#116886=CARTESIAN_POINT('Ctrl Pts',(72.1600311165813,-1.58978848469129,
0.));
#116887=CARTESIAN_POINT('Ctrl Pts',(72.1374084124829,-1.58082328707808,
0.));
#116888=CARTESIAN_POINT('Ctrl Pts',(72.1148157684987,-1.57189534006044,
0.));
#116889=CARTESIAN_POINT('Ctrl Pts',(72.092253314543,-1.56300463088811,0.));
#116890=CARTESIAN_POINT('Ctrl Pts',(72.0697211810548,-1.55415114666774,
0.));
#116891=CARTESIAN_POINT('Ctrl Pts',(72.0472194989968,-1.54533487435627,
0.));
#116892=CARTESIAN_POINT('Ctrl Pts',(72.0247483998582,-1.53655580075814,
0.));
#116893=CARTESIAN_POINT('Ctrl Pts',(72.0023080156647,-1.52781391253104,
0.));
#116894=CARTESIAN_POINT('Ctrl Pts',(71.9798984789828,-1.51910919618567,
0.));
#116895=CARTESIAN_POINT('Ctrl Pts',(71.9575199229241,-1.51044163808455,
0.));
#116896=CARTESIAN_POINT('Ctrl Pts',(71.935172481145,-1.50181122443536,0.));
#116897=CARTESIAN_POINT('Ctrl Pts',(71.9128562878491,-1.49321794128801,
0.));
#116898=CARTESIAN_POINT('Ctrl Pts',(71.8905714777972,-1.48466177454022,
0.));
#116899=CARTESIAN_POINT('Ctrl Pts',(71.8683181863123,-1.47614270993731,
0.));
#116900=CARTESIAN_POINT('Ctrl Pts',(71.8460965492836,-1.4676607330709,0.));
#116901=CARTESIAN_POINT('Ctrl Pts',(71.8239067031664,-1.45921582937229,
0.));
#116902=CARTESIAN_POINT('Ctrl Pts',(71.8017487849865,-1.45080798410957,
0.));
#116903=CARTESIAN_POINT('Ctrl Pts',(71.7796229323496,-1.44243718239305,
0.));
#116904=CARTESIAN_POINT('Ctrl Pts',(71.7575292834456,-1.4341034091749,0.));
#116905=CARTESIAN_POINT('Ctrl Pts',(71.7354679770537,-1.42580664924775,
0.));
#116906=CARTESIAN_POINT('Ctrl Pts',(71.7134391525417,-1.41754688723792,
0.));
#116907=CARTESIAN_POINT('Ctrl Pts',(71.6914429498702,-1.40932410760275,
0.));
#116908=CARTESIAN_POINT('Ctrl Pts',(71.6694795096034,-1.401138294636,0.));
#116909=CARTESIAN_POINT('Ctrl Pts',(71.6475489729149,-1.39298943246732,
0.));
#116910=CARTESIAN_POINT('Ctrl Pts',(71.6256514815918,-1.38487750506076,
0.));
#116911=CARTESIAN_POINT('Ctrl Pts',(71.6037871780347,-1.37680249620763,
0.));
#116912=CARTESIAN_POINT('Ctrl Pts',(71.5819562052613,-1.36876438952449,
0.));
#116913=CARTESIAN_POINT('Ctrl Pts',(71.5601587069175,-1.36076316845807,
0.));
#116914=CARTESIAN_POINT('Ctrl Pts',(71.538394827283,-1.35279881628454,0.));
#116915=CARTESIAN_POINT('Ctrl Pts',(71.5166647112766,-1.34487131610786,
0.));
#116916=CARTESIAN_POINT('Ctrl Pts',(71.4949685044559,-1.33698065085228,
0.));
#116917=CARTESIAN_POINT('Ctrl Pts',(71.4733063530227,-1.32912680326132,
0.));
#116918=CARTESIAN_POINT('Ctrl Pts',(71.4516784038346,-1.32130975590232,
0.));
#116919=CARTESIAN_POINT('Ctrl Pts',(71.4300848044095,-1.31352949116539,
0.));
#116920=CARTESIAN_POINT('Ctrl Pts',(71.4085257029308,-1.3057859912614,0.));
#116921=CARTESIAN_POINT('Ctrl Pts',(71.3870012482474,-1.29807923821414,
0.));
#116922=CARTESIAN_POINT('Ctrl Pts',(71.3655115898801,-1.29040921386061,
0.));
#116923=CARTESIAN_POINT('Ctrl Pts',(71.344056878033,-1.28277589985475,0.));
#116924=CARTESIAN_POINT('Ctrl Pts',(71.3226372635993,-1.27517927766611,
0.));
#116925=CARTESIAN_POINT('Ctrl Pts',(71.301252898167,-1.26761932857724,0.));
#116926=CARTESIAN_POINT('Ctrl Pts',(71.2799039340191,-1.26009603367565,
0.));
#116927=CARTESIAN_POINT('Ctrl Pts',(71.2585905241422,-1.25260937385561,
0.));
#116928=CARTESIAN_POINT('Ctrl Pts',(71.2373128222359,-1.24515932982108,
0.));
#116929=CARTESIAN_POINT('Ctrl Pts',(71.2160709827189,-1.23774588208427,
0.));
#116930=CARTESIAN_POINT('Ctrl Pts',(71.1948651607319,-1.23036901096246,
0.));
#116931=CARTESIAN_POINT('Ctrl Pts',(71.1736955121361,-1.22302869657029,
0.));
#116932=CARTESIAN_POINT('Ctrl Pts',(71.1525621935266,-1.21572491882274,
0.));
#116933=CARTESIAN_POINT('Ctrl Pts',(71.1314653622442,-1.20845765743655,
0.));
#116934=CARTESIAN_POINT('Ctrl Pts',(71.1104051763839,-1.20122689192837,
0.));
#116935=CARTESIAN_POINT('Ctrl Pts',(71.089381794801,-1.19403260160998,0.));
#116936=CARTESIAN_POINT('Ctrl Pts',(71.0683953771147,-1.18687476558127,
0.));
#116937=CARTESIAN_POINT('Ctrl Pts',(71.0474460837157,-1.179753362735,0.));
#116938=CARTESIAN_POINT('Ctrl Pts',(71.0265340757697,-1.17266837175776,
0.));
#116939=CARTESIAN_POINT('Ctrl Pts',(71.0056595152204,-1.16561977112883,
0.));
#116940=CARTESIAN_POINT('Ctrl Pts',(70.9848225647876,-1.1586075391149,0.));
#116941=CARTESIAN_POINT('Ctrl Pts',(70.9640233879671,-1.15163165376531,
0.));
#116942=CARTESIAN_POINT('Ctrl Pts',(70.943262149058,-1.14469209291494,0.));
#116943=CARTESIAN_POINT('Ctrl Pts',(70.9225390131835,-1.13778883418217,
0.));
#116944=CARTESIAN_POINT('Ctrl Pts',(70.9018541463083,-1.13092185496564,
0.));
#116945=CARTESIAN_POINT('Ctrl Pts',(70.8812077152564,-1.12409113243511,
0.));
#116946=CARTESIAN_POINT('Ctrl Pts',(70.860599887712,-1.11729664352991,0.));
#116947=CARTESIAN_POINT('Ctrl Pts',(70.8400308322013,-1.11053836496638,
0.));
#116948=CARTESIAN_POINT('Ctrl Pts',(70.8195007180739,-1.10381627323946,
0.));
#116949=CARTESIAN_POINT('Ctrl Pts',(70.7990097154855,-1.0971303446227,0.));
#116950=CARTESIAN_POINT('Ctrl Pts',(70.7785579953611,-1.09048055516434,
0.));
#116951=CARTESIAN_POINT('Ctrl Pts',(70.7581457294475,-1.08386688068349,
0.));
#116952=CARTESIAN_POINT('Ctrl Pts',(70.737773090397,-1.07728929676412,0.));
#116953=CARTESIAN_POINT('Ctrl Pts',(70.7174402518378,-1.07074777874597,
0.));
#116954=CARTESIAN_POINT('Ctrl Pts',(70.6971473884443,-1.0642423017128,0.));
#116955=CARTESIAN_POINT('Ctrl Pts',(70.6768946760063,-1.05777284047728,
0.));
#116956=CARTESIAN_POINT('Ctrl Pts',(70.6566822912965,-1.05133936960069,
0.));
#116957=CARTESIAN_POINT('Ctrl Pts',(70.6365104119238,-1.04494186341156,
0.));
#116958=CARTESIAN_POINT('Ctrl Pts',(70.6163792162079,-1.03858029601906,
0.));
#116959=CARTESIAN_POINT('Ctrl Pts',(70.5962888829958,-1.03225464132873,
0.));
#116960=CARTESIAN_POINT('Ctrl Pts',(70.5762395916412,-1.02596487304049,
0.));
#116961=CARTESIAN_POINT('Ctrl Pts',(70.5562315224219,-1.01971096460599,
0.));
#116962=CARTESIAN_POINT('Ctrl Pts',(70.5362648569072,-1.0134928891854,0.));
#116963=CARTESIAN_POINT('Ctrl Pts',(70.5163397782699,-1.00731061960968,
0.));
#116964=CARTESIAN_POINT('Ctrl Pts',(70.4964564717917,-1.00116412831438,
0.));
#116965=CARTESIAN_POINT('Ctrl Pts',(70.476615124517,-0.995053387379685,
0.));
#116966=CARTESIAN_POINT('Ctrl Pts',(70.4568159243131,-0.988978368643593,
0.));
#116967=CARTESIAN_POINT('Ctrl Pts',(70.4370590590839,-0.982939043792163,
0.));
#116968=CARTESIAN_POINT('Ctrl Pts',(70.41734471596,-0.976935384450131,0.));
#116969=CARTESIAN_POINT('Ctrl Pts',(70.3976730803664,-0.970967362281305,
0.));
#116970=CARTESIAN_POINT('Ctrl Pts',(70.3780443378003,-0.965034948786564,
0.));
#116971=CARTESIAN_POINT('Ctrl Pts',(70.3584586759561,-0.959138115058888,
0.));
#116972=CARTESIAN_POINT('Ctrl Pts',(70.338916286457,-0.953276831581237,
0.));
#116973=CARTESIAN_POINT('Ctrl Pts',(70.3194173673635,-0.947451067929568,
0.));
#116974=CARTESIAN_POINT('Ctrl Pts',(70.2999621233938,-0.941660792742957,
0.));
#116975=CARTESIAN_POINT('Ctrl Pts',(70.2805507606832,-0.935905974336494,
0.));
#116976=CARTESIAN_POINT('Ctrl Pts',(70.2611834821711,-0.93018658123558,
0.));
#116977=CARTESIAN_POINT('Ctrl Pts',(70.241860483586,-0.924502582639455,
0.));
#116978=CARTESIAN_POINT('Ctrl Pts',(70.2225819470306,-0.918853949157049,
0.));
#116979=CARTESIAN_POINT('Ctrl Pts',(70.2033480471749,-0.913240652090843,
0.));
#116980=CARTESIAN_POINT('Ctrl Pts',(70.184158963563,-0.907662662015655,
0.));
#116981=CARTESIAN_POINT('Ctrl Pts',(70.1650148905109,-0.902119947629777,
0.));
#116982=CARTESIAN_POINT('Ctrl Pts',(70.1459160490366,-0.896612474372089,
0.));
#116983=CARTESIAN_POINT('Ctrl Pts',(70.1268626950031,-0.891140203464729,
0.));
#116984=CARTESIAN_POINT('Ctrl Pts',(70.1078550938801,-0.885703094803091,
0.));
#116985=CARTESIAN_POINT('Ctrl Pts',(70.0888934967772,-0.880301109661041,
0.));
#116986=CARTESIAN_POINT('Ctrl Pts',(70.0699781184013,-0.874934213255575,
0.));
#116987=CARTESIAN_POINT('Ctrl Pts',(70.0511091083285,-0.869602377870143,
0.));
#116988=CARTESIAN_POINT('Ctrl Pts',(70.0322865493339,-0.864305583660094,
0.));
#116989=CARTESIAN_POINT('Ctrl Pts',(70.0172656934192,-0.860096170667403,
0.));
#116990=CARTESIAN_POINT('Ctrl Pts',(70.0060209754332,-0.856954870258375,
0.));
#116991=CARTESIAN_POINT('Ctrl Pts',(69.9985337959499,-0.854867673848295,
0.));
#116992=CARTESIAN_POINT('Ctrl Pts',(69.9947925310006,-0.853825826608997,
0.));
#116993=CARTESIAN_POINT('Ctrl Pts',(73.9415940197274,-9.10443154852689,
0.));
#116994=CARTESIAN_POINT('Ctrl Pts',(73.9415940197274,-9.10443154852689,
12.));
#116995=CARTESIAN_POINT('Ctrl Pts',(73.9368365074299,-9.10148558516537,
0.));
#116996=CARTESIAN_POINT('Ctrl Pts',(73.9368365074299,-9.10148558516537,
12.));
#116997=CARTESIAN_POINT('Ctrl Pts',(73.9273231219835,-9.09559760529042,
0.));
#116998=CARTESIAN_POINT('Ctrl Pts',(73.9273231219835,-9.09559760529042,
12.));
#116999=CARTESIAN_POINT('Ctrl Pts',(73.9130579612604,-9.08677747602206,
0.));
#117000=CARTESIAN_POINT('Ctrl Pts',(73.9130579612604,-9.08677747602206,
12.));
#117001=CARTESIAN_POINT('Ctrl Pts',(73.8940475822492,-9.07504098571707,
0.));
#117002=CARTESIAN_POINT('Ctrl Pts',(73.8940475822492,-9.07504098571707,
12.));
#117003=CARTESIAN_POINT('Ctrl Pts',(73.8703010078091,-9.06040984890246,
0.));
#117004=CARTESIAN_POINT('Ctrl Pts',(73.8703010078091,-9.06040984890246,
12.));
#117005=CARTESIAN_POINT('Ctrl Pts',(73.8465708501057,-9.04581819646985,
0.));
#117006=CARTESIAN_POINT('Ctrl Pts',(73.8465708501057,-9.04581819646985,
12.));
#117007=CARTESIAN_POINT('Ctrl Pts',(73.8228571411697,-9.03126603778126,
0.));
#117008=CARTESIAN_POINT('Ctrl Pts',(73.8228571411697,-9.03126603778126,
12.));
#117009=CARTESIAN_POINT('Ctrl Pts',(73.7991599312592,-9.01675338208004,
0.));
#117010=CARTESIAN_POINT('Ctrl Pts',(73.7991599312592,-9.01675338208004,
12.));
#117011=CARTESIAN_POINT('Ctrl Pts',(73.7754792943665,-9.00228023701055,
0.));
#117012=CARTESIAN_POINT('Ctrl Pts',(73.7754792943665,-9.00228023701055,
12.));
#117013=CARTESIAN_POINT('Ctrl Pts',(73.7518153261981,-8.98784660837398,
0.));
#117014=CARTESIAN_POINT('Ctrl Pts',(73.7518153261981,-8.98784660837398,
12.));
#117015=CARTESIAN_POINT('Ctrl Pts',(73.728168136383,-8.97345250083601,0.));
#117016=CARTESIAN_POINT('Ctrl Pts',(73.728168136383,-8.97345250083601,12.));
#117017=CARTESIAN_POINT('Ctrl Pts',(73.7045378422686,-8.95909791836153,
0.));
#117018=CARTESIAN_POINT('Ctrl Pts',(73.7045378422686,-8.95909791836153,
12.));
#117019=CARTESIAN_POINT('Ctrl Pts',(73.6809245622383,-8.94478286474419,
0.));
#117020=CARTESIAN_POINT('Ctrl Pts',(73.6809245622383,-8.94478286474419,
12.));
#117021=CARTESIAN_POINT('Ctrl Pts',(73.6573284088184,-8.93050734412124,
0.));
#117022=CARTESIAN_POINT('Ctrl Pts',(73.6573284088184,-8.93050734412124,
12.));
#117023=CARTESIAN_POINT('Ctrl Pts',(73.633749483097,-8.91627136140084,0.));
#117024=CARTESIAN_POINT('Ctrl Pts',(73.633749483097,-8.91627136140084,12.));
#117025=CARTESIAN_POINT('Ctrl Pts',(73.6101878785976,-8.90207492199043,
0.));
#117026=CARTESIAN_POINT('Ctrl Pts',(73.6101878785976,-8.90207492199043,
12.));
#117027=CARTESIAN_POINT('Ctrl Pts',(73.5866436840556,-8.88791803160442,
0.));
#117028=CARTESIAN_POINT('Ctrl Pts',(73.5866436840556,-8.88791803160442,
12.));
#117029=CARTESIAN_POINT('Ctrl Pts',(73.5631169867122,-8.8738006960297,0.));
#117030=CARTESIAN_POINT('Ctrl Pts',(73.5631169867122,-8.8738006960297,12.));
#117031=CARTESIAN_POINT('Ctrl Pts',(73.5396078751639,-8.8597229209213,0.));
#117032=CARTESIAN_POINT('Ctrl Pts',(73.5396078751639,-8.8597229209213,12.));
#117033=CARTESIAN_POINT('Ctrl Pts',(73.5161164429709,-8.84568471153805,
0.));
#117034=CARTESIAN_POINT('Ctrl Pts',(73.5161164429709,-8.84568471153805,
12.));
#117035=CARTESIAN_POINT('Ctrl Pts',(73.492642788273,-8.83168607277325,0.));
#117036=CARTESIAN_POINT('Ctrl Pts',(73.492642788273,-8.83168607277325,12.));
#117037=CARTESIAN_POINT('Ctrl Pts',(73.4691870121567,-8.8177270092753,0.));
#117038=CARTESIAN_POINT('Ctrl Pts',(73.4691870121567,-8.8177270092753,12.));
#117039=CARTESIAN_POINT('Ctrl Pts',(73.4457492173933,-8.80380752553692,
0.));
#117040=CARTESIAN_POINT('Ctrl Pts',(73.4457492173933,-8.80380752553692,
12.));
#117041=CARTESIAN_POINT('Ctrl Pts',(73.422329507113,-8.78992762598756,0.));
#117042=CARTESIAN_POINT('Ctrl Pts',(73.422329507113,-8.78992762598756,12.));
#117043=CARTESIAN_POINT('Ctrl Pts',(73.3989279832835,-8.77608731509348,
0.));
#117044=CARTESIAN_POINT('Ctrl Pts',(73.3989279832835,-8.77608731509348,
12.));
#117045=CARTESIAN_POINT('Ctrl Pts',(73.3755447460269,-8.76228659740357,
0.));
#117046=CARTESIAN_POINT('Ctrl Pts',(73.3755447460269,-8.76228659740357,
12.));
#117047=CARTESIAN_POINT('Ctrl Pts',(73.3521798944622,-8.74852547749778,
0.));
#117048=CARTESIAN_POINT('Ctrl Pts',(73.3521798944622,-8.74852547749778,
12.));
#117049=CARTESIAN_POINT('Ctrl Pts',(73.3288335272002,-8.7348039599538,0.));
#117050=CARTESIAN_POINT('Ctrl Pts',(73.3288335272002,-8.7348039599538,12.));
#117051=CARTESIAN_POINT('Ctrl Pts',(73.3055057429742,-8.72112204930232,
0.));
#117052=CARTESIAN_POINT('Ctrl Pts',(73.3055057429742,-8.72112204930232,
12.));
#117053=CARTESIAN_POINT('Ctrl Pts',(73.2821966412148,-8.70747974998229,
0.));
#117054=CARTESIAN_POINT('Ctrl Pts',(73.2821966412148,-8.70747974998229,
12.));
#117055=CARTESIAN_POINT('Ctrl Pts',(73.2589063226358,-8.69387706629285,
0.));
#117056=CARTESIAN_POINT('Ctrl Pts',(73.2589063226358,-8.69387706629285,
12.));
#117057=CARTESIAN_POINT('Ctrl Pts',(73.2356348889693,-8.68031400241872,
0.));
#117058=CARTESIAN_POINT('Ctrl Pts',(73.2356348889693,-8.68031400241872,
12.));
#117059=CARTESIAN_POINT('Ctrl Pts',(73.2123824427208,-8.66679056245092,
0.));
#117060=CARTESIAN_POINT('Ctrl Pts',(73.2123824427208,-8.66679056245092,
12.));
#117061=CARTESIAN_POINT('Ctrl Pts',(73.1891490869056,-8.65330675040537,
0.));
#117062=CARTESIAN_POINT('Ctrl Pts',(73.1891490869056,-8.65330675040537,
12.));
#117063=CARTESIAN_POINT('Ctrl Pts',(73.1659349248132,-8.63986257023739,
0.));
#117064=CARTESIAN_POINT('Ctrl Pts',(73.1659349248132,-8.63986257023739,
12.));
#117065=CARTESIAN_POINT('Ctrl Pts',(73.1427400597037,-8.62645802585484,
0.));
#117066=CARTESIAN_POINT('Ctrl Pts',(73.1427400597037,-8.62645802585484,
12.));
#117067=CARTESIAN_POINT('Ctrl Pts',(73.1195645948178,-8.61309312112002,
0.));
#117068=CARTESIAN_POINT('Ctrl Pts',(73.1195645948178,-8.61309312112002,
12.));
#117069=CARTESIAN_POINT('Ctrl Pts',(73.0964086335235,-8.59976785984551,
0.));
#117070=CARTESIAN_POINT('Ctrl Pts',(73.0964086335235,-8.59976785984551,
12.));
#117071=CARTESIAN_POINT('Ctrl Pts',(73.0732722794195,-8.58648224578731,
0.));
#117072=CARTESIAN_POINT('Ctrl Pts',(73.0732722794195,-8.58648224578731,
12.));
#117073=CARTESIAN_POINT('Ctrl Pts',(73.0501556364479,-8.57323628263593,
0.));
#117074=CARTESIAN_POINT('Ctrl Pts',(73.0501556364479,-8.57323628263593,
12.));
#117075=CARTESIAN_POINT('Ctrl Pts',(73.0270588090183,-8.56002997400084,
0.));
#117076=CARTESIAN_POINT('Ctrl Pts',(73.0270588090183,-8.56002997400084,
12.));
#117077=CARTESIAN_POINT('Ctrl Pts',(73.0039819020648,-8.54686332340418,
0.));
#117078=CARTESIAN_POINT('Ctrl Pts',(73.0039819020648,-8.54686332340418,
12.));
#117079=CARTESIAN_POINT('Ctrl Pts',(72.9809250209828,-8.53373633429281,
0.));
#117080=CARTESIAN_POINT('Ctrl Pts',(72.9809250209828,-8.53373633429281,
12.));
#117081=CARTESIAN_POINT('Ctrl Pts',(72.9578882715912,-8.52064901004227,
0.));
#117082=CARTESIAN_POINT('Ctrl Pts',(72.9578882715912,-8.52064901004227,
12.));
#117083=CARTESIAN_POINT('Ctrl Pts',(72.9348717600838,-8.50760135395983,
0.));
#117084=CARTESIAN_POINT('Ctrl Pts',(72.9348717600838,-8.50760135395983,
12.));
#117085=CARTESIAN_POINT('Ctrl Pts',(72.9118755929795,-8.49459336928296,
0.));
#117086=CARTESIAN_POINT('Ctrl Pts',(72.9118755929795,-8.49459336928296,
12.));
#117087=CARTESIAN_POINT('Ctrl Pts',(72.8888998770785,-8.48162505917658,
0.));
#117088=CARTESIAN_POINT('Ctrl Pts',(72.8888998770785,-8.48162505917658,
12.));
#117089=CARTESIAN_POINT('Ctrl Pts',(72.8659447194933,-8.46869642673794,
0.));
#117090=CARTESIAN_POINT('Ctrl Pts',(72.8659447194933,-8.46869642673794,
12.));
#117091=CARTESIAN_POINT('Ctrl Pts',(72.8430102276713,-8.45580747499793,
0.));
#117092=CARTESIAN_POINT('Ctrl Pts',(72.8430102276713,-8.45580747499793,
12.));
#117093=CARTESIAN_POINT('Ctrl Pts',(72.8200965094199,-8.44295820691911,
0.));
#117094=CARTESIAN_POINT('Ctrl Pts',(72.8200965094199,-8.44295820691911,
12.));
#117095=CARTESIAN_POINT('Ctrl Pts',(72.7972036729276,-8.43014862539158,
0.));
#117096=CARTESIAN_POINT('Ctrl Pts',(72.7972036729276,-8.43014862539158,
12.));
#117097=CARTESIAN_POINT('Ctrl Pts',(72.7743318267865,-8.4173787332233,0.));
#117098=CARTESIAN_POINT('Ctrl Pts',(72.7743318267865,-8.4173787332233,12.));
#117099=CARTESIAN_POINT('Ctrl Pts',(72.751481079992,-8.40464853314468,0.));
#117100=CARTESIAN_POINT('Ctrl Pts',(72.751481079992,-8.40464853314468,12.));
#117101=CARTESIAN_POINT('Ctrl Pts',(72.7286515419373,-8.3919580278139,0.));
#117102=CARTESIAN_POINT('Ctrl Pts',(72.7286515419373,-8.3919580278139,12.));
#117103=CARTESIAN_POINT('Ctrl Pts',(72.705843322407,-8.37930721981731,0.));
#117104=CARTESIAN_POINT('Ctrl Pts',(72.705843322407,-8.37930721981731,12.));
#117105=CARTESIAN_POINT('Ctrl Pts',(72.6830565315703,-8.36669611166842,
0.));
#117106=CARTESIAN_POINT('Ctrl Pts',(72.6830565315703,-8.36669611166842,
12.));
#117107=CARTESIAN_POINT('Ctrl Pts',(72.6602912799696,-8.35412470580101,
0.));
#117108=CARTESIAN_POINT('Ctrl Pts',(72.6602912799696,-8.35412470580101,
12.));
#117109=CARTESIAN_POINT('Ctrl Pts',(72.6375476785215,-8.34159300456986,
0.));
#117110=CARTESIAN_POINT('Ctrl Pts',(72.6375476785215,-8.34159300456986,
12.));
#117111=CARTESIAN_POINT('Ctrl Pts',(72.6148258385296,-8.3291010102567,0.));
#117112=CARTESIAN_POINT('Ctrl Pts',(72.6148258385296,-8.3291010102567,12.));
#117113=CARTESIAN_POINT('Ctrl Pts',(72.5921258716901,-8.31664872507016,
0.));
#117114=CARTESIAN_POINT('Ctrl Pts',(72.5921258716901,-8.31664872507016,
12.));
#117115=CARTESIAN_POINT('Ctrl Pts',(72.5694478900982,-8.30423615114453,
0.));
#117116=CARTESIAN_POINT('Ctrl Pts',(72.5694478900982,-8.30423615114453,
12.));
#117117=CARTESIAN_POINT('Ctrl Pts',(72.5467920062521,-8.29186329053279,
0.));
#117118=CARTESIAN_POINT('Ctrl Pts',(72.5467920062521,-8.29186329053279,
12.));
#117119=CARTESIAN_POINT('Ctrl Pts',(72.5241583330562,-8.27953014520376,
0.));
#117120=CARTESIAN_POINT('Ctrl Pts',(72.5241583330562,-8.27953014520376,
12.));
#117121=CARTESIAN_POINT('Ctrl Pts',(72.5015469838254,-8.2672367170492,0.));
#117122=CARTESIAN_POINT('Ctrl Pts',(72.5015469838254,-8.2672367170492,12.));
#117123=CARTESIAN_POINT('Ctrl Pts',(72.4789580722875,-8.25498300788493,
0.));
#117124=CARTESIAN_POINT('Ctrl Pts',(72.4789580722875,-8.25498300788493,
12.));
#117125=CARTESIAN_POINT('Ctrl Pts',(72.4563917125842,-8.2427690194504,0.));
#117126=CARTESIAN_POINT('Ctrl Pts',(72.4563917125842,-8.2427690194504,12.));
#117127=CARTESIAN_POINT('Ctrl Pts',(72.4338480192695,-8.23059475340357,
0.));
#117128=CARTESIAN_POINT('Ctrl Pts',(72.4338480192695,-8.23059475340357,
12.));
#117129=CARTESIAN_POINT('Ctrl Pts',(72.4113271073079,-8.21846021131561,
0.));
#117130=CARTESIAN_POINT('Ctrl Pts',(72.4113271073079,-8.21846021131561,
12.));
#117131=CARTESIAN_POINT('Ctrl Pts',(72.3888290920832,-8.20636539467776,
0.));
#117132=CARTESIAN_POINT('Ctrl Pts',(72.3888290920832,-8.20636539467776,
12.));
#117133=CARTESIAN_POINT('Ctrl Pts',(72.3663540894026,-8.19431030490314,
0.));
#117134=CARTESIAN_POINT('Ctrl Pts',(72.3663540894026,-8.19431030490314,
12.));
#117135=CARTESIAN_POINT('Ctrl Pts',(72.3439022155007,-8.18229494332624,
0.));
#117136=CARTESIAN_POINT('Ctrl Pts',(72.3439022155007,-8.18229494332624,
12.));
#117137=CARTESIAN_POINT('Ctrl Pts',(72.3214735870409,-8.1703193111989,0.));
#117138=CARTESIAN_POINT('Ctrl Pts',(72.3214735870409,-8.1703193111989,12.));
#117139=CARTESIAN_POINT('Ctrl Pts',(72.2990683211162,-8.15838340968336,
0.));
#117140=CARTESIAN_POINT('Ctrl Pts',(72.2990683211162,-8.15838340968336,
12.));
#117141=CARTESIAN_POINT('Ctrl Pts',(72.2766865352555,-8.14648723985797,
0.));
#117142=CARTESIAN_POINT('Ctrl Pts',(72.2766865352555,-8.14648723985797,
12.));
#117143=CARTESIAN_POINT('Ctrl Pts',(72.2543283474278,-8.13463080272029,
0.));
#117144=CARTESIAN_POINT('Ctrl Pts',(72.2543283474278,-8.13463080272029,
12.));
#117145=CARTESIAN_POINT('Ctrl Pts',(72.2319938760449,-8.12281409918661,
0.));
#117146=CARTESIAN_POINT('Ctrl Pts',(72.2319938760449,-8.12281409918661,
12.));
#117147=CARTESIAN_POINT('Ctrl Pts',(72.209683239963,-8.11103713008928,0.));
#117148=CARTESIAN_POINT('Ctrl Pts',(72.209683239963,-8.11103713008928,12.));
#117149=CARTESIAN_POINT('Ctrl Pts',(72.1873965584813,-8.0992998961689,0.));
#117150=CARTESIAN_POINT('Ctrl Pts',(72.1873965584813,-8.0992998961689,12.));
#117151=CARTESIAN_POINT('Ctrl Pts',(72.1651339513477,-8.08760239807836,
0.));
#117152=CARTESIAN_POINT('Ctrl Pts',(72.1651339513477,-8.08760239807836,
12.));
#117153=CARTESIAN_POINT('Ctrl Pts',(72.1428955387663,-8.07594463638719,
0.));
#117154=CARTESIAN_POINT('Ctrl Pts',(72.1428955387663,-8.07594463638719,
12.));
#117155=CARTESIAN_POINT('Ctrl Pts',(72.1206814413988,-8.06432661158096,
0.));
#117156=CARTESIAN_POINT('Ctrl Pts',(72.1206814413988,-8.06432661158096,
12.));
#117157=CARTESIAN_POINT('Ctrl Pts',(72.0984917803693,-8.05274832405948,
0.));
#117158=CARTESIAN_POINT('Ctrl Pts',(72.0984917803693,-8.05274832405948,
12.));
#117159=CARTESIAN_POINT('Ctrl Pts',(72.0763266772615,-8.04120977412872,
0.));
#117160=CARTESIAN_POINT('Ctrl Pts',(72.0763266772615,-8.04120977412872,
12.));
#117161=CARTESIAN_POINT('Ctrl Pts',(72.0541862541243,-8.02971096200307,
0.));
#117162=CARTESIAN_POINT('Ctrl Pts',(72.0541862541243,-8.02971096200307,
12.));
#117163=CARTESIAN_POINT('Ctrl Pts',(72.032070633479,-8.01825188781056,0.));
#117164=CARTESIAN_POINT('Ctrl Pts',(72.032070633479,-8.01825188781056,12.));
#117165=CARTESIAN_POINT('Ctrl Pts',(72.0099799383213,-8.00683255159247,
0.));
#117166=CARTESIAN_POINT('Ctrl Pts',(72.0099799383213,-8.00683255159247,
12.));
#117167=CARTESIAN_POINT('Ctrl Pts',(71.9879142921254,-7.99545295330191,
0.));
#117168=CARTESIAN_POINT('Ctrl Pts',(71.9879142921254,-7.99545295330191,
12.));
#117169=CARTESIAN_POINT('Ctrl Pts',(71.965873818843,-7.98411309279612,0.));
#117170=CARTESIAN_POINT('Ctrl Pts',(71.965873818843,-7.98411309279612,12.));
#117171=CARTESIAN_POINT('Ctrl Pts',(71.9438586429081,-7.97281296983718,
0.));
#117172=CARTESIAN_POINT('Ctrl Pts',(71.9438586429081,-7.97281296983718,
12.));
#117173=CARTESIAN_POINT('Ctrl Pts',(71.9218688892431,-7.96155258409763,
0.));
#117174=CARTESIAN_POINT('Ctrl Pts',(71.9218688892431,-7.96155258409763,
12.));
#117175=CARTESIAN_POINT('Ctrl Pts',(71.8999046832643,-7.9503319351605,0.));
#117176=CARTESIAN_POINT('Ctrl Pts',(71.8999046832643,-7.9503319351605,12.));
#117177=CARTESIAN_POINT('Ctrl Pts',(71.8779661508832,-7.93915102251794,
0.));
#117178=CARTESIAN_POINT('Ctrl Pts',(71.8779661508832,-7.93915102251794,
12.));
#117179=CARTESIAN_POINT('Ctrl Pts',(71.8560534185071,-7.92800984556396,
0.));
#117180=CARTESIAN_POINT('Ctrl Pts',(71.8560534185071,-7.92800984556396,
12.));
#117181=CARTESIAN_POINT('Ctrl Pts',(71.8341666130426,-7.91690840359367,
0.));
#117182=CARTESIAN_POINT('Ctrl Pts',(71.8341666130426,-7.91690840359367,
12.));
#117183=CARTESIAN_POINT('Ctrl Pts',(71.8123058619042,-7.90584669580955,
0.));
#117184=CARTESIAN_POINT('Ctrl Pts',(71.8123058619042,-7.90584669580955,
12.));
#117185=CARTESIAN_POINT('Ctrl Pts',(71.7904712930175,-7.89482472132137,
0.));
#117186=CARTESIAN_POINT('Ctrl Pts',(71.7904712930175,-7.89482472132137,
12.));
#117187=CARTESIAN_POINT('Ctrl Pts',(71.7686630348238,-7.88384247914524,
0.));
#117188=CARTESIAN_POINT('Ctrl Pts',(71.7686630348238,-7.88384247914524,
12.));
#117189=CARTESIAN_POINT('Ctrl Pts',(71.7468812162788,-7.87289996819653,
0.));
#117190=CARTESIAN_POINT('Ctrl Pts',(71.7468812162788,-7.87289996819653,
12.));
#117191=CARTESIAN_POINT('Ctrl Pts',(71.7251259668563,-7.86199718728826,
0.));
#117192=CARTESIAN_POINT('Ctrl Pts',(71.7251259668563,-7.86199718728826,
12.));
#117193=CARTESIAN_POINT('Ctrl Pts',(71.7033974165568,-7.85113413513736,
0.));
#117194=CARTESIAN_POINT('Ctrl Pts',(71.7033974165568,-7.85113413513736,
12.));
#117195=CARTESIAN_POINT('Ctrl Pts',(71.6816956959117,-7.84031081036489,
0.));
#117196=CARTESIAN_POINT('Ctrl Pts',(71.6816956959117,-7.84031081036489,
12.));
#117197=CARTESIAN_POINT('Ctrl Pts',(71.6600209359872,-7.82952721149507,
0.));
#117198=CARTESIAN_POINT('Ctrl Pts',(71.6600209359872,-7.82952721149507,
12.));
#117199=CARTESIAN_POINT('Ctrl Pts',(71.6383732683844,-7.8187833369486,0.));
#117200=CARTESIAN_POINT('Ctrl Pts',(71.6383732683844,-7.8187833369486,12.));
#117201=CARTESIAN_POINT('Ctrl Pts',(71.6167528252423,-7.80807918504021,
0.));
#117202=CARTESIAN_POINT('Ctrl Pts',(71.6167528252423,-7.80807918504021,
12.));
#117203=CARTESIAN_POINT('Ctrl Pts',(71.5951597392471,-7.79741475398513,
0.));
#117204=CARTESIAN_POINT('Ctrl Pts',(71.5951597392471,-7.79741475398513,
12.));
#117205=CARTESIAN_POINT('Ctrl Pts',(71.5735941436364,-7.78679004189935,
0.));
#117206=CARTESIAN_POINT('Ctrl Pts',(71.5735941436364,-7.78679004189935,
12.));
#117207=CARTESIAN_POINT('Ctrl Pts',(71.5520561722039,-7.77620504679869,
0.));
#117208=CARTESIAN_POINT('Ctrl Pts',(71.5520561722039,-7.77620504679869,
12.));
#117209=CARTESIAN_POINT('Ctrl Pts',(71.5305459592994,-7.76565976659226,
0.));
#117210=CARTESIAN_POINT('Ctrl Pts',(71.5305459592994,-7.76565976659226,
12.));
#117211=CARTESIAN_POINT('Ctrl Pts',(71.5090636398318,-7.75515419907966,
0.));
#117212=CARTESIAN_POINT('Ctrl Pts',(71.5090636398318,-7.75515419907966,
12.));
#117213=CARTESIAN_POINT('Ctrl Pts',(71.4876093492781,-7.74468834195746,
0.));
#117214=CARTESIAN_POINT('Ctrl Pts',(71.4876093492781,-7.74468834195746,
12.));
#117215=CARTESIAN_POINT('Ctrl Pts',(71.4661832236888,-7.7342621928194,0.));
#117216=CARTESIAN_POINT('Ctrl Pts',(71.4661832236888,-7.7342621928194,12.));
#117217=CARTESIAN_POINT('Ctrl Pts',(71.4447853996916,-7.72387574915544,
0.));
#117218=CARTESIAN_POINT('Ctrl Pts',(71.4447853996916,-7.72387574915544,
12.));
#117219=CARTESIAN_POINT('Ctrl Pts',(71.4234160144925,-7.7135290083452,0.));
#117220=CARTESIAN_POINT('Ctrl Pts',(71.4234160144925,-7.7135290083452,12.));
#117221=CARTESIAN_POINT('Ctrl Pts',(71.4020752058796,-7.70322196765538,
0.));
#117222=CARTESIAN_POINT('Ctrl Pts',(71.4020752058796,-7.70322196765538,
12.));
#117223=CARTESIAN_POINT('Ctrl Pts',(71.3807631122331,-7.69295462424612,
0.));
#117224=CARTESIAN_POINT('Ctrl Pts',(71.3807631122331,-7.69295462424612,
12.));
#117225=CARTESIAN_POINT('Ctrl Pts',(71.3594798725281,-7.68272697517086,
0.));
#117226=CARTESIAN_POINT('Ctrl Pts',(71.3594798725281,-7.68272697517086,
12.));
#117227=CARTESIAN_POINT('Ctrl Pts',(71.3382256263414,-7.67253901737552,
0.));
#117228=CARTESIAN_POINT('Ctrl Pts',(71.3382256263414,-7.67253901737552,
12.));
#117229=CARTESIAN_POINT('Ctrl Pts',(71.3170005138502,-7.66239074769163,
0.));
#117230=CARTESIAN_POINT('Ctrl Pts',(71.3170005138502,-7.66239074769163,
12.));
#117231=CARTESIAN_POINT('Ctrl Pts',(71.2958046758372,-7.65228216283404,
0.));
#117232=CARTESIAN_POINT('Ctrl Pts',(71.2958046758372,-7.65228216283404,
12.));
#117233=CARTESIAN_POINT('Ctrl Pts',(71.2746382537007,-7.64221325940724,
0.));
#117234=CARTESIAN_POINT('Ctrl Pts',(71.2746382537007,-7.64221325940724,
12.));
#117235=CARTESIAN_POINT('Ctrl Pts',(71.2535013894602,-7.63218403390537,
0.));
#117236=CARTESIAN_POINT('Ctrl Pts',(71.2535013894602,-7.63218403390537,
12.));
#117237=CARTESIAN_POINT('Ctrl Pts',(71.2323942257609,-7.62219448271109,
0.));
#117238=CARTESIAN_POINT('Ctrl Pts',(71.2323942257609,-7.62219448271109,
12.));
#117239=CARTESIAN_POINT('Ctrl Pts',(71.211316905874,-7.61224460208837,0.));
#117240=CARTESIAN_POINT('Ctrl Pts',(71.211316905874,-7.61224460208837,12.));
#117241=CARTESIAN_POINT('Ctrl Pts',(71.1902695737013,-7.60233438818096,
0.));
#117242=CARTESIAN_POINT('Ctrl Pts',(71.1902695737013,-7.60233438818096,
12.));
#117243=CARTESIAN_POINT('Ctrl Pts',(71.1692523737844,-7.59246383701814,
0.));
#117244=CARTESIAN_POINT('Ctrl Pts',(71.1692523737844,-7.59246383701814,
12.));
#117245=CARTESIAN_POINT('Ctrl Pts',(71.1482654513119,-7.58263294451452,
0.));
#117246=CARTESIAN_POINT('Ctrl Pts',(71.1482654513119,-7.58263294451452,
12.));
#117247=CARTESIAN_POINT('Ctrl Pts',(71.1273089521234,-7.57284170646886,
0.));
#117248=CARTESIAN_POINT('Ctrl Pts',(71.1273089521234,-7.57284170646886,
12.));
#117249=CARTESIAN_POINT('Ctrl Pts',(71.106383022711,-7.56309011855657,0.));
#117250=CARTESIAN_POINT('Ctrl Pts',(71.106383022711,-7.56309011855657,12.));
#117251=CARTESIAN_POINT('Ctrl Pts',(71.0854878102243,-7.55337817632916,
0.));
#117252=CARTESIAN_POINT('Ctrl Pts',(71.0854878102243,-7.55337817632916,
12.));
#117253=CARTESIAN_POINT('Ctrl Pts',(71.0646234624811,-7.54370587521979,
0.));
#117254=CARTESIAN_POINT('Ctrl Pts',(71.0646234624811,-7.54370587521979,
12.));
#117255=CARTESIAN_POINT('Ctrl Pts',(71.043790127973,-7.53407321054262,0.));
#117256=CARTESIAN_POINT('Ctrl Pts',(71.043790127973,-7.53407321054262,12.));
#117257=CARTESIAN_POINT('Ctrl Pts',(71.0229879558699,-7.52448017749125,
0.));
#117258=CARTESIAN_POINT('Ctrl Pts',(71.0229879558699,-7.52448017749125,
12.));
#117259=CARTESIAN_POINT('Ctrl Pts',(71.002217096021,-7.5149267711309,0.));
#117260=CARTESIAN_POINT('Ctrl Pts',(71.002217096021,-7.5149267711309,12.));
#117261=CARTESIAN_POINT('Ctrl Pts',(70.9814776989612,-7.50541298639928,
0.));
#117262=CARTESIAN_POINT('Ctrl Pts',(70.9814776989612,-7.50541298639928,
12.));
#117263=CARTESIAN_POINT('Ctrl Pts',(70.9607699159218,-7.4959388181113,0.));
#117264=CARTESIAN_POINT('Ctrl Pts',(70.9607699159218,-7.4959388181113,12.));
#117265=CARTESIAN_POINT('Ctrl Pts',(70.940093898837,-7.48650426095824,0.));
#117266=CARTESIAN_POINT('Ctrl Pts',(70.940093898837,-7.48650426095824,12.));
#117267=CARTESIAN_POINT('Ctrl Pts',(70.9194498003493,-7.47710930950562,
0.));
#117268=CARTESIAN_POINT('Ctrl Pts',(70.9194498003493,-7.47710930950562,
12.));
#117269=CARTESIAN_POINT('Ctrl Pts',(70.8988377738104,-7.46775395818527,
0.));
#117270=CARTESIAN_POINT('Ctrl Pts',(70.8988377738104,-7.46775395818527,
12.));
#117271=CARTESIAN_POINT('Ctrl Pts',(70.87825797329,-7.45843820129782,0.));
#117272=CARTESIAN_POINT('Ctrl Pts',(70.87825797329,-7.45843820129782,12.));
#117273=CARTESIAN_POINT('Ctrl Pts',(70.8577105535848,-7.44916203301647,
0.));
#117274=CARTESIAN_POINT('Ctrl Pts',(70.8577105535848,-7.44916203301647,
12.));
#117275=CARTESIAN_POINT('Ctrl Pts',(70.8371956702241,-7.43992544738606,
0.));
#117276=CARTESIAN_POINT('Ctrl Pts',(70.8371956702241,-7.43992544738606,
12.));
#117277=CARTESIAN_POINT('Ctrl Pts',(70.8167134794737,-7.43072843832014,
0.));
#117278=CARTESIAN_POINT('Ctrl Pts',(70.8167134794737,-7.43072843832014,
12.));
#117279=CARTESIAN_POINT('Ctrl Pts',(70.796264138335,-7.42157099959326,0.));
#117280=CARTESIAN_POINT('Ctrl Pts',(70.796264138335,-7.42157099959326,12.));
#117281=CARTESIAN_POINT('Ctrl Pts',(70.7758478045576,-7.41245312484498,
0.));
#117282=CARTESIAN_POINT('Ctrl Pts',(70.7758478045576,-7.41245312484498,
12.));
#117283=CARTESIAN_POINT('Ctrl Pts',(70.7554646366514,-7.40337480758237,
0.));
#117284=CARTESIAN_POINT('Ctrl Pts',(70.7554646366514,-7.40337480758237,
12.));
#117285=CARTESIAN_POINT('Ctrl Pts',(70.735114793895,-7.39433604117891,0.));
#117286=CARTESIAN_POINT('Ctrl Pts',(70.735114793895,-7.39433604117891,12.));
#117287=CARTESIAN_POINT('Ctrl Pts',(70.7147984363423,-7.38533681887028,
0.));
#117288=CARTESIAN_POINT('Ctrl Pts',(70.7147984363423,-7.38533681887028,
12.));
#117289=CARTESIAN_POINT('Ctrl Pts',(70.6945157248269,-7.37637713374761,
0.));
#117290=CARTESIAN_POINT('Ctrl Pts',(70.6945157248269,-7.37637713374761,
12.));
#117291=CARTESIAN_POINT('Ctrl Pts',(70.6742668209685,-7.36745697876295,
0.));
#117292=CARTESIAN_POINT('Ctrl Pts',(70.6742668209685,-7.36745697876295,
12.));
#117293=CARTESIAN_POINT('Ctrl Pts',(70.6540518871772,-7.35857634673052,
0.));
#117294=CARTESIAN_POINT('Ctrl Pts',(70.6540518871772,-7.35857634673052,
12.));
#117295=CARTESIAN_POINT('Ctrl Pts',(70.6338710866562,-7.3497352303258,0.));
#117296=CARTESIAN_POINT('Ctrl Pts',(70.6338710866562,-7.3497352303258,12.));
#117297=CARTESIAN_POINT('Ctrl Pts',(70.6137245834002,-7.34093362208018,
0.));
#117298=CARTESIAN_POINT('Ctrl Pts',(70.6137245834002,-7.34093362208018,
12.));
#117299=CARTESIAN_POINT('Ctrl Pts',(70.5936125421958,-7.33217151437608,
0.));
#117300=CARTESIAN_POINT('Ctrl Pts',(70.5936125421958,-7.33217151437608,
12.));
#117301=CARTESIAN_POINT('Ctrl Pts',(70.573535128649,-7.32344889945237,0.));
#117302=CARTESIAN_POINT('Ctrl Pts',(70.573535128649,-7.32344889945237,12.));
#117303=CARTESIAN_POINT('Ctrl Pts',(70.5534925092053,-7.31476576940403,
0.));
#117304=CARTESIAN_POINT('Ctrl Pts',(70.5534925092053,-7.31476576940403,
12.));
#117305=CARTESIAN_POINT('Ctrl Pts',(70.5334848511675,-7.30612211618047,
0.));
#117306=CARTESIAN_POINT('Ctrl Pts',(70.5334848511675,-7.30612211618047,
12.));
#117307=CARTESIAN_POINT('Ctrl Pts',(70.5135123227147,-7.29751793157801,
0.));
#117308=CARTESIAN_POINT('Ctrl Pts',(70.5135123227147,-7.29751793157801,
12.));
#117309=CARTESIAN_POINT('Ctrl Pts',(70.4935750929029,-7.28895320723835,
0.));
#117310=CARTESIAN_POINT('Ctrl Pts',(70.4935750929029,-7.28895320723835,
12.));
#117311=CARTESIAN_POINT('Ctrl Pts',(70.4736733316463,-7.28042793465449,
0.));
#117312=CARTESIAN_POINT('Ctrl Pts',(70.4736733316463,-7.28042793465449,
12.));
#117313=CARTESIAN_POINT('Ctrl Pts',(70.4538072096986,-7.27194210517057,
0.));
#117314=CARTESIAN_POINT('Ctrl Pts',(70.4538072096986,-7.27194210517057,
12.));
#117315=CARTESIAN_POINT('Ctrl Pts',(70.433976898636,-7.2634957099805,0.));
#117316=CARTESIAN_POINT('Ctrl Pts',(70.433976898636,-7.2634957099805,12.));
#117317=CARTESIAN_POINT('Ctrl Pts',(70.4141825708207,-7.25508874012076,
0.));
#117318=CARTESIAN_POINT('Ctrl Pts',(70.4141825708207,-7.25508874012076,
12.));
#117319=CARTESIAN_POINT('Ctrl Pts',(70.3944243994532,-7.24672118647116,
0.));
#117320=CARTESIAN_POINT('Ctrl Pts',(70.3944243994532,-7.24672118647116,
12.));
#117321=CARTESIAN_POINT('Ctrl Pts',(70.3747025586569,-7.23839303975626,
0.));
#117322=CARTESIAN_POINT('Ctrl Pts',(70.3747025586569,-7.23839303975626,
12.));
#117323=CARTESIAN_POINT('Ctrl Pts',(70.3550172235486,-7.23010429054231,
0.));
#117324=CARTESIAN_POINT('Ctrl Pts',(70.3550172235486,-7.23010429054231,
12.));
#117325=CARTESIAN_POINT('Ctrl Pts',(70.3353685703097,-7.22185492923178,
0.));
#117326=CARTESIAN_POINT('Ctrl Pts',(70.3353685703097,-7.22185492923178,
12.));
#117327=CARTESIAN_POINT('Ctrl Pts',(70.3157567762561,-7.21364494605425,
0.));
#117328=CARTESIAN_POINT('Ctrl Pts',(70.3157567762561,-7.21364494605425,
12.));
#117329=CARTESIAN_POINT('Ctrl Pts',(70.2961820197051,-7.20547433107457,
0.));
#117330=CARTESIAN_POINT('Ctrl Pts',(70.2961820197051,-7.20547433107457,
12.));
#117331=CARTESIAN_POINT('Ctrl Pts',(70.276644479827,-7.19734307419861,0.));
#117332=CARTESIAN_POINT('Ctrl Pts',(70.276644479827,-7.19734307419861,12.));
#117333=CARTESIAN_POINT('Ctrl Pts',(70.2571443365198,-7.18925116517562,
0.));
#117334=CARTESIAN_POINT('Ctrl Pts',(70.2571443365198,-7.18925116517562,
12.));
#117335=CARTESIAN_POINT('Ctrl Pts',(70.2376817702239,-7.181198593598,0.));
#117336=CARTESIAN_POINT('Ctrl Pts',(70.2376817702239,-7.181198593598,12.));
#117337=CARTESIAN_POINT('Ctrl Pts',(70.2182569619028,-7.17318534889747,
0.));
#117338=CARTESIAN_POINT('Ctrl Pts',(70.2182569619028,-7.17318534889747,
12.));
#117339=CARTESIAN_POINT('Ctrl Pts',(70.1988700934622,-7.16521142033892,
0.));
#117340=CARTESIAN_POINT('Ctrl Pts',(70.1988700934622,-7.16521142033892,
12.));
#117341=CARTESIAN_POINT('Ctrl Pts',(70.1795213481196,-7.15727679700946,
0.));
#117342=CARTESIAN_POINT('Ctrl Pts',(70.1795213481196,-7.15727679700946,
12.));
#117343=CARTESIAN_POINT('Ctrl Pts',(70.1602109107188,-7.14938146780801,
0.));
#117344=CARTESIAN_POINT('Ctrl Pts',(70.1602109107188,-7.14938146780801,
12.));
#117345=CARTESIAN_POINT('Ctrl Pts',(70.1409389682389,-7.14152542142339,
0.));
#117346=CARTESIAN_POINT('Ctrl Pts',(70.1409389682389,-7.14152542142339,
12.));
#117347=CARTESIAN_POINT('Ctrl Pts',(70.1217057094456,-7.13370864634398,
0.));
#117348=CARTESIAN_POINT('Ctrl Pts',(70.1217057094456,-7.13370864634398,
12.));
#117349=CARTESIAN_POINT('Ctrl Pts',(70.1025113239463,-7.12593113088871,
0.));
#117350=CARTESIAN_POINT('Ctrl Pts',(70.1025113239463,-7.12593113088871,
12.));
#117351=CARTESIAN_POINT('Ctrl Pts',(70.0833560013971,-7.11819286322824,
0.));
#117352=CARTESIAN_POINT('Ctrl Pts',(70.0833560013971,-7.11819286322824,
12.));
#117353=CARTESIAN_POINT('Ctrl Pts',(70.06423993069,-7.11049383140482,0.));
#117354=CARTESIAN_POINT('Ctrl Pts',(70.06423993069,-7.11049383140482,12.));
#117355=CARTESIAN_POINT('Ctrl Pts',(70.0451632990137,-7.10283402335091,
0.));
#117356=CARTESIAN_POINT('Ctrl Pts',(70.0451632990137,-7.10283402335091,
12.));
#117357=CARTESIAN_POINT('Ctrl Pts',(70.0261262936435,-7.09521342684301,
0.));
#117358=CARTESIAN_POINT('Ctrl Pts',(70.0261262936435,-7.09521342684301,
12.));
#117359=CARTESIAN_POINT('Ctrl Pts',(70.0071291040791,-7.08763202944274,
0.));
#117360=CARTESIAN_POINT('Ctrl Pts',(70.0071291040791,-7.08763202944274,
12.));
#117361=CARTESIAN_POINT('Ctrl Pts',(69.988171923787,-7.08008981844643,0.));
#117362=CARTESIAN_POINT('Ctrl Pts',(69.988171923787,-7.08008981844643,12.));
#117363=CARTESIAN_POINT('Ctrl Pts',(69.9692549527256,-7.07258678080793,
0.));
#117364=CARTESIAN_POINT('Ctrl Pts',(69.9692549527256,-7.07258678080793,
12.));
#117365=CARTESIAN_POINT('Ctrl Pts',(69.9503783975676,-7.06512290312803,
0.));
#117366=CARTESIAN_POINT('Ctrl Pts',(69.9503783975676,-7.06512290312803,
12.));
#117367=CARTESIAN_POINT('Ctrl Pts',(69.9315424664252,-7.05769817180824,
0.));
#117368=CARTESIAN_POINT('Ctrl Pts',(69.9315424664252,-7.05769817180824,
12.));
#117369=CARTESIAN_POINT('Ctrl Pts',(69.9127473642087,-7.05031257318108,
0.));
#117370=CARTESIAN_POINT('Ctrl Pts',(69.9127473642087,-7.05031257318108,
12.));
#117371=CARTESIAN_POINT('Ctrl Pts',(69.8939932885864,-7.04296609362187,
0.));
#117372=CARTESIAN_POINT('Ctrl Pts',(69.8939932885864,-7.04296609362187,
12.));
#117373=CARTESIAN_POINT('Ctrl Pts',(69.8752804235296,-7.03565871972265,
0.));
#117374=CARTESIAN_POINT('Ctrl Pts',(69.8752804235296,-7.03565871972265,
12.));
#117375=CARTESIAN_POINT('Ctrl Pts',(69.8566089455448,-7.02839043811863,
0.));
#117376=CARTESIAN_POINT('Ctrl Pts',(69.8566089455448,-7.02839043811863,
12.));
#117377=CARTESIAN_POINT('Ctrl Pts',(69.8379790360574,-7.02116123514487,
0.));
#117378=CARTESIAN_POINT('Ctrl Pts',(69.8379790360574,-7.02116123514487,
12.));
#117379=CARTESIAN_POINT('Ctrl Pts',(69.8193908913722,-7.01397109655455,
0.));
#117380=CARTESIAN_POINT('Ctrl Pts',(69.8193908913722,-7.01397109655455,
12.));
#117381=CARTESIAN_POINT('Ctrl Pts',(69.8008447346782,-7.00682000718105,
0.));
#117382=CARTESIAN_POINT('Ctrl Pts',(69.8008447346782,-7.00682000718105,
12.));
#117383=CARTESIAN_POINT('Ctrl Pts',(69.7823408242446,-6.99970795069399,
0.));
#117384=CARTESIAN_POINT('Ctrl Pts',(69.7823408242446,-6.99970795069399,
12.));
#117385=CARTESIAN_POINT('Ctrl Pts',(69.7638794280263,-6.9926349102786,0.));
#117386=CARTESIAN_POINT('Ctrl Pts',(69.7638794280263,-6.9926349102786,12.));
#117387=CARTESIAN_POINT('Ctrl Pts',(69.7454607995524,-6.98560086924173,
0.));
#117388=CARTESIAN_POINT('Ctrl Pts',(69.7454607995524,-6.98560086924173,
12.));
#117389=CARTESIAN_POINT('Ctrl Pts',(69.7270851557443,-6.97860581164569,
0.));
#117390=CARTESIAN_POINT('Ctrl Pts',(69.7270851557443,-6.97860581164569,
12.));
#117391=CARTESIAN_POINT('Ctrl Pts',(69.7087526480249,-6.97164972291582,
0.));
#117392=CARTESIAN_POINT('Ctrl Pts',(69.7087526480249,-6.97164972291582,
12.));
#117393=CARTESIAN_POINT('Ctrl Pts',(69.6904633605834,-6.96473259049729,
0.));
#117394=CARTESIAN_POINT('Ctrl Pts',(69.6904633605834,-6.96473259049729,
12.));
#117395=CARTESIAN_POINT('Ctrl Pts',(69.6758665380764,-6.95923004173795,
0.));
#117396=CARTESIAN_POINT('Ctrl Pts',(69.6758665380764,-6.95923004173795,
12.));
#117397=CARTESIAN_POINT('Ctrl Pts',(69.6649383920075,-6.95512065317731,
0.));
#117398=CARTESIAN_POINT('Ctrl Pts',(69.6649383920075,-6.95512065317731,
12.));
#117399=CARTESIAN_POINT('Ctrl Pts',(69.6576616146559,-6.95238884849075,
0.));
#117400=CARTESIAN_POINT('Ctrl Pts',(69.6576616146559,-6.95238884849075,
12.));
#117401=CARTESIAN_POINT('Ctrl Pts',(69.6540253893193,-6.95102489306927,
0.));
#117402=CARTESIAN_POINT('Ctrl Pts',(69.6540253893193,-6.95102489306927,
12.));
#117403=CARTESIAN_POINT('',(69.6540253893193,-6.95102489306927,12.));
#117404=CARTESIAN_POINT('Ctrl Pts',(69.6540253893193,-6.95102489306927,
12.));
#117405=CARTESIAN_POINT('Ctrl Pts',(69.6576616146559,-6.95238884849075,
12.));
#117406=CARTESIAN_POINT('Ctrl Pts',(69.6649383920075,-6.95512065317731,
12.));
#117407=CARTESIAN_POINT('Ctrl Pts',(69.6758665380764,-6.95923004173795,
12.));
#117408=CARTESIAN_POINT('Ctrl Pts',(69.6904633605834,-6.96473259049729,
12.));
#117409=CARTESIAN_POINT('Ctrl Pts',(69.7087526480249,-6.97164972291582,
12.));
#117410=CARTESIAN_POINT('Ctrl Pts',(69.7270851557443,-6.97860581164569,
12.));
#117411=CARTESIAN_POINT('Ctrl Pts',(69.7454607995524,-6.98560086924173,
12.));
#117412=CARTESIAN_POINT('Ctrl Pts',(69.7638794280263,-6.9926349102786,12.));
#117413=CARTESIAN_POINT('Ctrl Pts',(69.7823408242446,-6.99970795069399,
12.));
#117414=CARTESIAN_POINT('Ctrl Pts',(69.8008447346782,-7.00682000718105,
12.));
#117415=CARTESIAN_POINT('Ctrl Pts',(69.8193908913722,-7.01397109655455,
12.));
#117416=CARTESIAN_POINT('Ctrl Pts',(69.8379790360574,-7.02116123514487,
12.));
#117417=CARTESIAN_POINT('Ctrl Pts',(69.8566089455448,-7.02839043811863,
12.));
#117418=CARTESIAN_POINT('Ctrl Pts',(69.8752804235296,-7.03565871972265,
12.));
#117419=CARTESIAN_POINT('Ctrl Pts',(69.8939932885864,-7.04296609362187,
12.));
#117420=CARTESIAN_POINT('Ctrl Pts',(69.9127473642087,-7.05031257318108,
12.));
#117421=CARTESIAN_POINT('Ctrl Pts',(69.9315424664252,-7.05769817180824,
12.));
#117422=CARTESIAN_POINT('Ctrl Pts',(69.9503783975676,-7.06512290312803,
12.));
#117423=CARTESIAN_POINT('Ctrl Pts',(69.9692549527256,-7.07258678080793,
12.));
#117424=CARTESIAN_POINT('Ctrl Pts',(69.988171923787,-7.08008981844643,12.));
#117425=CARTESIAN_POINT('Ctrl Pts',(70.0071291040791,-7.08763202944274,
12.));
#117426=CARTESIAN_POINT('Ctrl Pts',(70.0261262936435,-7.09521342684301,
12.));
#117427=CARTESIAN_POINT('Ctrl Pts',(70.0451632990137,-7.10283402335091,
12.));
#117428=CARTESIAN_POINT('Ctrl Pts',(70.06423993069,-7.11049383140482,12.));
#117429=CARTESIAN_POINT('Ctrl Pts',(70.0833560013971,-7.11819286322824,
12.));
#117430=CARTESIAN_POINT('Ctrl Pts',(70.1025113239463,-7.12593113088871,
12.));
#117431=CARTESIAN_POINT('Ctrl Pts',(70.1217057094456,-7.13370864634398,
12.));
#117432=CARTESIAN_POINT('Ctrl Pts',(70.1409389682389,-7.14152542142339,
12.));
#117433=CARTESIAN_POINT('Ctrl Pts',(70.1602109107188,-7.14938146780801,
12.));
#117434=CARTESIAN_POINT('Ctrl Pts',(70.1795213481196,-7.15727679700946,
12.));
#117435=CARTESIAN_POINT('Ctrl Pts',(70.1988700934622,-7.16521142033892,
12.));
#117436=CARTESIAN_POINT('Ctrl Pts',(70.2182569619028,-7.17318534889747,
12.));
#117437=CARTESIAN_POINT('Ctrl Pts',(70.2376817702239,-7.181198593598,12.));
#117438=CARTESIAN_POINT('Ctrl Pts',(70.2571443365198,-7.18925116517562,
12.));
#117439=CARTESIAN_POINT('Ctrl Pts',(70.276644479827,-7.19734307419861,12.));
#117440=CARTESIAN_POINT('Ctrl Pts',(70.2961820197051,-7.20547433107457,
12.));
#117441=CARTESIAN_POINT('Ctrl Pts',(70.3157567762561,-7.21364494605425,
12.));
#117442=CARTESIAN_POINT('Ctrl Pts',(70.3353685703097,-7.22185492923178,
12.));
#117443=CARTESIAN_POINT('Ctrl Pts',(70.3550172235486,-7.23010429054231,
12.));
#117444=CARTESIAN_POINT('Ctrl Pts',(70.3747025586569,-7.23839303975626,
12.));
#117445=CARTESIAN_POINT('Ctrl Pts',(70.3944243994532,-7.24672118647116,
12.));
#117446=CARTESIAN_POINT('Ctrl Pts',(70.4141825708207,-7.25508874012076,
12.));
#117447=CARTESIAN_POINT('Ctrl Pts',(70.433976898636,-7.2634957099805,12.));
#117448=CARTESIAN_POINT('Ctrl Pts',(70.4538072096986,-7.27194210517057,
12.));
#117449=CARTESIAN_POINT('Ctrl Pts',(70.4736733316463,-7.28042793465449,
12.));
#117450=CARTESIAN_POINT('Ctrl Pts',(70.4935750929029,-7.28895320723835,
12.));
#117451=CARTESIAN_POINT('Ctrl Pts',(70.5135123227147,-7.29751793157801,
12.));
#117452=CARTESIAN_POINT('Ctrl Pts',(70.5334848511675,-7.30612211618047,
12.));
#117453=CARTESIAN_POINT('Ctrl Pts',(70.5534925092053,-7.31476576940403,
12.));
#117454=CARTESIAN_POINT('Ctrl Pts',(70.573535128649,-7.32344889945237,12.));
#117455=CARTESIAN_POINT('Ctrl Pts',(70.5936125421958,-7.33217151437608,
12.));
#117456=CARTESIAN_POINT('Ctrl Pts',(70.6137245834002,-7.34093362208018,
12.));
#117457=CARTESIAN_POINT('Ctrl Pts',(70.6338710866562,-7.3497352303258,12.));
#117458=CARTESIAN_POINT('Ctrl Pts',(70.6540518871772,-7.35857634673052,
12.));
#117459=CARTESIAN_POINT('Ctrl Pts',(70.6742668209685,-7.36745697876295,
12.));
#117460=CARTESIAN_POINT('Ctrl Pts',(70.6945157248269,-7.37637713374761,
12.));
#117461=CARTESIAN_POINT('Ctrl Pts',(70.7147984363423,-7.38533681887028,
12.));
#117462=CARTESIAN_POINT('Ctrl Pts',(70.735114793895,-7.39433604117891,12.));
#117463=CARTESIAN_POINT('Ctrl Pts',(70.7554646366514,-7.40337480758237,
12.));
#117464=CARTESIAN_POINT('Ctrl Pts',(70.7758478045576,-7.41245312484498,
12.));
#117465=CARTESIAN_POINT('Ctrl Pts',(70.796264138335,-7.42157099959326,12.));
#117466=CARTESIAN_POINT('Ctrl Pts',(70.8167134794737,-7.43072843832014,
12.));
#117467=CARTESIAN_POINT('Ctrl Pts',(70.8371956702241,-7.43992544738606,
12.));
#117468=CARTESIAN_POINT('Ctrl Pts',(70.8577105535848,-7.44916203301647,
12.));
#117469=CARTESIAN_POINT('Ctrl Pts',(70.87825797329,-7.45843820129782,12.));
#117470=CARTESIAN_POINT('Ctrl Pts',(70.8988377738104,-7.46775395818527,
12.));
#117471=CARTESIAN_POINT('Ctrl Pts',(70.9194498003493,-7.47710930950562,
12.));
#117472=CARTESIAN_POINT('Ctrl Pts',(70.940093898837,-7.48650426095824,12.));
#117473=CARTESIAN_POINT('Ctrl Pts',(70.9607699159218,-7.4959388181113,12.));
#117474=CARTESIAN_POINT('Ctrl Pts',(70.9814776989612,-7.50541298639928,
12.));
#117475=CARTESIAN_POINT('Ctrl Pts',(71.002217096021,-7.5149267711309,12.));
#117476=CARTESIAN_POINT('Ctrl Pts',(71.0229879558699,-7.52448017749125,
12.));
#117477=CARTESIAN_POINT('Ctrl Pts',(71.043790127973,-7.53407321054262,12.));
#117478=CARTESIAN_POINT('Ctrl Pts',(71.0646234624811,-7.54370587521979,
12.));
#117479=CARTESIAN_POINT('Ctrl Pts',(71.0854878102243,-7.55337817632916,
12.));
#117480=CARTESIAN_POINT('Ctrl Pts',(71.106383022711,-7.56309011855657,12.));
#117481=CARTESIAN_POINT('Ctrl Pts',(71.1273089521234,-7.57284170646886,
12.));
#117482=CARTESIAN_POINT('Ctrl Pts',(71.1482654513119,-7.58263294451452,
12.));
#117483=CARTESIAN_POINT('Ctrl Pts',(71.1692523737844,-7.59246383701814,
12.));
#117484=CARTESIAN_POINT('Ctrl Pts',(71.1902695737013,-7.60233438818096,
12.));
#117485=CARTESIAN_POINT('Ctrl Pts',(71.211316905874,-7.61224460208837,12.));
#117486=CARTESIAN_POINT('Ctrl Pts',(71.2323942257609,-7.62219448271109,
12.));
#117487=CARTESIAN_POINT('Ctrl Pts',(71.2535013894602,-7.63218403390537,
12.));
#117488=CARTESIAN_POINT('Ctrl Pts',(71.2746382537007,-7.64221325940724,
12.));
#117489=CARTESIAN_POINT('Ctrl Pts',(71.2958046758372,-7.65228216283404,
12.));
#117490=CARTESIAN_POINT('Ctrl Pts',(71.3170005138502,-7.66239074769163,
12.));
#117491=CARTESIAN_POINT('Ctrl Pts',(71.3382256263414,-7.67253901737552,
12.));
#117492=CARTESIAN_POINT('Ctrl Pts',(71.3594798725281,-7.68272697517086,
12.));
#117493=CARTESIAN_POINT('Ctrl Pts',(71.3807631122331,-7.69295462424612,
12.));
#117494=CARTESIAN_POINT('Ctrl Pts',(71.4020752058796,-7.70322196765538,
12.));
#117495=CARTESIAN_POINT('Ctrl Pts',(71.4234160144925,-7.7135290083452,12.));
#117496=CARTESIAN_POINT('Ctrl Pts',(71.4447853996916,-7.72387574915544,
12.));
#117497=CARTESIAN_POINT('Ctrl Pts',(71.4661832236888,-7.7342621928194,12.));
#117498=CARTESIAN_POINT('Ctrl Pts',(71.4876093492781,-7.74468834195746,
12.));
#117499=CARTESIAN_POINT('Ctrl Pts',(71.5090636398318,-7.75515419907966,
12.));
#117500=CARTESIAN_POINT('Ctrl Pts',(71.5305459592994,-7.76565976659226,
12.));
#117501=CARTESIAN_POINT('Ctrl Pts',(71.5520561722039,-7.77620504679869,
12.));
#117502=CARTESIAN_POINT('Ctrl Pts',(71.5735941436364,-7.78679004189935,
12.));
#117503=CARTESIAN_POINT('Ctrl Pts',(71.5951597392471,-7.79741475398513,
12.));
#117504=CARTESIAN_POINT('Ctrl Pts',(71.6167528252423,-7.80807918504021,
12.));
#117505=CARTESIAN_POINT('Ctrl Pts',(71.6383732683844,-7.8187833369486,12.));
#117506=CARTESIAN_POINT('Ctrl Pts',(71.6600209359872,-7.82952721149507,
12.));
#117507=CARTESIAN_POINT('Ctrl Pts',(71.6816956959117,-7.84031081036489,
12.));
#117508=CARTESIAN_POINT('Ctrl Pts',(71.7033974165568,-7.85113413513736,
12.));
#117509=CARTESIAN_POINT('Ctrl Pts',(71.7251259668563,-7.86199718728826,
12.));
#117510=CARTESIAN_POINT('Ctrl Pts',(71.7468812162788,-7.87289996819653,
12.));
#117511=CARTESIAN_POINT('Ctrl Pts',(71.7686630348238,-7.88384247914524,
12.));
#117512=CARTESIAN_POINT('Ctrl Pts',(71.7904712930175,-7.89482472132137,
12.));
#117513=CARTESIAN_POINT('Ctrl Pts',(71.8123058619042,-7.90584669580955,
12.));
#117514=CARTESIAN_POINT('Ctrl Pts',(71.8341666130426,-7.91690840359367,
12.));
#117515=CARTESIAN_POINT('Ctrl Pts',(71.8560534185071,-7.92800984556396,
12.));
#117516=CARTESIAN_POINT('Ctrl Pts',(71.8779661508832,-7.93915102251794,
12.));
#117517=CARTESIAN_POINT('Ctrl Pts',(71.8999046832643,-7.9503319351605,12.));
#117518=CARTESIAN_POINT('Ctrl Pts',(71.9218688892431,-7.96155258409763,
12.));
#117519=CARTESIAN_POINT('Ctrl Pts',(71.9438586429081,-7.97281296983718,
12.));
#117520=CARTESIAN_POINT('Ctrl Pts',(71.965873818843,-7.98411309279612,12.));
#117521=CARTESIAN_POINT('Ctrl Pts',(71.9879142921254,-7.99545295330191,
12.));
#117522=CARTESIAN_POINT('Ctrl Pts',(72.0099799383213,-8.00683255159247,
12.));
#117523=CARTESIAN_POINT('Ctrl Pts',(72.032070633479,-8.01825188781056,12.));
#117524=CARTESIAN_POINT('Ctrl Pts',(72.0541862541243,-8.02971096200307,
12.));
#117525=CARTESIAN_POINT('Ctrl Pts',(72.0763266772615,-8.04120977412872,
12.));
#117526=CARTESIAN_POINT('Ctrl Pts',(72.0984917803693,-8.05274832405948,
12.));
#117527=CARTESIAN_POINT('Ctrl Pts',(72.1206814413988,-8.06432661158096,
12.));
#117528=CARTESIAN_POINT('Ctrl Pts',(72.1428955387663,-8.07594463638719,
12.));
#117529=CARTESIAN_POINT('Ctrl Pts',(72.1651339513477,-8.08760239807836,
12.));
#117530=CARTESIAN_POINT('Ctrl Pts',(72.1873965584813,-8.0992998961689,12.));
#117531=CARTESIAN_POINT('Ctrl Pts',(72.209683239963,-8.11103713008928,12.));
#117532=CARTESIAN_POINT('Ctrl Pts',(72.2319938760449,-8.12281409918661,
12.));
#117533=CARTESIAN_POINT('Ctrl Pts',(72.2543283474278,-8.13463080272029,
12.));
#117534=CARTESIAN_POINT('Ctrl Pts',(72.2766865352555,-8.14648723985797,
12.));
#117535=CARTESIAN_POINT('Ctrl Pts',(72.2990683211162,-8.15838340968336,
12.));
#117536=CARTESIAN_POINT('Ctrl Pts',(72.3214735870409,-8.1703193111989,12.));
#117537=CARTESIAN_POINT('Ctrl Pts',(72.3439022155007,-8.18229494332624,
12.));
#117538=CARTESIAN_POINT('Ctrl Pts',(72.3663540894026,-8.19431030490314,
12.));
#117539=CARTESIAN_POINT('Ctrl Pts',(72.3888290920832,-8.20636539467776,
12.));
#117540=CARTESIAN_POINT('Ctrl Pts',(72.4113271073079,-8.21846021131561,
12.));
#117541=CARTESIAN_POINT('Ctrl Pts',(72.4338480192695,-8.23059475340357,
12.));
#117542=CARTESIAN_POINT('Ctrl Pts',(72.4563917125842,-8.2427690194504,12.));
#117543=CARTESIAN_POINT('Ctrl Pts',(72.4789580722875,-8.25498300788493,
12.));
#117544=CARTESIAN_POINT('Ctrl Pts',(72.5015469838254,-8.2672367170492,12.));
#117545=CARTESIAN_POINT('Ctrl Pts',(72.5241583330562,-8.27953014520376,
12.));
#117546=CARTESIAN_POINT('Ctrl Pts',(72.5467920062521,-8.29186329053279,
12.));
#117547=CARTESIAN_POINT('Ctrl Pts',(72.5694478900982,-8.30423615114453,
12.));
#117548=CARTESIAN_POINT('Ctrl Pts',(72.5921258716901,-8.31664872507016,
12.));
#117549=CARTESIAN_POINT('Ctrl Pts',(72.6148258385296,-8.3291010102567,12.));
#117550=CARTESIAN_POINT('Ctrl Pts',(72.6375476785215,-8.34159300456986,
12.));
#117551=CARTESIAN_POINT('Ctrl Pts',(72.6602912799696,-8.35412470580101,
12.));
#117552=CARTESIAN_POINT('Ctrl Pts',(72.6830565315703,-8.36669611166842,
12.));
#117553=CARTESIAN_POINT('Ctrl Pts',(72.705843322407,-8.37930721981731,12.));
#117554=CARTESIAN_POINT('Ctrl Pts',(72.7286515419373,-8.3919580278139,12.));
#117555=CARTESIAN_POINT('Ctrl Pts',(72.751481079992,-8.40464853314468,12.));
#117556=CARTESIAN_POINT('Ctrl Pts',(72.7743318267865,-8.4173787332233,12.));
#117557=CARTESIAN_POINT('Ctrl Pts',(72.7972036729276,-8.43014862539158,
12.));
#117558=CARTESIAN_POINT('Ctrl Pts',(72.8200965094199,-8.44295820691911,
12.));
#117559=CARTESIAN_POINT('Ctrl Pts',(72.8430102276713,-8.45580747499793,
12.));
#117560=CARTESIAN_POINT('Ctrl Pts',(72.8659447194933,-8.46869642673794,
12.));
#117561=CARTESIAN_POINT('Ctrl Pts',(72.8888998770785,-8.48162505917658,
12.));
#117562=CARTESIAN_POINT('Ctrl Pts',(72.9118755929795,-8.49459336928296,
12.));
#117563=CARTESIAN_POINT('Ctrl Pts',(72.9348717600838,-8.50760135395983,
12.));
#117564=CARTESIAN_POINT('Ctrl Pts',(72.9578882715912,-8.52064901004227,
12.));
#117565=CARTESIAN_POINT('Ctrl Pts',(72.9809250209828,-8.53373633429281,
12.));
#117566=CARTESIAN_POINT('Ctrl Pts',(73.0039819020648,-8.54686332340418,
12.));
#117567=CARTESIAN_POINT('Ctrl Pts',(73.0270588090183,-8.56002997400084,
12.));
#117568=CARTESIAN_POINT('Ctrl Pts',(73.0501556364479,-8.57323628263593,
12.));
#117569=CARTESIAN_POINT('Ctrl Pts',(73.0732722794195,-8.58648224578731,
12.));
#117570=CARTESIAN_POINT('Ctrl Pts',(73.0964086335235,-8.59976785984551,
12.));
#117571=CARTESIAN_POINT('Ctrl Pts',(73.1195645948178,-8.61309312112002,
12.));
#117572=CARTESIAN_POINT('Ctrl Pts',(73.1427400597037,-8.62645802585484,
12.));
#117573=CARTESIAN_POINT('Ctrl Pts',(73.1659349248132,-8.63986257023739,
12.));
#117574=CARTESIAN_POINT('Ctrl Pts',(73.1891490869056,-8.65330675040537,
12.));
#117575=CARTESIAN_POINT('Ctrl Pts',(73.2123824427208,-8.66679056245092,
12.));
#117576=CARTESIAN_POINT('Ctrl Pts',(73.2356348889693,-8.68031400241872,
12.));
#117577=CARTESIAN_POINT('Ctrl Pts',(73.2589063226358,-8.69387706629285,
12.));
#117578=CARTESIAN_POINT('Ctrl Pts',(73.2821966412148,-8.70747974998229,
12.));
#117579=CARTESIAN_POINT('Ctrl Pts',(73.3055057429742,-8.72112204930232,
12.));
#117580=CARTESIAN_POINT('Ctrl Pts',(73.3288335272002,-8.7348039599538,12.));
#117581=CARTESIAN_POINT('Ctrl Pts',(73.3521798944622,-8.74852547749778,
12.));
#117582=CARTESIAN_POINT('Ctrl Pts',(73.3755447460269,-8.76228659740357,
12.));
#117583=CARTESIAN_POINT('Ctrl Pts',(73.3989279832835,-8.77608731509348,
12.));
#117584=CARTESIAN_POINT('Ctrl Pts',(73.422329507113,-8.78992762598756,12.));
#117585=CARTESIAN_POINT('Ctrl Pts',(73.4457492173933,-8.80380752553692,
12.));
#117586=CARTESIAN_POINT('Ctrl Pts',(73.4691870121567,-8.8177270092753,12.));
#117587=CARTESIAN_POINT('Ctrl Pts',(73.492642788273,-8.83168607277325,12.));
#117588=CARTESIAN_POINT('Ctrl Pts',(73.5161164429709,-8.84568471153805,
12.));
#117589=CARTESIAN_POINT('Ctrl Pts',(73.5396078751639,-8.8597229209213,12.));
#117590=CARTESIAN_POINT('Ctrl Pts',(73.5631169867122,-8.8738006960297,12.));
#117591=CARTESIAN_POINT('Ctrl Pts',(73.5866436840556,-8.88791803160442,
12.));
#117592=CARTESIAN_POINT('Ctrl Pts',(73.6101878785976,-8.90207492199043,
12.));
#117593=CARTESIAN_POINT('Ctrl Pts',(73.630384739363,-8.91424402151603,12.));
#117594=CARTESIAN_POINT('Ctrl Pts',(73.6458786306025,-8.923595181785,12.));
#117595=CARTESIAN_POINT('Ctrl Pts',(73.6566618622077,-8.9301108881733,12.));
#117596=CARTESIAN_POINT('Ctrl Pts',(73.6627293782591,-8.93377955965654,
12.));
#117597=CARTESIAN_POINT('Ctrl Pts',(73.664078719806,-8.93459554657865,12.));
#117598=CARTESIAN_POINT('',(69.6540253893193,-6.95102489306927,0.));
#117599=CARTESIAN_POINT('',(69.6540253893193,-6.95102489306927,0.));
#117600=CARTESIAN_POINT('Ctrl Pts',(73.6640787198059,-8.93459554657863,
0.));
#117601=CARTESIAN_POINT('Ctrl Pts',(73.6627293782591,-8.93377955965652,
0.));
#117602=CARTESIAN_POINT('Ctrl Pts',(73.6566618622076,-8.93011088817329,
0.));
#117603=CARTESIAN_POINT('Ctrl Pts',(73.6458786306025,-8.92359518178499,
0.));
#117604=CARTESIAN_POINT('Ctrl Pts',(73.630384739363,-8.91424402151603,0.));
#117605=CARTESIAN_POINT('Ctrl Pts',(73.6101878785976,-8.90207492199043,
0.));
#117606=CARTESIAN_POINT('Ctrl Pts',(73.5866436840556,-8.88791803160442,
0.));
#117607=CARTESIAN_POINT('Ctrl Pts',(73.5631169867122,-8.8738006960297,0.));
#117608=CARTESIAN_POINT('Ctrl Pts',(73.5396078751639,-8.8597229209213,0.));
#117609=CARTESIAN_POINT('Ctrl Pts',(73.5161164429709,-8.84568471153805,
0.));
#117610=CARTESIAN_POINT('Ctrl Pts',(73.492642788273,-8.83168607277325,0.));
#117611=CARTESIAN_POINT('Ctrl Pts',(73.4691870121567,-8.8177270092753,0.));
#117612=CARTESIAN_POINT('Ctrl Pts',(73.4457492173933,-8.80380752553692,
0.));
#117613=CARTESIAN_POINT('Ctrl Pts',(73.422329507113,-8.78992762598756,0.));
#117614=CARTESIAN_POINT('Ctrl Pts',(73.3989279832835,-8.77608731509348,
0.));
#117615=CARTESIAN_POINT('Ctrl Pts',(73.3755447460269,-8.76228659740357,
0.));
#117616=CARTESIAN_POINT('Ctrl Pts',(73.3521798944622,-8.74852547749778,
0.));
#117617=CARTESIAN_POINT('Ctrl Pts',(73.3288335272002,-8.7348039599538,0.));
#117618=CARTESIAN_POINT('Ctrl Pts',(73.3055057429742,-8.72112204930232,
0.));
#117619=CARTESIAN_POINT('Ctrl Pts',(73.2821966412148,-8.70747974998229,
0.));
#117620=CARTESIAN_POINT('Ctrl Pts',(73.2589063226358,-8.69387706629285,
0.));
#117621=CARTESIAN_POINT('Ctrl Pts',(73.2356348889693,-8.68031400241872,
0.));
#117622=CARTESIAN_POINT('Ctrl Pts',(73.2123824427208,-8.66679056245092,
0.));
#117623=CARTESIAN_POINT('Ctrl Pts',(73.1891490869056,-8.65330675040537,
0.));
#117624=CARTESIAN_POINT('Ctrl Pts',(73.1659349248132,-8.63986257023739,
0.));
#117625=CARTESIAN_POINT('Ctrl Pts',(73.1427400597037,-8.62645802585484,
0.));
#117626=CARTESIAN_POINT('Ctrl Pts',(73.1195645948178,-8.61309312112002,
0.));
#117627=CARTESIAN_POINT('Ctrl Pts',(73.0964086335235,-8.59976785984551,
0.));
#117628=CARTESIAN_POINT('Ctrl Pts',(73.0732722794195,-8.58648224578731,
0.));
#117629=CARTESIAN_POINT('Ctrl Pts',(73.0501556364479,-8.57323628263593,
0.));
#117630=CARTESIAN_POINT('Ctrl Pts',(73.0270588090183,-8.56002997400084,
0.));
#117631=CARTESIAN_POINT('Ctrl Pts',(73.0039819020648,-8.54686332340418,
0.));
#117632=CARTESIAN_POINT('Ctrl Pts',(72.9809250209828,-8.53373633429281,
0.));
#117633=CARTESIAN_POINT('Ctrl Pts',(72.9578882715912,-8.52064901004227,
0.));
#117634=CARTESIAN_POINT('Ctrl Pts',(72.9348717600838,-8.50760135395983,
0.));
#117635=CARTESIAN_POINT('Ctrl Pts',(72.9118755929795,-8.49459336928296,
0.));
#117636=CARTESIAN_POINT('Ctrl Pts',(72.8888998770785,-8.48162505917658,
0.));
#117637=CARTESIAN_POINT('Ctrl Pts',(72.8659447194933,-8.46869642673794,
0.));
#117638=CARTESIAN_POINT('Ctrl Pts',(72.8430102276713,-8.45580747499793,
0.));
#117639=CARTESIAN_POINT('Ctrl Pts',(72.8200965094199,-8.44295820691911,
0.));
#117640=CARTESIAN_POINT('Ctrl Pts',(72.7972036729276,-8.43014862539158,
0.));
#117641=CARTESIAN_POINT('Ctrl Pts',(72.7743318267865,-8.4173787332233,0.));
#117642=CARTESIAN_POINT('Ctrl Pts',(72.751481079992,-8.40464853314468,0.));
#117643=CARTESIAN_POINT('Ctrl Pts',(72.7286515419373,-8.3919580278139,0.));
#117644=CARTESIAN_POINT('Ctrl Pts',(72.705843322407,-8.37930721981731,0.));
#117645=CARTESIAN_POINT('Ctrl Pts',(72.6830565315703,-8.36669611166842,
0.));
#117646=CARTESIAN_POINT('Ctrl Pts',(72.6602912799696,-8.35412470580101,
0.));
#117647=CARTESIAN_POINT('Ctrl Pts',(72.6375476785215,-8.34159300456986,
0.));
#117648=CARTESIAN_POINT('Ctrl Pts',(72.6148258385296,-8.3291010102567,0.));
#117649=CARTESIAN_POINT('Ctrl Pts',(72.5921258716901,-8.31664872507016,
0.));
#117650=CARTESIAN_POINT('Ctrl Pts',(72.5694478900982,-8.30423615114453,
0.));
#117651=CARTESIAN_POINT('Ctrl Pts',(72.5467920062521,-8.29186329053279,
0.));
#117652=CARTESIAN_POINT('Ctrl Pts',(72.5241583330562,-8.27953014520376,
0.));
#117653=CARTESIAN_POINT('Ctrl Pts',(72.5015469838254,-8.2672367170492,0.));
#117654=CARTESIAN_POINT('Ctrl Pts',(72.4789580722875,-8.25498300788493,
0.));
#117655=CARTESIAN_POINT('Ctrl Pts',(72.4563917125842,-8.2427690194504,0.));
#117656=CARTESIAN_POINT('Ctrl Pts',(72.4338480192695,-8.23059475340357,
0.));
#117657=CARTESIAN_POINT('Ctrl Pts',(72.4113271073079,-8.21846021131561,
0.));
#117658=CARTESIAN_POINT('Ctrl Pts',(72.3888290920832,-8.20636539467776,
0.));
#117659=CARTESIAN_POINT('Ctrl Pts',(72.3663540894026,-8.19431030490314,
0.));
#117660=CARTESIAN_POINT('Ctrl Pts',(72.3439022155007,-8.18229494332624,
0.));
#117661=CARTESIAN_POINT('Ctrl Pts',(72.3214735870409,-8.1703193111989,0.));
#117662=CARTESIAN_POINT('Ctrl Pts',(72.2990683211162,-8.15838340968336,
0.));
#117663=CARTESIAN_POINT('Ctrl Pts',(72.2766865352555,-8.14648723985797,
0.));
#117664=CARTESIAN_POINT('Ctrl Pts',(72.2543283474278,-8.13463080272029,
0.));
#117665=CARTESIAN_POINT('Ctrl Pts',(72.2319938760449,-8.12281409918661,
0.));
#117666=CARTESIAN_POINT('Ctrl Pts',(72.209683239963,-8.11103713008928,0.));
#117667=CARTESIAN_POINT('Ctrl Pts',(72.1873965584813,-8.0992998961689,0.));
#117668=CARTESIAN_POINT('Ctrl Pts',(72.1651339513477,-8.08760239807836,
0.));
#117669=CARTESIAN_POINT('Ctrl Pts',(72.1428955387663,-8.07594463638719,
0.));
#117670=CARTESIAN_POINT('Ctrl Pts',(72.1206814413988,-8.06432661158096,
0.));
#117671=CARTESIAN_POINT('Ctrl Pts',(72.0984917803693,-8.05274832405948,
0.));
#117672=CARTESIAN_POINT('Ctrl Pts',(72.0763266772615,-8.04120977412872,
0.));
#117673=CARTESIAN_POINT('Ctrl Pts',(72.0541862541243,-8.02971096200307,
0.));
#117674=CARTESIAN_POINT('Ctrl Pts',(72.032070633479,-8.01825188781056,0.));
#117675=CARTESIAN_POINT('Ctrl Pts',(72.0099799383213,-8.00683255159247,
0.));
#117676=CARTESIAN_POINT('Ctrl Pts',(71.9879142921254,-7.99545295330191,
0.));
#117677=CARTESIAN_POINT('Ctrl Pts',(71.965873818843,-7.98411309279612,0.));
#117678=CARTESIAN_POINT('Ctrl Pts',(71.9438586429081,-7.97281296983718,
0.));
#117679=CARTESIAN_POINT('Ctrl Pts',(71.9218688892431,-7.96155258409763,
0.));
#117680=CARTESIAN_POINT('Ctrl Pts',(71.8999046832643,-7.9503319351605,0.));
#117681=CARTESIAN_POINT('Ctrl Pts',(71.8779661508832,-7.93915102251794,
0.));
#117682=CARTESIAN_POINT('Ctrl Pts',(71.8560534185071,-7.92800984556396,
0.));
#117683=CARTESIAN_POINT('Ctrl Pts',(71.8341666130426,-7.91690840359367,
0.));
#117684=CARTESIAN_POINT('Ctrl Pts',(71.8123058619042,-7.90584669580955,
0.));
#117685=CARTESIAN_POINT('Ctrl Pts',(71.7904712930175,-7.89482472132137,
0.));
#117686=CARTESIAN_POINT('Ctrl Pts',(71.7686630348238,-7.88384247914524,
0.));
#117687=CARTESIAN_POINT('Ctrl Pts',(71.7468812162788,-7.87289996819653,
0.));
#117688=CARTESIAN_POINT('Ctrl Pts',(71.7251259668563,-7.86199718728826,
0.));
#117689=CARTESIAN_POINT('Ctrl Pts',(71.7033974165568,-7.85113413513736,
0.));
#117690=CARTESIAN_POINT('Ctrl Pts',(71.6816956959117,-7.84031081036489,
0.));
#117691=CARTESIAN_POINT('Ctrl Pts',(71.6600209359872,-7.82952721149507,
0.));
#117692=CARTESIAN_POINT('Ctrl Pts',(71.6383732683844,-7.8187833369486,0.));
#117693=CARTESIAN_POINT('Ctrl Pts',(71.6167528252423,-7.80807918504021,
0.));
#117694=CARTESIAN_POINT('Ctrl Pts',(71.5951597392471,-7.79741475398513,
0.));
#117695=CARTESIAN_POINT('Ctrl Pts',(71.5735941436364,-7.78679004189935,
0.));
#117696=CARTESIAN_POINT('Ctrl Pts',(71.5520561722039,-7.77620504679869,
0.));
#117697=CARTESIAN_POINT('Ctrl Pts',(71.5305459592994,-7.76565976659226,
0.));
#117698=CARTESIAN_POINT('Ctrl Pts',(71.5090636398318,-7.75515419907966,
0.));
#117699=CARTESIAN_POINT('Ctrl Pts',(71.4876093492781,-7.74468834195746,
0.));
#117700=CARTESIAN_POINT('Ctrl Pts',(71.4661832236888,-7.7342621928194,0.));
#117701=CARTESIAN_POINT('Ctrl Pts',(71.4447853996916,-7.72387574915544,
0.));
#117702=CARTESIAN_POINT('Ctrl Pts',(71.4234160144925,-7.7135290083452,0.));
#117703=CARTESIAN_POINT('Ctrl Pts',(71.4020752058796,-7.70322196765538,
0.));
#117704=CARTESIAN_POINT('Ctrl Pts',(71.3807631122331,-7.69295462424612,
0.));
#117705=CARTESIAN_POINT('Ctrl Pts',(71.3594798725281,-7.68272697517086,
0.));
#117706=CARTESIAN_POINT('Ctrl Pts',(71.3382256263414,-7.67253901737552,
0.));
#117707=CARTESIAN_POINT('Ctrl Pts',(71.3170005138502,-7.66239074769163,
0.));
#117708=CARTESIAN_POINT('Ctrl Pts',(71.2958046758372,-7.65228216283404,
0.));
#117709=CARTESIAN_POINT('Ctrl Pts',(71.2746382537007,-7.64221325940724,
0.));
#117710=CARTESIAN_POINT('Ctrl Pts',(71.2535013894602,-7.63218403390537,
0.));
#117711=CARTESIAN_POINT('Ctrl Pts',(71.2323942257609,-7.62219448271109,
0.));
#117712=CARTESIAN_POINT('Ctrl Pts',(71.211316905874,-7.61224460208837,0.));
#117713=CARTESIAN_POINT('Ctrl Pts',(71.1902695737013,-7.60233438818096,
0.));
#117714=CARTESIAN_POINT('Ctrl Pts',(71.1692523737844,-7.59246383701814,
0.));
#117715=CARTESIAN_POINT('Ctrl Pts',(71.1482654513119,-7.58263294451452,
0.));
#117716=CARTESIAN_POINT('Ctrl Pts',(71.1273089521234,-7.57284170646886,
0.));
#117717=CARTESIAN_POINT('Ctrl Pts',(71.106383022711,-7.56309011855657,0.));
#117718=CARTESIAN_POINT('Ctrl Pts',(71.0854878102243,-7.55337817632916,
0.));
#117719=CARTESIAN_POINT('Ctrl Pts',(71.0646234624811,-7.54370587521979,
0.));
#117720=CARTESIAN_POINT('Ctrl Pts',(71.043790127973,-7.53407321054262,0.));
#117721=CARTESIAN_POINT('Ctrl Pts',(71.0229879558699,-7.52448017749125,
0.));
#117722=CARTESIAN_POINT('Ctrl Pts',(71.002217096021,-7.5149267711309,0.));
#117723=CARTESIAN_POINT('Ctrl Pts',(70.9814776989612,-7.50541298639928,
0.));
#117724=CARTESIAN_POINT('Ctrl Pts',(70.9607699159218,-7.4959388181113,0.));
#117725=CARTESIAN_POINT('Ctrl Pts',(70.940093898837,-7.48650426095824,0.));
#117726=CARTESIAN_POINT('Ctrl Pts',(70.9194498003493,-7.47710930950562,
0.));
#117727=CARTESIAN_POINT('Ctrl Pts',(70.8988377738104,-7.46775395818527,
0.));
#117728=CARTESIAN_POINT('Ctrl Pts',(70.87825797329,-7.45843820129782,0.));
#117729=CARTESIAN_POINT('Ctrl Pts',(70.8577105535848,-7.44916203301647,
0.));
#117730=CARTESIAN_POINT('Ctrl Pts',(70.8371956702241,-7.43992544738606,
0.));
#117731=CARTESIAN_POINT('Ctrl Pts',(70.8167134794737,-7.43072843832014,
0.));
#117732=CARTESIAN_POINT('Ctrl Pts',(70.796264138335,-7.42157099959326,0.));
#117733=CARTESIAN_POINT('Ctrl Pts',(70.7758478045576,-7.41245312484498,
0.));
#117734=CARTESIAN_POINT('Ctrl Pts',(70.7554646366514,-7.40337480758237,
0.));
#117735=CARTESIAN_POINT('Ctrl Pts',(70.735114793895,-7.39433604117891,0.));
#117736=CARTESIAN_POINT('Ctrl Pts',(70.7147984363423,-7.38533681887028,
0.));
#117737=CARTESIAN_POINT('Ctrl Pts',(70.6945157248269,-7.37637713374761,
0.));
#117738=CARTESIAN_POINT('Ctrl Pts',(70.6742668209685,-7.36745697876295,
0.));
#117739=CARTESIAN_POINT('Ctrl Pts',(70.6540518871772,-7.35857634673052,
0.));
#117740=CARTESIAN_POINT('Ctrl Pts',(70.6338710866562,-7.3497352303258,0.));
#117741=CARTESIAN_POINT('Ctrl Pts',(70.6137245834002,-7.34093362208018,
0.));
#117742=CARTESIAN_POINT('Ctrl Pts',(70.5936125421958,-7.33217151437608,
0.));
#117743=CARTESIAN_POINT('Ctrl Pts',(70.573535128649,-7.32344889945237,0.));
#117744=CARTESIAN_POINT('Ctrl Pts',(70.5534925092053,-7.31476576940403,
0.));
#117745=CARTESIAN_POINT('Ctrl Pts',(70.5334848511675,-7.30612211618047,
0.));
#117746=CARTESIAN_POINT('Ctrl Pts',(70.5135123227147,-7.29751793157801,
0.));
#117747=CARTESIAN_POINT('Ctrl Pts',(70.4935750929029,-7.28895320723835,
0.));
#117748=CARTESIAN_POINT('Ctrl Pts',(70.4736733316463,-7.28042793465449,
0.));
#117749=CARTESIAN_POINT('Ctrl Pts',(70.4538072096986,-7.27194210517057,
0.));
#117750=CARTESIAN_POINT('Ctrl Pts',(70.433976898636,-7.2634957099805,0.));
#117751=CARTESIAN_POINT('Ctrl Pts',(70.4141825708207,-7.25508874012076,
0.));
#117752=CARTESIAN_POINT('Ctrl Pts',(70.3944243994532,-7.24672118647116,
0.));
#117753=CARTESIAN_POINT('Ctrl Pts',(70.3747025586569,-7.23839303975626,
0.));
#117754=CARTESIAN_POINT('Ctrl Pts',(70.3550172235486,-7.23010429054231,
0.));
#117755=CARTESIAN_POINT('Ctrl Pts',(70.3353685703097,-7.22185492923178,
0.));
#117756=CARTESIAN_POINT('Ctrl Pts',(70.3157567762561,-7.21364494605425,
0.));
#117757=CARTESIAN_POINT('Ctrl Pts',(70.2961820197051,-7.20547433107457,
0.));
#117758=CARTESIAN_POINT('Ctrl Pts',(70.276644479827,-7.19734307419861,0.));
#117759=CARTESIAN_POINT('Ctrl Pts',(70.2571443365198,-7.18925116517562,
0.));
#117760=CARTESIAN_POINT('Ctrl Pts',(70.2376817702239,-7.181198593598,0.));
#117761=CARTESIAN_POINT('Ctrl Pts',(70.2182569619028,-7.17318534889747,
0.));
#117762=CARTESIAN_POINT('Ctrl Pts',(70.1988700934622,-7.16521142033892,
0.));
#117763=CARTESIAN_POINT('Ctrl Pts',(70.1795213481196,-7.15727679700946,
0.));
#117764=CARTESIAN_POINT('Ctrl Pts',(70.1602109107188,-7.14938146780801,
0.));
#117765=CARTESIAN_POINT('Ctrl Pts',(70.1409389682389,-7.14152542142339,
0.));
#117766=CARTESIAN_POINT('Ctrl Pts',(70.1217057094456,-7.13370864634398,
0.));
#117767=CARTESIAN_POINT('Ctrl Pts',(70.1025113239463,-7.12593113088871,
0.));
#117768=CARTESIAN_POINT('Ctrl Pts',(70.0833560013971,-7.11819286322824,
0.));
#117769=CARTESIAN_POINT('Ctrl Pts',(70.06423993069,-7.11049383140482,0.));
#117770=CARTESIAN_POINT('Ctrl Pts',(70.0451632990137,-7.10283402335091,
0.));
#117771=CARTESIAN_POINT('Ctrl Pts',(70.0261262936435,-7.09521342684301,
0.));
#117772=CARTESIAN_POINT('Ctrl Pts',(70.0071291040791,-7.08763202944274,
0.));
#117773=CARTESIAN_POINT('Ctrl Pts',(69.988171923787,-7.08008981844643,0.));
#117774=CARTESIAN_POINT('Ctrl Pts',(69.9692549527256,-7.07258678080793,
0.));
#117775=CARTESIAN_POINT('Ctrl Pts',(69.9503783975676,-7.06512290312803,
0.));
#117776=CARTESIAN_POINT('Ctrl Pts',(69.9315424664252,-7.05769817180824,
0.));
#117777=CARTESIAN_POINT('Ctrl Pts',(69.9127473642087,-7.05031257318108,
0.));
#117778=CARTESIAN_POINT('Ctrl Pts',(69.8939932885864,-7.04296609362187,
0.));
#117779=CARTESIAN_POINT('Ctrl Pts',(69.8752804235296,-7.03565871972265,
0.));
#117780=CARTESIAN_POINT('Ctrl Pts',(69.8566089455448,-7.02839043811863,
0.));
#117781=CARTESIAN_POINT('Ctrl Pts',(69.8379790360574,-7.02116123514487,
0.));
#117782=CARTESIAN_POINT('Ctrl Pts',(69.8193908913722,-7.01397109655455,
0.));
#117783=CARTESIAN_POINT('Ctrl Pts',(69.8008447346782,-7.00682000718105,
0.));
#117784=CARTESIAN_POINT('Ctrl Pts',(69.7823408242446,-6.99970795069399,
0.));
#117785=CARTESIAN_POINT('Ctrl Pts',(69.7638794280263,-6.9926349102786,0.));
#117786=CARTESIAN_POINT('Ctrl Pts',(69.7454607995524,-6.98560086924173,
0.));
#117787=CARTESIAN_POINT('Ctrl Pts',(69.7270851557443,-6.97860581164569,
0.));
#117788=CARTESIAN_POINT('Ctrl Pts',(69.7087526480249,-6.97164972291582,
0.));
#117789=CARTESIAN_POINT('Ctrl Pts',(69.6904633605834,-6.96473259049729,
0.));
#117790=CARTESIAN_POINT('Ctrl Pts',(69.6758665380764,-6.95923004173795,
0.));
#117791=CARTESIAN_POINT('Ctrl Pts',(69.6649383920075,-6.95512065317731,
0.));
#117792=CARTESIAN_POINT('Ctrl Pts',(69.6576616146559,-6.95238884849075,
0.));
#117793=CARTESIAN_POINT('Ctrl Pts',(69.6540253893193,-6.95102489306927,
0.));
#117794=CARTESIAN_POINT('Ctrl Pts',(72.8667204369977,-15.5142209845168,
0.));
#117795=CARTESIAN_POINT('Ctrl Pts',(72.8667204369977,-15.5142209845168,
12.));
#117796=CARTESIAN_POINT('Ctrl Pts',(72.8622377860957,-15.5108715869174,
0.));
#117797=CARTESIAN_POINT('Ctrl Pts',(72.8622377860957,-15.5108715869174,
12.));
#117798=CARTESIAN_POINT('Ctrl Pts',(72.8532737732124,-15.5041768664089,
0.));
#117799=CARTESIAN_POINT('Ctrl Pts',(72.8532737732124,-15.5041768664089,
12.));
#117800=CARTESIAN_POINT('Ctrl Pts',(72.8398316206501,-15.494147009717,0.));
#117801=CARTESIAN_POINT('Ctrl Pts',(72.8398316206501,-15.494147009717,12.));
#117802=CARTESIAN_POINT('Ctrl Pts',(72.8219164844002,-15.4807983165984,
0.));
#117803=CARTESIAN_POINT('Ctrl Pts',(72.8219164844002,-15.4807983165984,
12.));
#117804=CARTESIAN_POINT('Ctrl Pts',(72.7995354604414,-15.4641532053435,
0.));
#117805=CARTESIAN_POINT('Ctrl Pts',(72.7995354604414,-15.4641532053435,
12.));
#117806=CARTESIAN_POINT('Ctrl Pts',(72.7771673494582,-15.4475488590336,
0.));
#117807=CARTESIAN_POINT('Ctrl Pts',(72.7771673494582,-15.4475488590336,
12.));
#117808=CARTESIAN_POINT('Ctrl Pts',(72.7548121825431,-15.4309852897866,
0.));
#117809=CARTESIAN_POINT('Ctrl Pts',(72.7548121825431,-15.4309852897866,
12.));
#117810=CARTESIAN_POINT('Ctrl Pts',(72.7324700089576,-15.4144625111911,
0.));
#117811=CARTESIAN_POINT('Ctrl Pts',(72.7324700089576,-15.4144625111911,
12.));
#117812=CARTESIAN_POINT('Ctrl Pts',(72.710140901746,-15.397980537311,0.));
#117813=CARTESIAN_POINT('Ctrl Pts',(72.710140901746,-15.397980537311,12.));
#117814=CARTESIAN_POINT('Ctrl Pts',(72.6878249557452,-15.3815393822669,
0.));
#117815=CARTESIAN_POINT('Ctrl Pts',(72.6878249557452,-15.3815393822669,
12.));
#117816=CARTESIAN_POINT('Ctrl Pts',(72.6655222797603,-15.3651390602616,
0.));
#117817=CARTESIAN_POINT('Ctrl Pts',(72.6655222797603,-15.3651390602616,
12.));
#117818=CARTESIAN_POINT('Ctrl Pts',(72.6432329903466,-15.3487795854723,
0.));
#117819=CARTESIAN_POINT('Ctrl Pts',(72.6432329903466,-15.3487795854723,
12.));
#117820=CARTESIAN_POINT('Ctrl Pts',(72.6209572051064,-15.3324609719961,
0.));
#117821=CARTESIAN_POINT('Ctrl Pts',(72.6209572051064,-15.3324609719961,
12.));
#117822=CARTESIAN_POINT('Ctrl Pts',(72.5986950357771,-15.3161832337617,
0.));
#117823=CARTESIAN_POINT('Ctrl Pts',(72.5986950357771,-15.3161832337617,
12.));
#117824=CARTESIAN_POINT('Ctrl Pts',(72.5764465826345,-15.2999463844691,
0.));
#117825=CARTESIAN_POINT('Ctrl Pts',(72.5764465826345,-15.2999463844691,
12.));
#117826=CARTESIAN_POINT('Ctrl Pts',(72.5542119383748,-15.2837504376562,
0.));
#117827=CARTESIAN_POINT('Ctrl Pts',(72.5542119383748,-15.2837504376562,
12.));
#117828=CARTESIAN_POINT('Ctrl Pts',(72.5319911908978,-15.2675954067495,
0.));
#117829=CARTESIAN_POINT('Ctrl Pts',(72.5319911908978,-15.2675954067495,
12.));
#117830=CARTESIAN_POINT('Ctrl Pts',(72.5097844266083,-15.2514813051174,
0.));
#117831=CARTESIAN_POINT('Ctrl Pts',(72.5097844266083,-15.2514813051174,
12.));
#117832=CARTESIAN_POINT('Ctrl Pts',(72.4875917332729,-15.2354081461151,
0.));
#117833=CARTESIAN_POINT('Ctrl Pts',(72.4875917332729,-15.2354081461151,
12.));
#117834=CARTESIAN_POINT('Ctrl Pts',(72.4654132036373,-15.2193759431359,
0.));
#117835=CARTESIAN_POINT('Ctrl Pts',(72.4654132036373,-15.2193759431359,
12.));
#117836=CARTESIAN_POINT('Ctrl Pts',(72.4432489350415,-15.2033847096077,
0.));
#117837=CARTESIAN_POINT('Ctrl Pts',(72.4432489350415,-15.2033847096077,
12.));
#117838=CARTESIAN_POINT('Ctrl Pts',(72.4210990277819,-15.1874344589716,
0.));
#117839=CARTESIAN_POINT('Ctrl Pts',(72.4210990277819,-15.1874344589716,
12.));
#117840=CARTESIAN_POINT('Ctrl Pts',(72.3989635838476,-15.1715252046602,
0.));
#117841=CARTESIAN_POINT('Ctrl Pts',(72.3989635838476,-15.1715252046602,
12.));
#117842=CARTESIAN_POINT('Ctrl Pts',(72.37684270559,-15.1556569600747,0.));
#117843=CARTESIAN_POINT('Ctrl Pts',(72.37684270559,-15.1556569600747,12.));
#117844=CARTESIAN_POINT('Ctrl Pts',(72.3547364941996,-15.1398297385513,
0.));
#117845=CARTESIAN_POINT('Ctrl Pts',(72.3547364941996,-15.1398297385513,
12.));
#117846=CARTESIAN_POINT('Ctrl Pts',(72.332645049021,-15.1240435533478,0.));
#117847=CARTESIAN_POINT('Ctrl Pts',(72.332645049021,-15.1240435533478,12.));
#117848=CARTESIAN_POINT('Ctrl Pts',(72.3105684683971,-15.1082984176655,
0.));
#117849=CARTESIAN_POINT('Ctrl Pts',(72.3105684683971,-15.1082984176655,
12.));
#117850=CARTESIAN_POINT('Ctrl Pts',(72.2885068501641,-15.0925943446593,
0.));
#117851=CARTESIAN_POINT('Ctrl Pts',(72.2885068501641,-15.0925943446593,
12.));
#117852=CARTESIAN_POINT('Ctrl Pts',(72.266460292285,-15.0769313474476,0.));
#117853=CARTESIAN_POINT('Ctrl Pts',(72.266460292285,-15.0769313474476,12.));
#117854=CARTESIAN_POINT('Ctrl Pts',(72.244428893425,-15.0613094391186,0.));
#117855=CARTESIAN_POINT('Ctrl Pts',(72.244428893425,-15.0613094391186,12.));
#117856=CARTESIAN_POINT('Ctrl Pts',(72.2224127535401,-15.0457286327328,
0.));
#117857=CARTESIAN_POINT('Ctrl Pts',(72.2224127535401,-15.0457286327328,
12.));
#117858=CARTESIAN_POINT('Ctrl Pts',(72.2004119736104,-15.0301889413255,
0.));
#117859=CARTESIAN_POINT('Ctrl Pts',(72.2004119736104,-15.0301889413255,
12.));
#117860=CARTESIAN_POINT('Ctrl Pts',(72.1784266553948,-15.0146903779061,
0.));
#117861=CARTESIAN_POINT('Ctrl Pts',(72.1784266553948,-15.0146903779061,
12.));
#117862=CARTESIAN_POINT('Ctrl Pts',(72.1564569011668,-14.9992329554537,
0.));
#117863=CARTESIAN_POINT('Ctrl Pts',(72.1564569011668,-14.9992329554537,
12.));
#117864=CARTESIAN_POINT('Ctrl Pts',(72.1345028134779,-14.9838166869107,
0.));
#117865=CARTESIAN_POINT('Ctrl Pts',(72.1345028134779,-14.9838166869107,
12.));
#117866=CARTESIAN_POINT('Ctrl Pts',(72.1125644948547,-14.9684415851699,
0.));
#117867=CARTESIAN_POINT('Ctrl Pts',(72.1125644948547,-14.9684415851699,
12.));
#117868=CARTESIAN_POINT('Ctrl Pts',(72.0906420478085,-14.953107663077,0.));
#117869=CARTESIAN_POINT('Ctrl Pts',(72.0906420478085,-14.953107663077,12.));
#117870=CARTESIAN_POINT('Ctrl Pts',(72.0687355749815,-14.937814933439,0.));
#117871=CARTESIAN_POINT('Ctrl Pts',(72.0687355749815,-14.937814933439,12.));
#117872=CARTESIAN_POINT('Ctrl Pts',(72.046845179251,-14.9225634090269,0.));
#117873=CARTESIAN_POINT('Ctrl Pts',(72.046845179251,-14.9225634090269,12.));
#117874=CARTESIAN_POINT('Ctrl Pts',(72.0249709638419,-14.9073531025763,
0.));
#117875=CARTESIAN_POINT('Ctrl Pts',(72.0249709638419,-14.9073531025763,
12.));
#117876=CARTESIAN_POINT('Ctrl Pts',(72.0031130324519,-14.8921840267829,
0.));
#117877=CARTESIAN_POINT('Ctrl Pts',(72.0031130324519,-14.8921840267829,
12.));
#117878=CARTESIAN_POINT('Ctrl Pts',(71.9812714893087,-14.8770561943011,
0.));
#117879=CARTESIAN_POINT('Ctrl Pts',(71.9812714893087,-14.8770561943011,
12.));
#117880=CARTESIAN_POINT('Ctrl Pts',(71.9594464391063,-14.8619696177503,
0.));
#117881=CARTESIAN_POINT('Ctrl Pts',(71.9594464391063,-14.8619696177503,
12.));
#117882=CARTESIAN_POINT('Ctrl Pts',(71.9376379869668,-14.846924309716,0.));
#117883=CARTESIAN_POINT('Ctrl Pts',(71.9376379869668,-14.846924309716,12.));
#117884=CARTESIAN_POINT('Ctrl Pts',(71.9158462383915,-14.8319202827482,
0.));
#117885=CARTESIAN_POINT('Ctrl Pts',(71.9158462383915,-14.8319202827482,
12.));
#117886=CARTESIAN_POINT('Ctrl Pts',(71.8940712992119,-14.8169575493559,
0.));
#117887=CARTESIAN_POINT('Ctrl Pts',(71.8940712992119,-14.8169575493559,
12.));
#117888=CARTESIAN_POINT('Ctrl Pts',(71.872313275546,-14.8020361220003,0.));
#117889=CARTESIAN_POINT('Ctrl Pts',(71.872313275546,-14.8020361220003,12.));
#117890=CARTESIAN_POINT('Ctrl Pts',(71.8505722738286,-14.7871560131021,
0.));
#117891=CARTESIAN_POINT('Ctrl Pts',(71.8505722738286,-14.7871560131021,
12.));
#117892=CARTESIAN_POINT('Ctrl Pts',(71.8288484008343,-14.7723172350454,
0.));
#117893=CARTESIAN_POINT('Ctrl Pts',(71.8288484008343,-14.7723172350454,
12.));
#117894=CARTESIAN_POINT('Ctrl Pts',(71.8071417637019,-14.7575198001776,
0.));
#117895=CARTESIAN_POINT('Ctrl Pts',(71.8071417637019,-14.7575198001776,
12.));
#117896=CARTESIAN_POINT('Ctrl Pts',(71.7854524699563,-14.7427637208071,
0.));
#117897=CARTESIAN_POINT('Ctrl Pts',(71.7854524699563,-14.7427637208071,
12.));
#117898=CARTESIAN_POINT('Ctrl Pts',(71.7637806275316,-14.7280490091954,
0.));
#117899=CARTESIAN_POINT('Ctrl Pts',(71.7637806275316,-14.7280490091954,
12.));
#117900=CARTESIAN_POINT('Ctrl Pts',(71.7421263447707,-14.7133756775622,
0.));
#117901=CARTESIAN_POINT('Ctrl Pts',(71.7421263447707,-14.7133756775622,
12.));
#117902=CARTESIAN_POINT('Ctrl Pts',(71.7204897304186,-14.6987437380898,
0.));
#117903=CARTESIAN_POINT('Ctrl Pts',(71.7204897304186,-14.6987437380898,
12.));
#117904=CARTESIAN_POINT('Ctrl Pts',(71.698870893617,-14.6841532029231,0.));
#117905=CARTESIAN_POINT('Ctrl Pts',(71.698870893617,-14.6841532029231,12.));
#117906=CARTESIAN_POINT('Ctrl Pts',(71.6772699438966,-14.6696040841679,
0.));
#117907=CARTESIAN_POINT('Ctrl Pts',(71.6772699438966,-14.6696040841679,
12.));
#117908=CARTESIAN_POINT('Ctrl Pts',(71.6556869911669,-14.6550963938832,
0.));
#117909=CARTESIAN_POINT('Ctrl Pts',(71.6556869911669,-14.6550963938832,
12.));
#117910=CARTESIAN_POINT('Ctrl Pts',(71.6341221457175,-14.6406301440817,
0.));
#117911=CARTESIAN_POINT('Ctrl Pts',(71.6341221457175,-14.6406301440817,
12.));
#117912=CARTESIAN_POINT('Ctrl Pts',(71.6125755182295,-14.6262053467372,
0.));
#117913=CARTESIAN_POINT('Ctrl Pts',(71.6125755182295,-14.6262053467372,
12.));
#117914=CARTESIAN_POINT('Ctrl Pts',(71.5910472197815,-14.611822013785,0.));
#117915=CARTESIAN_POINT('Ctrl Pts',(71.5910472197815,-14.611822013785,12.));
#117916=CARTESIAN_POINT('Ctrl Pts',(71.569537361856,-14.597480157121,0.));
#117917=CARTESIAN_POINT('Ctrl Pts',(71.569537361856,-14.597480157121,12.));
#117918=CARTESIAN_POINT('Ctrl Pts',(71.5480460563445,-14.5831797885951,
0.));
#117919=CARTESIAN_POINT('Ctrl Pts',(71.5480460563445,-14.5831797885951,
12.));
#117920=CARTESIAN_POINT('Ctrl Pts',(71.52657341555,-14.568920920009,0.));
#117921=CARTESIAN_POINT('Ctrl Pts',(71.52657341555,-14.568920920009,12.));
#117922=CARTESIAN_POINT('Ctrl Pts',(71.5051195521914,-14.5547035631234,
0.));
#117923=CARTESIAN_POINT('Ctrl Pts',(71.5051195521914,-14.5547035631234,
12.));
#117924=CARTESIAN_POINT('Ctrl Pts',(71.4836845794052,-14.540527729659,0.));
#117925=CARTESIAN_POINT('Ctrl Pts',(71.4836845794052,-14.540527729659,12.));
#117926=CARTESIAN_POINT('Ctrl Pts',(71.4622686107475,-14.5263934312969,
0.));
#117927=CARTESIAN_POINT('Ctrl Pts',(71.4622686107475,-14.5263934312969,
12.));
#117928=CARTESIAN_POINT('Ctrl Pts',(71.4408717601917,-14.5123006796728,
0.));
#117929=CARTESIAN_POINT('Ctrl Pts',(71.4408717601917,-14.5123006796728,
12.));
#117930=CARTESIAN_POINT('Ctrl Pts',(71.4194941421279,-14.4982494863716,
0.));
#117931=CARTESIAN_POINT('Ctrl Pts',(71.4194941421279,-14.4982494863716,
12.));
#117932=CARTESIAN_POINT('Ctrl Pts',(71.398135871371,-14.4842398629353,0.));
#117933=CARTESIAN_POINT('Ctrl Pts',(71.398135871371,-14.4842398629353,12.));
#117934=CARTESIAN_POINT('Ctrl Pts',(71.3767970631642,-14.470271820865,0.));
#117935=CARTESIAN_POINT('Ctrl Pts',(71.3767970631642,-14.470271820865,12.));
#117936=CARTESIAN_POINT('Ctrl Pts',(71.3554778331835,-14.4563453716204,
0.));
#117937=CARTESIAN_POINT('Ctrl Pts',(71.3554778331835,-14.4563453716204,
12.));
#117938=CARTESIAN_POINT('Ctrl Pts',(71.3341782975393,-14.4424605266166,
0.));
#117939=CARTESIAN_POINT('Ctrl Pts',(71.3341782975393,-14.4424605266166,
12.));
#117940=CARTESIAN_POINT('Ctrl Pts',(71.3128985727777,-14.4286172972168,
0.));
#117941=CARTESIAN_POINT('Ctrl Pts',(71.3128985727777,-14.4286172972168,
12.));
#117942=CARTESIAN_POINT('Ctrl Pts',(71.2916387758864,-14.4148156947384,
0.));
#117943=CARTESIAN_POINT('Ctrl Pts',(71.2916387758864,-14.4148156947384,
12.));
#117944=CARTESIAN_POINT('Ctrl Pts',(71.2703990242986,-14.401055730457,0.));
#117945=CARTESIAN_POINT('Ctrl Pts',(71.2703990242986,-14.401055730457,12.));
#117946=CARTESIAN_POINT('Ctrl Pts',(71.2491794358956,-14.3873374156056,
0.));
#117947=CARTESIAN_POINT('Ctrl Pts',(71.2491794358956,-14.3873374156056,
12.));
#117948=CARTESIAN_POINT('Ctrl Pts',(71.2279801290088,-14.3736607613723,
0.));
#117949=CARTESIAN_POINT('Ctrl Pts',(71.2279801290088,-14.3736607613723,
12.));
#117950=CARTESIAN_POINT('Ctrl Pts',(71.2068012224187,-14.3600257788927,
0.));
#117951=CARTESIAN_POINT('Ctrl Pts',(71.2068012224187,-14.3600257788927,
12.));
#117952=CARTESIAN_POINT('Ctrl Pts',(71.185642835361,-14.3464324792537,0.));
#117953=CARTESIAN_POINT('Ctrl Pts',(71.185642835361,-14.3464324792537,12.));
#117954=CARTESIAN_POINT('Ctrl Pts',(71.1645050875323,-14.3328808734993,
0.));
#117955=CARTESIAN_POINT('Ctrl Pts',(71.1645050875323,-14.3328808734993,
12.));
#117956=CARTESIAN_POINT('Ctrl Pts',(71.1433880990932,-14.3193709726295,
0.));
#117957=CARTESIAN_POINT('Ctrl Pts',(71.1433880990932,-14.3193709726295,
12.));
#117958=CARTESIAN_POINT('Ctrl Pts',(71.1222919906718,-14.3059027875993,
0.));
#117959=CARTESIAN_POINT('Ctrl Pts',(71.1222919906718,-14.3059027875993,
12.));
#117960=CARTESIAN_POINT('Ctrl Pts',(71.1012168833626,-14.2924763293101,
0.));
#117961=CARTESIAN_POINT('Ctrl Pts',(71.1012168833626,-14.2924763293101,
12.));
#117962=CARTESIAN_POINT('Ctrl Pts',(71.0801628987314,-14.2790916086129,
0.));
#117963=CARTESIAN_POINT('Ctrl Pts',(71.0801628987314,-14.2790916086129,
12.));
#117964=CARTESIAN_POINT('Ctrl Pts',(71.059130158822,-14.2657486363136,0.));
#117965=CARTESIAN_POINT('Ctrl Pts',(71.059130158822,-14.2657486363136,12.));
#117966=CARTESIAN_POINT('Ctrl Pts',(71.0381187861585,-14.2524474231732,
0.));
#117967=CARTESIAN_POINT('Ctrl Pts',(71.0381187861585,-14.2524474231732,
12.));
#117968=CARTESIAN_POINT('Ctrl Pts',(71.0171289037493,-14.2391879799063,
0.));
#117969=CARTESIAN_POINT('Ctrl Pts',(71.0171289037493,-14.2391879799063,
12.));
#117970=CARTESIAN_POINT('Ctrl Pts',(70.996160635087,-14.2259703171739,0.));
#117971=CARTESIAN_POINT('Ctrl Pts',(70.996160635087,-14.2259703171739,12.));
#117972=CARTESIAN_POINT('Ctrl Pts',(70.9752141041527,-14.2127944455841,
0.));
#117973=CARTESIAN_POINT('Ctrl Pts',(70.9752141041527,-14.2127944455841,
12.));
#117974=CARTESIAN_POINT('Ctrl Pts',(70.9542894354221,-14.1996603756984,
0.));
#117975=CARTESIAN_POINT('Ctrl Pts',(70.9542894354221,-14.1996603756984,
12.));
#117976=CARTESIAN_POINT('Ctrl Pts',(70.9333867538705,-14.1865681180321,
0.));
#117977=CARTESIAN_POINT('Ctrl Pts',(70.9333867538705,-14.1865681180321,
12.));
#117978=CARTESIAN_POINT('Ctrl Pts',(70.9125061849744,-14.1735176830533,
0.));
#117979=CARTESIAN_POINT('Ctrl Pts',(70.9125061849744,-14.1735176830533,
12.));
#117980=CARTESIAN_POINT('Ctrl Pts',(70.8916478547131,-14.1605090811754,
0.));
#117981=CARTESIAN_POINT('Ctrl Pts',(70.8916478547131,-14.1605090811754,
12.));
#117982=CARTESIAN_POINT('Ctrl Pts',(70.8708118895718,-14.1475423227567,
0.));
#117983=CARTESIAN_POINT('Ctrl Pts',(70.8708118895718,-14.1475423227567,
12.));
#117984=CARTESIAN_POINT('Ctrl Pts',(70.8499984165493,-14.1346174181079,
0.));
#117985=CARTESIAN_POINT('Ctrl Pts',(70.8499984165493,-14.1346174181079,
12.));
#117986=CARTESIAN_POINT('Ctrl Pts',(70.8292075631624,-14.1217343774914,
0.));
#117987=CARTESIAN_POINT('Ctrl Pts',(70.8292075631624,-14.1217343774914,
12.));
#117988=CARTESIAN_POINT('Ctrl Pts',(70.8084394574491,-14.1088932111214,
0.));
#117989=CARTESIAN_POINT('Ctrl Pts',(70.8084394574491,-14.1088932111214,
12.));
#117990=CARTESIAN_POINT('Ctrl Pts',(70.787694227969,-14.0960939291568,0.));
#117991=CARTESIAN_POINT('Ctrl Pts',(70.787694227969,-14.0960939291568,12.));
#117992=CARTESIAN_POINT('Ctrl Pts',(70.7669720038067,-14.0833365416995,
0.));
#117993=CARTESIAN_POINT('Ctrl Pts',(70.7669720038067,-14.0833365416995,
12.));
#117994=CARTESIAN_POINT('Ctrl Pts',(70.7462729145799,-14.0706210588015,
0.));
#117995=CARTESIAN_POINT('Ctrl Pts',(70.7462729145799,-14.0706210588015,
12.));
#117996=CARTESIAN_POINT('Ctrl Pts',(70.7255970904433,-14.0579474904657,
0.));
#117997=CARTESIAN_POINT('Ctrl Pts',(70.7255970904433,-14.0579474904657,
12.));
#117998=CARTESIAN_POINT('Ctrl Pts',(70.7049446620931,-14.0453158466451,
0.));
#117999=CARTESIAN_POINT('Ctrl Pts',(70.7049446620931,-14.0453158466451,
12.));
#118000=CARTESIAN_POINT('Ctrl Pts',(70.6843157607672,-14.0327261372363,
0.));
#118001=CARTESIAN_POINT('Ctrl Pts',(70.6843157607672,-14.0327261372363,
12.));
#118002=CARTESIAN_POINT('Ctrl Pts',(70.6637105182487,-14.020178372077,0.));
#118003=CARTESIAN_POINT('Ctrl Pts',(70.6637105182487,-14.020178372077,12.));
#118004=CARTESIAN_POINT('Ctrl Pts',(70.6431290668744,-14.0076725609537,
0.));
#118005=CARTESIAN_POINT('Ctrl Pts',(70.6431290668744,-14.0076725609537,
12.));
#118006=CARTESIAN_POINT('Ctrl Pts',(70.6225715395392,-13.9952087136018,
0.));
#118007=CARTESIAN_POINT('Ctrl Pts',(70.6225715395392,-13.9952087136018,
12.));
#118008=CARTESIAN_POINT('Ctrl Pts',(70.6020380697004,-13.9827868397057,
0.));
#118009=CARTESIAN_POINT('Ctrl Pts',(70.6020380697004,-13.9827868397057,
12.));
#118010=CARTESIAN_POINT('Ctrl Pts',(70.5815287913791,-13.9704069488918,
0.));
#118011=CARTESIAN_POINT('Ctrl Pts',(70.5815287913791,-13.9704069488918,
12.));
#118012=CARTESIAN_POINT('Ctrl Pts',(70.5610438391622,-13.9580690507262,
0.));
#118013=CARTESIAN_POINT('Ctrl Pts',(70.5610438391622,-13.9580690507262,
12.));
#118014=CARTESIAN_POINT('Ctrl Pts',(70.5405833482123,-13.9457731547217,
0.));
#118015=CARTESIAN_POINT('Ctrl Pts',(70.5405833482123,-13.9457731547217,
12.));
#118016=CARTESIAN_POINT('Ctrl Pts',(70.5201474542717,-13.9335192703389,
0.));
#118017=CARTESIAN_POINT('Ctrl Pts',(70.5201474542717,-13.9335192703389,
12.));
#118018=CARTESIAN_POINT('Ctrl Pts',(70.4997362936671,-13.9213074069852,
0.));
#118019=CARTESIAN_POINT('Ctrl Pts',(70.4997362936671,-13.9213074069852,
12.));
#118020=CARTESIAN_POINT('Ctrl Pts',(70.4793500033106,-13.9091375740084,
0.));
#118021=CARTESIAN_POINT('Ctrl Pts',(70.4793500033106,-13.9091375740084,
12.));
#118022=CARTESIAN_POINT('Ctrl Pts',(70.4589887207043,-13.8970097806947,
0.));
#118023=CARTESIAN_POINT('Ctrl Pts',(70.4589887207043,-13.8970097806947,
12.));
#118024=CARTESIAN_POINT('Ctrl Pts',(70.4386525839492,-13.8849240362757,
0.));
#118025=CARTESIAN_POINT('Ctrl Pts',(70.4386525839492,-13.8849240362757,
12.));
#118026=CARTESIAN_POINT('Ctrl Pts',(70.4183417317486,-13.8728803499284,
0.));
#118027=CARTESIAN_POINT('Ctrl Pts',(70.4183417317486,-13.8728803499284,
12.));
#118028=CARTESIAN_POINT('Ctrl Pts',(70.3980563034142,-13.8608787307753,
0.));
#118029=CARTESIAN_POINT('Ctrl Pts',(70.3980563034142,-13.8608787307753,
12.));
#118030=CARTESIAN_POINT('Ctrl Pts',(70.377796438866,-13.8489191878774,0.));
#118031=CARTESIAN_POINT('Ctrl Pts',(70.377796438866,-13.8489191878774,12.));
#118032=CARTESIAN_POINT('Ctrl Pts',(70.3575622786373,-13.8370017302319,
0.));
#118033=CARTESIAN_POINT('Ctrl Pts',(70.3575622786373,-13.8370017302319,
12.));
#118034=CARTESIAN_POINT('Ctrl Pts',(70.3373539638841,-13.8251263667799,
0.));
#118035=CARTESIAN_POINT('Ctrl Pts',(70.3373539638841,-13.8251263667799,
12.));
#118036=CARTESIAN_POINT('Ctrl Pts',(70.3171716363912,-13.8132931064067,
0.));
#118037=CARTESIAN_POINT('Ctrl Pts',(70.3171716363912,-13.8132931064067,
12.));
#118038=CARTESIAN_POINT('Ctrl Pts',(70.2970154385763,-13.8015019579411,
0.));
#118039=CARTESIAN_POINT('Ctrl Pts',(70.2970154385763,-13.8015019579411,
12.));
#118040=CARTESIAN_POINT('Ctrl Pts',(70.2768855134909,-13.7897529301483,
0.));
#118041=CARTESIAN_POINT('Ctrl Pts',(70.2768855134909,-13.7897529301483,
12.));
#118042=CARTESIAN_POINT('Ctrl Pts',(70.2567820048253,-13.7780460317284,
0.));
#118043=CARTESIAN_POINT('Ctrl Pts',(70.2567820048253,-13.7780460317284,
12.));
#118044=CARTESIAN_POINT('Ctrl Pts',(70.2367050569174,-13.7663812713235,
0.));
#118045=CARTESIAN_POINT('Ctrl Pts',(70.2367050569174,-13.7663812713235,
12.));
#118046=CARTESIAN_POINT('Ctrl Pts',(70.216654814759,-13.7547586575178,0.));
#118047=CARTESIAN_POINT('Ctrl Pts',(70.216654814759,-13.7547586575178,12.));
#118048=CARTESIAN_POINT('Ctrl Pts',(70.1966314240012,-13.7431781988368,
0.));
#118049=CARTESIAN_POINT('Ctrl Pts',(70.1966314240012,-13.7431781988368,
12.));
#118050=CARTESIAN_POINT('Ctrl Pts',(70.1766350309554,-13.73163990374,0.));
#118051=CARTESIAN_POINT('Ctrl Pts',(70.1766350309554,-13.73163990374,12.));
#118052=CARTESIAN_POINT('Ctrl Pts',(70.1566657825989,-13.7201437806207,
0.));
#118053=CARTESIAN_POINT('Ctrl Pts',(70.1566657825989,-13.7201437806207,
12.));
#118054=CARTESIAN_POINT('Ctrl Pts',(70.1367238265853,-13.7086898378127,
0.));
#118055=CARTESIAN_POINT('Ctrl Pts',(70.1367238265853,-13.7086898378127,
12.));
#118056=CARTESIAN_POINT('Ctrl Pts',(70.1168093112493,-13.6972780835898,
0.));
#118057=CARTESIAN_POINT('Ctrl Pts',(70.1168093112493,-13.6972780835898,
12.));
#118058=CARTESIAN_POINT('Ctrl Pts',(70.0969223856123,-13.685908526165,0.));
#118059=CARTESIAN_POINT('Ctrl Pts',(70.0969223856123,-13.685908526165,12.));
#118060=CARTESIAN_POINT('Ctrl Pts',(70.0770631993831,-13.6745811736825,
0.));
#118061=CARTESIAN_POINT('Ctrl Pts',(70.0770631993831,-13.6745811736825,
12.));
#118062=CARTESIAN_POINT('Ctrl Pts',(70.057231902965,-13.6632960342192,0.));
#118063=CARTESIAN_POINT('Ctrl Pts',(70.057231902965,-13.6632960342192,12.));
#118064=CARTESIAN_POINT('Ctrl Pts',(70.037428647466,-13.6520531157904,0.));
#118065=CARTESIAN_POINT('Ctrl Pts',(70.037428647466,-13.6520531157904,12.));
#118066=CARTESIAN_POINT('Ctrl Pts',(70.0176535847047,-13.6408524263496,
0.));
#118067=CARTESIAN_POINT('Ctrl Pts',(70.0176535847047,-13.6408524263496,
12.));
#118068=CARTESIAN_POINT('Ctrl Pts',(69.9979068672163,-13.6296939737866,
0.));
#118069=CARTESIAN_POINT('Ctrl Pts',(69.9979068672163,-13.6296939737866,
12.));
#118070=CARTESIAN_POINT('Ctrl Pts',(69.9781886482543,-13.61857776592,0.));
#118071=CARTESIAN_POINT('Ctrl Pts',(69.9781886482543,-13.61857776592,12.));
#118072=CARTESIAN_POINT('Ctrl Pts',(69.9584990817989,-13.6075038105,0.));
#118073=CARTESIAN_POINT('Ctrl Pts',(69.9584990817989,-13.6075038105,12.));
#118074=CARTESIAN_POINT('Ctrl Pts',(69.9388383225655,-13.5964721152136,
0.));
#118075=CARTESIAN_POINT('Ctrl Pts',(69.9388383225655,-13.5964721152136,
12.));
#118076=CARTESIAN_POINT('Ctrl Pts',(69.9192065260107,-13.5854826876834,
0.));
#118077=CARTESIAN_POINT('Ctrl Pts',(69.9192065260107,-13.5854826876834,
12.));
#118078=CARTESIAN_POINT('Ctrl Pts',(69.899603848336,-13.5745355354657,0.));
#118079=CARTESIAN_POINT('Ctrl Pts',(69.899603848336,-13.5745355354657,12.));
#118080=CARTESIAN_POINT('Ctrl Pts',(69.880030446488,-13.5636306660422,0.));
#118081=CARTESIAN_POINT('Ctrl Pts',(69.880030446488,-13.5636306660422,12.));
#118082=CARTESIAN_POINT('Ctrl Pts',(69.8604864781705,-13.5527680868256,
0.));
#118083=CARTESIAN_POINT('Ctrl Pts',(69.8604864781705,-13.5527680868256,
12.));
#118084=CARTESIAN_POINT('Ctrl Pts',(69.840972101856,-13.5419478051626,0.));
#118085=CARTESIAN_POINT('Ctrl Pts',(69.840972101856,-13.5419478051626,12.));
#118086=CARTESIAN_POINT('Ctrl Pts',(69.8214874767944,-13.5311698283339,
0.));
#118087=CARTESIAN_POINT('Ctrl Pts',(69.8214874767944,-13.5311698283339,
12.));
#118088=CARTESIAN_POINT('Ctrl Pts',(69.8020327630204,-13.5204341635507,
0.));
#118089=CARTESIAN_POINT('Ctrl Pts',(69.8020327630204,-13.5204341635507,
12.));
#118090=CARTESIAN_POINT('Ctrl Pts',(69.7826081213575,-13.5097408179478,
0.));
#118091=CARTESIAN_POINT('Ctrl Pts',(69.7826081213575,-13.5097408179478,
12.));
#118092=CARTESIAN_POINT('Ctrl Pts',(69.7632137134247,-13.4990897985904,
0.));
#118093=CARTESIAN_POINT('Ctrl Pts',(69.7632137134247,-13.4990897985904,
12.));
#118094=CARTESIAN_POINT('Ctrl Pts',(69.7438497016404,-13.4884811124748,
0.));
#118095=CARTESIAN_POINT('Ctrl Pts',(69.7438497016404,-13.4884811124748,
12.));
#118096=CARTESIAN_POINT('Ctrl Pts',(69.7245162492251,-13.4779147665285,
0.));
#118097=CARTESIAN_POINT('Ctrl Pts',(69.7245162492251,-13.4779147665285,
12.));
#118098=CARTESIAN_POINT('Ctrl Pts',(69.7052135202003,-13.4673907676045,
0.));
#118099=CARTESIAN_POINT('Ctrl Pts',(69.7052135202003,-13.4673907676045,
12.));
#118100=CARTESIAN_POINT('Ctrl Pts',(69.6859416793898,-13.4569091224762,
0.));
#118101=CARTESIAN_POINT('Ctrl Pts',(69.6859416793898,-13.4569091224762,
12.));
#118102=CARTESIAN_POINT('Ctrl Pts',(69.6667008924454,-13.4464698378456,
0.));
#118103=CARTESIAN_POINT('Ctrl Pts',(69.6667008924454,-13.4464698378456,
12.));
#118104=CARTESIAN_POINT('Ctrl Pts',(69.6474913258684,-13.4360729203444,
0.));
#118105=CARTESIAN_POINT('Ctrl Pts',(69.6474913258684,-13.4360729203444,
12.));
#118106=CARTESIAN_POINT('Ctrl Pts',(69.6283131470267,-13.425718376534,0.));
#118107=CARTESIAN_POINT('Ctrl Pts',(69.6283131470267,-13.425718376534,12.));
#118108=CARTESIAN_POINT('Ctrl Pts',(69.6091665241743,-13.4154062128998,
0.));
#118109=CARTESIAN_POINT('Ctrl Pts',(69.6091665241743,-13.4154062128998,
12.));
#118110=CARTESIAN_POINT('Ctrl Pts',(69.5900516264524,-13.4051364358494,
0.));
#118111=CARTESIAN_POINT('Ctrl Pts',(69.5900516264524,-13.4051364358494,
12.));
#118112=CARTESIAN_POINT('Ctrl Pts',(69.5709686238701,-13.3949090517173,
0.));
#118113=CARTESIAN_POINT('Ctrl Pts',(69.5709686238701,-13.3949090517173,
12.));
#118114=CARTESIAN_POINT('Ctrl Pts',(69.5519176872857,-13.3847240667626,
0.));
#118115=CARTESIAN_POINT('Ctrl Pts',(69.5519176872857,-13.3847240667626,
12.));
#118116=CARTESIAN_POINT('Ctrl Pts',(69.5328989883899,-13.3745814871667,
0.));
#118117=CARTESIAN_POINT('Ctrl Pts',(69.5328989883899,-13.3745814871667,
12.));
#118118=CARTESIAN_POINT('Ctrl Pts',(69.5139126996703,-13.3644813190225,
0.));
#118119=CARTESIAN_POINT('Ctrl Pts',(69.5139126996703,-13.3644813190225,
12.));
#118120=CARTESIAN_POINT('Ctrl Pts',(69.4949589944633,-13.3544235683399,
0.));
#118121=CARTESIAN_POINT('Ctrl Pts',(69.4949589944633,-13.3544235683399,
12.));
#118122=CARTESIAN_POINT('Ctrl Pts',(69.4760380470382,-13.3444082410546,
0.));
#118123=CARTESIAN_POINT('Ctrl Pts',(69.4760380470382,-13.3444082410546,
12.));
#118124=CARTESIAN_POINT('Ctrl Pts',(69.4571500326673,-13.3344353430313,
0.));
#118125=CARTESIAN_POINT('Ctrl Pts',(69.4571500326673,-13.3344353430313,
12.));
#118126=CARTESIAN_POINT('Ctrl Pts',(69.4382951276983,-13.3245048800641,
0.));
#118127=CARTESIAN_POINT('Ctrl Pts',(69.4382951276983,-13.3245048800641,
12.));
#118128=CARTESIAN_POINT('Ctrl Pts',(69.4194735096238,-13.3146168578738,
0.));
#118129=CARTESIAN_POINT('Ctrl Pts',(69.4194735096238,-13.3146168578738,
12.));
#118130=CARTESIAN_POINT('Ctrl Pts',(69.4006853569485,-13.3047712821046,
0.));
#118131=CARTESIAN_POINT('Ctrl Pts',(69.4006853569485,-13.3047712821046,
12.));
#118132=CARTESIAN_POINT('Ctrl Pts',(69.3819308490408,-13.2949681583164,
0.));
#118133=CARTESIAN_POINT('Ctrl Pts',(69.3819308490408,-13.2949681583164,
12.));
#118134=CARTESIAN_POINT('Ctrl Pts',(69.3632101660072,-13.2852074919767,
0.));
#118135=CARTESIAN_POINT('Ctrl Pts',(69.3632101660072,-13.2852074919767,
12.));
#118136=CARTESIAN_POINT('Ctrl Pts',(69.3445234885088,-13.2754892884437,
0.));
#118137=CARTESIAN_POINT('Ctrl Pts',(69.3445234885088,-13.2754892884437,
12.));
#118138=CARTESIAN_POINT('Ctrl Pts',(69.3258709977416,-13.2658135529616,
0.));
#118139=CARTESIAN_POINT('Ctrl Pts',(69.3258709977416,-13.2658135529616,
12.));
#118140=CARTESIAN_POINT('Ctrl Pts',(69.3072528758546,-13.2561802906901,
0.));
#118141=CARTESIAN_POINT('Ctrl Pts',(69.3072528758546,-13.2561802906901,
12.));
#118142=CARTESIAN_POINT('Ctrl Pts',(69.2886693063193,-13.2465895067264,
0.));
#118143=CARTESIAN_POINT('Ctrl Pts',(69.2886693063193,-13.2465895067264,
12.));
#118144=CARTESIAN_POINT('Ctrl Pts',(69.2701204742436,-13.2370412061218,
0.));
#118145=CARTESIAN_POINT('Ctrl Pts',(69.2701204742436,-13.2370412061218,
12.));
#118146=CARTESIAN_POINT('Ctrl Pts',(69.2516065668809,-13.2275353939044,
0.));
#118147=CARTESIAN_POINT('Ctrl Pts',(69.2516065668809,-13.2275353939044,
12.));
#118148=CARTESIAN_POINT('Ctrl Pts',(69.2331277732819,-13.2180720750585,
0.));
#118149=CARTESIAN_POINT('Ctrl Pts',(69.2331277732819,-13.2180720750585,
12.));
#118150=CARTESIAN_POINT('Ctrl Pts',(69.2146842833506,-13.2086512544729,
0.));
#118151=CARTESIAN_POINT('Ctrl Pts',(69.2146842833506,-13.2086512544729,
12.));
#118152=CARTESIAN_POINT('Ctrl Pts',(69.1962762870524,-13.1992729368928,
0.));
#118153=CARTESIAN_POINT('Ctrl Pts',(69.1962762870524,-13.1992729368928,
12.));
#118154=CARTESIAN_POINT('Ctrl Pts',(69.1779039736026,-13.1899371268689,
0.));
#118155=CARTESIAN_POINT('Ctrl Pts',(69.1779039736026,-13.1899371268689,
12.));
#118156=CARTESIAN_POINT('Ctrl Pts',(69.1595675305294,-13.1806438286944,
0.));
#118157=CARTESIAN_POINT('Ctrl Pts',(69.1595675305294,-13.1806438286944,
12.));
#118158=CARTESIAN_POINT('Ctrl Pts',(69.141267145461,-13.1713930465142,0.));
#118159=CARTESIAN_POINT('Ctrl Pts',(69.141267145461,-13.1713930465142,12.));
#118160=CARTESIAN_POINT('Ctrl Pts',(69.1230030082597,-13.1621847844533,
0.));
#118161=CARTESIAN_POINT('Ctrl Pts',(69.1230030082597,-13.1621847844533,
12.));
#118162=CARTESIAN_POINT('Ctrl Pts',(69.1047753127633,-13.1530190467181,
0.));
#118163=CARTESIAN_POINT('Ctrl Pts',(69.1047753127633,-13.1530190467181,
12.));
#118164=CARTESIAN_POINT('Ctrl Pts',(69.0865842593063,-13.1438958377397,
0.));
#118165=CARTESIAN_POINT('Ctrl Pts',(69.0865842593063,-13.1438958377397,
12.));
#118166=CARTESIAN_POINT('Ctrl Pts',(69.0684300549426,-13.1348151621824,
0.));
#118167=CARTESIAN_POINT('Ctrl Pts',(69.0684300549426,-13.1348151621824,
12.));
#118168=CARTESIAN_POINT('Ctrl Pts',(69.0503129081778,-13.1257770246379,
0.));
#118169=CARTESIAN_POINT('Ctrl Pts',(69.0503129081778,-13.1257770246379,
12.));
#118170=CARTESIAN_POINT('Ctrl Pts',(69.0322330243336,-13.1167814293495,
0.));
#118171=CARTESIAN_POINT('Ctrl Pts',(69.0322330243336,-13.1167814293495,
12.));
#118172=CARTESIAN_POINT('Ctrl Pts',(69.0141906015137,-13.1078283799726,
0.));
#118173=CARTESIAN_POINT('Ctrl Pts',(69.0141906015137,-13.1078283799726,
12.));
#118174=CARTESIAN_POINT('Ctrl Pts',(68.9961858241577,-13.0989178791843,
0.));
#118175=CARTESIAN_POINT('Ctrl Pts',(68.9961858241577,-13.0989178791843,
12.));
#118176=CARTESIAN_POINT('Ctrl Pts',(68.9782188692654,-13.0900499290541,
0.));
#118177=CARTESIAN_POINT('Ctrl Pts',(68.9782188692654,-13.0900499290541,
12.));
#118178=CARTESIAN_POINT('Ctrl Pts',(68.9602899187628,-13.0812245317816,
0.));
#118179=CARTESIAN_POINT('Ctrl Pts',(68.9602899187628,-13.0812245317816,
12.));
#118180=CARTESIAN_POINT('Ctrl Pts',(68.9423991694493,-13.072441690283,0.));
#118181=CARTESIAN_POINT('Ctrl Pts',(68.9423991694493,-13.072441690283,12.));
#118182=CARTESIAN_POINT('Ctrl Pts',(68.9245468449865,-13.0637014089018,
0.));
#118183=CARTESIAN_POINT('Ctrl Pts',(68.9245468449865,-13.0637014089018,
12.));
#118184=CARTESIAN_POINT('Ctrl Pts',(68.9067332040842,-13.0550036938793,
0.));
#118185=CARTESIAN_POINT('Ctrl Pts',(68.9067332040842,-13.0550036938793,
12.));
#118186=CARTESIAN_POINT('Ctrl Pts',(68.8889585151431,-13.0463485518185,
0.));
#118187=CARTESIAN_POINT('Ctrl Pts',(68.8889585151431,-13.0463485518185,
12.));
#118188=CARTESIAN_POINT('Ctrl Pts',(68.8712230321823,-13.0377359881864,
0.));
#118189=CARTESIAN_POINT('Ctrl Pts',(68.8712230321823,-13.0377359881864,
12.));
#118190=CARTESIAN_POINT('Ctrl Pts',(68.8535269726871,-13.0291660060118,
0.));
#118191=CARTESIAN_POINT('Ctrl Pts',(68.8535269726871,-13.0291660060118,
12.));
#118192=CARTESIAN_POINT('Ctrl Pts',(68.835870488774,-13.0206386039729,0.));
#118193=CARTESIAN_POINT('Ctrl Pts',(68.835870488774,-13.0206386039729,12.));
#118194=CARTESIAN_POINT('Ctrl Pts',(68.8182536654067,-13.0121537769003,
0.));
#118195=CARTESIAN_POINT('Ctrl Pts',(68.8182536654067,-13.0121537769003,
12.));
#118196=CARTESIAN_POINT('Ctrl Pts',(68.8041919669403,-13.0053999700929,
0.));
#118197=CARTESIAN_POINT('Ctrl Pts',(68.8041919669403,-13.0053999700929,
12.));
#118198=CARTESIAN_POINT('Ctrl Pts',(68.7936635625788,-13.0003537683089,
0.));
#118199=CARTESIAN_POINT('Ctrl Pts',(68.7936635625788,-13.0003537683089,
12.));
#118200=CARTESIAN_POINT('Ctrl Pts',(68.7866525680284,-12.996998146029,0.));
#118201=CARTESIAN_POINT('Ctrl Pts',(68.7866525680284,-12.996998146029,12.));
#118202=CARTESIAN_POINT('Ctrl Pts',(68.7831490561748,-12.9953224629497,
0.));
#118203=CARTESIAN_POINT('Ctrl Pts',(68.7831490561748,-12.9953224629497,
12.));
#118204=CARTESIAN_POINT('',(68.7831490561748,-12.9953224629497,12.));
#118205=CARTESIAN_POINT('Ctrl Pts',(68.7831490561748,-12.9953224629497,
12.));
#118206=CARTESIAN_POINT('Ctrl Pts',(68.7866525680284,-12.996998146029,12.));
#118207=CARTESIAN_POINT('Ctrl Pts',(68.7936635625788,-13.0003537683089,
12.));
#118208=CARTESIAN_POINT('Ctrl Pts',(68.8041919669403,-13.0053999700929,
12.));
#118209=CARTESIAN_POINT('Ctrl Pts',(68.8182536654067,-13.0121537769003,
12.));
#118210=CARTESIAN_POINT('Ctrl Pts',(68.835870488774,-13.0206386039729,12.));
#118211=CARTESIAN_POINT('Ctrl Pts',(68.8535269726871,-13.0291660060118,
12.));
#118212=CARTESIAN_POINT('Ctrl Pts',(68.8712230321823,-13.0377359881864,
12.));
#118213=CARTESIAN_POINT('Ctrl Pts',(68.8889585151431,-13.0463485518185,
12.));
#118214=CARTESIAN_POINT('Ctrl Pts',(68.9067332040842,-13.0550036938793,
12.));
#118215=CARTESIAN_POINT('Ctrl Pts',(68.9245468449865,-13.0637014089018,
12.));
#118216=CARTESIAN_POINT('Ctrl Pts',(68.9423991694493,-13.072441690283,12.));
#118217=CARTESIAN_POINT('Ctrl Pts',(68.9602899187628,-13.0812245317816,
12.));
#118218=CARTESIAN_POINT('Ctrl Pts',(68.9782188692654,-13.0900499290541,
12.));
#118219=CARTESIAN_POINT('Ctrl Pts',(68.9961858241577,-13.0989178791843,
12.));
#118220=CARTESIAN_POINT('Ctrl Pts',(69.0141906015137,-13.1078283799726,
12.));
#118221=CARTESIAN_POINT('Ctrl Pts',(69.0322330243336,-13.1167814293495,
12.));
#118222=CARTESIAN_POINT('Ctrl Pts',(69.0503129081778,-13.1257770246379,
12.));
#118223=CARTESIAN_POINT('Ctrl Pts',(69.0684300549426,-13.1348151621824,
12.));
#118224=CARTESIAN_POINT('Ctrl Pts',(69.0865842593063,-13.1438958377397,
12.));
#118225=CARTESIAN_POINT('Ctrl Pts',(69.1047753127633,-13.1530190467181,
12.));
#118226=CARTESIAN_POINT('Ctrl Pts',(69.1230030082597,-13.1621847844533,
12.));
#118227=CARTESIAN_POINT('Ctrl Pts',(69.141267145461,-13.1713930465142,12.));
#118228=CARTESIAN_POINT('Ctrl Pts',(69.1595675305294,-13.1806438286944,
12.));
#118229=CARTESIAN_POINT('Ctrl Pts',(69.1779039736026,-13.1899371268689,
12.));
#118230=CARTESIAN_POINT('Ctrl Pts',(69.1962762870524,-13.1992729368928,
12.));
#118231=CARTESIAN_POINT('Ctrl Pts',(69.2146842833506,-13.2086512544729,
12.));
#118232=CARTESIAN_POINT('Ctrl Pts',(69.2331277732819,-13.2180720750585,
12.));
#118233=CARTESIAN_POINT('Ctrl Pts',(69.2516065668809,-13.2275353939044,
12.));
#118234=CARTESIAN_POINT('Ctrl Pts',(69.2701204742436,-13.2370412061218,
12.));
#118235=CARTESIAN_POINT('Ctrl Pts',(69.2886693063193,-13.2465895067264,
12.));
#118236=CARTESIAN_POINT('Ctrl Pts',(69.3072528758546,-13.2561802906901,
12.));
#118237=CARTESIAN_POINT('Ctrl Pts',(69.3258709977416,-13.2658135529616,
12.));
#118238=CARTESIAN_POINT('Ctrl Pts',(69.3445234885088,-13.2754892884437,
12.));
#118239=CARTESIAN_POINT('Ctrl Pts',(69.3632101660072,-13.2852074919767,
12.));
#118240=CARTESIAN_POINT('Ctrl Pts',(69.3819308490408,-13.2949681583164,
12.));
#118241=CARTESIAN_POINT('Ctrl Pts',(69.4006853569485,-13.3047712821046,
12.));
#118242=CARTESIAN_POINT('Ctrl Pts',(69.4194735096238,-13.3146168578738,
12.));
#118243=CARTESIAN_POINT('Ctrl Pts',(69.4382951276983,-13.3245048800641,
12.));
#118244=CARTESIAN_POINT('Ctrl Pts',(69.4571500326673,-13.3344353430313,
12.));
#118245=CARTESIAN_POINT('Ctrl Pts',(69.4760380470382,-13.3444082410546,
12.));
#118246=CARTESIAN_POINT('Ctrl Pts',(69.4949589944633,-13.3544235683399,
12.));
#118247=CARTESIAN_POINT('Ctrl Pts',(69.5139126996703,-13.3644813190225,
12.));
#118248=CARTESIAN_POINT('Ctrl Pts',(69.5328989883899,-13.3745814871667,
12.));
#118249=CARTESIAN_POINT('Ctrl Pts',(69.5519176872857,-13.3847240667626,
12.));
#118250=CARTESIAN_POINT('Ctrl Pts',(69.5709686238701,-13.3949090517173,
12.));
#118251=CARTESIAN_POINT('Ctrl Pts',(69.5900516264524,-13.4051364358494,
12.));
#118252=CARTESIAN_POINT('Ctrl Pts',(69.6091665241743,-13.4154062128998,
12.));
#118253=CARTESIAN_POINT('Ctrl Pts',(69.6283131470267,-13.425718376534,12.));
#118254=CARTESIAN_POINT('Ctrl Pts',(69.6474913258684,-13.4360729203444,
12.));
#118255=CARTESIAN_POINT('Ctrl Pts',(69.6667008924454,-13.4464698378456,
12.));
#118256=CARTESIAN_POINT('Ctrl Pts',(69.6859416793898,-13.4569091224762,
12.));
#118257=CARTESIAN_POINT('Ctrl Pts',(69.7052135202003,-13.4673907676045,
12.));
#118258=CARTESIAN_POINT('Ctrl Pts',(69.7245162492251,-13.4779147665285,
12.));
#118259=CARTESIAN_POINT('Ctrl Pts',(69.7438497016404,-13.4884811124748,
12.));
#118260=CARTESIAN_POINT('Ctrl Pts',(69.7632137134247,-13.4990897985904,
12.));
#118261=CARTESIAN_POINT('Ctrl Pts',(69.7826081213575,-13.5097408179478,
12.));
#118262=CARTESIAN_POINT('Ctrl Pts',(69.8020327630204,-13.5204341635507,
12.));
#118263=CARTESIAN_POINT('Ctrl Pts',(69.8214874767944,-13.5311698283339,
12.));
#118264=CARTESIAN_POINT('Ctrl Pts',(69.840972101856,-13.5419478051626,12.));
#118265=CARTESIAN_POINT('Ctrl Pts',(69.8604864781705,-13.5527680868256,
12.));
#118266=CARTESIAN_POINT('Ctrl Pts',(69.880030446488,-13.5636306660422,12.));
#118267=CARTESIAN_POINT('Ctrl Pts',(69.899603848336,-13.5745355354657,12.));
#118268=CARTESIAN_POINT('Ctrl Pts',(69.9192065260107,-13.5854826876834,
12.));
#118269=CARTESIAN_POINT('Ctrl Pts',(69.9388383225655,-13.5964721152136,
12.));
#118270=CARTESIAN_POINT('Ctrl Pts',(69.9584990817989,-13.6075038105,12.));
#118271=CARTESIAN_POINT('Ctrl Pts',(69.9781886482543,-13.61857776592,12.));
#118272=CARTESIAN_POINT('Ctrl Pts',(69.9979068672163,-13.6296939737866,
12.));
#118273=CARTESIAN_POINT('Ctrl Pts',(70.0176535847047,-13.6408524263496,
12.));
#118274=CARTESIAN_POINT('Ctrl Pts',(70.037428647466,-13.6520531157904,12.));
#118275=CARTESIAN_POINT('Ctrl Pts',(70.057231902965,-13.6632960342192,12.));
#118276=CARTESIAN_POINT('Ctrl Pts',(70.0770631993831,-13.6745811736825,
12.));
#118277=CARTESIAN_POINT('Ctrl Pts',(70.0969223856123,-13.685908526165,12.));
#118278=CARTESIAN_POINT('Ctrl Pts',(70.1168093112493,-13.6972780835898,
12.));
#118279=CARTESIAN_POINT('Ctrl Pts',(70.1367238265853,-13.7086898378127,
12.));
#118280=CARTESIAN_POINT('Ctrl Pts',(70.1566657825989,-13.7201437806207,
12.));
#118281=CARTESIAN_POINT('Ctrl Pts',(70.1766350309554,-13.73163990374,12.));
#118282=CARTESIAN_POINT('Ctrl Pts',(70.1966314240012,-13.7431781988368,
12.));
#118283=CARTESIAN_POINT('Ctrl Pts',(70.216654814759,-13.7547586575178,12.));
#118284=CARTESIAN_POINT('Ctrl Pts',(70.2367050569174,-13.7663812713235,
12.));
#118285=CARTESIAN_POINT('Ctrl Pts',(70.2567820048253,-13.7780460317284,
12.));
#118286=CARTESIAN_POINT('Ctrl Pts',(70.2768855134909,-13.7897529301483,
12.));
#118287=CARTESIAN_POINT('Ctrl Pts',(70.2970154385763,-13.8015019579411,
12.));
#118288=CARTESIAN_POINT('Ctrl Pts',(70.3171716363912,-13.8132931064067,
12.));
#118289=CARTESIAN_POINT('Ctrl Pts',(70.3373539638841,-13.8251263667799,
12.));
#118290=CARTESIAN_POINT('Ctrl Pts',(70.3575622786373,-13.8370017302319,
12.));
#118291=CARTESIAN_POINT('Ctrl Pts',(70.377796438866,-13.8489191878774,12.));
#118292=CARTESIAN_POINT('Ctrl Pts',(70.3980563034142,-13.8608787307753,
12.));
#118293=CARTESIAN_POINT('Ctrl Pts',(70.4183417317486,-13.8728803499284,
12.));
#118294=CARTESIAN_POINT('Ctrl Pts',(70.4386525839492,-13.8849240362757,
12.));
#118295=CARTESIAN_POINT('Ctrl Pts',(70.4589887207043,-13.8970097806947,
12.));
#118296=CARTESIAN_POINT('Ctrl Pts',(70.4793500033106,-13.9091375740084,
12.));
#118297=CARTESIAN_POINT('Ctrl Pts',(70.4997362936671,-13.9213074069852,
12.));
#118298=CARTESIAN_POINT('Ctrl Pts',(70.5201474542717,-13.9335192703389,
12.));
#118299=CARTESIAN_POINT('Ctrl Pts',(70.5405833482123,-13.9457731547217,
12.));
#118300=CARTESIAN_POINT('Ctrl Pts',(70.5610438391622,-13.9580690507262,
12.));
#118301=CARTESIAN_POINT('Ctrl Pts',(70.5815287913791,-13.9704069488918,
12.));
#118302=CARTESIAN_POINT('Ctrl Pts',(70.6020380697004,-13.9827868397057,
12.));
#118303=CARTESIAN_POINT('Ctrl Pts',(70.6225715395392,-13.9952087136018,
12.));
#118304=CARTESIAN_POINT('Ctrl Pts',(70.6431290668744,-14.0076725609537,
12.));
#118305=CARTESIAN_POINT('Ctrl Pts',(70.6637105182487,-14.020178372077,12.));
#118306=CARTESIAN_POINT('Ctrl Pts',(70.6843157607672,-14.0327261372363,
12.));
#118307=CARTESIAN_POINT('Ctrl Pts',(70.7049446620931,-14.0453158466451,
12.));
#118308=CARTESIAN_POINT('Ctrl Pts',(70.7255970904433,-14.0579474904657,
12.));
#118309=CARTESIAN_POINT('Ctrl Pts',(70.7462729145799,-14.0706210588015,
12.));
#118310=CARTESIAN_POINT('Ctrl Pts',(70.7669720038067,-14.0833365416995,
12.));
#118311=CARTESIAN_POINT('Ctrl Pts',(70.787694227969,-14.0960939291568,12.));
#118312=CARTESIAN_POINT('Ctrl Pts',(70.8084394574491,-14.1088932111214,
12.));
#118313=CARTESIAN_POINT('Ctrl Pts',(70.8292075631624,-14.1217343774914,
12.));
#118314=CARTESIAN_POINT('Ctrl Pts',(70.8499984165493,-14.1346174181079,
12.));
#118315=CARTESIAN_POINT('Ctrl Pts',(70.8708118895718,-14.1475423227567,
12.));
#118316=CARTESIAN_POINT('Ctrl Pts',(70.8916478547131,-14.1605090811754,
12.));
#118317=CARTESIAN_POINT('Ctrl Pts',(70.9125061849744,-14.1735176830533,
12.));
#118318=CARTESIAN_POINT('Ctrl Pts',(70.9333867538705,-14.1865681180321,
12.));
#118319=CARTESIAN_POINT('Ctrl Pts',(70.9542894354221,-14.1996603756984,
12.));
#118320=CARTESIAN_POINT('Ctrl Pts',(70.9752141041527,-14.2127944455841,
12.));
#118321=CARTESIAN_POINT('Ctrl Pts',(70.996160635087,-14.2259703171739,12.));
#118322=CARTESIAN_POINT('Ctrl Pts',(71.0171289037493,-14.2391879799063,
12.));
#118323=CARTESIAN_POINT('Ctrl Pts',(71.0381187861585,-14.2524474231732,
12.));
#118324=CARTESIAN_POINT('Ctrl Pts',(71.059130158822,-14.2657486363136,12.));
#118325=CARTESIAN_POINT('Ctrl Pts',(71.0801628987314,-14.2790916086129,
12.));
#118326=CARTESIAN_POINT('Ctrl Pts',(71.1012168833626,-14.2924763293101,
12.));
#118327=CARTESIAN_POINT('Ctrl Pts',(71.1222919906718,-14.3059027875993,
12.));
#118328=CARTESIAN_POINT('Ctrl Pts',(71.1433880990932,-14.3193709726295,
12.));
#118329=CARTESIAN_POINT('Ctrl Pts',(71.1645050875323,-14.3328808734993,
12.));
#118330=CARTESIAN_POINT('Ctrl Pts',(71.185642835361,-14.3464324792537,12.));
#118331=CARTESIAN_POINT('Ctrl Pts',(71.2068012224187,-14.3600257788927,
12.));
#118332=CARTESIAN_POINT('Ctrl Pts',(71.2279801290088,-14.3736607613723,
12.));
#118333=CARTESIAN_POINT('Ctrl Pts',(71.2491794358956,-14.3873374156056,
12.));
#118334=CARTESIAN_POINT('Ctrl Pts',(71.2703990242986,-14.401055730457,12.));
#118335=CARTESIAN_POINT('Ctrl Pts',(71.2916387758864,-14.4148156947384,
12.));
#118336=CARTESIAN_POINT('Ctrl Pts',(71.3128985727777,-14.4286172972168,
12.));
#118337=CARTESIAN_POINT('Ctrl Pts',(71.3341782975393,-14.4424605266166,
12.));
#118338=CARTESIAN_POINT('Ctrl Pts',(71.3554778331835,-14.4563453716204,
12.));
#118339=CARTESIAN_POINT('Ctrl Pts',(71.3767970631642,-14.470271820865,12.));
#118340=CARTESIAN_POINT('Ctrl Pts',(71.398135871371,-14.4842398629353,12.));
#118341=CARTESIAN_POINT('Ctrl Pts',(71.4194941421279,-14.4982494863716,
12.));
#118342=CARTESIAN_POINT('Ctrl Pts',(71.4408717601917,-14.5123006796728,
12.));
#118343=CARTESIAN_POINT('Ctrl Pts',(71.4622686107475,-14.5263934312969,
12.));
#118344=CARTESIAN_POINT('Ctrl Pts',(71.4836845794052,-14.540527729659,12.));
#118345=CARTESIAN_POINT('Ctrl Pts',(71.5051195521914,-14.5547035631234,
12.));
#118346=CARTESIAN_POINT('Ctrl Pts',(71.52657341555,-14.568920920009,12.));
#118347=CARTESIAN_POINT('Ctrl Pts',(71.5480460563445,-14.5831797885951,
12.));
#118348=CARTESIAN_POINT('Ctrl Pts',(71.569537361856,-14.597480157121,12.));
#118349=CARTESIAN_POINT('Ctrl Pts',(71.5910472197815,-14.611822013785,12.));
#118350=CARTESIAN_POINT('Ctrl Pts',(71.6125755182295,-14.6262053467372,
12.));
#118351=CARTESIAN_POINT('Ctrl Pts',(71.6341221457175,-14.6406301440817,
12.));
#118352=CARTESIAN_POINT('Ctrl Pts',(71.6556869911669,-14.6550963938832,
12.));
#118353=CARTESIAN_POINT('Ctrl Pts',(71.6772699438966,-14.6696040841679,
12.));
#118354=CARTESIAN_POINT('Ctrl Pts',(71.698870893617,-14.6841532029231,12.));
#118355=CARTESIAN_POINT('Ctrl Pts',(71.7204897304186,-14.6987437380898,
12.));
#118356=CARTESIAN_POINT('Ctrl Pts',(71.7421263447707,-14.7133756775622,
12.));
#118357=CARTESIAN_POINT('Ctrl Pts',(71.7637806275316,-14.7280490091954,
12.));
#118358=CARTESIAN_POINT('Ctrl Pts',(71.7854524699563,-14.7427637208071,
12.));
#118359=CARTESIAN_POINT('Ctrl Pts',(71.8071417637019,-14.7575198001776,
12.));
#118360=CARTESIAN_POINT('Ctrl Pts',(71.8288484008343,-14.7723172350454,
12.));
#118361=CARTESIAN_POINT('Ctrl Pts',(71.8505722738286,-14.7871560131021,
12.));
#118362=CARTESIAN_POINT('Ctrl Pts',(71.872313275546,-14.8020361220003,12.));
#118363=CARTESIAN_POINT('Ctrl Pts',(71.8940712992119,-14.8169575493559,
12.));
#118364=CARTESIAN_POINT('Ctrl Pts',(71.9158462383915,-14.8319202827482,
12.));
#118365=CARTESIAN_POINT('Ctrl Pts',(71.9376379869668,-14.846924309716,12.));
#118366=CARTESIAN_POINT('Ctrl Pts',(71.9594464391063,-14.8619696177503,
12.));
#118367=CARTESIAN_POINT('Ctrl Pts',(71.9812714893087,-14.8770561943011,
12.));
#118368=CARTESIAN_POINT('Ctrl Pts',(72.0031130324519,-14.8921840267829,
12.));
#118369=CARTESIAN_POINT('Ctrl Pts',(72.0249709638419,-14.9073531025763,
12.));
#118370=CARTESIAN_POINT('Ctrl Pts',(72.046845179251,-14.9225634090269,12.));
#118371=CARTESIAN_POINT('Ctrl Pts',(72.0687355749815,-14.937814933439,12.));
#118372=CARTESIAN_POINT('Ctrl Pts',(72.0906420478085,-14.953107663077,12.));
#118373=CARTESIAN_POINT('Ctrl Pts',(72.1125644948547,-14.9684415851699,
12.));
#118374=CARTESIAN_POINT('Ctrl Pts',(72.1345028134779,-14.9838166869107,
12.));
#118375=CARTESIAN_POINT('Ctrl Pts',(72.1564569011668,-14.9992329554537,
12.));
#118376=CARTESIAN_POINT('Ctrl Pts',(72.1784266553948,-15.0146903779061,
12.));
#118377=CARTESIAN_POINT('Ctrl Pts',(72.2004119736104,-15.0301889413255,
12.));
#118378=CARTESIAN_POINT('Ctrl Pts',(72.2224127535401,-15.0457286327328,
12.));
#118379=CARTESIAN_POINT('Ctrl Pts',(72.244428893425,-15.0613094391186,12.));
#118380=CARTESIAN_POINT('Ctrl Pts',(72.266460292285,-15.0769313474476,12.));
#118381=CARTESIAN_POINT('Ctrl Pts',(72.2885068501641,-15.0925943446593,
12.));
#118382=CARTESIAN_POINT('Ctrl Pts',(72.3105684683971,-15.1082984176655,
12.));
#118383=CARTESIAN_POINT('Ctrl Pts',(72.332645049021,-15.1240435533478,12.));
#118384=CARTESIAN_POINT('Ctrl Pts',(72.3547364941996,-15.1398297385513,
12.));
#118385=CARTESIAN_POINT('Ctrl Pts',(72.37684270559,-15.1556569600747,12.));
#118386=CARTESIAN_POINT('Ctrl Pts',(72.3989635838476,-15.1715252046602,
12.));
#118387=CARTESIAN_POINT('Ctrl Pts',(72.4210990277819,-15.1874344589716,
12.));
#118388=CARTESIAN_POINT('Ctrl Pts',(72.4432489350415,-15.2033847096077,
12.));
#118389=CARTESIAN_POINT('Ctrl Pts',(72.4654132036373,-15.2193759431359,
12.));
#118390=CARTESIAN_POINT('Ctrl Pts',(72.4875917332729,-15.2354081461151,
12.));
#118391=CARTESIAN_POINT('Ctrl Pts',(72.5097844266083,-15.2514813051174,
12.));
#118392=CARTESIAN_POINT('Ctrl Pts',(72.5319911908978,-15.2675954067495,
12.));
#118393=CARTESIAN_POINT('Ctrl Pts',(72.5542119383748,-15.2837504376562,
12.));
#118394=CARTESIAN_POINT('Ctrl Pts',(72.5732713370797,-15.2976335024853,
12.));
#118395=CARTESIAN_POINT('Ctrl Pts',(72.5878912620665,-15.3082994603653,
12.));
#118396=CARTESIAN_POINT('Ctrl Pts',(72.59806557899,-15.3157301930834,12.));
#118397=CARTESIAN_POINT('Ctrl Pts',(72.6037902605231,-15.3199137230322,
12.));
#118398=CARTESIAN_POINT('Ctrl Pts',(72.6050633494717,-15.3208442077424,
12.));
#118399=CARTESIAN_POINT('',(68.7831490561748,-12.9953224629497,0.));
#118400=CARTESIAN_POINT('',(68.7831490561748,-12.9953224629497,0.));
#118401=CARTESIAN_POINT('Ctrl Pts',(72.6050633494716,-15.3208442077424,
0.));
#118402=CARTESIAN_POINT('Ctrl Pts',(72.603790260523,-15.3199137230321,0.));
#118403=CARTESIAN_POINT('Ctrl Pts',(72.59806557899,-15.3157301930834,0.));
#118404=CARTESIAN_POINT('Ctrl Pts',(72.5878912620664,-15.3082994603653,
0.));
#118405=CARTESIAN_POINT('Ctrl Pts',(72.5732713370797,-15.2976335024853,
0.));
#118406=CARTESIAN_POINT('Ctrl Pts',(72.5542119383748,-15.2837504376562,
0.));
#118407=CARTESIAN_POINT('Ctrl Pts',(72.5319911908978,-15.2675954067495,
0.));
#118408=CARTESIAN_POINT('Ctrl Pts',(72.5097844266083,-15.2514813051174,
0.));
#118409=CARTESIAN_POINT('Ctrl Pts',(72.4875917332729,-15.2354081461151,
0.));
#118410=CARTESIAN_POINT('Ctrl Pts',(72.4654132036373,-15.2193759431359,
0.));
#118411=CARTESIAN_POINT('Ctrl Pts',(72.4432489350415,-15.2033847096077,
0.));
#118412=CARTESIAN_POINT('Ctrl Pts',(72.4210990277819,-15.1874344589716,
0.));
#118413=CARTESIAN_POINT('Ctrl Pts',(72.3989635838476,-15.1715252046602,
0.));
#118414=CARTESIAN_POINT('Ctrl Pts',(72.37684270559,-15.1556569600747,0.));
#118415=CARTESIAN_POINT('Ctrl Pts',(72.3547364941996,-15.1398297385513,
0.));
#118416=CARTESIAN_POINT('Ctrl Pts',(72.332645049021,-15.1240435533478,0.));
#118417=CARTESIAN_POINT('Ctrl Pts',(72.3105684683971,-15.1082984176655,
0.));
#118418=CARTESIAN_POINT('Ctrl Pts',(72.2885068501641,-15.0925943446593,
0.));
#118419=CARTESIAN_POINT('Ctrl Pts',(72.266460292285,-15.0769313474476,0.));
#118420=CARTESIAN_POINT('Ctrl Pts',(72.244428893425,-15.0613094391186,0.));
#118421=CARTESIAN_POINT('Ctrl Pts',(72.2224127535401,-15.0457286327328,
0.));
#118422=CARTESIAN_POINT('Ctrl Pts',(72.2004119736104,-15.0301889413255,
0.));
#118423=CARTESIAN_POINT('Ctrl Pts',(72.1784266553948,-15.0146903779061,
0.));
#118424=CARTESIAN_POINT('Ctrl Pts',(72.1564569011668,-14.9992329554537,
0.));
#118425=CARTESIAN_POINT('Ctrl Pts',(72.1345028134779,-14.9838166869107,
0.));
#118426=CARTESIAN_POINT('Ctrl Pts',(72.1125644948547,-14.9684415851699,
0.));
#118427=CARTESIAN_POINT('Ctrl Pts',(72.0906420478085,-14.953107663077,0.));
#118428=CARTESIAN_POINT('Ctrl Pts',(72.0687355749815,-14.937814933439,0.));
#118429=CARTESIAN_POINT('Ctrl Pts',(72.046845179251,-14.9225634090269,0.));
#118430=CARTESIAN_POINT('Ctrl Pts',(72.0249709638419,-14.9073531025763,
0.));
#118431=CARTESIAN_POINT('Ctrl Pts',(72.0031130324519,-14.8921840267829,
0.));
#118432=CARTESIAN_POINT('Ctrl Pts',(71.9812714893087,-14.8770561943011,
0.));
#118433=CARTESIAN_POINT('Ctrl Pts',(71.9594464391063,-14.8619696177503,
0.));
#118434=CARTESIAN_POINT('Ctrl Pts',(71.9376379869668,-14.846924309716,0.));
#118435=CARTESIAN_POINT('Ctrl Pts',(71.9158462383915,-14.8319202827482,
0.));
#118436=CARTESIAN_POINT('Ctrl Pts',(71.8940712992119,-14.8169575493559,
0.));
#118437=CARTESIAN_POINT('Ctrl Pts',(71.872313275546,-14.8020361220003,0.));
#118438=CARTESIAN_POINT('Ctrl Pts',(71.8505722738286,-14.7871560131021,
0.));
#118439=CARTESIAN_POINT('Ctrl Pts',(71.8288484008343,-14.7723172350454,
0.));
#118440=CARTESIAN_POINT('Ctrl Pts',(71.8071417637019,-14.7575198001776,
0.));
#118441=CARTESIAN_POINT('Ctrl Pts',(71.7854524699563,-14.7427637208071,
0.));
#118442=CARTESIAN_POINT('Ctrl Pts',(71.7637806275316,-14.7280490091954,
0.));
#118443=CARTESIAN_POINT('Ctrl Pts',(71.7421263447707,-14.7133756775622,
0.));
#118444=CARTESIAN_POINT('Ctrl Pts',(71.7204897304186,-14.6987437380898,
0.));
#118445=CARTESIAN_POINT('Ctrl Pts',(71.698870893617,-14.6841532029231,0.));
#118446=CARTESIAN_POINT('Ctrl Pts',(71.6772699438966,-14.6696040841679,
0.));
#118447=CARTESIAN_POINT('Ctrl Pts',(71.6556869911669,-14.6550963938832,
0.));
#118448=CARTESIAN_POINT('Ctrl Pts',(71.6341221457175,-14.6406301440817,
0.));
#118449=CARTESIAN_POINT('Ctrl Pts',(71.6125755182295,-14.6262053467372,
0.));
#118450=CARTESIAN_POINT('Ctrl Pts',(71.5910472197815,-14.611822013785,0.));
#118451=CARTESIAN_POINT('Ctrl Pts',(71.569537361856,-14.597480157121,0.));
#118452=CARTESIAN_POINT('Ctrl Pts',(71.5480460563445,-14.5831797885951,
0.));
#118453=CARTESIAN_POINT('Ctrl Pts',(71.52657341555,-14.568920920009,0.));
#118454=CARTESIAN_POINT('Ctrl Pts',(71.5051195521914,-14.5547035631234,
0.));
#118455=CARTESIAN_POINT('Ctrl Pts',(71.4836845794052,-14.540527729659,0.));
#118456=CARTESIAN_POINT('Ctrl Pts',(71.4622686107475,-14.5263934312969,
0.));
#118457=CARTESIAN_POINT('Ctrl Pts',(71.4408717601917,-14.5123006796728,
0.));
#118458=CARTESIAN_POINT('Ctrl Pts',(71.4194941421279,-14.4982494863716,
0.));
#118459=CARTESIAN_POINT('Ctrl Pts',(71.398135871371,-14.4842398629353,0.));
#118460=CARTESIAN_POINT('Ctrl Pts',(71.3767970631642,-14.470271820865,0.));
#118461=CARTESIAN_POINT('Ctrl Pts',(71.3554778331835,-14.4563453716204,
0.));
#118462=CARTESIAN_POINT('Ctrl Pts',(71.3341782975393,-14.4424605266166,
0.));
#118463=CARTESIAN_POINT('Ctrl Pts',(71.3128985727777,-14.4286172972168,
0.));
#118464=CARTESIAN_POINT('Ctrl Pts',(71.2916387758864,-14.4148156947384,
0.));
#118465=CARTESIAN_POINT('Ctrl Pts',(71.2703990242986,-14.401055730457,0.));
#118466=CARTESIAN_POINT('Ctrl Pts',(71.2491794358956,-14.3873374156056,
0.));
#118467=CARTESIAN_POINT('Ctrl Pts',(71.2279801290088,-14.3736607613723,
0.));
#118468=CARTESIAN_POINT('Ctrl Pts',(71.2068012224187,-14.3600257788927,
0.));
#118469=CARTESIAN_POINT('Ctrl Pts',(71.185642835361,-14.3464324792537,0.));
#118470=CARTESIAN_POINT('Ctrl Pts',(71.1645050875323,-14.3328808734993,
0.));
#118471=CARTESIAN_POINT('Ctrl Pts',(71.1433880990932,-14.3193709726295,
0.));
#118472=CARTESIAN_POINT('Ctrl Pts',(71.1222919906718,-14.3059027875993,
0.));
#118473=CARTESIAN_POINT('Ctrl Pts',(71.1012168833626,-14.2924763293101,
0.));
#118474=CARTESIAN_POINT('Ctrl Pts',(71.0801628987314,-14.2790916086129,
0.));
#118475=CARTESIAN_POINT('Ctrl Pts',(71.059130158822,-14.2657486363136,0.));
#118476=CARTESIAN_POINT('Ctrl Pts',(71.0381187861585,-14.2524474231732,
0.));
#118477=CARTESIAN_POINT('Ctrl Pts',(71.0171289037493,-14.2391879799063,
0.));
#118478=CARTESIAN_POINT('Ctrl Pts',(70.996160635087,-14.2259703171739,0.));
#118479=CARTESIAN_POINT('Ctrl Pts',(70.9752141041527,-14.2127944455841,
0.));
#118480=CARTESIAN_POINT('Ctrl Pts',(70.9542894354221,-14.1996603756984,
0.));
#118481=CARTESIAN_POINT('Ctrl Pts',(70.9333867538705,-14.1865681180321,
0.));
#118482=CARTESIAN_POINT('Ctrl Pts',(70.9125061849744,-14.1735176830533,
0.));
#118483=CARTESIAN_POINT('Ctrl Pts',(70.8916478547131,-14.1605090811754,
0.));
#118484=CARTESIAN_POINT('Ctrl Pts',(70.8708118895718,-14.1475423227567,
0.));
#118485=CARTESIAN_POINT('Ctrl Pts',(70.8499984165493,-14.1346174181079,
0.));
#118486=CARTESIAN_POINT('Ctrl Pts',(70.8292075631624,-14.1217343774914,
0.));
#118487=CARTESIAN_POINT('Ctrl Pts',(70.8084394574491,-14.1088932111214,
0.));
#118488=CARTESIAN_POINT('Ctrl Pts',(70.787694227969,-14.0960939291568,0.));
#118489=CARTESIAN_POINT('Ctrl Pts',(70.7669720038067,-14.0833365416995,
0.));
#118490=CARTESIAN_POINT('Ctrl Pts',(70.7462729145799,-14.0706210588015,
0.));
#118491=CARTESIAN_POINT('Ctrl Pts',(70.7255970904433,-14.0579474904657,
0.));
#118492=CARTESIAN_POINT('Ctrl Pts',(70.7049446620931,-14.0453158466451,
0.));
#118493=CARTESIAN_POINT('Ctrl Pts',(70.6843157607672,-14.0327261372363,
0.));
#118494=CARTESIAN_POINT('Ctrl Pts',(70.6637105182487,-14.020178372077,0.));
#118495=CARTESIAN_POINT('Ctrl Pts',(70.6431290668744,-14.0076725609537,
0.));
#118496=CARTESIAN_POINT('Ctrl Pts',(70.6225715395392,-13.9952087136018,
0.));
#118497=CARTESIAN_POINT('Ctrl Pts',(70.6020380697004,-13.9827868397057,
0.));
#118498=CARTESIAN_POINT('Ctrl Pts',(70.5815287913791,-13.9704069488918,
0.));
#118499=CARTESIAN_POINT('Ctrl Pts',(70.5610438391622,-13.9580690507262,
0.));
#118500=CARTESIAN_POINT('Ctrl Pts',(70.5405833482123,-13.9457731547217,
0.));
#118501=CARTESIAN_POINT('Ctrl Pts',(70.5201474542717,-13.9335192703389,
0.));
#118502=CARTESIAN_POINT('Ctrl Pts',(70.4997362936671,-13.9213074069852,
0.));
#118503=CARTESIAN_POINT('Ctrl Pts',(70.4793500033106,-13.9091375740084,
0.));
#118504=CARTESIAN_POINT('Ctrl Pts',(70.4589887207043,-13.8970097806947,
0.));
#118505=CARTESIAN_POINT('Ctrl Pts',(70.4386525839492,-13.8849240362757,
0.));
#118506=CARTESIAN_POINT('Ctrl Pts',(70.4183417317486,-13.8728803499284,
0.));
#118507=CARTESIAN_POINT('Ctrl Pts',(70.3980563034142,-13.8608787307753,
0.));
#118508=CARTESIAN_POINT('Ctrl Pts',(70.377796438866,-13.8489191878774,0.));
#118509=CARTESIAN_POINT('Ctrl Pts',(70.3575622786373,-13.8370017302319,
0.));
#118510=CARTESIAN_POINT('Ctrl Pts',(70.3373539638841,-13.8251263667799,
0.));
#118511=CARTESIAN_POINT('Ctrl Pts',(70.3171716363912,-13.8132931064067,
0.));
#118512=CARTESIAN_POINT('Ctrl Pts',(70.2970154385763,-13.8015019579411,
0.));
#118513=CARTESIAN_POINT('Ctrl Pts',(70.2768855134909,-13.7897529301483,
0.));
#118514=CARTESIAN_POINT('Ctrl Pts',(70.2567820048253,-13.7780460317284,
0.));
#118515=CARTESIAN_POINT('Ctrl Pts',(70.2367050569174,-13.7663812713235,
0.));
#118516=CARTESIAN_POINT('Ctrl Pts',(70.216654814759,-13.7547586575178,0.));
#118517=CARTESIAN_POINT('Ctrl Pts',(70.1966314240012,-13.7431781988368,
0.));
#118518=CARTESIAN_POINT('Ctrl Pts',(70.1766350309554,-13.73163990374,0.));
#118519=CARTESIAN_POINT('Ctrl Pts',(70.1566657825989,-13.7201437806207,
0.));
#118520=CARTESIAN_POINT('Ctrl Pts',(70.1367238265853,-13.7086898378127,
0.));
#118521=CARTESIAN_POINT('Ctrl Pts',(70.1168093112493,-13.6972780835898,
0.));
#118522=CARTESIAN_POINT('Ctrl Pts',(70.0969223856123,-13.685908526165,0.));
#118523=CARTESIAN_POINT('Ctrl Pts',(70.0770631993831,-13.6745811736825,
0.));
#118524=CARTESIAN_POINT('Ctrl Pts',(70.057231902965,-13.6632960342192,0.));
#118525=CARTESIAN_POINT('Ctrl Pts',(70.037428647466,-13.6520531157904,0.));
#118526=CARTESIAN_POINT('Ctrl Pts',(70.0176535847047,-13.6408524263496,
0.));
#118527=CARTESIAN_POINT('Ctrl Pts',(69.9979068672163,-13.6296939737866,
0.));
#118528=CARTESIAN_POINT('Ctrl Pts',(69.9781886482543,-13.61857776592,0.));
#118529=CARTESIAN_POINT('Ctrl Pts',(69.9584990817989,-13.6075038105,0.));
#118530=CARTESIAN_POINT('Ctrl Pts',(69.9388383225655,-13.5964721152136,
0.));
#118531=CARTESIAN_POINT('Ctrl Pts',(69.9192065260107,-13.5854826876834,
0.));
#118532=CARTESIAN_POINT('Ctrl Pts',(69.899603848336,-13.5745355354657,0.));
#118533=CARTESIAN_POINT('Ctrl Pts',(69.880030446488,-13.5636306660422,0.));
#118534=CARTESIAN_POINT('Ctrl Pts',(69.8604864781705,-13.5527680868256,
0.));
#118535=CARTESIAN_POINT('Ctrl Pts',(69.840972101856,-13.5419478051626,0.));
#118536=CARTESIAN_POINT('Ctrl Pts',(69.8214874767944,-13.5311698283339,
0.));
#118537=CARTESIAN_POINT('Ctrl Pts',(69.8020327630204,-13.5204341635507,
0.));
#118538=CARTESIAN_POINT('Ctrl Pts',(69.7826081213575,-13.5097408179478,
0.));
#118539=CARTESIAN_POINT('Ctrl Pts',(69.7632137134247,-13.4990897985904,
0.));
#118540=CARTESIAN_POINT('Ctrl Pts',(69.7438497016404,-13.4884811124748,
0.));
#118541=CARTESIAN_POINT('Ctrl Pts',(69.7245162492251,-13.4779147665285,
0.));
#118542=CARTESIAN_POINT('Ctrl Pts',(69.7052135202003,-13.4673907676045,
0.));
#118543=CARTESIAN_POINT('Ctrl Pts',(69.6859416793898,-13.4569091224762,
0.));
#118544=CARTESIAN_POINT('Ctrl Pts',(69.6667008924454,-13.4464698378456,
0.));
#118545=CARTESIAN_POINT('Ctrl Pts',(69.6474913258684,-13.4360729203444,
0.));
#118546=CARTESIAN_POINT('Ctrl Pts',(69.6283131470267,-13.425718376534,0.));
#118547=CARTESIAN_POINT('Ctrl Pts',(69.6091665241743,-13.4154062128998,
0.));
#118548=CARTESIAN_POINT('Ctrl Pts',(69.5900516264524,-13.4051364358494,
0.));
#118549=CARTESIAN_POINT('Ctrl Pts',(69.5709686238701,-13.3949090517173,
0.));
#118550=CARTESIAN_POINT('Ctrl Pts',(69.5519176872857,-13.3847240667626,
0.));
#118551=CARTESIAN_POINT('Ctrl Pts',(69.5328989883899,-13.3745814871667,
0.));
#118552=CARTESIAN_POINT('Ctrl Pts',(69.5139126996703,-13.3644813190225,
0.));
#118553=CARTESIAN_POINT('Ctrl Pts',(69.4949589944633,-13.3544235683399,
0.));
#118554=CARTESIAN_POINT('Ctrl Pts',(69.4760380470382,-13.3444082410546,
0.));
#118555=CARTESIAN_POINT('Ctrl Pts',(69.4571500326673,-13.3344353430313,
0.));
#118556=CARTESIAN_POINT('Ctrl Pts',(69.4382951276983,-13.3245048800641,
0.));
#118557=CARTESIAN_POINT('Ctrl Pts',(69.4194735096238,-13.3146168578738,
0.));
#118558=CARTESIAN_POINT('Ctrl Pts',(69.4006853569485,-13.3047712821046,
0.));
#118559=CARTESIAN_POINT('Ctrl Pts',(69.3819308490408,-13.2949681583164,
0.));
#118560=CARTESIAN_POINT('Ctrl Pts',(69.3632101660072,-13.2852074919767,
0.));
#118561=CARTESIAN_POINT('Ctrl Pts',(69.3445234885088,-13.2754892884437,
0.));
#118562=CARTESIAN_POINT('Ctrl Pts',(69.3258709977416,-13.2658135529616,
0.));
#118563=CARTESIAN_POINT('Ctrl Pts',(69.3072528758546,-13.2561802906901,
0.));
#118564=CARTESIAN_POINT('Ctrl Pts',(69.2886693063193,-13.2465895067264,
0.));
#118565=CARTESIAN_POINT('Ctrl Pts',(69.2701204742436,-13.2370412061218,
0.));
#118566=CARTESIAN_POINT('Ctrl Pts',(69.2516065668809,-13.2275353939044,
0.));
#118567=CARTESIAN_POINT('Ctrl Pts',(69.2331277732819,-13.2180720750585,
0.));
#118568=CARTESIAN_POINT('Ctrl Pts',(69.2146842833506,-13.2086512544729,
0.));
#118569=CARTESIAN_POINT('Ctrl Pts',(69.1962762870524,-13.1992729368928,
0.));
#118570=CARTESIAN_POINT('Ctrl Pts',(69.1779039736026,-13.1899371268689,
0.));
#118571=CARTESIAN_POINT('Ctrl Pts',(69.1595675305294,-13.1806438286944,
0.));
#118572=CARTESIAN_POINT('Ctrl Pts',(69.141267145461,-13.1713930465142,0.));
#118573=CARTESIAN_POINT('Ctrl Pts',(69.1230030082597,-13.1621847844533,
0.));
#118574=CARTESIAN_POINT('Ctrl Pts',(69.1047753127633,-13.1530190467181,
0.));
#118575=CARTESIAN_POINT('Ctrl Pts',(69.0865842593063,-13.1438958377397,
0.));
#118576=CARTESIAN_POINT('Ctrl Pts',(69.0684300549426,-13.1348151621824,
0.));
#118577=CARTESIAN_POINT('Ctrl Pts',(69.0503129081778,-13.1257770246379,
0.));
#118578=CARTESIAN_POINT('Ctrl Pts',(69.0322330243336,-13.1167814293495,
0.));
#118579=CARTESIAN_POINT('Ctrl Pts',(69.0141906015137,-13.1078283799726,
0.));
#118580=CARTESIAN_POINT('Ctrl Pts',(68.9961858241577,-13.0989178791843,
0.));
#118581=CARTESIAN_POINT('Ctrl Pts',(68.9782188692654,-13.0900499290541,
0.));
#118582=CARTESIAN_POINT('Ctrl Pts',(68.9602899187628,-13.0812245317816,
0.));
#118583=CARTESIAN_POINT('Ctrl Pts',(68.9423991694493,-13.072441690283,0.));
#118584=CARTESIAN_POINT('Ctrl Pts',(68.9245468449865,-13.0637014089018,
0.));
#118585=CARTESIAN_POINT('Ctrl Pts',(68.9067332040842,-13.0550036938793,
0.));
#118586=CARTESIAN_POINT('Ctrl Pts',(68.8889585151431,-13.0463485518185,
0.));
#118587=CARTESIAN_POINT('Ctrl Pts',(68.8712230321823,-13.0377359881864,
0.));
#118588=CARTESIAN_POINT('Ctrl Pts',(68.8535269726871,-13.0291660060118,
0.));
#118589=CARTESIAN_POINT('Ctrl Pts',(68.835870488774,-13.0206386039729,0.));
#118590=CARTESIAN_POINT('Ctrl Pts',(68.8182536654067,-13.0121537769003,
0.));
#118591=CARTESIAN_POINT('Ctrl Pts',(68.8041919669403,-13.0053999700929,
0.));
#118592=CARTESIAN_POINT('Ctrl Pts',(68.7936635625788,-13.0003537683089,
0.));
#118593=CARTESIAN_POINT('Ctrl Pts',(68.7866525680284,-12.996998146029,0.));
#118594=CARTESIAN_POINT('Ctrl Pts',(68.7831490561748,-12.9953224629497,
0.));
#118595=CARTESIAN_POINT('Ctrl Pts',(71.2372871136136,-21.8059378310719,
0.));
#118596=CARTESIAN_POINT('Ctrl Pts',(71.2372871136136,-21.8059378310719,
12.));
#118597=CARTESIAN_POINT('Ctrl Pts',(71.2331134397872,-21.8022104901727,
0.));
#118598=CARTESIAN_POINT('Ctrl Pts',(71.2331134397872,-21.8022104901727,
12.));
#118599=CARTESIAN_POINT('Ctrl Pts',(71.2247670210176,-21.7947599798961,
0.));
#118600=CARTESIAN_POINT('Ctrl Pts',(71.2247670210176,-21.7947599798961,
12.));
#118601=CARTESIAN_POINT('Ctrl Pts',(71.2122501795138,-21.7835967290463,
0.));
#118602=CARTESIAN_POINT('Ctrl Pts',(71.2122501795138,-21.7835967290463,
12.));
#118603=CARTESIAN_POINT('Ctrl Pts',(71.1955666310295,-21.7687374247288,
0.));
#118604=CARTESIAN_POINT('Ctrl Pts',(71.1955666310295,-21.7687374247288,
12.));
#118605=CARTESIAN_POINT('Ctrl Pts',(71.1747214906585,-21.750205018381,0.));
#118606=CARTESIAN_POINT('Ctrl Pts',(71.1747214906585,-21.750205018381,12.));
#118607=CARTESIAN_POINT('Ctrl Pts',(71.1538856612261,-21.7317143472952,
0.));
#118608=CARTESIAN_POINT('Ctrl Pts',(71.1538856612261,-21.7317143472952,
12.));
#118609=CARTESIAN_POINT('Ctrl Pts',(71.1330591726506,-21.7132654262531,
0.));
#118610=CARTESIAN_POINT('Ctrl Pts',(71.1330591726506,-21.7132654262531,
12.));
#118611=CARTESIAN_POINT('Ctrl Pts',(71.1122420728216,-21.694858273085,0.));
#118612=CARTESIAN_POINT('Ctrl Pts',(71.1122420728216,-21.694858273085,12.));
#118613=CARTESIAN_POINT('Ctrl Pts',(71.0914344332798,-21.6764929081677,
0.));
#118614=CARTESIAN_POINT('Ctrl Pts',(71.0914344332798,-21.6764929081677,
12.));
#118615=CARTESIAN_POINT('Ctrl Pts',(71.0706363472704,-21.6581693538335,
0.));
#118616=CARTESIAN_POINT('Ctrl Pts',(71.0706363472704,-21.6581693538335,
12.));
#118617=CARTESIAN_POINT('Ctrl Pts',(71.0498479219467,-21.6398876337141,
0.));
#118618=CARTESIAN_POINT('Ctrl Pts',(71.0498479219467,-21.6398876337141,
12.));
#118619=CARTESIAN_POINT('Ctrl Pts',(71.0290692721847,-21.6216477720913,
0.));
#118620=CARTESIAN_POINT('Ctrl Pts',(71.0290692721847,-21.6216477720913,
12.));
#118621=CARTESIAN_POINT('Ctrl Pts',(71.0083005139107,-21.6034497932581,
0.));
#118622=CARTESIAN_POINT('Ctrl Pts',(71.0083005139107,-21.6034497932581,
12.));
#118623=CARTESIAN_POINT('Ctrl Pts',(70.987541757223,-21.585293720829,0.));
#118624=CARTESIAN_POINT('Ctrl Pts',(70.987541757223,-21.585293720829,12.));
#118625=CARTESIAN_POINT('Ctrl Pts',(70.9667931008215,-21.5671795771914,
0.));
#118626=CARTESIAN_POINT('Ctrl Pts',(70.9667931008215,-21.5671795771914,
12.));
#118627=CARTESIAN_POINT('Ctrl Pts',(70.94605463587,-21.5491073839106,0.));
#118628=CARTESIAN_POINT('Ctrl Pts',(70.94605463587,-21.5491073839106,12.));
#118629=CARTESIAN_POINT('Ctrl Pts',(70.9253264487636,-21.5310771620231,
0.));
#118630=CARTESIAN_POINT('Ctrl Pts',(70.9253264487636,-21.5310771620231,
12.));
#118631=CARTESIAN_POINT('Ctrl Pts',(70.9046086244131,-21.513088932377,0.));
#118632=CARTESIAN_POINT('Ctrl Pts',(70.9046086244131,-21.513088932377,12.));
#118633=CARTESIAN_POINT('Ctrl Pts',(70.8839012490871,-21.4951427159262,
0.));
#118634=CARTESIAN_POINT('Ctrl Pts',(70.8839012490871,-21.4951427159262,
12.));
#118635=CARTESIAN_POINT('Ctrl Pts',(70.8632044140112,-21.477238534096,0.));
#118636=CARTESIAN_POINT('Ctrl Pts',(70.8632044140112,-21.477238534096,12.));
#118637=CARTESIAN_POINT('Ctrl Pts',(70.8425182149846,-21.4593764087474,
0.));
#118638=CARTESIAN_POINT('Ctrl Pts',(70.8425182149846,-21.4593764087474,
12.));
#118639=CARTESIAN_POINT('Ctrl Pts',(70.8218427507506,-21.4415563620114,
0.));
#118640=CARTESIAN_POINT('Ctrl Pts',(70.8218427507506,-21.4415563620114,
12.));
#118641=CARTESIAN_POINT('Ctrl Pts',(70.8011781217394,-21.4237784161588,
0.));
#118642=CARTESIAN_POINT('Ctrl Pts',(70.8011781217394,-21.4237784161588,
12.));
#118643=CARTESIAN_POINT('Ctrl Pts',(70.780524428745,-21.4060425934599,0.));
#118644=CARTESIAN_POINT('Ctrl Pts',(70.780524428745,-21.4060425934599,12.));
#118645=CARTESIAN_POINT('Ctrl Pts',(70.7598817714105,-21.3883489160196,
0.));
#118646=CARTESIAN_POINT('Ctrl Pts',(70.7598817714105,-21.3883489160196,
12.));
#118647=CARTESIAN_POINT('Ctrl Pts',(70.7392502475469,-21.3706974057039,
0.));
#118648=CARTESIAN_POINT('Ctrl Pts',(70.7392502475469,-21.3706974057039,
12.));
#118649=CARTESIAN_POINT('Ctrl Pts',(70.7186299539724,-21.3530880842349,
0.));
#118650=CARTESIAN_POINT('Ctrl Pts',(70.7186299539724,-21.3530880842349,
12.));
#118651=CARTESIAN_POINT('Ctrl Pts',(70.6980209870044,-21.3355209732443,
0.));
#118652=CARTESIAN_POINT('Ctrl Pts',(70.6980209870044,-21.3355209732443,
12.));
#118653=CARTESIAN_POINT('Ctrl Pts',(70.6774234430897,-21.3179960943389,
0.));
#118654=CARTESIAN_POINT('Ctrl Pts',(70.6774234430897,-21.3179960943389,
12.));
#118655=CARTESIAN_POINT('Ctrl Pts',(70.6568374193774,-21.300513469156,0.));
#118656=CARTESIAN_POINT('Ctrl Pts',(70.6568374193774,-21.300513469156,12.));
#118657=CARTESIAN_POINT('Ctrl Pts',(70.6362630143047,-21.2830731194183,
0.));
#118658=CARTESIAN_POINT('Ctrl Pts',(70.6362630143047,-21.2830731194183,
12.));
#118659=CARTESIAN_POINT('Ctrl Pts',(70.6157003273316,-21.2656750669126,
0.));
#118660=CARTESIAN_POINT('Ctrl Pts',(70.6157003273316,-21.2656750669126,
12.));
#118661=CARTESIAN_POINT('Ctrl Pts',(70.5951494586957,-21.2483193334676,
0.));
#118662=CARTESIAN_POINT('Ctrl Pts',(70.5951494586957,-21.2483193334676,
12.));
#118663=CARTESIAN_POINT('Ctrl Pts',(70.5746105091502,-21.2310059409266,
0.));
#118664=CARTESIAN_POINT('Ctrl Pts',(70.5746105091502,-21.2310059409266,
12.));
#118665=CARTESIAN_POINT('Ctrl Pts',(70.5540835797283,-21.2137349111208,
0.));
#118666=CARTESIAN_POINT('Ctrl Pts',(70.5540835797283,-21.2137349111208,
12.));
#118667=CARTESIAN_POINT('Ctrl Pts',(70.5335687714428,-21.1965062658298,
0.));
#118668=CARTESIAN_POINT('Ctrl Pts',(70.5335687714428,-21.1965062658298,
12.));
#118669=CARTESIAN_POINT('Ctrl Pts',(70.5130661852955,-21.1793200267847,
0.));
#118670=CARTESIAN_POINT('Ctrl Pts',(70.5130661852955,-21.1793200267847,
12.));
#118671=CARTESIAN_POINT('Ctrl Pts',(70.4925759224216,-21.1621762156897,
0.));
#118672=CARTESIAN_POINT('Ctrl Pts',(70.4925759224216,-21.1621762156897,
12.));
#118673=CARTESIAN_POINT('Ctrl Pts',(70.4720980841939,-21.1450748542337,
0.));
#118674=CARTESIAN_POINT('Ctrl Pts',(70.4720980841939,-21.1450748542337,
12.));
#118675=CARTESIAN_POINT('Ctrl Pts',(70.4516327723346,-21.1280159641003,
0.));
#118676=CARTESIAN_POINT('Ctrl Pts',(70.4516327723346,-21.1280159641003,
12.));
#118677=CARTESIAN_POINT('Ctrl Pts',(70.4311800890401,-21.1109995669747,
0.));
#118678=CARTESIAN_POINT('Ctrl Pts',(70.4311800890401,-21.1109995669747,
12.));
#118679=CARTESIAN_POINT('Ctrl Pts',(70.4107401370389,-21.0940256845473,
0.));
#118680=CARTESIAN_POINT('Ctrl Pts',(70.4107401370389,-21.0940256845473,
12.));
#118681=CARTESIAN_POINT('Ctrl Pts',(70.3903130195264,-21.0770943385141,
0.));
#118682=CARTESIAN_POINT('Ctrl Pts',(70.3903130195264,-21.0770943385141,
12.));
#118683=CARTESIAN_POINT('Ctrl Pts',(70.3698988401281,-21.0602055505748,
0.));
#118684=CARTESIAN_POINT('Ctrl Pts',(70.3698988401281,-21.0602055505748,
12.));
#118685=CARTESIAN_POINT('Ctrl Pts',(70.3494977028498,-21.0433593424267,
0.));
#118686=CARTESIAN_POINT('Ctrl Pts',(70.3494977028498,-21.0433593424267,
12.));
#118687=CARTESIAN_POINT('Ctrl Pts',(70.3291097120302,-21.0265557357548,
0.));
#118688=CARTESIAN_POINT('Ctrl Pts',(70.3291097120302,-21.0265557357548,
12.));
#118689=CARTESIAN_POINT('Ctrl Pts',(70.3087349722973,-21.0097947522218,
0.));
#118690=CARTESIAN_POINT('Ctrl Pts',(70.3087349722973,-21.0097947522218,
12.));
#118691=CARTESIAN_POINT('Ctrl Pts',(70.2883735885984,-20.9930764134776,
0.));
#118692=CARTESIAN_POINT('Ctrl Pts',(70.2883735885984,-20.9930764134776,
12.));
#118693=CARTESIAN_POINT('Ctrl Pts',(70.2680256662224,-20.9764007411653,
0.));
#118694=CARTESIAN_POINT('Ctrl Pts',(70.2680256662224,-20.9764007411653,
12.));
#118695=CARTESIAN_POINT('Ctrl Pts',(70.2476913108244,-20.9597677569228,
0.));
#118696=CARTESIAN_POINT('Ctrl Pts',(70.2476913108244,-20.9597677569228,
12.));
#118697=CARTESIAN_POINT('Ctrl Pts',(70.2273706284472,-20.9431774823831,
0.));
#118698=CARTESIAN_POINT('Ctrl Pts',(70.2273706284472,-20.9431774823831,
12.));
#118699=CARTESIAN_POINT('Ctrl Pts',(70.2070637255458,-20.9266299391684,
0.));
#118700=CARTESIAN_POINT('Ctrl Pts',(70.2070637255458,-20.9266299391684,
12.));
#118701=CARTESIAN_POINT('Ctrl Pts',(70.1867707089854,-20.9101251488944,
0.));
#118702=CARTESIAN_POINT('Ctrl Pts',(70.1867707089854,-20.9101251488944,
12.));
#118703=CARTESIAN_POINT('Ctrl Pts',(70.1664916860358,-20.8936631331748,
0.));
#118704=CARTESIAN_POINT('Ctrl Pts',(70.1664916860358,-20.8936631331748,
12.));
#118705=CARTESIAN_POINT('Ctrl Pts',(70.1462267643646,-20.8772439136206,
0.));
#118706=CARTESIAN_POINT('Ctrl Pts',(70.1462267643646,-20.8772439136206,
12.));
#118707=CARTESIAN_POINT('Ctrl Pts',(70.1259760520309,-20.8608675118379,
0.));
#118708=CARTESIAN_POINT('Ctrl Pts',(70.1259760520309,-20.8608675118379,
12.));
#118709=CARTESIAN_POINT('Ctrl Pts',(70.1057396574747,-20.8445339494188,
0.));
#118710=CARTESIAN_POINT('Ctrl Pts',(70.1057396574747,-20.8445339494188,
12.));
#118711=CARTESIAN_POINT('Ctrl Pts',(70.0855176895191,-20.8282432479429,
0.));
#118712=CARTESIAN_POINT('Ctrl Pts',(70.0855176895191,-20.8282432479429,
12.));
#118713=CARTESIAN_POINT('Ctrl Pts',(70.0653102573803,-20.8119954289849,
0.));
#118714=CARTESIAN_POINT('Ctrl Pts',(70.0653102573803,-20.8119954289849,
12.));
#118715=CARTESIAN_POINT('Ctrl Pts',(70.0451174706741,-20.7957905141157,
0.));
#118716=CARTESIAN_POINT('Ctrl Pts',(70.0451174706741,-20.7957905141157,
12.));
#118717=CARTESIAN_POINT('Ctrl Pts',(70.024939439422,-20.7796285249022,0.));
#118718=CARTESIAN_POINT('Ctrl Pts',(70.024939439422,-20.7796285249022,12.));
#118719=CARTESIAN_POINT('Ctrl Pts',(70.0047762740568,-20.7635094829016,
0.));
#118720=CARTESIAN_POINT('Ctrl Pts',(70.0047762740568,-20.7635094829016,
12.));
#118721=CARTESIAN_POINT('Ctrl Pts',(69.9846280854257,-20.7474334096581,
0.));
#118722=CARTESIAN_POINT('Ctrl Pts',(69.9846280854257,-20.7474334096581,
12.));
#118723=CARTESIAN_POINT('Ctrl Pts',(69.9644949847934,-20.7314003267119,
0.));
#118724=CARTESIAN_POINT('Ctrl Pts',(69.9644949847934,-20.7314003267119,
12.));
#118725=CARTESIAN_POINT('Ctrl Pts',(69.9443770838448,-20.7154102555997,
0.));
#118726=CARTESIAN_POINT('Ctrl Pts',(69.9443770838448,-20.7154102555997,
12.));
#118727=CARTESIAN_POINT('Ctrl Pts',(69.9242744946854,-20.6994632178552,
0.));
#118728=CARTESIAN_POINT('Ctrl Pts',(69.9242744946854,-20.6994632178552,
12.));
#118729=CARTESIAN_POINT('Ctrl Pts',(69.904187329841,-20.683559235003,0.));
#118730=CARTESIAN_POINT('Ctrl Pts',(69.904187329841,-20.683559235003,12.));
#118731=CARTESIAN_POINT('Ctrl Pts',(69.8841157022567,-20.667698328554,0.));
#118732=CARTESIAN_POINT('Ctrl Pts',(69.8841157022567,-20.667698328554,12.));
#118733=CARTESIAN_POINT('Ctrl Pts',(69.8640597253045,-20.6518805200129,
0.));
#118734=CARTESIAN_POINT('Ctrl Pts',(69.8640597253045,-20.6518805200129,
12.));
#118735=CARTESIAN_POINT('Ctrl Pts',(69.8440195127866,-20.6361058308811,
0.));
#118736=CARTESIAN_POINT('Ctrl Pts',(69.8440195127866,-20.6361058308811,
12.));
#118737=CARTESIAN_POINT('Ctrl Pts',(69.8239951789402,-20.6203742826566,
0.));
#118738=CARTESIAN_POINT('Ctrl Pts',(69.8239951789402,-20.6203742826566,
12.));
#118739=CARTESIAN_POINT('Ctrl Pts',(69.8039868384389,-20.6046858968308,
0.));
#118740=CARTESIAN_POINT('Ctrl Pts',(69.8039868384389,-20.6046858968308,
12.));
#118741=CARTESIAN_POINT('Ctrl Pts',(69.7839946063949,-20.5890406948811,
0.));
#118742=CARTESIAN_POINT('Ctrl Pts',(69.7839946063949,-20.5890406948811,
12.));
#118743=CARTESIAN_POINT('Ctrl Pts',(69.7640185983644,-20.5734386982783,
0.));
#118744=CARTESIAN_POINT('Ctrl Pts',(69.7640185983644,-20.5734386982783,
12.));
#118745=CARTESIAN_POINT('Ctrl Pts',(69.744058930351,-20.5578799284898,0.));
#118746=CARTESIAN_POINT('Ctrl Pts',(69.744058930351,-20.5578799284898,12.));
#118747=CARTESIAN_POINT('Ctrl Pts',(69.7241157188083,-20.54236440698,0.));
#118748=CARTESIAN_POINT('Ctrl Pts',(69.7241157188083,-20.54236440698,12.));
#118749=CARTESIAN_POINT('Ctrl Pts',(69.7041890806424,-20.5268921552077,
0.));
#118750=CARTESIAN_POINT('Ctrl Pts',(69.7041890806424,-20.5268921552077,
12.));
#118751=CARTESIAN_POINT('Ctrl Pts',(69.6842791332115,-20.5114631946185,
0.));
#118752=CARTESIAN_POINT('Ctrl Pts',(69.6842791332115,-20.5114631946185,
12.));
#118753=CARTESIAN_POINT('Ctrl Pts',(69.6643859943308,-20.4960775466492,
0.));
#118754=CARTESIAN_POINT('Ctrl Pts',(69.6643859943308,-20.4960775466492,
12.));
#118755=CARTESIAN_POINT('Ctrl Pts',(69.6445097822792,-20.480735232734,0.));
#118756=CARTESIAN_POINT('Ctrl Pts',(69.6445097822792,-20.480735232734,12.));
#118757=CARTESIAN_POINT('Ctrl Pts',(69.6246506158013,-20.4654362743038,
0.));
#118758=CARTESIAN_POINT('Ctrl Pts',(69.6246506158013,-20.4654362743038,
12.));
#118759=CARTESIAN_POINT('Ctrl Pts',(69.6048086141113,-20.4501806927852,
0.));
#118760=CARTESIAN_POINT('Ctrl Pts',(69.6048086141113,-20.4501806927852,
12.));
#118761=CARTESIAN_POINT('Ctrl Pts',(69.5849838968928,-20.4349685095924,
0.));
#118762=CARTESIAN_POINT('Ctrl Pts',(69.5849838968928,-20.4349685095924,
12.));
#118763=CARTESIAN_POINT('Ctrl Pts',(69.5651765843033,-20.4197997461301,
0.));
#118764=CARTESIAN_POINT('Ctrl Pts',(69.5651765843033,-20.4197997461301,
12.));
#118765=CARTESIAN_POINT('Ctrl Pts',(69.5453867969804,-20.4046744237999,
0.));
#118766=CARTESIAN_POINT('Ctrl Pts',(69.5453867969804,-20.4046744237999,
12.));
#118767=CARTESIAN_POINT('Ctrl Pts',(69.5256146560441,-20.3895925640005,
0.));
#118768=CARTESIAN_POINT('Ctrl Pts',(69.5256146560441,-20.3895925640005,
12.));
#118769=CARTESIAN_POINT('Ctrl Pts',(69.5058602831008,-20.3745541881269,
0.));
#118770=CARTESIAN_POINT('Ctrl Pts',(69.5058602831008,-20.3745541881269,
12.));
#118771=CARTESIAN_POINT('Ctrl Pts',(69.4861238002441,-20.3595593175623,
0.));
#118772=CARTESIAN_POINT('Ctrl Pts',(69.4861238002441,-20.3595593175623,
12.));
#118773=CARTESIAN_POINT('Ctrl Pts',(69.4664053300587,-20.3446079736802,
0.));
#118774=CARTESIAN_POINT('Ctrl Pts',(69.4664053300587,-20.3446079736802,
12.));
#118775=CARTESIAN_POINT('Ctrl Pts',(69.4467049956262,-20.3297001778507,
0.));
#118776=CARTESIAN_POINT('Ctrl Pts',(69.4467049956262,-20.3297001778507,
12.));
#118777=CARTESIAN_POINT('Ctrl Pts',(69.4270229205296,-20.3148359514415,
0.));
#118778=CARTESIAN_POINT('Ctrl Pts',(69.4270229205296,-20.3148359514415,
12.));
#118779=CARTESIAN_POINT('Ctrl Pts',(69.407359228856,-20.3000153158167,0.));
#118780=CARTESIAN_POINT('Ctrl Pts',(69.407359228856,-20.3000153158167,12.));
#118781=CARTESIAN_POINT('Ctrl Pts',(69.3877140451975,-20.2852382923299,
0.));
#118782=CARTESIAN_POINT('Ctrl Pts',(69.3877140451975,-20.2852382923299,
12.));
#118783=CARTESIAN_POINT('Ctrl Pts',(69.368087494655,-20.2705049023241,0.));
#118784=CARTESIAN_POINT('Ctrl Pts',(69.368087494655,-20.2705049023241,12.));
#118785=CARTESIAN_POINT('Ctrl Pts',(69.3484797028458,-20.2558151671391,
0.));
#118786=CARTESIAN_POINT('Ctrl Pts',(69.3484797028458,-20.2558151671391,
12.));
#118787=CARTESIAN_POINT('Ctrl Pts',(69.3288907959067,-20.2411691081123,
0.));
#118788=CARTESIAN_POINT('Ctrl Pts',(69.3288907959067,-20.2411691081123,
12.));
#118789=CARTESIAN_POINT('Ctrl Pts',(69.3093209004984,-20.2265667465784,
0.));
#118790=CARTESIAN_POINT('Ctrl Pts',(69.3093209004984,-20.2265667465784,
12.));
#118791=CARTESIAN_POINT('Ctrl Pts',(69.2897701438059,-20.2120081038621,
0.));
#118792=CARTESIAN_POINT('Ctrl Pts',(69.2897701438059,-20.2120081038621,
12.));
#118793=CARTESIAN_POINT('Ctrl Pts',(69.2702386535422,-20.1974932012773,
0.));
#118794=CARTESIAN_POINT('Ctrl Pts',(69.2702386535422,-20.1974932012773,
12.));
#118795=CARTESIAN_POINT('Ctrl Pts',(69.2507265579554,-20.1830220601349,
0.));
#118796=CARTESIAN_POINT('Ctrl Pts',(69.2507265579554,-20.1830220601349,
12.));
#118797=CARTESIAN_POINT('Ctrl Pts',(69.2312339858335,-20.1685947017433,
0.));
#118798=CARTESIAN_POINT('Ctrl Pts',(69.2312339858335,-20.1685947017433,
12.));
#118799=CARTESIAN_POINT('Ctrl Pts',(69.2117610665076,-20.1542111474087,
0.));
#118800=CARTESIAN_POINT('Ctrl Pts',(69.2117610665076,-20.1542111474087,
12.));
#118801=CARTESIAN_POINT('Ctrl Pts',(69.1923079298538,-20.139871418428,0.));
#118802=CARTESIAN_POINT('Ctrl Pts',(69.1923079298538,-20.139871418428,12.));
#118803=CARTESIAN_POINT('Ctrl Pts',(69.1728747062963,-20.1255755360872,
0.));
#118804=CARTESIAN_POINT('Ctrl Pts',(69.1728747062963,-20.1255755360872,
12.));
#118805=CARTESIAN_POINT('Ctrl Pts',(69.1534615268152,-20.1113235216694,
0.));
#118806=CARTESIAN_POINT('Ctrl Pts',(69.1534615268152,-20.1113235216694,
12.));
#118807=CARTESIAN_POINT('Ctrl Pts',(69.1340685229514,-20.0971153964557,
0.));
#118808=CARTESIAN_POINT('Ctrl Pts',(69.1340685229514,-20.0971153964557,
12.));
#118809=CARTESIAN_POINT('Ctrl Pts',(69.1146958268104,-20.0829511817251,
0.));
#118810=CARTESIAN_POINT('Ctrl Pts',(69.1146958268104,-20.0829511817251,
12.));
#118811=CARTESIAN_POINT('Ctrl Pts',(69.095343571064,-20.068830898748,0.));
#118812=CARTESIAN_POINT('Ctrl Pts',(69.095343571064,-20.068830898748,12.));
#118813=CARTESIAN_POINT('Ctrl Pts',(69.0760118889535,-20.0547545687842,
0.));
#118814=CARTESIAN_POINT('Ctrl Pts',(69.0760118889535,-20.0547545687842,
12.));
#118815=CARTESIAN_POINT('Ctrl Pts',(69.0567009142978,-20.0407222130906,
0.));
#118816=CARTESIAN_POINT('Ctrl Pts',(69.0567009142978,-20.0407222130906,
12.));
#118817=CARTESIAN_POINT('Ctrl Pts',(69.0374107814984,-20.0267338529223,
0.));
#118818=CARTESIAN_POINT('Ctrl Pts',(69.0374107814984,-20.0267338529223,
12.));
#118819=CARTESIAN_POINT('Ctrl Pts',(69.0181416255431,-20.0127895095327,
0.));
#118820=CARTESIAN_POINT('Ctrl Pts',(69.0181416255431,-20.0127895095327,
12.));
#118821=CARTESIAN_POINT('Ctrl Pts',(68.9988935820084,-19.9988892041666,
0.));
#118822=CARTESIAN_POINT('Ctrl Pts',(68.9988935820084,-19.9988892041666,
12.));
#118823=CARTESIAN_POINT('Ctrl Pts',(68.9796667870638,-19.9850329580591,
0.));
#118824=CARTESIAN_POINT('Ctrl Pts',(68.9796667870638,-19.9850329580591,
12.));
#118825=CARTESIAN_POINT('Ctrl Pts',(68.9604613774802,-19.9712207924429,
0.));
#118826=CARTESIAN_POINT('Ctrl Pts',(68.9604613774802,-19.9712207924429,
12.));
#118827=CARTESIAN_POINT('Ctrl Pts',(68.9412774906333,-19.9574527285488,
0.));
#118828=CARTESIAN_POINT('Ctrl Pts',(68.9412774906333,-19.9574527285488,
12.));
#118829=CARTESIAN_POINT('Ctrl Pts',(68.9221152645095,-19.9437287876066,
0.));
#118830=CARTESIAN_POINT('Ctrl Pts',(68.9221152645095,-19.9437287876066,
12.));
#118831=CARTESIAN_POINT('Ctrl Pts',(68.9029748377067,-19.9300489908374,
0.));
#118832=CARTESIAN_POINT('Ctrl Pts',(68.9029748377067,-19.9300489908374,
12.));
#118833=CARTESIAN_POINT('Ctrl Pts',(68.8838563494393,-19.9164133594526,
0.));
#118834=CARTESIAN_POINT('Ctrl Pts',(68.8838563494393,-19.9164133594526,
12.));
#118835=CARTESIAN_POINT('Ctrl Pts',(68.8647599395469,-19.9028219146618,
0.));
#118836=CARTESIAN_POINT('Ctrl Pts',(68.8647599395469,-19.9028219146618,
12.));
#118837=CARTESIAN_POINT('Ctrl Pts',(68.8456857485002,-19.8892746776739,
0.));
#118838=CARTESIAN_POINT('Ctrl Pts',(68.8456857485002,-19.8892746776739,
12.));
#118839=CARTESIAN_POINT('Ctrl Pts',(68.8266339174056,-19.8757716696966,
0.));
#118840=CARTESIAN_POINT('Ctrl Pts',(68.8266339174056,-19.8757716696966,
12.));
#118841=CARTESIAN_POINT('Ctrl Pts',(68.8076045880065,-19.8623129119293,
0.));
#118842=CARTESIAN_POINT('Ctrl Pts',(68.8076045880065,-19.8623129119293,
12.));
#118843=CARTESIAN_POINT('Ctrl Pts',(68.7885979026878,-19.8488984255627,
0.));
#118844=CARTESIAN_POINT('Ctrl Pts',(68.7885979026878,-19.8488984255627,
12.));
#118845=CARTESIAN_POINT('Ctrl Pts',(68.7696140044851,-19.8355282317858,
0.));
#118846=CARTESIAN_POINT('Ctrl Pts',(68.7696140044851,-19.8355282317858,
12.));
#118847=CARTESIAN_POINT('Ctrl Pts',(68.7506530370904,-19.8222023517871,
0.));
#118848=CARTESIAN_POINT('Ctrl Pts',(68.7506530370904,-19.8222023517871,
12.));
#118849=CARTESIAN_POINT('Ctrl Pts',(68.7317151448573,-19.8089208067538,
0.));
#118850=CARTESIAN_POINT('Ctrl Pts',(68.7317151448573,-19.8089208067538,
12.));
#118851=CARTESIAN_POINT('Ctrl Pts',(68.7128004728033,-19.7956836178651,
0.));
#118852=CARTESIAN_POINT('Ctrl Pts',(68.7128004728033,-19.7956836178651,
12.));
#118853=CARTESIAN_POINT('Ctrl Pts',(68.6939091666149,-19.7824908062925,
0.));
#118854=CARTESIAN_POINT('Ctrl Pts',(68.6939091666149,-19.7824908062925,
12.));
#118855=CARTESIAN_POINT('Ctrl Pts',(68.6750413726574,-19.7693423932067,
0.));
#118856=CARTESIAN_POINT('Ctrl Pts',(68.6750413726574,-19.7693423932067,
12.));
#118857=CARTESIAN_POINT('Ctrl Pts',(68.65619723798,-19.7562383997784,0.));
#118858=CARTESIAN_POINT('Ctrl Pts',(68.65619723798,-19.7562383997784,12.));
#118859=CARTESIAN_POINT('Ctrl Pts',(68.6373769103211,-19.7431788471773,
0.));
#118860=CARTESIAN_POINT('Ctrl Pts',(68.6373769103211,-19.7431788471773,
12.));
#118861=CARTESIAN_POINT('Ctrl Pts',(68.6185805381102,-19.7301637565646,
0.));
#118862=CARTESIAN_POINT('Ctrl Pts',(68.6185805381102,-19.7301637565646,
12.));
#118863=CARTESIAN_POINT('Ctrl Pts',(68.5998082704741,-19.717193149095,0.));
#118864=CARTESIAN_POINT('Ctrl Pts',(68.5998082704741,-19.717193149095,12.));
#118865=CARTESIAN_POINT('Ctrl Pts',(68.5810602572474,-19.7042670459234,
0.));
#118866=CARTESIAN_POINT('Ctrl Pts',(68.5810602572474,-19.7042670459234,
12.));
#118867=CARTESIAN_POINT('Ctrl Pts',(68.5623366489776,-19.6913854682046,
0.));
#118868=CARTESIAN_POINT('Ctrl Pts',(68.5623366489776,-19.6913854682046,
12.));
#118869=CARTESIAN_POINT('Ctrl Pts',(68.543637596932,-19.6785484370929,0.));
#118870=CARTESIAN_POINT('Ctrl Pts',(68.543637596932,-19.6785484370929,12.));
#118871=CARTESIAN_POINT('Ctrl Pts',(68.5249632530994,-19.665755973734,0.));
#118872=CARTESIAN_POINT('Ctrl Pts',(68.5249632530994,-19.665755973734,12.));
#118873=CARTESIAN_POINT('Ctrl Pts',(68.5063137701986,-19.653008099269,0.));
#118874=CARTESIAN_POINT('Ctrl Pts',(68.5063137701986,-19.653008099269,12.));
#118875=CARTESIAN_POINT('Ctrl Pts',(68.4876893016863,-19.6403048348397,
0.));
#118876=CARTESIAN_POINT('Ctrl Pts',(68.4876893016863,-19.6403048348397,
12.));
#118877=CARTESIAN_POINT('Ctrl Pts',(68.4690900017631,-19.6276462015888,
0.));
#118878=CARTESIAN_POINT('Ctrl Pts',(68.4690900017631,-19.6276462015888,
12.));
#118879=CARTESIAN_POINT('Ctrl Pts',(68.4505160253777,-19.6150322206578,
0.));
#118880=CARTESIAN_POINT('Ctrl Pts',(68.4505160253777,-19.6150322206578,
12.));
#118881=CARTESIAN_POINT('Ctrl Pts',(68.4319675282273,-19.6024629131786,
0.));
#118882=CARTESIAN_POINT('Ctrl Pts',(68.4319675282273,-19.6024629131786,
12.));
#118883=CARTESIAN_POINT('Ctrl Pts',(68.4134446667695,-19.5899383002804,
0.));
#118884=CARTESIAN_POINT('Ctrl Pts',(68.4134446667695,-19.5899383002804,
12.));
#118885=CARTESIAN_POINT('Ctrl Pts',(68.3949475982334,-19.5774584030939,
0.));
#118886=CARTESIAN_POINT('Ctrl Pts',(68.3949475982334,-19.5774584030939,
12.));
#118887=CARTESIAN_POINT('Ctrl Pts',(68.3764764806287,-19.5650232427516,
0.));
#118888=CARTESIAN_POINT('Ctrl Pts',(68.3764764806287,-19.5650232427516,
12.));
#118889=CARTESIAN_POINT('Ctrl Pts',(68.3580314727522,-19.5526328403852,
0.));
#118890=CARTESIAN_POINT('Ctrl Pts',(68.3580314727522,-19.5526328403852,
12.));
#118891=CARTESIAN_POINT('Ctrl Pts',(68.3396127341937,-19.540287217119,0.));
#118892=CARTESIAN_POINT('Ctrl Pts',(68.3396127341937,-19.540287217119,12.));
#118893=CARTESIAN_POINT('Ctrl Pts',(68.3212204253415,-19.5279863940773,
0.));
#118894=CARTESIAN_POINT('Ctrl Pts',(68.3212204253415,-19.5279863940773,
12.));
#118895=CARTESIAN_POINT('Ctrl Pts',(68.3028547073862,-19.5157303923856,
0.));
#118896=CARTESIAN_POINT('Ctrl Pts',(68.3028547073862,-19.5157303923856,
12.));
#118897=CARTESIAN_POINT('Ctrl Pts',(68.2845157423233,-19.5035192331706,
0.));
#118898=CARTESIAN_POINT('Ctrl Pts',(68.2845157423233,-19.5035192331706,
12.));
#118899=CARTESIAN_POINT('Ctrl Pts',(68.2662036929531,-19.4913529375546,
0.));
#118900=CARTESIAN_POINT('Ctrl Pts',(68.2662036929531,-19.4913529375546,
12.));
#118901=CARTESIAN_POINT('Ctrl Pts',(68.2479187228815,-19.4792315266505,
0.));
#118902=CARTESIAN_POINT('Ctrl Pts',(68.2479187228815,-19.4792315266505,
12.));
#118903=CARTESIAN_POINT('Ctrl Pts',(68.2296609965461,-19.4671550215725,
0.));
#118904=CARTESIAN_POINT('Ctrl Pts',(68.2296609965461,-19.4671550215725,
12.));
#118905=CARTESIAN_POINT('Ctrl Pts',(68.2114306792366,-19.4551234434384,
0.));
#118906=CARTESIAN_POINT('Ctrl Pts',(68.2114306792366,-19.4551234434384,
12.));
#118907=CARTESIAN_POINT('Ctrl Pts',(68.193227937112,-19.4431368133718,0.));
#118908=CARTESIAN_POINT('Ctrl Pts',(68.193227937112,-19.4431368133718,12.));
#118909=CARTESIAN_POINT('Ctrl Pts',(68.1750529372211,-19.4311951524977,
0.));
#118910=CARTESIAN_POINT('Ctrl Pts',(68.1750529372211,-19.4311951524977,
12.));
#118911=CARTESIAN_POINT('Ctrl Pts',(68.1569058475026,-19.4192984819411,
0.));
#118912=CARTESIAN_POINT('Ctrl Pts',(68.1569058475026,-19.4192984819411,
12.));
#118913=CARTESIAN_POINT('Ctrl Pts',(68.1387868367668,-19.4074468228294,
0.));
#118914=CARTESIAN_POINT('Ctrl Pts',(68.1387868367668,-19.4074468228294,
12.));
#118915=CARTESIAN_POINT('Ctrl Pts',(68.1206960746763,-19.3956401962894,
0.));
#118916=CARTESIAN_POINT('Ctrl Pts',(68.1206960746763,-19.3956401962894,
12.));
#118917=CARTESIAN_POINT('Ctrl Pts',(68.1026337317298,-19.3838786234426,
0.));
#118918=CARTESIAN_POINT('Ctrl Pts',(68.1026337317298,-19.3838786234426,
12.));
#118919=CARTESIAN_POINT('Ctrl Pts',(68.0845999792274,-19.3721621253921,
0.));
#118920=CARTESIAN_POINT('Ctrl Pts',(68.0845999792274,-19.3721621253921,
12.));
#118921=CARTESIAN_POINT('Ctrl Pts',(68.0665949893221,-19.3604907232322,
0.));
#118922=CARTESIAN_POINT('Ctrl Pts',(68.0665949893221,-19.3604907232322,
12.));
#118923=CARTESIAN_POINT('Ctrl Pts',(68.0486189351027,-19.3488644380646,
0.));
#118924=CARTESIAN_POINT('Ctrl Pts',(68.0486189351027,-19.3488644380646,
12.));
#118925=CARTESIAN_POINT('Ctrl Pts',(68.0306719906636,-19.3372832910077,
0.));
#118926=CARTESIAN_POINT('Ctrl Pts',(68.0306719906636,-19.3372832910077,
12.));
#118927=CARTESIAN_POINT('Ctrl Pts',(68.0127543311761,-19.3257473032031,
0.));
#118928=CARTESIAN_POINT('Ctrl Pts',(68.0127543311761,-19.3257473032031,
12.));
#118929=CARTESIAN_POINT('Ctrl Pts',(67.9948661329591,-19.3142564958196,
0.));
#118930=CARTESIAN_POINT('Ctrl Pts',(67.9948661329591,-19.3142564958196,
12.));
#118931=CARTESIAN_POINT('Ctrl Pts',(67.977007573346,-19.3028108900374,0.));
#118932=CARTESIAN_POINT('Ctrl Pts',(67.977007573346,-19.3028108900374,12.));
#118933=CARTESIAN_POINT('Ctrl Pts',(67.959178830538,-19.2914105070283,0.));
#118934=CARTESIAN_POINT('Ctrl Pts',(67.959178830538,-19.2914105070283,12.));
#118935=CARTESIAN_POINT('Ctrl Pts',(67.9413800834798,-19.2800553679362,
0.));
#118936=CARTESIAN_POINT('Ctrl Pts',(67.9413800834798,-19.2800553679362,
12.));
#118937=CARTESIAN_POINT('Ctrl Pts',(67.9236115116781,-19.2687454938449,
0.));
#118938=CARTESIAN_POINT('Ctrl Pts',(67.9236115116781,-19.2687454938449,
12.));
#118939=CARTESIAN_POINT('Ctrl Pts',(67.9058732951822,-19.2574809057705,
0.));
#118940=CARTESIAN_POINT('Ctrl Pts',(67.9058732951822,-19.2574809057705,
12.));
#118941=CARTESIAN_POINT('Ctrl Pts',(67.8881656149983,-19.2462616247287,
0.));
#118942=CARTESIAN_POINT('Ctrl Pts',(67.8881656149983,-19.2462616247287,
12.));
#118943=CARTESIAN_POINT('Ctrl Pts',(67.8704886534555,-19.2350876717878,
0.));
#118944=CARTESIAN_POINT('Ctrl Pts',(67.8704886534555,-19.2350876717878,
12.));
#118945=CARTESIAN_POINT('Ctrl Pts',(67.852842594517,-19.223959068113,0.));
#118946=CARTESIAN_POINT('Ctrl Pts',(67.852842594517,-19.223959068113,12.));
#118947=CARTESIAN_POINT('Ctrl Pts',(67.8352276242856,-19.2128758350336,
0.));
#118948=CARTESIAN_POINT('Ctrl Pts',(67.8352276242856,-19.2128758350336,
12.));
#118949=CARTESIAN_POINT('Ctrl Pts',(67.817643930658,-19.2018379939918,0.));
#118950=CARTESIAN_POINT('Ctrl Pts',(67.817643930658,-19.2018379939918,12.));
#118951=CARTESIAN_POINT('Ctrl Pts',(67.8000917023896,-19.1908455664089,
0.));
#118952=CARTESIAN_POINT('Ctrl Pts',(67.8000917023896,-19.1908455664089,
12.));
#118953=CARTESIAN_POINT('Ctrl Pts',(67.7825711283092,-19.1798985735687,
0.));
#118954=CARTESIAN_POINT('Ctrl Pts',(67.7825711283092,-19.1798985735687,
12.));
#118955=CARTESIAN_POINT('Ctrl Pts',(67.7650823965156,-19.1689970364959,
0.));
#118956=CARTESIAN_POINT('Ctrl Pts',(67.7650823965156,-19.1689970364959,
12.));
#118957=CARTESIAN_POINT('Ctrl Pts',(67.7476256934492,-19.1581409758112,
0.));
#118958=CARTESIAN_POINT('Ctrl Pts',(67.7476256934492,-19.1581409758112,
12.));
#118959=CARTESIAN_POINT('Ctrl Pts',(67.7302012056629,-19.1473304119969,
0.));
#118960=CARTESIAN_POINT('Ctrl Pts',(67.7302012056629,-19.1473304119969,
12.));
#118961=CARTESIAN_POINT('Ctrl Pts',(67.7128091219372,-19.1365653657098,
0.));
#118962=CARTESIAN_POINT('Ctrl Pts',(67.7128091219372,-19.1365653657098,
12.));
#118963=CARTESIAN_POINT('Ctrl Pts',(67.6954496350053,-19.1258458580343,
0.));
#118964=CARTESIAN_POINT('Ctrl Pts',(67.6954496350053,-19.1258458580343,
12.));
#118965=CARTESIAN_POINT('Ctrl Pts',(67.6781229440535,-19.115171910845,0.));
#118966=CARTESIAN_POINT('Ctrl Pts',(67.6781229440535,-19.115171910845,12.));
#118967=CARTESIAN_POINT('Ctrl Pts',(67.6608292549412,-19.1045435468345,
0.));
#118968=CARTESIAN_POINT('Ctrl Pts',(67.6608292549412,-19.1045435468345,
12.));
#118969=CARTESIAN_POINT('Ctrl Pts',(67.6435687749802,-19.0939607887492,
0.));
#118970=CARTESIAN_POINT('Ctrl Pts',(67.6435687749802,-19.0939607887492,
12.));
#118971=CARTESIAN_POINT('Ctrl Pts',(67.6263417083413,-19.0834236587115,
0.));
#118972=CARTESIAN_POINT('Ctrl Pts',(67.6263417083413,-19.0834236587115,
12.));
#118973=CARTESIAN_POINT('Ctrl Pts',(67.6091482520557,-19.0729321776287,
0.));
#118974=CARTESIAN_POINT('Ctrl Pts',(67.6091482520557,-19.0729321776287,
12.));
#118975=CARTESIAN_POINT('Ctrl Pts',(67.5919885896278,-19.0624863642425,
0.));
#118976=CARTESIAN_POINT('Ctrl Pts',(67.5919885896278,-19.0624863642425,
12.));
#118977=CARTESIAN_POINT('Ctrl Pts',(67.5748628972035,-19.0520862360414,
0.));
#118978=CARTESIAN_POINT('Ctrl Pts',(67.5748628972035,-19.0520862360414,
12.));
#118979=CARTESIAN_POINT('Ctrl Pts',(67.5577713558248,-19.0417318110721,
0.));
#118980=CARTESIAN_POINT('Ctrl Pts',(67.5577713558248,-19.0417318110721,
12.));
#118981=CARTESIAN_POINT('Ctrl Pts',(67.540714161288,-19.0314231093924,0.));
#118982=CARTESIAN_POINT('Ctrl Pts',(67.540714161288,-19.0314231093924,12.));
#118983=CARTESIAN_POINT('Ctrl Pts',(67.5236915360253,-19.0211601548222,
0.));
#118984=CARTESIAN_POINT('Ctrl Pts',(67.5236915360253,-19.0211601548222,
12.));
#118985=CARTESIAN_POINT('Ctrl Pts',(67.5067037372177,-19.0109429761274,
0.));
#118986=CARTESIAN_POINT('Ctrl Pts',(67.5067037372177,-19.0109429761274,
12.));
#118987=CARTESIAN_POINT('Ctrl Pts',(67.4897510316692,-19.0007716032785,
0.));
#118988=CARTESIAN_POINT('Ctrl Pts',(67.4897510316692,-19.0007716032785,
12.));
#118989=CARTESIAN_POINT('Ctrl Pts',(67.4728336719558,-18.9906460638607,
0.));
#118990=CARTESIAN_POINT('Ctrl Pts',(67.4728336719558,-18.9906460638607,
12.));
#118991=CARTESIAN_POINT('Ctrl Pts',(67.4559518744713,-18.9805663798466,
0.));
#118992=CARTESIAN_POINT('Ctrl Pts',(67.4559518744713,-18.9805663798466,
12.));
#118993=CARTESIAN_POINT('Ctrl Pts',(67.4391057908687,-18.9705325631773,
0.));
#118994=CARTESIAN_POINT('Ctrl Pts',(67.4391057908687,-18.9705325631773,
12.));
#118995=CARTESIAN_POINT('Ctrl Pts',(67.4222955062384,-18.9605446161079,
0.));
#118996=CARTESIAN_POINT('Ctrl Pts',(67.4222955062384,-18.9605446161079,
12.));
#118997=CARTESIAN_POINT('Ctrl Pts',(67.4088759498287,-18.9525909518003,
0.));
#118998=CARTESIAN_POINT('Ctrl Pts',(67.4088759498287,-18.9525909518003,
12.));
#118999=CARTESIAN_POINT('Ctrl Pts',(67.398827414689,-18.9466463414355,0.));
#119000=CARTESIAN_POINT('Ctrl Pts',(67.398827414689,-18.9466463414355,12.));
#119001=CARTESIAN_POINT('Ctrl Pts',(67.3921355608417,-18.942692439874,0.));
#119002=CARTESIAN_POINT('Ctrl Pts',(67.3921355608417,-18.942692439874,12.));
#119003=CARTESIAN_POINT('Ctrl Pts',(67.3887914263118,-18.9407177820969,
0.));
#119004=CARTESIAN_POINT('Ctrl Pts',(67.3887914263118,-18.9407177820969,
12.));
#119005=CARTESIAN_POINT('',(67.3887914263118,-18.9407177820969,12.));
#119006=CARTESIAN_POINT('Ctrl Pts',(67.3887914263118,-18.9407177820969,
12.));
#119007=CARTESIAN_POINT('Ctrl Pts',(67.3921355608417,-18.942692439874,12.));
#119008=CARTESIAN_POINT('Ctrl Pts',(67.398827414689,-18.9466463414355,12.));
#119009=CARTESIAN_POINT('Ctrl Pts',(67.4088759498287,-18.9525909518003,
12.));
#119010=CARTESIAN_POINT('Ctrl Pts',(67.4222955062384,-18.9605446161079,
12.));
#119011=CARTESIAN_POINT('Ctrl Pts',(67.4391057908687,-18.9705325631773,
12.));
#119012=CARTESIAN_POINT('Ctrl Pts',(67.4559518744713,-18.9805663798466,
12.));
#119013=CARTESIAN_POINT('Ctrl Pts',(67.4728336719558,-18.9906460638607,
12.));
#119014=CARTESIAN_POINT('Ctrl Pts',(67.4897510316692,-19.0007716032785,
12.));
#119015=CARTESIAN_POINT('Ctrl Pts',(67.5067037372177,-19.0109429761274,
12.));
#119016=CARTESIAN_POINT('Ctrl Pts',(67.5236915360253,-19.0211601548222,
12.));
#119017=CARTESIAN_POINT('Ctrl Pts',(67.540714161288,-19.0314231093924,12.));
#119018=CARTESIAN_POINT('Ctrl Pts',(67.5577713558248,-19.0417318110721,
12.));
#119019=CARTESIAN_POINT('Ctrl Pts',(67.5748628972035,-19.0520862360414,
12.));
#119020=CARTESIAN_POINT('Ctrl Pts',(67.5919885896278,-19.0624863642425,
12.));
#119021=CARTESIAN_POINT('Ctrl Pts',(67.6091482520557,-19.0729321776287,
12.));
#119022=CARTESIAN_POINT('Ctrl Pts',(67.6263417083413,-19.0834236587115,
12.));
#119023=CARTESIAN_POINT('Ctrl Pts',(67.6435687749802,-19.0939607887492,
12.));
#119024=CARTESIAN_POINT('Ctrl Pts',(67.6608292549412,-19.1045435468345,
12.));
#119025=CARTESIAN_POINT('Ctrl Pts',(67.6781229440535,-19.115171910845,12.));
#119026=CARTESIAN_POINT('Ctrl Pts',(67.6954496350053,-19.1258458580343,
12.));
#119027=CARTESIAN_POINT('Ctrl Pts',(67.7128091219372,-19.1365653657098,
12.));
#119028=CARTESIAN_POINT('Ctrl Pts',(67.7302012056629,-19.1473304119969,
12.));
#119029=CARTESIAN_POINT('Ctrl Pts',(67.7476256934492,-19.1581409758112,
12.));
#119030=CARTESIAN_POINT('Ctrl Pts',(67.7650823965156,-19.1689970364959,
12.));
#119031=CARTESIAN_POINT('Ctrl Pts',(67.7825711283092,-19.1798985735687,
12.));
#119032=CARTESIAN_POINT('Ctrl Pts',(67.8000917023896,-19.1908455664089,
12.));
#119033=CARTESIAN_POINT('Ctrl Pts',(67.817643930658,-19.2018379939918,12.));
#119034=CARTESIAN_POINT('Ctrl Pts',(67.8352276242856,-19.2128758350336,
12.));
#119035=CARTESIAN_POINT('Ctrl Pts',(67.852842594517,-19.223959068113,12.));
#119036=CARTESIAN_POINT('Ctrl Pts',(67.8704886534555,-19.2350876717878,
12.));
#119037=CARTESIAN_POINT('Ctrl Pts',(67.8881656149983,-19.2462616247287,
12.));
#119038=CARTESIAN_POINT('Ctrl Pts',(67.9058732951822,-19.2574809057705,
12.));
#119039=CARTESIAN_POINT('Ctrl Pts',(67.9236115116781,-19.2687454938449,
12.));
#119040=CARTESIAN_POINT('Ctrl Pts',(67.9413800834798,-19.2800553679362,
12.));
#119041=CARTESIAN_POINT('Ctrl Pts',(67.959178830538,-19.2914105070283,12.));
#119042=CARTESIAN_POINT('Ctrl Pts',(67.977007573346,-19.3028108900374,12.));
#119043=CARTESIAN_POINT('Ctrl Pts',(67.9948661329591,-19.3142564958196,
12.));
#119044=CARTESIAN_POINT('Ctrl Pts',(68.0127543311761,-19.3257473032031,
12.));
#119045=CARTESIAN_POINT('Ctrl Pts',(68.0306719906636,-19.3372832910077,
12.));
#119046=CARTESIAN_POINT('Ctrl Pts',(68.0486189351027,-19.3488644380646,
12.));
#119047=CARTESIAN_POINT('Ctrl Pts',(68.0665949893221,-19.3604907232322,
12.));
#119048=CARTESIAN_POINT('Ctrl Pts',(68.0845999792274,-19.3721621253921,
12.));
#119049=CARTESIAN_POINT('Ctrl Pts',(68.1026337317298,-19.3838786234426,
12.));
#119050=CARTESIAN_POINT('Ctrl Pts',(68.1206960746763,-19.3956401962894,
12.));
#119051=CARTESIAN_POINT('Ctrl Pts',(68.1387868367668,-19.4074468228294,
12.));
#119052=CARTESIAN_POINT('Ctrl Pts',(68.1569058475026,-19.4192984819411,
12.));
#119053=CARTESIAN_POINT('Ctrl Pts',(68.1750529372211,-19.4311951524977,
12.));
#119054=CARTESIAN_POINT('Ctrl Pts',(68.193227937112,-19.4431368133718,12.));
#119055=CARTESIAN_POINT('Ctrl Pts',(68.2114306792366,-19.4551234434384,
12.));
#119056=CARTESIAN_POINT('Ctrl Pts',(68.2296609965461,-19.4671550215725,
12.));
#119057=CARTESIAN_POINT('Ctrl Pts',(68.2479187228815,-19.4792315266505,
12.));
#119058=CARTESIAN_POINT('Ctrl Pts',(68.2662036929531,-19.4913529375546,
12.));
#119059=CARTESIAN_POINT('Ctrl Pts',(68.2845157423233,-19.5035192331706,
12.));
#119060=CARTESIAN_POINT('Ctrl Pts',(68.3028547073862,-19.5157303923856,
12.));
#119061=CARTESIAN_POINT('Ctrl Pts',(68.3212204253415,-19.5279863940773,
12.));
#119062=CARTESIAN_POINT('Ctrl Pts',(68.3396127341937,-19.540287217119,12.));
#119063=CARTESIAN_POINT('Ctrl Pts',(68.3580314727522,-19.5526328403852,
12.));
#119064=CARTESIAN_POINT('Ctrl Pts',(68.3764764806287,-19.5650232427516,
12.));
#119065=CARTESIAN_POINT('Ctrl Pts',(68.3949475982334,-19.5774584030939,
12.));
#119066=CARTESIAN_POINT('Ctrl Pts',(68.4134446667695,-19.5899383002804,
12.));
#119067=CARTESIAN_POINT('Ctrl Pts',(68.4319675282273,-19.6024629131786,
12.));
#119068=CARTESIAN_POINT('Ctrl Pts',(68.4505160253777,-19.6150322206578,
12.));
#119069=CARTESIAN_POINT('Ctrl Pts',(68.4690900017631,-19.6276462015888,
12.));
#119070=CARTESIAN_POINT('Ctrl Pts',(68.4876893016863,-19.6403048348397,
12.));
#119071=CARTESIAN_POINT('Ctrl Pts',(68.5063137701986,-19.653008099269,12.));
#119072=CARTESIAN_POINT('Ctrl Pts',(68.5249632530994,-19.665755973734,12.));
#119073=CARTESIAN_POINT('Ctrl Pts',(68.543637596932,-19.6785484370929,12.));
#119074=CARTESIAN_POINT('Ctrl Pts',(68.5623366489776,-19.6913854682046,
12.));
#119075=CARTESIAN_POINT('Ctrl Pts',(68.5810602572474,-19.7042670459234,
12.));
#119076=CARTESIAN_POINT('Ctrl Pts',(68.5998082704741,-19.717193149095,12.));
#119077=CARTESIAN_POINT('Ctrl Pts',(68.6185805381102,-19.7301637565646,
12.));
#119078=CARTESIAN_POINT('Ctrl Pts',(68.6373769103211,-19.7431788471773,
12.));
#119079=CARTESIAN_POINT('Ctrl Pts',(68.65619723798,-19.7562383997784,12.));
#119080=CARTESIAN_POINT('Ctrl Pts',(68.6750413726574,-19.7693423932067,
12.));
#119081=CARTESIAN_POINT('Ctrl Pts',(68.6939091666149,-19.7824908062925,
12.));
#119082=CARTESIAN_POINT('Ctrl Pts',(68.7128004728033,-19.7956836178651,
12.));
#119083=CARTESIAN_POINT('Ctrl Pts',(68.7317151448573,-19.8089208067538,
12.));
#119084=CARTESIAN_POINT('Ctrl Pts',(68.7506530370904,-19.8222023517871,
12.));
#119085=CARTESIAN_POINT('Ctrl Pts',(68.7696140044851,-19.8355282317858,
12.));
#119086=CARTESIAN_POINT('Ctrl Pts',(68.7885979026878,-19.8488984255627,
12.));
#119087=CARTESIAN_POINT('Ctrl Pts',(68.8076045880065,-19.8623129119293,
12.));
#119088=CARTESIAN_POINT('Ctrl Pts',(68.8266339174056,-19.8757716696966,
12.));
#119089=CARTESIAN_POINT('Ctrl Pts',(68.8456857485002,-19.8892746776739,
12.));
#119090=CARTESIAN_POINT('Ctrl Pts',(68.8647599395469,-19.9028219146618,
12.));
#119091=CARTESIAN_POINT('Ctrl Pts',(68.8838563494393,-19.9164133594526,
12.));
#119092=CARTESIAN_POINT('Ctrl Pts',(68.9029748377067,-19.9300489908374,
12.));
#119093=CARTESIAN_POINT('Ctrl Pts',(68.9221152645095,-19.9437287876066,
12.));
#119094=CARTESIAN_POINT('Ctrl Pts',(68.9412774906333,-19.9574527285488,
12.));
#119095=CARTESIAN_POINT('Ctrl Pts',(68.9604613774802,-19.9712207924429,
12.));
#119096=CARTESIAN_POINT('Ctrl Pts',(68.9796667870638,-19.9850329580591,
12.));
#119097=CARTESIAN_POINT('Ctrl Pts',(68.9988935820084,-19.9988892041666,
12.));
#119098=CARTESIAN_POINT('Ctrl Pts',(69.0181416255431,-20.0127895095327,
12.));
#119099=CARTESIAN_POINT('Ctrl Pts',(69.0374107814984,-20.0267338529223,
12.));
#119100=CARTESIAN_POINT('Ctrl Pts',(69.0567009142978,-20.0407222130906,
12.));
#119101=CARTESIAN_POINT('Ctrl Pts',(69.0760118889535,-20.0547545687842,
12.));
#119102=CARTESIAN_POINT('Ctrl Pts',(69.095343571064,-20.068830898748,12.));
#119103=CARTESIAN_POINT('Ctrl Pts',(69.1146958268104,-20.0829511817251,
12.));
#119104=CARTESIAN_POINT('Ctrl Pts',(69.1340685229514,-20.0971153964557,
12.));
#119105=CARTESIAN_POINT('Ctrl Pts',(69.1534615268152,-20.1113235216694,
12.));
#119106=CARTESIAN_POINT('Ctrl Pts',(69.1728747062963,-20.1255755360872,
12.));
#119107=CARTESIAN_POINT('Ctrl Pts',(69.1923079298538,-20.139871418428,12.));
#119108=CARTESIAN_POINT('Ctrl Pts',(69.2117610665076,-20.1542111474087,
12.));
#119109=CARTESIAN_POINT('Ctrl Pts',(69.2312339858335,-20.1685947017433,
12.));
#119110=CARTESIAN_POINT('Ctrl Pts',(69.2507265579554,-20.1830220601349,
12.));
#119111=CARTESIAN_POINT('Ctrl Pts',(69.2702386535422,-20.1974932012773,
12.));
#119112=CARTESIAN_POINT('Ctrl Pts',(69.2897701438059,-20.2120081038621,
12.));
#119113=CARTESIAN_POINT('Ctrl Pts',(69.3093209004984,-20.2265667465784,
12.));
#119114=CARTESIAN_POINT('Ctrl Pts',(69.3288907959067,-20.2411691081123,
12.));
#119115=CARTESIAN_POINT('Ctrl Pts',(69.3484797028458,-20.2558151671391,
12.));
#119116=CARTESIAN_POINT('Ctrl Pts',(69.368087494655,-20.2705049023241,12.));
#119117=CARTESIAN_POINT('Ctrl Pts',(69.3877140451975,-20.2852382923299,
12.));
#119118=CARTESIAN_POINT('Ctrl Pts',(69.407359228856,-20.3000153158167,12.));
#119119=CARTESIAN_POINT('Ctrl Pts',(69.4270229205296,-20.3148359514415,
12.));
#119120=CARTESIAN_POINT('Ctrl Pts',(69.4467049956262,-20.3297001778507,
12.));
#119121=CARTESIAN_POINT('Ctrl Pts',(69.4664053300587,-20.3446079736802,
12.));
#119122=CARTESIAN_POINT('Ctrl Pts',(69.4861238002441,-20.3595593175623,
12.));
#119123=CARTESIAN_POINT('Ctrl Pts',(69.5058602831008,-20.3745541881269,
12.));
#119124=CARTESIAN_POINT('Ctrl Pts',(69.5256146560441,-20.3895925640005,
12.));
#119125=CARTESIAN_POINT('Ctrl Pts',(69.5453867969804,-20.4046744237999,
12.));
#119126=CARTESIAN_POINT('Ctrl Pts',(69.5651765843033,-20.4197997461301,
12.));
#119127=CARTESIAN_POINT('Ctrl Pts',(69.5849838968928,-20.4349685095924,
12.));
#119128=CARTESIAN_POINT('Ctrl Pts',(69.6048086141113,-20.4501806927852,
12.));
#119129=CARTESIAN_POINT('Ctrl Pts',(69.6246506158013,-20.4654362743038,
12.));
#119130=CARTESIAN_POINT('Ctrl Pts',(69.6445097822792,-20.480735232734,12.));
#119131=CARTESIAN_POINT('Ctrl Pts',(69.6643859943308,-20.4960775466492,
12.));
#119132=CARTESIAN_POINT('Ctrl Pts',(69.6842791332115,-20.5114631946185,
12.));
#119133=CARTESIAN_POINT('Ctrl Pts',(69.7041890806424,-20.5268921552077,
12.));
#119134=CARTESIAN_POINT('Ctrl Pts',(69.7241157188083,-20.54236440698,12.));
#119135=CARTESIAN_POINT('Ctrl Pts',(69.744058930351,-20.5578799284898,12.));
#119136=CARTESIAN_POINT('Ctrl Pts',(69.7640185983644,-20.5734386982783,
12.));
#119137=CARTESIAN_POINT('Ctrl Pts',(69.7839946063949,-20.5890406948811,
12.));
#119138=CARTESIAN_POINT('Ctrl Pts',(69.8039868384389,-20.6046858968308,
12.));
#119139=CARTESIAN_POINT('Ctrl Pts',(69.8239951789402,-20.6203742826566,
12.));
#119140=CARTESIAN_POINT('Ctrl Pts',(69.8440195127866,-20.6361058308811,
12.));
#119141=CARTESIAN_POINT('Ctrl Pts',(69.8640597253045,-20.6518805200129,
12.));
#119142=CARTESIAN_POINT('Ctrl Pts',(69.8841157022567,-20.667698328554,12.));
#119143=CARTESIAN_POINT('Ctrl Pts',(69.904187329841,-20.683559235003,12.));
#119144=CARTESIAN_POINT('Ctrl Pts',(69.9242744946854,-20.6994632178552,
12.));
#119145=CARTESIAN_POINT('Ctrl Pts',(69.9443770838448,-20.7154102555997,
12.));
#119146=CARTESIAN_POINT('Ctrl Pts',(69.9644949847934,-20.7314003267119,
12.));
#119147=CARTESIAN_POINT('Ctrl Pts',(69.9846280854257,-20.7474334096581,
12.));
#119148=CARTESIAN_POINT('Ctrl Pts',(70.0047762740568,-20.7635094829016,
12.));
#119149=CARTESIAN_POINT('Ctrl Pts',(70.024939439422,-20.7796285249022,12.));
#119150=CARTESIAN_POINT('Ctrl Pts',(70.0451174706741,-20.7957905141157,
12.));
#119151=CARTESIAN_POINT('Ctrl Pts',(70.0653102573803,-20.8119954289849,
12.));
#119152=CARTESIAN_POINT('Ctrl Pts',(70.0855176895191,-20.8282432479429,
12.));
#119153=CARTESIAN_POINT('Ctrl Pts',(70.1057396574747,-20.8445339494188,
12.));
#119154=CARTESIAN_POINT('Ctrl Pts',(70.1259760520309,-20.8608675118379,
12.));
#119155=CARTESIAN_POINT('Ctrl Pts',(70.1462267643646,-20.8772439136206,
12.));
#119156=CARTESIAN_POINT('Ctrl Pts',(70.1664916860358,-20.8936631331748,
12.));
#119157=CARTESIAN_POINT('Ctrl Pts',(70.1867707089854,-20.9101251488944,
12.));
#119158=CARTESIAN_POINT('Ctrl Pts',(70.2070637255458,-20.9266299391684,
12.));
#119159=CARTESIAN_POINT('Ctrl Pts',(70.2273706284472,-20.9431774823831,
12.));
#119160=CARTESIAN_POINT('Ctrl Pts',(70.2476913108244,-20.9597677569228,
12.));
#119161=CARTESIAN_POINT('Ctrl Pts',(70.2680256662224,-20.9764007411653,
12.));
#119162=CARTESIAN_POINT('Ctrl Pts',(70.2883735885984,-20.9930764134776,
12.));
#119163=CARTESIAN_POINT('Ctrl Pts',(70.3087349722973,-21.0097947522218,
12.));
#119164=CARTESIAN_POINT('Ctrl Pts',(70.3291097120302,-21.0265557357548,
12.));
#119165=CARTESIAN_POINT('Ctrl Pts',(70.3494977028498,-21.0433593424267,
12.));
#119166=CARTESIAN_POINT('Ctrl Pts',(70.3698988401281,-21.0602055505748,
12.));
#119167=CARTESIAN_POINT('Ctrl Pts',(70.3903130195264,-21.0770943385141,
12.));
#119168=CARTESIAN_POINT('Ctrl Pts',(70.4107401370389,-21.0940256845473,
12.));
#119169=CARTESIAN_POINT('Ctrl Pts',(70.4311800890401,-21.1109995669747,
12.));
#119170=CARTESIAN_POINT('Ctrl Pts',(70.4516327723346,-21.1280159641003,
12.));
#119171=CARTESIAN_POINT('Ctrl Pts',(70.4720980841939,-21.1450748542337,
12.));
#119172=CARTESIAN_POINT('Ctrl Pts',(70.4925759224216,-21.1621762156897,
12.));
#119173=CARTESIAN_POINT('Ctrl Pts',(70.5130661852955,-21.1793200267847,
12.));
#119174=CARTESIAN_POINT('Ctrl Pts',(70.5335687714428,-21.1965062658298,
12.));
#119175=CARTESIAN_POINT('Ctrl Pts',(70.5540835797283,-21.2137349111208,
12.));
#119176=CARTESIAN_POINT('Ctrl Pts',(70.5746105091502,-21.2310059409266,
12.));
#119177=CARTESIAN_POINT('Ctrl Pts',(70.5951494586957,-21.2483193334676,
12.));
#119178=CARTESIAN_POINT('Ctrl Pts',(70.6157003273316,-21.2656750669126,
12.));
#119179=CARTESIAN_POINT('Ctrl Pts',(70.6362630143047,-21.2830731194183,
12.));
#119180=CARTESIAN_POINT('Ctrl Pts',(70.6568374193774,-21.300513469156,12.));
#119181=CARTESIAN_POINT('Ctrl Pts',(70.6774234430897,-21.3179960943389,
12.));
#119182=CARTESIAN_POINT('Ctrl Pts',(70.6980209870044,-21.3355209732443,
12.));
#119183=CARTESIAN_POINT('Ctrl Pts',(70.7186299539724,-21.3530880842349,
12.));
#119184=CARTESIAN_POINT('Ctrl Pts',(70.7392502475469,-21.3706974057039,
12.));
#119185=CARTESIAN_POINT('Ctrl Pts',(70.7598817714105,-21.3883489160196,
12.));
#119186=CARTESIAN_POINT('Ctrl Pts',(70.780524428745,-21.4060425934599,12.));
#119187=CARTESIAN_POINT('Ctrl Pts',(70.8011781217394,-21.4237784161588,
12.));
#119188=CARTESIAN_POINT('Ctrl Pts',(70.8218427507506,-21.4415563620114,
12.));
#119189=CARTESIAN_POINT('Ctrl Pts',(70.8425182149846,-21.4593764087474,
12.));
#119190=CARTESIAN_POINT('Ctrl Pts',(70.8632044140112,-21.477238534096,12.));
#119191=CARTESIAN_POINT('Ctrl Pts',(70.8839012490871,-21.4951427159262,
12.));
#119192=CARTESIAN_POINT('Ctrl Pts',(70.9046086244131,-21.513088932377,12.));
#119193=CARTESIAN_POINT('Ctrl Pts',(70.9253264487636,-21.5310771620231,
12.));
#119194=CARTESIAN_POINT('Ctrl Pts',(70.94605463587,-21.5491073839106,12.));
#119195=CARTESIAN_POINT('Ctrl Pts',(70.9638315189817,-21.564598755537,12.));
#119196=CARTESIAN_POINT('Ctrl Pts',(70.9774662112589,-21.5764983366482,
12.));
#119197=CARTESIAN_POINT('Ctrl Pts',(70.9869541808056,-21.5847875433333,
12.));
#119198=CARTESIAN_POINT('Ctrl Pts',(70.9922924595369,-21.5894540925585,
12.));
#119199=CARTESIAN_POINT('Ctrl Pts',(70.9934796069117,-21.5904919935063,
12.));
#119200=CARTESIAN_POINT('',(67.3887914263118,-18.9407177820969,0.));
#119201=CARTESIAN_POINT('',(67.3887914263118,-18.9407177820969,0.));
#119202=CARTESIAN_POINT('Ctrl Pts',(70.9934796069117,-21.5904919935063,
0.));
#119203=CARTESIAN_POINT('Ctrl Pts',(70.9922924595369,-21.5894540925585,
0.));
#119204=CARTESIAN_POINT('Ctrl Pts',(70.9869541808056,-21.5847875433333,
0.));
#119205=CARTESIAN_POINT('Ctrl Pts',(70.9774662112589,-21.5764983366482,
0.));
#119206=CARTESIAN_POINT('Ctrl Pts',(70.9638315189817,-21.564598755537,0.));
#119207=CARTESIAN_POINT('Ctrl Pts',(70.94605463587,-21.5491073839106,0.));
#119208=CARTESIAN_POINT('Ctrl Pts',(70.9253264487636,-21.5310771620231,
0.));
#119209=CARTESIAN_POINT('Ctrl Pts',(70.9046086244131,-21.513088932377,0.));
#119210=CARTESIAN_POINT('Ctrl Pts',(70.8839012490871,-21.4951427159262,
0.));
#119211=CARTESIAN_POINT('Ctrl Pts',(70.8632044140112,-21.477238534096,0.));
#119212=CARTESIAN_POINT('Ctrl Pts',(70.8425182149846,-21.4593764087474,
0.));
#119213=CARTESIAN_POINT('Ctrl Pts',(70.8218427507506,-21.4415563620114,
0.));
#119214=CARTESIAN_POINT('Ctrl Pts',(70.8011781217394,-21.4237784161588,
0.));
#119215=CARTESIAN_POINT('Ctrl Pts',(70.780524428745,-21.4060425934599,0.));
#119216=CARTESIAN_POINT('Ctrl Pts',(70.7598817714105,-21.3883489160196,
0.));
#119217=CARTESIAN_POINT('Ctrl Pts',(70.7392502475469,-21.3706974057039,
0.));
#119218=CARTESIAN_POINT('Ctrl Pts',(70.7186299539724,-21.3530880842349,
0.));
#119219=CARTESIAN_POINT('Ctrl Pts',(70.6980209870044,-21.3355209732443,
0.));
#119220=CARTESIAN_POINT('Ctrl Pts',(70.6774234430897,-21.3179960943389,
0.));
#119221=CARTESIAN_POINT('Ctrl Pts',(70.6568374193774,-21.300513469156,0.));
#119222=CARTESIAN_POINT('Ctrl Pts',(70.6362630143047,-21.2830731194183,
0.));
#119223=CARTESIAN_POINT('Ctrl Pts',(70.6157003273316,-21.2656750669126,
0.));
#119224=CARTESIAN_POINT('Ctrl Pts',(70.5951494586957,-21.2483193334676,
0.));
#119225=CARTESIAN_POINT('Ctrl Pts',(70.5746105091502,-21.2310059409266,
0.));
#119226=CARTESIAN_POINT('Ctrl Pts',(70.5540835797283,-21.2137349111208,
0.));
#119227=CARTESIAN_POINT('Ctrl Pts',(70.5335687714428,-21.1965062658298,
0.));
#119228=CARTESIAN_POINT('Ctrl Pts',(70.5130661852955,-21.1793200267847,
0.));
#119229=CARTESIAN_POINT('Ctrl Pts',(70.4925759224216,-21.1621762156897,
0.));
#119230=CARTESIAN_POINT('Ctrl Pts',(70.4720980841939,-21.1450748542337,
0.));
#119231=CARTESIAN_POINT('Ctrl Pts',(70.4516327723346,-21.1280159641003,
0.));
#119232=CARTESIAN_POINT('Ctrl Pts',(70.4311800890401,-21.1109995669747,
0.));
#119233=CARTESIAN_POINT('Ctrl Pts',(70.4107401370389,-21.0940256845473,
0.));
#119234=CARTESIAN_POINT('Ctrl Pts',(70.3903130195264,-21.0770943385141,
0.));
#119235=CARTESIAN_POINT('Ctrl Pts',(70.3698988401281,-21.0602055505748,
0.));
#119236=CARTESIAN_POINT('Ctrl Pts',(70.3494977028498,-21.0433593424267,
0.));
#119237=CARTESIAN_POINT('Ctrl Pts',(70.3291097120302,-21.0265557357548,
0.));
#119238=CARTESIAN_POINT('Ctrl Pts',(70.3087349722973,-21.0097947522218,
0.));
#119239=CARTESIAN_POINT('Ctrl Pts',(70.2883735885984,-20.9930764134776,
0.));
#119240=CARTESIAN_POINT('Ctrl Pts',(70.2680256662224,-20.9764007411653,
0.));
#119241=CARTESIAN_POINT('Ctrl Pts',(70.2476913108244,-20.9597677569228,
0.));
#119242=CARTESIAN_POINT('Ctrl Pts',(70.2273706284472,-20.9431774823831,
0.));
#119243=CARTESIAN_POINT('Ctrl Pts',(70.2070637255458,-20.9266299391684,
0.));
#119244=CARTESIAN_POINT('Ctrl Pts',(70.1867707089854,-20.9101251488944,
0.));
#119245=CARTESIAN_POINT('Ctrl Pts',(70.1664916860358,-20.8936631331748,
0.));
#119246=CARTESIAN_POINT('Ctrl Pts',(70.1462267643646,-20.8772439136206,
0.));
#119247=CARTESIAN_POINT('Ctrl Pts',(70.1259760520309,-20.8608675118379,
0.));
#119248=CARTESIAN_POINT('Ctrl Pts',(70.1057396574747,-20.8445339494188,
0.));
#119249=CARTESIAN_POINT('Ctrl Pts',(70.0855176895191,-20.8282432479429,
0.));
#119250=CARTESIAN_POINT('Ctrl Pts',(70.0653102573803,-20.8119954289849,
0.));
#119251=CARTESIAN_POINT('Ctrl Pts',(70.0451174706741,-20.7957905141157,
0.));
#119252=CARTESIAN_POINT('Ctrl Pts',(70.024939439422,-20.7796285249022,0.));
#119253=CARTESIAN_POINT('Ctrl Pts',(70.0047762740568,-20.7635094829016,
0.));
#119254=CARTESIAN_POINT('Ctrl Pts',(69.9846280854257,-20.7474334096581,
0.));
#119255=CARTESIAN_POINT('Ctrl Pts',(69.9644949847934,-20.7314003267119,
0.));
#119256=CARTESIAN_POINT('Ctrl Pts',(69.9443770838448,-20.7154102555997,
0.));
#119257=CARTESIAN_POINT('Ctrl Pts',(69.9242744946854,-20.6994632178552,
0.));
#119258=CARTESIAN_POINT('Ctrl Pts',(69.904187329841,-20.683559235003,0.));
#119259=CARTESIAN_POINT('Ctrl Pts',(69.8841157022567,-20.667698328554,0.));
#119260=CARTESIAN_POINT('Ctrl Pts',(69.8640597253045,-20.6518805200129,
0.));
#119261=CARTESIAN_POINT('Ctrl Pts',(69.8440195127866,-20.6361058308811,
0.));
#119262=CARTESIAN_POINT('Ctrl Pts',(69.8239951789402,-20.6203742826566,
0.));
#119263=CARTESIAN_POINT('Ctrl Pts',(69.8039868384389,-20.6046858968308,
0.));
#119264=CARTESIAN_POINT('Ctrl Pts',(69.7839946063949,-20.5890406948811,
0.));
#119265=CARTESIAN_POINT('Ctrl Pts',(69.7640185983644,-20.5734386982783,
0.));
#119266=CARTESIAN_POINT('Ctrl Pts',(69.744058930351,-20.5578799284898,0.));
#119267=CARTESIAN_POINT('Ctrl Pts',(69.7241157188083,-20.54236440698,0.));
#119268=CARTESIAN_POINT('Ctrl Pts',(69.7041890806424,-20.5268921552077,
0.));
#119269=CARTESIAN_POINT('Ctrl Pts',(69.6842791332115,-20.5114631946185,
0.));
#119270=CARTESIAN_POINT('Ctrl Pts',(69.6643859943308,-20.4960775466492,
0.));
#119271=CARTESIAN_POINT('Ctrl Pts',(69.6445097822792,-20.480735232734,0.));
#119272=CARTESIAN_POINT('Ctrl Pts',(69.6246506158013,-20.4654362743038,
0.));
#119273=CARTESIAN_POINT('Ctrl Pts',(69.6048086141113,-20.4501806927852,
0.));
#119274=CARTESIAN_POINT('Ctrl Pts',(69.5849838968928,-20.4349685095924,
0.));
#119275=CARTESIAN_POINT('Ctrl Pts',(69.5651765843033,-20.4197997461301,
0.));
#119276=CARTESIAN_POINT('Ctrl Pts',(69.5453867969804,-20.4046744237999,
0.));
#119277=CARTESIAN_POINT('Ctrl Pts',(69.5256146560441,-20.3895925640005,
0.));
#119278=CARTESIAN_POINT('Ctrl Pts',(69.5058602831008,-20.3745541881269,
0.));
#119279=CARTESIAN_POINT('Ctrl Pts',(69.4861238002441,-20.3595593175623,
0.));
#119280=CARTESIAN_POINT('Ctrl Pts',(69.4664053300587,-20.3446079736802,
0.));
#119281=CARTESIAN_POINT('Ctrl Pts',(69.4467049956262,-20.3297001778507,
0.));
#119282=CARTESIAN_POINT('Ctrl Pts',(69.4270229205296,-20.3148359514415,
0.));
#119283=CARTESIAN_POINT('Ctrl Pts',(69.407359228856,-20.3000153158167,0.));
#119284=CARTESIAN_POINT('Ctrl Pts',(69.3877140451975,-20.2852382923299,
0.));
#119285=CARTESIAN_POINT('Ctrl Pts',(69.368087494655,-20.2705049023241,0.));
#119286=CARTESIAN_POINT('Ctrl Pts',(69.3484797028458,-20.2558151671391,
0.));
#119287=CARTESIAN_POINT('Ctrl Pts',(69.3288907959067,-20.2411691081123,
0.));
#119288=CARTESIAN_POINT('Ctrl Pts',(69.3093209004984,-20.2265667465784,
0.));
#119289=CARTESIAN_POINT('Ctrl Pts',(69.2897701438059,-20.2120081038621,
0.));
#119290=CARTESIAN_POINT('Ctrl Pts',(69.2702386535422,-20.1974932012773,
0.));
#119291=CARTESIAN_POINT('Ctrl Pts',(69.2507265579554,-20.1830220601349,
0.));
#119292=CARTESIAN_POINT('Ctrl Pts',(69.2312339858335,-20.1685947017433,
0.));
#119293=CARTESIAN_POINT('Ctrl Pts',(69.2117610665076,-20.1542111474087,
0.));
#119294=CARTESIAN_POINT('Ctrl Pts',(69.1923079298538,-20.139871418428,0.));
#119295=CARTESIAN_POINT('Ctrl Pts',(69.1728747062963,-20.1255755360872,
0.));
#119296=CARTESIAN_POINT('Ctrl Pts',(69.1534615268152,-20.1113235216694,
0.));
#119297=CARTESIAN_POINT('Ctrl Pts',(69.1340685229514,-20.0971153964557,
0.));
#119298=CARTESIAN_POINT('Ctrl Pts',(69.1146958268104,-20.0829511817251,
0.));
#119299=CARTESIAN_POINT('Ctrl Pts',(69.095343571064,-20.068830898748,0.));
#119300=CARTESIAN_POINT('Ctrl Pts',(69.0760118889535,-20.0547545687842,
0.));
#119301=CARTESIAN_POINT('Ctrl Pts',(69.0567009142978,-20.0407222130906,
0.));
#119302=CARTESIAN_POINT('Ctrl Pts',(69.0374107814984,-20.0267338529223,
0.));
#119303=CARTESIAN_POINT('Ctrl Pts',(69.0181416255431,-20.0127895095327,
0.));
#119304=CARTESIAN_POINT('Ctrl Pts',(68.9988935820084,-19.9988892041666,
0.));
#119305=CARTESIAN_POINT('Ctrl Pts',(68.9796667870638,-19.9850329580591,
0.));
#119306=CARTESIAN_POINT('Ctrl Pts',(68.9604613774802,-19.9712207924429,
0.));
#119307=CARTESIAN_POINT('Ctrl Pts',(68.9412774906333,-19.9574527285488,
0.));
#119308=CARTESIAN_POINT('Ctrl Pts',(68.9221152645095,-19.9437287876066,
0.));
#119309=CARTESIAN_POINT('Ctrl Pts',(68.9029748377067,-19.9300489908374,
0.));
#119310=CARTESIAN_POINT('Ctrl Pts',(68.8838563494393,-19.9164133594526,
0.));
#119311=CARTESIAN_POINT('Ctrl Pts',(68.8647599395469,-19.9028219146618,
0.));
#119312=CARTESIAN_POINT('Ctrl Pts',(68.8456857485002,-19.8892746776739,
0.));
#119313=CARTESIAN_POINT('Ctrl Pts',(68.8266339174056,-19.8757716696966,
0.));
#119314=CARTESIAN_POINT('Ctrl Pts',(68.8076045880065,-19.8623129119293,
0.));
#119315=CARTESIAN_POINT('Ctrl Pts',(68.7885979026878,-19.8488984255627,
0.));
#119316=CARTESIAN_POINT('Ctrl Pts',(68.7696140044851,-19.8355282317858,
0.));
#119317=CARTESIAN_POINT('Ctrl Pts',(68.7506530370904,-19.8222023517871,
0.));
#119318=CARTESIAN_POINT('Ctrl Pts',(68.7317151448573,-19.8089208067538,
0.));
#119319=CARTESIAN_POINT('Ctrl Pts',(68.7128004728033,-19.7956836178651,
0.));
#119320=CARTESIAN_POINT('Ctrl Pts',(68.6939091666149,-19.7824908062925,
0.));
#119321=CARTESIAN_POINT('Ctrl Pts',(68.6750413726574,-19.7693423932067,
0.));
#119322=CARTESIAN_POINT('Ctrl Pts',(68.65619723798,-19.7562383997784,0.));
#119323=CARTESIAN_POINT('Ctrl Pts',(68.6373769103211,-19.7431788471773,
0.));
#119324=CARTESIAN_POINT('Ctrl Pts',(68.6185805381102,-19.7301637565646,
0.));
#119325=CARTESIAN_POINT('Ctrl Pts',(68.5998082704741,-19.717193149095,0.));
#119326=CARTESIAN_POINT('Ctrl Pts',(68.5810602572474,-19.7042670459234,
0.));
#119327=CARTESIAN_POINT('Ctrl Pts',(68.5623366489776,-19.6913854682046,
0.));
#119328=CARTESIAN_POINT('Ctrl Pts',(68.543637596932,-19.6785484370929,0.));
#119329=CARTESIAN_POINT('Ctrl Pts',(68.5249632530994,-19.665755973734,0.));
#119330=CARTESIAN_POINT('Ctrl Pts',(68.5063137701986,-19.653008099269,0.));
#119331=CARTESIAN_POINT('Ctrl Pts',(68.4876893016863,-19.6403048348397,
0.));
#119332=CARTESIAN_POINT('Ctrl Pts',(68.4690900017631,-19.6276462015888,
0.));
#119333=CARTESIAN_POINT('Ctrl Pts',(68.4505160253777,-19.6150322206578,
0.));
#119334=CARTESIAN_POINT('Ctrl Pts',(68.4319675282273,-19.6024629131786,
0.));
#119335=CARTESIAN_POINT('Ctrl Pts',(68.4134446667695,-19.5899383002804,
0.));
#119336=CARTESIAN_POINT('Ctrl Pts',(68.3949475982334,-19.5774584030939,
0.));
#119337=CARTESIAN_POINT('Ctrl Pts',(68.3764764806287,-19.5650232427516,
0.));
#119338=CARTESIAN_POINT('Ctrl Pts',(68.3580314727522,-19.5526328403852,
0.));
#119339=CARTESIAN_POINT('Ctrl Pts',(68.3396127341937,-19.540287217119,0.));
#119340=CARTESIAN_POINT('Ctrl Pts',(68.3212204253415,-19.5279863940773,
0.));
#119341=CARTESIAN_POINT('Ctrl Pts',(68.3028547073862,-19.5157303923856,
0.));
#119342=CARTESIAN_POINT('Ctrl Pts',(68.2845157423233,-19.5035192331706,
0.));
#119343=CARTESIAN_POINT('Ctrl Pts',(68.2662036929531,-19.4913529375546,
0.));
#119344=CARTESIAN_POINT('Ctrl Pts',(68.2479187228815,-19.4792315266505,
0.));
#119345=CARTESIAN_POINT('Ctrl Pts',(68.2296609965461,-19.4671550215725,
0.));
#119346=CARTESIAN_POINT('Ctrl Pts',(68.2114306792366,-19.4551234434384,
0.));
#119347=CARTESIAN_POINT('Ctrl Pts',(68.193227937112,-19.4431368133718,0.));
#119348=CARTESIAN_POINT('Ctrl Pts',(68.1750529372211,-19.4311951524977,
0.));
#119349=CARTESIAN_POINT('Ctrl Pts',(68.1569058475026,-19.4192984819411,
0.));
#119350=CARTESIAN_POINT('Ctrl Pts',(68.1387868367668,-19.4074468228294,
0.));
#119351=CARTESIAN_POINT('Ctrl Pts',(68.1206960746763,-19.3956401962894,
0.));
#119352=CARTESIAN_POINT('Ctrl Pts',(68.1026337317298,-19.3838786234426,
0.));
#119353=CARTESIAN_POINT('Ctrl Pts',(68.0845999792274,-19.3721621253921,
0.));
#119354=CARTESIAN_POINT('Ctrl Pts',(68.0665949893221,-19.3604907232322,
0.));
#119355=CARTESIAN_POINT('Ctrl Pts',(68.0486189351027,-19.3488644380646,
0.));
#119356=CARTESIAN_POINT('Ctrl Pts',(68.0306719906636,-19.3372832910077,
0.));
#119357=CARTESIAN_POINT('Ctrl Pts',(68.0127543311761,-19.3257473032031,
0.));
#119358=CARTESIAN_POINT('Ctrl Pts',(67.9948661329591,-19.3142564958196,
0.));
#119359=CARTESIAN_POINT('Ctrl Pts',(67.977007573346,-19.3028108900374,0.));
#119360=CARTESIAN_POINT('Ctrl Pts',(67.959178830538,-19.2914105070283,0.));
#119361=CARTESIAN_POINT('Ctrl Pts',(67.9413800834798,-19.2800553679362,
0.));
#119362=CARTESIAN_POINT('Ctrl Pts',(67.9236115116781,-19.2687454938449,
0.));
#119363=CARTESIAN_POINT('Ctrl Pts',(67.9058732951822,-19.2574809057705,
0.));
#119364=CARTESIAN_POINT('Ctrl Pts',(67.8881656149983,-19.2462616247287,
0.));
#119365=CARTESIAN_POINT('Ctrl Pts',(67.8704886534555,-19.2350876717878,
0.));
#119366=CARTESIAN_POINT('Ctrl Pts',(67.852842594517,-19.223959068113,0.));
#119367=CARTESIAN_POINT('Ctrl Pts',(67.8352276242856,-19.2128758350336,
0.));
#119368=CARTESIAN_POINT('Ctrl Pts',(67.817643930658,-19.2018379939918,0.));
#119369=CARTESIAN_POINT('Ctrl Pts',(67.8000917023896,-19.1908455664089,
0.));
#119370=CARTESIAN_POINT('Ctrl Pts',(67.7825711283092,-19.1798985735687,
0.));
#119371=CARTESIAN_POINT('Ctrl Pts',(67.7650823965156,-19.1689970364959,
0.));
#119372=CARTESIAN_POINT('Ctrl Pts',(67.7476256934492,-19.1581409758112,
0.));
#119373=CARTESIAN_POINT('Ctrl Pts',(67.7302012056629,-19.1473304119969,
0.));
#119374=CARTESIAN_POINT('Ctrl Pts',(67.7128091219372,-19.1365653657098,
0.));
#119375=CARTESIAN_POINT('Ctrl Pts',(67.6954496350053,-19.1258458580343,
0.));
#119376=CARTESIAN_POINT('Ctrl Pts',(67.6781229440535,-19.115171910845,0.));
#119377=CARTESIAN_POINT('Ctrl Pts',(67.6608292549412,-19.1045435468345,
0.));
#119378=CARTESIAN_POINT('Ctrl Pts',(67.6435687749802,-19.0939607887492,
0.));
#119379=CARTESIAN_POINT('Ctrl Pts',(67.6263417083413,-19.0834236587115,
0.));
#119380=CARTESIAN_POINT('Ctrl Pts',(67.6091482520557,-19.0729321776287,
0.));
#119381=CARTESIAN_POINT('Ctrl Pts',(67.5919885896278,-19.0624863642425,
0.));
#119382=CARTESIAN_POINT('Ctrl Pts',(67.5748628972035,-19.0520862360414,
0.));
#119383=CARTESIAN_POINT('Ctrl Pts',(67.5577713558248,-19.0417318110721,
0.));
#119384=CARTESIAN_POINT('Ctrl Pts',(67.540714161288,-19.0314231093924,0.));
#119385=CARTESIAN_POINT('Ctrl Pts',(67.5236915360253,-19.0211601548222,
0.));
#119386=CARTESIAN_POINT('Ctrl Pts',(67.5067037372177,-19.0109429761274,
0.));
#119387=CARTESIAN_POINT('Ctrl Pts',(67.4897510316692,-19.0007716032785,
0.));
#119388=CARTESIAN_POINT('Ctrl Pts',(67.4728336719558,-18.9906460638607,
0.));
#119389=CARTESIAN_POINT('Ctrl Pts',(67.4559518744713,-18.9805663798466,
0.));
#119390=CARTESIAN_POINT('Ctrl Pts',(67.4391057908687,-18.9705325631773,
0.));
#119391=CARTESIAN_POINT('Ctrl Pts',(67.4222955062384,-18.9605446161079,
0.));
#119392=CARTESIAN_POINT('Ctrl Pts',(67.4088759498287,-18.9525909518003,
0.));
#119393=CARTESIAN_POINT('Ctrl Pts',(67.398827414689,-18.9466463414355,0.));
#119394=CARTESIAN_POINT('Ctrl Pts',(67.3921355608417,-18.942692439874,0.));
#119395=CARTESIAN_POINT('Ctrl Pts',(67.3887914263118,-18.9407177820969,
0.));
#119396=CARTESIAN_POINT('Ctrl Pts',(69.065695021045,-27.9316983239472,0.));
#119397=CARTESIAN_POINT('Ctrl Pts',(69.065695021045,-27.9316983239472,12.));
#119398=CARTESIAN_POINT('Ctrl Pts',(69.0618620884721,-27.9276214070632,
0.));
#119399=CARTESIAN_POINT('Ctrl Pts',(69.0618620884721,-27.9276214070632,
12.));
#119400=CARTESIAN_POINT('Ctrl Pts',(69.0541967851028,-27.9194718099003,
0.));
#119401=CARTESIAN_POINT('Ctrl Pts',(69.0541967851028,-27.9194718099003,
12.));
#119402=CARTESIAN_POINT('Ctrl Pts',(69.0427005153791,-27.9072601239722,
0.));
#119403=CARTESIAN_POINT('Ctrl Pts',(69.0427005153791,-27.9072601239722,
12.));
#119404=CARTESIAN_POINT('Ctrl Pts',(69.0273755265382,-27.8910032967339,
0.));
#119405=CARTESIAN_POINT('Ctrl Pts',(69.0273755265382,-27.8910032967339,
12.));
#119406=CARTESIAN_POINT('Ctrl Pts',(69.0082249138598,-27.8707246380957,
0.));
#119407=CARTESIAN_POINT('Ctrl Pts',(69.0082249138598,-27.8707246380957,
12.));
#119408=CARTESIAN_POINT('Ctrl Pts',(68.9890799392213,-27.8504883674059,
0.));
#119409=CARTESIAN_POINT('Ctrl Pts',(68.9890799392213,-27.8504883674059,
12.));
#119410=CARTESIAN_POINT('Ctrl Pts',(68.9699406311389,-27.8302945019977,
0.));
#119411=CARTESIAN_POINT('Ctrl Pts',(68.9699406311389,-27.8302945019977,
12.));
#119412=CARTESIAN_POINT('Ctrl Pts',(68.9508070357658,-27.8101430638072,
0.));
#119413=CARTESIAN_POINT('Ctrl Pts',(68.9508070357658,-27.8101430638072,
12.));
#119414=CARTESIAN_POINT('Ctrl Pts',(68.9316792225946,-27.7900340793689,
0.));
#119415=CARTESIAN_POINT('Ctrl Pts',(68.9316792225946,-27.7900340793689,
12.));
#119416=CARTESIAN_POINT('Ctrl Pts',(68.9125572825693,-27.7699675790571,
0.));
#119417=CARTESIAN_POINT('Ctrl Pts',(68.9125572825693,-27.7699675790571,
12.));
#119418=CARTESIAN_POINT('Ctrl Pts',(68.8934413203759,-27.7499435957525,
0.));
#119419=CARTESIAN_POINT('Ctrl Pts',(68.8934413203759,-27.7499435957525,
12.));
#119420=CARTESIAN_POINT('Ctrl Pts',(68.8743314483369,-27.7299621636566,
0.));
#119421=CARTESIAN_POINT('Ctrl Pts',(68.8743314483369,-27.7299621636566,
12.));
#119422=CARTESIAN_POINT('Ctrl Pts',(68.85522777982,-27.7100233170738,0.));
#119423=CARTESIAN_POINT('Ctrl Pts',(68.85522777982,-27.7100233170738,12.));
#119424=CARTESIAN_POINT('Ctrl Pts',(68.8361304224467,-27.6901270891241,
0.));
#119425=CARTESIAN_POINT('Ctrl Pts',(68.8361304224467,-27.6901270891241,
12.));
#119426=CARTESIAN_POINT('Ctrl Pts',(68.81703947259,-27.6702735107121,0.));
#119427=CARTESIAN_POINT('Ctrl Pts',(68.81703947259,-27.6702735107121,12.));
#119428=CARTESIAN_POINT('Ctrl Pts',(68.7979550191872,-27.6504626112666,
0.));
#119429=CARTESIAN_POINT('Ctrl Pts',(68.7979550191872,-27.6504626112666,
12.));
#119430=CARTESIAN_POINT('Ctrl Pts',(68.7788771464713,-27.6306944192738,
0.));
#119431=CARTESIAN_POINT('Ctrl Pts',(68.7788771464713,-27.6306944192738,
12.));
#119432=CARTESIAN_POINT('Ctrl Pts',(68.7598059372129,-27.6109689629029,
0.));
#119433=CARTESIAN_POINT('Ctrl Pts',(68.7598059372129,-27.6109689629029,
12.));
#119434=CARTESIAN_POINT('Ctrl Pts',(68.7407414755259,-27.5912862705469,
0.));
#119435=CARTESIAN_POINT('Ctrl Pts',(68.7407414755259,-27.5912862705469,
12.));
#119436=CARTESIAN_POINT('Ctrl Pts',(68.7216838504218,-27.5716463715005,
0.));
#119437=CARTESIAN_POINT('Ctrl Pts',(68.7216838504218,-27.5716463715005,
12.));
#119438=CARTESIAN_POINT('Ctrl Pts',(68.7026331554296,-27.5520492958907,
0.));
#119439=CARTESIAN_POINT('Ctrl Pts',(68.7026331554296,-27.5520492958907,
12.));
#119440=CARTESIAN_POINT('Ctrl Pts',(68.6835894869882,-27.5324950743706,
0.));
#119441=CARTESIAN_POINT('Ctrl Pts',(68.6835894869882,-27.5324950743706,
12.));
#119442=CARTESIAN_POINT('Ctrl Pts',(68.6645529432045,-27.5129837378792,
0.));
#119443=CARTESIAN_POINT('Ctrl Pts',(68.6645529432045,-27.5129837378792,
12.));
#119444=CARTESIAN_POINT('Ctrl Pts',(68.645523622548,-27.4935153173868,0.));
#119445=CARTESIAN_POINT('Ctrl Pts',(68.645523622548,-27.4935153173868,12.));
#119446=CARTESIAN_POINT('Ctrl Pts',(68.6265016223561,-27.4740898435989,
0.));
#119447=CARTESIAN_POINT('Ctrl Pts',(68.6265016223561,-27.4740898435989,
12.));
#119448=CARTESIAN_POINT('Ctrl Pts',(68.6074870381619,-27.4547073468227,
0.));
#119449=CARTESIAN_POINT('Ctrl Pts',(68.6074870381619,-27.4547073468227,
12.));
#119450=CARTESIAN_POINT('Ctrl Pts',(68.5884799645218,-27.4353678571361,
0.));
#119451=CARTESIAN_POINT('Ctrl Pts',(68.5884799645218,-27.4353678571361,
12.));
#119452=CARTESIAN_POINT('Ctrl Pts',(68.5694804955014,-27.4160714044831,
0.));
#119453=CARTESIAN_POINT('Ctrl Pts',(68.5694804955014,-27.4160714044831,
12.));
#119454=CARTESIAN_POINT('Ctrl Pts',(68.5504887252975,-27.3968180187941,
0.));
#119455=CARTESIAN_POINT('Ctrl Pts',(68.5504887252975,-27.3968180187941,
12.));
#119456=CARTESIAN_POINT('Ctrl Pts',(68.5315047488035,-27.3776077300914,
0.));
#119457=CARTESIAN_POINT('Ctrl Pts',(68.5315047488035,-27.3776077300914,
12.));
#119458=CARTESIAN_POINT('Ctrl Pts',(68.5125286621888,-27.3584405685942,
0.));
#119459=CARTESIAN_POINT('Ctrl Pts',(68.5125286621888,-27.3584405685942,
12.));
#119460=CARTESIAN_POINT('Ctrl Pts',(68.4935605626361,-27.3393165646748,
0.));
#119461=CARTESIAN_POINT('Ctrl Pts',(68.4935605626361,-27.3393165646748,
12.));
#119462=CARTESIAN_POINT('Ctrl Pts',(68.4746005480992,-27.3202357488153,
0.));
#119463=CARTESIAN_POINT('Ctrl Pts',(68.4746005480992,-27.3202357488153,
12.));
#119464=CARTESIAN_POINT('Ctrl Pts',(68.455648717044,-27.3011981515571,0.));
#119465=CARTESIAN_POINT('Ctrl Pts',(68.455648717044,-27.3011981515571,12.));
#119466=CARTESIAN_POINT('Ctrl Pts',(68.4367051682166,-27.2822038034539,
0.));
#119467=CARTESIAN_POINT('Ctrl Pts',(68.4367051682166,-27.2822038034539,
12.));
#119468=CARTESIAN_POINT('Ctrl Pts',(68.4177700003471,-27.2632527350062,
0.));
#119469=CARTESIAN_POINT('Ctrl Pts',(68.4177700003471,-27.2632527350062,
12.));
#119470=CARTESIAN_POINT('Ctrl Pts',(68.3988433121589,-27.2443449766654,
0.));
#119471=CARTESIAN_POINT('Ctrl Pts',(68.3988433121589,-27.2443449766654,
12.));
#119472=CARTESIAN_POINT('Ctrl Pts',(68.379925202511,-27.2254805588677,0.));
#119473=CARTESIAN_POINT('Ctrl Pts',(68.379925202511,-27.2254805588677,12.));
#119474=CARTESIAN_POINT('Ctrl Pts',(68.3610157704999,-27.2066595120544,
0.));
#119475=CARTESIAN_POINT('Ctrl Pts',(68.3610157704999,-27.2066595120544,
12.));
#119476=CARTESIAN_POINT('Ctrl Pts',(68.3421151155708,-27.1878818666925,
0.));
#119477=CARTESIAN_POINT('Ctrl Pts',(68.3421151155708,-27.1878818666925,
12.));
#119478=CARTESIAN_POINT('Ctrl Pts',(68.3232233376415,-27.1691476532917,
0.));
#119479=CARTESIAN_POINT('Ctrl Pts',(68.3232233376415,-27.1691476532917,
12.));
#119480=CARTESIAN_POINT('Ctrl Pts',(68.3043405371589,-27.1504569024131,
0.));
#119481=CARTESIAN_POINT('Ctrl Pts',(68.3043405371589,-27.1504569024131,
12.));
#119482=CARTESIAN_POINT('Ctrl Pts',(68.285466815035,-27.1318096446643,0.));
#119483=CARTESIAN_POINT('Ctrl Pts',(68.285466815035,-27.1318096446643,12.));
#119484=CARTESIAN_POINT('Ctrl Pts',(68.2666022726094,-27.1132059106939,
0.));
#119485=CARTESIAN_POINT('Ctrl Pts',(68.2666022726094,-27.1132059106939,
12.));
#119486=CARTESIAN_POINT('Ctrl Pts',(68.2477470116014,-27.0946457311814,
0.));
#119487=CARTESIAN_POINT('Ctrl Pts',(68.2477470116014,-27.0946457311814,
12.));
#119488=CARTESIAN_POINT('Ctrl Pts',(68.2289011340624,-27.0761291368231,
0.));
#119489=CARTESIAN_POINT('Ctrl Pts',(68.2289011340624,-27.0761291368231,
12.));
#119490=CARTESIAN_POINT('Ctrl Pts',(68.2100647423345,-27.0576561583179,
0.));
#119491=CARTESIAN_POINT('Ctrl Pts',(68.2100647423345,-27.0576561583179,
12.));
#119492=CARTESIAN_POINT('Ctrl Pts',(68.1912379390786,-27.0392268263805,
0.));
#119493=CARTESIAN_POINT('Ctrl Pts',(68.1912379390786,-27.0392268263805,
12.));
#119494=CARTESIAN_POINT('Ctrl Pts',(68.1724208272967,-27.0208411717477,
0.));
#119495=CARTESIAN_POINT('Ctrl Pts',(68.1724208272967,-27.0208411717477,
12.));
#119496=CARTESIAN_POINT('Ctrl Pts',(68.1536135103558,-27.0024992251839,
0.));
#119497=CARTESIAN_POINT('Ctrl Pts',(68.1536135103558,-27.0024992251839,
12.));
#119498=CARTESIAN_POINT('Ctrl Pts',(68.13481609201,-26.9842010174819,0.));
#119499=CARTESIAN_POINT('Ctrl Pts',(68.13481609201,-26.9842010174819,12.));
#119500=CARTESIAN_POINT('Ctrl Pts',(68.1160286764244,-26.9659465794596,
0.));
#119501=CARTESIAN_POINT('Ctrl Pts',(68.1160286764244,-26.9659465794596,
12.));
#119502=CARTESIAN_POINT('Ctrl Pts',(68.0972513681739,-26.9477359419647,
0.));
#119503=CARTESIAN_POINT('Ctrl Pts',(68.0972513681739,-26.9477359419647,
12.));
#119504=CARTESIAN_POINT('Ctrl Pts',(68.0784842722362,-26.9295691358775,
0.));
#119505=CARTESIAN_POINT('Ctrl Pts',(68.0784842722362,-26.9295691358775,
12.));
#119506=CARTESIAN_POINT('Ctrl Pts',(68.0597274939857,-26.9114461921109,
0.));
#119507=CARTESIAN_POINT('Ctrl Pts',(68.0597274939857,-26.9114461921109,
12.));
#119508=CARTESIAN_POINT('Ctrl Pts',(68.0409811391871,-26.8933671416065,
0.));
#119509=CARTESIAN_POINT('Ctrl Pts',(68.0409811391871,-26.8933671416065,
12.));
#119510=CARTESIAN_POINT('Ctrl Pts',(68.0222453139862,-26.8753320153255,
0.));
#119511=CARTESIAN_POINT('Ctrl Pts',(68.0222453139862,-26.8753320153255,
12.));
#119512=CARTESIAN_POINT('Ctrl Pts',(68.0035201249108,-26.85734084425,0.));
#119513=CARTESIAN_POINT('Ctrl Pts',(68.0035201249108,-26.85734084425,12.));
#119514=CARTESIAN_POINT('Ctrl Pts',(67.9848056788814,-26.8393936593914,
0.));
#119515=CARTESIAN_POINT('Ctrl Pts',(67.9848056788814,-26.8393936593914,
12.));
#119516=CARTESIAN_POINT('Ctrl Pts',(67.9661020832165,-26.8214904917922,
0.));
#119517=CARTESIAN_POINT('Ctrl Pts',(67.9661020832165,-26.8214904917922,
12.));
#119518=CARTESIAN_POINT('Ctrl Pts',(67.9474094456395,-26.8036313725262,
0.));
#119519=CARTESIAN_POINT('Ctrl Pts',(67.9474094456395,-26.8036313725262,
12.));
#119520=CARTESIAN_POINT('Ctrl Pts',(67.9287278742839,-26.7858163326933,
0.));
#119521=CARTESIAN_POINT('Ctrl Pts',(67.9287278742839,-26.7858163326933,
12.));
#119522=CARTESIAN_POINT('Ctrl Pts',(67.9100574776974,-26.7680454034169,
0.));
#119523=CARTESIAN_POINT('Ctrl Pts',(67.9100574776974,-26.7680454034169,
12.));
#119524=CARTESIAN_POINT('Ctrl Pts',(67.8913983648441,-26.7503186158524,
0.));
#119525=CARTESIAN_POINT('Ctrl Pts',(67.8913983648441,-26.7503186158524,
12.));
#119526=CARTESIAN_POINT('Ctrl Pts',(67.8727506451067,-26.7326360011886,
0.));
#119527=CARTESIAN_POINT('Ctrl Pts',(67.8727506451067,-26.7326360011886,
12.));
#119528=CARTESIAN_POINT('Ctrl Pts',(67.8541144282875,-26.7149975906478,
0.));
#119529=CARTESIAN_POINT('Ctrl Pts',(67.8541144282875,-26.7149975906478,
12.));
#119530=CARTESIAN_POINT('Ctrl Pts',(67.8354898246079,-26.6974034154803,
0.));
#119531=CARTESIAN_POINT('Ctrl Pts',(67.8354898246079,-26.6974034154803,
12.));
#119532=CARTESIAN_POINT('Ctrl Pts',(67.8168769447086,-26.6798535069586,
0.));
#119533=CARTESIAN_POINT('Ctrl Pts',(67.8168769447086,-26.6798535069586,
12.));
#119534=CARTESIAN_POINT('Ctrl Pts',(67.7982758996557,-26.6623478963867,
0.));
#119535=CARTESIAN_POINT('Ctrl Pts',(67.7982758996557,-26.6623478963867,
12.));
#119536=CARTESIAN_POINT('Ctrl Pts',(67.7796868009447,-26.6448866151027,
0.));
#119537=CARTESIAN_POINT('Ctrl Pts',(67.7796868009447,-26.6448866151027,
12.));
#119538=CARTESIAN_POINT('Ctrl Pts',(67.7611097605042,-26.6274696944793,
0.));
#119539=CARTESIAN_POINT('Ctrl Pts',(67.7611097605042,-26.6274696944793,
12.));
#119540=CARTESIAN_POINT('Ctrl Pts',(67.7425448906983,-26.6100971659205,
0.));
#119541=CARTESIAN_POINT('Ctrl Pts',(67.7425448906983,-26.6100971659205,
12.));
#119542=CARTESIAN_POINT('Ctrl Pts',(67.7239923043295,-26.5927690608547,
0.));
#119543=CARTESIAN_POINT('Ctrl Pts',(67.7239923043295,-26.5927690608547,
12.));
#119544=CARTESIAN_POINT('Ctrl Pts',(67.7054521146427,-26.5754854107422,
0.));
#119545=CARTESIAN_POINT('Ctrl Pts',(67.7054521146427,-26.5754854107422,
12.));
#119546=CARTESIAN_POINT('Ctrl Pts',(67.6869244353292,-26.5582462470794,
0.));
#119547=CARTESIAN_POINT('Ctrl Pts',(67.6869244353292,-26.5582462470794,
12.));
#119548=CARTESIAN_POINT('Ctrl Pts',(67.6684093805288,-26.5410516013984,
0.));
#119549=CARTESIAN_POINT('Ctrl Pts',(67.6684093805288,-26.5410516013984,
12.));
#119550=CARTESIAN_POINT('Ctrl Pts',(67.6499070648323,-26.5239015052656,
0.));
#119551=CARTESIAN_POINT('Ctrl Pts',(67.6499070648323,-26.5239015052656,
12.));
#119552=CARTESIAN_POINT('Ctrl Pts',(67.6314176032823,-26.5067959902731,
0.));
#119553=CARTESIAN_POINT('Ctrl Pts',(67.6314176032823,-26.5067959902731,
12.));
#119554=CARTESIAN_POINT('Ctrl Pts',(67.6129411113774,-26.4897350880447,
0.));
#119555=CARTESIAN_POINT('Ctrl Pts',(67.6129411113774,-26.4897350880447,
12.));
#119556=CARTESIAN_POINT('Ctrl Pts',(67.5944777050782,-26.4727188302415,
0.));
#119557=CARTESIAN_POINT('Ctrl Pts',(67.5944777050782,-26.4727188302415,
12.));
#119558=CARTESIAN_POINT('Ctrl Pts',(67.5760275008096,-26.4557472485622,
0.));
#119559=CARTESIAN_POINT('Ctrl Pts',(67.5760275008096,-26.4557472485622,
12.));
#119560=CARTESIAN_POINT('Ctrl Pts',(67.5575906154648,-26.4388203747422,
0.));
#119561=CARTESIAN_POINT('Ctrl Pts',(67.5575906154648,-26.4388203747422,
12.));
#119562=CARTESIAN_POINT('Ctrl Pts',(67.5391671664055,-26.4219382405452,
0.));
#119563=CARTESIAN_POINT('Ctrl Pts',(67.5391671664055,-26.4219382405452,
12.));
#119564=CARTESIAN_POINT('Ctrl Pts',(67.5207572714666,-26.4051008777669,
0.));
#119565=CARTESIAN_POINT('Ctrl Pts',(67.5207572714666,-26.4051008777669,
12.));
#119566=CARTESIAN_POINT('Ctrl Pts',(67.5023610489611,-26.3883083182417,
0.));
#119567=CARTESIAN_POINT('Ctrl Pts',(67.5023610489611,-26.3883083182417,
12.));
#119568=CARTESIAN_POINT('Ctrl Pts',(67.4839786176833,-26.3715605938432,
0.));
#119569=CARTESIAN_POINT('Ctrl Pts',(67.4839786176833,-26.3715605938432,
12.));
#119570=CARTESIAN_POINT('Ctrl Pts',(67.4656100969121,-26.3548577364835,
0.));
#119571=CARTESIAN_POINT('Ctrl Pts',(67.4656100969121,-26.3548577364835,
12.));
#119572=CARTESIAN_POINT('Ctrl Pts',(67.4472556064127,-26.3381997781059,
0.));
#119573=CARTESIAN_POINT('Ctrl Pts',(67.4472556064127,-26.3381997781059,
12.));
#119574=CARTESIAN_POINT('Ctrl Pts',(67.4289152664406,-26.3215867506864,
0.));
#119575=CARTESIAN_POINT('Ctrl Pts',(67.4289152664406,-26.3215867506864,
12.));
#119576=CARTESIAN_POINT('Ctrl Pts',(67.4105891977465,-26.305018686241,0.));
#119577=CARTESIAN_POINT('Ctrl Pts',(67.4105891977465,-26.305018686241,12.));
#119578=CARTESIAN_POINT('Ctrl Pts',(67.392277521581,-26.2884956168271,0.));
#119579=CARTESIAN_POINT('Ctrl Pts',(67.392277521581,-26.2884956168271,12.));
#119580=CARTESIAN_POINT('Ctrl Pts',(67.3739803596967,-26.2720175745423,
0.));
#119581=CARTESIAN_POINT('Ctrl Pts',(67.3739803596967,-26.2720175745423,
12.));
#119582=CARTESIAN_POINT('Ctrl Pts',(67.3556978343506,-26.255584591518,0.));
#119583=CARTESIAN_POINT('Ctrl Pts',(67.3556978343506,-26.255584591518,12.));
#119584=CARTESIAN_POINT('Ctrl Pts',(67.3374300683076,-26.2391966999192,
0.));
#119585=CARTESIAN_POINT('Ctrl Pts',(67.3374300683076,-26.2391966999192,
12.));
#119586=CARTESIAN_POINT('Ctrl Pts',(67.3191771848468,-26.2228539319528,
0.));
#119587=CARTESIAN_POINT('Ctrl Pts',(67.3191771848468,-26.2228539319528,
12.));
#119588=CARTESIAN_POINT('Ctrl Pts',(67.3009393077654,-26.2065563198685,
0.));
#119589=CARTESIAN_POINT('Ctrl Pts',(67.3009393077654,-26.2065563198685,
12.));
#119590=CARTESIAN_POINT('Ctrl Pts',(67.2827165613828,-26.1903038959589,
0.));
#119591=CARTESIAN_POINT('Ctrl Pts',(67.2827165613828,-26.1903038959589,
12.));
#119592=CARTESIAN_POINT('Ctrl Pts',(67.2645090705414,-26.1740966925527,
0.));
#119593=CARTESIAN_POINT('Ctrl Pts',(67.2645090705414,-26.1740966925527,
12.));
#119594=CARTESIAN_POINT('Ctrl Pts',(67.2463169606105,-26.1579347420135,
0.));
#119595=CARTESIAN_POINT('Ctrl Pts',(67.2463169606105,-26.1579347420135,
12.));
#119596=CARTESIAN_POINT('Ctrl Pts',(67.228140357493,-26.1418180767487,0.));
#119597=CARTESIAN_POINT('Ctrl Pts',(67.228140357493,-26.1418180767487,12.));
#119598=CARTESIAN_POINT('Ctrl Pts',(67.2099793876295,-26.1257467292102,
0.));
#119599=CARTESIAN_POINT('Ctrl Pts',(67.2099793876295,-26.1257467292102,
12.));
#119600=CARTESIAN_POINT('Ctrl Pts',(67.191834178002,-26.109720731895,0.));
#119601=CARTESIAN_POINT('Ctrl Pts',(67.191834178002,-26.109720731895,12.));
#119602=CARTESIAN_POINT('Ctrl Pts',(67.1737048561364,-26.0937401173385,
0.));
#119603=CARTESIAN_POINT('Ctrl Pts',(67.1737048561364,-26.0937401173385,
12.));
#119604=CARTESIAN_POINT('Ctrl Pts',(67.1555915501052,-26.077804918113,0.));
#119605=CARTESIAN_POINT('Ctrl Pts',(67.1555915501052,-26.077804918113,12.));
#119606=CARTESIAN_POINT('Ctrl Pts',(67.1374943885353,-26.0619151668361,
0.));
#119607=CARTESIAN_POINT('Ctrl Pts',(67.1374943885353,-26.0619151668361,
12.));
#119608=CARTESIAN_POINT('Ctrl Pts',(67.1194135006122,-26.0460708961725,
0.));
#119609=CARTESIAN_POINT('Ctrl Pts',(67.1194135006122,-26.0460708961725,
12.));
#119610=CARTESIAN_POINT('Ctrl Pts',(67.101349016084,-26.030272138834,0.));
#119611=CARTESIAN_POINT('Ctrl Pts',(67.101349016084,-26.030272138834,12.));
#119612=CARTESIAN_POINT('Ctrl Pts',(67.083301065264,-26.0145189275733,0.));
#119613=CARTESIAN_POINT('Ctrl Pts',(67.083301065264,-26.0145189275733,12.));
#119614=CARTESIAN_POINT('Ctrl Pts',(67.0652697790335,-25.9988112951819,
0.));
#119615=CARTESIAN_POINT('Ctrl Pts',(67.0652697790335,-25.9988112951819,
12.));
#119616=CARTESIAN_POINT('Ctrl Pts',(67.0472552888495,-25.9831492744988,
0.));
#119617=CARTESIAN_POINT('Ctrl Pts',(67.0472552888495,-25.9831492744988,
12.));
#119618=CARTESIAN_POINT('Ctrl Pts',(67.0292577267495,-25.9675328984123,
0.));
#119619=CARTESIAN_POINT('Ctrl Pts',(67.0292577267495,-25.9675328984123,
12.));
#119620=CARTESIAN_POINT('Ctrl Pts',(67.0112772253553,-25.9519621998598,
0.));
#119621=CARTESIAN_POINT('Ctrl Pts',(67.0112772253553,-25.9519621998598,
12.));
#119622=CARTESIAN_POINT('Ctrl Pts',(66.993313917876,-25.9364372118216,0.));
#119623=CARTESIAN_POINT('Ctrl Pts',(66.993313917876,-25.9364372118216,12.));
#119624=CARTESIAN_POINT('Ctrl Pts',(66.9753679381122,-25.9209579673198,
0.));
#119625=CARTESIAN_POINT('Ctrl Pts',(66.9753679381122,-25.9209579673198,
12.));
#119626=CARTESIAN_POINT('Ctrl Pts',(66.9574394204635,-25.9055244994267,
0.));
#119627=CARTESIAN_POINT('Ctrl Pts',(66.9574394204635,-25.9055244994267,
12.));
#119628=CARTESIAN_POINT('Ctrl Pts',(66.9395284999327,-25.8901368412655,
0.));
#119629=CARTESIAN_POINT('Ctrl Pts',(66.9395284999327,-25.8901368412655,
12.));
#119630=CARTESIAN_POINT('Ctrl Pts',(66.9216353121308,-25.8747950260115,
0.));
#119631=CARTESIAN_POINT('Ctrl Pts',(66.9216353121308,-25.8747950260115,
12.));
#119632=CARTESIAN_POINT('Ctrl Pts',(66.9037599932787,-25.8594990868845,
0.));
#119633=CARTESIAN_POINT('Ctrl Pts',(66.9037599932787,-25.8594990868845,
12.));
#119634=CARTESIAN_POINT('Ctrl Pts',(66.8859026802123,-25.8442490571486,
0.));
#119635=CARTESIAN_POINT('Ctrl Pts',(66.8859026802123,-25.8442490571486,
12.));
#119636=CARTESIAN_POINT('Ctrl Pts',(66.8680635103907,-25.8290449701207,
0.));
#119637=CARTESIAN_POINT('Ctrl Pts',(66.8680635103907,-25.8290449701207,
12.));
#119638=CARTESIAN_POINT('Ctrl Pts',(66.8502426219015,-25.8138868591715,
0.));
#119639=CARTESIAN_POINT('Ctrl Pts',(66.8502426219015,-25.8138868591715,
12.));
#119640=CARTESIAN_POINT('Ctrl Pts',(66.8324401534657,-25.7987747577265,
0.));
#119641=CARTESIAN_POINT('Ctrl Pts',(66.8324401534657,-25.7987747577265,
12.));
#119642=CARTESIAN_POINT('Ctrl Pts',(66.8146562444397,-25.7837086992581,
0.));
#119643=CARTESIAN_POINT('Ctrl Pts',(66.8146562444397,-25.7837086992581,
12.));
#119644=CARTESIAN_POINT('Ctrl Pts',(66.7968910348199,-25.7686887172859,
0.));
#119645=CARTESIAN_POINT('Ctrl Pts',(66.7968910348199,-25.7686887172859,
12.));
#119646=CARTESIAN_POINT('Ctrl Pts',(66.7791446652505,-25.7537148453848,
0.));
#119647=CARTESIAN_POINT('Ctrl Pts',(66.7791446652505,-25.7537148453848,
12.));
#119648=CARTESIAN_POINT('Ctrl Pts',(66.7614172770302,-25.7387871171861,
0.));
#119649=CARTESIAN_POINT('Ctrl Pts',(66.7614172770302,-25.7387871171861,
12.));
#119650=CARTESIAN_POINT('Ctrl Pts',(66.7437090121168,-25.7239055663778,
0.));
#119651=CARTESIAN_POINT('Ctrl Pts',(66.7437090121168,-25.7239055663778,
12.));
#119652=CARTESIAN_POINT('Ctrl Pts',(66.72602001313,-25.7090702266976,0.));
#119653=CARTESIAN_POINT('Ctrl Pts',(66.72602001313,-25.7090702266976,12.));
#119654=CARTESIAN_POINT('Ctrl Pts',(66.7083504233566,-25.6942811319337,
0.));
#119655=CARTESIAN_POINT('Ctrl Pts',(66.7083504233566,-25.6942811319337,
12.));
#119656=CARTESIAN_POINT('Ctrl Pts',(66.6907003867599,-25.679538315933,0.));
#119657=CARTESIAN_POINT('Ctrl Pts',(66.6907003867599,-25.679538315933,12.));
#119658=CARTESIAN_POINT('Ctrl Pts',(66.6730700479843,-25.6648418126016,
0.));
#119659=CARTESIAN_POINT('Ctrl Pts',(66.6730700479843,-25.6648418126016,
12.));
#119660=CARTESIAN_POINT('Ctrl Pts',(66.6554595523611,-25.6501916559051,
0.));
#119661=CARTESIAN_POINT('Ctrl Pts',(66.6554595523611,-25.6501916559051,
12.));
#119662=CARTESIAN_POINT('Ctrl Pts',(66.6378690459105,-25.6355878798605,
0.));
#119663=CARTESIAN_POINT('Ctrl Pts',(66.6378690459105,-25.6355878798605,
12.));
#119664=CARTESIAN_POINT('Ctrl Pts',(66.6202986753482,-25.6210305185395,
0.));
#119665=CARTESIAN_POINT('Ctrl Pts',(66.6202986753482,-25.6210305185395,
12.));
#119666=CARTESIAN_POINT('Ctrl Pts',(66.6027485880947,-25.6065196060751,
0.));
#119667=CARTESIAN_POINT('Ctrl Pts',(66.6027485880947,-25.6065196060751,
12.));
#119668=CARTESIAN_POINT('Ctrl Pts',(66.585218932281,-25.5920551766629,0.));
#119669=CARTESIAN_POINT('Ctrl Pts',(66.585218932281,-25.5920551766629,12.));
#119670=CARTESIAN_POINT('Ctrl Pts',(66.567709856755,-25.5776372645605,0.));
#119671=CARTESIAN_POINT('Ctrl Pts',(66.567709856755,-25.5776372645605,12.));
#119672=CARTESIAN_POINT('Ctrl Pts',(66.5502215110843,-25.5632659040797,
0.));
#119673=CARTESIAN_POINT('Ctrl Pts',(66.5502215110843,-25.5632659040797,
12.));
#119674=CARTESIAN_POINT('Ctrl Pts',(66.5327540455638,-25.5489411295917,
0.));
#119675=CARTESIAN_POINT('Ctrl Pts',(66.5327540455638,-25.5489411295917,
12.));
#119676=CARTESIAN_POINT('Ctrl Pts',(66.5153076112237,-25.5346629755323,
0.));
#119677=CARTESIAN_POINT('Ctrl Pts',(66.5153076112237,-25.5346629755323,
12.));
#119678=CARTESIAN_POINT('Ctrl Pts',(66.4978823598352,-25.5204314764033,
0.));
#119679=CARTESIAN_POINT('Ctrl Pts',(66.4978823598352,-25.5204314764033,
12.));
#119680=CARTESIAN_POINT('Ctrl Pts',(66.4804784439146,-25.5062466667703,
0.));
#119681=CARTESIAN_POINT('Ctrl Pts',(66.4804784439146,-25.5062466667703,
12.));
#119682=CARTESIAN_POINT('Ctrl Pts',(66.463096016725,-25.4921085812548,0.));
#119683=CARTESIAN_POINT('Ctrl Pts',(66.463096016725,-25.4921085812548,12.));
#119684=CARTESIAN_POINT('Ctrl Pts',(66.445735232287,-25.4780172545418,0.));
#119685=CARTESIAN_POINT('Ctrl Pts',(66.445735232287,-25.4780172545418,12.));
#119686=CARTESIAN_POINT('Ctrl Pts',(66.4283962453899,-25.463972721385,0.));
#119687=CARTESIAN_POINT('Ctrl Pts',(66.4283962453899,-25.463972721385,12.));
#119688=CARTESIAN_POINT('Ctrl Pts',(66.4110792116,-25.4499750166079,0.));
#119689=CARTESIAN_POINT('Ctrl Pts',(66.4110792116,-25.4499750166079,12.));
#119690=CARTESIAN_POINT('Ctrl Pts',(66.3937842872684,-25.4360241751017,
0.));
#119691=CARTESIAN_POINT('Ctrl Pts',(66.3937842872684,-25.4360241751017,
12.));
#119692=CARTESIAN_POINT('Ctrl Pts',(66.3765116295363,-25.4221202318198,
0.));
#119693=CARTESIAN_POINT('Ctrl Pts',(66.3765116295363,-25.4221202318198,
12.));
#119694=CARTESIAN_POINT('Ctrl Pts',(66.3592613963407,-25.4082632217846,
0.));
#119695=CARTESIAN_POINT('Ctrl Pts',(66.3592613963407,-25.4082632217846,
12.));
#119696=CARTESIAN_POINT('Ctrl Pts',(66.3420337464176,-25.3944531800901,
0.));
#119697=CARTESIAN_POINT('Ctrl Pts',(66.3420337464176,-25.3944531800901,
12.));
#119698=CARTESIAN_POINT('Ctrl Pts',(66.3248288393046,-25.3806901419013,
0.));
#119699=CARTESIAN_POINT('Ctrl Pts',(66.3248288393046,-25.3806901419013,
12.));
#119700=CARTESIAN_POINT('Ctrl Pts',(66.3076468353417,-25.3669741424491,
0.));
#119701=CARTESIAN_POINT('Ctrl Pts',(66.3076468353417,-25.3669741424491,
12.));
#119702=CARTESIAN_POINT('Ctrl Pts',(66.2904878956721,-25.3533052170254,
0.));
#119703=CARTESIAN_POINT('Ctrl Pts',(66.2904878956721,-25.3533052170254,
12.));
#119704=CARTESIAN_POINT('Ctrl Pts',(66.2733521822675,-25.3396834009955,
0.));
#119705=CARTESIAN_POINT('Ctrl Pts',(66.2733521822675,-25.3396834009955,
12.));
#119706=CARTESIAN_POINT('Ctrl Pts',(66.2562398579479,-25.326108729803,0.));
#119707=CARTESIAN_POINT('Ctrl Pts',(66.2562398579479,-25.326108729803,12.));
#119708=CARTESIAN_POINT('Ctrl Pts',(66.2391510863992,-25.3125812389728,
0.));
#119709=CARTESIAN_POINT('Ctrl Pts',(66.2391510863992,-25.3125812389728,
12.));
#119710=CARTESIAN_POINT('Ctrl Pts',(66.2220860321931,-25.2991009641087,
0.));
#119711=CARTESIAN_POINT('Ctrl Pts',(66.2220860321931,-25.2991009641087,
12.));
#119712=CARTESIAN_POINT('Ctrl Pts',(66.2050448607883,-25.2856679408921,
0.));
#119713=CARTESIAN_POINT('Ctrl Pts',(66.2050448607883,-25.2856679408921,
12.));
#119714=CARTESIAN_POINT('Ctrl Pts',(66.1880277385114,-25.2722822050829,
0.));
#119715=CARTESIAN_POINT('Ctrl Pts',(66.1880277385114,-25.2722822050829,
12.));
#119716=CARTESIAN_POINT('Ctrl Pts',(66.1710348325378,-25.2589437925145,
0.));
#119717=CARTESIAN_POINT('Ctrl Pts',(66.1710348325378,-25.2589437925145,
12.));
#119718=CARTESIAN_POINT('Ctrl Pts',(66.1540663108767,-25.245652739088,0.));
#119719=CARTESIAN_POINT('Ctrl Pts',(66.1540663108767,-25.245652739088,12.));
#119720=CARTESIAN_POINT('Ctrl Pts',(66.1371223423371,-25.2324090807561,
0.));
#119721=CARTESIAN_POINT('Ctrl Pts',(66.1371223423371,-25.2324090807561,
12.));
#119722=CARTESIAN_POINT('Ctrl Pts',(66.1202030965784,-25.2192128535367,
0.));
#119723=CARTESIAN_POINT('Ctrl Pts',(66.1202030965784,-25.2192128535367,
12.));
#119724=CARTESIAN_POINT('Ctrl Pts',(66.1033087441916,-25.2060640935372,
0.));
#119725=CARTESIAN_POINT('Ctrl Pts',(66.1033087441916,-25.2060640935372,
12.));
#119726=CARTESIAN_POINT('Ctrl Pts',(66.086439456768,-25.1929628369685,0.));
#119727=CARTESIAN_POINT('Ctrl Pts',(66.086439456768,-25.1929628369685,12.));
#119728=CARTESIAN_POINT('Ctrl Pts',(66.0695954069698,-25.1799091201594,
0.));
#119729=CARTESIAN_POINT('Ctrl Pts',(66.0695954069698,-25.1799091201594,
12.));
#119730=CARTESIAN_POINT('Ctrl Pts',(66.0527767686,-25.1669029795652,0.));
#119731=CARTESIAN_POINT('Ctrl Pts',(66.0527767686,-25.1669029795652,12.));
#119732=CARTESIAN_POINT('Ctrl Pts',(66.0359837164709,-25.153944451741,0.));
#119733=CARTESIAN_POINT('Ctrl Pts',(66.0359837164709,-25.153944451741,12.));
#119734=CARTESIAN_POINT('Ctrl Pts',(66.0192164262607,-25.1410335733094,
0.));
#119735=CARTESIAN_POINT('Ctrl Pts',(66.0192164262607,-25.1410335733094,
12.));
#119736=CARTESIAN_POINT('Ctrl Pts',(66.0024750743902,-25.12817038093,0.));
#119737=CARTESIAN_POINT('Ctrl Pts',(66.0024750743902,-25.12817038093,12.));
#119738=CARTESIAN_POINT('Ctrl Pts',(65.9857598378455,-25.1153549112512,
0.));
#119739=CARTESIAN_POINT('Ctrl Pts',(65.9857598378455,-25.1153549112512,
12.));
#119740=CARTESIAN_POINT('Ctrl Pts',(65.9690708941591,-25.1025872009016,
0.));
#119741=CARTESIAN_POINT('Ctrl Pts',(65.9690708941591,-25.1025872009016,
12.));
#119742=CARTESIAN_POINT('Ctrl Pts',(65.9524084218167,-25.0898672865926,
0.));
#119743=CARTESIAN_POINT('Ctrl Pts',(65.9524084218167,-25.0898672865926,
12.));
#119744=CARTESIAN_POINT('Ctrl Pts',(65.9357726006174,-25.0771952052033,
0.));
#119745=CARTESIAN_POINT('Ctrl Pts',(65.9357726006174,-25.0771952052033,
12.));
#119746=CARTESIAN_POINT('Ctrl Pts',(65.9191636119796,-25.0645709938519,
0.));
#119747=CARTESIAN_POINT('Ctrl Pts',(65.9191636119796,-25.0645709938519,
12.));
#119748=CARTESIAN_POINT('Ctrl Pts',(65.9025816394391,-25.0519946900066,
0.));
#119749=CARTESIAN_POINT('Ctrl Pts',(65.9025816394391,-25.0519946900066,
12.));
#119750=CARTESIAN_POINT('Ctrl Pts',(65.8860268683088,-25.039466331404,0.));
#119751=CARTESIAN_POINT('Ctrl Pts',(65.8860268683088,-25.039466331404,12.));
#119752=CARTESIAN_POINT('Ctrl Pts',(65.8694994847587,-25.0269859558351,
0.));
#119753=CARTESIAN_POINT('Ctrl Pts',(65.8694994847587,-25.0269859558351,
12.));
#119754=CARTESIAN_POINT('Ctrl Pts',(65.8529996750441,-25.0145536009604,
0.));
#119755=CARTESIAN_POINT('Ctrl Pts',(65.8529996750441,-25.0145536009604,
12.));
#119756=CARTESIAN_POINT('Ctrl Pts',(65.8365276247157,-25.0021693041181,
0.));
#119757=CARTESIAN_POINT('Ctrl Pts',(65.8365276247157,-25.0021693041181,
12.));
#119758=CARTESIAN_POINT('Ctrl Pts',(65.8200835177071,-24.9898331021002,
0.));
#119759=CARTESIAN_POINT('Ctrl Pts',(65.8200835177071,-24.9898331021002,
12.));
#119760=CARTESIAN_POINT('Ctrl Pts',(65.8036675380761,-24.97754503157,0.));
#119761=CARTESIAN_POINT('Ctrl Pts',(65.8036675380761,-24.97754503157,12.));
#119762=CARTESIAN_POINT('Ctrl Pts',(65.7872798720847,-24.965305129559,0.));
#119763=CARTESIAN_POINT('Ctrl Pts',(65.7872798720847,-24.965305129559,12.));
#119764=CARTESIAN_POINT('Ctrl Pts',(65.7709207098949,-24.9531134338693,
0.));
#119765=CARTESIAN_POINT('Ctrl Pts',(65.7709207098949,-24.9531134338693,
12.));
#119766=CARTESIAN_POINT('Ctrl Pts',(65.7545902480286,-24.9409699836524,
0.));
#119767=CARTESIAN_POINT('Ctrl Pts',(65.7545902480286,-24.9409699836524,
12.));
#119768=CARTESIAN_POINT('Ctrl Pts',(65.7382886895839,-24.9288748194562,
0.));
#119769=CARTESIAN_POINT('Ctrl Pts',(65.7382886895839,-24.9288748194562,
12.));
#119770=CARTESIAN_POINT('Ctrl Pts',(65.7220162391016,-24.9168279820093,
0.));
#119771=CARTESIAN_POINT('Ctrl Pts',(65.7220162391016,-24.9168279820093,
12.));
#119772=CARTESIAN_POINT('Ctrl Pts',(65.7057730980471,-24.9048295111444,
0.));
#119773=CARTESIAN_POINT('Ctrl Pts',(65.7057730980471,-24.9048295111444,
12.));
#119774=CARTESIAN_POINT('Ctrl Pts',(65.6895594608798,-24.8928794448616,
0.));
#119775=CARTESIAN_POINT('Ctrl Pts',(65.6895594608798,-24.8928794448616,
12.));
#119776=CARTESIAN_POINT('Ctrl Pts',(65.6733755087723,-24.8809778178248,
0.));
#119777=CARTESIAN_POINT('Ctrl Pts',(65.6733755087723,-24.8809778178248,
12.));
#119778=CARTESIAN_POINT('Ctrl Pts',(65.6572214156761,-24.8691246628081,
0.));
#119779=CARTESIAN_POINT('Ctrl Pts',(65.6572214156761,-24.8691246628081,
12.));
#119780=CARTESIAN_POINT('Ctrl Pts',(65.6410973603713,-24.8573200135684,
0.));
#119781=CARTESIAN_POINT('Ctrl Pts',(65.6410973603713,-24.8573200135684,
12.));
#119782=CARTESIAN_POINT('Ctrl Pts',(65.6250035361612,-24.8455639071517,
0.));
#119783=CARTESIAN_POINT('Ctrl Pts',(65.6250035361612,-24.8455639071517,
12.));
#119784=CARTESIAN_POINT('Ctrl Pts',(65.6089401625551,-24.8338563866739,
0.));
#119785=CARTESIAN_POINT('Ctrl Pts',(65.6089401625551,-24.8338563866739,
12.));
#119786=CARTESIAN_POINT('Ctrl Pts',(65.5929074932487,-24.8221975032059,
0.));
#119787=CARTESIAN_POINT('Ctrl Pts',(65.5929074932487,-24.8221975032059,
12.));
#119788=CARTESIAN_POINT('Ctrl Pts',(65.5769057914184,-24.8105873098578,
0.));
#119789=CARTESIAN_POINT('Ctrl Pts',(65.5769057914184,-24.8105873098578,
12.));
#119790=CARTESIAN_POINT('Ctrl Pts',(65.5609353062749,-24.7990258561234,
0.));
#119791=CARTESIAN_POINT('Ctrl Pts',(65.5609353062749,-24.7990258561234,
12.));
#119792=CARTESIAN_POINT('Ctrl Pts',(65.5449962514735,-24.7875131827515,
0.));
#119793=CARTESIAN_POINT('Ctrl Pts',(65.5449962514735,-24.7875131827515,
12.));
#119794=CARTESIAN_POINT('Ctrl Pts',(65.5290887770493,-24.7760493148551,
0.));
#119795=CARTESIAN_POINT('Ctrl Pts',(65.5290887770493,-24.7760493148551,
12.));
#119796=CARTESIAN_POINT('Ctrl Pts',(65.5132129675727,-24.764634262097,0.));
#119797=CARTESIAN_POINT('Ctrl Pts',(65.5132129675727,-24.764634262097,12.));
#119798=CARTESIAN_POINT('Ctrl Pts',(65.5005376841469,-24.7555412724771,
0.));
#119799=CARTESIAN_POINT('Ctrl Pts',(65.5005376841469,-24.7555412724771,
12.));
#119800=CARTESIAN_POINT('Ctrl Pts',(65.4910454936487,-24.7487434956058,
0.));
#119801=CARTESIAN_POINT('Ctrl Pts',(65.4910454936487,-24.7487434956058,
12.));
#119802=CARTESIAN_POINT('Ctrl Pts',(65.484723709553,-24.7442214063411,0.));
#119803=CARTESIAN_POINT('Ctrl Pts',(65.484723709553,-24.7442214063411,12.));
#119804=CARTESIAN_POINT('Ctrl Pts',(65.4815644032299,-24.7419628022042,
0.));
#119805=CARTESIAN_POINT('Ctrl Pts',(65.4815644032299,-24.7419628022042,
12.));
#119806=CARTESIAN_POINT('',(65.4815644032299,-24.7419628022042,12.));
#119807=CARTESIAN_POINT('Ctrl Pts',(65.4815644032299,-24.7419628022042,
12.));
#119808=CARTESIAN_POINT('Ctrl Pts',(65.484723709553,-24.7442214063411,12.));
#119809=CARTESIAN_POINT('Ctrl Pts',(65.4910454936487,-24.7487434956058,
12.));
#119810=CARTESIAN_POINT('Ctrl Pts',(65.5005376841469,-24.7555412724771,
12.));
#119811=CARTESIAN_POINT('Ctrl Pts',(65.5132129675727,-24.764634262097,12.));
#119812=CARTESIAN_POINT('Ctrl Pts',(65.5290887770493,-24.7760493148551,
12.));
#119813=CARTESIAN_POINT('Ctrl Pts',(65.5449962514735,-24.7875131827515,
12.));
#119814=CARTESIAN_POINT('Ctrl Pts',(65.5609353062749,-24.7990258561234,
12.));
#119815=CARTESIAN_POINT('Ctrl Pts',(65.5769057914184,-24.8105873098578,
12.));
#119816=CARTESIAN_POINT('Ctrl Pts',(65.5929074932487,-24.8221975032059,
12.));
#119817=CARTESIAN_POINT('Ctrl Pts',(65.6089401625551,-24.8338563866739,
12.));
#119818=CARTESIAN_POINT('Ctrl Pts',(65.6250035361612,-24.8455639071517,
12.));
#119819=CARTESIAN_POINT('Ctrl Pts',(65.6410973603713,-24.8573200135684,
12.));
#119820=CARTESIAN_POINT('Ctrl Pts',(65.6572214156761,-24.8691246628081,
12.));
#119821=CARTESIAN_POINT('Ctrl Pts',(65.6733755087723,-24.8809778178248,
12.));
#119822=CARTESIAN_POINT('Ctrl Pts',(65.6895594608798,-24.8928794448616,
12.));
#119823=CARTESIAN_POINT('Ctrl Pts',(65.7057730980471,-24.9048295111444,
12.));
#119824=CARTESIAN_POINT('Ctrl Pts',(65.7220162391016,-24.9168279820093,
12.));
#119825=CARTESIAN_POINT('Ctrl Pts',(65.7382886895839,-24.9288748194562,
12.));
#119826=CARTESIAN_POINT('Ctrl Pts',(65.7545902480286,-24.9409699836524,
12.));
#119827=CARTESIAN_POINT('Ctrl Pts',(65.7709207098949,-24.9531134338693,
12.));
#119828=CARTESIAN_POINT('Ctrl Pts',(65.7872798720847,-24.965305129559,12.));
#119829=CARTESIAN_POINT('Ctrl Pts',(65.8036675380761,-24.97754503157,12.));
#119830=CARTESIAN_POINT('Ctrl Pts',(65.8200835177071,-24.9898331021002,
12.));
#119831=CARTESIAN_POINT('Ctrl Pts',(65.8365276247157,-25.0021693041181,
12.));
#119832=CARTESIAN_POINT('Ctrl Pts',(65.8529996750441,-25.0145536009604,
12.));
#119833=CARTESIAN_POINT('Ctrl Pts',(65.8694994847587,-25.0269859558351,
12.));
#119834=CARTESIAN_POINT('Ctrl Pts',(65.8860268683088,-25.039466331404,12.));
#119835=CARTESIAN_POINT('Ctrl Pts',(65.9025816394391,-25.0519946900066,
12.));
#119836=CARTESIAN_POINT('Ctrl Pts',(65.9191636119796,-25.0645709938519,
12.));
#119837=CARTESIAN_POINT('Ctrl Pts',(65.9357726006174,-25.0771952052033,
12.));
#119838=CARTESIAN_POINT('Ctrl Pts',(65.9524084218167,-25.0898672865926,
12.));
#119839=CARTESIAN_POINT('Ctrl Pts',(65.9690708941591,-25.1025872009016,
12.));
#119840=CARTESIAN_POINT('Ctrl Pts',(65.9857598378455,-25.1153549112512,
12.));
#119841=CARTESIAN_POINT('Ctrl Pts',(66.0024750743902,-25.12817038093,12.));
#119842=CARTESIAN_POINT('Ctrl Pts',(66.0192164262607,-25.1410335733094,
12.));
#119843=CARTESIAN_POINT('Ctrl Pts',(66.0359837164709,-25.153944451741,12.));
#119844=CARTESIAN_POINT('Ctrl Pts',(66.0527767686,-25.1669029795652,12.));
#119845=CARTESIAN_POINT('Ctrl Pts',(66.0695954069698,-25.1799091201594,
12.));
#119846=CARTESIAN_POINT('Ctrl Pts',(66.086439456768,-25.1929628369685,12.));
#119847=CARTESIAN_POINT('Ctrl Pts',(66.1033087441916,-25.2060640935372,
12.));
#119848=CARTESIAN_POINT('Ctrl Pts',(66.1202030965784,-25.2192128535367,
12.));
#119849=CARTESIAN_POINT('Ctrl Pts',(66.1371223423371,-25.2324090807561,
12.));
#119850=CARTESIAN_POINT('Ctrl Pts',(66.1540663108767,-25.245652739088,12.));
#119851=CARTESIAN_POINT('Ctrl Pts',(66.1710348325378,-25.2589437925145,
12.));
#119852=CARTESIAN_POINT('Ctrl Pts',(66.1880277385114,-25.2722822050829,
12.));
#119853=CARTESIAN_POINT('Ctrl Pts',(66.2050448607883,-25.2856679408921,
12.));
#119854=CARTESIAN_POINT('Ctrl Pts',(66.2220860321931,-25.2991009641087,
12.));
#119855=CARTESIAN_POINT('Ctrl Pts',(66.2391510863992,-25.3125812389728,
12.));
#119856=CARTESIAN_POINT('Ctrl Pts',(66.2562398579479,-25.326108729803,12.));
#119857=CARTESIAN_POINT('Ctrl Pts',(66.2733521822675,-25.3396834009955,
12.));
#119858=CARTESIAN_POINT('Ctrl Pts',(66.2904878956721,-25.3533052170254,
12.));
#119859=CARTESIAN_POINT('Ctrl Pts',(66.3076468353417,-25.3669741424491,
12.));
#119860=CARTESIAN_POINT('Ctrl Pts',(66.3248288393046,-25.3806901419013,
12.));
#119861=CARTESIAN_POINT('Ctrl Pts',(66.3420337464176,-25.3944531800901,
12.));
#119862=CARTESIAN_POINT('Ctrl Pts',(66.3592613963407,-25.4082632217846,
12.));
#119863=CARTESIAN_POINT('Ctrl Pts',(66.3765116295363,-25.4221202318198,
12.));
#119864=CARTESIAN_POINT('Ctrl Pts',(66.3937842872684,-25.4360241751017,
12.));
#119865=CARTESIAN_POINT('Ctrl Pts',(66.4110792116,-25.4499750166079,12.));
#119866=CARTESIAN_POINT('Ctrl Pts',(66.4283962453899,-25.463972721385,12.));
#119867=CARTESIAN_POINT('Ctrl Pts',(66.445735232287,-25.4780172545418,12.));
#119868=CARTESIAN_POINT('Ctrl Pts',(66.463096016725,-25.4921085812548,12.));
#119869=CARTESIAN_POINT('Ctrl Pts',(66.4804784439146,-25.5062466667703,
12.));
#119870=CARTESIAN_POINT('Ctrl Pts',(66.4978823598352,-25.5204314764033,
12.));
#119871=CARTESIAN_POINT('Ctrl Pts',(66.5153076112237,-25.5346629755323,
12.));
#119872=CARTESIAN_POINT('Ctrl Pts',(66.5327540455638,-25.5489411295917,
12.));
#119873=CARTESIAN_POINT('Ctrl Pts',(66.5502215110843,-25.5632659040797,
12.));
#119874=CARTESIAN_POINT('Ctrl Pts',(66.567709856755,-25.5776372645605,12.));
#119875=CARTESIAN_POINT('Ctrl Pts',(66.585218932281,-25.5920551766629,12.));
#119876=CARTESIAN_POINT('Ctrl Pts',(66.6027485880947,-25.6065196060751,
12.));
#119877=CARTESIAN_POINT('Ctrl Pts',(66.6202986753482,-25.6210305185395,
12.));
#119878=CARTESIAN_POINT('Ctrl Pts',(66.6378690459105,-25.6355878798605,
12.));
#119879=CARTESIAN_POINT('Ctrl Pts',(66.6554595523611,-25.6501916559051,
12.));
#119880=CARTESIAN_POINT('Ctrl Pts',(66.6730700479843,-25.6648418126016,
12.));
#119881=CARTESIAN_POINT('Ctrl Pts',(66.6907003867599,-25.679538315933,12.));
#119882=CARTESIAN_POINT('Ctrl Pts',(66.7083504233566,-25.6942811319337,
12.));
#119883=CARTESIAN_POINT('Ctrl Pts',(66.72602001313,-25.7090702266976,12.));
#119884=CARTESIAN_POINT('Ctrl Pts',(66.7437090121168,-25.7239055663778,
12.));
#119885=CARTESIAN_POINT('Ctrl Pts',(66.7614172770302,-25.7387871171861,
12.));
#119886=CARTESIAN_POINT('Ctrl Pts',(66.7791446652505,-25.7537148453848,
12.));
#119887=CARTESIAN_POINT('Ctrl Pts',(66.7968910348199,-25.7686887172859,
12.));
#119888=CARTESIAN_POINT('Ctrl Pts',(66.8146562444397,-25.7837086992581,
12.));
#119889=CARTESIAN_POINT('Ctrl Pts',(66.8324401534657,-25.7987747577265,
12.));
#119890=CARTESIAN_POINT('Ctrl Pts',(66.8502426219015,-25.8138868591715,
12.));
#119891=CARTESIAN_POINT('Ctrl Pts',(66.8680635103907,-25.8290449701207,
12.));
#119892=CARTESIAN_POINT('Ctrl Pts',(66.8859026802123,-25.8442490571486,
12.));
#119893=CARTESIAN_POINT('Ctrl Pts',(66.9037599932787,-25.8594990868845,
12.));
#119894=CARTESIAN_POINT('Ctrl Pts',(66.9216353121308,-25.8747950260115,
12.));
#119895=CARTESIAN_POINT('Ctrl Pts',(66.9395284999327,-25.8901368412655,
12.));
#119896=CARTESIAN_POINT('Ctrl Pts',(66.9574394204635,-25.9055244994267,
12.));
#119897=CARTESIAN_POINT('Ctrl Pts',(66.9753679381122,-25.9209579673198,
12.));
#119898=CARTESIAN_POINT('Ctrl Pts',(66.993313917876,-25.9364372118216,12.));
#119899=CARTESIAN_POINT('Ctrl Pts',(67.0112772253553,-25.9519621998598,
12.));
#119900=CARTESIAN_POINT('Ctrl Pts',(67.0292577267495,-25.9675328984123,
12.));
#119901=CARTESIAN_POINT('Ctrl Pts',(67.0472552888495,-25.9831492744988,
12.));
#119902=CARTESIAN_POINT('Ctrl Pts',(67.0652697790335,-25.9988112951819,
12.));
#119903=CARTESIAN_POINT('Ctrl Pts',(67.083301065264,-26.0145189275733,12.));
#119904=CARTESIAN_POINT('Ctrl Pts',(67.101349016084,-26.030272138834,12.));
#119905=CARTESIAN_POINT('Ctrl Pts',(67.1194135006122,-26.0460708961725,
12.));
#119906=CARTESIAN_POINT('Ctrl Pts',(67.1374943885353,-26.0619151668361,
12.));
#119907=CARTESIAN_POINT('Ctrl Pts',(67.1555915501052,-26.077804918113,12.));
#119908=CARTESIAN_POINT('Ctrl Pts',(67.1737048561364,-26.0937401173385,
12.));
#119909=CARTESIAN_POINT('Ctrl Pts',(67.191834178002,-26.109720731895,12.));
#119910=CARTESIAN_POINT('Ctrl Pts',(67.2099793876295,-26.1257467292102,
12.));
#119911=CARTESIAN_POINT('Ctrl Pts',(67.228140357493,-26.1418180767487,12.));
#119912=CARTESIAN_POINT('Ctrl Pts',(67.2463169606105,-26.1579347420135,
12.));
#119913=CARTESIAN_POINT('Ctrl Pts',(67.2645090705414,-26.1740966925527,
12.));
#119914=CARTESIAN_POINT('Ctrl Pts',(67.2827165613828,-26.1903038959589,
12.));
#119915=CARTESIAN_POINT('Ctrl Pts',(67.3009393077654,-26.2065563198685,
12.));
#119916=CARTESIAN_POINT('Ctrl Pts',(67.3191771848468,-26.2228539319528,
12.));
#119917=CARTESIAN_POINT('Ctrl Pts',(67.3374300683076,-26.2391966999192,
12.));
#119918=CARTESIAN_POINT('Ctrl Pts',(67.3556978343506,-26.255584591518,12.));
#119919=CARTESIAN_POINT('Ctrl Pts',(67.3739803596967,-26.2720175745423,
12.));
#119920=CARTESIAN_POINT('Ctrl Pts',(67.392277521581,-26.2884956168271,12.));
#119921=CARTESIAN_POINT('Ctrl Pts',(67.4105891977465,-26.305018686241,12.));
#119922=CARTESIAN_POINT('Ctrl Pts',(67.4289152664406,-26.3215867506864,
12.));
#119923=CARTESIAN_POINT('Ctrl Pts',(67.4472556064127,-26.3381997781059,
12.));
#119924=CARTESIAN_POINT('Ctrl Pts',(67.4656100969121,-26.3548577364835,
12.));
#119925=CARTESIAN_POINT('Ctrl Pts',(67.4839786176833,-26.3715605938432,
12.));
#119926=CARTESIAN_POINT('Ctrl Pts',(67.5023610489611,-26.3883083182417,
12.));
#119927=CARTESIAN_POINT('Ctrl Pts',(67.5207572714666,-26.4051008777669,
12.));
#119928=CARTESIAN_POINT('Ctrl Pts',(67.5391671664055,-26.4219382405452,
12.));
#119929=CARTESIAN_POINT('Ctrl Pts',(67.5575906154648,-26.4388203747422,
12.));
#119930=CARTESIAN_POINT('Ctrl Pts',(67.5760275008096,-26.4557472485622,
12.));
#119931=CARTESIAN_POINT('Ctrl Pts',(67.5944777050782,-26.4727188302415,
12.));
#119932=CARTESIAN_POINT('Ctrl Pts',(67.6129411113774,-26.4897350880447,
12.));
#119933=CARTESIAN_POINT('Ctrl Pts',(67.6314176032823,-26.5067959902731,
12.));
#119934=CARTESIAN_POINT('Ctrl Pts',(67.6499070648323,-26.5239015052656,
12.));
#119935=CARTESIAN_POINT('Ctrl Pts',(67.6684093805288,-26.5410516013984,
12.));
#119936=CARTESIAN_POINT('Ctrl Pts',(67.6869244353292,-26.5582462470794,
12.));
#119937=CARTESIAN_POINT('Ctrl Pts',(67.7054521146427,-26.5754854107422,
12.));
#119938=CARTESIAN_POINT('Ctrl Pts',(67.7239923043295,-26.5927690608547,
12.));
#119939=CARTESIAN_POINT('Ctrl Pts',(67.7425448906983,-26.6100971659205,
12.));
#119940=CARTESIAN_POINT('Ctrl Pts',(67.7611097605042,-26.6274696944793,
12.));
#119941=CARTESIAN_POINT('Ctrl Pts',(67.7796868009447,-26.6448866151027,
12.));
#119942=CARTESIAN_POINT('Ctrl Pts',(67.7982758996557,-26.6623478963867,
12.));
#119943=CARTESIAN_POINT('Ctrl Pts',(67.8168769447086,-26.6798535069586,
12.));
#119944=CARTESIAN_POINT('Ctrl Pts',(67.8354898246079,-26.6974034154803,
12.));
#119945=CARTESIAN_POINT('Ctrl Pts',(67.8541144282875,-26.7149975906478,
12.));
#119946=CARTESIAN_POINT('Ctrl Pts',(67.8727506451067,-26.7326360011886,
12.));
#119947=CARTESIAN_POINT('Ctrl Pts',(67.8913983648441,-26.7503186158524,
12.));
#119948=CARTESIAN_POINT('Ctrl Pts',(67.9100574776974,-26.7680454034169,
12.));
#119949=CARTESIAN_POINT('Ctrl Pts',(67.9287278742839,-26.7858163326933,
12.));
#119950=CARTESIAN_POINT('Ctrl Pts',(67.9474094456395,-26.8036313725262,
12.));
#119951=CARTESIAN_POINT('Ctrl Pts',(67.9661020832165,-26.8214904917922,
12.));
#119952=CARTESIAN_POINT('Ctrl Pts',(67.9848056788814,-26.8393936593914,
12.));
#119953=CARTESIAN_POINT('Ctrl Pts',(68.0035201249108,-26.85734084425,12.));
#119954=CARTESIAN_POINT('Ctrl Pts',(68.0222453139862,-26.8753320153255,
12.));
#119955=CARTESIAN_POINT('Ctrl Pts',(68.0409811391871,-26.8933671416065,
12.));
#119956=CARTESIAN_POINT('Ctrl Pts',(68.0597274939857,-26.9114461921109,
12.));
#119957=CARTESIAN_POINT('Ctrl Pts',(68.0784842722362,-26.9295691358775,
12.));
#119958=CARTESIAN_POINT('Ctrl Pts',(68.0972513681739,-26.9477359419647,
12.));
#119959=CARTESIAN_POINT('Ctrl Pts',(68.1160286764244,-26.9659465794596,
12.));
#119960=CARTESIAN_POINT('Ctrl Pts',(68.13481609201,-26.9842010174819,12.));
#119961=CARTESIAN_POINT('Ctrl Pts',(68.1536135103558,-27.0024992251839,
12.));
#119962=CARTESIAN_POINT('Ctrl Pts',(68.1724208272967,-27.0208411717477,
12.));
#119963=CARTESIAN_POINT('Ctrl Pts',(68.1912379390786,-27.0392268263805,
12.));
#119964=CARTESIAN_POINT('Ctrl Pts',(68.2100647423345,-27.0576561583179,
12.));
#119965=CARTESIAN_POINT('Ctrl Pts',(68.2289011340624,-27.0761291368231,
12.));
#119966=CARTESIAN_POINT('Ctrl Pts',(68.2477470116014,-27.0946457311814,
12.));
#119967=CARTESIAN_POINT('Ctrl Pts',(68.2666022726094,-27.1132059106939,
12.));
#119968=CARTESIAN_POINT('Ctrl Pts',(68.285466815035,-27.1318096446643,12.));
#119969=CARTESIAN_POINT('Ctrl Pts',(68.3043405371589,-27.1504569024131,
12.));
#119970=CARTESIAN_POINT('Ctrl Pts',(68.3232233376415,-27.1691476532917,
12.));
#119971=CARTESIAN_POINT('Ctrl Pts',(68.3421151155708,-27.1878818666925,
12.));
#119972=CARTESIAN_POINT('Ctrl Pts',(68.3610157704999,-27.2066595120544,
12.));
#119973=CARTESIAN_POINT('Ctrl Pts',(68.379925202511,-27.2254805588677,12.));
#119974=CARTESIAN_POINT('Ctrl Pts',(68.3988433121589,-27.2443449766654,
12.));
#119975=CARTESIAN_POINT('Ctrl Pts',(68.4177700003471,-27.2632527350062,
12.));
#119976=CARTESIAN_POINT('Ctrl Pts',(68.4367051682166,-27.2822038034539,
12.));
#119977=CARTESIAN_POINT('Ctrl Pts',(68.455648717044,-27.3011981515571,12.));
#119978=CARTESIAN_POINT('Ctrl Pts',(68.4746005480992,-27.3202357488153,
12.));
#119979=CARTESIAN_POINT('Ctrl Pts',(68.4935605626361,-27.3393165646748,
12.));
#119980=CARTESIAN_POINT('Ctrl Pts',(68.5125286621888,-27.3584405685942,
12.));
#119981=CARTESIAN_POINT('Ctrl Pts',(68.5315047488035,-27.3776077300914,
12.));
#119982=CARTESIAN_POINT('Ctrl Pts',(68.5504887252975,-27.3968180187941,
12.));
#119983=CARTESIAN_POINT('Ctrl Pts',(68.5694804955014,-27.4160714044831,
12.));
#119984=CARTESIAN_POINT('Ctrl Pts',(68.5884799645218,-27.4353678571361,
12.));
#119985=CARTESIAN_POINT('Ctrl Pts',(68.6074870381619,-27.4547073468227,
12.));
#119986=CARTESIAN_POINT('Ctrl Pts',(68.6265016223561,-27.4740898435989,
12.));
#119987=CARTESIAN_POINT('Ctrl Pts',(68.645523622548,-27.4935153173868,12.));
#119988=CARTESIAN_POINT('Ctrl Pts',(68.6645529432045,-27.5129837378792,
12.));
#119989=CARTESIAN_POINT('Ctrl Pts',(68.6835894869882,-27.5324950743706,
12.));
#119990=CARTESIAN_POINT('Ctrl Pts',(68.7026331554296,-27.5520492958907,
12.));
#119991=CARTESIAN_POINT('Ctrl Pts',(68.7216838504218,-27.5716463715005,
12.));
#119992=CARTESIAN_POINT('Ctrl Pts',(68.7407414755259,-27.5912862705469,
12.));
#119993=CARTESIAN_POINT('Ctrl Pts',(68.7598059372129,-27.6109689629029,
12.));
#119994=CARTESIAN_POINT('Ctrl Pts',(68.7788771464713,-27.6306944192738,
12.));
#119995=CARTESIAN_POINT('Ctrl Pts',(68.7979550191872,-27.6504626112666,
12.));
#119996=CARTESIAN_POINT('Ctrl Pts',(68.8143140938914,-27.6674443909983,
12.));
#119997=CARTESIAN_POINT('Ctrl Pts',(68.8268597852178,-27.6804870323433,
12.));
#119998=CARTESIAN_POINT('Ctrl Pts',(68.8355891982104,-27.6895716271273,
12.));
#119999=CARTESIAN_POINT('Ctrl Pts',(68.8405004466157,-27.6946856803716,
12.));
#120000=CARTESIAN_POINT('Ctrl Pts',(68.8415926175082,-27.6958230985041,
12.));
#120001=CARTESIAN_POINT('',(65.4815644032299,-24.7419628022042,0.));
#120002=CARTESIAN_POINT('',(65.4815644032299,-24.7419628022042,0.));
#120003=CARTESIAN_POINT('Ctrl Pts',(68.8415926175082,-27.6958230985041,
0.));
#120004=CARTESIAN_POINT('Ctrl Pts',(68.8405004466157,-27.6946856803716,
0.));
#120005=CARTESIAN_POINT('Ctrl Pts',(68.8355891982104,-27.6895716271273,
0.));
#120006=CARTESIAN_POINT('Ctrl Pts',(68.8268597852178,-27.6804870323433,
0.));
#120007=CARTESIAN_POINT('Ctrl Pts',(68.8143140938914,-27.6674443909983,
0.));
#120008=CARTESIAN_POINT('Ctrl Pts',(68.7979550191872,-27.6504626112666,
0.));
#120009=CARTESIAN_POINT('Ctrl Pts',(68.7788771464713,-27.6306944192738,
0.));
#120010=CARTESIAN_POINT('Ctrl Pts',(68.7598059372129,-27.6109689629029,
0.));
#120011=CARTESIAN_POINT('Ctrl Pts',(68.7407414755259,-27.5912862705469,
0.));
#120012=CARTESIAN_POINT('Ctrl Pts',(68.7216838504218,-27.5716463715005,
0.));
#120013=CARTESIAN_POINT('Ctrl Pts',(68.7026331554296,-27.5520492958907,
0.));
#120014=CARTESIAN_POINT('Ctrl Pts',(68.6835894869882,-27.5324950743706,
0.));
#120015=CARTESIAN_POINT('Ctrl Pts',(68.6645529432045,-27.5129837378792,
0.));
#120016=CARTESIAN_POINT('Ctrl Pts',(68.645523622548,-27.4935153173868,0.));
#120017=CARTESIAN_POINT('Ctrl Pts',(68.6265016223561,-27.4740898435989,
0.));
#120018=CARTESIAN_POINT('Ctrl Pts',(68.6074870381619,-27.4547073468227,
0.));
#120019=CARTESIAN_POINT('Ctrl Pts',(68.5884799645218,-27.4353678571361,
0.));
#120020=CARTESIAN_POINT('Ctrl Pts',(68.5694804955014,-27.4160714044831,
0.));
#120021=CARTESIAN_POINT('Ctrl Pts',(68.5504887252975,-27.3968180187941,
0.));
#120022=CARTESIAN_POINT('Ctrl Pts',(68.5315047488035,-27.3776077300914,
0.));
#120023=CARTESIAN_POINT('Ctrl Pts',(68.5125286621888,-27.3584405685942,
0.));
#120024=CARTESIAN_POINT('Ctrl Pts',(68.4935605626361,-27.3393165646748,
0.));
#120025=CARTESIAN_POINT('Ctrl Pts',(68.4746005480992,-27.3202357488153,
0.));
#120026=CARTESIAN_POINT('Ctrl Pts',(68.455648717044,-27.3011981515571,0.));
#120027=CARTESIAN_POINT('Ctrl Pts',(68.4367051682166,-27.2822038034539,
0.));
#120028=CARTESIAN_POINT('Ctrl Pts',(68.4177700003471,-27.2632527350062,
0.));
#120029=CARTESIAN_POINT('Ctrl Pts',(68.3988433121589,-27.2443449766654,
0.));
#120030=CARTESIAN_POINT('Ctrl Pts',(68.379925202511,-27.2254805588677,0.));
#120031=CARTESIAN_POINT('Ctrl Pts',(68.3610157704999,-27.2066595120544,
0.));
#120032=CARTESIAN_POINT('Ctrl Pts',(68.3421151155708,-27.1878818666925,
0.));
#120033=CARTESIAN_POINT('Ctrl Pts',(68.3232233376415,-27.1691476532917,
0.));
#120034=CARTESIAN_POINT('Ctrl Pts',(68.3043405371589,-27.1504569024131,
0.));
#120035=CARTESIAN_POINT('Ctrl Pts',(68.285466815035,-27.1318096446643,0.));
#120036=CARTESIAN_POINT('Ctrl Pts',(68.2666022726094,-27.1132059106939,
0.));
#120037=CARTESIAN_POINT('Ctrl Pts',(68.2477470116014,-27.0946457311814,
0.));
#120038=CARTESIAN_POINT('Ctrl Pts',(68.2289011340624,-27.0761291368231,
0.));
#120039=CARTESIAN_POINT('Ctrl Pts',(68.2100647423345,-27.0576561583179,
0.));
#120040=CARTESIAN_POINT('Ctrl Pts',(68.1912379390786,-27.0392268263805,
0.));
#120041=CARTESIAN_POINT('Ctrl Pts',(68.1724208272967,-27.0208411717477,
0.));
#120042=CARTESIAN_POINT('Ctrl Pts',(68.1536135103558,-27.0024992251839,
0.));
#120043=CARTESIAN_POINT('Ctrl Pts',(68.13481609201,-26.9842010174819,0.));
#120044=CARTESIAN_POINT('Ctrl Pts',(68.1160286764244,-26.9659465794596,
0.));
#120045=CARTESIAN_POINT('Ctrl Pts',(68.0972513681739,-26.9477359419647,
0.));
#120046=CARTESIAN_POINT('Ctrl Pts',(68.0784842722362,-26.9295691358775,
0.));
#120047=CARTESIAN_POINT('Ctrl Pts',(68.0597274939857,-26.9114461921109,
0.));
#120048=CARTESIAN_POINT('Ctrl Pts',(68.0409811391871,-26.8933671416065,
0.));
#120049=CARTESIAN_POINT('Ctrl Pts',(68.0222453139862,-26.8753320153255,
0.));
#120050=CARTESIAN_POINT('Ctrl Pts',(68.0035201249108,-26.85734084425,0.));
#120051=CARTESIAN_POINT('Ctrl Pts',(67.9848056788814,-26.8393936593914,
0.));
#120052=CARTESIAN_POINT('Ctrl Pts',(67.9661020832165,-26.8214904917922,
0.));
#120053=CARTESIAN_POINT('Ctrl Pts',(67.9474094456395,-26.8036313725262,
0.));
#120054=CARTESIAN_POINT('Ctrl Pts',(67.9287278742839,-26.7858163326933,
0.));
#120055=CARTESIAN_POINT('Ctrl Pts',(67.9100574776974,-26.7680454034169,
0.));
#120056=CARTESIAN_POINT('Ctrl Pts',(67.8913983648441,-26.7503186158524,
0.));
#120057=CARTESIAN_POINT('Ctrl Pts',(67.8727506451067,-26.7326360011886,
0.));
#120058=CARTESIAN_POINT('Ctrl Pts',(67.8541144282875,-26.7149975906478,
0.));
#120059=CARTESIAN_POINT('Ctrl Pts',(67.8354898246079,-26.6974034154803,
0.));
#120060=CARTESIAN_POINT('Ctrl Pts',(67.8168769447086,-26.6798535069586,
0.));
#120061=CARTESIAN_POINT('Ctrl Pts',(67.7982758996557,-26.6623478963867,
0.));
#120062=CARTESIAN_POINT('Ctrl Pts',(67.7796868009447,-26.6448866151027,
0.));
#120063=CARTESIAN_POINT('Ctrl Pts',(67.7611097605042,-26.6274696944793,
0.));
#120064=CARTESIAN_POINT('Ctrl Pts',(67.7425448906983,-26.6100971659205,
0.));
#120065=CARTESIAN_POINT('Ctrl Pts',(67.7239923043295,-26.5927690608547,
0.));
#120066=CARTESIAN_POINT('Ctrl Pts',(67.7054521146427,-26.5754854107422,
0.));
#120067=CARTESIAN_POINT('Ctrl Pts',(67.6869244353292,-26.5582462470794,
0.));
#120068=CARTESIAN_POINT('Ctrl Pts',(67.6684093805288,-26.5410516013984,
0.));
#120069=CARTESIAN_POINT('Ctrl Pts',(67.6499070648323,-26.5239015052656,
0.));
#120070=CARTESIAN_POINT('Ctrl Pts',(67.6314176032823,-26.5067959902731,
0.));
#120071=CARTESIAN_POINT('Ctrl Pts',(67.6129411113774,-26.4897350880447,
0.));
#120072=CARTESIAN_POINT('Ctrl Pts',(67.5944777050782,-26.4727188302415,
0.));
#120073=CARTESIAN_POINT('Ctrl Pts',(67.5760275008096,-26.4557472485622,
0.));
#120074=CARTESIAN_POINT('Ctrl Pts',(67.5575906154648,-26.4388203747422,
0.));
#120075=CARTESIAN_POINT('Ctrl Pts',(67.5391671664055,-26.4219382405452,
0.));
#120076=CARTESIAN_POINT('Ctrl Pts',(67.5207572714666,-26.4051008777669,
0.));
#120077=CARTESIAN_POINT('Ctrl Pts',(67.5023610489611,-26.3883083182417,
0.));
#120078=CARTESIAN_POINT('Ctrl Pts',(67.4839786176833,-26.3715605938432,
0.));
#120079=CARTESIAN_POINT('Ctrl Pts',(67.4656100969121,-26.3548577364835,
0.));
#120080=CARTESIAN_POINT('Ctrl Pts',(67.4472556064127,-26.3381997781059,
0.));
#120081=CARTESIAN_POINT('Ctrl Pts',(67.4289152664406,-26.3215867506864,
0.));
#120082=CARTESIAN_POINT('Ctrl Pts',(67.4105891977465,-26.305018686241,0.));
#120083=CARTESIAN_POINT('Ctrl Pts',(67.392277521581,-26.2884956168271,0.));
#120084=CARTESIAN_POINT('Ctrl Pts',(67.3739803596967,-26.2720175745423,
0.));
#120085=CARTESIAN_POINT('Ctrl Pts',(67.3556978343506,-26.255584591518,0.));
#120086=CARTESIAN_POINT('Ctrl Pts',(67.3374300683076,-26.2391966999192,
0.));
#120087=CARTESIAN_POINT('Ctrl Pts',(67.3191771848468,-26.2228539319528,
0.));
#120088=CARTESIAN_POINT('Ctrl Pts',(67.3009393077654,-26.2065563198685,
0.));
#120089=CARTESIAN_POINT('Ctrl Pts',(67.2827165613828,-26.1903038959589,
0.));
#120090=CARTESIAN_POINT('Ctrl Pts',(67.2645090705414,-26.1740966925527,
0.));
#120091=CARTESIAN_POINT('Ctrl Pts',(67.2463169606105,-26.1579347420135,
0.));
#120092=CARTESIAN_POINT('Ctrl Pts',(67.228140357493,-26.1418180767487,0.));
#120093=CARTESIAN_POINT('Ctrl Pts',(67.2099793876295,-26.1257467292102,
0.));
#120094=CARTESIAN_POINT('Ctrl Pts',(67.191834178002,-26.109720731895,0.));
#120095=CARTESIAN_POINT('Ctrl Pts',(67.1737048561364,-26.0937401173385,
0.));
#120096=CARTESIAN_POINT('Ctrl Pts',(67.1555915501052,-26.077804918113,0.));
#120097=CARTESIAN_POINT('Ctrl Pts',(67.1374943885353,-26.0619151668361,
0.));
#120098=CARTESIAN_POINT('Ctrl Pts',(67.1194135006122,-26.0460708961725,
0.));
#120099=CARTESIAN_POINT('Ctrl Pts',(67.101349016084,-26.030272138834,0.));
#120100=CARTESIAN_POINT('Ctrl Pts',(67.083301065264,-26.0145189275733,0.));
#120101=CARTESIAN_POINT('Ctrl Pts',(67.0652697790335,-25.9988112951819,
0.));
#120102=CARTESIAN_POINT('Ctrl Pts',(67.0472552888495,-25.9831492744988,
0.));
#120103=CARTESIAN_POINT('Ctrl Pts',(67.0292577267495,-25.9675328984123,
0.));
#120104=CARTESIAN_POINT('Ctrl Pts',(67.0112772253553,-25.9519621998598,
0.));
#120105=CARTESIAN_POINT('Ctrl Pts',(66.993313917876,-25.9364372118216,0.));
#120106=CARTESIAN_POINT('Ctrl Pts',(66.9753679381122,-25.9209579673198,
0.));
#120107=CARTESIAN_POINT('Ctrl Pts',(66.9574394204635,-25.9055244994267,
0.));
#120108=CARTESIAN_POINT('Ctrl Pts',(66.9395284999327,-25.8901368412655,
0.));
#120109=CARTESIAN_POINT('Ctrl Pts',(66.9216353121308,-25.8747950260115,
0.));
#120110=CARTESIAN_POINT('Ctrl Pts',(66.9037599932787,-25.8594990868845,
0.));
#120111=CARTESIAN_POINT('Ctrl Pts',(66.8859026802123,-25.8442490571486,
0.));
#120112=CARTESIAN_POINT('Ctrl Pts',(66.8680635103907,-25.8290449701207,
0.));
#120113=CARTESIAN_POINT('Ctrl Pts',(66.8502426219015,-25.8138868591715,
0.));
#120114=CARTESIAN_POINT('Ctrl Pts',(66.8324401534657,-25.7987747577265,
0.));
#120115=CARTESIAN_POINT('Ctrl Pts',(66.8146562444397,-25.7837086992581,
0.));
#120116=CARTESIAN_POINT('Ctrl Pts',(66.7968910348199,-25.7686887172859,
0.));
#120117=CARTESIAN_POINT('Ctrl Pts',(66.7791446652505,-25.7537148453848,
0.));
#120118=CARTESIAN_POINT('Ctrl Pts',(66.7614172770302,-25.7387871171861,
0.));
#120119=CARTESIAN_POINT('Ctrl Pts',(66.7437090121168,-25.7239055663778,
0.));
#120120=CARTESIAN_POINT('Ctrl Pts',(66.72602001313,-25.7090702266976,0.));
#120121=CARTESIAN_POINT('Ctrl Pts',(66.7083504233566,-25.6942811319337,
0.));
#120122=CARTESIAN_POINT('Ctrl Pts',(66.6907003867599,-25.679538315933,0.));
#120123=CARTESIAN_POINT('Ctrl Pts',(66.6730700479843,-25.6648418126016,
0.));
#120124=CARTESIAN_POINT('Ctrl Pts',(66.6554595523611,-25.6501916559051,
0.));
#120125=CARTESIAN_POINT('Ctrl Pts',(66.6378690459105,-25.6355878798605,
0.));
#120126=CARTESIAN_POINT('Ctrl Pts',(66.6202986753482,-25.6210305185395,
0.));
#120127=CARTESIAN_POINT('Ctrl Pts',(66.6027485880947,-25.6065196060751,
0.));
#120128=CARTESIAN_POINT('Ctrl Pts',(66.585218932281,-25.5920551766629,0.));
#120129=CARTESIAN_POINT('Ctrl Pts',(66.567709856755,-25.5776372645605,0.));
#120130=CARTESIAN_POINT('Ctrl Pts',(66.5502215110843,-25.5632659040797,
0.));
#120131=CARTESIAN_POINT('Ctrl Pts',(66.5327540455638,-25.5489411295917,
0.));
#120132=CARTESIAN_POINT('Ctrl Pts',(66.5153076112237,-25.5346629755323,
0.));
#120133=CARTESIAN_POINT('Ctrl Pts',(66.4978823598352,-25.5204314764033,
0.));
#120134=CARTESIAN_POINT('Ctrl Pts',(66.4804784439146,-25.5062466667703,
0.));
#120135=CARTESIAN_POINT('Ctrl Pts',(66.463096016725,-25.4921085812548,0.));
#120136=CARTESIAN_POINT('Ctrl Pts',(66.445735232287,-25.4780172545418,0.));
#120137=CARTESIAN_POINT('Ctrl Pts',(66.4283962453899,-25.463972721385,0.));
#120138=CARTESIAN_POINT('Ctrl Pts',(66.4110792116,-25.4499750166079,0.));
#120139=CARTESIAN_POINT('Ctrl Pts',(66.3937842872684,-25.4360241751017,
0.));
#120140=CARTESIAN_POINT('Ctrl Pts',(66.3765116295363,-25.4221202318198,
0.));
#120141=CARTESIAN_POINT('Ctrl Pts',(66.3592613963407,-25.4082632217846,
0.));
#120142=CARTESIAN_POINT('Ctrl Pts',(66.3420337464176,-25.3944531800901,
0.));
#120143=CARTESIAN_POINT('Ctrl Pts',(66.3248288393046,-25.3806901419013,
0.));
#120144=CARTESIAN_POINT('Ctrl Pts',(66.3076468353417,-25.3669741424491,
0.));
#120145=CARTESIAN_POINT('Ctrl Pts',(66.2904878956721,-25.3533052170254,
0.));
#120146=CARTESIAN_POINT('Ctrl Pts',(66.2733521822675,-25.3396834009955,
0.));
#120147=CARTESIAN_POINT('Ctrl Pts',(66.2562398579479,-25.326108729803,0.));
#120148=CARTESIAN_POINT('Ctrl Pts',(66.2391510863992,-25.3125812389728,
0.));
#120149=CARTESIAN_POINT('Ctrl Pts',(66.2220860321931,-25.2991009641087,
0.));
#120150=CARTESIAN_POINT('Ctrl Pts',(66.2050448607883,-25.2856679408921,
0.));
#120151=CARTESIAN_POINT('Ctrl Pts',(66.1880277385114,-25.2722822050829,
0.));
#120152=CARTESIAN_POINT('Ctrl Pts',(66.1710348325378,-25.2589437925145,
0.));
#120153=CARTESIAN_POINT('Ctrl Pts',(66.1540663108767,-25.245652739088,0.));
#120154=CARTESIAN_POINT('Ctrl Pts',(66.1371223423371,-25.2324090807561,
0.));
#120155=CARTESIAN_POINT('Ctrl Pts',(66.1202030965784,-25.2192128535367,
0.));
#120156=CARTESIAN_POINT('Ctrl Pts',(66.1033087441916,-25.2060640935372,
0.));
#120157=CARTESIAN_POINT('Ctrl Pts',(66.086439456768,-25.1929628369685,0.));
#120158=CARTESIAN_POINT('Ctrl Pts',(66.0695954069698,-25.1799091201594,
0.));
#120159=CARTESIAN_POINT('Ctrl Pts',(66.0527767686,-25.1669029795652,0.));
#120160=CARTESIAN_POINT('Ctrl Pts',(66.0359837164709,-25.153944451741,0.));
#120161=CARTESIAN_POINT('Ctrl Pts',(66.0192164262607,-25.1410335733094,
0.));
#120162=CARTESIAN_POINT('Ctrl Pts',(66.0024750743902,-25.12817038093,0.));
#120163=CARTESIAN_POINT('Ctrl Pts',(65.9857598378455,-25.1153549112512,
0.));
#120164=CARTESIAN_POINT('Ctrl Pts',(65.9690708941591,-25.1025872009016,
0.));
#120165=CARTESIAN_POINT('Ctrl Pts',(65.9524084218167,-25.0898672865926,
0.));
#120166=CARTESIAN_POINT('Ctrl Pts',(65.9357726006174,-25.0771952052033,
0.));
#120167=CARTESIAN_POINT('Ctrl Pts',(65.9191636119796,-25.0645709938519,
0.));
#120168=CARTESIAN_POINT('Ctrl Pts',(65.9025816394391,-25.0519946900066,
0.));
#120169=CARTESIAN_POINT('Ctrl Pts',(65.8860268683088,-25.039466331404,0.));
#120170=CARTESIAN_POINT('Ctrl Pts',(65.8694994847587,-25.0269859558351,
0.));
#120171=CARTESIAN_POINT('Ctrl Pts',(65.8529996750441,-25.0145536009604,
0.));
#120172=CARTESIAN_POINT('Ctrl Pts',(65.8365276247157,-25.0021693041181,
0.));
#120173=CARTESIAN_POINT('Ctrl Pts',(65.8200835177071,-24.9898331021002,
0.));
#120174=CARTESIAN_POINT('Ctrl Pts',(65.8036675380761,-24.97754503157,0.));
#120175=CARTESIAN_POINT('Ctrl Pts',(65.7872798720847,-24.965305129559,0.));
#120176=CARTESIAN_POINT('Ctrl Pts',(65.7709207098949,-24.9531134338693,
0.));
#120177=CARTESIAN_POINT('Ctrl Pts',(65.7545902480286,-24.9409699836524,
0.));
#120178=CARTESIAN_POINT('Ctrl Pts',(65.7382886895839,-24.9288748194562,
0.));
#120179=CARTESIAN_POINT('Ctrl Pts',(65.7220162391016,-24.9168279820093,
0.));
#120180=CARTESIAN_POINT('Ctrl Pts',(65.7057730980471,-24.9048295111444,
0.));
#120181=CARTESIAN_POINT('Ctrl Pts',(65.6895594608798,-24.8928794448616,
0.));
#120182=CARTESIAN_POINT('Ctrl Pts',(65.6733755087723,-24.8809778178248,
0.));
#120183=CARTESIAN_POINT('Ctrl Pts',(65.6572214156761,-24.8691246628081,
0.));
#120184=CARTESIAN_POINT('Ctrl Pts',(65.6410973603713,-24.8573200135684,
0.));
#120185=CARTESIAN_POINT('Ctrl Pts',(65.6250035361612,-24.8455639071517,
0.));
#120186=CARTESIAN_POINT('Ctrl Pts',(65.6089401625551,-24.8338563866739,
0.));
#120187=CARTESIAN_POINT('Ctrl Pts',(65.5929074932487,-24.8221975032059,
0.));
#120188=CARTESIAN_POINT('Ctrl Pts',(65.5769057914184,-24.8105873098578,
0.));
#120189=CARTESIAN_POINT('Ctrl Pts',(65.5609353062749,-24.7990258561234,
0.));
#120190=CARTESIAN_POINT('Ctrl Pts',(65.5449962514735,-24.7875131827515,
0.));
#120191=CARTESIAN_POINT('Ctrl Pts',(65.5290887770493,-24.7760493148551,
0.));
#120192=CARTESIAN_POINT('Ctrl Pts',(65.5132129675727,-24.764634262097,0.));
#120193=CARTESIAN_POINT('Ctrl Pts',(65.5005376841469,-24.7555412724771,
0.));
#120194=CARTESIAN_POINT('Ctrl Pts',(65.4910454936487,-24.7487434956058,
0.));
#120195=CARTESIAN_POINT('Ctrl Pts',(65.484723709553,-24.7442214063411,0.));
#120196=CARTESIAN_POINT('Ctrl Pts',(65.4815644032299,-24.7419628022042,
0.));
#120197=CARTESIAN_POINT('Ctrl Pts',(66.3684712863594,-33.8448817269567,
0.));
#120198=CARTESIAN_POINT('Ctrl Pts',(66.3684712863594,-33.8448817269567,
12.));
#120199=CARTESIAN_POINT('Ctrl Pts',(66.3650082659712,-33.840486261887,0.));
#120200=CARTESIAN_POINT('Ctrl Pts',(66.3650082659712,-33.840486261887,12.));
#120201=CARTESIAN_POINT('Ctrl Pts',(66.3580824155893,-33.8316996011932,
0.));
#120202=CARTESIAN_POINT('Ctrl Pts',(66.3580824155893,-33.8316996011932,
12.));
#120203=CARTESIAN_POINT('Ctrl Pts',(66.3476942112,-33.8185324184903,0.));
#120204=CARTESIAN_POINT('Ctrl Pts',(66.3476942112,-33.8185324184903,12.));
#120205=CARTESIAN_POINT('Ctrl Pts',(66.3338444144211,-33.8010017926027,
0.));
#120206=CARTESIAN_POINT('Ctrl Pts',(66.3338444144211,-33.8010017926027,
12.));
#120207=CARTESIAN_POINT('Ctrl Pts',(66.3165340771611,-33.7791312145108,
0.));
#120208=CARTESIAN_POINT('Ctrl Pts',(66.3165340771611,-33.7791312145108,
12.));
#120209=CARTESIAN_POINT('Ctrl Pts',(66.2992256621336,-33.7573033544559,
0.));
#120210=CARTESIAN_POINT('Ctrl Pts',(66.2992256621336,-33.7573033544559,
12.));
#120211=CARTESIAN_POINT('Ctrl Pts',(66.2819191962353,-33.7355182321907,
0.));
#120212=CARTESIAN_POINT('Ctrl Pts',(66.2819191962353,-33.7355182321907,
12.));
#120213=CARTESIAN_POINT('Ctrl Pts',(66.2646147235321,-33.7137758735903,
0.));
#120214=CARTESIAN_POINT('Ctrl Pts',(66.2646147235321,-33.7137758735903,
12.));
#120215=CARTESIAN_POINT('Ctrl Pts',(66.2473123109395,-33.6920763111448,
0.));
#120216=CARTESIAN_POINT('Ctrl Pts',(66.2473123109395,-33.6920763111448,
12.));
#120217=CARTESIAN_POINT('Ctrl Pts',(66.2300120464082,-33.6704195830392,
0.));
#120218=CARTESIAN_POINT('Ctrl Pts',(66.2300120464082,-33.6704195830392,
12.));
#120219=CARTESIAN_POINT('Ctrl Pts',(66.2127140313598,-33.6488057311532,
0.));
#120220=CARTESIAN_POINT('Ctrl Pts',(66.2127140313598,-33.6488057311532,
12.));
#120221=CARTESIAN_POINT('Ctrl Pts',(66.1954183747088,-33.6272347993476,
0.));
#120222=CARTESIAN_POINT('Ctrl Pts',(66.1954183747088,-33.6272347993476,
12.));
#120223=CARTESIAN_POINT('Ctrl Pts',(66.1781251864017,-33.6057068316769,
0.));
#120224=CARTESIAN_POINT('Ctrl Pts',(66.1781251864017,-33.6057068316769,
12.));
#120225=CARTESIAN_POINT('Ctrl Pts',(66.1608345707636,-33.5842218705151,
0.));
#120226=CARTESIAN_POINT('Ctrl Pts',(66.1608345707636,-33.5842218705151,
12.));
#120227=CARTESIAN_POINT('Ctrl Pts',(66.1435466211076,-33.5627799550483,
0.));
#120228=CARTESIAN_POINT('Ctrl Pts',(66.1435466211076,-33.5627799550483,
12.));
#120229=CARTESIAN_POINT('Ctrl Pts',(66.1262614234674,-33.5413811223451,
0.));
#120230=CARTESIAN_POINT('Ctrl Pts',(66.1262614234674,-33.5413811223451,
12.));
#120231=CARTESIAN_POINT('Ctrl Pts',(66.1089790592729,-33.5200254081243,
0.));
#120232=CARTESIAN_POINT('Ctrl Pts',(66.1089790592729,-33.5200254081243,
12.));
#120233=CARTESIAN_POINT('Ctrl Pts',(66.0916996085244,-33.4987128476622,
0.));
#120234=CARTESIAN_POINT('Ctrl Pts',(66.0916996085244,-33.4987128476622,
12.));
#120235=CARTESIAN_POINT('Ctrl Pts',(66.0744231525415,-33.4774434765746,
0.));
#120236=CARTESIAN_POINT('Ctrl Pts',(66.0744231525415,-33.4774434765746,
12.));
#120237=CARTESIAN_POINT('Ctrl Pts',(66.0571497774434,-33.4562173318025,
0.));
#120238=CARTESIAN_POINT('Ctrl Pts',(66.0571497774434,-33.4562173318025,
12.));
#120239=CARTESIAN_POINT('Ctrl Pts',(66.0398795737777,-33.4350344515101,
0.));
#120240=CARTESIAN_POINT('Ctrl Pts',(66.0398795737777,-33.4350344515101,
12.));
#120241=CARTESIAN_POINT('Ctrl Pts',(66.0226126349446,-33.4138948746388,
0.));
#120242=CARTESIAN_POINT('Ctrl Pts',(66.0226126349446,-33.4138948746388,
12.));
#120243=CARTESIAN_POINT('Ctrl Pts',(66.0053490559812,-33.3927986405605,
0.));
#120244=CARTESIAN_POINT('Ctrl Pts',(66.0053490559812,-33.3927986405605,
12.));
#120245=CARTESIAN_POINT('Ctrl Pts',(65.9880889322831,-33.37174578871,0.));
#120246=CARTESIAN_POINT('Ctrl Pts',(65.9880889322831,-33.37174578871,12.));
#120247=CARTESIAN_POINT('Ctrl Pts',(65.970832358141,-33.3507363581593,0.));
#120248=CARTESIAN_POINT('Ctrl Pts',(65.970832358141,-33.3507363581593,12.));
#120249=CARTESIAN_POINT('Ctrl Pts',(65.9535794260831,-33.3297703874266,
0.));
#120250=CARTESIAN_POINT('Ctrl Pts',(65.9535794260831,-33.3297703874266,
12.));
#120251=CARTESIAN_POINT('Ctrl Pts',(65.9363302276846,-33.3088479147164,
0.));
#120252=CARTESIAN_POINT('Ctrl Pts',(65.9363302276846,-33.3088479147164,
12.));
#120253=CARTESIAN_POINT('Ctrl Pts',(65.9190848540433,-33.2879689780573,
0.));
#120254=CARTESIAN_POINT('Ctrl Pts',(65.9190848540433,-33.2879689780573,
12.));
#120255=CARTESIAN_POINT('Ctrl Pts',(65.9018433963889,-33.2671336154754,
0.));
#120256=CARTESIAN_POINT('Ctrl Pts',(65.9018433963889,-33.2671336154754,
12.));
#120257=CARTESIAN_POINT('Ctrl Pts',(65.8846059466371,-33.2463418651493,
0.));
#120258=CARTESIAN_POINT('Ctrl Pts',(65.8846059466371,-33.2463418651493,
12.));
#120259=CARTESIAN_POINT('Ctrl Pts',(65.8673725979577,-33.2255937655649,
0.));
#120260=CARTESIAN_POINT('Ctrl Pts',(65.8673725979577,-33.2255937655649,
12.));
#120261=CARTESIAN_POINT('Ctrl Pts',(65.8501434445164,-33.2048893554491,
0.));
#120262=CARTESIAN_POINT('Ctrl Pts',(65.8501434445164,-33.2048893554491,
12.));
#120263=CARTESIAN_POINT('Ctrl Pts',(65.8329185812375,-33.1842286737051,
0.));
#120264=CARTESIAN_POINT('Ctrl Pts',(65.8329185812375,-33.1842286737051,
12.));
#120265=CARTESIAN_POINT('Ctrl Pts',(65.8156981035503,-33.16361175934,0.));
#120266=CARTESIAN_POINT('Ctrl Pts',(65.8156981035503,-33.16361175934,12.));
#120267=CARTESIAN_POINT('Ctrl Pts',(65.7984821071623,-33.1430386513976,
0.));
#120268=CARTESIAN_POINT('Ctrl Pts',(65.7984821071623,-33.1430386513976,
12.));
#120269=CARTESIAN_POINT('Ctrl Pts',(65.7812706877696,-33.1225093888672,
0.));
#120270=CARTESIAN_POINT('Ctrl Pts',(65.7812706877696,-33.1225093888672,
12.));
#120271=CARTESIAN_POINT('Ctrl Pts',(65.7640639410661,-33.1020240106885,
0.));
#120272=CARTESIAN_POINT('Ctrl Pts',(65.7640639410661,-33.1020240106885,
12.));
#120273=CARTESIAN_POINT('Ctrl Pts',(65.7468619628815,-33.081582555798,0.));
#120274=CARTESIAN_POINT('Ctrl Pts',(65.7468619628815,-33.081582555798,12.));
#120275=CARTESIAN_POINT('Ctrl Pts',(65.7296648492824,-33.0611850631582,
0.));
#120276=CARTESIAN_POINT('Ctrl Pts',(65.7296648492824,-33.0611850631582,
12.));
#120277=CARTESIAN_POINT('Ctrl Pts',(65.7124726966802,-33.0408315717873,
0.));
#120278=CARTESIAN_POINT('Ctrl Pts',(65.7124726966802,-33.0408315717873,
12.));
#120279=CARTESIAN_POINT('Ctrl Pts',(65.6952856019533,-33.0205221207873,
0.));
#120280=CARTESIAN_POINT('Ctrl Pts',(65.6952856019533,-33.0205221207873,
12.));
#120281=CARTESIAN_POINT('Ctrl Pts',(65.6781036625027,-33.0002567493574,
0.));
#120282=CARTESIAN_POINT('Ctrl Pts',(65.6781036625027,-33.0002567493574,
12.));
#120283=CARTESIAN_POINT('Ctrl Pts',(65.6609269761888,-32.980035496784,0.));
#120284=CARTESIAN_POINT('Ctrl Pts',(65.6609269761888,-32.980035496784,12.));
#120285=CARTESIAN_POINT('Ctrl Pts',(65.6437556412946,-32.9598584024313,
0.));
#120286=CARTESIAN_POINT('Ctrl Pts',(65.6437556412946,-32.9598584024313,
12.));
#120287=CARTESIAN_POINT('Ctrl Pts',(65.6265897564783,-32.9397255057274,
0.));
#120288=CARTESIAN_POINT('Ctrl Pts',(65.6265897564783,-32.9397255057274,
12.));
#120289=CARTESIAN_POINT('Ctrl Pts',(65.6094294207276,-32.9196368461463,
0.));
#120290=CARTESIAN_POINT('Ctrl Pts',(65.6094294207276,-32.9196368461463,
12.));
#120291=CARTESIAN_POINT('Ctrl Pts',(65.5922747333194,-32.8995924631898,
0.));
#120292=CARTESIAN_POINT('Ctrl Pts',(65.5922747333194,-32.8995924631898,
12.));
#120293=CARTESIAN_POINT('Ctrl Pts',(65.5751257938472,-32.879592396403,0.));
#120294=CARTESIAN_POINT('Ctrl Pts',(65.5751257938472,-32.879592396403,12.));
#120295=CARTESIAN_POINT('Ctrl Pts',(65.5579827022421,-32.8596366853832,
0.));
#120296=CARTESIAN_POINT('Ctrl Pts',(65.5579827022421,-32.8596366853832,
12.));
#120297=CARTESIAN_POINT('Ctrl Pts',(65.5408455587964,-32.8397253697866,
0.));
#120298=CARTESIAN_POINT('Ctrl Pts',(65.5408455587964,-32.8397253697866,
12.));
#120299=CARTESIAN_POINT('Ctrl Pts',(65.5237144641857,-32.8198584893316,
0.));
#120300=CARTESIAN_POINT('Ctrl Pts',(65.5237144641857,-32.8198584893316,
12.));
#120301=CARTESIAN_POINT('Ctrl Pts',(65.5065895194928,-32.8000360837975,
0.));
#120302=CARTESIAN_POINT('Ctrl Pts',(65.5065895194928,-32.8000360837975,
12.));
#120303=CARTESIAN_POINT('Ctrl Pts',(65.489470826206,-32.7802581930287,0.));
#120304=CARTESIAN_POINT('Ctrl Pts',(65.489470826206,-32.7802581930287,12.));
#120305=CARTESIAN_POINT('Ctrl Pts',(65.4723584862122,-32.7605248569378,
0.));
#120306=CARTESIAN_POINT('Ctrl Pts',(65.4723584862122,-32.7605248569378,
12.));
#120307=CARTESIAN_POINT('Ctrl Pts',(65.4552526017905,-32.7408361155037,
0.));
#120308=CARTESIAN_POINT('Ctrl Pts',(65.4552526017905,-32.7408361155037,
12.));
#120309=CARTESIAN_POINT('Ctrl Pts',(65.4381532756065,-32.7211920087684,
0.));
#120310=CARTESIAN_POINT('Ctrl Pts',(65.4381532756065,-32.7211920087684,
12.));
#120311=CARTESIAN_POINT('Ctrl Pts',(65.4210606107035,-32.7015925768265,
0.));
#120312=CARTESIAN_POINT('Ctrl Pts',(65.4210606107035,-32.7015925768265,
12.));
#120313=CARTESIAN_POINT('Ctrl Pts',(65.4039747105038,-32.6820378598267,
0.));
#120314=CARTESIAN_POINT('Ctrl Pts',(65.4039747105038,-32.6820378598267,
12.));
#120315=CARTESIAN_POINT('Ctrl Pts',(65.3868956788182,-32.6625278979811,
0.));
#120316=CARTESIAN_POINT('Ctrl Pts',(65.3868956788182,-32.6625278979811,
12.));
#120317=CARTESIAN_POINT('Ctrl Pts',(65.3698236198512,-32.6430627315674,
0.));
#120318=CARTESIAN_POINT('Ctrl Pts',(65.3698236198512,-32.6430627315674,
12.));
#120319=CARTESIAN_POINT('Ctrl Pts',(65.3527586382081,-32.6236424009301,
0.));
#120320=CARTESIAN_POINT('Ctrl Pts',(65.3527586382081,-32.6236424009301,
12.));
#120321=CARTESIAN_POINT('Ctrl Pts',(65.3357008389003,-32.6042669464751,
0.));
#120322=CARTESIAN_POINT('Ctrl Pts',(65.3357008389003,-32.6042669464751,
12.));
#120323=CARTESIAN_POINT('Ctrl Pts',(65.31865032735,-32.5849364086679,0.));
#120324=CARTESIAN_POINT('Ctrl Pts',(65.31865032735,-32.5849364086679,12.));
#120325=CARTESIAN_POINT('Ctrl Pts',(65.3016072093912,-32.5656508280422,
0.));
#120326=CARTESIAN_POINT('Ctrl Pts',(65.3016072093912,-32.5656508280422,
12.));
#120327=CARTESIAN_POINT('Ctrl Pts',(65.2845715912721,-32.5464102452015,
0.));
#120328=CARTESIAN_POINT('Ctrl Pts',(65.2845715912721,-32.5464102452015,
12.));
#120329=CARTESIAN_POINT('Ctrl Pts',(65.2675435796558,-32.5272147008191,
0.));
#120330=CARTESIAN_POINT('Ctrl Pts',(65.2675435796558,-32.5272147008191,
12.));
#120331=CARTESIAN_POINT('Ctrl Pts',(65.2505232816209,-32.5080642356328,
0.));
#120332=CARTESIAN_POINT('Ctrl Pts',(65.2505232816209,-32.5080642356328,
12.));
#120333=CARTESIAN_POINT('Ctrl Pts',(65.2335108046614,-32.4889588904392,
0.));
#120334=CARTESIAN_POINT('Ctrl Pts',(65.2335108046614,-32.4889588904392,
12.));
#120335=CARTESIAN_POINT('Ctrl Pts',(65.2165062566924,-32.4698987061032,
0.));
#120336=CARTESIAN_POINT('Ctrl Pts',(65.2165062566924,-32.4698987061032,
12.));
#120337=CARTESIAN_POINT('Ctrl Pts',(65.1995097460538,-32.450883723561,0.));
#120338=CARTESIAN_POINT('Ctrl Pts',(65.1995097460538,-32.450883723561,12.));
#120339=CARTESIAN_POINT('Ctrl Pts',(65.182521381514,-32.4319139838213,0.));
#120340=CARTESIAN_POINT('Ctrl Pts',(65.182521381514,-32.4319139838213,12.));
#120341=CARTESIAN_POINT('Ctrl Pts',(65.1655412722725,-32.4129895279615,
0.));
#120342=CARTESIAN_POINT('Ctrl Pts',(65.1655412722725,-32.4129895279615,
12.));
#120343=CARTESIAN_POINT('Ctrl Pts',(65.1485695279635,-32.3941103971221,
0.));
#120344=CARTESIAN_POINT('Ctrl Pts',(65.1485695279635,-32.3941103971221,
12.));
#120345=CARTESIAN_POINT('Ctrl Pts',(65.1316062586588,-32.3752766325136,
0.));
#120346=CARTESIAN_POINT('Ctrl Pts',(65.1316062586588,-32.3752766325136,
12.));
#120347=CARTESIAN_POINT('Ctrl Pts',(65.1146515748722,-32.3564882754212,
0.));
#120348=CARTESIAN_POINT('Ctrl Pts',(65.1146515748722,-32.3564882754212,
12.));
#120349=CARTESIAN_POINT('Ctrl Pts',(65.0977055875607,-32.3377453672051,
0.));
#120350=CARTESIAN_POINT('Ctrl Pts',(65.0977055875607,-32.3377453672051,
12.));
#120351=CARTESIAN_POINT('Ctrl Pts',(65.0807684081281,-32.3190479492987,
0.));
#120352=CARTESIAN_POINT('Ctrl Pts',(65.0807684081281,-32.3190479492987,
12.));
#120353=CARTESIAN_POINT('Ctrl Pts',(65.0638401484257,-32.3003960632007,
0.));
#120354=CARTESIAN_POINT('Ctrl Pts',(65.0638401484257,-32.3003960632007,
12.));
#120355=CARTESIAN_POINT('Ctrl Pts',(65.0469209207563,-32.2817897504807,
0.));
#120356=CARTESIAN_POINT('Ctrl Pts',(65.0469209207563,-32.2817897504807,
12.));
#120357=CARTESIAN_POINT('Ctrl Pts',(65.03001083788,-32.2632290527862,0.));
#120358=CARTESIAN_POINT('Ctrl Pts',(65.03001083788,-32.2632290527862,12.));
#120359=CARTESIAN_POINT('Ctrl Pts',(65.0131100130157,-32.2447140118422,
0.));
#120360=CARTESIAN_POINT('Ctrl Pts',(65.0131100130157,-32.2447140118422,
12.));
#120361=CARTESIAN_POINT('Ctrl Pts',(64.9962185598461,-32.2262446694513,
0.));
#120362=CARTESIAN_POINT('Ctrl Pts',(64.9962185598461,-32.2262446694513,
12.));
#120363=CARTESIAN_POINT('Ctrl Pts',(64.9793365925178,-32.207821067485,0.));
#120364=CARTESIAN_POINT('Ctrl Pts',(64.9793365925178,-32.207821067485,12.));
#120365=CARTESIAN_POINT('Ctrl Pts',(64.9624642256461,-32.1894432478881,
0.));
#120366=CARTESIAN_POINT('Ctrl Pts',(64.9624642256461,-32.1894432478881,
12.));
#120367=CARTESIAN_POINT('Ctrl Pts',(64.9456015743192,-32.1711112526855,
0.));
#120368=CARTESIAN_POINT('Ctrl Pts',(64.9456015743192,-32.1711112526855,
12.));
#120369=CARTESIAN_POINT('Ctrl Pts',(64.9287487541015,-32.1528251239831,
0.));
#120370=CARTESIAN_POINT('Ctrl Pts',(64.9287487541015,-32.1528251239831,
12.));
#120371=CARTESIAN_POINT('Ctrl Pts',(64.9119058810366,-32.1345849039674,
0.));
#120372=CARTESIAN_POINT('Ctrl Pts',(64.9119058810366,-32.1345849039674,
12.));
#120373=CARTESIAN_POINT('Ctrl Pts',(64.8950730716501,-32.1163906348984,
0.));
#120374=CARTESIAN_POINT('Ctrl Pts',(64.8950730716501,-32.1163906348984,
12.));
#120375=CARTESIAN_POINT('Ctrl Pts',(64.8782504429527,-32.0982423591113,
0.));
#120376=CARTESIAN_POINT('Ctrl Pts',(64.8782504429527,-32.0982423591113,
12.));
#120377=CARTESIAN_POINT('Ctrl Pts',(64.8614381124454,-32.0801401190244,
0.));
#120378=CARTESIAN_POINT('Ctrl Pts',(64.8614381124454,-32.0801401190244,
12.));
#120379=CARTESIAN_POINT('Ctrl Pts',(64.8446361981234,-32.0620839571409,
0.));
#120380=CARTESIAN_POINT('Ctrl Pts',(64.8446361981234,-32.0620839571409,
12.));
#120381=CARTESIAN_POINT('Ctrl Pts',(64.8278448184785,-32.0440739160477,
0.));
#120382=CARTESIAN_POINT('Ctrl Pts',(64.8278448184785,-32.0440739160477,
12.));
#120383=CARTESIAN_POINT('Ctrl Pts',(64.811064092502,-32.0261100384092,0.));
#120384=CARTESIAN_POINT('Ctrl Pts',(64.811064092502,-32.0261100384092,12.));
#120385=CARTESIAN_POINT('Ctrl Pts',(64.7942941396883,-32.0081923669678,
0.));
#120386=CARTESIAN_POINT('Ctrl Pts',(64.7942941396883,-32.0081923669678,
12.));
#120387=CARTESIAN_POINT('Ctrl Pts',(64.7775350800404,-31.9903209445522,
0.));
#120388=CARTESIAN_POINT('Ctrl Pts',(64.7775350800404,-31.9903209445522,
12.));
#120389=CARTESIAN_POINT('Ctrl Pts',(64.7607870340738,-31.9724958140791,
0.));
#120390=CARTESIAN_POINT('Ctrl Pts',(64.7607870340738,-31.9724958140791,
12.));
#120391=CARTESIAN_POINT('Ctrl Pts',(64.74405012282,-31.9547170185533,0.));
#120392=CARTESIAN_POINT('Ctrl Pts',(64.74405012282,-31.9547170185533,12.));
#120393=CARTESIAN_POINT('Ctrl Pts',(64.727324467829,-31.9369846010613,0.));
#120394=CARTESIAN_POINT('Ctrl Pts',(64.727324467829,-31.9369846010613,12.));
#120395=CARTESIAN_POINT('Ctrl Pts',(64.7106101911722,-31.9192986047702,
0.));
#120396=CARTESIAN_POINT('Ctrl Pts',(64.7106101911722,-31.9192986047702,
12.));
#120397=CARTESIAN_POINT('Ctrl Pts',(64.693907415449,-31.9016590729371,0.));
#120398=CARTESIAN_POINT('Ctrl Pts',(64.693907415449,-31.9016590729371,12.));
#120399=CARTESIAN_POINT('Ctrl Pts',(64.6772162637904,-31.8840660489106,
0.));
#120400=CARTESIAN_POINT('Ctrl Pts',(64.6772162637904,-31.8840660489106,
12.));
#120401=CARTESIAN_POINT('Ctrl Pts',(64.6605368598631,-31.8665195761312,
0.));
#120402=CARTESIAN_POINT('Ctrl Pts',(64.6605368598631,-31.8665195761312,
12.));
#120403=CARTESIAN_POINT('Ctrl Pts',(64.6438693278718,-31.849019698125,0.));
#120404=CARTESIAN_POINT('Ctrl Pts',(64.6438693278718,-31.849019698125,12.));
#120405=CARTESIAN_POINT('Ctrl Pts',(64.6272137925629,-31.8315664585027,
0.));
#120406=CARTESIAN_POINT('Ctrl Pts',(64.6272137925629,-31.8315664585027,
12.));
#120407=CARTESIAN_POINT('Ctrl Pts',(64.6105703792311,-31.8141599009685,
0.));
#120408=CARTESIAN_POINT('Ctrl Pts',(64.6105703792311,-31.8141599009685,
12.));
#120409=CARTESIAN_POINT('Ctrl Pts',(64.5939392137233,-31.7968000693218,
0.));
#120410=CARTESIAN_POINT('Ctrl Pts',(64.5939392137233,-31.7968000693218,
12.));
#120411=CARTESIAN_POINT('Ctrl Pts',(64.5773204224429,-31.7794870074584,
0.));
#120412=CARTESIAN_POINT('Ctrl Pts',(64.5773204224429,-31.7794870074584,
12.));
#120413=CARTESIAN_POINT('Ctrl Pts',(64.5607141323527,-31.7622207593637,
0.));
#120414=CARTESIAN_POINT('Ctrl Pts',(64.5607141323527,-31.7622207593637,
12.));
#120415=CARTESIAN_POINT('Ctrl Pts',(64.5441204709779,-31.7450013691117,
0.));
#120416=CARTESIAN_POINT('Ctrl Pts',(64.5441204709779,-31.7450013691117,
12.));
#120417=CARTESIAN_POINT('Ctrl Pts',(64.5275395664134,-31.7278288808736,
0.));
#120418=CARTESIAN_POINT('Ctrl Pts',(64.5275395664134,-31.7278288808736,
12.));
#120419=CARTESIAN_POINT('Ctrl Pts',(64.5109715473276,-31.7107033389204,
0.));
#120420=CARTESIAN_POINT('Ctrl Pts',(64.5109715473276,-31.7107033389204,
12.));
#120421=CARTESIAN_POINT('Ctrl Pts',(64.4944165429672,-31.6936247876228,
0.));
#120422=CARTESIAN_POINT('Ctrl Pts',(64.4944165429672,-31.6936247876228,
12.));
#120423=CARTESIAN_POINT('Ctrl Pts',(64.4778746831597,-31.6765932714456,
0.));
#120424=CARTESIAN_POINT('Ctrl Pts',(64.4778746831597,-31.6765932714456,
12.));
#120425=CARTESIAN_POINT('Ctrl Pts',(64.4613460983186,-31.6596088349468,
0.));
#120426=CARTESIAN_POINT('Ctrl Pts',(64.4613460983186,-31.6596088349468,
12.));
#120427=CARTESIAN_POINT('Ctrl Pts',(64.4448309194498,-31.6426715227865,
0.));
#120428=CARTESIAN_POINT('Ctrl Pts',(64.4448309194498,-31.6426715227865,
12.));
#120429=CARTESIAN_POINT('Ctrl Pts',(64.4283292781553,-31.6257813797282,
0.));
#120430=CARTESIAN_POINT('Ctrl Pts',(64.4283292781553,-31.6257813797282,
12.));
#120431=CARTESIAN_POINT('Ctrl Pts',(64.4118413066386,-31.6089384506399,
0.));
#120432=CARTESIAN_POINT('Ctrl Pts',(64.4118413066386,-31.6089384506399,
12.));
#120433=CARTESIAN_POINT('Ctrl Pts',(64.3953671377071,-31.5921427804879,
0.));
#120434=CARTESIAN_POINT('Ctrl Pts',(64.3953671377071,-31.5921427804879,
12.));
#120435=CARTESIAN_POINT('Ctrl Pts',(64.3789069047768,-31.5753944143355,
0.));
#120436=CARTESIAN_POINT('Ctrl Pts',(64.3789069047768,-31.5753944143355,
12.));
#120437=CARTESIAN_POINT('Ctrl Pts',(64.3624607418798,-31.5586933973532,
0.));
#120438=CARTESIAN_POINT('Ctrl Pts',(64.3624607418798,-31.5586933973532,
12.));
#120439=CARTESIAN_POINT('Ctrl Pts',(64.34602878367,-31.5420397748198,0.));
#120440=CARTESIAN_POINT('Ctrl Pts',(64.34602878367,-31.5420397748198,12.));
#120441=CARTESIAN_POINT('Ctrl Pts',(64.3296111654273,-31.525433592124,0.));
#120442=CARTESIAN_POINT('Ctrl Pts',(64.3296111654273,-31.525433592124,12.));
#120443=CARTESIAN_POINT('Ctrl Pts',(64.3132080230603,-31.5088748947565,
0.));
#120444=CARTESIAN_POINT('Ctrl Pts',(64.3132080230603,-31.5088748947565,
12.));
#120445=CARTESIAN_POINT('Ctrl Pts',(64.2968194931113,-31.4923637283109,
0.));
#120446=CARTESIAN_POINT('Ctrl Pts',(64.2968194931113,-31.4923637283109,
12.));
#120447=CARTESIAN_POINT('Ctrl Pts',(64.2804457127633,-31.4759001384923,
0.));
#120448=CARTESIAN_POINT('Ctrl Pts',(64.2804457127633,-31.4759001384923,
12.));
#120449=CARTESIAN_POINT('Ctrl Pts',(64.264086819846,-31.4594841711189,0.));
#120450=CARTESIAN_POINT('Ctrl Pts',(64.264086819846,-31.4594841711189,12.));
#120451=CARTESIAN_POINT('Ctrl Pts',(64.2477429528408,-31.443115872123,0.));
#120452=CARTESIAN_POINT('Ctrl Pts',(64.2477429528408,-31.443115872123,12.));
#120453=CARTESIAN_POINT('Ctrl Pts',(64.2314142508843,-31.426795287544,0.));
#120454=CARTESIAN_POINT('Ctrl Pts',(64.2314142508843,-31.426795287544,12.));
#120455=CARTESIAN_POINT('Ctrl Pts',(64.2151008537733,-31.4105224635298,
0.));
#120456=CARTESIAN_POINT('Ctrl Pts',(64.2151008537733,-31.4105224635298,
12.));
#120457=CARTESIAN_POINT('Ctrl Pts',(64.1988029019733,-31.3942974463458,
0.));
#120458=CARTESIAN_POINT('Ctrl Pts',(64.1988029019733,-31.3942974463458,
12.));
#120459=CARTESIAN_POINT('Ctrl Pts',(64.1825205366231,-31.3781202823758,
0.));
#120460=CARTESIAN_POINT('Ctrl Pts',(64.1825205366231,-31.3781202823758,
12.));
#120461=CARTESIAN_POINT('Ctrl Pts',(64.1662538995407,-31.3619910181223,
0.));
#120462=CARTESIAN_POINT('Ctrl Pts',(64.1662538995407,-31.3619910181223,
12.));
#120463=CARTESIAN_POINT('Ctrl Pts',(64.150003133226,-31.3459097001996,0.));
#120464=CARTESIAN_POINT('Ctrl Pts',(64.150003133226,-31.3459097001996,12.));
#120465=CARTESIAN_POINT('Ctrl Pts',(64.1337683808667,-31.3298763753366,
0.));
#120466=CARTESIAN_POINT('Ctrl Pts',(64.1337683808667,-31.3298763753366,
12.));
#120467=CARTESIAN_POINT('Ctrl Pts',(64.1175497863475,-31.3138910903852,
0.));
#120468=CARTESIAN_POINT('Ctrl Pts',(64.1175497863475,-31.3138910903852,
12.));
#120469=CARTESIAN_POINT('Ctrl Pts',(64.1013474942554,-31.2979538923214,
0.));
#120470=CARTESIAN_POINT('Ctrl Pts',(64.1013474942554,-31.2979538923214,
12.));
#120471=CARTESIAN_POINT('Ctrl Pts',(64.0851616498861,-31.2820648282451,
0.));
#120472=CARTESIAN_POINT('Ctrl Pts',(64.0851616498861,-31.2820648282451,
12.));
#120473=CARTESIAN_POINT('Ctrl Pts',(64.0689923992474,-31.2662239453734,
0.));
#120474=CARTESIAN_POINT('Ctrl Pts',(64.0689923992474,-31.2662239453734,
12.));
#120475=CARTESIAN_POINT('Ctrl Pts',(64.0528398890671,-31.2504312910457,
0.));
#120476=CARTESIAN_POINT('Ctrl Pts',(64.0528398890671,-31.2504312910457,
12.));
#120477=CARTESIAN_POINT('Ctrl Pts',(64.036704266799,-31.23468691273,0.));
#120478=CARTESIAN_POINT('Ctrl Pts',(64.036704266799,-31.23468691273,12.));
#120479=CARTESIAN_POINT('Ctrl Pts',(64.0205856806298,-31.2189908580245,
0.));
#120480=CARTESIAN_POINT('Ctrl Pts',(64.0205856806298,-31.2189908580245,
12.));
#120481=CARTESIAN_POINT('Ctrl Pts',(64.004484279483,-31.2033431746559,0.));
#120482=CARTESIAN_POINT('Ctrl Pts',(64.004484279483,-31.2033431746559,12.));
#120483=CARTESIAN_POINT('Ctrl Pts',(63.9884002130209,-31.1877439104717,
0.));
#120484=CARTESIAN_POINT('Ctrl Pts',(63.9884002130209,-31.1877439104717,
12.));
#120485=CARTESIAN_POINT('Ctrl Pts',(63.972333631655,-31.1721931134488,0.));
#120486=CARTESIAN_POINT('Ctrl Pts',(63.972333631655,-31.1721931134488,12.));
#120487=CARTESIAN_POINT('Ctrl Pts',(63.9562846865566,-31.1566908316993,
0.));
#120488=CARTESIAN_POINT('Ctrl Pts',(63.9562846865566,-31.1566908316993,
12.));
#120489=CARTESIAN_POINT('Ctrl Pts',(63.940253529665,-31.1412371134727,0.));
#120490=CARTESIAN_POINT('Ctrl Pts',(63.940253529665,-31.1412371134727,12.));
#120491=CARTESIAN_POINT('Ctrl Pts',(63.9242403136954,-31.1258320071545,
0.));
#120492=CARTESIAN_POINT('Ctrl Pts',(63.9242403136954,-31.1258320071545,
12.));
#120493=CARTESIAN_POINT('Ctrl Pts',(63.9082451921447,-31.1104755612606,
0.));
#120494=CARTESIAN_POINT('Ctrl Pts',(63.9082451921447,-31.1104755612606,
12.));
#120495=CARTESIAN_POINT('Ctrl Pts',(63.8922683192962,-31.0951678244454,
0.));
#120496=CARTESIAN_POINT('Ctrl Pts',(63.8922683192962,-31.0951678244454,
12.));
#120497=CARTESIAN_POINT('Ctrl Pts',(63.8763098502235,-31.079908845504,0.));
#120498=CARTESIAN_POINT('Ctrl Pts',(63.8763098502235,-31.079908845504,12.));
#120499=CARTESIAN_POINT('Ctrl Pts',(63.8603699407922,-31.0646986733724,
0.));
#120500=CARTESIAN_POINT('Ctrl Pts',(63.8603699407922,-31.0646986733724,
12.));
#120501=CARTESIAN_POINT('Ctrl Pts',(63.8444487476615,-31.0495373571218,
0.));
#120502=CARTESIAN_POINT('Ctrl Pts',(63.8444487476615,-31.0495373571218,
12.));
#120503=CARTESIAN_POINT('Ctrl Pts',(63.8285464282857,-31.0344249459544,
0.));
#120504=CARTESIAN_POINT('Ctrl Pts',(63.8285464282857,-31.0344249459544,
12.));
#120505=CARTESIAN_POINT('Ctrl Pts',(63.8126631409376,-31.0193614892177,
0.));
#120506=CARTESIAN_POINT('Ctrl Pts',(63.8126631409376,-31.0193614892177,
12.));
#120507=CARTESIAN_POINT('Ctrl Pts',(63.7967990447287,-31.0043470364112,
0.));
#120508=CARTESIAN_POINT('Ctrl Pts',(63.7967990447287,-31.0043470364112,
12.));
#120509=CARTESIAN_POINT('Ctrl Pts',(63.7809542996258,-30.9893816371907,
0.));
#120510=CARTESIAN_POINT('Ctrl Pts',(63.7809542996258,-30.9893816371907,
12.));
#120511=CARTESIAN_POINT('Ctrl Pts',(63.7651290664713,-30.9744653413679,
0.));
#120512=CARTESIAN_POINT('Ctrl Pts',(63.7651290664713,-30.9744653413679,
12.));
#120513=CARTESIAN_POINT('Ctrl Pts',(63.7493235069844,-30.9595981989091,
0.));
#120514=CARTESIAN_POINT('Ctrl Pts',(63.7493235069844,-30.9595981989091,
12.));
#120515=CARTESIAN_POINT('Ctrl Pts',(63.733537783742,-30.9447802599345,0.));
#120516=CARTESIAN_POINT('Ctrl Pts',(63.733537783742,-30.9447802599345,12.));
#120517=CARTESIAN_POINT('Ctrl Pts',(63.7177720601604,-30.9300115747113,
0.));
#120518=CARTESIAN_POINT('Ctrl Pts',(63.7177720601604,-30.9300115747113,
12.));
#120519=CARTESIAN_POINT('Ctrl Pts',(63.7020265004805,-30.9152921936471,
0.));
#120520=CARTESIAN_POINT('Ctrl Pts',(63.7020265004805,-30.9152921936471,
12.));
#120521=CARTESIAN_POINT('Ctrl Pts',(63.6863012697353,-30.9006221672703,
0.));
#120522=CARTESIAN_POINT('Ctrl Pts',(63.6863012697353,-30.9006221672703,
12.));
#120523=CARTESIAN_POINT('Ctrl Pts',(63.6705965337996,-30.8860015462488,
0.));
#120524=CARTESIAN_POINT('Ctrl Pts',(63.6705965337996,-30.8860015462488,
12.));
#120525=CARTESIAN_POINT('Ctrl Pts',(63.6549124594681,-30.8714303814202,
0.));
#120526=CARTESIAN_POINT('Ctrl Pts',(63.6549124594681,-30.8714303814202,
12.));
#120527=CARTESIAN_POINT('Ctrl Pts',(63.6392492145233,-30.8569087238132,
0.));
#120528=CARTESIAN_POINT('Ctrl Pts',(63.6392492145233,-30.8569087238132,
12.));
#120529=CARTESIAN_POINT('Ctrl Pts',(63.6236069678041,-30.8424366246665,
0.));
#120530=CARTESIAN_POINT('Ctrl Pts',(63.6236069678041,-30.8424366246665,
12.));
#120531=CARTESIAN_POINT('Ctrl Pts',(63.6079858892746,-30.8280141354448,
0.));
#120532=CARTESIAN_POINT('Ctrl Pts',(63.6079858892746,-30.8280141354448,
12.));
#120533=CARTESIAN_POINT('Ctrl Pts',(63.5923861498963,-30.8136413077999,
0.));
#120534=CARTESIAN_POINT('Ctrl Pts',(63.5923861498963,-30.8136413077999,
12.));
#120535=CARTESIAN_POINT('Ctrl Pts',(63.5768079214868,-30.7993181935265,
0.));
#120536=CARTESIAN_POINT('Ctrl Pts',(63.5768079214868,-30.7993181935265,
12.));
#120537=CARTESIAN_POINT('Ctrl Pts',(63.5612513766005,-30.7850448445207,
0.));
#120538=CARTESIAN_POINT('Ctrl Pts',(63.5612513766005,-30.7850448445207,
12.));
#120539=CARTESIAN_POINT('Ctrl Pts',(63.5457166883558,-30.7708213127169,
0.));
#120540=CARTESIAN_POINT('Ctrl Pts',(63.5457166883558,-30.7708213127169,
12.));
#120541=CARTESIAN_POINT('Ctrl Pts',(63.5302040304173,-30.7566476500772,
0.));
#120542=CARTESIAN_POINT('Ctrl Pts',(63.5302040304173,-30.7566476500772,
12.));
#120543=CARTESIAN_POINT('Ctrl Pts',(63.514713577392,-30.7425239087294,0.));
#120544=CARTESIAN_POINT('Ctrl Pts',(63.514713577392,-30.7425239087294,12.));
#120545=CARTESIAN_POINT('Ctrl Pts',(63.4992455051805,-30.7284501410827,
0.));
#120546=CARTESIAN_POINT('Ctrl Pts',(63.4992455051805,-30.7284501410827,
12.));
#120547=CARTESIAN_POINT('Ctrl Pts',(63.4837999912758,-30.7144263999259,
0.));
#120548=CARTESIAN_POINT('Ctrl Pts',(63.4837999912758,-30.7144263999259,
12.));
#120549=CARTESIAN_POINT('Ctrl Pts',(63.4683772152497,-30.7004527385806,
0.));
#120550=CARTESIAN_POINT('Ctrl Pts',(63.4683772152497,-30.7004527385806,
12.));
#120551=CARTESIAN_POINT('Ctrl Pts',(63.452977358421,-30.6865292107911,0.));
#120552=CARTESIAN_POINT('Ctrl Pts',(63.452977358421,-30.6865292107911,12.));
#120553=CARTESIAN_POINT('Ctrl Pts',(63.4376006029575,-30.6726558704302,
0.));
#120554=CARTESIAN_POINT('Ctrl Pts',(63.4376006029575,-30.6726558704302,
12.));
#120555=CARTESIAN_POINT('Ctrl Pts',(63.4222471311236,-30.6588327712482,
0.));
#120556=CARTESIAN_POINT('Ctrl Pts',(63.4222471311236,-30.6588327712482,
12.));
#120557=CARTESIAN_POINT('Ctrl Pts',(63.4069171245093,-30.6450599666135,
0.));
#120558=CARTESIAN_POINT('Ctrl Pts',(63.4069171245093,-30.6450599666135,
12.));
#120559=CARTESIAN_POINT('Ctrl Pts',(63.3916107631421,-30.6313375092085,
0.));
#120560=CARTESIAN_POINT('Ctrl Pts',(63.3916107631421,-30.6313375092085,
12.));
#120561=CARTESIAN_POINT('Ctrl Pts',(63.3763282271838,-30.6176654515988,
0.));
#120562=CARTESIAN_POINT('Ctrl Pts',(63.3763282271838,-30.6176654515988,
12.));
#120563=CARTESIAN_POINT('Ctrl Pts',(63.3610696989599,-30.604043846909,0.));
#120564=CARTESIAN_POINT('Ctrl Pts',(63.3610696989599,-30.604043846909,12.));
#120565=CARTESIAN_POINT('Ctrl Pts',(63.3458353646144,-30.5904727493707,
0.));
#120566=CARTESIAN_POINT('Ctrl Pts',(63.3458353646144,-30.5904727493707,
12.));
#120567=CARTESIAN_POINT('Ctrl Pts',(63.330625416509,-30.5769522151147,0.));
#120568=CARTESIAN_POINT('Ctrl Pts',(63.330625416509,-30.5769522151147,12.));
#120569=CARTESIAN_POINT('Ctrl Pts',(63.315440053435,-30.5634823022358,0.));
#120570=CARTESIAN_POINT('Ctrl Pts',(63.315440053435,-30.5634823022358,12.));
#120571=CARTESIAN_POINT('Ctrl Pts',(63.3002794756049,-30.5500630691343,
0.));
#120572=CARTESIAN_POINT('Ctrl Pts',(63.3002794756049,-30.5500630691343,
12.));
#120573=CARTESIAN_POINT('Ctrl Pts',(63.2851438802462,-30.5366945730503,
0.));
#120574=CARTESIAN_POINT('Ctrl Pts',(63.2851438802462,-30.5366945730503,
12.));
#120575=CARTESIAN_POINT('Ctrl Pts',(63.2700334577661,-30.5233768687875,
0.));
#120576=CARTESIAN_POINT('Ctrl Pts',(63.2700334577661,-30.5233768687875,
12.));
#120577=CARTESIAN_POINT('Ctrl Pts',(63.2549483856268,-30.5101100066683,
0.));
#120578=CARTESIAN_POINT('Ctrl Pts',(63.2549483856268,-30.5101100066683,
12.));
#120579=CARTESIAN_POINT('Ctrl Pts',(63.2398888342612,-30.4968940345028,
0.));
#120580=CARTESIAN_POINT('Ctrl Pts',(63.2398888342612,-30.4968940345028,
12.));
#120581=CARTESIAN_POINT('Ctrl Pts',(63.2248549788272,-30.4837290015011,
0.));
#120582=CARTESIAN_POINT('Ctrl Pts',(63.2248549788272,-30.4837290015011,
12.));
#120583=CARTESIAN_POINT('Ctrl Pts',(63.2098470086636,-30.470614961416,0.));
#120584=CARTESIAN_POINT('Ctrl Pts',(63.2098470086636,-30.470614961416,12.));
#120585=CARTESIAN_POINT('Ctrl Pts',(63.1948651386868,-30.4575519763305,
0.));
#120586=CARTESIAN_POINT('Ctrl Pts',(63.1948651386868,-30.4575519763305,
12.));
#120587=CARTESIAN_POINT('Ctrl Pts',(63.1799096171757,-30.4445401192324,
0.));
#120588=CARTESIAN_POINT('Ctrl Pts',(63.1799096171757,-30.4445401192324,
12.));
#120589=CARTESIAN_POINT('Ctrl Pts',(63.1649807016766,-30.431579465967,0.));
#120590=CARTESIAN_POINT('Ctrl Pts',(63.1649807016766,-30.431579465967,12.));
#120591=CARTESIAN_POINT('Ctrl Pts',(63.1500786361382,-30.4186700875598,
0.));
#120592=CARTESIAN_POINT('Ctrl Pts',(63.1500786361382,-30.4186700875598,
12.));
#120593=CARTESIAN_POINT('Ctrl Pts',(63.1352036298512,-30.4058120432259,
0.));
#120594=CARTESIAN_POINT('Ctrl Pts',(63.1352036298512,-30.4058120432259,
12.));
#120595=CARTESIAN_POINT('Ctrl Pts',(63.1203558300911,-30.3930053710592,
0.));
#120596=CARTESIAN_POINT('Ctrl Pts',(63.1203558300911,-30.3930053710592,
12.));
#120597=CARTESIAN_POINT('Ctrl Pts',(63.1055353202641,-30.3802500880565,
0.));
#120598=CARTESIAN_POINT('Ctrl Pts',(63.1055353202641,-30.3802500880565,
12.));
#120599=CARTESIAN_POINT('Ctrl Pts',(63.0937007763826,-30.3700869762658,
0.));
#120600=CARTESIAN_POINT('Ctrl Pts',(63.0937007763826,-30.3700869762658,
12.));
#120601=CARTESIAN_POINT('Ctrl Pts',(63.0848371718274,-30.3624877680747,
0.));
#120602=CARTESIAN_POINT('Ctrl Pts',(63.0848371718274,-30.3624877680747,
12.));
#120603=CARTESIAN_POINT('Ctrl Pts',(63.0789335700774,-30.3574319069366,
0.));
#120604=CARTESIAN_POINT('Ctrl Pts',(63.0789335700774,-30.3574319069366,
12.));
#120605=CARTESIAN_POINT('Ctrl Pts',(63.0759831361898,-30.3549065457811,
0.));
#120606=CARTESIAN_POINT('Ctrl Pts',(63.0759831361898,-30.3549065457811,
12.));
#120607=CARTESIAN_POINT('',(63.0759831361898,-30.3549065457811,12.));
#120608=CARTESIAN_POINT('Ctrl Pts',(63.0759831361898,-30.3549065457811,
12.));
#120609=CARTESIAN_POINT('Ctrl Pts',(63.0789335700774,-30.3574319069366,
12.));
#120610=CARTESIAN_POINT('Ctrl Pts',(63.0848371718274,-30.3624877680747,
12.));
#120611=CARTESIAN_POINT('Ctrl Pts',(63.0937007763826,-30.3700869762658,
12.));
#120612=CARTESIAN_POINT('Ctrl Pts',(63.1055353202641,-30.3802500880565,
12.));
#120613=CARTESIAN_POINT('Ctrl Pts',(63.1203558300911,-30.3930053710592,
12.));
#120614=CARTESIAN_POINT('Ctrl Pts',(63.1352036298512,-30.4058120432259,
12.));
#120615=CARTESIAN_POINT('Ctrl Pts',(63.1500786361382,-30.4186700875598,
12.));
#120616=CARTESIAN_POINT('Ctrl Pts',(63.1649807016766,-30.431579465967,12.));
#120617=CARTESIAN_POINT('Ctrl Pts',(63.1799096171757,-30.4445401192324,
12.));
#120618=CARTESIAN_POINT('Ctrl Pts',(63.1948651386868,-30.4575519763305,
12.));
#120619=CARTESIAN_POINT('Ctrl Pts',(63.2098470086636,-30.470614961416,12.));
#120620=CARTESIAN_POINT('Ctrl Pts',(63.2248549788272,-30.4837290015011,
12.));
#120621=CARTESIAN_POINT('Ctrl Pts',(63.2398888342612,-30.4968940345028,
12.));
#120622=CARTESIAN_POINT('Ctrl Pts',(63.2549483856268,-30.5101100066683,
12.));
#120623=CARTESIAN_POINT('Ctrl Pts',(63.2700334577661,-30.5233768687875,
12.));
#120624=CARTESIAN_POINT('Ctrl Pts',(63.2851438802462,-30.5366945730503,
12.));
#120625=CARTESIAN_POINT('Ctrl Pts',(63.3002794756049,-30.5500630691343,
12.));
#120626=CARTESIAN_POINT('Ctrl Pts',(63.315440053435,-30.5634823022358,12.));
#120627=CARTESIAN_POINT('Ctrl Pts',(63.330625416509,-30.5769522151147,12.));
#120628=CARTESIAN_POINT('Ctrl Pts',(63.3458353646144,-30.5904727493707,
12.));
#120629=CARTESIAN_POINT('Ctrl Pts',(63.3610696989599,-30.604043846909,12.));
#120630=CARTESIAN_POINT('Ctrl Pts',(63.3763282271838,-30.6176654515988,
12.));
#120631=CARTESIAN_POINT('Ctrl Pts',(63.3916107631421,-30.6313375092085,
12.));
#120632=CARTESIAN_POINT('Ctrl Pts',(63.4069171245093,-30.6450599666135,
12.));
#120633=CARTESIAN_POINT('Ctrl Pts',(63.4222471311236,-30.6588327712482,
12.));
#120634=CARTESIAN_POINT('Ctrl Pts',(63.4376006029575,-30.6726558704302,
12.));
#120635=CARTESIAN_POINT('Ctrl Pts',(63.452977358421,-30.6865292107911,12.));
#120636=CARTESIAN_POINT('Ctrl Pts',(63.4683772152497,-30.7004527385806,
12.));
#120637=CARTESIAN_POINT('Ctrl Pts',(63.4837999912758,-30.7144263999259,
12.));
#120638=CARTESIAN_POINT('Ctrl Pts',(63.4992455051805,-30.7284501410827,
12.));
#120639=CARTESIAN_POINT('Ctrl Pts',(63.514713577392,-30.7425239087294,12.));
#120640=CARTESIAN_POINT('Ctrl Pts',(63.5302040304173,-30.7566476500772,
12.));
#120641=CARTESIAN_POINT('Ctrl Pts',(63.5457166883558,-30.7708213127169,
12.));
#120642=CARTESIAN_POINT('Ctrl Pts',(63.5612513766005,-30.7850448445207,
12.));
#120643=CARTESIAN_POINT('Ctrl Pts',(63.5768079214868,-30.7993181935265,
12.));
#120644=CARTESIAN_POINT('Ctrl Pts',(63.5923861498963,-30.8136413077999,
12.));
#120645=CARTESIAN_POINT('Ctrl Pts',(63.6079858892746,-30.8280141354448,
12.));
#120646=CARTESIAN_POINT('Ctrl Pts',(63.6236069678041,-30.8424366246665,
12.));
#120647=CARTESIAN_POINT('Ctrl Pts',(63.6392492145233,-30.8569087238132,
12.));
#120648=CARTESIAN_POINT('Ctrl Pts',(63.6549124594681,-30.8714303814202,
12.));
#120649=CARTESIAN_POINT('Ctrl Pts',(63.6705965337996,-30.8860015462488,
12.));
#120650=CARTESIAN_POINT('Ctrl Pts',(63.6863012697353,-30.9006221672703,
12.));
#120651=CARTESIAN_POINT('Ctrl Pts',(63.7020265004805,-30.9152921936471,
12.));
#120652=CARTESIAN_POINT('Ctrl Pts',(63.7177720601604,-30.9300115747113,
12.));
#120653=CARTESIAN_POINT('Ctrl Pts',(63.733537783742,-30.9447802599345,12.));
#120654=CARTESIAN_POINT('Ctrl Pts',(63.7493235069844,-30.9595981989091,
12.));
#120655=CARTESIAN_POINT('Ctrl Pts',(63.7651290664713,-30.9744653413679,
12.));
#120656=CARTESIAN_POINT('Ctrl Pts',(63.7809542996258,-30.9893816371907,
12.));
#120657=CARTESIAN_POINT('Ctrl Pts',(63.7967990447287,-31.0043470364112,
12.));
#120658=CARTESIAN_POINT('Ctrl Pts',(63.8126631409376,-31.0193614892177,
12.));
#120659=CARTESIAN_POINT('Ctrl Pts',(63.8285464282857,-31.0344249459544,
12.));
#120660=CARTESIAN_POINT('Ctrl Pts',(63.8444487476615,-31.0495373571218,
12.));
#120661=CARTESIAN_POINT('Ctrl Pts',(63.8603699407922,-31.0646986733724,
12.));
#120662=CARTESIAN_POINT('Ctrl Pts',(63.8763098502235,-31.079908845504,12.));
#120663=CARTESIAN_POINT('Ctrl Pts',(63.8922683192962,-31.0951678244454,
12.));
#120664=CARTESIAN_POINT('Ctrl Pts',(63.9082451921447,-31.1104755612606,
12.));
#120665=CARTESIAN_POINT('Ctrl Pts',(63.9242403136954,-31.1258320071545,
12.));
#120666=CARTESIAN_POINT('Ctrl Pts',(63.940253529665,-31.1412371134727,12.));
#120667=CARTESIAN_POINT('Ctrl Pts',(63.9562846865566,-31.1566908316993,
12.));
#120668=CARTESIAN_POINT('Ctrl Pts',(63.972333631655,-31.1721931134488,12.));
#120669=CARTESIAN_POINT('Ctrl Pts',(63.9884002130209,-31.1877439104717,
12.));
#120670=CARTESIAN_POINT('Ctrl Pts',(64.004484279483,-31.2033431746559,12.));
#120671=CARTESIAN_POINT('Ctrl Pts',(64.0205856806298,-31.2189908580245,
12.));
#120672=CARTESIAN_POINT('Ctrl Pts',(64.036704266799,-31.23468691273,12.));
#120673=CARTESIAN_POINT('Ctrl Pts',(64.0528398890671,-31.2504312910457,
12.));
#120674=CARTESIAN_POINT('Ctrl Pts',(64.0689923992474,-31.2662239453734,
12.));
#120675=CARTESIAN_POINT('Ctrl Pts',(64.0851616498861,-31.2820648282451,
12.));
#120676=CARTESIAN_POINT('Ctrl Pts',(64.1013474942554,-31.2979538923214,
12.));
#120677=CARTESIAN_POINT('Ctrl Pts',(64.1175497863475,-31.3138910903852,
12.));
#120678=CARTESIAN_POINT('Ctrl Pts',(64.1337683808667,-31.3298763753366,
12.));
#120679=CARTESIAN_POINT('Ctrl Pts',(64.150003133226,-31.3459097001996,12.));
#120680=CARTESIAN_POINT('Ctrl Pts',(64.1662538995407,-31.3619910181223,
12.));
#120681=CARTESIAN_POINT('Ctrl Pts',(64.1825205366231,-31.3781202823758,
12.));
#120682=CARTESIAN_POINT('Ctrl Pts',(64.1988029019733,-31.3942974463458,
12.));
#120683=CARTESIAN_POINT('Ctrl Pts',(64.2151008537733,-31.4105224635298,
12.));
#120684=CARTESIAN_POINT('Ctrl Pts',(64.2314142508843,-31.426795287544,12.));
#120685=CARTESIAN_POINT('Ctrl Pts',(64.2477429528408,-31.443115872123,12.));
#120686=CARTESIAN_POINT('Ctrl Pts',(64.264086819846,-31.4594841711189,12.));
#120687=CARTESIAN_POINT('Ctrl Pts',(64.2804457127633,-31.4759001384923,
12.));
#120688=CARTESIAN_POINT('Ctrl Pts',(64.2968194931113,-31.4923637283109,
12.));
#120689=CARTESIAN_POINT('Ctrl Pts',(64.3132080230603,-31.5088748947565,
12.));
#120690=CARTESIAN_POINT('Ctrl Pts',(64.3296111654273,-31.525433592124,12.));
#120691=CARTESIAN_POINT('Ctrl Pts',(64.34602878367,-31.5420397748198,12.));
#120692=CARTESIAN_POINT('Ctrl Pts',(64.3624607418798,-31.5586933973532,
12.));
#120693=CARTESIAN_POINT('Ctrl Pts',(64.3789069047768,-31.5753944143355,
12.));
#120694=CARTESIAN_POINT('Ctrl Pts',(64.3953671377071,-31.5921427804879,
12.));
#120695=CARTESIAN_POINT('Ctrl Pts',(64.4118413066386,-31.6089384506399,
12.));
#120696=CARTESIAN_POINT('Ctrl Pts',(64.4283292781553,-31.6257813797282,
12.));
#120697=CARTESIAN_POINT('Ctrl Pts',(64.4448309194498,-31.6426715227865,
12.));
#120698=CARTESIAN_POINT('Ctrl Pts',(64.4613460983186,-31.6596088349468,
12.));
#120699=CARTESIAN_POINT('Ctrl Pts',(64.4778746831597,-31.6765932714456,
12.));
#120700=CARTESIAN_POINT('Ctrl Pts',(64.4944165429672,-31.6936247876228,
12.));
#120701=CARTESIAN_POINT('Ctrl Pts',(64.5109715473276,-31.7107033389204,
12.));
#120702=CARTESIAN_POINT('Ctrl Pts',(64.5275395664134,-31.7278288808736,
12.));
#120703=CARTESIAN_POINT('Ctrl Pts',(64.5441204709779,-31.7450013691117,
12.));
#120704=CARTESIAN_POINT('Ctrl Pts',(64.5607141323527,-31.7622207593637,
12.));
#120705=CARTESIAN_POINT('Ctrl Pts',(64.5773204224429,-31.7794870074584,
12.));
#120706=CARTESIAN_POINT('Ctrl Pts',(64.5939392137233,-31.7968000693218,
12.));
#120707=CARTESIAN_POINT('Ctrl Pts',(64.6105703792311,-31.8141599009685,
12.));
#120708=CARTESIAN_POINT('Ctrl Pts',(64.6272137925629,-31.8315664585027,
12.));
#120709=CARTESIAN_POINT('Ctrl Pts',(64.6438693278718,-31.849019698125,12.));
#120710=CARTESIAN_POINT('Ctrl Pts',(64.6605368598631,-31.8665195761312,
12.));
#120711=CARTESIAN_POINT('Ctrl Pts',(64.6772162637904,-31.8840660489106,
12.));
#120712=CARTESIAN_POINT('Ctrl Pts',(64.693907415449,-31.9016590729371,12.));
#120713=CARTESIAN_POINT('Ctrl Pts',(64.7106101911722,-31.9192986047702,
12.));
#120714=CARTESIAN_POINT('Ctrl Pts',(64.727324467829,-31.9369846010613,12.));
#120715=CARTESIAN_POINT('Ctrl Pts',(64.74405012282,-31.9547170185533,12.));
#120716=CARTESIAN_POINT('Ctrl Pts',(64.7607870340738,-31.9724958140791,
12.));
#120717=CARTESIAN_POINT('Ctrl Pts',(64.7775350800404,-31.9903209445522,
12.));
#120718=CARTESIAN_POINT('Ctrl Pts',(64.7942941396883,-32.0081923669678,
12.));
#120719=CARTESIAN_POINT('Ctrl Pts',(64.811064092502,-32.0261100384092,12.));
#120720=CARTESIAN_POINT('Ctrl Pts',(64.8278448184785,-32.0440739160477,
12.));
#120721=CARTESIAN_POINT('Ctrl Pts',(64.8446361981234,-32.0620839571409,
12.));
#120722=CARTESIAN_POINT('Ctrl Pts',(64.8614381124454,-32.0801401190244,
12.));
#120723=CARTESIAN_POINT('Ctrl Pts',(64.8782504429527,-32.0982423591113,
12.));
#120724=CARTESIAN_POINT('Ctrl Pts',(64.8950730716501,-32.1163906348984,
12.));
#120725=CARTESIAN_POINT('Ctrl Pts',(64.9119058810366,-32.1345849039674,
12.));
#120726=CARTESIAN_POINT('Ctrl Pts',(64.9287487541015,-32.1528251239831,
12.));
#120727=CARTESIAN_POINT('Ctrl Pts',(64.9456015743192,-32.1711112526855,
12.));
#120728=CARTESIAN_POINT('Ctrl Pts',(64.9624642256461,-32.1894432478881,
12.));
#120729=CARTESIAN_POINT('Ctrl Pts',(64.9793365925178,-32.207821067485,12.));
#120730=CARTESIAN_POINT('Ctrl Pts',(64.9962185598461,-32.2262446694513,
12.));
#120731=CARTESIAN_POINT('Ctrl Pts',(65.0131100130157,-32.2447140118422,
12.));
#120732=CARTESIAN_POINT('Ctrl Pts',(65.03001083788,-32.2632290527862,12.));
#120733=CARTESIAN_POINT('Ctrl Pts',(65.0469209207563,-32.2817897504807,
12.));
#120734=CARTESIAN_POINT('Ctrl Pts',(65.0638401484257,-32.3003960632007,
12.));
#120735=CARTESIAN_POINT('Ctrl Pts',(65.0807684081281,-32.3190479492987,
12.));
#120736=CARTESIAN_POINT('Ctrl Pts',(65.0977055875607,-32.3377453672051,
12.));
#120737=CARTESIAN_POINT('Ctrl Pts',(65.1146515748722,-32.3564882754212,
12.));
#120738=CARTESIAN_POINT('Ctrl Pts',(65.1316062586588,-32.3752766325136,
12.));
#120739=CARTESIAN_POINT('Ctrl Pts',(65.1485695279635,-32.3941103971221,
12.));
#120740=CARTESIAN_POINT('Ctrl Pts',(65.1655412722725,-32.4129895279615,
12.));
#120741=CARTESIAN_POINT('Ctrl Pts',(65.182521381514,-32.4319139838213,12.));
#120742=CARTESIAN_POINT('Ctrl Pts',(65.1995097460538,-32.450883723561,12.));
#120743=CARTESIAN_POINT('Ctrl Pts',(65.2165062566924,-32.4698987061032,
12.));
#120744=CARTESIAN_POINT('Ctrl Pts',(65.2335108046614,-32.4889588904392,
12.));
#120745=CARTESIAN_POINT('Ctrl Pts',(65.2505232816209,-32.5080642356328,
12.));
#120746=CARTESIAN_POINT('Ctrl Pts',(65.2675435796558,-32.5272147008191,
12.));
#120747=CARTESIAN_POINT('Ctrl Pts',(65.2845715912721,-32.5464102452015,
12.));
#120748=CARTESIAN_POINT('Ctrl Pts',(65.3016072093912,-32.5656508280422,
12.));
#120749=CARTESIAN_POINT('Ctrl Pts',(65.31865032735,-32.5849364086679,12.));
#120750=CARTESIAN_POINT('Ctrl Pts',(65.3357008389003,-32.6042669464751,
12.));
#120751=CARTESIAN_POINT('Ctrl Pts',(65.3527586382081,-32.6236424009301,
12.));
#120752=CARTESIAN_POINT('Ctrl Pts',(65.3698236198512,-32.6430627315674,
12.));
#120753=CARTESIAN_POINT('Ctrl Pts',(65.3868956788182,-32.6625278979811,
12.));
#120754=CARTESIAN_POINT('Ctrl Pts',(65.4039747105038,-32.6820378598267,
12.));
#120755=CARTESIAN_POINT('Ctrl Pts',(65.4210606107035,-32.7015925768265,
12.));
#120756=CARTESIAN_POINT('Ctrl Pts',(65.4381532756065,-32.7211920087684,
12.));
#120757=CARTESIAN_POINT('Ctrl Pts',(65.4552526017905,-32.7408361155037,
12.));
#120758=CARTESIAN_POINT('Ctrl Pts',(65.4723584862122,-32.7605248569378,
12.));
#120759=CARTESIAN_POINT('Ctrl Pts',(65.489470826206,-32.7802581930287,12.));
#120760=CARTESIAN_POINT('Ctrl Pts',(65.5065895194928,-32.8000360837975,
12.));
#120761=CARTESIAN_POINT('Ctrl Pts',(65.5237144641857,-32.8198584893316,
12.));
#120762=CARTESIAN_POINT('Ctrl Pts',(65.5408455587964,-32.8397253697866,
12.));
#120763=CARTESIAN_POINT('Ctrl Pts',(65.5579827022421,-32.8596366853832,
12.));
#120764=CARTESIAN_POINT('Ctrl Pts',(65.5751257938472,-32.879592396403,12.));
#120765=CARTESIAN_POINT('Ctrl Pts',(65.5922747333194,-32.8995924631898,
12.));
#120766=CARTESIAN_POINT('Ctrl Pts',(65.6094294207276,-32.9196368461463,
12.));
#120767=CARTESIAN_POINT('Ctrl Pts',(65.6265897564783,-32.9397255057274,
12.));
#120768=CARTESIAN_POINT('Ctrl Pts',(65.6437556412946,-32.9598584024313,
12.));
#120769=CARTESIAN_POINT('Ctrl Pts',(65.6609269761888,-32.980035496784,12.));
#120770=CARTESIAN_POINT('Ctrl Pts',(65.6781036625027,-33.0002567493574,
12.));
#120771=CARTESIAN_POINT('Ctrl Pts',(65.6952856019533,-33.0205221207873,
12.));
#120772=CARTESIAN_POINT('Ctrl Pts',(65.7124726966802,-33.0408315717873,
12.));
#120773=CARTESIAN_POINT('Ctrl Pts',(65.7296648492824,-33.0611850631582,
12.));
#120774=CARTESIAN_POINT('Ctrl Pts',(65.7468619628815,-33.081582555798,12.));
#120775=CARTESIAN_POINT('Ctrl Pts',(65.7640639410661,-33.1020240106885,
12.));
#120776=CARTESIAN_POINT('Ctrl Pts',(65.7812706877696,-33.1225093888672,
12.));
#120777=CARTESIAN_POINT('Ctrl Pts',(65.7984821071623,-33.1430386513976,
12.));
#120778=CARTESIAN_POINT('Ctrl Pts',(65.8156981035503,-33.16361175934,12.));
#120779=CARTESIAN_POINT('Ctrl Pts',(65.8329185812375,-33.1842286737051,
12.));
#120780=CARTESIAN_POINT('Ctrl Pts',(65.8501434445164,-33.2048893554491,
12.));
#120781=CARTESIAN_POINT('Ctrl Pts',(65.8673725979577,-33.2255937655649,
12.));
#120782=CARTESIAN_POINT('Ctrl Pts',(65.8846059466371,-33.2463418651493,
12.));
#120783=CARTESIAN_POINT('Ctrl Pts',(65.9018433963889,-33.2671336154754,
12.));
#120784=CARTESIAN_POINT('Ctrl Pts',(65.9190848540433,-33.2879689780573,
12.));
#120785=CARTESIAN_POINT('Ctrl Pts',(65.9363302276846,-33.3088479147164,
12.));
#120786=CARTESIAN_POINT('Ctrl Pts',(65.9535794260831,-33.3297703874266,
12.));
#120787=CARTESIAN_POINT('Ctrl Pts',(65.970832358141,-33.3507363581593,12.));
#120788=CARTESIAN_POINT('Ctrl Pts',(65.9880889322831,-33.37174578871,12.));
#120789=CARTESIAN_POINT('Ctrl Pts',(66.0053490559812,-33.3927986405605,
12.));
#120790=CARTESIAN_POINT('Ctrl Pts',(66.0226126349446,-33.4138948746388,
12.));
#120791=CARTESIAN_POINT('Ctrl Pts',(66.0398795737777,-33.4350344515101,
12.));
#120792=CARTESIAN_POINT('Ctrl Pts',(66.0571497774434,-33.4562173318025,
12.));
#120793=CARTESIAN_POINT('Ctrl Pts',(66.0744231525415,-33.4774434765746,
12.));
#120794=CARTESIAN_POINT('Ctrl Pts',(66.0916996085244,-33.4987128476622,
12.));
#120795=CARTESIAN_POINT('Ctrl Pts',(66.1089790592729,-33.5200254081243,
12.));
#120796=CARTESIAN_POINT('Ctrl Pts',(66.1262614234674,-33.5413811223451,
12.));
#120797=CARTESIAN_POINT('Ctrl Pts',(66.1410781873278,-33.5597240685846,
12.));
#120798=CARTESIAN_POINT('Ctrl Pts',(66.1524393974174,-33.5738105077875,
12.));
#120799=CARTESIAN_POINT('Ctrl Pts',(66.1603438177522,-33.5836213514189,
12.));
#120800=CARTESIAN_POINT('Ctrl Pts',(66.1647906582657,-33.5891439876494,
12.));
#120801=CARTESIAN_POINT('Ctrl Pts',(66.1657795405962,-33.590372266528,12.));
#120802=CARTESIAN_POINT('',(63.0759831361898,-30.3549065457811,0.));
#120803=CARTESIAN_POINT('',(63.0759831361898,-30.3549065457811,0.));
#120804=CARTESIAN_POINT('Ctrl Pts',(66.1657795405962,-33.590372266528,0.));
#120805=CARTESIAN_POINT('Ctrl Pts',(66.1647906582657,-33.5891439876494,
0.));
#120806=CARTESIAN_POINT('Ctrl Pts',(66.1603438177522,-33.5836213514189,
0.));
#120807=CARTESIAN_POINT('Ctrl Pts',(66.1524393974174,-33.5738105077875,
0.));
#120808=CARTESIAN_POINT('Ctrl Pts',(66.1410781873278,-33.5597240685846,
0.));
#120809=CARTESIAN_POINT('Ctrl Pts',(66.1262614234674,-33.5413811223451,
0.));
#120810=CARTESIAN_POINT('Ctrl Pts',(66.1089790592729,-33.5200254081243,
0.));
#120811=CARTESIAN_POINT('Ctrl Pts',(66.0916996085244,-33.4987128476622,
0.));
#120812=CARTESIAN_POINT('Ctrl Pts',(66.0744231525415,-33.4774434765746,
0.));
#120813=CARTESIAN_POINT('Ctrl Pts',(66.0571497774434,-33.4562173318025,
0.));
#120814=CARTESIAN_POINT('Ctrl Pts',(66.0398795737777,-33.4350344515101,
0.));
#120815=CARTESIAN_POINT('Ctrl Pts',(66.0226126349446,-33.4138948746388,
0.));
#120816=CARTESIAN_POINT('Ctrl Pts',(66.0053490559812,-33.3927986405605,
0.));
#120817=CARTESIAN_POINT('Ctrl Pts',(65.9880889322831,-33.37174578871,0.));
#120818=CARTESIAN_POINT('Ctrl Pts',(65.970832358141,-33.3507363581593,0.));
#120819=CARTESIAN_POINT('Ctrl Pts',(65.9535794260831,-33.3297703874266,
0.));
#120820=CARTESIAN_POINT('Ctrl Pts',(65.9363302276846,-33.3088479147164,
0.));
#120821=CARTESIAN_POINT('Ctrl Pts',(65.9190848540433,-33.2879689780573,
0.));
#120822=CARTESIAN_POINT('Ctrl Pts',(65.9018433963889,-33.2671336154754,
0.));
#120823=CARTESIAN_POINT('Ctrl Pts',(65.8846059466371,-33.2463418651493,
0.));
#120824=CARTESIAN_POINT('Ctrl Pts',(65.8673725979577,-33.2255937655649,
0.));
#120825=CARTESIAN_POINT('Ctrl Pts',(65.8501434445164,-33.2048893554491,
0.));
#120826=CARTESIAN_POINT('Ctrl Pts',(65.8329185812375,-33.1842286737051,
0.));
#120827=CARTESIAN_POINT('Ctrl Pts',(65.8156981035503,-33.16361175934,0.));
#120828=CARTESIAN_POINT('Ctrl Pts',(65.7984821071623,-33.1430386513976,
0.));
#120829=CARTESIAN_POINT('Ctrl Pts',(65.7812706877696,-33.1225093888672,
0.));
#120830=CARTESIAN_POINT('Ctrl Pts',(65.7640639410661,-33.1020240106885,
0.));
#120831=CARTESIAN_POINT('Ctrl Pts',(65.7468619628815,-33.081582555798,0.));
#120832=CARTESIAN_POINT('Ctrl Pts',(65.7296648492824,-33.0611850631582,
0.));
#120833=CARTESIAN_POINT('Ctrl Pts',(65.7124726966802,-33.0408315717873,
0.));
#120834=CARTESIAN_POINT('Ctrl Pts',(65.6952856019533,-33.0205221207873,
0.));
#120835=CARTESIAN_POINT('Ctrl Pts',(65.6781036625027,-33.0002567493574,
0.));
#120836=CARTESIAN_POINT('Ctrl Pts',(65.6609269761888,-32.980035496784,0.));
#120837=CARTESIAN_POINT('Ctrl Pts',(65.6437556412946,-32.9598584024313,
0.));
#120838=CARTESIAN_POINT('Ctrl Pts',(65.6265897564783,-32.9397255057274,
0.));
#120839=CARTESIAN_POINT('Ctrl Pts',(65.6094294207276,-32.9196368461463,
0.));
#120840=CARTESIAN_POINT('Ctrl Pts',(65.5922747333194,-32.8995924631898,
0.));
#120841=CARTESIAN_POINT('Ctrl Pts',(65.5751257938472,-32.879592396403,0.));
#120842=CARTESIAN_POINT('Ctrl Pts',(65.5579827022421,-32.8596366853832,
0.));
#120843=CARTESIAN_POINT('Ctrl Pts',(65.5408455587964,-32.8397253697866,
0.));
#120844=CARTESIAN_POINT('Ctrl Pts',(65.5237144641857,-32.8198584893316,
0.));
#120845=CARTESIAN_POINT('Ctrl Pts',(65.5065895194928,-32.8000360837975,
0.));
#120846=CARTESIAN_POINT('Ctrl Pts',(65.489470826206,-32.7802581930287,0.));
#120847=CARTESIAN_POINT('Ctrl Pts',(65.4723584862122,-32.7605248569378,
0.));
#120848=CARTESIAN_POINT('Ctrl Pts',(65.4552526017905,-32.7408361155037,
0.));
#120849=CARTESIAN_POINT('Ctrl Pts',(65.4381532756065,-32.7211920087684,
0.));
#120850=CARTESIAN_POINT('Ctrl Pts',(65.4210606107035,-32.7015925768265,
0.));
#120851=CARTESIAN_POINT('Ctrl Pts',(65.4039747105038,-32.6820378598267,
0.));
#120852=CARTESIAN_POINT('Ctrl Pts',(65.3868956788182,-32.6625278979811,
0.));
#120853=CARTESIAN_POINT('Ctrl Pts',(65.3698236198512,-32.6430627315674,
0.));
#120854=CARTESIAN_POINT('Ctrl Pts',(65.3527586382081,-32.6236424009301,
0.));
#120855=CARTESIAN_POINT('Ctrl Pts',(65.3357008389003,-32.6042669464751,
0.));
#120856=CARTESIAN_POINT('Ctrl Pts',(65.31865032735,-32.5849364086679,0.));
#120857=CARTESIAN_POINT('Ctrl Pts',(65.3016072093912,-32.5656508280422,
0.));
#120858=CARTESIAN_POINT('Ctrl Pts',(65.2845715912721,-32.5464102452015,
0.));
#120859=CARTESIAN_POINT('Ctrl Pts',(65.2675435796558,-32.5272147008191,
0.));
#120860=CARTESIAN_POINT('Ctrl Pts',(65.2505232816209,-32.5080642356328,
0.));
#120861=CARTESIAN_POINT('Ctrl Pts',(65.2335108046614,-32.4889588904392,
0.));
#120862=CARTESIAN_POINT('Ctrl Pts',(65.2165062566924,-32.4698987061032,
0.));
#120863=CARTESIAN_POINT('Ctrl Pts',(65.1995097460538,-32.450883723561,0.));
#120864=CARTESIAN_POINT('Ctrl Pts',(65.182521381514,-32.4319139838213,0.));
#120865=CARTESIAN_POINT('Ctrl Pts',(65.1655412722725,-32.4129895279615,
0.));
#120866=CARTESIAN_POINT('Ctrl Pts',(65.1485695279635,-32.3941103971221,
0.));
#120867=CARTESIAN_POINT('Ctrl Pts',(65.1316062586588,-32.3752766325136,
0.));
#120868=CARTESIAN_POINT('Ctrl Pts',(65.1146515748722,-32.3564882754212,
0.));
#120869=CARTESIAN_POINT('Ctrl Pts',(65.0977055875607,-32.3377453672051,
0.));
#120870=CARTESIAN_POINT('Ctrl Pts',(65.0807684081281,-32.3190479492987,
0.));
#120871=CARTESIAN_POINT('Ctrl Pts',(65.0638401484257,-32.3003960632007,
0.));
#120872=CARTESIAN_POINT('Ctrl Pts',(65.0469209207563,-32.2817897504807,
0.));
#120873=CARTESIAN_POINT('Ctrl Pts',(65.03001083788,-32.2632290527862,0.));
#120874=CARTESIAN_POINT('Ctrl Pts',(65.0131100130157,-32.2447140118422,
0.));
#120875=CARTESIAN_POINT('Ctrl Pts',(64.9962185598461,-32.2262446694513,
0.));
#120876=CARTESIAN_POINT('Ctrl Pts',(64.9793365925178,-32.207821067485,0.));
#120877=CARTESIAN_POINT('Ctrl Pts',(64.9624642256461,-32.1894432478881,
0.));
#120878=CARTESIAN_POINT('Ctrl Pts',(64.9456015743192,-32.1711112526855,
0.));
#120879=CARTESIAN_POINT('Ctrl Pts',(64.9287487541015,-32.1528251239831,
0.));
#120880=CARTESIAN_POINT('Ctrl Pts',(64.9119058810366,-32.1345849039674,
0.));
#120881=CARTESIAN_POINT('Ctrl Pts',(64.8950730716501,-32.1163906348984,
0.));
#120882=CARTESIAN_POINT('Ctrl Pts',(64.8782504429527,-32.0982423591113,
0.));
#120883=CARTESIAN_POINT('Ctrl Pts',(64.8614381124454,-32.0801401190244,
0.));
#120884=CARTESIAN_POINT('Ctrl Pts',(64.8446361981234,-32.0620839571409,
0.));
#120885=CARTESIAN_POINT('Ctrl Pts',(64.8278448184785,-32.0440739160477,
0.));
#120886=CARTESIAN_POINT('Ctrl Pts',(64.811064092502,-32.0261100384092,0.));
#120887=CARTESIAN_POINT('Ctrl Pts',(64.7942941396883,-32.0081923669678,
0.));
#120888=CARTESIAN_POINT('Ctrl Pts',(64.7775350800404,-31.9903209445522,
0.));
#120889=CARTESIAN_POINT('Ctrl Pts',(64.7607870340738,-31.9724958140791,
0.));
#120890=CARTESIAN_POINT('Ctrl Pts',(64.74405012282,-31.9547170185533,0.));
#120891=CARTESIAN_POINT('Ctrl Pts',(64.727324467829,-31.9369846010613,0.));
#120892=CARTESIAN_POINT('Ctrl Pts',(64.7106101911722,-31.9192986047702,
0.));
#120893=CARTESIAN_POINT('Ctrl Pts',(64.693907415449,-31.9016590729371,0.));
#120894=CARTESIAN_POINT('Ctrl Pts',(64.6772162637904,-31.8840660489106,
0.));
#120895=CARTESIAN_POINT('Ctrl Pts',(64.6605368598631,-31.8665195761312,
0.));
#120896=CARTESIAN_POINT('Ctrl Pts',(64.6438693278718,-31.849019698125,0.));
#120897=CARTESIAN_POINT('Ctrl Pts',(64.6272137925629,-31.8315664585027,
0.));
#120898=CARTESIAN_POINT('Ctrl Pts',(64.6105703792311,-31.8141599009685,
0.));
#120899=CARTESIAN_POINT('Ctrl Pts',(64.5939392137233,-31.7968000693218,
0.));
#120900=CARTESIAN_POINT('Ctrl Pts',(64.5773204224429,-31.7794870074584,
0.));
#120901=CARTESIAN_POINT('Ctrl Pts',(64.5607141323527,-31.7622207593637,
0.));
#120902=CARTESIAN_POINT('Ctrl Pts',(64.5441204709779,-31.7450013691117,
0.));
#120903=CARTESIAN_POINT('Ctrl Pts',(64.5275395664134,-31.7278288808736,
0.));
#120904=CARTESIAN_POINT('Ctrl Pts',(64.5109715473276,-31.7107033389204,
0.));
#120905=CARTESIAN_POINT('Ctrl Pts',(64.4944165429672,-31.6936247876228,
0.));
#120906=CARTESIAN_POINT('Ctrl Pts',(64.4778746831597,-31.6765932714456,
0.));
#120907=CARTESIAN_POINT('Ctrl Pts',(64.4613460983186,-31.6596088349468,
0.));
#120908=CARTESIAN_POINT('Ctrl Pts',(64.4448309194498,-31.6426715227865,
0.));
#120909=CARTESIAN_POINT('Ctrl Pts',(64.4283292781553,-31.6257813797282,
0.));
#120910=CARTESIAN_POINT('Ctrl Pts',(64.4118413066386,-31.6089384506399,
0.));
#120911=CARTESIAN_POINT('Ctrl Pts',(64.3953671377071,-31.5921427804879,
0.));
#120912=CARTESIAN_POINT('Ctrl Pts',(64.3789069047768,-31.5753944143355,
0.));
#120913=CARTESIAN_POINT('Ctrl Pts',(64.3624607418798,-31.5586933973532,
0.));
#120914=CARTESIAN_POINT('Ctrl Pts',(64.34602878367,-31.5420397748198,0.));
#120915=CARTESIAN_POINT('Ctrl Pts',(64.3296111654273,-31.525433592124,0.));
#120916=CARTESIAN_POINT('Ctrl Pts',(64.3132080230603,-31.5088748947565,
0.));
#120917=CARTESIAN_POINT('Ctrl Pts',(64.2968194931113,-31.4923637283109,
0.));
#120918=CARTESIAN_POINT('Ctrl Pts',(64.2804457127633,-31.4759001384923,
0.));
#120919=CARTESIAN_POINT('Ctrl Pts',(64.264086819846,-31.4594841711189,0.));
#120920=CARTESIAN_POINT('Ctrl Pts',(64.2477429528408,-31.443115872123,0.));
#120921=CARTESIAN_POINT('Ctrl Pts',(64.2314142508843,-31.426795287544,0.));
#120922=CARTESIAN_POINT('Ctrl Pts',(64.2151008537733,-31.4105224635298,
0.));
#120923=CARTESIAN_POINT('Ctrl Pts',(64.1988029019733,-31.3942974463458,
0.));
#120924=CARTESIAN_POINT('Ctrl Pts',(64.1825205366231,-31.3781202823758,
0.));
#120925=CARTESIAN_POINT('Ctrl Pts',(64.1662538995407,-31.3619910181223,
0.));
#120926=CARTESIAN_POINT('Ctrl Pts',(64.150003133226,-31.3459097001996,0.));
#120927=CARTESIAN_POINT('Ctrl Pts',(64.1337683808667,-31.3298763753366,
0.));
#120928=CARTESIAN_POINT('Ctrl Pts',(64.1175497863475,-31.3138910903852,
0.));
#120929=CARTESIAN_POINT('Ctrl Pts',(64.1013474942554,-31.2979538923214,
0.));
#120930=CARTESIAN_POINT('Ctrl Pts',(64.0851616498861,-31.2820648282451,
0.));
#120931=CARTESIAN_POINT('Ctrl Pts',(64.0689923992474,-31.2662239453734,
0.));
#120932=CARTESIAN_POINT('Ctrl Pts',(64.0528398890671,-31.2504312910457,
0.));
#120933=CARTESIAN_POINT('Ctrl Pts',(64.036704266799,-31.23468691273,0.));
#120934=CARTESIAN_POINT('Ctrl Pts',(64.0205856806298,-31.2189908580245,
0.));
#120935=CARTESIAN_POINT('Ctrl Pts',(64.004484279483,-31.2033431746559,0.));
#120936=CARTESIAN_POINT('Ctrl Pts',(63.9884002130209,-31.1877439104717,
0.));
#120937=CARTESIAN_POINT('Ctrl Pts',(63.972333631655,-31.1721931134488,0.));
#120938=CARTESIAN_POINT('Ctrl Pts',(63.9562846865566,-31.1566908316993,
0.));
#120939=CARTESIAN_POINT('Ctrl Pts',(63.940253529665,-31.1412371134727,0.));
#120940=CARTESIAN_POINT('Ctrl Pts',(63.9242403136954,-31.1258320071545,
0.));
#120941=CARTESIAN_POINT('Ctrl Pts',(63.9082451921447,-31.1104755612606,
0.));
#120942=CARTESIAN_POINT('Ctrl Pts',(63.8922683192962,-31.0951678244454,
0.));
#120943=CARTESIAN_POINT('Ctrl Pts',(63.8763098502235,-31.079908845504,0.));
#120944=CARTESIAN_POINT('Ctrl Pts',(63.8603699407922,-31.0646986733724,
0.));
#120945=CARTESIAN_POINT('Ctrl Pts',(63.8444487476615,-31.0495373571218,
0.));
#120946=CARTESIAN_POINT('Ctrl Pts',(63.8285464282857,-31.0344249459544,
0.));
#120947=CARTESIAN_POINT('Ctrl Pts',(63.8126631409376,-31.0193614892177,
0.));
#120948=CARTESIAN_POINT('Ctrl Pts',(63.7967990447287,-31.0043470364112,
0.));
#120949=CARTESIAN_POINT('Ctrl Pts',(63.7809542996258,-30.9893816371907,
0.));
#120950=CARTESIAN_POINT('Ctrl Pts',(63.7651290664713,-30.9744653413679,
0.));
#120951=CARTESIAN_POINT('Ctrl Pts',(63.7493235069844,-30.9595981989091,
0.));
#120952=CARTESIAN_POINT('Ctrl Pts',(63.733537783742,-30.9447802599345,0.));
#120953=CARTESIAN_POINT('Ctrl Pts',(63.7177720601604,-30.9300115747113,
0.));
#120954=CARTESIAN_POINT('Ctrl Pts',(63.7020265004805,-30.9152921936471,
0.));
#120955=CARTESIAN_POINT('Ctrl Pts',(63.6863012697353,-30.9006221672703,
0.));
#120956=CARTESIAN_POINT('Ctrl Pts',(63.6705965337996,-30.8860015462488,
0.));
#120957=CARTESIAN_POINT('Ctrl Pts',(63.6549124594681,-30.8714303814202,
0.));
#120958=CARTESIAN_POINT('Ctrl Pts',(63.6392492145233,-30.8569087238132,
0.));
#120959=CARTESIAN_POINT('Ctrl Pts',(63.6236069678041,-30.8424366246665,
0.));
#120960=CARTESIAN_POINT('Ctrl Pts',(63.6079858892746,-30.8280141354448,
0.));
#120961=CARTESIAN_POINT('Ctrl Pts',(63.5923861498963,-30.8136413077999,
0.));
#120962=CARTESIAN_POINT('Ctrl Pts',(63.5768079214868,-30.7993181935265,
0.));
#120963=CARTESIAN_POINT('Ctrl Pts',(63.5612513766005,-30.7850448445207,
0.));
#120964=CARTESIAN_POINT('Ctrl Pts',(63.5457166883558,-30.7708213127169,
0.));
#120965=CARTESIAN_POINT('Ctrl Pts',(63.5302040304173,-30.7566476500772,
0.));
#120966=CARTESIAN_POINT('Ctrl Pts',(63.514713577392,-30.7425239087294,0.));
#120967=CARTESIAN_POINT('Ctrl Pts',(63.4992455051805,-30.7284501410827,
0.));
#120968=CARTESIAN_POINT('Ctrl Pts',(63.4837999912758,-30.7144263999259,
0.));
#120969=CARTESIAN_POINT('Ctrl Pts',(63.4683772152497,-30.7004527385806,
0.));
#120970=CARTESIAN_POINT('Ctrl Pts',(63.452977358421,-30.6865292107911,0.));
#120971=CARTESIAN_POINT('Ctrl Pts',(63.4376006029575,-30.6726558704302,
0.));
#120972=CARTESIAN_POINT('Ctrl Pts',(63.4222471311236,-30.6588327712482,
0.));
#120973=CARTESIAN_POINT('Ctrl Pts',(63.4069171245093,-30.6450599666135,
0.));
#120974=CARTESIAN_POINT('Ctrl Pts',(63.3916107631421,-30.6313375092085,
0.));
#120975=CARTESIAN_POINT('Ctrl Pts',(63.3763282271838,-30.6176654515988,
0.));
#120976=CARTESIAN_POINT('Ctrl Pts',(63.3610696989599,-30.604043846909,0.));
#120977=CARTESIAN_POINT('Ctrl Pts',(63.3458353646144,-30.5904727493707,
0.));
#120978=CARTESIAN_POINT('Ctrl Pts',(63.330625416509,-30.5769522151147,0.));
#120979=CARTESIAN_POINT('Ctrl Pts',(63.315440053435,-30.5634823022358,0.));
#120980=CARTESIAN_POINT('Ctrl Pts',(63.3002794756049,-30.5500630691343,
0.));
#120981=CARTESIAN_POINT('Ctrl Pts',(63.2851438802462,-30.5366945730503,
0.));
#120982=CARTESIAN_POINT('Ctrl Pts',(63.2700334577661,-30.5233768687875,
0.));
#120983=CARTESIAN_POINT('Ctrl Pts',(63.2549483856268,-30.5101100066683,
0.));
#120984=CARTESIAN_POINT('Ctrl Pts',(63.2398888342612,-30.4968940345028,
0.));
#120985=CARTESIAN_POINT('Ctrl Pts',(63.2248549788272,-30.4837290015011,
0.));
#120986=CARTESIAN_POINT('Ctrl Pts',(63.2098470086636,-30.470614961416,0.));
#120987=CARTESIAN_POINT('Ctrl Pts',(63.1948651386868,-30.4575519763305,
0.));
#120988=CARTESIAN_POINT('Ctrl Pts',(63.1799096171757,-30.4445401192324,
0.));
#120989=CARTESIAN_POINT('Ctrl Pts',(63.1649807016766,-30.431579465967,0.));
#120990=CARTESIAN_POINT('Ctrl Pts',(63.1500786361382,-30.4186700875598,
0.));
#120991=CARTESIAN_POINT('Ctrl Pts',(63.1352036298512,-30.4058120432259,
0.));
#120992=CARTESIAN_POINT('Ctrl Pts',(63.1203558300911,-30.3930053710592,
0.));
#120993=CARTESIAN_POINT('Ctrl Pts',(63.1055353202641,-30.3802500880565,
0.));
#120994=CARTESIAN_POINT('Ctrl Pts',(63.0937007763826,-30.3700869762658,
0.));
#120995=CARTESIAN_POINT('Ctrl Pts',(63.0848371718274,-30.3624877680747,
0.));
#120996=CARTESIAN_POINT('Ctrl Pts',(63.0789335700774,-30.3574319069366,
0.));
#120997=CARTESIAN_POINT('Ctrl Pts',(63.0759831361898,-30.3549065457811,
0.));
#120998=CARTESIAN_POINT('Ctrl Pts',(63.1661434108059,-39.5004851439258,
0.));
#120999=CARTESIAN_POINT('Ctrl Pts',(63.1661434108059,-39.5004851439258,
12.));
#121000=CARTESIAN_POINT('Ctrl Pts',(63.1630766582787,-39.4958045828135,
0.));
#121001=CARTESIAN_POINT('Ctrl Pts',(63.1630766582787,-39.4958045828135,
12.));
#121002=CARTESIAN_POINT('Ctrl Pts',(63.1569429707875,-39.4864477303823,
0.));
#121003=CARTESIAN_POINT('Ctrl Pts',(63.1569429707875,-39.4864477303823,
12.));
#121004=CARTESIAN_POINT('Ctrl Pts',(63.1477418922405,-39.4724252611155,
0.));
#121005=CARTESIAN_POINT('Ctrl Pts',(63.1477418922405,-39.4724252611155,
12.));
#121006=CARTESIAN_POINT('Ctrl Pts',(63.1354726928398,-39.4537542552269,
0.));
#121007=CARTESIAN_POINT('Ctrl Pts',(63.1354726928398,-39.4537542552269,
12.));
#121008=CARTESIAN_POINT('Ctrl Pts',(63.1201343731172,-39.4304582059864,
0.));
#121009=CARTESIAN_POINT('Ctrl Pts',(63.1201343731172,-39.4304582059864,
12.));
#121010=CARTESIAN_POINT('Ctrl Pts',(63.10479424519,-39.4072048797616,0.));
#121011=CARTESIAN_POINT('Ctrl Pts',(63.10479424519,-39.4072048797616,12.));
#121012=CARTESIAN_POINT('Ctrl Pts',(63.0894523341314,-39.383994298574,0.));
#121013=CARTESIAN_POINT('Ctrl Pts',(63.0894523341314,-39.383994298574,12.));
#121014=CARTESIAN_POINT('Ctrl Pts',(63.0741086815841,-39.3608264920409,
0.));
#121015=CARTESIAN_POINT('Ctrl Pts',(63.0741086815841,-39.3608264920409,
12.));
#121016=CARTESIAN_POINT('Ctrl Pts',(63.0587633513774,-39.3377014983609,
0.));
#121017=CARTESIAN_POINT('Ctrl Pts',(63.0587633513774,-39.3377014983609,
12.));
#121018=CARTESIAN_POINT('Ctrl Pts',(63.0434164277992,-39.3146193632392,
0.));
#121019=CARTESIAN_POINT('Ctrl Pts',(63.0434164277992,-39.3146193632392,
12.));
#121020=CARTESIAN_POINT('Ctrl Pts',(63.0280680082352,-39.2915801372354,
0.));
#121021=CARTESIAN_POINT('Ctrl Pts',(63.0280680082352,-39.2915801372354,
12.));
#121022=CARTESIAN_POINT('Ctrl Pts',(63.0127181973628,-39.2685838735361,
0.));
#121023=CARTESIAN_POINT('Ctrl Pts',(63.0127181973628,-39.2685838735361,
12.));
#121024=CARTESIAN_POINT('Ctrl Pts',(62.9973671008703,-39.2456306256104,
0.));
#121025=CARTESIAN_POINT('Ctrl Pts',(62.9973671008703,-39.2456306256104,
12.));
#121026=CARTESIAN_POINT('Ctrl Pts',(62.9820148189929,-39.2227204447638,
0.));
#121027=CARTESIAN_POINT('Ctrl Pts',(62.9820148189929,-39.2227204447638,
12.));
#121028=CARTESIAN_POINT('Ctrl Pts',(62.9666614412731,-39.1998533781661,
0.));
#121029=CARTESIAN_POINT('Ctrl Pts',(62.9666614412731,-39.1998533781661,
12.));
#121030=CARTESIAN_POINT('Ctrl Pts',(62.9513070501867,-39.1770294702428,
0.));
#121031=CARTESIAN_POINT('Ctrl Pts',(62.9513070501867,-39.1770294702428,
12.));
#121032=CARTESIAN_POINT('Ctrl Pts',(62.9359517237404,-39.1542487636744,
0.));
#121033=CARTESIAN_POINT('Ctrl Pts',(62.9359517237404,-39.1542487636744,
12.));
#121034=CARTESIAN_POINT('Ctrl Pts',(62.9205955385558,-39.131511300575,0.));
#121035=CARTESIAN_POINT('Ctrl Pts',(62.9205955385558,-39.131511300575,12.));
#121036=CARTESIAN_POINT('Ctrl Pts',(62.9052385725387,-39.1088171235125,
0.));
#121037=CARTESIAN_POINT('Ctrl Pts',(62.9052385725387,-39.1088171235125,
12.));
#121038=CARTESIAN_POINT('Ctrl Pts',(62.8898809082611,-39.0861662767932,
0.));
#121039=CARTESIAN_POINT('Ctrl Pts',(62.8898809082611,-39.0861662767932,
12.));
#121040=CARTESIAN_POINT('Ctrl Pts',(62.8745226325998,-39.0635588063277,
0.));
#121041=CARTESIAN_POINT('Ctrl Pts',(62.8745226325998,-39.0635588063277,
12.));
#121042=CARTESIAN_POINT('Ctrl Pts',(62.8591638352055,-39.0409947590497,
0.));
#121043=CARTESIAN_POINT('Ctrl Pts',(62.8591638352055,-39.0409947590497,
12.));
#121044=CARTESIAN_POINT('Ctrl Pts',(62.8438046073224,-39.0184741824641,
0.));
#121045=CARTESIAN_POINT('Ctrl Pts',(62.8438046073224,-39.0184741824641,
12.));
#121046=CARTESIAN_POINT('Ctrl Pts',(62.8284450405459,-38.9959971241701,
0.));
#121047=CARTESIAN_POINT('Ctrl Pts',(62.8284450405459,-38.9959971241701,
12.));
#121048=CARTESIAN_POINT('Ctrl Pts',(62.8130852254027,-38.9735636313089,
0.));
#121049=CARTESIAN_POINT('Ctrl Pts',(62.8130852254027,-38.9735636313089,
12.));
#121050=CARTESIAN_POINT('Ctrl Pts',(62.7977252507117,-38.9511737503165,
0.));
#121051=CARTESIAN_POINT('Ctrl Pts',(62.7977252507117,-38.9511737503165,
12.));
#121052=CARTESIAN_POINT('Ctrl Pts',(62.78236520437,-38.9288275272335,0.));
#121053=CARTESIAN_POINT('Ctrl Pts',(62.78236520437,-38.9288275272335,12.));
#121054=CARTESIAN_POINT('Ctrl Pts',(62.7670051738143,-38.9065250078832,
0.));
#121055=CARTESIAN_POINT('Ctrl Pts',(62.7670051738143,-38.9065250078832,
12.));
#121056=CARTESIAN_POINT('Ctrl Pts',(62.7516452466128,-38.8842662380984,
0.));
#121057=CARTESIAN_POINT('Ctrl Pts',(62.7516452466128,-38.8842662380984,
12.));
#121058=CARTESIAN_POINT('Ctrl Pts',(62.7362855110042,-38.8620512639233,
0.));
#121059=CARTESIAN_POINT('Ctrl Pts',(62.7362855110042,-38.8620512639233,
12.));
#121060=CARTESIAN_POINT('Ctrl Pts',(62.7209260564493,-38.8398801318177,
0.));
#121061=CARTESIAN_POINT('Ctrl Pts',(62.7209260564493,-38.8398801318177,
12.));
#121062=CARTESIAN_POINT('Ctrl Pts',(62.7055669733802,-38.8177528885681,
0.));
#121063=CARTESIAN_POINT('Ctrl Pts',(62.7055669733802,-38.8177528885681,
12.));
#121064=CARTESIAN_POINT('Ctrl Pts',(62.6902083529694,-38.795669581203,0.));
#121065=CARTESIAN_POINT('Ctrl Pts',(62.6902083529694,-38.795669581203,12.));
#121066=CARTESIAN_POINT('Ctrl Pts',(62.6748502868835,-38.7736302568982,
0.));
#121067=CARTESIAN_POINT('Ctrl Pts',(62.6748502868835,-38.7736302568982,
12.));
#121068=CARTESIAN_POINT('Ctrl Pts',(62.6594928670628,-38.7516349628904,
0.));
#121069=CARTESIAN_POINT('Ctrl Pts',(62.6594928670628,-38.7516349628904,
12.));
#121070=CARTESIAN_POINT('Ctrl Pts',(62.6441361854411,-38.7296837463609,
0.));
#121071=CARTESIAN_POINT('Ctrl Pts',(62.6441361854411,-38.7296837463609,
12.));
#121072=CARTESIAN_POINT('Ctrl Pts',(62.6287803339542,-38.7077766544416,
0.));
#121073=CARTESIAN_POINT('Ctrl Pts',(62.6287803339542,-38.7077766544416,
12.));
#121074=CARTESIAN_POINT('Ctrl Pts',(62.6134254046739,-38.6859137342731,
0.));
#121075=CARTESIAN_POINT('Ctrl Pts',(62.6134254046739,-38.6859137342731,
12.));
#121076=CARTESIAN_POINT('Ctrl Pts',(62.5980714899052,-38.6640950330421,
0.));
#121077=CARTESIAN_POINT('Ctrl Pts',(62.5980714899052,-38.6640950330421,
12.));
#121078=CARTESIAN_POINT('Ctrl Pts',(62.582718682292,-38.6423205980213,0.));
#121079=CARTESIAN_POINT('Ctrl Pts',(62.582718682292,-38.6423205980213,12.));
#121080=CARTESIAN_POINT('Ctrl Pts',(62.5673670749361,-38.6205904766073,
0.));
#121081=CARTESIAN_POINT('Ctrl Pts',(62.5673670749361,-38.6205904766073,
12.));
#121082=CARTESIAN_POINT('Ctrl Pts',(62.5520167614516,-38.5989047163393,
0.));
#121083=CARTESIAN_POINT('Ctrl Pts',(62.5520167614516,-38.5989047163393,
12.));
#121084=CARTESIAN_POINT('Ctrl Pts',(62.5366678359023,-38.5772633648833,
0.));
#121085=CARTESIAN_POINT('Ctrl Pts',(62.5366678359023,-38.5772633648833,
12.));
#121086=CARTESIAN_POINT('Ctrl Pts',(62.5213203927663,-38.5556664700195,
0.));
#121087=CARTESIAN_POINT('Ctrl Pts',(62.5213203927663,-38.5556664700195,
12.));
#121088=CARTESIAN_POINT('Ctrl Pts',(62.5059745268901,-38.5341140796248,
0.));
#121089=CARTESIAN_POINT('Ctrl Pts',(62.5059745268901,-38.5341140796248,
12.));
#121090=CARTESIAN_POINT('Ctrl Pts',(62.4906303334443,-38.5126062416502,
0.));
#121091=CARTESIAN_POINT('Ctrl Pts',(62.4906303334443,-38.5126062416502,
12.));
#121092=CARTESIAN_POINT('Ctrl Pts',(62.4752879078854,-38.4911430040997,
0.));
#121093=CARTESIAN_POINT('Ctrl Pts',(62.4752879078854,-38.4911430040997,
12.));
#121094=CARTESIAN_POINT('Ctrl Pts',(62.4599473459811,-38.4697244150482,
0.));
#121095=CARTESIAN_POINT('Ctrl Pts',(62.4599473459811,-38.4697244150482,
12.));
#121096=CARTESIAN_POINT('Ctrl Pts',(62.4446087438312,-38.4483505226518,
0.));
#121097=CARTESIAN_POINT('Ctrl Pts',(62.4446087438312,-38.4483505226518,
12.));
#121098=CARTESIAN_POINT('Ctrl Pts',(62.4292721978901,-38.4270213751568,
0.));
#121099=CARTESIAN_POINT('Ctrl Pts',(62.4292721978901,-38.4270213751568,
12.));
#121100=CARTESIAN_POINT('Ctrl Pts',(62.4139378049885,-38.405737020905,0.));
#121101=CARTESIAN_POINT('Ctrl Pts',(62.4139378049885,-38.405737020905,12.));
#121102=CARTESIAN_POINT('Ctrl Pts',(62.3986056623577,-38.3844975083344,
0.));
#121103=CARTESIAN_POINT('Ctrl Pts',(62.3986056623577,-38.3844975083344,
12.));
#121104=CARTESIAN_POINT('Ctrl Pts',(62.3832758676271,-38.3633028859828,
0.));
#121105=CARTESIAN_POINT('Ctrl Pts',(62.3832758676271,-38.3633028859828,
12.));
#121106=CARTESIAN_POINT('Ctrl Pts',(62.3679485188171,-38.342153202491,0.));
#121107=CARTESIAN_POINT('Ctrl Pts',(62.3679485188171,-38.342153202491,12.));
#121108=CARTESIAN_POINT('Ctrl Pts',(62.3526237143336,-38.3210485066001,
0.));
#121109=CARTESIAN_POINT('Ctrl Pts',(62.3526237143336,-38.3210485066001,
12.));
#121110=CARTESIAN_POINT('Ctrl Pts',(62.3373015529613,-38.2999888471476,
0.));
#121111=CARTESIAN_POINT('Ctrl Pts',(62.3373015529613,-38.2999888471476,
12.));
#121112=CARTESIAN_POINT('Ctrl Pts',(62.3219821338569,-38.2789742730564,
0.));
#121113=CARTESIAN_POINT('Ctrl Pts',(62.3219821338569,-38.2789742730564,
12.));
#121114=CARTESIAN_POINT('Ctrl Pts',(62.3066655565503,-38.2580048333361,
0.));
#121115=CARTESIAN_POINT('Ctrl Pts',(62.3066655565503,-38.2580048333361,
12.));
#121116=CARTESIAN_POINT('Ctrl Pts',(62.2913519209521,-38.2370805770935,
0.));
#121117=CARTESIAN_POINT('Ctrl Pts',(62.2913519209521,-38.2370805770935,
12.));
#121118=CARTESIAN_POINT('Ctrl Pts',(62.2760413273602,-38.2162015535353,
0.));
#121119=CARTESIAN_POINT('Ctrl Pts',(62.2760413273602,-38.2162015535353,
12.));
#121120=CARTESIAN_POINT('Ctrl Pts',(62.2607338764654,-38.1953678119691,
0.));
#121121=CARTESIAN_POINT('Ctrl Pts',(62.2607338764654,-38.1953678119691,
12.));
#121122=CARTESIAN_POINT('Ctrl Pts',(62.245429669358,-38.1745794017996,0.));
#121123=CARTESIAN_POINT('Ctrl Pts',(62.245429669358,-38.1745794017996,12.));
#121124=CARTESIAN_POINT('Ctrl Pts',(62.2301288075321,-38.1538363725264,
0.));
#121125=CARTESIAN_POINT('Ctrl Pts',(62.2301288075321,-38.1538363725264,
12.));
#121126=CARTESIAN_POINT('Ctrl Pts',(62.2148313928863,-38.133138773753,0.));
#121127=CARTESIAN_POINT('Ctrl Pts',(62.2148313928863,-38.133138773753,12.));
#121128=CARTESIAN_POINT('Ctrl Pts',(62.1995375277257,-38.1124866551886,
0.));
#121129=CARTESIAN_POINT('Ctrl Pts',(62.1995375277257,-38.1124866551886,
12.));
#121130=CARTESIAN_POINT('Ctrl Pts',(62.1842473147626,-38.0918800666479,
0.));
#121131=CARTESIAN_POINT('Ctrl Pts',(62.1842473147626,-38.0918800666479,
12.));
#121132=CARTESIAN_POINT('Ctrl Pts',(62.1689608571176,-38.0713190580463,
0.));
#121133=CARTESIAN_POINT('Ctrl Pts',(62.1689608571176,-38.0713190580463,
12.));
#121134=CARTESIAN_POINT('Ctrl Pts',(62.1536782583199,-38.0508036793939,
0.));
#121135=CARTESIAN_POINT('Ctrl Pts',(62.1536782583199,-38.0508036793939,
12.));
#121136=CARTESIAN_POINT('Ctrl Pts',(62.1383996223124,-38.0303339808053,
0.));
#121137=CARTESIAN_POINT('Ctrl Pts',(62.1383996223124,-38.0303339808053,
12.));
#121138=CARTESIAN_POINT('Ctrl Pts',(62.123125053455,-38.0099100125037,0.));
#121139=CARTESIAN_POINT('Ctrl Pts',(62.123125053455,-38.0099100125037,12.));
#121140=CARTESIAN_POINT('Ctrl Pts',(62.107854656528,-37.9895318248212,0.));
#121141=CARTESIAN_POINT('Ctrl Pts',(62.107854656528,-37.9895318248212,12.));
#121142=CARTESIAN_POINT('Ctrl Pts',(62.0925885367352,-37.9691994681966,
0.));
#121143=CARTESIAN_POINT('Ctrl Pts',(62.0925885367352,-37.9691994681966,
12.));
#121144=CARTESIAN_POINT('Ctrl Pts',(62.0773267997078,-37.9489129931689,
0.));
#121145=CARTESIAN_POINT('Ctrl Pts',(62.0773267997078,-37.9489129931689,
12.));
#121146=CARTESIAN_POINT('Ctrl Pts',(62.0620695515074,-37.9286724503851,
0.));
#121147=CARTESIAN_POINT('Ctrl Pts',(62.0620695515074,-37.9286724503851,
12.));
#121148=CARTESIAN_POINT('Ctrl Pts',(62.0468168986288,-37.9084778906053,
0.));
#121149=CARTESIAN_POINT('Ctrl Pts',(62.0468168986288,-37.9084778906053,
12.));
#121150=CARTESIAN_POINT('Ctrl Pts',(62.031568948002,-37.8883293647029,0.));
#121151=CARTESIAN_POINT('Ctrl Pts',(62.031568948002,-37.8883293647029,12.));
#121152=CARTESIAN_POINT('Ctrl Pts',(62.0163258069957,-37.868226923663,0.));
#121153=CARTESIAN_POINT('Ctrl Pts',(62.0163258069957,-37.868226923663,12.));
#121154=CARTESIAN_POINT('Ctrl Pts',(62.0010875834187,-37.8481706185749,
0.));
#121155=CARTESIAN_POINT('Ctrl Pts',(62.0010875834187,-37.8481706185749,
12.));
#121156=CARTESIAN_POINT('Ctrl Pts',(61.9858543855236,-37.8281605006381,
0.));
#121157=CARTESIAN_POINT('Ctrl Pts',(61.9858543855236,-37.8281605006381,
12.));
#121158=CARTESIAN_POINT('Ctrl Pts',(61.9706263220114,-37.8081966211689,
0.));
#121159=CARTESIAN_POINT('Ctrl Pts',(61.9706263220114,-37.8081966211689,
12.));
#121160=CARTESIAN_POINT('Ctrl Pts',(61.9554035020338,-37.7882790316014,
0.));
#121161=CARTESIAN_POINT('Ctrl Pts',(61.9554035020338,-37.7882790316014,
12.));
#121162=CARTESIAN_POINT('Ctrl Pts',(61.9401860351972,-37.7684077834873,
0.));
#121163=CARTESIAN_POINT('Ctrl Pts',(61.9401860351972,-37.7684077834873,
12.));
#121164=CARTESIAN_POINT('Ctrl Pts',(61.9249740315649,-37.7485829284872,
0.));
#121165=CARTESIAN_POINT('Ctrl Pts',(61.9249740315649,-37.7485829284872,
12.));
#121166=CARTESIAN_POINT('Ctrl Pts',(61.9097676016601,-37.7288045183756,
0.));
#121167=CARTESIAN_POINT('Ctrl Pts',(61.9097676016601,-37.7288045183756,
12.));
#121168=CARTESIAN_POINT('Ctrl Pts',(61.8945668564704,-37.7090726050482,
0.));
#121169=CARTESIAN_POINT('Ctrl Pts',(61.8945668564704,-37.7090726050482,
12.));
#121170=CARTESIAN_POINT('Ctrl Pts',(61.8793719074507,-37.6893872405228,
0.));
#121171=CARTESIAN_POINT('Ctrl Pts',(61.8793719074507,-37.6893872405228,
12.));
#121172=CARTESIAN_POINT('Ctrl Pts',(61.8641828665261,-37.6697484769392,
0.));
#121173=CARTESIAN_POINT('Ctrl Pts',(61.8641828665261,-37.6697484769392,
12.));
#121174=CARTESIAN_POINT('Ctrl Pts',(61.8489998460957,-37.6501563665524,
0.));
#121175=CARTESIAN_POINT('Ctrl Pts',(61.8489998460957,-37.6501563665524,
12.));
#121176=CARTESIAN_POINT('Ctrl Pts',(61.8338229590352,-37.6306109617347,
0.));
#121177=CARTESIAN_POINT('Ctrl Pts',(61.8338229590352,-37.6306109617347,
12.));
#121178=CARTESIAN_POINT('Ctrl Pts',(61.8186523187015,-37.6111123149839,
0.));
#121179=CARTESIAN_POINT('Ctrl Pts',(61.8186523187015,-37.6111123149839,
12.));
#121180=CARTESIAN_POINT('Ctrl Pts',(61.8034880389362,-37.5916604789253,
0.));
#121181=CARTESIAN_POINT('Ctrl Pts',(61.8034880389362,-37.5916604789253,
12.));
#121182=CARTESIAN_POINT('Ctrl Pts',(61.7883302340687,-37.5722555063111,
0.));
#121183=CARTESIAN_POINT('Ctrl Pts',(61.7883302340687,-37.5722555063111,
12.));
#121184=CARTESIAN_POINT('Ctrl Pts',(61.773179018919,-37.5528974500142,0.));
#121185=CARTESIAN_POINT('Ctrl Pts',(61.773179018919,-37.5528974500142,12.));
#121186=CARTESIAN_POINT('Ctrl Pts',(61.7580345088016,-37.5335863630287,
0.));
#121187=CARTESIAN_POINT('Ctrl Pts',(61.7580345088016,-37.5335863630287,
12.));
#121188=CARTESIAN_POINT('Ctrl Pts',(61.7428968195299,-37.5143222984796,
0.));
#121189=CARTESIAN_POINT('Ctrl Pts',(61.7428968195299,-37.5143222984796,
12.));
#121190=CARTESIAN_POINT('Ctrl Pts',(61.7277660674205,-37.4951053096237,
0.));
#121191=CARTESIAN_POINT('Ctrl Pts',(61.7277660674205,-37.4951053096237,
12.));
#121192=CARTESIAN_POINT('Ctrl Pts',(61.7126423692963,-37.4759354498509,
0.));
#121193=CARTESIAN_POINT('Ctrl Pts',(61.7126423692963,-37.4759354498509,
12.));
#121194=CARTESIAN_POINT('Ctrl Pts',(61.6975258424894,-37.4568127726773,
0.));
#121195=CARTESIAN_POINT('Ctrl Pts',(61.6975258424894,-37.4568127726773,
12.));
#121196=CARTESIAN_POINT('Ctrl Pts',(61.6824166048444,-37.4377373317451,
0.));
#121197=CARTESIAN_POINT('Ctrl Pts',(61.6824166048444,-37.4377373317451,
12.));
#121198=CARTESIAN_POINT('Ctrl Pts',(61.6673147747242,-37.4187091808321,
0.));
#121199=CARTESIAN_POINT('Ctrl Pts',(61.6673147747242,-37.4187091808321,
12.));
#121200=CARTESIAN_POINT('Ctrl Pts',(61.6522204710131,-37.3997283738533,
0.));
#121201=CARTESIAN_POINT('Ctrl Pts',(61.6522204710131,-37.3997283738533,
12.));
#121202=CARTESIAN_POINT('Ctrl Pts',(61.637133813121,-37.3807949648624,0.));
#121203=CARTESIAN_POINT('Ctrl Pts',(61.637133813121,-37.3807949648624,12.));
#121204=CARTESIAN_POINT('Ctrl Pts',(61.6220549209866,-37.361909008045,0.));
#121205=CARTESIAN_POINT('Ctrl Pts',(61.6220549209866,-37.361909008045,12.));
#121206=CARTESIAN_POINT('Ctrl Pts',(61.6069839150807,-37.343070557718,0.));
#121207=CARTESIAN_POINT('Ctrl Pts',(61.6069839150807,-37.343070557718,12.));
#121208=CARTESIAN_POINT('Ctrl Pts',(61.591920916412,-37.3242796683395,0.));
#121209=CARTESIAN_POINT('Ctrl Pts',(61.591920916412,-37.3242796683395,12.));
#121210=CARTESIAN_POINT('Ctrl Pts',(61.5768660465311,-37.3055363945108,
0.));
#121211=CARTESIAN_POINT('Ctrl Pts',(61.5768660465311,-37.3055363945108,
12.));
#121212=CARTESIAN_POINT('Ctrl Pts',(61.5618194275348,-37.2868407909771,
0.));
#121213=CARTESIAN_POINT('Ctrl Pts',(61.5618194275348,-37.2868407909771,
12.));
#121214=CARTESIAN_POINT('Ctrl Pts',(61.5467811820691,-37.2681929126221,
0.));
#121215=CARTESIAN_POINT('Ctrl Pts',(61.5467811820691,-37.2681929126221,
12.));
#121216=CARTESIAN_POINT('Ctrl Pts',(61.5317514333328,-37.2495928144667,
0.));
#121217=CARTESIAN_POINT('Ctrl Pts',(61.5317514333328,-37.2495928144667,
12.));
#121218=CARTESIAN_POINT('Ctrl Pts',(61.5167303050832,-37.2310405516781,
0.));
#121219=CARTESIAN_POINT('Ctrl Pts',(61.5167303050832,-37.2310405516781,
12.));
#121220=CARTESIAN_POINT('Ctrl Pts',(61.501717921641,-37.2125361795731,0.));
#121221=CARTESIAN_POINT('Ctrl Pts',(61.501717921641,-37.2125361795731,12.));
#121222=CARTESIAN_POINT('Ctrl Pts',(61.4867144078936,-37.1940797536181,
0.));
#121223=CARTESIAN_POINT('Ctrl Pts',(61.4867144078936,-37.1940797536181,
12.));
#121224=CARTESIAN_POINT('Ctrl Pts',(61.4717198892994,-37.175671329424,0.));
#121225=CARTESIAN_POINT('Ctrl Pts',(61.4717198892994,-37.175671329424,12.));
#121226=CARTESIAN_POINT('Ctrl Pts',(61.4567344918919,-37.1573109627454,
0.));
#121227=CARTESIAN_POINT('Ctrl Pts',(61.4567344918919,-37.1573109627454,
12.));
#121228=CARTESIAN_POINT('Ctrl Pts',(61.4417583422863,-37.1389987094905,
0.));
#121229=CARTESIAN_POINT('Ctrl Pts',(61.4417583422863,-37.1389987094905,
12.));
#121230=CARTESIAN_POINT('Ctrl Pts',(61.4267915676822,-37.1207346257222,
0.));
#121231=CARTESIAN_POINT('Ctrl Pts',(61.4267915676822,-37.1207346257222,
12.));
#121232=CARTESIAN_POINT('Ctrl Pts',(61.4118342958697,-37.1025187676602,
0.));
#121233=CARTESIAN_POINT('Ctrl Pts',(61.4118342958697,-37.1025187676602,
12.));
#121234=CARTESIAN_POINT('Ctrl Pts',(61.3968866552317,-37.0843511916745,
0.));
#121235=CARTESIAN_POINT('Ctrl Pts',(61.3968866552317,-37.0843511916745,
12.));
#121236=CARTESIAN_POINT('Ctrl Pts',(61.381948774749,-37.0662319542849,0.));
#121237=CARTESIAN_POINT('Ctrl Pts',(61.381948774749,-37.0662319542849,12.));
#121238=CARTESIAN_POINT('Ctrl Pts',(61.3670207840068,-37.0481611121717,
0.));
#121239=CARTESIAN_POINT('Ctrl Pts',(61.3670207840068,-37.0481611121717,
12.));
#121240=CARTESIAN_POINT('Ctrl Pts',(61.3521028132003,-37.0301387221774,
0.));
#121241=CARTESIAN_POINT('Ctrl Pts',(61.3521028132003,-37.0301387221774,
12.));
#121242=CARTESIAN_POINT('Ctrl Pts',(61.3371949931387,-37.0121648413082,
0.));
#121243=CARTESIAN_POINT('Ctrl Pts',(61.3371949931387,-37.0121648413082,
12.));
#121244=CARTESIAN_POINT('Ctrl Pts',(61.3222974552486,-36.994239526727,0.));
#121245=CARTESIAN_POINT('Ctrl Pts',(61.3222974552486,-36.994239526727,12.));
#121246=CARTESIAN_POINT('Ctrl Pts',(61.3074103315791,-36.9763628357544,
0.));
#121247=CARTESIAN_POINT('Ctrl Pts',(61.3074103315791,-36.9763628357544,
12.));
#121248=CARTESIAN_POINT('Ctrl Pts',(61.2925337548077,-36.9585348258776,
0.));
#121249=CARTESIAN_POINT('Ctrl Pts',(61.2925337548077,-36.9585348258776,
12.));
#121250=CARTESIAN_POINT('Ctrl Pts',(61.2776678582461,-36.9407555547535,
0.));
#121251=CARTESIAN_POINT('Ctrl Pts',(61.2776678582461,-36.9407555547535,
12.));
#121252=CARTESIAN_POINT('Ctrl Pts',(61.2628127758457,-36.9230250802088,
0.));
#121253=CARTESIAN_POINT('Ctrl Pts',(61.2628127758457,-36.9230250802088,
12.));
#121254=CARTESIAN_POINT('Ctrl Pts',(61.247968642201,-36.9053434602343,0.));
#121255=CARTESIAN_POINT('Ctrl Pts',(61.247968642201,-36.9053434602343,12.));
#121256=CARTESIAN_POINT('Ctrl Pts',(61.2331355925547,-36.8877107529865,
0.));
#121257=CARTESIAN_POINT('Ctrl Pts',(61.2331355925547,-36.8877107529865,
12.));
#121258=CARTESIAN_POINT('Ctrl Pts',(61.2183137628056,-36.8701270167969,
0.));
#121259=CARTESIAN_POINT('Ctrl Pts',(61.2183137628056,-36.8701270167969,
12.));
#121260=CARTESIAN_POINT('Ctrl Pts',(61.2035032895127,-36.852592310174,0.));
#121261=CARTESIAN_POINT('Ctrl Pts',(61.2035032895127,-36.852592310174,12.));
#121262=CARTESIAN_POINT('Ctrl Pts',(61.1887043099014,-36.8351066918036,
0.));
#121263=CARTESIAN_POINT('Ctrl Pts',(61.1887043099014,-36.8351066918036,
12.));
#121264=CARTESIAN_POINT('Ctrl Pts',(61.1739169618666,-36.8176702205423,
0.));
#121265=CARTESIAN_POINT('Ctrl Pts',(61.1739169618666,-36.8176702205423,
12.));
#121266=CARTESIAN_POINT('Ctrl Pts',(61.1591413839787,-36.8002829554209,
0.));
#121267=CARTESIAN_POINT('Ctrl Pts',(61.1591413839787,-36.8002829554209,
12.));
#121268=CARTESIAN_POINT('Ctrl Pts',(61.1443777154911,-36.7829449556532,
0.));
#121269=CARTESIAN_POINT('Ctrl Pts',(61.1443777154911,-36.7829449556532,
12.));
#121270=CARTESIAN_POINT('Ctrl Pts',(61.1296260963466,-36.765656280638,0.));
#121271=CARTESIAN_POINT('Ctrl Pts',(61.1296260963466,-36.765656280638,12.));
#121272=CARTESIAN_POINT('Ctrl Pts',(61.1148866671829,-36.7484169899596,
0.));
#121273=CARTESIAN_POINT('Ctrl Pts',(61.1148866671829,-36.7484169899596,
12.));
#121274=CARTESIAN_POINT('Ctrl Pts',(61.100159569337,-36.7312271433807,0.));
#121275=CARTESIAN_POINT('Ctrl Pts',(61.100159569337,-36.7312271433807,12.));
#121276=CARTESIAN_POINT('Ctrl Pts',(61.0854449448524,-36.7140868008486,
0.));
#121277=CARTESIAN_POINT('Ctrl Pts',(61.0854449448524,-36.7140868008486,
12.));
#121278=CARTESIAN_POINT('Ctrl Pts',(61.0707429364847,-36.6969960225022,
0.));
#121279=CARTESIAN_POINT('Ctrl Pts',(61.0707429364847,-36.6969960225022,
12.));
#121280=CARTESIAN_POINT('Ctrl Pts',(61.0560536877083,-36.679954868674,0.));
#121281=CARTESIAN_POINT('Ctrl Pts',(61.0560536877083,-36.679954868674,12.));
#121282=CARTESIAN_POINT('Ctrl Pts',(61.0413773427203,-36.6629633998886,
0.));
#121283=CARTESIAN_POINT('Ctrl Pts',(61.0413773427203,-36.6629633998886,
12.));
#121284=CARTESIAN_POINT('Ctrl Pts',(61.0267140464432,-36.6460216768553,
0.));
#121285=CARTESIAN_POINT('Ctrl Pts',(61.0267140464432,-36.6460216768553,
12.));
#121286=CARTESIAN_POINT('Ctrl Pts',(61.0120639445349,-36.6291297604776,
0.));
#121287=CARTESIAN_POINT('Ctrl Pts',(61.0120639445349,-36.6291297604776,
12.));
#121288=CARTESIAN_POINT('Ctrl Pts',(60.9974271833981,-36.61228771186,0.));
#121289=CARTESIAN_POINT('Ctrl Pts',(60.9974271833981,-36.61228771186,12.));
#121290=CARTESIAN_POINT('Ctrl Pts',(60.9828039101887,-36.5954955923109,
0.));
#121291=CARTESIAN_POINT('Ctrl Pts',(60.9828039101887,-36.5954955923109,
12.));
#121292=CARTESIAN_POINT('Ctrl Pts',(60.9681942728236,-36.5787534633416,
0.));
#121293=CARTESIAN_POINT('Ctrl Pts',(60.9681942728236,-36.5787534633416,
12.));
#121294=CARTESIAN_POINT('Ctrl Pts',(60.9535984199873,-36.5620613866615,
0.));
#121295=CARTESIAN_POINT('Ctrl Pts',(60.9535984199873,-36.5620613866615,
12.));
#121296=CARTESIAN_POINT('Ctrl Pts',(60.9390165011355,-36.5454194241865,
0.));
#121297=CARTESIAN_POINT('Ctrl Pts',(60.9390165011355,-36.5454194241865,
12.));
#121298=CARTESIAN_POINT('Ctrl Pts',(60.9244486664987,-36.5288276380416,
0.));
#121299=CARTESIAN_POINT('Ctrl Pts',(60.9244486664987,-36.5288276380416,
12.));
#121300=CARTESIAN_POINT('Ctrl Pts',(60.9098950670847,-36.5122860905612,
0.));
#121301=CARTESIAN_POINT('Ctrl Pts',(60.9098950670847,-36.5122860905612,
12.));
#121302=CARTESIAN_POINT('Ctrl Pts',(60.8953558546795,-36.4957948442835,
0.));
#121303=CARTESIAN_POINT('Ctrl Pts',(60.8953558546795,-36.4957948442835,
12.));
#121304=CARTESIAN_POINT('Ctrl Pts',(60.8808311818499,-36.4793539619466,
0.));
#121305=CARTESIAN_POINT('Ctrl Pts',(60.8808311818499,-36.4793539619466,
12.));
#121306=CARTESIAN_POINT('Ctrl Pts',(60.8663212019657,-36.4629635065045,
0.));
#121307=CARTESIAN_POINT('Ctrl Pts',(60.8663212019657,-36.4629635065045,
12.));
#121308=CARTESIAN_POINT('Ctrl Pts',(60.8518260692188,-36.4466235411358,
0.));
#121309=CARTESIAN_POINT('Ctrl Pts',(60.8518260692188,-36.4466235411358,
12.));
#121310=CARTESIAN_POINT('Ctrl Pts',(60.8373459386392,-36.4303341292494,
0.));
#121311=CARTESIAN_POINT('Ctrl Pts',(60.8373459386392,-36.4303341292494,
12.));
#121312=CARTESIAN_POINT('Ctrl Pts',(60.822880966116,-36.4140953344859,0.));
#121313=CARTESIAN_POINT('Ctrl Pts',(60.822880966116,-36.4140953344859,12.));
#121314=CARTESIAN_POINT('Ctrl Pts',(60.8084313083984,-36.397907220716,0.));
#121315=CARTESIAN_POINT('Ctrl Pts',(60.8084313083984,-36.397907220716,12.));
#121316=CARTESIAN_POINT('Ctrl Pts',(60.793997123076,-36.3817698520388,0.));
#121317=CARTESIAN_POINT('Ctrl Pts',(60.793997123076,-36.3817698520388,12.));
#121318=CARTESIAN_POINT('Ctrl Pts',(60.7795785685625,-36.365683292773,0.));
#121319=CARTESIAN_POINT('Ctrl Pts',(60.7795785685625,-36.365683292773,12.));
#121320=CARTESIAN_POINT('Ctrl Pts',(60.7651758040803,-36.3496476074488,
0.));
#121321=CARTESIAN_POINT('Ctrl Pts',(60.7651758040803,-36.3496476074488,
12.));
#121322=CARTESIAN_POINT('Ctrl Pts',(60.7507889896308,-36.3336628607859,
0.));
#121323=CARTESIAN_POINT('Ctrl Pts',(60.7507889896308,-36.3336628607859,
12.));
#121324=CARTESIAN_POINT('Ctrl Pts',(60.7364182860412,-36.3177291177163,
0.));
#121325=CARTESIAN_POINT('Ctrl Pts',(60.7364182860412,-36.3177291177163,
12.));
#121326=CARTESIAN_POINT('Ctrl Pts',(60.722063855041,-36.3018464434214,0.));
#121327=CARTESIAN_POINT('Ctrl Pts',(60.722063855041,-36.3018464434214,12.));
#121328=CARTESIAN_POINT('Ctrl Pts',(60.7077258593268,-36.2860149033587,
0.));
#121329=CARTESIAN_POINT('Ctrl Pts',(60.7077258593268,-36.2860149033587,
12.));
#121330=CARTESIAN_POINT('Ctrl Pts',(60.6934044626291,-36.2702345632875,
0.));
#121331=CARTESIAN_POINT('Ctrl Pts',(60.6934044626291,-36.2702345632875,
12.));
#121332=CARTESIAN_POINT('Ctrl Pts',(60.67909982978,-36.2545054892897,0.));
#121333=CARTESIAN_POINT('Ctrl Pts',(60.67909982978,-36.2545054892897,12.));
#121334=CARTESIAN_POINT('Ctrl Pts',(60.6648121265885,-36.2388277477212,
0.));
#121335=CARTESIAN_POINT('Ctrl Pts',(60.6648121265885,-36.2388277477212,
12.));
#121336=CARTESIAN_POINT('Ctrl Pts',(60.6505415197042,-36.2232014051541,
0.));
#121337=CARTESIAN_POINT('Ctrl Pts',(60.6505415197042,-36.2232014051541,
12.));
#121338=CARTESIAN_POINT('Ctrl Pts',(60.6362881765019,-36.2076265283264,
0.));
#121339=CARTESIAN_POINT('Ctrl Pts',(60.6362881765019,-36.2076265283264,
12.));
#121340=CARTESIAN_POINT('Ctrl Pts',(60.6220522649149,-36.192103184063,0.));
#121341=CARTESIAN_POINT('Ctrl Pts',(60.6220522649149,-36.192103184063,12.));
#121342=CARTESIAN_POINT('Ctrl Pts',(60.6078339534181,-36.1766314392641,
0.));
#121343=CARTESIAN_POINT('Ctrl Pts',(60.6078339534181,-36.1766314392641,
12.));
#121344=CARTESIAN_POINT('Ctrl Pts',(60.5936334114108,-36.1612113610773,
0.));
#121345=CARTESIAN_POINT('Ctrl Pts',(60.5936334114108,-36.1612113610773,
12.));
#121346=CARTESIAN_POINT('Ctrl Pts',(60.5794508095564,-36.1458430170431,
0.));
#121347=CARTESIAN_POINT('Ctrl Pts',(60.5794508095564,-36.1458430170431,
12.));
#121348=CARTESIAN_POINT('Ctrl Pts',(60.565286320072,-36.1305264752188,0.));
#121349=CARTESIAN_POINT('Ctrl Pts',(60.565286320072,-36.1305264752188,12.));
#121350=CARTESIAN_POINT('Ctrl Pts',(60.5511401171984,-36.1152618043739,
0.));
#121351=CARTESIAN_POINT('Ctrl Pts',(60.5511401171984,-36.1152618043739,
12.));
#121352=CARTESIAN_POINT('Ctrl Pts',(60.5370123768804,-36.1000490738511,
0.));
#121353=CARTESIAN_POINT('Ctrl Pts',(60.5370123768804,-36.1000490738511,
12.));
#121354=CARTESIAN_POINT('Ctrl Pts',(60.5229032758973,-36.0848883531952,
0.));
#121355=CARTESIAN_POINT('Ctrl Pts',(60.5229032758973,-36.0848883531952,
12.));
#121356=CARTESIAN_POINT('Ctrl Pts',(60.5088129911354,-36.0697797118376,
0.));
#121357=CARTESIAN_POINT('Ctrl Pts',(60.5088129911354,-36.0697797118376,
12.));
#121358=CARTESIAN_POINT('Ctrl Pts',(60.4947416988422,-36.0547232187698,
0.));
#121359=CARTESIAN_POINT('Ctrl Pts',(60.4947416988422,-36.0547232187698,
12.));
#121360=CARTESIAN_POINT('Ctrl Pts',(60.4806895737686,-36.0397189421644,
0.));
#121361=CARTESIAN_POINT('Ctrl Pts',(60.4806895737686,-36.0397189421644,
12.));
#121362=CARTESIAN_POINT('Ctrl Pts',(60.4666567908093,-36.0247669500892,
0.));
#121363=CARTESIAN_POINT('Ctrl Pts',(60.4666567908093,-36.0247669500892,
12.));
#121364=CARTESIAN_POINT('Ctrl Pts',(60.4526435269662,-36.009867311357,0.));
#121365=CARTESIAN_POINT('Ctrl Pts',(60.4526435269662,-36.009867311357,12.));
#121366=CARTESIAN_POINT('Ctrl Pts',(60.4386499629481,-35.995020096217,0.));
#121367=CARTESIAN_POINT('Ctrl Pts',(60.4386499629481,-35.995020096217,12.));
#121368=CARTESIAN_POINT('Ctrl Pts',(60.4246762854926,-35.9802253773515,
0.));
#121369=CARTESIAN_POINT('Ctrl Pts',(60.4246762854926,-35.9802253773515,
12.));
#121370=CARTESIAN_POINT('Ctrl Pts',(60.4107226875714,-35.9654832299601,
0.));
#121371=CARTESIAN_POINT('Ctrl Pts',(60.4107226875714,-35.9654832299601,
12.));
#121372=CARTESIAN_POINT('Ctrl Pts',(60.3967893635452,-35.9507937296707,
0.));
#121373=CARTESIAN_POINT('Ctrl Pts',(60.3967893635452,-35.9507937296707,
12.));
#121374=CARTESIAN_POINT('Ctrl Pts',(60.3828765049019,-35.936156950695,0.));
#121375=CARTESIAN_POINT('Ctrl Pts',(60.3828765049019,-35.936156950695,12.));
#121376=CARTESIAN_POINT('Ctrl Pts',(60.3689842965481,-35.9215729642231,
0.));
#121377=CARTESIAN_POINT('Ctrl Pts',(60.3689842965481,-35.9215729642231,
12.));
#121378=CARTESIAN_POINT('Ctrl Pts',(60.3551129108845,-35.907041835853,0.));
#121379=CARTESIAN_POINT('Ctrl Pts',(60.3551129108845,-35.907041835853,12.));
#121380=CARTESIAN_POINT('Ctrl Pts',(60.3412625135287,-35.8925636280668,
0.));
#121381=CARTESIAN_POINT('Ctrl Pts',(60.3412625135287,-35.8925636280668,
12.));
#121382=CARTESIAN_POINT('Ctrl Pts',(60.327433274683,-35.8781384051537,0.));
#121383=CARTESIAN_POINT('Ctrl Pts',(60.327433274683,-35.8781384051537,12.));
#121384=CARTESIAN_POINT('Ctrl Pts',(60.3136253782809,-35.8637662371635,
0.));
#121385=CARTESIAN_POINT('Ctrl Pts',(60.3136253782809,-35.8637662371635,
12.));
#121386=CARTESIAN_POINT('Ctrl Pts',(60.2998390330102,-35.8494472046746,
0.));
#121387=CARTESIAN_POINT('Ctrl Pts',(60.2998390330102,-35.8494472046746,
12.));
#121388=CARTESIAN_POINT('Ctrl Pts',(60.2860744798436,-35.8351814020357,
0.));
#121389=CARTESIAN_POINT('Ctrl Pts',(60.2860744798436,-35.8351814020357,
12.));
#121390=CARTESIAN_POINT('Ctrl Pts',(60.2723319687369,-35.8209689272501,
0.));
#121391=CARTESIAN_POINT('Ctrl Pts',(60.2723319687369,-35.8209689272501,
12.));
#121392=CARTESIAN_POINT('Ctrl Pts',(60.2586117365205,-35.8068098723347,
0.));
#121393=CARTESIAN_POINT('Ctrl Pts',(60.2586117365205,-35.8068098723347,
12.));
#121394=CARTESIAN_POINT('Ctrl Pts',(60.2449139865274,-35.7927043145201,
0.));
#121395=CARTESIAN_POINT('Ctrl Pts',(60.2449139865274,-35.7927043145201,
12.));
#121396=CARTESIAN_POINT('Ctrl Pts',(60.2312388621529,-35.7786523045912,
0.));
#121397=CARTESIAN_POINT('Ctrl Pts',(60.2312388621529,-35.7786523045912,
12.));
#121398=CARTESIAN_POINT('Ctrl Pts',(60.2175864450043,-35.7646538667493,
0.));
#121399=CARTESIAN_POINT('Ctrl Pts',(60.2175864450043,-35.7646538667493,
12.));
#121400=CARTESIAN_POINT('Ctrl Pts',(60.206682708692,-35.7534979802053,0.));
#121401=CARTESIAN_POINT('Ctrl Pts',(60.206682708692,-35.7534979802053,12.));
#121402=CARTESIAN_POINT('Ctrl Pts',(60.1985151474623,-35.7451551752572,
0.));
#121403=CARTESIAN_POINT('Ctrl Pts',(60.1985151474623,-35.7451551752572,
12.));
#121404=CARTESIAN_POINT('Ctrl Pts',(60.193074658032,-35.7396040204017,0.));
#121405=CARTESIAN_POINT('Ctrl Pts',(60.193074658032,-35.7396040204017,12.));
#121406=CARTESIAN_POINT('Ctrl Pts',(60.1903555511633,-35.736831121751,0.));
#121407=CARTESIAN_POINT('Ctrl Pts',(60.1903555511633,-35.736831121751,12.));
#121408=CARTESIAN_POINT('',(60.1903555511633,-35.736831121751,12.));
#121409=CARTESIAN_POINT('Ctrl Pts',(60.1903555511633,-35.736831121751,12.));
#121410=CARTESIAN_POINT('Ctrl Pts',(60.193074658032,-35.7396040204017,12.));
#121411=CARTESIAN_POINT('Ctrl Pts',(60.1985151474623,-35.7451551752572,
12.));
#121412=CARTESIAN_POINT('Ctrl Pts',(60.206682708692,-35.7534979802053,12.));
#121413=CARTESIAN_POINT('Ctrl Pts',(60.2175864450043,-35.7646538667493,
12.));
#121414=CARTESIAN_POINT('Ctrl Pts',(60.2312388621529,-35.7786523045912,
12.));
#121415=CARTESIAN_POINT('Ctrl Pts',(60.2449139865274,-35.7927043145201,
12.));
#121416=CARTESIAN_POINT('Ctrl Pts',(60.2586117365205,-35.8068098723347,
12.));
#121417=CARTESIAN_POINT('Ctrl Pts',(60.2723319687369,-35.8209689272501,
12.));
#121418=CARTESIAN_POINT('Ctrl Pts',(60.2860744798436,-35.8351814020357,
12.));
#121419=CARTESIAN_POINT('Ctrl Pts',(60.2998390330102,-35.8494472046746,
12.));
#121420=CARTESIAN_POINT('Ctrl Pts',(60.3136253782809,-35.8637662371635,
12.));
#121421=CARTESIAN_POINT('Ctrl Pts',(60.327433274683,-35.8781384051537,12.));
#121422=CARTESIAN_POINT('Ctrl Pts',(60.3412625135287,-35.8925636280668,
12.));
#121423=CARTESIAN_POINT('Ctrl Pts',(60.3551129108845,-35.907041835853,12.));
#121424=CARTESIAN_POINT('Ctrl Pts',(60.3689842965481,-35.9215729642231,
12.));
#121425=CARTESIAN_POINT('Ctrl Pts',(60.3828765049019,-35.936156950695,12.));
#121426=CARTESIAN_POINT('Ctrl Pts',(60.3967893635452,-35.9507937296707,
12.));
#121427=CARTESIAN_POINT('Ctrl Pts',(60.4107226875714,-35.9654832299601,
12.));
#121428=CARTESIAN_POINT('Ctrl Pts',(60.4246762854926,-35.9802253773515,
12.));
#121429=CARTESIAN_POINT('Ctrl Pts',(60.4386499629481,-35.995020096217,12.));
#121430=CARTESIAN_POINT('Ctrl Pts',(60.4526435269662,-36.009867311357,12.));
#121431=CARTESIAN_POINT('Ctrl Pts',(60.4666567908093,-36.0247669500892,
12.));
#121432=CARTESIAN_POINT('Ctrl Pts',(60.4806895737686,-36.0397189421644,
12.));
#121433=CARTESIAN_POINT('Ctrl Pts',(60.4947416988422,-36.0547232187698,
12.));
#121434=CARTESIAN_POINT('Ctrl Pts',(60.5088129911354,-36.0697797118376,
12.));
#121435=CARTESIAN_POINT('Ctrl Pts',(60.5229032758973,-36.0848883531952,
12.));
#121436=CARTESIAN_POINT('Ctrl Pts',(60.5370123768804,-36.1000490738511,
12.));
#121437=CARTESIAN_POINT('Ctrl Pts',(60.5511401171984,-36.1152618043739,
12.));
#121438=CARTESIAN_POINT('Ctrl Pts',(60.565286320072,-36.1305264752188,12.));
#121439=CARTESIAN_POINT('Ctrl Pts',(60.5794508095564,-36.1458430170431,
12.));
#121440=CARTESIAN_POINT('Ctrl Pts',(60.5936334114108,-36.1612113610773,
12.));
#121441=CARTESIAN_POINT('Ctrl Pts',(60.6078339534181,-36.1766314392641,
12.));
#121442=CARTESIAN_POINT('Ctrl Pts',(60.6220522649149,-36.192103184063,12.));
#121443=CARTESIAN_POINT('Ctrl Pts',(60.6362881765019,-36.2076265283264,
12.));
#121444=CARTESIAN_POINT('Ctrl Pts',(60.6505415197042,-36.2232014051541,
12.));
#121445=CARTESIAN_POINT('Ctrl Pts',(60.6648121265885,-36.2388277477212,
12.));
#121446=CARTESIAN_POINT('Ctrl Pts',(60.67909982978,-36.2545054892897,12.));
#121447=CARTESIAN_POINT('Ctrl Pts',(60.6934044626291,-36.2702345632875,
12.));
#121448=CARTESIAN_POINT('Ctrl Pts',(60.7077258593268,-36.2860149033587,
12.));
#121449=CARTESIAN_POINT('Ctrl Pts',(60.722063855041,-36.3018464434214,12.));
#121450=CARTESIAN_POINT('Ctrl Pts',(60.7364182860412,-36.3177291177163,
12.));
#121451=CARTESIAN_POINT('Ctrl Pts',(60.7507889896308,-36.3336628607859,
12.));
#121452=CARTESIAN_POINT('Ctrl Pts',(60.7651758040803,-36.3496476074488,
12.));
#121453=CARTESIAN_POINT('Ctrl Pts',(60.7795785685625,-36.365683292773,12.));
#121454=CARTESIAN_POINT('Ctrl Pts',(60.793997123076,-36.3817698520388,12.));
#121455=CARTESIAN_POINT('Ctrl Pts',(60.8084313083984,-36.397907220716,12.));
#121456=CARTESIAN_POINT('Ctrl Pts',(60.822880966116,-36.4140953344859,12.));
#121457=CARTESIAN_POINT('Ctrl Pts',(60.8373459386392,-36.4303341292494,
12.));
#121458=CARTESIAN_POINT('Ctrl Pts',(60.8518260692188,-36.4466235411358,
12.));
#121459=CARTESIAN_POINT('Ctrl Pts',(60.8663212019657,-36.4629635065045,
12.));
#121460=CARTESIAN_POINT('Ctrl Pts',(60.8808311818499,-36.4793539619466,
12.));
#121461=CARTESIAN_POINT('Ctrl Pts',(60.8953558546795,-36.4957948442835,
12.));
#121462=CARTESIAN_POINT('Ctrl Pts',(60.9098950670847,-36.5122860905612,
12.));
#121463=CARTESIAN_POINT('Ctrl Pts',(60.9244486664987,-36.5288276380416,
12.));
#121464=CARTESIAN_POINT('Ctrl Pts',(60.9390165011355,-36.5454194241865,
12.));
#121465=CARTESIAN_POINT('Ctrl Pts',(60.9535984199873,-36.5620613866615,
12.));
#121466=CARTESIAN_POINT('Ctrl Pts',(60.9681942728236,-36.5787534633416,
12.));
#121467=CARTESIAN_POINT('Ctrl Pts',(60.9828039101887,-36.5954955923109,
12.));
#121468=CARTESIAN_POINT('Ctrl Pts',(60.9974271833981,-36.61228771186,12.));
#121469=CARTESIAN_POINT('Ctrl Pts',(61.0120639445349,-36.6291297604776,
12.));
#121470=CARTESIAN_POINT('Ctrl Pts',(61.0267140464432,-36.6460216768553,
12.));
#121471=CARTESIAN_POINT('Ctrl Pts',(61.0413773427203,-36.6629633998886,
12.));
#121472=CARTESIAN_POINT('Ctrl Pts',(61.0560536877083,-36.679954868674,12.));
#121473=CARTESIAN_POINT('Ctrl Pts',(61.0707429364847,-36.6969960225022,
12.));
#121474=CARTESIAN_POINT('Ctrl Pts',(61.0854449448524,-36.7140868008486,
12.));
#121475=CARTESIAN_POINT('Ctrl Pts',(61.100159569337,-36.7312271433807,12.));
#121476=CARTESIAN_POINT('Ctrl Pts',(61.1148866671829,-36.7484169899596,
12.));
#121477=CARTESIAN_POINT('Ctrl Pts',(61.1296260963466,-36.765656280638,12.));
#121478=CARTESIAN_POINT('Ctrl Pts',(61.1443777154911,-36.7829449556532,
12.));
#121479=CARTESIAN_POINT('Ctrl Pts',(61.1591413839787,-36.8002829554209,
12.));
#121480=CARTESIAN_POINT('Ctrl Pts',(61.1739169618666,-36.8176702205423,
12.));
#121481=CARTESIAN_POINT('Ctrl Pts',(61.1887043099014,-36.8351066918036,
12.));
#121482=CARTESIAN_POINT('Ctrl Pts',(61.2035032895127,-36.852592310174,12.));
#121483=CARTESIAN_POINT('Ctrl Pts',(61.2183137628056,-36.8701270167969,
12.));
#121484=CARTESIAN_POINT('Ctrl Pts',(61.2331355925547,-36.8877107529865,
12.));
#121485=CARTESIAN_POINT('Ctrl Pts',(61.247968642201,-36.9053434602343,12.));
#121486=CARTESIAN_POINT('Ctrl Pts',(61.2628127758457,-36.9230250802088,
12.));
#121487=CARTESIAN_POINT('Ctrl Pts',(61.2776678582461,-36.9407555547535,
12.));
#121488=CARTESIAN_POINT('Ctrl Pts',(61.2925337548077,-36.9585348258776,
12.));
#121489=CARTESIAN_POINT('Ctrl Pts',(61.3074103315791,-36.9763628357544,
12.));
#121490=CARTESIAN_POINT('Ctrl Pts',(61.3222974552486,-36.994239526727,12.));
#121491=CARTESIAN_POINT('Ctrl Pts',(61.3371949931387,-37.0121648413082,
12.));
#121492=CARTESIAN_POINT('Ctrl Pts',(61.3521028132003,-37.0301387221774,
12.));
#121493=CARTESIAN_POINT('Ctrl Pts',(61.3670207840068,-37.0481611121717,
12.));
#121494=CARTESIAN_POINT('Ctrl Pts',(61.381948774749,-37.0662319542849,12.));
#121495=CARTESIAN_POINT('Ctrl Pts',(61.3968866552317,-37.0843511916745,
12.));
#121496=CARTESIAN_POINT('Ctrl Pts',(61.4118342958697,-37.1025187676602,
12.));
#121497=CARTESIAN_POINT('Ctrl Pts',(61.4267915676822,-37.1207346257222,
12.));
#121498=CARTESIAN_POINT('Ctrl Pts',(61.4417583422863,-37.1389987094905,
12.));
#121499=CARTESIAN_POINT('Ctrl Pts',(61.4567344918919,-37.1573109627454,
12.));
#121500=CARTESIAN_POINT('Ctrl Pts',(61.4717198892994,-37.175671329424,12.));
#121501=CARTESIAN_POINT('Ctrl Pts',(61.4867144078936,-37.1940797536181,
12.));
#121502=CARTESIAN_POINT('Ctrl Pts',(61.501717921641,-37.2125361795731,12.));
#121503=CARTESIAN_POINT('Ctrl Pts',(61.5167303050832,-37.2310405516781,
12.));
#121504=CARTESIAN_POINT('Ctrl Pts',(61.5317514333328,-37.2495928144667,
12.));
#121505=CARTESIAN_POINT('Ctrl Pts',(61.5467811820691,-37.2681929126221,
12.));
#121506=CARTESIAN_POINT('Ctrl Pts',(61.5618194275348,-37.2868407909771,
12.));
#121507=CARTESIAN_POINT('Ctrl Pts',(61.5768660465311,-37.3055363945108,
12.));
#121508=CARTESIAN_POINT('Ctrl Pts',(61.591920916412,-37.3242796683395,12.));
#121509=CARTESIAN_POINT('Ctrl Pts',(61.6069839150807,-37.343070557718,12.));
#121510=CARTESIAN_POINT('Ctrl Pts',(61.6220549209866,-37.361909008045,12.));
#121511=CARTESIAN_POINT('Ctrl Pts',(61.637133813121,-37.3807949648624,12.));
#121512=CARTESIAN_POINT('Ctrl Pts',(61.6522204710131,-37.3997283738533,
12.));
#121513=CARTESIAN_POINT('Ctrl Pts',(61.6673147747242,-37.4187091808321,
12.));
#121514=CARTESIAN_POINT('Ctrl Pts',(61.6824166048444,-37.4377373317451,
12.));
#121515=CARTESIAN_POINT('Ctrl Pts',(61.6975258424894,-37.4568127726773,
12.));
#121516=CARTESIAN_POINT('Ctrl Pts',(61.7126423692963,-37.4759354498509,
12.));
#121517=CARTESIAN_POINT('Ctrl Pts',(61.7277660674205,-37.4951053096237,
12.));
#121518=CARTESIAN_POINT('Ctrl Pts',(61.7428968195299,-37.5143222984796,
12.));
#121519=CARTESIAN_POINT('Ctrl Pts',(61.7580345088016,-37.5335863630287,
12.));
#121520=CARTESIAN_POINT('Ctrl Pts',(61.773179018919,-37.5528974500142,12.));
#121521=CARTESIAN_POINT('Ctrl Pts',(61.7883302340687,-37.5722555063111,
12.));
#121522=CARTESIAN_POINT('Ctrl Pts',(61.8034880389362,-37.5916604789253,
12.));
#121523=CARTESIAN_POINT('Ctrl Pts',(61.8186523187015,-37.6111123149839,
12.));
#121524=CARTESIAN_POINT('Ctrl Pts',(61.8338229590352,-37.6306109617347,
12.));
#121525=CARTESIAN_POINT('Ctrl Pts',(61.8489998460957,-37.6501563665524,
12.));
#121526=CARTESIAN_POINT('Ctrl Pts',(61.8641828665261,-37.6697484769392,
12.));
#121527=CARTESIAN_POINT('Ctrl Pts',(61.8793719074507,-37.6893872405228,
12.));
#121528=CARTESIAN_POINT('Ctrl Pts',(61.8945668564704,-37.7090726050482,
12.));
#121529=CARTESIAN_POINT('Ctrl Pts',(61.9097676016601,-37.7288045183756,
12.));
#121530=CARTESIAN_POINT('Ctrl Pts',(61.9249740315649,-37.7485829284872,
12.));
#121531=CARTESIAN_POINT('Ctrl Pts',(61.9401860351972,-37.7684077834873,
12.));
#121532=CARTESIAN_POINT('Ctrl Pts',(61.9554035020338,-37.7882790316014,
12.));
#121533=CARTESIAN_POINT('Ctrl Pts',(61.9706263220114,-37.8081966211689,
12.));
#121534=CARTESIAN_POINT('Ctrl Pts',(61.9858543855236,-37.8281605006381,
12.));
#121535=CARTESIAN_POINT('Ctrl Pts',(62.0010875834187,-37.8481706185749,
12.));
#121536=CARTESIAN_POINT('Ctrl Pts',(62.0163258069957,-37.868226923663,12.));
#121537=CARTESIAN_POINT('Ctrl Pts',(62.031568948002,-37.8883293647029,12.));
#121538=CARTESIAN_POINT('Ctrl Pts',(62.0468168986288,-37.9084778906053,
12.));
#121539=CARTESIAN_POINT('Ctrl Pts',(62.0620695515074,-37.9286724503851,
12.));
#121540=CARTESIAN_POINT('Ctrl Pts',(62.0773267997078,-37.9489129931689,
12.));
#121541=CARTESIAN_POINT('Ctrl Pts',(62.0925885367352,-37.9691994681966,
12.));
#121542=CARTESIAN_POINT('Ctrl Pts',(62.107854656528,-37.9895318248212,12.));
#121543=CARTESIAN_POINT('Ctrl Pts',(62.123125053455,-38.0099100125037,12.));
#121544=CARTESIAN_POINT('Ctrl Pts',(62.1383996223124,-38.0303339808053,
12.));
#121545=CARTESIAN_POINT('Ctrl Pts',(62.1536782583199,-38.0508036793939,
12.));
#121546=CARTESIAN_POINT('Ctrl Pts',(62.1689608571176,-38.0713190580463,
12.));
#121547=CARTESIAN_POINT('Ctrl Pts',(62.1842473147626,-38.0918800666479,
12.));
#121548=CARTESIAN_POINT('Ctrl Pts',(62.1995375277257,-38.1124866551886,
12.));
#121549=CARTESIAN_POINT('Ctrl Pts',(62.2148313928863,-38.133138773753,12.));
#121550=CARTESIAN_POINT('Ctrl Pts',(62.2301288075321,-38.1538363725264,
12.));
#121551=CARTESIAN_POINT('Ctrl Pts',(62.245429669358,-38.1745794017996,12.));
#121552=CARTESIAN_POINT('Ctrl Pts',(62.2607338764654,-38.1953678119691,
12.));
#121553=CARTESIAN_POINT('Ctrl Pts',(62.2760413273602,-38.2162015535353,
12.));
#121554=CARTESIAN_POINT('Ctrl Pts',(62.2913519209521,-38.2370805770935,
12.));
#121555=CARTESIAN_POINT('Ctrl Pts',(62.3066655565503,-38.2580048333361,
12.));
#121556=CARTESIAN_POINT('Ctrl Pts',(62.3219821338569,-38.2789742730564,
12.));
#121557=CARTESIAN_POINT('Ctrl Pts',(62.3373015529613,-38.2999888471476,
12.));
#121558=CARTESIAN_POINT('Ctrl Pts',(62.3526237143336,-38.3210485066001,
12.));
#121559=CARTESIAN_POINT('Ctrl Pts',(62.3679485188171,-38.342153202491,12.));
#121560=CARTESIAN_POINT('Ctrl Pts',(62.3832758676271,-38.3633028859828,
12.));
#121561=CARTESIAN_POINT('Ctrl Pts',(62.3986056623577,-38.3844975083344,
12.));
#121562=CARTESIAN_POINT('Ctrl Pts',(62.4139378049885,-38.405737020905,12.));
#121563=CARTESIAN_POINT('Ctrl Pts',(62.4292721978901,-38.4270213751568,
12.));
#121564=CARTESIAN_POINT('Ctrl Pts',(62.4446087438312,-38.4483505226518,
12.));
#121565=CARTESIAN_POINT('Ctrl Pts',(62.4599473459811,-38.4697244150482,
12.));
#121566=CARTESIAN_POINT('Ctrl Pts',(62.4752879078854,-38.4911430040997,
12.));
#121567=CARTESIAN_POINT('Ctrl Pts',(62.4906303334443,-38.5126062416502,
12.));
#121568=CARTESIAN_POINT('Ctrl Pts',(62.5059745268901,-38.5341140796248,
12.));
#121569=CARTESIAN_POINT('Ctrl Pts',(62.5213203927663,-38.5556664700195,
12.));
#121570=CARTESIAN_POINT('Ctrl Pts',(62.5366678359023,-38.5772633648833,
12.));
#121571=CARTESIAN_POINT('Ctrl Pts',(62.5520167614516,-38.5989047163393,
12.));
#121572=CARTESIAN_POINT('Ctrl Pts',(62.5673670749361,-38.6205904766073,
12.));
#121573=CARTESIAN_POINT('Ctrl Pts',(62.582718682292,-38.6423205980213,12.));
#121574=CARTESIAN_POINT('Ctrl Pts',(62.5980714899052,-38.6640950330421,
12.));
#121575=CARTESIAN_POINT('Ctrl Pts',(62.6134254046739,-38.6859137342731,
12.));
#121576=CARTESIAN_POINT('Ctrl Pts',(62.6287803339542,-38.7077766544416,
12.));
#121577=CARTESIAN_POINT('Ctrl Pts',(62.6441361854411,-38.7296837463609,
12.));
#121578=CARTESIAN_POINT('Ctrl Pts',(62.6594928670628,-38.7516349628904,
12.));
#121579=CARTESIAN_POINT('Ctrl Pts',(62.6748502868835,-38.7736302568982,
12.));
#121580=CARTESIAN_POINT('Ctrl Pts',(62.6902083529694,-38.795669581203,12.));
#121581=CARTESIAN_POINT('Ctrl Pts',(62.7055669733802,-38.8177528885681,
12.));
#121582=CARTESIAN_POINT('Ctrl Pts',(62.7209260564493,-38.8398801318177,
12.));
#121583=CARTESIAN_POINT('Ctrl Pts',(62.7362855110042,-38.8620512639233,
12.));
#121584=CARTESIAN_POINT('Ctrl Pts',(62.7516452466128,-38.8842662380984,
12.));
#121585=CARTESIAN_POINT('Ctrl Pts',(62.7670051738143,-38.9065250078832,
12.));
#121586=CARTESIAN_POINT('Ctrl Pts',(62.78236520437,-38.9288275272335,12.));
#121587=CARTESIAN_POINT('Ctrl Pts',(62.7977252507117,-38.9511737503165,
12.));
#121588=CARTESIAN_POINT('Ctrl Pts',(62.8130852254027,-38.9735636313089,
12.));
#121589=CARTESIAN_POINT('Ctrl Pts',(62.8284450405459,-38.9959971241701,
12.));
#121590=CARTESIAN_POINT('Ctrl Pts',(62.8438046073224,-39.0184741824641,
12.));
#121591=CARTESIAN_POINT('Ctrl Pts',(62.8591638352055,-39.0409947590497,
12.));
#121592=CARTESIAN_POINT('Ctrl Pts',(62.8745226325998,-39.0635588063277,
12.));
#121593=CARTESIAN_POINT('Ctrl Pts',(62.8898809082611,-39.0861662767932,
12.));
#121594=CARTESIAN_POINT('Ctrl Pts',(62.9052385725387,-39.1088171235125,
12.));
#121595=CARTESIAN_POINT('Ctrl Pts',(62.9205955385558,-39.131511300575,12.));
#121596=CARTESIAN_POINT('Ctrl Pts',(62.9359517237404,-39.1542487636744,
12.));
#121597=CARTESIAN_POINT('Ctrl Pts',(62.9513070501867,-39.1770294702428,
12.));
#121598=CARTESIAN_POINT('Ctrl Pts',(62.9644687386836,-39.1965939820933,
12.));
#121599=CARTESIAN_POINT('Ctrl Pts',(62.9745590018672,-39.2116170128461,
12.));
#121600=CARTESIAN_POINT('Ctrl Pts',(62.9815782721325,-39.2220794388807,
12.));
#121601=CARTESIAN_POINT('Ctrl Pts',(62.9855268616127,-39.2279686275006,
12.));
#121602=CARTESIAN_POINT('Ctrl Pts',(62.9864049293894,-39.2292784191812,
12.));
#121603=CARTESIAN_POINT('',(60.1903555511633,-35.736831121751,0.));
#121604=CARTESIAN_POINT('',(60.1903555511633,-35.736831121751,0.));
#121605=CARTESIAN_POINT('Ctrl Pts',(62.9864049293894,-39.2292784191813,
0.));
#121606=CARTESIAN_POINT('Ctrl Pts',(62.9855268616127,-39.2279686275007,
0.));
#121607=CARTESIAN_POINT('Ctrl Pts',(62.9815782721326,-39.2220794388807,
0.));
#121608=CARTESIAN_POINT('Ctrl Pts',(62.9745590018672,-39.2116170128461,
0.));
#121609=CARTESIAN_POINT('Ctrl Pts',(62.9644687386836,-39.1965939820933,
0.));
#121610=CARTESIAN_POINT('Ctrl Pts',(62.9513070501867,-39.1770294702428,
0.));
#121611=CARTESIAN_POINT('Ctrl Pts',(62.9359517237404,-39.1542487636744,
0.));
#121612=CARTESIAN_POINT('Ctrl Pts',(62.9205955385558,-39.131511300575,0.));
#121613=CARTESIAN_POINT('Ctrl Pts',(62.9052385725387,-39.1088171235125,
0.));
#121614=CARTESIAN_POINT('Ctrl Pts',(62.8898809082611,-39.0861662767932,
0.));
#121615=CARTESIAN_POINT('Ctrl Pts',(62.8745226325998,-39.0635588063277,
0.));
#121616=CARTESIAN_POINT('Ctrl Pts',(62.8591638352055,-39.0409947590497,
0.));
#121617=CARTESIAN_POINT('Ctrl Pts',(62.8438046073224,-39.0184741824641,
0.));
#121618=CARTESIAN_POINT('Ctrl Pts',(62.8284450405459,-38.9959971241701,
0.));
#121619=CARTESIAN_POINT('Ctrl Pts',(62.8130852254027,-38.9735636313089,
0.));
#121620=CARTESIAN_POINT('Ctrl Pts',(62.7977252507117,-38.9511737503165,
0.));
#121621=CARTESIAN_POINT('Ctrl Pts',(62.78236520437,-38.9288275272335,0.));
#121622=CARTESIAN_POINT('Ctrl Pts',(62.7670051738143,-38.9065250078832,
0.));
#121623=CARTESIAN_POINT('Ctrl Pts',(62.7516452466128,-38.8842662380984,
0.));
#121624=CARTESIAN_POINT('Ctrl Pts',(62.7362855110042,-38.8620512639233,
0.));
#121625=CARTESIAN_POINT('Ctrl Pts',(62.7209260564493,-38.8398801318177,
0.));
#121626=CARTESIAN_POINT('Ctrl Pts',(62.7055669733802,-38.8177528885681,
0.));
#121627=CARTESIAN_POINT('Ctrl Pts',(62.6902083529694,-38.795669581203,0.));
#121628=CARTESIAN_POINT('Ctrl Pts',(62.6748502868835,-38.7736302568982,
0.));
#121629=CARTESIAN_POINT('Ctrl Pts',(62.6594928670628,-38.7516349628904,
0.));
#121630=CARTESIAN_POINT('Ctrl Pts',(62.6441361854411,-38.7296837463609,
0.));
#121631=CARTESIAN_POINT('Ctrl Pts',(62.6287803339542,-38.7077766544416,
0.));
#121632=CARTESIAN_POINT('Ctrl Pts',(62.6134254046739,-38.6859137342731,
0.));
#121633=CARTESIAN_POINT('Ctrl Pts',(62.5980714899052,-38.6640950330421,
0.));
#121634=CARTESIAN_POINT('Ctrl Pts',(62.582718682292,-38.6423205980213,0.));
#121635=CARTESIAN_POINT('Ctrl Pts',(62.5673670749361,-38.6205904766073,
0.));
#121636=CARTESIAN_POINT('Ctrl Pts',(62.5520167614516,-38.5989047163393,
0.));
#121637=CARTESIAN_POINT('Ctrl Pts',(62.5366678359023,-38.5772633648833,
0.));
#121638=CARTESIAN_POINT('Ctrl Pts',(62.5213203927663,-38.5556664700195,
0.));
#121639=CARTESIAN_POINT('Ctrl Pts',(62.5059745268901,-38.5341140796248,
0.));
#121640=CARTESIAN_POINT('Ctrl Pts',(62.4906303334443,-38.5126062416502,
0.));
#121641=CARTESIAN_POINT('Ctrl Pts',(62.4752879078854,-38.4911430040997,
0.));
#121642=CARTESIAN_POINT('Ctrl Pts',(62.4599473459811,-38.4697244150482,
0.));
#121643=CARTESIAN_POINT('Ctrl Pts',(62.4446087438312,-38.4483505226518,
0.));
#121644=CARTESIAN_POINT('Ctrl Pts',(62.4292721978901,-38.4270213751568,
0.));
#121645=CARTESIAN_POINT('Ctrl Pts',(62.4139378049885,-38.405737020905,0.));
#121646=CARTESIAN_POINT('Ctrl Pts',(62.3986056623577,-38.3844975083344,
0.));
#121647=CARTESIAN_POINT('Ctrl Pts',(62.3832758676271,-38.3633028859828,
0.));
#121648=CARTESIAN_POINT('Ctrl Pts',(62.3679485188171,-38.342153202491,0.));
#121649=CARTESIAN_POINT('Ctrl Pts',(62.3526237143336,-38.3210485066001,
0.));
#121650=CARTESIAN_POINT('Ctrl Pts',(62.3373015529613,-38.2999888471476,
0.));
#121651=CARTESIAN_POINT('Ctrl Pts',(62.3219821338569,-38.2789742730564,
0.));
#121652=CARTESIAN_POINT('Ctrl Pts',(62.3066655565503,-38.2580048333361,
0.));
#121653=CARTESIAN_POINT('Ctrl Pts',(62.2913519209521,-38.2370805770935,
0.));
#121654=CARTESIAN_POINT('Ctrl Pts',(62.2760413273602,-38.2162015535353,
0.));
#121655=CARTESIAN_POINT('Ctrl Pts',(62.2607338764654,-38.1953678119691,
0.));
#121656=CARTESIAN_POINT('Ctrl Pts',(62.245429669358,-38.1745794017996,0.));
#121657=CARTESIAN_POINT('Ctrl Pts',(62.2301288075321,-38.1538363725264,
0.));
#121658=CARTESIAN_POINT('Ctrl Pts',(62.2148313928863,-38.133138773753,0.));
#121659=CARTESIAN_POINT('Ctrl Pts',(62.1995375277257,-38.1124866551886,
0.));
#121660=CARTESIAN_POINT('Ctrl Pts',(62.1842473147626,-38.0918800666479,
0.));
#121661=CARTESIAN_POINT('Ctrl Pts',(62.1689608571176,-38.0713190580463,
0.));
#121662=CARTESIAN_POINT('Ctrl Pts',(62.1536782583199,-38.0508036793939,
0.));
#121663=CARTESIAN_POINT('Ctrl Pts',(62.1383996223124,-38.0303339808053,
0.));
#121664=CARTESIAN_POINT('Ctrl Pts',(62.123125053455,-38.0099100125037,0.));
#121665=CARTESIAN_POINT('Ctrl Pts',(62.107854656528,-37.9895318248212,0.));
#121666=CARTESIAN_POINT('Ctrl Pts',(62.0925885367352,-37.9691994681966,
0.));
#121667=CARTESIAN_POINT('Ctrl Pts',(62.0773267997078,-37.9489129931689,
0.));
#121668=CARTESIAN_POINT('Ctrl Pts',(62.0620695515074,-37.9286724503851,
0.));
#121669=CARTESIAN_POINT('Ctrl Pts',(62.0468168986288,-37.9084778906053,
0.));
#121670=CARTESIAN_POINT('Ctrl Pts',(62.031568948002,-37.8883293647029,0.));
#121671=CARTESIAN_POINT('Ctrl Pts',(62.0163258069957,-37.868226923663,0.));
#121672=CARTESIAN_POINT('Ctrl Pts',(62.0010875834187,-37.8481706185749,
0.));
#121673=CARTESIAN_POINT('Ctrl Pts',(61.9858543855236,-37.8281605006381,
0.));
#121674=CARTESIAN_POINT('Ctrl Pts',(61.9706263220114,-37.8081966211689,
0.));
#121675=CARTESIAN_POINT('Ctrl Pts',(61.9554035020338,-37.7882790316014,
0.));
#121676=CARTESIAN_POINT('Ctrl Pts',(61.9401860351972,-37.7684077834873,
0.));
#121677=CARTESIAN_POINT('Ctrl Pts',(61.9249740315649,-37.7485829284872,
0.));
#121678=CARTESIAN_POINT('Ctrl Pts',(61.9097676016601,-37.7288045183756,
0.));
#121679=CARTESIAN_POINT('Ctrl Pts',(61.8945668564704,-37.7090726050482,
0.));
#121680=CARTESIAN_POINT('Ctrl Pts',(61.8793719074507,-37.6893872405228,
0.));
#121681=CARTESIAN_POINT('Ctrl Pts',(61.8641828665261,-37.6697484769392,
0.));
#121682=CARTESIAN_POINT('Ctrl Pts',(61.8489998460957,-37.6501563665524,
0.));
#121683=CARTESIAN_POINT('Ctrl Pts',(61.8338229590352,-37.6306109617347,
0.));
#121684=CARTESIAN_POINT('Ctrl Pts',(61.8186523187015,-37.6111123149839,
0.));
#121685=CARTESIAN_POINT('Ctrl Pts',(61.8034880389362,-37.5916604789253,
0.));
#121686=CARTESIAN_POINT('Ctrl Pts',(61.7883302340687,-37.5722555063111,
0.));
#121687=CARTESIAN_POINT('Ctrl Pts',(61.773179018919,-37.5528974500142,0.));
#121688=CARTESIAN_POINT('Ctrl Pts',(61.7580345088016,-37.5335863630287,
0.));
#121689=CARTESIAN_POINT('Ctrl Pts',(61.7428968195299,-37.5143222984796,
0.));
#121690=CARTESIAN_POINT('Ctrl Pts',(61.7277660674205,-37.4951053096237,
0.));
#121691=CARTESIAN_POINT('Ctrl Pts',(61.7126423692963,-37.4759354498509,
0.));
#121692=CARTESIAN_POINT('Ctrl Pts',(61.6975258424894,-37.4568127726773,
0.));
#121693=CARTESIAN_POINT('Ctrl Pts',(61.6824166048444,-37.4377373317451,
0.));
#121694=CARTESIAN_POINT('Ctrl Pts',(61.6673147747242,-37.4187091808321,
0.));
#121695=CARTESIAN_POINT('Ctrl Pts',(61.6522204710131,-37.3997283738533,
0.));
#121696=CARTESIAN_POINT('Ctrl Pts',(61.637133813121,-37.3807949648624,0.));
#121697=CARTESIAN_POINT('Ctrl Pts',(61.6220549209866,-37.361909008045,0.));
#121698=CARTESIAN_POINT('Ctrl Pts',(61.6069839150807,-37.343070557718,0.));
#121699=CARTESIAN_POINT('Ctrl Pts',(61.591920916412,-37.3242796683395,0.));
#121700=CARTESIAN_POINT('Ctrl Pts',(61.5768660465311,-37.3055363945108,
0.));
#121701=CARTESIAN_POINT('Ctrl Pts',(61.5618194275348,-37.2868407909771,
0.));
#121702=CARTESIAN_POINT('Ctrl Pts',(61.5467811820691,-37.2681929126221,
0.));
#121703=CARTESIAN_POINT('Ctrl Pts',(61.5317514333328,-37.2495928144667,
0.));
#121704=CARTESIAN_POINT('Ctrl Pts',(61.5167303050832,-37.2310405516781,
0.));
#121705=CARTESIAN_POINT('Ctrl Pts',(61.501717921641,-37.2125361795731,0.));
#121706=CARTESIAN_POINT('Ctrl Pts',(61.4867144078936,-37.1940797536181,
0.));
#121707=CARTESIAN_POINT('Ctrl Pts',(61.4717198892994,-37.175671329424,0.));
#121708=CARTESIAN_POINT('Ctrl Pts',(61.4567344918919,-37.1573109627454,
0.));
#121709=CARTESIAN_POINT('Ctrl Pts',(61.4417583422863,-37.1389987094905,
0.));
#121710=CARTESIAN_POINT('Ctrl Pts',(61.4267915676822,-37.1207346257222,
0.));
#121711=CARTESIAN_POINT('Ctrl Pts',(61.4118342958697,-37.1025187676602,
0.));
#121712=CARTESIAN_POINT('Ctrl Pts',(61.3968866552317,-37.0843511916745,
0.));
#121713=CARTESIAN_POINT('Ctrl Pts',(61.381948774749,-37.0662319542849,0.));
#121714=CARTESIAN_POINT('Ctrl Pts',(61.3670207840068,-37.0481611121717,
0.));
#121715=CARTESIAN_POINT('Ctrl Pts',(61.3521028132003,-37.0301387221774,
0.));
#121716=CARTESIAN_POINT('Ctrl Pts',(61.3371949931387,-37.0121648413082,
0.));
#121717=CARTESIAN_POINT('Ctrl Pts',(61.3222974552486,-36.994239526727,0.));
#121718=CARTESIAN_POINT('Ctrl Pts',(61.3074103315791,-36.9763628357544,
0.));
#121719=CARTESIAN_POINT('Ctrl Pts',(61.2925337548077,-36.9585348258776,
0.));
#121720=CARTESIAN_POINT('Ctrl Pts',(61.2776678582461,-36.9407555547535,
0.));
#121721=CARTESIAN_POINT('Ctrl Pts',(61.2628127758457,-36.9230250802088,
0.));
#121722=CARTESIAN_POINT('Ctrl Pts',(61.247968642201,-36.9053434602343,0.));
#121723=CARTESIAN_POINT('Ctrl Pts',(61.2331355925547,-36.8877107529865,
0.));
#121724=CARTESIAN_POINT('Ctrl Pts',(61.2183137628056,-36.8701270167969,
0.));
#121725=CARTESIAN_POINT('Ctrl Pts',(61.2035032895127,-36.852592310174,0.));
#121726=CARTESIAN_POINT('Ctrl Pts',(61.1887043099014,-36.8351066918036,
0.));
#121727=CARTESIAN_POINT('Ctrl Pts',(61.1739169618666,-36.8176702205423,
0.));
#121728=CARTESIAN_POINT('Ctrl Pts',(61.1591413839787,-36.8002829554209,
0.));
#121729=CARTESIAN_POINT('Ctrl Pts',(61.1443777154911,-36.7829449556532,
0.));
#121730=CARTESIAN_POINT('Ctrl Pts',(61.1296260963466,-36.765656280638,0.));
#121731=CARTESIAN_POINT('Ctrl Pts',(61.1148866671829,-36.7484169899596,
0.));
#121732=CARTESIAN_POINT('Ctrl Pts',(61.100159569337,-36.7312271433807,0.));
#121733=CARTESIAN_POINT('Ctrl Pts',(61.0854449448524,-36.7140868008486,
0.));
#121734=CARTESIAN_POINT('Ctrl Pts',(61.0707429364847,-36.6969960225022,
0.));
#121735=CARTESIAN_POINT('Ctrl Pts',(61.0560536877083,-36.679954868674,0.));
#121736=CARTESIAN_POINT('Ctrl Pts',(61.0413773427203,-36.6629633998886,
0.));
#121737=CARTESIAN_POINT('Ctrl Pts',(61.0267140464432,-36.6460216768553,
0.));
#121738=CARTESIAN_POINT('Ctrl Pts',(61.0120639445349,-36.6291297604776,
0.));
#121739=CARTESIAN_POINT('Ctrl Pts',(60.9974271833981,-36.61228771186,0.));
#121740=CARTESIAN_POINT('Ctrl Pts',(60.9828039101887,-36.5954955923109,
0.));
#121741=CARTESIAN_POINT('Ctrl Pts',(60.9681942728236,-36.5787534633416,
0.));
#121742=CARTESIAN_POINT('Ctrl Pts',(60.9535984199873,-36.5620613866615,
0.));
#121743=CARTESIAN_POINT('Ctrl Pts',(60.9390165011355,-36.5454194241865,
0.));
#121744=CARTESIAN_POINT('Ctrl Pts',(60.9244486664987,-36.5288276380416,
0.));
#121745=CARTESIAN_POINT('Ctrl Pts',(60.9098950670847,-36.5122860905612,
0.));
#121746=CARTESIAN_POINT('Ctrl Pts',(60.8953558546795,-36.4957948442835,
0.));
#121747=CARTESIAN_POINT('Ctrl Pts',(60.8808311818499,-36.4793539619466,
0.));
#121748=CARTESIAN_POINT('Ctrl Pts',(60.8663212019657,-36.4629635065045,
0.));
#121749=CARTESIAN_POINT('Ctrl Pts',(60.8518260692188,-36.4466235411358,
0.));
#121750=CARTESIAN_POINT('Ctrl Pts',(60.8373459386392,-36.4303341292494,
0.));
#121751=CARTESIAN_POINT('Ctrl Pts',(60.822880966116,-36.4140953344859,0.));
#121752=CARTESIAN_POINT('Ctrl Pts',(60.8084313083984,-36.397907220716,0.));
#121753=CARTESIAN_POINT('Ctrl Pts',(60.793997123076,-36.3817698520388,0.));
#121754=CARTESIAN_POINT('Ctrl Pts',(60.7795785685625,-36.365683292773,0.));
#121755=CARTESIAN_POINT('Ctrl Pts',(60.7651758040803,-36.3496476074488,
0.));
#121756=CARTESIAN_POINT('Ctrl Pts',(60.7507889896308,-36.3336628607859,
0.));
#121757=CARTESIAN_POINT('Ctrl Pts',(60.7364182860412,-36.3177291177163,
0.));
#121758=CARTESIAN_POINT('Ctrl Pts',(60.722063855041,-36.3018464434214,0.));
#121759=CARTESIAN_POINT('Ctrl Pts',(60.7077258593268,-36.2860149033587,
0.));
#121760=CARTESIAN_POINT('Ctrl Pts',(60.6934044626291,-36.2702345632875,
0.));
#121761=CARTESIAN_POINT('Ctrl Pts',(60.67909982978,-36.2545054892897,0.));
#121762=CARTESIAN_POINT('Ctrl Pts',(60.6648121265885,-36.2388277477212,
0.));
#121763=CARTESIAN_POINT('Ctrl Pts',(60.6505415197042,-36.2232014051541,
0.));
#121764=CARTESIAN_POINT('Ctrl Pts',(60.6362881765019,-36.2076265283264,
0.));
#121765=CARTESIAN_POINT('Ctrl Pts',(60.6220522649149,-36.192103184063,0.));
#121766=CARTESIAN_POINT('Ctrl Pts',(60.6078339534181,-36.1766314392641,
0.));
#121767=CARTESIAN_POINT('Ctrl Pts',(60.5936334114108,-36.1612113610773,
0.));
#121768=CARTESIAN_POINT('Ctrl Pts',(60.5794508095564,-36.1458430170431,
0.));
#121769=CARTESIAN_POINT('Ctrl Pts',(60.565286320072,-36.1305264752188,0.));
#121770=CARTESIAN_POINT('Ctrl Pts',(60.5511401171984,-36.1152618043739,
0.));
#121771=CARTESIAN_POINT('Ctrl Pts',(60.5370123768804,-36.1000490738511,
0.));
#121772=CARTESIAN_POINT('Ctrl Pts',(60.5229032758973,-36.0848883531952,
0.));
#121773=CARTESIAN_POINT('Ctrl Pts',(60.5088129911354,-36.0697797118376,
0.));
#121774=CARTESIAN_POINT('Ctrl Pts',(60.4947416988422,-36.0547232187698,
0.));
#121775=CARTESIAN_POINT('Ctrl Pts',(60.4806895737686,-36.0397189421644,
0.));
#121776=CARTESIAN_POINT('Ctrl Pts',(60.4666567908093,-36.0247669500892,
0.));
#121777=CARTESIAN_POINT('Ctrl Pts',(60.4526435269662,-36.009867311357,0.));
#121778=CARTESIAN_POINT('Ctrl Pts',(60.4386499629481,-35.995020096217,0.));
#121779=CARTESIAN_POINT('Ctrl Pts',(60.4246762854926,-35.9802253773515,
0.));
#121780=CARTESIAN_POINT('Ctrl Pts',(60.4107226875714,-35.9654832299601,
0.));
#121781=CARTESIAN_POINT('Ctrl Pts',(60.3967893635452,-35.9507937296707,
0.));
#121782=CARTESIAN_POINT('Ctrl Pts',(60.3828765049019,-35.936156950695,0.));
#121783=CARTESIAN_POINT('Ctrl Pts',(60.3689842965481,-35.9215729642231,
0.));
#121784=CARTESIAN_POINT('Ctrl Pts',(60.3551129108845,-35.907041835853,0.));
#121785=CARTESIAN_POINT('Ctrl Pts',(60.3412625135287,-35.8925636280668,
0.));
#121786=CARTESIAN_POINT('Ctrl Pts',(60.327433274683,-35.8781384051537,0.));
#121787=CARTESIAN_POINT('Ctrl Pts',(60.3136253782809,-35.8637662371635,
0.));
#121788=CARTESIAN_POINT('Ctrl Pts',(60.2998390330102,-35.8494472046746,
0.));
#121789=CARTESIAN_POINT('Ctrl Pts',(60.2860744798436,-35.8351814020357,
0.));
#121790=CARTESIAN_POINT('Ctrl Pts',(60.2723319687369,-35.8209689272501,
0.));
#121791=CARTESIAN_POINT('Ctrl Pts',(60.2586117365205,-35.8068098723347,
0.));
#121792=CARTESIAN_POINT('Ctrl Pts',(60.2449139865274,-35.7927043145201,
0.));
#121793=CARTESIAN_POINT('Ctrl Pts',(60.2312388621529,-35.7786523045912,
0.));
#121794=CARTESIAN_POINT('Ctrl Pts',(60.2175864450043,-35.7646538667493,
0.));
#121795=CARTESIAN_POINT('Ctrl Pts',(60.206682708692,-35.7534979802053,0.));
#121796=CARTESIAN_POINT('Ctrl Pts',(60.1985151474623,-35.7451551752572,
0.));
#121797=CARTESIAN_POINT('Ctrl Pts',(60.193074658032,-35.7396040204017,0.));
#121798=CARTESIAN_POINT('Ctrl Pts',(60.1903555511633,-35.736831121751,0.));
#121799=CARTESIAN_POINT('Ctrl Pts',(59.483083043136,-44.8554660179045,0.));
#121800=CARTESIAN_POINT('Ctrl Pts',(59.483083043136,-44.8554660179045,12.));
#121801=CARTESIAN_POINT('Ctrl Pts',(59.4804358983083,-44.8505359826461,
0.));
#121802=CARTESIAN_POINT('Ctrl Pts',(59.4804358983083,-44.8505359826461,
12.));
#121803=CARTESIAN_POINT('Ctrl Pts',(59.4751410547732,-44.8406801497742,
0.));
#121804=CARTESIAN_POINT('Ctrl Pts',(59.4751410547732,-44.8406801497742,
12.));
#121805=CARTESIAN_POINT('Ctrl Pts',(59.4671971278321,-44.8259091134016,
0.));
#121806=CARTESIAN_POINT('Ctrl Pts',(59.4671971278321,-44.8259091134016,
12.));
#121807=CARTESIAN_POINT('Ctrl Pts',(59.4566019018253,-44.8062398251406,
0.));
#121808=CARTESIAN_POINT('Ctrl Pts',(59.4566019018253,-44.8062398251406,
12.));
#121809=CARTESIAN_POINT('Ctrl Pts',(59.4433523335147,-44.7816956017528,
0.));
#121810=CARTESIAN_POINT('Ctrl Pts',(59.4433523335147,-44.7816956017528,
12.));
#121811=CARTESIAN_POINT('Ctrl Pts',(59.430097240324,-44.7571937812113,0.));
#121812=CARTESIAN_POINT('Ctrl Pts',(59.430097240324,-44.7571937812113,12.));
#121813=CARTESIAN_POINT('Ctrl Pts',(59.4168366453118,-44.7327343876391,
0.));
#121814=CARTESIAN_POINT('Ctrl Pts',(59.4168366453118,-44.7327343876391,
12.));
#121815=CARTESIAN_POINT('Ctrl Pts',(59.4035705873811,-44.7083174541702,
0.));
#121816=CARTESIAN_POINT('Ctrl Pts',(59.4035705873811,-44.7083174541702,
12.));
#121817=CARTESIAN_POINT('Ctrl Pts',(59.3902991267889,-44.683943024421,0.));
#121818=CARTESIAN_POINT('Ctrl Pts',(59.3902991267889,-44.683943024421,12.));
#121819=CARTESIAN_POINT('Ctrl Pts',(59.377022343519,-44.6596111512687,0.));
#121820=CARTESIAN_POINT('Ctrl Pts',(59.377022343519,-44.6596111512687,12.));
#121821=CARTESIAN_POINT('Ctrl Pts',(59.36374033018,-44.6353218935685,0.));
#121822=CARTESIAN_POINT('Ctrl Pts',(59.36374033018,-44.6353218935685,12.));
#121823=CARTESIAN_POINT('Ctrl Pts',(59.3504531864154,-44.6110753134277,
0.));
#121824=CARTESIAN_POINT('Ctrl Pts',(59.3504531864154,-44.6110753134277,
12.));
#121825=CARTESIAN_POINT('Ctrl Pts',(59.3371610128511,-44.5868714733234,
0.));
#121826=CARTESIAN_POINT('Ctrl Pts',(59.3371610128511,-44.5868714733234,
12.));
#121827=CARTESIAN_POINT('Ctrl Pts',(59.3238639048694,-44.5627104331017,
0.));
#121828=CARTESIAN_POINT('Ctrl Pts',(59.3238639048694,-44.5627104331017,
12.));
#121829=CARTESIAN_POINT('Ctrl Pts',(59.3105619475609,-44.5385922475573,
0.));
#121830=CARTESIAN_POINT('Ctrl Pts',(59.3105619475609,-44.5385922475573,
12.));
#121831=CARTESIAN_POINT('Ctrl Pts',(59.2972552192156,-44.5145169681349,
0.));
#121832=CARTESIAN_POINT('Ctrl Pts',(59.2972552192156,-44.5145169681349,
12.));
#121833=CARTESIAN_POINT('Ctrl Pts',(59.2839437938237,-44.490484644151,0.));
#121834=CARTESIAN_POINT('Ctrl Pts',(59.2839437938237,-44.490484644151,12.));
#121835=CARTESIAN_POINT('Ctrl Pts',(59.2706277440445,-44.4664953242379,
0.));
#121836=CARTESIAN_POINT('Ctrl Pts',(59.2706277440445,-44.4664953242379,
12.));
#121837=CARTESIAN_POINT('Ctrl Pts',(59.2573071437774,-44.4425490575911,
0.));
#121838=CARTESIAN_POINT('Ctrl Pts',(59.2573071437774,-44.4425490575911,
12.));
#121839=CARTESIAN_POINT('Ctrl Pts',(59.2439820714187,-44.4186458955451,
0.));
#121840=CARTESIAN_POINT('Ctrl Pts',(59.2439820714187,-44.4186458955451,
12.));
#121841=CARTESIAN_POINT('Ctrl Pts',(59.2306526095131,-44.3947858914074,
0.));
#121842=CARTESIAN_POINT('Ctrl Pts',(59.2306526095131,-44.3947858914074,
12.));
#121843=CARTESIAN_POINT('Ctrl Pts',(59.2173188432798,-44.370969099747,0.));
#121844=CARTESIAN_POINT('Ctrl Pts',(59.2173188432798,-44.370969099747,12.));
#121845=CARTESIAN_POINT('Ctrl Pts',(59.2039808594752,-44.3471955758403,
0.));
#121846=CARTESIAN_POINT('Ctrl Pts',(59.2039808594752,-44.3471955758403,
12.));
#121847=CARTESIAN_POINT('Ctrl Pts',(59.1906387451979,-44.3234653750884,
0.));
#121848=CARTESIAN_POINT('Ctrl Pts',(59.1906387451979,-44.3234653750884,
12.));
#121849=CARTESIAN_POINT('Ctrl Pts',(59.1772925865213,-44.2997785523431,
0.));
#121850=CARTESIAN_POINT('Ctrl Pts',(59.1772925865213,-44.2997785523431,
12.));
#121851=CARTESIAN_POINT('Ctrl Pts',(59.1639424678793,-44.2761351616048,
0.));
#121852=CARTESIAN_POINT('Ctrl Pts',(59.1639424678793,-44.2761351616048,
12.));
#121853=CARTESIAN_POINT('Ctrl Pts',(59.1505884728215,-44.2525352563996,
0.));
#121854=CARTESIAN_POINT('Ctrl Pts',(59.1505884728215,-44.2525352563996,
12.));
#121855=CARTESIAN_POINT('Ctrl Pts',(59.1372306844585,-44.228978889997,0.));
#121856=CARTESIAN_POINT('Ctrl Pts',(59.1372306844585,-44.228978889997,12.));
#121857=CARTESIAN_POINT('Ctrl Pts',(59.1238691860306,-44.2054661156875,
0.));
#121858=CARTESIAN_POINT('Ctrl Pts',(59.1238691860306,-44.2054661156875,
12.));
#121859=CARTESIAN_POINT('Ctrl Pts',(59.1105040614275,-44.1819969870307,
0.));
#121860=CARTESIAN_POINT('Ctrl Pts',(59.1105040614275,-44.1819969870307,
12.));
#121861=CARTESIAN_POINT('Ctrl Pts',(59.0971353957206,-44.1585715581065,
0.));
#121862=CARTESIAN_POINT('Ctrl Pts',(59.0971353957206,-44.1585715581065,
12.));
#121863=CARTESIAN_POINT('Ctrl Pts',(59.08376327492,-44.1351898834051,0.));
#121864=CARTESIAN_POINT('Ctrl Pts',(59.08376327492,-44.1351898834051,12.));
#121865=CARTESIAN_POINT('Ctrl Pts',(59.0703877857525,-44.1118520177221,
0.));
#121866=CARTESIAN_POINT('Ctrl Pts',(59.0703877857525,-44.1118520177221,
12.));
#121867=CARTESIAN_POINT('Ctrl Pts',(59.0570090154242,-44.0885580160433,
0.));
#121868=CARTESIAN_POINT('Ctrl Pts',(59.0570090154242,-44.0885580160433,
12.));
#121869=CARTESIAN_POINT('Ctrl Pts',(59.0436270514086,-44.0653079334385,
0.));
#121870=CARTESIAN_POINT('Ctrl Pts',(59.0436270514086,-44.0653079334385,
12.));
#121871=CARTESIAN_POINT('Ctrl Pts',(59.0302419811777,-44.0421018249223,
0.));
#121872=CARTESIAN_POINT('Ctrl Pts',(59.0302419811777,-44.0421018249223,
12.));
#121873=CARTESIAN_POINT('Ctrl Pts',(59.0168538922095,-44.0189397454599,
0.));
#121874=CARTESIAN_POINT('Ctrl Pts',(59.0168538922095,-44.0189397454599,
12.));
#121875=CARTESIAN_POINT('Ctrl Pts',(59.0034628721167,-43.9958217500369,
0.));
#121876=CARTESIAN_POINT('Ctrl Pts',(59.0034628721167,-43.9958217500369,
12.));
#121877=CARTESIAN_POINT('Ctrl Pts',(58.9900690087408,-43.9727478937056,
0.));
#121878=CARTESIAN_POINT('Ctrl Pts',(58.9900690087408,-43.9727478937056,
12.));
#121879=CARTESIAN_POINT('Ctrl Pts',(58.9766723902529,-43.9497182316331,
0.));
#121880=CARTESIAN_POINT('Ctrl Pts',(58.9766723902529,-43.9497182316331,
12.));
#121881=CARTESIAN_POINT('Ctrl Pts',(58.9632731052696,-43.9267328191501,
0.));
#121882=CARTESIAN_POINT('Ctrl Pts',(58.9632731052696,-43.9267328191501,
12.));
#121883=CARTESIAN_POINT('Ctrl Pts',(58.9498712429054,-43.9037917117739,
0.));
#121884=CARTESIAN_POINT('Ctrl Pts',(58.9498712429054,-43.9037917117739,
12.));
#121885=CARTESIAN_POINT('Ctrl Pts',(58.936466892712,-43.8808949651873,0.));
#121886=CARTESIAN_POINT('Ctrl Pts',(58.936466892712,-43.8808949651873,12.));
#121887=CARTESIAN_POINT('Ctrl Pts',(58.9230601446436,-43.858042635223,0.));
#121888=CARTESIAN_POINT('Ctrl Pts',(58.9230601446436,-43.858042635223,12.));
#121889=CARTESIAN_POINT('Ctrl Pts',(58.9096510890129,-43.835234777842,0.));
#121890=CARTESIAN_POINT('Ctrl Pts',(58.9096510890129,-43.835234777842,12.));
#121891=CARTESIAN_POINT('Ctrl Pts',(58.8962398164493,-43.8124714491077,
0.));
#121892=CARTESIAN_POINT('Ctrl Pts',(58.8962398164493,-43.8124714491077,
12.));
#121893=CARTESIAN_POINT('Ctrl Pts',(58.8828264178621,-43.7897527051609,
0.));
#121894=CARTESIAN_POINT('Ctrl Pts',(58.8828264178621,-43.7897527051609,
12.));
#121895=CARTESIAN_POINT('Ctrl Pts',(58.8694109844647,-43.7670786022402,
0.));
#121896=CARTESIAN_POINT('Ctrl Pts',(58.8694109844647,-43.7670786022402,
12.));
#121897=CARTESIAN_POINT('Ctrl Pts',(58.855993607794,-43.7444491966942,0.));
#121898=CARTESIAN_POINT('Ctrl Pts',(58.855993607794,-43.7444491966942,12.));
#121899=CARTESIAN_POINT('Ctrl Pts',(58.8425743797326,-43.7218645449922,
0.));
#121900=CARTESIAN_POINT('Ctrl Pts',(58.8425743797326,-43.7218645449922,
12.));
#121901=CARTESIAN_POINT('Ctrl Pts',(58.8291533925293,-43.6993247037314,
0.));
#121902=CARTESIAN_POINT('Ctrl Pts',(58.8291533925293,-43.6993247037314,
12.));
#121903=CARTESIAN_POINT('Ctrl Pts',(58.8157307388238,-43.6768297296395,
0.));
#121904=CARTESIAN_POINT('Ctrl Pts',(58.8157307388238,-43.6768297296395,
12.));
#121905=CARTESIAN_POINT('Ctrl Pts',(58.8023065116436,-43.6543796795789,
0.));
#121906=CARTESIAN_POINT('Ctrl Pts',(58.8023065116436,-43.6543796795789,
12.));
#121907=CARTESIAN_POINT('Ctrl Pts',(58.788880804397,-43.6319746105482,0.));
#121908=CARTESIAN_POINT('Ctrl Pts',(58.788880804397,-43.6319746105482,12.));
#121909=CARTESIAN_POINT('Ctrl Pts',(58.775453710867,-43.6096145796797,0.));
#121910=CARTESIAN_POINT('Ctrl Pts',(58.775453710867,-43.6096145796797,12.));
#121911=CARTESIAN_POINT('Ctrl Pts',(58.7620253252062,-43.5872996442345,
0.));
#121912=CARTESIAN_POINT('Ctrl Pts',(58.7620253252062,-43.5872996442345,
12.));
#121913=CARTESIAN_POINT('Ctrl Pts',(58.74859574193,-43.5650298615917,0.));
#121914=CARTESIAN_POINT('Ctrl Pts',(58.74859574193,-43.5650298615917,12.));
#121915=CARTESIAN_POINT('Ctrl Pts',(58.735165055918,-43.5428052892488,0.));
#121916=CARTESIAN_POINT('Ctrl Pts',(58.735165055918,-43.5428052892488,12.));
#121917=CARTESIAN_POINT('Ctrl Pts',(58.7217333624209,-43.5206259848338,
0.));
#121918=CARTESIAN_POINT('Ctrl Pts',(58.7217333624209,-43.5206259848338,
12.));
#121919=CARTESIAN_POINT('Ctrl Pts',(58.7083007570661,-43.4984920061073,
0.));
#121920=CARTESIAN_POINT('Ctrl Pts',(58.7083007570661,-43.4984920061073,
12.));
#121921=CARTESIAN_POINT('Ctrl Pts',(58.6948673358638,-43.4764034109654,
0.));
#121922=CARTESIAN_POINT('Ctrl Pts',(58.6948673358638,-43.4764034109654,
12.));
#121923=CARTESIAN_POINT('Ctrl Pts',(58.6814331952138,-43.4543602574351,
0.));
#121924=CARTESIAN_POINT('Ctrl Pts',(58.6814331952138,-43.4543602574351,
12.));
#121925=CARTESIAN_POINT('Ctrl Pts',(58.6679984319097,-43.4323626036737,
0.));
#121926=CARTESIAN_POINT('Ctrl Pts',(58.6679984319097,-43.4323626036737,
12.));
#121927=CARTESIAN_POINT('Ctrl Pts',(58.6545631431393,-43.4104105079768,
0.));
#121928=CARTESIAN_POINT('Ctrl Pts',(58.6545631431393,-43.4104105079768,
12.));
#121929=CARTESIAN_POINT('Ctrl Pts',(58.6411274264857,-43.388504028781,0.));
#121930=CARTESIAN_POINT('Ctrl Pts',(58.6411274264857,-43.388504028781,12.));
#121931=CARTESIAN_POINT('Ctrl Pts',(58.627691379929,-43.3666432246635,0.));
#121932=CARTESIAN_POINT('Ctrl Pts',(58.627691379929,-43.3666432246635,12.));
#121933=CARTESIAN_POINT('Ctrl Pts',(58.6142551018467,-43.3448281543372,
0.));
#121934=CARTESIAN_POINT('Ctrl Pts',(58.6142551018467,-43.3448281543372,
12.));
#121935=CARTESIAN_POINT('Ctrl Pts',(58.6008186910156,-43.3230588766449,
0.));
#121936=CARTESIAN_POINT('Ctrl Pts',(58.6008186910156,-43.3230588766449,
12.));
#121937=CARTESIAN_POINT('Ctrl Pts',(58.5873822466152,-43.3013354505701,
0.));
#121938=CARTESIAN_POINT('Ctrl Pts',(58.5873822466152,-43.3013354505701,
12.));
#121939=CARTESIAN_POINT('Ctrl Pts',(58.573945868231,-43.2796579352401,0.));
#121940=CARTESIAN_POINT('Ctrl Pts',(58.573945868231,-43.2796579352401,12.));
#121941=CARTESIAN_POINT('Ctrl Pts',(58.5605096558578,-43.2580263899278,
0.));
#121942=CARTESIAN_POINT('Ctrl Pts',(58.5605096558578,-43.2580263899278,
12.));
#121943=CARTESIAN_POINT('Ctrl Pts',(58.5470737099032,-43.2364408740493,
0.));
#121944=CARTESIAN_POINT('Ctrl Pts',(58.5470737099032,-43.2364408740493,
12.));
#121945=CARTESIAN_POINT('Ctrl Pts',(58.5336381311917,-43.2149014471574,
0.));
#121946=CARTESIAN_POINT('Ctrl Pts',(58.5336381311917,-43.2149014471574,
12.));
#121947=CARTESIAN_POINT('Ctrl Pts',(58.5202030209669,-43.1934081689505,
0.));
#121948=CARTESIAN_POINT('Ctrl Pts',(58.5202030209669,-43.1934081689505,
12.));
#121949=CARTESIAN_POINT('Ctrl Pts',(58.5067684808944,-43.1719610992771,
0.));
#121950=CARTESIAN_POINT('Ctrl Pts',(58.5067684808944,-43.1719610992771,
12.));
#121951=CARTESIAN_POINT('Ctrl Pts',(58.4933346130636,-43.1505602981365,
0.));
#121952=CARTESIAN_POINT('Ctrl Pts',(58.4933346130636,-43.1505602981365,
12.));
#121953=CARTESIAN_POINT('Ctrl Pts',(58.4799015199907,-43.1292058256777,
0.));
#121954=CARTESIAN_POINT('Ctrl Pts',(58.4799015199907,-43.1292058256777,
12.));
#121955=CARTESIAN_POINT('Ctrl Pts',(58.4664693046217,-43.1078977421916,
0.));
#121956=CARTESIAN_POINT('Ctrl Pts',(58.4664693046217,-43.1078977421916,
12.));
#121957=CARTESIAN_POINT('Ctrl Pts',(58.4530380703348,-43.0866361081177,
0.));
#121958=CARTESIAN_POINT('Ctrl Pts',(58.4530380703348,-43.0866361081177,
12.));
#121959=CARTESIAN_POINT('Ctrl Pts',(58.439607920945,-43.0654209840511,0.));
#121960=CARTESIAN_POINT('Ctrl Pts',(58.439607920945,-43.0654209840511,12.));
#121961=CARTESIAN_POINT('Ctrl Pts',(58.4261789607058,-43.0442524307434,
0.));
#121962=CARTESIAN_POINT('Ctrl Pts',(58.4261789607058,-43.0442524307434,
12.));
#121963=CARTESIAN_POINT('Ctrl Pts',(58.4127512943136,-43.0231305091027,
0.));
#121964=CARTESIAN_POINT('Ctrl Pts',(58.4127512943136,-43.0231305091027,
12.));
#121965=CARTESIAN_POINT('Ctrl Pts',(58.3993250269101,-43.0020552801859,
0.));
#121966=CARTESIAN_POINT('Ctrl Pts',(58.3993250269101,-43.0020552801859,
12.));
#121967=CARTESIAN_POINT('Ctrl Pts',(58.3859002640856,-42.9810268052032,
0.));
#121968=CARTESIAN_POINT('Ctrl Pts',(58.3859002640856,-42.9810268052032,
12.));
#121969=CARTESIAN_POINT('Ctrl Pts',(58.3724771118826,-42.960045145526,0.));
#121970=CARTESIAN_POINT('Ctrl Pts',(58.3724771118826,-42.960045145526,12.));
#121971=CARTESIAN_POINT('Ctrl Pts',(58.3590556767978,-42.9391103626879,
0.));
#121972=CARTESIAN_POINT('Ctrl Pts',(58.3590556767978,-42.9391103626879,
12.));
#121973=CARTESIAN_POINT('Ctrl Pts',(58.3456360657865,-42.9182225183855,
0.));
#121974=CARTESIAN_POINT('Ctrl Pts',(58.3456360657865,-42.9182225183855,
12.));
#121975=CARTESIAN_POINT('Ctrl Pts',(58.3322183862654,-42.8973816744709,
0.));
#121976=CARTESIAN_POINT('Ctrl Pts',(58.3322183862654,-42.8973816744709,
12.));
#121977=CARTESIAN_POINT('Ctrl Pts',(58.3188027461164,-42.8765878929551,
0.));
#121978=CARTESIAN_POINT('Ctrl Pts',(58.3188027461164,-42.8765878929551,
12.));
#121979=CARTESIAN_POINT('Ctrl Pts',(58.3053892536894,-42.8558412360158,
0.));
#121980=CARTESIAN_POINT('Ctrl Pts',(58.3053892536894,-42.8558412360158,
12.));
#121981=CARTESIAN_POINT('Ctrl Pts',(58.2919780178064,-42.8351417659999,
0.));
#121982=CARTESIAN_POINT('Ctrl Pts',(58.2919780178064,-42.8351417659999,
12.));
#121983=CARTESIAN_POINT('Ctrl Pts',(58.2785691477638,-42.8144895454233,
0.));
#121984=CARTESIAN_POINT('Ctrl Pts',(58.2785691477638,-42.8144895454233,
12.));
#121985=CARTESIAN_POINT('Ctrl Pts',(58.2651627533368,-42.7938846369651,
0.));
#121986=CARTESIAN_POINT('Ctrl Pts',(58.2651627533368,-42.7938846369651,
12.));
#121987=CARTESIAN_POINT('Ctrl Pts',(58.251758944782,-42.773327103468,0.));
#121988=CARTESIAN_POINT('Ctrl Pts',(58.251758944782,-42.773327103468,12.));
#121989=CARTESIAN_POINT('Ctrl Pts',(58.2383578328424,-42.7528170079485,
0.));
#121990=CARTESIAN_POINT('Ctrl Pts',(58.2383578328424,-42.7528170079485,
12.));
#121991=CARTESIAN_POINT('Ctrl Pts',(58.22495952875,-42.7323544135985,0.));
#121992=CARTESIAN_POINT('Ctrl Pts',(58.22495952875,-42.7323544135985,12.));
#121993=CARTESIAN_POINT('Ctrl Pts',(58.21156414423,-42.7119393837866,0.));
#121994=CARTESIAN_POINT('Ctrl Pts',(58.21156414423,-42.7119393837866,12.));
#121995=CARTESIAN_POINT('Ctrl Pts',(58.1981717915037,-42.6915719820513,
0.));
#121996=CARTESIAN_POINT('Ctrl Pts',(58.1981717915037,-42.6915719820513,
12.));
#121997=CARTESIAN_POINT('Ctrl Pts',(58.1847825832923,-42.6712522721016,
0.));
#121998=CARTESIAN_POINT('Ctrl Pts',(58.1847825832923,-42.6712522721016,
12.));
#121999=CARTESIAN_POINT('Ctrl Pts',(58.171396632821,-42.6509803178265,0.));
#122000=CARTESIAN_POINT('Ctrl Pts',(58.171396632821,-42.6509803178265,12.));
#122001=CARTESIAN_POINT('Ctrl Pts',(58.1580140538228,-42.6307561832976,
0.));
#122002=CARTESIAN_POINT('Ctrl Pts',(58.1580140538228,-42.6307561832976,
12.));
#122003=CARTESIAN_POINT('Ctrl Pts',(58.1446349605421,-42.6105799327699,
0.));
#122004=CARTESIAN_POINT('Ctrl Pts',(58.1446349605421,-42.6105799327699,
12.));
#122005=CARTESIAN_POINT('Ctrl Pts',(58.1312594677386,-42.5904516306762,
0.));
#122006=CARTESIAN_POINT('Ctrl Pts',(58.1312594677386,-42.5904516306762,
12.));
#122007=CARTESIAN_POINT('Ctrl Pts',(58.1178876906907,-42.5703713416265,
0.));
#122008=CARTESIAN_POINT('Ctrl Pts',(58.1178876906907,-42.5703713416265,
12.));
#122009=CARTESIAN_POINT('Ctrl Pts',(58.1045197452002,-42.5503391304183,
0.));
#122010=CARTESIAN_POINT('Ctrl Pts',(58.1045197452002,-42.5503391304183,
12.));
#122011=CARTESIAN_POINT('Ctrl Pts',(58.0911557475965,-42.5303550620387,
0.));
#122012=CARTESIAN_POINT('Ctrl Pts',(58.0911557475965,-42.5303550620387,
12.));
#122013=CARTESIAN_POINT('Ctrl Pts',(58.0777958147403,-42.5104192016664,
0.));
#122014=CARTESIAN_POINT('Ctrl Pts',(58.0777958147403,-42.5104192016664,
12.));
#122015=CARTESIAN_POINT('Ctrl Pts',(58.0644400640275,-42.4905316146654,
0.));
#122016=CARTESIAN_POINT('Ctrl Pts',(58.0644400640275,-42.4905316146654,
12.));
#122017=CARTESIAN_POINT('Ctrl Pts',(58.0510886133926,-42.4706923665845,
0.));
#122018=CARTESIAN_POINT('Ctrl Pts',(58.0510886133926,-42.4706923665845,
12.));
#122019=CARTESIAN_POINT('Ctrl Pts',(58.037741581314,-42.4509015231674,0.));
#122020=CARTESIAN_POINT('Ctrl Pts',(58.037741581314,-42.4509015231674,12.));
#122021=CARTESIAN_POINT('Ctrl Pts',(58.0243990868181,-42.4311591503555,
0.));
#122022=CARTESIAN_POINT('Ctrl Pts',(58.0243990868181,-42.4311591503555,
12.));
#122023=CARTESIAN_POINT('Ctrl Pts',(58.0110612494828,-42.411465314289,0.));
#122024=CARTESIAN_POINT('Ctrl Pts',(58.0110612494828,-42.411465314289,12.));
#122025=CARTESIAN_POINT('Ctrl Pts',(57.9977281894422,-42.3918200813014,
0.));
#122026=CARTESIAN_POINT('Ctrl Pts',(57.9977281894422,-42.3918200813014,
12.));
#122027=CARTESIAN_POINT('Ctrl Pts',(57.9844000273911,-42.3722235179198,
0.));
#122028=CARTESIAN_POINT('Ctrl Pts',(57.9844000273911,-42.3722235179198,
12.));
#122029=CARTESIAN_POINT('Ctrl Pts',(57.9710768845899,-42.3526756908747,
0.));
#122030=CARTESIAN_POINT('Ctrl Pts',(57.9710768845899,-42.3526756908747,
12.));
#122031=CARTESIAN_POINT('Ctrl Pts',(57.9577588828682,-42.333176667102,0.));
#122032=CARTESIAN_POINT('Ctrl Pts',(57.9577588828682,-42.333176667102,12.));
#122033=CARTESIAN_POINT('Ctrl Pts',(57.9444461446299,-42.3137265137452,
0.));
#122034=CARTESIAN_POINT('Ctrl Pts',(57.9444461446299,-42.3137265137452,
12.));
#122035=CARTESIAN_POINT('Ctrl Pts',(57.9311387928563,-42.2943252981489,
0.));
#122036=CARTESIAN_POINT('Ctrl Pts',(57.9311387928563,-42.2943252981489,
12.));
#122037=CARTESIAN_POINT('Ctrl Pts',(57.9178369511114,-42.2749730878595,
0.));
#122038=CARTESIAN_POINT('Ctrl Pts',(57.9178369511114,-42.2749730878595,
12.));
#122039=CARTESIAN_POINT('Ctrl Pts',(57.9045407435474,-42.2556699506353,
0.));
#122040=CARTESIAN_POINT('Ctrl Pts',(57.9045407435474,-42.2556699506353,
12.));
#122041=CARTESIAN_POINT('Ctrl Pts',(57.8912502949096,-42.2364159544501,
0.));
#122042=CARTESIAN_POINT('Ctrl Pts',(57.8912502949096,-42.2364159544501,
12.));
#122043=CARTESIAN_POINT('Ctrl Pts',(57.8779657305413,-42.2172111674938,
0.));
#122044=CARTESIAN_POINT('Ctrl Pts',(57.8779657305413,-42.2172111674938,
12.));
#122045=CARTESIAN_POINT('Ctrl Pts',(57.864687176387,-42.1980556581665,0.));
#122046=CARTESIAN_POINT('Ctrl Pts',(57.864687176387,-42.1980556581665,12.));
#122047=CARTESIAN_POINT('Ctrl Pts',(57.8514147589972,-42.1789494950794,
0.));
#122048=CARTESIAN_POINT('Ctrl Pts',(57.8514147589972,-42.1789494950794,
12.));
#122049=CARTESIAN_POINT('Ctrl Pts',(57.8381486055342,-42.1598927470646,
0.));
#122050=CARTESIAN_POINT('Ctrl Pts',(57.8381486055342,-42.1598927470646,
12.));
#122051=CARTESIAN_POINT('Ctrl Pts',(57.8248888437775,-42.1408854831783,
0.));
#122052=CARTESIAN_POINT('Ctrl Pts',(57.8248888437775,-42.1408854831783,
12.));
#122053=CARTESIAN_POINT('Ctrl Pts',(57.8116356021288,-42.1219277727021,
0.));
#122054=CARTESIAN_POINT('Ctrl Pts',(57.8116356021288,-42.1219277727021,
12.));
#122055=CARTESIAN_POINT('Ctrl Pts',(57.798389009616,-42.1030196851366,0.));
#122056=CARTESIAN_POINT('Ctrl Pts',(57.798389009616,-42.1030196851366,12.));
#122057=CARTESIAN_POINT('Ctrl Pts',(57.7851491958987,-42.0841612902042,
0.));
#122058=CARTESIAN_POINT('Ctrl Pts',(57.7851491958987,-42.0841612902042,
12.));
#122059=CARTESIAN_POINT('Ctrl Pts',(57.7719162912744,-42.0653526578588,
0.));
#122060=CARTESIAN_POINT('Ctrl Pts',(57.7719162912744,-42.0653526578588,
12.));
#122061=CARTESIAN_POINT('Ctrl Pts',(57.7586904266834,-42.0465938582882,
0.));
#122062=CARTESIAN_POINT('Ctrl Pts',(57.7586904266834,-42.0465938582882,
12.));
#122063=CARTESIAN_POINT('Ctrl Pts',(57.745471733714,-42.0278849619148,0.));
#122064=CARTESIAN_POINT('Ctrl Pts',(57.745471733714,-42.0278849619148,12.));
#122065=CARTESIAN_POINT('Ctrl Pts',(57.7322603446066,-42.0092260393897,
0.));
#122066=CARTESIAN_POINT('Ctrl Pts',(57.7322603446066,-42.0092260393897,
12.));
#122067=CARTESIAN_POINT('Ctrl Pts',(57.7190563922593,-41.990617161596,0.));
#122068=CARTESIAN_POINT('Ctrl Pts',(57.7190563922593,-41.990617161596,12.));
#122069=CARTESIAN_POINT('Ctrl Pts',(57.7058600102351,-41.9720583996592,
0.));
#122070=CARTESIAN_POINT('Ctrl Pts',(57.7058600102351,-41.9720583996592,
12.));
#122071=CARTESIAN_POINT('Ctrl Pts',(57.6926713327672,-41.9535498249488,
0.));
#122072=CARTESIAN_POINT('Ctrl Pts',(57.6926713327672,-41.9535498249488,
12.));
#122073=CARTESIAN_POINT('Ctrl Pts',(57.6794904947649,-41.9350915090797,
0.));
#122074=CARTESIAN_POINT('Ctrl Pts',(57.6794904947649,-41.9350915090797,
12.));
#122075=CARTESIAN_POINT('Ctrl Pts',(57.6663176318189,-41.9166835239054,
0.));
#122076=CARTESIAN_POINT('Ctrl Pts',(57.6663176318189,-41.9166835239054,
12.));
#122077=CARTESIAN_POINT('Ctrl Pts',(57.6531528802072,-41.8983259415253,
0.));
#122078=CARTESIAN_POINT('Ctrl Pts',(57.6531528802072,-41.8983259415253,
12.));
#122079=CARTESIAN_POINT('Ctrl Pts',(57.6399963769009,-41.8800188342912,
0.));
#122080=CARTESIAN_POINT('Ctrl Pts',(57.6399963769009,-41.8800188342912,
12.));
#122081=CARTESIAN_POINT('Ctrl Pts',(57.6268482595701,-41.8617622748107,
0.));
#122082=CARTESIAN_POINT('Ctrl Pts',(57.6268482595701,-41.8617622748107,
12.));
#122083=CARTESIAN_POINT('Ctrl Pts',(57.613708666588,-41.8435563359456,0.));
#122084=CARTESIAN_POINT('Ctrl Pts',(57.613708666588,-41.8435563359456,12.));
#122085=CARTESIAN_POINT('Ctrl Pts',(57.6005777370347,-41.8254010908051,
0.));
#122086=CARTESIAN_POINT('Ctrl Pts',(57.6005777370347,-41.8254010908051,
12.));
#122087=CARTESIAN_POINT('Ctrl Pts',(57.5874556107054,-41.8072966127559,
0.));
#122088=CARTESIAN_POINT('Ctrl Pts',(57.5874556107054,-41.8072966127559,
12.));
#122089=CARTESIAN_POINT('Ctrl Pts',(57.5743424281204,-41.7892429754298,
0.));
#122090=CARTESIAN_POINT('Ctrl Pts',(57.5743424281204,-41.7892429754298,
12.));
#122091=CARTESIAN_POINT('Ctrl Pts',(57.561238330532,-41.7712402527273,0.));
#122092=CARTESIAN_POINT('Ctrl Pts',(57.561238330532,-41.7712402527273,12.));
#122093=CARTESIAN_POINT('Ctrl Pts',(57.5481434599334,-41.7532885188174,
0.));
#122094=CARTESIAN_POINT('Ctrl Pts',(57.5481434599334,-41.7532885188174,
12.));
#122095=CARTESIAN_POINT('Ctrl Pts',(57.5350579590648,-41.7353878481336,
0.));
#122096=CARTESIAN_POINT('Ctrl Pts',(57.5350579590648,-41.7353878481336,
12.));
#122097=CARTESIAN_POINT('Ctrl Pts',(57.5219819714169,-41.7175383153819,
0.));
#122098=CARTESIAN_POINT('Ctrl Pts',(57.5219819714169,-41.7175383153819,
12.));
#122099=CARTESIAN_POINT('Ctrl Pts',(57.5089156412341,-41.6997399955445,
0.));
#122100=CARTESIAN_POINT('Ctrl Pts',(57.5089156412341,-41.6997399955445,
12.));
#122101=CARTESIAN_POINT('Ctrl Pts',(57.4958591135165,-41.6819929638797,
0.));
#122102=CARTESIAN_POINT('Ctrl Pts',(57.4958591135165,-41.6819929638797,
12.));
#122103=CARTESIAN_POINT('Ctrl Pts',(57.4828125340222,-41.6642972959168,
0.));
#122104=CARTESIAN_POINT('Ctrl Pts',(57.4828125340222,-41.6642972959168,
12.));
#122105=CARTESIAN_POINT('Ctrl Pts',(57.4697760492693,-41.6466530674522,
0.));
#122106=CARTESIAN_POINT('Ctrl Pts',(57.4697760492693,-41.6466530674522,
12.));
#122107=CARTESIAN_POINT('Ctrl Pts',(57.4567498065573,-41.6290603545674,
0.));
#122108=CARTESIAN_POINT('Ctrl Pts',(57.4567498065573,-41.6290603545674,
12.));
#122109=CARTESIAN_POINT('Ctrl Pts',(57.4437339539848,-41.6115192336394,
0.));
#122110=CARTESIAN_POINT('Ctrl Pts',(57.4437339539848,-41.6115192336394,
12.));
#122111=CARTESIAN_POINT('Ctrl Pts',(57.4307286404656,-41.5940297813474,
0.));
#122112=CARTESIAN_POINT('Ctrl Pts',(57.4307286404656,-41.5940297813474,
12.));
#122113=CARTESIAN_POINT('Ctrl Pts',(57.417734015749,-41.5765920746764,0.));
#122114=CARTESIAN_POINT('Ctrl Pts',(57.417734015749,-41.5765920746764,12.));
#122115=CARTESIAN_POINT('Ctrl Pts',(57.4047502304207,-41.5592061909159,
0.));
#122116=CARTESIAN_POINT('Ctrl Pts',(57.4047502304207,-41.5592061909159,
12.));
#122117=CARTESIAN_POINT('Ctrl Pts',(57.3917774358844,-41.5418722076558,
0.));
#122118=CARTESIAN_POINT('Ctrl Pts',(57.3917774358844,-41.5418722076558,
12.));
#122119=CARTESIAN_POINT('Ctrl Pts',(57.378815784345,-41.5245902027767,0.));
#122120=CARTESIAN_POINT('Ctrl Pts',(57.378815784345,-41.5245902027767,12.));
#122121=CARTESIAN_POINT('Ctrl Pts',(57.3658654287948,-41.5073602544404,
0.));
#122122=CARTESIAN_POINT('Ctrl Pts',(57.3658654287948,-41.5073602544404,
12.));
#122123=CARTESIAN_POINT('Ctrl Pts',(57.3529265229858,-41.4901824410654,
0.));
#122124=CARTESIAN_POINT('Ctrl Pts',(57.3529265229858,-41.4901824410654,
12.));
#122125=CARTESIAN_POINT('Ctrl Pts',(57.339999221474,-41.4730568413535,0.));
#122126=CARTESIAN_POINT('Ctrl Pts',(57.339999221474,-41.4730568413535,12.));
#122127=CARTESIAN_POINT('Ctrl Pts',(57.3270836796925,-41.4559835343339,
0.));
#122128=CARTESIAN_POINT('Ctrl Pts',(57.3270836796925,-41.4559835343339,
12.));
#122129=CARTESIAN_POINT('Ctrl Pts',(57.3141800540137,-41.4389625993948,
0.));
#122130=CARTESIAN_POINT('Ctrl Pts',(57.3141800540137,-41.4389625993948,
12.));
#122131=CARTESIAN_POINT('Ctrl Pts',(57.3012885018139,-41.4219941163155,
0.));
#122132=CARTESIAN_POINT('Ctrl Pts',(57.3012885018139,-41.4219941163155,
12.));
#122133=CARTESIAN_POINT('Ctrl Pts',(57.2884091815384,-41.4050781652923,
0.));
#122134=CARTESIAN_POINT('Ctrl Pts',(57.2884091815384,-41.4050781652923,
12.));
#122135=CARTESIAN_POINT('Ctrl Pts',(57.2755422525822,-41.3882148268798,
0.));
#122136=CARTESIAN_POINT('Ctrl Pts',(57.2755422525822,-41.3882148268798,
12.));
#122137=CARTESIAN_POINT('Ctrl Pts',(57.2626878751584,-41.3714041819215,
0.));
#122138=CARTESIAN_POINT('Ctrl Pts',(57.2626878751584,-41.3714041819215,
12.));
#122139=CARTESIAN_POINT('Ctrl Pts',(57.2498462101883,-41.3546463114889,
0.));
#122140=CARTESIAN_POINT('Ctrl Pts',(57.2498462101883,-41.3546463114889,
12.));
#122141=CARTESIAN_POINT('Ctrl Pts',(57.237017419142,-41.3379412967889,0.));
#122142=CARTESIAN_POINT('Ctrl Pts',(57.237017419142,-41.3379412967889,12.));
#122143=CARTESIAN_POINT('Ctrl Pts',(57.2242016640226,-41.321289219151,0.));
#122144=CARTESIAN_POINT('Ctrl Pts',(57.2242016640226,-41.321289219151,12.));
#122145=CARTESIAN_POINT('Ctrl Pts',(57.2113991077325,-41.304690160231,0.));
#122146=CARTESIAN_POINT('Ctrl Pts',(57.2113991077325,-41.304690160231,12.));
#122147=CARTESIAN_POINT('Ctrl Pts',(57.1986099143992,-41.288144202187,0.));
#122148=CARTESIAN_POINT('Ctrl Pts',(57.1986099143992,-41.288144202187,12.));
#122149=CARTESIAN_POINT('Ctrl Pts',(57.1858342496526,-41.2716514278268,
0.));
#122150=CARTESIAN_POINT('Ctrl Pts',(57.1858342496526,-41.2716514278268,
12.));
#122151=CARTESIAN_POINT('Ctrl Pts',(57.1730722810771,-41.2552119208445,
0.));
#122152=CARTESIAN_POINT('Ctrl Pts',(57.1730722810771,-41.2552119208445,
12.));
#122153=CARTESIAN_POINT('Ctrl Pts',(57.1603241779042,-41.2388257656534,
0.));
#122154=CARTESIAN_POINT('Ctrl Pts',(57.1603241779042,-41.2388257656534,
12.));
#122155=CARTESIAN_POINT('Ctrl Pts',(57.1475901101794,-41.2224930469412,
0.));
#122156=CARTESIAN_POINT('Ctrl Pts',(57.1475901101794,-41.2224930469412,
12.));
#122157=CARTESIAN_POINT('Ctrl Pts',(57.1348702480644,-41.2062138492913,
0.));
#122158=CARTESIAN_POINT('Ctrl Pts',(57.1348702480644,-41.2062138492913,
12.));
#122159=CARTESIAN_POINT('Ctrl Pts',(57.1221647611231,-41.1899882567941,
0.));
#122160=CARTESIAN_POINT('Ctrl Pts',(57.1221647611231,-41.1899882567941,
12.));
#122161=CARTESIAN_POINT('Ctrl Pts',(57.1094738174998,-41.1738163525932,
0.));
#122162=CARTESIAN_POINT('Ctrl Pts',(57.1094738174998,-41.1738163525932,
12.));
#122163=CARTESIAN_POINT('Ctrl Pts',(57.0967975854912,-41.1576982197403,
0.));
#122164=CARTESIAN_POINT('Ctrl Pts',(57.0967975854912,-41.1576982197403,
12.));
#122165=CARTESIAN_POINT('Ctrl Pts',(57.084136235428,-41.1416339422132,0.));
#122166=CARTESIAN_POINT('Ctrl Pts',(57.084136235428,-41.1416339422132,12.));
#122167=CARTESIAN_POINT('Ctrl Pts',(57.0714899412091,-41.1256236057437,
0.));
#122168=CARTESIAN_POINT('Ctrl Pts',(57.0714899412091,-41.1256236057437,
12.));
#122169=CARTESIAN_POINT('Ctrl Pts',(57.0588588825266,-41.1096672990125,
0.));
#122170=CARTESIAN_POINT('Ctrl Pts',(57.0588588825266,-41.1096672990125,
12.));
#122171=CARTESIAN_POINT('Ctrl Pts',(57.0462432450637,-41.093765113752,0.));
#122172=CARTESIAN_POINT('Ctrl Pts',(57.0462432450637,-41.093765113752,12.));
#122173=CARTESIAN_POINT('Ctrl Pts',(57.0336432158503,-41.0779171422415,
0.));
#122174=CARTESIAN_POINT('Ctrl Pts',(57.0336432158503,-41.0779171422415,
12.));
#122175=CARTESIAN_POINT('Ctrl Pts',(57.0210589791777,-41.0621234751,0.));
#122176=CARTESIAN_POINT('Ctrl Pts',(57.0210589791777,-41.0621234751,12.));
#122177=CARTESIAN_POINT('Ctrl Pts',(57.008490713044,-41.0463841993622,0.));
#122178=CARTESIAN_POINT('Ctrl Pts',(57.008490713044,-41.0463841993622,12.));
#122179=CARTESIAN_POINT('Ctrl Pts',(56.9959385834768,-41.0306993954021,
0.));
#122180=CARTESIAN_POINT('Ctrl Pts',(56.9959385834768,-41.0306993954021,
12.));
#122181=CARTESIAN_POINT('Ctrl Pts',(56.9834027500178,-41.0150691398988,
0.));
#122182=CARTESIAN_POINT('Ctrl Pts',(56.9834027500178,-41.0150691398988,
12.));
#122183=CARTESIAN_POINT('Ctrl Pts',(56.9708833766183,-40.9994935117307,
0.));
#122184=CARTESIAN_POINT('Ctrl Pts',(56.9708833766183,-40.9994935117307,
12.));
#122185=CARTESIAN_POINT('Ctrl Pts',(56.9583806404069,-40.9839725967121,
0.));
#122186=CARTESIAN_POINT('Ctrl Pts',(56.9583806404069,-40.9839725967121,
12.));
#122187=CARTESIAN_POINT('Ctrl Pts',(56.9458947422541,-40.968506493303,0.));
#122188=CARTESIAN_POINT('Ctrl Pts',(56.9458947422541,-40.968506493303,12.));
#122189=CARTESIAN_POINT('Ctrl Pts',(56.9334259139928,-40.9530953164952,
0.));
#122190=CARTESIAN_POINT('Ctrl Pts',(56.9334259139928,-40.9530953164952,
12.));
#122191=CARTESIAN_POINT('Ctrl Pts',(56.9209743960861,-40.9377391857044,
0.));
#122192=CARTESIAN_POINT('Ctrl Pts',(56.9209743960861,-40.9377391857044,
12.));
#122193=CARTESIAN_POINT('Ctrl Pts',(56.9085404164432,-40.9224382132382,
0.));
#122194=CARTESIAN_POINT('Ctrl Pts',(56.9085404164432,-40.9224382132382,
12.));
#122195=CARTESIAN_POINT('Ctrl Pts',(56.8961241708926,-40.9071924937551,
0.));
#122196=CARTESIAN_POINT('Ctrl Pts',(56.8961241708926,-40.9071924937551,
12.));
#122197=CARTESIAN_POINT('Ctrl Pts',(56.8837257978574,-40.8920020903443,
0.));
#122198=CARTESIAN_POINT('Ctrl Pts',(56.8837257978574,-40.8920020903443,
12.));
#122199=CARTESIAN_POINT('Ctrl Pts',(56.8713453765252,-40.8768670342278,
0.));
#122200=CARTESIAN_POINT('Ctrl Pts',(56.8713453765252,-40.8768670342278,
12.));
#122201=CARTESIAN_POINT('Ctrl Pts',(56.8614554317993,-40.8648032759631,
0.));
#122202=CARTESIAN_POINT('Ctrl Pts',(56.8614554317993,-40.8648032759631,
12.));
#122203=CARTESIAN_POINT('Ctrl Pts',(56.8540460739677,-40.8557803680412,
0.));
#122204=CARTESIAN_POINT('Ctrl Pts',(56.8540460739677,-40.8557803680412,
12.));
#122205=CARTESIAN_POINT('Ctrl Pts',(56.8491101022668,-40.8497761671086,
0.));
#122206=CARTESIAN_POINT('Ctrl Pts',(56.8491101022668,-40.8497761671086,
12.));
#122207=CARTESIAN_POINT('Ctrl Pts',(56.8466430164621,-40.8467768343957,
0.));
#122208=CARTESIAN_POINT('Ctrl Pts',(56.8466430164621,-40.8467768343957,
12.));
#122209=CARTESIAN_POINT('',(56.8466430164621,-40.8467768343957,12.));
#122210=CARTESIAN_POINT('Ctrl Pts',(56.8466430164621,-40.8467768343957,
12.));
#122211=CARTESIAN_POINT('Ctrl Pts',(56.8491101022668,-40.8497761671086,
12.));
#122212=CARTESIAN_POINT('Ctrl Pts',(56.8540460739677,-40.8557803680412,
12.));
#122213=CARTESIAN_POINT('Ctrl Pts',(56.8614554317993,-40.8648032759631,
12.));
#122214=CARTESIAN_POINT('Ctrl Pts',(56.8713453765252,-40.8768670342278,
12.));
#122215=CARTESIAN_POINT('Ctrl Pts',(56.8837257978574,-40.8920020903443,
12.));
#122216=CARTESIAN_POINT('Ctrl Pts',(56.8961241708926,-40.9071924937551,
12.));
#122217=CARTESIAN_POINT('Ctrl Pts',(56.9085404164432,-40.9224382132382,
12.));
#122218=CARTESIAN_POINT('Ctrl Pts',(56.9209743960861,-40.9377391857044,
12.));
#122219=CARTESIAN_POINT('Ctrl Pts',(56.9334259139928,-40.9530953164952,
12.));
#122220=CARTESIAN_POINT('Ctrl Pts',(56.9458947422541,-40.968506493303,12.));
#122221=CARTESIAN_POINT('Ctrl Pts',(56.9583806404069,-40.9839725967121,
12.));
#122222=CARTESIAN_POINT('Ctrl Pts',(56.9708833766183,-40.9994935117307,
12.));
#122223=CARTESIAN_POINT('Ctrl Pts',(56.9834027500178,-41.0150691398988,
12.));
#122224=CARTESIAN_POINT('Ctrl Pts',(56.9959385834768,-41.0306993954021,
12.));
#122225=CARTESIAN_POINT('Ctrl Pts',(57.008490713044,-41.0463841993622,12.));
#122226=CARTESIAN_POINT('Ctrl Pts',(57.0210589791777,-41.0621234751,12.));
#122227=CARTESIAN_POINT('Ctrl Pts',(57.0336432158503,-41.0779171422415,
12.));
#122228=CARTESIAN_POINT('Ctrl Pts',(57.0462432450637,-41.093765113752,12.));
#122229=CARTESIAN_POINT('Ctrl Pts',(57.0588588825266,-41.1096672990125,
12.));
#122230=CARTESIAN_POINT('Ctrl Pts',(57.0714899412091,-41.1256236057437,
12.));
#122231=CARTESIAN_POINT('Ctrl Pts',(57.084136235428,-41.1416339422132,12.));
#122232=CARTESIAN_POINT('Ctrl Pts',(57.0967975854912,-41.1576982197403,
12.));
#122233=CARTESIAN_POINT('Ctrl Pts',(57.1094738174998,-41.1738163525932,
12.));
#122234=CARTESIAN_POINT('Ctrl Pts',(57.1221647611231,-41.1899882567941,
12.));
#122235=CARTESIAN_POINT('Ctrl Pts',(57.1348702480644,-41.2062138492913,
12.));
#122236=CARTESIAN_POINT('Ctrl Pts',(57.1475901101794,-41.2224930469412,
12.));
#122237=CARTESIAN_POINT('Ctrl Pts',(57.1603241779042,-41.2388257656534,
12.));
#122238=CARTESIAN_POINT('Ctrl Pts',(57.1730722810771,-41.2552119208445,
12.));
#122239=CARTESIAN_POINT('Ctrl Pts',(57.1858342496526,-41.2716514278268,
12.));
#122240=CARTESIAN_POINT('Ctrl Pts',(57.1986099143992,-41.288144202187,12.));
#122241=CARTESIAN_POINT('Ctrl Pts',(57.2113991077325,-41.304690160231,12.));
#122242=CARTESIAN_POINT('Ctrl Pts',(57.2242016640226,-41.321289219151,12.));
#122243=CARTESIAN_POINT('Ctrl Pts',(57.237017419142,-41.3379412967889,12.));
#122244=CARTESIAN_POINT('Ctrl Pts',(57.2498462101883,-41.3546463114889,
12.));
#122245=CARTESIAN_POINT('Ctrl Pts',(57.2626878751584,-41.3714041819215,
12.));
#122246=CARTESIAN_POINT('Ctrl Pts',(57.2755422525822,-41.3882148268798,
12.));
#122247=CARTESIAN_POINT('Ctrl Pts',(57.2884091815384,-41.4050781652923,
12.));
#122248=CARTESIAN_POINT('Ctrl Pts',(57.3012885018139,-41.4219941163155,
12.));
#122249=CARTESIAN_POINT('Ctrl Pts',(57.3141800540137,-41.4389625993948,
12.));
#122250=CARTESIAN_POINT('Ctrl Pts',(57.3270836796925,-41.4559835343339,
12.));
#122251=CARTESIAN_POINT('Ctrl Pts',(57.339999221474,-41.4730568413535,12.));
#122252=CARTESIAN_POINT('Ctrl Pts',(57.3529265229858,-41.4901824410654,
12.));
#122253=CARTESIAN_POINT('Ctrl Pts',(57.3658654287948,-41.5073602544404,
12.));
#122254=CARTESIAN_POINT('Ctrl Pts',(57.378815784345,-41.5245902027767,12.));
#122255=CARTESIAN_POINT('Ctrl Pts',(57.3917774358844,-41.5418722076558,
12.));
#122256=CARTESIAN_POINT('Ctrl Pts',(57.4047502304207,-41.5592061909159,
12.));
#122257=CARTESIAN_POINT('Ctrl Pts',(57.417734015749,-41.5765920746764,12.));
#122258=CARTESIAN_POINT('Ctrl Pts',(57.4307286404656,-41.5940297813474,
12.));
#122259=CARTESIAN_POINT('Ctrl Pts',(57.4437339539848,-41.6115192336394,
12.));
#122260=CARTESIAN_POINT('Ctrl Pts',(57.4567498065573,-41.6290603545674,
12.));
#122261=CARTESIAN_POINT('Ctrl Pts',(57.4697760492693,-41.6466530674522,
12.));
#122262=CARTESIAN_POINT('Ctrl Pts',(57.4828125340222,-41.6642972959168,
12.));
#122263=CARTESIAN_POINT('Ctrl Pts',(57.4958591135165,-41.6819929638797,
12.));
#122264=CARTESIAN_POINT('Ctrl Pts',(57.5089156412341,-41.6997399955445,
12.));
#122265=CARTESIAN_POINT('Ctrl Pts',(57.5219819714169,-41.7175383153819,
12.));
#122266=CARTESIAN_POINT('Ctrl Pts',(57.5350579590648,-41.7353878481336,
12.));
#122267=CARTESIAN_POINT('Ctrl Pts',(57.5481434599334,-41.7532885188174,
12.));
#122268=CARTESIAN_POINT('Ctrl Pts',(57.561238330532,-41.7712402527273,12.));
#122269=CARTESIAN_POINT('Ctrl Pts',(57.5743424281204,-41.7892429754298,
12.));
#122270=CARTESIAN_POINT('Ctrl Pts',(57.5874556107054,-41.8072966127559,
12.));
#122271=CARTESIAN_POINT('Ctrl Pts',(57.6005777370347,-41.8254010908051,
12.));
#122272=CARTESIAN_POINT('Ctrl Pts',(57.613708666588,-41.8435563359456,12.));
#122273=CARTESIAN_POINT('Ctrl Pts',(57.6268482595701,-41.8617622748107,
12.));
#122274=CARTESIAN_POINT('Ctrl Pts',(57.6399963769009,-41.8800188342912,
12.));
#122275=CARTESIAN_POINT('Ctrl Pts',(57.6531528802072,-41.8983259415253,
12.));
#122276=CARTESIAN_POINT('Ctrl Pts',(57.6663176318189,-41.9166835239054,
12.));
#122277=CARTESIAN_POINT('Ctrl Pts',(57.6794904947649,-41.9350915090797,
12.));
#122278=CARTESIAN_POINT('Ctrl Pts',(57.6926713327672,-41.9535498249488,
12.));
#122279=CARTESIAN_POINT('Ctrl Pts',(57.7058600102351,-41.9720583996592,
12.));
#122280=CARTESIAN_POINT('Ctrl Pts',(57.7190563922593,-41.990617161596,12.));
#122281=CARTESIAN_POINT('Ctrl Pts',(57.7322603446066,-42.0092260393897,
12.));
#122282=CARTESIAN_POINT('Ctrl Pts',(57.745471733714,-42.0278849619148,12.));
#122283=CARTESIAN_POINT('Ctrl Pts',(57.7586904266834,-42.0465938582882,
12.));
#122284=CARTESIAN_POINT('Ctrl Pts',(57.7719162912744,-42.0653526578588,
12.));
#122285=CARTESIAN_POINT('Ctrl Pts',(57.7851491958987,-42.0841612902042,
12.));
#122286=CARTESIAN_POINT('Ctrl Pts',(57.798389009616,-42.1030196851366,12.));
#122287=CARTESIAN_POINT('Ctrl Pts',(57.8116356021288,-42.1219277727021,
12.));
#122288=CARTESIAN_POINT('Ctrl Pts',(57.8248888437775,-42.1408854831783,
12.));
#122289=CARTESIAN_POINT('Ctrl Pts',(57.8381486055342,-42.1598927470646,
12.));
#122290=CARTESIAN_POINT('Ctrl Pts',(57.8514147589972,-42.1789494950794,
12.));
#122291=CARTESIAN_POINT('Ctrl Pts',(57.864687176387,-42.1980556581665,12.));
#122292=CARTESIAN_POINT('Ctrl Pts',(57.8779657305413,-42.2172111674938,
12.));
#122293=CARTESIAN_POINT('Ctrl Pts',(57.8912502949096,-42.2364159544501,
12.));
#122294=CARTESIAN_POINT('Ctrl Pts',(57.9045407435474,-42.2556699506353,
12.));
#122295=CARTESIAN_POINT('Ctrl Pts',(57.9178369511114,-42.2749730878595,
12.));
#122296=CARTESIAN_POINT('Ctrl Pts',(57.9311387928563,-42.2943252981489,
12.));
#122297=CARTESIAN_POINT('Ctrl Pts',(57.9444461446299,-42.3137265137452,
12.));
#122298=CARTESIAN_POINT('Ctrl Pts',(57.9577588828682,-42.333176667102,12.));
#122299=CARTESIAN_POINT('Ctrl Pts',(57.9710768845899,-42.3526756908747,
12.));
#122300=CARTESIAN_POINT('Ctrl Pts',(57.9844000273911,-42.3722235179198,
12.));
#122301=CARTESIAN_POINT('Ctrl Pts',(57.9977281894422,-42.3918200813014,
12.));
#122302=CARTESIAN_POINT('Ctrl Pts',(58.0110612494828,-42.411465314289,12.));
#122303=CARTESIAN_POINT('Ctrl Pts',(58.0243990868181,-42.4311591503555,
12.));
#122304=CARTESIAN_POINT('Ctrl Pts',(58.037741581314,-42.4509015231674,12.));
#122305=CARTESIAN_POINT('Ctrl Pts',(58.0510886133926,-42.4706923665845,
12.));
#122306=CARTESIAN_POINT('Ctrl Pts',(58.0644400640275,-42.4905316146654,
12.));
#122307=CARTESIAN_POINT('Ctrl Pts',(58.0777958147403,-42.5104192016664,
12.));
#122308=CARTESIAN_POINT('Ctrl Pts',(58.0911557475965,-42.5303550620387,
12.));
#122309=CARTESIAN_POINT('Ctrl Pts',(58.1045197452002,-42.5503391304183,
12.));
#122310=CARTESIAN_POINT('Ctrl Pts',(58.1178876906907,-42.5703713416265,
12.));
#122311=CARTESIAN_POINT('Ctrl Pts',(58.1312594677386,-42.5904516306762,
12.));
#122312=CARTESIAN_POINT('Ctrl Pts',(58.1446349605421,-42.6105799327699,
12.));
#122313=CARTESIAN_POINT('Ctrl Pts',(58.1580140538228,-42.6307561832976,
12.));
#122314=CARTESIAN_POINT('Ctrl Pts',(58.171396632821,-42.6509803178265,12.));
#122315=CARTESIAN_POINT('Ctrl Pts',(58.1847825832923,-42.6712522721016,
12.));
#122316=CARTESIAN_POINT('Ctrl Pts',(58.1981717915037,-42.6915719820513,
12.));
#122317=CARTESIAN_POINT('Ctrl Pts',(58.21156414423,-42.7119393837866,12.));
#122318=CARTESIAN_POINT('Ctrl Pts',(58.22495952875,-42.7323544135985,12.));
#122319=CARTESIAN_POINT('Ctrl Pts',(58.2383578328424,-42.7528170079485,
12.));
#122320=CARTESIAN_POINT('Ctrl Pts',(58.251758944782,-42.773327103468,12.));
#122321=CARTESIAN_POINT('Ctrl Pts',(58.2651627533368,-42.7938846369651,
12.));
#122322=CARTESIAN_POINT('Ctrl Pts',(58.2785691477638,-42.8144895454233,
12.));
#122323=CARTESIAN_POINT('Ctrl Pts',(58.2919780178064,-42.8351417659999,
12.));
#122324=CARTESIAN_POINT('Ctrl Pts',(58.3053892536894,-42.8558412360158,
12.));
#122325=CARTESIAN_POINT('Ctrl Pts',(58.3188027461164,-42.8765878929551,
12.));
#122326=CARTESIAN_POINT('Ctrl Pts',(58.3322183862654,-42.8973816744709,
12.));
#122327=CARTESIAN_POINT('Ctrl Pts',(58.3456360657865,-42.9182225183855,
12.));
#122328=CARTESIAN_POINT('Ctrl Pts',(58.3590556767978,-42.9391103626879,
12.));
#122329=CARTESIAN_POINT('Ctrl Pts',(58.3724771118826,-42.960045145526,12.));
#122330=CARTESIAN_POINT('Ctrl Pts',(58.3859002640856,-42.9810268052032,
12.));
#122331=CARTESIAN_POINT('Ctrl Pts',(58.3993250269101,-43.0020552801859,
12.));
#122332=CARTESIAN_POINT('Ctrl Pts',(58.4127512943136,-43.0231305091027,
12.));
#122333=CARTESIAN_POINT('Ctrl Pts',(58.4261789607058,-43.0442524307434,
12.));
#122334=CARTESIAN_POINT('Ctrl Pts',(58.439607920945,-43.0654209840511,12.));
#122335=CARTESIAN_POINT('Ctrl Pts',(58.4530380703348,-43.0866361081177,
12.));
#122336=CARTESIAN_POINT('Ctrl Pts',(58.4664693046217,-43.1078977421916,
12.));
#122337=CARTESIAN_POINT('Ctrl Pts',(58.4799015199907,-43.1292058256777,
12.));
#122338=CARTESIAN_POINT('Ctrl Pts',(58.4933346130636,-43.1505602981365,
12.));
#122339=CARTESIAN_POINT('Ctrl Pts',(58.5067684808944,-43.1719610992771,
12.));
#122340=CARTESIAN_POINT('Ctrl Pts',(58.5202030209669,-43.1934081689505,
12.));
#122341=CARTESIAN_POINT('Ctrl Pts',(58.5336381311917,-43.2149014471574,
12.));
#122342=CARTESIAN_POINT('Ctrl Pts',(58.5470737099032,-43.2364408740493,
12.));
#122343=CARTESIAN_POINT('Ctrl Pts',(58.5605096558578,-43.2580263899278,
12.));
#122344=CARTESIAN_POINT('Ctrl Pts',(58.573945868231,-43.2796579352401,12.));
#122345=CARTESIAN_POINT('Ctrl Pts',(58.5873822466152,-43.3013354505701,
12.));
#122346=CARTESIAN_POINT('Ctrl Pts',(58.6008186910156,-43.3230588766449,
12.));
#122347=CARTESIAN_POINT('Ctrl Pts',(58.6142551018467,-43.3448281543372,
12.));
#122348=CARTESIAN_POINT('Ctrl Pts',(58.627691379929,-43.3666432246635,12.));
#122349=CARTESIAN_POINT('Ctrl Pts',(58.6411274264857,-43.388504028781,12.));
#122350=CARTESIAN_POINT('Ctrl Pts',(58.6545631431393,-43.4104105079768,
12.));
#122351=CARTESIAN_POINT('Ctrl Pts',(58.6679984319097,-43.4323626036737,
12.));
#122352=CARTESIAN_POINT('Ctrl Pts',(58.6814331952138,-43.4543602574351,
12.));
#122353=CARTESIAN_POINT('Ctrl Pts',(58.6948673358638,-43.4764034109654,
12.));
#122354=CARTESIAN_POINT('Ctrl Pts',(58.7083007570661,-43.4984920061073,
12.));
#122355=CARTESIAN_POINT('Ctrl Pts',(58.7217333624209,-43.5206259848338,
12.));
#122356=CARTESIAN_POINT('Ctrl Pts',(58.735165055918,-43.5428052892488,12.));
#122357=CARTESIAN_POINT('Ctrl Pts',(58.74859574193,-43.5650298615917,12.));
#122358=CARTESIAN_POINT('Ctrl Pts',(58.7620253252062,-43.5872996442345,
12.));
#122359=CARTESIAN_POINT('Ctrl Pts',(58.775453710867,-43.6096145796797,12.));
#122360=CARTESIAN_POINT('Ctrl Pts',(58.788880804397,-43.6319746105482,12.));
#122361=CARTESIAN_POINT('Ctrl Pts',(58.8023065116436,-43.6543796795789,
12.));
#122362=CARTESIAN_POINT('Ctrl Pts',(58.8157307388238,-43.6768297296395,
12.));
#122363=CARTESIAN_POINT('Ctrl Pts',(58.8291533925293,-43.6993247037314,
12.));
#122364=CARTESIAN_POINT('Ctrl Pts',(58.8425743797326,-43.7218645449922,
12.));
#122365=CARTESIAN_POINT('Ctrl Pts',(58.855993607794,-43.7444491966942,12.));
#122366=CARTESIAN_POINT('Ctrl Pts',(58.8694109844647,-43.7670786022402,
12.));
#122367=CARTESIAN_POINT('Ctrl Pts',(58.8828264178621,-43.7897527051609,
12.));
#122368=CARTESIAN_POINT('Ctrl Pts',(58.8962398164493,-43.8124714491077,
12.));
#122369=CARTESIAN_POINT('Ctrl Pts',(58.9096510890129,-43.835234777842,12.));
#122370=CARTESIAN_POINT('Ctrl Pts',(58.9230601446436,-43.858042635223,12.));
#122371=CARTESIAN_POINT('Ctrl Pts',(58.936466892712,-43.8808949651873,12.));
#122372=CARTESIAN_POINT('Ctrl Pts',(58.9498712429054,-43.9037917117739,
12.));
#122373=CARTESIAN_POINT('Ctrl Pts',(58.9632731052696,-43.9267328191501,
12.));
#122374=CARTESIAN_POINT('Ctrl Pts',(58.9766723902529,-43.9497182316331,
12.));
#122375=CARTESIAN_POINT('Ctrl Pts',(58.9900690087408,-43.9727478937056,
12.));
#122376=CARTESIAN_POINT('Ctrl Pts',(59.0034628721167,-43.9958217500369,
12.));
#122377=CARTESIAN_POINT('Ctrl Pts',(59.0168538922095,-44.0189397454599,
12.));
#122378=CARTESIAN_POINT('Ctrl Pts',(59.0302419811777,-44.0421018249223,
12.));
#122379=CARTESIAN_POINT('Ctrl Pts',(59.0436270514086,-44.0653079334385,
12.));
#122380=CARTESIAN_POINT('Ctrl Pts',(59.0570090154242,-44.0885580160433,
12.));
#122381=CARTESIAN_POINT('Ctrl Pts',(59.0703877857525,-44.1118520177221,
12.));
#122382=CARTESIAN_POINT('Ctrl Pts',(59.08376327492,-44.1351898834051,12.));
#122383=CARTESIAN_POINT('Ctrl Pts',(59.0971353957206,-44.1585715581065,
12.));
#122384=CARTESIAN_POINT('Ctrl Pts',(59.1105040614275,-44.1819969870307,
12.));
#122385=CARTESIAN_POINT('Ctrl Pts',(59.1238691860306,-44.2054661156875,
12.));
#122386=CARTESIAN_POINT('Ctrl Pts',(59.1372306844585,-44.228978889997,12.));
#122387=CARTESIAN_POINT('Ctrl Pts',(59.1505884728215,-44.2525352563996,
12.));
#122388=CARTESIAN_POINT('Ctrl Pts',(59.1639424678793,-44.2761351616048,
12.));
#122389=CARTESIAN_POINT('Ctrl Pts',(59.1772925865213,-44.2997785523431,
12.));
#122390=CARTESIAN_POINT('Ctrl Pts',(59.1906387451979,-44.3234653750884,
12.));
#122391=CARTESIAN_POINT('Ctrl Pts',(59.2039808594752,-44.3471955758403,
12.));
#122392=CARTESIAN_POINT('Ctrl Pts',(59.2173188432798,-44.370969099747,12.));
#122393=CARTESIAN_POINT('Ctrl Pts',(59.2306526095131,-44.3947858914074,
12.));
#122394=CARTESIAN_POINT('Ctrl Pts',(59.2439820714187,-44.4186458955451,
12.));
#122395=CARTESIAN_POINT('Ctrl Pts',(59.2573071437774,-44.4425490575911,
12.));
#122396=CARTESIAN_POINT('Ctrl Pts',(59.2706277440445,-44.4664953242379,
12.));
#122397=CARTESIAN_POINT('Ctrl Pts',(59.2839437938237,-44.490484644151,12.));
#122398=CARTESIAN_POINT('Ctrl Pts',(59.2972552192156,-44.5145169681349,
12.));
#122399=CARTESIAN_POINT('Ctrl Pts',(59.3086616639523,-44.5351541478479,
12.));
#122400=CARTESIAN_POINT('Ctrl Pts',(59.3174041872347,-44.5509994358154,
12.));
#122401=CARTESIAN_POINT('Ctrl Pts',(59.3234848865455,-44.5620338188738,
12.));
#122402=CARTESIAN_POINT('Ctrl Pts',(59.3269051738423,-44.5682447396021,
12.));
#122403=CARTESIAN_POINT('Ctrl Pts',(59.3276657444392,-44.5696260757792,
12.));
#122404=CARTESIAN_POINT('',(56.8466430164621,-40.8467768343957,0.));
#122405=CARTESIAN_POINT('',(56.8466430164621,-40.8467768343957,0.));
#122406=CARTESIAN_POINT('Ctrl Pts',(59.3276657444391,-44.569626075779,0.));
#122407=CARTESIAN_POINT('Ctrl Pts',(59.3269051738422,-44.568244739602,0.));
#122408=CARTESIAN_POINT('Ctrl Pts',(59.3234848865455,-44.5620338188737,
0.));
#122409=CARTESIAN_POINT('Ctrl Pts',(59.3174041872347,-44.5509994358153,
0.));
#122410=CARTESIAN_POINT('Ctrl Pts',(59.3086616639523,-44.5351541478479,
0.));
#122411=CARTESIAN_POINT('Ctrl Pts',(59.2972552192156,-44.5145169681349,
0.));
#122412=CARTESIAN_POINT('Ctrl Pts',(59.2839437938237,-44.490484644151,0.));
#122413=CARTESIAN_POINT('Ctrl Pts',(59.2706277440445,-44.4664953242379,
0.));
#122414=CARTESIAN_POINT('Ctrl Pts',(59.2573071437774,-44.4425490575911,
0.));
#122415=CARTESIAN_POINT('Ctrl Pts',(59.2439820714187,-44.4186458955451,
0.));
#122416=CARTESIAN_POINT('Ctrl Pts',(59.2306526095131,-44.3947858914074,
0.));
#122417=CARTESIAN_POINT('Ctrl Pts',(59.2173188432798,-44.370969099747,0.));
#122418=CARTESIAN_POINT('Ctrl Pts',(59.2039808594752,-44.3471955758403,
0.));
#122419=CARTESIAN_POINT('Ctrl Pts',(59.1906387451979,-44.3234653750884,
0.));
#122420=CARTESIAN_POINT('Ctrl Pts',(59.1772925865213,-44.2997785523431,
0.));
#122421=CARTESIAN_POINT('Ctrl Pts',(59.1639424678793,-44.2761351616048,
0.));
#122422=CARTESIAN_POINT('Ctrl Pts',(59.1505884728215,-44.2525352563996,
0.));
#122423=CARTESIAN_POINT('Ctrl Pts',(59.1372306844585,-44.228978889997,0.));
#122424=CARTESIAN_POINT('Ctrl Pts',(59.1238691860306,-44.2054661156875,
0.));
#122425=CARTESIAN_POINT('Ctrl Pts',(59.1105040614275,-44.1819969870307,
0.));
#122426=CARTESIAN_POINT('Ctrl Pts',(59.0971353957206,-44.1585715581065,
0.));
#122427=CARTESIAN_POINT('Ctrl Pts',(59.08376327492,-44.1351898834051,0.));
#122428=CARTESIAN_POINT('Ctrl Pts',(59.0703877857525,-44.1118520177221,
0.));
#122429=CARTESIAN_POINT('Ctrl Pts',(59.0570090154242,-44.0885580160433,
0.));
#122430=CARTESIAN_POINT('Ctrl Pts',(59.0436270514086,-44.0653079334385,
0.));
#122431=CARTESIAN_POINT('Ctrl Pts',(59.0302419811777,-44.0421018249223,
0.));
#122432=CARTESIAN_POINT('Ctrl Pts',(59.0168538922095,-44.0189397454599,
0.));
#122433=CARTESIAN_POINT('Ctrl Pts',(59.0034628721167,-43.9958217500369,
0.));
#122434=CARTESIAN_POINT('Ctrl Pts',(58.9900690087408,-43.9727478937056,
0.));
#122435=CARTESIAN_POINT('Ctrl Pts',(58.9766723902529,-43.9497182316331,
0.));
#122436=CARTESIAN_POINT('Ctrl Pts',(58.9632731052696,-43.9267328191501,
0.));
#122437=CARTESIAN_POINT('Ctrl Pts',(58.9498712429054,-43.9037917117739,
0.));
#122438=CARTESIAN_POINT('Ctrl Pts',(58.936466892712,-43.8808949651873,0.));
#122439=CARTESIAN_POINT('Ctrl Pts',(58.9230601446436,-43.858042635223,0.));
#122440=CARTESIAN_POINT('Ctrl Pts',(58.9096510890129,-43.835234777842,0.));
#122441=CARTESIAN_POINT('Ctrl Pts',(58.8962398164493,-43.8124714491077,
0.));
#122442=CARTESIAN_POINT('Ctrl Pts',(58.8828264178621,-43.7897527051609,
0.));
#122443=CARTESIAN_POINT('Ctrl Pts',(58.8694109844647,-43.7670786022402,
0.));
#122444=CARTESIAN_POINT('Ctrl Pts',(58.855993607794,-43.7444491966942,0.));
#122445=CARTESIAN_POINT('Ctrl Pts',(58.8425743797326,-43.7218645449922,
0.));
#122446=CARTESIAN_POINT('Ctrl Pts',(58.8291533925293,-43.6993247037314,
0.));
#122447=CARTESIAN_POINT('Ctrl Pts',(58.8157307388238,-43.6768297296395,
0.));
#122448=CARTESIAN_POINT('Ctrl Pts',(58.8023065116436,-43.6543796795789,
0.));
#122449=CARTESIAN_POINT('Ctrl Pts',(58.788880804397,-43.6319746105482,0.));
#122450=CARTESIAN_POINT('Ctrl Pts',(58.775453710867,-43.6096145796797,0.));
#122451=CARTESIAN_POINT('Ctrl Pts',(58.7620253252062,-43.5872996442345,
0.));
#122452=CARTESIAN_POINT('Ctrl Pts',(58.74859574193,-43.5650298615917,0.));
#122453=CARTESIAN_POINT('Ctrl Pts',(58.735165055918,-43.5428052892488,0.));
#122454=CARTESIAN_POINT('Ctrl Pts',(58.7217333624209,-43.5206259848338,
0.));
#122455=CARTESIAN_POINT('Ctrl Pts',(58.7083007570661,-43.4984920061073,
0.));
#122456=CARTESIAN_POINT('Ctrl Pts',(58.6948673358638,-43.4764034109654,
0.));
#122457=CARTESIAN_POINT('Ctrl Pts',(58.6814331952138,-43.4543602574351,
0.));
#122458=CARTESIAN_POINT('Ctrl Pts',(58.6679984319097,-43.4323626036737,
0.));
#122459=CARTESIAN_POINT('Ctrl Pts',(58.6545631431393,-43.4104105079768,
0.));
#122460=CARTESIAN_POINT('Ctrl Pts',(58.6411274264857,-43.388504028781,0.));
#122461=CARTESIAN_POINT('Ctrl Pts',(58.627691379929,-43.3666432246635,0.));
#122462=CARTESIAN_POINT('Ctrl Pts',(58.6142551018467,-43.3448281543372,
0.));
#122463=CARTESIAN_POINT('Ctrl Pts',(58.6008186910156,-43.3230588766449,
0.));
#122464=CARTESIAN_POINT('Ctrl Pts',(58.5873822466152,-43.3013354505701,
0.));
#122465=CARTESIAN_POINT('Ctrl Pts',(58.573945868231,-43.2796579352401,0.));
#122466=CARTESIAN_POINT('Ctrl Pts',(58.5605096558578,-43.2580263899278,
0.));
#122467=CARTESIAN_POINT('Ctrl Pts',(58.5470737099032,-43.2364408740493,
0.));
#122468=CARTESIAN_POINT('Ctrl Pts',(58.5336381311917,-43.2149014471574,
0.));
#122469=CARTESIAN_POINT('Ctrl Pts',(58.5202030209669,-43.1934081689505,
0.));
#122470=CARTESIAN_POINT('Ctrl Pts',(58.5067684808944,-43.1719610992771,
0.));
#122471=CARTESIAN_POINT('Ctrl Pts',(58.4933346130636,-43.1505602981365,
0.));
#122472=CARTESIAN_POINT('Ctrl Pts',(58.4799015199907,-43.1292058256777,
0.));
#122473=CARTESIAN_POINT('Ctrl Pts',(58.4664693046217,-43.1078977421916,
0.));
#122474=CARTESIAN_POINT('Ctrl Pts',(58.4530380703348,-43.0866361081177,
0.));
#122475=CARTESIAN_POINT('Ctrl Pts',(58.439607920945,-43.0654209840511,0.));
#122476=CARTESIAN_POINT('Ctrl Pts',(58.4261789607058,-43.0442524307434,
0.));
#122477=CARTESIAN_POINT('Ctrl Pts',(58.4127512943136,-43.0231305091027,
0.));
#122478=CARTESIAN_POINT('Ctrl Pts',(58.3993250269101,-43.0020552801859,
0.));
#122479=CARTESIAN_POINT('Ctrl Pts',(58.3859002640856,-42.9810268052032,
0.));
#122480=CARTESIAN_POINT('Ctrl Pts',(58.3724771118826,-42.960045145526,0.));
#122481=CARTESIAN_POINT('Ctrl Pts',(58.3590556767978,-42.9391103626879,
0.));
#122482=CARTESIAN_POINT('Ctrl Pts',(58.3456360657865,-42.9182225183855,
0.));
#122483=CARTESIAN_POINT('Ctrl Pts',(58.3322183862654,-42.8973816744709,
0.));
#122484=CARTESIAN_POINT('Ctrl Pts',(58.3188027461164,-42.8765878929551,
0.));
#122485=CARTESIAN_POINT('Ctrl Pts',(58.3053892536894,-42.8558412360158,
0.));
#122486=CARTESIAN_POINT('Ctrl Pts',(58.2919780178064,-42.8351417659999,
0.));
#122487=CARTESIAN_POINT('Ctrl Pts',(58.2785691477638,-42.8144895454233,
0.));
#122488=CARTESIAN_POINT('Ctrl Pts',(58.2651627533368,-42.7938846369651,
0.));
#122489=CARTESIAN_POINT('Ctrl Pts',(58.251758944782,-42.773327103468,0.));
#122490=CARTESIAN_POINT('Ctrl Pts',(58.2383578328424,-42.7528170079485,
0.));
#122491=CARTESIAN_POINT('Ctrl Pts',(58.22495952875,-42.7323544135985,0.));
#122492=CARTESIAN_POINT('Ctrl Pts',(58.21156414423,-42.7119393837866,0.));
#122493=CARTESIAN_POINT('Ctrl Pts',(58.1981717915037,-42.6915719820513,
0.));
#122494=CARTESIAN_POINT('Ctrl Pts',(58.1847825832923,-42.6712522721016,
0.));
#122495=CARTESIAN_POINT('Ctrl Pts',(58.171396632821,-42.6509803178265,0.));
#122496=CARTESIAN_POINT('Ctrl Pts',(58.1580140538228,-42.6307561832976,
0.));
#122497=CARTESIAN_POINT('Ctrl Pts',(58.1446349605421,-42.6105799327699,
0.));
#122498=CARTESIAN_POINT('Ctrl Pts',(58.1312594677386,-42.5904516306762,
0.));
#122499=CARTESIAN_POINT('Ctrl Pts',(58.1178876906907,-42.5703713416265,
0.));
#122500=CARTESIAN_POINT('Ctrl Pts',(58.1045197452002,-42.5503391304183,
0.));
#122501=CARTESIAN_POINT('Ctrl Pts',(58.0911557475965,-42.5303550620387,
0.));
#122502=CARTESIAN_POINT('Ctrl Pts',(58.0777958147403,-42.5104192016664,
0.));
#122503=CARTESIAN_POINT('Ctrl Pts',(58.0644400640275,-42.4905316146654,
0.));
#122504=CARTESIAN_POINT('Ctrl Pts',(58.0510886133926,-42.4706923665845,
0.));
#122505=CARTESIAN_POINT('Ctrl Pts',(58.037741581314,-42.4509015231674,0.));
#122506=CARTESIAN_POINT('Ctrl Pts',(58.0243990868181,-42.4311591503555,
0.));
#122507=CARTESIAN_POINT('Ctrl Pts',(58.0110612494828,-42.411465314289,0.));
#122508=CARTESIAN_POINT('Ctrl Pts',(57.9977281894422,-42.3918200813014,
0.));
#122509=CARTESIAN_POINT('Ctrl Pts',(57.9844000273911,-42.3722235179198,
0.));
#122510=CARTESIAN_POINT('Ctrl Pts',(57.9710768845899,-42.3526756908747,
0.));
#122511=CARTESIAN_POINT('Ctrl Pts',(57.9577588828682,-42.333176667102,0.));
#122512=CARTESIAN_POINT('Ctrl Pts',(57.9444461446299,-42.3137265137452,
0.));
#122513=CARTESIAN_POINT('Ctrl Pts',(57.9311387928563,-42.2943252981489,
0.));
#122514=CARTESIAN_POINT('Ctrl Pts',(57.9178369511114,-42.2749730878595,
0.));
#122515=CARTESIAN_POINT('Ctrl Pts',(57.9045407435474,-42.2556699506353,
0.));
#122516=CARTESIAN_POINT('Ctrl Pts',(57.8912502949096,-42.2364159544501,
0.));
#122517=CARTESIAN_POINT('Ctrl Pts',(57.8779657305413,-42.2172111674938,
0.));
#122518=CARTESIAN_POINT('Ctrl Pts',(57.864687176387,-42.1980556581665,0.));
#122519=CARTESIAN_POINT('Ctrl Pts',(57.8514147589972,-42.1789494950794,
0.));
#122520=CARTESIAN_POINT('Ctrl Pts',(57.8381486055342,-42.1598927470646,
0.));
#122521=CARTESIAN_POINT('Ctrl Pts',(57.8248888437775,-42.1408854831783,
0.));
#122522=CARTESIAN_POINT('Ctrl Pts',(57.8116356021288,-42.1219277727021,
0.));
#122523=CARTESIAN_POINT('Ctrl Pts',(57.798389009616,-42.1030196851366,0.));
#122524=CARTESIAN_POINT('Ctrl Pts',(57.7851491958987,-42.0841612902042,
0.));
#122525=CARTESIAN_POINT('Ctrl Pts',(57.7719162912744,-42.0653526578588,
0.));
#122526=CARTESIAN_POINT('Ctrl Pts',(57.7586904266834,-42.0465938582882,
0.));
#122527=CARTESIAN_POINT('Ctrl Pts',(57.745471733714,-42.0278849619148,0.));
#122528=CARTESIAN_POINT('Ctrl Pts',(57.7322603446066,-42.0092260393897,
0.));
#122529=CARTESIAN_POINT('Ctrl Pts',(57.7190563922593,-41.990617161596,0.));
#122530=CARTESIAN_POINT('Ctrl Pts',(57.7058600102351,-41.9720583996592,
0.));
#122531=CARTESIAN_POINT('Ctrl Pts',(57.6926713327672,-41.9535498249488,
0.));
#122532=CARTESIAN_POINT('Ctrl Pts',(57.6794904947649,-41.9350915090797,
0.));
#122533=CARTESIAN_POINT('Ctrl Pts',(57.6663176318189,-41.9166835239054,
0.));
#122534=CARTESIAN_POINT('Ctrl Pts',(57.6531528802072,-41.8983259415253,
0.));
#122535=CARTESIAN_POINT('Ctrl Pts',(57.6399963769009,-41.8800188342912,
0.));
#122536=CARTESIAN_POINT('Ctrl Pts',(57.6268482595701,-41.8617622748107,
0.));
#122537=CARTESIAN_POINT('Ctrl Pts',(57.613708666588,-41.8435563359456,0.));
#122538=CARTESIAN_POINT('Ctrl Pts',(57.6005777370347,-41.8254010908051,
0.));
#122539=CARTESIAN_POINT('Ctrl Pts',(57.5874556107054,-41.8072966127559,
0.));
#122540=CARTESIAN_POINT('Ctrl Pts',(57.5743424281204,-41.7892429754298,
0.));
#122541=CARTESIAN_POINT('Ctrl Pts',(57.561238330532,-41.7712402527273,0.));
#122542=CARTESIAN_POINT('Ctrl Pts',(57.5481434599334,-41.7532885188174,
0.));
#122543=CARTESIAN_POINT('Ctrl Pts',(57.5350579590648,-41.7353878481336,
0.));
#122544=CARTESIAN_POINT('Ctrl Pts',(57.5219819714169,-41.7175383153819,
0.));
#122545=CARTESIAN_POINT('Ctrl Pts',(57.5089156412341,-41.6997399955445,
0.));
#122546=CARTESIAN_POINT('Ctrl Pts',(57.4958591135165,-41.6819929638797,
0.));
#122547=CARTESIAN_POINT('Ctrl Pts',(57.4828125340222,-41.6642972959168,
0.));
#122548=CARTESIAN_POINT('Ctrl Pts',(57.4697760492693,-41.6466530674522,
0.));
#122549=CARTESIAN_POINT('Ctrl Pts',(57.4567498065573,-41.6290603545674,
0.));
#122550=CARTESIAN_POINT('Ctrl Pts',(57.4437339539848,-41.6115192336394,
0.));
#122551=CARTESIAN_POINT('Ctrl Pts',(57.4307286404656,-41.5940297813474,
0.));
#122552=CARTESIAN_POINT('Ctrl Pts',(57.417734015749,-41.5765920746764,0.));
#122553=CARTESIAN_POINT('Ctrl Pts',(57.4047502304207,-41.5592061909159,
0.));
#122554=CARTESIAN_POINT('Ctrl Pts',(57.3917774358844,-41.5418722076558,
0.));
#122555=CARTESIAN_POINT('Ctrl Pts',(57.378815784345,-41.5245902027767,0.));
#122556=CARTESIAN_POINT('Ctrl Pts',(57.3658654287948,-41.5073602544404,
0.));
#122557=CARTESIAN_POINT('Ctrl Pts',(57.3529265229858,-41.4901824410654,
0.));
#122558=CARTESIAN_POINT('Ctrl Pts',(57.339999221474,-41.4730568413535,0.));
#122559=CARTESIAN_POINT('Ctrl Pts',(57.3270836796925,-41.4559835343339,
0.));
#122560=CARTESIAN_POINT('Ctrl Pts',(57.3141800540137,-41.4389625993948,
0.));
#122561=CARTESIAN_POINT('Ctrl Pts',(57.3012885018139,-41.4219941163155,
0.));
#122562=CARTESIAN_POINT('Ctrl Pts',(57.2884091815384,-41.4050781652923,
0.));
#122563=CARTESIAN_POINT('Ctrl Pts',(57.2755422525822,-41.3882148268798,
0.));
#122564=CARTESIAN_POINT('Ctrl Pts',(57.2626878751584,-41.3714041819215,
0.));
#122565=CARTESIAN_POINT('Ctrl Pts',(57.2498462101883,-41.3546463114889,
0.));
#122566=CARTESIAN_POINT('Ctrl Pts',(57.237017419142,-41.3379412967889,0.));
#122567=CARTESIAN_POINT('Ctrl Pts',(57.2242016640226,-41.321289219151,0.));
#122568=CARTESIAN_POINT('Ctrl Pts',(57.2113991077325,-41.304690160231,0.));
#122569=CARTESIAN_POINT('Ctrl Pts',(57.1986099143992,-41.288144202187,0.));
#122570=CARTESIAN_POINT('Ctrl Pts',(57.1858342496526,-41.2716514278268,
0.));
#122571=CARTESIAN_POINT('Ctrl Pts',(57.1730722810771,-41.2552119208445,
0.));
#122572=CARTESIAN_POINT('Ctrl Pts',(57.1603241779042,-41.2388257656534,
0.));
#122573=CARTESIAN_POINT('Ctrl Pts',(57.1475901101794,-41.2224930469412,
0.));
#122574=CARTESIAN_POINT('Ctrl Pts',(57.1348702480644,-41.2062138492913,
0.));
#122575=CARTESIAN_POINT('Ctrl Pts',(57.1221647611231,-41.1899882567941,
0.));
#122576=CARTESIAN_POINT('Ctrl Pts',(57.1094738174998,-41.1738163525932,
0.));
#122577=CARTESIAN_POINT('Ctrl Pts',(57.0967975854912,-41.1576982197403,
0.));
#122578=CARTESIAN_POINT('Ctrl Pts',(57.084136235428,-41.1416339422132,0.));
#122579=CARTESIAN_POINT('Ctrl Pts',(57.0714899412091,-41.1256236057437,
0.));
#122580=CARTESIAN_POINT('Ctrl Pts',(57.0588588825266,-41.1096672990125,
0.));
#122581=CARTESIAN_POINT('Ctrl Pts',(57.0462432450637,-41.093765113752,0.));
#122582=CARTESIAN_POINT('Ctrl Pts',(57.0336432158503,-41.0779171422415,
0.));
#122583=CARTESIAN_POINT('Ctrl Pts',(57.0210589791777,-41.0621234751,0.));
#122584=CARTESIAN_POINT('Ctrl Pts',(57.008490713044,-41.0463841993622,0.));
#122585=CARTESIAN_POINT('Ctrl Pts',(56.9959385834768,-41.0306993954021,
0.));
#122586=CARTESIAN_POINT('Ctrl Pts',(56.9834027500178,-41.0150691398988,
0.));
#122587=CARTESIAN_POINT('Ctrl Pts',(56.9708833766183,-40.9994935117307,
0.));
#122588=CARTESIAN_POINT('Ctrl Pts',(56.9583806404069,-40.9839725967121,
0.));
#122589=CARTESIAN_POINT('Ctrl Pts',(56.9458947422541,-40.968506493303,0.));
#122590=CARTESIAN_POINT('Ctrl Pts',(56.9334259139928,-40.9530953164952,
0.));
#122591=CARTESIAN_POINT('Ctrl Pts',(56.9209743960861,-40.9377391857044,
0.));
#122592=CARTESIAN_POINT('Ctrl Pts',(56.9085404164432,-40.9224382132382,
0.));
#122593=CARTESIAN_POINT('Ctrl Pts',(56.8961241708926,-40.9071924937551,
0.));
#122594=CARTESIAN_POINT('Ctrl Pts',(56.8837257978574,-40.8920020903443,
0.));
#122595=CARTESIAN_POINT('Ctrl Pts',(56.8713453765252,-40.8768670342278,
0.));
#122596=CARTESIAN_POINT('Ctrl Pts',(56.8614554317993,-40.8648032759631,
0.));
#122597=CARTESIAN_POINT('Ctrl Pts',(56.8540460739677,-40.8557803680412,
0.));
#122598=CARTESIAN_POINT('Ctrl Pts',(56.8491101022668,-40.8497761671086,
0.));
#122599=CARTESIAN_POINT('Ctrl Pts',(56.8466430164621,-40.8467768343957,
0.));
#122600=CARTESIAN_POINT('Ctrl Pts',(55.3473204966403,-49.8690697110161,
0.));
#122601=CARTESIAN_POINT('Ctrl Pts',(55.3473204966403,-49.8690697110161,
12.));
#122602=CARTESIAN_POINT('Ctrl Pts',(55.3451131058826,-49.8639277221566,
0.));
#122603=CARTESIAN_POINT('Ctrl Pts',(55.3451131058826,-49.8639277221566,
12.));
#122604=CARTESIAN_POINT('Ctrl Pts',(55.34069740326,-49.8536479176833,0.));
#122605=CARTESIAN_POINT('Ctrl Pts',(55.34069740326,-49.8536479176833,12.));
#122606=CARTESIAN_POINT('Ctrl Pts',(55.3340710860055,-49.8382407307107,
0.));
#122607=CARTESIAN_POINT('Ctrl Pts',(55.3340710860055,-49.8382407307107,
12.));
#122608=CARTESIAN_POINT('Ctrl Pts',(55.3252304694602,-49.8177228552377,
0.));
#122609=CARTESIAN_POINT('Ctrl Pts',(55.3252304694602,-49.8177228552377,
12.));
#122610=CARTESIAN_POINT('Ctrl Pts',(55.3141704897766,-49.7921172540628,
0.));
#122611=CARTESIAN_POINT('Ctrl Pts',(55.3141704897766,-49.7921172540628,
12.));
#122612=CARTESIAN_POINT('Ctrl Pts',(55.3031013105853,-49.7665534128535,
0.));
#122613=CARTESIAN_POINT('Ctrl Pts',(55.3031013105853,-49.7665534128535,
12.));
#122614=CARTESIAN_POINT('Ctrl Pts',(55.2920229527546,-49.7410313576508,
0.));
#122615=CARTESIAN_POINT('Ctrl Pts',(55.2920229527546,-49.7410313576508,
12.));
#122616=CARTESIAN_POINT('Ctrl Pts',(55.2809354521515,-49.7155511248531,
0.));
#122617=CARTESIAN_POINT('Ctrl Pts',(55.2809354521515,-49.7155511248531,
12.));
#122618=CARTESIAN_POINT('Ctrl Pts',(55.2698388650025,-49.6901127631627,
0.));
#122619=CARTESIAN_POINT('Ctrl Pts',(55.2698388650025,-49.6901127631627,
12.));
#122620=CARTESIAN_POINT('Ctrl Pts',(55.2587332663783,-49.6647163322266,
0.));
#122621=CARTESIAN_POINT('Ctrl Pts',(55.2587332663783,-49.6647163322266,
12.));
#122622=CARTESIAN_POINT('Ctrl Pts',(55.2476187434057,-49.6393618987473,
0.));
#122623=CARTESIAN_POINT('Ctrl Pts',(55.2476187434057,-49.6393618987473,
12.));
#122624=CARTESIAN_POINT('Ctrl Pts',(55.2364953899358,-49.6140495332804,
0.));
#122625=CARTESIAN_POINT('Ctrl Pts',(55.2364953899358,-49.6140495332804,
12.));
#122626=CARTESIAN_POINT('Ctrl Pts',(55.2253633007666,-49.5887793068352,
0.));
#122627=CARTESIAN_POINT('Ctrl Pts',(55.2253633007666,-49.5887793068352,
12.));
#122628=CARTESIAN_POINT('Ctrl Pts',(55.2142225657013,-49.5635512873435,
0.));
#122629=CARTESIAN_POINT('Ctrl Pts',(55.2142225657013,-49.5635512873435,
12.));
#122630=CARTESIAN_POINT('Ctrl Pts',(55.2030732647312,-49.5383655368074,
0.));
#122631=CARTESIAN_POINT('Ctrl Pts',(55.2030732647312,-49.5383655368074,
12.));
#122632=CARTESIAN_POINT('Ctrl Pts',(55.1919154713647,-49.5132221132992,
0.));
#122633=CARTESIAN_POINT('Ctrl Pts',(55.1919154713647,-49.5132221132992,
12.));
#122634=CARTESIAN_POINT('Ctrl Pts',(55.1807492550119,-49.4881210723966,
0.));
#122635=CARTESIAN_POINT('Ctrl Pts',(55.1807492550119,-49.4881210723966,
12.));
#122636=CARTESIAN_POINT('Ctrl Pts',(55.1695746838174,-49.4630624688793,
0.));
#122637=CARTESIAN_POINT('Ctrl Pts',(55.1695746838174,-49.4630624688793,
12.));
#122638=CARTESIAN_POINT('Ctrl Pts',(55.1583918271116,-49.4380463581965,
0.));
#122639=CARTESIAN_POINT('Ctrl Pts',(55.1583918271116,-49.4380463581965,
12.));
#122640=CARTESIAN_POINT('Ctrl Pts',(55.1472007585183,-49.4130727983201,
0.));
#122641=CARTESIAN_POINT('Ctrl Pts',(55.1472007585183,-49.4130727983201,
12.));
#122642=CARTESIAN_POINT('Ctrl Pts',(55.136001555622,-49.3881418495489,0.));
#122643=CARTESIAN_POINT('Ctrl Pts',(55.136001555622,-49.3881418495489,12.));
#122644=CARTESIAN_POINT('Ctrl Pts',(55.1247942985619,-49.3632535736715,
0.));
#122645=CARTESIAN_POINT('Ctrl Pts',(55.1247942985619,-49.3632535736715,
12.));
#122646=CARTESIAN_POINT('Ctrl Pts',(55.1135790689464,-49.3384080333155,
0.));
#122647=CARTESIAN_POINT('Ctrl Pts',(55.1135790689464,-49.3384080333155,
12.));
#122648=CARTESIAN_POINT('Ctrl Pts',(55.102355948714,-49.3136052912622,0.));
#122649=CARTESIAN_POINT('Ctrl Pts',(55.102355948714,-49.3136052912622,12.));
#122650=CARTESIAN_POINT('Ctrl Pts',(55.0911250188302,-49.2888454096563,
0.));
#122651=CARTESIAN_POINT('Ctrl Pts',(55.0911250188302,-49.2888454096563,
12.));
#122652=CARTESIAN_POINT('Ctrl Pts',(55.079886358701,-49.264128449652,0.));
#122653=CARTESIAN_POINT('Ctrl Pts',(55.079886358701,-49.264128449652,12.));
#122654=CARTESIAN_POINT('Ctrl Pts',(55.0686400468931,-49.2394544718531,
0.));
#122655=CARTESIAN_POINT('Ctrl Pts',(55.0686400468931,-49.2394544718531,
12.));
#122656=CARTESIAN_POINT('Ctrl Pts',(55.0573861615579,-49.2148235365704,
0.));
#122657=CARTESIAN_POINT('Ctrl Pts',(55.0573861615579,-49.2148235365704,
12.));
#122658=CARTESIAN_POINT('Ctrl Pts',(55.0461247809744,-49.1902357041461,
0.));
#122659=CARTESIAN_POINT('Ctrl Pts',(55.0461247809744,-49.1902357041461,
12.));
#122660=CARTESIAN_POINT('Ctrl Pts',(55.0348559840453,-49.1656910352476,
0.));
#122661=CARTESIAN_POINT('Ctrl Pts',(55.0348559840453,-49.1656910352476,
12.));
#122662=CARTESIAN_POINT('Ctrl Pts',(55.0235798508045,-49.1411895911635,
0.));
#122663=CARTESIAN_POINT('Ctrl Pts',(55.0235798508045,-49.1411895911635,
12.));
#122664=CARTESIAN_POINT('Ctrl Pts',(55.012296462186,-49.116731433673,0.));
#122665=CARTESIAN_POINT('Ctrl Pts',(55.012296462186,-49.116731433673,12.));
#122666=CARTESIAN_POINT('Ctrl Pts',(55.0010058998107,-49.0923166249219,
0.));
#122667=CARTESIAN_POINT('Ctrl Pts',(55.0010058998107,-49.0923166249219,
12.));
#122668=CARTESIAN_POINT('Ctrl Pts',(54.9897082457606,-49.067945227287,0.));
#122669=CARTESIAN_POINT('Ctrl Pts',(54.9897082457606,-49.067945227287,12.));
#122670=CARTESIAN_POINT('Ctrl Pts',(54.9784035823765,-49.0436173032528,
0.));
#122671=CARTESIAN_POINT('Ctrl Pts',(54.9784035823765,-49.0436173032528,
12.));
#122672=CARTESIAN_POINT('Ctrl Pts',(54.9670919920029,-49.0193329152479,
0.));
#122673=CARTESIAN_POINT('Ctrl Pts',(54.9670919920029,-49.0193329152479,
12.));
#122674=CARTESIAN_POINT('Ctrl Pts',(54.9557735569943,-48.9950921256527,
0.));
#122675=CARTESIAN_POINT('Ctrl Pts',(54.9557735569943,-48.9950921256527,
12.));
#122676=CARTESIAN_POINT('Ctrl Pts',(54.9444483598378,-48.9708949968795,
0.));
#122677=CARTESIAN_POINT('Ctrl Pts',(54.9444483598378,-48.9708949968795,
12.));
#122678=CARTESIAN_POINT('Ctrl Pts',(54.9331164832423,-48.9467415914269,
0.));
#122679=CARTESIAN_POINT('Ctrl Pts',(54.9331164832423,-48.9467415914269,
12.));
#122680=CARTESIAN_POINT('Ctrl Pts',(54.9217780102355,-48.9226319719369,
0.));
#122681=CARTESIAN_POINT('Ctrl Pts',(54.9217780102355,-48.9226319719369,
12.));
#122682=CARTESIAN_POINT('Ctrl Pts',(54.9104330242742,-48.8985662012528,
0.));
#122683=CARTESIAN_POINT('Ctrl Pts',(54.9104330242742,-48.8985662012528,
12.));
#122684=CARTESIAN_POINT('Ctrl Pts',(54.8990816092953,-48.8745443424477,
0.));
#122685=CARTESIAN_POINT('Ctrl Pts',(54.8990816092953,-48.8745443424477,
12.));
#122686=CARTESIAN_POINT('Ctrl Pts',(54.8877238496565,-48.8505664587974,
0.));
#122687=CARTESIAN_POINT('Ctrl Pts',(54.8877238496565,-48.8505664587974,
12.));
#122688=CARTESIAN_POINT('Ctrl Pts',(54.8763598301037,-48.8266326137622,
0.));
#122689=CARTESIAN_POINT('Ctrl Pts',(54.8763598301037,-48.8266326137622,
12.));
#122690=CARTESIAN_POINT('Ctrl Pts',(54.8649896357285,-48.8027428709614,
0.));
#122691=CARTESIAN_POINT('Ctrl Pts',(54.8649896357285,-48.8027428709614,
12.));
#122692=CARTESIAN_POINT('Ctrl Pts',(54.8536133519292,-48.7788972941438,
0.));
#122693=CARTESIAN_POINT('Ctrl Pts',(54.8536133519292,-48.7788972941438,
12.));
#122694=CARTESIAN_POINT('Ctrl Pts',(54.8422310643763,-48.7550959471601,
0.));
#122695=CARTESIAN_POINT('Ctrl Pts',(54.8422310643763,-48.7550959471601,
12.));
#122696=CARTESIAN_POINT('Ctrl Pts',(54.8308428590344,-48.7313388939845,
0.));
#122697=CARTESIAN_POINT('Ctrl Pts',(54.8308428590344,-48.7313388939845,
12.));
#122698=CARTESIAN_POINT('Ctrl Pts',(54.819448822181,-48.7076261987292,0.));
#122699=CARTESIAN_POINT('Ctrl Pts',(54.819448822181,-48.7076261987292,12.));
#122700=CARTESIAN_POINT('Ctrl Pts',(54.8080490404275,-48.6839579256566,
0.));
#122701=CARTESIAN_POINT('Ctrl Pts',(54.8080490404275,-48.6839579256566,
12.));
#122702=CARTESIAN_POINT('Ctrl Pts',(54.7966436007389,-48.6603341391886,
0.));
#122703=CARTESIAN_POINT('Ctrl Pts',(54.7966436007389,-48.6603341391886,
12.));
#122704=CARTESIAN_POINT('Ctrl Pts',(54.7852325904583,-48.6367549039112,
0.));
#122705=CARTESIAN_POINT('Ctrl Pts',(54.7852325904583,-48.6367549039112,
12.));
#122706=CARTESIAN_POINT('Ctrl Pts',(54.7738160973031,-48.6132202845783,
0.));
#122707=CARTESIAN_POINT('Ctrl Pts',(54.7738160973031,-48.6132202845783,
12.));
#122708=CARTESIAN_POINT('Ctrl Pts',(54.7623942093586,-48.5897303461125,
0.));
#122709=CARTESIAN_POINT('Ctrl Pts',(54.7623942093586,-48.5897303461125,
12.));
#122710=CARTESIAN_POINT('Ctrl Pts',(54.7509670150714,-48.5662851536026,
0.));
#122711=CARTESIAN_POINT('Ctrl Pts',(54.7509670150714,-48.5662851536026,
12.));
#122712=CARTESIAN_POINT('Ctrl Pts',(54.7395346032453,-48.5428847722977,
0.));
#122713=CARTESIAN_POINT('Ctrl Pts',(54.7395346032453,-48.5428847722977,
12.));
#122714=CARTESIAN_POINT('Ctrl Pts',(54.7280970630351,-48.519529267596,0.));
#122715=CARTESIAN_POINT('Ctrl Pts',(54.7280970630351,-48.519529267596,12.));
#122716=CARTESIAN_POINT('Ctrl Pts',(54.716654483948,-48.4962187050457,0.));
#122717=CARTESIAN_POINT('Ctrl Pts',(54.716654483948,-48.4962187050457,12.));
#122718=CARTESIAN_POINT('Ctrl Pts',(54.7052069558497,-48.472953150357,0.));
#122719=CARTESIAN_POINT('Ctrl Pts',(54.7052069558497,-48.472953150357,12.));
#122720=CARTESIAN_POINT('Ctrl Pts',(54.6937545689695,-48.4497326694052,
0.));
#122721=CARTESIAN_POINT('Ctrl Pts',(54.6937545689695,-48.4497326694052,
12.));
#122722=CARTESIAN_POINT('Ctrl Pts',(54.6822974139063,-48.426557328234,0.));
#122723=CARTESIAN_POINT('Ctrl Pts',(54.6822974139063,-48.426557328234,12.));
#122724=CARTESIAN_POINT('Ctrl Pts',(54.6708355816358,-48.4034271930514,
0.));
#122725=CARTESIAN_POINT('Ctrl Pts',(54.6708355816358,-48.4034271930514,
12.));
#122726=CARTESIAN_POINT('Ctrl Pts',(54.6593691635145,-48.3803423302294,
0.));
#122727=CARTESIAN_POINT('Ctrl Pts',(54.6593691635145,-48.3803423302294,
12.));
#122728=CARTESIAN_POINT('Ctrl Pts',(54.6478982512794,-48.3573028063124,
0.));
#122729=CARTESIAN_POINT('Ctrl Pts',(54.6478982512794,-48.3573028063124,
12.));
#122730=CARTESIAN_POINT('Ctrl Pts',(54.6364229370494,-48.3343086880194,
0.));
#122731=CARTESIAN_POINT('Ctrl Pts',(54.6364229370494,-48.3343086880194,
12.));
#122732=CARTESIAN_POINT('Ctrl Pts',(54.6249433133261,-48.3113600422443,
0.));
#122733=CARTESIAN_POINT('Ctrl Pts',(54.6249433133261,-48.3113600422443,
12.));
#122734=CARTESIAN_POINT('Ctrl Pts',(54.6134594729959,-48.2884569360506,
0.));
#122735=CARTESIAN_POINT('Ctrl Pts',(54.6134594729959,-48.2884569360506,
12.));
#122736=CARTESIAN_POINT('Ctrl Pts',(54.6019715093309,-48.2655994366665,
0.));
#122737=CARTESIAN_POINT('Ctrl Pts',(54.6019715093309,-48.2655994366665,
12.));
#122738=CARTESIAN_POINT('Ctrl Pts',(54.5904795159926,-48.2427876114947,
0.));
#122739=CARTESIAN_POINT('Ctrl Pts',(54.5904795159926,-48.2427876114947,
12.));
#122740=CARTESIAN_POINT('Ctrl Pts',(54.5789835870342,-48.2200215281173,
0.));
#122741=CARTESIAN_POINT('Ctrl Pts',(54.5789835870342,-48.2200215281173,
12.));
#122742=CARTESIAN_POINT('Ctrl Pts',(54.5674838169041,-48.1973012542966,
0.));
#122743=CARTESIAN_POINT('Ctrl Pts',(54.5674838169041,-48.1973012542966,
12.));
#122744=CARTESIAN_POINT('Ctrl Pts',(54.5559803004492,-48.1746268579736,
0.));
#122745=CARTESIAN_POINT('Ctrl Pts',(54.5559803004492,-48.1746268579736,
12.));
#122746=CARTESIAN_POINT('Ctrl Pts',(54.5444731329201,-48.1519984072622,
0.));
#122747=CARTESIAN_POINT('Ctrl Pts',(54.5444731329201,-48.1519984072622,
12.));
#122748=CARTESIAN_POINT('Ctrl Pts',(54.5329624099721,-48.1294159704573,
0.));
#122749=CARTESIAN_POINT('Ctrl Pts',(54.5329624099721,-48.1294159704573,
12.));
#122750=CARTESIAN_POINT('Ctrl Pts',(54.5214482276678,-48.1068796160405,
0.));
#122751=CARTESIAN_POINT('Ctrl Pts',(54.5214482276678,-48.1068796160405,
12.));
#122752=CARTESIAN_POINT('Ctrl Pts',(54.5099306824786,-48.0843894126806,
0.));
#122753=CARTESIAN_POINT('Ctrl Pts',(54.5099306824786,-48.0843894126806,
12.));
#122754=CARTESIAN_POINT('Ctrl Pts',(54.4984098712886,-48.0619454292324,
0.));
#122755=CARTESIAN_POINT('Ctrl Pts',(54.4984098712886,-48.0619454292324,
12.));
#122756=CARTESIAN_POINT('Ctrl Pts',(54.4868858913971,-48.0395477347298,
0.));
#122757=CARTESIAN_POINT('Ctrl Pts',(54.4868858913971,-48.0395477347298,
12.));
#122758=CARTESIAN_POINT('Ctrl Pts',(54.4753588405215,-48.0171963983924,
0.));
#122759=CARTESIAN_POINT('Ctrl Pts',(54.4753588405215,-48.0171963983924,
12.));
#122760=CARTESIAN_POINT('Ctrl Pts',(54.4638288168003,-47.9948914896326,
0.));
#122761=CARTESIAN_POINT('Ctrl Pts',(54.4638288168003,-47.9948914896326,
12.));
#122762=CARTESIAN_POINT('Ctrl Pts',(54.4522959187955,-47.9726330780572,
0.));
#122763=CARTESIAN_POINT('Ctrl Pts',(54.4522959187955,-47.9726330780572,
12.));
#122764=CARTESIAN_POINT('Ctrl Pts',(54.4407602454967,-47.9504212334675,
0.));
#122765=CARTESIAN_POINT('Ctrl Pts',(54.4407602454967,-47.9504212334675,
12.));
#122766=CARTESIAN_POINT('Ctrl Pts',(54.429221896324,-47.9282560258516,0.));
#122767=CARTESIAN_POINT('Ctrl Pts',(54.429221896324,-47.9282560258516,12.));
#122768=CARTESIAN_POINT('Ctrl Pts',(54.4176809711311,-47.9061375253897,
0.));
#122769=CARTESIAN_POINT('Ctrl Pts',(54.4176809711311,-47.9061375253897,
12.));
#122770=CARTESIAN_POINT('Ctrl Pts',(54.4061375702079,-47.8840658024618,
0.));
#122771=CARTESIAN_POINT('Ctrl Pts',(54.4061375702079,-47.8840658024618,
12.));
#122772=CARTESIAN_POINT('Ctrl Pts',(54.3945917942832,-47.8620409276493,
0.));
#122773=CARTESIAN_POINT('Ctrl Pts',(54.3945917942832,-47.8620409276493,
12.));
#122774=CARTESIAN_POINT('Ctrl Pts',(54.3830437445278,-47.8400629717355,
0.));
#122775=CARTESIAN_POINT('Ctrl Pts',(54.3830437445278,-47.8400629717355,
12.));
#122776=CARTESIAN_POINT('Ctrl Pts',(54.3714935225591,-47.8181320056995,
0.));
#122777=CARTESIAN_POINT('Ctrl Pts',(54.3714935225591,-47.8181320056995,
12.));
#122778=CARTESIAN_POINT('Ctrl Pts',(54.3599412304437,-47.7962481007185,
0.));
#122779=CARTESIAN_POINT('Ctrl Pts',(54.3599412304437,-47.7962481007185,
12.));
#122780=CARTESIAN_POINT('Ctrl Pts',(54.3483869707002,-47.7744113281771,
0.));
#122781=CARTESIAN_POINT('Ctrl Pts',(54.3483869707002,-47.7744113281771,
12.));
#122782=CARTESIAN_POINT('Ctrl Pts',(54.3368308463023,-47.7526217596694,
0.));
#122783=CARTESIAN_POINT('Ctrl Pts',(54.3368308463023,-47.7526217596694,
12.));
#122784=CARTESIAN_POINT('Ctrl Pts',(54.3252729606823,-47.7308794669993,
0.));
#122785=CARTESIAN_POINT('Ctrl Pts',(54.3252729606823,-47.7308794669993,
12.));
#122786=CARTESIAN_POINT('Ctrl Pts',(54.3137134177345,-47.7091845221747,
0.));
#122787=CARTESIAN_POINT('Ctrl Pts',(54.3137134177345,-47.7091845221747,
12.));
#122788=CARTESIAN_POINT('Ctrl Pts',(54.302152321819,-47.6875369974087,0.));
#122789=CARTESIAN_POINT('Ctrl Pts',(54.302152321819,-47.6875369974087,12.));
#122790=CARTESIAN_POINT('Ctrl Pts',(54.290589777765,-47.6659369651301,0.));
#122791=CARTESIAN_POINT('Ctrl Pts',(54.290589777765,-47.6659369651301,12.));
#122792=CARTESIAN_POINT('Ctrl Pts',(54.2790258908738,-47.6443844979848,
0.));
#122793=CARTESIAN_POINT('Ctrl Pts',(54.2790258908738,-47.6443844979848,
12.));
#122794=CARTESIAN_POINT('Ctrl Pts',(54.2674607669226,-47.6228796688375,
0.));
#122795=CARTESIAN_POINT('Ctrl Pts',(54.2674607669226,-47.6228796688375,
12.));
#122796=CARTESIAN_POINT('Ctrl Pts',(54.2558945121678,-47.6014225507659,
0.));
#122797=CARTESIAN_POINT('Ctrl Pts',(54.2558945121678,-47.6014225507659,
12.));
#122798=CARTESIAN_POINT('Ctrl Pts',(54.244327233349,-47.5800132170608,0.));
#122799=CARTESIAN_POINT('Ctrl Pts',(54.244327233349,-47.5800132170608,12.));
#122800=CARTESIAN_POINT('Ctrl Pts',(54.2327590376924,-47.5586517412363,
0.));
#122801=CARTESIAN_POINT('Ctrl Pts',(54.2327590376924,-47.5586517412363,
12.));
#122802=CARTESIAN_POINT('Ctrl Pts',(54.2211900329138,-47.5373381970326,
0.));
#122803=CARTESIAN_POINT('Ctrl Pts',(54.2211900329138,-47.5373381970326,
12.));
#122804=CARTESIAN_POINT('Ctrl Pts',(54.209620327223,-47.5160726584174,0.));
#122805=CARTESIAN_POINT('Ctrl Pts',(54.209620327223,-47.5160726584174,12.));
#122806=CARTESIAN_POINT('Ctrl Pts',(54.198050029327,-47.4948551995801,0.));
#122807=CARTESIAN_POINT('Ctrl Pts',(54.198050029327,-47.4948551995801,12.));
#122808=CARTESIAN_POINT('Ctrl Pts',(54.1864792484345,-47.4736858949322,
0.));
#122809=CARTESIAN_POINT('Ctrl Pts',(54.1864792484345,-47.4736858949322,
12.));
#122810=CARTESIAN_POINT('Ctrl Pts',(54.1749080942593,-47.4525648191173,
0.));
#122811=CARTESIAN_POINT('Ctrl Pts',(54.1749080942593,-47.4525648191173,
12.));
#122812=CARTESIAN_POINT('Ctrl Pts',(54.1633366770239,-47.4314920470141,
0.));
#122813=CARTESIAN_POINT('Ctrl Pts',(54.1633366770239,-47.4314920470141,
12.));
#122814=CARTESIAN_POINT('Ctrl Pts',(54.1517651074637,-47.4104676537381,
0.));
#122815=CARTESIAN_POINT('Ctrl Pts',(54.1517651074637,-47.4104676537381,
12.));
#122816=CARTESIAN_POINT('Ctrl Pts',(54.1401934968311,-47.3894917146365,
0.));
#122817=CARTESIAN_POINT('Ctrl Pts',(54.1401934968311,-47.3894917146365,
12.));
#122818=CARTESIAN_POINT('Ctrl Pts',(54.1286219568989,-47.3685643052874,
0.));
#122819=CARTESIAN_POINT('Ctrl Pts',(54.1286219568989,-47.3685643052874,
12.));
#122820=CARTESIAN_POINT('Ctrl Pts',(54.1170505999645,-47.3476855015102,
0.));
#122821=CARTESIAN_POINT('Ctrl Pts',(54.1170505999645,-47.3476855015102,
12.));
#122822=CARTESIAN_POINT('Ctrl Pts',(54.1054795388543,-47.3268553793694,
0.));
#122823=CARTESIAN_POINT('Ctrl Pts',(54.1054795388543,-47.3268553793694,
12.));
#122824=CARTESIAN_POINT('Ctrl Pts',(54.0939088869268,-47.3060740151752,
0.));
#122825=CARTESIAN_POINT('Ctrl Pts',(54.0939088869268,-47.3060740151752,
12.));
#122826=CARTESIAN_POINT('Ctrl Pts',(54.0823387580776,-47.2853414854793,
0.));
#122827=CARTESIAN_POINT('Ctrl Pts',(54.0823387580776,-47.2853414854793,
12.));
#122828=CARTESIAN_POINT('Ctrl Pts',(54.0707692667438,-47.2646578670746,
0.));
#122829=CARTESIAN_POINT('Ctrl Pts',(54.0707692667438,-47.2646578670746,
12.));
#122830=CARTESIAN_POINT('Ctrl Pts',(54.0592005279086,-47.2440232370065,
0.));
#122831=CARTESIAN_POINT('Ctrl Pts',(54.0592005279086,-47.2440232370065,
12.));
#122832=CARTESIAN_POINT('Ctrl Pts',(54.047632657104,-47.2234376725743,0.));
#122833=CARTESIAN_POINT('Ctrl Pts',(54.047632657104,-47.2234376725743,12.));
#122834=CARTESIAN_POINT('Ctrl Pts',(54.0360657704163,-47.202901251334,0.));
#122835=CARTESIAN_POINT('Ctrl Pts',(54.0360657704163,-47.202901251334,12.));
#122836=CARTESIAN_POINT('Ctrl Pts',(54.0244999844893,-47.1824140510926,
0.));
#122837=CARTESIAN_POINT('Ctrl Pts',(54.0244999844893,-47.1824140510926,
12.));
#122838=CARTESIAN_POINT('Ctrl Pts',(54.0129354165297,-47.1619761499087,
0.));
#122839=CARTESIAN_POINT('Ctrl Pts',(54.0129354165297,-47.1619761499087,
12.));
#122840=CARTESIAN_POINT('Ctrl Pts',(54.0013721843118,-47.1415876261035,
0.));
#122841=CARTESIAN_POINT('Ctrl Pts',(54.0013721843118,-47.1415876261035,
12.));
#122842=CARTESIAN_POINT('Ctrl Pts',(53.989810406182,-47.1212485582643,0.));
#122843=CARTESIAN_POINT('Ctrl Pts',(53.989810406182,-47.1212485582643,12.));
#122844=CARTESIAN_POINT('Ctrl Pts',(53.9782502010634,-47.1009590252458,
0.));
#122845=CARTESIAN_POINT('Ctrl Pts',(53.9782502010634,-47.1009590252458,
12.));
#122846=CARTESIAN_POINT('Ctrl Pts',(53.9666916884596,-47.0807191061648,
0.));
#122847=CARTESIAN_POINT('Ctrl Pts',(53.9666916884596,-47.0807191061648,
12.));
#122848=CARTESIAN_POINT('Ctrl Pts',(53.9551349884599,-47.0605288804008,
0.));
#122849=CARTESIAN_POINT('Ctrl Pts',(53.9551349884599,-47.0605288804008,
12.));
#122850=CARTESIAN_POINT('Ctrl Pts',(53.9435802217436,-47.0403884276072,
0.));
#122851=CARTESIAN_POINT('Ctrl Pts',(53.9435802217436,-47.0403884276072,
12.));
#122852=CARTESIAN_POINT('Ctrl Pts',(53.9320275095853,-47.0202978277138,
0.));
#122853=CARTESIAN_POINT('Ctrl Pts',(53.9320275095853,-47.0202978277138,
12.));
#122854=CARTESIAN_POINT('Ctrl Pts',(53.9204769738596,-47.0002571609297,
0.));
#122855=CARTESIAN_POINT('Ctrl Pts',(53.9204769738596,-47.0002571609297,
12.));
#122856=CARTESIAN_POINT('Ctrl Pts',(53.9089287370463,-46.9802665077366,
0.));
#122857=CARTESIAN_POINT('Ctrl Pts',(53.9089287370463,-46.9802665077366,
12.));
#122858=CARTESIAN_POINT('Ctrl Pts',(53.8973829222347,-46.9603259488921,
0.));
#122859=CARTESIAN_POINT('Ctrl Pts',(53.8973829222347,-46.9603259488921,
12.));
#122860=CARTESIAN_POINT('Ctrl Pts',(53.8858396531298,-46.9404355654401,
0.));
#122861=CARTESIAN_POINT('Ctrl Pts',(53.8858396531298,-46.9404355654401,
12.));
#122862=CARTESIAN_POINT('Ctrl Pts',(53.8742990540563,-46.9205954387133,
0.));
#122863=CARTESIAN_POINT('Ctrl Pts',(53.8742990540563,-46.9205954387133,
12.));
#122864=CARTESIAN_POINT('Ctrl Pts',(53.8627612499638,-46.9008056503351,
0.));
#122865=CARTESIAN_POINT('Ctrl Pts',(53.8627612499638,-46.9008056503351,
12.));
#122866=CARTESIAN_POINT('Ctrl Pts',(53.8512263664321,-46.881066282213,0.));
#122867=CARTESIAN_POINT('Ctrl Pts',(53.8512263664321,-46.881066282213,12.));
#122868=CARTESIAN_POINT('Ctrl Pts',(53.8396945296757,-46.8613774165435,
0.));
#122869=CARTESIAN_POINT('Ctrl Pts',(53.8396945296757,-46.8613774165435,
12.));
#122870=CARTESIAN_POINT('Ctrl Pts',(53.8281658665503,-46.841739135822,0.));
#122871=CARTESIAN_POINT('Ctrl Pts',(53.8281658665503,-46.841739135822,12.));
#122872=CARTESIAN_POINT('Ctrl Pts',(53.816640504558,-46.8221515228457,0.));
#122873=CARTESIAN_POINT('Ctrl Pts',(53.816640504558,-46.8221515228457,12.));
#122874=CARTESIAN_POINT('Ctrl Pts',(53.8051185718532,-46.802614660715,0.));
#122875=CARTESIAN_POINT('Ctrl Pts',(53.8051185718532,-46.802614660715,12.));
#122876=CARTESIAN_POINT('Ctrl Pts',(53.793600197248,-46.7831286328278,0.));
#122877=CARTESIAN_POINT('Ctrl Pts',(53.793600197248,-46.7831286328278,12.));
#122878=CARTESIAN_POINT('Ctrl Pts',(53.7820855102182,-46.7636935228861,
0.));
#122879=CARTESIAN_POINT('Ctrl Pts',(53.7820855102182,-46.7636935228861,
12.));
#122880=CARTESIAN_POINT('Ctrl Pts',(53.7705746409075,-46.7443094149045,
0.));
#122881=CARTESIAN_POINT('Ctrl Pts',(53.7705746409075,-46.7443094149045,
12.));
#122882=CARTESIAN_POINT('Ctrl Pts',(53.7590677201342,-46.7249763932129,
0.));
#122883=CARTESIAN_POINT('Ctrl Pts',(53.7590677201342,-46.7249763932129,
12.));
#122884=CARTESIAN_POINT('Ctrl Pts',(53.7475648793946,-46.7056945424559,
0.));
#122885=CARTESIAN_POINT('Ctrl Pts',(53.7475648793946,-46.7056945424559,
12.));
#122886=CARTESIAN_POINT('Ctrl Pts',(53.7360662508675,-46.6864639475862,
0.));
#122887=CARTESIAN_POINT('Ctrl Pts',(53.7360662508675,-46.6864639475862,
12.));
#122888=CARTESIAN_POINT('Ctrl Pts',(53.7245719674221,-46.6672846938752,
0.));
#122889=CARTESIAN_POINT('Ctrl Pts',(53.7245719674221,-46.6672846938752,
12.));
#122890=CARTESIAN_POINT('Ctrl Pts',(53.7130821626262,-46.6481568669217,
0.));
#122891=CARTESIAN_POINT('Ctrl Pts',(53.7130821626262,-46.6481568669217,
12.));
#122892=CARTESIAN_POINT('Ctrl Pts',(53.7015969707541,-46.6290805526559,
0.));
#122893=CARTESIAN_POINT('Ctrl Pts',(53.7015969707541,-46.6290805526559,
12.));
#122894=CARTESIAN_POINT('Ctrl Pts',(53.690116526794,-46.6100558373401,0.));
#122895=CARTESIAN_POINT('Ctrl Pts',(53.690116526794,-46.6100558373401,12.));
#122896=CARTESIAN_POINT('Ctrl Pts',(53.678640966456,-46.5910828075652,0.));
#122897=CARTESIAN_POINT('Ctrl Pts',(53.678640966456,-46.5910828075652,12.));
#122898=CARTESIAN_POINT('Ctrl Pts',(53.6671704261735,-46.572161550259,0.));
#122899=CARTESIAN_POINT('Ctrl Pts',(53.6671704261735,-46.572161550259,12.));
#122900=CARTESIAN_POINT('Ctrl Pts',(53.6557050431069,-46.5532921526899,
0.));
#122901=CARTESIAN_POINT('Ctrl Pts',(53.6557050431069,-46.5532921526899,
12.));
#122902=CARTESIAN_POINT('Ctrl Pts',(53.6442449551455,-46.5344747024677,
0.));
#122903=CARTESIAN_POINT('Ctrl Pts',(53.6442449551455,-46.5344747024677,
12.));
#122904=CARTESIAN_POINT('Ctrl Pts',(53.6327903009097,-46.5157092875377,
0.));
#122905=CARTESIAN_POINT('Ctrl Pts',(53.6327903009097,-46.5157092875377,
12.));
#122906=CARTESIAN_POINT('Ctrl Pts',(53.6213412197542,-46.4969959961779,
0.));
#122907=CARTESIAN_POINT('Ctrl Pts',(53.6213412197542,-46.4969959961779,
12.));
#122908=CARTESIAN_POINT('Ctrl Pts',(53.6098978517869,-46.4783349170182,
0.));
#122909=CARTESIAN_POINT('Ctrl Pts',(53.6098978517869,-46.4783349170182,
12.));
#122910=CARTESIAN_POINT('Ctrl Pts',(53.5984603378861,-46.4597261390526,
0.));
#122911=CARTESIAN_POINT('Ctrl Pts',(53.5984603378861,-46.4597261390526,
12.));
#122912=CARTESIAN_POINT('Ctrl Pts',(53.5870288197161,-46.4411697516474,
0.));
#122913=CARTESIAN_POINT('Ctrl Pts',(53.5870288197161,-46.4411697516474,
12.));
#122914=CARTESIAN_POINT('Ctrl Pts',(53.5756034397464,-46.422665844546,0.));
#122915=CARTESIAN_POINT('Ctrl Pts',(53.5756034397464,-46.422665844546,12.));
#122916=CARTESIAN_POINT('Ctrl Pts',(53.5641843412537,-46.4042145078682,
0.));
#122917=CARTESIAN_POINT('Ctrl Pts',(53.5641843412537,-46.4042145078682,
12.));
#122918=CARTESIAN_POINT('Ctrl Pts',(53.5527716683029,-46.3858158321044,
0.));
#122919=CARTESIAN_POINT('Ctrl Pts',(53.5527716683029,-46.3858158321044,
12.));
#122920=CARTESIAN_POINT('Ctrl Pts',(53.5413655657323,-46.3674699081043,
0.));
#122921=CARTESIAN_POINT('Ctrl Pts',(53.5413655657323,-46.3674699081043,
12.));
#122922=CARTESIAN_POINT('Ctrl Pts',(53.5299661791396,-46.3491768270664,
0.));
#122923=CARTESIAN_POINT('Ctrl Pts',(53.5299661791396,-46.3491768270664,
12.));
#122924=CARTESIAN_POINT('Ctrl Pts',(53.518573654857,-46.3309366805112,0.));
#122925=CARTESIAN_POINT('Ctrl Pts',(53.518573654857,-46.3309366805112,12.));
#122926=CARTESIAN_POINT('Ctrl Pts',(53.5071881399932,-46.3127495603117,
0.));
#122927=CARTESIAN_POINT('Ctrl Pts',(53.5071881399932,-46.3127495603117,
12.));
#122928=CARTESIAN_POINT('Ctrl Pts',(53.4958097825019,-46.2946155587428,
0.));
#122929=CARTESIAN_POINT('Ctrl Pts',(53.4958097825019,-46.2946155587428,
12.));
#122930=CARTESIAN_POINT('Ctrl Pts',(53.4844387312414,-46.2765347685198,
0.));
#122931=CARTESIAN_POINT('Ctrl Pts',(53.4844387312414,-46.2765347685198,
12.));
#122932=CARTESIAN_POINT('Ctrl Pts',(53.4730751360359,-46.2585072828343,
0.));
#122933=CARTESIAN_POINT('Ctrl Pts',(53.4730751360359,-46.2585072828343,
12.));
#122934=CARTESIAN_POINT('Ctrl Pts',(53.4617191477382,-46.2405331953872,
0.));
#122935=CARTESIAN_POINT('Ctrl Pts',(53.4617191477382,-46.2405331953872,
12.));
#122936=CARTESIAN_POINT('Ctrl Pts',(53.4503709181158,-46.2226126003185,
0.));
#122937=CARTESIAN_POINT('Ctrl Pts',(53.4503709181158,-46.2226126003185,
12.));
#122938=CARTESIAN_POINT('Ctrl Pts',(53.4390305997263,-46.2047455921276,
0.));
#122939=CARTESIAN_POINT('Ctrl Pts',(53.4390305997263,-46.2047455921276,
12.));
#122940=CARTESIAN_POINT('Ctrl Pts',(53.4276983458129,-46.1869322656027,
0.));
#122941=CARTESIAN_POINT('Ctrl Pts',(53.4276983458129,-46.1869322656027,
12.));
#122942=CARTESIAN_POINT('Ctrl Pts',(53.4163743101534,-46.1691727157149,
0.));
#122943=CARTESIAN_POINT('Ctrl Pts',(53.4163743101534,-46.1691727157149,
12.));
#122944=CARTESIAN_POINT('Ctrl Pts',(53.4050586470463,-46.1514670376035,
0.));
#122945=CARTESIAN_POINT('Ctrl Pts',(53.4050586470463,-46.1514670376035,
12.));
#122946=CARTESIAN_POINT('Ctrl Pts',(53.3937515116572,-46.1338153268116,
0.));
#122947=CARTESIAN_POINT('Ctrl Pts',(53.3937515116572,-46.1338153268116,
12.));
#122948=CARTESIAN_POINT('Ctrl Pts',(53.3824530603284,-46.1162176794891,
0.));
#122949=CARTESIAN_POINT('Ctrl Pts',(53.3824530603284,-46.1162176794891,
12.));
#122950=CARTESIAN_POINT('Ctrl Pts',(53.3711634508426,-46.0986741925646,
0.));
#122951=CARTESIAN_POINT('Ctrl Pts',(53.3711634508426,-46.0986741925646,
12.));
#122952=CARTESIAN_POINT('Ctrl Pts',(53.3598828428519,-46.0811849640195,
0.));
#122953=CARTESIAN_POINT('Ctrl Pts',(53.3598828428519,-46.0811849640195,
12.));
#122954=CARTESIAN_POINT('Ctrl Pts',(53.3486113975868,-46.0637500926954,
0.));
#122955=CARTESIAN_POINT('Ctrl Pts',(53.3486113975868,-46.0637500926954,
12.));
#122956=CARTESIAN_POINT('Ctrl Pts',(53.3373492770647,-46.046369677778,0.));
#122957=CARTESIAN_POINT('Ctrl Pts',(53.3373492770647,-46.046369677778,12.));
#122958=CARTESIAN_POINT('Ctrl Pts',(53.3260966434277,-46.0290438183598,
0.));
#122959=CARTESIAN_POINT('Ctrl Pts',(53.3260966434277,-46.0290438183598,
12.));
#122960=CARTESIAN_POINT('Ctrl Pts',(53.3148536582658,-46.0117726129893,
0.));
#122961=CARTESIAN_POINT('Ctrl Pts',(53.3148536582658,-46.0117726129893,
12.));
#122962=CARTESIAN_POINT('Ctrl Pts',(53.3036204818367,-45.9945561591486,
0.));
#122963=CARTESIAN_POINT('Ctrl Pts',(53.3036204818367,-45.9945561591486,
12.));
#122964=CARTESIAN_POINT('Ctrl Pts',(53.2923972745585,-45.9773945542415,
0.));
#122965=CARTESIAN_POINT('Ctrl Pts',(53.2923972745585,-45.9773945542415,
12.));
#122966=CARTESIAN_POINT('Ctrl Pts',(53.2811841987945,-45.9602878967715,
0.));
#122967=CARTESIAN_POINT('Ctrl Pts',(53.2811841987945,-45.9602878967715,
12.));
#122968=CARTESIAN_POINT('Ctrl Pts',(53.2699814203097,-45.9432362873001,
0.));
#122969=CARTESIAN_POINT('Ctrl Pts',(53.2699814203097,-45.9432362873001,
12.));
#122970=CARTESIAN_POINT('Ctrl Pts',(53.2587891103835,-45.9262398298323,
0.));
#122971=CARTESIAN_POINT('Ctrl Pts',(53.2587891103835,-45.9262398298323,
12.));
#122972=CARTESIAN_POINT('Ctrl Pts',(53.2476074459977,-45.9092986319343,
0.));
#122973=CARTESIAN_POINT('Ctrl Pts',(53.2476074459977,-45.9092986319343,
12.));
#122974=CARTESIAN_POINT('Ctrl Pts',(53.2364366054276,-45.8924128018354,
0.));
#122975=CARTESIAN_POINT('Ctrl Pts',(53.2364366054276,-45.8924128018354,
12.));
#122976=CARTESIAN_POINT('Ctrl Pts',(53.2252767643652,-45.8755824458715,
0.));
#122977=CARTESIAN_POINT('Ctrl Pts',(53.2252767643652,-45.8755824458715,
12.));
#122978=CARTESIAN_POINT('Ctrl Pts',(53.2141280925458,-45.8588076662598,
0.));
#122979=CARTESIAN_POINT('Ctrl Pts',(53.2141280925458,-45.8588076662598,
12.));
#122980=CARTESIAN_POINT('Ctrl Pts',(53.2029907483602,-45.8420885575386,
0.));
#122981=CARTESIAN_POINT('Ctrl Pts',(53.2029907483602,-45.8420885575386,
12.));
#122982=CARTESIAN_POINT('Ctrl Pts',(53.1918648840598,-45.8254252100003,
0.));
#122983=CARTESIAN_POINT('Ctrl Pts',(53.1918648840598,-45.8254252100003,
12.));
#122984=CARTESIAN_POINT('Ctrl Pts',(53.1807506560977,-45.8088177165124,
0.));
#122985=CARTESIAN_POINT('Ctrl Pts',(53.1807506560977,-45.8088177165124,
12.));
#122986=CARTESIAN_POINT('Ctrl Pts',(53.1696482334487,-45.7922661780005,
0.));
#122987=CARTESIAN_POINT('Ctrl Pts',(53.1696482334487,-45.7922661780005,
12.));
#122988=CARTESIAN_POINT('Ctrl Pts',(53.158557807638,-45.7757707100568,0.));
#122989=CARTESIAN_POINT('Ctrl Pts',(53.158557807638,-45.7757707100568,12.));
#122990=CARTESIAN_POINT('Ctrl Pts',(53.147479599594,-45.7593314474413,0.));
#122991=CARTESIAN_POINT('Ctrl Pts',(53.147479599594,-45.7593314474413,12.));
#122992=CARTESIAN_POINT('Ctrl Pts',(53.136413838457,-45.7429485300727,0.));
#122993=CARTESIAN_POINT('Ctrl Pts',(53.136413838457,-45.7429485300727,12.));
#122994=CARTESIAN_POINT('Ctrl Pts',(53.1253607414806,-45.7266220896951,
0.));
#122995=CARTESIAN_POINT('Ctrl Pts',(53.1253607414806,-45.7266220896951,
12.));
#122996=CARTESIAN_POINT('Ctrl Pts',(53.1143204954981,-45.7103522376744,
0.));
#122997=CARTESIAN_POINT('Ctrl Pts',(53.1143204954981,-45.7103522376744,
12.));
#122998=CARTESIAN_POINT('Ctrl Pts',(53.1032932329074,-45.6941390489239,
0.));
#122999=CARTESIAN_POINT('Ctrl Pts',(53.1032932329074,-45.6941390489239,
12.));
#123000=CARTESIAN_POINT('Ctrl Pts',(53.0922790298736,-45.6779825614486,
0.));
#123001=CARTESIAN_POINT('Ctrl Pts',(53.0922790298736,-45.6779825614486,
12.));
#123002=CARTESIAN_POINT('Ctrl Pts',(53.083478145185,-45.665102743948,0.));
#123003=CARTESIAN_POINT('Ctrl Pts',(53.083478145185,-45.665102743948,12.));
#123004=CARTESIAN_POINT('Ctrl Pts',(53.0768833804386,-45.6554684028296,
0.));
#123005=CARTESIAN_POINT('Ctrl Pts',(53.0768833804386,-45.6554684028296,
12.));
#123006=CARTESIAN_POINT('Ctrl Pts',(53.0724894921921,-45.6490568514146,
0.));
#123007=CARTESIAN_POINT('Ctrl Pts',(53.0724894921921,-45.6490568514146,
12.));
#123008=CARTESIAN_POINT('Ctrl Pts',(53.0702932034641,-45.6458539113724,
0.));
#123009=CARTESIAN_POINT('Ctrl Pts',(53.0702932034641,-45.6458539113724,
12.));
#123010=CARTESIAN_POINT('',(53.0702932034641,-45.6458539113724,12.));
#123011=CARTESIAN_POINT('Ctrl Pts',(53.0702932034641,-45.6458539113724,
12.));
#123012=CARTESIAN_POINT('Ctrl Pts',(53.0724894921921,-45.6490568514146,
12.));
#123013=CARTESIAN_POINT('Ctrl Pts',(53.0768833804386,-45.6554684028296,
12.));
#123014=CARTESIAN_POINT('Ctrl Pts',(53.083478145185,-45.665102743948,12.));
#123015=CARTESIAN_POINT('Ctrl Pts',(53.0922790298736,-45.6779825614486,
12.));
#123016=CARTESIAN_POINT('Ctrl Pts',(53.1032932329074,-45.6941390489239,
12.));
#123017=CARTESIAN_POINT('Ctrl Pts',(53.1143204954981,-45.7103522376744,
12.));
#123018=CARTESIAN_POINT('Ctrl Pts',(53.1253607414806,-45.7266220896951,
12.));
#123019=CARTESIAN_POINT('Ctrl Pts',(53.136413838457,-45.7429485300727,12.));
#123020=CARTESIAN_POINT('Ctrl Pts',(53.147479599594,-45.7593314474413,12.));
#123021=CARTESIAN_POINT('Ctrl Pts',(53.158557807638,-45.7757707100568,12.));
#123022=CARTESIAN_POINT('Ctrl Pts',(53.1696482334487,-45.7922661780005,
12.));
#123023=CARTESIAN_POINT('Ctrl Pts',(53.1807506560977,-45.8088177165124,
12.));
#123024=CARTESIAN_POINT('Ctrl Pts',(53.1918648840598,-45.8254252100003,
12.));
#123025=CARTESIAN_POINT('Ctrl Pts',(53.2029907483602,-45.8420885575386,
12.));
#123026=CARTESIAN_POINT('Ctrl Pts',(53.2141280925458,-45.8588076662598,
12.));
#123027=CARTESIAN_POINT('Ctrl Pts',(53.2252767643652,-45.8755824458715,
12.));
#123028=CARTESIAN_POINT('Ctrl Pts',(53.2364366054276,-45.8924128018354,
12.));
#123029=CARTESIAN_POINT('Ctrl Pts',(53.2476074459977,-45.9092986319343,
12.));
#123030=CARTESIAN_POINT('Ctrl Pts',(53.2587891103835,-45.9262398298323,
12.));
#123031=CARTESIAN_POINT('Ctrl Pts',(53.2699814203097,-45.9432362873001,
12.));
#123032=CARTESIAN_POINT('Ctrl Pts',(53.2811841987945,-45.9602878967715,
12.));
#123033=CARTESIAN_POINT('Ctrl Pts',(53.2923972745585,-45.9773945542415,
12.));
#123034=CARTESIAN_POINT('Ctrl Pts',(53.3036204818367,-45.9945561591486,
12.));
#123035=CARTESIAN_POINT('Ctrl Pts',(53.3148536582658,-46.0117726129893,
12.));
#123036=CARTESIAN_POINT('Ctrl Pts',(53.3260966434277,-46.0290438183598,
12.));
#123037=CARTESIAN_POINT('Ctrl Pts',(53.3373492770647,-46.046369677778,12.));
#123038=CARTESIAN_POINT('Ctrl Pts',(53.3486113975868,-46.0637500926954,
12.));
#123039=CARTESIAN_POINT('Ctrl Pts',(53.3598828428519,-46.0811849640195,
12.));
#123040=CARTESIAN_POINT('Ctrl Pts',(53.3711634508426,-46.0986741925646,
12.));
#123041=CARTESIAN_POINT('Ctrl Pts',(53.3824530603284,-46.1162176794891,
12.));
#123042=CARTESIAN_POINT('Ctrl Pts',(53.3937515116572,-46.1338153268116,
12.));
#123043=CARTESIAN_POINT('Ctrl Pts',(53.4050586470463,-46.1514670376035,
12.));
#123044=CARTESIAN_POINT('Ctrl Pts',(53.4163743101534,-46.1691727157149,
12.));
#123045=CARTESIAN_POINT('Ctrl Pts',(53.4276983458129,-46.1869322656027,
12.));
#123046=CARTESIAN_POINT('Ctrl Pts',(53.4390305997263,-46.2047455921276,
12.));
#123047=CARTESIAN_POINT('Ctrl Pts',(53.4503709181158,-46.2226126003185,
12.));
#123048=CARTESIAN_POINT('Ctrl Pts',(53.4617191477382,-46.2405331953872,
12.));
#123049=CARTESIAN_POINT('Ctrl Pts',(53.4730751360359,-46.2585072828343,
12.));
#123050=CARTESIAN_POINT('Ctrl Pts',(53.4844387312414,-46.2765347685198,
12.));
#123051=CARTESIAN_POINT('Ctrl Pts',(53.4958097825019,-46.2946155587428,
12.));
#123052=CARTESIAN_POINT('Ctrl Pts',(53.5071881399932,-46.3127495603117,
12.));
#123053=CARTESIAN_POINT('Ctrl Pts',(53.518573654857,-46.3309366805112,12.));
#123054=CARTESIAN_POINT('Ctrl Pts',(53.5299661791396,-46.3491768270664,
12.));
#123055=CARTESIAN_POINT('Ctrl Pts',(53.5413655657323,-46.3674699081043,
12.));
#123056=CARTESIAN_POINT('Ctrl Pts',(53.5527716683029,-46.3858158321044,
12.));
#123057=CARTESIAN_POINT('Ctrl Pts',(53.5641843412537,-46.4042145078682,
12.));
#123058=CARTESIAN_POINT('Ctrl Pts',(53.5756034397464,-46.422665844546,12.));
#123059=CARTESIAN_POINT('Ctrl Pts',(53.5870288197161,-46.4411697516474,
12.));
#123060=CARTESIAN_POINT('Ctrl Pts',(53.5984603378861,-46.4597261390526,
12.));
#123061=CARTESIAN_POINT('Ctrl Pts',(53.6098978517869,-46.4783349170182,
12.));
#123062=CARTESIAN_POINT('Ctrl Pts',(53.6213412197542,-46.4969959961779,
12.));
#123063=CARTESIAN_POINT('Ctrl Pts',(53.6327903009097,-46.5157092875377,
12.));
#123064=CARTESIAN_POINT('Ctrl Pts',(53.6442449551455,-46.5344747024677,
12.));
#123065=CARTESIAN_POINT('Ctrl Pts',(53.6557050431069,-46.5532921526899,
12.));
#123066=CARTESIAN_POINT('Ctrl Pts',(53.6671704261735,-46.572161550259,12.));
#123067=CARTESIAN_POINT('Ctrl Pts',(53.678640966456,-46.5910828075652,12.));
#123068=CARTESIAN_POINT('Ctrl Pts',(53.690116526794,-46.6100558373401,12.));
#123069=CARTESIAN_POINT('Ctrl Pts',(53.7015969707541,-46.6290805526559,
12.));
#123070=CARTESIAN_POINT('Ctrl Pts',(53.7130821626262,-46.6481568669217,
12.));
#123071=CARTESIAN_POINT('Ctrl Pts',(53.7245719674221,-46.6672846938752,
12.));
#123072=CARTESIAN_POINT('Ctrl Pts',(53.7360662508675,-46.6864639475862,
12.));
#123073=CARTESIAN_POINT('Ctrl Pts',(53.7475648793946,-46.7056945424559,
12.));
#123074=CARTESIAN_POINT('Ctrl Pts',(53.7590677201342,-46.7249763932129,
12.));
#123075=CARTESIAN_POINT('Ctrl Pts',(53.7705746409075,-46.7443094149045,
12.));
#123076=CARTESIAN_POINT('Ctrl Pts',(53.7820855102182,-46.7636935228861,
12.));
#123077=CARTESIAN_POINT('Ctrl Pts',(53.793600197248,-46.7831286328278,12.));
#123078=CARTESIAN_POINT('Ctrl Pts',(53.8051185718532,-46.802614660715,12.));
#123079=CARTESIAN_POINT('Ctrl Pts',(53.816640504558,-46.8221515228457,12.));
#123080=CARTESIAN_POINT('Ctrl Pts',(53.8281658665503,-46.841739135822,12.));
#123081=CARTESIAN_POINT('Ctrl Pts',(53.8396945296757,-46.8613774165435,
12.));
#123082=CARTESIAN_POINT('Ctrl Pts',(53.8512263664321,-46.881066282213,12.));
#123083=CARTESIAN_POINT('Ctrl Pts',(53.8627612499638,-46.9008056503351,
12.));
#123084=CARTESIAN_POINT('Ctrl Pts',(53.8742990540563,-46.9205954387133,
12.));
#123085=CARTESIAN_POINT('Ctrl Pts',(53.8858396531298,-46.9404355654401,
12.));
#123086=CARTESIAN_POINT('Ctrl Pts',(53.8973829222347,-46.9603259488921,
12.));
#123087=CARTESIAN_POINT('Ctrl Pts',(53.9089287370463,-46.9802665077366,
12.));
#123088=CARTESIAN_POINT('Ctrl Pts',(53.9204769738596,-47.0002571609297,
12.));
#123089=CARTESIAN_POINT('Ctrl Pts',(53.9320275095853,-47.0202978277138,
12.));
#123090=CARTESIAN_POINT('Ctrl Pts',(53.9435802217436,-47.0403884276072,
12.));
#123091=CARTESIAN_POINT('Ctrl Pts',(53.9551349884599,-47.0605288804008,
12.));
#123092=CARTESIAN_POINT('Ctrl Pts',(53.9666916884596,-47.0807191061648,
12.));
#123093=CARTESIAN_POINT('Ctrl Pts',(53.9782502010634,-47.1009590252458,
12.));
#123094=CARTESIAN_POINT('Ctrl Pts',(53.989810406182,-47.1212485582643,12.));
#123095=CARTESIAN_POINT('Ctrl Pts',(54.0013721843118,-47.1415876261035,
12.));
#123096=CARTESIAN_POINT('Ctrl Pts',(54.0129354165297,-47.1619761499087,
12.));
#123097=CARTESIAN_POINT('Ctrl Pts',(54.0244999844893,-47.1824140510926,
12.));
#123098=CARTESIAN_POINT('Ctrl Pts',(54.0360657704163,-47.202901251334,12.));
#123099=CARTESIAN_POINT('Ctrl Pts',(54.047632657104,-47.2234376725743,12.));
#123100=CARTESIAN_POINT('Ctrl Pts',(54.0592005279086,-47.2440232370065,
12.));
#123101=CARTESIAN_POINT('Ctrl Pts',(54.0707692667438,-47.2646578670746,
12.));
#123102=CARTESIAN_POINT('Ctrl Pts',(54.0823387580776,-47.2853414854793,
12.));
#123103=CARTESIAN_POINT('Ctrl Pts',(54.0939088869268,-47.3060740151752,
12.));
#123104=CARTESIAN_POINT('Ctrl Pts',(54.1054795388543,-47.3268553793694,
12.));
#123105=CARTESIAN_POINT('Ctrl Pts',(54.1170505999645,-47.3476855015102,
12.));
#123106=CARTESIAN_POINT('Ctrl Pts',(54.1286219568989,-47.3685643052874,
12.));
#123107=CARTESIAN_POINT('Ctrl Pts',(54.1401934968311,-47.3894917146365,
12.));
#123108=CARTESIAN_POINT('Ctrl Pts',(54.1517651074637,-47.4104676537381,
12.));
#123109=CARTESIAN_POINT('Ctrl Pts',(54.1633366770239,-47.4314920470141,
12.));
#123110=CARTESIAN_POINT('Ctrl Pts',(54.1749080942593,-47.4525648191173,
12.));
#123111=CARTESIAN_POINT('Ctrl Pts',(54.1864792484345,-47.4736858949322,
12.));
#123112=CARTESIAN_POINT('Ctrl Pts',(54.198050029327,-47.4948551995801,12.));
#123113=CARTESIAN_POINT('Ctrl Pts',(54.209620327223,-47.5160726584174,12.));
#123114=CARTESIAN_POINT('Ctrl Pts',(54.2211900329138,-47.5373381970326,
12.));
#123115=CARTESIAN_POINT('Ctrl Pts',(54.2327590376924,-47.5586517412363,
12.));
#123116=CARTESIAN_POINT('Ctrl Pts',(54.244327233349,-47.5800132170608,12.));
#123117=CARTESIAN_POINT('Ctrl Pts',(54.2558945121678,-47.6014225507659,
12.));
#123118=CARTESIAN_POINT('Ctrl Pts',(54.2674607669226,-47.6228796688375,
12.));
#123119=CARTESIAN_POINT('Ctrl Pts',(54.2790258908738,-47.6443844979848,
12.));
#123120=CARTESIAN_POINT('Ctrl Pts',(54.290589777765,-47.6659369651301,12.));
#123121=CARTESIAN_POINT('Ctrl Pts',(54.302152321819,-47.6875369974087,12.));
#123122=CARTESIAN_POINT('Ctrl Pts',(54.3137134177345,-47.7091845221747,
12.));
#123123=CARTESIAN_POINT('Ctrl Pts',(54.3252729606823,-47.7308794669993,
12.));
#123124=CARTESIAN_POINT('Ctrl Pts',(54.3368308463023,-47.7526217596694,
12.));
#123125=CARTESIAN_POINT('Ctrl Pts',(54.3483869707002,-47.7744113281771,
12.));
#123126=CARTESIAN_POINT('Ctrl Pts',(54.3599412304437,-47.7962481007185,
12.));
#123127=CARTESIAN_POINT('Ctrl Pts',(54.3714935225591,-47.8181320056995,
12.));
#123128=CARTESIAN_POINT('Ctrl Pts',(54.3830437445278,-47.8400629717355,
12.));
#123129=CARTESIAN_POINT('Ctrl Pts',(54.3945917942832,-47.8620409276493,
12.));
#123130=CARTESIAN_POINT('Ctrl Pts',(54.4061375702079,-47.8840658024618,
12.));
#123131=CARTESIAN_POINT('Ctrl Pts',(54.4176809711311,-47.9061375253897,
12.));
#123132=CARTESIAN_POINT('Ctrl Pts',(54.429221896324,-47.9282560258516,12.));
#123133=CARTESIAN_POINT('Ctrl Pts',(54.4407602454967,-47.9504212334675,
12.));
#123134=CARTESIAN_POINT('Ctrl Pts',(54.4522959187955,-47.9726330780572,
12.));
#123135=CARTESIAN_POINT('Ctrl Pts',(54.4638288168003,-47.9948914896326,
12.));
#123136=CARTESIAN_POINT('Ctrl Pts',(54.4753588405215,-48.0171963983924,
12.));
#123137=CARTESIAN_POINT('Ctrl Pts',(54.4868858913971,-48.0395477347298,
12.));
#123138=CARTESIAN_POINT('Ctrl Pts',(54.4984098712886,-48.0619454292324,
12.));
#123139=CARTESIAN_POINT('Ctrl Pts',(54.5099306824786,-48.0843894126806,
12.));
#123140=CARTESIAN_POINT('Ctrl Pts',(54.5214482276678,-48.1068796160405,
12.));
#123141=CARTESIAN_POINT('Ctrl Pts',(54.5329624099721,-48.1294159704573,
12.));
#123142=CARTESIAN_POINT('Ctrl Pts',(54.5444731329201,-48.1519984072622,
12.));
#123143=CARTESIAN_POINT('Ctrl Pts',(54.5559803004492,-48.1746268579736,
12.));
#123144=CARTESIAN_POINT('Ctrl Pts',(54.5674838169041,-48.1973012542966,
12.));
#123145=CARTESIAN_POINT('Ctrl Pts',(54.5789835870342,-48.2200215281173,
12.));
#123146=CARTESIAN_POINT('Ctrl Pts',(54.5904795159926,-48.2427876114947,
12.));
#123147=CARTESIAN_POINT('Ctrl Pts',(54.6019715093309,-48.2655994366665,
12.));
#123148=CARTESIAN_POINT('Ctrl Pts',(54.6134594729959,-48.2884569360506,
12.));
#123149=CARTESIAN_POINT('Ctrl Pts',(54.6249433133261,-48.3113600422443,
12.));
#123150=CARTESIAN_POINT('Ctrl Pts',(54.6364229370494,-48.3343086880194,
12.));
#123151=CARTESIAN_POINT('Ctrl Pts',(54.6478982512794,-48.3573028063124,
12.));
#123152=CARTESIAN_POINT('Ctrl Pts',(54.6593691635145,-48.3803423302294,
12.));
#123153=CARTESIAN_POINT('Ctrl Pts',(54.6708355816358,-48.4034271930514,
12.));
#123154=CARTESIAN_POINT('Ctrl Pts',(54.6822974139063,-48.426557328234,12.));
#123155=CARTESIAN_POINT('Ctrl Pts',(54.6937545689695,-48.4497326694052,
12.));
#123156=CARTESIAN_POINT('Ctrl Pts',(54.7052069558497,-48.472953150357,12.));
#123157=CARTESIAN_POINT('Ctrl Pts',(54.716654483948,-48.4962187050457,12.));
#123158=CARTESIAN_POINT('Ctrl Pts',(54.7280970630351,-48.519529267596,12.));
#123159=CARTESIAN_POINT('Ctrl Pts',(54.7395346032453,-48.5428847722977,
12.));
#123160=CARTESIAN_POINT('Ctrl Pts',(54.7509670150714,-48.5662851536026,
12.));
#123161=CARTESIAN_POINT('Ctrl Pts',(54.7623942093586,-48.5897303461125,
12.));
#123162=CARTESIAN_POINT('Ctrl Pts',(54.7738160973031,-48.6132202845783,
12.));
#123163=CARTESIAN_POINT('Ctrl Pts',(54.7852325904583,-48.6367549039112,
12.));
#123164=CARTESIAN_POINT('Ctrl Pts',(54.7966436007389,-48.6603341391886,
12.));
#123165=CARTESIAN_POINT('Ctrl Pts',(54.8080490404275,-48.6839579256566,
12.));
#123166=CARTESIAN_POINT('Ctrl Pts',(54.819448822181,-48.7076261987292,12.));
#123167=CARTESIAN_POINT('Ctrl Pts',(54.8308428590344,-48.7313388939845,
12.));
#123168=CARTESIAN_POINT('Ctrl Pts',(54.8422310643763,-48.7550959471601,
12.));
#123169=CARTESIAN_POINT('Ctrl Pts',(54.8536133519292,-48.7788972941438,
12.));
#123170=CARTESIAN_POINT('Ctrl Pts',(54.8649896357285,-48.8027428709614,
12.));
#123171=CARTESIAN_POINT('Ctrl Pts',(54.8763598301037,-48.8266326137622,
12.));
#123172=CARTESIAN_POINT('Ctrl Pts',(54.8877238496565,-48.8505664587974,
12.));
#123173=CARTESIAN_POINT('Ctrl Pts',(54.8990816092953,-48.8745443424477,
12.));
#123174=CARTESIAN_POINT('Ctrl Pts',(54.9104330242742,-48.8985662012528,
12.));
#123175=CARTESIAN_POINT('Ctrl Pts',(54.9217780102355,-48.9226319719369,
12.));
#123176=CARTESIAN_POINT('Ctrl Pts',(54.9331164832423,-48.9467415914269,
12.));
#123177=CARTESIAN_POINT('Ctrl Pts',(54.9444483598378,-48.9708949968795,
12.));
#123178=CARTESIAN_POINT('Ctrl Pts',(54.9557735569943,-48.9950921256527,
12.));
#123179=CARTESIAN_POINT('Ctrl Pts',(54.9670919920029,-49.0193329152479,
12.));
#123180=CARTESIAN_POINT('Ctrl Pts',(54.9784035823765,-49.0436173032528,
12.));
#123181=CARTESIAN_POINT('Ctrl Pts',(54.9897082457606,-49.067945227287,12.));
#123182=CARTESIAN_POINT('Ctrl Pts',(55.0010058998107,-49.0923166249219,
12.));
#123183=CARTESIAN_POINT('Ctrl Pts',(55.012296462186,-49.116731433673,12.));
#123184=CARTESIAN_POINT('Ctrl Pts',(55.0235798508045,-49.1411895911635,
12.));
#123185=CARTESIAN_POINT('Ctrl Pts',(55.0348559840453,-49.1656910352476,
12.));
#123186=CARTESIAN_POINT('Ctrl Pts',(55.0461247809744,-49.1902357041461,
12.));
#123187=CARTESIAN_POINT('Ctrl Pts',(55.0573861615579,-49.2148235365704,
12.));
#123188=CARTESIAN_POINT('Ctrl Pts',(55.0686400468931,-49.2394544718531,
12.));
#123189=CARTESIAN_POINT('Ctrl Pts',(55.079886358701,-49.264128449652,12.));
#123190=CARTESIAN_POINT('Ctrl Pts',(55.0911250188302,-49.2888454096563,
12.));
#123191=CARTESIAN_POINT('Ctrl Pts',(55.102355948714,-49.3136052912622,12.));
#123192=CARTESIAN_POINT('Ctrl Pts',(55.1135790689464,-49.3384080333155,
12.));
#123193=CARTESIAN_POINT('Ctrl Pts',(55.1247942985619,-49.3632535736715,
12.));
#123194=CARTESIAN_POINT('Ctrl Pts',(55.136001555622,-49.3881418495489,12.));
#123195=CARTESIAN_POINT('Ctrl Pts',(55.1472007585183,-49.4130727983201,
12.));
#123196=CARTESIAN_POINT('Ctrl Pts',(55.1583918271116,-49.4380463581965,
12.));
#123197=CARTESIAN_POINT('Ctrl Pts',(55.1695746838174,-49.4630624688793,
12.));
#123198=CARTESIAN_POINT('Ctrl Pts',(55.1807492550119,-49.4881210723966,
12.));
#123199=CARTESIAN_POINT('Ctrl Pts',(55.1919154713647,-49.5132221132992,
12.));
#123200=CARTESIAN_POINT('Ctrl Pts',(55.2014798624094,-49.534774899476,12.));
#123201=CARTESIAN_POINT('Ctrl Pts',(55.2088081099093,-49.5513218524491,
12.));
#123202=CARTESIAN_POINT('Ctrl Pts',(55.2139039604723,-49.5628442142135,
12.));
#123203=CARTESIAN_POINT('Ctrl Pts',(55.216769915134,-49.5693295981931,12.));
#123204=CARTESIAN_POINT('Ctrl Pts',(55.2174072001497,-49.5707719660643,
12.));
#123205=CARTESIAN_POINT('',(53.0702932034641,-45.6458539113724,0.));
#123206=CARTESIAN_POINT('',(53.0702932034641,-45.6458539113724,0.));
#123207=CARTESIAN_POINT('Ctrl Pts',(55.2174072001497,-49.5707719660643,
0.));
#123208=CARTESIAN_POINT('Ctrl Pts',(55.216769915134,-49.5693295981931,0.));
#123209=CARTESIAN_POINT('Ctrl Pts',(55.2139039604723,-49.5628442142135,
0.));
#123210=CARTESIAN_POINT('Ctrl Pts',(55.2088081099093,-49.5513218524491,
0.));
#123211=CARTESIAN_POINT('Ctrl Pts',(55.2014798624094,-49.534774899476,0.));
#123212=CARTESIAN_POINT('Ctrl Pts',(55.1919154713647,-49.5132221132992,
0.));
#123213=CARTESIAN_POINT('Ctrl Pts',(55.1807492550119,-49.4881210723966,
0.));
#123214=CARTESIAN_POINT('Ctrl Pts',(55.1695746838174,-49.4630624688793,
0.));
#123215=CARTESIAN_POINT('Ctrl Pts',(55.1583918271116,-49.4380463581965,
0.));
#123216=CARTESIAN_POINT('Ctrl Pts',(55.1472007585183,-49.4130727983201,
0.));
#123217=CARTESIAN_POINT('Ctrl Pts',(55.136001555622,-49.3881418495489,0.));
#123218=CARTESIAN_POINT('Ctrl Pts',(55.1247942985619,-49.3632535736715,
0.));
#123219=CARTESIAN_POINT('Ctrl Pts',(55.1135790689464,-49.3384080333155,
0.));
#123220=CARTESIAN_POINT('Ctrl Pts',(55.102355948714,-49.3136052912622,0.));
#123221=CARTESIAN_POINT('Ctrl Pts',(55.0911250188302,-49.2888454096563,
0.));
#123222=CARTESIAN_POINT('Ctrl Pts',(55.079886358701,-49.264128449652,0.));
#123223=CARTESIAN_POINT('Ctrl Pts',(55.0686400468931,-49.2394544718531,
0.));
#123224=CARTESIAN_POINT('Ctrl Pts',(55.0573861615579,-49.2148235365704,
0.));
#123225=CARTESIAN_POINT('Ctrl Pts',(55.0461247809744,-49.1902357041461,
0.));
#123226=CARTESIAN_POINT('Ctrl Pts',(55.0348559840453,-49.1656910352476,
0.));
#123227=CARTESIAN_POINT('Ctrl Pts',(55.0235798508045,-49.1411895911635,
0.));
#123228=CARTESIAN_POINT('Ctrl Pts',(55.012296462186,-49.116731433673,0.));
#123229=CARTESIAN_POINT('Ctrl Pts',(55.0010058998107,-49.0923166249219,
0.));
#123230=CARTESIAN_POINT('Ctrl Pts',(54.9897082457606,-49.067945227287,0.));
#123231=CARTESIAN_POINT('Ctrl Pts',(54.9784035823765,-49.0436173032528,
0.));
#123232=CARTESIAN_POINT('Ctrl Pts',(54.9670919920029,-49.0193329152479,
0.));
#123233=CARTESIAN_POINT('Ctrl Pts',(54.9557735569943,-48.9950921256527,
0.));
#123234=CARTESIAN_POINT('Ctrl Pts',(54.9444483598378,-48.9708949968795,
0.));
#123235=CARTESIAN_POINT('Ctrl Pts',(54.9331164832423,-48.9467415914269,
0.));
#123236=CARTESIAN_POINT('Ctrl Pts',(54.9217780102355,-48.9226319719369,
0.));
#123237=CARTESIAN_POINT('Ctrl Pts',(54.9104330242742,-48.8985662012528,
0.));
#123238=CARTESIAN_POINT('Ctrl Pts',(54.8990816092953,-48.8745443424477,
0.));
#123239=CARTESIAN_POINT('Ctrl Pts',(54.8877238496565,-48.8505664587974,
0.));
#123240=CARTESIAN_POINT('Ctrl Pts',(54.8763598301037,-48.8266326137622,
0.));
#123241=CARTESIAN_POINT('Ctrl Pts',(54.8649896357285,-48.8027428709614,
0.));
#123242=CARTESIAN_POINT('Ctrl Pts',(54.8536133519292,-48.7788972941438,
0.));
#123243=CARTESIAN_POINT('Ctrl Pts',(54.8422310643763,-48.7550959471601,
0.));
#123244=CARTESIAN_POINT('Ctrl Pts',(54.8308428590344,-48.7313388939845,
0.));
#123245=CARTESIAN_POINT('Ctrl Pts',(54.819448822181,-48.7076261987292,0.));
#123246=CARTESIAN_POINT('Ctrl Pts',(54.8080490404275,-48.6839579256566,
0.));
#123247=CARTESIAN_POINT('Ctrl Pts',(54.7966436007389,-48.6603341391886,
0.));
#123248=CARTESIAN_POINT('Ctrl Pts',(54.7852325904583,-48.6367549039112,
0.));
#123249=CARTESIAN_POINT('Ctrl Pts',(54.7738160973031,-48.6132202845783,
0.));
#123250=CARTESIAN_POINT('Ctrl Pts',(54.7623942093586,-48.5897303461125,
0.));
#123251=CARTESIAN_POINT('Ctrl Pts',(54.7509670150714,-48.5662851536026,
0.));
#123252=CARTESIAN_POINT('Ctrl Pts',(54.7395346032453,-48.5428847722977,
0.));
#123253=CARTESIAN_POINT('Ctrl Pts',(54.7280970630351,-48.519529267596,0.));
#123254=CARTESIAN_POINT('Ctrl Pts',(54.716654483948,-48.4962187050457,0.));
#123255=CARTESIAN_POINT('Ctrl Pts',(54.7052069558497,-48.472953150357,0.));
#123256=CARTESIAN_POINT('Ctrl Pts',(54.6937545689695,-48.4497326694052,
0.));
#123257=CARTESIAN_POINT('Ctrl Pts',(54.6822974139063,-48.426557328234,0.));
#123258=CARTESIAN_POINT('Ctrl Pts',(54.6708355816358,-48.4034271930514,
0.));
#123259=CARTESIAN_POINT('Ctrl Pts',(54.6593691635145,-48.3803423302294,
0.));
#123260=CARTESIAN_POINT('Ctrl Pts',(54.6478982512794,-48.3573028063124,
0.));
#123261=CARTESIAN_POINT('Ctrl Pts',(54.6364229370494,-48.3343086880194,
0.));
#123262=CARTESIAN_POINT('Ctrl Pts',(54.6249433133261,-48.3113600422443,
0.));
#123263=CARTESIAN_POINT('Ctrl Pts',(54.6134594729959,-48.2884569360506,
0.));
#123264=CARTESIAN_POINT('Ctrl Pts',(54.6019715093309,-48.2655994366665,
0.));
#123265=CARTESIAN_POINT('Ctrl Pts',(54.5904795159926,-48.2427876114947,
0.));
#123266=CARTESIAN_POINT('Ctrl Pts',(54.5789835870342,-48.2200215281173,
0.));
#123267=CARTESIAN_POINT('Ctrl Pts',(54.5674838169041,-48.1973012542966,
0.));
#123268=CARTESIAN_POINT('Ctrl Pts',(54.5559803004492,-48.1746268579736,
0.));
#123269=CARTESIAN_POINT('Ctrl Pts',(54.5444731329201,-48.1519984072622,
0.));
#123270=CARTESIAN_POINT('Ctrl Pts',(54.5329624099721,-48.1294159704573,
0.));
#123271=CARTESIAN_POINT('Ctrl Pts',(54.5214482276678,-48.1068796160405,
0.));
#123272=CARTESIAN_POINT('Ctrl Pts',(54.5099306824786,-48.0843894126806,
0.));
#123273=CARTESIAN_POINT('Ctrl Pts',(54.4984098712886,-48.0619454292324,
0.));
#123274=CARTESIAN_POINT('Ctrl Pts',(54.4868858913971,-48.0395477347298,
0.));
#123275=CARTESIAN_POINT('Ctrl Pts',(54.4753588405215,-48.0171963983924,
0.));
#123276=CARTESIAN_POINT('Ctrl Pts',(54.4638288168003,-47.9948914896326,
0.));
#123277=CARTESIAN_POINT('Ctrl Pts',(54.4522959187955,-47.9726330780572,
0.));
#123278=CARTESIAN_POINT('Ctrl Pts',(54.4407602454967,-47.9504212334675,
0.));
#123279=CARTESIAN_POINT('Ctrl Pts',(54.429221896324,-47.9282560258516,0.));
#123280=CARTESIAN_POINT('Ctrl Pts',(54.4176809711311,-47.9061375253897,
0.));
#123281=CARTESIAN_POINT('Ctrl Pts',(54.4061375702079,-47.8840658024618,
0.));
#123282=CARTESIAN_POINT('Ctrl Pts',(54.3945917942832,-47.8620409276493,
0.));
#123283=CARTESIAN_POINT('Ctrl Pts',(54.3830437445278,-47.8400629717355,
0.));
#123284=CARTESIAN_POINT('Ctrl Pts',(54.3714935225591,-47.8181320056995,
0.));
#123285=CARTESIAN_POINT('Ctrl Pts',(54.3599412304437,-47.7962481007185,
0.));
#123286=CARTESIAN_POINT('Ctrl Pts',(54.3483869707002,-47.7744113281771,
0.));
#123287=CARTESIAN_POINT('Ctrl Pts',(54.3368308463023,-47.7526217596694,
0.));
#123288=CARTESIAN_POINT('Ctrl Pts',(54.3252729606823,-47.7308794669993,
0.));
#123289=CARTESIAN_POINT('Ctrl Pts',(54.3137134177345,-47.7091845221747,
0.));
#123290=CARTESIAN_POINT('Ctrl Pts',(54.302152321819,-47.6875369974087,0.));
#123291=CARTESIAN_POINT('Ctrl Pts',(54.290589777765,-47.6659369651301,0.));
#123292=CARTESIAN_POINT('Ctrl Pts',(54.2790258908738,-47.6443844979848,
0.));
#123293=CARTESIAN_POINT('Ctrl Pts',(54.2674607669226,-47.6228796688375,
0.));
#123294=CARTESIAN_POINT('Ctrl Pts',(54.2558945121678,-47.6014225507659,
0.));
#123295=CARTESIAN_POINT('Ctrl Pts',(54.244327233349,-47.5800132170608,0.));
#123296=CARTESIAN_POINT('Ctrl Pts',(54.2327590376924,-47.5586517412363,
0.));
#123297=CARTESIAN_POINT('Ctrl Pts',(54.2211900329138,-47.5373381970326,
0.));
#123298=CARTESIAN_POINT('Ctrl Pts',(54.209620327223,-47.5160726584174,0.));
#123299=CARTESIAN_POINT('Ctrl Pts',(54.198050029327,-47.4948551995801,0.));
#123300=CARTESIAN_POINT('Ctrl Pts',(54.1864792484345,-47.4736858949322,
0.));
#123301=CARTESIAN_POINT('Ctrl Pts',(54.1749080942593,-47.4525648191173,
0.));
#123302=CARTESIAN_POINT('Ctrl Pts',(54.1633366770239,-47.4314920470141,
0.));
#123303=CARTESIAN_POINT('Ctrl Pts',(54.1517651074637,-47.4104676537381,
0.));
#123304=CARTESIAN_POINT('Ctrl Pts',(54.1401934968311,-47.3894917146365,
0.));
#123305=CARTESIAN_POINT('Ctrl Pts',(54.1286219568989,-47.3685643052874,
0.));
#123306=CARTESIAN_POINT('Ctrl Pts',(54.1170505999645,-47.3476855015102,
0.));
#123307=CARTESIAN_POINT('Ctrl Pts',(54.1054795388543,-47.3268553793694,
0.));
#123308=CARTESIAN_POINT('Ctrl Pts',(54.0939088869268,-47.3060740151752,
0.));
#123309=CARTESIAN_POINT('Ctrl Pts',(54.0823387580776,-47.2853414854793,
0.));
#123310=CARTESIAN_POINT('Ctrl Pts',(54.0707692667438,-47.2646578670746,
0.));
#123311=CARTESIAN_POINT('Ctrl Pts',(54.0592005279086,-47.2440232370065,
0.));
#123312=CARTESIAN_POINT('Ctrl Pts',(54.047632657104,-47.2234376725743,0.));
#123313=CARTESIAN_POINT('Ctrl Pts',(54.0360657704163,-47.202901251334,0.));
#123314=CARTESIAN_POINT('Ctrl Pts',(54.0244999844893,-47.1824140510926,
0.));
#123315=CARTESIAN_POINT('Ctrl Pts',(54.0129354165297,-47.1619761499087,
0.));
#123316=CARTESIAN_POINT('Ctrl Pts',(54.0013721843118,-47.1415876261035,
0.));
#123317=CARTESIAN_POINT('Ctrl Pts',(53.989810406182,-47.1212485582643,0.));
#123318=CARTESIAN_POINT('Ctrl Pts',(53.9782502010634,-47.1009590252458,
0.));
#123319=CARTESIAN_POINT('Ctrl Pts',(53.9666916884596,-47.0807191061648,
0.));
#123320=CARTESIAN_POINT('Ctrl Pts',(53.9551349884599,-47.0605288804008,
0.));
#123321=CARTESIAN_POINT('Ctrl Pts',(53.9435802217436,-47.0403884276072,
0.));
#123322=CARTESIAN_POINT('Ctrl Pts',(53.9320275095853,-47.0202978277138,
0.));
#123323=CARTESIAN_POINT('Ctrl Pts',(53.9204769738596,-47.0002571609297,
0.));
#123324=CARTESIAN_POINT('Ctrl Pts',(53.9089287370463,-46.9802665077366,
0.));
#123325=CARTESIAN_POINT('Ctrl Pts',(53.8973829222347,-46.9603259488921,
0.));
#123326=CARTESIAN_POINT('Ctrl Pts',(53.8858396531298,-46.9404355654401,
0.));
#123327=CARTESIAN_POINT('Ctrl Pts',(53.8742990540563,-46.9205954387133,
0.));
#123328=CARTESIAN_POINT('Ctrl Pts',(53.8627612499638,-46.9008056503351,
0.));
#123329=CARTESIAN_POINT('Ctrl Pts',(53.8512263664321,-46.881066282213,0.));
#123330=CARTESIAN_POINT('Ctrl Pts',(53.8396945296757,-46.8613774165435,
0.));
#123331=CARTESIAN_POINT('Ctrl Pts',(53.8281658665503,-46.841739135822,0.));
#123332=CARTESIAN_POINT('Ctrl Pts',(53.816640504558,-46.8221515228457,0.));
#123333=CARTESIAN_POINT('Ctrl Pts',(53.8051185718532,-46.802614660715,0.));
#123334=CARTESIAN_POINT('Ctrl Pts',(53.793600197248,-46.7831286328278,0.));
#123335=CARTESIAN_POINT('Ctrl Pts',(53.7820855102182,-46.7636935228861,
0.));
#123336=CARTESIAN_POINT('Ctrl Pts',(53.7705746409075,-46.7443094149045,
0.));
#123337=CARTESIAN_POINT('Ctrl Pts',(53.7590677201342,-46.7249763932129,
0.));
#123338=CARTESIAN_POINT('Ctrl Pts',(53.7475648793946,-46.7056945424559,
0.));
#123339=CARTESIAN_POINT('Ctrl Pts',(53.7360662508675,-46.6864639475862,
0.));
#123340=CARTESIAN_POINT('Ctrl Pts',(53.7245719674221,-46.6672846938752,
0.));
#123341=CARTESIAN_POINT('Ctrl Pts',(53.7130821626262,-46.6481568669217,
0.));
#123342=CARTESIAN_POINT('Ctrl Pts',(53.7015969707541,-46.6290805526559,
0.));
#123343=CARTESIAN_POINT('Ctrl Pts',(53.690116526794,-46.6100558373401,0.));
#123344=CARTESIAN_POINT('Ctrl Pts',(53.678640966456,-46.5910828075652,0.));
#123345=CARTESIAN_POINT('Ctrl Pts',(53.6671704261735,-46.572161550259,0.));
#123346=CARTESIAN_POINT('Ctrl Pts',(53.6557050431069,-46.5532921526899,
0.));
#123347=CARTESIAN_POINT('Ctrl Pts',(53.6442449551455,-46.5344747024677,
0.));
#123348=CARTESIAN_POINT('Ctrl Pts',(53.6327903009097,-46.5157092875377,
0.));
#123349=CARTESIAN_POINT('Ctrl Pts',(53.6213412197542,-46.4969959961779,
0.));
#123350=CARTESIAN_POINT('Ctrl Pts',(53.6098978517869,-46.4783349170182,
0.));
#123351=CARTESIAN_POINT('Ctrl Pts',(53.5984603378861,-46.4597261390526,
0.));
#123352=CARTESIAN_POINT('Ctrl Pts',(53.5870288197161,-46.4411697516474,
0.));
#123353=CARTESIAN_POINT('Ctrl Pts',(53.5756034397464,-46.422665844546,0.));
#123354=CARTESIAN_POINT('Ctrl Pts',(53.5641843412537,-46.4042145078682,
0.));
#123355=CARTESIAN_POINT('Ctrl Pts',(53.5527716683029,-46.3858158321044,
0.));
#123356=CARTESIAN_POINT('Ctrl Pts',(53.5413655657323,-46.3674699081043,
0.));
#123357=CARTESIAN_POINT('Ctrl Pts',(53.5299661791396,-46.3491768270664,
0.));
#123358=CARTESIAN_POINT('Ctrl Pts',(53.518573654857,-46.3309366805112,0.));
#123359=CARTESIAN_POINT('Ctrl Pts',(53.5071881399932,-46.3127495603117,
0.));
#123360=CARTESIAN_POINT('Ctrl Pts',(53.4958097825019,-46.2946155587428,
0.));
#123361=CARTESIAN_POINT('Ctrl Pts',(53.4844387312414,-46.2765347685198,
0.));
#123362=CARTESIAN_POINT('Ctrl Pts',(53.4730751360359,-46.2585072828343,
0.));
#123363=CARTESIAN_POINT('Ctrl Pts',(53.4617191477382,-46.2405331953872,
0.));
#123364=CARTESIAN_POINT('Ctrl Pts',(53.4503709181158,-46.2226126003185,
0.));
#123365=CARTESIAN_POINT('Ctrl Pts',(53.4390305997263,-46.2047455921276,
0.));
#123366=CARTESIAN_POINT('Ctrl Pts',(53.4276983458129,-46.1869322656027,
0.));
#123367=CARTESIAN_POINT('Ctrl Pts',(53.4163743101534,-46.1691727157149,
0.));
#123368=CARTESIAN_POINT('Ctrl Pts',(53.4050586470463,-46.1514670376035,
0.));
#123369=CARTESIAN_POINT('Ctrl Pts',(53.3937515116572,-46.1338153268116,
0.));
#123370=CARTESIAN_POINT('Ctrl Pts',(53.3824530603284,-46.1162176794891,
0.));
#123371=CARTESIAN_POINT('Ctrl Pts',(53.3711634508426,-46.0986741925646,
0.));
#123372=CARTESIAN_POINT('Ctrl Pts',(53.3598828428519,-46.0811849640195,
0.));
#123373=CARTESIAN_POINT('Ctrl Pts',(53.3486113975868,-46.0637500926954,
0.));
#123374=CARTESIAN_POINT('Ctrl Pts',(53.3373492770647,-46.046369677778,0.));
#123375=CARTESIAN_POINT('Ctrl Pts',(53.3260966434277,-46.0290438183598,
0.));
#123376=CARTESIAN_POINT('Ctrl Pts',(53.3148536582658,-46.0117726129893,
0.));
#123377=CARTESIAN_POINT('Ctrl Pts',(53.3036204818367,-45.9945561591486,
0.));
#123378=CARTESIAN_POINT('Ctrl Pts',(53.2923972745585,-45.9773945542415,
0.));
#123379=CARTESIAN_POINT('Ctrl Pts',(53.2811841987945,-45.9602878967715,
0.));
#123380=CARTESIAN_POINT('Ctrl Pts',(53.2699814203097,-45.9432362873001,
0.));
#123381=CARTESIAN_POINT('Ctrl Pts',(53.2587891103835,-45.9262398298323,
0.));
#123382=CARTESIAN_POINT('Ctrl Pts',(53.2476074459977,-45.9092986319343,
0.));
#123383=CARTESIAN_POINT('Ctrl Pts',(53.2364366054276,-45.8924128018354,
0.));
#123384=CARTESIAN_POINT('Ctrl Pts',(53.2252767643652,-45.8755824458715,
0.));
#123385=CARTESIAN_POINT('Ctrl Pts',(53.2141280925458,-45.8588076662598,
0.));
#123386=CARTESIAN_POINT('Ctrl Pts',(53.2029907483602,-45.8420885575386,
0.));
#123387=CARTESIAN_POINT('Ctrl Pts',(53.1918648840598,-45.8254252100003,
0.));
#123388=CARTESIAN_POINT('Ctrl Pts',(53.1807506560977,-45.8088177165124,
0.));
#123389=CARTESIAN_POINT('Ctrl Pts',(53.1696482334487,-45.7922661780005,
0.));
#123390=CARTESIAN_POINT('Ctrl Pts',(53.158557807638,-45.7757707100568,0.));
#123391=CARTESIAN_POINT('Ctrl Pts',(53.147479599594,-45.7593314474413,0.));
#123392=CARTESIAN_POINT('Ctrl Pts',(53.136413838457,-45.7429485300727,0.));
#123393=CARTESIAN_POINT('Ctrl Pts',(53.1253607414806,-45.7266220896951,
0.));
#123394=CARTESIAN_POINT('Ctrl Pts',(53.1143204954981,-45.7103522376744,
0.));
#123395=CARTESIAN_POINT('Ctrl Pts',(53.1032932329074,-45.6941390489239,
0.));
#123396=CARTESIAN_POINT('Ctrl Pts',(53.0922790298736,-45.6779825614486,
0.));
#123397=CARTESIAN_POINT('Ctrl Pts',(53.083478145185,-45.665102743948,0.));
#123398=CARTESIAN_POINT('Ctrl Pts',(53.0768833804386,-45.6554684028296,
0.));
#123399=CARTESIAN_POINT('Ctrl Pts',(53.0724894921921,-45.6490568514146,
0.));
#123400=CARTESIAN_POINT('Ctrl Pts',(53.0702932034641,-45.6458539113724,
0.));
#123401=CARTESIAN_POINT('Ctrl Pts',(50.7903314215393,-54.5031396718592,
0.));
#123402=CARTESIAN_POINT('Ctrl Pts',(50.7903314215393,-54.5031396718592,
12.));
#123403=CARTESIAN_POINT('Ctrl Pts',(50.7885805844281,-54.4978248630387,
0.));
#123404=CARTESIAN_POINT('Ctrl Pts',(50.7885805844281,-54.4978248630387,
12.));
#123405=CARTESIAN_POINT('Ctrl Pts',(50.7850776288813,-54.4871993224832,
0.));
#123406=CARTESIAN_POINT('Ctrl Pts',(50.7850776288813,-54.4871993224832,
12.));
#123407=CARTESIAN_POINT('Ctrl Pts',(50.7798193515888,-54.4712732429066,
0.));
#123408=CARTESIAN_POINT('Ctrl Pts',(50.7798193515888,-54.4712732429066,
12.));
#123409=CARTESIAN_POINT('Ctrl Pts',(50.7728006269349,-54.4500629336429,
0.));
#123410=CARTESIAN_POINT('Ctrl Pts',(50.7728006269349,-54.4500629336429,
12.));
#123411=CARTESIAN_POINT('Ctrl Pts',(50.764014409002,-54.423590828767,0.));
#123412=CARTESIAN_POINT('Ctrl Pts',(50.764014409002,-54.423590828767,12.));
#123413=CARTESIAN_POINT('Ctrl Pts',(50.7552153869475,-54.3971595231574,
0.));
#123414=CARTESIAN_POINT('Ctrl Pts',(50.7552153869475,-54.3971595231574,
12.));
#123415=CARTESIAN_POINT('Ctrl Pts',(50.7464035792906,-54.3707690445749,
0.));
#123416=CARTESIAN_POINT('Ctrl Pts',(50.7464035792906,-54.3707690445749,
12.));
#123417=CARTESIAN_POINT('Ctrl Pts',(50.7375790185896,-54.3444194324054,
0.));
#123418=CARTESIAN_POINT('Ctrl Pts',(50.7375790185896,-54.3444194324054,
12.));
#123419=CARTESIAN_POINT('Ctrl Pts',(50.7287417566123,-54.3181107400663,
0.));
#123420=CARTESIAN_POINT('Ctrl Pts',(50.7287417566123,-54.3181107400663,
12.));
#123421=CARTESIAN_POINT('Ctrl Pts',(50.7198918629451,-54.2918430335206,
0.));
#123422=CARTESIAN_POINT('Ctrl Pts',(50.7198918629451,-54.2918430335206,
12.));
#123423=CARTESIAN_POINT('Ctrl Pts',(50.7110294185698,-54.2656163868104,
0.));
#123424=CARTESIAN_POINT('Ctrl Pts',(50.7110294185698,-54.2656163868104,
12.));
#123425=CARTESIAN_POINT('Ctrl Pts',(50.7021545108311,-54.2394308784026,
0.));
#123426=CARTESIAN_POINT('Ctrl Pts',(50.7021545108311,-54.2394308784026,
12.));
#123427=CARTESIAN_POINT('Ctrl Pts',(50.6932672279772,-54.2132865872985,
0.));
#123428=CARTESIAN_POINT('Ctrl Pts',(50.6932672279772,-54.2132865872985,
12.));
#123429=CARTESIAN_POINT('Ctrl Pts',(50.6843676535492,-54.1871835889981,
0.));
#123430=CARTESIAN_POINT('Ctrl Pts',(50.6843676535492,-54.1871835889981,
12.));
#123431=CARTESIAN_POINT('Ctrl Pts',(50.67545586183,-54.1611219522394,0.));
#123432=CARTESIAN_POINT('Ctrl Pts',(50.67545586183,-54.1611219522394,12.));
#123433=CARTESIAN_POINT('Ctrl Pts',(50.6665319209869,-54.1351017412804,
0.));
#123434=CARTESIAN_POINT('Ctrl Pts',(50.6665319209869,-54.1351017412804,
12.));
#123435=CARTESIAN_POINT('Ctrl Pts',(50.6575958953221,-54.1091230175367,
0.));
#123436=CARTESIAN_POINT('Ctrl Pts',(50.6575958953221,-54.1091230175367,
12.));
#123437=CARTESIAN_POINT('Ctrl Pts',(50.6486478479465,-54.0831858415189,
0.));
#123438=CARTESIAN_POINT('Ctrl Pts',(50.6486478479465,-54.0831858415189,
12.));
#123439=CARTESIAN_POINT('Ctrl Pts',(50.6396878430939,-54.0572902745076,
0.));
#123440=CARTESIAN_POINT('Ctrl Pts',(50.6396878430939,-54.0572902745076,
12.));
#123441=CARTESIAN_POINT('Ctrl Pts',(50.6307159490553,-54.0314363806708,
0.));
#123442=CARTESIAN_POINT('Ctrl Pts',(50.6307159490553,-54.0314363806708,
12.));
#123443=CARTESIAN_POINT('Ctrl Pts',(50.6217322378648,-54.0056242268399,
0.));
#123444=CARTESIAN_POINT('Ctrl Pts',(50.6217322378648,-54.0056242268399,
12.));
#123445=CARTESIAN_POINT('Ctrl Pts',(50.6127367839711,-53.979853881553,0.));
#123446=CARTESIAN_POINT('Ctrl Pts',(50.6127367839711,-53.979853881553,12.));
#123447=CARTESIAN_POINT('Ctrl Pts',(50.6037296632139,-53.9541254143119,
0.));
#123448=CARTESIAN_POINT('Ctrl Pts',(50.6037296632139,-53.9541254143119,
12.));
#123449=CARTESIAN_POINT('Ctrl Pts',(50.5947109517483,-53.9284388948004,
0.));
#123450=CARTESIAN_POINT('Ctrl Pts',(50.5947109517483,-53.9284388948004,
12.));
#123451=CARTESIAN_POINT('Ctrl Pts',(50.5856807248151,-53.9027943919836,
0.));
#123452=CARTESIAN_POINT('Ctrl Pts',(50.5856807248151,-53.9027943919836,
12.));
#123453=CARTESIAN_POINT('Ctrl Pts',(50.5766390561884,-53.8771919737032,
0.));
#123454=CARTESIAN_POINT('Ctrl Pts',(50.5766390561884,-53.8771919737032,
12.));
#123455=CARTESIAN_POINT('Ctrl Pts',(50.5675860188538,-53.8516317071804,
0.));
#123456=CARTESIAN_POINT('Ctrl Pts',(50.5675860188538,-53.8516317071804,
12.));
#123457=CARTESIAN_POINT('Ctrl Pts',(50.5585216854091,-53.8261136593075,
0.));
#123458=CARTESIAN_POINT('Ctrl Pts',(50.5585216854091,-53.8261136593075,
12.));
#123459=CARTESIAN_POINT('Ctrl Pts',(50.5494461285761,-53.8006378970197,
0.));
#123460=CARTESIAN_POINT('Ctrl Pts',(50.5494461285761,-53.8006378970197,
12.));
#123461=CARTESIAN_POINT('Ctrl Pts',(50.5403594216698,-53.7752044876304,
0.));
#123462=CARTESIAN_POINT('Ctrl Pts',(50.5403594216698,-53.7752044876304,
12.));
#123463=CARTESIAN_POINT('Ctrl Pts',(50.5312616390779,-53.7498134991703,
0.));
#123464=CARTESIAN_POINT('Ctrl Pts',(50.5312616390779,-53.7498134991703,
12.));
#123465=CARTESIAN_POINT('Ctrl Pts',(50.522152856042,-53.7244650002374,0.));
#123466=CARTESIAN_POINT('Ctrl Pts',(50.522152856042,-53.7244650002374,12.));
#123467=CARTESIAN_POINT('Ctrl Pts',(50.513033148456,-53.6991590598548,0.));
#123468=CARTESIAN_POINT('Ctrl Pts',(50.513033148456,-53.6991590598548,12.));
#123469=CARTESIAN_POINT('Ctrl Pts',(50.503902592653,-53.6738957473158,0.));
#123470=CARTESIAN_POINT('Ctrl Pts',(50.503902592653,-53.6738957473158,12.));
#123471=CARTESIAN_POINT('Ctrl Pts',(50.4947612652148,-53.6486751320436,
0.));
#123472=CARTESIAN_POINT('Ctrl Pts',(50.4947612652148,-53.6486751320436,
12.));
#123473=CARTESIAN_POINT('Ctrl Pts',(50.4856092427314,-53.623497283406,0.));
#123474=CARTESIAN_POINT('Ctrl Pts',(50.4856092427314,-53.623497283406,12.));
#123475=CARTESIAN_POINT('Ctrl Pts',(50.4764466018071,-53.5983622707238,
0.));
#123476=CARTESIAN_POINT('Ctrl Pts',(50.4764466018071,-53.5983622707238,
12.));
#123477=CARTESIAN_POINT('Ctrl Pts',(50.4672734191756,-53.5732701633609,
0.));
#123478=CARTESIAN_POINT('Ctrl Pts',(50.4672734191756,-53.5732701633609,
12.));
#123479=CARTESIAN_POINT('Ctrl Pts',(50.4580897717838,-53.5482210307868,
0.));
#123480=CARTESIAN_POINT('Ctrl Pts',(50.4580897717838,-53.5482210307868,
12.));
#123481=CARTESIAN_POINT('Ctrl Pts',(50.4488957368839,-53.5232149426413,
0.));
#123482=CARTESIAN_POINT('Ctrl Pts',(50.4488957368839,-53.5232149426413,
12.));
#123483=CARTESIAN_POINT('Ctrl Pts',(50.4396913921381,-53.4982519688024,
0.));
#123484=CARTESIAN_POINT('Ctrl Pts',(50.4396913921381,-53.4982519688024,
12.));
#123485=CARTESIAN_POINT('Ctrl Pts',(50.4304768156666,-53.4733321794188,
0.));
#123486=CARTESIAN_POINT('Ctrl Pts',(50.4304768156666,-53.4733321794188,
12.));
#123487=CARTESIAN_POINT('Ctrl Pts',(50.4212520859914,-53.4484556448776,
0.));
#123488=CARTESIAN_POINT('Ctrl Pts',(50.4212520859914,-53.4484556448776,
12.));
#123489=CARTESIAN_POINT('Ctrl Pts',(50.4120172820047,-53.4236224357838,
0.));
#123490=CARTESIAN_POINT('Ctrl Pts',(50.4120172820047,-53.4236224357838,
12.));
#123491=CARTESIAN_POINT('Ctrl Pts',(50.4027724829297,-53.398832622931,0.));
#123492=CARTESIAN_POINT('Ctrl Pts',(50.4027724829297,-53.398832622931,12.));
#123493=CARTESIAN_POINT('Ctrl Pts',(50.3935177682837,-53.3740862772681,
0.));
#123494=CARTESIAN_POINT('Ctrl Pts',(50.3935177682837,-53.3740862772681,
12.));
#123495=CARTESIAN_POINT('Ctrl Pts',(50.384253217846,-53.3493834698697,0.));
#123496=CARTESIAN_POINT('Ctrl Pts',(50.384253217846,-53.3493834698697,12.));
#123497=CARTESIAN_POINT('Ctrl Pts',(50.3749789116786,-53.3247242719587,
0.));
#123498=CARTESIAN_POINT('Ctrl Pts',(50.3749789116786,-53.3247242719587,
12.));
#123499=CARTESIAN_POINT('Ctrl Pts',(50.365694930143,-53.300108754923,0.));
#123500=CARTESIAN_POINT('Ctrl Pts',(50.365694930143,-53.300108754923,12.));
#123501=CARTESIAN_POINT('Ctrl Pts',(50.3564013539199,-53.2755369903293,
0.));
#123502=CARTESIAN_POINT('Ctrl Pts',(50.3564013539199,-53.2755369903293,
12.));
#123503=CARTESIAN_POINT('Ctrl Pts',(50.3470982640289,-53.2510090499336,
0.));
#123504=CARTESIAN_POINT('Ctrl Pts',(50.3470982640289,-53.2510090499336,
12.));
#123505=CARTESIAN_POINT('Ctrl Pts',(50.3377857418514,-53.2265250056887,
0.));
#123506=CARTESIAN_POINT('Ctrl Pts',(50.3377857418514,-53.2265250056887,
12.));
#123507=CARTESIAN_POINT('Ctrl Pts',(50.3284638691278,-53.2020849297471,
0.));
#123508=CARTESIAN_POINT('Ctrl Pts',(50.3284638691278,-53.2020849297471,
12.));
#123509=CARTESIAN_POINT('Ctrl Pts',(50.3191327279492,-53.1776888944616,
0.));
#123510=CARTESIAN_POINT('Ctrl Pts',(50.3191327279492,-53.1776888944616,
12.));
#123511=CARTESIAN_POINT('Ctrl Pts',(50.3097924007534,-53.1533369723818,
0.));
#123512=CARTESIAN_POINT('Ctrl Pts',(50.3097924007534,-53.1533369723818,
12.));
#123513=CARTESIAN_POINT('Ctrl Pts',(50.300442970319,-53.1290292362485,0.));
#123514=CARTESIAN_POINT('Ctrl Pts',(50.300442970319,-53.1290292362485,12.));
#123515=CARTESIAN_POINT('Ctrl Pts',(50.2910845197619,-53.1047657589812,
0.));
#123516=CARTESIAN_POINT('Ctrl Pts',(50.2910845197619,-53.1047657589812,
12.));
#123517=CARTESIAN_POINT('Ctrl Pts',(50.2817171325358,-53.0805466136798,
0.));
#123518=CARTESIAN_POINT('Ctrl Pts',(50.2817171325358,-53.0805466136798,
12.));
#123519=CARTESIAN_POINT('Ctrl Pts',(50.2723408924373,-53.0563718736366,
0.));
#123520=CARTESIAN_POINT('Ctrl Pts',(50.2723408924373,-53.0563718736366,
12.));
#123521=CARTESIAN_POINT('Ctrl Pts',(50.2629558836111,-53.0322416123406,
0.));
#123522=CARTESIAN_POINT('Ctrl Pts',(50.2629558836111,-53.0322416123406,
12.));
#123523=CARTESIAN_POINT('Ctrl Pts',(50.2535621905552,-53.0081559034801,
0.));
#123524=CARTESIAN_POINT('Ctrl Pts',(50.2535621905552,-53.0081559034801,
12.));
#123525=CARTESIAN_POINT('Ctrl Pts',(50.2441598981286,-52.9841148209402,
0.));
#123526=CARTESIAN_POINT('Ctrl Pts',(50.2441598981286,-52.9841148209402,
12.));
#123527=CARTESIAN_POINT('Ctrl Pts',(50.2347490915555,-52.9601184388028,
0.));
#123528=CARTESIAN_POINT('Ctrl Pts',(50.2347490915555,-52.9601184388028,
12.));
#123529=CARTESIAN_POINT('Ctrl Pts',(50.2253298564241,-52.9361668313542,
0.));
#123530=CARTESIAN_POINT('Ctrl Pts',(50.2253298564241,-52.9361668313542,
12.));
#123531=CARTESIAN_POINT('Ctrl Pts',(50.2159022786879,-52.9122600730884,
0.));
#123532=CARTESIAN_POINT('Ctrl Pts',(50.2159022786879,-52.9122600730884,
12.));
#123533=CARTESIAN_POINT('Ctrl Pts',(50.2064664446663,-52.8883982387068,
0.));
#123534=CARTESIAN_POINT('Ctrl Pts',(50.2064664446663,-52.8883982387068,
12.));
#123535=CARTESIAN_POINT('Ctrl Pts',(50.1970224410471,-52.8645814031133,
0.));
#123536=CARTESIAN_POINT('Ctrl Pts',(50.1970224410471,-52.8645814031133,
12.));
#123537=CARTESIAN_POINT('Ctrl Pts',(50.1875703548884,-52.8408096414093,
0.));
#123538=CARTESIAN_POINT('Ctrl Pts',(50.1875703548884,-52.8408096414093,
12.));
#123539=CARTESIAN_POINT('Ctrl Pts',(50.1781102736205,-52.8170830289044,
0.));
#123540=CARTESIAN_POINT('Ctrl Pts',(50.1781102736205,-52.8170830289044,
12.));
#123541=CARTESIAN_POINT('Ctrl Pts',(50.1686422850487,-52.7934016411205,
0.));
#123542=CARTESIAN_POINT('Ctrl Pts',(50.1686422850487,-52.7934016411205,
12.));
#123543=CARTESIAN_POINT('Ctrl Pts',(50.1591664773561,-52.769765553794,0.));
#123544=CARTESIAN_POINT('Ctrl Pts',(50.1591664773561,-52.769765553794,12.));
#123545=CARTESIAN_POINT('Ctrl Pts',(50.1496829391073,-52.7461748428738,
0.));
#123546=CARTESIAN_POINT('Ctrl Pts',(50.1496829391073,-52.7461748428738,
12.));
#123547=CARTESIAN_POINT('Ctrl Pts',(50.1401917592537,-52.7226295845161,
0.));
#123548=CARTESIAN_POINT('Ctrl Pts',(50.1401917592537,-52.7226295845161,
12.));
#123549=CARTESIAN_POINT('Ctrl Pts',(50.1306930271345,-52.699129855093,0.));
#123550=CARTESIAN_POINT('Ctrl Pts',(50.1306930271345,-52.699129855093,12.));
#123551=CARTESIAN_POINT('Ctrl Pts',(50.121186832478,-52.6756757311978,0.));
#123552=CARTESIAN_POINT('Ctrl Pts',(50.121186832478,-52.6756757311978,12.));
#123553=CARTESIAN_POINT('Ctrl Pts',(50.111673265404,-52.652267289646,0.));
#123554=CARTESIAN_POINT('Ctrl Pts',(50.111673265404,-52.652267289646,12.));
#123555=CARTESIAN_POINT('Ctrl Pts',(50.1021524164264,-52.6289046074746,
0.));
#123556=CARTESIAN_POINT('Ctrl Pts',(50.1021524164264,-52.6289046074746,
12.));
#123557=CARTESIAN_POINT('Ctrl Pts',(50.0926243764578,-52.6055877619348,
0.));
#123558=CARTESIAN_POINT('Ctrl Pts',(50.0926243764578,-52.6055877619348,
12.));
#123559=CARTESIAN_POINT('Ctrl Pts',(50.0830892368107,-52.5823168304994,
0.));
#123560=CARTESIAN_POINT('Ctrl Pts',(50.0830892368107,-52.5823168304994,
12.));
#123561=CARTESIAN_POINT('Ctrl Pts',(50.0735470892007,-52.5590918908702,
0.));
#123562=CARTESIAN_POINT('Ctrl Pts',(50.0735470892007,-52.5590918908702,
12.));
#123563=CARTESIAN_POINT('Ctrl Pts',(50.0639980257479,-52.5359130209792,
0.));
#123564=CARTESIAN_POINT('Ctrl Pts',(50.0639980257479,-52.5359130209792,
12.));
#123565=CARTESIAN_POINT('Ctrl Pts',(50.0544421389817,-52.5127802989896,
0.));
#123566=CARTESIAN_POINT('Ctrl Pts',(50.0544421389817,-52.5127802989896,
12.));
#123567=CARTESIAN_POINT('Ctrl Pts',(50.0448795218441,-52.4896938032884,
0.));
#123568=CARTESIAN_POINT('Ctrl Pts',(50.0448795218441,-52.4896938032884,
12.));
#123569=CARTESIAN_POINT('Ctrl Pts',(50.0353102676921,-52.4666536124913,
0.));
#123570=CARTESIAN_POINT('Ctrl Pts',(50.0353102676921,-52.4666536124913,
12.));
#123571=CARTESIAN_POINT('Ctrl Pts',(50.0257344703,-52.4436598054515,0.));
#123572=CARTESIAN_POINT('Ctrl Pts',(50.0257344703,-52.4436598054515,12.));
#123573=CARTESIAN_POINT('Ctrl Pts',(50.0161522238616,-52.4207124612608,
0.));
#123574=CARTESIAN_POINT('Ctrl Pts',(50.0161522238616,-52.4207124612608,
12.));
#123575=CARTESIAN_POINT('Ctrl Pts',(50.0065636229938,-52.3978116592509,
0.));
#123576=CARTESIAN_POINT('Ctrl Pts',(50.0065636229938,-52.3978116592509,
12.));
#123577=CARTESIAN_POINT('Ctrl Pts',(49.9969687627408,-52.3749574789871,
0.));
#123578=CARTESIAN_POINT('Ctrl Pts',(49.9969687627408,-52.3749574789871,
12.));
#123579=CARTESIAN_POINT('Ctrl Pts',(49.9873677385775,-52.3521500002718,
0.));
#123580=CARTESIAN_POINT('Ctrl Pts',(49.9873677385775,-52.3521500002718,
12.));
#123581=CARTESIAN_POINT('Ctrl Pts',(49.9777606464106,-52.3293893031528,
0.));
#123582=CARTESIAN_POINT('Ctrl Pts',(49.9777606464106,-52.3293893031528,
12.));
#123583=CARTESIAN_POINT('Ctrl Pts',(49.9681475825824,-52.3066754679265,
0.));
#123584=CARTESIAN_POINT('Ctrl Pts',(49.9681475825824,-52.3066754679265,
12.));
#123585=CARTESIAN_POINT('Ctrl Pts',(49.9585286438733,-52.2840085751384,
0.));
#123586=CARTESIAN_POINT('Ctrl Pts',(49.9585286438733,-52.2840085751384,
12.));
#123587=CARTESIAN_POINT('Ctrl Pts',(49.9489039275064,-52.2613887055773,
0.));
#123588=CARTESIAN_POINT('Ctrl Pts',(49.9489039275064,-52.2613887055773,
12.));
#123589=CARTESIAN_POINT('Ctrl Pts',(49.9392735311509,-52.2388159402771,
0.));
#123590=CARTESIAN_POINT('Ctrl Pts',(49.9392735311509,-52.2388159402771,
12.));
#123591=CARTESIAN_POINT('Ctrl Pts',(49.9296375529245,-52.2162903605275,
0.));
#123592=CARTESIAN_POINT('Ctrl Pts',(49.9296375529245,-52.2162903605275,
12.));
#123593=CARTESIAN_POINT('Ctrl Pts',(49.9199960913962,-52.1938120478754,
0.));
#123594=CARTESIAN_POINT('Ctrl Pts',(49.9199960913962,-52.1938120478754,
12.));
#123595=CARTESIAN_POINT('Ctrl Pts',(49.9103492455902,-52.1713810841276,
0.));
#123596=CARTESIAN_POINT('Ctrl Pts',(49.9103492455902,-52.1713810841276,
12.));
#123597=CARTESIAN_POINT('Ctrl Pts',(49.9006971149894,-52.1489975513445,
0.));
#123598=CARTESIAN_POINT('Ctrl Pts',(49.9006971149894,-52.1489975513445,
12.));
#123599=CARTESIAN_POINT('Ctrl Pts',(49.8910397995397,-52.1266615318407,
0.));
#123600=CARTESIAN_POINT('Ctrl Pts',(49.8910397995397,-52.1266615318407,
12.));
#123601=CARTESIAN_POINT('Ctrl Pts',(49.8813773996517,-52.1043731081962,
0.));
#123602=CARTESIAN_POINT('Ctrl Pts',(49.8813773996517,-52.1043731081962,
12.));
#123603=CARTESIAN_POINT('Ctrl Pts',(49.8717100162048,-52.0821323632587,
0.));
#123604=CARTESIAN_POINT('Ctrl Pts',(49.8717100162048,-52.0821323632587,
12.));
#123605=CARTESIAN_POINT('Ctrl Pts',(49.86203775055,-52.0599393801452,0.));
#123606=CARTESIAN_POINT('Ctrl Pts',(49.86203775055,-52.0599393801452,12.));
#123607=CARTESIAN_POINT('Ctrl Pts',(49.8523607045149,-52.0377942422376,
0.));
#123608=CARTESIAN_POINT('Ctrl Pts',(49.8523607045149,-52.0377942422376,
12.));
#123609=CARTESIAN_POINT('Ctrl Pts',(49.8426789804071,-52.0156970331823,
0.));
#123610=CARTESIAN_POINT('Ctrl Pts',(49.8426789804071,-52.0156970331823,
12.));
#123611=CARTESIAN_POINT('Ctrl Pts',(49.8329926810171,-51.9936478369008,
0.));
#123612=CARTESIAN_POINT('Ctrl Pts',(49.8329926810171,-51.9936478369008,
12.));
#123613=CARTESIAN_POINT('Ctrl Pts',(49.8233019096222,-51.9716467375937,
0.));
#123614=CARTESIAN_POINT('Ctrl Pts',(49.8233019096222,-51.9716467375937,
12.));
#123615=CARTESIAN_POINT('Ctrl Pts',(49.8136067699896,-51.9496938197418,
0.));
#123616=CARTESIAN_POINT('Ctrl Pts',(49.8136067699896,-51.9496938197418,
12.));
#123617=CARTESIAN_POINT('Ctrl Pts',(49.8039073663812,-51.9277891681018,
0.));
#123618=CARTESIAN_POINT('Ctrl Pts',(49.8039073663812,-51.9277891681018,
12.));
#123619=CARTESIAN_POINT('Ctrl Pts',(49.7942038035576,-51.9059328677059,
0.));
#123620=CARTESIAN_POINT('Ctrl Pts',(49.7942038035576,-51.9059328677059,
12.));
#123621=CARTESIAN_POINT('Ctrl Pts',(49.7844961867807,-51.8841250038724,
0.));
#123622=CARTESIAN_POINT('Ctrl Pts',(49.7844961867807,-51.8841250038724,
12.));
#123623=CARTESIAN_POINT('Ctrl Pts',(49.7747846218182,-51.8623656622097,
0.));
#123624=CARTESIAN_POINT('Ctrl Pts',(49.7747846218182,-51.8623656622097,
12.));
#123625=CARTESIAN_POINT('Ctrl Pts',(49.7650692149462,-51.8406549286175,
0.));
#123626=CARTESIAN_POINT('Ctrl Pts',(49.7650692149462,-51.8406549286175,
12.));
#123627=CARTESIAN_POINT('Ctrl Pts',(49.755350072955,-51.8189928892828,0.));
#123628=CARTESIAN_POINT('Ctrl Pts',(49.755350072955,-51.8189928892828,12.));
#123629=CARTESIAN_POINT('Ctrl Pts',(49.7456273031534,-51.7973796306803,
0.));
#123630=CARTESIAN_POINT('Ctrl Pts',(49.7456273031534,-51.7973796306803,
12.));
#123631=CARTESIAN_POINT('Ctrl Pts',(49.7359010133721,-51.7758152395836,
0.));
#123632=CARTESIAN_POINT('Ctrl Pts',(49.7359010133721,-51.7758152395836,
12.));
#123633=CARTESIAN_POINT('Ctrl Pts',(49.7261713119663,-51.754299803067,0.));
#123634=CARTESIAN_POINT('Ctrl Pts',(49.7261713119663,-51.754299803067,12.));
#123635=CARTESIAN_POINT('Ctrl Pts',(49.7164383078212,-51.7328334085091,
0.));
#123636=CARTESIAN_POINT('Ctrl Pts',(49.7164383078212,-51.7328334085091,
12.));
#123637=CARTESIAN_POINT('Ctrl Pts',(49.7067021103553,-51.7114161435869,
0.));
#123638=CARTESIAN_POINT('Ctrl Pts',(49.7067021103553,-51.7114161435869,
12.));
#123639=CARTESIAN_POINT('Ctrl Pts',(49.6969628295262,-51.6900480962773,
0.));
#123640=CARTESIAN_POINT('Ctrl Pts',(49.6969628295262,-51.6900480962773,
12.));
#123641=CARTESIAN_POINT('Ctrl Pts',(49.6872205758336,-51.6687293548682,
0.));
#123642=CARTESIAN_POINT('Ctrl Pts',(49.6872205758336,-51.6687293548682,
12.));
#123643=CARTESIAN_POINT('Ctrl Pts',(49.6774754603245,-51.6474600079622,
0.));
#123644=CARTESIAN_POINT('Ctrl Pts',(49.6774754603245,-51.6474600079622,
12.));
#123645=CARTESIAN_POINT('Ctrl Pts',(49.6677275945967,-51.6262401444791,
0.));
#123646=CARTESIAN_POINT('Ctrl Pts',(49.6677275945967,-51.6262401444791,
12.));
#123647=CARTESIAN_POINT('Ctrl Pts',(49.6579770908037,-51.6050698536496,
0.));
#123648=CARTESIAN_POINT('Ctrl Pts',(49.6579770908037,-51.6050698536496,
12.));
#123649=CARTESIAN_POINT('Ctrl Pts',(49.6482240616593,-51.5839492250181,
0.));
#123650=CARTESIAN_POINT('Ctrl Pts',(49.6482240616593,-51.5839492250181,
12.));
#123651=CARTESIAN_POINT('Ctrl Pts',(49.6384686204413,-51.5628783484525,
0.));
#123652=CARTESIAN_POINT('Ctrl Pts',(49.6384686204413,-51.5628783484525,
12.));
#123653=CARTESIAN_POINT('Ctrl Pts',(49.6287108809965,-51.5418573141484,
0.));
#123654=CARTESIAN_POINT('Ctrl Pts',(49.6287108809965,-51.5418573141484,
12.));
#123655=CARTESIAN_POINT('Ctrl Pts',(49.6189509577452,-51.5208862126315,
0.));
#123656=CARTESIAN_POINT('Ctrl Pts',(49.6189509577452,-51.5208862126315,
12.));
#123657=CARTESIAN_POINT('Ctrl Pts',(49.6091889656866,-51.4999651347523,
0.));
#123658=CARTESIAN_POINT('Ctrl Pts',(49.6091889656866,-51.4999651347523,
12.));
#123659=CARTESIAN_POINT('Ctrl Pts',(49.5994250204031,-51.4790941716888,
0.));
#123660=CARTESIAN_POINT('Ctrl Pts',(49.5994250204031,-51.4790941716888,
12.));
#123661=CARTESIAN_POINT('Ctrl Pts',(49.5896592380654,-51.4582734149583,
0.));
#123662=CARTESIAN_POINT('Ctrl Pts',(49.5896592380654,-51.4582734149583,
12.));
#123663=CARTESIAN_POINT('Ctrl Pts',(49.5798917354365,-51.4375029564197,
0.));
#123664=CARTESIAN_POINT('Ctrl Pts',(49.5798917354365,-51.4375029564197,
12.));
#123665=CARTESIAN_POINT('Ctrl Pts',(49.5701226298769,-51.4167828882756,
0.));
#123666=CARTESIAN_POINT('Ctrl Pts',(49.5701226298769,-51.4167828882756,
12.));
#123667=CARTESIAN_POINT('Ctrl Pts',(49.5603520393496,-51.396113303067,0.));
#123668=CARTESIAN_POINT('Ctrl Pts',(49.5603520393496,-51.396113303067,12.));
#123669=CARTESIAN_POINT('Ctrl Pts',(49.550580082425,-51.3754942936778,0.));
#123670=CARTESIAN_POINT('Ctrl Pts',(49.550580082425,-51.3754942936778,12.));
#123671=CARTESIAN_POINT('Ctrl Pts',(49.5408068782859,-51.3549259533458,
0.));
#123672=CARTESIAN_POINT('Ctrl Pts',(49.5408068782859,-51.3549259533458,
12.));
#123673=CARTESIAN_POINT('Ctrl Pts',(49.5310325467332,-51.3344083756657,
0.));
#123674=CARTESIAN_POINT('Ctrl Pts',(49.5310325467332,-51.3344083756657,
12.));
#123675=CARTESIAN_POINT('Ctrl Pts',(49.5212572081908,-51.313941654591,0.));
#123676=CARTESIAN_POINT('Ctrl Pts',(49.5212572081908,-51.313941654591,12.));
#123677=CARTESIAN_POINT('Ctrl Pts',(49.5114809837122,-51.2935258844289,
0.));
#123678=CARTESIAN_POINT('Ctrl Pts',(49.5114809837122,-51.2935258844289,
12.));
#123679=CARTESIAN_POINT('Ctrl Pts',(49.5017039949852,-51.2731611598475,
0.));
#123680=CARTESIAN_POINT('Ctrl Pts',(49.5017039949852,-51.2731611598475,
12.));
#123681=CARTESIAN_POINT('Ctrl Pts',(49.4919263643362,-51.2528475758846,
0.));
#123682=CARTESIAN_POINT('Ctrl Pts',(49.4919263643362,-51.2528475758846,
12.));
#123683=CARTESIAN_POINT('Ctrl Pts',(49.4821482147356,-51.2325852279506,
0.));
#123684=CARTESIAN_POINT('Ctrl Pts',(49.4821482147356,-51.2325852279506,
12.));
#123685=CARTESIAN_POINT('Ctrl Pts',(49.4723696698021,-51.2123742118287,
0.));
#123686=CARTESIAN_POINT('Ctrl Pts',(49.4723696698021,-51.2123742118287,
12.));
#123687=CARTESIAN_POINT('Ctrl Pts',(49.4625908538074,-51.1922146236686,
0.));
#123688=CARTESIAN_POINT('Ctrl Pts',(49.4625908538074,-51.1922146236686,
12.));
#123689=CARTESIAN_POINT('Ctrl Pts',(49.4528118916832,-51.1721065599973,
0.));
#123690=CARTESIAN_POINT('Ctrl Pts',(49.4528118916832,-51.1721065599973,
12.));
#123691=CARTESIAN_POINT('Ctrl Pts',(49.4430329090287,-51.1520501177291,
0.));
#123692=CARTESIAN_POINT('Ctrl Pts',(49.4430329090287,-51.1520501177291,
12.));
#123693=CARTESIAN_POINT('Ctrl Pts',(49.4332540321178,-51.1320453941702,
0.));
#123694=CARTESIAN_POINT('Ctrl Pts',(49.4332540321178,-51.1320453941702,
12.));
#123695=CARTESIAN_POINT('Ctrl Pts',(49.423475387907,-51.1120924870195,0.));
#123696=CARTESIAN_POINT('Ctrl Pts',(49.423475387907,-51.1120924870195,12.));
#123697=CARTESIAN_POINT('Ctrl Pts',(49.4136971040428,-51.0921914943662,
0.));
#123698=CARTESIAN_POINT('Ctrl Pts',(49.4136971040428,-51.0921914943662,
12.));
#123699=CARTESIAN_POINT('Ctrl Pts',(49.4039193088634,-51.0723425146985,
0.));
#123700=CARTESIAN_POINT('Ctrl Pts',(49.4039193088634,-51.0723425146985,
12.));
#123701=CARTESIAN_POINT('Ctrl Pts',(49.3941421314012,-51.052545646907,0.));
#123702=CARTESIAN_POINT('Ctrl Pts',(49.3941421314012,-51.052545646907,12.));
#123703=CARTESIAN_POINT('Ctrl Pts',(49.3843657013852,-51.0328009902858,
0.));
#123704=CARTESIAN_POINT('Ctrl Pts',(49.3843657013852,-51.0328009902858,
12.));
#123705=CARTESIAN_POINT('Ctrl Pts',(49.3745901492432,-51.0131086445272,
0.));
#123706=CARTESIAN_POINT('Ctrl Pts',(49.3745901492432,-51.0131086445272,
12.));
#123707=CARTESIAN_POINT('Ctrl Pts',(49.3648156061058,-50.9934687097188,
0.));
#123708=CARTESIAN_POINT('Ctrl Pts',(49.3648156061058,-50.9934687097188,
12.));
#123709=CARTESIAN_POINT('Ctrl Pts',(49.355042203823,-50.9738812863646,0.));
#123710=CARTESIAN_POINT('Ctrl Pts',(49.355042203823,-50.9738812863646,12.));
#123711=CARTESIAN_POINT('Ctrl Pts',(49.345270074981,-50.9543464753981,0.));
#123712=CARTESIAN_POINT('Ctrl Pts',(49.345270074981,-50.9543464753981,12.));
#123713=CARTESIAN_POINT('Ctrl Pts',(49.3354993529158,-50.9348643781924,
0.));
#123714=CARTESIAN_POINT('Ctrl Pts',(49.3354993529158,-50.9348643781924,
12.));
#123715=CARTESIAN_POINT('Ctrl Pts',(49.3257301717335,-50.9154350965666,
0.));
#123716=CARTESIAN_POINT('Ctrl Pts',(49.3257301717335,-50.9154350965666,
12.));
#123717=CARTESIAN_POINT('Ctrl Pts',(49.3159626663109,-50.8960587327848,
0.));
#123718=CARTESIAN_POINT('Ctrl Pts',(49.3159626663109,-50.8960587327848,
12.));
#123719=CARTESIAN_POINT('Ctrl Pts',(49.3061969722781,-50.8767353895492,
0.));
#123720=CARTESIAN_POINT('Ctrl Pts',(49.3061969722781,-50.8767353895492,
12.));
#123721=CARTESIAN_POINT('Ctrl Pts',(49.2964332260039,-50.8574651699873,
0.));
#123722=CARTESIAN_POINT('Ctrl Pts',(49.2964332260039,-50.8574651699873,
12.));
#123723=CARTESIAN_POINT('Ctrl Pts',(49.2866715645838,-50.8382481776403,
0.));
#123724=CARTESIAN_POINT('Ctrl Pts',(49.2866715645838,-50.8382481776403,
12.));
#123725=CARTESIAN_POINT('Ctrl Pts',(49.2769121258164,-50.819084516434,0.));
#123726=CARTESIAN_POINT('Ctrl Pts',(49.2769121258164,-50.819084516434,12.));
#123727=CARTESIAN_POINT('Ctrl Pts',(49.2671550482435,-50.7999742907131,
0.));
#123728=CARTESIAN_POINT('Ctrl Pts',(49.2671550482435,-50.7999742907131,
12.));
#123729=CARTESIAN_POINT('Ctrl Pts',(49.2574004712134,-50.7809176052966,
0.));
#123730=CARTESIAN_POINT('Ctrl Pts',(49.2574004712134,-50.7809176052966,
12.));
#123731=CARTESIAN_POINT('Ctrl Pts',(49.2476485349373,-50.7619145655207,
0.));
#123732=CARTESIAN_POINT('Ctrl Pts',(49.2476485349373,-50.7619145655207,
12.));
#123733=CARTESIAN_POINT('Ctrl Pts',(49.2378993805471,-50.7429652772805,
0.));
#123734=CARTESIAN_POINT('Ctrl Pts',(49.2378993805471,-50.7429652772805,
12.));
#123735=CARTESIAN_POINT('Ctrl Pts',(49.228153150155,-50.7240698470679,0.));
#123736=CARTESIAN_POINT('Ctrl Pts',(49.228153150155,-50.7240698470679,12.));
#123737=CARTESIAN_POINT('Ctrl Pts',(49.2184099867461,-50.7052283818922,
0.));
#123738=CARTESIAN_POINT('Ctrl Pts',(49.2184099867461,-50.7052283818922,
12.));
#123739=CARTESIAN_POINT('Ctrl Pts',(49.2086700340614,-50.6864409891895,
0.));
#123740=CARTESIAN_POINT('Ctrl Pts',(49.2086700340614,-50.6864409891895,
12.));
#123741=CARTESIAN_POINT('Ctrl Pts',(49.1989334364995,-50.6677077767432,
0.));
#123742=CARTESIAN_POINT('Ctrl Pts',(49.1989334364995,-50.6677077767432,
12.));
#123743=CARTESIAN_POINT('Ctrl Pts',(49.189200338976,-50.6490288525656,0.));
#123744=CARTESIAN_POINT('Ctrl Pts',(49.189200338976,-50.6490288525656,12.));
#123745=CARTESIAN_POINT('Ctrl Pts',(49.1794708869099,-50.6304043248821,
0.));
#123746=CARTESIAN_POINT('Ctrl Pts',(49.1794708869099,-50.6304043248821,
12.));
#123747=CARTESIAN_POINT('Ctrl Pts',(49.1697452265494,-50.6118343023958,
0.));
#123748=CARTESIAN_POINT('Ctrl Pts',(49.1697452265494,-50.6118343023958,
12.));
#123749=CARTESIAN_POINT('Ctrl Pts',(49.1600235052621,-50.5933188945168,
0.));
#123750=CARTESIAN_POINT('Ctrl Pts',(49.1600235052621,-50.5933188945168,
12.));
#123751=CARTESIAN_POINT('Ctrl Pts',(49.1503058717821,-50.5748582115565,
0.));
#123752=CARTESIAN_POINT('Ctrl Pts',(49.1503058717821,-50.5748582115565,
12.));
#123753=CARTESIAN_POINT('Ctrl Pts',(49.1405924766144,-50.556452365038,0.));
#123754=CARTESIAN_POINT('Ctrl Pts',(49.1405924766144,-50.556452365038,12.));
#123755=CARTESIAN_POINT('Ctrl Pts',(49.1308834717615,-50.5381014674791,
0.));
#123756=CARTESIAN_POINT('Ctrl Pts',(49.1308834717615,-50.5381014674791,
12.));
#123757=CARTESIAN_POINT('Ctrl Pts',(49.1211790099795,-50.5198056318089,
0.));
#123758=CARTESIAN_POINT('Ctrl Pts',(49.1211790099795,-50.5198056318089,
12.));
#123759=CARTESIAN_POINT('Ctrl Pts',(49.1114792441571,-50.501564970874,0.));
#123760=CARTESIAN_POINT('Ctrl Pts',(49.1114792441571,-50.501564970874,12.));
#123761=CARTESIAN_POINT('Ctrl Pts',(49.1017843266803,-50.4833795969318,
0.));
#123762=CARTESIAN_POINT('Ctrl Pts',(49.1017843266803,-50.4833795969318,
12.));
#123763=CARTESIAN_POINT('Ctrl Pts',(49.0920944087008,-50.4652496210607,
0.));
#123764=CARTESIAN_POINT('Ctrl Pts',(49.0920944087008,-50.4652496210607,
12.));
#123765=CARTESIAN_POINT('Ctrl Pts',(49.0824096415371,-50.4471751542751,
0.));
#123766=CARTESIAN_POINT('Ctrl Pts',(49.0824096415371,-50.4471751542751,
12.));
#123767=CARTESIAN_POINT('Ctrl Pts',(49.0727301783494,-50.4291563088547,
0.));
#123768=CARTESIAN_POINT('Ctrl Pts',(49.0727301783494,-50.4291563088547,
12.));
#123769=CARTESIAN_POINT('Ctrl Pts',(49.0630561755075,-50.4111931994257,
0.));
#123770=CARTESIAN_POINT('Ctrl Pts',(49.0630561755075,-50.4111931994257,
12.));
#123771=CARTESIAN_POINT('Ctrl Pts',(49.0533877945744,-50.3932859445252,
0.));
#123772=CARTESIAN_POINT('Ctrl Pts',(49.0533877945744,-50.3932859445252,
12.));
#123773=CARTESIAN_POINT('Ctrl Pts',(49.0437252024832,-50.3754346667353,
0.));
#123774=CARTESIAN_POINT('Ctrl Pts',(49.0437252024832,-50.3754346667353,
12.));
#123775=CARTESIAN_POINT('Ctrl Pts',(49.0340685673982,-50.3576394894108,
0.));
#123776=CARTESIAN_POINT('Ctrl Pts',(49.0340685673982,-50.3576394894108,
12.));
#123777=CARTESIAN_POINT('Ctrl Pts',(49.024418055075,-50.3399005337958,0.));
#123778=CARTESIAN_POINT('Ctrl Pts',(49.024418055075,-50.3399005337958,12.));
#123779=CARTESIAN_POINT('Ctrl Pts',(49.0147738256942,-50.3222179165119,
0.));
#123780=CARTESIAN_POINT('Ctrl Pts',(49.0147738256942,-50.3222179165119,
12.));
#123781=CARTESIAN_POINT('Ctrl Pts',(49.0051360288044,-50.3045917455424,
0.));
#123782=CARTESIAN_POINT('Ctrl Pts',(49.0051360288044,-50.3045917455424,
12.));
#123783=CARTESIAN_POINT('Ctrl Pts',(48.9955048082081,-50.2870221241054,
0.));
#123784=CARTESIAN_POINT('Ctrl Pts',(48.9955048082081,-50.2870221241054,
12.));
#123785=CARTESIAN_POINT('Ctrl Pts',(48.9858803116689,-50.2695091583511,
0.));
#123786=CARTESIAN_POINT('Ctrl Pts',(48.9858803116689,-50.2695091583511,
12.));
#123787=CARTESIAN_POINT('Ctrl Pts',(48.9762626987227,-50.252052963548,0.));
#123788=CARTESIAN_POINT('Ctrl Pts',(48.9762626987227,-50.252052963548,12.));
#123789=CARTESIAN_POINT('Ctrl Pts',(48.9666521500911,-50.234653671541,0.));
#123790=CARTESIAN_POINT('Ctrl Pts',(48.9666521500911,-50.234653671541,12.));
#123791=CARTESIAN_POINT('Ctrl Pts',(48.9570488741167,-50.2173114358325,
0.));
#123792=CARTESIAN_POINT('Ctrl Pts',(48.9570488741167,-50.2173114358325,
12.));
#123793=CARTESIAN_POINT('Ctrl Pts',(48.9474530868733,-50.2000264157797,
0.));
#123794=CARTESIAN_POINT('Ctrl Pts',(48.9474530868733,-50.2000264157797,
12.));
#123795=CARTESIAN_POINT('Ctrl Pts',(48.9378649933055,-50.1827987615602,
0.));
#123796=CARTESIAN_POINT('Ctrl Pts',(48.9378649933055,-50.1827987615602,
12.));
#123797=CARTESIAN_POINT('Ctrl Pts',(48.9282847698294,-50.1656286003997,
0.));
#123798=CARTESIAN_POINT('Ctrl Pts',(48.9282847698294,-50.1656286003997,
12.));
#123799=CARTESIAN_POINT('Ctrl Pts',(48.9187125418099,-50.1485160184657,
0.));
#123800=CARTESIAN_POINT('Ctrl Pts',(48.9187125418099,-50.1485160184657,
12.));
#123801=CARTESIAN_POINT('Ctrl Pts',(48.90914838181,-50.1314610602569,0.));
#123802=CARTESIAN_POINT('Ctrl Pts',(48.90914838181,-50.1314610602569,12.));
#123803=CARTESIAN_POINT('Ctrl Pts',(48.9015035372055,-50.1178632067084,
0.));
#123804=CARTESIAN_POINT('Ctrl Pts',(48.9015035372055,-50.1178632067084,
12.));
#123805=CARTESIAN_POINT('Ctrl Pts',(48.895773555686,-50.1076907555471,0.));
#123806=CARTESIAN_POINT('Ctrl Pts',(48.895773555686,-50.1076907555471,12.));
#123807=CARTESIAN_POINT('Ctrl Pts',(48.8919551910366,-50.1009206494272,
0.));
#123808=CARTESIAN_POINT('Ctrl Pts',(48.8919551910366,-50.1009206494272,
12.));
#123809=CARTESIAN_POINT('Ctrl Pts',(48.8900464144686,-50.0975384783635,
0.));
#123810=CARTESIAN_POINT('Ctrl Pts',(48.8900464144686,-50.0975384783635,
12.));
#123811=CARTESIAN_POINT('',(48.8900464144686,-50.0975384783635,12.));
#123812=CARTESIAN_POINT('Ctrl Pts',(48.8900464144686,-50.0975384783635,
12.));
#123813=CARTESIAN_POINT('Ctrl Pts',(48.8919551910366,-50.1009206494272,
12.));
#123814=CARTESIAN_POINT('Ctrl Pts',(48.895773555686,-50.1076907555471,12.));
#123815=CARTESIAN_POINT('Ctrl Pts',(48.9015035372055,-50.1178632067084,
12.));
#123816=CARTESIAN_POINT('Ctrl Pts',(48.90914838181,-50.1314610602569,12.));
#123817=CARTESIAN_POINT('Ctrl Pts',(48.9187125418099,-50.1485160184657,
12.));
#123818=CARTESIAN_POINT('Ctrl Pts',(48.9282847698294,-50.1656286003997,
12.));
#123819=CARTESIAN_POINT('Ctrl Pts',(48.9378649933055,-50.1827987615602,
12.));
#123820=CARTESIAN_POINT('Ctrl Pts',(48.9474530868733,-50.2000264157797,
12.));
#123821=CARTESIAN_POINT('Ctrl Pts',(48.9570488741167,-50.2173114358325,
12.));
#123822=CARTESIAN_POINT('Ctrl Pts',(48.9666521500911,-50.234653671541,12.));
#123823=CARTESIAN_POINT('Ctrl Pts',(48.9762626987227,-50.252052963548,12.));
#123824=CARTESIAN_POINT('Ctrl Pts',(48.9858803116689,-50.2695091583511,
12.));
#123825=CARTESIAN_POINT('Ctrl Pts',(48.9955048082081,-50.2870221241054,
12.));
#123826=CARTESIAN_POINT('Ctrl Pts',(49.0051360288044,-50.3045917455424,
12.));
#123827=CARTESIAN_POINT('Ctrl Pts',(49.0147738256942,-50.3222179165119,
12.));
#123828=CARTESIAN_POINT('Ctrl Pts',(49.024418055075,-50.3399005337958,12.));
#123829=CARTESIAN_POINT('Ctrl Pts',(49.0340685673982,-50.3576394894108,
12.));
#123830=CARTESIAN_POINT('Ctrl Pts',(49.0437252024832,-50.3754346667353,
12.));
#123831=CARTESIAN_POINT('Ctrl Pts',(49.0533877945744,-50.3932859445252,
12.));
#123832=CARTESIAN_POINT('Ctrl Pts',(49.0630561755075,-50.4111931994257,
12.));
#123833=CARTESIAN_POINT('Ctrl Pts',(49.0727301783494,-50.4291563088547,
12.));
#123834=CARTESIAN_POINT('Ctrl Pts',(49.0824096415371,-50.4471751542751,
12.));
#123835=CARTESIAN_POINT('Ctrl Pts',(49.0920944087008,-50.4652496210607,
12.));
#123836=CARTESIAN_POINT('Ctrl Pts',(49.1017843266803,-50.4833795969318,
12.));
#123837=CARTESIAN_POINT('Ctrl Pts',(49.1114792441571,-50.501564970874,12.));
#123838=CARTESIAN_POINT('Ctrl Pts',(49.1211790099795,-50.5198056318089,
12.));
#123839=CARTESIAN_POINT('Ctrl Pts',(49.1308834717615,-50.5381014674791,
12.));
#123840=CARTESIAN_POINT('Ctrl Pts',(49.1405924766144,-50.556452365038,12.));
#123841=CARTESIAN_POINT('Ctrl Pts',(49.1503058717821,-50.5748582115565,
12.));
#123842=CARTESIAN_POINT('Ctrl Pts',(49.1600235052621,-50.5933188945168,
12.));
#123843=CARTESIAN_POINT('Ctrl Pts',(49.1697452265494,-50.6118343023958,
12.));
#123844=CARTESIAN_POINT('Ctrl Pts',(49.1794708869099,-50.6304043248821,
12.));
#123845=CARTESIAN_POINT('Ctrl Pts',(49.189200338976,-50.6490288525656,12.));
#123846=CARTESIAN_POINT('Ctrl Pts',(49.1989334364995,-50.6677077767432,
12.));
#123847=CARTESIAN_POINT('Ctrl Pts',(49.2086700340614,-50.6864409891895,
12.));
#123848=CARTESIAN_POINT('Ctrl Pts',(49.2184099867461,-50.7052283818922,
12.));
#123849=CARTESIAN_POINT('Ctrl Pts',(49.228153150155,-50.7240698470679,12.));
#123850=CARTESIAN_POINT('Ctrl Pts',(49.2378993805471,-50.7429652772805,
12.));
#123851=CARTESIAN_POINT('Ctrl Pts',(49.2476485349373,-50.7619145655207,
12.));
#123852=CARTESIAN_POINT('Ctrl Pts',(49.2574004712134,-50.7809176052966,
12.));
#123853=CARTESIAN_POINT('Ctrl Pts',(49.2671550482435,-50.7999742907131,
12.));
#123854=CARTESIAN_POINT('Ctrl Pts',(49.2769121258164,-50.819084516434,12.));
#123855=CARTESIAN_POINT('Ctrl Pts',(49.2866715645838,-50.8382481776403,
12.));
#123856=CARTESIAN_POINT('Ctrl Pts',(49.2964332260039,-50.8574651699873,
12.));
#123857=CARTESIAN_POINT('Ctrl Pts',(49.3061969722781,-50.8767353895492,
12.));
#123858=CARTESIAN_POINT('Ctrl Pts',(49.3159626663109,-50.8960587327848,
12.));
#123859=CARTESIAN_POINT('Ctrl Pts',(49.3257301717335,-50.9154350965666,
12.));
#123860=CARTESIAN_POINT('Ctrl Pts',(49.3354993529158,-50.9348643781924,
12.));
#123861=CARTESIAN_POINT('Ctrl Pts',(49.345270074981,-50.9543464753981,12.));
#123862=CARTESIAN_POINT('Ctrl Pts',(49.355042203823,-50.9738812863646,12.));
#123863=CARTESIAN_POINT('Ctrl Pts',(49.3648156061058,-50.9934687097188,
12.));
#123864=CARTESIAN_POINT('Ctrl Pts',(49.3745901492432,-51.0131086445272,
12.));
#123865=CARTESIAN_POINT('Ctrl Pts',(49.3843657013852,-51.0328009902858,
12.));
#123866=CARTESIAN_POINT('Ctrl Pts',(49.3941421314012,-51.052545646907,12.));
#123867=CARTESIAN_POINT('Ctrl Pts',(49.4039193088634,-51.0723425146985,
12.));
#123868=CARTESIAN_POINT('Ctrl Pts',(49.4136971040428,-51.0921914943662,
12.));
#123869=CARTESIAN_POINT('Ctrl Pts',(49.423475387907,-51.1120924870195,12.));
#123870=CARTESIAN_POINT('Ctrl Pts',(49.4332540321178,-51.1320453941702,
12.));
#123871=CARTESIAN_POINT('Ctrl Pts',(49.4430329090287,-51.1520501177291,
12.));
#123872=CARTESIAN_POINT('Ctrl Pts',(49.4528118916832,-51.1721065599973,
12.));
#123873=CARTESIAN_POINT('Ctrl Pts',(49.4625908538074,-51.1922146236686,
12.));
#123874=CARTESIAN_POINT('Ctrl Pts',(49.4723696698021,-51.2123742118287,
12.));
#123875=CARTESIAN_POINT('Ctrl Pts',(49.4821482147356,-51.2325852279506,
12.));
#123876=CARTESIAN_POINT('Ctrl Pts',(49.4919263643362,-51.2528475758846,
12.));
#123877=CARTESIAN_POINT('Ctrl Pts',(49.5017039949852,-51.2731611598475,
12.));
#123878=CARTESIAN_POINT('Ctrl Pts',(49.5114809837122,-51.2935258844289,
12.));
#123879=CARTESIAN_POINT('Ctrl Pts',(49.5212572081908,-51.313941654591,12.));
#123880=CARTESIAN_POINT('Ctrl Pts',(49.5310325467332,-51.3344083756657,
12.));
#123881=CARTESIAN_POINT('Ctrl Pts',(49.5408068782859,-51.3549259533458,
12.));
#123882=CARTESIAN_POINT('Ctrl Pts',(49.550580082425,-51.3754942936778,12.));
#123883=CARTESIAN_POINT('Ctrl Pts',(49.5603520393496,-51.396113303067,12.));
#123884=CARTESIAN_POINT('Ctrl Pts',(49.5701226298769,-51.4167828882756,
12.));
#123885=CARTESIAN_POINT('Ctrl Pts',(49.5798917354365,-51.4375029564197,
12.));
#123886=CARTESIAN_POINT('Ctrl Pts',(49.5896592380654,-51.4582734149583,
12.));
#123887=CARTESIAN_POINT('Ctrl Pts',(49.5994250204031,-51.4790941716888,
12.));
#123888=CARTESIAN_POINT('Ctrl Pts',(49.6091889656866,-51.4999651347523,
12.));
#123889=CARTESIAN_POINT('Ctrl Pts',(49.6189509577452,-51.5208862126315,
12.));
#123890=CARTESIAN_POINT('Ctrl Pts',(49.6287108809965,-51.5418573141484,
12.));
#123891=CARTESIAN_POINT('Ctrl Pts',(49.6384686204413,-51.5628783484525,
12.));
#123892=CARTESIAN_POINT('Ctrl Pts',(49.6482240616593,-51.5839492250181,
12.));
#123893=CARTESIAN_POINT('Ctrl Pts',(49.6579770908037,-51.6050698536496,
12.));
#123894=CARTESIAN_POINT('Ctrl Pts',(49.6677275945967,-51.6262401444791,
12.));
#123895=CARTESIAN_POINT('Ctrl Pts',(49.6774754603245,-51.6474600079622,
12.));
#123896=CARTESIAN_POINT('Ctrl Pts',(49.6872205758336,-51.6687293548682,
12.));
#123897=CARTESIAN_POINT('Ctrl Pts',(49.6969628295262,-51.6900480962773,
12.));
#123898=CARTESIAN_POINT('Ctrl Pts',(49.7067021103553,-51.7114161435869,
12.));
#123899=CARTESIAN_POINT('Ctrl Pts',(49.7164383078212,-51.7328334085091,
12.));
#123900=CARTESIAN_POINT('Ctrl Pts',(49.7261713119663,-51.754299803067,12.));
#123901=CARTESIAN_POINT('Ctrl Pts',(49.7359010133721,-51.7758152395836,
12.));
#123902=CARTESIAN_POINT('Ctrl Pts',(49.7456273031534,-51.7973796306803,
12.));
#123903=CARTESIAN_POINT('Ctrl Pts',(49.755350072955,-51.8189928892828,12.));
#123904=CARTESIAN_POINT('Ctrl Pts',(49.7650692149462,-51.8406549286175,
12.));
#123905=CARTESIAN_POINT('Ctrl Pts',(49.7747846218182,-51.8623656622097,
12.));
#123906=CARTESIAN_POINT('Ctrl Pts',(49.7844961867807,-51.8841250038724,
12.));
#123907=CARTESIAN_POINT('Ctrl Pts',(49.7942038035576,-51.9059328677059,
12.));
#123908=CARTESIAN_POINT('Ctrl Pts',(49.8039073663812,-51.9277891681018,
12.));
#123909=CARTESIAN_POINT('Ctrl Pts',(49.8136067699896,-51.9496938197418,
12.));
#123910=CARTESIAN_POINT('Ctrl Pts',(49.8233019096222,-51.9716467375937,
12.));
#123911=CARTESIAN_POINT('Ctrl Pts',(49.8329926810171,-51.9936478369008,
12.));
#123912=CARTESIAN_POINT('Ctrl Pts',(49.8426789804071,-52.0156970331823,
12.));
#123913=CARTESIAN_POINT('Ctrl Pts',(49.8523607045149,-52.0377942422376,
12.));
#123914=CARTESIAN_POINT('Ctrl Pts',(49.86203775055,-52.0599393801452,12.));
#123915=CARTESIAN_POINT('Ctrl Pts',(49.8717100162048,-52.0821323632587,
12.));
#123916=CARTESIAN_POINT('Ctrl Pts',(49.8813773996517,-52.1043731081962,
12.));
#123917=CARTESIAN_POINT('Ctrl Pts',(49.8910397995397,-52.1266615318407,
12.));
#123918=CARTESIAN_POINT('Ctrl Pts',(49.9006971149894,-52.1489975513445,
12.));
#123919=CARTESIAN_POINT('Ctrl Pts',(49.9103492455902,-52.1713810841276,
12.));
#123920=CARTESIAN_POINT('Ctrl Pts',(49.9199960913962,-52.1938120478754,
12.));
#123921=CARTESIAN_POINT('Ctrl Pts',(49.9296375529245,-52.2162903605275,
12.));
#123922=CARTESIAN_POINT('Ctrl Pts',(49.9392735311509,-52.2388159402771,
12.));
#123923=CARTESIAN_POINT('Ctrl Pts',(49.9489039275064,-52.2613887055773,
12.));
#123924=CARTESIAN_POINT('Ctrl Pts',(49.9585286438733,-52.2840085751384,
12.));
#123925=CARTESIAN_POINT('Ctrl Pts',(49.9681475825824,-52.3066754679265,
12.));
#123926=CARTESIAN_POINT('Ctrl Pts',(49.9777606464106,-52.3293893031528,
12.));
#123927=CARTESIAN_POINT('Ctrl Pts',(49.9873677385775,-52.3521500002718,
12.));
#123928=CARTESIAN_POINT('Ctrl Pts',(49.9969687627408,-52.3749574789871,
12.));
#123929=CARTESIAN_POINT('Ctrl Pts',(50.0065636229938,-52.3978116592509,
12.));
#123930=CARTESIAN_POINT('Ctrl Pts',(50.0161522238616,-52.4207124612608,
12.));
#123931=CARTESIAN_POINT('Ctrl Pts',(50.0257344703,-52.4436598054515,12.));
#123932=CARTESIAN_POINT('Ctrl Pts',(50.0353102676921,-52.4666536124913,
12.));
#123933=CARTESIAN_POINT('Ctrl Pts',(50.0448795218441,-52.4896938032884,
12.));
#123934=CARTESIAN_POINT('Ctrl Pts',(50.0544421389817,-52.5127802989896,
12.));
#123935=CARTESIAN_POINT('Ctrl Pts',(50.0639980257479,-52.5359130209792,
12.));
#123936=CARTESIAN_POINT('Ctrl Pts',(50.0735470892007,-52.5590918908702,
12.));
#123937=CARTESIAN_POINT('Ctrl Pts',(50.0830892368107,-52.5823168304994,
12.));
#123938=CARTESIAN_POINT('Ctrl Pts',(50.0926243764578,-52.6055877619348,
12.));
#123939=CARTESIAN_POINT('Ctrl Pts',(50.1021524164264,-52.6289046074746,
12.));
#123940=CARTESIAN_POINT('Ctrl Pts',(50.111673265404,-52.652267289646,12.));
#123941=CARTESIAN_POINT('Ctrl Pts',(50.121186832478,-52.6756757311978,12.));
#123942=CARTESIAN_POINT('Ctrl Pts',(50.1306930271345,-52.699129855093,12.));
#123943=CARTESIAN_POINT('Ctrl Pts',(50.1401917592537,-52.7226295845161,
12.));
#123944=CARTESIAN_POINT('Ctrl Pts',(50.1496829391073,-52.7461748428738,
12.));
#123945=CARTESIAN_POINT('Ctrl Pts',(50.1591664773561,-52.769765553794,12.));
#123946=CARTESIAN_POINT('Ctrl Pts',(50.1686422850487,-52.7934016411205,
12.));
#123947=CARTESIAN_POINT('Ctrl Pts',(50.1781102736205,-52.8170830289044,
12.));
#123948=CARTESIAN_POINT('Ctrl Pts',(50.1875703548884,-52.8408096414093,
12.));
#123949=CARTESIAN_POINT('Ctrl Pts',(50.1970224410471,-52.8645814031133,
12.));
#123950=CARTESIAN_POINT('Ctrl Pts',(50.2064664446663,-52.8883982387068,
12.));
#123951=CARTESIAN_POINT('Ctrl Pts',(50.2159022786879,-52.9122600730884,
12.));
#123952=CARTESIAN_POINT('Ctrl Pts',(50.2253298564241,-52.9361668313542,
12.));
#123953=CARTESIAN_POINT('Ctrl Pts',(50.2347490915555,-52.9601184388028,
12.));
#123954=CARTESIAN_POINT('Ctrl Pts',(50.2441598981286,-52.9841148209402,
12.));
#123955=CARTESIAN_POINT('Ctrl Pts',(50.2535621905552,-53.0081559034801,
12.));
#123956=CARTESIAN_POINT('Ctrl Pts',(50.2629558836111,-53.0322416123406,
12.));
#123957=CARTESIAN_POINT('Ctrl Pts',(50.2723408924373,-53.0563718736366,
12.));
#123958=CARTESIAN_POINT('Ctrl Pts',(50.2817171325358,-53.0805466136798,
12.));
#123959=CARTESIAN_POINT('Ctrl Pts',(50.2910845197619,-53.1047657589812,
12.));
#123960=CARTESIAN_POINT('Ctrl Pts',(50.300442970319,-53.1290292362485,12.));
#123961=CARTESIAN_POINT('Ctrl Pts',(50.3097924007534,-53.1533369723818,
12.));
#123962=CARTESIAN_POINT('Ctrl Pts',(50.3191327279492,-53.1776888944616,
12.));
#123963=CARTESIAN_POINT('Ctrl Pts',(50.3284638691278,-53.2020849297471,
12.));
#123964=CARTESIAN_POINT('Ctrl Pts',(50.3377857418514,-53.2265250056887,
12.));
#123965=CARTESIAN_POINT('Ctrl Pts',(50.3470982640289,-53.2510090499336,
12.));
#123966=CARTESIAN_POINT('Ctrl Pts',(50.3564013539199,-53.2755369903293,
12.));
#123967=CARTESIAN_POINT('Ctrl Pts',(50.365694930143,-53.300108754923,12.));
#123968=CARTESIAN_POINT('Ctrl Pts',(50.3749789116786,-53.3247242719587,
12.));
#123969=CARTESIAN_POINT('Ctrl Pts',(50.384253217846,-53.3493834698697,12.));
#123970=CARTESIAN_POINT('Ctrl Pts',(50.3935177682837,-53.3740862772681,
12.));
#123971=CARTESIAN_POINT('Ctrl Pts',(50.4027724829297,-53.398832622931,12.));
#123972=CARTESIAN_POINT('Ctrl Pts',(50.4120172820047,-53.4236224357838,
12.));
#123973=CARTESIAN_POINT('Ctrl Pts',(50.4212520859914,-53.4484556448776,
12.));
#123974=CARTESIAN_POINT('Ctrl Pts',(50.4304768156666,-53.4733321794188,
12.));
#123975=CARTESIAN_POINT('Ctrl Pts',(50.4396913921381,-53.4982519688024,
12.));
#123976=CARTESIAN_POINT('Ctrl Pts',(50.4488957368839,-53.5232149426413,
12.));
#123977=CARTESIAN_POINT('Ctrl Pts',(50.4580897717838,-53.5482210307868,
12.));
#123978=CARTESIAN_POINT('Ctrl Pts',(50.4672734191756,-53.5732701633609,
12.));
#123979=CARTESIAN_POINT('Ctrl Pts',(50.4764466018071,-53.5983622707238,
12.));
#123980=CARTESIAN_POINT('Ctrl Pts',(50.4856092427314,-53.623497283406,12.));
#123981=CARTESIAN_POINT('Ctrl Pts',(50.4947612652148,-53.6486751320436,
12.));
#123982=CARTESIAN_POINT('Ctrl Pts',(50.503902592653,-53.6738957473158,12.));
#123983=CARTESIAN_POINT('Ctrl Pts',(50.513033148456,-53.6991590598548,12.));
#123984=CARTESIAN_POINT('Ctrl Pts',(50.522152856042,-53.7244650002374,12.));
#123985=CARTESIAN_POINT('Ctrl Pts',(50.5312616390779,-53.7498134991703,
12.));
#123986=CARTESIAN_POINT('Ctrl Pts',(50.5403594216698,-53.7752044876304,
12.));
#123987=CARTESIAN_POINT('Ctrl Pts',(50.5494461285761,-53.8006378970197,
12.));
#123988=CARTESIAN_POINT('Ctrl Pts',(50.5585216854091,-53.8261136593075,
12.));
#123989=CARTESIAN_POINT('Ctrl Pts',(50.5675860188538,-53.8516317071804,
12.));
#123990=CARTESIAN_POINT('Ctrl Pts',(50.5766390561884,-53.8771919737032,
12.));
#123991=CARTESIAN_POINT('Ctrl Pts',(50.5856807248151,-53.9027943919836,
12.));
#123992=CARTESIAN_POINT('Ctrl Pts',(50.5947109517483,-53.9284388948004,
12.));
#123993=CARTESIAN_POINT('Ctrl Pts',(50.6037296632139,-53.9541254143119,
12.));
#123994=CARTESIAN_POINT('Ctrl Pts',(50.6127367839711,-53.979853881553,12.));
#123995=CARTESIAN_POINT('Ctrl Pts',(50.6217322378648,-54.0056242268399,
12.));
#123996=CARTESIAN_POINT('Ctrl Pts',(50.6307159490553,-54.0314363806708,
12.));
#123997=CARTESIAN_POINT('Ctrl Pts',(50.6396878430939,-54.0572902745076,
12.));
#123998=CARTESIAN_POINT('Ctrl Pts',(50.6486478479465,-54.0831858415189,
12.));
#123999=CARTESIAN_POINT('Ctrl Pts',(50.6575958953221,-54.1091230175367,
12.));
#124000=CARTESIAN_POINT('Ctrl Pts',(50.6665319209869,-54.1351017412804,
12.));
#124001=CARTESIAN_POINT('Ctrl Pts',(50.6741814675485,-54.1574061042042,
12.));
#124002=CARTESIAN_POINT('Ctrl Pts',(50.6800396668777,-54.1745287898794,
12.));
#124003=CARTESIAN_POINT('Ctrl Pts',(50.684111886193,-54.1864514382193,12.));
#124004=CARTESIAN_POINT('Ctrl Pts',(50.6864016965742,-54.1931619277619,
12.));
#124005=CARTESIAN_POINT('Ctrl Pts',(50.6869108458849,-54.1946543500368,
12.));
#124006=CARTESIAN_POINT('',(48.8900464144686,-50.0975384783635,0.));
#124007=CARTESIAN_POINT('',(48.8900464144686,-50.0975384783634,0.));
#124008=CARTESIAN_POINT('Ctrl Pts',(50.6869108458849,-54.1946543500368,
0.));
#124009=CARTESIAN_POINT('Ctrl Pts',(50.6864016965742,-54.1931619277619,
0.));
#124010=CARTESIAN_POINT('Ctrl Pts',(50.684111886193,-54.1864514382193,0.));
#124011=CARTESIAN_POINT('Ctrl Pts',(50.6800396668777,-54.1745287898794,
0.));
#124012=CARTESIAN_POINT('Ctrl Pts',(50.6741814675486,-54.1574061042042,
0.));
#124013=CARTESIAN_POINT('Ctrl Pts',(50.6665319209869,-54.1351017412804,
0.));
#124014=CARTESIAN_POINT('Ctrl Pts',(50.6575958953221,-54.1091230175367,
0.));
#124015=CARTESIAN_POINT('Ctrl Pts',(50.6486478479465,-54.0831858415189,
0.));
#124016=CARTESIAN_POINT('Ctrl Pts',(50.6396878430939,-54.0572902745076,
0.));
#124017=CARTESIAN_POINT('Ctrl Pts',(50.6307159490553,-54.0314363806708,
0.));
#124018=CARTESIAN_POINT('Ctrl Pts',(50.6217322378648,-54.0056242268399,
0.));
#124019=CARTESIAN_POINT('Ctrl Pts',(50.6127367839711,-53.979853881553,0.));
#124020=CARTESIAN_POINT('Ctrl Pts',(50.6037296632139,-53.9541254143119,
0.));
#124021=CARTESIAN_POINT('Ctrl Pts',(50.5947109517483,-53.9284388948004,
0.));
#124022=CARTESIAN_POINT('Ctrl Pts',(50.5856807248151,-53.9027943919836,
0.));
#124023=CARTESIAN_POINT('Ctrl Pts',(50.5766390561884,-53.8771919737032,
0.));
#124024=CARTESIAN_POINT('Ctrl Pts',(50.5675860188538,-53.8516317071804,
0.));
#124025=CARTESIAN_POINT('Ctrl Pts',(50.5585216854091,-53.8261136593075,
0.));
#124026=CARTESIAN_POINT('Ctrl Pts',(50.5494461285761,-53.8006378970197,
0.));
#124027=CARTESIAN_POINT('Ctrl Pts',(50.5403594216698,-53.7752044876304,
0.));
#124028=CARTESIAN_POINT('Ctrl Pts',(50.5312616390779,-53.7498134991703,
0.));
#124029=CARTESIAN_POINT('Ctrl Pts',(50.522152856042,-53.7244650002374,0.));
#124030=CARTESIAN_POINT('Ctrl Pts',(50.513033148456,-53.6991590598548,0.));
#124031=CARTESIAN_POINT('Ctrl Pts',(50.503902592653,-53.6738957473158,0.));
#124032=CARTESIAN_POINT('Ctrl Pts',(50.4947612652148,-53.6486751320436,
0.));
#124033=CARTESIAN_POINT('Ctrl Pts',(50.4856092427314,-53.623497283406,0.));
#124034=CARTESIAN_POINT('Ctrl Pts',(50.4764466018071,-53.5983622707238,
0.));
#124035=CARTESIAN_POINT('Ctrl Pts',(50.4672734191756,-53.5732701633609,
0.));
#124036=CARTESIAN_POINT('Ctrl Pts',(50.4580897717838,-53.5482210307868,
0.));
#124037=CARTESIAN_POINT('Ctrl Pts',(50.4488957368839,-53.5232149426413,
0.));
#124038=CARTESIAN_POINT('Ctrl Pts',(50.4396913921381,-53.4982519688024,
0.));
#124039=CARTESIAN_POINT('Ctrl Pts',(50.4304768156666,-53.4733321794188,
0.));
#124040=CARTESIAN_POINT('Ctrl Pts',(50.4212520859914,-53.4484556448776,
0.));
#124041=CARTESIAN_POINT('Ctrl Pts',(50.4120172820047,-53.4236224357838,
0.));
#124042=CARTESIAN_POINT('Ctrl Pts',(50.4027724829297,-53.398832622931,0.));
#124043=CARTESIAN_POINT('Ctrl Pts',(50.3935177682837,-53.3740862772681,
0.));
#124044=CARTESIAN_POINT('Ctrl Pts',(50.384253217846,-53.3493834698697,0.));
#124045=CARTESIAN_POINT('Ctrl Pts',(50.3749789116786,-53.3247242719587,
0.));
#124046=CARTESIAN_POINT('Ctrl Pts',(50.365694930143,-53.300108754923,0.));
#124047=CARTESIAN_POINT('Ctrl Pts',(50.3564013539199,-53.2755369903293,
0.));
#124048=CARTESIAN_POINT('Ctrl Pts',(50.3470982640289,-53.2510090499336,
0.));
#124049=CARTESIAN_POINT('Ctrl Pts',(50.3377857418514,-53.2265250056887,
0.));
#124050=CARTESIAN_POINT('Ctrl Pts',(50.3284638691278,-53.2020849297471,
0.));
#124051=CARTESIAN_POINT('Ctrl Pts',(50.3191327279492,-53.1776888944616,
0.));
#124052=CARTESIAN_POINT('Ctrl Pts',(50.3097924007534,-53.1533369723818,
0.));
#124053=CARTESIAN_POINT('Ctrl Pts',(50.300442970319,-53.1290292362485,0.));
#124054=CARTESIAN_POINT('Ctrl Pts',(50.2910845197619,-53.1047657589812,
0.));
#124055=CARTESIAN_POINT('Ctrl Pts',(50.2817171325358,-53.0805466136798,
0.));
#124056=CARTESIAN_POINT('Ctrl Pts',(50.2723408924373,-53.0563718736366,
0.));
#124057=CARTESIAN_POINT('Ctrl Pts',(50.2629558836111,-53.0322416123406,
0.));
#124058=CARTESIAN_POINT('Ctrl Pts',(50.2535621905552,-53.0081559034801,
0.));
#124059=CARTESIAN_POINT('Ctrl Pts',(50.2441598981286,-52.9841148209402,
0.));
#124060=CARTESIAN_POINT('Ctrl Pts',(50.2347490915555,-52.9601184388028,
0.));
#124061=CARTESIAN_POINT('Ctrl Pts',(50.2253298564241,-52.9361668313542,
0.));
#124062=CARTESIAN_POINT('Ctrl Pts',(50.2159022786879,-52.9122600730884,
0.));
#124063=CARTESIAN_POINT('Ctrl Pts',(50.2064664446663,-52.8883982387068,
0.));
#124064=CARTESIAN_POINT('Ctrl Pts',(50.1970224410471,-52.8645814031133,
0.));
#124065=CARTESIAN_POINT('Ctrl Pts',(50.1875703548884,-52.8408096414093,
0.));
#124066=CARTESIAN_POINT('Ctrl Pts',(50.1781102736205,-52.8170830289044,
0.));
#124067=CARTESIAN_POINT('Ctrl Pts',(50.1686422850487,-52.7934016411205,
0.));
#124068=CARTESIAN_POINT('Ctrl Pts',(50.1591664773561,-52.769765553794,0.));
#124069=CARTESIAN_POINT('Ctrl Pts',(50.1496829391073,-52.7461748428738,
0.));
#124070=CARTESIAN_POINT('Ctrl Pts',(50.1401917592537,-52.7226295845161,
0.));
#124071=CARTESIAN_POINT('Ctrl Pts',(50.1306930271345,-52.699129855093,0.));
#124072=CARTESIAN_POINT('Ctrl Pts',(50.121186832478,-52.6756757311978,0.));
#124073=CARTESIAN_POINT('Ctrl Pts',(50.111673265404,-52.652267289646,0.));
#124074=CARTESIAN_POINT('Ctrl Pts',(50.1021524164264,-52.6289046074746,
0.));
#124075=CARTESIAN_POINT('Ctrl Pts',(50.0926243764578,-52.6055877619348,
0.));
#124076=CARTESIAN_POINT('Ctrl Pts',(50.0830892368107,-52.5823168304994,
0.));
#124077=CARTESIAN_POINT('Ctrl Pts',(50.0735470892007,-52.5590918908702,
0.));
#124078=CARTESIAN_POINT('Ctrl Pts',(50.0639980257479,-52.5359130209792,
0.));
#124079=CARTESIAN_POINT('Ctrl Pts',(50.0544421389817,-52.5127802989896,
0.));
#124080=CARTESIAN_POINT('Ctrl Pts',(50.0448795218441,-52.4896938032884,
0.));
#124081=CARTESIAN_POINT('Ctrl Pts',(50.0353102676921,-52.4666536124913,
0.));
#124082=CARTESIAN_POINT('Ctrl Pts',(50.0257344703,-52.4436598054515,0.));
#124083=CARTESIAN_POINT('Ctrl Pts',(50.0161522238616,-52.4207124612608,
0.));
#124084=CARTESIAN_POINT('Ctrl Pts',(50.0065636229938,-52.3978116592509,
0.));
#124085=CARTESIAN_POINT('Ctrl Pts',(49.9969687627408,-52.3749574789871,
0.));
#124086=CARTESIAN_POINT('Ctrl Pts',(49.9873677385775,-52.3521500002718,
0.));
#124087=CARTESIAN_POINT('Ctrl Pts',(49.9777606464106,-52.3293893031528,
0.));
#124088=CARTESIAN_POINT('Ctrl Pts',(49.9681475825824,-52.3066754679265,
0.));
#124089=CARTESIAN_POINT('Ctrl Pts',(49.9585286438733,-52.2840085751384,
0.));
#124090=CARTESIAN_POINT('Ctrl Pts',(49.9489039275064,-52.2613887055773,
0.));
#124091=CARTESIAN_POINT('Ctrl Pts',(49.9392735311509,-52.2388159402771,
0.));
#124092=CARTESIAN_POINT('Ctrl Pts',(49.9296375529245,-52.2162903605275,
0.));
#124093=CARTESIAN_POINT('Ctrl Pts',(49.9199960913962,-52.1938120478754,
0.));
#124094=CARTESIAN_POINT('Ctrl Pts',(49.9103492455902,-52.1713810841276,
0.));
#124095=CARTESIAN_POINT('Ctrl Pts',(49.9006971149894,-52.1489975513445,
0.));
#124096=CARTESIAN_POINT('Ctrl Pts',(49.8910397995397,-52.1266615318407,
0.));
#124097=CARTESIAN_POINT('Ctrl Pts',(49.8813773996517,-52.1043731081962,
0.));
#124098=CARTESIAN_POINT('Ctrl Pts',(49.8717100162048,-52.0821323632587,
0.));
#124099=CARTESIAN_POINT('Ctrl Pts',(49.86203775055,-52.0599393801452,0.));
#124100=CARTESIAN_POINT('Ctrl Pts',(49.8523607045149,-52.0377942422376,
0.));
#124101=CARTESIAN_POINT('Ctrl Pts',(49.8426789804071,-52.0156970331823,
0.));
#124102=CARTESIAN_POINT('Ctrl Pts',(49.8329926810171,-51.9936478369008,
0.));
#124103=CARTESIAN_POINT('Ctrl Pts',(49.8233019096222,-51.9716467375937,
0.));
#124104=CARTESIAN_POINT('Ctrl Pts',(49.8136067699896,-51.9496938197418,
0.));
#124105=CARTESIAN_POINT('Ctrl Pts',(49.8039073663812,-51.9277891681018,
0.));
#124106=CARTESIAN_POINT('Ctrl Pts',(49.7942038035576,-51.9059328677059,
0.));
#124107=CARTESIAN_POINT('Ctrl Pts',(49.7844961867807,-51.8841250038724,
0.));
#124108=CARTESIAN_POINT('Ctrl Pts',(49.7747846218182,-51.8623656622097,
0.));
#124109=CARTESIAN_POINT('Ctrl Pts',(49.7650692149462,-51.8406549286175,
0.));
#124110=CARTESIAN_POINT('Ctrl Pts',(49.755350072955,-51.8189928892828,0.));
#124111=CARTESIAN_POINT('Ctrl Pts',(49.7456273031534,-51.7973796306803,
0.));
#124112=CARTESIAN_POINT('Ctrl Pts',(49.7359010133721,-51.7758152395836,
0.));
#124113=CARTESIAN_POINT('Ctrl Pts',(49.7261713119663,-51.754299803067,0.));
#124114=CARTESIAN_POINT('Ctrl Pts',(49.7164383078212,-51.7328334085091,
0.));
#124115=CARTESIAN_POINT('Ctrl Pts',(49.7067021103553,-51.7114161435869,
0.));
#124116=CARTESIAN_POINT('Ctrl Pts',(49.6969628295262,-51.6900480962773,
0.));
#124117=CARTESIAN_POINT('Ctrl Pts',(49.6872205758336,-51.6687293548682,
0.));
#124118=CARTESIAN_POINT('Ctrl Pts',(49.6774754603245,-51.6474600079622,
0.));
#124119=CARTESIAN_POINT('Ctrl Pts',(49.6677275945967,-51.6262401444791,
0.));
#124120=CARTESIAN_POINT('Ctrl Pts',(49.6579770908037,-51.6050698536496,
0.));
#124121=CARTESIAN_POINT('Ctrl Pts',(49.6482240616593,-51.5839492250181,
0.));
#124122=CARTESIAN_POINT('Ctrl Pts',(49.6384686204413,-51.5628783484525,
0.));
#124123=CARTESIAN_POINT('Ctrl Pts',(49.6287108809965,-51.5418573141484,
0.));
#124124=CARTESIAN_POINT('Ctrl Pts',(49.6189509577452,-51.5208862126315,
0.));
#124125=CARTESIAN_POINT('Ctrl Pts',(49.6091889656866,-51.4999651347523,
0.));
#124126=CARTESIAN_POINT('Ctrl Pts',(49.5994250204031,-51.4790941716888,
0.));
#124127=CARTESIAN_POINT('Ctrl Pts',(49.5896592380654,-51.4582734149583,
0.));
#124128=CARTESIAN_POINT('Ctrl Pts',(49.5798917354365,-51.4375029564197,
0.));
#124129=CARTESIAN_POINT('Ctrl Pts',(49.5701226298769,-51.4167828882756,
0.));
#124130=CARTESIAN_POINT('Ctrl Pts',(49.5603520393496,-51.396113303067,0.));
#124131=CARTESIAN_POINT('Ctrl Pts',(49.550580082425,-51.3754942936778,0.));
#124132=CARTESIAN_POINT('Ctrl Pts',(49.5408068782859,-51.3549259533458,
0.));
#124133=CARTESIAN_POINT('Ctrl Pts',(49.5310325467332,-51.3344083756657,
0.));
#124134=CARTESIAN_POINT('Ctrl Pts',(49.5212572081908,-51.313941654591,0.));
#124135=CARTESIAN_POINT('Ctrl Pts',(49.5114809837122,-51.2935258844289,
0.));
#124136=CARTESIAN_POINT('Ctrl Pts',(49.5017039949852,-51.2731611598475,
0.));
#124137=CARTESIAN_POINT('Ctrl Pts',(49.4919263643362,-51.2528475758846,
0.));
#124138=CARTESIAN_POINT('Ctrl Pts',(49.4821482147356,-51.2325852279506,
0.));
#124139=CARTESIAN_POINT('Ctrl Pts',(49.4723696698021,-51.2123742118287,
0.));
#124140=CARTESIAN_POINT('Ctrl Pts',(49.4625908538074,-51.1922146236686,
0.));
#124141=CARTESIAN_POINT('Ctrl Pts',(49.4528118916832,-51.1721065599973,
0.));
#124142=CARTESIAN_POINT('Ctrl Pts',(49.4430329090287,-51.1520501177291,
0.));
#124143=CARTESIAN_POINT('Ctrl Pts',(49.4332540321178,-51.1320453941702,
0.));
#124144=CARTESIAN_POINT('Ctrl Pts',(49.423475387907,-51.1120924870195,0.));
#124145=CARTESIAN_POINT('Ctrl Pts',(49.4136971040428,-51.0921914943662,
0.));
#124146=CARTESIAN_POINT('Ctrl Pts',(49.4039193088634,-51.0723425146985,
0.));
#124147=CARTESIAN_POINT('Ctrl Pts',(49.3941421314012,-51.052545646907,0.));
#124148=CARTESIAN_POINT('Ctrl Pts',(49.3843657013852,-51.0328009902858,
0.));
#124149=CARTESIAN_POINT('Ctrl Pts',(49.3745901492432,-51.0131086445272,
0.));
#124150=CARTESIAN_POINT('Ctrl Pts',(49.3648156061058,-50.9934687097188,
0.));
#124151=CARTESIAN_POINT('Ctrl Pts',(49.355042203823,-50.9738812863646,0.));
#124152=CARTESIAN_POINT('Ctrl Pts',(49.345270074981,-50.9543464753981,0.));
#124153=CARTESIAN_POINT('Ctrl Pts',(49.3354993529158,-50.9348643781924,
0.));
#124154=CARTESIAN_POINT('Ctrl Pts',(49.3257301717335,-50.9154350965666,
0.));
#124155=CARTESIAN_POINT('Ctrl Pts',(49.3159626663109,-50.8960587327848,
0.));
#124156=CARTESIAN_POINT('Ctrl Pts',(49.3061969722781,-50.8767353895492,
0.));
#124157=CARTESIAN_POINT('Ctrl Pts',(49.2964332260039,-50.8574651699873,
0.));
#124158=CARTESIAN_POINT('Ctrl Pts',(49.2866715645838,-50.8382481776403,
0.));
#124159=CARTESIAN_POINT('Ctrl Pts',(49.2769121258164,-50.819084516434,0.));
#124160=CARTESIAN_POINT('Ctrl Pts',(49.2671550482435,-50.7999742907131,
0.));
#124161=CARTESIAN_POINT('Ctrl Pts',(49.2574004712134,-50.7809176052966,
0.));
#124162=CARTESIAN_POINT('Ctrl Pts',(49.2476485349373,-50.7619145655207,
0.));
#124163=CARTESIAN_POINT('Ctrl Pts',(49.2378993805471,-50.7429652772805,
0.));
#124164=CARTESIAN_POINT('Ctrl Pts',(49.228153150155,-50.7240698470679,0.));
#124165=CARTESIAN_POINT('Ctrl Pts',(49.2184099867461,-50.7052283818922,
0.));
#124166=CARTESIAN_POINT('Ctrl Pts',(49.2086700340614,-50.6864409891895,
0.));
#124167=CARTESIAN_POINT('Ctrl Pts',(49.1989334364995,-50.6677077767432,
0.));
#124168=CARTESIAN_POINT('Ctrl Pts',(49.189200338976,-50.6490288525656,0.));
#124169=CARTESIAN_POINT('Ctrl Pts',(49.1794708869099,-50.6304043248821,
0.));
#124170=CARTESIAN_POINT('Ctrl Pts',(49.1697452265494,-50.6118343023958,
0.));
#124171=CARTESIAN_POINT('Ctrl Pts',(49.1600235052621,-50.5933188945168,
0.));
#124172=CARTESIAN_POINT('Ctrl Pts',(49.1503058717821,-50.5748582115565,
0.));
#124173=CARTESIAN_POINT('Ctrl Pts',(49.1405924766144,-50.556452365038,0.));
#124174=CARTESIAN_POINT('Ctrl Pts',(49.1308834717615,-50.5381014674791,
0.));
#124175=CARTESIAN_POINT('Ctrl Pts',(49.1211790099795,-50.5198056318089,
0.));
#124176=CARTESIAN_POINT('Ctrl Pts',(49.1114792441571,-50.501564970874,0.));
#124177=CARTESIAN_POINT('Ctrl Pts',(49.1017843266803,-50.4833795969318,
0.));
#124178=CARTESIAN_POINT('Ctrl Pts',(49.0920944087008,-50.4652496210607,
0.));
#124179=CARTESIAN_POINT('Ctrl Pts',(49.0824096415371,-50.4471751542751,
0.));
#124180=CARTESIAN_POINT('Ctrl Pts',(49.0727301783494,-50.4291563088547,
0.));
#124181=CARTESIAN_POINT('Ctrl Pts',(49.0630561755075,-50.4111931994257,
0.));
#124182=CARTESIAN_POINT('Ctrl Pts',(49.0533877945744,-50.3932859445252,
0.));
#124183=CARTESIAN_POINT('Ctrl Pts',(49.0437252024832,-50.3754346667353,
0.));
#124184=CARTESIAN_POINT('Ctrl Pts',(49.0340685673982,-50.3576394894108,
0.));
#124185=CARTESIAN_POINT('Ctrl Pts',(49.024418055075,-50.3399005337958,0.));
#124186=CARTESIAN_POINT('Ctrl Pts',(49.0147738256942,-50.3222179165119,
0.));
#124187=CARTESIAN_POINT('Ctrl Pts',(49.0051360288044,-50.3045917455424,
0.));
#124188=CARTESIAN_POINT('Ctrl Pts',(48.9955048082081,-50.2870221241054,
0.));
#124189=CARTESIAN_POINT('Ctrl Pts',(48.9858803116689,-50.2695091583511,
0.));
#124190=CARTESIAN_POINT('Ctrl Pts',(48.9762626987227,-50.252052963548,0.));
#124191=CARTESIAN_POINT('Ctrl Pts',(48.9666521500911,-50.234653671541,0.));
#124192=CARTESIAN_POINT('Ctrl Pts',(48.9570488741167,-50.2173114358325,
0.));
#124193=CARTESIAN_POINT('Ctrl Pts',(48.9474530868733,-50.2000264157797,
0.));
#124194=CARTESIAN_POINT('Ctrl Pts',(48.9378649933055,-50.1827987615602,
0.));
#124195=CARTESIAN_POINT('Ctrl Pts',(48.9282847698294,-50.1656286003997,
0.));
#124196=CARTESIAN_POINT('Ctrl Pts',(48.9187125418099,-50.1485160184657,
0.));
#124197=CARTESIAN_POINT('Ctrl Pts',(48.90914838181,-50.1314610602569,0.));
#124198=CARTESIAN_POINT('Ctrl Pts',(48.9015035372055,-50.1178632067084,
0.));
#124199=CARTESIAN_POINT('Ctrl Pts',(48.895773555686,-50.1076907555471,0.));
#124200=CARTESIAN_POINT('Ctrl Pts',(48.8919551910366,-50.1009206494272,
0.));
#124201=CARTESIAN_POINT('Ctrl Pts',(48.8900464144686,-50.0975384783635,
0.));
#124202=CARTESIAN_POINT('Ctrl Pts',(45.8467972562798,-58.722407829904,0.));
#124203=CARTESIAN_POINT('Ctrl Pts',(45.8467972562798,-58.722407829904,12.));
#124204=CARTESIAN_POINT('Ctrl Pts',(45.8455162977427,-58.7169606500268,
0.));
#124205=CARTESIAN_POINT('Ctrl Pts',(45.8455162977427,-58.7169606500268,
12.));
#124206=CARTESIAN_POINT('Ctrl Pts',(45.8429527488786,-58.7060702401686,
0.));
#124207=CARTESIAN_POINT('Ctrl Pts',(45.8429527488786,-58.7060702401686,
12.));
#124208=CARTESIAN_POINT('Ctrl Pts',(45.8391025302132,-58.6897464750699,
0.));
#124209=CARTESIAN_POINT('Ctrl Pts',(45.8391025302132,-58.6897464750699,
12.));
#124210=CARTESIAN_POINT('Ctrl Pts',(45.8339591141834,-58.6680051552762,
0.));
#124211=CARTESIAN_POINT('Ctrl Pts',(45.8339591141834,-58.6680051552762,
12.));
#124212=CARTESIAN_POINT('Ctrl Pts',(45.827513526425,-58.6408680154016,0.));
#124213=CARTESIAN_POINT('Ctrl Pts',(45.827513526425,-58.6408680154016,12.));
#124214=CARTESIAN_POINT('Ctrl Pts',(45.8210516273781,-58.6137704035871,
0.));
#124215=CARTESIAN_POINT('Ctrl Pts',(45.8210516273781,-58.6137704035871,
12.));
#124216=CARTESIAN_POINT('Ctrl Pts',(45.814573433072,-58.5867123491018,0.));
#124217=CARTESIAN_POINT('Ctrl Pts',(45.814573433072,-58.5867123491018,12.));
#124218=CARTESIAN_POINT('Ctrl Pts',(45.8080789725084,-58.5596938940195,
0.));
#124219=CARTESIAN_POINT('Ctrl Pts',(45.8080789725084,-58.5596938940195,
12.));
#124220=CARTESIAN_POINT('Ctrl Pts',(45.8015682926025,-58.5327150960661,
0.));
#124221=CARTESIAN_POINT('Ctrl Pts',(45.8015682926025,-58.5327150960661,
12.));
#124222=CARTESIAN_POINT('Ctrl Pts',(45.7950414569268,-58.5057760270184,
0.));
#124223=CARTESIAN_POINT('Ctrl Pts',(45.7950414569268,-58.5057760270184,
12.));
#124224=CARTESIAN_POINT('Ctrl Pts',(45.7884985397018,-58.4788767676949,
0.));
#124225=CARTESIAN_POINT('Ctrl Pts',(45.7884985397018,-58.4788767676949,
12.));
#124226=CARTESIAN_POINT('Ctrl Pts',(45.7819396211009,-58.4520174038764,
0.));
#124227=CARTESIAN_POINT('Ctrl Pts',(45.7819396211009,-58.4520174038764,
12.));
#124228=CARTESIAN_POINT('Ctrl Pts',(45.7753647821513,-58.425198021955,0.));
#124229=CARTESIAN_POINT('Ctrl Pts',(45.7753647821513,-58.425198021955,12.));
#124230=CARTESIAN_POINT('Ctrl Pts',(45.7687740994957,-58.3984187044245,
0.));
#124231=CARTESIAN_POINT('Ctrl Pts',(45.7687740994957,-58.3984187044245,
12.));
#124232=CARTESIAN_POINT('Ctrl Pts',(45.7621676411434,-58.3716795262353,
0.));
#124233=CARTESIAN_POINT('Ctrl Pts',(45.7621676411434,-58.3716795262353,
12.));
#124234=CARTESIAN_POINT('Ctrl Pts',(45.755545469402,-58.3449805573423,0.));
#124235=CARTESIAN_POINT('Ctrl Pts',(45.755545469402,-58.3449805573423,12.));
#124236=CARTESIAN_POINT('Ctrl Pts',(45.7489076429763,-58.3183218645316,
0.));
#124237=CARTESIAN_POINT('Ctrl Pts',(45.7489076429763,-58.3183218645316,
12.));
#124238=CARTESIAN_POINT('Ctrl Pts',(45.742254219463,-58.291703513584,0.));
#124239=CARTESIAN_POINT('Ctrl Pts',(45.742254219463,-58.291703513584,12.));
#124240=CARTESIAN_POINT('Ctrl Pts',(45.7355852575107,-58.2651255711453,
0.));
#124241=CARTESIAN_POINT('Ctrl Pts',(45.7355852575107,-58.2651255711453,
12.));
#124242=CARTESIAN_POINT('Ctrl Pts',(45.7289008195579,-58.2385881070913,
0.));
#124243=CARTESIAN_POINT('Ctrl Pts',(45.7289008195579,-58.2385881070913,
12.));
#124244=CARTESIAN_POINT('Ctrl Pts',(45.7222009715397,-58.2120911942772,
0.));
#124245=CARTESIAN_POINT('Ctrl Pts',(45.7222009715397,-58.2120911942772,
12.));
#124246=CARTESIAN_POINT('Ctrl Pts',(45.7154857816483,-58.185634907469,0.));
#124247=CARTESIAN_POINT('Ctrl Pts',(45.7154857816483,-58.185634907469,12.));
#124248=CARTESIAN_POINT('Ctrl Pts',(45.7087553193771,-58.1592193225137,
0.));
#124249=CARTESIAN_POINT('Ctrl Pts',(45.7087553193771,-58.1592193225137,
12.));
#124250=CARTESIAN_POINT('Ctrl Pts',(45.702009654518,-58.1328445154676,0.));
#124251=CARTESIAN_POINT('Ctrl Pts',(45.702009654518,-58.1328445154676,12.));
#124252=CARTESIAN_POINT('Ctrl Pts',(45.695248856015,-58.1065105615907,0.));
#124253=CARTESIAN_POINT('Ctrl Pts',(45.695248856015,-58.1065105615907,12.));
#124254=CARTESIAN_POINT('Ctrl Pts',(45.6884729914485,-58.0802175348966,
0.));
#124255=CARTESIAN_POINT('Ctrl Pts',(45.6884729914485,-58.0802175348966,
12.));
#124256=CARTESIAN_POINT('Ctrl Pts',(45.6816821276678,-58.0539655087117,
0.));
#124257=CARTESIAN_POINT('Ctrl Pts',(45.6816821276678,-58.0539655087117,
12.));
#124258=CARTESIAN_POINT('Ctrl Pts',(45.6748763311643,-58.0277545560012,
0.));
#124259=CARTESIAN_POINT('Ctrl Pts',(45.6748763311643,-58.0277545560012,
12.));
#124260=CARTESIAN_POINT('Ctrl Pts',(45.6680556685493,-58.0015847497837,
0.));
#124261=CARTESIAN_POINT('Ctrl Pts',(45.6680556685493,-58.0015847497837,
12.));
#124262=CARTESIAN_POINT('Ctrl Pts',(45.661220206992,-57.9754561635061,0.));
#124263=CARTESIAN_POINT('Ctrl Pts',(45.661220206992,-57.9754561635061,12.));
#124264=CARTESIAN_POINT('Ctrl Pts',(45.6543700146679,-57.9493688714237,
0.));
#124265=CARTESIAN_POINT('Ctrl Pts',(45.6543700146679,-57.9493688714237,
12.));
#124266=CARTESIAN_POINT('Ctrl Pts',(45.6475051605535,-57.9233229484311,
0.));
#124267=CARTESIAN_POINT('Ctrl Pts',(45.6475051605535,-57.9233229484311,
12.));
#124268=CARTESIAN_POINT('Ctrl Pts',(45.6406257142382,-57.8973184699034,
0.));
#124269=CARTESIAN_POINT('Ctrl Pts',(45.6406257142382,-57.8973184699034,
12.));
#124270=CARTESIAN_POINT('Ctrl Pts',(45.6337317457252,-57.8713555115232,
0.));
#124271=CARTESIAN_POINT('Ctrl Pts',(45.6337317457252,-57.8713555115232,
12.));
#124272=CARTESIAN_POINT('Ctrl Pts',(45.6268233252544,-57.8454341491238,
0.));
#124273=CARTESIAN_POINT('Ctrl Pts',(45.6268233252544,-57.8454341491238,
12.));
#124274=CARTESIAN_POINT('Ctrl Pts',(45.6199005230784,-57.8195544584845,
0.));
#124275=CARTESIAN_POINT('Ctrl Pts',(45.6199005230784,-57.8195544584845,
12.));
#124276=CARTESIAN_POINT('Ctrl Pts',(45.6129634094683,-57.7937165153387,
0.));
#124277=CARTESIAN_POINT('Ctrl Pts',(45.6129634094683,-57.7937165153387,
12.));
#124278=CARTESIAN_POINT('Ctrl Pts',(45.6060120548205,-57.7679203954742,
0.));
#124279=CARTESIAN_POINT('Ctrl Pts',(45.6060120548205,-57.7679203954742,
12.));
#124280=CARTESIAN_POINT('Ctrl Pts',(45.5990465297344,-57.7421661748026,
0.));
#124281=CARTESIAN_POINT('Ctrl Pts',(45.5990465297344,-57.7421661748026,
12.));
#124282=CARTESIAN_POINT('Ctrl Pts',(45.5920669050986,-57.7164539294314,
0.));
#124283=CARTESIAN_POINT('Ctrl Pts',(45.5920669050986,-57.7164539294314,
12.));
#124284=CARTESIAN_POINT('Ctrl Pts',(45.5850732521896,-57.6907837357417,
0.));
#124285=CARTESIAN_POINT('Ctrl Pts',(45.5850732521896,-57.6907837357417,
12.));
#124286=CARTESIAN_POINT('Ctrl Pts',(45.5780656427163,-57.6651556704237,
0.));
#124287=CARTESIAN_POINT('Ctrl Pts',(45.5780656427163,-57.6651556704237,
12.));
#124288=CARTESIAN_POINT('Ctrl Pts',(45.5710441487674,-57.6395698104404,
0.));
#124289=CARTESIAN_POINT('Ctrl Pts',(45.5710441487674,-57.6395698104404,
12.));
#124290=CARTESIAN_POINT('Ctrl Pts',(45.5640088427813,-57.614026233004,0.));
#124291=CARTESIAN_POINT('Ctrl Pts',(45.5640088427813,-57.614026233004,12.));
#124292=CARTESIAN_POINT('Ctrl Pts',(45.5569597975096,-57.5885250155433,
0.));
#124293=CARTESIAN_POINT('Ctrl Pts',(45.5569597975096,-57.5885250155433,
12.));
#124294=CARTESIAN_POINT('Ctrl Pts',(45.5498970859835,-57.563066235668,0.));
#124295=CARTESIAN_POINT('Ctrl Pts',(45.5498970859835,-57.563066235668,12.));
#124296=CARTESIAN_POINT('Ctrl Pts',(45.542820781484,-57.537649971135,0.));
#124297=CARTESIAN_POINT('Ctrl Pts',(45.542820781484,-57.537649971135,12.));
#124298=CARTESIAN_POINT('Ctrl Pts',(45.5357309575611,-57.5122762998745,
0.));
#124299=CARTESIAN_POINT('Ctrl Pts',(45.5357309575611,-57.5122762998745,
12.));
#124300=CARTESIAN_POINT('Ctrl Pts',(45.5286276880485,-57.4869453000063,
0.));
#124301=CARTESIAN_POINT('Ctrl Pts',(45.5286276880485,-57.4869453000063,
12.));
#124302=CARTESIAN_POINT('Ctrl Pts',(45.5215110470825,-57.4616570498568,
0.));
#124303=CARTESIAN_POINT('Ctrl Pts',(45.5215110470825,-57.4616570498568,
12.));
#124304=CARTESIAN_POINT('Ctrl Pts',(45.5143811091205,-57.4364116279702,
0.));
#124305=CARTESIAN_POINT('Ctrl Pts',(45.5143811091205,-57.4364116279702,
12.));
#124306=CARTESIAN_POINT('Ctrl Pts',(45.5072379489631,-57.4112091131183,
0.));
#124307=CARTESIAN_POINT('Ctrl Pts',(45.5072379489631,-57.4112091131183,
12.));
#124308=CARTESIAN_POINT('Ctrl Pts',(45.500081641751,-57.3860495843033,0.));
#124309=CARTESIAN_POINT('Ctrl Pts',(45.500081641751,-57.3860495843033,12.));
#124310=CARTESIAN_POINT('Ctrl Pts',(45.4929122629572,-57.3609331207574,
0.));
#124311=CARTESIAN_POINT('Ctrl Pts',(45.4929122629572,-57.3609331207574,
12.));
#124312=CARTESIAN_POINT('Ctrl Pts',(45.4857298883824,-57.3358598019389,
0.));
#124313=CARTESIAN_POINT('Ctrl Pts',(45.4857298883824,-57.3358598019389,
12.));
#124314=CARTESIAN_POINT('Ctrl Pts',(45.4785345941507,-57.3108297075265,
0.));
#124315=CARTESIAN_POINT('Ctrl Pts',(45.4785345941507,-57.3108297075265,
12.));
#124316=CARTESIAN_POINT('Ctrl Pts',(45.4713264567063,-57.2858429174062,
0.));
#124317=CARTESIAN_POINT('Ctrl Pts',(45.4713264567063,-57.2858429174062,
12.));
#124318=CARTESIAN_POINT('Ctrl Pts',(45.4641055528141,-57.2608995116733,
0.));
#124319=CARTESIAN_POINT('Ctrl Pts',(45.4641055528141,-57.2608995116733,
12.));
#124320=CARTESIAN_POINT('Ctrl Pts',(45.4568719595642,-57.2359995706447,
0.));
#124321=CARTESIAN_POINT('Ctrl Pts',(45.4568719595642,-57.2359995706447,
12.));
#124322=CARTESIAN_POINT('Ctrl Pts',(45.4496257543759,-57.2111431748631,
0.));
#124323=CARTESIAN_POINT('Ctrl Pts',(45.4496257543759,-57.2111431748631,
12.));
#124324=CARTESIAN_POINT('Ctrl Pts',(45.4423670150034,-57.186330405101,0.));
#124325=CARTESIAN_POINT('Ctrl Pts',(45.4423670150034,-57.186330405101,12.));
#124326=CARTESIAN_POINT('Ctrl Pts',(45.4350958195434,-57.1615613423584,
0.));
#124327=CARTESIAN_POINT('Ctrl Pts',(45.4350958195434,-57.1615613423584,
12.));
#124328=CARTESIAN_POINT('Ctrl Pts',(45.4278122464389,-57.136836067863,0.));
#124329=CARTESIAN_POINT('Ctrl Pts',(45.4278122464389,-57.136836067863,12.));
#124330=CARTESIAN_POINT('Ctrl Pts',(45.4205163744782,-57.112154663078,0.));
#124331=CARTESIAN_POINT('Ctrl Pts',(45.4205163744782,-57.112154663078,12.));
#124332=CARTESIAN_POINT('Ctrl Pts',(45.4132082827948,-57.0875172097051,
0.));
#124333=CARTESIAN_POINT('Ctrl Pts',(45.4132082827948,-57.0875172097051,
12.));
#124334=CARTESIAN_POINT('Ctrl Pts',(45.4058880508693,-57.0629237896848,
0.));
#124335=CARTESIAN_POINT('Ctrl Pts',(45.4058880508693,-57.0629237896848,
12.));
#124336=CARTESIAN_POINT('Ctrl Pts',(45.3985557585311,-57.0383744851913,
0.));
#124337=CARTESIAN_POINT('Ctrl Pts',(45.3985557585311,-57.0383744851913,
12.));
#124338=CARTESIAN_POINT('Ctrl Pts',(45.3912114859616,-57.0138693786278,
0.));
#124339=CARTESIAN_POINT('Ctrl Pts',(45.3912114859616,-57.0138693786278,
12.));
#124340=CARTESIAN_POINT('Ctrl Pts',(45.3838553136948,-56.9894085526373,
0.));
#124341=CARTESIAN_POINT('Ctrl Pts',(45.3838553136948,-56.9894085526373,
12.));
#124342=CARTESIAN_POINT('Ctrl Pts',(45.3764873226196,-56.9649920901073,
0.));
#124343=CARTESIAN_POINT('Ctrl Pts',(45.3764873226196,-56.9649920901073,
12.));
#124344=CARTESIAN_POINT('Ctrl Pts',(45.3691075939827,-56.9406200741714,
0.));
#124345=CARTESIAN_POINT('Ctrl Pts',(45.3691075939827,-56.9406200741714,
12.));
#124346=CARTESIAN_POINT('Ctrl Pts',(45.3617162093923,-56.9162925882085,
0.));
#124347=CARTESIAN_POINT('Ctrl Pts',(45.3617162093923,-56.9162925882085,
12.));
#124348=CARTESIAN_POINT('Ctrl Pts',(45.3543132508239,-56.8920097158377,
0.));
#124349=CARTESIAN_POINT('Ctrl Pts',(45.3543132508239,-56.8920097158377,
12.));
#124350=CARTESIAN_POINT('Ctrl Pts',(45.3468988006203,-56.8677715409268,
0.));
#124351=CARTESIAN_POINT('Ctrl Pts',(45.3468988006203,-56.8677715409268,
12.));
#124352=CARTESIAN_POINT('Ctrl Pts',(45.3394729414931,-56.8435781475981,
0.));
#124353=CARTESIAN_POINT('Ctrl Pts',(45.3394729414931,-56.8435781475981,
12.));
#124354=CARTESIAN_POINT('Ctrl Pts',(45.332035756524,-56.8194296202291,0.));
#124355=CARTESIAN_POINT('Ctrl Pts',(45.332035756524,-56.8194296202291,12.));
#124356=CARTESIAN_POINT('Ctrl Pts',(45.3245873291684,-56.7953260434524,
0.));
#124357=CARTESIAN_POINT('Ctrl Pts',(45.3245873291684,-56.7953260434524,
12.));
#124358=CARTESIAN_POINT('Ctrl Pts',(45.31712774326,-56.7712675021491,0.));
#124359=CARTESIAN_POINT('Ctrl Pts',(45.31712774326,-56.7712675021491,12.));
#124360=CARTESIAN_POINT('Ctrl Pts',(45.3096570830118,-56.7472540814553,
0.));
#124361=CARTESIAN_POINT('Ctrl Pts',(45.3096570830118,-56.7472540814553,
12.));
#124362=CARTESIAN_POINT('Ctrl Pts',(45.3021754330179,-56.7232858667709,
0.));
#124363=CARTESIAN_POINT('Ctrl Pts',(45.3021754330179,-56.7232858667709,
12.));
#124364=CARTESIAN_POINT('Ctrl Pts',(45.2946828782559,-56.69936294376,0.));
#124365=CARTESIAN_POINT('Ctrl Pts',(45.2946828782559,-56.69936294376,12.));
#124366=CARTESIAN_POINT('Ctrl Pts',(45.2871795040906,-56.6754853983528,
0.));
#124367=CARTESIAN_POINT('Ctrl Pts',(45.2871795040906,-56.6754853983528,
12.));
#124368=CARTESIAN_POINT('Ctrl Pts',(45.2796653962785,-56.6516533167384,
0.));
#124369=CARTESIAN_POINT('Ctrl Pts',(45.2796653962785,-56.6516533167384,
12.));
#124370=CARTESIAN_POINT('Ctrl Pts',(45.2721406409695,-56.6278667853702,
0.));
#124371=CARTESIAN_POINT('Ctrl Pts',(45.2721406409695,-56.6278667853702,
12.));
#124372=CARTESIAN_POINT('Ctrl Pts',(45.2646053247087,-56.6041258909741,
0.));
#124373=CARTESIAN_POINT('Ctrl Pts',(45.2646053247087,-56.6041258909741,
12.));
#124374=CARTESIAN_POINT('Ctrl Pts',(45.257059534438,-56.5804307205505,0.));
#124375=CARTESIAN_POINT('Ctrl Pts',(45.257059534438,-56.5804307205505,12.));
#124376=CARTESIAN_POINT('Ctrl Pts',(45.2495033575,-56.5567813613756,0.));
#124377=CARTESIAN_POINT('Ctrl Pts',(45.2495033575,-56.5567813613756,12.));
#124378=CARTESIAN_POINT('Ctrl Pts',(45.2419368816429,-56.5331779009958,
0.));
#124379=CARTESIAN_POINT('Ctrl Pts',(45.2419368816429,-56.5331779009958,
12.));
#124380=CARTESIAN_POINT('Ctrl Pts',(45.2343601950228,-56.5096204272306,
0.));
#124381=CARTESIAN_POINT('Ctrl Pts',(45.2343601950228,-56.5096204272306,
12.));
#124382=CARTESIAN_POINT('Ctrl Pts',(45.2267733862049,-56.4861090281823,
0.));
#124383=CARTESIAN_POINT('Ctrl Pts',(45.2267733862049,-56.4861090281823,
12.));
#124384=CARTESIAN_POINT('Ctrl Pts',(45.2191765441667,-56.4626437922386,
0.));
#124385=CARTESIAN_POINT('Ctrl Pts',(45.2191765441667,-56.4626437922386,
12.));
#124386=CARTESIAN_POINT('Ctrl Pts',(45.2115697583001,-56.4392248080732,
0.));
#124387=CARTESIAN_POINT('Ctrl Pts',(45.2115697583001,-56.4392248080732,
12.));
#124388=CARTESIAN_POINT('Ctrl Pts',(45.2039531184172,-56.4158521646411,
0.));
#124389=CARTESIAN_POINT('Ctrl Pts',(45.2039531184172,-56.4158521646411,
12.));
#124390=CARTESIAN_POINT('Ctrl Pts',(45.1963267147529,-56.3925259511806,
0.));
#124391=CARTESIAN_POINT('Ctrl Pts',(45.1963267147529,-56.3925259511806,
12.));
#124392=CARTESIAN_POINT('Ctrl Pts',(45.1886906379667,-56.3692462572231,
0.));
#124393=CARTESIAN_POINT('Ctrl Pts',(45.1886906379667,-56.3692462572231,
12.));
#124394=CARTESIAN_POINT('Ctrl Pts',(45.1810449791453,-56.3460131725964,
0.));
#124395=CARTESIAN_POINT('Ctrl Pts',(45.1810449791453,-56.3460131725964,
12.));
#124396=CARTESIAN_POINT('Ctrl Pts',(45.1733898298061,-56.3228267874264,
0.));
#124397=CARTESIAN_POINT('Ctrl Pts',(45.1733898298061,-56.3228267874264,
12.));
#124398=CARTESIAN_POINT('Ctrl Pts',(45.1657252819013,-56.2996871921316,
0.));
#124399=CARTESIAN_POINT('Ctrl Pts',(45.1657252819013,-56.2996871921316,
12.));
#124400=CARTESIAN_POINT('Ctrl Pts',(45.1580514278223,-56.2765944774245,
0.));
#124401=CARTESIAN_POINT('Ctrl Pts',(45.1580514278223,-56.2765944774245,
12.));
#124402=CARTESIAN_POINT('Ctrl Pts',(45.1503683604005,-56.2535487343221,
0.));
#124403=CARTESIAN_POINT('Ctrl Pts',(45.1503683604005,-56.2535487343221,
12.));
#124404=CARTESIAN_POINT('Ctrl Pts',(45.1426761729105,-56.2305500541489,
0.));
#124405=CARTESIAN_POINT('Ctrl Pts',(45.1426761729105,-56.2305500541489,
12.));
#124406=CARTESIAN_POINT('Ctrl Pts',(45.1349749590738,-56.2075985285393,
0.));
#124407=CARTESIAN_POINT('Ctrl Pts',(45.1349749590738,-56.2075985285393,
12.));
#124408=CARTESIAN_POINT('Ctrl Pts',(45.127264813063,-56.1846942494325,0.));
#124409=CARTESIAN_POINT('Ctrl Pts',(45.127264813063,-56.1846942494325,12.));
#124410=CARTESIAN_POINT('Ctrl Pts',(45.1195458295063,-56.1618373090732,
0.));
#124411=CARTESIAN_POINT('Ctrl Pts',(45.1195458295063,-56.1618373090732,
12.));
#124412=CARTESIAN_POINT('Ctrl Pts',(45.1118181034888,-56.1390278000226,
0.));
#124413=CARTESIAN_POINT('Ctrl Pts',(45.1118181034888,-56.1390278000226,
12.));
#124414=CARTESIAN_POINT('Ctrl Pts',(45.1040817305561,-56.116265815162,0.));
#124415=CARTESIAN_POINT('Ctrl Pts',(45.1040817305561,-56.116265815162,12.));
#124416=CARTESIAN_POINT('Ctrl Pts',(45.0963368067177,-56.0935514476945,
0.));
#124417=CARTESIAN_POINT('Ctrl Pts',(45.0963368067177,-56.0935514476945,
12.));
#124418=CARTESIAN_POINT('Ctrl Pts',(45.0885834284517,-56.0708847911416,
0.));
#124419=CARTESIAN_POINT('Ctrl Pts',(45.0885834284517,-56.0708847911416,
12.));
#124420=CARTESIAN_POINT('Ctrl Pts',(45.0808216927089,-56.048265939342,0.));
#124421=CARTESIAN_POINT('Ctrl Pts',(45.0808216927089,-56.048265939342,12.));
#124422=CARTESIAN_POINT('Ctrl Pts',(45.0730516969149,-56.0256949864639,
0.));
#124423=CARTESIAN_POINT('Ctrl Pts',(45.0730516969149,-56.0256949864639,
12.));
#124424=CARTESIAN_POINT('Ctrl Pts',(45.0652735389733,-56.003172027008,0.));
#124425=CARTESIAN_POINT('Ctrl Pts',(45.0652735389733,-56.003172027008,12.));
#124426=CARTESIAN_POINT('Ctrl Pts',(45.0574873172695,-55.9806971558097,
0.));
#124427=CARTESIAN_POINT('Ctrl Pts',(45.0574873172695,-55.9806971558097,
12.));
#124428=CARTESIAN_POINT('Ctrl Pts',(45.0496931306755,-55.9582704680356,
0.));
#124429=CARTESIAN_POINT('Ctrl Pts',(45.0496931306755,-55.9582704680356,
12.));
#124430=CARTESIAN_POINT('Ctrl Pts',(45.0418910785551,-55.9358920591837,
0.));
#124431=CARTESIAN_POINT('Ctrl Pts',(45.0418910785551,-55.9358920591837,
12.));
#124432=CARTESIAN_POINT('Ctrl Pts',(45.0340812607657,-55.9135620250954,
0.));
#124433=CARTESIAN_POINT('Ctrl Pts',(45.0340812607657,-55.9135620250954,
12.));
#124434=CARTESIAN_POINT('Ctrl Pts',(45.0262637776615,-55.8912804619577,
0.));
#124435=CARTESIAN_POINT('Ctrl Pts',(45.0262637776615,-55.8912804619577,
12.));
#124436=CARTESIAN_POINT('Ctrl Pts',(45.0184387300973,-55.8690474663065,
0.));
#124437=CARTESIAN_POINT('Ctrl Pts',(45.0184387300973,-55.8690474663065,
12.));
#124438=CARTESIAN_POINT('Ctrl Pts',(45.0106062194342,-55.8468631350218,
0.));
#124439=CARTESIAN_POINT('Ctrl Pts',(45.0106062194342,-55.8468631350218,
12.));
#124440=CARTESIAN_POINT('Ctrl Pts',(45.0027663475433,-55.8247275653289,
0.));
#124441=CARTESIAN_POINT('Ctrl Pts',(45.0027663475433,-55.8247275653289,
12.));
#124442=CARTESIAN_POINT('Ctrl Pts',(44.9949192168093,-55.8026408548105,
0.));
#124443=CARTESIAN_POINT('Ctrl Pts',(44.9949192168093,-55.8026408548105,
12.));
#124444=CARTESIAN_POINT('Ctrl Pts',(44.9870649301342,-55.7806031014106,
0.));
#124445=CARTESIAN_POINT('Ctrl Pts',(44.9870649301342,-55.7806031014106,
12.));
#124446=CARTESIAN_POINT('Ctrl Pts',(44.9792035909413,-55.7586144034367,
0.));
#124447=CARTESIAN_POINT('Ctrl Pts',(44.9792035909413,-55.7586144034367,
12.));
#124448=CARTESIAN_POINT('Ctrl Pts',(44.9713353031804,-55.7366748595551,
0.));
#124449=CARTESIAN_POINT('Ctrl Pts',(44.9713353031804,-55.7366748595551,
12.));
#124450=CARTESIAN_POINT('Ctrl Pts',(44.9634601713321,-55.714784568793,0.));
#124451=CARTESIAN_POINT('Ctrl Pts',(44.9634601713321,-55.714784568793,12.));
#124452=CARTESIAN_POINT('Ctrl Pts',(44.9555783004106,-55.6929436305489,
0.));
#124453=CARTESIAN_POINT('Ctrl Pts',(44.9555783004106,-55.6929436305489,
12.));
#124454=CARTESIAN_POINT('Ctrl Pts',(44.9476897959685,-55.6711521445979,
0.));
#124455=CARTESIAN_POINT('Ctrl Pts',(44.9476897959685,-55.6711521445979,
12.));
#124456=CARTESIAN_POINT('Ctrl Pts',(44.9397947641007,-55.6494102110935,
0.));
#124457=CARTESIAN_POINT('Ctrl Pts',(44.9397947641007,-55.6494102110935,
12.));
#124458=CARTESIAN_POINT('Ctrl Pts',(44.9318933114507,-55.6277179305633,
0.));
#124459=CARTESIAN_POINT('Ctrl Pts',(44.9318933114507,-55.6277179305633,
12.));
#124460=CARTESIAN_POINT('Ctrl Pts',(44.9239855452144,-55.6060754039121,
0.));
#124461=CARTESIAN_POINT('Ctrl Pts',(44.9239855452144,-55.6060754039121,
12.));
#124462=CARTESIAN_POINT('Ctrl Pts',(44.9160715731443,-55.5844827324338,
0.));
#124463=CARTESIAN_POINT('Ctrl Pts',(44.9160715731443,-55.5844827324338,
12.));
#124464=CARTESIAN_POINT('Ctrl Pts',(44.908151503553,-55.5629400178142,0.));
#124465=CARTESIAN_POINT('Ctrl Pts',(44.908151503553,-55.5629400178142,12.));
#124466=CARTESIAN_POINT('Ctrl Pts',(44.9002254453183,-55.541447362134,0.));
#124467=CARTESIAN_POINT('Ctrl Pts',(44.9002254453183,-55.541447362134,12.));
#124468=CARTESIAN_POINT('Ctrl Pts',(44.8922935078889,-55.5200048678629,
0.));
#124469=CARTESIAN_POINT('Ctrl Pts',(44.8922935078889,-55.5200048678629,
12.));
#124470=CARTESIAN_POINT('Ctrl Pts',(44.8843558012886,-55.4986126378656,
0.));
#124471=CARTESIAN_POINT('Ctrl Pts',(44.8843558012886,-55.4986126378656,
12.));
#124472=CARTESIAN_POINT('Ctrl Pts',(44.8764124361207,-55.4772707754126,
0.));
#124473=CARTESIAN_POINT('Ctrl Pts',(44.8764124361207,-55.4772707754126,
12.));
#124474=CARTESIAN_POINT('Ctrl Pts',(44.8684635235725,-55.4559793841836,
0.));
#124475=CARTESIAN_POINT('Ctrl Pts',(44.8684635235725,-55.4559793841836,
12.));
#124476=CARTESIAN_POINT('Ctrl Pts',(44.8605091754214,-55.4347385682704,
0.));
#124477=CARTESIAN_POINT('Ctrl Pts',(44.8605091754214,-55.4347385682704,
12.));
#124478=CARTESIAN_POINT('Ctrl Pts',(44.8525495040408,-55.4135484321718,
0.));
#124479=CARTESIAN_POINT('Ctrl Pts',(44.8525495040408,-55.4135484321718,
12.));
#124480=CARTESIAN_POINT('Ctrl Pts',(44.8445846224044,-55.3924090808014,
0.));
#124481=CARTESIAN_POINT('Ctrl Pts',(44.8445846224044,-55.3924090808014,
12.));
#124482=CARTESIAN_POINT('Ctrl Pts',(44.8366146440901,-55.3713206194967,
0.));
#124483=CARTESIAN_POINT('Ctrl Pts',(44.8366146440901,-55.3713206194967,
12.));
#124484=CARTESIAN_POINT('Ctrl Pts',(44.8286396832848,-55.3502831540228,
0.));
#124485=CARTESIAN_POINT('Ctrl Pts',(44.8286396832848,-55.3502831540228,
12.));
#124486=CARTESIAN_POINT('Ctrl Pts',(44.8206598547888,-55.3292967905725,
0.));
#124487=CARTESIAN_POINT('Ctrl Pts',(44.8206598547888,-55.3292967905725,
12.));
#124488=CARTESIAN_POINT('Ctrl Pts',(44.8126752740208,-55.3083616357605,
0.));
#124489=CARTESIAN_POINT('Ctrl Pts',(44.8126752740208,-55.3083616357605,
12.));
#124490=CARTESIAN_POINT('Ctrl Pts',(44.8046860570244,-55.287477796635,0.));
#124491=CARTESIAN_POINT('Ctrl Pts',(44.8046860570244,-55.287477796635,12.));
#124492=CARTESIAN_POINT('Ctrl Pts',(44.796692320474,-55.2666453806883,0.));
#124493=CARTESIAN_POINT('Ctrl Pts',(44.796692320474,-55.2666453806883,12.));
#124494=CARTESIAN_POINT('Ctrl Pts',(44.7886941816823,-55.2458644958617,
0.));
#124495=CARTESIAN_POINT('Ctrl Pts',(44.7886941816823,-55.2458644958617,
12.));
#124496=CARTESIAN_POINT('Ctrl Pts',(44.7806917586077,-55.2251352505474,
0.));
#124497=CARTESIAN_POINT('Ctrl Pts',(44.7806917586077,-55.2251352505474,
12.));
#124498=CARTESIAN_POINT('Ctrl Pts',(44.7726851698618,-55.2044577535865,
0.));
#124499=CARTESIAN_POINT('Ctrl Pts',(44.7726851698618,-55.2044577535865,
12.));
#124500=CARTESIAN_POINT('Ctrl Pts',(44.7646745347108,-55.1838321142777,
0.));
#124501=CARTESIAN_POINT('Ctrl Pts',(44.7646745347108,-55.1838321142777,
12.));
#124502=CARTESIAN_POINT('Ctrl Pts',(44.7566599730771,-55.1632584423813,
0.));
#124503=CARTESIAN_POINT('Ctrl Pts',(44.7566599730771,-55.1632584423813,
12.));
#124504=CARTESIAN_POINT('Ctrl Pts',(44.748641605542,-55.1427368481201,0.));
#124505=CARTESIAN_POINT('Ctrl Pts',(44.748641605542,-55.1427368481201,12.));
#124506=CARTESIAN_POINT('Ctrl Pts',(44.7406195533483,-55.1222674421747,
0.));
#124507=CARTESIAN_POINT('Ctrl Pts',(44.7406195533483,-55.1222674421747,
12.));
#124508=CARTESIAN_POINT('Ctrl Pts',(44.7325939384042,-55.1018503356806,
0.));
#124509=CARTESIAN_POINT('Ctrl Pts',(44.7325939384042,-55.1018503356806,
12.));
#124510=CARTESIAN_POINT('Ctrl Pts',(44.7245648832988,-55.0814856402507,
0.));
#124511=CARTESIAN_POINT('Ctrl Pts',(44.7245648832988,-55.0814856402507,
12.));
#124512=CARTESIAN_POINT('Ctrl Pts',(44.7165325113165,-55.0611734679902,
0.));
#124513=CARTESIAN_POINT('Ctrl Pts',(44.7165325113165,-55.0611734679902,
12.));
#124514=CARTESIAN_POINT('Ctrl Pts',(44.7084969464509,-55.0409139315074,
0.));
#124515=CARTESIAN_POINT('Ctrl Pts',(44.7084969464509,-55.0409139315074,
12.));
#124516=CARTESIAN_POINT('Ctrl Pts',(44.7004583134235,-55.020707143922,0.));
#124517=CARTESIAN_POINT('Ctrl Pts',(44.7004583134235,-55.020707143922,12.));
#124518=CARTESIAN_POINT('Ctrl Pts',(44.6924167376851,-55.0005532188644,
0.));
#124519=CARTESIAN_POINT('Ctrl Pts',(44.6924167376851,-55.0005532188644,
12.));
#124520=CARTESIAN_POINT('Ctrl Pts',(44.6843723453985,-54.9804522704668,
0.));
#124521=CARTESIAN_POINT('Ctrl Pts',(44.6843723453985,-54.9804522704668,
12.));
#124522=CARTESIAN_POINT('Ctrl Pts',(44.6763252634255,-54.9604044133497,
0.));
#124523=CARTESIAN_POINT('Ctrl Pts',(44.6763252634255,-54.9604044133497,
12.));
#124524=CARTESIAN_POINT('Ctrl Pts',(44.6682756193156,-54.9404097626088,
0.));
#124525=CARTESIAN_POINT('Ctrl Pts',(44.6682756193156,-54.9404097626088,
12.));
#124526=CARTESIAN_POINT('Ctrl Pts',(44.6602235412854,-54.9204684337845,
0.));
#124527=CARTESIAN_POINT('Ctrl Pts',(44.6602235412854,-54.9204684337845,
12.));
#124528=CARTESIAN_POINT('Ctrl Pts',(44.6521691582551,-54.9005805428991,
0.));
#124529=CARTESIAN_POINT('Ctrl Pts',(44.6521691582551,-54.9005805428991,
12.));
#124530=CARTESIAN_POINT('Ctrl Pts',(44.6441125999074,-54.8807462065177,
0.));
#124531=CARTESIAN_POINT('Ctrl Pts',(44.6441125999074,-54.8807462065177,
12.));
#124532=CARTESIAN_POINT('Ctrl Pts',(44.6360539967392,-54.860965541796,0.));
#124533=CARTESIAN_POINT('Ctrl Pts',(44.6360539967392,-54.860965541796,12.));
#124534=CARTESIAN_POINT('Ctrl Pts',(44.6279934801159,-54.8412386665264,
0.));
#124535=CARTESIAN_POINT('Ctrl Pts',(44.6279934801159,-54.8412386665264,
12.));
#124536=CARTESIAN_POINT('Ctrl Pts',(44.6199311823276,-54.8215656991817,
0.));
#124537=CARTESIAN_POINT('Ctrl Pts',(44.6199311823276,-54.8215656991817,
12.));
#124538=CARTESIAN_POINT('Ctrl Pts',(44.6118672364889,-54.8019467588257,
0.));
#124539=CARTESIAN_POINT('Ctrl Pts',(44.6118672364889,-54.8019467588257,
12.));
#124540=CARTESIAN_POINT('Ctrl Pts',(44.60380177643,-54.7823819650137,0.));
#124541=CARTESIAN_POINT('Ctrl Pts',(44.60380177643,-54.7823819650137,12.));
#124542=CARTESIAN_POINT('Ctrl Pts',(44.5957349366062,-54.7628714377041,
0.));
#124543=CARTESIAN_POINT('Ctrl Pts',(44.5957349366062,-54.7628714377041,
12.));
#124544=CARTESIAN_POINT('Ctrl Pts',(44.5876668519676,-54.7434152971285,
0.));
#124545=CARTESIAN_POINT('Ctrl Pts',(44.5876668519676,-54.7434152971285,
12.));
#124546=CARTESIAN_POINT('Ctrl Pts',(44.5795976579476,-54.7240136637744,
0.));
#124547=CARTESIAN_POINT('Ctrl Pts',(44.5795976579476,-54.7240136637744,
12.));
#124548=CARTESIAN_POINT('Ctrl Pts',(44.5715274907637,-54.7046666586776,
0.));
#124549=CARTESIAN_POINT('Ctrl Pts',(44.5715274907637,-54.7046666586776,
12.));
#124550=CARTESIAN_POINT('Ctrl Pts',(44.563456487687,-54.685374403676,0.));
#124551=CARTESIAN_POINT('Ctrl Pts',(44.563456487687,-54.685374403676,12.));
#124552=CARTESIAN_POINT('Ctrl Pts',(44.5553847872712,-54.6661370216242,
0.));
#124553=CARTESIAN_POINT('Ctrl Pts',(44.5553847872712,-54.6661370216242,
12.));
#124554=CARTESIAN_POINT('Ctrl Pts',(44.5473125297289,-54.6469546367381,
0.));
#124555=CARTESIAN_POINT('Ctrl Pts',(44.5473125297289,-54.6469546367381,
12.));
#124556=CARTESIAN_POINT('Ctrl Pts',(44.5392398566775,-54.6278273743554,
0.));
#124557=CARTESIAN_POINT('Ctrl Pts',(44.5392398566775,-54.6278273743554,
12.));
#124558=CARTESIAN_POINT('Ctrl Pts',(44.5311669104495,-54.6087553602889,
0.));
#124559=CARTESIAN_POINT('Ctrl Pts',(44.5311669104495,-54.6087553602889,
12.));
#124560=CARTESIAN_POINT('Ctrl Pts',(44.5230938335165,-54.5897387202812,
0.));
#124561=CARTESIAN_POINT('Ctrl Pts',(44.5230938335165,-54.5897387202812,
12.));
#124562=CARTESIAN_POINT('Ctrl Pts',(44.5150207679007,-54.5707775794436,
0.));
#124563=CARTESIAN_POINT('Ctrl Pts',(44.5150207679007,-54.5707775794436,
12.));
#124564=CARTESIAN_POINT('Ctrl Pts',(44.5069478544977,-54.5518720616056,
0.));
#124565=CARTESIAN_POINT('Ctrl Pts',(44.5069478544977,-54.5518720616056,
12.));
#124566=CARTESIAN_POINT('Ctrl Pts',(44.4988752343744,-54.5330222905475,
0.));
#124567=CARTESIAN_POINT('Ctrl Pts',(44.4988752343744,-54.5330222905475,
12.));
#124568=CARTESIAN_POINT('Ctrl Pts',(44.4908030503225,-54.5142283914704,
0.));
#124569=CARTESIAN_POINT('Ctrl Pts',(44.4908030503225,-54.5142283914704,
12.));
#124570=CARTESIAN_POINT('Ctrl Pts',(44.4827314481264,-54.495490492193,0.));
#124571=CARTESIAN_POINT('Ctrl Pts',(44.4827314481264,-54.495490492193,12.));
#124572=CARTESIAN_POINT('Ctrl Pts',(44.4746605784031,-54.4768087248824,
0.));
#124573=CARTESIAN_POINT('Ctrl Pts',(44.4746605784031,-54.4768087248824,
12.));
#124574=CARTESIAN_POINT('Ctrl Pts',(44.4665905967668,-54.4581832262033,
0.));
#124575=CARTESIAN_POINT('Ctrl Pts',(44.4665905967668,-54.4581832262033,
12.));
#124576=CARTESIAN_POINT('Ctrl Pts',(44.4585216599908,-54.4396141336978,
0.));
#124577=CARTESIAN_POINT('Ctrl Pts',(44.4585216599908,-54.4396141336978,
12.));
#124578=CARTESIAN_POINT('Ctrl Pts',(44.4504539226328,-54.421101582595,0.));
#124579=CARTESIAN_POINT('Ctrl Pts',(44.4504539226328,-54.421101582595,12.));
#124580=CARTESIAN_POINT('Ctrl Pts',(44.4423875340996,-54.4026457030335,
0.));
#124581=CARTESIAN_POINT('Ctrl Pts',(44.4423875340996,-54.4026457030335,
12.));
#124582=CARTESIAN_POINT('Ctrl Pts',(44.4343226339593,-54.3842466156196,
0.));
#124583=CARTESIAN_POINT('Ctrl Pts',(44.4343226339593,-54.3842466156196,
12.));
#124584=CARTESIAN_POINT('Ctrl Pts',(44.4262593564712,-54.3659044357119,
0.));
#124585=CARTESIAN_POINT('Ctrl Pts',(44.4262593564712,-54.3659044357119,
12.));
#124586=CARTESIAN_POINT('Ctrl Pts',(44.4181978395851,-54.3476192819352,
0.));
#124587=CARTESIAN_POINT('Ctrl Pts',(44.4181978395851,-54.3476192819352,
12.));
#124588=CARTESIAN_POINT('Ctrl Pts',(44.4101382321834,-54.3293912830237,
0.));
#124589=CARTESIAN_POINT('Ctrl Pts',(44.4101382321834,-54.3293912830237,
12.));
#124590=CARTESIAN_POINT('Ctrl Pts',(44.402080702809,-54.3112205860716,0.));
#124591=CARTESIAN_POINT('Ctrl Pts',(44.402080702809,-54.3112205860716,12.));
#124592=CARTESIAN_POINT('Ctrl Pts',(44.3940254456331,-54.2931073621553,
0.));
#124593=CARTESIAN_POINT('Ctrl Pts',(44.3940254456331,-54.2931073621553,
12.));
#124594=CARTESIAN_POINT('Ctrl Pts',(44.3859726620183,-54.2750517888579,
0.));
#124595=CARTESIAN_POINT('Ctrl Pts',(44.3859726620183,-54.2750517888579,
12.));
#124596=CARTESIAN_POINT('Ctrl Pts',(44.3779225430406,-54.2570540336475,
0.));
#124597=CARTESIAN_POINT('Ctrl Pts',(44.3779225430406,-54.2570540336475,
12.));
#124598=CARTESIAN_POINT('Ctrl Pts',(44.3698752533562,-54.2391142386412,
0.));
#124599=CARTESIAN_POINT('Ctrl Pts',(44.3698752533562,-54.2391142386412,
12.));
#124600=CARTESIAN_POINT('Ctrl Pts',(44.361830910343,-54.2212325006052,0.));
#124601=CARTESIAN_POINT('Ctrl Pts',(44.361830910343,-54.2212325006052,12.));
#124602=CARTESIAN_POINT('Ctrl Pts',(44.3537895824096,-54.2034088701928,
0.));
#124603=CARTESIAN_POINT('Ctrl Pts',(44.3537895824096,-54.2034088701928,
12.));
#124604=CARTESIAN_POINT('Ctrl Pts',(44.3473589597726,-54.1891964684727,
0.));
#124605=CARTESIAN_POINT('Ctrl Pts',(44.3473589597726,-54.1891964684727,
12.));
#124606=CARTESIAN_POINT('Ctrl Pts',(44.3425373700993,-54.1785633257639,
0.));
#124607=CARTESIAN_POINT('Ctrl Pts',(44.3425373700993,-54.1785633257639,
12.));
#124608=CARTESIAN_POINT('Ctrl Pts',(44.3393235891075,-54.1714861895346,
0.));
#124609=CARTESIAN_POINT('Ctrl Pts',(44.3393235891075,-54.1714861895346,
12.));
#124610=CARTESIAN_POINT('Ctrl Pts',(44.3377168516418,-54.1679505278134,
0.));
#124611=CARTESIAN_POINT('Ctrl Pts',(44.3377168516418,-54.1679505278134,
12.));
#124612=CARTESIAN_POINT('',(44.3377168516418,-54.1679505278134,12.));
#124613=CARTESIAN_POINT('Ctrl Pts',(44.3377168516418,-54.1679505278134,
12.));
#124614=CARTESIAN_POINT('Ctrl Pts',(44.3393235891075,-54.1714861895346,
12.));
#124615=CARTESIAN_POINT('Ctrl Pts',(44.3425373700993,-54.1785633257639,
12.));
#124616=CARTESIAN_POINT('Ctrl Pts',(44.3473589597726,-54.1891964684727,
12.));
#124617=CARTESIAN_POINT('Ctrl Pts',(44.3537895824096,-54.2034088701928,
12.));
#124618=CARTESIAN_POINT('Ctrl Pts',(44.361830910343,-54.2212325006052,12.));
#124619=CARTESIAN_POINT('Ctrl Pts',(44.3698752533562,-54.2391142386412,
12.));
#124620=CARTESIAN_POINT('Ctrl Pts',(44.3779225430406,-54.2570540336475,
12.));
#124621=CARTESIAN_POINT('Ctrl Pts',(44.3859726620183,-54.2750517888579,
12.));
#124622=CARTESIAN_POINT('Ctrl Pts',(44.3940254456331,-54.2931073621553,
12.));
#124623=CARTESIAN_POINT('Ctrl Pts',(44.402080702809,-54.3112205860716,12.));
#124624=CARTESIAN_POINT('Ctrl Pts',(44.4101382321834,-54.3293912830237,
12.));
#124625=CARTESIAN_POINT('Ctrl Pts',(44.4181978395851,-54.3476192819352,
12.));
#124626=CARTESIAN_POINT('Ctrl Pts',(44.4262593564712,-54.3659044357119,
12.));
#124627=CARTESIAN_POINT('Ctrl Pts',(44.4343226339593,-54.3842466156196,
12.));
#124628=CARTESIAN_POINT('Ctrl Pts',(44.4423875340996,-54.4026457030335,
12.));
#124629=CARTESIAN_POINT('Ctrl Pts',(44.4504539226328,-54.421101582595,12.));
#124630=CARTESIAN_POINT('Ctrl Pts',(44.4585216599908,-54.4396141336978,
12.));
#124631=CARTESIAN_POINT('Ctrl Pts',(44.4665905967668,-54.4581832262033,
12.));
#124632=CARTESIAN_POINT('Ctrl Pts',(44.4746605784031,-54.4768087248824,
12.));
#124633=CARTESIAN_POINT('Ctrl Pts',(44.4827314481264,-54.495490492193,12.));
#124634=CARTESIAN_POINT('Ctrl Pts',(44.4908030503225,-54.5142283914704,
12.));
#124635=CARTESIAN_POINT('Ctrl Pts',(44.4988752343744,-54.5330222905475,
12.));
#124636=CARTESIAN_POINT('Ctrl Pts',(44.5069478544977,-54.5518720616056,
12.));
#124637=CARTESIAN_POINT('Ctrl Pts',(44.5150207679007,-54.5707775794436,
12.));
#124638=CARTESIAN_POINT('Ctrl Pts',(44.5230938335165,-54.5897387202812,
12.));
#124639=CARTESIAN_POINT('Ctrl Pts',(44.5311669104495,-54.6087553602889,
12.));
#124640=CARTESIAN_POINT('Ctrl Pts',(44.5392398566775,-54.6278273743554,
12.));
#124641=CARTESIAN_POINT('Ctrl Pts',(44.5473125297289,-54.6469546367381,
12.));
#124642=CARTESIAN_POINT('Ctrl Pts',(44.5553847872712,-54.6661370216242,
12.));
#124643=CARTESIAN_POINT('Ctrl Pts',(44.563456487687,-54.685374403676,12.));
#124644=CARTESIAN_POINT('Ctrl Pts',(44.5715274907637,-54.7046666586776,
12.));
#124645=CARTESIAN_POINT('Ctrl Pts',(44.5795976579476,-54.7240136637744,
12.));
#124646=CARTESIAN_POINT('Ctrl Pts',(44.5876668519676,-54.7434152971285,
12.));
#124647=CARTESIAN_POINT('Ctrl Pts',(44.5957349366062,-54.7628714377041,
12.));
#124648=CARTESIAN_POINT('Ctrl Pts',(44.60380177643,-54.7823819650137,12.));
#124649=CARTESIAN_POINT('Ctrl Pts',(44.6118672364889,-54.8019467588257,
12.));
#124650=CARTESIAN_POINT('Ctrl Pts',(44.6199311823276,-54.8215656991817,
12.));
#124651=CARTESIAN_POINT('Ctrl Pts',(44.6279934801159,-54.8412386665264,
12.));
#124652=CARTESIAN_POINT('Ctrl Pts',(44.6360539967392,-54.860965541796,12.));
#124653=CARTESIAN_POINT('Ctrl Pts',(44.6441125999074,-54.8807462065177,
12.));
#124654=CARTESIAN_POINT('Ctrl Pts',(44.6521691582551,-54.9005805428991,
12.));
#124655=CARTESIAN_POINT('Ctrl Pts',(44.6602235412854,-54.9204684337845,
12.));
#124656=CARTESIAN_POINT('Ctrl Pts',(44.6682756193156,-54.9404097626088,
12.));
#124657=CARTESIAN_POINT('Ctrl Pts',(44.6763252634255,-54.9604044133497,
12.));
#124658=CARTESIAN_POINT('Ctrl Pts',(44.6843723453985,-54.9804522704668,
12.));
#124659=CARTESIAN_POINT('Ctrl Pts',(44.6924167376851,-55.0005532188644,
12.));
#124660=CARTESIAN_POINT('Ctrl Pts',(44.7004583134235,-55.020707143922,12.));
#124661=CARTESIAN_POINT('Ctrl Pts',(44.7084969464509,-55.0409139315074,
12.));
#124662=CARTESIAN_POINT('Ctrl Pts',(44.7165325113165,-55.0611734679902,
12.));
#124663=CARTESIAN_POINT('Ctrl Pts',(44.7245648832988,-55.0814856402507,
12.));
#124664=CARTESIAN_POINT('Ctrl Pts',(44.7325939384042,-55.1018503356806,
12.));
#124665=CARTESIAN_POINT('Ctrl Pts',(44.7406195533483,-55.1222674421747,
12.));
#124666=CARTESIAN_POINT('Ctrl Pts',(44.748641605542,-55.1427368481201,12.));
#124667=CARTESIAN_POINT('Ctrl Pts',(44.7566599730771,-55.1632584423813,
12.));
#124668=CARTESIAN_POINT('Ctrl Pts',(44.7646745347108,-55.1838321142777,
12.));
#124669=CARTESIAN_POINT('Ctrl Pts',(44.7726851698618,-55.2044577535865,
12.));
#124670=CARTESIAN_POINT('Ctrl Pts',(44.7806917586077,-55.2251352505474,
12.));
#124671=CARTESIAN_POINT('Ctrl Pts',(44.7886941816823,-55.2458644958617,
12.));
#124672=CARTESIAN_POINT('Ctrl Pts',(44.796692320474,-55.2666453806883,12.));
#124673=CARTESIAN_POINT('Ctrl Pts',(44.8046860570244,-55.287477796635,12.));
#124674=CARTESIAN_POINT('Ctrl Pts',(44.8126752740208,-55.3083616357605,
12.));
#124675=CARTESIAN_POINT('Ctrl Pts',(44.8206598547888,-55.3292967905725,
12.));
#124676=CARTESIAN_POINT('Ctrl Pts',(44.8286396832848,-55.3502831540228,
12.));
#124677=CARTESIAN_POINT('Ctrl Pts',(44.8366146440901,-55.3713206194967,
12.));
#124678=CARTESIAN_POINT('Ctrl Pts',(44.8445846224044,-55.3924090808014,
12.));
#124679=CARTESIAN_POINT('Ctrl Pts',(44.8525495040408,-55.4135484321718,
12.));
#124680=CARTESIAN_POINT('Ctrl Pts',(44.8605091754214,-55.4347385682704,
12.));
#124681=CARTESIAN_POINT('Ctrl Pts',(44.8684635235725,-55.4559793841836,
12.));
#124682=CARTESIAN_POINT('Ctrl Pts',(44.8764124361207,-55.4772707754126,
12.));
#124683=CARTESIAN_POINT('Ctrl Pts',(44.8843558012886,-55.4986126378656,
12.));
#124684=CARTESIAN_POINT('Ctrl Pts',(44.8922935078889,-55.5200048678629,
12.));
#124685=CARTESIAN_POINT('Ctrl Pts',(44.9002254453183,-55.541447362134,12.));
#124686=CARTESIAN_POINT('Ctrl Pts',(44.908151503553,-55.5629400178142,12.));
#124687=CARTESIAN_POINT('Ctrl Pts',(44.9160715731443,-55.5844827324338,
12.));
#124688=CARTESIAN_POINT('Ctrl Pts',(44.9239855452144,-55.6060754039121,
12.));
#124689=CARTESIAN_POINT('Ctrl Pts',(44.9318933114507,-55.6277179305633,
12.));
#124690=CARTESIAN_POINT('Ctrl Pts',(44.9397947641007,-55.6494102110935,
12.));
#124691=CARTESIAN_POINT('Ctrl Pts',(44.9476897959685,-55.6711521445979,
12.));
#124692=CARTESIAN_POINT('Ctrl Pts',(44.9555783004106,-55.6929436305489,
12.));
#124693=CARTESIAN_POINT('Ctrl Pts',(44.9634601713321,-55.714784568793,12.));
#124694=CARTESIAN_POINT('Ctrl Pts',(44.9713353031804,-55.7366748595551,
12.));
#124695=CARTESIAN_POINT('Ctrl Pts',(44.9792035909413,-55.7586144034367,
12.));
#124696=CARTESIAN_POINT('Ctrl Pts',(44.9870649301342,-55.7806031014106,
12.));
#124697=CARTESIAN_POINT('Ctrl Pts',(44.9949192168093,-55.8026408548105,
12.));
#124698=CARTESIAN_POINT('Ctrl Pts',(45.0027663475433,-55.8247275653289,
12.));
#124699=CARTESIAN_POINT('Ctrl Pts',(45.0106062194342,-55.8468631350218,
12.));
#124700=CARTESIAN_POINT('Ctrl Pts',(45.0184387300973,-55.8690474663065,
12.));
#124701=CARTESIAN_POINT('Ctrl Pts',(45.0262637776615,-55.8912804619577,
12.));
#124702=CARTESIAN_POINT('Ctrl Pts',(45.0340812607657,-55.9135620250954,
12.));
#124703=CARTESIAN_POINT('Ctrl Pts',(45.0418910785551,-55.9358920591837,
12.));
#124704=CARTESIAN_POINT('Ctrl Pts',(45.0496931306755,-55.9582704680356,
12.));
#124705=CARTESIAN_POINT('Ctrl Pts',(45.0574873172695,-55.9806971558097,
12.));
#124706=CARTESIAN_POINT('Ctrl Pts',(45.0652735389733,-56.003172027008,12.));
#124707=CARTESIAN_POINT('Ctrl Pts',(45.0730516969149,-56.0256949864639,
12.));
#124708=CARTESIAN_POINT('Ctrl Pts',(45.0808216927089,-56.048265939342,12.));
#124709=CARTESIAN_POINT('Ctrl Pts',(45.0885834284517,-56.0708847911416,
12.));
#124710=CARTESIAN_POINT('Ctrl Pts',(45.0963368067177,-56.0935514476945,
12.));
#124711=CARTESIAN_POINT('Ctrl Pts',(45.1040817305561,-56.116265815162,12.));
#124712=CARTESIAN_POINT('Ctrl Pts',(45.1118181034888,-56.1390278000226,
12.));
#124713=CARTESIAN_POINT('Ctrl Pts',(45.1195458295063,-56.1618373090732,
12.));
#124714=CARTESIAN_POINT('Ctrl Pts',(45.127264813063,-56.1846942494325,12.));
#124715=CARTESIAN_POINT('Ctrl Pts',(45.1349749590738,-56.2075985285393,
12.));
#124716=CARTESIAN_POINT('Ctrl Pts',(45.1426761729105,-56.2305500541489,
12.));
#124717=CARTESIAN_POINT('Ctrl Pts',(45.1503683604005,-56.2535487343221,
12.));
#124718=CARTESIAN_POINT('Ctrl Pts',(45.1580514278223,-56.2765944774245,
12.));
#124719=CARTESIAN_POINT('Ctrl Pts',(45.1657252819013,-56.2996871921316,
12.));
#124720=CARTESIAN_POINT('Ctrl Pts',(45.1733898298061,-56.3228267874264,
12.));
#124721=CARTESIAN_POINT('Ctrl Pts',(45.1810449791453,-56.3460131725964,
12.));
#124722=CARTESIAN_POINT('Ctrl Pts',(45.1886906379667,-56.3692462572231,
12.));
#124723=CARTESIAN_POINT('Ctrl Pts',(45.1963267147529,-56.3925259511806,
12.));
#124724=CARTESIAN_POINT('Ctrl Pts',(45.2039531184172,-56.4158521646411,
12.));
#124725=CARTESIAN_POINT('Ctrl Pts',(45.2115697583001,-56.4392248080732,
12.));
#124726=CARTESIAN_POINT('Ctrl Pts',(45.2191765441667,-56.4626437922386,
12.));
#124727=CARTESIAN_POINT('Ctrl Pts',(45.2267733862049,-56.4861090281823,
12.));
#124728=CARTESIAN_POINT('Ctrl Pts',(45.2343601950228,-56.5096204272306,
12.));
#124729=CARTESIAN_POINT('Ctrl Pts',(45.2419368816429,-56.5331779009958,
12.));
#124730=CARTESIAN_POINT('Ctrl Pts',(45.2495033575,-56.5567813613756,12.));
#124731=CARTESIAN_POINT('Ctrl Pts',(45.257059534438,-56.5804307205505,12.));
#124732=CARTESIAN_POINT('Ctrl Pts',(45.2646053247087,-56.6041258909741,
12.));
#124733=CARTESIAN_POINT('Ctrl Pts',(45.2721406409695,-56.6278667853702,
12.));
#124734=CARTESIAN_POINT('Ctrl Pts',(45.2796653962785,-56.6516533167384,
12.));
#124735=CARTESIAN_POINT('Ctrl Pts',(45.2871795040906,-56.6754853983528,
12.));
#124736=CARTESIAN_POINT('Ctrl Pts',(45.2946828782559,-56.69936294376,12.));
#124737=CARTESIAN_POINT('Ctrl Pts',(45.3021754330179,-56.7232858667709,
12.));
#124738=CARTESIAN_POINT('Ctrl Pts',(45.3096570830118,-56.7472540814553,
12.));
#124739=CARTESIAN_POINT('Ctrl Pts',(45.31712774326,-56.7712675021491,12.));
#124740=CARTESIAN_POINT('Ctrl Pts',(45.3245873291684,-56.7953260434524,
12.));
#124741=CARTESIAN_POINT('Ctrl Pts',(45.332035756524,-56.8194296202291,12.));
#124742=CARTESIAN_POINT('Ctrl Pts',(45.3394729414931,-56.8435781475981,
12.));
#124743=CARTESIAN_POINT('Ctrl Pts',(45.3468988006203,-56.8677715409268,
12.));
#124744=CARTESIAN_POINT('Ctrl Pts',(45.3543132508239,-56.8920097158377,
12.));
#124745=CARTESIAN_POINT('Ctrl Pts',(45.3617162093923,-56.9162925882085,
12.));
#124746=CARTESIAN_POINT('Ctrl Pts',(45.3691075939827,-56.9406200741714,
12.));
#124747=CARTESIAN_POINT('Ctrl Pts',(45.3764873226196,-56.9649920901073,
12.));
#124748=CARTESIAN_POINT('Ctrl Pts',(45.3838553136948,-56.9894085526373,
12.));
#124749=CARTESIAN_POINT('Ctrl Pts',(45.3912114859616,-57.0138693786278,
12.));
#124750=CARTESIAN_POINT('Ctrl Pts',(45.3985557585311,-57.0383744851913,
12.));
#124751=CARTESIAN_POINT('Ctrl Pts',(45.4058880508693,-57.0629237896848,
12.));
#124752=CARTESIAN_POINT('Ctrl Pts',(45.4132082827948,-57.0875172097051,
12.));
#124753=CARTESIAN_POINT('Ctrl Pts',(45.4205163744782,-57.112154663078,12.));
#124754=CARTESIAN_POINT('Ctrl Pts',(45.4278122464389,-57.136836067863,12.));
#124755=CARTESIAN_POINT('Ctrl Pts',(45.4350958195434,-57.1615613423584,
12.));
#124756=CARTESIAN_POINT('Ctrl Pts',(45.4423670150034,-57.186330405101,12.));
#124757=CARTESIAN_POINT('Ctrl Pts',(45.4496257543759,-57.2111431748631,
12.));
#124758=CARTESIAN_POINT('Ctrl Pts',(45.4568719595642,-57.2359995706447,
12.));
#124759=CARTESIAN_POINT('Ctrl Pts',(45.4641055528141,-57.2608995116733,
12.));
#124760=CARTESIAN_POINT('Ctrl Pts',(45.4713264567063,-57.2858429174062,
12.));
#124761=CARTESIAN_POINT('Ctrl Pts',(45.4785345941507,-57.3108297075265,
12.));
#124762=CARTESIAN_POINT('Ctrl Pts',(45.4857298883824,-57.3358598019389,
12.));
#124763=CARTESIAN_POINT('Ctrl Pts',(45.4929122629572,-57.3609331207574,
12.));
#124764=CARTESIAN_POINT('Ctrl Pts',(45.500081641751,-57.3860495843033,12.));
#124765=CARTESIAN_POINT('Ctrl Pts',(45.5072379489631,-57.4112091131183,
12.));
#124766=CARTESIAN_POINT('Ctrl Pts',(45.5143811091205,-57.4364116279702,
12.));
#124767=CARTESIAN_POINT('Ctrl Pts',(45.5215110470825,-57.4616570498568,
12.));
#124768=CARTESIAN_POINT('Ctrl Pts',(45.5286276880485,-57.4869453000063,
12.));
#124769=CARTESIAN_POINT('Ctrl Pts',(45.5357309575611,-57.5122762998745,
12.));
#124770=CARTESIAN_POINT('Ctrl Pts',(45.542820781484,-57.537649971135,12.));
#124771=CARTESIAN_POINT('Ctrl Pts',(45.5498970859835,-57.563066235668,12.));
#124772=CARTESIAN_POINT('Ctrl Pts',(45.5569597975096,-57.5885250155433,
12.));
#124773=CARTESIAN_POINT('Ctrl Pts',(45.5640088427813,-57.614026233004,12.));
#124774=CARTESIAN_POINT('Ctrl Pts',(45.5710441487674,-57.6395698104404,
12.));
#124775=CARTESIAN_POINT('Ctrl Pts',(45.5780656427163,-57.6651556704237,
12.));
#124776=CARTESIAN_POINT('Ctrl Pts',(45.5850732521896,-57.6907837357417,
12.));
#124777=CARTESIAN_POINT('Ctrl Pts',(45.5920669050986,-57.7164539294314,
12.));
#124778=CARTESIAN_POINT('Ctrl Pts',(45.5990465297344,-57.7421661748026,
12.));
#124779=CARTESIAN_POINT('Ctrl Pts',(45.6060120548205,-57.7679203954742,
12.));
#124780=CARTESIAN_POINT('Ctrl Pts',(45.6129634094683,-57.7937165153387,
12.));
#124781=CARTESIAN_POINT('Ctrl Pts',(45.6199005230784,-57.8195544584845,
12.));
#124782=CARTESIAN_POINT('Ctrl Pts',(45.6268233252544,-57.8454341491238,
12.));
#124783=CARTESIAN_POINT('Ctrl Pts',(45.6337317457252,-57.8713555115232,
12.));
#124784=CARTESIAN_POINT('Ctrl Pts',(45.6406257142382,-57.8973184699034,
12.));
#124785=CARTESIAN_POINT('Ctrl Pts',(45.6475051605535,-57.9233229484311,
12.));
#124786=CARTESIAN_POINT('Ctrl Pts',(45.6543700146679,-57.9493688714237,
12.));
#124787=CARTESIAN_POINT('Ctrl Pts',(45.661220206992,-57.9754561635061,12.));
#124788=CARTESIAN_POINT('Ctrl Pts',(45.6680556685493,-58.0015847497837,
12.));
#124789=CARTESIAN_POINT('Ctrl Pts',(45.6748763311643,-58.0277545560012,
12.));
#124790=CARTESIAN_POINT('Ctrl Pts',(45.6816821276678,-58.0539655087117,
12.));
#124791=CARTESIAN_POINT('Ctrl Pts',(45.6884729914485,-58.0802175348966,
12.));
#124792=CARTESIAN_POINT('Ctrl Pts',(45.695248856015,-58.1065105615907,12.));
#124793=CARTESIAN_POINT('Ctrl Pts',(45.702009654518,-58.1328445154676,12.));
#124794=CARTESIAN_POINT('Ctrl Pts',(45.7087553193771,-58.1592193225137,
12.));
#124795=CARTESIAN_POINT('Ctrl Pts',(45.7154857816483,-58.185634907469,12.));
#124796=CARTESIAN_POINT('Ctrl Pts',(45.7222009715397,-58.2120911942772,
12.));
#124797=CARTESIAN_POINT('Ctrl Pts',(45.7289008195579,-58.2385881070913,
12.));
#124798=CARTESIAN_POINT('Ctrl Pts',(45.7355852575107,-58.2651255711453,
12.));
#124799=CARTESIAN_POINT('Ctrl Pts',(45.742254219463,-58.291703513584,12.));
#124800=CARTESIAN_POINT('Ctrl Pts',(45.7489076429763,-58.3183218645316,
12.));
#124801=CARTESIAN_POINT('Ctrl Pts',(45.755545469402,-58.3449805573423,12.));
#124802=CARTESIAN_POINT('Ctrl Pts',(45.7612219538124,-58.3678667473437,
12.));
#124803=CARTESIAN_POINT('Ctrl Pts',(45.7655655205367,-58.3854348517442,
12.));
#124804=CARTESIAN_POINT('Ctrl Pts',(45.7685831165564,-58.3976670481067,
12.));
#124805=CARTESIAN_POINT('Ctrl Pts',(45.7702793558176,-58.4045515723353,
12.));
#124806=CARTESIAN_POINT('Ctrl Pts',(45.7706564944895,-58.4060826907792,
12.));
#124807=CARTESIAN_POINT('',(44.3377168516418,-54.1679505278134,0.));
#124808=CARTESIAN_POINT('',(44.3377168516418,-54.1679505278134,0.));
#124809=CARTESIAN_POINT('Ctrl Pts',(45.7706564944895,-58.4060826907792,
0.));
#124810=CARTESIAN_POINT('Ctrl Pts',(45.7702793558176,-58.4045515723353,
0.));
#124811=CARTESIAN_POINT('Ctrl Pts',(45.7685831165564,-58.3976670481067,
0.));
#124812=CARTESIAN_POINT('Ctrl Pts',(45.7655655205367,-58.3854348517442,
0.));
#124813=CARTESIAN_POINT('Ctrl Pts',(45.7612219538124,-58.3678667473437,
0.));
#124814=CARTESIAN_POINT('Ctrl Pts',(45.755545469402,-58.3449805573423,0.));
#124815=CARTESIAN_POINT('Ctrl Pts',(45.7489076429763,-58.3183218645316,
0.));
#124816=CARTESIAN_POINT('Ctrl Pts',(45.742254219463,-58.291703513584,0.));
#124817=CARTESIAN_POINT('Ctrl Pts',(45.7355852575107,-58.2651255711453,
0.));
#124818=CARTESIAN_POINT('Ctrl Pts',(45.7289008195579,-58.2385881070913,
0.));
#124819=CARTESIAN_POINT('Ctrl Pts',(45.7222009715397,-58.2120911942772,
0.));
#124820=CARTESIAN_POINT('Ctrl Pts',(45.7154857816483,-58.185634907469,0.));
#124821=CARTESIAN_POINT('Ctrl Pts',(45.7087553193771,-58.1592193225137,
0.));
#124822=CARTESIAN_POINT('Ctrl Pts',(45.702009654518,-58.1328445154676,0.));
#124823=CARTESIAN_POINT('Ctrl Pts',(45.695248856015,-58.1065105615907,0.));
#124824=CARTESIAN_POINT('Ctrl Pts',(45.6884729914485,-58.0802175348966,
0.));
#124825=CARTESIAN_POINT('Ctrl Pts',(45.6816821276678,-58.0539655087117,
0.));
#124826=CARTESIAN_POINT('Ctrl Pts',(45.6748763311643,-58.0277545560012,
0.));
#124827=CARTESIAN_POINT('Ctrl Pts',(45.6680556685493,-58.0015847497837,
0.));
#124828=CARTESIAN_POINT('Ctrl Pts',(45.661220206992,-57.9754561635061,0.));
#124829=CARTESIAN_POINT('Ctrl Pts',(45.6543700146679,-57.9493688714237,
0.));
#124830=CARTESIAN_POINT('Ctrl Pts',(45.6475051605535,-57.9233229484311,
0.));
#124831=CARTESIAN_POINT('Ctrl Pts',(45.6406257142382,-57.8973184699034,
0.));
#124832=CARTESIAN_POINT('Ctrl Pts',(45.6337317457252,-57.8713555115232,
0.));
#124833=CARTESIAN_POINT('Ctrl Pts',(45.6268233252544,-57.8454341491238,
0.));
#124834=CARTESIAN_POINT('Ctrl Pts',(45.6199005230784,-57.8195544584845,
0.));
#124835=CARTESIAN_POINT('Ctrl Pts',(45.6129634094683,-57.7937165153387,
0.));
#124836=CARTESIAN_POINT('Ctrl Pts',(45.6060120548205,-57.7679203954742,
0.));
#124837=CARTESIAN_POINT('Ctrl Pts',(45.5990465297344,-57.7421661748026,
0.));
#124838=CARTESIAN_POINT('Ctrl Pts',(45.5920669050986,-57.7164539294314,
0.));
#124839=CARTESIAN_POINT('Ctrl Pts',(45.5850732521896,-57.6907837357417,
0.));
#124840=CARTESIAN_POINT('Ctrl Pts',(45.5780656427163,-57.6651556704237,
0.));
#124841=CARTESIAN_POINT('Ctrl Pts',(45.5710441487674,-57.6395698104404,
0.));
#124842=CARTESIAN_POINT('Ctrl Pts',(45.5640088427813,-57.614026233004,0.));
#124843=CARTESIAN_POINT('Ctrl Pts',(45.5569597975096,-57.5885250155433,
0.));
#124844=CARTESIAN_POINT('Ctrl Pts',(45.5498970859835,-57.563066235668,0.));
#124845=CARTESIAN_POINT('Ctrl Pts',(45.542820781484,-57.537649971135,0.));
#124846=CARTESIAN_POINT('Ctrl Pts',(45.5357309575611,-57.5122762998745,
0.));
#124847=CARTESIAN_POINT('Ctrl Pts',(45.5286276880485,-57.4869453000063,
0.));
#124848=CARTESIAN_POINT('Ctrl Pts',(45.5215110470825,-57.4616570498568,
0.));
#124849=CARTESIAN_POINT('Ctrl Pts',(45.5143811091205,-57.4364116279702,
0.));
#124850=CARTESIAN_POINT('Ctrl Pts',(45.5072379489631,-57.4112091131183,
0.));
#124851=CARTESIAN_POINT('Ctrl Pts',(45.500081641751,-57.3860495843033,0.));
#124852=CARTESIAN_POINT('Ctrl Pts',(45.4929122629572,-57.3609331207574,
0.));
#124853=CARTESIAN_POINT('Ctrl Pts',(45.4857298883824,-57.3358598019389,
0.));
#124854=CARTESIAN_POINT('Ctrl Pts',(45.4785345941507,-57.3108297075265,
0.));
#124855=CARTESIAN_POINT('Ctrl Pts',(45.4713264567063,-57.2858429174062,
0.));
#124856=CARTESIAN_POINT('Ctrl Pts',(45.4641055528141,-57.2608995116733,
0.));
#124857=CARTESIAN_POINT('Ctrl Pts',(45.4568719595642,-57.2359995706447,
0.));
#124858=CARTESIAN_POINT('Ctrl Pts',(45.4496257543759,-57.2111431748631,
0.));
#124859=CARTESIAN_POINT('Ctrl Pts',(45.4423670150034,-57.186330405101,0.));
#124860=CARTESIAN_POINT('Ctrl Pts',(45.4350958195434,-57.1615613423584,
0.));
#124861=CARTESIAN_POINT('Ctrl Pts',(45.4278122464389,-57.136836067863,0.));
#124862=CARTESIAN_POINT('Ctrl Pts',(45.4205163744782,-57.112154663078,0.));
#124863=CARTESIAN_POINT('Ctrl Pts',(45.4132082827948,-57.0875172097051,
0.));
#124864=CARTESIAN_POINT('Ctrl Pts',(45.4058880508693,-57.0629237896848,
0.));
#124865=CARTESIAN_POINT('Ctrl Pts',(45.3985557585311,-57.0383744851913,
0.));
#124866=CARTESIAN_POINT('Ctrl Pts',(45.3912114859616,-57.0138693786278,
0.));
#124867=CARTESIAN_POINT('Ctrl Pts',(45.3838553136948,-56.9894085526373,
0.));
#124868=CARTESIAN_POINT('Ctrl Pts',(45.3764873226196,-56.9649920901073,
0.));
#124869=CARTESIAN_POINT('Ctrl Pts',(45.3691075939827,-56.9406200741714,
0.));
#124870=CARTESIAN_POINT('Ctrl Pts',(45.3617162093923,-56.9162925882085,
0.));
#124871=CARTESIAN_POINT('Ctrl Pts',(45.3543132508239,-56.8920097158377,
0.));
#124872=CARTESIAN_POINT('Ctrl Pts',(45.3468988006203,-56.8677715409268,
0.));
#124873=CARTESIAN_POINT('Ctrl Pts',(45.3394729414931,-56.8435781475981,
0.));
#124874=CARTESIAN_POINT('Ctrl Pts',(45.332035756524,-56.8194296202291,0.));
#124875=CARTESIAN_POINT('Ctrl Pts',(45.3245873291684,-56.7953260434524,
0.));
#124876=CARTESIAN_POINT('Ctrl Pts',(45.31712774326,-56.7712675021491,0.));
#124877=CARTESIAN_POINT('Ctrl Pts',(45.3096570830118,-56.7472540814553,
0.));
#124878=CARTESIAN_POINT('Ctrl Pts',(45.3021754330179,-56.7232858667709,
0.));
#124879=CARTESIAN_POINT('Ctrl Pts',(45.2946828782559,-56.69936294376,0.));
#124880=CARTESIAN_POINT('Ctrl Pts',(45.2871795040906,-56.6754853983528,
0.));
#124881=CARTESIAN_POINT('Ctrl Pts',(45.2796653962785,-56.6516533167384,
0.));
#124882=CARTESIAN_POINT('Ctrl Pts',(45.2721406409695,-56.6278667853702,
0.));
#124883=CARTESIAN_POINT('Ctrl Pts',(45.2646053247087,-56.6041258909741,
0.));
#124884=CARTESIAN_POINT('Ctrl Pts',(45.257059534438,-56.5804307205505,0.));
#124885=CARTESIAN_POINT('Ctrl Pts',(45.2495033575,-56.5567813613756,0.));
#124886=CARTESIAN_POINT('Ctrl Pts',(45.2419368816429,-56.5331779009958,
0.));
#124887=CARTESIAN_POINT('Ctrl Pts',(45.2343601950228,-56.5096204272306,
0.));
#124888=CARTESIAN_POINT('Ctrl Pts',(45.2267733862049,-56.4861090281823,
0.));
#124889=CARTESIAN_POINT('Ctrl Pts',(45.2191765441667,-56.4626437922386,
0.));
#124890=CARTESIAN_POINT('Ctrl Pts',(45.2115697583001,-56.4392248080732,
0.));
#124891=CARTESIAN_POINT('Ctrl Pts',(45.2039531184172,-56.4158521646411,
0.));
#124892=CARTESIAN_POINT('Ctrl Pts',(45.1963267147529,-56.3925259511806,
0.));
#124893=CARTESIAN_POINT('Ctrl Pts',(45.1886906379667,-56.3692462572231,
0.));
#124894=CARTESIAN_POINT('Ctrl Pts',(45.1810449791453,-56.3460131725964,
0.));
#124895=CARTESIAN_POINT('Ctrl Pts',(45.1733898298061,-56.3228267874264,
0.));
#124896=CARTESIAN_POINT('Ctrl Pts',(45.1657252819013,-56.2996871921316,
0.));
#124897=CARTESIAN_POINT('Ctrl Pts',(45.1580514278223,-56.2765944774245,
0.));
#124898=CARTESIAN_POINT('Ctrl Pts',(45.1503683604005,-56.2535487343221,
0.));
#124899=CARTESIAN_POINT('Ctrl Pts',(45.1426761729105,-56.2305500541489,
0.));
#124900=CARTESIAN_POINT('Ctrl Pts',(45.1349749590738,-56.2075985285393,
0.));
#124901=CARTESIAN_POINT('Ctrl Pts',(45.127264813063,-56.1846942494325,0.));
#124902=CARTESIAN_POINT('Ctrl Pts',(45.1195458295063,-56.1618373090732,
0.));
#124903=CARTESIAN_POINT('Ctrl Pts',(45.1118181034888,-56.1390278000226,
0.));
#124904=CARTESIAN_POINT('Ctrl Pts',(45.1040817305561,-56.116265815162,0.));
#124905=CARTESIAN_POINT('Ctrl Pts',(45.0963368067177,-56.0935514476945,
0.));
#124906=CARTESIAN_POINT('Ctrl Pts',(45.0885834284517,-56.0708847911416,
0.));
#124907=CARTESIAN_POINT('Ctrl Pts',(45.0808216927089,-56.048265939342,0.));
#124908=CARTESIAN_POINT('Ctrl Pts',(45.0730516969149,-56.0256949864639,
0.));
#124909=CARTESIAN_POINT('Ctrl Pts',(45.0652735389733,-56.003172027008,0.));
#124910=CARTESIAN_POINT('Ctrl Pts',(45.0574873172695,-55.9806971558097,
0.));
#124911=CARTESIAN_POINT('Ctrl Pts',(45.0496931306755,-55.9582704680356,
0.));
#124912=CARTESIAN_POINT('Ctrl Pts',(45.0418910785551,-55.9358920591837,
0.));
#124913=CARTESIAN_POINT('Ctrl Pts',(45.0340812607657,-55.9135620250954,
0.));
#124914=CARTESIAN_POINT('Ctrl Pts',(45.0262637776615,-55.8912804619577,
0.));
#124915=CARTESIAN_POINT('Ctrl Pts',(45.0184387300973,-55.8690474663065,
0.));
#124916=CARTESIAN_POINT('Ctrl Pts',(45.0106062194342,-55.8468631350218,
0.));
#124917=CARTESIAN_POINT('Ctrl Pts',(45.0027663475433,-55.8247275653289,
0.));
#124918=CARTESIAN_POINT('Ctrl Pts',(44.9949192168093,-55.8026408548105,
0.));
#124919=CARTESIAN_POINT('Ctrl Pts',(44.9870649301342,-55.7806031014106,
0.));
#124920=CARTESIAN_POINT('Ctrl Pts',(44.9792035909413,-55.7586144034367,
0.));
#124921=CARTESIAN_POINT('Ctrl Pts',(44.9713353031804,-55.7366748595551,
0.));
#124922=CARTESIAN_POINT('Ctrl Pts',(44.9634601713321,-55.714784568793,0.));
#124923=CARTESIAN_POINT('Ctrl Pts',(44.9555783004106,-55.6929436305489,
0.));
#124924=CARTESIAN_POINT('Ctrl Pts',(44.9476897959685,-55.6711521445979,
0.));
#124925=CARTESIAN_POINT('Ctrl Pts',(44.9397947641007,-55.6494102110935,
0.));
#124926=CARTESIAN_POINT('Ctrl Pts',(44.9318933114507,-55.6277179305633,
0.));
#124927=CARTESIAN_POINT('Ctrl Pts',(44.9239855452144,-55.6060754039121,
0.));
#124928=CARTESIAN_POINT('Ctrl Pts',(44.9160715731443,-55.5844827324338,
0.));
#124929=CARTESIAN_POINT('Ctrl Pts',(44.908151503553,-55.5629400178142,0.));
#124930=CARTESIAN_POINT('Ctrl Pts',(44.9002254453183,-55.541447362134,0.));
#124931=CARTESIAN_POINT('Ctrl Pts',(44.8922935078889,-55.5200048678629,
0.));
#124932=CARTESIAN_POINT('Ctrl Pts',(44.8843558012886,-55.4986126378656,
0.));
#124933=CARTESIAN_POINT('Ctrl Pts',(44.8764124361207,-55.4772707754126,
0.));
#124934=CARTESIAN_POINT('Ctrl Pts',(44.8684635235725,-55.4559793841836,
0.));
#124935=CARTESIAN_POINT('Ctrl Pts',(44.8605091754214,-55.4347385682704,
0.));
#124936=CARTESIAN_POINT('Ctrl Pts',(44.8525495040408,-55.4135484321718,
0.));
#124937=CARTESIAN_POINT('Ctrl Pts',(44.8445846224044,-55.3924090808014,
0.));
#124938=CARTESIAN_POINT('Ctrl Pts',(44.8366146440901,-55.3713206194967,
0.));
#124939=CARTESIAN_POINT('Ctrl Pts',(44.8286396832848,-55.3502831540228,
0.));
#124940=CARTESIAN_POINT('Ctrl Pts',(44.8206598547888,-55.3292967905725,
0.));
#124941=CARTESIAN_POINT('Ctrl Pts',(44.8126752740208,-55.3083616357605,
0.));
#124942=CARTESIAN_POINT('Ctrl Pts',(44.8046860570244,-55.287477796635,0.));
#124943=CARTESIAN_POINT('Ctrl Pts',(44.796692320474,-55.2666453806883,0.));
#124944=CARTESIAN_POINT('Ctrl Pts',(44.7886941816823,-55.2458644958617,
0.));
#124945=CARTESIAN_POINT('Ctrl Pts',(44.7806917586077,-55.2251352505474,
0.));
#124946=CARTESIAN_POINT('Ctrl Pts',(44.7726851698618,-55.2044577535865,
0.));
#124947=CARTESIAN_POINT('Ctrl Pts',(44.7646745347108,-55.1838321142777,
0.));
#124948=CARTESIAN_POINT('Ctrl Pts',(44.7566599730771,-55.1632584423813,
0.));
#124949=CARTESIAN_POINT('Ctrl Pts',(44.748641605542,-55.1427368481201,0.));
#124950=CARTESIAN_POINT('Ctrl Pts',(44.7406195533483,-55.1222674421747,
0.));
#124951=CARTESIAN_POINT('Ctrl Pts',(44.7325939384042,-55.1018503356806,
0.));
#124952=CARTESIAN_POINT('Ctrl Pts',(44.7245648832988,-55.0814856402507,
0.));
#124953=CARTESIAN_POINT('Ctrl Pts',(44.7165325113165,-55.0611734679902,
0.));
#124954=CARTESIAN_POINT('Ctrl Pts',(44.7084969464509,-55.0409139315074,
0.));
#124955=CARTESIAN_POINT('Ctrl Pts',(44.7004583134235,-55.020707143922,0.));
#124956=CARTESIAN_POINT('Ctrl Pts',(44.6924167376851,-55.0005532188644,
0.));
#124957=CARTESIAN_POINT('Ctrl Pts',(44.6843723453985,-54.9804522704668,
0.));
#124958=CARTESIAN_POINT('Ctrl Pts',(44.6763252634255,-54.9604044133497,
0.));
#124959=CARTESIAN_POINT('Ctrl Pts',(44.6682756193156,-54.9404097626088,
0.));
#124960=CARTESIAN_POINT('Ctrl Pts',(44.6602235412854,-54.9204684337845,
0.));
#124961=CARTESIAN_POINT('Ctrl Pts',(44.6521691582551,-54.9005805428991,
0.));
#124962=CARTESIAN_POINT('Ctrl Pts',(44.6441125999074,-54.8807462065177,
0.));
#124963=CARTESIAN_POINT('Ctrl Pts',(44.6360539967392,-54.860965541796,0.));
#124964=CARTESIAN_POINT('Ctrl Pts',(44.6279934801159,-54.8412386665264,
0.));
#124965=CARTESIAN_POINT('Ctrl Pts',(44.6199311823276,-54.8215656991817,
0.));
#124966=CARTESIAN_POINT('Ctrl Pts',(44.6118672364889,-54.8019467588257,
0.));
#124967=CARTESIAN_POINT('Ctrl Pts',(44.60380177643,-54.7823819650137,0.));
#124968=CARTESIAN_POINT('Ctrl Pts',(44.5957349366062,-54.7628714377041,
0.));
#124969=CARTESIAN_POINT('Ctrl Pts',(44.5876668519676,-54.7434152971285,
0.));
#124970=CARTESIAN_POINT('Ctrl Pts',(44.5795976579476,-54.7240136637744,
0.));
#124971=CARTESIAN_POINT('Ctrl Pts',(44.5715274907637,-54.7046666586776,
0.));
#124972=CARTESIAN_POINT('Ctrl Pts',(44.563456487687,-54.685374403676,0.));
#124973=CARTESIAN_POINT('Ctrl Pts',(44.5553847872712,-54.6661370216242,
0.));
#124974=CARTESIAN_POINT('Ctrl Pts',(44.5473125297289,-54.6469546367381,
0.));
#124975=CARTESIAN_POINT('Ctrl Pts',(44.5392398566775,-54.6278273743554,
0.));
#124976=CARTESIAN_POINT('Ctrl Pts',(44.5311669104495,-54.6087553602889,
0.));
#124977=CARTESIAN_POINT('Ctrl Pts',(44.5230938335165,-54.5897387202812,
0.));
#124978=CARTESIAN_POINT('Ctrl Pts',(44.5150207679007,-54.5707775794436,
0.));
#124979=CARTESIAN_POINT('Ctrl Pts',(44.5069478544977,-54.5518720616056,
0.));
#124980=CARTESIAN_POINT('Ctrl Pts',(44.4988752343744,-54.5330222905475,
0.));
#124981=CARTESIAN_POINT('Ctrl Pts',(44.4908030503225,-54.5142283914704,
0.));
#124982=CARTESIAN_POINT('Ctrl Pts',(44.4827314481264,-54.495490492193,0.));
#124983=CARTESIAN_POINT('Ctrl Pts',(44.4746605784031,-54.4768087248824,
0.));
#124984=CARTESIAN_POINT('Ctrl Pts',(44.4665905967668,-54.4581832262033,
0.));
#124985=CARTESIAN_POINT('Ctrl Pts',(44.4585216599908,-54.4396141336978,
0.));
#124986=CARTESIAN_POINT('Ctrl Pts',(44.4504539226328,-54.421101582595,0.));
#124987=CARTESIAN_POINT('Ctrl Pts',(44.4423875340996,-54.4026457030335,
0.));
#124988=CARTESIAN_POINT('Ctrl Pts',(44.4343226339593,-54.3842466156196,
0.));
#124989=CARTESIAN_POINT('Ctrl Pts',(44.4262593564712,-54.3659044357119,
0.));
#124990=CARTESIAN_POINT('Ctrl Pts',(44.4181978395851,-54.3476192819352,
0.));
#124991=CARTESIAN_POINT('Ctrl Pts',(44.4101382321834,-54.3293912830237,
0.));
#124992=CARTESIAN_POINT('Ctrl Pts',(44.402080702809,-54.3112205860716,0.));
#124993=CARTESIAN_POINT('Ctrl Pts',(44.3940254456331,-54.2931073621553,
0.));
#124994=CARTESIAN_POINT('Ctrl Pts',(44.3859726620183,-54.2750517888579,
0.));
#124995=CARTESIAN_POINT('Ctrl Pts',(44.3779225430406,-54.2570540336475,
0.));
#124996=CARTESIAN_POINT('Ctrl Pts',(44.3698752533562,-54.2391142386412,
0.));
#124997=CARTESIAN_POINT('Ctrl Pts',(44.361830910343,-54.2212325006052,0.));
#124998=CARTESIAN_POINT('Ctrl Pts',(44.3537895824096,-54.2034088701928,
0.));
#124999=CARTESIAN_POINT('Ctrl Pts',(44.3473589597726,-54.1891964684727,
0.));
#125000=CARTESIAN_POINT('Ctrl Pts',(44.3425373700993,-54.1785633257639,
0.));
#125001=CARTESIAN_POINT('Ctrl Pts',(44.3393235891075,-54.1714861895346,
0.));
#125002=CARTESIAN_POINT('Ctrl Pts',(44.3377168516418,-54.1679505278134,
0.));
#125003=CARTESIAN_POINT('Ctrl Pts',(40.554341280847,-62.494763006804,0.));
#125004=CARTESIAN_POINT('Ctrl Pts',(40.554341280847,-62.494763006804,12.));
#125005=CARTESIAN_POINT('Ctrl Pts',(40.5535399497519,-62.489224912198,0.));
#125006=CARTESIAN_POINT('Ctrl Pts',(40.5535399497519,-62.489224912198,12.));
#125007=CARTESIAN_POINT('Ctrl Pts',(40.5519353177252,-62.4781525156318,
0.));
#125008=CARTESIAN_POINT('Ctrl Pts',(40.5519353177252,-62.4781525156318,
12.));
#125009=CARTESIAN_POINT('Ctrl Pts',(40.5495224601758,-62.4615552987202,
0.));
#125010=CARTESIAN_POINT('Ctrl Pts',(40.5495224601758,-62.4615552987202,
12.));
#125011=CARTESIAN_POINT('Ctrl Pts',(40.5462934972718,-62.4394484329678,
0.));
#125012=CARTESIAN_POINT('Ctrl Pts',(40.5462934972718,-62.4394484329678,
12.));
#125013=CARTESIAN_POINT('Ctrl Pts',(40.5422375945026,-62.4118527881148,
0.));
#125014=CARTESIAN_POINT('Ctrl Pts',(40.5422375945026,-62.4118527881148,
12.));
#125015=CARTESIAN_POINT('Ctrl Pts',(40.5381619974169,-62.3842950992832,
0.));
#125016=CARTESIAN_POINT('Ctrl Pts',(40.5381619974169,-62.3842950992832,
12.));
#125017=CARTESIAN_POINT('Ctrl Pts',(40.5340667194319,-62.3567753970279,
0.));
#125018=CARTESIAN_POINT('Ctrl Pts',(40.5340667194319,-62.3567753970279,
12.));
#125019=CARTESIAN_POINT('Ctrl Pts',(40.5299517857721,-62.3292937257901,
0.));
#125020=CARTESIAN_POINT('Ctrl Pts',(40.5299517857721,-62.3292937257901,
12.));
#125021=CARTESIAN_POINT('Ctrl Pts',(40.5258172381429,-62.301850147165,0.));
#125022=CARTESIAN_POINT('Ctrl Pts',(40.5258172381429,-62.301850147165,12.));
#125023=CARTESIAN_POINT('Ctrl Pts',(40.5216631336193,-62.2744447381971,
0.));
#125024=CARTESIAN_POINT('Ctrl Pts',(40.5216631336193,-62.2744447381971,
12.));
#125025=CARTESIAN_POINT('Ctrl Pts',(40.5174895390954,-62.247077585866,0.));
#125026=CARTESIAN_POINT('Ctrl Pts',(40.5174895390954,-62.247077585866,12.));
#125027=CARTESIAN_POINT('Ctrl Pts',(40.5132965269633,-62.2197487826136,
0.));
#125028=CARTESIAN_POINT('Ctrl Pts',(40.5132965269633,-62.2197487826136,
12.));
#125029=CARTESIAN_POINT('Ctrl Pts',(40.5090841704122,-62.1924584215653,
0.));
#125030=CARTESIAN_POINT('Ctrl Pts',(40.5090841704122,-62.1924584215653,
12.));
#125031=CARTESIAN_POINT('Ctrl Pts',(40.5048525386035,-62.1652065915808,
0.));
#125032=CARTESIAN_POINT('Ctrl Pts',(40.5048525386035,-62.1652065915808,
12.));
#125033=CARTESIAN_POINT('Ctrl Pts',(40.5006016927554,-62.1379933732528,
0.));
#125034=CARTESIAN_POINT('Ctrl Pts',(40.5006016927554,-62.1379933732528,
12.));
#125035=CARTESIAN_POINT('Ctrl Pts',(40.4963316888412,-62.1108188417003,
0.));
#125036=CARTESIAN_POINT('Ctrl Pts',(40.4963316888412,-62.1108188417003,
12.));
#125037=CARTESIAN_POINT('Ctrl Pts',(40.4920425795217,-62.0836830685719,
0.));
#125038=CARTESIAN_POINT('Ctrl Pts',(40.4920425795217,-62.0836830685719,
12.));
#125039=CARTESIAN_POINT('Ctrl Pts',(40.4877344164411,-62.0565861244178,
0.));
#125040=CARTESIAN_POINT('Ctrl Pts',(40.4877344164411,-62.0565861244178,
12.));
#125041=CARTESIAN_POINT('Ctrl Pts',(40.4834072522164,-62.029528080742,0.));
#125042=CARTESIAN_POINT('Ctrl Pts',(40.4834072522164,-62.029528080742,12.));
#125043=CARTESIAN_POINT('Ctrl Pts',(40.4790611429584,-62.0025090125959,
0.));
#125044=CARTESIAN_POINT('Ctrl Pts',(40.4790611429584,-62.0025090125959,
12.));
#125045=CARTESIAN_POINT('Ctrl Pts',(40.4746961480015,-61.9755289983044,
0.));
#125046=CARTESIAN_POINT('Ctrl Pts',(40.4746961480015,-61.9755289983044,
12.));
#125047=CARTESIAN_POINT('Ctrl Pts',(40.4703123287621,-61.9485881182921,
0.));
#125048=CARTESIAN_POINT('Ctrl Pts',(40.4703123287621,-61.9485881182921,
12.));
#125049=CARTESIAN_POINT('Ctrl Pts',(40.4659097478587,-61.9216864541744,
0.));
#125050=CARTESIAN_POINT('Ctrl Pts',(40.4659097478587,-61.9216864541744,
12.));
#125051=CARTESIAN_POINT('Ctrl Pts',(40.4614884681889,-61.8948240878007,
0.));
#125052=CARTESIAN_POINT('Ctrl Pts',(40.4614884681889,-61.8948240878007,
12.));
#125053=CARTESIAN_POINT('Ctrl Pts',(40.457048551875,-61.8680011001537,0.));
#125054=CARTESIAN_POINT('Ctrl Pts',(40.457048551875,-61.8680011001537,12.));
#125055=CARTESIAN_POINT('Ctrl Pts',(40.4525900597894,-61.8412175708552,
0.));
#125056=CARTESIAN_POINT('Ctrl Pts',(40.4525900597894,-61.8412175708552,
12.));
#125057=CARTESIAN_POINT('Ctrl Pts',(40.4481130521364,-61.814473578779,0.));
#125058=CARTESIAN_POINT('Ctrl Pts',(40.4481130521364,-61.814473578779,12.));
#125059=CARTESIAN_POINT('Ctrl Pts',(40.443617588795,-61.7877692024076,0.));
#125060=CARTESIAN_POINT('Ctrl Pts',(40.443617588795,-61.7877692024076,12.));
#125061=CARTESIAN_POINT('Ctrl Pts',(40.4391037297589,-61.7611045202874,
0.));
#125062=CARTESIAN_POINT('Ctrl Pts',(40.4391037297589,-61.7611045202874,
12.));
#125063=CARTESIAN_POINT('Ctrl Pts',(40.4345715355405,-61.7344796114399,
0.));
#125064=CARTESIAN_POINT('Ctrl Pts',(40.4345715355405,-61.7344796114399,
12.));
#125065=CARTESIAN_POINT('Ctrl Pts',(40.430021067584,-61.7078945557799,0.));
#125066=CARTESIAN_POINT('Ctrl Pts',(40.430021067584,-61.7078945557799,12.));
#125067=CARTESIAN_POINT('Ctrl Pts',(40.425452388076,-61.6813494339286,0.));
#125068=CARTESIAN_POINT('Ctrl Pts',(40.425452388076,-61.6813494339286,12.));
#125069=CARTESIAN_POINT('Ctrl Pts',(40.4208655597717,-61.6548443270394,
0.));
#125070=CARTESIAN_POINT('Ctrl Pts',(40.4208655597717,-61.6548443270394,
12.));
#125071=CARTESIAN_POINT('Ctrl Pts',(40.4162606458119,-61.6283793166079,
0.));
#125072=CARTESIAN_POINT('Ctrl Pts',(40.4162606458119,-61.6283793166079,
12.));
#125073=CARTESIAN_POINT('Ctrl Pts',(40.4116377095596,-61.601954484301,0.));
#125074=CARTESIAN_POINT('Ctrl Pts',(40.4116377095596,-61.601954484301,12.));
#125075=CARTESIAN_POINT('Ctrl Pts',(40.4069968143956,-61.5755699117324,
0.));
#125076=CARTESIAN_POINT('Ctrl Pts',(40.4069968143956,-61.5755699117324,
12.));
#125077=CARTESIAN_POINT('Ctrl Pts',(40.4023380237232,-61.5492256804717,
0.));
#125078=CARTESIAN_POINT('Ctrl Pts',(40.4023380237232,-61.5492256804717,
12.));
#125079=CARTESIAN_POINT('Ctrl Pts',(40.3976614010653,-61.522921872154,0.));
#125080=CARTESIAN_POINT('Ctrl Pts',(40.3976614010653,-61.522921872154,12.));
#125081=CARTESIAN_POINT('Ctrl Pts',(40.3929670101366,-61.4966585685549,
0.));
#125082=CARTESIAN_POINT('Ctrl Pts',(40.3929670101366,-61.4966585685549,
12.));
#125083=CARTESIAN_POINT('Ctrl Pts',(40.3882549149228,-61.4704358516709,
0.));
#125084=CARTESIAN_POINT('Ctrl Pts',(40.3882549149228,-61.4704358516709,
12.));
#125085=CARTESIAN_POINT('Ctrl Pts',(40.383525179772,-61.4442538038044,0.));
#125086=CARTESIAN_POINT('Ctrl Pts',(40.383525179772,-61.4442538038044,12.));
#125087=CARTESIAN_POINT('Ctrl Pts',(40.3787778694364,-61.4181125076037,
0.));
#125088=CARTESIAN_POINT('Ctrl Pts',(40.3787778694364,-61.4181125076037,
12.));
#125089=CARTESIAN_POINT('Ctrl Pts',(40.3740130490225,-61.3920120460219,
0.));
#125090=CARTESIAN_POINT('Ctrl Pts',(40.3740130490225,-61.3920120460219,
12.));
#125091=CARTESIAN_POINT('Ctrl Pts',(40.3692307839636,-61.3659525022908,
0.));
#125092=CARTESIAN_POINT('Ctrl Pts',(40.3692307839636,-61.3659525022908,
12.));
#125093=CARTESIAN_POINT('Ctrl Pts',(40.3644311399861,-61.3399339598853,
0.));
#125094=CARTESIAN_POINT('Ctrl Pts',(40.3644311399861,-61.3399339598853,
12.));
#125095=CARTESIAN_POINT('Ctrl Pts',(40.3596141830791,-61.3139565024847,
0.));
#125096=CARTESIAN_POINT('Ctrl Pts',(40.3596141830791,-61.3139565024847,
12.));
#125097=CARTESIAN_POINT('Ctrl Pts',(40.3547799794679,-61.2880202139371,
0.));
#125098=CARTESIAN_POINT('Ctrl Pts',(40.3547799794679,-61.2880202139371,
12.));
#125099=CARTESIAN_POINT('Ctrl Pts',(40.3499285956304,-61.2621251782863,
0.));
#125100=CARTESIAN_POINT('Ctrl Pts',(40.3499285956304,-61.2621251782863,
12.));
#125101=CARTESIAN_POINT('Ctrl Pts',(40.3450600983109,-61.2362714797899,
0.));
#125102=CARTESIAN_POINT('Ctrl Pts',(40.3450600983109,-61.2362714797899,
12.));
#125103=CARTESIAN_POINT('Ctrl Pts',(40.340174554537,-61.2104592029377,0.));
#125104=CARTESIAN_POINT('Ctrl Pts',(40.340174554537,-61.2104592029377,12.));
#125105=CARTESIAN_POINT('Ctrl Pts',(40.335272031637,-61.1846884324643,0.));
#125106=CARTESIAN_POINT('Ctrl Pts',(40.335272031637,-61.1846884324643,12.));
#125107=CARTESIAN_POINT('Ctrl Pts',(40.3303525972616,-61.1589592533613,
0.));
#125108=CARTESIAN_POINT('Ctrl Pts',(40.3303525972616,-61.1589592533613,
12.));
#125109=CARTESIAN_POINT('Ctrl Pts',(40.32541631938,-61.1332717508789,0.));
#125110=CARTESIAN_POINT('Ctrl Pts',(40.32541631938,-61.1332717508789,12.));
#125111=CARTESIAN_POINT('Ctrl Pts',(40.3204632662726,-61.1076260105258,
0.));
#125112=CARTESIAN_POINT('Ctrl Pts',(40.3204632662726,-61.1076260105258,
12.));
#125113=CARTESIAN_POINT('Ctrl Pts',(40.3154935065262,-61.0820221180645,
0.));
#125114=CARTESIAN_POINT('Ctrl Pts',(40.3154935065262,-61.0820221180645,
12.));
#125115=CARTESIAN_POINT('Ctrl Pts',(40.310507109031,-61.056460159505,0.));
#125116=CARTESIAN_POINT('Ctrl Pts',(40.310507109031,-61.056460159505,12.));
#125117=CARTESIAN_POINT('Ctrl Pts',(40.3055041429775,-61.0309402210921,
0.));
#125118=CARTESIAN_POINT('Ctrl Pts',(40.3055041429775,-61.0309402210921,
12.));
#125119=CARTESIAN_POINT('Ctrl Pts',(40.300484677858,-61.0054623893066,0.));
#125120=CARTESIAN_POINT('Ctrl Pts',(40.300484677858,-61.0054623893066,12.));
#125121=CARTESIAN_POINT('Ctrl Pts',(40.295448783469,-60.9800267508786,0.));
#125122=CARTESIAN_POINT('Ctrl Pts',(40.295448783469,-60.9800267508786,12.));
#125123=CARTESIAN_POINT('Ctrl Pts',(40.2903965299155,-60.954633392792,0.));
#125124=CARTESIAN_POINT('Ctrl Pts',(40.2903965299155,-60.954633392792,12.));
#125125=CARTESIAN_POINT('Ctrl Pts',(40.2853279876161,-60.9292824022887,
0.));
#125126=CARTESIAN_POINT('Ctrl Pts',(40.2853279876161,-60.9292824022887,
12.));
#125127=CARTESIAN_POINT('Ctrl Pts',(40.2802432273105,-60.9039738668668,
0.));
#125128=CARTESIAN_POINT('Ctrl Pts',(40.2802432273105,-60.9039738668668,
12.));
#125129=CARTESIAN_POINT('Ctrl Pts',(40.2751423200639,-60.8787078742818,
0.));
#125130=CARTESIAN_POINT('Ctrl Pts',(40.2751423200639,-60.8787078742818,
12.));
#125131=CARTESIAN_POINT('Ctrl Pts',(40.2700253372648,-60.8534845125538,
0.));
#125132=CARTESIAN_POINT('Ctrl Pts',(40.2700253372648,-60.8534845125538,
12.));
#125133=CARTESIAN_POINT('Ctrl Pts',(40.2648923506248,-60.8283038699706,
0.));
#125134=CARTESIAN_POINT('Ctrl Pts',(40.2648923506248,-60.8283038699706,
12.));
#125135=CARTESIAN_POINT('Ctrl Pts',(40.2597434321803,-60.8031660350879,
0.));
#125136=CARTESIAN_POINT('Ctrl Pts',(40.2597434321803,-60.8031660350879,
12.));
#125137=CARTESIAN_POINT('Ctrl Pts',(40.2545786542953,-60.7780710967248,
0.));
#125138=CARTESIAN_POINT('Ctrl Pts',(40.2545786542953,-60.7780710967248,
12.));
#125139=CARTESIAN_POINT('Ctrl Pts',(40.2493980896638,-60.7530191439593,
0.));
#125140=CARTESIAN_POINT('Ctrl Pts',(40.2493980896638,-60.7530191439593,
12.));
#125141=CARTESIAN_POINT('Ctrl Pts',(40.2442018113108,-60.728010266139,0.));
#125142=CARTESIAN_POINT('Ctrl Pts',(40.2442018113108,-60.728010266139,12.));
#125143=CARTESIAN_POINT('Ctrl Pts',(40.2389898925932,-60.7030445528857,
0.));
#125144=CARTESIAN_POINT('Ctrl Pts',(40.2389898925932,-60.7030445528857,
12.));
#125145=CARTESIAN_POINT('Ctrl Pts',(40.2337624072029,-60.678122094098,0.));
#125146=CARTESIAN_POINT('Ctrl Pts',(40.2337624072029,-60.678122094098,12.));
#125147=CARTESIAN_POINT('Ctrl Pts',(40.2285194291706,-60.6532429799499,
0.));
#125148=CARTESIAN_POINT('Ctrl Pts',(40.2285194291706,-60.6532429799499,
12.));
#125149=CARTESIAN_POINT('Ctrl Pts',(40.2232610328721,-60.6284073008871,
0.));
#125150=CARTESIAN_POINT('Ctrl Pts',(40.2232610328721,-60.6284073008871,
12.));
#125151=CARTESIAN_POINT('Ctrl Pts',(40.2179872930273,-60.6036151476349,
0.));
#125152=CARTESIAN_POINT('Ctrl Pts',(40.2179872930273,-60.6036151476349,
12.));
#125153=CARTESIAN_POINT('Ctrl Pts',(40.2126982847011,-60.5788666112042,
0.));
#125154=CARTESIAN_POINT('Ctrl Pts',(40.2126982847011,-60.5788666112042,
12.));
#125155=CARTESIAN_POINT('Ctrl Pts',(40.2073940833053,-60.5541617828925,
0.));
#125156=CARTESIAN_POINT('Ctrl Pts',(40.2073940833053,-60.5541617828925,
12.));
#125157=CARTESIAN_POINT('Ctrl Pts',(40.2020747646014,-60.5295007542841,
0.));
#125158=CARTESIAN_POINT('Ctrl Pts',(40.2020747646014,-60.5295007542841,
12.));
#125159=CARTESIAN_POINT('Ctrl Pts',(40.1967404047062,-60.5048836172435,
0.));
#125160=CARTESIAN_POINT('Ctrl Pts',(40.1967404047062,-60.5048836172435,
12.));
#125161=CARTESIAN_POINT('Ctrl Pts',(40.1913910800921,-60.4803104639225,
0.));
#125162=CARTESIAN_POINT('Ctrl Pts',(40.1913910800921,-60.4803104639225,
12.));
#125163=CARTESIAN_POINT('Ctrl Pts',(40.1860268675884,-60.455781386769,0.));
#125164=CARTESIAN_POINT('Ctrl Pts',(40.1860268675884,-60.455781386769,12.));
#125165=CARTESIAN_POINT('Ctrl Pts',(40.180647844383,-60.4312964785273,0.));
#125166=CARTESIAN_POINT('Ctrl Pts',(40.180647844383,-60.4312964785273,12.));
#125167=CARTESIAN_POINT('Ctrl Pts',(40.1752540880268,-60.4068558322407,
0.));
#125168=CARTESIAN_POINT('Ctrl Pts',(40.1752540880268,-60.4068558322407,
12.));
#125169=CARTESIAN_POINT('Ctrl Pts',(40.1698456764377,-60.3824595412445,
0.));
#125170=CARTESIAN_POINT('Ctrl Pts',(40.1698456764377,-60.3824595412445,
12.));
#125171=CARTESIAN_POINT('Ctrl Pts',(40.1644226879033,-60.3581076991716,
0.));
#125172=CARTESIAN_POINT('Ctrl Pts',(40.1644226879033,-60.3581076991716,
12.));
#125173=CARTESIAN_POINT('Ctrl Pts',(40.1589852010804,-60.3338003999606,
0.));
#125174=CARTESIAN_POINT('Ctrl Pts',(40.1589852010804,-60.3338003999606,
12.));
#125175=CARTESIAN_POINT('Ctrl Pts',(40.1535332949976,-60.3095377378586,
0.));
#125176=CARTESIAN_POINT('Ctrl Pts',(40.1535332949976,-60.3095377378586,
12.));
#125177=CARTESIAN_POINT('Ctrl Pts',(40.1480670490586,-60.285319807422,0.));
#125178=CARTESIAN_POINT('Ctrl Pts',(40.1480670490586,-60.285319807422,12.));
#125179=CARTESIAN_POINT('Ctrl Pts',(40.1425865430472,-60.2611467035116,
0.));
#125180=CARTESIAN_POINT('Ctrl Pts',(40.1425865430472,-60.2611467035116,
12.));
#125181=CARTESIAN_POINT('Ctrl Pts',(40.1370918571305,-60.2370185212964,
0.));
#125182=CARTESIAN_POINT('Ctrl Pts',(40.1370918571305,-60.2370185212964,
12.));
#125183=CARTESIAN_POINT('Ctrl Pts',(40.1315830718577,-60.2129353562622,
0.));
#125184=CARTESIAN_POINT('Ctrl Pts',(40.1315830718577,-60.2129353562622,
12.));
#125185=CARTESIAN_POINT('Ctrl Pts',(40.1260602681644,-60.1888973042152,
0.));
#125186=CARTESIAN_POINT('Ctrl Pts',(40.1260602681644,-60.1888973042152,
12.));
#125187=CARTESIAN_POINT('Ctrl Pts',(40.120523527374,-60.1649044612828,0.));
#125188=CARTESIAN_POINT('Ctrl Pts',(40.120523527374,-60.1649044612828,12.));
#125189=CARTESIAN_POINT('Ctrl Pts',(40.1149729312036,-60.1409569239092,
0.));
#125190=CARTESIAN_POINT('Ctrl Pts',(40.1149729312036,-60.1409569239092,
12.));
#125191=CARTESIAN_POINT('Ctrl Pts',(40.1094085617674,-60.1170547888574,
0.));
#125192=CARTESIAN_POINT('Ctrl Pts',(40.1094085617674,-60.1170547888574,
12.));
#125193=CARTESIAN_POINT('Ctrl Pts',(40.1038305015766,-60.0931981532197,
0.));
#125194=CARTESIAN_POINT('Ctrl Pts',(40.1038305015766,-60.0931981532197,
12.));
#125195=CARTESIAN_POINT('Ctrl Pts',(40.0982388335423,-60.069387114421,0.));
#125196=CARTESIAN_POINT('Ctrl Pts',(40.0982388335423,-60.069387114421,12.));
#125197=CARTESIAN_POINT('Ctrl Pts',(40.0926336409785,-60.0456217702201,
0.));
#125198=CARTESIAN_POINT('Ctrl Pts',(40.0926336409785,-60.0456217702201,
12.));
#125199=CARTESIAN_POINT('Ctrl Pts',(40.0870150076074,-60.021902218706,0.));
#125200=CARTESIAN_POINT('Ctrl Pts',(40.0870150076074,-60.021902218706,12.));
#125201=CARTESIAN_POINT('Ctrl Pts',(40.0813830175623,-59.9982285582983,
0.));
#125202=CARTESIAN_POINT('Ctrl Pts',(40.0813830175623,-59.9982285582983,
12.));
#125203=CARTESIAN_POINT('Ctrl Pts',(40.0757377553888,-59.9746008877584,
0.));
#125204=CARTESIAN_POINT('Ctrl Pts',(40.0757377553888,-59.9746008877584,
12.));
#125205=CARTESIAN_POINT('Ctrl Pts',(40.0700793060473,-59.9510193061927,
0.));
#125206=CARTESIAN_POINT('Ctrl Pts',(40.0700793060473,-59.9510193061927,
12.));
#125207=CARTESIAN_POINT('Ctrl Pts',(40.064407754916,-59.9274839130553,0.));
#125208=CARTESIAN_POINT('Ctrl Pts',(40.064407754916,-59.9274839130553,12.));
#125209=CARTESIAN_POINT('Ctrl Pts',(40.0587231877962,-59.9039948081432,
0.));
#125210=CARTESIAN_POINT('Ctrl Pts',(40.0587231877962,-59.9039948081432,
12.));
#125211=CARTESIAN_POINT('Ctrl Pts',(40.0530256909162,-59.8805520915975,
0.));
#125212=CARTESIAN_POINT('Ctrl Pts',(40.0530256909162,-59.8805520915975,
12.));
#125213=CARTESIAN_POINT('Ctrl Pts',(40.0473153509323,-59.8571558639144,
0.));
#125214=CARTESIAN_POINT('Ctrl Pts',(40.0473153509323,-59.8571558639144,
12.));
#125215=CARTESIAN_POINT('Ctrl Pts',(40.0415922549313,-59.8338062259491,
0.));
#125216=CARTESIAN_POINT('Ctrl Pts',(40.0415922549313,-59.8338062259491,
12.));
#125217=CARTESIAN_POINT('Ctrl Pts',(40.035856490434,-59.8105032789179,0.));
#125218=CARTESIAN_POINT('Ctrl Pts',(40.035856490434,-59.8105032789179,12.));
#125219=CARTESIAN_POINT('Ctrl Pts',(40.0301081454006,-59.7872471243948,
0.));
#125220=CARTESIAN_POINT('Ctrl Pts',(40.0301081454006,-59.7872471243948,
12.));
#125221=CARTESIAN_POINT('Ctrl Pts',(40.0243473082343,-59.7640378643114,
0.));
#125222=CARTESIAN_POINT('Ctrl Pts',(40.0243473082343,-59.7640378643114,
12.));
#125223=CARTESIAN_POINT('Ctrl Pts',(40.0185740677827,-59.7408756009688,
0.));
#125224=CARTESIAN_POINT('Ctrl Pts',(40.0185740677827,-59.7408756009688,
12.));
#125225=CARTESIAN_POINT('Ctrl Pts',(40.0127885133407,-59.7177604370409,
0.));
#125226=CARTESIAN_POINT('Ctrl Pts',(40.0127885133407,-59.7177604370409,
12.));
#125227=CARTESIAN_POINT('Ctrl Pts',(40.0069907346536,-59.6946924755771,
0.));
#125228=CARTESIAN_POINT('Ctrl Pts',(40.0069907346536,-59.6946924755771,
12.));
#125229=CARTESIAN_POINT('Ctrl Pts',(40.0011808219231,-59.671671819999,0.));
#125230=CARTESIAN_POINT('Ctrl Pts',(40.0011808219231,-59.671671819999,12.));
#125231=CARTESIAN_POINT('Ctrl Pts',(39.9953588658115,-59.6486985741015,
0.));
#125232=CARTESIAN_POINT('Ctrl Pts',(39.9953588658115,-59.6486985741015,
12.));
#125233=CARTESIAN_POINT('Ctrl Pts',(39.9895249574432,-59.6257728420644,
0.));
#125234=CARTESIAN_POINT('Ctrl Pts',(39.9895249574432,-59.6257728420644,
12.));
#125235=CARTESIAN_POINT('Ctrl Pts',(39.9836791884072,-59.6028947284551,
0.));
#125236=CARTESIAN_POINT('Ctrl Pts',(39.9836791884072,-59.6028947284551,
12.));
#125237=CARTESIAN_POINT('Ctrl Pts',(39.9778216507609,-59.5800643382322,
0.));
#125238=CARTESIAN_POINT('Ctrl Pts',(39.9778216507609,-59.5800643382322,
12.));
#125239=CARTESIAN_POINT('Ctrl Pts',(39.971952437036,-59.5572817767412,0.));
#125240=CARTESIAN_POINT('Ctrl Pts',(39.971952437036,-59.5572817767412,12.));
#125241=CARTESIAN_POINT('Ctrl Pts',(39.9660716402423,-59.5345471497162,
0.));
#125242=CARTESIAN_POINT('Ctrl Pts',(39.9660716402423,-59.5345471497162,
12.));
#125243=CARTESIAN_POINT('Ctrl Pts',(39.96017935387,-59.5118605632919,0.));
#125244=CARTESIAN_POINT('Ctrl Pts',(39.96017935387,-59.5118605632919,12.));
#125245=CARTESIAN_POINT('Ctrl Pts',(39.954275671893,-59.4892221240081,0.));
#125246=CARTESIAN_POINT('Ctrl Pts',(39.954275671893,-59.4892221240081,12.));
#125247=CARTESIAN_POINT('Ctrl Pts',(39.9483606887731,-59.4666319388123,
0.));
#125248=CARTESIAN_POINT('Ctrl Pts',(39.9483606887731,-59.4666319388123,
12.));
#125249=CARTESIAN_POINT('Ctrl Pts',(39.9424344994652,-59.444090115055,0.));
#125250=CARTESIAN_POINT('Ctrl Pts',(39.9424344994652,-59.444090115055,12.));
#125251=CARTESIAN_POINT('Ctrl Pts',(39.9364971994215,-59.4215967604925,
0.));
#125252=CARTESIAN_POINT('Ctrl Pts',(39.9364971994215,-59.4215967604925,
12.));
#125253=CARTESIAN_POINT('Ctrl Pts',(39.9305488845934,-59.3991519832981,
0.));
#125254=CARTESIAN_POINT('Ctrl Pts',(39.9305488845934,-59.3991519832981,
12.));
#125255=CARTESIAN_POINT('Ctrl Pts',(39.9245896514359,-59.3767558920663,
0.));
#125256=CARTESIAN_POINT('Ctrl Pts',(39.9245896514359,-59.3767558920663,
12.));
#125257=CARTESIAN_POINT('Ctrl Pts',(39.9186195969113,-59.3544085958165,
0.));
#125258=CARTESIAN_POINT('Ctrl Pts',(39.9186195969113,-59.3544085958165,
12.));
#125259=CARTESIAN_POINT('Ctrl Pts',(39.9126388184956,-59.3321102039883,
0.));
#125260=CARTESIAN_POINT('Ctrl Pts',(39.9126388184956,-59.3321102039883,
12.));
#125261=CARTESIAN_POINT('Ctrl Pts',(39.9066474141826,-59.3098608264452,
0.));
#125262=CARTESIAN_POINT('Ctrl Pts',(39.9066474141826,-59.3098608264452,
12.));
#125263=CARTESIAN_POINT('Ctrl Pts',(39.9006454824861,-59.287660573487,0.));
#125264=CARTESIAN_POINT('Ctrl Pts',(39.9006454824861,-59.287660573487,12.));
#125265=CARTESIAN_POINT('Ctrl Pts',(39.8946331224442,-59.2655095558527,
0.));
#125266=CARTESIAN_POINT('Ctrl Pts',(39.8946331224442,-59.2655095558527,
12.));
#125267=CARTESIAN_POINT('Ctrl Pts',(39.8886104336234,-59.2434078847236,
0.));
#125268=CARTESIAN_POINT('Ctrl Pts',(39.8886104336234,-59.2434078847236,
12.));
#125269=CARTESIAN_POINT('Ctrl Pts',(39.8825775161253,-59.2213556717188,
0.));
#125270=CARTESIAN_POINT('Ctrl Pts',(39.8825775161253,-59.2213556717188,
12.));
#125271=CARTESIAN_POINT('Ctrl Pts',(39.8765344705895,-59.1993530289008,
0.));
#125272=CARTESIAN_POINT('Ctrl Pts',(39.8765344705895,-59.1993530289008,
12.));
#125273=CARTESIAN_POINT('Ctrl Pts',(39.8704813981978,-59.1774000687865,
0.));
#125274=CARTESIAN_POINT('Ctrl Pts',(39.8704813981978,-59.1774000687865,
12.));
#125275=CARTESIAN_POINT('Ctrl Pts',(39.8644184006785,-59.155496904352,0.));
#125276=CARTESIAN_POINT('Ctrl Pts',(39.8644184006785,-59.155496904352,12.));
#125277=CARTESIAN_POINT('Ctrl Pts',(39.8583455803111,-59.133643649035,0.));
#125278=CARTESIAN_POINT('Ctrl Pts',(39.8583455803111,-59.133643649035,12.));
#125279=CARTESIAN_POINT('Ctrl Pts',(39.8522630399337,-59.1118404167304,
0.));
#125280=CARTESIAN_POINT('Ctrl Pts',(39.8522630399337,-59.1118404167304,
12.));
#125281=CARTESIAN_POINT('Ctrl Pts',(39.8461708829465,-59.0900873217992,
0.));
#125282=CARTESIAN_POINT('Ctrl Pts',(39.8461708829465,-59.0900873217992,
12.));
#125283=CARTESIAN_POINT('Ctrl Pts',(39.8400692133143,-59.068384479077,0.));
#125284=CARTESIAN_POINT('Ctrl Pts',(39.8400692133143,-59.068384479077,12.));
#125285=CARTESIAN_POINT('Ctrl Pts',(39.8339581355715,-59.0467320038782,
0.));
#125286=CARTESIAN_POINT('Ctrl Pts',(39.8339581355715,-59.0467320038782,
12.));
#125287=CARTESIAN_POINT('Ctrl Pts',(39.8278377548261,-59.0251300119972,
0.));
#125288=CARTESIAN_POINT('Ctrl Pts',(39.8278377548261,-59.0251300119972,
12.));
#125289=CARTESIAN_POINT('Ctrl Pts',(39.8217081767658,-59.0035786197024,
0.));
#125290=CARTESIAN_POINT('Ctrl Pts',(39.8217081767658,-59.0035786197024,
12.));
#125291=CARTESIAN_POINT('Ctrl Pts',(39.8155695076625,-58.9820779437485,
0.));
#125292=CARTESIAN_POINT('Ctrl Pts',(39.8155695076625,-58.9820779437485,
12.));
#125293=CARTESIAN_POINT('Ctrl Pts',(39.8094218543781,-58.9606281013875,
0.));
#125294=CARTESIAN_POINT('Ctrl Pts',(39.8094218543781,-58.9606281013875,
12.));
#125295=CARTESIAN_POINT('Ctrl Pts',(39.8032653243712,-58.9392292103747,
0.));
#125296=CARTESIAN_POINT('Ctrl Pts',(39.8032653243712,-58.9392292103747,
12.));
#125297=CARTESIAN_POINT('Ctrl Pts',(39.7971000257044,-58.9178813889703,
0.));
#125298=CARTESIAN_POINT('Ctrl Pts',(39.7971000257044,-58.9178813889703,
12.));
#125299=CARTESIAN_POINT('Ctrl Pts',(39.7909260670517,-58.8965847559389,
0.));
#125300=CARTESIAN_POINT('Ctrl Pts',(39.7909260670517,-58.8965847559389,
12.));
#125301=CARTESIAN_POINT('Ctrl Pts',(39.7847435576996,-58.8753394305583,
0.));
#125302=CARTESIAN_POINT('Ctrl Pts',(39.7847435576996,-58.8753394305583,
12.));
#125303=CARTESIAN_POINT('Ctrl Pts',(39.7785526075477,-58.8541455326229,
0.));
#125304=CARTESIAN_POINT('Ctrl Pts',(39.7785526075477,-58.8541455326229,
12.));
#125305=CARTESIAN_POINT('Ctrl Pts',(39.772353327112,-58.8330031824453,0.));
#125306=CARTESIAN_POINT('Ctrl Pts',(39.772353327112,-58.8330031824453,12.));
#125307=CARTESIAN_POINT('Ctrl Pts',(39.7661458275276,-58.8119125008521,
0.));
#125308=CARTESIAN_POINT('Ctrl Pts',(39.7661458275276,-58.8119125008521,
12.));
#125309=CARTESIAN_POINT('Ctrl Pts',(39.7599302205527,-58.7908736091808,
0.));
#125310=CARTESIAN_POINT('Ctrl Pts',(39.7599302205527,-58.7908736091808,
12.));
#125311=CARTESIAN_POINT('Ctrl Pts',(39.753706618582,-58.769886629304,0.));
#125312=CARTESIAN_POINT('Ctrl Pts',(39.753706618582,-58.769886629304,12.));
#125313=CARTESIAN_POINT('Ctrl Pts',(39.7474751346603,-58.7489516836452,
0.));
#125314=CARTESIAN_POINT('Ctrl Pts',(39.7474751346603,-58.7489516836452,
12.));
#125315=CARTESIAN_POINT('Ctrl Pts',(39.741235882495,-58.7280688951911,0.));
#125316=CARTESIAN_POINT('Ctrl Pts',(39.741235882495,-58.7280688951911,12.));
#125317=CARTESIAN_POINT('Ctrl Pts',(39.7349889764737,-58.7072383875009,
0.));
#125318=CARTESIAN_POINT('Ctrl Pts',(39.7349889764737,-58.7072383875009,
12.));
#125319=CARTESIAN_POINT('Ctrl Pts',(39.7287345316664,-58.6864602847064,
0.));
#125320=CARTESIAN_POINT('Ctrl Pts',(39.7287345316664,-58.6864602847064,
12.));
#125321=CARTESIAN_POINT('Ctrl Pts',(39.7224726638087,-58.6657347115014,
0.));
#125322=CARTESIAN_POINT('Ctrl Pts',(39.7224726638087,-58.6657347115014,
12.));
#125323=CARTESIAN_POINT('Ctrl Pts',(39.7162034892896,-58.6450617931269,
0.));
#125324=CARTESIAN_POINT('Ctrl Pts',(39.7162034892896,-58.6450617931269,
12.));
#125325=CARTESIAN_POINT('Ctrl Pts',(39.7099271251421,-58.6244416553574,
0.));
#125326=CARTESIAN_POINT('Ctrl Pts',(39.7099271251421,-58.6244416553574,
12.));
#125327=CARTESIAN_POINT('Ctrl Pts',(39.7036436890248,-58.6038744244683,
0.));
#125328=CARTESIAN_POINT('Ctrl Pts',(39.7036436890248,-58.6038744244683,
12.));
#125329=CARTESIAN_POINT('Ctrl Pts',(39.6973532992555,-58.5833602272767,
0.));
#125330=CARTESIAN_POINT('Ctrl Pts',(39.6973532992555,-58.5833602272767,
12.));
#125331=CARTESIAN_POINT('Ctrl Pts',(39.6910560748639,-58.5628991912067,
0.));
#125332=CARTESIAN_POINT('Ctrl Pts',(39.6910560748639,-58.5628991912067,
12.));
#125333=CARTESIAN_POINT('Ctrl Pts',(39.6847521356395,-58.5424914443415,
0.));
#125334=CARTESIAN_POINT('Ctrl Pts',(39.6847521356395,-58.5424914443415,
12.));
#125335=CARTESIAN_POINT('Ctrl Pts',(39.6784416021817,-58.5221371154748,
0.));
#125336=CARTESIAN_POINT('Ctrl Pts',(39.6784416021817,-58.5221371154748,
12.));
#125337=CARTESIAN_POINT('Ctrl Pts',(39.6721245959516,-58.5018363341582,
0.));
#125338=CARTESIAN_POINT('Ctrl Pts',(39.6721245959516,-58.5018363341582,
12.));
#125339=CARTESIAN_POINT('Ctrl Pts',(39.66580123918,-58.4815892306044,0.));
#125340=CARTESIAN_POINT('Ctrl Pts',(39.66580123918,-58.4815892306044,12.));
#125341=CARTESIAN_POINT('Ctrl Pts',(39.6594716547681,-58.4613959355776,
0.));
#125342=CARTESIAN_POINT('Ctrl Pts',(39.6594716547681,-58.4613959355776,
12.));
#125343=CARTESIAN_POINT('Ctrl Pts',(39.6531359662043,-58.4412565802984,
0.));
#125344=CARTESIAN_POINT('Ctrl Pts',(39.6531359662043,-58.4412565802984,
12.));
#125345=CARTESIAN_POINT('Ctrl Pts',(39.6467942974465,-58.4211712963023,
0.));
#125346=CARTESIAN_POINT('Ctrl Pts',(39.6467942974465,-58.4211712963023,
12.));
#125347=CARTESIAN_POINT('Ctrl Pts',(39.6404467729114,-58.4011402154225,
0.));
#125348=CARTESIAN_POINT('Ctrl Pts',(39.6404467729114,-58.4011402154225,
12.));
#125349=CARTESIAN_POINT('Ctrl Pts',(39.6340935177492,-58.3811634701061,
0.));
#125350=CARTESIAN_POINT('Ctrl Pts',(39.6340935177492,-58.3811634701061,
12.));
#125351=CARTESIAN_POINT('Ctrl Pts',(39.6277346580898,-58.3612411936914,
0.));
#125352=CARTESIAN_POINT('Ctrl Pts',(39.6277346580898,-58.3612411936914,
12.));
#125353=CARTESIAN_POINT('Ctrl Pts',(39.6213703212523,-58.3413735206412,
0.));
#125354=CARTESIAN_POINT('Ctrl Pts',(39.6213703212523,-58.3413735206412,
12.));
#125355=CARTESIAN_POINT('Ctrl Pts',(39.6150006360894,-58.3215605869192,
0.));
#125356=CARTESIAN_POINT('Ctrl Pts',(39.6150006360894,-58.3215605869192,
12.));
#125357=CARTESIAN_POINT('Ctrl Pts',(39.6086257327559,-58.3018025297288,
0.));
#125358=CARTESIAN_POINT('Ctrl Pts',(39.6086257327559,-58.3018025297288,
12.));
#125359=CARTESIAN_POINT('Ctrl Pts',(39.6022457420772,-58.2820994868092,
0.));
#125360=CARTESIAN_POINT('Ctrl Pts',(39.6022457420772,-58.2820994868092,
12.));
#125361=CARTESIAN_POINT('Ctrl Pts',(39.5958607950237,-58.2624515958416,
0.));
#125362=CARTESIAN_POINT('Ctrl Pts',(39.5958607950237,-58.2624515958416,
12.));
#125363=CARTESIAN_POINT('Ctrl Pts',(39.589471022173,-58.2428589938394,0.));
#125364=CARTESIAN_POINT('Ctrl Pts',(39.589471022173,-58.2428589938394,12.));
#125365=CARTESIAN_POINT('Ctrl Pts',(39.5830765530919,-58.2233218164407,
0.));
#125366=CARTESIAN_POINT('Ctrl Pts',(39.5830765530919,-58.2233218164407,
12.));
#125367=CARTESIAN_POINT('Ctrl Pts',(39.5766775175226,-58.2038401992496,
0.));
#125368=CARTESIAN_POINT('Ctrl Pts',(39.5766775175226,-58.2038401992496,
12.));
#125369=CARTESIAN_POINT('Ctrl Pts',(39.5702740468013,-58.1844142794359,
0.));
#125370=CARTESIAN_POINT('Ctrl Pts',(39.5702740468013,-58.1844142794359,
12.));
#125371=CARTESIAN_POINT('Ctrl Pts',(39.5638662750174,-58.1650441970378,
0.));
#125372=CARTESIAN_POINT('Ctrl Pts',(39.5638662750174,-58.1650441970378,
12.));
#125373=CARTESIAN_POINT('Ctrl Pts',(39.5574543406959,-58.1457300968466,
0.));
#125374=CARTESIAN_POINT('Ctrl Pts',(39.5574543406959,-58.1457300968466,
12.));
#125375=CARTESIAN_POINT('Ctrl Pts',(39.5510383869476,-58.1264721285697,
0.));
#125376=CARTESIAN_POINT('Ctrl Pts',(39.5510383869476,-58.1264721285697,
12.));
#125377=CARTESIAN_POINT('Ctrl Pts',(39.5446185579615,-58.1072704428895,
0.));
#125378=CARTESIAN_POINT('Ctrl Pts',(39.5446185579615,-58.1072704428895,
12.));
#125379=CARTESIAN_POINT('Ctrl Pts',(39.5381949959214,-58.088125187991,0.));
#125380=CARTESIAN_POINT('Ctrl Pts',(39.5381949959214,-58.088125187991,12.));
#125381=CARTESIAN_POINT('Ctrl Pts',(39.5317678383231,-58.0690365065393,
0.));
#125382=CARTESIAN_POINT('Ctrl Pts',(39.5317678383231,-58.0690365065393,
12.));
#125383=CARTESIAN_POINT('Ctrl Pts',(39.5253372136921,-58.0500045308459,
0.));
#125384=CARTESIAN_POINT('Ctrl Pts',(39.5253372136921,-58.0500045308459,
12.));
#125385=CARTESIAN_POINT('Ctrl Pts',(39.5189032457227,-58.0310293875321,
0.));
#125386=CARTESIAN_POINT('Ctrl Pts',(39.5189032457227,-58.0310293875321,
12.));
#125387=CARTESIAN_POINT('Ctrl Pts',(39.5124660615009,-58.012111206794,0.));
#125388=CARTESIAN_POINT('Ctrl Pts',(39.5124660615009,-58.012111206794,12.));
#125389=CARTESIAN_POINT('Ctrl Pts',(39.5060257981225,-57.9932501298522,
0.));
#125390=CARTESIAN_POINT('Ctrl Pts',(39.5060257981225,-57.9932501298522,
12.));
#125391=CARTESIAN_POINT('Ctrl Pts',(39.4995826106692,-57.9744463179305,
0.));
#125392=CARTESIAN_POINT('Ctrl Pts',(39.4995826106692,-57.9744463179305,
12.));
#125393=CARTESIAN_POINT('Ctrl Pts',(39.4931366776628,-57.9556999583777,
0.));
#125394=CARTESIAN_POINT('Ctrl Pts',(39.4931366776628,-57.9556999583777,
12.));
#125395=CARTESIAN_POINT('Ctrl Pts',(39.4866881842223,-57.9370112456506,
0.));
#125396=CARTESIAN_POINT('Ctrl Pts',(39.4866881842223,-57.9370112456506,
12.));
#125397=CARTESIAN_POINT('Ctrl Pts',(39.4802373061008,-57.9183803632337,
0.));
#125398=CARTESIAN_POINT('Ctrl Pts',(39.4802373061008,-57.9183803632337,
12.));
#125399=CARTESIAN_POINT('Ctrl Pts',(39.4737841949417,-57.899807467054,0.));
#125400=CARTESIAN_POINT('Ctrl Pts',(39.4737841949417,-57.899807467054,12.));
#125401=CARTESIAN_POINT('Ctrl Pts',(39.4673289592425,-57.8812926637397,
0.));
#125402=CARTESIAN_POINT('Ctrl Pts',(39.4673289592425,-57.8812926637397,
12.));
#125403=CARTESIAN_POINT('Ctrl Pts',(39.4608716627367,-57.8628360097134,
0.));
#125404=CARTESIAN_POINT('Ctrl Pts',(39.4608716627367,-57.8628360097134,
12.));
#125405=CARTESIAN_POINT('Ctrl Pts',(39.4557042029884,-57.8481172247804,
0.));
#125406=CARTESIAN_POINT('Ctrl Pts',(39.4557042029884,-57.8481172247804,
12.));
#125407=CARTESIAN_POINT('Ctrl Pts',(39.45182770037,-57.8371043151606,0.));
#125408=CARTESIAN_POINT('Ctrl Pts',(39.45182770037,-57.8371043151606,12.));
#125409=CARTESIAN_POINT('Ctrl Pts',(39.4492429618498,-57.829774010102,0.));
#125410=CARTESIAN_POINT('Ctrl Pts',(39.4492429618498,-57.829774010102,12.));
#125411=CARTESIAN_POINT('Ctrl Pts',(39.4479504917287,-57.8261117662439,
0.));
#125412=CARTESIAN_POINT('Ctrl Pts',(39.4479504917287,-57.8261117662439,
12.));
#125413=CARTESIAN_POINT('',(39.4479504917287,-57.8261117662439,12.));
#125414=CARTESIAN_POINT('Ctrl Pts',(39.4479504917287,-57.8261117662439,
12.));
#125415=CARTESIAN_POINT('Ctrl Pts',(39.4492429618498,-57.829774010102,12.));
#125416=CARTESIAN_POINT('Ctrl Pts',(39.45182770037,-57.8371043151606,12.));
#125417=CARTESIAN_POINT('Ctrl Pts',(39.4557042029884,-57.8481172247804,
12.));
#125418=CARTESIAN_POINT('Ctrl Pts',(39.4608716627367,-57.8628360097134,
12.));
#125419=CARTESIAN_POINT('Ctrl Pts',(39.4673289592425,-57.8812926637397,
12.));
#125420=CARTESIAN_POINT('Ctrl Pts',(39.4737841949417,-57.899807467054,12.));
#125421=CARTESIAN_POINT('Ctrl Pts',(39.4802373061008,-57.9183803632337,
12.));
#125422=CARTESIAN_POINT('Ctrl Pts',(39.4866881842223,-57.9370112456506,
12.));
#125423=CARTESIAN_POINT('Ctrl Pts',(39.4931366776628,-57.9556999583777,
12.));
#125424=CARTESIAN_POINT('Ctrl Pts',(39.4995826106692,-57.9744463179305,
12.));
#125425=CARTESIAN_POINT('Ctrl Pts',(39.5060257981225,-57.9932501298522,
12.));
#125426=CARTESIAN_POINT('Ctrl Pts',(39.5124660615009,-58.012111206794,12.));
#125427=CARTESIAN_POINT('Ctrl Pts',(39.5189032457227,-58.0310293875321,
12.));
#125428=CARTESIAN_POINT('Ctrl Pts',(39.5253372136921,-58.0500045308459,
12.));
#125429=CARTESIAN_POINT('Ctrl Pts',(39.5317678383231,-58.0690365065393,
12.));
#125430=CARTESIAN_POINT('Ctrl Pts',(39.5381949959214,-58.088125187991,12.));
#125431=CARTESIAN_POINT('Ctrl Pts',(39.5446185579615,-58.1072704428895,
12.));
#125432=CARTESIAN_POINT('Ctrl Pts',(39.5510383869476,-58.1264721285697,
12.));
#125433=CARTESIAN_POINT('Ctrl Pts',(39.5574543406959,-58.1457300968466,
12.));
#125434=CARTESIAN_POINT('Ctrl Pts',(39.5638662750174,-58.1650441970378,
12.));
#125435=CARTESIAN_POINT('Ctrl Pts',(39.5702740468013,-58.1844142794359,
12.));
#125436=CARTESIAN_POINT('Ctrl Pts',(39.5766775175226,-58.2038401992496,
12.));
#125437=CARTESIAN_POINT('Ctrl Pts',(39.5830765530919,-58.2233218164407,
12.));
#125438=CARTESIAN_POINT('Ctrl Pts',(39.589471022173,-58.2428589938394,12.));
#125439=CARTESIAN_POINT('Ctrl Pts',(39.5958607950237,-58.2624515958416,
12.));
#125440=CARTESIAN_POINT('Ctrl Pts',(39.6022457420772,-58.2820994868092,
12.));
#125441=CARTESIAN_POINT('Ctrl Pts',(39.6086257327559,-58.3018025297288,
12.));
#125442=CARTESIAN_POINT('Ctrl Pts',(39.6150006360894,-58.3215605869192,
12.));
#125443=CARTESIAN_POINT('Ctrl Pts',(39.6213703212523,-58.3413735206412,
12.));
#125444=CARTESIAN_POINT('Ctrl Pts',(39.6277346580898,-58.3612411936914,
12.));
#125445=CARTESIAN_POINT('Ctrl Pts',(39.6340935177492,-58.3811634701061,
12.));
#125446=CARTESIAN_POINT('Ctrl Pts',(39.6404467729114,-58.4011402154225,
12.));
#125447=CARTESIAN_POINT('Ctrl Pts',(39.6467942974465,-58.4211712963023,
12.));
#125448=CARTESIAN_POINT('Ctrl Pts',(39.6531359662043,-58.4412565802984,
12.));
#125449=CARTESIAN_POINT('Ctrl Pts',(39.6594716547681,-58.4613959355776,
12.));
#125450=CARTESIAN_POINT('Ctrl Pts',(39.66580123918,-58.4815892306044,12.));
#125451=CARTESIAN_POINT('Ctrl Pts',(39.6721245959516,-58.5018363341582,
12.));
#125452=CARTESIAN_POINT('Ctrl Pts',(39.6784416021817,-58.5221371154748,
12.));
#125453=CARTESIAN_POINT('Ctrl Pts',(39.6847521356395,-58.5424914443415,
12.));
#125454=CARTESIAN_POINT('Ctrl Pts',(39.6910560748639,-58.5628991912067,
12.));
#125455=CARTESIAN_POINT('Ctrl Pts',(39.6973532992555,-58.5833602272767,
12.));
#125456=CARTESIAN_POINT('Ctrl Pts',(39.7036436890248,-58.6038744244683,
12.));
#125457=CARTESIAN_POINT('Ctrl Pts',(39.7099271251421,-58.6244416553574,
12.));
#125458=CARTESIAN_POINT('Ctrl Pts',(39.7162034892896,-58.6450617931269,
12.));
#125459=CARTESIAN_POINT('Ctrl Pts',(39.7224726638087,-58.6657347115014,
12.));
#125460=CARTESIAN_POINT('Ctrl Pts',(39.7287345316664,-58.6864602847064,
12.));
#125461=CARTESIAN_POINT('Ctrl Pts',(39.7349889764737,-58.7072383875009,
12.));
#125462=CARTESIAN_POINT('Ctrl Pts',(39.741235882495,-58.7280688951911,12.));
#125463=CARTESIAN_POINT('Ctrl Pts',(39.7474751346603,-58.7489516836452,
12.));
#125464=CARTESIAN_POINT('Ctrl Pts',(39.753706618582,-58.769886629304,12.));
#125465=CARTESIAN_POINT('Ctrl Pts',(39.7599302205527,-58.7908736091808,
12.));
#125466=CARTESIAN_POINT('Ctrl Pts',(39.7661458275276,-58.8119125008521,
12.));
#125467=CARTESIAN_POINT('Ctrl Pts',(39.772353327112,-58.8330031824453,12.));
#125468=CARTESIAN_POINT('Ctrl Pts',(39.7785526075477,-58.8541455326229,
12.));
#125469=CARTESIAN_POINT('Ctrl Pts',(39.7847435576996,-58.8753394305583,
12.));
#125470=CARTESIAN_POINT('Ctrl Pts',(39.7909260670517,-58.8965847559389,
12.));
#125471=CARTESIAN_POINT('Ctrl Pts',(39.7971000257044,-58.9178813889703,
12.));
#125472=CARTESIAN_POINT('Ctrl Pts',(39.8032653243712,-58.9392292103747,
12.));
#125473=CARTESIAN_POINT('Ctrl Pts',(39.8094218543781,-58.9606281013875,
12.));
#125474=CARTESIAN_POINT('Ctrl Pts',(39.8155695076625,-58.9820779437485,
12.));
#125475=CARTESIAN_POINT('Ctrl Pts',(39.8217081767658,-59.0035786197024,
12.));
#125476=CARTESIAN_POINT('Ctrl Pts',(39.8278377548261,-59.0251300119972,
12.));
#125477=CARTESIAN_POINT('Ctrl Pts',(39.8339581355715,-59.0467320038782,
12.));
#125478=CARTESIAN_POINT('Ctrl Pts',(39.8400692133143,-59.068384479077,12.));
#125479=CARTESIAN_POINT('Ctrl Pts',(39.8461708829465,-59.0900873217992,
12.));
#125480=CARTESIAN_POINT('Ctrl Pts',(39.8522630399337,-59.1118404167304,
12.));
#125481=CARTESIAN_POINT('Ctrl Pts',(39.8583455803111,-59.133643649035,12.));
#125482=CARTESIAN_POINT('Ctrl Pts',(39.8644184006785,-59.155496904352,12.));
#125483=CARTESIAN_POINT('Ctrl Pts',(39.8704813981978,-59.1774000687865,
12.));
#125484=CARTESIAN_POINT('Ctrl Pts',(39.8765344705895,-59.1993530289008,
12.));
#125485=CARTESIAN_POINT('Ctrl Pts',(39.8825775161253,-59.2213556717188,
12.));
#125486=CARTESIAN_POINT('Ctrl Pts',(39.8886104336234,-59.2434078847236,
12.));
#125487=CARTESIAN_POINT('Ctrl Pts',(39.8946331224442,-59.2655095558527,
12.));
#125488=CARTESIAN_POINT('Ctrl Pts',(39.9006454824861,-59.287660573487,12.));
#125489=CARTESIAN_POINT('Ctrl Pts',(39.9066474141826,-59.3098608264452,
12.));
#125490=CARTESIAN_POINT('Ctrl Pts',(39.9126388184956,-59.3321102039883,
12.));
#125491=CARTESIAN_POINT('Ctrl Pts',(39.9186195969113,-59.3544085958165,
12.));
#125492=CARTESIAN_POINT('Ctrl Pts',(39.9245896514359,-59.3767558920663,
12.));
#125493=CARTESIAN_POINT('Ctrl Pts',(39.9305488845934,-59.3991519832981,
12.));
#125494=CARTESIAN_POINT('Ctrl Pts',(39.9364971994215,-59.4215967604925,
12.));
#125495=CARTESIAN_POINT('Ctrl Pts',(39.9424344994652,-59.444090115055,12.));
#125496=CARTESIAN_POINT('Ctrl Pts',(39.9483606887731,-59.4666319388123,
12.));
#125497=CARTESIAN_POINT('Ctrl Pts',(39.954275671893,-59.4892221240081,12.));
#125498=CARTESIAN_POINT('Ctrl Pts',(39.96017935387,-59.5118605632919,12.));
#125499=CARTESIAN_POINT('Ctrl Pts',(39.9660716402423,-59.5345471497162,
12.));
#125500=CARTESIAN_POINT('Ctrl Pts',(39.971952437036,-59.5572817767412,12.));
#125501=CARTESIAN_POINT('Ctrl Pts',(39.9778216507609,-59.5800643382322,
12.));
#125502=CARTESIAN_POINT('Ctrl Pts',(39.9836791884072,-59.6028947284551,
12.));
#125503=CARTESIAN_POINT('Ctrl Pts',(39.9895249574432,-59.6257728420644,
12.));
#125504=CARTESIAN_POINT('Ctrl Pts',(39.9953588658115,-59.6486985741015,
12.));
#125505=CARTESIAN_POINT('Ctrl Pts',(40.0011808219231,-59.671671819999,12.));
#125506=CARTESIAN_POINT('Ctrl Pts',(40.0069907346536,-59.6946924755771,
12.));
#125507=CARTESIAN_POINT('Ctrl Pts',(40.0127885133407,-59.7177604370409,
12.));
#125508=CARTESIAN_POINT('Ctrl Pts',(40.0185740677827,-59.7408756009688,
12.));
#125509=CARTESIAN_POINT('Ctrl Pts',(40.0243473082343,-59.7640378643114,
12.));
#125510=CARTESIAN_POINT('Ctrl Pts',(40.0301081454006,-59.7872471243948,
12.));
#125511=CARTESIAN_POINT('Ctrl Pts',(40.035856490434,-59.8105032789179,12.));
#125512=CARTESIAN_POINT('Ctrl Pts',(40.0415922549313,-59.8338062259491,
12.));
#125513=CARTESIAN_POINT('Ctrl Pts',(40.0473153509323,-59.8571558639144,
12.));
#125514=CARTESIAN_POINT('Ctrl Pts',(40.0530256909162,-59.8805520915975,
12.));
#125515=CARTESIAN_POINT('Ctrl Pts',(40.0587231877962,-59.9039948081432,
12.));
#125516=CARTESIAN_POINT('Ctrl Pts',(40.064407754916,-59.9274839130553,12.));
#125517=CARTESIAN_POINT('Ctrl Pts',(40.0700793060473,-59.9510193061927,
12.));
#125518=CARTESIAN_POINT('Ctrl Pts',(40.0757377553888,-59.9746008877584,
12.));
#125519=CARTESIAN_POINT('Ctrl Pts',(40.0813830175623,-59.9982285582983,
12.));
#125520=CARTESIAN_POINT('Ctrl Pts',(40.0870150076074,-60.021902218706,12.));
#125521=CARTESIAN_POINT('Ctrl Pts',(40.0926336409785,-60.0456217702201,
12.));
#125522=CARTESIAN_POINT('Ctrl Pts',(40.0982388335423,-60.069387114421,12.));
#125523=CARTESIAN_POINT('Ctrl Pts',(40.1038305015766,-60.0931981532197,
12.));
#125524=CARTESIAN_POINT('Ctrl Pts',(40.1094085617674,-60.1170547888574,
12.));
#125525=CARTESIAN_POINT('Ctrl Pts',(40.1149729312036,-60.1409569239092,
12.));
#125526=CARTESIAN_POINT('Ctrl Pts',(40.120523527374,-60.1649044612828,12.));
#125527=CARTESIAN_POINT('Ctrl Pts',(40.1260602681644,-60.1888973042152,
12.));
#125528=CARTESIAN_POINT('Ctrl Pts',(40.1315830718577,-60.2129353562622,
12.));
#125529=CARTESIAN_POINT('Ctrl Pts',(40.1370918571305,-60.2370185212964,
12.));
#125530=CARTESIAN_POINT('Ctrl Pts',(40.1425865430472,-60.2611467035116,
12.));
#125531=CARTESIAN_POINT('Ctrl Pts',(40.1480670490586,-60.285319807422,12.));
#125532=CARTESIAN_POINT('Ctrl Pts',(40.1535332949976,-60.3095377378586,
12.));
#125533=CARTESIAN_POINT('Ctrl Pts',(40.1589852010804,-60.3338003999606,
12.));
#125534=CARTESIAN_POINT('Ctrl Pts',(40.1644226879033,-60.3581076991716,
12.));
#125535=CARTESIAN_POINT('Ctrl Pts',(40.1698456764377,-60.3824595412445,
12.));
#125536=CARTESIAN_POINT('Ctrl Pts',(40.1752540880268,-60.4068558322407,
12.));
#125537=CARTESIAN_POINT('Ctrl Pts',(40.180647844383,-60.4312964785273,12.));
#125538=CARTESIAN_POINT('Ctrl Pts',(40.1860268675884,-60.455781386769,12.));
#125539=CARTESIAN_POINT('Ctrl Pts',(40.1913910800921,-60.4803104639225,
12.));
#125540=CARTESIAN_POINT('Ctrl Pts',(40.1967404047062,-60.5048836172435,
12.));
#125541=CARTESIAN_POINT('Ctrl Pts',(40.2020747646014,-60.5295007542841,
12.));
#125542=CARTESIAN_POINT('Ctrl Pts',(40.2073940833053,-60.5541617828925,
12.));
#125543=CARTESIAN_POINT('Ctrl Pts',(40.2126982847011,-60.5788666112042,
12.));
#125544=CARTESIAN_POINT('Ctrl Pts',(40.2179872930273,-60.6036151476349,
12.));
#125545=CARTESIAN_POINT('Ctrl Pts',(40.2232610328721,-60.6284073008871,
12.));
#125546=CARTESIAN_POINT('Ctrl Pts',(40.2285194291706,-60.6532429799499,
12.));
#125547=CARTESIAN_POINT('Ctrl Pts',(40.2337624072029,-60.678122094098,12.));
#125548=CARTESIAN_POINT('Ctrl Pts',(40.2389898925932,-60.7030445528857,
12.));
#125549=CARTESIAN_POINT('Ctrl Pts',(40.2442018113108,-60.728010266139,12.));
#125550=CARTESIAN_POINT('Ctrl Pts',(40.2493980896638,-60.7530191439593,
12.));
#125551=CARTESIAN_POINT('Ctrl Pts',(40.2545786542953,-60.7780710967248,
12.));
#125552=CARTESIAN_POINT('Ctrl Pts',(40.2597434321803,-60.8031660350879,
12.));
#125553=CARTESIAN_POINT('Ctrl Pts',(40.2648923506248,-60.8283038699706,
12.));
#125554=CARTESIAN_POINT('Ctrl Pts',(40.2700253372648,-60.8534845125538,
12.));
#125555=CARTESIAN_POINT('Ctrl Pts',(40.2751423200639,-60.8787078742818,
12.));
#125556=CARTESIAN_POINT('Ctrl Pts',(40.2802432273105,-60.9039738668668,
12.));
#125557=CARTESIAN_POINT('Ctrl Pts',(40.2853279876161,-60.9292824022887,
12.));
#125558=CARTESIAN_POINT('Ctrl Pts',(40.2903965299155,-60.954633392792,12.));
#125559=CARTESIAN_POINT('Ctrl Pts',(40.295448783469,-60.9800267508786,12.));
#125560=CARTESIAN_POINT('Ctrl Pts',(40.300484677858,-61.0054623893066,12.));
#125561=CARTESIAN_POINT('Ctrl Pts',(40.3055041429775,-61.0309402210921,
12.));
#125562=CARTESIAN_POINT('Ctrl Pts',(40.310507109031,-61.056460159505,12.));
#125563=CARTESIAN_POINT('Ctrl Pts',(40.3154935065262,-61.0820221180645,
12.));
#125564=CARTESIAN_POINT('Ctrl Pts',(40.3204632662726,-61.1076260105258,
12.));
#125565=CARTESIAN_POINT('Ctrl Pts',(40.32541631938,-61.1332717508789,12.));
#125566=CARTESIAN_POINT('Ctrl Pts',(40.3303525972616,-61.1589592533613,
12.));
#125567=CARTESIAN_POINT('Ctrl Pts',(40.335272031637,-61.1846884324643,12.));
#125568=CARTESIAN_POINT('Ctrl Pts',(40.340174554537,-61.2104592029377,12.));
#125569=CARTESIAN_POINT('Ctrl Pts',(40.3450600983109,-61.2362714797899,
12.));
#125570=CARTESIAN_POINT('Ctrl Pts',(40.3499285956304,-61.2621251782863,
12.));
#125571=CARTESIAN_POINT('Ctrl Pts',(40.3547799794679,-61.2880202139371,
12.));
#125572=CARTESIAN_POINT('Ctrl Pts',(40.3596141830791,-61.3139565024847,
12.));
#125573=CARTESIAN_POINT('Ctrl Pts',(40.3644311399861,-61.3399339598853,
12.));
#125574=CARTESIAN_POINT('Ctrl Pts',(40.3692307839636,-61.3659525022908,
12.));
#125575=CARTESIAN_POINT('Ctrl Pts',(40.3740130490225,-61.3920120460219,
12.));
#125576=CARTESIAN_POINT('Ctrl Pts',(40.3787778694364,-61.4181125076037,
12.));
#125577=CARTESIAN_POINT('Ctrl Pts',(40.383525179772,-61.4442538038044,12.));
#125578=CARTESIAN_POINT('Ctrl Pts',(40.3882549149228,-61.4704358516709,
12.));
#125579=CARTESIAN_POINT('Ctrl Pts',(40.3929670101366,-61.4966585685549,
12.));
#125580=CARTESIAN_POINT('Ctrl Pts',(40.3976614010653,-61.522921872154,12.));
#125581=CARTESIAN_POINT('Ctrl Pts',(40.4023380237232,-61.5492256804717,
12.));
#125582=CARTESIAN_POINT('Ctrl Pts',(40.4069968143956,-61.5755699117324,
12.));
#125583=CARTESIAN_POINT('Ctrl Pts',(40.4116377095596,-61.601954484301,12.));
#125584=CARTESIAN_POINT('Ctrl Pts',(40.4162606458119,-61.6283793166079,
12.));
#125585=CARTESIAN_POINT('Ctrl Pts',(40.4208655597717,-61.6548443270394,
12.));
#125586=CARTESIAN_POINT('Ctrl Pts',(40.425452388076,-61.6813494339286,12.));
#125587=CARTESIAN_POINT('Ctrl Pts',(40.430021067584,-61.7078945557799,12.));
#125588=CARTESIAN_POINT('Ctrl Pts',(40.4345715355405,-61.7344796114399,
12.));
#125589=CARTESIAN_POINT('Ctrl Pts',(40.4391037297589,-61.7611045202874,
12.));
#125590=CARTESIAN_POINT('Ctrl Pts',(40.443617588795,-61.7877692024076,12.));
#125591=CARTESIAN_POINT('Ctrl Pts',(40.4481130521364,-61.814473578779,12.));
#125592=CARTESIAN_POINT('Ctrl Pts',(40.4525900597894,-61.8412175708552,
12.));
#125593=CARTESIAN_POINT('Ctrl Pts',(40.457048551875,-61.8680011001537,12.));
#125594=CARTESIAN_POINT('Ctrl Pts',(40.4614884681889,-61.8948240878007,
12.));
#125595=CARTESIAN_POINT('Ctrl Pts',(40.4659097478587,-61.9216864541744,
12.));
#125596=CARTESIAN_POINT('Ctrl Pts',(40.4703123287621,-61.9485881182921,
12.));
#125597=CARTESIAN_POINT('Ctrl Pts',(40.4746961480015,-61.9755289983044,
12.));
#125598=CARTESIAN_POINT('Ctrl Pts',(40.4790611429584,-62.0025090125959,
12.));
#125599=CARTESIAN_POINT('Ctrl Pts',(40.4834072522164,-62.029528080742,12.));
#125600=CARTESIAN_POINT('Ctrl Pts',(40.4877344164411,-62.0565861244178,
12.));
#125601=CARTESIAN_POINT('Ctrl Pts',(40.4920425795217,-62.0836830685719,
12.));
#125602=CARTESIAN_POINT('Ctrl Pts',(40.4963316888412,-62.1108188417003,
12.));
#125603=CARTESIAN_POINT('Ctrl Pts',(40.4999919096264,-62.1341126810542,
12.));
#125604=CARTESIAN_POINT('Ctrl Pts',(40.5027877865803,-62.1519925002976,
12.));
#125605=CARTESIAN_POINT('Ctrl Pts',(40.5047277935767,-62.1644411502823,
12.));
#125606=CARTESIAN_POINT('Ctrl Pts',(40.5058175523128,-62.1714473138104,
12.));
#125607=CARTESIAN_POINT('Ctrl Pts',(40.506059810093,-62.1730054756875,12.));
#125608=CARTESIAN_POINT('',(39.4479504917287,-57.8261117662439,0.));
#125609=CARTESIAN_POINT('',(39.4479504917286,-57.8261117662438,0.));
#125610=CARTESIAN_POINT('Ctrl Pts',(40.506059810093,-62.1730054756875,0.));
#125611=CARTESIAN_POINT('Ctrl Pts',(40.5058175523128,-62.1714473138104,
0.));
#125612=CARTESIAN_POINT('Ctrl Pts',(40.5047277935767,-62.1644411502823,
0.));
#125613=CARTESIAN_POINT('Ctrl Pts',(40.5027877865803,-62.1519925002976,
0.));
#125614=CARTESIAN_POINT('Ctrl Pts',(40.4999919096264,-62.1341126810542,
0.));
#125615=CARTESIAN_POINT('Ctrl Pts',(40.4963316888412,-62.1108188417003,
0.));
#125616=CARTESIAN_POINT('Ctrl Pts',(40.4920425795217,-62.0836830685719,
0.));
#125617=CARTESIAN_POINT('Ctrl Pts',(40.4877344164411,-62.0565861244178,
0.));
#125618=CARTESIAN_POINT('Ctrl Pts',(40.4834072522164,-62.029528080742,0.));
#125619=CARTESIAN_POINT('Ctrl Pts',(40.4790611429584,-62.0025090125959,
0.));
#125620=CARTESIAN_POINT('Ctrl Pts',(40.4746961480015,-61.9755289983044,
0.));
#125621=CARTESIAN_POINT('Ctrl Pts',(40.4703123287621,-61.9485881182921,
0.));
#125622=CARTESIAN_POINT('Ctrl Pts',(40.4659097478587,-61.9216864541744,
0.));
#125623=CARTESIAN_POINT('Ctrl Pts',(40.4614884681889,-61.8948240878007,
0.));
#125624=CARTESIAN_POINT('Ctrl Pts',(40.457048551875,-61.8680011001537,0.));
#125625=CARTESIAN_POINT('Ctrl Pts',(40.4525900597894,-61.8412175708552,
0.));
#125626=CARTESIAN_POINT('Ctrl Pts',(40.4481130521364,-61.814473578779,0.));
#125627=CARTESIAN_POINT('Ctrl Pts',(40.443617588795,-61.7877692024076,0.));
#125628=CARTESIAN_POINT('Ctrl Pts',(40.4391037297589,-61.7611045202874,
0.));
#125629=CARTESIAN_POINT('Ctrl Pts',(40.4345715355405,-61.7344796114399,
0.));
#125630=CARTESIAN_POINT('Ctrl Pts',(40.430021067584,-61.7078945557799,0.));
#125631=CARTESIAN_POINT('Ctrl Pts',(40.425452388076,-61.6813494339286,0.));
#125632=CARTESIAN_POINT('Ctrl Pts',(40.4208655597717,-61.6548443270394,
0.));
#125633=CARTESIAN_POINT('Ctrl Pts',(40.4162606458119,-61.6283793166079,
0.));
#125634=CARTESIAN_POINT('Ctrl Pts',(40.4116377095596,-61.601954484301,0.));
#125635=CARTESIAN_POINT('Ctrl Pts',(40.4069968143956,-61.5755699117324,
0.));
#125636=CARTESIAN_POINT('Ctrl Pts',(40.4023380237232,-61.5492256804717,
0.));
#125637=CARTESIAN_POINT('Ctrl Pts',(40.3976614010653,-61.522921872154,0.));
#125638=CARTESIAN_POINT('Ctrl Pts',(40.3929670101366,-61.4966585685549,
0.));
#125639=CARTESIAN_POINT('Ctrl Pts',(40.3882549149228,-61.4704358516709,
0.));
#125640=CARTESIAN_POINT('Ctrl Pts',(40.383525179772,-61.4442538038044,0.));
#125641=CARTESIAN_POINT('Ctrl Pts',(40.3787778694364,-61.4181125076037,
0.));
#125642=CARTESIAN_POINT('Ctrl Pts',(40.3740130490225,-61.3920120460219,
0.));
#125643=CARTESIAN_POINT('Ctrl Pts',(40.3692307839636,-61.3659525022908,
0.));
#125644=CARTESIAN_POINT('Ctrl Pts',(40.3644311399861,-61.3399339598853,
0.));
#125645=CARTESIAN_POINT('Ctrl Pts',(40.3596141830791,-61.3139565024847,
0.));
#125646=CARTESIAN_POINT('Ctrl Pts',(40.3547799794679,-61.2880202139371,
0.));
#125647=CARTESIAN_POINT('Ctrl Pts',(40.3499285956304,-61.2621251782863,
0.));
#125648=CARTESIAN_POINT('Ctrl Pts',(40.3450600983109,-61.2362714797899,
0.));
#125649=CARTESIAN_POINT('Ctrl Pts',(40.340174554537,-61.2104592029377,0.));
#125650=CARTESIAN_POINT('Ctrl Pts',(40.335272031637,-61.1846884324643,0.));
#125651=CARTESIAN_POINT('Ctrl Pts',(40.3303525972616,-61.1589592533613,
0.));
#125652=CARTESIAN_POINT('Ctrl Pts',(40.32541631938,-61.1332717508789,0.));
#125653=CARTESIAN_POINT('Ctrl Pts',(40.3204632662726,-61.1076260105258,
0.));
#125654=CARTESIAN_POINT('Ctrl Pts',(40.3154935065262,-61.0820221180645,
0.));
#125655=CARTESIAN_POINT('Ctrl Pts',(40.310507109031,-61.056460159505,0.));
#125656=CARTESIAN_POINT('Ctrl Pts',(40.3055041429775,-61.0309402210921,
0.));
#125657=CARTESIAN_POINT('Ctrl Pts',(40.300484677858,-61.0054623893066,0.));
#125658=CARTESIAN_POINT('Ctrl Pts',(40.295448783469,-60.9800267508786,0.));
#125659=CARTESIAN_POINT('Ctrl Pts',(40.2903965299155,-60.954633392792,0.));
#125660=CARTESIAN_POINT('Ctrl Pts',(40.2853279876161,-60.9292824022887,
0.));
#125661=CARTESIAN_POINT('Ctrl Pts',(40.2802432273105,-60.9039738668668,
0.));
#125662=CARTESIAN_POINT('Ctrl Pts',(40.2751423200639,-60.8787078742818,
0.));
#125663=CARTESIAN_POINT('Ctrl Pts',(40.2700253372648,-60.8534845125538,
0.));
#125664=CARTESIAN_POINT('Ctrl Pts',(40.2648923506248,-60.8283038699706,
0.));
#125665=CARTESIAN_POINT('Ctrl Pts',(40.2597434321803,-60.8031660350879,
0.));
#125666=CARTESIAN_POINT('Ctrl Pts',(40.2545786542953,-60.7780710967248,
0.));
#125667=CARTESIAN_POINT('Ctrl Pts',(40.2493980896638,-60.7530191439593,
0.));
#125668=CARTESIAN_POINT('Ctrl Pts',(40.2442018113108,-60.728010266139,0.));
#125669=CARTESIAN_POINT('Ctrl Pts',(40.2389898925932,-60.7030445528857,
0.));
#125670=CARTESIAN_POINT('Ctrl Pts',(40.2337624072029,-60.678122094098,0.));
#125671=CARTESIAN_POINT('Ctrl Pts',(40.2285194291706,-60.6532429799499,
0.));
#125672=CARTESIAN_POINT('Ctrl Pts',(40.2232610328721,-60.6284073008871,
0.));
#125673=CARTESIAN_POINT('Ctrl Pts',(40.2179872930273,-60.6036151476349,
0.));
#125674=CARTESIAN_POINT('Ctrl Pts',(40.2126982847011,-60.5788666112042,
0.));
#125675=CARTESIAN_POINT('Ctrl Pts',(40.2073940833053,-60.5541617828925,
0.));
#125676=CARTESIAN_POINT('Ctrl Pts',(40.2020747646014,-60.5295007542841,
0.));
#125677=CARTESIAN_POINT('Ctrl Pts',(40.1967404047062,-60.5048836172435,
0.));
#125678=CARTESIAN_POINT('Ctrl Pts',(40.1913910800921,-60.4803104639225,
0.));
#125679=CARTESIAN_POINT('Ctrl Pts',(40.1860268675884,-60.455781386769,0.));
#125680=CARTESIAN_POINT('Ctrl Pts',(40.180647844383,-60.4312964785273,0.));
#125681=CARTESIAN_POINT('Ctrl Pts',(40.1752540880268,-60.4068558322407,
0.));
#125682=CARTESIAN_POINT('Ctrl Pts',(40.1698456764377,-60.3824595412445,
0.));
#125683=CARTESIAN_POINT('Ctrl Pts',(40.1644226879033,-60.3581076991716,
0.));
#125684=CARTESIAN_POINT('Ctrl Pts',(40.1589852010804,-60.3338003999606,
0.));
#125685=CARTESIAN_POINT('Ctrl Pts',(40.1535332949976,-60.3095377378586,
0.));
#125686=CARTESIAN_POINT('Ctrl Pts',(40.1480670490586,-60.285319807422,0.));
#125687=CARTESIAN_POINT('Ctrl Pts',(40.1425865430472,-60.2611467035116,
0.));
#125688=CARTESIAN_POINT('Ctrl Pts',(40.1370918571305,-60.2370185212964,
0.));
#125689=CARTESIAN_POINT('Ctrl Pts',(40.1315830718577,-60.2129353562622,
0.));
#125690=CARTESIAN_POINT('Ctrl Pts',(40.1260602681644,-60.1888973042152,
0.));
#125691=CARTESIAN_POINT('Ctrl Pts',(40.120523527374,-60.1649044612828,0.));
#125692=CARTESIAN_POINT('Ctrl Pts',(40.1149729312036,-60.1409569239092,
0.));
#125693=CARTESIAN_POINT('Ctrl Pts',(40.1094085617674,-60.1170547888574,
0.));
#125694=CARTESIAN_POINT('Ctrl Pts',(40.1038305015766,-60.0931981532197,
0.));
#125695=CARTESIAN_POINT('Ctrl Pts',(40.0982388335423,-60.069387114421,0.));
#125696=CARTESIAN_POINT('Ctrl Pts',(40.0926336409785,-60.0456217702201,
0.));
#125697=CARTESIAN_POINT('Ctrl Pts',(40.0870150076074,-60.021902218706,0.));
#125698=CARTESIAN_POINT('Ctrl Pts',(40.0813830175623,-59.9982285582983,
0.));
#125699=CARTESIAN_POINT('Ctrl Pts',(40.0757377553888,-59.9746008877584,
0.));
#125700=CARTESIAN_POINT('Ctrl Pts',(40.0700793060473,-59.9510193061927,
0.));
#125701=CARTESIAN_POINT('Ctrl Pts',(40.064407754916,-59.9274839130553,0.));
#125702=CARTESIAN_POINT('Ctrl Pts',(40.0587231877962,-59.9039948081432,
0.));
#125703=CARTESIAN_POINT('Ctrl Pts',(40.0530256909162,-59.8805520915975,
0.));
#125704=CARTESIAN_POINT('Ctrl Pts',(40.0473153509323,-59.8571558639144,
0.));
#125705=CARTESIAN_POINT('Ctrl Pts',(40.0415922549313,-59.8338062259491,
0.));
#125706=CARTESIAN_POINT('Ctrl Pts',(40.035856490434,-59.8105032789179,0.));
#125707=CARTESIAN_POINT('Ctrl Pts',(40.0301081454006,-59.7872471243948,
0.));
#125708=CARTESIAN_POINT('Ctrl Pts',(40.0243473082343,-59.7640378643114,
0.));
#125709=CARTESIAN_POINT('Ctrl Pts',(40.0185740677827,-59.7408756009688,
0.));
#125710=CARTESIAN_POINT('Ctrl Pts',(40.0127885133407,-59.7177604370409,
0.));
#125711=CARTESIAN_POINT('Ctrl Pts',(40.0069907346536,-59.6946924755771,
0.));
#125712=CARTESIAN_POINT('Ctrl Pts',(40.0011808219231,-59.671671819999,0.));
#125713=CARTESIAN_POINT('Ctrl Pts',(39.9953588658115,-59.6486985741015,
0.));
#125714=CARTESIAN_POINT('Ctrl Pts',(39.9895249574432,-59.6257728420644,
0.));
#125715=CARTESIAN_POINT('Ctrl Pts',(39.9836791884072,-59.6028947284551,
0.));
#125716=CARTESIAN_POINT('Ctrl Pts',(39.9778216507609,-59.5800643382322,
0.));
#125717=CARTESIAN_POINT('Ctrl Pts',(39.971952437036,-59.5572817767412,0.));
#125718=CARTESIAN_POINT('Ctrl Pts',(39.9660716402423,-59.5345471497162,
0.));
#125719=CARTESIAN_POINT('Ctrl Pts',(39.96017935387,-59.5118605632919,0.));
#125720=CARTESIAN_POINT('Ctrl Pts',(39.954275671893,-59.4892221240081,0.));
#125721=CARTESIAN_POINT('Ctrl Pts',(39.9483606887731,-59.4666319388123,
0.));
#125722=CARTESIAN_POINT('Ctrl Pts',(39.9424344994652,-59.444090115055,0.));
#125723=CARTESIAN_POINT('Ctrl Pts',(39.9364971994215,-59.4215967604925,
0.));
#125724=CARTESIAN_POINT('Ctrl Pts',(39.9305488845934,-59.3991519832981,
0.));
#125725=CARTESIAN_POINT('Ctrl Pts',(39.9245896514359,-59.3767558920663,
0.));
#125726=CARTESIAN_POINT('Ctrl Pts',(39.9186195969113,-59.3544085958165,
0.));
#125727=CARTESIAN_POINT('Ctrl Pts',(39.9126388184956,-59.3321102039883,
0.));
#125728=CARTESIAN_POINT('Ctrl Pts',(39.9066474141826,-59.3098608264452,
0.));
#125729=CARTESIAN_POINT('Ctrl Pts',(39.9006454824861,-59.287660573487,0.));
#125730=CARTESIAN_POINT('Ctrl Pts',(39.8946331224442,-59.2655095558527,
0.));
#125731=CARTESIAN_POINT('Ctrl Pts',(39.8886104336234,-59.2434078847236,
0.));
#125732=CARTESIAN_POINT('Ctrl Pts',(39.8825775161253,-59.2213556717188,
0.));
#125733=CARTESIAN_POINT('Ctrl Pts',(39.8765344705895,-59.1993530289008,
0.));
#125734=CARTESIAN_POINT('Ctrl Pts',(39.8704813981978,-59.1774000687865,
0.));
#125735=CARTESIAN_POINT('Ctrl Pts',(39.8644184006785,-59.155496904352,0.));
#125736=CARTESIAN_POINT('Ctrl Pts',(39.8583455803111,-59.133643649035,0.));
#125737=CARTESIAN_POINT('Ctrl Pts',(39.8522630399337,-59.1118404167304,
0.));
#125738=CARTESIAN_POINT('Ctrl Pts',(39.8461708829465,-59.0900873217992,
0.));
#125739=CARTESIAN_POINT('Ctrl Pts',(39.8400692133143,-59.068384479077,0.));
#125740=CARTESIAN_POINT('Ctrl Pts',(39.8339581355715,-59.0467320038782,
0.));
#125741=CARTESIAN_POINT('Ctrl Pts',(39.8278377548261,-59.0251300119972,
0.));
#125742=CARTESIAN_POINT('Ctrl Pts',(39.8217081767658,-59.0035786197024,
0.));
#125743=CARTESIAN_POINT('Ctrl Pts',(39.8155695076625,-58.9820779437485,
0.));
#125744=CARTESIAN_POINT('Ctrl Pts',(39.8094218543781,-58.9606281013875,
0.));
#125745=CARTESIAN_POINT('Ctrl Pts',(39.8032653243712,-58.9392292103747,
0.));
#125746=CARTESIAN_POINT('Ctrl Pts',(39.7971000257044,-58.9178813889703,
0.));
#125747=CARTESIAN_POINT('Ctrl Pts',(39.7909260670517,-58.8965847559389,
0.));
#125748=CARTESIAN_POINT('Ctrl Pts',(39.7847435576996,-58.8753394305583,
0.));
#125749=CARTESIAN_POINT('Ctrl Pts',(39.7785526075477,-58.8541455326229,
0.));
#125750=CARTESIAN_POINT('Ctrl Pts',(39.772353327112,-58.8330031824453,0.));
#125751=CARTESIAN_POINT('Ctrl Pts',(39.7661458275276,-58.8119125008521,
0.));
#125752=CARTESIAN_POINT('Ctrl Pts',(39.7599302205527,-58.7908736091808,
0.));
#125753=CARTESIAN_POINT('Ctrl Pts',(39.753706618582,-58.769886629304,0.));
#125754=CARTESIAN_POINT('Ctrl Pts',(39.7474751346603,-58.7489516836452,
0.));
#125755=CARTESIAN_POINT('Ctrl Pts',(39.741235882495,-58.7280688951911,0.));
#125756=CARTESIAN_POINT('Ctrl Pts',(39.7349889764737,-58.7072383875009,
0.));
#125757=CARTESIAN_POINT('Ctrl Pts',(39.7287345316664,-58.6864602847064,
0.));
#125758=CARTESIAN_POINT('Ctrl Pts',(39.7224726638087,-58.6657347115014,
0.));
#125759=CARTESIAN_POINT('Ctrl Pts',(39.7162034892896,-58.6450617931269,
0.));
#125760=CARTESIAN_POINT('Ctrl Pts',(39.7099271251421,-58.6244416553574,
0.));
#125761=CARTESIAN_POINT('Ctrl Pts',(39.7036436890248,-58.6038744244683,
0.));
#125762=CARTESIAN_POINT('Ctrl Pts',(39.6973532992555,-58.5833602272767,
0.));
#125763=CARTESIAN_POINT('Ctrl Pts',(39.6910560748639,-58.5628991912067,
0.));
#125764=CARTESIAN_POINT('Ctrl Pts',(39.6847521356395,-58.5424914443415,
0.));
#125765=CARTESIAN_POINT('Ctrl Pts',(39.6784416021817,-58.5221371154748,
0.));
#125766=CARTESIAN_POINT('Ctrl Pts',(39.6721245959516,-58.5018363341582,
0.));
#125767=CARTESIAN_POINT('Ctrl Pts',(39.66580123918,-58.4815892306044,0.));
#125768=CARTESIAN_POINT('Ctrl Pts',(39.6594716547681,-58.4613959355776,
0.));
#125769=CARTESIAN_POINT('Ctrl Pts',(39.6531359662043,-58.4412565802984,
0.));
#125770=CARTESIAN_POINT('Ctrl Pts',(39.6467942974465,-58.4211712963023,
0.));
#125771=CARTESIAN_POINT('Ctrl Pts',(39.6404467729114,-58.4011402154225,
0.));
#125772=CARTESIAN_POINT('Ctrl Pts',(39.6340935177492,-58.3811634701061,
0.));
#125773=CARTESIAN_POINT('Ctrl Pts',(39.6277346580898,-58.3612411936914,
0.));
#125774=CARTESIAN_POINT('Ctrl Pts',(39.6213703212523,-58.3413735206412,
0.));
#125775=CARTESIAN_POINT('Ctrl Pts',(39.6150006360894,-58.3215605869192,
0.));
#125776=CARTESIAN_POINT('Ctrl Pts',(39.6086257327559,-58.3018025297288,
0.));
#125777=CARTESIAN_POINT('Ctrl Pts',(39.6022457420772,-58.2820994868092,
0.));
#125778=CARTESIAN_POINT('Ctrl Pts',(39.5958607950237,-58.2624515958416,
0.));
#125779=CARTESIAN_POINT('Ctrl Pts',(39.589471022173,-58.2428589938394,0.));
#125780=CARTESIAN_POINT('Ctrl Pts',(39.5830765530919,-58.2233218164407,
0.));
#125781=CARTESIAN_POINT('Ctrl Pts',(39.5766775175226,-58.2038401992496,
0.));
#125782=CARTESIAN_POINT('Ctrl Pts',(39.5702740468013,-58.1844142794359,
0.));
#125783=CARTESIAN_POINT('Ctrl Pts',(39.5638662750174,-58.1650441970378,
0.));
#125784=CARTESIAN_POINT('Ctrl Pts',(39.5574543406959,-58.1457300968466,
0.));
#125785=CARTESIAN_POINT('Ctrl Pts',(39.5510383869476,-58.1264721285697,
0.));
#125786=CARTESIAN_POINT('Ctrl Pts',(39.5446185579615,-58.1072704428895,
0.));
#125787=CARTESIAN_POINT('Ctrl Pts',(39.5381949959214,-58.088125187991,0.));
#125788=CARTESIAN_POINT('Ctrl Pts',(39.5317678383231,-58.0690365065393,
0.));
#125789=CARTESIAN_POINT('Ctrl Pts',(39.5253372136921,-58.0500045308459,
0.));
#125790=CARTESIAN_POINT('Ctrl Pts',(39.5189032457227,-58.0310293875321,
0.));
#125791=CARTESIAN_POINT('Ctrl Pts',(39.5124660615009,-58.012111206794,0.));
#125792=CARTESIAN_POINT('Ctrl Pts',(39.5060257981225,-57.9932501298522,
0.));
#125793=CARTESIAN_POINT('Ctrl Pts',(39.4995826106692,-57.9744463179305,
0.));
#125794=CARTESIAN_POINT('Ctrl Pts',(39.4931366776628,-57.9556999583777,
0.));
#125795=CARTESIAN_POINT('Ctrl Pts',(39.4866881842223,-57.9370112456506,
0.));
#125796=CARTESIAN_POINT('Ctrl Pts',(39.4802373061008,-57.9183803632337,
0.));
#125797=CARTESIAN_POINT('Ctrl Pts',(39.4737841949417,-57.899807467054,0.));
#125798=CARTESIAN_POINT('Ctrl Pts',(39.4673289592425,-57.8812926637397,
0.));
#125799=CARTESIAN_POINT('Ctrl Pts',(39.4608716627367,-57.8628360097134,
0.));
#125800=CARTESIAN_POINT('Ctrl Pts',(39.4557042029884,-57.8481172247804,
0.));
#125801=CARTESIAN_POINT('Ctrl Pts',(39.45182770037,-57.8371043151606,0.));
#125802=CARTESIAN_POINT('Ctrl Pts',(39.4492429618498,-57.829774010102,0.));
#125803=CARTESIAN_POINT('Ctrl Pts',(39.4479504917287,-57.8261117662439,
0.));
#125804=CARTESIAN_POINT('Ctrl Pts',(34.953242280886,-65.7914953018525,0.));
#125805=CARTESIAN_POINT('Ctrl Pts',(34.953242280886,-65.7914953018525,12.));
#125806=CARTESIAN_POINT('Ctrl Pts',(34.9529266758465,-65.7859084407618,
0.));
#125807=CARTESIAN_POINT('Ctrl Pts',(34.9529266758465,-65.7859084407618,
12.));
#125808=CARTESIAN_POINT('Ctrl Pts',(34.9522931728758,-65.7747383251112,
0.));
#125809=CARTESIAN_POINT('Ctrl Pts',(34.9522931728758,-65.7747383251112,
12.));
#125810=CARTESIAN_POINT('Ctrl Pts',(34.9513360397454,-65.7579939712289,
0.));
#125811=CARTESIAN_POINT('Ctrl Pts',(34.9513360397454,-65.7579939712289,
12.));
#125812=CARTESIAN_POINT('Ctrl Pts',(34.9500461043246,-65.7356898061148,
0.));
#125813=CARTESIAN_POINT('Ctrl Pts',(34.9500461043246,-65.7356898061148,
12.));
#125814=CARTESIAN_POINT('Ctrl Pts',(34.9484107544136,-65.7078456758034,
0.));
#125815=CARTESIAN_POINT('Ctrl Pts',(34.9484107544136,-65.7078456758034,
12.));
#125816=CARTESIAN_POINT('Ctrl Pts',(34.9467524770438,-65.6800376406066,
0.));
#125817=CARTESIAN_POINT('Ctrl Pts',(34.9467524770438,-65.6800376406066,
12.));
#125818=CARTESIAN_POINT('Ctrl Pts',(34.9450712829182,-65.6522657321322,
0.));
#125819=CARTESIAN_POINT('Ctrl Pts',(34.9450712829182,-65.6522657321322,
12.));
#125820=CARTESIAN_POINT('Ctrl Pts',(34.943367193292,-65.624529996851,0.));
#125821=CARTESIAN_POINT('Ctrl Pts',(34.943367193292,-65.624529996851,12.));
#125822=CARTESIAN_POINT('Ctrl Pts',(34.9416402443435,-65.5968304997585,
0.));
#125823=CARTESIAN_POINT('Ctrl Pts',(34.9416402443435,-65.5968304997585,
12.));
#125824=CARTESIAN_POINT('Ctrl Pts',(34.9398904862157,-65.5691673225803,
0.));
#125825=CARTESIAN_POINT('Ctrl Pts',(34.9398904862157,-65.5691673225803,
12.));
#125826=CARTESIAN_POINT('Ctrl Pts',(34.9381179779673,-65.5415405577955,
0.));
#125827=CARTESIAN_POINT('Ctrl Pts',(34.9381179779673,-65.5415405577955,
12.));
#125828=CARTESIAN_POINT('Ctrl Pts',(34.9363227836581,-65.5139503038036,
0.));
#125829=CARTESIAN_POINT('Ctrl Pts',(34.9363227836581,-65.5139503038036,
12.));
#125830=CARTESIAN_POINT('Ctrl Pts',(34.9345049680825,-65.4863966597544,
0.));
#125831=CARTESIAN_POINT('Ctrl Pts',(34.9345049680825,-65.4863966597544,
12.));
#125832=CARTESIAN_POINT('Ctrl Pts',(34.9326645923939,-65.4588797201972,
0.));
#125833=CARTESIAN_POINT('Ctrl Pts',(34.9326645923939,-65.4588797201972,
12.));
#125834=CARTESIAN_POINT('Ctrl Pts',(34.9308017105535,-65.4313995707536,
0.));
#125835=CARTESIAN_POINT('Ctrl Pts',(34.9308017105535,-65.4313995707536,
12.));
#125836=CARTESIAN_POINT('Ctrl Pts',(34.9289163717747,-65.4039562911353,
0.));
#125837=CARTESIAN_POINT('Ctrl Pts',(34.9289163717747,-65.4039562911353,
12.));
#125838=CARTESIAN_POINT('Ctrl Pts',(34.927008622273,-65.3765499573077,0.));
#125839=CARTESIAN_POINT('Ctrl Pts',(34.927008622273,-65.3765499573077,12.));
#125840=CARTESIAN_POINT('Ctrl Pts',(34.9250785073476,-65.3491806440537,
0.));
#125841=CARTESIAN_POINT('Ctrl Pts',(34.9250785073476,-65.3491806440537,
12.));
#125842=CARTESIAN_POINT('Ctrl Pts',(34.923126073183,-65.3218484271911,0.));
#125843=CARTESIAN_POINT('Ctrl Pts',(34.923126073183,-65.3218484271911,12.));
#125844=CARTESIAN_POINT('Ctrl Pts',(34.9211513691355,-65.2945533863762,
0.));
#125845=CARTESIAN_POINT('Ctrl Pts',(34.9211513691355,-65.2945533863762,
12.));
#125846=CARTESIAN_POINT('Ctrl Pts',(34.9191544474872,-65.267295604807,0.));
#125847=CARTESIAN_POINT('Ctrl Pts',(34.9191544474872,-65.267295604807,12.));
#125848=CARTESIAN_POINT('Ctrl Pts',(34.9171353624112,-65.2400751679549,
0.));
#125849=CARTESIAN_POINT('Ctrl Pts',(34.9171353624112,-65.2400751679549,
12.));
#125850=CARTESIAN_POINT('Ctrl Pts',(34.9150941691747,-65.2128921625824,
0.));
#125851=CARTESIAN_POINT('Ctrl Pts',(34.9150941691747,-65.2128921625824,
12.));
#125852=CARTESIAN_POINT('Ctrl Pts',(34.9130309233021,-65.1857466757092,
0.));
#125853=CARTESIAN_POINT('Ctrl Pts',(34.9130309233021,-65.1857466757092,
12.));
#125854=CARTESIAN_POINT('Ctrl Pts',(34.9109456796213,-65.1586387934241,
0.));
#125855=CARTESIAN_POINT('Ctrl Pts',(34.9109456796213,-65.1586387934241,
12.));
#125856=CARTESIAN_POINT('Ctrl Pts',(34.9088384918336,-65.1315686003516,
0.));
#125857=CARTESIAN_POINT('Ctrl Pts',(34.9088384918336,-65.1315686003516,
12.));
#125858=CARTESIAN_POINT('Ctrl Pts',(34.9067094130398,-65.1045361803122,
0.));
#125859=CARTESIAN_POINT('Ctrl Pts',(34.9067094130398,-65.1045361803122,
12.));
#125860=CARTESIAN_POINT('Ctrl Pts',(34.9045584960508,-65.0775416167086,
0.));
#125861=CARTESIAN_POINT('Ctrl Pts',(34.9045584960508,-65.0775416167086,
12.));
#125862=CARTESIAN_POINT('Ctrl Pts',(34.9023857937865,-65.0505849930172,
0.));
#125863=CARTESIAN_POINT('Ctrl Pts',(34.9023857937865,-65.0505849930172,
12.));
#125864=CARTESIAN_POINT('Ctrl Pts',(34.9001913596416,-65.0236663932328,
0.));
#125865=CARTESIAN_POINT('Ctrl Pts',(34.9001913596416,-65.0236663932328,
12.));
#125866=CARTESIAN_POINT('Ctrl Pts',(34.8979752478615,-64.9967859023212,
0.));
#125867=CARTESIAN_POINT('Ctrl Pts',(34.8979752478615,-64.9967859023212,
12.));
#125868=CARTESIAN_POINT('Ctrl Pts',(34.8957375133697,-64.9699436060169,
0.));
#125869=CARTESIAN_POINT('Ctrl Pts',(34.8957375133697,-64.9699436060169,
12.));
#125870=CARTESIAN_POINT('Ctrl Pts',(34.8934782116094,-64.9431395906337,
0.));
#125871=CARTESIAN_POINT('Ctrl Pts',(34.8934782116094,-64.9431395906337,
12.));
#125872=CARTESIAN_POINT('Ctrl Pts',(34.8911973983784,-64.9163739428605,
0.));
#125873=CARTESIAN_POINT('Ctrl Pts',(34.8911973983784,-64.9163739428605,
12.));
#125874=CARTESIAN_POINT('Ctrl Pts',(34.888895129681,-64.8896467495757,0.));
#125875=CARTESIAN_POINT('Ctrl Pts',(34.888895129681,-64.8896467495757,12.));
#125876=CARTESIAN_POINT('Ctrl Pts',(34.8865714615435,-64.8629580976063,
0.));
#125877=CARTESIAN_POINT('Ctrl Pts',(34.8865714615435,-64.8629580976063,
12.));
#125878=CARTESIAN_POINT('Ctrl Pts',(34.8842264500188,-64.8363080737378,
0.));
#125879=CARTESIAN_POINT('Ctrl Pts',(34.8842264500188,-64.8363080737378,
12.));
#125880=CARTESIAN_POINT('Ctrl Pts',(34.881860151273,-64.8096967648308,0.));
#125881=CARTESIAN_POINT('Ctrl Pts',(34.881860151273,-64.8096967648308,12.));
#125882=CARTESIAN_POINT('Ctrl Pts',(34.8794726216512,-64.7831242579028,
0.));
#125883=CARTESIAN_POINT('Ctrl Pts',(34.8794726216512,-64.7831242579028,
12.));
#125884=CARTESIAN_POINT('Ctrl Pts',(34.8770639177492,-64.7565906402151,
0.));
#125885=CARTESIAN_POINT('Ctrl Pts',(34.8770639177492,-64.7565906402151,
12.));
#125886=CARTESIAN_POINT('Ctrl Pts',(34.8746340964971,-64.7300959993653,
0.));
#125887=CARTESIAN_POINT('Ctrl Pts',(34.8746340964971,-64.7300959993653,
12.));
#125888=CARTESIAN_POINT('Ctrl Pts',(34.8721832151974,-64.7036404233306,
0.));
#125889=CARTESIAN_POINT('Ctrl Pts',(34.8721832151974,-64.7036404233306,
12.));
#125890=CARTESIAN_POINT('Ctrl Pts',(34.8697113314789,-64.6772240004228,
0.));
#125891=CARTESIAN_POINT('Ctrl Pts',(34.8697113314789,-64.6772240004228,
12.));
#125892=CARTESIAN_POINT('Ctrl Pts',(34.8672185032719,-64.65084681926,0.));
#125893=CARTESIAN_POINT('Ctrl Pts',(34.8672185032719,-64.65084681926,12.));
#125894=CARTESIAN_POINT('Ctrl Pts',(34.8647047887774,-64.6245089687277,
0.));
#125895=CARTESIAN_POINT('Ctrl Pts',(34.8647047887774,-64.6245089687277,
12.));
#125896=CARTESIAN_POINT('Ctrl Pts',(34.8621702464401,-64.5982105379384,
0.));
#125897=CARTESIAN_POINT('Ctrl Pts',(34.8621702464401,-64.5982105379384,
12.));
#125898=CARTESIAN_POINT('Ctrl Pts',(34.8596149349256,-64.5719516161927,
0.));
#125899=CARTESIAN_POINT('Ctrl Pts',(34.8596149349256,-64.5719516161927,
12.));
#125900=CARTESIAN_POINT('Ctrl Pts',(34.857038913134,-64.5457322930088,0.));
#125901=CARTESIAN_POINT('Ctrl Pts',(34.857038913134,-64.5457322930088,12.));
#125902=CARTESIAN_POINT('Ctrl Pts',(34.8544422402118,-64.5195526581407,
0.));
#125903=CARTESIAN_POINT('Ctrl Pts',(34.8544422402118,-64.5195526581407,
12.));
#125904=CARTESIAN_POINT('Ctrl Pts',(34.851824975568,-64.4934128015985,0.));
#125905=CARTESIAN_POINT('Ctrl Pts',(34.851824975568,-64.4934128015985,12.));
#125906=CARTESIAN_POINT('Ctrl Pts',(34.8491871788895,-64.4673128136625,
0.));
#125907=CARTESIAN_POINT('Ctrl Pts',(34.8491871788895,-64.4673128136625,
12.));
#125908=CARTESIAN_POINT('Ctrl Pts',(34.8465289101621,-64.4412527848969,
0.));
#125909=CARTESIAN_POINT('Ctrl Pts',(34.8465289101621,-64.4412527848969,
12.));
#125910=CARTESIAN_POINT('Ctrl Pts',(34.8438502296664,-64.4152328061515,
0.));
#125911=CARTESIAN_POINT('Ctrl Pts',(34.8438502296664,-64.4152328061515,
12.));
#125912=CARTESIAN_POINT('Ctrl Pts',(34.8411511979702,-64.3892529685607,
0.));
#125913=CARTESIAN_POINT('Ctrl Pts',(34.8411511979702,-64.3892529685607,
12.));
#125914=CARTESIAN_POINT('Ctrl Pts',(34.8384318759248,-64.3633133635383,
0.));
#125915=CARTESIAN_POINT('Ctrl Pts',(34.8384318759248,-64.3633133635383,
12.));
#125916=CARTESIAN_POINT('Ctrl Pts',(34.8356923246617,-64.3374140827712,
0.));
#125917=CARTESIAN_POINT('Ctrl Pts',(34.8356923246617,-64.3374140827712,
12.));
#125918=CARTESIAN_POINT('Ctrl Pts',(34.8329326055918,-64.3115552182063,
0.));
#125919=CARTESIAN_POINT('Ctrl Pts',(34.8329326055918,-64.3115552182063,
12.));
#125920=CARTESIAN_POINT('Ctrl Pts',(34.8301527804054,-64.285736862052,0.));
#125921=CARTESIAN_POINT('Ctrl Pts',(34.8301527804054,-64.285736862052,12.));
#125922=CARTESIAN_POINT('Ctrl Pts',(34.8273529110743,-64.2599591067916,
0.));
#125923=CARTESIAN_POINT('Ctrl Pts',(34.8273529110743,-64.2599591067916,
12.));
#125924=CARTESIAN_POINT('Ctrl Pts',(34.8245330598559,-64.234222045188,0.));
#125925=CARTESIAN_POINT('Ctrl Pts',(34.8245330598559,-64.234222045188,12.));
#125926=CARTESIAN_POINT('Ctrl Pts',(34.8216932892968,-64.2085257702884,
0.));
#125927=CARTESIAN_POINT('Ctrl Pts',(34.8216932892968,-64.2085257702884,
12.));
#125928=CARTESIAN_POINT('Ctrl Pts',(34.8188336622418,-64.1828703754236,
0.));
#125929=CARTESIAN_POINT('Ctrl Pts',(34.8188336622418,-64.1828703754236,
12.));
#125930=CARTESIAN_POINT('Ctrl Pts',(34.8159542418374,-64.1572559542086,
0.));
#125931=CARTESIAN_POINT('Ctrl Pts',(34.8159542418374,-64.1572559542086,
12.));
#125932=CARTESIAN_POINT('Ctrl Pts',(34.8130550915286,-64.1316826005506,
0.));
#125933=CARTESIAN_POINT('Ctrl Pts',(34.8130550915286,-64.1316826005506,
12.));
#125934=CARTESIAN_POINT('Ctrl Pts',(34.8101362750597,-64.1061504086516,
0.));
#125935=CARTESIAN_POINT('Ctrl Pts',(34.8101362750597,-64.1061504086516,
12.));
#125936=CARTESIAN_POINT('Ctrl Pts',(34.8071978564747,-64.0806594730085,
0.));
#125937=CARTESIAN_POINT('Ctrl Pts',(34.8071978564747,-64.0806594730085,
12.));
#125938=CARTESIAN_POINT('Ctrl Pts',(34.804239900121,-64.0552098884096,0.));
#125939=CARTESIAN_POINT('Ctrl Pts',(34.804239900121,-64.0552098884096,12.));
#125940=CARTESIAN_POINT('Ctrl Pts',(34.8012624706526,-64.0298017499294,
0.));
#125941=CARTESIAN_POINT('Ctrl Pts',(34.8012624706526,-64.0298017499294,
12.));
#125942=CARTESIAN_POINT('Ctrl Pts',(34.7982656330293,-64.0044351529402,
0.));
#125943=CARTESIAN_POINT('Ctrl Pts',(34.7982656330293,-64.0044351529402,
12.));
#125944=CARTESIAN_POINT('Ctrl Pts',(34.7952494525177,-63.9791101931162,
0.));
#125945=CARTESIAN_POINT('Ctrl Pts',(34.7952494525177,-63.9791101931162,
12.));
#125946=CARTESIAN_POINT('Ctrl Pts',(34.7922139946942,-63.9538269664366,
0.));
#125947=CARTESIAN_POINT('Ctrl Pts',(34.7922139946942,-63.9538269664366,
12.));
#125948=CARTESIAN_POINT('Ctrl Pts',(34.7891593254488,-63.9285855691845,
0.));
#125949=CARTESIAN_POINT('Ctrl Pts',(34.7891593254488,-63.9285855691845,
12.));
#125950=CARTESIAN_POINT('Ctrl Pts',(34.7860855109911,-63.9033860979435,
0.));
#125951=CARTESIAN_POINT('Ctrl Pts',(34.7860855109911,-63.9033860979435,
12.));
#125952=CARTESIAN_POINT('Ctrl Pts',(34.7829926178496,-63.8782286496062,
0.));
#125953=CARTESIAN_POINT('Ctrl Pts',(34.7829926178496,-63.8782286496062,
12.));
#125954=CARTESIAN_POINT('Ctrl Pts',(34.7798807128714,-63.8531133213793,
0.));
#125955=CARTESIAN_POINT('Ctrl Pts',(34.7798807128714,-63.8531133213793,
12.));
#125956=CARTESIAN_POINT('Ctrl Pts',(34.7767498632242,-63.8280402107856,
0.));
#125957=CARTESIAN_POINT('Ctrl Pts',(34.7767498632242,-63.8280402107856,
12.));
#125958=CARTESIAN_POINT('Ctrl Pts',(34.7736001363992,-63.8030094156639,
0.));
#125959=CARTESIAN_POINT('Ctrl Pts',(34.7736001363992,-63.8030094156639,
12.));
#125960=CARTESIAN_POINT('Ctrl Pts',(34.7704316002171,-63.778021034163,0.));
#125961=CARTESIAN_POINT('Ctrl Pts',(34.7704316002171,-63.778021034163,12.));
#125962=CARTESIAN_POINT('Ctrl Pts',(34.7672443228274,-63.7530751647494,
0.));
#125963=CARTESIAN_POINT('Ctrl Pts',(34.7672443228274,-63.7530751647494,
12.));
#125964=CARTESIAN_POINT('Ctrl Pts',(34.76403837271,-63.7281719062149,0.));
#125965=CARTESIAN_POINT('Ctrl Pts',(34.76403837271,-63.7281719062149,12.));
#125966=CARTESIAN_POINT('Ctrl Pts',(34.7608138186759,-63.7033113576786,
0.));
#125967=CARTESIAN_POINT('Ctrl Pts',(34.7608138186759,-63.7033113576786,
12.));
#125968=CARTESIAN_POINT('Ctrl Pts',(34.7575707298713,-63.6784936185885,
0.));
#125969=CARTESIAN_POINT('Ctrl Pts',(34.7575707298713,-63.6784936185885,
12.));
#125970=CARTESIAN_POINT('Ctrl Pts',(34.7543091757833,-63.6537187887159,
0.));
#125971=CARTESIAN_POINT('Ctrl Pts',(34.7543091757833,-63.6537187887159,
12.));
#125972=CARTESIAN_POINT('Ctrl Pts',(34.7510292262406,-63.6289869681604,
0.));
#125973=CARTESIAN_POINT('Ctrl Pts',(34.7510292262406,-63.6289869681604,
12.));
#125974=CARTESIAN_POINT('Ctrl Pts',(34.7477309514136,-63.6042982573588,
0.));
#125975=CARTESIAN_POINT('Ctrl Pts',(34.7477309514136,-63.6042982573588,
12.));
#125976=CARTESIAN_POINT('Ctrl Pts',(34.744414421816,-63.5796527570872,0.));
#125977=CARTESIAN_POINT('Ctrl Pts',(34.744414421816,-63.5796527570872,12.));
#125978=CARTESIAN_POINT('Ctrl Pts',(34.741079708308,-63.5550505684626,0.));
#125979=CARTESIAN_POINT('Ctrl Pts',(34.741079708308,-63.5550505684626,12.));
#125980=CARTESIAN_POINT('Ctrl Pts',(34.7377268821025,-63.5304917929386,
0.));
#125981=CARTESIAN_POINT('Ctrl Pts',(34.7377268821025,-63.5304917929386,
12.));
#125982=CARTESIAN_POINT('Ctrl Pts',(34.7343560147667,-63.505976532309,0.));
#125983=CARTESIAN_POINT('Ctrl Pts',(34.7343560147667,-63.505976532309,12.));
#125984=CARTESIAN_POINT('Ctrl Pts',(34.7309671782213,-63.4815048887166,
0.));
#125985=CARTESIAN_POINT('Ctrl Pts',(34.7309671782213,-63.4815048887166,
12.));
#125986=CARTESIAN_POINT('Ctrl Pts',(34.7275604447438,-63.4570769646569,
0.));
#125987=CARTESIAN_POINT('Ctrl Pts',(34.7275604447438,-63.4570769646569,
12.));
#125988=CARTESIAN_POINT('Ctrl Pts',(34.72413588697,-63.4326928629795,0.));
#125989=CARTESIAN_POINT('Ctrl Pts',(34.72413588697,-63.4326928629795,12.));
#125990=CARTESIAN_POINT('Ctrl Pts',(34.7206935779007,-63.4083526868837,
0.));
#125991=CARTESIAN_POINT('Ctrl Pts',(34.7206935779007,-63.4083526868837,
12.));
#125992=CARTESIAN_POINT('Ctrl Pts',(34.7172335909038,-63.3840565399208,
0.));
#125993=CARTESIAN_POINT('Ctrl Pts',(34.7172335909038,-63.3840565399208,
12.));
#125994=CARTESIAN_POINT('Ctrl Pts',(34.7137559997145,-63.3598045260053,
0.));
#125995=CARTESIAN_POINT('Ctrl Pts',(34.7137559997145,-63.3598045260053,
12.));
#125996=CARTESIAN_POINT('Ctrl Pts',(34.7102608784374,-63.3355967494172,
0.));
#125997=CARTESIAN_POINT('Ctrl Pts',(34.7102608784374,-63.3355967494172,
12.));
#125998=CARTESIAN_POINT('Ctrl Pts',(34.706748301549,-63.3114333148048,0.));
#125999=CARTESIAN_POINT('Ctrl Pts',(34.706748301549,-63.3114333148048,12.));
#126000=CARTESIAN_POINT('Ctrl Pts',(34.703218343904,-63.2873143271807,0.));
#126001=CARTESIAN_POINT('Ctrl Pts',(34.703218343904,-63.2873143271807,12.));
#126002=CARTESIAN_POINT('Ctrl Pts',(34.6996710807378,-63.2632398919225,
0.));
#126003=CARTESIAN_POINT('Ctrl Pts',(34.6996710807378,-63.2632398919225,
12.));
#126004=CARTESIAN_POINT('Ctrl Pts',(34.6961065876666,-63.2392101147847,
0.));
#126005=CARTESIAN_POINT('Ctrl Pts',(34.6961065876666,-63.2392101147847,
12.));
#126006=CARTESIAN_POINT('Ctrl Pts',(34.6925249406896,-63.2152251019012,
0.));
#126007=CARTESIAN_POINT('Ctrl Pts',(34.6925249406896,-63.2152251019012,
12.));
#126008=CARTESIAN_POINT('Ctrl Pts',(34.6889262161924,-63.1912849597888,
0.));
#126009=CARTESIAN_POINT('Ctrl Pts',(34.6889262161924,-63.1912849597888,
12.));
#126010=CARTESIAN_POINT('Ctrl Pts',(34.6853104909518,-63.1673897953429,
0.));
#126011=CARTESIAN_POINT('Ctrl Pts',(34.6853104909518,-63.1673897953429,
12.));
#126012=CARTESIAN_POINT('Ctrl Pts',(34.6816778421402,-63.1435397158389,
0.));
#126013=CARTESIAN_POINT('Ctrl Pts',(34.6816778421402,-63.1435397158389,
12.));
#126014=CARTESIAN_POINT('Ctrl Pts',(34.6780283473251,-63.119734828943,0.));
#126015=CARTESIAN_POINT('Ctrl Pts',(34.6780283473251,-63.119734828943,12.));
#126016=CARTESIAN_POINT('Ctrl Pts',(34.674362084472,-63.0959752427168,0.));
#126017=CARTESIAN_POINT('Ctrl Pts',(34.674362084472,-63.0959752427168,12.));
#126018=CARTESIAN_POINT('Ctrl Pts',(34.670679131947,-63.0722610656194,0.));
#126019=CARTESIAN_POINT('Ctrl Pts',(34.670679131947,-63.0722610656194,12.));
#126020=CARTESIAN_POINT('Ctrl Pts',(34.6669795685228,-63.0485924065045,
0.));
#126021=CARTESIAN_POINT('Ctrl Pts',(34.6669795685228,-63.0485924065045,
12.));
#126022=CARTESIAN_POINT('Ctrl Pts',(34.6632634733824,-63.0249693746208,
0.));
#126023=CARTESIAN_POINT('Ctrl Pts',(34.6632634733824,-63.0249693746208,
12.));
#126024=CARTESIAN_POINT('Ctrl Pts',(34.659530926119,-63.0013920796235,0.));
#126025=CARTESIAN_POINT('Ctrl Pts',(34.659530926119,-63.0013920796235,12.));
#126026=CARTESIAN_POINT('Ctrl Pts',(34.6557820067392,-62.9778606315783,
0.));
#126027=CARTESIAN_POINT('Ctrl Pts',(34.6557820067392,-62.9778606315783,
12.));
#126028=CARTESIAN_POINT('Ctrl Pts',(34.6520167956655,-62.9543751409646,
0.));
#126029=CARTESIAN_POINT('Ctrl Pts',(34.6520167956655,-62.9543751409646,
12.));
#126030=CARTESIAN_POINT('Ctrl Pts',(34.6482353737424,-62.9309357186717,
0.));
#126031=CARTESIAN_POINT('Ctrl Pts',(34.6482353737424,-62.9309357186717,
12.));
#126032=CARTESIAN_POINT('Ctrl Pts',(34.644437822241,-62.9075424760015,0.));
#126033=CARTESIAN_POINT('Ctrl Pts',(34.644437822241,-62.9075424760015,12.));
#126034=CARTESIAN_POINT('Ctrl Pts',(34.6406242228591,-62.8841955246794,
0.));
#126035=CARTESIAN_POINT('Ctrl Pts',(34.6406242228591,-62.8841955246794,
12.));
#126036=CARTESIAN_POINT('Ctrl Pts',(34.6367946577234,-62.8608949768571,
0.));
#126037=CARTESIAN_POINT('Ctrl Pts',(34.6367946577234,-62.8608949768571,
12.));
#126038=CARTESIAN_POINT('Ctrl Pts',(34.6329492093935,-62.8376409451175,
0.));
#126039=CARTESIAN_POINT('Ctrl Pts',(34.6329492093935,-62.8376409451175,
12.));
#126040=CARTESIAN_POINT('Ctrl Pts',(34.6290879608672,-62.8144335424697,
0.));
#126041=CARTESIAN_POINT('Ctrl Pts',(34.6290879608672,-62.8144335424697,
12.));
#126042=CARTESIAN_POINT('Ctrl Pts',(34.6252109955852,-62.7912728823518,
0.));
#126043=CARTESIAN_POINT('Ctrl Pts',(34.6252109955852,-62.7912728823518,
12.));
#126044=CARTESIAN_POINT('Ctrl Pts',(34.6213183974317,-62.7681590786429,
0.));
#126045=CARTESIAN_POINT('Ctrl Pts',(34.6213183974317,-62.7681590786429,
12.));
#126046=CARTESIAN_POINT('Ctrl Pts',(34.6174102507374,-62.7450922456676,
0.));
#126047=CARTESIAN_POINT('Ctrl Pts',(34.6174102507374,-62.7450922456676,
12.));
#126048=CARTESIAN_POINT('Ctrl Pts',(34.6134866402836,-62.7220724981995,
0.));
#126049=CARTESIAN_POINT('Ctrl Pts',(34.6134866402836,-62.7220724981995,
12.));
#126050=CARTESIAN_POINT('Ctrl Pts',(34.6095476513076,-62.6990999514563,
0.));
#126051=CARTESIAN_POINT('Ctrl Pts',(34.6095476513076,-62.6990999514563,
12.));
#126052=CARTESIAN_POINT('Ctrl Pts',(34.6055933695069,-62.6761747211037,
0.));
#126053=CARTESIAN_POINT('Ctrl Pts',(34.6055933695069,-62.6761747211037,
12.));
#126054=CARTESIAN_POINT('Ctrl Pts',(34.6016238810398,-62.6532969232658,
0.));
#126055=CARTESIAN_POINT('Ctrl Pts',(34.6016238810398,-62.6532969232658,
12.));
#126056=CARTESIAN_POINT('Ctrl Pts',(34.5976392725296,-62.6304666745307,
0.));
#126057=CARTESIAN_POINT('Ctrl Pts',(34.5976392725296,-62.6304666745307,
12.));
#126058=CARTESIAN_POINT('Ctrl Pts',(34.5936396310679,-62.6076840919536,
0.));
#126059=CARTESIAN_POINT('Ctrl Pts',(34.5936396310679,-62.6076840919536,
12.));
#126060=CARTESIAN_POINT('Ctrl Pts',(34.5896250442216,-62.5849492930533,
0.));
#126061=CARTESIAN_POINT('Ctrl Pts',(34.5896250442216,-62.5849492930533,
12.));
#126062=CARTESIAN_POINT('Ctrl Pts',(34.5855956000362,-62.5622623958161,
0.));
#126063=CARTESIAN_POINT('Ctrl Pts',(34.5855956000362,-62.5622623958161,
12.));
#126064=CARTESIAN_POINT('Ctrl Pts',(34.5815513870376,-62.5396235187079,
0.));
#126065=CARTESIAN_POINT('Ctrl Pts',(34.5815513870376,-62.5396235187079,
12.));
#126066=CARTESIAN_POINT('Ctrl Pts',(34.5774924942354,-62.5170327806781,
0.));
#126067=CARTESIAN_POINT('Ctrl Pts',(34.5774924942354,-62.5170327806781,
12.));
#126068=CARTESIAN_POINT('Ctrl Pts',(34.5734190111272,-62.4944903011628,
0.));
#126069=CARTESIAN_POINT('Ctrl Pts',(34.5734190111272,-62.4944903011628,
12.));
#126070=CARTESIAN_POINT('Ctrl Pts',(34.5693310277051,-62.4719962000808,
0.));
#126071=CARTESIAN_POINT('Ctrl Pts',(34.5693310277051,-62.4719962000808,
12.));
#126072=CARTESIAN_POINT('Ctrl Pts',(34.5652286344592,-62.4495505978393,
0.));
#126073=CARTESIAN_POINT('Ctrl Pts',(34.5652286344592,-62.4495505978393,
12.));
#126074=CARTESIAN_POINT('Ctrl Pts',(34.5611119223798,-62.4271536153459,
0.));
#126075=CARTESIAN_POINT('Ctrl Pts',(34.5611119223798,-62.4271536153459,
12.));
#126076=CARTESIAN_POINT('Ctrl Pts',(34.5569809829613,-62.4048053740127,
0.));
#126077=CARTESIAN_POINT('Ctrl Pts',(34.5569809829613,-62.4048053740127,
12.));
#126078=CARTESIAN_POINT('Ctrl Pts',(34.5528359082074,-62.3825059957601,
0.));
#126079=CARTESIAN_POINT('Ctrl Pts',(34.5528359082074,-62.3825059957601,
12.));
#126080=CARTESIAN_POINT('Ctrl Pts',(34.5486767906384,-62.3602556030127,
0.));
#126081=CARTESIAN_POINT('Ctrl Pts',(34.5486767906384,-62.3602556030127,
12.));
#126082=CARTESIAN_POINT('Ctrl Pts',(34.5445037232936,-62.338054318708,0.));
#126083=CARTESIAN_POINT('Ctrl Pts',(34.5445037232936,-62.338054318708,12.));
#126084=CARTESIAN_POINT('Ctrl Pts',(34.5403167997337,-62.3159022663058,
0.));
#126085=CARTESIAN_POINT('Ctrl Pts',(34.5403167997337,-62.3159022663058,
12.));
#126086=CARTESIAN_POINT('Ctrl Pts',(34.5361161140449,-62.2937995697926,
0.));
#126087=CARTESIAN_POINT('Ctrl Pts',(34.5361161140449,-62.2937995697926,
12.));
#126088=CARTESIAN_POINT('Ctrl Pts',(34.5319017608433,-62.2717463536828,
0.));
#126089=CARTESIAN_POINT('Ctrl Pts',(34.5319017608433,-62.2717463536828,
12.));
#126090=CARTESIAN_POINT('Ctrl Pts',(34.5276738352808,-62.2497427430135,
0.));
#126091=CARTESIAN_POINT('Ctrl Pts',(34.5276738352808,-62.2497427430135,
12.));
#126092=CARTESIAN_POINT('Ctrl Pts',(34.523432433049,-62.2277888633577,0.));
#126093=CARTESIAN_POINT('Ctrl Pts',(34.523432433049,-62.2277888633577,12.));
#126094=CARTESIAN_POINT('Ctrl Pts',(34.5191776503842,-62.2058848408347,
0.));
#126095=CARTESIAN_POINT('Ctrl Pts',(34.5191776503842,-62.2058848408347,
12.));
#126096=CARTESIAN_POINT('Ctrl Pts',(34.5149095840729,-62.1840308021171,
0.));
#126097=CARTESIAN_POINT('Ctrl Pts',(34.5149095840729,-62.1840308021171,
12.));
#126098=CARTESIAN_POINT('Ctrl Pts',(34.5106283314594,-62.1622268744336,
0.));
#126099=CARTESIAN_POINT('Ctrl Pts',(34.5106283314594,-62.1622268744336,
12.));
#126100=CARTESIAN_POINT('Ctrl Pts',(34.5063339904533,-62.1404731855686,
0.));
#126101=CARTESIAN_POINT('Ctrl Pts',(34.5063339904533,-62.1404731855686,
12.));
#126102=CARTESIAN_POINT('Ctrl Pts',(34.5020266595292,-62.1187698638705,
0.));
#126103=CARTESIAN_POINT('Ctrl Pts',(34.5020266595292,-62.1187698638705,
12.));
#126104=CARTESIAN_POINT('Ctrl Pts',(34.4977064377281,-62.0971170382565,
0.));
#126105=CARTESIAN_POINT('Ctrl Pts',(34.4977064377281,-62.0971170382565,
12.));
#126106=CARTESIAN_POINT('Ctrl Pts',(34.4933734246592,-62.0755148382136,
0.));
#126107=CARTESIAN_POINT('Ctrl Pts',(34.4933734246592,-62.0755148382136,
12.));
#126108=CARTESIAN_POINT('Ctrl Pts',(34.4890277205041,-62.0539633937944,
0.));
#126109=CARTESIAN_POINT('Ctrl Pts',(34.4890277205041,-62.0539633937944,
12.));
#126110=CARTESIAN_POINT('Ctrl Pts',(34.4846694260205,-62.0324628356152,
0.));
#126111=CARTESIAN_POINT('Ctrl Pts',(34.4846694260205,-62.0324628356152,
12.));
#126112=CARTESIAN_POINT('Ctrl Pts',(34.4802986425534,-62.0110132948807,
0.));
#126113=CARTESIAN_POINT('Ctrl Pts',(34.4802986425534,-62.0110132948807,
12.));
#126114=CARTESIAN_POINT('Ctrl Pts',(34.4759154720477,-61.9896149034009,
0.));
#126115=CARTESIAN_POINT('Ctrl Pts',(34.4759154720477,-61.9896149034009,
12.));
#126116=CARTESIAN_POINT('Ctrl Pts',(34.4715200170588,-61.9682677936048,
0.));
#126117=CARTESIAN_POINT('Ctrl Pts',(34.4715200170588,-61.9682677936048,
12.));
#126118=CARTESIAN_POINT('Ctrl Pts',(34.4671123807705,-61.9469720985512,
0.));
#126119=CARTESIAN_POINT('Ctrl Pts',(34.4671123807705,-61.9469720985512,
12.));
#126120=CARTESIAN_POINT('Ctrl Pts',(34.462692666996,-61.9257279519283,0.));
#126121=CARTESIAN_POINT('Ctrl Pts',(34.462692666996,-61.9257279519283,12.));
#126122=CARTESIAN_POINT('Ctrl Pts',(34.4582609801625,-61.9045354880424,
0.));
#126123=CARTESIAN_POINT('Ctrl Pts',(34.4582609801625,-61.9045354880424,
12.));
#126124=CARTESIAN_POINT('Ctrl Pts',(34.4538174253009,-61.883394841802,0.));
#126125=CARTESIAN_POINT('Ctrl Pts',(34.4538174253009,-61.883394841802,12.));
#126126=CARTESIAN_POINT('Ctrl Pts',(34.4493621080367,-61.8623061487031,
0.));
#126127=CARTESIAN_POINT('Ctrl Pts',(34.4493621080367,-61.8623061487031,
12.));
#126128=CARTESIAN_POINT('Ctrl Pts',(34.4448951345753,-61.8412695447951,
0.));
#126129=CARTESIAN_POINT('Ctrl Pts',(34.4448951345753,-61.8412695447951,
12.));
#126130=CARTESIAN_POINT('Ctrl Pts',(34.4404166117312,-61.8202851667247,
0.));
#126131=CARTESIAN_POINT('Ctrl Pts',(34.4404166117312,-61.8202851667247,
12.));
#126132=CARTESIAN_POINT('Ctrl Pts',(34.4359266469757,-61.7993531518052,
0.));
#126133=CARTESIAN_POINT('Ctrl Pts',(34.4359266469757,-61.7993531518052,
12.));
#126134=CARTESIAN_POINT('Ctrl Pts',(34.4314253484791,-61.7784736380728,
0.));
#126135=CARTESIAN_POINT('Ctrl Pts',(34.4314253484791,-61.7784736380728,
12.));
#126136=CARTESIAN_POINT('Ctrl Pts',(34.4269128251568,-61.7576467643419,
0.));
#126137=CARTESIAN_POINT('Ctrl Pts',(34.4269128251568,-61.7576467643419,
12.));
#126138=CARTESIAN_POINT('Ctrl Pts',(34.4223891867166,-61.7368726702573,
0.));
#126139=CARTESIAN_POINT('Ctrl Pts',(34.4223891867166,-61.7368726702573,
12.));
#126140=CARTESIAN_POINT('Ctrl Pts',(34.4178545435753,-61.7161514961892,
0.));
#126141=CARTESIAN_POINT('Ctrl Pts',(34.4178545435753,-61.7161514961892,
12.));
#126142=CARTESIAN_POINT('Ctrl Pts',(34.4133090067696,-61.6954833831158,
0.));
#126143=CARTESIAN_POINT('Ctrl Pts',(34.4133090067696,-61.6954833831158,
12.));
#126144=CARTESIAN_POINT('Ctrl Pts',(34.4087526878814,-61.674868472521,0.));
#126145=CARTESIAN_POINT('Ctrl Pts',(34.4087526878814,-61.674868472521,12.));
#126146=CARTESIAN_POINT('Ctrl Pts',(34.4041856989328,-61.6543069062436,
0.));
#126147=CARTESIAN_POINT('Ctrl Pts',(34.4041856989328,-61.6543069062436,
12.));
#126148=CARTESIAN_POINT('Ctrl Pts',(34.399608152377,-61.6337988264586,0.));
#126149=CARTESIAN_POINT('Ctrl Pts',(34.399608152377,-61.6337988264586,12.));
#126150=CARTESIAN_POINT('Ctrl Pts',(34.3950201613446,-61.6133443760168,
0.));
#126151=CARTESIAN_POINT('Ctrl Pts',(34.3950201613446,-61.6133443760168,
12.));
#126152=CARTESIAN_POINT('Ctrl Pts',(34.3904218398641,-61.5929436987419,
0.));
#126153=CARTESIAN_POINT('Ctrl Pts',(34.3904218398641,-61.5929436987419,
12.));
#126154=CARTESIAN_POINT('Ctrl Pts',(34.3858133030511,-61.5725969396817,
0.));
#126155=CARTESIAN_POINT('Ctrl Pts',(34.3858133030511,-61.5725969396817,
12.));
#126156=CARTESIAN_POINT('Ctrl Pts',(34.3811946674179,-61.5523042455128,
0.));
#126157=CARTESIAN_POINT('Ctrl Pts',(34.3811946674179,-61.5523042455128,
12.));
#126158=CARTESIAN_POINT('Ctrl Pts',(34.3765660506659,-61.5320657642601,
0.));
#126159=CARTESIAN_POINT('Ctrl Pts',(34.3765660506659,-61.5320657642601,
12.));
#126160=CARTESIAN_POINT('Ctrl Pts',(34.3719275711179,-61.511881644541,0.));
#126161=CARTESIAN_POINT('Ctrl Pts',(34.3719275711179,-61.511881644541,12.));
#126162=CARTESIAN_POINT('Ctrl Pts',(34.3672793472463,-61.4917520349276,
0.));
#126163=CARTESIAN_POINT('Ctrl Pts',(34.3672793472463,-61.4917520349276,
12.));
#126164=CARTESIAN_POINT('Ctrl Pts',(34.3626214971903,-61.4716770832924,
0.));
#126165=CARTESIAN_POINT('Ctrl Pts',(34.3626214971903,-61.4716770832924,
12.));
#126166=CARTESIAN_POINT('Ctrl Pts',(34.357954138202,-61.4516569360499,0.));
#126167=CARTESIAN_POINT('Ctrl Pts',(34.357954138202,-61.4516569360499,12.));
#126168=CARTESIAN_POINT('Ctrl Pts',(34.3532773877111,-61.4316917395959,
0.));
#126169=CARTESIAN_POINT('Ctrl Pts',(34.3532773877111,-61.4316917395959,
12.));
#126170=CARTESIAN_POINT('Ctrl Pts',(34.3485913645991,-61.4117816420251,
0.));
#126171=CARTESIAN_POINT('Ctrl Pts',(34.3485913645991,-61.4117816420251,
12.));
#126172=CARTESIAN_POINT('Ctrl Pts',(34.34389619024,-61.3919267945294,0.));
#126173=CARTESIAN_POINT('Ctrl Pts',(34.34389619024,-61.3919267945294,12.));
#126174=CARTESIAN_POINT('Ctrl Pts',(34.339191990012,-61.3721273534222,0.));
#126175=CARTESIAN_POINT('Ctrl Pts',(34.339191990012,-61.3721273534222,12.));
#126176=CARTESIAN_POINT('Ctrl Pts',(34.3344788934337,-61.3523834803144,
0.));
#126177=CARTESIAN_POINT('Ctrl Pts',(34.3344788934337,-61.3523834803144,
12.));
#126178=CARTESIAN_POINT('Ctrl Pts',(34.3297570310126,-61.3326953378817,
0.));
#126179=CARTESIAN_POINT('Ctrl Pts',(34.3297570310126,-61.3326953378817,
12.));
#126180=CARTESIAN_POINT('Ctrl Pts',(34.3250265314761,-61.3130630861375,
0.));
#126181=CARTESIAN_POINT('Ctrl Pts',(34.3250265314761,-61.3130630861375,
12.));
#126182=CARTESIAN_POINT('Ctrl Pts',(34.3202875193629,-61.2934868791876,
0.));
#126183=CARTESIAN_POINT('Ctrl Pts',(34.3202875193629,-61.2934868791876,
12.));
#126184=CARTESIAN_POINT('Ctrl Pts',(34.3155401111776,-61.2739668600416,
0.));
#126185=CARTESIAN_POINT('Ctrl Pts',(34.3155401111776,-61.2739668600416,
12.));
#126186=CARTESIAN_POINT('Ctrl Pts',(34.3107844191081,-61.2545031656196,
0.));
#126187=CARTESIAN_POINT('Ctrl Pts',(34.3107844191081,-61.2545031656196,
12.));
#126188=CARTESIAN_POINT('Ctrl Pts',(34.3060205584093,-61.2350959366987,
0.));
#126189=CARTESIAN_POINT('Ctrl Pts',(34.3060205584093,-61.2350959366987,
12.));
#126190=CARTESIAN_POINT('Ctrl Pts',(34.3012486533473,-61.2157453259108,
0.));
#126191=CARTESIAN_POINT('Ctrl Pts',(34.3012486533473,-61.2157453259108,
12.));
#126192=CARTESIAN_POINT('Ctrl Pts',(34.296468844362,-61.1964515073823,0.));
#126193=CARTESIAN_POINT('Ctrl Pts',(34.296468844362,-61.1964515073823,12.));
#126194=CARTESIAN_POINT('Ctrl Pts',(34.2916812929674,-61.1772146833083,
0.));
#126195=CARTESIAN_POINT('Ctrl Pts',(34.2916812929674,-61.1772146833083,
12.));
#126196=CARTESIAN_POINT('Ctrl Pts',(34.2868861666301,-61.15803506354,0.));
#126197=CARTESIAN_POINT('Ctrl Pts',(34.2868861666301,-61.15803506354,12.));
#126198=CARTESIAN_POINT('Ctrl Pts',(34.2820836244425,-61.1389128461815,
0.));
#126199=CARTESIAN_POINT('Ctrl Pts',(34.2820836244425,-61.1389128461815,
12.));
#126200=CARTESIAN_POINT('Ctrl Pts',(34.2772738038811,-61.119848199783,0.));
#126201=CARTESIAN_POINT('Ctrl Pts',(34.2772738038811,-61.119848199783,12.));
#126202=CARTESIAN_POINT('Ctrl Pts',(34.2724568037373,-61.1008412400231,
0.));
#126203=CARTESIAN_POINT('Ctrl Pts',(34.2724568037373,-61.1008412400231,
12.));
#126204=CARTESIAN_POINT('Ctrl Pts',(34.2676326825845,-61.0818920286645,
0.));
#126205=CARTESIAN_POINT('Ctrl Pts',(34.2676326825845,-61.0818920286645,
12.));
#126206=CARTESIAN_POINT('Ctrl Pts',(34.2637677132139,-61.0667788793594,
0.));
#126207=CARTESIAN_POINT('Ctrl Pts',(34.2637677132139,-61.0667788793594,
12.));
#126208=CARTESIAN_POINT('Ctrl Pts',(34.260865800176,-61.0554700177207,0.));
#126209=CARTESIAN_POINT('Ctrl Pts',(34.260865800176,-61.0554700177207,12.));
#126210=CARTESIAN_POINT('Ctrl Pts',(34.2589297755482,-61.0479423318803,
0.));
#126211=CARTESIAN_POINT('Ctrl Pts',(34.2589297755482,-61.0479423318803,
12.));
#126212=CARTESIAN_POINT('Ctrl Pts',(34.2579614092496,-61.0441813777723,
0.));
#126213=CARTESIAN_POINT('Ctrl Pts',(34.2579614092496,-61.0441813777723,
12.));
#126214=CARTESIAN_POINT('',(34.2579614092496,-61.0441813777723,12.));
#126215=CARTESIAN_POINT('Ctrl Pts',(34.2579614092496,-61.0441813777723,
12.));
#126216=CARTESIAN_POINT('Ctrl Pts',(34.2589297755482,-61.0479423318803,
12.));
#126217=CARTESIAN_POINT('Ctrl Pts',(34.260865800176,-61.0554700177207,12.));
#126218=CARTESIAN_POINT('Ctrl Pts',(34.2637677132139,-61.0667788793594,
12.));
#126219=CARTESIAN_POINT('Ctrl Pts',(34.2676326825845,-61.0818920286645,
12.));
#126220=CARTESIAN_POINT('Ctrl Pts',(34.2724568037373,-61.1008412400231,
12.));
#126221=CARTESIAN_POINT('Ctrl Pts',(34.2772738038811,-61.119848199783,12.));
#126222=CARTESIAN_POINT('Ctrl Pts',(34.2820836244425,-61.1389128461815,
12.));
#126223=CARTESIAN_POINT('Ctrl Pts',(34.2868861666301,-61.15803506354,12.));
#126224=CARTESIAN_POINT('Ctrl Pts',(34.2916812929674,-61.1772146833083,
12.));
#126225=CARTESIAN_POINT('Ctrl Pts',(34.296468844362,-61.1964515073823,12.));
#126226=CARTESIAN_POINT('Ctrl Pts',(34.3012486533473,-61.2157453259108,
12.));
#126227=CARTESIAN_POINT('Ctrl Pts',(34.3060205584093,-61.2350959366987,
12.));
#126228=CARTESIAN_POINT('Ctrl Pts',(34.3107844191081,-61.2545031656196,
12.));
#126229=CARTESIAN_POINT('Ctrl Pts',(34.3155401111776,-61.2739668600416,
12.));
#126230=CARTESIAN_POINT('Ctrl Pts',(34.3202875193629,-61.2934868791876,
12.));
#126231=CARTESIAN_POINT('Ctrl Pts',(34.3250265314761,-61.3130630861375,
12.));
#126232=CARTESIAN_POINT('Ctrl Pts',(34.3297570310126,-61.3326953378817,
12.));
#126233=CARTESIAN_POINT('Ctrl Pts',(34.3344788934337,-61.3523834803144,
12.));
#126234=CARTESIAN_POINT('Ctrl Pts',(34.339191990012,-61.3721273534222,12.));
#126235=CARTESIAN_POINT('Ctrl Pts',(34.34389619024,-61.3919267945294,12.));
#126236=CARTESIAN_POINT('Ctrl Pts',(34.3485913645991,-61.4117816420251,
12.));
#126237=CARTESIAN_POINT('Ctrl Pts',(34.3532773877111,-61.4316917395959,
12.));
#126238=CARTESIAN_POINT('Ctrl Pts',(34.357954138202,-61.4516569360499,12.));
#126239=CARTESIAN_POINT('Ctrl Pts',(34.3626214971903,-61.4716770832924,
12.));
#126240=CARTESIAN_POINT('Ctrl Pts',(34.3672793472463,-61.4917520349276,
12.));
#126241=CARTESIAN_POINT('Ctrl Pts',(34.3719275711179,-61.511881644541,12.));
#126242=CARTESIAN_POINT('Ctrl Pts',(34.3765660506659,-61.5320657642601,
12.));
#126243=CARTESIAN_POINT('Ctrl Pts',(34.3811946674179,-61.5523042455128,
12.));
#126244=CARTESIAN_POINT('Ctrl Pts',(34.3858133030511,-61.5725969396817,
12.));
#126245=CARTESIAN_POINT('Ctrl Pts',(34.3904218398641,-61.5929436987419,
12.));
#126246=CARTESIAN_POINT('Ctrl Pts',(34.3950201613446,-61.6133443760168,
12.));
#126247=CARTESIAN_POINT('Ctrl Pts',(34.399608152377,-61.6337988264586,12.));
#126248=CARTESIAN_POINT('Ctrl Pts',(34.4041856989328,-61.6543069062436,
12.));
#126249=CARTESIAN_POINT('Ctrl Pts',(34.4087526878814,-61.674868472521,12.));
#126250=CARTESIAN_POINT('Ctrl Pts',(34.4133090067696,-61.6954833831158,
12.));
#126251=CARTESIAN_POINT('Ctrl Pts',(34.4178545435753,-61.7161514961892,
12.));
#126252=CARTESIAN_POINT('Ctrl Pts',(34.4223891867166,-61.7368726702573,
12.));
#126253=CARTESIAN_POINT('Ctrl Pts',(34.4269128251568,-61.7576467643419,
12.));
#126254=CARTESIAN_POINT('Ctrl Pts',(34.4314253484791,-61.7784736380728,
12.));
#126255=CARTESIAN_POINT('Ctrl Pts',(34.4359266469757,-61.7993531518052,
12.));
#126256=CARTESIAN_POINT('Ctrl Pts',(34.4404166117312,-61.8202851667247,
12.));
#126257=CARTESIAN_POINT('Ctrl Pts',(34.4448951345753,-61.8412695447951,
12.));
#126258=CARTESIAN_POINT('Ctrl Pts',(34.4493621080367,-61.8623061487031,
12.));
#126259=CARTESIAN_POINT('Ctrl Pts',(34.4538174253009,-61.883394841802,12.));
#126260=CARTESIAN_POINT('Ctrl Pts',(34.4582609801625,-61.9045354880424,
12.));
#126261=CARTESIAN_POINT('Ctrl Pts',(34.462692666996,-61.9257279519283,12.));
#126262=CARTESIAN_POINT('Ctrl Pts',(34.4671123807705,-61.9469720985512,
12.));
#126263=CARTESIAN_POINT('Ctrl Pts',(34.4715200170588,-61.9682677936048,
12.));
#126264=CARTESIAN_POINT('Ctrl Pts',(34.4759154720477,-61.9896149034009,
12.));
#126265=CARTESIAN_POINT('Ctrl Pts',(34.4802986425534,-62.0110132948807,
12.));
#126266=CARTESIAN_POINT('Ctrl Pts',(34.4846694260205,-62.0324628356152,
12.));
#126267=CARTESIAN_POINT('Ctrl Pts',(34.4890277205041,-62.0539633937944,
12.));
#126268=CARTESIAN_POINT('Ctrl Pts',(34.4933734246592,-62.0755148382136,
12.));
#126269=CARTESIAN_POINT('Ctrl Pts',(34.4977064377281,-62.0971170382565,
12.));
#126270=CARTESIAN_POINT('Ctrl Pts',(34.5020266595292,-62.1187698638705,
12.));
#126271=CARTESIAN_POINT('Ctrl Pts',(34.5063339904533,-62.1404731855686,
12.));
#126272=CARTESIAN_POINT('Ctrl Pts',(34.5106283314594,-62.1622268744336,
12.));
#126273=CARTESIAN_POINT('Ctrl Pts',(34.5149095840729,-62.1840308021171,
12.));
#126274=CARTESIAN_POINT('Ctrl Pts',(34.5191776503842,-62.2058848408347,
12.));
#126275=CARTESIAN_POINT('Ctrl Pts',(34.523432433049,-62.2277888633577,12.));
#126276=CARTESIAN_POINT('Ctrl Pts',(34.5276738352808,-62.2497427430135,
12.));
#126277=CARTESIAN_POINT('Ctrl Pts',(34.5319017608433,-62.2717463536828,
12.));
#126278=CARTESIAN_POINT('Ctrl Pts',(34.5361161140449,-62.2937995697926,
12.));
#126279=CARTESIAN_POINT('Ctrl Pts',(34.5403167997337,-62.3159022663058,
12.));
#126280=CARTESIAN_POINT('Ctrl Pts',(34.5445037232936,-62.338054318708,12.));
#126281=CARTESIAN_POINT('Ctrl Pts',(34.5486767906384,-62.3602556030127,
12.));
#126282=CARTESIAN_POINT('Ctrl Pts',(34.5528359082074,-62.3825059957601,
12.));
#126283=CARTESIAN_POINT('Ctrl Pts',(34.5569809829613,-62.4048053740127,
12.));
#126284=CARTESIAN_POINT('Ctrl Pts',(34.5611119223798,-62.4271536153459,
12.));
#126285=CARTESIAN_POINT('Ctrl Pts',(34.5652286344592,-62.4495505978393,
12.));
#126286=CARTESIAN_POINT('Ctrl Pts',(34.5693310277051,-62.4719962000808,
12.));
#126287=CARTESIAN_POINT('Ctrl Pts',(34.5734190111272,-62.4944903011628,
12.));
#126288=CARTESIAN_POINT('Ctrl Pts',(34.5774924942354,-62.5170327806781,
12.));
#126289=CARTESIAN_POINT('Ctrl Pts',(34.5815513870376,-62.5396235187079,
12.));
#126290=CARTESIAN_POINT('Ctrl Pts',(34.5855956000362,-62.5622623958161,
12.));
#126291=CARTESIAN_POINT('Ctrl Pts',(34.5896250442216,-62.5849492930533,
12.));
#126292=CARTESIAN_POINT('Ctrl Pts',(34.5936396310679,-62.6076840919536,
12.));
#126293=CARTESIAN_POINT('Ctrl Pts',(34.5976392725296,-62.6304666745307,
12.));
#126294=CARTESIAN_POINT('Ctrl Pts',(34.6016238810398,-62.6532969232658,
12.));
#126295=CARTESIAN_POINT('Ctrl Pts',(34.6055933695069,-62.6761747211037,
12.));
#126296=CARTESIAN_POINT('Ctrl Pts',(34.6095476513076,-62.6990999514563,
12.));
#126297=CARTESIAN_POINT('Ctrl Pts',(34.6134866402836,-62.7220724981995,
12.));
#126298=CARTESIAN_POINT('Ctrl Pts',(34.6174102507374,-62.7450922456676,
12.));
#126299=CARTESIAN_POINT('Ctrl Pts',(34.6213183974317,-62.7681590786429,
12.));
#126300=CARTESIAN_POINT('Ctrl Pts',(34.6252109955852,-62.7912728823518,
12.));
#126301=CARTESIAN_POINT('Ctrl Pts',(34.6290879608672,-62.8144335424697,
12.));
#126302=CARTESIAN_POINT('Ctrl Pts',(34.6329492093935,-62.8376409451175,
12.));
#126303=CARTESIAN_POINT('Ctrl Pts',(34.6367946577234,-62.8608949768571,
12.));
#126304=CARTESIAN_POINT('Ctrl Pts',(34.6406242228591,-62.8841955246794,
12.));
#126305=CARTESIAN_POINT('Ctrl Pts',(34.644437822241,-62.9075424760015,12.));
#126306=CARTESIAN_POINT('Ctrl Pts',(34.6482353737424,-62.9309357186717,
12.));
#126307=CARTESIAN_POINT('Ctrl Pts',(34.6520167956655,-62.9543751409646,
12.));
#126308=CARTESIAN_POINT('Ctrl Pts',(34.6557820067392,-62.9778606315783,
12.));
#126309=CARTESIAN_POINT('Ctrl Pts',(34.659530926119,-63.0013920796235,12.));
#126310=CARTESIAN_POINT('Ctrl Pts',(34.6632634733824,-63.0249693746208,
12.));
#126311=CARTESIAN_POINT('Ctrl Pts',(34.6669795685228,-63.0485924065045,
12.));
#126312=CARTESIAN_POINT('Ctrl Pts',(34.670679131947,-63.0722610656194,12.));
#126313=CARTESIAN_POINT('Ctrl Pts',(34.674362084472,-63.0959752427168,12.));
#126314=CARTESIAN_POINT('Ctrl Pts',(34.6780283473251,-63.119734828943,12.));
#126315=CARTESIAN_POINT('Ctrl Pts',(34.6816778421402,-63.1435397158389,
12.));
#126316=CARTESIAN_POINT('Ctrl Pts',(34.6853104909518,-63.1673897953429,
12.));
#126317=CARTESIAN_POINT('Ctrl Pts',(34.6889262161924,-63.1912849597888,
12.));
#126318=CARTESIAN_POINT('Ctrl Pts',(34.6925249406896,-63.2152251019012,
12.));
#126319=CARTESIAN_POINT('Ctrl Pts',(34.6961065876666,-63.2392101147847,
12.));
#126320=CARTESIAN_POINT('Ctrl Pts',(34.6996710807378,-63.2632398919225,
12.));
#126321=CARTESIAN_POINT('Ctrl Pts',(34.703218343904,-63.2873143271807,12.));
#126322=CARTESIAN_POINT('Ctrl Pts',(34.706748301549,-63.3114333148048,12.));
#126323=CARTESIAN_POINT('Ctrl Pts',(34.7102608784374,-63.3355967494172,
12.));
#126324=CARTESIAN_POINT('Ctrl Pts',(34.7137559997145,-63.3598045260053,
12.));
#126325=CARTESIAN_POINT('Ctrl Pts',(34.7172335909038,-63.3840565399208,
12.));
#126326=CARTESIAN_POINT('Ctrl Pts',(34.7206935779007,-63.4083526868837,
12.));
#126327=CARTESIAN_POINT('Ctrl Pts',(34.72413588697,-63.4326928629795,12.));
#126328=CARTESIAN_POINT('Ctrl Pts',(34.7275604447438,-63.4570769646569,
12.));
#126329=CARTESIAN_POINT('Ctrl Pts',(34.7309671782213,-63.4815048887166,
12.));
#126330=CARTESIAN_POINT('Ctrl Pts',(34.7343560147667,-63.505976532309,12.));
#126331=CARTESIAN_POINT('Ctrl Pts',(34.7377268821025,-63.5304917929386,
12.));
#126332=CARTESIAN_POINT('Ctrl Pts',(34.741079708308,-63.5550505684626,12.));
#126333=CARTESIAN_POINT('Ctrl Pts',(34.744414421816,-63.5796527570872,12.));
#126334=CARTESIAN_POINT('Ctrl Pts',(34.7477309514136,-63.6042982573588,
12.));
#126335=CARTESIAN_POINT('Ctrl Pts',(34.7510292262406,-63.6289869681604,
12.));
#126336=CARTESIAN_POINT('Ctrl Pts',(34.7543091757833,-63.6537187887159,
12.));
#126337=CARTESIAN_POINT('Ctrl Pts',(34.7575707298713,-63.6784936185885,
12.));
#126338=CARTESIAN_POINT('Ctrl Pts',(34.7608138186759,-63.7033113576786,
12.));
#126339=CARTESIAN_POINT('Ctrl Pts',(34.76403837271,-63.7281719062149,12.));
#126340=CARTESIAN_POINT('Ctrl Pts',(34.7672443228274,-63.7530751647494,
12.));
#126341=CARTESIAN_POINT('Ctrl Pts',(34.7704316002171,-63.778021034163,12.));
#126342=CARTESIAN_POINT('Ctrl Pts',(34.7736001363992,-63.8030094156639,
12.));
#126343=CARTESIAN_POINT('Ctrl Pts',(34.7767498632242,-63.8280402107856,
12.));
#126344=CARTESIAN_POINT('Ctrl Pts',(34.7798807128714,-63.8531133213793,
12.));
#126345=CARTESIAN_POINT('Ctrl Pts',(34.7829926178496,-63.8782286496062,
12.));
#126346=CARTESIAN_POINT('Ctrl Pts',(34.7860855109911,-63.9033860979435,
12.));
#126347=CARTESIAN_POINT('Ctrl Pts',(34.7891593254488,-63.9285855691845,
12.));
#126348=CARTESIAN_POINT('Ctrl Pts',(34.7922139946942,-63.9538269664366,
12.));
#126349=CARTESIAN_POINT('Ctrl Pts',(34.7952494525177,-63.9791101931162,
12.));
#126350=CARTESIAN_POINT('Ctrl Pts',(34.7982656330293,-64.0044351529402,
12.));
#126351=CARTESIAN_POINT('Ctrl Pts',(34.8012624706526,-64.0298017499294,
12.));
#126352=CARTESIAN_POINT('Ctrl Pts',(34.804239900121,-64.0552098884096,12.));
#126353=CARTESIAN_POINT('Ctrl Pts',(34.8071978564747,-64.0806594730085,
12.));
#126354=CARTESIAN_POINT('Ctrl Pts',(34.8101362750597,-64.1061504086516,
12.));
#126355=CARTESIAN_POINT('Ctrl Pts',(34.8130550915286,-64.1316826005506,
12.));
#126356=CARTESIAN_POINT('Ctrl Pts',(34.8159542418374,-64.1572559542086,
12.));
#126357=CARTESIAN_POINT('Ctrl Pts',(34.8188336622418,-64.1828703754236,
12.));
#126358=CARTESIAN_POINT('Ctrl Pts',(34.8216932892968,-64.2085257702884,
12.));
#126359=CARTESIAN_POINT('Ctrl Pts',(34.8245330598559,-64.234222045188,12.));
#126360=CARTESIAN_POINT('Ctrl Pts',(34.8273529110743,-64.2599591067916,
12.));
#126361=CARTESIAN_POINT('Ctrl Pts',(34.8301527804054,-64.285736862052,12.));
#126362=CARTESIAN_POINT('Ctrl Pts',(34.8329326055918,-64.3115552182063,
12.));
#126363=CARTESIAN_POINT('Ctrl Pts',(34.8356923246617,-64.3374140827712,
12.));
#126364=CARTESIAN_POINT('Ctrl Pts',(34.8384318759248,-64.3633133635383,
12.));
#126365=CARTESIAN_POINT('Ctrl Pts',(34.8411511979702,-64.3892529685607,
12.));
#126366=CARTESIAN_POINT('Ctrl Pts',(34.8438502296664,-64.4152328061515,
12.));
#126367=CARTESIAN_POINT('Ctrl Pts',(34.8465289101621,-64.4412527848969,
12.));
#126368=CARTESIAN_POINT('Ctrl Pts',(34.8491871788895,-64.4673128136625,
12.));
#126369=CARTESIAN_POINT('Ctrl Pts',(34.851824975568,-64.4934128015985,12.));
#126370=CARTESIAN_POINT('Ctrl Pts',(34.8544422402118,-64.5195526581407,
12.));
#126371=CARTESIAN_POINT('Ctrl Pts',(34.857038913134,-64.5457322930088,12.));
#126372=CARTESIAN_POINT('Ctrl Pts',(34.8596149349256,-64.5719516161927,
12.));
#126373=CARTESIAN_POINT('Ctrl Pts',(34.8621702464401,-64.5982105379384,
12.));
#126374=CARTESIAN_POINT('Ctrl Pts',(34.8647047887774,-64.6245089687277,
12.));
#126375=CARTESIAN_POINT('Ctrl Pts',(34.8672185032719,-64.65084681926,12.));
#126376=CARTESIAN_POINT('Ctrl Pts',(34.8697113314789,-64.6772240004228,
12.));
#126377=CARTESIAN_POINT('Ctrl Pts',(34.8721832151974,-64.7036404233306,
12.));
#126378=CARTESIAN_POINT('Ctrl Pts',(34.8746340964971,-64.7300959993653,
12.));
#126379=CARTESIAN_POINT('Ctrl Pts',(34.8770639177492,-64.7565906402151,
12.));
#126380=CARTESIAN_POINT('Ctrl Pts',(34.8794726216512,-64.7831242579028,
12.));
#126381=CARTESIAN_POINT('Ctrl Pts',(34.881860151273,-64.8096967648308,12.));
#126382=CARTESIAN_POINT('Ctrl Pts',(34.8842264500188,-64.8363080737378,
12.));
#126383=CARTESIAN_POINT('Ctrl Pts',(34.8865714615435,-64.8629580976063,
12.));
#126384=CARTESIAN_POINT('Ctrl Pts',(34.888895129681,-64.8896467495757,12.));
#126385=CARTESIAN_POINT('Ctrl Pts',(34.8911973983784,-64.9163739428605,
12.));
#126386=CARTESIAN_POINT('Ctrl Pts',(34.8934782116094,-64.9431395906337,
12.));
#126387=CARTESIAN_POINT('Ctrl Pts',(34.8957375133697,-64.9699436060169,
12.));
#126388=CARTESIAN_POINT('Ctrl Pts',(34.8979752478615,-64.9967859023212,
12.));
#126389=CARTESIAN_POINT('Ctrl Pts',(34.9001913596416,-65.0236663932328,
12.));
#126390=CARTESIAN_POINT('Ctrl Pts',(34.9023857937865,-65.0505849930172,
12.));
#126391=CARTESIAN_POINT('Ctrl Pts',(34.9045584960508,-65.0775416167086,
12.));
#126392=CARTESIAN_POINT('Ctrl Pts',(34.9067094130398,-65.1045361803122,
12.));
#126393=CARTESIAN_POINT('Ctrl Pts',(34.9088384918336,-65.1315686003516,
12.));
#126394=CARTESIAN_POINT('Ctrl Pts',(34.9109456796213,-65.1586387934241,
12.));
#126395=CARTESIAN_POINT('Ctrl Pts',(34.9130309233021,-65.1857466757092,
12.));
#126396=CARTESIAN_POINT('Ctrl Pts',(34.9150941691747,-65.2128921625824,
12.));
#126397=CARTESIAN_POINT('Ctrl Pts',(34.9171353624112,-65.2400751679549,
12.));
#126398=CARTESIAN_POINT('Ctrl Pts',(34.9191544474872,-65.267295604807,12.));
#126399=CARTESIAN_POINT('Ctrl Pts',(34.9211513691355,-65.2945533863762,
12.));
#126400=CARTESIAN_POINT('Ctrl Pts',(34.923126073183,-65.3218484271911,12.));
#126401=CARTESIAN_POINT('Ctrl Pts',(34.9250785073476,-65.3491806440537,
12.));
#126402=CARTESIAN_POINT('Ctrl Pts',(34.927008622273,-65.3765499573077,12.));
#126403=CARTESIAN_POINT('Ctrl Pts',(34.9289163717747,-65.4039562911353,
12.));
#126404=CARTESIAN_POINT('Ctrl Pts',(34.9305324724444,-65.4274804996591,
12.));
#126405=CARTESIAN_POINT('Ctrl Pts',(34.931759381316,-65.4455359575249,12.));
#126406=CARTESIAN_POINT('Ctrl Pts',(34.9326070346645,-65.4581063193889,
12.));
#126407=CARTESIAN_POINT('Ctrl Pts',(34.9330820191535,-65.4651808010818,
12.));
#126408=CARTESIAN_POINT('Ctrl Pts',(34.933187552314,-65.4667541478394,12.));
#126409=CARTESIAN_POINT('',(34.2579614092496,-61.0441813777723,0.));
#126410=CARTESIAN_POINT('',(34.2579614092496,-61.0441813777723,0.));
#126411=CARTESIAN_POINT('Ctrl Pts',(34.933187552314,-65.4667541478395,0.));
#126412=CARTESIAN_POINT('Ctrl Pts',(34.9330820191535,-65.4651808010819,
0.));
#126413=CARTESIAN_POINT('Ctrl Pts',(34.9326070346645,-65.458106319389,0.));
#126414=CARTESIAN_POINT('Ctrl Pts',(34.931759381316,-65.4455359575249,0.));
#126415=CARTESIAN_POINT('Ctrl Pts',(34.9305324724444,-65.4274804996591,
0.));
#126416=CARTESIAN_POINT('Ctrl Pts',(34.9289163717747,-65.4039562911353,
0.));
#126417=CARTESIAN_POINT('Ctrl Pts',(34.927008622273,-65.3765499573077,0.));
#126418=CARTESIAN_POINT('Ctrl Pts',(34.9250785073476,-65.3491806440537,
0.));
#126419=CARTESIAN_POINT('Ctrl Pts',(34.923126073183,-65.3218484271911,0.));
#126420=CARTESIAN_POINT('Ctrl Pts',(34.9211513691355,-65.2945533863762,
0.));
#126421=CARTESIAN_POINT('Ctrl Pts',(34.9191544474872,-65.267295604807,0.));
#126422=CARTESIAN_POINT('Ctrl Pts',(34.9171353624112,-65.2400751679549,
0.));
#126423=CARTESIAN_POINT('Ctrl Pts',(34.9150941691747,-65.2128921625824,
0.));
#126424=CARTESIAN_POINT('Ctrl Pts',(34.9130309233021,-65.1857466757092,
0.));
#126425=CARTESIAN_POINT('Ctrl Pts',(34.9109456796213,-65.1586387934241,
0.));
#126426=CARTESIAN_POINT('Ctrl Pts',(34.9088384918336,-65.1315686003516,
0.));
#126427=CARTESIAN_POINT('Ctrl Pts',(34.9067094130398,-65.1045361803122,
0.));
#126428=CARTESIAN_POINT('Ctrl Pts',(34.9045584960508,-65.0775416167086,
0.));
#126429=CARTESIAN_POINT('Ctrl Pts',(34.9023857937865,-65.0505849930172,
0.));
#126430=CARTESIAN_POINT('Ctrl Pts',(34.9001913596416,-65.0236663932328,
0.));
#126431=CARTESIAN_POINT('Ctrl Pts',(34.8979752478615,-64.9967859023212,
0.));
#126432=CARTESIAN_POINT('Ctrl Pts',(34.8957375133697,-64.9699436060169,
0.));
#126433=CARTESIAN_POINT('Ctrl Pts',(34.8934782116094,-64.9431395906337,
0.));
#126434=CARTESIAN_POINT('Ctrl Pts',(34.8911973983784,-64.9163739428605,
0.));
#126435=CARTESIAN_POINT('Ctrl Pts',(34.888895129681,-64.8896467495757,0.));
#126436=CARTESIAN_POINT('Ctrl Pts',(34.8865714615435,-64.8629580976063,
0.));
#126437=CARTESIAN_POINT('Ctrl Pts',(34.8842264500188,-64.8363080737378,
0.));
#126438=CARTESIAN_POINT('Ctrl Pts',(34.881860151273,-64.8096967648308,0.));
#126439=CARTESIAN_POINT('Ctrl Pts',(34.8794726216512,-64.7831242579028,
0.));
#126440=CARTESIAN_POINT('Ctrl Pts',(34.8770639177492,-64.7565906402151,
0.));
#126441=CARTESIAN_POINT('Ctrl Pts',(34.8746340964971,-64.7300959993653,
0.));
#126442=CARTESIAN_POINT('Ctrl Pts',(34.8721832151974,-64.7036404233306,
0.));
#126443=CARTESIAN_POINT('Ctrl Pts',(34.8697113314789,-64.6772240004228,
0.));
#126444=CARTESIAN_POINT('Ctrl Pts',(34.8672185032719,-64.65084681926,0.));
#126445=CARTESIAN_POINT('Ctrl Pts',(34.8647047887774,-64.6245089687277,
0.));
#126446=CARTESIAN_POINT('Ctrl Pts',(34.8621702464401,-64.5982105379384,
0.));
#126447=CARTESIAN_POINT('Ctrl Pts',(34.8596149349256,-64.5719516161927,
0.));
#126448=CARTESIAN_POINT('Ctrl Pts',(34.857038913134,-64.5457322930088,0.));
#126449=CARTESIAN_POINT('Ctrl Pts',(34.8544422402118,-64.5195526581407,
0.));
#126450=CARTESIAN_POINT('Ctrl Pts',(34.851824975568,-64.4934128015985,0.));
#126451=CARTESIAN_POINT('Ctrl Pts',(34.8491871788895,-64.4673128136625,
0.));
#126452=CARTESIAN_POINT('Ctrl Pts',(34.8465289101621,-64.4412527848969,
0.));
#126453=CARTESIAN_POINT('Ctrl Pts',(34.8438502296664,-64.4152328061515,
0.));
#126454=CARTESIAN_POINT('Ctrl Pts',(34.8411511979702,-64.3892529685607,
0.));
#126455=CARTESIAN_POINT('Ctrl Pts',(34.8384318759248,-64.3633133635383,
0.));
#126456=CARTESIAN_POINT('Ctrl Pts',(34.8356923246617,-64.3374140827712,
0.));
#126457=CARTESIAN_POINT('Ctrl Pts',(34.8329326055918,-64.3115552182063,
0.));
#126458=CARTESIAN_POINT('Ctrl Pts',(34.8301527804054,-64.285736862052,0.));
#126459=CARTESIAN_POINT('Ctrl Pts',(34.8273529110743,-64.2599591067916,
0.));
#126460=CARTESIAN_POINT('Ctrl Pts',(34.8245330598559,-64.234222045188,0.));
#126461=CARTESIAN_POINT('Ctrl Pts',(34.8216932892968,-64.2085257702884,
0.));
#126462=CARTESIAN_POINT('Ctrl Pts',(34.8188336622418,-64.1828703754236,
0.));
#126463=CARTESIAN_POINT('Ctrl Pts',(34.8159542418374,-64.1572559542086,
0.));
#126464=CARTESIAN_POINT('Ctrl Pts',(34.8130550915286,-64.1316826005506,
0.));
#126465=CARTESIAN_POINT('Ctrl Pts',(34.8101362750597,-64.1061504086516,
0.));
#126466=CARTESIAN_POINT('Ctrl Pts',(34.8071978564747,-64.0806594730085,
0.));
#126467=CARTESIAN_POINT('Ctrl Pts',(34.804239900121,-64.0552098884096,0.));
#126468=CARTESIAN_POINT('Ctrl Pts',(34.8012624706526,-64.0298017499294,
0.));
#126469=CARTESIAN_POINT('Ctrl Pts',(34.7982656330293,-64.0044351529402,
0.));
#126470=CARTESIAN_POINT('Ctrl Pts',(34.7952494525177,-63.9791101931162,
0.));
#126471=CARTESIAN_POINT('Ctrl Pts',(34.7922139946942,-63.9538269664366,
0.));
#126472=CARTESIAN_POINT('Ctrl Pts',(34.7891593254488,-63.9285855691845,
0.));
#126473=CARTESIAN_POINT('Ctrl Pts',(34.7860855109911,-63.9033860979435,
0.));
#126474=CARTESIAN_POINT('Ctrl Pts',(34.7829926178496,-63.8782286496062,
0.));
#126475=CARTESIAN_POINT('Ctrl Pts',(34.7798807128714,-63.8531133213793,
0.));
#126476=CARTESIAN_POINT('Ctrl Pts',(34.7767498632242,-63.8280402107856,
0.));
#126477=CARTESIAN_POINT('Ctrl Pts',(34.7736001363992,-63.8030094156639,
0.));
#126478=CARTESIAN_POINT('Ctrl Pts',(34.7704316002171,-63.778021034163,0.));
#126479=CARTESIAN_POINT('Ctrl Pts',(34.7672443228274,-63.7530751647494,
0.));
#126480=CARTESIAN_POINT('Ctrl Pts',(34.76403837271,-63.7281719062149,0.));
#126481=CARTESIAN_POINT('Ctrl Pts',(34.7608138186759,-63.7033113576786,
0.));
#126482=CARTESIAN_POINT('Ctrl Pts',(34.7575707298713,-63.6784936185885,
0.));
#126483=CARTESIAN_POINT('Ctrl Pts',(34.7543091757833,-63.6537187887159,
0.));
#126484=CARTESIAN_POINT('Ctrl Pts',(34.7510292262406,-63.6289869681604,
0.));
#126485=CARTESIAN_POINT('Ctrl Pts',(34.7477309514136,-63.6042982573588,
0.));
#126486=CARTESIAN_POINT('Ctrl Pts',(34.744414421816,-63.5796527570872,0.));
#126487=CARTESIAN_POINT('Ctrl Pts',(34.741079708308,-63.5550505684626,0.));
#126488=CARTESIAN_POINT('Ctrl Pts',(34.7377268821025,-63.5304917929386,
0.));
#126489=CARTESIAN_POINT('Ctrl Pts',(34.7343560147667,-63.505976532309,0.));
#126490=CARTESIAN_POINT('Ctrl Pts',(34.7309671782213,-63.4815048887166,
0.));
#126491=CARTESIAN_POINT('Ctrl Pts',(34.7275604447438,-63.4570769646569,
0.));
#126492=CARTESIAN_POINT('Ctrl Pts',(34.72413588697,-63.4326928629795,0.));
#126493=CARTESIAN_POINT('Ctrl Pts',(34.7206935779007,-63.4083526868837,
0.));
#126494=CARTESIAN_POINT('Ctrl Pts',(34.7172335909038,-63.3840565399208,
0.));
#126495=CARTESIAN_POINT('Ctrl Pts',(34.7137559997145,-63.3598045260053,
0.));
#126496=CARTESIAN_POINT('Ctrl Pts',(34.7102608784374,-63.3355967494172,
0.));
#126497=CARTESIAN_POINT('Ctrl Pts',(34.706748301549,-63.3114333148048,0.));
#126498=CARTESIAN_POINT('Ctrl Pts',(34.703218343904,-63.2873143271807,0.));
#126499=CARTESIAN_POINT('Ctrl Pts',(34.6996710807378,-63.2632398919225,
0.));
#126500=CARTESIAN_POINT('Ctrl Pts',(34.6961065876666,-63.2392101147847,
0.));
#126501=CARTESIAN_POINT('Ctrl Pts',(34.6925249406896,-63.2152251019012,
0.));
#126502=CARTESIAN_POINT('Ctrl Pts',(34.6889262161924,-63.1912849597888,
0.));
#126503=CARTESIAN_POINT('Ctrl Pts',(34.6853104909518,-63.1673897953429,
0.));
#126504=CARTESIAN_POINT('Ctrl Pts',(34.6816778421402,-63.1435397158389,
0.));
#126505=CARTESIAN_POINT('Ctrl Pts',(34.6780283473251,-63.119734828943,0.));
#126506=CARTESIAN_POINT('Ctrl Pts',(34.674362084472,-63.0959752427168,0.));
#126507=CARTESIAN_POINT('Ctrl Pts',(34.670679131947,-63.0722610656194,0.));
#126508=CARTESIAN_POINT('Ctrl Pts',(34.6669795685228,-63.0485924065045,
0.));
#126509=CARTESIAN_POINT('Ctrl Pts',(34.6632634733824,-63.0249693746208,
0.));
#126510=CARTESIAN_POINT('Ctrl Pts',(34.659530926119,-63.0013920796235,0.));
#126511=CARTESIAN_POINT('Ctrl Pts',(34.6557820067392,-62.9778606315783,
0.));
#126512=CARTESIAN_POINT('Ctrl Pts',(34.6520167956655,-62.9543751409646,
0.));
#126513=CARTESIAN_POINT('Ctrl Pts',(34.6482353737424,-62.9309357186717,
0.));
#126514=CARTESIAN_POINT('Ctrl Pts',(34.644437822241,-62.9075424760015,0.));
#126515=CARTESIAN_POINT('Ctrl Pts',(34.6406242228591,-62.8841955246794,
0.));
#126516=CARTESIAN_POINT('Ctrl Pts',(34.6367946577234,-62.8608949768571,
0.));
#126517=CARTESIAN_POINT('Ctrl Pts',(34.6329492093935,-62.8376409451175,
0.));
#126518=CARTESIAN_POINT('Ctrl Pts',(34.6290879608672,-62.8144335424697,
0.));
#126519=CARTESIAN_POINT('Ctrl Pts',(34.6252109955852,-62.7912728823518,
0.));
#126520=CARTESIAN_POINT('Ctrl Pts',(34.6213183974317,-62.7681590786429,
0.));
#126521=CARTESIAN_POINT('Ctrl Pts',(34.6174102507374,-62.7450922456676,
0.));
#126522=CARTESIAN_POINT('Ctrl Pts',(34.6134866402836,-62.7220724981995,
0.));
#126523=CARTESIAN_POINT('Ctrl Pts',(34.6095476513076,-62.6990999514563,
0.));
#126524=CARTESIAN_POINT('Ctrl Pts',(34.6055933695069,-62.6761747211037,
0.));
#126525=CARTESIAN_POINT('Ctrl Pts',(34.6016238810398,-62.6532969232658,
0.));
#126526=CARTESIAN_POINT('Ctrl Pts',(34.5976392725296,-62.6304666745307,
0.));
#126527=CARTESIAN_POINT('Ctrl Pts',(34.5936396310679,-62.6076840919536,
0.));
#126528=CARTESIAN_POINT('Ctrl Pts',(34.5896250442216,-62.5849492930533,
0.));
#126529=CARTESIAN_POINT('Ctrl Pts',(34.5855956000362,-62.5622623958161,
0.));
#126530=CARTESIAN_POINT('Ctrl Pts',(34.5815513870376,-62.5396235187079,
0.));
#126531=CARTESIAN_POINT('Ctrl Pts',(34.5774924942354,-62.5170327806781,
0.));
#126532=CARTESIAN_POINT('Ctrl Pts',(34.5734190111272,-62.4944903011628,
0.));
#126533=CARTESIAN_POINT('Ctrl Pts',(34.5693310277051,-62.4719962000808,
0.));
#126534=CARTESIAN_POINT('Ctrl Pts',(34.5652286344592,-62.4495505978393,
0.));
#126535=CARTESIAN_POINT('Ctrl Pts',(34.5611119223798,-62.4271536153459,
0.));
#126536=CARTESIAN_POINT('Ctrl Pts',(34.5569809829613,-62.4048053740127,
0.));
#126537=CARTESIAN_POINT('Ctrl Pts',(34.5528359082074,-62.3825059957601,
0.));
#126538=CARTESIAN_POINT('Ctrl Pts',(34.5486767906384,-62.3602556030127,
0.));
#126539=CARTESIAN_POINT('Ctrl Pts',(34.5445037232936,-62.338054318708,0.));
#126540=CARTESIAN_POINT('Ctrl Pts',(34.5403167997337,-62.3159022663058,
0.));
#126541=CARTESIAN_POINT('Ctrl Pts',(34.5361161140449,-62.2937995697926,
0.));
#126542=CARTESIAN_POINT('Ctrl Pts',(34.5319017608433,-62.2717463536828,
0.));
#126543=CARTESIAN_POINT('Ctrl Pts',(34.5276738352808,-62.2497427430135,
0.));
#126544=CARTESIAN_POINT('Ctrl Pts',(34.523432433049,-62.2277888633577,0.));
#126545=CARTESIAN_POINT('Ctrl Pts',(34.5191776503842,-62.2058848408347,
0.));
#126546=CARTESIAN_POINT('Ctrl Pts',(34.5149095840729,-62.1840308021171,
0.));
#126547=CARTESIAN_POINT('Ctrl Pts',(34.5106283314594,-62.1622268744336,
0.));
#126548=CARTESIAN_POINT('Ctrl Pts',(34.5063339904533,-62.1404731855686,
0.));
#126549=CARTESIAN_POINT('Ctrl Pts',(34.5020266595292,-62.1187698638705,
0.));
#126550=CARTESIAN_POINT('Ctrl Pts',(34.4977064377281,-62.0971170382565,
0.));
#126551=CARTESIAN_POINT('Ctrl Pts',(34.4933734246592,-62.0755148382136,
0.));
#126552=CARTESIAN_POINT('Ctrl Pts',(34.4890277205041,-62.0539633937944,
0.));
#126553=CARTESIAN_POINT('Ctrl Pts',(34.4846694260205,-62.0324628356152,
0.));
#126554=CARTESIAN_POINT('Ctrl Pts',(34.4802986425534,-62.0110132948807,
0.));
#126555=CARTESIAN_POINT('Ctrl Pts',(34.4759154720477,-61.9896149034009,
0.));
#126556=CARTESIAN_POINT('Ctrl Pts',(34.4715200170588,-61.9682677936048,
0.));
#126557=CARTESIAN_POINT('Ctrl Pts',(34.4671123807705,-61.9469720985512,
0.));
#126558=CARTESIAN_POINT('Ctrl Pts',(34.462692666996,-61.9257279519283,0.));
#126559=CARTESIAN_POINT('Ctrl Pts',(34.4582609801625,-61.9045354880424,
0.));
#126560=CARTESIAN_POINT('Ctrl Pts',(34.4538174253009,-61.883394841802,0.));
#126561=CARTESIAN_POINT('Ctrl Pts',(34.4493621080367,-61.8623061487031,
0.));
#126562=CARTESIAN_POINT('Ctrl Pts',(34.4448951345753,-61.8412695447951,
0.));
#126563=CARTESIAN_POINT('Ctrl Pts',(34.4404166117312,-61.8202851667247,
0.));
#126564=CARTESIAN_POINT('Ctrl Pts',(34.4359266469757,-61.7993531518052,
0.));
#126565=CARTESIAN_POINT('Ctrl Pts',(34.4314253484791,-61.7784736380728,
0.));
#126566=CARTESIAN_POINT('Ctrl Pts',(34.4269128251568,-61.7576467643419,
0.));
#126567=CARTESIAN_POINT('Ctrl Pts',(34.4223891867166,-61.7368726702573,
0.));
#126568=CARTESIAN_POINT('Ctrl Pts',(34.4178545435753,-61.7161514961892,
0.));
#126569=CARTESIAN_POINT('Ctrl Pts',(34.4133090067696,-61.6954833831158,
0.));
#126570=CARTESIAN_POINT('Ctrl Pts',(34.4087526878814,-61.674868472521,0.));
#126571=CARTESIAN_POINT('Ctrl Pts',(34.4041856989328,-61.6543069062436,
0.));
#126572=CARTESIAN_POINT('Ctrl Pts',(34.399608152377,-61.6337988264586,0.));
#126573=CARTESIAN_POINT('Ctrl Pts',(34.3950201613446,-61.6133443760168,
0.));
#126574=CARTESIAN_POINT('Ctrl Pts',(34.3904218398641,-61.5929436987419,
0.));
#126575=CARTESIAN_POINT('Ctrl Pts',(34.3858133030511,-61.5725969396817,
0.));
#126576=CARTESIAN_POINT('Ctrl Pts',(34.3811946674179,-61.5523042455128,
0.));
#126577=CARTESIAN_POINT('Ctrl Pts',(34.3765660506659,-61.5320657642601,
0.));
#126578=CARTESIAN_POINT('Ctrl Pts',(34.3719275711179,-61.511881644541,0.));
#126579=CARTESIAN_POINT('Ctrl Pts',(34.3672793472463,-61.4917520349276,
0.));
#126580=CARTESIAN_POINT('Ctrl Pts',(34.3626214971903,-61.4716770832924,
0.));
#126581=CARTESIAN_POINT('Ctrl Pts',(34.357954138202,-61.4516569360499,0.));
#126582=CARTESIAN_POINT('Ctrl Pts',(34.3532773877111,-61.4316917395959,
0.));
#126583=CARTESIAN_POINT('Ctrl Pts',(34.3485913645991,-61.4117816420251,
0.));
#126584=CARTESIAN_POINT('Ctrl Pts',(34.34389619024,-61.3919267945294,0.));
#126585=CARTESIAN_POINT('Ctrl Pts',(34.339191990012,-61.3721273534222,0.));
#126586=CARTESIAN_POINT('Ctrl Pts',(34.3344788934337,-61.3523834803144,
0.));
#126587=CARTESIAN_POINT('Ctrl Pts',(34.3297570310126,-61.3326953378817,
0.));
#126588=CARTESIAN_POINT('Ctrl Pts',(34.3250265314761,-61.3130630861375,
0.));
#126589=CARTESIAN_POINT('Ctrl Pts',(34.3202875193629,-61.2934868791876,
0.));
#126590=CARTESIAN_POINT('Ctrl Pts',(34.3155401111776,-61.2739668600416,
0.));
#126591=CARTESIAN_POINT('Ctrl Pts',(34.3107844191081,-61.2545031656196,
0.));
#126592=CARTESIAN_POINT('Ctrl Pts',(34.3060205584093,-61.2350959366987,
0.));
#126593=CARTESIAN_POINT('Ctrl Pts',(34.3012486533473,-61.2157453259108,
0.));
#126594=CARTESIAN_POINT('Ctrl Pts',(34.296468844362,-61.1964515073823,0.));
#126595=CARTESIAN_POINT('Ctrl Pts',(34.2916812929674,-61.1772146833083,
0.));
#126596=CARTESIAN_POINT('Ctrl Pts',(34.2868861666301,-61.15803506354,0.));
#126597=CARTESIAN_POINT('Ctrl Pts',(34.2820836244425,-61.1389128461815,
0.));
#126598=CARTESIAN_POINT('Ctrl Pts',(34.2772738038811,-61.119848199783,0.));
#126599=CARTESIAN_POINT('Ctrl Pts',(34.2724568037373,-61.1008412400231,
0.));
#126600=CARTESIAN_POINT('Ctrl Pts',(34.2676326825845,-61.0818920286645,
0.));
#126601=CARTESIAN_POINT('Ctrl Pts',(34.2637677132139,-61.0667788793594,
0.));
#126602=CARTESIAN_POINT('Ctrl Pts',(34.260865800176,-61.0554700177207,0.));
#126603=CARTESIAN_POINT('Ctrl Pts',(34.2589297755482,-61.0479423318803,
0.));
#126604=CARTESIAN_POINT('Ctrl Pts',(34.2579614092496,-61.0441813777723,
0.));
#126605=CARTESIAN_POINT('Ctrl Pts',(29.0861280018229,-68.5875145916629,
0.));
#126606=CARTESIAN_POINT('Ctrl Pts',(29.0861280018229,-68.5875145916629,
12.));
#126607=CARTESIAN_POINT('Ctrl Pts',(29.0863005247838,-68.5819214834737,
0.));
#126608=CARTESIAN_POINT('Ctrl Pts',(29.0863005247838,-68.5819214834737,
12.));
#126609=CARTESIAN_POINT('Ctrl Pts',(29.0866429722093,-68.5707386600636,
0.));
#126610=CARTESIAN_POINT('Ctrl Pts',(29.0866429722093,-68.5707386600636,
12.));
#126611=CARTESIAN_POINT('Ctrl Pts',(29.0871488478588,-68.5539746038542,
0.));
#126612=CARTESIAN_POINT('Ctrl Pts',(29.0871488478588,-68.5539746038542,
12.));
#126613=CARTESIAN_POINT('Ctrl Pts',(29.0878077571086,-68.5316428875424,
0.));
#126614=CARTESIAN_POINT('Ctrl Pts',(29.0878077571086,-68.5316428875424,
12.));
#126615=CARTESIAN_POINT('Ctrl Pts',(29.0886054060562,-68.5037621824171,
0.));
#126616=CARTESIAN_POINT('Ctrl Pts',(29.0886054060562,-68.5037621824171,
12.));
#126617=CARTESIAN_POINT('Ctrl Pts',(29.0893770688944,-68.4759154367939,
0.));
#126618=CARTESIAN_POINT('Ctrl Pts',(29.0893770688944,-68.4759154367939,
12.));
#126619=CARTESIAN_POINT('Ctrl Pts',(29.0901227535306,-68.4481026830931,
0.));
#126620=CARTESIAN_POINT('Ctrl Pts',(29.0901227535306,-68.4481026830931,
12.));
#126621=CARTESIAN_POINT('Ctrl Pts',(29.090842477089,-68.4203239694612,0.));
#126622=CARTESIAN_POINT('Ctrl Pts',(29.090842477089,-68.4203239694612,12.));
#126623=CARTESIAN_POINT('Ctrl Pts',(29.0915362699455,-68.3925793637995,
0.));
#126624=CARTESIAN_POINT('Ctrl Pts',(29.0915362699455,-68.3925793637995,
12.));
#126625=CARTESIAN_POINT('Ctrl Pts',(29.0922041749293,-68.364868951893,0.));
#126626=CARTESIAN_POINT('Ctrl Pts',(29.0922041749293,-68.364868951893,12.));
#126627=CARTESIAN_POINT('Ctrl Pts',(29.0928462428145,-68.3371928310161,
0.));
#126628=CARTESIAN_POINT('Ctrl Pts',(29.0928462428145,-68.3371928310161,
12.));
#126629=CARTESIAN_POINT('Ctrl Pts',(29.0934625288409,-68.3095511047769,
0.));
#126630=CARTESIAN_POINT('Ctrl Pts',(29.0934625288409,-68.3095511047769,
12.));
#126631=CARTESIAN_POINT('Ctrl Pts',(29.0940530889149,-68.2819438775953,
0.));
#126632=CARTESIAN_POINT('Ctrl Pts',(29.0940530889149,-68.2819438775953,
12.));
#126633=CARTESIAN_POINT('Ctrl Pts',(29.0946179757167,-68.2543712489906,
0.));
#126634=CARTESIAN_POINT('Ctrl Pts',(29.0946179757167,-68.2543712489906,
12.));
#126635=CARTESIAN_POINT('Ctrl Pts',(29.0951572355397,-68.2268333089617,
0.));
#126636=CARTESIAN_POINT('Ctrl Pts',(29.0951572355397,-68.2268333089617,
12.));
#126637=CARTESIAN_POINT('Ctrl Pts',(29.0956709104627,-68.1993301412061,
0.));
#126638=CARTESIAN_POINT('Ctrl Pts',(29.0956709104627,-68.1993301412061,
12.));
#126639=CARTESIAN_POINT('Ctrl Pts',(29.0961590399046,-68.1718618254281,
0.));
#126640=CARTESIAN_POINT('Ctrl Pts',(29.0961590399046,-68.1718618254281,
12.));
#126641=CARTESIAN_POINT('Ctrl Pts',(29.0966216624743,-68.1444284400742,
0.));
#126642=CARTESIAN_POINT('Ctrl Pts',(29.0966216624743,-68.1444284400742,
12.));
#126643=CARTESIAN_POINT('Ctrl Pts',(29.0970588175728,-68.1170300646987,
0.));
#126644=CARTESIAN_POINT('Ctrl Pts',(29.0970588175728,-68.1170300646987,
12.));
#126645=CARTESIAN_POINT('Ctrl Pts',(29.0974705474258,-68.0896667829568,
0.));
#126646=CARTESIAN_POINT('Ctrl Pts',(29.0974705474258,-68.0896667829568,
12.));
#126647=CARTESIAN_POINT('Ctrl Pts',(29.0978568968656,-68.0623386822863,
0.));
#126648=CARTESIAN_POINT('Ctrl Pts',(29.0978568968656,-68.0623386822863,
12.));
#126649=CARTESIAN_POINT('Ctrl Pts',(29.0982179124097,-68.0350458525551,
0.));
#126650=CARTESIAN_POINT('Ctrl Pts',(29.0982179124097,-68.0350458525551,
12.));
#126651=CARTESIAN_POINT('Ctrl Pts',(29.098553641553,-68.0077883850121,0.));
#126652=CARTESIAN_POINT('Ctrl Pts',(29.098553641553,-68.0077883850121,12.));
#126653=CARTESIAN_POINT('Ctrl Pts',(29.0988641320246,-67.9805663711855,
0.));
#126654=CARTESIAN_POINT('Ctrl Pts',(29.0988641320246,-67.9805663711855,
12.));
#126655=CARTESIAN_POINT('Ctrl Pts',(29.0991494309404,-67.9533799016148,
0.));
#126656=CARTESIAN_POINT('Ctrl Pts',(29.0991494309404,-67.9533799016148,
12.));
#126657=CARTESIAN_POINT('Ctrl Pts',(29.099409584422,-67.9262290652829,0.));
#126658=CARTESIAN_POINT('Ctrl Pts',(29.099409584422,-67.9262290652829,12.));
#126659=CARTESIAN_POINT('Ctrl Pts',(29.0996446380626,-67.8991139503193,
0.));
#126660=CARTESIAN_POINT('Ctrl Pts',(29.0996446380626,-67.8991139503193,
12.));
#126661=CARTESIAN_POINT('Ctrl Pts',(29.0998546372032,-67.8720346444124,
0.));
#126662=CARTESIAN_POINT('Ctrl Pts',(29.0998546372032,-67.8720346444124,
12.));
#126663=CARTESIAN_POINT('Ctrl Pts',(29.1000396272867,-67.8449912353329,
0.));
#126664=CARTESIAN_POINT('Ctrl Pts',(29.1000396272867,-67.8449912353329,
12.));
#126665=CARTESIAN_POINT('Ctrl Pts',(29.1001996541841,-67.8179838114099,
0.));
#126666=CARTESIAN_POINT('Ctrl Pts',(29.1001996541841,-67.8179838114099,
12.));
#126667=CARTESIAN_POINT('Ctrl Pts',(29.1003347645293,-67.7910124620135,
0.));
#126668=CARTESIAN_POINT('Ctrl Pts',(29.1003347645293,-67.7910124620135,
12.));
#126669=CARTESIAN_POINT('Ctrl Pts',(29.1004450055642,-67.7640772773388,
0.));
#126670=CARTESIAN_POINT('Ctrl Pts',(29.1004450055642,-67.7640772773388,
12.));
#126671=CARTESIAN_POINT('Ctrl Pts',(29.1005304249986,-67.7371783482035,
0.));
#126672=CARTESIAN_POINT('Ctrl Pts',(29.1005304249986,-67.7371783482035,
12.));
#126673=CARTESIAN_POINT('Ctrl Pts',(29.1005910708624,-67.7103157658296,
0.));
#126674=CARTESIAN_POINT('Ctrl Pts',(29.1005910708624,-67.7103157658296,
12.));
#126675=CARTESIAN_POINT('Ctrl Pts',(29.1006269913747,-67.6834896216461,
0.));
#126676=CARTESIAN_POINT('Ctrl Pts',(29.1006269913747,-67.6834896216461,
12.));
#126677=CARTESIAN_POINT('Ctrl Pts',(29.1006382347814,-67.6567000070326,
0.));
#126678=CARTESIAN_POINT('Ctrl Pts',(29.1006382347814,-67.6567000070326,
12.));
#126679=CARTESIAN_POINT('Ctrl Pts',(29.100624849358,-67.6299470133295,0.));
#126680=CARTESIAN_POINT('Ctrl Pts',(29.100624849358,-67.6299470133295,12.));
#126681=CARTESIAN_POINT('Ctrl Pts',(29.1005868834866,-67.6032307319623,
0.));
#126682=CARTESIAN_POINT('Ctrl Pts',(29.1005868834866,-67.6032307319623,
12.));
#126683=CARTESIAN_POINT('Ctrl Pts',(29.1005243857138,-67.5765512545282,
0.));
#126684=CARTESIAN_POINT('Ctrl Pts',(29.1005243857138,-67.5765512545282,
12.));
#126685=CARTESIAN_POINT('Ctrl Pts',(29.1004374048147,-67.5499086728889,
0.));
#126686=CARTESIAN_POINT('Ctrl Pts',(29.1004374048147,-67.5499086728889,
12.));
#126687=CARTESIAN_POINT('Ctrl Pts',(29.1003259898681,-67.5233030792704,
0.));
#126688=CARTESIAN_POINT('Ctrl Pts',(29.1003259898681,-67.5233030792704,
12.));
#126689=CARTESIAN_POINT('Ctrl Pts',(29.1001901902908,-67.4967345663096,
0.));
#126690=CARTESIAN_POINT('Ctrl Pts',(29.1001901902908,-67.4967345663096,
12.));
#126691=CARTESIAN_POINT('Ctrl Pts',(29.1000300557955,-67.4702032270049,
0.));
#126692=CARTESIAN_POINT('Ctrl Pts',(29.1000300557955,-67.4702032270049,
12.));
#126693=CARTESIAN_POINT('Ctrl Pts',(29.0998456363682,-67.4437091546859,
0.));
#126694=CARTESIAN_POINT('Ctrl Pts',(29.0998456363682,-67.4437091546859,
12.));
#126695=CARTESIAN_POINT('Ctrl Pts',(29.0996369822418,-67.4172524429728,
0.));
#126696=CARTESIAN_POINT('Ctrl Pts',(29.0996369822418,-67.4172524429728,
12.));
#126697=CARTESIAN_POINT('Ctrl Pts',(29.0994041438718,-67.3908331857323,
0.));
#126698=CARTESIAN_POINT('Ctrl Pts',(29.0994041438718,-67.3908331857323,
12.));
#126699=CARTESIAN_POINT('Ctrl Pts',(29.0991471719176,-67.3644514770387,
0.));
#126700=CARTESIAN_POINT('Ctrl Pts',(29.0991471719176,-67.3644514770387,
12.));
#126701=CARTESIAN_POINT('Ctrl Pts',(29.098866117253,-67.3381074112027,0.));
#126702=CARTESIAN_POINT('Ctrl Pts',(29.098866117253,-67.3381074112027,12.));
#126703=CARTESIAN_POINT('Ctrl Pts',(29.098561030977,-67.311801082792,0.));
#126704=CARTESIAN_POINT('Ctrl Pts',(29.098561030977,-67.311801082792,12.));
#126705=CARTESIAN_POINT('Ctrl Pts',(29.0982319644276,-67.2855325866517,
0.));
#126706=CARTESIAN_POINT('Ctrl Pts',(29.0982319644276,-67.2855325866517,
12.));
#126707=CARTESIAN_POINT('Ctrl Pts',(29.0978789691962,-67.2593020179209,
0.));
#126708=CARTESIAN_POINT('Ctrl Pts',(29.0978789691962,-67.2593020179209,
12.));
#126709=CARTESIAN_POINT('Ctrl Pts',(29.0975020971469,-67.2331094720471,
0.));
#126710=CARTESIAN_POINT('Ctrl Pts',(29.0975020971469,-67.2331094720471,
12.));
#126711=CARTESIAN_POINT('Ctrl Pts',(29.097101400413,-67.2069550447884,0.));
#126712=CARTESIAN_POINT('Ctrl Pts',(29.097101400413,-67.2069550447884,12.));
#126713=CARTESIAN_POINT('Ctrl Pts',(29.096676931389,-67.1808388322109,0.));
#126714=CARTESIAN_POINT('Ctrl Pts',(29.096676931389,-67.1808388322109,12.));
#126715=CARTESIAN_POINT('Ctrl Pts',(29.0962287427273,-67.1547609306843,
0.));
#126716=CARTESIAN_POINT('Ctrl Pts',(29.0962287427273,-67.1547609306843,
12.));
#126717=CARTESIAN_POINT('Ctrl Pts',(29.0957568873358,-67.1287214368746,
0.));
#126718=CARTESIAN_POINT('Ctrl Pts',(29.0957568873358,-67.1287214368746,
12.));
#126719=CARTESIAN_POINT('Ctrl Pts',(29.0952614183779,-67.1027204477311,
0.));
#126720=CARTESIAN_POINT('Ctrl Pts',(29.0952614183779,-67.1027204477311,
12.));
#126721=CARTESIAN_POINT('Ctrl Pts',(29.0947423892726,-67.0767580604879,
0.));
#126722=CARTESIAN_POINT('Ctrl Pts',(29.0947423892726,-67.0767580604879,
12.));
#126723=CARTESIAN_POINT('Ctrl Pts',(29.0941998536958,-67.0508343726777,
0.));
#126724=CARTESIAN_POINT('Ctrl Pts',(29.0941998536958,-67.0508343726777,
12.));
#126725=CARTESIAN_POINT('Ctrl Pts',(29.0936338655828,-67.0249494821363,
0.));
#126726=CARTESIAN_POINT('Ctrl Pts',(29.0936338655828,-67.0249494821363,
12.));
#126727=CARTESIAN_POINT('Ctrl Pts',(29.0930444791328,-66.9991034870083,
0.));
#126728=CARTESIAN_POINT('Ctrl Pts',(29.0930444791328,-66.9991034870083,
12.));
#126729=CARTESIAN_POINT('Ctrl Pts',(29.092431748817,-66.9732964857466,0.));
#126730=CARTESIAN_POINT('Ctrl Pts',(29.092431748817,-66.9732964857466,12.));
#126731=CARTESIAN_POINT('Ctrl Pts',(29.0917957293826,-66.9475285771135,
0.));
#126732=CARTESIAN_POINT('Ctrl Pts',(29.0917957293826,-66.9475285771135,
12.));
#126733=CARTESIAN_POINT('Ctrl Pts',(29.0911364758486,-66.9217998601885,
0.));
#126734=CARTESIAN_POINT('Ctrl Pts',(29.0911364758486,-66.9217998601885,
12.));
#126735=CARTESIAN_POINT('Ctrl Pts',(29.0904540435065,-66.8961104343707,
0.));
#126736=CARTESIAN_POINT('Ctrl Pts',(29.0904540435065,-66.8961104343707,
12.));
#126737=CARTESIAN_POINT('Ctrl Pts',(29.0897484879207,-66.8704603993794,
0.));
#126738=CARTESIAN_POINT('Ctrl Pts',(29.0897484879207,-66.8704603993794,
12.));
#126739=CARTESIAN_POINT('Ctrl Pts',(29.0890198649323,-66.8448498552503,
0.));
#126740=CARTESIAN_POINT('Ctrl Pts',(29.0890198649323,-66.8448498552503,
12.));
#126741=CARTESIAN_POINT('Ctrl Pts',(29.088268230663,-66.8192789023312,0.));
#126742=CARTESIAN_POINT('Ctrl Pts',(29.088268230663,-66.8192789023312,12.));
#126743=CARTESIAN_POINT('Ctrl Pts',(29.0874936415131,-66.793747641293,0.));
#126744=CARTESIAN_POINT('Ctrl Pts',(29.0874936415131,-66.793747641293,12.));
#126745=CARTESIAN_POINT('Ctrl Pts',(29.0866961541625,-66.7682561731342,
0.));
#126746=CARTESIAN_POINT('Ctrl Pts',(29.0866961541625,-66.7682561731342,
12.));
#126747=CARTESIAN_POINT('Ctrl Pts',(29.0858758255728,-66.7428045991841,
0.));
#126748=CARTESIAN_POINT('Ctrl Pts',(29.0858758255728,-66.7428045991841,
12.));
#126749=CARTESIAN_POINT('Ctrl Pts',(29.0850327129916,-66.7173930211022,
0.));
#126750=CARTESIAN_POINT('Ctrl Pts',(29.0850327129916,-66.7173930211022,
12.));
#126751=CARTESIAN_POINT('Ctrl Pts',(29.0841668739588,-66.6920215408751,
0.));
#126752=CARTESIAN_POINT('Ctrl Pts',(29.0841668739588,-66.6920215408751,
12.));
#126753=CARTESIAN_POINT('Ctrl Pts',(29.0832783663049,-66.6666902608249,
0.));
#126754=CARTESIAN_POINT('Ctrl Pts',(29.0832783663049,-66.6666902608249,
12.));
#126755=CARTESIAN_POINT('Ctrl Pts',(29.0823672481507,-66.6413992836147,
0.));
#126756=CARTESIAN_POINT('Ctrl Pts',(29.0823672481507,-66.6413992836147,
12.));
#126757=CARTESIAN_POINT('Ctrl Pts',(29.0814335779084,-66.6161487122502,
0.));
#126758=CARTESIAN_POINT('Ctrl Pts',(29.0814335779084,-66.6161487122502,
12.));
#126759=CARTESIAN_POINT('Ctrl Pts',(29.0804774142853,-66.59093865008,0.));
#126760=CARTESIAN_POINT('Ctrl Pts',(29.0804774142853,-66.59093865008,12.));
#126761=CARTESIAN_POINT('Ctrl Pts',(29.0794988162897,-66.5657692007906,
0.));
#126762=CARTESIAN_POINT('Ctrl Pts',(29.0794988162897,-66.5657692007906,
12.));
#126763=CARTESIAN_POINT('Ctrl Pts',(29.07849784323,-66.5406404684132,0.));
#126764=CARTESIAN_POINT('Ctrl Pts',(29.07849784323,-66.5406404684132,12.));
#126765=CARTESIAN_POINT('Ctrl Pts',(29.0774745547151,-66.5155525573323,
0.));
#126766=CARTESIAN_POINT('Ctrl Pts',(29.0774745547151,-66.5155525573323,
12.));
#126767=CARTESIAN_POINT('Ctrl Pts',(29.0764290106554,-66.4905055722868,
0.));
#126768=CARTESIAN_POINT('Ctrl Pts',(29.0764290106554,-66.4905055722868,
12.));
#126769=CARTESIAN_POINT('Ctrl Pts',(29.0753612712665,-66.4654996183731,
0.));
#126770=CARTESIAN_POINT('Ctrl Pts',(29.0753612712665,-66.4654996183731,
12.));
#126771=CARTESIAN_POINT('Ctrl Pts',(29.0742713970755,-66.4405348010388,
0.));
#126772=CARTESIAN_POINT('Ctrl Pts',(29.0742713970755,-66.4405348010388,
12.));
#126773=CARTESIAN_POINT('Ctrl Pts',(29.0731594489211,-66.4156112260887,
0.));
#126774=CARTESIAN_POINT('Ctrl Pts',(29.0731594489211,-66.4156112260887,
12.));
#126775=CARTESIAN_POINT('Ctrl Pts',(29.072025487953,-66.3907289996932,0.));
#126776=CARTESIAN_POINT('Ctrl Pts',(29.072025487953,-66.3907289996932,12.));
#126777=CARTESIAN_POINT('Ctrl Pts',(29.0708695756334,-66.3658882283903,
0.));
#126778=CARTESIAN_POINT('Ctrl Pts',(29.0708695756334,-66.3658882283903,
12.));
#126779=CARTESIAN_POINT('Ctrl Pts',(29.0696917737399,-66.3410890190884,
0.));
#126780=CARTESIAN_POINT('Ctrl Pts',(29.0696917737399,-66.3410890190884,
12.));
#126781=CARTESIAN_POINT('Ctrl Pts',(29.0684921443721,-66.3163314790615,
0.));
#126782=CARTESIAN_POINT('Ctrl Pts',(29.0684921443721,-66.3163314790615,
12.));
#126783=CARTESIAN_POINT('Ctrl Pts',(29.0672707499529,-66.2916157159536,
0.));
#126784=CARTESIAN_POINT('Ctrl Pts',(29.0672707499529,-66.2916157159536,
12.));
#126785=CARTESIAN_POINT('Ctrl Pts',(29.0660276532273,-66.2669418377871,
0.));
#126786=CARTESIAN_POINT('Ctrl Pts',(29.0660276532273,-66.2669418377871,
12.));
#126787=CARTESIAN_POINT('Ctrl Pts',(29.0647629172644,-66.2423099529669,
0.));
#126788=CARTESIAN_POINT('Ctrl Pts',(29.0647629172644,-66.2423099529669,
12.));
#126789=CARTESIAN_POINT('Ctrl Pts',(29.0634766054598,-66.2177201702818,
0.));
#126790=CARTESIAN_POINT('Ctrl Pts',(29.0634766054598,-66.2177201702818,
12.));
#126791=CARTESIAN_POINT('Ctrl Pts',(29.062168781542,-66.1931725989008,0.));
#126792=CARTESIAN_POINT('Ctrl Pts',(29.062168781542,-66.1931725989008,12.));
#126793=CARTESIAN_POINT('Ctrl Pts',(29.0608395095746,-66.1686673483757,
0.));
#126794=CARTESIAN_POINT('Ctrl Pts',(29.0608395095746,-66.1686673483757,
12.));
#126795=CARTESIAN_POINT('Ctrl Pts',(29.0594888539557,-66.144204528652,0.));
#126796=CARTESIAN_POINT('Ctrl Pts',(29.0594888539557,-66.144204528652,12.));
#126797=CARTESIAN_POINT('Ctrl Pts',(29.058116879419,-66.1197842500714,0.));
#126798=CARTESIAN_POINT('Ctrl Pts',(29.058116879419,-66.1197842500714,12.));
#126799=CARTESIAN_POINT('Ctrl Pts',(29.0567236510372,-66.0954066233752,
0.));
#126800=CARTESIAN_POINT('Ctrl Pts',(29.0567236510372,-66.0954066233752,
12.));
#126801=CARTESIAN_POINT('Ctrl Pts',(29.0553092342274,-66.0710717597003,
0.));
#126802=CARTESIAN_POINT('Ctrl Pts',(29.0553092342274,-66.0710717597003,
12.));
#126803=CARTESIAN_POINT('Ctrl Pts',(29.0538736947547,-66.0467797705806,
0.));
#126804=CARTESIAN_POINT('Ctrl Pts',(29.0538736947547,-66.0467797705806,
12.));
#126805=CARTESIAN_POINT('Ctrl Pts',(29.0524170987302,-66.0225307679584,
0.));
#126806=CARTESIAN_POINT('Ctrl Pts',(29.0524170987302,-66.0225307679584,
12.));
#126807=CARTESIAN_POINT('Ctrl Pts',(29.0509395126141,-65.9983248641877,
0.));
#126808=CARTESIAN_POINT('Ctrl Pts',(29.0509395126141,-65.9983248641877,
12.));
#126809=CARTESIAN_POINT('Ctrl Pts',(29.0494410032173,-65.9741621720372,
0.));
#126810=CARTESIAN_POINT('Ctrl Pts',(29.0494410032173,-65.9741621720372,
12.));
#126811=CARTESIAN_POINT('Ctrl Pts',(29.0479216377082,-65.9500428046873,
0.));
#126812=CARTESIAN_POINT('Ctrl Pts',(29.0479216377082,-65.9500428046873,
12.));
#126813=CARTESIAN_POINT('Ctrl Pts',(29.0463814836158,-65.925966875731,0.));
#126814=CARTESIAN_POINT('Ctrl Pts',(29.0463814836158,-65.925966875731,12.));
#126815=CARTESIAN_POINT('Ctrl Pts',(29.0448206088288,-65.9019344991854,
0.));
#126816=CARTESIAN_POINT('Ctrl Pts',(29.0448206088288,-65.9019344991854,
12.));
#126817=CARTESIAN_POINT('Ctrl Pts',(29.0432390815976,-65.8779457894959,
0.));
#126818=CARTESIAN_POINT('Ctrl Pts',(29.0432390815976,-65.8779457894959,
12.));
#126819=CARTESIAN_POINT('Ctrl Pts',(29.0416369705375,-65.854000861539,0.));
#126820=CARTESIAN_POINT('Ctrl Pts',(29.0416369705375,-65.854000861539,12.));
#126821=CARTESIAN_POINT('Ctrl Pts',(29.040014344634,-65.8300998306198,0.));
#126822=CARTESIAN_POINT('Ctrl Pts',(29.040014344634,-65.8300998306198,12.));
#126823=CARTESIAN_POINT('Ctrl Pts',(29.0383712732473,-65.8062428124723,
0.));
#126824=CARTESIAN_POINT('Ctrl Pts',(29.0383712732473,-65.8062428124723,
12.));
#126825=CARTESIAN_POINT('Ctrl Pts',(29.0367078261107,-65.7824299232715,
0.));
#126826=CARTESIAN_POINT('Ctrl Pts',(29.0367078261107,-65.7824299232715,
12.));
#126827=CARTESIAN_POINT('Ctrl Pts',(29.0350240733332,-65.7586612796375,
0.));
#126828=CARTESIAN_POINT('Ctrl Pts',(29.0350240733332,-65.7586612796375,
12.));
#126829=CARTESIAN_POINT('Ctrl Pts',(29.0333200854026,-65.7349369986382,
0.));
#126830=CARTESIAN_POINT('Ctrl Pts',(29.0333200854026,-65.7349369986382,
12.));
#126831=CARTESIAN_POINT('Ctrl Pts',(29.0315959331911,-65.7112571977874,
0.));
#126832=CARTESIAN_POINT('Ctrl Pts',(29.0315959331911,-65.7112571977874,
12.));
#126833=CARTESIAN_POINT('Ctrl Pts',(29.0298516879599,-65.6876219950465,
0.));
#126834=CARTESIAN_POINT('Ctrl Pts',(29.0298516879599,-65.6876219950465,
12.));
#126835=CARTESIAN_POINT('Ctrl Pts',(29.0280874213584,-65.6640315088361,
0.));
#126836=CARTESIAN_POINT('Ctrl Pts',(29.0280874213584,-65.6640315088361,
12.));
#126837=CARTESIAN_POINT('Ctrl Pts',(29.0263032054261,-65.6404858580391,
0.));
#126838=CARTESIAN_POINT('Ctrl Pts',(29.0263032054261,-65.6404858580391,
12.));
#126839=CARTESIAN_POINT('Ctrl Pts',(29.0244991125961,-65.6169851620054,
0.));
#126840=CARTESIAN_POINT('Ctrl Pts',(29.0244991125961,-65.6169851620054,
12.));
#126841=CARTESIAN_POINT('Ctrl Pts',(29.0226752157013,-65.593529540548,0.));
#126842=CARTESIAN_POINT('Ctrl Pts',(29.0226752157013,-65.593529540548,12.));
#126843=CARTESIAN_POINT('Ctrl Pts',(29.0208315879778,-65.5701191139455,
0.));
#126844=CARTESIAN_POINT('Ctrl Pts',(29.0208315879778,-65.5701191139455,
12.));
#126845=CARTESIAN_POINT('Ctrl Pts',(29.0189683030654,-65.5467540029546,
0.));
#126846=CARTESIAN_POINT('Ctrl Pts',(29.0189683030654,-65.5467540029546,
12.));
#126847=CARTESIAN_POINT('Ctrl Pts',(29.01708543501,-65.523434328815,0.));
#126848=CARTESIAN_POINT('Ctrl Pts',(29.01708543501,-65.523434328815,12.));
#126849=CARTESIAN_POINT('Ctrl Pts',(29.015183058267,-65.5001602132524,0.));
#126850=CARTESIAN_POINT('Ctrl Pts',(29.015183058267,-65.5001602132524,12.));
#126851=CARTESIAN_POINT('Ctrl Pts',(29.0132612477075,-65.4769317784754,
0.));
#126852=CARTESIAN_POINT('Ctrl Pts',(29.0132612477075,-65.4769317784754,
12.));
#126853=CARTESIAN_POINT('Ctrl Pts',(29.0113200786218,-65.4537491471782,
0.));
#126854=CARTESIAN_POINT('Ctrl Pts',(29.0113200786218,-65.4537491471782,
12.));
#126855=CARTESIAN_POINT('Ctrl Pts',(29.0093596267198,-65.4306124425524,
0.));
#126856=CARTESIAN_POINT('Ctrl Pts',(29.0093596267198,-65.4306124425524,
12.));
#126857=CARTESIAN_POINT('Ctrl Pts',(29.0073799681335,-65.4075217882921,
0.));
#126858=CARTESIAN_POINT('Ctrl Pts',(29.0073799681335,-65.4075217882921,
12.));
#126859=CARTESIAN_POINT('Ctrl Pts',(29.0053811794213,-65.3844773085977,
0.));
#126860=CARTESIAN_POINT('Ctrl Pts',(29.0053811794213,-65.3844773085977,
12.));
#126861=CARTESIAN_POINT('Ctrl Pts',(29.0033633375744,-65.3614791281726,
0.));
#126862=CARTESIAN_POINT('Ctrl Pts',(29.0033633375744,-65.3614791281726,
12.));
#126863=CARTESIAN_POINT('Ctrl Pts',(29.0013265200201,-65.3385273722279,
0.));
#126864=CARTESIAN_POINT('Ctrl Pts',(29.0013265200201,-65.3385273722279,
12.));
#126865=CARTESIAN_POINT('Ctrl Pts',(28.9992708046223,-65.3156221664942,
0.));
#126866=CARTESIAN_POINT('Ctrl Pts',(28.9992708046223,-65.3156221664942,
12.));
#126867=CARTESIAN_POINT('Ctrl Pts',(28.9971962696848,-65.2927636372261,
0.));
#126868=CARTESIAN_POINT('Ctrl Pts',(28.9971962696848,-65.2927636372261,
12.));
#126869=CARTESIAN_POINT('Ctrl Pts',(28.9951029939551,-65.2699519112052,
0.));
#126870=CARTESIAN_POINT('Ctrl Pts',(28.9951029939551,-65.2699519112052,
12.));
#126871=CARTESIAN_POINT('Ctrl Pts',(28.9929910566314,-65.2471871157375,
0.));
#126872=CARTESIAN_POINT('Ctrl Pts',(28.9929910566314,-65.2471871157375,
12.));
#126873=CARTESIAN_POINT('Ctrl Pts',(28.9908605373651,-65.2244693786586,
0.));
#126874=CARTESIAN_POINT('Ctrl Pts',(28.9908605373651,-65.2244693786586,
12.));
#126875=CARTESIAN_POINT('Ctrl Pts',(28.9887115162626,-65.2017988283465,
0.));
#126876=CARTESIAN_POINT('Ctrl Pts',(28.9887115162626,-65.2017988283465,
12.));
#126877=CARTESIAN_POINT('Ctrl Pts',(28.9865440738882,-65.1791755937254,
0.));
#126878=CARTESIAN_POINT('Ctrl Pts',(28.9865440738882,-65.1791755937254,
12.));
#126879=CARTESIAN_POINT('Ctrl Pts',(28.9843582912696,-65.1565998042706,
0.));
#126880=CARTESIAN_POINT('Ctrl Pts',(28.9843582912696,-65.1565998042706,
12.));
#126881=CARTESIAN_POINT('Ctrl Pts',(28.9821542499049,-65.1340715900042,
0.));
#126882=CARTESIAN_POINT('Ctrl Pts',(28.9821542499049,-65.1340715900042,
12.));
#126883=CARTESIAN_POINT('Ctrl Pts',(28.9799320317648,-65.1115910815051,
0.));
#126884=CARTESIAN_POINT('Ctrl Pts',(28.9799320317648,-65.1115910815051,
12.));
#126885=CARTESIAN_POINT('Ctrl Pts',(28.9776917192936,-65.0891584099174,
0.));
#126886=CARTESIAN_POINT('Ctrl Pts',(28.9776917192936,-65.0891584099174,
12.));
#126887=CARTESIAN_POINT('Ctrl Pts',(28.9754333954134,-65.0667737069562,
0.));
#126888=CARTESIAN_POINT('Ctrl Pts',(28.9754333954134,-65.0667737069562,
12.));
#126889=CARTESIAN_POINT('Ctrl Pts',(28.9731571435281,-65.0444371049082,
0.));
#126890=CARTESIAN_POINT('Ctrl Pts',(28.9731571435281,-65.0444371049082,
12.));
#126891=CARTESIAN_POINT('Ctrl Pts',(28.9708630475298,-65.022148736628,0.));
#126892=CARTESIAN_POINT('Ctrl Pts',(28.9708630475298,-65.022148736628,12.));
#126893=CARTESIAN_POINT('Ctrl Pts',(28.9685511918016,-64.9999087355504,
0.));
#126894=CARTESIAN_POINT('Ctrl Pts',(28.9685511918016,-64.9999087355504,
12.));
#126895=CARTESIAN_POINT('Ctrl Pts',(28.9662216612216,-64.9777172357028,
0.));
#126896=CARTESIAN_POINT('Ctrl Pts',(28.9662216612216,-64.9777172357028,
12.));
#126897=CARTESIAN_POINT('Ctrl Pts',(28.9638745411676,-64.955574371711,0.));
#126898=CARTESIAN_POINT('Ctrl Pts',(28.9638745411676,-64.955574371711,12.));
#126899=CARTESIAN_POINT('Ctrl Pts',(28.9615099175249,-64.9334802788037,
0.));
#126900=CARTESIAN_POINT('Ctrl Pts',(28.9615099175249,-64.9334802788037,
12.));
#126901=CARTESIAN_POINT('Ctrl Pts',(28.9591278766934,-64.9114350928124,
0.));
#126902=CARTESIAN_POINT('Ctrl Pts',(28.9591278766934,-64.9114350928124,
12.));
#126903=CARTESIAN_POINT('Ctrl Pts',(28.9567285055865,-64.8894389501799,
0.));
#126904=CARTESIAN_POINT('Ctrl Pts',(28.9567285055865,-64.8894389501799,
12.));
#126905=CARTESIAN_POINT('Ctrl Pts',(28.9543118916327,-64.8674919879646,
0.));
#126906=CARTESIAN_POINT('Ctrl Pts',(28.9543118916327,-64.8674919879646,
12.));
#126907=CARTESIAN_POINT('Ctrl Pts',(28.9518781227764,-64.8455943438424,
0.));
#126908=CARTESIAN_POINT('Ctrl Pts',(28.9518781227764,-64.8455943438424,
12.));
#126909=CARTESIAN_POINT('Ctrl Pts',(28.9494272874833,-64.8237461561024,
0.));
#126910=CARTESIAN_POINT('Ctrl Pts',(28.9494272874833,-64.8237461561024,
12.));
#126911=CARTESIAN_POINT('Ctrl Pts',(28.9469594747436,-64.8019475636454,
0.));
#126912=CARTESIAN_POINT('Ctrl Pts',(28.9469594747436,-64.8019475636454,
12.));
#126913=CARTESIAN_POINT('Ctrl Pts',(28.9444747740815,-64.7801987060097,
0.));
#126914=CARTESIAN_POINT('Ctrl Pts',(28.9444747740815,-64.7801987060097,
12.));
#126915=CARTESIAN_POINT('Ctrl Pts',(28.9419732755659,-64.7584997233889,
0.));
#126916=CARTESIAN_POINT('Ctrl Pts',(28.9419732755659,-64.7584997233889,
12.));
#126917=CARTESIAN_POINT('Ctrl Pts',(28.9394550698201,-64.7368507566462,
0.));
#126918=CARTESIAN_POINT('Ctrl Pts',(28.9394550698201,-64.7368507566462,
12.));
#126919=CARTESIAN_POINT('Ctrl Pts',(28.9369202480383,-64.715251947327,0.));
#126920=CARTESIAN_POINT('Ctrl Pts',(28.9369202480383,-64.715251947327,12.));
#126921=CARTESIAN_POINT('Ctrl Pts',(28.9343689019869,-64.6937034376591,
0.));
#126922=CARTESIAN_POINT('Ctrl Pts',(28.9343689019869,-64.6937034376591,
12.));
#126923=CARTESIAN_POINT('Ctrl Pts',(28.9318011239905,-64.6722053705389,
0.));
#126924=CARTESIAN_POINT('Ctrl Pts',(28.9318011239905,-64.6722053705389,
12.));
#126925=CARTESIAN_POINT('Ctrl Pts',(28.9292170069219,-64.6507578895155,
0.));
#126926=CARTESIAN_POINT('Ctrl Pts',(28.9292170069219,-64.6507578895155,
12.));
#126927=CARTESIAN_POINT('Ctrl Pts',(28.9266166441956,-64.6293611387754,
0.));
#126928=CARTESIAN_POINT('Ctrl Pts',(28.9266166441956,-64.6293611387754,
12.));
#126929=CARTESIAN_POINT('Ctrl Pts',(28.9240001297553,-64.6080152631066,
0.));
#126930=CARTESIAN_POINT('Ctrl Pts',(28.9240001297553,-64.6080152631066,
12.));
#126931=CARTESIAN_POINT('Ctrl Pts',(28.9213675580996,-64.5867204079452,
0.));
#126932=CARTESIAN_POINT('Ctrl Pts',(28.9213675580996,-64.5867204079452,
12.));
#126933=CARTESIAN_POINT('Ctrl Pts',(28.918719024323,-64.5654767194488,0.));
#126934=CARTESIAN_POINT('Ctrl Pts',(28.918719024323,-64.5654767194488,12.));
#126935=CARTESIAN_POINT('Ctrl Pts',(28.9160546241538,-64.544284344556,0.));
#126936=CARTESIAN_POINT('Ctrl Pts',(28.9160546241538,-64.544284344556,12.));
#126937=CARTESIAN_POINT('Ctrl Pts',(28.9133744539942,-64.5231434310457,
0.));
#126938=CARTESIAN_POINT('Ctrl Pts',(28.9133744539942,-64.5231434310457,
12.));
#126939=CARTESIAN_POINT('Ctrl Pts',(28.9106786109638,-64.5020541275927,
0.));
#126940=CARTESIAN_POINT('Ctrl Pts',(28.9106786109638,-64.5020541275927,
12.));
#126941=CARTESIAN_POINT('Ctrl Pts',(28.9079671928252,-64.4810165836568,
0.));
#126942=CARTESIAN_POINT('Ctrl Pts',(28.9079671928252,-64.4810165836568,
12.));
#126943=CARTESIAN_POINT('Ctrl Pts',(28.9052402979055,-64.460030949357,0.));
#126944=CARTESIAN_POINT('Ctrl Pts',(28.9052402979055,-64.460030949357,12.));
#126945=CARTESIAN_POINT('Ctrl Pts',(28.9024980250309,-64.439097375364,0.));
#126946=CARTESIAN_POINT('Ctrl Pts',(28.9024980250309,-64.439097375364,12.));
#126947=CARTESIAN_POINT('Ctrl Pts',(28.8997404734349,-64.4182160127401,
0.));
#126948=CARTESIAN_POINT('Ctrl Pts',(28.8997404734349,-64.4182160127401,
12.));
#126949=CARTESIAN_POINT('Ctrl Pts',(28.8969677427518,-64.3973870129201,
0.));
#126950=CARTESIAN_POINT('Ctrl Pts',(28.8969677427518,-64.3973870129201,
12.));
#126951=CARTESIAN_POINT('Ctrl Pts',(28.8941799332312,-64.3766105280715,
0.));
#126952=CARTESIAN_POINT('Ctrl Pts',(28.8941799332312,-64.3766105280715,
12.));
#126953=CARTESIAN_POINT('Ctrl Pts',(28.8913771459327,-64.3558867114087,
0.));
#126954=CARTESIAN_POINT('Ctrl Pts',(28.8913771459327,-64.3558867114087,
12.));
#126955=CARTESIAN_POINT('Ctrl Pts',(28.8885594828919,-64.3352157174607,
0.));
#126956=CARTESIAN_POINT('Ctrl Pts',(28.8885594828919,-64.3352157174607,
12.));
#126957=CARTESIAN_POINT('Ctrl Pts',(28.8857270473944,-64.3145977025005,
0.));
#126958=CARTESIAN_POINT('Ctrl Pts',(28.8857270473944,-64.3145977025005,
12.));
#126959=CARTESIAN_POINT('Ctrl Pts',(28.8828799437922,-64.2940328242483,
0.));
#126960=CARTESIAN_POINT('Ctrl Pts',(28.8828799437922,-64.2940328242483,
12.));
#126961=CARTESIAN_POINT('Ctrl Pts',(28.8800182770051,-64.2735212410682,
0.));
#126962=CARTESIAN_POINT('Ctrl Pts',(28.8800182770051,-64.2735212410682,
12.));
#126963=CARTESIAN_POINT('Ctrl Pts',(28.8771421521058,-64.2530631112927,
0.));
#126964=CARTESIAN_POINT('Ctrl Pts',(28.8771421521058,-64.2530631112927,
12.));
#126965=CARTESIAN_POINT('Ctrl Pts',(28.8742516738958,-64.232658592528,0.));
#126966=CARTESIAN_POINT('Ctrl Pts',(28.8742516738958,-64.232658592528,12.));
#126967=CARTESIAN_POINT('Ctrl Pts',(28.8713469464205,-64.2123078408507,
0.));
#126968=CARTESIAN_POINT('Ctrl Pts',(28.8713469464205,-64.2123078408507,
12.));
#126969=CARTESIAN_POINT('Ctrl Pts',(28.8684280739032,-64.1920110123342,
0.));
#126970=CARTESIAN_POINT('Ctrl Pts',(28.8684280739032,-64.1920110123342,
12.));
#126971=CARTESIAN_POINT('Ctrl Pts',(28.8654951618658,-64.1717682648708,
0.));
#126972=CARTESIAN_POINT('Ctrl Pts',(28.8654951618658,-64.1717682648708,
12.));
#126973=CARTESIAN_POINT('Ctrl Pts',(28.8625483180433,-64.1515797596555,
0.));
#126974=CARTESIAN_POINT('Ctrl Pts',(28.8625483180433,-64.1515797596555,
12.));
#126975=CARTESIAN_POINT('Ctrl Pts',(28.8595876537131,-64.1314456633345,
0.));
#126976=CARTESIAN_POINT('Ctrl Pts',(28.8595876537131,-64.1314456633345,
12.));
#126977=CARTESIAN_POINT('Ctrl Pts',(28.8566132838156,-64.1113661481918,
0.));
#126978=CARTESIAN_POINT('Ctrl Pts',(28.8566132838156,-64.1113661481918,
12.));
#126979=CARTESIAN_POINT('Ctrl Pts',(28.8536253241836,-64.0913413876586,
0.));
#126980=CARTESIAN_POINT('Ctrl Pts',(28.8536253241836,-64.0913413876586,
12.));
#126981=CARTESIAN_POINT('Ctrl Pts',(28.8506238891086,-64.0713715523588,
0.));
#126982=CARTESIAN_POINT('Ctrl Pts',(28.8506238891086,-64.0713715523588,
12.));
#126983=CARTESIAN_POINT('Ctrl Pts',(28.8476090892242,-64.0514568066659,
0.));
#126984=CARTESIAN_POINT('Ctrl Pts',(28.8476090892242,-64.0514568066659,
12.));
#126985=CARTESIAN_POINT('Ctrl Pts',(28.8445810281275,-64.0315973031995,
0.));
#126986=CARTESIAN_POINT('Ctrl Pts',(28.8445810281275,-64.0315973031995,
12.));
#126987=CARTESIAN_POINT('Ctrl Pts',(28.841539805646,-64.0117931881364,0.));
#126988=CARTESIAN_POINT('Ctrl Pts',(28.841539805646,-64.0117931881364,12.));
#126989=CARTESIAN_POINT('Ctrl Pts',(28.8384855243267,-63.9920446117632,
0.));
#126990=CARTESIAN_POINT('Ctrl Pts',(28.8384855243267,-63.9920446117632,
12.));
#126991=CARTESIAN_POINT('Ctrl Pts',(28.83541829466,-63.9723517369614,0.));
#126992=CARTESIAN_POINT('Ctrl Pts',(28.83541829466,-63.9723517369614,12.));
#126993=CARTESIAN_POINT('Ctrl Pts',(28.8323382413752,-63.9527147494351,
0.));
#126994=CARTESIAN_POINT('Ctrl Pts',(28.8323382413752,-63.9527147494351,
12.));
#126995=CARTESIAN_POINT('Ctrl Pts',(28.8292455077494,-63.9331338646868,
0.));
#126996=CARTESIAN_POINT('Ctrl Pts',(28.8292455077494,-63.9331338646868,
12.));
#126997=CARTESIAN_POINT('Ctrl Pts',(28.8261402423219,-63.9136093063647,
0.));
#126998=CARTESIAN_POINT('Ctrl Pts',(28.8261402423219,-63.9136093063647,
12.));
#126999=CARTESIAN_POINT('Ctrl Pts',(28.8230225863142,-63.894141285685,0.));
#127000=CARTESIAN_POINT('Ctrl Pts',(28.8230225863142,-63.894141285685,12.));
#127001=CARTESIAN_POINT('Ctrl Pts',(28.8198926619892,-63.8747299825383,
0.));
#127002=CARTESIAN_POINT('Ctrl Pts',(28.8198926619892,-63.8747299825383,
12.));
#127003=CARTESIAN_POINT('Ctrl Pts',(28.8167505576805,-63.8553755207732,
0.));
#127004=CARTESIAN_POINT('Ctrl Pts',(28.8167505576805,-63.8553755207732,
12.));
#127005=CARTESIAN_POINT('Ctrl Pts',(28.8135963263556,-63.8360779670226,
0.));
#127006=CARTESIAN_POINT('Ctrl Pts',(28.8135963263556,-63.8360779670226,
12.));
#127007=CARTESIAN_POINT('Ctrl Pts',(28.8110632621132,-63.8206854735372,
0.));
#127008=CARTESIAN_POINT('Ctrl Pts',(28.8110632621132,-63.8206854735372,
12.));
#127009=CARTESIAN_POINT('Ctrl Pts',(28.8091580239664,-63.8091667271451,
0.));
#127010=CARTESIAN_POINT('Ctrl Pts',(28.8091580239664,-63.8091667271451,
12.));
#127011=CARTESIAN_POINT('Ctrl Pts',(28.8078854475473,-63.8014989507576,
0.));
#127012=CARTESIAN_POINT('Ctrl Pts',(28.8078854475473,-63.8014989507576,
12.));
#127013=CARTESIAN_POINT('Ctrl Pts',(28.8072485549236,-63.7976679095314,
0.));
#127014=CARTESIAN_POINT('Ctrl Pts',(28.8072485549236,-63.7976679095314,
12.));
#127015=CARTESIAN_POINT('',(28.8072485549236,-63.7976679095314,12.));
#127016=CARTESIAN_POINT('Ctrl Pts',(28.8072485549236,-63.7976679095314,
12.));
#127017=CARTESIAN_POINT('Ctrl Pts',(28.8078854475473,-63.8014989507576,
12.));
#127018=CARTESIAN_POINT('Ctrl Pts',(28.8091580239664,-63.8091667271451,
12.));
#127019=CARTESIAN_POINT('Ctrl Pts',(28.8110632621132,-63.8206854735372,
12.));
#127020=CARTESIAN_POINT('Ctrl Pts',(28.8135963263556,-63.8360779670226,
12.));
#127021=CARTESIAN_POINT('Ctrl Pts',(28.8167505576805,-63.8553755207732,
12.));
#127022=CARTESIAN_POINT('Ctrl Pts',(28.8198926619892,-63.8747299825383,
12.));
#127023=CARTESIAN_POINT('Ctrl Pts',(28.8230225863142,-63.894141285685,12.));
#127024=CARTESIAN_POINT('Ctrl Pts',(28.8261402423219,-63.9136093063647,
12.));
#127025=CARTESIAN_POINT('Ctrl Pts',(28.8292455077494,-63.9331338646868,
12.));
#127026=CARTESIAN_POINT('Ctrl Pts',(28.8323382413752,-63.9527147494351,
12.));
#127027=CARTESIAN_POINT('Ctrl Pts',(28.83541829466,-63.9723517369614,12.));
#127028=CARTESIAN_POINT('Ctrl Pts',(28.8384855243267,-63.9920446117632,
12.));
#127029=CARTESIAN_POINT('Ctrl Pts',(28.841539805646,-64.0117931881364,12.));
#127030=CARTESIAN_POINT('Ctrl Pts',(28.8445810281275,-64.0315973031995,
12.));
#127031=CARTESIAN_POINT('Ctrl Pts',(28.8476090892242,-64.0514568066659,
12.));
#127032=CARTESIAN_POINT('Ctrl Pts',(28.8506238891086,-64.0713715523588,
12.));
#127033=CARTESIAN_POINT('Ctrl Pts',(28.8536253241836,-64.0913413876586,
12.));
#127034=CARTESIAN_POINT('Ctrl Pts',(28.8566132838156,-64.1113661481918,
12.));
#127035=CARTESIAN_POINT('Ctrl Pts',(28.8595876537131,-64.1314456633345,
12.));
#127036=CARTESIAN_POINT('Ctrl Pts',(28.8625483180433,-64.1515797596555,
12.));
#127037=CARTESIAN_POINT('Ctrl Pts',(28.8654951618658,-64.1717682648708,
12.));
#127038=CARTESIAN_POINT('Ctrl Pts',(28.8684280739032,-64.1920110123342,
12.));
#127039=CARTESIAN_POINT('Ctrl Pts',(28.8713469464205,-64.2123078408507,
12.));
#127040=CARTESIAN_POINT('Ctrl Pts',(28.8742516738958,-64.232658592528,12.));
#127041=CARTESIAN_POINT('Ctrl Pts',(28.8771421521058,-64.2530631112927,
12.));
#127042=CARTESIAN_POINT('Ctrl Pts',(28.8800182770051,-64.2735212410682,
12.));
#127043=CARTESIAN_POINT('Ctrl Pts',(28.8828799437922,-64.2940328242483,
12.));
#127044=CARTESIAN_POINT('Ctrl Pts',(28.8857270473944,-64.3145977025005,
12.));
#127045=CARTESIAN_POINT('Ctrl Pts',(28.8885594828919,-64.3352157174607,
12.));
#127046=CARTESIAN_POINT('Ctrl Pts',(28.8913771459327,-64.3558867114087,
12.));
#127047=CARTESIAN_POINT('Ctrl Pts',(28.8941799332312,-64.3766105280715,
12.));
#127048=CARTESIAN_POINT('Ctrl Pts',(28.8969677427518,-64.3973870129201,
12.));
#127049=CARTESIAN_POINT('Ctrl Pts',(28.8997404734349,-64.4182160127401,
12.));
#127050=CARTESIAN_POINT('Ctrl Pts',(28.9024980250309,-64.439097375364,12.));
#127051=CARTESIAN_POINT('Ctrl Pts',(28.9052402979055,-64.460030949357,12.));
#127052=CARTESIAN_POINT('Ctrl Pts',(28.9079671928252,-64.4810165836568,
12.));
#127053=CARTESIAN_POINT('Ctrl Pts',(28.9106786109638,-64.5020541275927,
12.));
#127054=CARTESIAN_POINT('Ctrl Pts',(28.9133744539942,-64.5231434310457,
12.));
#127055=CARTESIAN_POINT('Ctrl Pts',(28.9160546241538,-64.544284344556,12.));
#127056=CARTESIAN_POINT('Ctrl Pts',(28.918719024323,-64.5654767194488,12.));
#127057=CARTESIAN_POINT('Ctrl Pts',(28.9213675580996,-64.5867204079452,
12.));
#127058=CARTESIAN_POINT('Ctrl Pts',(28.9240001297553,-64.6080152631066,
12.));
#127059=CARTESIAN_POINT('Ctrl Pts',(28.9266166441956,-64.6293611387754,
12.));
#127060=CARTESIAN_POINT('Ctrl Pts',(28.9292170069219,-64.6507578895155,
12.));
#127061=CARTESIAN_POINT('Ctrl Pts',(28.9318011239905,-64.6722053705389,
12.));
#127062=CARTESIAN_POINT('Ctrl Pts',(28.9343689019869,-64.6937034376591,
12.));
#127063=CARTESIAN_POINT('Ctrl Pts',(28.9369202480383,-64.715251947327,12.));
#127064=CARTESIAN_POINT('Ctrl Pts',(28.9394550698201,-64.7368507566462,
12.));
#127065=CARTESIAN_POINT('Ctrl Pts',(28.9419732755659,-64.7584997233889,
12.));
#127066=CARTESIAN_POINT('Ctrl Pts',(28.9444747740815,-64.7801987060097,
12.));
#127067=CARTESIAN_POINT('Ctrl Pts',(28.9469594747436,-64.8019475636454,
12.));
#127068=CARTESIAN_POINT('Ctrl Pts',(28.9494272874833,-64.8237461561024,
12.));
#127069=CARTESIAN_POINT('Ctrl Pts',(28.9518781227764,-64.8455943438424,
12.));
#127070=CARTESIAN_POINT('Ctrl Pts',(28.9543118916327,-64.8674919879646,
12.));
#127071=CARTESIAN_POINT('Ctrl Pts',(28.9567285055865,-64.8894389501799,
12.));
#127072=CARTESIAN_POINT('Ctrl Pts',(28.9591278766934,-64.9114350928124,
12.));
#127073=CARTESIAN_POINT('Ctrl Pts',(28.9615099175249,-64.9334802788037,
12.));
#127074=CARTESIAN_POINT('Ctrl Pts',(28.9638745411676,-64.955574371711,12.));
#127075=CARTESIAN_POINT('Ctrl Pts',(28.9662216612216,-64.9777172357028,
12.));
#127076=CARTESIAN_POINT('Ctrl Pts',(28.9685511918016,-64.9999087355504,
12.));
#127077=CARTESIAN_POINT('Ctrl Pts',(28.9708630475298,-65.022148736628,12.));
#127078=CARTESIAN_POINT('Ctrl Pts',(28.9731571435281,-65.0444371049082,
12.));
#127079=CARTESIAN_POINT('Ctrl Pts',(28.9754333954134,-65.0667737069562,
12.));
#127080=CARTESIAN_POINT('Ctrl Pts',(28.9776917192936,-65.0891584099174,
12.));
#127081=CARTESIAN_POINT('Ctrl Pts',(28.9799320317648,-65.1115910815051,
12.));
#127082=CARTESIAN_POINT('Ctrl Pts',(28.9821542499049,-65.1340715900042,
12.));
#127083=CARTESIAN_POINT('Ctrl Pts',(28.9843582912696,-65.1565998042706,
12.));
#127084=CARTESIAN_POINT('Ctrl Pts',(28.9865440738882,-65.1791755937254,
12.));
#127085=CARTESIAN_POINT('Ctrl Pts',(28.9887115162626,-65.2017988283465,
12.));
#127086=CARTESIAN_POINT('Ctrl Pts',(28.9908605373651,-65.2244693786586,
12.));
#127087=CARTESIAN_POINT('Ctrl Pts',(28.9929910566314,-65.2471871157375,
12.));
#127088=CARTESIAN_POINT('Ctrl Pts',(28.9951029939551,-65.2699519112052,
12.));
#127089=CARTESIAN_POINT('Ctrl Pts',(28.9971962696848,-65.2927636372261,
12.));
#127090=CARTESIAN_POINT('Ctrl Pts',(28.9992708046223,-65.3156221664942,
12.));
#127091=CARTESIAN_POINT('Ctrl Pts',(29.0013265200201,-65.3385273722279,
12.));
#127092=CARTESIAN_POINT('Ctrl Pts',(29.0033633375744,-65.3614791281726,
12.));
#127093=CARTESIAN_POINT('Ctrl Pts',(29.0053811794213,-65.3844773085977,
12.));
#127094=CARTESIAN_POINT('Ctrl Pts',(29.0073799681335,-65.4075217882921,
12.));
#127095=CARTESIAN_POINT('Ctrl Pts',(29.0093596267198,-65.4306124425524,
12.));
#127096=CARTESIAN_POINT('Ctrl Pts',(29.0113200786218,-65.4537491471782,
12.));
#127097=CARTESIAN_POINT('Ctrl Pts',(29.0132612477075,-65.4769317784754,
12.));
#127098=CARTESIAN_POINT('Ctrl Pts',(29.015183058267,-65.5001602132524,12.));
#127099=CARTESIAN_POINT('Ctrl Pts',(29.01708543501,-65.523434328815,12.));
#127100=CARTESIAN_POINT('Ctrl Pts',(29.0189683030654,-65.5467540029546,
12.));
#127101=CARTESIAN_POINT('Ctrl Pts',(29.0208315879778,-65.5701191139455,
12.));
#127102=CARTESIAN_POINT('Ctrl Pts',(29.0226752157013,-65.593529540548,12.));
#127103=CARTESIAN_POINT('Ctrl Pts',(29.0244991125961,-65.6169851620054,
12.));
#127104=CARTESIAN_POINT('Ctrl Pts',(29.0263032054261,-65.6404858580391,
12.));
#127105=CARTESIAN_POINT('Ctrl Pts',(29.0280874213584,-65.6640315088361,
12.));
#127106=CARTESIAN_POINT('Ctrl Pts',(29.0298516879599,-65.6876219950465,
12.));
#127107=CARTESIAN_POINT('Ctrl Pts',(29.0315959331911,-65.7112571977874,
12.));
#127108=CARTESIAN_POINT('Ctrl Pts',(29.0333200854026,-65.7349369986382,
12.));
#127109=CARTESIAN_POINT('Ctrl Pts',(29.0350240733332,-65.7586612796375,
12.));
#127110=CARTESIAN_POINT('Ctrl Pts',(29.0367078261107,-65.7824299232715,
12.));
#127111=CARTESIAN_POINT('Ctrl Pts',(29.0383712732473,-65.8062428124723,
12.));
#127112=CARTESIAN_POINT('Ctrl Pts',(29.040014344634,-65.8300998306198,12.));
#127113=CARTESIAN_POINT('Ctrl Pts',(29.0416369705375,-65.854000861539,12.));
#127114=CARTESIAN_POINT('Ctrl Pts',(29.0432390815976,-65.8779457894959,
12.));
#127115=CARTESIAN_POINT('Ctrl Pts',(29.0448206088288,-65.9019344991854,
12.));
#127116=CARTESIAN_POINT('Ctrl Pts',(29.0463814836158,-65.925966875731,12.));
#127117=CARTESIAN_POINT('Ctrl Pts',(29.0479216377082,-65.9500428046873,
12.));
#127118=CARTESIAN_POINT('Ctrl Pts',(29.0494410032173,-65.9741621720372,
12.));
#127119=CARTESIAN_POINT('Ctrl Pts',(29.0509395126141,-65.9983248641877,
12.));
#127120=CARTESIAN_POINT('Ctrl Pts',(29.0524170987302,-66.0225307679584,
12.));
#127121=CARTESIAN_POINT('Ctrl Pts',(29.0538736947547,-66.0467797705806,
12.));
#127122=CARTESIAN_POINT('Ctrl Pts',(29.0553092342274,-66.0710717597003,
12.));
#127123=CARTESIAN_POINT('Ctrl Pts',(29.0567236510372,-66.0954066233752,
12.));
#127124=CARTESIAN_POINT('Ctrl Pts',(29.058116879419,-66.1197842500714,12.));
#127125=CARTESIAN_POINT('Ctrl Pts',(29.0594888539557,-66.144204528652,12.));
#127126=CARTESIAN_POINT('Ctrl Pts',(29.0608395095746,-66.1686673483757,
12.));
#127127=CARTESIAN_POINT('Ctrl Pts',(29.062168781542,-66.1931725989008,12.));
#127128=CARTESIAN_POINT('Ctrl Pts',(29.0634766054598,-66.2177201702818,
12.));
#127129=CARTESIAN_POINT('Ctrl Pts',(29.0647629172644,-66.2423099529669,
12.));
#127130=CARTESIAN_POINT('Ctrl Pts',(29.0660276532273,-66.2669418377871,
12.));
#127131=CARTESIAN_POINT('Ctrl Pts',(29.0672707499529,-66.2916157159536,
12.));
#127132=CARTESIAN_POINT('Ctrl Pts',(29.0684921443721,-66.3163314790615,
12.));
#127133=CARTESIAN_POINT('Ctrl Pts',(29.0696917737399,-66.3410890190884,
12.));
#127134=CARTESIAN_POINT('Ctrl Pts',(29.0708695756334,-66.3658882283903,
12.));
#127135=CARTESIAN_POINT('Ctrl Pts',(29.072025487953,-66.3907289996932,12.));
#127136=CARTESIAN_POINT('Ctrl Pts',(29.0731594489211,-66.4156112260887,
12.));
#127137=CARTESIAN_POINT('Ctrl Pts',(29.0742713970755,-66.4405348010388,
12.));
#127138=CARTESIAN_POINT('Ctrl Pts',(29.0753612712665,-66.4654996183731,
12.));
#127139=CARTESIAN_POINT('Ctrl Pts',(29.0764290106554,-66.4905055722868,
12.));
#127140=CARTESIAN_POINT('Ctrl Pts',(29.0774745547151,-66.5155525573323,
12.));
#127141=CARTESIAN_POINT('Ctrl Pts',(29.07849784323,-66.5406404684132,12.));
#127142=CARTESIAN_POINT('Ctrl Pts',(29.0794988162897,-66.5657692007906,
12.));
#127143=CARTESIAN_POINT('Ctrl Pts',(29.0804774142853,-66.59093865008,12.));
#127144=CARTESIAN_POINT('Ctrl Pts',(29.0814335779084,-66.6161487122502,
12.));
#127145=CARTESIAN_POINT('Ctrl Pts',(29.0823672481507,-66.6413992836147,
12.));
#127146=CARTESIAN_POINT('Ctrl Pts',(29.0832783663049,-66.6666902608249,
12.));
#127147=CARTESIAN_POINT('Ctrl Pts',(29.0841668739588,-66.6920215408751,
12.));
#127148=CARTESIAN_POINT('Ctrl Pts',(29.0850327129916,-66.7173930211022,
12.));
#127149=CARTESIAN_POINT('Ctrl Pts',(29.0858758255728,-66.7428045991841,
12.));
#127150=CARTESIAN_POINT('Ctrl Pts',(29.0866961541625,-66.7682561731342,
12.));
#127151=CARTESIAN_POINT('Ctrl Pts',(29.0874936415131,-66.793747641293,12.));
#127152=CARTESIAN_POINT('Ctrl Pts',(29.088268230663,-66.8192789023312,12.));
#127153=CARTESIAN_POINT('Ctrl Pts',(29.0890198649323,-66.8448498552503,
12.));
#127154=CARTESIAN_POINT('Ctrl Pts',(29.0897484879207,-66.8704603993794,
12.));
#127155=CARTESIAN_POINT('Ctrl Pts',(29.0904540435065,-66.8961104343707,
12.));
#127156=CARTESIAN_POINT('Ctrl Pts',(29.0911364758486,-66.9217998601885,
12.));
#127157=CARTESIAN_POINT('Ctrl Pts',(29.0917957293826,-66.9475285771135,
12.));
#127158=CARTESIAN_POINT('Ctrl Pts',(29.092431748817,-66.9732964857466,12.));
#127159=CARTESIAN_POINT('Ctrl Pts',(29.0930444791328,-66.9991034870083,
12.));
#127160=CARTESIAN_POINT('Ctrl Pts',(29.0936338655828,-67.0249494821363,
12.));
#127161=CARTESIAN_POINT('Ctrl Pts',(29.0941998536958,-67.0508343726777,
12.));
#127162=CARTESIAN_POINT('Ctrl Pts',(29.0947423892726,-67.0767580604879,
12.));
#127163=CARTESIAN_POINT('Ctrl Pts',(29.0952614183779,-67.1027204477311,
12.));
#127164=CARTESIAN_POINT('Ctrl Pts',(29.0957568873358,-67.1287214368746,
12.));
#127165=CARTESIAN_POINT('Ctrl Pts',(29.0962287427273,-67.1547609306843,
12.));
#127166=CARTESIAN_POINT('Ctrl Pts',(29.096676931389,-67.1808388322109,12.));
#127167=CARTESIAN_POINT('Ctrl Pts',(29.097101400413,-67.2069550447884,12.));
#127168=CARTESIAN_POINT('Ctrl Pts',(29.0975020971469,-67.2331094720471,
12.));
#127169=CARTESIAN_POINT('Ctrl Pts',(29.0978789691962,-67.2593020179209,
12.));
#127170=CARTESIAN_POINT('Ctrl Pts',(29.0982319644276,-67.2855325866517,
12.));
#127171=CARTESIAN_POINT('Ctrl Pts',(29.098561030977,-67.311801082792,12.));
#127172=CARTESIAN_POINT('Ctrl Pts',(29.098866117253,-67.3381074112027,12.));
#127173=CARTESIAN_POINT('Ctrl Pts',(29.0991471719176,-67.3644514770387,
12.));
#127174=CARTESIAN_POINT('Ctrl Pts',(29.0994041438718,-67.3908331857323,
12.));
#127175=CARTESIAN_POINT('Ctrl Pts',(29.0996369822418,-67.4172524429728,
12.));
#127176=CARTESIAN_POINT('Ctrl Pts',(29.0998456363682,-67.4437091546859,
12.));
#127177=CARTESIAN_POINT('Ctrl Pts',(29.1000300557955,-67.4702032270049,
12.));
#127178=CARTESIAN_POINT('Ctrl Pts',(29.1001901902908,-67.4967345663096,
12.));
#127179=CARTESIAN_POINT('Ctrl Pts',(29.1003259898681,-67.5233030792704,
12.));
#127180=CARTESIAN_POINT('Ctrl Pts',(29.1004374048147,-67.5499086728889,
12.));
#127181=CARTESIAN_POINT('Ctrl Pts',(29.1005243857138,-67.5765512545282,
12.));
#127182=CARTESIAN_POINT('Ctrl Pts',(29.1005868834866,-67.6032307319623,
12.));
#127183=CARTESIAN_POINT('Ctrl Pts',(29.100624849358,-67.6299470133295,12.));
#127184=CARTESIAN_POINT('Ctrl Pts',(29.1006382347814,-67.6567000070326,
12.));
#127185=CARTESIAN_POINT('Ctrl Pts',(29.1006269913747,-67.6834896216461,
12.));
#127186=CARTESIAN_POINT('Ctrl Pts',(29.1005910708624,-67.7103157658296,
12.));
#127187=CARTESIAN_POINT('Ctrl Pts',(29.1005304249986,-67.7371783482035,
12.));
#127188=CARTESIAN_POINT('Ctrl Pts',(29.1004450055642,-67.7640772773388,
12.));
#127189=CARTESIAN_POINT('Ctrl Pts',(29.1003347645293,-67.7910124620135,
12.));
#127190=CARTESIAN_POINT('Ctrl Pts',(29.1001996541841,-67.8179838114099,
12.));
#127191=CARTESIAN_POINT('Ctrl Pts',(29.1000396272867,-67.8449912353329,
12.));
#127192=CARTESIAN_POINT('Ctrl Pts',(29.0998546372032,-67.8720346444124,
12.));
#127193=CARTESIAN_POINT('Ctrl Pts',(29.0996446380626,-67.8991139503193,
12.));
#127194=CARTESIAN_POINT('Ctrl Pts',(29.099409584422,-67.9262290652829,12.));
#127195=CARTESIAN_POINT('Ctrl Pts',(29.0991494309404,-67.9533799016148,
12.));
#127196=CARTESIAN_POINT('Ctrl Pts',(29.0988641320246,-67.9805663711855,
12.));
#127197=CARTESIAN_POINT('Ctrl Pts',(29.098553641553,-68.0077883850121,12.));
#127198=CARTESIAN_POINT('Ctrl Pts',(29.0982179124097,-68.0350458525551,
12.));
#127199=CARTESIAN_POINT('Ctrl Pts',(29.0978568968656,-68.0623386822863,
12.));
#127200=CARTESIAN_POINT('Ctrl Pts',(29.0974705474258,-68.0896667829568,
12.));
#127201=CARTESIAN_POINT('Ctrl Pts',(29.0970588175728,-68.1170300646987,
12.));
#127202=CARTESIAN_POINT('Ctrl Pts',(29.0966216624743,-68.1444284400742,
12.));
#127203=CARTESIAN_POINT('Ctrl Pts',(29.0961590399046,-68.1718618254281,
12.));
#127204=CARTESIAN_POINT('Ctrl Pts',(29.0956709104627,-68.1993301412061,
12.));
#127205=CARTESIAN_POINT('Ctrl Pts',(29.095230591515,-68.2229056854684,12.));
#127206=CARTESIAN_POINT('Ctrl Pts',(29.094879194787,-68.2409993690197,12.));
#127207=CARTESIAN_POINT('Ctrl Pts',(29.0946280433337,-68.2535957747188,
12.));
#127208=CARTESIAN_POINT('Ctrl Pts',(29.0944846386568,-68.2606847334988,
12.));
#127209=CARTESIAN_POINT('Ctrl Pts',(29.0944526440265,-68.2622612910179,
12.));
#127210=CARTESIAN_POINT('',(28.8072485549236,-63.7976679095314,0.));
#127211=CARTESIAN_POINT('',(28.8072485549236,-63.7976679095314,0.));
#127212=CARTESIAN_POINT('Ctrl Pts',(29.0944526440265,-68.2622612910179,
0.));
#127213=CARTESIAN_POINT('Ctrl Pts',(29.0944846386568,-68.2606847334988,
0.));
#127214=CARTESIAN_POINT('Ctrl Pts',(29.0946280433337,-68.2535957747188,
0.));
#127215=CARTESIAN_POINT('Ctrl Pts',(29.094879194787,-68.2409993690197,0.));
#127216=CARTESIAN_POINT('Ctrl Pts',(29.095230591515,-68.2229056854684,0.));
#127217=CARTESIAN_POINT('Ctrl Pts',(29.0956709104627,-68.1993301412061,
0.));
#127218=CARTESIAN_POINT('Ctrl Pts',(29.0961590399046,-68.1718618254281,
0.));
#127219=CARTESIAN_POINT('Ctrl Pts',(29.0966216624743,-68.1444284400742,
0.));
#127220=CARTESIAN_POINT('Ctrl Pts',(29.0970588175728,-68.1170300646987,
0.));
#127221=CARTESIAN_POINT('Ctrl Pts',(29.0974705474258,-68.0896667829568,
0.));
#127222=CARTESIAN_POINT('Ctrl Pts',(29.0978568968656,-68.0623386822863,
0.));
#127223=CARTESIAN_POINT('Ctrl Pts',(29.0982179124097,-68.0350458525551,
0.));
#127224=CARTESIAN_POINT('Ctrl Pts',(29.098553641553,-68.0077883850121,0.));
#127225=CARTESIAN_POINT('Ctrl Pts',(29.0988641320246,-67.9805663711855,
0.));
#127226=CARTESIAN_POINT('Ctrl Pts',(29.0991494309404,-67.9533799016148,
0.));
#127227=CARTESIAN_POINT('Ctrl Pts',(29.099409584422,-67.9262290652829,0.));
#127228=CARTESIAN_POINT('Ctrl Pts',(29.0996446380626,-67.8991139503193,
0.));
#127229=CARTESIAN_POINT('Ctrl Pts',(29.0998546372032,-67.8720346444124,
0.));
#127230=CARTESIAN_POINT('Ctrl Pts',(29.1000396272867,-67.8449912353329,
0.));
#127231=CARTESIAN_POINT('Ctrl Pts',(29.1001996541841,-67.8179838114099,
0.));
#127232=CARTESIAN_POINT('Ctrl Pts',(29.1003347645293,-67.7910124620135,
0.));
#127233=CARTESIAN_POINT('Ctrl Pts',(29.1004450055642,-67.7640772773388,
0.));
#127234=CARTESIAN_POINT('Ctrl Pts',(29.1005304249986,-67.7371783482035,
0.));
#127235=CARTESIAN_POINT('Ctrl Pts',(29.1005910708624,-67.7103157658296,
0.));
#127236=CARTESIAN_POINT('Ctrl Pts',(29.1006269913747,-67.6834896216461,
0.));
#127237=CARTESIAN_POINT('Ctrl Pts',(29.1006382347814,-67.6567000070326,
0.));
#127238=CARTESIAN_POINT('Ctrl Pts',(29.100624849358,-67.6299470133295,0.));
#127239=CARTESIAN_POINT('Ctrl Pts',(29.1005868834866,-67.6032307319623,
0.));
#127240=CARTESIAN_POINT('Ctrl Pts',(29.1005243857138,-67.5765512545282,
0.));
#127241=CARTESIAN_POINT('Ctrl Pts',(29.1004374048147,-67.5499086728889,
0.));
#127242=CARTESIAN_POINT('Ctrl Pts',(29.1003259898681,-67.5233030792704,
0.));
#127243=CARTESIAN_POINT('Ctrl Pts',(29.1001901902908,-67.4967345663096,
0.));
#127244=CARTESIAN_POINT('Ctrl Pts',(29.1000300557955,-67.4702032270049,
0.));
#127245=CARTESIAN_POINT('Ctrl Pts',(29.0998456363682,-67.4437091546859,
0.));
#127246=CARTESIAN_POINT('Ctrl Pts',(29.0996369822418,-67.4172524429728,
0.));
#127247=CARTESIAN_POINT('Ctrl Pts',(29.0994041438718,-67.3908331857323,
0.));
#127248=CARTESIAN_POINT('Ctrl Pts',(29.0991471719176,-67.3644514770387,
0.));
#127249=CARTESIAN_POINT('Ctrl Pts',(29.098866117253,-67.3381074112027,0.));
#127250=CARTESIAN_POINT('Ctrl Pts',(29.098561030977,-67.311801082792,0.));
#127251=CARTESIAN_POINT('Ctrl Pts',(29.0982319644276,-67.2855325866517,
0.));
#127252=CARTESIAN_POINT('Ctrl Pts',(29.0978789691962,-67.2593020179209,
0.));
#127253=CARTESIAN_POINT('Ctrl Pts',(29.0975020971469,-67.2331094720471,
0.));
#127254=CARTESIAN_POINT('Ctrl Pts',(29.097101400413,-67.2069550447884,0.));
#127255=CARTESIAN_POINT('Ctrl Pts',(29.096676931389,-67.1808388322109,0.));
#127256=CARTESIAN_POINT('Ctrl Pts',(29.0962287427273,-67.1547609306843,
0.));
#127257=CARTESIAN_POINT('Ctrl Pts',(29.0957568873358,-67.1287214368746,
0.));
#127258=CARTESIAN_POINT('Ctrl Pts',(29.0952614183779,-67.1027204477311,
0.));
#127259=CARTESIAN_POINT('Ctrl Pts',(29.0947423892726,-67.0767580604879,
0.));
#127260=CARTESIAN_POINT('Ctrl Pts',(29.0941998536958,-67.0508343726777,
0.));
#127261=CARTESIAN_POINT('Ctrl Pts',(29.0936338655828,-67.0249494821363,
0.));
#127262=CARTESIAN_POINT('Ctrl Pts',(29.0930444791328,-66.9991034870083,
0.));
#127263=CARTESIAN_POINT('Ctrl Pts',(29.092431748817,-66.9732964857466,0.));
#127264=CARTESIAN_POINT('Ctrl Pts',(29.0917957293826,-66.9475285771135,
0.));
#127265=CARTESIAN_POINT('Ctrl Pts',(29.0911364758486,-66.9217998601885,
0.));
#127266=CARTESIAN_POINT('Ctrl Pts',(29.0904540435065,-66.8961104343707,
0.));
#127267=CARTESIAN_POINT('Ctrl Pts',(29.0897484879207,-66.8704603993794,
0.));
#127268=CARTESIAN_POINT('Ctrl Pts',(29.0890198649323,-66.8448498552503,
0.));
#127269=CARTESIAN_POINT('Ctrl Pts',(29.088268230663,-66.8192789023312,0.));
#127270=CARTESIAN_POINT('Ctrl Pts',(29.0874936415131,-66.793747641293,0.));
#127271=CARTESIAN_POINT('Ctrl Pts',(29.0866961541625,-66.7682561731342,
0.));
#127272=CARTESIAN_POINT('Ctrl Pts',(29.0858758255728,-66.7428045991841,
0.));
#127273=CARTESIAN_POINT('Ctrl Pts',(29.0850327129916,-66.7173930211022,
0.));
#127274=CARTESIAN_POINT('Ctrl Pts',(29.0841668739588,-66.6920215408751,
0.));
#127275=CARTESIAN_POINT('Ctrl Pts',(29.0832783663049,-66.6666902608249,
0.));
#127276=CARTESIAN_POINT('Ctrl Pts',(29.0823672481507,-66.6413992836147,
0.));
#127277=CARTESIAN_POINT('Ctrl Pts',(29.0814335779084,-66.6161487122502,
0.));
#127278=CARTESIAN_POINT('Ctrl Pts',(29.0804774142853,-66.59093865008,0.));
#127279=CARTESIAN_POINT('Ctrl Pts',(29.0794988162897,-66.5657692007906,
0.));
#127280=CARTESIAN_POINT('Ctrl Pts',(29.07849784323,-66.5406404684132,0.));
#127281=CARTESIAN_POINT('Ctrl Pts',(29.0774745547151,-66.5155525573323,
0.));
#127282=CARTESIAN_POINT('Ctrl Pts',(29.0764290106554,-66.4905055722868,
0.));
#127283=CARTESIAN_POINT('Ctrl Pts',(29.0753612712665,-66.4654996183731,
0.));
#127284=CARTESIAN_POINT('Ctrl Pts',(29.0742713970755,-66.4405348010388,
0.));
#127285=CARTESIAN_POINT('Ctrl Pts',(29.0731594489211,-66.4156112260887,
0.));
#127286=CARTESIAN_POINT('Ctrl Pts',(29.072025487953,-66.3907289996932,0.));
#127287=CARTESIAN_POINT('Ctrl Pts',(29.0708695756334,-66.3658882283903,
0.));
#127288=CARTESIAN_POINT('Ctrl Pts',(29.0696917737399,-66.3410890190884,
0.));
#127289=CARTESIAN_POINT('Ctrl Pts',(29.0684921443721,-66.3163314790615,
0.));
#127290=CARTESIAN_POINT('Ctrl Pts',(29.0672707499529,-66.2916157159536,
0.));
#127291=CARTESIAN_POINT('Ctrl Pts',(29.0660276532273,-66.2669418377871,
0.));
#127292=CARTESIAN_POINT('Ctrl Pts',(29.0647629172644,-66.2423099529669,
0.));
#127293=CARTESIAN_POINT('Ctrl Pts',(29.0634766054598,-66.2177201702818,
0.));
#127294=CARTESIAN_POINT('Ctrl Pts',(29.062168781542,-66.1931725989008,0.));
#127295=CARTESIAN_POINT('Ctrl Pts',(29.0608395095746,-66.1686673483757,
0.));
#127296=CARTESIAN_POINT('Ctrl Pts',(29.0594888539557,-66.144204528652,0.));
#127297=CARTESIAN_POINT('Ctrl Pts',(29.058116879419,-66.1197842500714,0.));
#127298=CARTESIAN_POINT('Ctrl Pts',(29.0567236510372,-66.0954066233752,
0.));
#127299=CARTESIAN_POINT('Ctrl Pts',(29.0553092342274,-66.0710717597003,
0.));
#127300=CARTESIAN_POINT('Ctrl Pts',(29.0538736947547,-66.0467797705806,
0.));
#127301=CARTESIAN_POINT('Ctrl Pts',(29.0524170987302,-66.0225307679584,
0.));
#127302=CARTESIAN_POINT('Ctrl Pts',(29.0509395126141,-65.9983248641877,
0.));
#127303=CARTESIAN_POINT('Ctrl Pts',(29.0494410032173,-65.9741621720372,
0.));
#127304=CARTESIAN_POINT('Ctrl Pts',(29.0479216377082,-65.9500428046873,
0.));
#127305=CARTESIAN_POINT('Ctrl Pts',(29.0463814836158,-65.925966875731,0.));
#127306=CARTESIAN_POINT('Ctrl Pts',(29.0448206088288,-65.9019344991854,
0.));
#127307=CARTESIAN_POINT('Ctrl Pts',(29.0432390815976,-65.8779457894959,
0.));
#127308=CARTESIAN_POINT('Ctrl Pts',(29.0416369705375,-65.854000861539,0.));
#127309=CARTESIAN_POINT('Ctrl Pts',(29.040014344634,-65.8300998306198,0.));
#127310=CARTESIAN_POINT('Ctrl Pts',(29.0383712732473,-65.8062428124723,
0.));
#127311=CARTESIAN_POINT('Ctrl Pts',(29.0367078261107,-65.7824299232715,
0.));
#127312=CARTESIAN_POINT('Ctrl Pts',(29.0350240733332,-65.7586612796375,
0.));
#127313=CARTESIAN_POINT('Ctrl Pts',(29.0333200854026,-65.7349369986382,
0.));
#127314=CARTESIAN_POINT('Ctrl Pts',(29.0315959331911,-65.7112571977874,
0.));
#127315=CARTESIAN_POINT('Ctrl Pts',(29.0298516879599,-65.6876219950465,
0.));
#127316=CARTESIAN_POINT('Ctrl Pts',(29.0280874213584,-65.6640315088361,
0.));
#127317=CARTESIAN_POINT('Ctrl Pts',(29.0263032054261,-65.6404858580391,
0.));
#127318=CARTESIAN_POINT('Ctrl Pts',(29.0244991125961,-65.6169851620054,
0.));
#127319=CARTESIAN_POINT('Ctrl Pts',(29.0226752157013,-65.593529540548,0.));
#127320=CARTESIAN_POINT('Ctrl Pts',(29.0208315879778,-65.5701191139455,
0.));
#127321=CARTESIAN_POINT('Ctrl Pts',(29.0189683030654,-65.5467540029546,
0.));
#127322=CARTESIAN_POINT('Ctrl Pts',(29.01708543501,-65.523434328815,0.));
#127323=CARTESIAN_POINT('Ctrl Pts',(29.015183058267,-65.5001602132524,0.));
#127324=CARTESIAN_POINT('Ctrl Pts',(29.0132612477075,-65.4769317784754,
0.));
#127325=CARTESIAN_POINT('Ctrl Pts',(29.0113200786218,-65.4537491471782,
0.));
#127326=CARTESIAN_POINT('Ctrl Pts',(29.0093596267198,-65.4306124425524,
0.));
#127327=CARTESIAN_POINT('Ctrl Pts',(29.0073799681335,-65.4075217882921,
0.));
#127328=CARTESIAN_POINT('Ctrl Pts',(29.0053811794213,-65.3844773085977,
0.));
#127329=CARTESIAN_POINT('Ctrl Pts',(29.0033633375744,-65.3614791281726,
0.));
#127330=CARTESIAN_POINT('Ctrl Pts',(29.0013265200201,-65.3385273722279,
0.));
#127331=CARTESIAN_POINT('Ctrl Pts',(28.9992708046223,-65.3156221664942,
0.));
#127332=CARTESIAN_POINT('Ctrl Pts',(28.9971962696848,-65.2927636372261,
0.));
#127333=CARTESIAN_POINT('Ctrl Pts',(28.9951029939551,-65.2699519112052,
0.));
#127334=CARTESIAN_POINT('Ctrl Pts',(28.9929910566314,-65.2471871157375,
0.));
#127335=CARTESIAN_POINT('Ctrl Pts',(28.9908605373651,-65.2244693786586,
0.));
#127336=CARTESIAN_POINT('Ctrl Pts',(28.9887115162626,-65.2017988283465,
0.));
#127337=CARTESIAN_POINT('Ctrl Pts',(28.9865440738882,-65.1791755937254,
0.));
#127338=CARTESIAN_POINT('Ctrl Pts',(28.9843582912696,-65.1565998042706,
0.));
#127339=CARTESIAN_POINT('Ctrl Pts',(28.9821542499049,-65.1340715900042,
0.));
#127340=CARTESIAN_POINT('Ctrl Pts',(28.9799320317648,-65.1115910815051,
0.));
#127341=CARTESIAN_POINT('Ctrl Pts',(28.9776917192936,-65.0891584099174,
0.));
#127342=CARTESIAN_POINT('Ctrl Pts',(28.9754333954134,-65.0667737069562,
0.));
#127343=CARTESIAN_POINT('Ctrl Pts',(28.9731571435281,-65.0444371049082,
0.));
#127344=CARTESIAN_POINT('Ctrl Pts',(28.9708630475298,-65.022148736628,0.));
#127345=CARTESIAN_POINT('Ctrl Pts',(28.9685511918016,-64.9999087355504,
0.));
#127346=CARTESIAN_POINT('Ctrl Pts',(28.9662216612216,-64.9777172357028,
0.));
#127347=CARTESIAN_POINT('Ctrl Pts',(28.9638745411676,-64.955574371711,0.));
#127348=CARTESIAN_POINT('Ctrl Pts',(28.9615099175249,-64.9334802788037,
0.));
#127349=CARTESIAN_POINT('Ctrl Pts',(28.9591278766934,-64.9114350928124,
0.));
#127350=CARTESIAN_POINT('Ctrl Pts',(28.9567285055865,-64.8894389501799,
0.));
#127351=CARTESIAN_POINT('Ctrl Pts',(28.9543118916327,-64.8674919879646,
0.));
#127352=CARTESIAN_POINT('Ctrl Pts',(28.9518781227764,-64.8455943438424,
0.));
#127353=CARTESIAN_POINT('Ctrl Pts',(28.9494272874833,-64.8237461561024,
0.));
#127354=CARTESIAN_POINT('Ctrl Pts',(28.9469594747436,-64.8019475636454,
0.));
#127355=CARTESIAN_POINT('Ctrl Pts',(28.9444747740815,-64.7801987060097,
0.));
#127356=CARTESIAN_POINT('Ctrl Pts',(28.9419732755659,-64.7584997233889,
0.));
#127357=CARTESIAN_POINT('Ctrl Pts',(28.9394550698201,-64.7368507566462,
0.));
#127358=CARTESIAN_POINT('Ctrl Pts',(28.9369202480383,-64.715251947327,0.));
#127359=CARTESIAN_POINT('Ctrl Pts',(28.9343689019869,-64.6937034376591,
0.));
#127360=CARTESIAN_POINT('Ctrl Pts',(28.9318011239905,-64.6722053705389,
0.));
#127361=CARTESIAN_POINT('Ctrl Pts',(28.9292170069219,-64.6507578895155,
0.));
#127362=CARTESIAN_POINT('Ctrl Pts',(28.9266166441956,-64.6293611387754,
0.));
#127363=CARTESIAN_POINT('Ctrl Pts',(28.9240001297553,-64.6080152631066,
0.));
#127364=CARTESIAN_POINT('Ctrl Pts',(28.9213675580996,-64.5867204079452,
0.));
#127365=CARTESIAN_POINT('Ctrl Pts',(28.918719024323,-64.5654767194488,0.));
#127366=CARTESIAN_POINT('Ctrl Pts',(28.9160546241538,-64.544284344556,0.));
#127367=CARTESIAN_POINT('Ctrl Pts',(28.9133744539942,-64.5231434310457,
0.));
#127368=CARTESIAN_POINT('Ctrl Pts',(28.9106786109638,-64.5020541275927,
0.));
#127369=CARTESIAN_POINT('Ctrl Pts',(28.9079671928252,-64.4810165836568,
0.));
#127370=CARTESIAN_POINT('Ctrl Pts',(28.9052402979055,-64.460030949357,0.));
#127371=CARTESIAN_POINT('Ctrl Pts',(28.9024980250309,-64.439097375364,0.));
#127372=CARTESIAN_POINT('Ctrl Pts',(28.8997404734349,-64.4182160127401,
0.));
#127373=CARTESIAN_POINT('Ctrl Pts',(28.8969677427518,-64.3973870129201,
0.));
#127374=CARTESIAN_POINT('Ctrl Pts',(28.8941799332312,-64.3766105280715,
0.));
#127375=CARTESIAN_POINT('Ctrl Pts',(28.8913771459327,-64.3558867114087,
0.));
#127376=CARTESIAN_POINT('Ctrl Pts',(28.8885594828919,-64.3352157174607,
0.));
#127377=CARTESIAN_POINT('Ctrl Pts',(28.8857270473944,-64.3145977025005,
0.));
#127378=CARTESIAN_POINT('Ctrl Pts',(28.8828799437922,-64.2940328242483,
0.));
#127379=CARTESIAN_POINT('Ctrl Pts',(28.8800182770051,-64.2735212410682,
0.));
#127380=CARTESIAN_POINT('Ctrl Pts',(28.8771421521058,-64.2530631112927,
0.));
#127381=CARTESIAN_POINT('Ctrl Pts',(28.8742516738958,-64.232658592528,0.));
#127382=CARTESIAN_POINT('Ctrl Pts',(28.8713469464205,-64.2123078408507,
0.));
#127383=CARTESIAN_POINT('Ctrl Pts',(28.8684280739032,-64.1920110123342,
0.));
#127384=CARTESIAN_POINT('Ctrl Pts',(28.8654951618658,-64.1717682648708,
0.));
#127385=CARTESIAN_POINT('Ctrl Pts',(28.8625483180433,-64.1515797596555,
0.));
#127386=CARTESIAN_POINT('Ctrl Pts',(28.8595876537131,-64.1314456633345,
0.));
#127387=CARTESIAN_POINT('Ctrl Pts',(28.8566132838156,-64.1113661481918,
0.));
#127388=CARTESIAN_POINT('Ctrl Pts',(28.8536253241836,-64.0913413876586,
0.));
#127389=CARTESIAN_POINT('Ctrl Pts',(28.8506238891086,-64.0713715523588,
0.));
#127390=CARTESIAN_POINT('Ctrl Pts',(28.8476090892242,-64.0514568066659,
0.));
#127391=CARTESIAN_POINT('Ctrl Pts',(28.8445810281275,-64.0315973031995,
0.));
#127392=CARTESIAN_POINT('Ctrl Pts',(28.841539805646,-64.0117931881364,0.));
#127393=CARTESIAN_POINT('Ctrl Pts',(28.8384855243267,-63.9920446117632,
0.));
#127394=CARTESIAN_POINT('Ctrl Pts',(28.83541829466,-63.9723517369614,0.));
#127395=CARTESIAN_POINT('Ctrl Pts',(28.8323382413752,-63.9527147494351,
0.));
#127396=CARTESIAN_POINT('Ctrl Pts',(28.8292455077494,-63.9331338646868,
0.));
#127397=CARTESIAN_POINT('Ctrl Pts',(28.8261402423219,-63.9136093063647,
0.));
#127398=CARTESIAN_POINT('Ctrl Pts',(28.8230225863142,-63.894141285685,0.));
#127399=CARTESIAN_POINT('Ctrl Pts',(28.8198926619892,-63.8747299825383,
0.));
#127400=CARTESIAN_POINT('Ctrl Pts',(28.8167505576805,-63.8553755207732,
0.));
#127401=CARTESIAN_POINT('Ctrl Pts',(28.8135963263556,-63.8360779670226,
0.));
#127402=CARTESIAN_POINT('Ctrl Pts',(28.8110632621132,-63.8206854735372,
0.));
#127403=CARTESIAN_POINT('Ctrl Pts',(28.8091580239664,-63.8091667271451,
0.));
#127404=CARTESIAN_POINT('Ctrl Pts',(28.8078854475473,-63.8014989507576,
0.));
#127405=CARTESIAN_POINT('Ctrl Pts',(28.8072485549236,-63.7976679095314,
0.));
#127406=CARTESIAN_POINT('Ctrl Pts',(22.9976507259816,-70.8615414811572,
0.));
#127407=CARTESIAN_POINT('Ctrl Pts',(22.9976507259816,-70.8615414811572,
12.));
#127408=CARTESIAN_POINT('Ctrl Pts',(22.9983100639391,-70.8559846928,0.));
#127409=CARTESIAN_POINT('Ctrl Pts',(22.9983100639391,-70.8559846928,12.));
#127410=CARTESIAN_POINT('Ctrl Pts',(22.999625855529,-70.8448742696689,0.));
#127411=CARTESIAN_POINT('Ctrl Pts',(22.999625855529,-70.8448742696689,12.));
#127412=CARTESIAN_POINT('Ctrl Pts',(23.0015908899394,-70.8282180957225,
0.));
#127413=CARTESIAN_POINT('Ctrl Pts',(23.0015908899394,-70.8282180957225,
12.));
#127414=CARTESIAN_POINT('Ctrl Pts',(23.0041936291625,-70.8060287860585,
0.));
#127415=CARTESIAN_POINT('Ctrl Pts',(23.0041936291625,-70.8060287860585,
12.));
#127416=CARTESIAN_POINT('Ctrl Pts',(23.0074182063786,-70.7783236951202,
0.));
#127417=CARTESIAN_POINT('Ctrl Pts',(23.0074182063786,-70.7783236951202,
12.));
#127418=CARTESIAN_POINT('Ctrl Pts',(23.0106139366046,-70.750650169619,0.));
#127419=CARTESIAN_POINT('Ctrl Pts',(23.0106139366046,-70.750650169619,12.));
#127420=CARTESIAN_POINT('Ctrl Pts',(23.0137808248923,-70.7230082425413,
0.));
#127421=CARTESIAN_POINT('Ctrl Pts',(23.0137808248923,-70.7230082425413,
12.));
#127422=CARTESIAN_POINT('Ctrl Pts',(23.0169188841044,-70.6953979633426,
0.));
#127423=CARTESIAN_POINT('Ctrl Pts',(23.0169188841044,-70.6953979633426,
12.));
#127424=CARTESIAN_POINT('Ctrl Pts',(23.0200281385833,-70.6678194023135,
0.));
#127425=CARTESIAN_POINT('Ctrl Pts',(23.0200281385833,-70.6678194023135,
12.));
#127426=CARTESIAN_POINT('Ctrl Pts',(23.0231086235186,-70.6402726486453,
0.));
#127427=CARTESIAN_POINT('Ctrl Pts',(23.0231086235186,-70.6402726486453,
12.));
#127428=CARTESIAN_POINT('Ctrl Pts',(23.026160381013,-70.6127578036674,0.));
#127429=CARTESIAN_POINT('Ctrl Pts',(23.026160381013,-70.6127578036674,12.));
#127430=CARTESIAN_POINT('Ctrl Pts',(23.0291834570662,-70.5852749754082,
0.));
#127431=CARTESIAN_POINT('Ctrl Pts',(23.0291834570662,-70.5852749754082,
12.));
#127432=CARTESIAN_POINT('Ctrl Pts',(23.0321778982711,-70.5578242727627,
0.));
#127433=CARTESIAN_POINT('Ctrl Pts',(23.0321778982711,-70.5578242727627,
12.));
#127434=CARTESIAN_POINT('Ctrl Pts',(23.0351437484336,-70.5304057994631,
0.));
#127435=CARTESIAN_POINT('Ctrl Pts',(23.0351437484336,-70.5304057994631,
12.));
#127436=CARTESIAN_POINT('Ctrl Pts',(23.0380810458271,-70.5030196492003,
0.));
#127437=CARTESIAN_POINT('Ctrl Pts',(23.0380810458271,-70.5030196492003,
12.));
#127438=CARTESIAN_POINT('Ctrl Pts',(23.0409898250756,-70.4756659090209,
0.));
#127439=CARTESIAN_POINT('Ctrl Pts',(23.0409898250756,-70.4756659090209,
12.));
#127440=CARTESIAN_POINT('Ctrl Pts',(23.0438701185012,-70.4483446617614,
0.));
#127441=CARTESIAN_POINT('Ctrl Pts',(23.0438701185012,-70.4483446617614,
12.));
#127442=CARTESIAN_POINT('Ctrl Pts',(23.046721957729,-70.4210559889348,0.));
#127443=CARTESIAN_POINT('Ctrl Pts',(23.046721957729,-70.4210559889348,12.));
#127444=CARTESIAN_POINT('Ctrl Pts',(23.0495453750763,-70.3937999732267,
0.));
#127445=CARTESIAN_POINT('Ctrl Pts',(23.0495453750763,-70.3937999732267,
12.));
#127446=CARTESIAN_POINT('Ctrl Pts',(23.0523404053172,-70.3665767016542,
0.));
#127447=CARTESIAN_POINT('Ctrl Pts',(23.0523404053172,-70.3665767016542,
12.));
#127448=CARTESIAN_POINT('Ctrl Pts',(23.0551070854926,-70.3393862652297,
0.));
#127449=CARTESIAN_POINT('Ctrl Pts',(23.0551070854926,-70.3393862652297,
12.));
#127450=CARTESIAN_POINT('Ctrl Pts',(23.0578454541104,-70.3122287575335,
0.));
#127451=CARTESIAN_POINT('Ctrl Pts',(23.0578454541104,-70.3122287575335,
12.));
#127452=CARTESIAN_POINT('Ctrl Pts',(23.0605555505321,-70.2851042736066,
0.));
#127453=CARTESIAN_POINT('Ctrl Pts',(23.0605555505321,-70.2851042736066,
12.));
#127454=CARTESIAN_POINT('Ctrl Pts',(23.0632374143279,-70.2580129087888,
0.));
#127455=CARTESIAN_POINT('Ctrl Pts',(23.0632374143279,-70.2580129087888,
12.));
#127456=CARTESIAN_POINT('Ctrl Pts',(23.0658910845432,-70.2309547573815,
0.));
#127457=CARTESIAN_POINT('Ctrl Pts',(23.0658910845432,-70.2309547573815,
12.));
#127458=CARTESIAN_POINT('Ctrl Pts',(23.068516599369,-70.2039299120488,0.));
#127459=CARTESIAN_POINT('Ctrl Pts',(23.068516599369,-70.2039299120488,12.));
#127460=CARTESIAN_POINT('Ctrl Pts',(23.0711139965439,-70.1769384645587,
0.));
#127461=CARTESIAN_POINT('Ctrl Pts',(23.0711139965439,-70.1769384645587,
12.));
#127462=CARTESIAN_POINT('Ctrl Pts',(23.0736833135938,-70.1499805062172,
0.));
#127463=CARTESIAN_POINT('Ctrl Pts',(23.0736833135938,-70.1499805062172,
12.));
#127464=CARTESIAN_POINT('Ctrl Pts',(23.0762245881389,-70.1230561284221,
0.));
#127465=CARTESIAN_POINT('Ctrl Pts',(23.0762245881389,-70.1230561284221,
12.));
#127466=CARTESIAN_POINT('Ctrl Pts',(23.0787378581774,-70.0961654231639,
0.));
#127467=CARTESIAN_POINT('Ctrl Pts',(23.0787378581774,-70.0961654231639,
12.));
#127468=CARTESIAN_POINT('Ctrl Pts',(23.0812231623765,-70.0693084835373,
0.));
#127469=CARTESIAN_POINT('Ctrl Pts',(23.0812231623765,-70.0693084835373,
12.));
#127470=CARTESIAN_POINT('Ctrl Pts',(23.0836805399374,-70.0424854035115,
0.));
#127471=CARTESIAN_POINT('Ctrl Pts',(23.0836805399374,-70.0424854035115,
12.));
#127472=CARTESIAN_POINT('Ctrl Pts',(23.0861100304729,-70.0156962777169,
0.));
#127473=CARTESIAN_POINT('Ctrl Pts',(23.0861100304729,-70.0156962777169,
12.));
#127474=CARTESIAN_POINT('Ctrl Pts',(23.0885116738797,-69.9889412012143,
0.));
#127475=CARTESIAN_POINT('Ctrl Pts',(23.0885116738797,-69.9889412012143,
12.));
#127476=CARTESIAN_POINT('Ctrl Pts',(23.090885510225,-69.9622202692873,0.));
#127477=CARTESIAN_POINT('Ctrl Pts',(23.090885510225,-69.9622202692873,12.));
#127478=CARTESIAN_POINT('Ctrl Pts',(23.0932315796067,-69.9355335771729,
0.));
#127479=CARTESIAN_POINT('Ctrl Pts',(23.0932315796067,-69.9355335771729,
12.));
#127480=CARTESIAN_POINT('Ctrl Pts',(23.0955499221558,-69.9088812200713,
0.));
#127481=CARTESIAN_POINT('Ctrl Pts',(23.0955499221558,-69.9088812200713,
12.));
#127482=CARTESIAN_POINT('Ctrl Pts',(23.097840578102,-69.8822632932768,0.));
#127483=CARTESIAN_POINT('Ctrl Pts',(23.097840578102,-69.8822632932768,12.));
#127484=CARTESIAN_POINT('Ctrl Pts',(23.1001035878241,-69.8556798922693,
0.));
#127485=CARTESIAN_POINT('Ctrl Pts',(23.1001035878241,-69.8556798922693,
12.));
#127486=CARTESIAN_POINT('Ctrl Pts',(23.1023389919051,-69.8291311128119,
0.));
#127487=CARTESIAN_POINT('Ctrl Pts',(23.1023389919051,-69.8291311128119,
12.));
#127488=CARTESIAN_POINT('Ctrl Pts',(23.104546831199,-69.8026170510572,0.));
#127489=CARTESIAN_POINT('Ctrl Pts',(23.104546831199,-69.8026170510572,12.));
#127490=CARTESIAN_POINT('Ctrl Pts',(23.1067271468609,-69.7761378035964,
0.));
#127491=CARTESIAN_POINT('Ctrl Pts',(23.1067271468609,-69.7761378035964,
12.));
#127492=CARTESIAN_POINT('Ctrl Pts',(23.1088799803089,-69.7496934674069,
0.));
#127493=CARTESIAN_POINT('Ctrl Pts',(23.1088799803089,-69.7496934674069,
12.));
#127494=CARTESIAN_POINT('Ctrl Pts',(23.1110053732046,-69.7232841398197,
0.));
#127495=CARTESIAN_POINT('Ctrl Pts',(23.1110053732046,-69.7232841398197,
12.));
#127496=CARTESIAN_POINT('Ctrl Pts',(23.1131033674301,-69.6969099184767,
0.));
#127497=CARTESIAN_POINT('Ctrl Pts',(23.1131033674301,-69.6969099184767,
12.));
#127498=CARTESIAN_POINT('Ctrl Pts',(23.115174005068,-69.6705709012852,0.));
#127499=CARTESIAN_POINT('Ctrl Pts',(23.115174005068,-69.6705709012852,12.));
#127500=CARTESIAN_POINT('Ctrl Pts',(23.1172173283858,-69.6442671863765,
0.));
#127501=CARTESIAN_POINT('Ctrl Pts',(23.1172173283858,-69.6442671863765,
12.));
#127502=CARTESIAN_POINT('Ctrl Pts',(23.1192333798441,-69.6179988721365,
0.));
#127503=CARTESIAN_POINT('Ctrl Pts',(23.1192333798441,-69.6179988721365,
12.));
#127504=CARTESIAN_POINT('Ctrl Pts',(23.1212222021051,-69.5917660572265,
0.));
#127505=CARTESIAN_POINT('Ctrl Pts',(23.1212222021051,-69.5917660572265,
12.));
#127506=CARTESIAN_POINT('Ctrl Pts',(23.1231838380452,-69.5655688406052,
0.));
#127507=CARTESIAN_POINT('Ctrl Pts',(23.1231838380452,-69.5655688406052,
12.));
#127508=CARTESIAN_POINT('Ctrl Pts',(23.1251183307676,-69.539407321546,0.));
#127509=CARTESIAN_POINT('Ctrl Pts',(23.1251183307676,-69.539407321546,12.));
#127510=CARTESIAN_POINT('Ctrl Pts',(23.1270257236204,-69.5132815996537,
0.));
#127511=CARTESIAN_POINT('Ctrl Pts',(23.1270257236204,-69.5132815996537,
12.));
#127512=CARTESIAN_POINT('Ctrl Pts',(23.1289060601924,-69.4871917748654,
0.));
#127513=CARTESIAN_POINT('Ctrl Pts',(23.1289060601924,-69.4871917748654,
12.));
#127514=CARTESIAN_POINT('Ctrl Pts',(23.1307593843061,-69.4611379474484,
0.));
#127515=CARTESIAN_POINT('Ctrl Pts',(23.1307593843061,-69.4611379474484,
12.));
#127516=CARTESIAN_POINT('Ctrl Pts',(23.1325857400144,-69.4351202179946,
0.));
#127517=CARTESIAN_POINT('Ctrl Pts',(23.1325857400144,-69.4351202179946,
12.));
#127518=CARTESIAN_POINT('Ctrl Pts',(23.1343851715989,-69.4091386874132,
0.));
#127519=CARTESIAN_POINT('Ctrl Pts',(23.1343851715989,-69.4091386874132,
12.));
#127520=CARTESIAN_POINT('Ctrl Pts',(23.1361577235709,-69.3831934569183,
0.));
#127521=CARTESIAN_POINT('Ctrl Pts',(23.1361577235709,-69.3831934569183,
12.));
#127522=CARTESIAN_POINT('Ctrl Pts',(23.1379034406718,-69.3572846280297,
0.));
#127523=CARTESIAN_POINT('Ctrl Pts',(23.1379034406718,-69.3572846280297,
12.));
#127524=CARTESIAN_POINT('Ctrl Pts',(23.1396223678725,-69.3314123025869,
0.));
#127525=CARTESIAN_POINT('Ctrl Pts',(23.1396223678725,-69.3314123025869,
12.));
#127526=CARTESIAN_POINT('Ctrl Pts',(23.1413145503762,-69.3055765827546,
0.));
#127527=CARTESIAN_POINT('Ctrl Pts',(23.1413145503762,-69.3055765827546,
12.));
#127528=CARTESIAN_POINT('Ctrl Pts',(23.142980033622,-69.2797775710273,0.));
#127529=CARTESIAN_POINT('Ctrl Pts',(23.142980033622,-69.2797775710273,12.));
#127530=CARTESIAN_POINT('Ctrl Pts',(23.1446188632931,-69.254015370231,0.));
#127531=CARTESIAN_POINT('Ctrl Pts',(23.1446188632931,-69.254015370231,12.));
#127532=CARTESIAN_POINT('Ctrl Pts',(23.1462310853206,-69.2282900835236,
0.));
#127533=CARTESIAN_POINT('Ctrl Pts',(23.1462310853206,-69.2282900835236,
12.));
#127534=CARTESIAN_POINT('Ctrl Pts',(23.1478167458789,-69.2026018144028,
0.));
#127535=CARTESIAN_POINT('Ctrl Pts',(23.1478167458789,-69.2026018144028,
12.));
#127536=CARTESIAN_POINT('Ctrl Pts',(23.1493758913858,-69.1769506667084,
0.));
#127537=CARTESIAN_POINT('Ctrl Pts',(23.1493758913858,-69.1769506667084,
12.));
#127538=CARTESIAN_POINT('Ctrl Pts',(23.1509085685032,-69.1513367446231,
0.));
#127539=CARTESIAN_POINT('Ctrl Pts',(23.1509085685032,-69.1513367446231,
12.));
#127540=CARTESIAN_POINT('Ctrl Pts',(23.152414824141,-69.1257601526687,0.));
#127541=CARTESIAN_POINT('Ctrl Pts',(23.152414824141,-69.1257601526687,12.));
#127542=CARTESIAN_POINT('Ctrl Pts',(23.1538947054614,-69.1002209957025,
0.));
#127543=CARTESIAN_POINT('Ctrl Pts',(23.1538947054614,-69.1002209957025,
12.));
#127544=CARTESIAN_POINT('Ctrl Pts',(23.1553482598762,-69.074719378928,0.));
#127545=CARTESIAN_POINT('Ctrl Pts',(23.1553482598762,-69.074719378928,12.));
#127546=CARTESIAN_POINT('Ctrl Pts',(23.1567755350469,-69.0492554078992,
0.));
#127547=CARTESIAN_POINT('Ctrl Pts',(23.1567755350469,-69.0492554078992,
12.));
#127548=CARTESIAN_POINT('Ctrl Pts',(23.1581765788868,-69.0238291885245,
0.));
#127549=CARTESIAN_POINT('Ctrl Pts',(23.1581765788868,-69.0238291885245,
12.));
#127550=CARTESIAN_POINT('Ctrl Pts',(23.1595514395656,-68.9984408270659,
0.));
#127551=CARTESIAN_POINT('Ctrl Pts',(23.1595514395656,-68.9984408270659,
12.));
#127552=CARTESIAN_POINT('Ctrl Pts',(23.1609001655155,-68.9730904301369,
0.));
#127553=CARTESIAN_POINT('Ctrl Pts',(23.1609001655155,-68.9730904301369,
12.));
#127554=CARTESIAN_POINT('Ctrl Pts',(23.1622228054291,-68.9477781047106,
0.));
#127555=CARTESIAN_POINT('Ctrl Pts',(23.1622228054291,-68.9477781047106,
12.));
#127556=CARTESIAN_POINT('Ctrl Pts',(23.1635194082581,-68.9225039581248,
0.));
#127557=CARTESIAN_POINT('Ctrl Pts',(23.1635194082581,-68.9225039581248,
12.));
#127558=CARTESIAN_POINT('Ctrl Pts',(23.164790023215,-68.8972680980842,0.));
#127559=CARTESIAN_POINT('Ctrl Pts',(23.164790023215,-68.8972680980842,12.));
#127560=CARTESIAN_POINT('Ctrl Pts',(23.1660346997763,-68.872070632661,0.));
#127561=CARTESIAN_POINT('Ctrl Pts',(23.1660346997763,-68.872070632661,12.));
#127562=CARTESIAN_POINT('Ctrl Pts',(23.1672534876889,-68.8469116702898,
0.));
#127563=CARTESIAN_POINT('Ctrl Pts',(23.1672534876889,-68.8469116702898,
12.));
#127564=CARTESIAN_POINT('Ctrl Pts',(23.1684464369686,-68.8217913197752,
0.));
#127565=CARTESIAN_POINT('Ctrl Pts',(23.1684464369686,-68.8217913197752,
12.));
#127566=CARTESIAN_POINT('Ctrl Pts',(23.1696135978997,-68.7967096902996,
0.));
#127567=CARTESIAN_POINT('Ctrl Pts',(23.1696135978997,-68.7967096902996,
12.));
#127568=CARTESIAN_POINT('Ctrl Pts',(23.170755021036,-68.771666891425,0.));
#127569=CARTESIAN_POINT('Ctrl Pts',(23.170755021036,-68.771666891425,12.));
#127570=CARTESIAN_POINT('Ctrl Pts',(23.1718707572043,-68.746663033096,0.));
#127571=CARTESIAN_POINT('Ctrl Pts',(23.1718707572043,-68.746663033096,12.));
#127572=CARTESIAN_POINT('Ctrl Pts',(23.1729608575109,-68.7216982256341,
0.));
#127573=CARTESIAN_POINT('Ctrl Pts',(23.1729608575109,-68.7216982256341,
12.));
#127574=CARTESIAN_POINT('Ctrl Pts',(23.1740253733417,-68.696772579744,0.));
#127575=CARTESIAN_POINT('Ctrl Pts',(23.1740253733417,-68.696772579744,12.));
#127576=CARTESIAN_POINT('Ctrl Pts',(23.1750643563601,-68.6718862065216,
0.));
#127577=CARTESIAN_POINT('Ctrl Pts',(23.1750643563601,-68.6718862065216,
12.));
#127578=CARTESIAN_POINT('Ctrl Pts',(23.1760778585092,-68.6470392174564,
0.));
#127579=CARTESIAN_POINT('Ctrl Pts',(23.1760778585092,-68.6470392174564,
12.));
#127580=CARTESIAN_POINT('Ctrl Pts',(23.1770659320137,-68.6222317244342,
0.));
#127581=CARTESIAN_POINT('Ctrl Pts',(23.1770659320137,-68.6222317244342,
12.));
#127582=CARTESIAN_POINT('Ctrl Pts',(23.1780286293875,-68.597463839733,0.));
#127583=CARTESIAN_POINT('Ctrl Pts',(23.1780286293875,-68.597463839733,12.));
#127584=CARTESIAN_POINT('Ctrl Pts',(23.1789660034341,-68.5727356760278,
0.));
#127585=CARTESIAN_POINT('Ctrl Pts',(23.1789660034341,-68.5727356760278,
12.));
#127586=CARTESIAN_POINT('Ctrl Pts',(23.1798781072449,-68.5480473463985,
0.));
#127587=CARTESIAN_POINT('Ctrl Pts',(23.1798781072449,-68.5480473463985,
12.));
#127588=CARTESIAN_POINT('Ctrl Pts',(23.180764994201,-68.5233989643345,0.));
#127589=CARTESIAN_POINT('Ctrl Pts',(23.180764994201,-68.5233989643345,12.));
#127590=CARTESIAN_POINT('Ctrl Pts',(23.1816267179751,-68.4987906437356,
0.));
#127591=CARTESIAN_POINT('Ctrl Pts',(23.1816267179751,-68.4987906437356,
12.));
#127592=CARTESIAN_POINT('Ctrl Pts',(23.1824633325384,-68.4742224989099,
0.));
#127593=CARTESIAN_POINT('Ctrl Pts',(23.1824633325384,-68.4742224989099,
12.));
#127594=CARTESIAN_POINT('Ctrl Pts',(23.183274892163,-68.4496946445758,0.));
#127595=CARTESIAN_POINT('Ctrl Pts',(23.183274892163,-68.4496946445758,12.));
#127596=CARTESIAN_POINT('Ctrl Pts',(23.1840614514192,-68.4252071958729,
0.));
#127597=CARTESIAN_POINT('Ctrl Pts',(23.1840614514192,-68.4252071958729,
12.));
#127598=CARTESIAN_POINT('Ctrl Pts',(23.1848230651776,-68.4007602683652,
0.));
#127599=CARTESIAN_POINT('Ctrl Pts',(23.1848230651776,-68.4007602683652,
12.));
#127600=CARTESIAN_POINT('Ctrl Pts',(23.1855597886115,-68.376353978044,0.));
#127601=CARTESIAN_POINT('Ctrl Pts',(23.1855597886115,-68.376353978044,12.));
#127602=CARTESIAN_POINT('Ctrl Pts',(23.186271677203,-68.3519884413246,0.));
#127603=CARTESIAN_POINT('Ctrl Pts',(23.186271677203,-68.3519884413246,12.));
#127604=CARTESIAN_POINT('Ctrl Pts',(23.1869587867459,-68.3276637750485,
0.));
#127605=CARTESIAN_POINT('Ctrl Pts',(23.1869587867459,-68.3276637750485,
12.));
#127606=CARTESIAN_POINT('Ctrl Pts',(23.1876211733435,-68.3033800964939,
0.));
#127607=CARTESIAN_POINT('Ctrl Pts',(23.1876211733435,-68.3033800964939,
12.));
#127608=CARTESIAN_POINT('Ctrl Pts',(23.1882588934106,-68.2791375233795,
0.));
#127609=CARTESIAN_POINT('Ctrl Pts',(23.1882588934106,-68.2791375233795,
12.));
#127610=CARTESIAN_POINT('Ctrl Pts',(23.1888720036757,-68.2549361738681,
0.));
#127611=CARTESIAN_POINT('Ctrl Pts',(23.1888720036757,-68.2549361738681,
12.));
#127612=CARTESIAN_POINT('Ctrl Pts',(23.1894605611871,-68.2307761665633,
0.));
#127613=CARTESIAN_POINT('Ctrl Pts',(23.1894605611871,-68.2307761665633,
12.));
#127614=CARTESIAN_POINT('Ctrl Pts',(23.1900246233165,-68.2066576205116,
0.));
#127615=CARTESIAN_POINT('Ctrl Pts',(23.1900246233165,-68.2066576205116,
12.));
#127616=CARTESIAN_POINT('Ctrl Pts',(23.1905642477571,-68.1825806552129,
0.));
#127617=CARTESIAN_POINT('Ctrl Pts',(23.1905642477571,-68.1825806552129,
12.));
#127618=CARTESIAN_POINT('Ctrl Pts',(23.1910794925251,-68.1585453906257,
0.));
#127619=CARTESIAN_POINT('Ctrl Pts',(23.1910794925251,-68.1585453906257,
12.));
#127620=CARTESIAN_POINT('Ctrl Pts',(23.1915704159623,-68.1345519471695,
0.));
#127621=CARTESIAN_POINT('Ctrl Pts',(23.1915704159623,-68.1345519471695,
12.));
#127622=CARTESIAN_POINT('Ctrl Pts',(23.1920370767425,-68.110600445723,0.));
#127623=CARTESIAN_POINT('Ctrl Pts',(23.1920370767425,-68.110600445723,12.));
#127624=CARTESIAN_POINT('Ctrl Pts',(23.1924795338749,-68.0866910076251,
0.));
#127625=CARTESIAN_POINT('Ctrl Pts',(23.1924795338749,-68.0866910076251,
12.));
#127626=CARTESIAN_POINT('Ctrl Pts',(23.192897846702,-68.0628237546863,0.));
#127627=CARTESIAN_POINT('Ctrl Pts',(23.192897846702,-68.0628237546863,12.));
#127628=CARTESIAN_POINT('Ctrl Pts',(23.1932920749023,-68.0389988091933,
0.));
#127629=CARTESIAN_POINT('Ctrl Pts',(23.1932920749023,-68.0389988091933,
12.));
#127630=CARTESIAN_POINT('Ctrl Pts',(23.1936622784918,-68.0152162939121,
0.));
#127631=CARTESIAN_POINT('Ctrl Pts',(23.1936622784918,-68.0152162939121,
12.));
#127632=CARTESIAN_POINT('Ctrl Pts',(23.1940085178313,-67.991476332086,0.));
#127633=CARTESIAN_POINT('Ctrl Pts',(23.1940085178313,-67.991476332086,12.));
#127634=CARTESIAN_POINT('Ctrl Pts',(23.1943308536297,-67.9677790474385,
0.));
#127635=CARTESIAN_POINT('Ctrl Pts',(23.1943308536297,-67.9677790474385,
12.));
#127636=CARTESIAN_POINT('Ctrl Pts',(23.1946293469427,-67.9441245641842,
0.));
#127637=CARTESIAN_POINT('Ctrl Pts',(23.1946293469427,-67.9441245641842,
12.));
#127638=CARTESIAN_POINT('Ctrl Pts',(23.1949040591744,-67.9205130070324,
0.));
#127639=CARTESIAN_POINT('Ctrl Pts',(23.1949040591744,-67.9205130070324,
12.));
#127640=CARTESIAN_POINT('Ctrl Pts',(23.1951550520802,-67.8969445011916,
0.));
#127641=CARTESIAN_POINT('Ctrl Pts',(23.1951550520802,-67.8969445011916,
12.));
#127642=CARTESIAN_POINT('Ctrl Pts',(23.1953823877734,-67.8734191723667,
0.));
#127643=CARTESIAN_POINT('Ctrl Pts',(23.1953823877734,-67.8734191723667,
12.));
#127644=CARTESIAN_POINT('Ctrl Pts',(23.1955861287286,-67.8499371467616,
0.));
#127645=CARTESIAN_POINT('Ctrl Pts',(23.1955861287286,-67.8499371467616,
12.));
#127646=CARTESIAN_POINT('Ctrl Pts',(23.1957663377806,-67.8264985510917,
0.));
#127647=CARTESIAN_POINT('Ctrl Pts',(23.1957663377806,-67.8264985510917,
12.));
#127648=CARTESIAN_POINT('Ctrl Pts',(23.1959230781269,-67.8031035125887,
0.));
#127649=CARTESIAN_POINT('Ctrl Pts',(23.1959230781269,-67.8031035125887,
12.));
#127650=CARTESIAN_POINT('Ctrl Pts',(23.1960564133304,-67.7797521590045,
0.));
#127651=CARTESIAN_POINT('Ctrl Pts',(23.1960564133304,-67.7797521590045,
12.));
#127652=CARTESIAN_POINT('Ctrl Pts',(23.1961664073261,-67.7564446186079,
0.));
#127653=CARTESIAN_POINT('Ctrl Pts',(23.1961664073261,-67.7564446186079,
12.));
#127654=CARTESIAN_POINT('Ctrl Pts',(23.1962531244245,-67.7331810201883,
0.));
#127655=CARTESIAN_POINT('Ctrl Pts',(23.1962531244245,-67.7331810201883,
12.));
#127656=CARTESIAN_POINT('Ctrl Pts',(23.1963166293102,-67.7099614930671,
0.));
#127657=CARTESIAN_POINT('Ctrl Pts',(23.1963166293102,-67.7099614930671,
12.));
#127658=CARTESIAN_POINT('Ctrl Pts',(23.1963569870451,-67.6867861671031,
0.));
#127659=CARTESIAN_POINT('Ctrl Pts',(23.1963569870451,-67.6867861671031,
12.));
#127660=CARTESIAN_POINT('Ctrl Pts',(23.1963742630714,-67.6636551726964,
0.));
#127661=CARTESIAN_POINT('Ctrl Pts',(23.1963742630714,-67.6636551726964,
12.));
#127662=CARTESIAN_POINT('Ctrl Pts',(23.1963685232187,-67.6405686407863,
0.));
#127663=CARTESIAN_POINT('Ctrl Pts',(23.1963685232187,-67.6405686407863,
12.));
#127664=CARTESIAN_POINT('Ctrl Pts',(23.1963398337068,-67.6175267028555,
0.));
#127665=CARTESIAN_POINT('Ctrl Pts',(23.1963398337068,-67.6175267028555,
12.));
#127666=CARTESIAN_POINT('Ctrl Pts',(23.1962882611452,-67.5945294909426,
0.));
#127667=CARTESIAN_POINT('Ctrl Pts',(23.1962882611452,-67.5945294909426,
12.));
#127668=CARTESIAN_POINT('Ctrl Pts',(23.196213872536,-67.5715771376461,0.));
#127669=CARTESIAN_POINT('Ctrl Pts',(23.196213872536,-67.5715771376461,12.));
#127670=CARTESIAN_POINT('Ctrl Pts',(23.1961167352771,-67.5486697761288,
0.));
#127671=CARTESIAN_POINT('Ctrl Pts',(23.1961167352771,-67.5486697761288,
12.));
#127672=CARTESIAN_POINT('Ctrl Pts',(23.19599691717,-67.5258075401146,0.));
#127673=CARTESIAN_POINT('Ctrl Pts',(23.19599691717,-67.5258075401146,12.));
#127674=CARTESIAN_POINT('Ctrl Pts',(23.1958544864215,-67.502990563895,0.));
#127675=CARTESIAN_POINT('Ctrl Pts',(23.1958544864215,-67.502990563895,12.));
#127676=CARTESIAN_POINT('Ctrl Pts',(23.195689511644,-67.4802189823408,0.));
#127677=CARTESIAN_POINT('Ctrl Pts',(23.195689511644,-67.4802189823408,12.));
#127678=CARTESIAN_POINT('Ctrl Pts',(23.1955020618589,-67.4574929309076,
0.));
#127679=CARTESIAN_POINT('Ctrl Pts',(23.1955020618589,-67.4574929309076,
12.));
#127680=CARTESIAN_POINT('Ctrl Pts',(23.1952922065012,-67.4348125456398,
0.));
#127681=CARTESIAN_POINT('Ctrl Pts',(23.1952922065012,-67.4348125456398,
12.));
#127682=CARTESIAN_POINT('Ctrl Pts',(23.1950600154265,-67.412177963168,0.));
#127683=CARTESIAN_POINT('Ctrl Pts',(23.1950600154265,-67.412177963168,12.));
#127684=CARTESIAN_POINT('Ctrl Pts',(23.1948055589128,-67.3895893207182,
0.));
#127685=CARTESIAN_POINT('Ctrl Pts',(23.1948055589128,-67.3895893207182,
12.));
#127686=CARTESIAN_POINT('Ctrl Pts',(23.194528907661,-67.3670467561212,0.));
#127687=CARTESIAN_POINT('Ctrl Pts',(23.194528907661,-67.3670467561212,12.));
#127688=CARTESIAN_POINT('Ctrl Pts',(23.1942301327978,-67.3445504078176,
0.));
#127689=CARTESIAN_POINT('Ctrl Pts',(23.1942301327978,-67.3445504078176,
12.));
#127690=CARTESIAN_POINT('Ctrl Pts',(23.1939093058801,-67.3221004148604,
0.));
#127691=CARTESIAN_POINT('Ctrl Pts',(23.1939093058801,-67.3221004148604,
12.));
#127692=CARTESIAN_POINT('Ctrl Pts',(23.1935664989018,-67.2996969169098,
0.));
#127693=CARTESIAN_POINT('Ctrl Pts',(23.1935664989018,-67.2996969169098,
12.));
#127694=CARTESIAN_POINT('Ctrl Pts',(23.1932017842952,-67.2773400542477,
0.));
#127695=CARTESIAN_POINT('Ctrl Pts',(23.1932017842952,-67.2773400542477,
12.));
#127696=CARTESIAN_POINT('Ctrl Pts',(23.1928152349342,-67.2550299677888,
0.));
#127697=CARTESIAN_POINT('Ctrl Pts',(23.1928152349342,-67.2550299677888,
12.));
#127698=CARTESIAN_POINT('Ctrl Pts',(23.1924069241385,-67.232766799088,0.));
#127699=CARTESIAN_POINT('Ctrl Pts',(23.1924069241385,-67.232766799088,12.));
#127700=CARTESIAN_POINT('Ctrl Pts',(23.1919769256803,-67.2105506903447,
0.));
#127701=CARTESIAN_POINT('Ctrl Pts',(23.1919769256803,-67.2105506903447,
12.));
#127702=CARTESIAN_POINT('Ctrl Pts',(23.1915253137923,-67.1883817844038,
0.));
#127703=CARTESIAN_POINT('Ctrl Pts',(23.1915253137923,-67.1883817844038,
12.));
#127704=CARTESIAN_POINT('Ctrl Pts',(23.1910521631657,-67.1662602247639,
0.));
#127705=CARTESIAN_POINT('Ctrl Pts',(23.1910521631657,-67.1662602247639,
12.));
#127706=CARTESIAN_POINT('Ctrl Pts',(23.1905575489504,-67.1441861555817,
0.));
#127707=CARTESIAN_POINT('Ctrl Pts',(23.1905575489504,-67.1441861555817,
12.));
#127708=CARTESIAN_POINT('Ctrl Pts',(23.1900415467574,-67.1221597216741,
0.));
#127709=CARTESIAN_POINT('Ctrl Pts',(23.1900415467574,-67.1221597216741,
12.));
#127710=CARTESIAN_POINT('Ctrl Pts',(23.1895042326626,-67.1001810685143,
0.));
#127711=CARTESIAN_POINT('Ctrl Pts',(23.1895042326626,-67.1001810685143,
12.));
#127712=CARTESIAN_POINT('Ctrl Pts',(23.1889456832119,-67.0782503422305,
0.));
#127713=CARTESIAN_POINT('Ctrl Pts',(23.1889456832119,-67.0782503422305,
12.));
#127714=CARTESIAN_POINT('Ctrl Pts',(23.1883659754271,-67.0563676896325,
0.));
#127715=CARTESIAN_POINT('Ctrl Pts',(23.1883659754271,-67.0563676896325,
12.));
#127716=CARTESIAN_POINT('Ctrl Pts',(23.1877651868157,-67.0345332582306,
0.));
#127717=CARTESIAN_POINT('Ctrl Pts',(23.1877651868157,-67.0345332582306,
12.));
#127718=CARTESIAN_POINT('Ctrl Pts',(23.1871433953793,-67.0127471962501,
0.));
#127719=CARTESIAN_POINT('Ctrl Pts',(23.1871433953793,-67.0127471962501,
12.));
#127720=CARTESIAN_POINT('Ctrl Pts',(23.1865006796283,-66.9910096526462,
0.));
#127721=CARTESIAN_POINT('Ctrl Pts',(23.1865006796283,-66.9910096526462,
12.));
#127722=CARTESIAN_POINT('Ctrl Pts',(23.1858371185842,-66.9693207771031,
0.));
#127723=CARTESIAN_POINT('Ctrl Pts',(23.1858371185842,-66.9693207771031,
12.));
#127724=CARTESIAN_POINT('Ctrl Pts',(23.1851527917657,-66.9476807200203,
0.));
#127725=CARTESIAN_POINT('Ctrl Pts',(23.1851527917657,-66.9476807200203,
12.));
#127726=CARTESIAN_POINT('Ctrl Pts',(23.1844477791814,-66.9260896324949,
0.));
#127727=CARTESIAN_POINT('Ctrl Pts',(23.1844477791814,-66.9260896324949,
12.));
#127728=CARTESIAN_POINT('Ctrl Pts',(23.1837221613235,-66.9045476663063,
0.));
#127729=CARTESIAN_POINT('Ctrl Pts',(23.1837221613235,-66.9045476663063,
12.));
#127730=CARTESIAN_POINT('Ctrl Pts',(23.1829760191591,-66.8830549738795,
0.));
#127731=CARTESIAN_POINT('Ctrl Pts',(23.1829760191591,-66.8830549738795,
12.));
#127732=CARTESIAN_POINT('Ctrl Pts',(23.1822094341517,-66.8616117083331,
0.));
#127733=CARTESIAN_POINT('Ctrl Pts',(23.1822094341517,-66.8616117083331,
12.));
#127734=CARTESIAN_POINT('Ctrl Pts',(23.1814224882953,-66.8402180235566,
0.));
#127735=CARTESIAN_POINT('Ctrl Pts',(23.1814224882953,-66.8402180235566,
12.));
#127736=CARTESIAN_POINT('Ctrl Pts',(23.1806152641475,-66.8188740742727,
0.));
#127737=CARTESIAN_POINT('Ctrl Pts',(23.1806152641475,-66.8188740742727,
12.));
#127738=CARTESIAN_POINT('Ctrl Pts',(23.1797878448639,-66.7975800161,0.));
#127739=CARTESIAN_POINT('Ctrl Pts',(23.1797878448639,-66.7975800161,12.));
#127740=CARTESIAN_POINT('Ctrl Pts',(23.1789403142366,-66.7763360056121,
0.));
#127741=CARTESIAN_POINT('Ctrl Pts',(23.1789403142366,-66.7763360056121,
12.));
#127742=CARTESIAN_POINT('Ctrl Pts',(23.17807275663,-66.7551422002204,0.));
#127743=CARTESIAN_POINT('Ctrl Pts',(23.17807275663,-66.7551422002204,12.));
#127744=CARTESIAN_POINT('Ctrl Pts',(23.1771852569131,-66.7339987580427,
0.));
#127745=CARTESIAN_POINT('Ctrl Pts',(23.1771852569131,-66.7339987580427,
12.));
#127746=CARTESIAN_POINT('Ctrl Pts',(23.1762779004044,-66.7129058377896,
0.));
#127747=CARTESIAN_POINT('Ctrl Pts',(23.1762779004044,-66.7129058377896,
12.));
#127748=CARTESIAN_POINT('Ctrl Pts',(23.1753507727939,-66.6918635985972,
0.));
#127749=CARTESIAN_POINT('Ctrl Pts',(23.1753507727939,-66.6918635985972,
12.));
#127750=CARTESIAN_POINT('Ctrl Pts',(23.1744039601381,-66.6708722000079,
0.));
#127751=CARTESIAN_POINT('Ctrl Pts',(23.1744039601381,-66.6708722000079,
12.));
#127752=CARTESIAN_POINT('Ctrl Pts',(23.1734375490431,-66.6499318023473,
0.));
#127753=CARTESIAN_POINT('Ctrl Pts',(23.1734375490431,-66.6499318023473,
12.));
#127754=CARTESIAN_POINT('Ctrl Pts',(23.1724516268302,-66.6290425670549,
0.));
#127755=CARTESIAN_POINT('Ctrl Pts',(23.1724516268302,-66.6290425670549,
12.));
#127756=CARTESIAN_POINT('Ctrl Pts',(23.1714462816789,-66.6082046569644,
0.));
#127757=CARTESIAN_POINT('Ctrl Pts',(23.1714462816789,-66.6082046569644,
12.));
#127758=CARTESIAN_POINT('Ctrl Pts',(23.1704216028614,-66.5874182367563,
0.));
#127759=CARTESIAN_POINT('Ctrl Pts',(23.1704216028614,-66.5874182367563,
12.));
#127760=CARTESIAN_POINT('Ctrl Pts',(23.1693776805865,-66.5666834726454,
0.));
#127761=CARTESIAN_POINT('Ctrl Pts',(23.1693776805865,-66.5666834726454,
12.));
#127762=CARTESIAN_POINT('Ctrl Pts',(23.1683146055726,-66.5460005315376,
0.));
#127763=CARTESIAN_POINT('Ctrl Pts',(23.1683146055726,-66.5460005315376,
12.));
#127764=CARTESIAN_POINT('Ctrl Pts',(23.1672324686926,-66.5253695803206,
0.));
#127765=CARTESIAN_POINT('Ctrl Pts',(23.1672324686926,-66.5253695803206,
12.));
#127766=CARTESIAN_POINT('Ctrl Pts',(23.1661313606132,-66.5047907851348,
0.));
#127767=CARTESIAN_POINT('Ctrl Pts',(23.1661313606132,-66.5047907851348,
12.));
#127768=CARTESIAN_POINT('Ctrl Pts',(23.1650113713808,-66.4842643105311,
0.));
#127769=CARTESIAN_POINT('Ctrl Pts',(23.1650113713808,-66.4842643105311,
12.));
#127770=CARTESIAN_POINT('Ctrl Pts',(23.1638725912195,-66.4637903210727,
0.));
#127771=CARTESIAN_POINT('Ctrl Pts',(23.1638725912195,-66.4637903210727,
12.));
#127772=CARTESIAN_POINT('Ctrl Pts',(23.1627151114883,-66.4433689832478,
0.));
#127773=CARTESIAN_POINT('Ctrl Pts',(23.1627151114883,-66.4433689832478,
12.));
#127774=CARTESIAN_POINT('Ctrl Pts',(23.1615390254631,-66.4230004670278,
0.));
#127775=CARTESIAN_POINT('Ctrl Pts',(23.1615390254631,-66.4230004670278,
12.));
#127776=CARTESIAN_POINT('Ctrl Pts',(23.160344429474,-66.4026849481232,0.));
#127777=CARTESIAN_POINT('Ctrl Pts',(23.160344429474,-66.4026849481232,12.));
#127778=CARTESIAN_POINT('Ctrl Pts',(23.1591314230083,-66.3824226081802,
0.));
#127779=CARTESIAN_POINT('Ctrl Pts',(23.1591314230083,-66.3824226081802,
12.));
#127780=CARTESIAN_POINT('Ctrl Pts',(23.1579001063423,-66.3622136300654,
0.));
#127781=CARTESIAN_POINT('Ctrl Pts',(23.1579001063423,-66.3622136300654,
12.));
#127782=CARTESIAN_POINT('Ctrl Pts',(23.1566505784621,-66.3420581937147,
0.));
#127783=CARTESIAN_POINT('Ctrl Pts',(23.1566505784621,-66.3420581937147,
12.));
#127784=CARTESIAN_POINT('Ctrl Pts',(23.1553829352539,-66.3219564725184,
0.));
#127785=CARTESIAN_POINT('Ctrl Pts',(23.1553829352539,-66.3219564725184,
12.));
#127786=CARTESIAN_POINT('Ctrl Pts',(23.154097266619,-66.3019086275445,0.));
#127787=CARTESIAN_POINT('Ctrl Pts',(23.154097266619,-66.3019086275445,12.));
#127788=CARTESIAN_POINT('Ctrl Pts',(23.1527936592651,-66.281914813114,0.));
#127789=CARTESIAN_POINT('Ctrl Pts',(23.1527936592651,-66.281914813114,12.));
#127790=CARTESIAN_POINT('Ctrl Pts',(23.1514722022503,-66.2619751878793,
0.));
#127791=CARTESIAN_POINT('Ctrl Pts',(23.1514722022503,-66.2619751878793,
12.));
#127792=CARTESIAN_POINT('Ctrl Pts',(23.1501329914487,-66.2420899237318,
0.));
#127793=CARTESIAN_POINT('Ctrl Pts',(23.1501329914487,-66.2420899237318,
12.));
#127794=CARTESIAN_POINT('Ctrl Pts',(23.1487761349297,-66.2222592165398,
0.));
#127795=CARTESIAN_POINT('Ctrl Pts',(23.1487761349297,-66.2222592165398,
12.));
#127796=CARTESIAN_POINT('Ctrl Pts',(23.147401756643,-66.2024832934733,0.));
#127797=CARTESIAN_POINT('Ctrl Pts',(23.147401756643,-66.2024832934733,12.));
#127798=CARTESIAN_POINT('Ctrl Pts',(23.1460099850704,-66.1827623902755,
0.));
#127799=CARTESIAN_POINT('Ctrl Pts',(23.1460099850704,-66.1827623902755,
12.));
#127800=CARTESIAN_POINT('Ctrl Pts',(23.1446009424871,-66.163096729667,0.));
#127801=CARTESIAN_POINT('Ctrl Pts',(23.1446009424871,-66.163096729667,12.));
#127802=CARTESIAN_POINT('Ctrl Pts',(23.1431747350127,-66.14348650151,0.));
#127803=CARTESIAN_POINT('Ctrl Pts',(23.1431747350127,-66.14348650151,12.));
#127804=CARTESIAN_POINT('Ctrl Pts',(23.1417314398501,-66.1239318368803,
0.));
#127805=CARTESIAN_POINT('Ctrl Pts',(23.1417314398501,-66.1239318368803,
12.));
#127806=CARTESIAN_POINT('Ctrl Pts',(23.140271103958,-66.1044328067739,0.));
#127807=CARTESIAN_POINT('Ctrl Pts',(23.140271103958,-66.1044328067739,12.));
#127808=CARTESIAN_POINT('Ctrl Pts',(23.1390892229923,-66.0888781152779,
0.));
#127809=CARTESIAN_POINT('Ctrl Pts',(23.1390892229923,-66.0888781152779,
12.));
#127810=CARTESIAN_POINT('Ctrl Pts',(23.1381951597491,-66.0772371487475,
0.));
#127811=CARTESIAN_POINT('Ctrl Pts',(23.1381951597491,-66.0772371487475,
12.));
#127812=CARTESIAN_POINT('Ctrl Pts',(23.1375957166138,-66.0694876382212,
0.));
#127813=CARTESIAN_POINT('Ctrl Pts',(23.1375957166138,-66.0694876382212,
12.));
#127814=CARTESIAN_POINT('Ctrl Pts',(23.1372951448023,-66.0656156664139,
0.));
#127815=CARTESIAN_POINT('Ctrl Pts',(23.1372951448023,-66.0656156664139,
12.));
#127816=CARTESIAN_POINT('',(23.1372951448023,-66.0656156664139,12.));
#127817=CARTESIAN_POINT('Ctrl Pts',(23.1372951448023,-66.0656156664139,
12.));
#127818=CARTESIAN_POINT('Ctrl Pts',(23.1375957166138,-66.0694876382212,
12.));
#127819=CARTESIAN_POINT('Ctrl Pts',(23.1381951597491,-66.0772371487475,
12.));
#127820=CARTESIAN_POINT('Ctrl Pts',(23.1390892229923,-66.0888781152779,
12.));
#127821=CARTESIAN_POINT('Ctrl Pts',(23.140271103958,-66.1044328067739,12.));
#127822=CARTESIAN_POINT('Ctrl Pts',(23.1417314398501,-66.1239318368803,
12.));
#127823=CARTESIAN_POINT('Ctrl Pts',(23.1431747350127,-66.14348650151,12.));
#127824=CARTESIAN_POINT('Ctrl Pts',(23.1446009424871,-66.163096729667,12.));
#127825=CARTESIAN_POINT('Ctrl Pts',(23.1460099850704,-66.1827623902755,
12.));
#127826=CARTESIAN_POINT('Ctrl Pts',(23.147401756643,-66.2024832934733,12.));
#127827=CARTESIAN_POINT('Ctrl Pts',(23.1487761349297,-66.2222592165398,
12.));
#127828=CARTESIAN_POINT('Ctrl Pts',(23.1501329914487,-66.2420899237318,
12.));
#127829=CARTESIAN_POINT('Ctrl Pts',(23.1514722022503,-66.2619751878793,
12.));
#127830=CARTESIAN_POINT('Ctrl Pts',(23.1527936592651,-66.281914813114,12.));
#127831=CARTESIAN_POINT('Ctrl Pts',(23.154097266619,-66.3019086275445,12.));
#127832=CARTESIAN_POINT('Ctrl Pts',(23.1553829352539,-66.3219564725184,
12.));
#127833=CARTESIAN_POINT('Ctrl Pts',(23.1566505784621,-66.3420581937147,
12.));
#127834=CARTESIAN_POINT('Ctrl Pts',(23.1579001063423,-66.3622136300654,
12.));
#127835=CARTESIAN_POINT('Ctrl Pts',(23.1591314230083,-66.3824226081802,
12.));
#127836=CARTESIAN_POINT('Ctrl Pts',(23.160344429474,-66.4026849481232,12.));
#127837=CARTESIAN_POINT('Ctrl Pts',(23.1615390254631,-66.4230004670278,
12.));
#127838=CARTESIAN_POINT('Ctrl Pts',(23.1627151114883,-66.4433689832478,
12.));
#127839=CARTESIAN_POINT('Ctrl Pts',(23.1638725912195,-66.4637903210727,
12.));
#127840=CARTESIAN_POINT('Ctrl Pts',(23.1650113713808,-66.4842643105311,
12.));
#127841=CARTESIAN_POINT('Ctrl Pts',(23.1661313606132,-66.5047907851348,
12.));
#127842=CARTESIAN_POINT('Ctrl Pts',(23.1672324686926,-66.5253695803206,
12.));
#127843=CARTESIAN_POINT('Ctrl Pts',(23.1683146055726,-66.5460005315376,
12.));
#127844=CARTESIAN_POINT('Ctrl Pts',(23.1693776805865,-66.5666834726454,
12.));
#127845=CARTESIAN_POINT('Ctrl Pts',(23.1704216028614,-66.5874182367563,
12.));
#127846=CARTESIAN_POINT('Ctrl Pts',(23.1714462816789,-66.6082046569644,
12.));
#127847=CARTESIAN_POINT('Ctrl Pts',(23.1724516268302,-66.6290425670549,
12.));
#127848=CARTESIAN_POINT('Ctrl Pts',(23.1734375490431,-66.6499318023473,
12.));
#127849=CARTESIAN_POINT('Ctrl Pts',(23.1744039601381,-66.6708722000079,
12.));
#127850=CARTESIAN_POINT('Ctrl Pts',(23.1753507727939,-66.6918635985972,
12.));
#127851=CARTESIAN_POINT('Ctrl Pts',(23.1762779004044,-66.7129058377896,
12.));
#127852=CARTESIAN_POINT('Ctrl Pts',(23.1771852569131,-66.7339987580427,
12.));
#127853=CARTESIAN_POINT('Ctrl Pts',(23.17807275663,-66.7551422002204,12.));
#127854=CARTESIAN_POINT('Ctrl Pts',(23.1789403142366,-66.7763360056121,
12.));
#127855=CARTESIAN_POINT('Ctrl Pts',(23.1797878448639,-66.7975800161,12.));
#127856=CARTESIAN_POINT('Ctrl Pts',(23.1806152641475,-66.8188740742727,
12.));
#127857=CARTESIAN_POINT('Ctrl Pts',(23.1814224882953,-66.8402180235566,
12.));
#127858=CARTESIAN_POINT('Ctrl Pts',(23.1822094341517,-66.8616117083331,
12.));
#127859=CARTESIAN_POINT('Ctrl Pts',(23.1829760191591,-66.8830549738795,
12.));
#127860=CARTESIAN_POINT('Ctrl Pts',(23.1837221613235,-66.9045476663063,
12.));
#127861=CARTESIAN_POINT('Ctrl Pts',(23.1844477791814,-66.9260896324949,
12.));
#127862=CARTESIAN_POINT('Ctrl Pts',(23.1851527917657,-66.9476807200203,
12.));
#127863=CARTESIAN_POINT('Ctrl Pts',(23.1858371185842,-66.9693207771031,
12.));
#127864=CARTESIAN_POINT('Ctrl Pts',(23.1865006796283,-66.9910096526462,
12.));
#127865=CARTESIAN_POINT('Ctrl Pts',(23.1871433953793,-67.0127471962501,
12.));
#127866=CARTESIAN_POINT('Ctrl Pts',(23.1877651868157,-67.0345332582306,
12.));
#127867=CARTESIAN_POINT('Ctrl Pts',(23.1883659754271,-67.0563676896325,
12.));
#127868=CARTESIAN_POINT('Ctrl Pts',(23.1889456832119,-67.0782503422305,
12.));
#127869=CARTESIAN_POINT('Ctrl Pts',(23.1895042326626,-67.1001810685143,
12.));
#127870=CARTESIAN_POINT('Ctrl Pts',(23.1900415467574,-67.1221597216741,
12.));
#127871=CARTESIAN_POINT('Ctrl Pts',(23.1905575489504,-67.1441861555817,
12.));
#127872=CARTESIAN_POINT('Ctrl Pts',(23.1910521631657,-67.1662602247639,
12.));
#127873=CARTESIAN_POINT('Ctrl Pts',(23.1915253137923,-67.1883817844038,
12.));
#127874=CARTESIAN_POINT('Ctrl Pts',(23.1919769256803,-67.2105506903447,
12.));
#127875=CARTESIAN_POINT('Ctrl Pts',(23.1924069241385,-67.232766799088,12.));
#127876=CARTESIAN_POINT('Ctrl Pts',(23.1928152349342,-67.2550299677888,
12.));
#127877=CARTESIAN_POINT('Ctrl Pts',(23.1932017842952,-67.2773400542477,
12.));
#127878=CARTESIAN_POINT('Ctrl Pts',(23.1935664989018,-67.2996969169098,
12.));
#127879=CARTESIAN_POINT('Ctrl Pts',(23.1939093058801,-67.3221004148604,
12.));
#127880=CARTESIAN_POINT('Ctrl Pts',(23.1942301327978,-67.3445504078176,
12.));
#127881=CARTESIAN_POINT('Ctrl Pts',(23.194528907661,-67.3670467561212,12.));
#127882=CARTESIAN_POINT('Ctrl Pts',(23.1948055589128,-67.3895893207182,
12.));
#127883=CARTESIAN_POINT('Ctrl Pts',(23.1950600154265,-67.412177963168,12.));
#127884=CARTESIAN_POINT('Ctrl Pts',(23.1952922065012,-67.4348125456398,
12.));
#127885=CARTESIAN_POINT('Ctrl Pts',(23.1955020618589,-67.4574929309076,
12.));
#127886=CARTESIAN_POINT('Ctrl Pts',(23.195689511644,-67.4802189823408,12.));
#127887=CARTESIAN_POINT('Ctrl Pts',(23.1958544864215,-67.502990563895,12.));
#127888=CARTESIAN_POINT('Ctrl Pts',(23.19599691717,-67.5258075401146,12.));
#127889=CARTESIAN_POINT('Ctrl Pts',(23.1961167352771,-67.5486697761288,
12.));
#127890=CARTESIAN_POINT('Ctrl Pts',(23.196213872536,-67.5715771376461,12.));
#127891=CARTESIAN_POINT('Ctrl Pts',(23.1962882611452,-67.5945294909426,
12.));
#127892=CARTESIAN_POINT('Ctrl Pts',(23.1963398337068,-67.6175267028555,
12.));
#127893=CARTESIAN_POINT('Ctrl Pts',(23.1963685232187,-67.6405686407863,
12.));
#127894=CARTESIAN_POINT('Ctrl Pts',(23.1963742630714,-67.6636551726964,
12.));
#127895=CARTESIAN_POINT('Ctrl Pts',(23.1963569870451,-67.6867861671031,
12.));
#127896=CARTESIAN_POINT('Ctrl Pts',(23.1963166293102,-67.7099614930671,
12.));
#127897=CARTESIAN_POINT('Ctrl Pts',(23.1962531244245,-67.7331810201883,
12.));
#127898=CARTESIAN_POINT('Ctrl Pts',(23.1961664073261,-67.7564446186079,
12.));
#127899=CARTESIAN_POINT('Ctrl Pts',(23.1960564133304,-67.7797521590045,
12.));
#127900=CARTESIAN_POINT('Ctrl Pts',(23.1959230781269,-67.8031035125887,
12.));
#127901=CARTESIAN_POINT('Ctrl Pts',(23.1957663377806,-67.8264985510917,
12.));
#127902=CARTESIAN_POINT('Ctrl Pts',(23.1955861287286,-67.8499371467616,
12.));
#127903=CARTESIAN_POINT('Ctrl Pts',(23.1953823877734,-67.8734191723667,
12.));
#127904=CARTESIAN_POINT('Ctrl Pts',(23.1951550520802,-67.8969445011916,
12.));
#127905=CARTESIAN_POINT('Ctrl Pts',(23.1949040591744,-67.9205130070324,
12.));
#127906=CARTESIAN_POINT('Ctrl Pts',(23.1946293469427,-67.9441245641842,
12.));
#127907=CARTESIAN_POINT('Ctrl Pts',(23.1943308536297,-67.9677790474385,
12.));
#127908=CARTESIAN_POINT('Ctrl Pts',(23.1940085178313,-67.991476332086,12.));
#127909=CARTESIAN_POINT('Ctrl Pts',(23.1936622784918,-68.0152162939121,
12.));
#127910=CARTESIAN_POINT('Ctrl Pts',(23.1932920749023,-68.0389988091933,
12.));
#127911=CARTESIAN_POINT('Ctrl Pts',(23.192897846702,-68.0628237546863,12.));
#127912=CARTESIAN_POINT('Ctrl Pts',(23.1924795338749,-68.0866910076251,
12.));
#127913=CARTESIAN_POINT('Ctrl Pts',(23.1920370767425,-68.110600445723,12.));
#127914=CARTESIAN_POINT('Ctrl Pts',(23.1915704159623,-68.1345519471695,
12.));
#127915=CARTESIAN_POINT('Ctrl Pts',(23.1910794925251,-68.1585453906257,
12.));
#127916=CARTESIAN_POINT('Ctrl Pts',(23.1905642477571,-68.1825806552129,
12.));
#127917=CARTESIAN_POINT('Ctrl Pts',(23.1900246233165,-68.2066576205116,
12.));
#127918=CARTESIAN_POINT('Ctrl Pts',(23.1894605611871,-68.2307761665633,
12.));
#127919=CARTESIAN_POINT('Ctrl Pts',(23.1888720036757,-68.2549361738681,
12.));
#127920=CARTESIAN_POINT('Ctrl Pts',(23.1882588934106,-68.2791375233795,
12.));
#127921=CARTESIAN_POINT('Ctrl Pts',(23.1876211733435,-68.3033800964939,
12.));
#127922=CARTESIAN_POINT('Ctrl Pts',(23.1869587867459,-68.3276637750485,
12.));
#127923=CARTESIAN_POINT('Ctrl Pts',(23.186271677203,-68.3519884413246,12.));
#127924=CARTESIAN_POINT('Ctrl Pts',(23.1855597886115,-68.376353978044,12.));
#127925=CARTESIAN_POINT('Ctrl Pts',(23.1848230651776,-68.4007602683652,
12.));
#127926=CARTESIAN_POINT('Ctrl Pts',(23.1840614514192,-68.4252071958729,
12.));
#127927=CARTESIAN_POINT('Ctrl Pts',(23.183274892163,-68.4496946445758,12.));
#127928=CARTESIAN_POINT('Ctrl Pts',(23.1824633325384,-68.4742224989099,
12.));
#127929=CARTESIAN_POINT('Ctrl Pts',(23.1816267179751,-68.4987906437356,
12.));
#127930=CARTESIAN_POINT('Ctrl Pts',(23.180764994201,-68.5233989643345,12.));
#127931=CARTESIAN_POINT('Ctrl Pts',(23.1798781072449,-68.5480473463985,
12.));
#127932=CARTESIAN_POINT('Ctrl Pts',(23.1789660034341,-68.5727356760278,
12.));
#127933=CARTESIAN_POINT('Ctrl Pts',(23.1780286293875,-68.597463839733,12.));
#127934=CARTESIAN_POINT('Ctrl Pts',(23.1770659320137,-68.6222317244342,
12.));
#127935=CARTESIAN_POINT('Ctrl Pts',(23.1760778585092,-68.6470392174564,
12.));
#127936=CARTESIAN_POINT('Ctrl Pts',(23.1750643563601,-68.6718862065216,
12.));
#127937=CARTESIAN_POINT('Ctrl Pts',(23.1740253733417,-68.696772579744,12.));
#127938=CARTESIAN_POINT('Ctrl Pts',(23.1729608575109,-68.7216982256341,
12.));
#127939=CARTESIAN_POINT('Ctrl Pts',(23.1718707572043,-68.746663033096,12.));
#127940=CARTESIAN_POINT('Ctrl Pts',(23.170755021036,-68.771666891425,12.));
#127941=CARTESIAN_POINT('Ctrl Pts',(23.1696135978997,-68.7967096902996,
12.));
#127942=CARTESIAN_POINT('Ctrl Pts',(23.1684464369686,-68.8217913197752,
12.));
#127943=CARTESIAN_POINT('Ctrl Pts',(23.1672534876889,-68.8469116702898,
12.));
#127944=CARTESIAN_POINT('Ctrl Pts',(23.1660346997763,-68.872070632661,12.));
#127945=CARTESIAN_POINT('Ctrl Pts',(23.164790023215,-68.8972680980842,12.));
#127946=CARTESIAN_POINT('Ctrl Pts',(23.1635194082581,-68.9225039581248,
12.));
#127947=CARTESIAN_POINT('Ctrl Pts',(23.1622228054291,-68.9477781047106,
12.));
#127948=CARTESIAN_POINT('Ctrl Pts',(23.1609001655155,-68.9730904301369,
12.));
#127949=CARTESIAN_POINT('Ctrl Pts',(23.1595514395656,-68.9984408270659,
12.));
#127950=CARTESIAN_POINT('Ctrl Pts',(23.1581765788868,-69.0238291885245,
12.));
#127951=CARTESIAN_POINT('Ctrl Pts',(23.1567755350469,-69.0492554078992,
12.));
#127952=CARTESIAN_POINT('Ctrl Pts',(23.1553482598762,-69.074719378928,12.));
#127953=CARTESIAN_POINT('Ctrl Pts',(23.1538947054614,-69.1002209957025,
12.));
#127954=CARTESIAN_POINT('Ctrl Pts',(23.152414824141,-69.1257601526687,12.));
#127955=CARTESIAN_POINT('Ctrl Pts',(23.1509085685032,-69.1513367446231,
12.));
#127956=CARTESIAN_POINT('Ctrl Pts',(23.1493758913858,-69.1769506667084,
12.));
#127957=CARTESIAN_POINT('Ctrl Pts',(23.1478167458789,-69.2026018144028,
12.));
#127958=CARTESIAN_POINT('Ctrl Pts',(23.1462310853206,-69.2282900835236,
12.));
#127959=CARTESIAN_POINT('Ctrl Pts',(23.1446188632931,-69.254015370231,12.));
#127960=CARTESIAN_POINT('Ctrl Pts',(23.142980033622,-69.2797775710273,12.));
#127961=CARTESIAN_POINT('Ctrl Pts',(23.1413145503762,-69.3055765827546,
12.));
#127962=CARTESIAN_POINT('Ctrl Pts',(23.1396223678725,-69.3314123025869,
12.));
#127963=CARTESIAN_POINT('Ctrl Pts',(23.1379034406718,-69.3572846280297,
12.));
#127964=CARTESIAN_POINT('Ctrl Pts',(23.1361577235709,-69.3831934569183,
12.));
#127965=CARTESIAN_POINT('Ctrl Pts',(23.1343851715989,-69.4091386874132,
12.));
#127966=CARTESIAN_POINT('Ctrl Pts',(23.1325857400144,-69.4351202179946,
12.));
#127967=CARTESIAN_POINT('Ctrl Pts',(23.1307593843061,-69.4611379474484,
12.));
#127968=CARTESIAN_POINT('Ctrl Pts',(23.1289060601924,-69.4871917748654,
12.));
#127969=CARTESIAN_POINT('Ctrl Pts',(23.1270257236204,-69.5132815996537,
12.));
#127970=CARTESIAN_POINT('Ctrl Pts',(23.1251183307676,-69.539407321546,12.));
#127971=CARTESIAN_POINT('Ctrl Pts',(23.1231838380452,-69.5655688406052,
12.));
#127972=CARTESIAN_POINT('Ctrl Pts',(23.1212222021051,-69.5917660572265,
12.));
#127973=CARTESIAN_POINT('Ctrl Pts',(23.1192333798441,-69.6179988721365,
12.));
#127974=CARTESIAN_POINT('Ctrl Pts',(23.1172173283858,-69.6442671863765,
12.));
#127975=CARTESIAN_POINT('Ctrl Pts',(23.115174005068,-69.6705709012852,12.));
#127976=CARTESIAN_POINT('Ctrl Pts',(23.1131033674301,-69.6969099184767,
12.));
#127977=CARTESIAN_POINT('Ctrl Pts',(23.1110053732046,-69.7232841398197,
12.));
#127978=CARTESIAN_POINT('Ctrl Pts',(23.1088799803089,-69.7496934674069,
12.));
#127979=CARTESIAN_POINT('Ctrl Pts',(23.1067271468609,-69.7761378035964,
12.));
#127980=CARTESIAN_POINT('Ctrl Pts',(23.104546831199,-69.8026170510572,12.));
#127981=CARTESIAN_POINT('Ctrl Pts',(23.1023389919051,-69.8291311128119,
12.));
#127982=CARTESIAN_POINT('Ctrl Pts',(23.1001035878241,-69.8556798922693,
12.));
#127983=CARTESIAN_POINT('Ctrl Pts',(23.097840578102,-69.8822632932768,12.));
#127984=CARTESIAN_POINT('Ctrl Pts',(23.0955499221558,-69.9088812200713,
12.));
#127985=CARTESIAN_POINT('Ctrl Pts',(23.0932315796067,-69.9355335771729,
12.));
#127986=CARTESIAN_POINT('Ctrl Pts',(23.090885510225,-69.9622202692873,12.));
#127987=CARTESIAN_POINT('Ctrl Pts',(23.0885116738797,-69.9889412012143,
12.));
#127988=CARTESIAN_POINT('Ctrl Pts',(23.0861100304729,-70.0156962777169,
12.));
#127989=CARTESIAN_POINT('Ctrl Pts',(23.0836805399374,-70.0424854035115,
12.));
#127990=CARTESIAN_POINT('Ctrl Pts',(23.0812231623765,-70.0693084835373,
12.));
#127991=CARTESIAN_POINT('Ctrl Pts',(23.0787378581774,-70.0961654231639,
12.));
#127992=CARTESIAN_POINT('Ctrl Pts',(23.0762245881389,-70.1230561284221,
12.));
#127993=CARTESIAN_POINT('Ctrl Pts',(23.0736833135938,-70.1499805062172,
12.));
#127994=CARTESIAN_POINT('Ctrl Pts',(23.0711139965439,-70.1769384645587,
12.));
#127995=CARTESIAN_POINT('Ctrl Pts',(23.068516599369,-70.2039299120488,12.));
#127996=CARTESIAN_POINT('Ctrl Pts',(23.0658910845432,-70.2309547573815,
12.));
#127997=CARTESIAN_POINT('Ctrl Pts',(23.0632374143279,-70.2580129087888,
12.));
#127998=CARTESIAN_POINT('Ctrl Pts',(23.0605555505321,-70.2851042736066,
12.));
#127999=CARTESIAN_POINT('Ctrl Pts',(23.0578454541104,-70.3122287575335,
12.));
#128000=CARTESIAN_POINT('Ctrl Pts',(23.0551070854926,-70.3393862652297,
12.));
#128001=CARTESIAN_POINT('Ctrl Pts',(23.0523404053172,-70.3665767016542,
12.));
#128002=CARTESIAN_POINT('Ctrl Pts',(23.0495453750763,-70.3937999732267,
12.));
#128003=CARTESIAN_POINT('Ctrl Pts',(23.046721957729,-70.4210559889348,12.));
#128004=CARTESIAN_POINT('Ctrl Pts',(23.0438701185012,-70.4483446617614,
12.));
#128005=CARTESIAN_POINT('Ctrl Pts',(23.0409898250756,-70.4756659090209,
12.));
#128006=CARTESIAN_POINT('Ctrl Pts',(23.0384964376036,-70.4991133648947,
12.));
#128007=CARTESIAN_POINT('Ctrl Pts',(23.0365694096172,-70.5171075702746,
12.));
#128008=CARTESIAN_POINT('Ctrl Pts',(23.0352213647764,-70.5296341535556,
12.));
#128009=CARTESIAN_POINT('Ctrl Pts',(23.0344606623298,-70.5366836381661,
12.));
#128010=CARTESIAN_POINT('Ctrl Pts',(23.0342913834072,-70.538251407892,12.));
#128011=CARTESIAN_POINT('',(23.1372951448023,-66.0656156664139,0.));
#128012=CARTESIAN_POINT('',(23.1372951448023,-66.0656156664138,0.));
#128013=CARTESIAN_POINT('Ctrl Pts',(23.0342913834072,-70.538251407892,0.));
#128014=CARTESIAN_POINT('Ctrl Pts',(23.0344606623298,-70.5366836381661,
0.));
#128015=CARTESIAN_POINT('Ctrl Pts',(23.0352213647764,-70.5296341535556,
0.));
#128016=CARTESIAN_POINT('Ctrl Pts',(23.0365694096172,-70.5171075702746,
0.));
#128017=CARTESIAN_POINT('Ctrl Pts',(23.0384964376036,-70.4991133648947,
0.));
#128018=CARTESIAN_POINT('Ctrl Pts',(23.0409898250756,-70.4756659090209,
0.));
#128019=CARTESIAN_POINT('Ctrl Pts',(23.0438701185012,-70.4483446617614,
0.));
#128020=CARTESIAN_POINT('Ctrl Pts',(23.046721957729,-70.4210559889348,0.));
#128021=CARTESIAN_POINT('Ctrl Pts',(23.0495453750763,-70.3937999732267,
0.));
#128022=CARTESIAN_POINT('Ctrl Pts',(23.0523404053172,-70.3665767016542,
0.));
#128023=CARTESIAN_POINT('Ctrl Pts',(23.0551070854926,-70.3393862652297,
0.));
#128024=CARTESIAN_POINT('Ctrl Pts',(23.0578454541104,-70.3122287575335,
0.));
#128025=CARTESIAN_POINT('Ctrl Pts',(23.0605555505321,-70.2851042736066,
0.));
#128026=CARTESIAN_POINT('Ctrl Pts',(23.0632374143279,-70.2580129087888,
0.));
#128027=CARTESIAN_POINT('Ctrl Pts',(23.0658910845432,-70.2309547573815,
0.));
#128028=CARTESIAN_POINT('Ctrl Pts',(23.068516599369,-70.2039299120488,0.));
#128029=CARTESIAN_POINT('Ctrl Pts',(23.0711139965439,-70.1769384645587,
0.));
#128030=CARTESIAN_POINT('Ctrl Pts',(23.0736833135938,-70.1499805062172,
0.));
#128031=CARTESIAN_POINT('Ctrl Pts',(23.0762245881389,-70.1230561284221,
0.));
#128032=CARTESIAN_POINT('Ctrl Pts',(23.0787378581774,-70.0961654231639,
0.));
#128033=CARTESIAN_POINT('Ctrl Pts',(23.0812231623765,-70.0693084835373,
0.));
#128034=CARTESIAN_POINT('Ctrl Pts',(23.0836805399374,-70.0424854035115,
0.));
#128035=CARTESIAN_POINT('Ctrl Pts',(23.0861100304729,-70.0156962777169,
0.));
#128036=CARTESIAN_POINT('Ctrl Pts',(23.0885116738797,-69.9889412012143,
0.));
#128037=CARTESIAN_POINT('Ctrl Pts',(23.090885510225,-69.9622202692873,0.));
#128038=CARTESIAN_POINT('Ctrl Pts',(23.0932315796067,-69.9355335771729,
0.));
#128039=CARTESIAN_POINT('Ctrl Pts',(23.0955499221558,-69.9088812200713,
0.));
#128040=CARTESIAN_POINT('Ctrl Pts',(23.097840578102,-69.8822632932768,0.));
#128041=CARTESIAN_POINT('Ctrl Pts',(23.1001035878241,-69.8556798922693,
0.));
#128042=CARTESIAN_POINT('Ctrl Pts',(23.1023389919051,-69.8291311128119,
0.));
#128043=CARTESIAN_POINT('Ctrl Pts',(23.104546831199,-69.8026170510572,0.));
#128044=CARTESIAN_POINT('Ctrl Pts',(23.1067271468609,-69.7761378035964,
0.));
#128045=CARTESIAN_POINT('Ctrl Pts',(23.1088799803089,-69.7496934674069,
0.));
#128046=CARTESIAN_POINT('Ctrl Pts',(23.1110053732046,-69.7232841398197,
0.));
#128047=CARTESIAN_POINT('Ctrl Pts',(23.1131033674301,-69.6969099184767,
0.));
#128048=CARTESIAN_POINT('Ctrl Pts',(23.115174005068,-69.6705709012852,0.));
#128049=CARTESIAN_POINT('Ctrl Pts',(23.1172173283858,-69.6442671863765,
0.));
#128050=CARTESIAN_POINT('Ctrl Pts',(23.1192333798441,-69.6179988721365,
0.));
#128051=CARTESIAN_POINT('Ctrl Pts',(23.1212222021051,-69.5917660572265,
0.));
#128052=CARTESIAN_POINT('Ctrl Pts',(23.1231838380452,-69.5655688406052,
0.));
#128053=CARTESIAN_POINT('Ctrl Pts',(23.1251183307676,-69.539407321546,0.));
#128054=CARTESIAN_POINT('Ctrl Pts',(23.1270257236204,-69.5132815996537,
0.));
#128055=CARTESIAN_POINT('Ctrl Pts',(23.1289060601924,-69.4871917748654,
0.));
#128056=CARTESIAN_POINT('Ctrl Pts',(23.1307593843061,-69.4611379474484,
0.));
#128057=CARTESIAN_POINT('Ctrl Pts',(23.1325857400144,-69.4351202179946,
0.));
#128058=CARTESIAN_POINT('Ctrl Pts',(23.1343851715989,-69.4091386874132,
0.));
#128059=CARTESIAN_POINT('Ctrl Pts',(23.1361577235709,-69.3831934569183,
0.));
#128060=CARTESIAN_POINT('Ctrl Pts',(23.1379034406718,-69.3572846280297,
0.));
#128061=CARTESIAN_POINT('Ctrl Pts',(23.1396223678725,-69.3314123025869,
0.));
#128062=CARTESIAN_POINT('Ctrl Pts',(23.1413145503762,-69.3055765827546,
0.));
#128063=CARTESIAN_POINT('Ctrl Pts',(23.142980033622,-69.2797775710273,0.));
#128064=CARTESIAN_POINT('Ctrl Pts',(23.1446188632931,-69.254015370231,0.));
#128065=CARTESIAN_POINT('Ctrl Pts',(23.1462310853206,-69.2282900835236,
0.));
#128066=CARTESIAN_POINT('Ctrl Pts',(23.1478167458789,-69.2026018144028,
0.));
#128067=CARTESIAN_POINT('Ctrl Pts',(23.1493758913858,-69.1769506667084,
0.));
#128068=CARTESIAN_POINT('Ctrl Pts',(23.1509085685032,-69.1513367446231,
0.));
#128069=CARTESIAN_POINT('Ctrl Pts',(23.152414824141,-69.1257601526687,0.));
#128070=CARTESIAN_POINT('Ctrl Pts',(23.1538947054614,-69.1002209957025,
0.));
#128071=CARTESIAN_POINT('Ctrl Pts',(23.1553482598762,-69.074719378928,0.));
#128072=CARTESIAN_POINT('Ctrl Pts',(23.1567755350469,-69.0492554078992,
0.));
#128073=CARTESIAN_POINT('Ctrl Pts',(23.1581765788868,-69.0238291885245,
0.));
#128074=CARTESIAN_POINT('Ctrl Pts',(23.1595514395656,-68.9984408270659,
0.));
#128075=CARTESIAN_POINT('Ctrl Pts',(23.1609001655155,-68.9730904301369,
0.));
#128076=CARTESIAN_POINT('Ctrl Pts',(23.1622228054291,-68.9477781047106,
0.));
#128077=CARTESIAN_POINT('Ctrl Pts',(23.1635194082581,-68.9225039581248,
0.));
#128078=CARTESIAN_POINT('Ctrl Pts',(23.164790023215,-68.8972680980842,0.));
#128079=CARTESIAN_POINT('Ctrl Pts',(23.1660346997763,-68.872070632661,0.));
#128080=CARTESIAN_POINT('Ctrl Pts',(23.1672534876889,-68.8469116702898,
0.));
#128081=CARTESIAN_POINT('Ctrl Pts',(23.1684464369686,-68.8217913197752,
0.));
#128082=CARTESIAN_POINT('Ctrl Pts',(23.1696135978997,-68.7967096902996,
0.));
#128083=CARTESIAN_POINT('Ctrl Pts',(23.170755021036,-68.771666891425,0.));
#128084=CARTESIAN_POINT('Ctrl Pts',(23.1718707572043,-68.746663033096,0.));
#128085=CARTESIAN_POINT('Ctrl Pts',(23.1729608575109,-68.7216982256341,
0.));
#128086=CARTESIAN_POINT('Ctrl Pts',(23.1740253733417,-68.696772579744,0.));
#128087=CARTESIAN_POINT('Ctrl Pts',(23.1750643563601,-68.6718862065216,
0.));
#128088=CARTESIAN_POINT('Ctrl Pts',(23.1760778585092,-68.6470392174564,
0.));
#128089=CARTESIAN_POINT('Ctrl Pts',(23.1770659320137,-68.6222317244342,
0.));
#128090=CARTESIAN_POINT('Ctrl Pts',(23.1780286293875,-68.597463839733,0.));
#128091=CARTESIAN_POINT('Ctrl Pts',(23.1789660034341,-68.5727356760278,
0.));
#128092=CARTESIAN_POINT('Ctrl Pts',(23.1798781072449,-68.5480473463985,
0.));
#128093=CARTESIAN_POINT('Ctrl Pts',(23.180764994201,-68.5233989643345,0.));
#128094=CARTESIAN_POINT('Ctrl Pts',(23.1816267179751,-68.4987906437356,
0.));
#128095=CARTESIAN_POINT('Ctrl Pts',(23.1824633325384,-68.4742224989099,
0.));
#128096=CARTESIAN_POINT('Ctrl Pts',(23.183274892163,-68.4496946445758,0.));
#128097=CARTESIAN_POINT('Ctrl Pts',(23.1840614514192,-68.4252071958729,
0.));
#128098=CARTESIAN_POINT('Ctrl Pts',(23.1848230651776,-68.4007602683652,
0.));
#128099=CARTESIAN_POINT('Ctrl Pts',(23.1855597886115,-68.376353978044,0.));
#128100=CARTESIAN_POINT('Ctrl Pts',(23.186271677203,-68.3519884413246,0.));
#128101=CARTESIAN_POINT('Ctrl Pts',(23.1869587867459,-68.3276637750485,
0.));
#128102=CARTESIAN_POINT('Ctrl Pts',(23.1876211733435,-68.3033800964939,
0.));
#128103=CARTESIAN_POINT('Ctrl Pts',(23.1882588934106,-68.2791375233795,
0.));
#128104=CARTESIAN_POINT('Ctrl Pts',(23.1888720036757,-68.2549361738681,
0.));
#128105=CARTESIAN_POINT('Ctrl Pts',(23.1894605611871,-68.2307761665633,
0.));
#128106=CARTESIAN_POINT('Ctrl Pts',(23.1900246233165,-68.2066576205116,
0.));
#128107=CARTESIAN_POINT('Ctrl Pts',(23.1905642477571,-68.1825806552129,
0.));
#128108=CARTESIAN_POINT('Ctrl Pts',(23.1910794925251,-68.1585453906257,
0.));
#128109=CARTESIAN_POINT('Ctrl Pts',(23.1915704159623,-68.1345519471695,
0.));
#128110=CARTESIAN_POINT('Ctrl Pts',(23.1920370767425,-68.110600445723,0.));
#128111=CARTESIAN_POINT('Ctrl Pts',(23.1924795338749,-68.0866910076251,
0.));
#128112=CARTESIAN_POINT('Ctrl Pts',(23.192897846702,-68.0628237546863,0.));
#128113=CARTESIAN_POINT('Ctrl Pts',(23.1932920749023,-68.0389988091933,
0.));
#128114=CARTESIAN_POINT('Ctrl Pts',(23.1936622784918,-68.0152162939121,
0.));
#128115=CARTESIAN_POINT('Ctrl Pts',(23.1940085178313,-67.991476332086,0.));
#128116=CARTESIAN_POINT('Ctrl Pts',(23.1943308536297,-67.9677790474385,
0.));
#128117=CARTESIAN_POINT('Ctrl Pts',(23.1946293469427,-67.9441245641842,
0.));
#128118=CARTESIAN_POINT('Ctrl Pts',(23.1949040591744,-67.9205130070324,
0.));
#128119=CARTESIAN_POINT('Ctrl Pts',(23.1951550520802,-67.8969445011916,
0.));
#128120=CARTESIAN_POINT('Ctrl Pts',(23.1953823877734,-67.8734191723667,
0.));
#128121=CARTESIAN_POINT('Ctrl Pts',(23.1955861287286,-67.8499371467616,
0.));
#128122=CARTESIAN_POINT('Ctrl Pts',(23.1957663377806,-67.8264985510917,
0.));
#128123=CARTESIAN_POINT('Ctrl Pts',(23.1959230781269,-67.8031035125887,
0.));
#128124=CARTESIAN_POINT('Ctrl Pts',(23.1960564133304,-67.7797521590045,
0.));
#128125=CARTESIAN_POINT('Ctrl Pts',(23.1961664073261,-67.7564446186079,
0.));
#128126=CARTESIAN_POINT('Ctrl Pts',(23.1962531244245,-67.7331810201883,
0.));
#128127=CARTESIAN_POINT('Ctrl Pts',(23.1963166293102,-67.7099614930671,
0.));
#128128=CARTESIAN_POINT('Ctrl Pts',(23.1963569870451,-67.6867861671031,
0.));
#128129=CARTESIAN_POINT('Ctrl Pts',(23.1963742630714,-67.6636551726964,
0.));
#128130=CARTESIAN_POINT('Ctrl Pts',(23.1963685232187,-67.6405686407863,
0.));
#128131=CARTESIAN_POINT('Ctrl Pts',(23.1963398337068,-67.6175267028555,
0.));
#128132=CARTESIAN_POINT('Ctrl Pts',(23.1962882611452,-67.5945294909426,
0.));
#128133=CARTESIAN_POINT('Ctrl Pts',(23.196213872536,-67.5715771376461,0.));
#128134=CARTESIAN_POINT('Ctrl Pts',(23.1961167352771,-67.5486697761288,
0.));
#128135=CARTESIAN_POINT('Ctrl Pts',(23.19599691717,-67.5258075401146,0.));
#128136=CARTESIAN_POINT('Ctrl Pts',(23.1958544864215,-67.502990563895,0.));
#128137=CARTESIAN_POINT('Ctrl Pts',(23.195689511644,-67.4802189823408,0.));
#128138=CARTESIAN_POINT('Ctrl Pts',(23.1955020618589,-67.4574929309076,
0.));
#128139=CARTESIAN_POINT('Ctrl Pts',(23.1952922065012,-67.4348125456398,
0.));
#128140=CARTESIAN_POINT('Ctrl Pts',(23.1950600154265,-67.412177963168,0.));
#128141=CARTESIAN_POINT('Ctrl Pts',(23.1948055589128,-67.3895893207182,
0.));
#128142=CARTESIAN_POINT('Ctrl Pts',(23.194528907661,-67.3670467561212,0.));
#128143=CARTESIAN_POINT('Ctrl Pts',(23.1942301327978,-67.3445504078176,
0.));
#128144=CARTESIAN_POINT('Ctrl Pts',(23.1939093058801,-67.3221004148604,
0.));
#128145=CARTESIAN_POINT('Ctrl Pts',(23.1935664989018,-67.2996969169098,
0.));
#128146=CARTESIAN_POINT('Ctrl Pts',(23.1932017842952,-67.2773400542477,
0.));
#128147=CARTESIAN_POINT('Ctrl Pts',(23.1928152349342,-67.2550299677888,
0.));
#128148=CARTESIAN_POINT('Ctrl Pts',(23.1924069241385,-67.232766799088,0.));
#128149=CARTESIAN_POINT('Ctrl Pts',(23.1919769256803,-67.2105506903447,
0.));
#128150=CARTESIAN_POINT('Ctrl Pts',(23.1915253137923,-67.1883817844038,
0.));
#128151=CARTESIAN_POINT('Ctrl Pts',(23.1910521631657,-67.1662602247639,
0.));
#128152=CARTESIAN_POINT('Ctrl Pts',(23.1905575489504,-67.1441861555817,
0.));
#128153=CARTESIAN_POINT('Ctrl Pts',(23.1900415467574,-67.1221597216741,
0.));
#128154=CARTESIAN_POINT('Ctrl Pts',(23.1895042326626,-67.1001810685143,
0.));
#128155=CARTESIAN_POINT('Ctrl Pts',(23.1889456832119,-67.0782503422305,
0.));
#128156=CARTESIAN_POINT('Ctrl Pts',(23.1883659754271,-67.0563676896325,
0.));
#128157=CARTESIAN_POINT('Ctrl Pts',(23.1877651868157,-67.0345332582306,
0.));
#128158=CARTESIAN_POINT('Ctrl Pts',(23.1871433953793,-67.0127471962501,
0.));
#128159=CARTESIAN_POINT('Ctrl Pts',(23.1865006796283,-66.9910096526462,
0.));
#128160=CARTESIAN_POINT('Ctrl Pts',(23.1858371185842,-66.9693207771031,
0.));
#128161=CARTESIAN_POINT('Ctrl Pts',(23.1851527917657,-66.9476807200203,
0.));
#128162=CARTESIAN_POINT('Ctrl Pts',(23.1844477791814,-66.9260896324949,
0.));
#128163=CARTESIAN_POINT('Ctrl Pts',(23.1837221613235,-66.9045476663063,
0.));
#128164=CARTESIAN_POINT('Ctrl Pts',(23.1829760191591,-66.8830549738795,
0.));
#128165=CARTESIAN_POINT('Ctrl Pts',(23.1822094341517,-66.8616117083331,
0.));
#128166=CARTESIAN_POINT('Ctrl Pts',(23.1814224882953,-66.8402180235566,
0.));
#128167=CARTESIAN_POINT('Ctrl Pts',(23.1806152641475,-66.8188740742727,
0.));
#128168=CARTESIAN_POINT('Ctrl Pts',(23.1797878448639,-66.7975800161,0.));
#128169=CARTESIAN_POINT('Ctrl Pts',(23.1789403142366,-66.7763360056121,
0.));
#128170=CARTESIAN_POINT('Ctrl Pts',(23.17807275663,-66.7551422002204,0.));
#128171=CARTESIAN_POINT('Ctrl Pts',(23.1771852569131,-66.7339987580427,
0.));
#128172=CARTESIAN_POINT('Ctrl Pts',(23.1762779004044,-66.7129058377896,
0.));
#128173=CARTESIAN_POINT('Ctrl Pts',(23.1753507727939,-66.6918635985972,
0.));
#128174=CARTESIAN_POINT('Ctrl Pts',(23.1744039601381,-66.6708722000079,
0.));
#128175=CARTESIAN_POINT('Ctrl Pts',(23.1734375490431,-66.6499318023473,
0.));
#128176=CARTESIAN_POINT('Ctrl Pts',(23.1724516268302,-66.6290425670549,
0.));
#128177=CARTESIAN_POINT('Ctrl Pts',(23.1714462816789,-66.6082046569644,
0.));
#128178=CARTESIAN_POINT('Ctrl Pts',(23.1704216028614,-66.5874182367563,
0.));
#128179=CARTESIAN_POINT('Ctrl Pts',(23.1693776805865,-66.5666834726454,
0.));
#128180=CARTESIAN_POINT('Ctrl Pts',(23.1683146055726,-66.5460005315376,
0.));
#128181=CARTESIAN_POINT('Ctrl Pts',(23.1672324686926,-66.5253695803206,
0.));
#128182=CARTESIAN_POINT('Ctrl Pts',(23.1661313606132,-66.5047907851348,
0.));
#128183=CARTESIAN_POINT('Ctrl Pts',(23.1650113713808,-66.4842643105311,
0.));
#128184=CARTESIAN_POINT('Ctrl Pts',(23.1638725912195,-66.4637903210727,
0.));
#128185=CARTESIAN_POINT('Ctrl Pts',(23.1627151114883,-66.4433689832478,
0.));
#128186=CARTESIAN_POINT('Ctrl Pts',(23.1615390254631,-66.4230004670278,
0.));
#128187=CARTESIAN_POINT('Ctrl Pts',(23.160344429474,-66.4026849481232,0.));
#128188=CARTESIAN_POINT('Ctrl Pts',(23.1591314230083,-66.3824226081802,
0.));
#128189=CARTESIAN_POINT('Ctrl Pts',(23.1579001063423,-66.3622136300654,
0.));
#128190=CARTESIAN_POINT('Ctrl Pts',(23.1566505784621,-66.3420581937147,
0.));
#128191=CARTESIAN_POINT('Ctrl Pts',(23.1553829352539,-66.3219564725184,
0.));
#128192=CARTESIAN_POINT('Ctrl Pts',(23.154097266619,-66.3019086275445,0.));
#128193=CARTESIAN_POINT('Ctrl Pts',(23.1527936592651,-66.281914813114,0.));
#128194=CARTESIAN_POINT('Ctrl Pts',(23.1514722022503,-66.2619751878793,
0.));
#128195=CARTESIAN_POINT('Ctrl Pts',(23.1501329914487,-66.2420899237318,
0.));
#128196=CARTESIAN_POINT('Ctrl Pts',(23.1487761349297,-66.2222592165398,
0.));
#128197=CARTESIAN_POINT('Ctrl Pts',(23.147401756643,-66.2024832934733,0.));
#128198=CARTESIAN_POINT('Ctrl Pts',(23.1460099850704,-66.1827623902755,
0.));
#128199=CARTESIAN_POINT('Ctrl Pts',(23.1446009424871,-66.163096729667,0.));
#128200=CARTESIAN_POINT('Ctrl Pts',(23.1431747350127,-66.14348650151,0.));
#128201=CARTESIAN_POINT('Ctrl Pts',(23.1417314398501,-66.1239318368803,
0.));
#128202=CARTESIAN_POINT('Ctrl Pts',(23.140271103958,-66.1044328067739,0.));
#128203=CARTESIAN_POINT('Ctrl Pts',(23.1390892229923,-66.0888781152779,
0.));
#128204=CARTESIAN_POINT('Ctrl Pts',(23.1381951597491,-66.0772371487475,
0.));
#128205=CARTESIAN_POINT('Ctrl Pts',(23.1375957166138,-66.0694876382212,
0.));
#128206=CARTESIAN_POINT('Ctrl Pts',(23.1372951448023,-66.0656156664139,
0.));
#128207=CARTESIAN_POINT('Ctrl Pts',(16.7341474417544,-72.5962692526112,
0.));
#128208=CARTESIAN_POINT('Ctrl Pts',(16.7341474417544,-72.5962692526112,
12.));
#128209=CARTESIAN_POINT('Ctrl Pts',(16.7352885767485,-72.5907910746008,
0.));
#128210=CARTESIAN_POINT('Ctrl Pts',(16.7352885767485,-72.5907910746008,
12.));
#128211=CARTESIAN_POINT('Ctrl Pts',(16.7375676985344,-72.5798376087774,
0.));
#128212=CARTESIAN_POINT('Ctrl Pts',(16.7375676985344,-72.5798376087774,
12.));
#128213=CARTESIAN_POINT('Ctrl Pts',(16.7409769366072,-72.5634160806351,
0.));
#128214=CARTESIAN_POINT('Ctrl Pts',(16.7409769366072,-72.5634160806351,
12.));
#128215=CARTESIAN_POINT('Ctrl Pts',(16.7455036973866,-72.5415380516637,
0.));
#128216=CARTESIAN_POINT('Ctrl Pts',(16.7455036973866,-72.5415380516637,
12.));
#128217=CARTESIAN_POINT('Ctrl Pts',(16.7511306618915,-72.514219427383,0.));
#128218=CARTESIAN_POINT('Ctrl Pts',(16.7511306618915,-72.514219427383,12.));
#128219=CARTESIAN_POINT('Ctrl Pts',(16.7567261380687,-72.4869297342427,
0.));
#128220=CARTESIAN_POINT('Ctrl Pts',(16.7567261380687,-72.4869297342427,
12.));
#128221=CARTESIAN_POINT('Ctrl Pts',(16.7622901280758,-72.4596690055437,
0.));
#128222=CARTESIAN_POINT('Ctrl Pts',(16.7622901280758,-72.4596690055437,
12.));
#128223=CARTESIAN_POINT('Ctrl Pts',(16.7678226404162,-72.4324372916746,
0.));
#128224=CARTESIAN_POINT('Ctrl Pts',(16.7678226404162,-72.4324372916746,
12.));
#128225=CARTESIAN_POINT('Ctrl Pts',(16.7733236932135,-72.4052346647799,
0.));
#128226=CARTESIAN_POINT('Ctrl Pts',(16.7733236932135,-72.4052346647799,
12.));
#128227=CARTESIAN_POINT('Ctrl Pts',(16.7787933137498,-72.3780612167786,
0.));
#128228=CARTESIAN_POINT('Ctrl Pts',(16.7787933137498,-72.3780612167786,
12.));
#128229=CARTESIAN_POINT('Ctrl Pts',(16.7842315351362,-72.3509170522838,
0.));
#128230=CARTESIAN_POINT('Ctrl Pts',(16.7842315351362,-72.3509170522838,
12.));
#128231=CARTESIAN_POINT('Ctrl Pts',(16.7896383937821,-72.3238022829223,
0.));
#128232=CARTESIAN_POINT('Ctrl Pts',(16.7896383937821,-72.3238022829223,
12.));
#128233=CARTESIAN_POINT('Ctrl Pts',(16.7950139266121,-72.2967170212353,
0.));
#128234=CARTESIAN_POINT('Ctrl Pts',(16.7950139266121,-72.2967170212353,
12.));
#128235=CARTESIAN_POINT('Ctrl Pts',(16.8003581682248,-72.2696613743782,
0.));
#128236=CARTESIAN_POINT('Ctrl Pts',(16.8003581682248,-72.2696613743782,
12.));
#128237=CARTESIAN_POINT('Ctrl Pts',(16.8056711485821,-72.2426354390213,
0.));
#128238=CARTESIAN_POINT('Ctrl Pts',(16.8056711485821,-72.2426354390213,
12.));
#128239=CARTESIAN_POINT('Ctrl Pts',(16.8109528945896,-72.2156393048975,
0.));
#128240=CARTESIAN_POINT('Ctrl Pts',(16.8109528945896,-72.2156393048975,
12.));
#128241=CARTESIAN_POINT('Ctrl Pts',(16.8162034312269,-72.1886730573452,
0.));
#128242=CARTESIAN_POINT('Ctrl Pts',(16.8162034312269,-72.1886730573452,
12.));
#128243=CARTESIAN_POINT('Ctrl Pts',(16.8214227828942,-72.1617367803235,
0.));
#128244=CARTESIAN_POINT('Ctrl Pts',(16.8214227828942,-72.1617367803235,
12.));
#128245=CARTESIAN_POINT('Ctrl Pts',(16.8266109745795,-72.13483055902,0.));
#128246=CARTESIAN_POINT('Ctrl Pts',(16.8266109745795,-72.13483055902,12.));
#128247=CARTESIAN_POINT('Ctrl Pts',(16.8317680333404,-72.1079544831513,
0.));
#128248=CARTESIAN_POINT('Ctrl Pts',(16.8317680333404,-72.1079544831513,
12.));
#128249=CARTESIAN_POINT('Ctrl Pts',(16.8368939881446,-72.0811086466121,
0.));
#128250=CARTESIAN_POINT('Ctrl Pts',(16.8368939881446,-72.0811086466121,
12.));
#128251=CARTESIAN_POINT('Ctrl Pts',(16.8419888691976,-72.0542931459825,
0.));
#128252=CARTESIAN_POINT('Ctrl Pts',(16.8419888691976,-72.0542931459825,
12.));
#128253=CARTESIAN_POINT('Ctrl Pts',(16.8470527074275,-72.0275080793727,
0.));
#128254=CARTESIAN_POINT('Ctrl Pts',(16.8470527074275,-72.0275080793727,
12.));
#128255=CARTESIAN_POINT('Ctrl Pts',(16.8520855339445,-72.0007535452081,
0.));
#128256=CARTESIAN_POINT('Ctrl Pts',(16.8520855339445,-72.0007535452081,
12.));
#128257=CARTESIAN_POINT('Ctrl Pts',(16.8570873794269,-71.9740296408347,
0.));
#128258=CARTESIAN_POINT('Ctrl Pts',(16.8570873794269,-71.9740296408347,
12.));
#128259=CARTESIAN_POINT('Ctrl Pts',(16.8620582738437,-71.9473364618922,
0.));
#128260=CARTESIAN_POINT('Ctrl Pts',(16.8620582738437,-71.9473364618922,
12.));
#128261=CARTESIAN_POINT('Ctrl Pts',(16.866998246792,-71.9206741030887,0.));
#128262=CARTESIAN_POINT('Ctrl Pts',(16.866998246792,-71.9206741030887,12.));
#128263=CARTESIAN_POINT('Ctrl Pts',(16.871907327697,-71.8940426586534,0.));
#128264=CARTESIAN_POINT('Ctrl Pts',(16.871907327697,-71.8940426586534,12.));
#128265=CARTESIAN_POINT('Ctrl Pts',(16.87678554607,-71.8674422229149,0.));
#128266=CARTESIAN_POINT('Ctrl Pts',(16.87678554607,-71.8674422229149,12.));
#128267=CARTESIAN_POINT('Ctrl Pts',(16.881632931747,-71.8408728908258,0.));
#128268=CARTESIAN_POINT('Ctrl Pts',(16.881632931747,-71.8408728908258,12.));
#128269=CARTESIAN_POINT('Ctrl Pts',(16.8864495151344,-71.8143347584962,
0.));
#128270=CARTESIAN_POINT('Ctrl Pts',(16.8864495151344,-71.8143347584962,
12.));
#128271=CARTESIAN_POINT('Ctrl Pts',(16.8912353270942,-71.7878279229546,
0.));
#128272=CARTESIAN_POINT('Ctrl Pts',(16.8912353270942,-71.7878279229546,
12.));
#128273=CARTESIAN_POINT('Ctrl Pts',(16.8959903988409,-71.7613524819235,
0.));
#128274=CARTESIAN_POINT('Ctrl Pts',(16.8959903988409,-71.7613524819235,
12.));
#128275=CARTESIAN_POINT('Ctrl Pts',(16.9007147618344,-71.7349085335796,
0.));
#128276=CARTESIAN_POINT('Ctrl Pts',(16.9007147618344,-71.7349085335796,
12.));
#128277=CARTESIAN_POINT('Ctrl Pts',(16.9054084476847,-71.7084961763357,
0.));
#128278=CARTESIAN_POINT('Ctrl Pts',(16.9054084476847,-71.7084961763357,
12.));
#128279=CARTESIAN_POINT('Ctrl Pts',(16.9100714880368,-71.6821155085612,
0.));
#128280=CARTESIAN_POINT('Ctrl Pts',(16.9100714880368,-71.6821155085612,
12.));
#128281=CARTESIAN_POINT('Ctrl Pts',(16.9147039145717,-71.6557666285917,
0.));
#128282=CARTESIAN_POINT('Ctrl Pts',(16.9147039145717,-71.6557666285917,
12.));
#128283=CARTESIAN_POINT('Ctrl Pts',(16.9193057590607,-71.6294496348652,
0.));
#128284=CARTESIAN_POINT('Ctrl Pts',(16.9193057590607,-71.6294496348652,
12.));
#128285=CARTESIAN_POINT('Ctrl Pts',(16.9238770534071,-71.6031646260174,
0.));
#128286=CARTESIAN_POINT('Ctrl Pts',(16.9238770534071,-71.6031646260174,
12.));
#128287=CARTESIAN_POINT('Ctrl Pts',(16.9284178296933,-71.5769117009842,
0.));
#128288=CARTESIAN_POINT('Ctrl Pts',(16.9284178296933,-71.5769117009842,
12.));
#128289=CARTESIAN_POINT('Ctrl Pts',(16.9329281202377,-71.5506909591128,
0.));
#128290=CARTESIAN_POINT('Ctrl Pts',(16.9329281202377,-71.5506909591128,
12.));
#128291=CARTESIAN_POINT('Ctrl Pts',(16.9374079576201,-71.5245025002139,
0.));
#128292=CARTESIAN_POINT('Ctrl Pts',(16.9374079576201,-71.5245025002139,
12.));
#128293=CARTESIAN_POINT('Ctrl Pts',(16.9418573746488,-71.4983464245055,
0.));
#128294=CARTESIAN_POINT('Ctrl Pts',(16.9418573746488,-71.4983464245055,
12.));
#128295=CARTESIAN_POINT('Ctrl Pts',(16.9462764043443,-71.4722228325794,
0.));
#128296=CARTESIAN_POINT('Ctrl Pts',(16.9462764043443,-71.4722228325794,
12.));
#128297=CARTESIAN_POINT('Ctrl Pts',(16.9506650799188,-71.4461318253563,
0.));
#128298=CARTESIAN_POINT('Ctrl Pts',(16.9506650799188,-71.4461318253563,
12.));
#128299=CARTESIAN_POINT('Ctrl Pts',(16.955023434762,-71.4200735040384,0.));
#128300=CARTESIAN_POINT('Ctrl Pts',(16.955023434762,-71.4200735040384,12.));
#128301=CARTESIAN_POINT('Ctrl Pts',(16.9593515024276,-71.3940479700677,
0.));
#128302=CARTESIAN_POINT('Ctrl Pts',(16.9593515024276,-71.3940479700677,
12.));
#128303=CARTESIAN_POINT('Ctrl Pts',(16.9636493166397,-71.3680553251562,
0.));
#128304=CARTESIAN_POINT('Ctrl Pts',(16.9636493166397,-71.3680553251562,
12.));
#128305=CARTESIAN_POINT('Ctrl Pts',(16.9679169112994,-71.3420956713082,
0.));
#128306=CARTESIAN_POINT('Ctrl Pts',(16.9679169112994,-71.3420956713082,
12.));
#128307=CARTESIAN_POINT('Ctrl Pts',(16.9721543204951,-71.3161691108427,
0.));
#128308=CARTESIAN_POINT('Ctrl Pts',(16.9721543204951,-71.3161691108427,
12.));
#128309=CARTESIAN_POINT('Ctrl Pts',(16.9763615785136,-71.290275746412,0.));
#128310=CARTESIAN_POINT('Ctrl Pts',(16.9763615785136,-71.290275746412,12.));
#128311=CARTESIAN_POINT('Ctrl Pts',(16.9805387198571,-71.2644156810198,
0.));
#128312=CARTESIAN_POINT('Ctrl Pts',(16.9805387198571,-71.2644156810198,
12.));
#128313=CARTESIAN_POINT('Ctrl Pts',(16.9846857792383,-71.2385890180221,
0.));
#128314=CARTESIAN_POINT('Ctrl Pts',(16.9846857792383,-71.2385890180221,
12.));
#128315=CARTESIAN_POINT('Ctrl Pts',(16.9888027915742,-71.212795861124,0.));
#128316=CARTESIAN_POINT('Ctrl Pts',(16.9888027915742,-71.212795861124,12.));
#128317=CARTESIAN_POINT('Ctrl Pts',(16.9928897919828,-71.187036314374,0.));
#128318=CARTESIAN_POINT('Ctrl Pts',(16.9928897919828,-71.187036314374,12.));
#128319=CARTESIAN_POINT('Ctrl Pts',(16.9969468157824,-71.1613104821568,
0.));
#128320=CARTESIAN_POINT('Ctrl Pts',(16.9969468157824,-71.1613104821568,
12.));
#128321=CARTESIAN_POINT('Ctrl Pts',(17.0009738984935,-71.1356184691806,
0.));
#128322=CARTESIAN_POINT('Ctrl Pts',(17.0009738984935,-71.1356184691806,
12.));
#128323=CARTESIAN_POINT('Ctrl Pts',(17.0049710758393,-71.1099603804786,
0.));
#128324=CARTESIAN_POINT('Ctrl Pts',(17.0049710758393,-71.1099603804786,
12.));
#128325=CARTESIAN_POINT('Ctrl Pts',(17.0089383837437,-71.0843363214221,
0.));
#128326=CARTESIAN_POINT('Ctrl Pts',(17.0089383837437,-71.0843363214221,
12.));
#128327=CARTESIAN_POINT('Ctrl Pts',(17.0128758583334,-71.0587463977268,
0.));
#128328=CARTESIAN_POINT('Ctrl Pts',(17.0128758583334,-71.0587463977268,
12.));
#128329=CARTESIAN_POINT('Ctrl Pts',(17.0167835359419,-71.0331907154574,
0.));
#128330=CARTESIAN_POINT('Ctrl Pts',(17.0167835359419,-71.0331907154574,
12.));
#128331=CARTESIAN_POINT('Ctrl Pts',(17.0206614531166,-71.0076693810301,
0.));
#128332=CARTESIAN_POINT('Ctrl Pts',(17.0206614531166,-71.0076693810301,
12.));
#128333=CARTESIAN_POINT('Ctrl Pts',(17.0245096466229,-70.9821825012136,
0.));
#128334=CARTESIAN_POINT('Ctrl Pts',(17.0245096466229,-70.9821825012136,
12.));
#128335=CARTESIAN_POINT('Ctrl Pts',(17.0283281534392,-70.956730183136,0.));
#128336=CARTESIAN_POINT('Ctrl Pts',(17.0283281534392,-70.956730183136,12.));
#128337=CARTESIAN_POINT('Ctrl Pts',(17.0321170107564,-70.9313125342876,
0.));
#128338=CARTESIAN_POINT('Ctrl Pts',(17.0321170107564,-70.9313125342876,
12.));
#128339=CARTESIAN_POINT('Ctrl Pts',(17.0358762559786,-70.9059296625214,
0.));
#128340=CARTESIAN_POINT('Ctrl Pts',(17.0358762559786,-70.9059296625214,
12.));
#128341=CARTESIAN_POINT('Ctrl Pts',(17.0396059267277,-70.8805816760501,
0.));
#128342=CARTESIAN_POINT('Ctrl Pts',(17.0396059267277,-70.8805816760501,
12.));
#128343=CARTESIAN_POINT('Ctrl Pts',(17.0433060608474,-70.8552686834423,
0.));
#128344=CARTESIAN_POINT('Ctrl Pts',(17.0433060608474,-70.8552686834423,
12.));
#128345=CARTESIAN_POINT('Ctrl Pts',(17.0469766964001,-70.8299907936334,
0.));
#128346=CARTESIAN_POINT('Ctrl Pts',(17.0469766964001,-70.8299907936334,
12.));
#128347=CARTESIAN_POINT('Ctrl Pts',(17.0506178716661,-70.8047481159298,
0.));
#128348=CARTESIAN_POINT('Ctrl Pts',(17.0506178716661,-70.8047481159298,
12.));
#128349=CARTESIAN_POINT('Ctrl Pts',(17.0542296251462,-70.7795407600127,
0.));
#128350=CARTESIAN_POINT('Ctrl Pts',(17.0542296251462,-70.7795407600127,
12.));
#128351=CARTESIAN_POINT('Ctrl Pts',(17.0578119955651,-70.754368835938,0.));
#128352=CARTESIAN_POINT('Ctrl Pts',(17.0578119955651,-70.754368835938,12.));
#128353=CARTESIAN_POINT('Ctrl Pts',(17.0613650218788,-70.7292324541348,
0.));
#128354=CARTESIAN_POINT('Ctrl Pts',(17.0613650218788,-70.7292324541348,
12.));
#128355=CARTESIAN_POINT('Ctrl Pts',(17.0648887432714,-70.7041317254127,
0.));
#128356=CARTESIAN_POINT('Ctrl Pts',(17.0648887432714,-70.7041317254127,
12.));
#128357=CARTESIAN_POINT('Ctrl Pts',(17.0683831991532,-70.6790667609678,
0.));
#128358=CARTESIAN_POINT('Ctrl Pts',(17.0683831991532,-70.6790667609678,
12.));
#128359=CARTESIAN_POINT('Ctrl Pts',(17.0718484291623,-70.6540376723839,
0.));
#128360=CARTESIAN_POINT('Ctrl Pts',(17.0718484291623,-70.6540376723839,
12.));
#128361=CARTESIAN_POINT('Ctrl Pts',(17.0752844731679,-70.6290445716341,
0.));
#128362=CARTESIAN_POINT('Ctrl Pts',(17.0752844731679,-70.6290445716341,
12.));
#128363=CARTESIAN_POINT('Ctrl Pts',(17.0786913712766,-70.6040875710762,
0.));
#128364=CARTESIAN_POINT('Ctrl Pts',(17.0786913712766,-70.6040875710762,
12.));
#128365=CARTESIAN_POINT('Ctrl Pts',(17.0820691638314,-70.5791667834599,
0.));
#128366=CARTESIAN_POINT('Ctrl Pts',(17.0820691638314,-70.5791667834599,
12.));
#128367=CARTESIAN_POINT('Ctrl Pts',(17.085417891409,-70.5542823219346,0.));
#128368=CARTESIAN_POINT('Ctrl Pts',(17.085417891409,-70.5542823219346,12.));
#128369=CARTESIAN_POINT('Ctrl Pts',(17.0887375948221,-70.5294343000516,
0.));
#128370=CARTESIAN_POINT('Ctrl Pts',(17.0887375948221,-70.5294343000516,
12.));
#128371=CARTESIAN_POINT('Ctrl Pts',(17.0920283151217,-70.5046228317669,
0.));
#128372=CARTESIAN_POINT('Ctrl Pts',(17.0920283151217,-70.5046228317669,
12.));
#128373=CARTESIAN_POINT('Ctrl Pts',(17.0952900936044,-70.4798480314364,
0.));
#128374=CARTESIAN_POINT('Ctrl Pts',(17.0952900936044,-70.4798480314364,
12.));
#128375=CARTESIAN_POINT('Ctrl Pts',(17.098522971812,-70.4551100138221,0.));
#128376=CARTESIAN_POINT('Ctrl Pts',(17.098522971812,-70.4551100138221,12.));
#128377=CARTESIAN_POINT('Ctrl Pts',(17.1017269915289,-70.4304088940998,
0.));
#128378=CARTESIAN_POINT('Ctrl Pts',(17.1017269915289,-70.4304088940998,
12.));
#128379=CARTESIAN_POINT('Ctrl Pts',(17.1049021947833,-70.4057447878621,
0.));
#128380=CARTESIAN_POINT('Ctrl Pts',(17.1049021947833,-70.4057447878621,
12.));
#128381=CARTESIAN_POINT('Ctrl Pts',(17.1080486238499,-70.3811178111206,
0.));
#128382=CARTESIAN_POINT('Ctrl Pts',(17.1080486238499,-70.3811178111206,
12.));
#128383=CARTESIAN_POINT('Ctrl Pts',(17.111166321257,-70.356528080303,0.));
#128384=CARTESIAN_POINT('Ctrl Pts',(17.111166321257,-70.356528080303,12.));
#128385=CARTESIAN_POINT('Ctrl Pts',(17.1142553297869,-70.3319757122576,
0.));
#128386=CARTESIAN_POINT('Ctrl Pts',(17.1142553297869,-70.3319757122576,
12.));
#128387=CARTESIAN_POINT('Ctrl Pts',(17.1173156924733,-70.3074608242613,
0.));
#128388=CARTESIAN_POINT('Ctrl Pts',(17.1173156924733,-70.3074608242613,
12.));
#128389=CARTESIAN_POINT('Ctrl Pts',(17.1203474526031,-70.2829835340239,
0.));
#128390=CARTESIAN_POINT('Ctrl Pts',(17.1203474526031,-70.2829835340239,
12.));
#128391=CARTESIAN_POINT('Ctrl Pts',(17.1233506537176,-70.2585439596899,
0.));
#128392=CARTESIAN_POINT('Ctrl Pts',(17.1233506537176,-70.2585439596899,
12.));
#128393=CARTESIAN_POINT('Ctrl Pts',(17.1263253396202,-70.2341422198362,
0.));
#128394=CARTESIAN_POINT('Ctrl Pts',(17.1263253396202,-70.2341422198362,
12.));
#128395=CARTESIAN_POINT('Ctrl Pts',(17.1292715543779,-70.2097784334749,
0.));
#128396=CARTESIAN_POINT('Ctrl Pts',(17.1292715543779,-70.2097784334749,
12.));
#128397=CARTESIAN_POINT('Ctrl Pts',(17.1321893423183,-70.1854527200636,
0.));
#128398=CARTESIAN_POINT('Ctrl Pts',(17.1321893423183,-70.1854527200636,
12.));
#128399=CARTESIAN_POINT('Ctrl Pts',(17.1350787480313,-70.1611651995085,
0.));
#128400=CARTESIAN_POINT('Ctrl Pts',(17.1350787480313,-70.1611651995085,
12.));
#128401=CARTESIAN_POINT('Ctrl Pts',(17.1379398163708,-70.1369159921686,
0.));
#128402=CARTESIAN_POINT('Ctrl Pts',(17.1379398163708,-70.1369159921686,
12.));
#128403=CARTESIAN_POINT('Ctrl Pts',(17.1407725924615,-70.1127052188515,
0.));
#128404=CARTESIAN_POINT('Ctrl Pts',(17.1407725924615,-70.1127052188515,
12.));
#128405=CARTESIAN_POINT('Ctrl Pts',(17.1435771217015,-70.0885330008169,
0.));
#128406=CARTESIAN_POINT('Ctrl Pts',(17.1435771217015,-70.0885330008169,
12.));
#128407=CARTESIAN_POINT('Ctrl Pts',(17.1463534497592,-70.0643994597865,
0.));
#128408=CARTESIAN_POINT('Ctrl Pts',(17.1463534497592,-70.0643994597865,
12.));
#128409=CARTESIAN_POINT('Ctrl Pts',(17.1491016225748,-70.040304717948,0.));
#128410=CARTESIAN_POINT('Ctrl Pts',(17.1491016225748,-70.040304717948,12.));
#128411=CARTESIAN_POINT('Ctrl Pts',(17.1518216863624,-70.0162488979586,
0.));
#128412=CARTESIAN_POINT('Ctrl Pts',(17.1518216863624,-70.0162488979586,
12.));
#128413=CARTESIAN_POINT('Ctrl Pts',(17.1545136876161,-69.9922321229428,
0.));
#128414=CARTESIAN_POINT('Ctrl Pts',(17.1545136876161,-69.9922321229428,
12.));
#128415=CARTESIAN_POINT('Ctrl Pts',(17.157177673114,-69.9682545164942,0.));
#128416=CARTESIAN_POINT('Ctrl Pts',(17.157177673114,-69.9682545164942,12.));
#128417=CARTESIAN_POINT('Ctrl Pts',(17.1598136899144,-69.9443162026865,
0.));
#128418=CARTESIAN_POINT('Ctrl Pts',(17.1598136899144,-69.9443162026865,
12.));
#128419=CARTESIAN_POINT('Ctrl Pts',(17.1624217853577,-69.9204173060779,
0.));
#128420=CARTESIAN_POINT('Ctrl Pts',(17.1624217853577,-69.9204173060779,
12.));
#128421=CARTESIAN_POINT('Ctrl Pts',(17.1650020070686,-69.8965579517147,
0.));
#128422=CARTESIAN_POINT('Ctrl Pts',(17.1650020070686,-69.8965579517147,
12.));
#128423=CARTESIAN_POINT('Ctrl Pts',(17.1675544029621,-69.8727382651292,
0.));
#128424=CARTESIAN_POINT('Ctrl Pts',(17.1675544029621,-69.8727382651292,
12.));
#128425=CARTESIAN_POINT('Ctrl Pts',(17.1700790212476,-69.8489583723417,
0.));
#128426=CARTESIAN_POINT('Ctrl Pts',(17.1700790212476,-69.8489583723417,
12.));
#128427=CARTESIAN_POINT('Ctrl Pts',(17.1725759104254,-69.8252183998713,
0.));
#128428=CARTESIAN_POINT('Ctrl Pts',(17.1725759104254,-69.8252183998713,
12.));
#128429=CARTESIAN_POINT('Ctrl Pts',(17.1750451192887,-69.8015184747404,
0.));
#128430=CARTESIAN_POINT('Ctrl Pts',(17.1750451192887,-69.8015184747404,
12.));
#128431=CARTESIAN_POINT('Ctrl Pts',(17.1774866969255,-69.7778587244788,
0.));
#128432=CARTESIAN_POINT('Ctrl Pts',(17.1774866969255,-69.7778587244788,
12.));
#128433=CARTESIAN_POINT('Ctrl Pts',(17.1799006927255,-69.7542392771216,
0.));
#128434=CARTESIAN_POINT('Ctrl Pts',(17.1799006927255,-69.7542392771216,
12.));
#128435=CARTESIAN_POINT('Ctrl Pts',(17.1822871563834,-69.7306602612125,
0.));
#128436=CARTESIAN_POINT('Ctrl Pts',(17.1822871563834,-69.7306602612125,
12.));
#128437=CARTESIAN_POINT('Ctrl Pts',(17.1846461378966,-69.7071218058149,
0.));
#128438=CARTESIAN_POINT('Ctrl Pts',(17.1846461378966,-69.7071218058149,
12.));
#128439=CARTESIAN_POINT('Ctrl Pts',(17.1869776875663,-69.6836240405151,
0.));
#128440=CARTESIAN_POINT('Ctrl Pts',(17.1869776875663,-69.6836240405151,
12.));
#128441=CARTESIAN_POINT('Ctrl Pts',(17.1892818560004,-69.6601670954277,
0.));
#128442=CARTESIAN_POINT('Ctrl Pts',(17.1892818560004,-69.6601670954277,
12.));
#128443=CARTESIAN_POINT('Ctrl Pts',(17.1915586941198,-69.6367511011927,
0.));
#128444=CARTESIAN_POINT('Ctrl Pts',(17.1915586941198,-69.6367511011927,
12.));
#128445=CARTESIAN_POINT('Ctrl Pts',(17.1938082531619,-69.6133761889787,
0.));
#128446=CARTESIAN_POINT('Ctrl Pts',(17.1938082531619,-69.6133761889787,
12.));
#128447=CARTESIAN_POINT('Ctrl Pts',(17.1960305846787,-69.5900424904954,
0.));
#128448=CARTESIAN_POINT('Ctrl Pts',(17.1960305846787,-69.5900424904954,
12.));
#128449=CARTESIAN_POINT('Ctrl Pts',(17.198225740538,-69.5667501379984,0.));
#128450=CARTESIAN_POINT('Ctrl Pts',(17.198225740538,-69.5667501379984,12.));
#128451=CARTESIAN_POINT('Ctrl Pts',(17.2003937729266,-69.5434992642932,
0.));
#128452=CARTESIAN_POINT('Ctrl Pts',(17.2003937729266,-69.5434992642932,
12.));
#128453=CARTESIAN_POINT('Ctrl Pts',(17.2025347343568,-69.5202900027329,
0.));
#128454=CARTESIAN_POINT('Ctrl Pts',(17.2025347343568,-69.5202900027329,
12.));
#128455=CARTESIAN_POINT('Ctrl Pts',(17.2046486776697,-69.497122487222,0.));
#128456=CARTESIAN_POINT('Ctrl Pts',(17.2046486776697,-69.497122487222,12.));
#128457=CARTESIAN_POINT('Ctrl Pts',(17.2067356560326,-69.4739968522271,
0.));
#128458=CARTESIAN_POINT('Ctrl Pts',(17.2067356560326,-69.4739968522271,
12.));
#128459=CARTESIAN_POINT('Ctrl Pts',(17.208795722942,-69.4509132327836,0.));
#128460=CARTESIAN_POINT('Ctrl Pts',(17.208795722942,-69.4509132327836,12.));
#128461=CARTESIAN_POINT('Ctrl Pts',(17.2108289322258,-69.4278717644989,
0.));
#128462=CARTESIAN_POINT('Ctrl Pts',(17.2108289322258,-69.4278717644989,
12.));
#128463=CARTESIAN_POINT('Ctrl Pts',(17.2128353380511,-69.4048725835516,
0.));
#128464=CARTESIAN_POINT('Ctrl Pts',(17.2128353380511,-69.4048725835516,
12.));
#128465=CARTESIAN_POINT('Ctrl Pts',(17.2148149949261,-69.3819158266955,
0.));
#128466=CARTESIAN_POINT('Ctrl Pts',(17.2148149949261,-69.3819158266955,
12.));
#128467=CARTESIAN_POINT('Ctrl Pts',(17.2167679576991,-69.359001631272,0.));
#128468=CARTESIAN_POINT('Ctrl Pts',(17.2167679576991,-69.359001631272,12.));
#128469=CARTESIAN_POINT('Ctrl Pts',(17.2186942815603,-69.3361301352149,
0.));
#128470=CARTESIAN_POINT('Ctrl Pts',(17.2186942815603,-69.3361301352149,
12.));
#128471=CARTESIAN_POINT('Ctrl Pts',(17.2205940220455,-69.3133014770542,
0.));
#128472=CARTESIAN_POINT('Ctrl Pts',(17.2205940220455,-69.3133014770542,
12.));
#128473=CARTESIAN_POINT('Ctrl Pts',(17.2224672350432,-69.2905157959141,
0.));
#128474=CARTESIAN_POINT('Ctrl Pts',(17.2224672350432,-69.2905157959141,
12.));
#128475=CARTESIAN_POINT('Ctrl Pts',(17.2243139767963,-69.2677732315199,
0.));
#128476=CARTESIAN_POINT('Ctrl Pts',(17.2243139767963,-69.2677732315199,
12.));
#128477=CARTESIAN_POINT('Ctrl Pts',(17.2261343039015,-69.2450739242092,
0.));
#128478=CARTESIAN_POINT('Ctrl Pts',(17.2261343039015,-69.2450739242092,
12.));
#128479=CARTESIAN_POINT('Ctrl Pts',(17.2279282733119,-69.2224180149377,
0.));
#128480=CARTESIAN_POINT('Ctrl Pts',(17.2279282733119,-69.2224180149377,
12.));
#128481=CARTESIAN_POINT('Ctrl Pts',(17.229695942341,-69.1998056452837,0.));
#128482=CARTESIAN_POINT('Ctrl Pts',(17.229695942341,-69.1998056452837,12.));
#128483=CARTESIAN_POINT('Ctrl Pts',(17.2314373686705,-69.1772369574462,
0.));
#128484=CARTESIAN_POINT('Ctrl Pts',(17.2314373686705,-69.1772369574462,
12.));
#128485=CARTESIAN_POINT('Ctrl Pts',(17.2331526103511,-69.1547120942542,
0.));
#128486=CARTESIAN_POINT('Ctrl Pts',(17.2331526103511,-69.1547120942542,
12.));
#128487=CARTESIAN_POINT('Ctrl Pts',(17.2348417258017,-69.1322311991759,
0.));
#128488=CARTESIAN_POINT('Ctrl Pts',(17.2348417258017,-69.1322311991759,
12.));
#128489=CARTESIAN_POINT('Ctrl Pts',(17.2365047738125,-69.1097944163244,
0.));
#128490=CARTESIAN_POINT('Ctrl Pts',(17.2365047738125,-69.1097944163244,
12.));
#128491=CARTESIAN_POINT('Ctrl Pts',(17.2381418135489,-69.0874018904598,
0.));
#128492=CARTESIAN_POINT('Ctrl Pts',(17.2381418135489,-69.0874018904598,
12.));
#128493=CARTESIAN_POINT('Ctrl Pts',(17.2397529045587,-69.0650537669859,
0.));
#128494=CARTESIAN_POINT('Ctrl Pts',(17.2397529045587,-69.0650537669859,
12.));
#128495=CARTESIAN_POINT('Ctrl Pts',(17.2413381067722,-69.0427501919636,
0.));
#128496=CARTESIAN_POINT('Ctrl Pts',(17.2413381067722,-69.0427501919636,
12.));
#128497=CARTESIAN_POINT('Ctrl Pts',(17.2428974805043,-69.0204913121226,
0.));
#128498=CARTESIAN_POINT('Ctrl Pts',(17.2428974805043,-69.0204913121226,
12.));
#128499=CARTESIAN_POINT('Ctrl Pts',(17.2444310864585,-68.9982772748694,
0.));
#128500=CARTESIAN_POINT('Ctrl Pts',(17.2444310864585,-68.9982772748694,
12.));
#128501=CARTESIAN_POINT('Ctrl Pts',(17.2459389857327,-68.9761082282922,
0.));
#128502=CARTESIAN_POINT('Ctrl Pts',(17.2459389857327,-68.9761082282922,
12.));
#128503=CARTESIAN_POINT('Ctrl Pts',(17.2474212398275,-68.9539843211618,
0.));
#128504=CARTESIAN_POINT('Ctrl Pts',(17.2474212398275,-68.9539843211618,
12.));
#128505=CARTESIAN_POINT('Ctrl Pts',(17.248877910643,-68.9319057029407,0.));
#128506=CARTESIAN_POINT('Ctrl Pts',(17.248877910643,-68.9319057029407,12.));
#128507=CARTESIAN_POINT('Ctrl Pts',(17.2503090604792,-68.9098725237868,
0.));
#128508=CARTESIAN_POINT('Ctrl Pts',(17.2503090604792,-68.9098725237868,
12.));
#128509=CARTESIAN_POINT('Ctrl Pts',(17.2517147520376,-68.8878849345557,
0.));
#128510=CARTESIAN_POINT('Ctrl Pts',(17.2517147520376,-68.8878849345557,
12.));
#128511=CARTESIAN_POINT('Ctrl Pts',(17.2530950484259,-68.8659430867977,
0.));
#128512=CARTESIAN_POINT('Ctrl Pts',(17.2530950484259,-68.8659430867977,
12.));
#128513=CARTESIAN_POINT('Ctrl Pts',(17.2544500131627,-68.8440471327563,
0.));
#128514=CARTESIAN_POINT('Ctrl Pts',(17.2544500131627,-68.8440471327563,
12.));
#128515=CARTESIAN_POINT('Ctrl Pts',(17.2557797101815,-68.8221972253954,
0.));
#128516=CARTESIAN_POINT('Ctrl Pts',(17.2557797101815,-68.8221972253954,
12.));
#128517=CARTESIAN_POINT('Ctrl Pts',(17.2570842038385,-68.8003935184193,
0.));
#128518=CARTESIAN_POINT('Ctrl Pts',(17.2570842038385,-68.8003935184193,
12.));
#128519=CARTESIAN_POINT('Ctrl Pts',(17.2583635589196,-68.7786361662876,
0.));
#128520=CARTESIAN_POINT('Ctrl Pts',(17.2583635589196,-68.7786361662876,
12.));
#128521=CARTESIAN_POINT('Ctrl Pts',(17.2596178406545,-68.7569253242312,
0.));
#128522=CARTESIAN_POINT('Ctrl Pts',(17.2596178406545,-68.7569253242312,
12.));
#128523=CARTESIAN_POINT('Ctrl Pts',(17.2608471147178,-68.7352611482519,
0.));
#128524=CARTESIAN_POINT('Ctrl Pts',(17.2608471147178,-68.7352611482519,
12.));
#128525=CARTESIAN_POINT('Ctrl Pts',(17.2620514472176,-68.7136437951074,
0.));
#128526=CARTESIAN_POINT('Ctrl Pts',(17.2620514472176,-68.7136437951074,
12.));
#128527=CARTESIAN_POINT('Ctrl Pts',(17.263230904689,-68.6920734222932,0.));
#128528=CARTESIAN_POINT('Ctrl Pts',(17.263230904689,-68.6920734222932,12.));
#128529=CARTESIAN_POINT('Ctrl Pts',(17.2643855540895,-68.6705501880263,
0.));
#128530=CARTESIAN_POINT('Ctrl Pts',(17.2643855540895,-68.6705501880263,
12.));
#128531=CARTESIAN_POINT('Ctrl Pts',(17.2655154627935,-68.6490742512085,
0.));
#128532=CARTESIAN_POINT('Ctrl Pts',(17.2655154627935,-68.6490742512085,
12.));
#128533=CARTESIAN_POINT('Ctrl Pts',(17.266620698609,-68.6276457714757,0.));
#128534=CARTESIAN_POINT('Ctrl Pts',(17.266620698609,-68.6276457714757,12.));
#128535=CARTESIAN_POINT('Ctrl Pts',(17.2677013298061,-68.606264909278,0.));
#128536=CARTESIAN_POINT('Ctrl Pts',(17.2677013298061,-68.606264909278,12.));
#128537=CARTESIAN_POINT('Ctrl Pts',(17.2687574251428,-68.5849318259449,
0.));
#128538=CARTESIAN_POINT('Ctrl Pts',(17.2687574251428,-68.5849318259449,
12.));
#128539=CARTESIAN_POINT('Ctrl Pts',(17.2697890538956,-68.5636466837502,
0.));
#128540=CARTESIAN_POINT('Ctrl Pts',(17.2697890538956,-68.5636466837502,
12.));
#128541=CARTESIAN_POINT('Ctrl Pts',(17.2707962858912,-68.5424096459746,
0.));
#128542=CARTESIAN_POINT('Ctrl Pts',(17.2707962858912,-68.5424096459746,
12.));
#128543=CARTESIAN_POINT('Ctrl Pts',(17.2717791914537,-68.5212208767835,
0.));
#128544=CARTESIAN_POINT('Ctrl Pts',(17.2717791914537,-68.5212208767835,
12.));
#128545=CARTESIAN_POINT('Ctrl Pts',(17.2727378413485,-68.5000805410896,
0.));
#128546=CARTESIAN_POINT('Ctrl Pts',(17.2727378413485,-68.5000805410896,
12.));
#128547=CARTESIAN_POINT('Ctrl Pts',(17.2736723067366,-68.4789888044357,
0.));
#128548=CARTESIAN_POINT('Ctrl Pts',(17.2736723067366,-68.4789888044357,
12.));
#128549=CARTESIAN_POINT('Ctrl Pts',(17.2745826591125,-68.4579458328208,
0.));
#128550=CARTESIAN_POINT('Ctrl Pts',(17.2745826591125,-68.4579458328208,
12.));
#128551=CARTESIAN_POINT('Ctrl Pts',(17.2754689703001,-68.4369517926803,
0.));
#128552=CARTESIAN_POINT('Ctrl Pts',(17.2754689703001,-68.4369517926803,
12.));
#128553=CARTESIAN_POINT('Ctrl Pts',(17.2763313126025,-68.4160068512781,
0.));
#128554=CARTESIAN_POINT('Ctrl Pts',(17.2763313126025,-68.4160068512781,
12.));
#128555=CARTESIAN_POINT('Ctrl Pts',(17.2771697589387,-68.3951111770498,
0.));
#128556=CARTESIAN_POINT('Ctrl Pts',(17.2771697589387,-68.3951111770498,
12.));
#128557=CARTESIAN_POINT('Ctrl Pts',(17.2779843829605,-68.374264939895,0.));
#128558=CARTESIAN_POINT('Ctrl Pts',(17.2779843829605,-68.374264939895,12.));
#128559=CARTESIAN_POINT('Ctrl Pts',(17.2787752592475,-68.353468311648,0.));
#128560=CARTESIAN_POINT('Ctrl Pts',(17.2787752592475,-68.353468311648,12.));
#128561=CARTESIAN_POINT('Ctrl Pts',(17.2795424631789,-68.3327214657533,
0.));
#128562=CARTESIAN_POINT('Ctrl Pts',(17.2795424631789,-68.3327214657533,
12.));
#128563=CARTESIAN_POINT('Ctrl Pts',(17.2802860705807,-68.3120245763884,
0.));
#128564=CARTESIAN_POINT('Ctrl Pts',(17.2802860705807,-68.3120245763884,
12.));
#128565=CARTESIAN_POINT('Ctrl Pts',(17.2810061574352,-68.2913778177258,
0.));
#128566=CARTESIAN_POINT('Ctrl Pts',(17.2810061574352,-68.2913778177258,
12.));
#128567=CARTESIAN_POINT('Ctrl Pts',(17.2817027995838,-68.2707813631761,
0.));
#128568=CARTESIAN_POINT('Ctrl Pts',(17.2817027995838,-68.2707813631761,
12.));
#128569=CARTESIAN_POINT('Ctrl Pts',(17.2823760723886,-68.250235384512,0.));
#128570=CARTESIAN_POINT('Ctrl Pts',(17.2823760723886,-68.250235384512,12.));
#128571=CARTESIAN_POINT('Ctrl Pts',(17.2830260513878,-68.2297400535339,
0.));
#128572=CARTESIAN_POINT('Ctrl Pts',(17.2830260513878,-68.2297400535339,
12.));
#128573=CARTESIAN_POINT('Ctrl Pts',(17.2836528130825,-68.2092955440591,
0.));
#128574=CARTESIAN_POINT('Ctrl Pts',(17.2836528130825,-68.2092955440591,
12.));
#128575=CARTESIAN_POINT('Ctrl Pts',(17.2842564355796,-68.1889020335418,
0.));
#128576=CARTESIAN_POINT('Ctrl Pts',(17.2842564355796,-68.1889020335418,
12.));
#128577=CARTESIAN_POINT('Ctrl Pts',(17.2848369995283,-68.1685597054193,
0.));
#128578=CARTESIAN_POINT('Ctrl Pts',(17.2848369995283,-68.1685597054193,
12.));
#128579=CARTESIAN_POINT('Ctrl Pts',(17.2853945882059,-68.1482687493176,
0.));
#128580=CARTESIAN_POINT('Ctrl Pts',(17.2853945882059,-68.1482687493176,
12.));
#128581=CARTESIAN_POINT('Ctrl Pts',(17.2859292855694,-68.1280293561473,
0.));
#128582=CARTESIAN_POINT('Ctrl Pts',(17.2859292855694,-68.1280293561473,
12.));
#128583=CARTESIAN_POINT('Ctrl Pts',(17.2864411745455,-68.1078417137865,
0.));
#128584=CARTESIAN_POINT('Ctrl Pts',(17.2864411745455,-68.1078417137865,
12.));
#128585=CARTESIAN_POINT('Ctrl Pts',(17.2869303355438,-68.0877060033229,
0.));
#128586=CARTESIAN_POINT('Ctrl Pts',(17.2869303355438,-68.0877060033229,
12.));
#128587=CARTESIAN_POINT('Ctrl Pts',(17.2873968440855,-68.0676223930469,
0.));
#128588=CARTESIAN_POINT('Ctrl Pts',(17.2873968440855,-68.0676223930469,
12.));
#128589=CARTESIAN_POINT('Ctrl Pts',(17.2878407730981,-68.0475910442494,
0.));
#128590=CARTESIAN_POINT('Ctrl Pts',(17.2878407730981,-68.0475910442494,
12.));
#128591=CARTESIAN_POINT('Ctrl Pts',(17.2882621974737,-68.027612122741,0.));
#128592=CARTESIAN_POINT('Ctrl Pts',(17.2882621974737,-68.027612122741,12.));
#128593=CARTESIAN_POINT('Ctrl Pts',(17.28866119774,-68.007685808115,0.));
#128594=CARTESIAN_POINT('Ctrl Pts',(17.28866119774,-68.007685808115,12.));
#128595=CARTESIAN_POINT('Ctrl Pts',(17.2890378644843,-67.9878123049132,
0.));
#128596=CARTESIAN_POINT('Ctrl Pts',(17.2890378644843,-67.9878123049132,
12.));
#128597=CARTESIAN_POINT('Ctrl Pts',(17.2893923013852,-67.9679918502441,
0.));
#128598=CARTESIAN_POINT('Ctrl Pts',(17.2893923013852,-67.9679918502441,
12.));
#128599=CARTESIAN_POINT('Ctrl Pts',(17.2897246158895,-67.9482246901517,
0.));
#128600=CARTESIAN_POINT('Ctrl Pts',(17.2897246158895,-67.9482246901517,
12.));
#128601=CARTESIAN_POINT('Ctrl Pts',(17.2900349103956,-67.9285110571662,
0.));
#128602=CARTESIAN_POINT('Ctrl Pts',(17.2900349103956,-67.9285110571662,
12.));
#128603=CARTESIAN_POINT('Ctrl Pts',(17.2903232740717,-67.908851149676,0.));
#128604=CARTESIAN_POINT('Ctrl Pts',(17.2903232740717,-67.908851149676,12.));
#128605=CARTESIAN_POINT('Ctrl Pts',(17.2905897724029,-67.8892451049871,
0.));
#128606=CARTESIAN_POINT('Ctrl Pts',(17.2905897724029,-67.8892451049871,
12.));
#128607=CARTESIAN_POINT('Ctrl Pts',(17.2908344459816,-67.8696929979178,
0.));
#128608=CARTESIAN_POINT('Ctrl Pts',(17.2908344459816,-67.8696929979178,
12.));
#128609=CARTESIAN_POINT('Ctrl Pts',(17.2910127431203,-67.8540944890057,
0.));
#128610=CARTESIAN_POINT('Ctrl Pts',(17.2910127431203,-67.8540944890057,
12.));
#128611=CARTESIAN_POINT('Ctrl Pts',(17.2911366591419,-67.8424198971214,
0.));
#128612=CARTESIAN_POINT('Ctrl Pts',(17.2911366591419,-67.8424198971214,
12.));
#128613=CARTESIAN_POINT('Ctrl Pts',(17.2912149114145,-67.8346476309106,
0.));
#128614=CARTESIAN_POINT('Ctrl Pts',(17.2912149114145,-67.8346476309106,
12.));
#128615=CARTESIAN_POINT('Ctrl Pts',(17.2912529479484,-67.8307641965655,
0.));
#128616=CARTESIAN_POINT('Ctrl Pts',(17.2912529479484,-67.8307641965655,
12.));
#128617=CARTESIAN_POINT('',(17.2912529479484,-67.8307641965655,12.));
#128618=CARTESIAN_POINT('Ctrl Pts',(17.2912529479484,-67.8307641965655,
12.));
#128619=CARTESIAN_POINT('Ctrl Pts',(17.2912149114145,-67.8346476309106,
12.));
#128620=CARTESIAN_POINT('Ctrl Pts',(17.2911366591419,-67.8424198971214,
12.));
#128621=CARTESIAN_POINT('Ctrl Pts',(17.2910127431203,-67.8540944890057,
12.));
#128622=CARTESIAN_POINT('Ctrl Pts',(17.2908344459816,-67.8696929979178,
12.));
#128623=CARTESIAN_POINT('Ctrl Pts',(17.2905897724029,-67.8892451049871,
12.));
#128624=CARTESIAN_POINT('Ctrl Pts',(17.2903232740717,-67.908851149676,12.));
#128625=CARTESIAN_POINT('Ctrl Pts',(17.2900349103956,-67.9285110571662,
12.));
#128626=CARTESIAN_POINT('Ctrl Pts',(17.2897246158895,-67.9482246901517,
12.));
#128627=CARTESIAN_POINT('Ctrl Pts',(17.2893923013852,-67.9679918502441,
12.));
#128628=CARTESIAN_POINT('Ctrl Pts',(17.2890378644843,-67.9878123049132,
12.));
#128629=CARTESIAN_POINT('Ctrl Pts',(17.28866119774,-68.007685808115,12.));
#128630=CARTESIAN_POINT('Ctrl Pts',(17.2882621974737,-68.027612122741,12.));
#128631=CARTESIAN_POINT('Ctrl Pts',(17.2878407730981,-68.0475910442494,
12.));
#128632=CARTESIAN_POINT('Ctrl Pts',(17.2873968440855,-68.0676223930469,
12.));
#128633=CARTESIAN_POINT('Ctrl Pts',(17.2869303355438,-68.0877060033229,
12.));
#128634=CARTESIAN_POINT('Ctrl Pts',(17.2864411745455,-68.1078417137865,
12.));
#128635=CARTESIAN_POINT('Ctrl Pts',(17.2859292855694,-68.1280293561473,
12.));
#128636=CARTESIAN_POINT('Ctrl Pts',(17.2853945882059,-68.1482687493176,
12.));
#128637=CARTESIAN_POINT('Ctrl Pts',(17.2848369995283,-68.1685597054193,
12.));
#128638=CARTESIAN_POINT('Ctrl Pts',(17.2842564355796,-68.1889020335418,
12.));
#128639=CARTESIAN_POINT('Ctrl Pts',(17.2836528130825,-68.2092955440591,
12.));
#128640=CARTESIAN_POINT('Ctrl Pts',(17.2830260513878,-68.2297400535339,
12.));
#128641=CARTESIAN_POINT('Ctrl Pts',(17.2823760723886,-68.250235384512,12.));
#128642=CARTESIAN_POINT('Ctrl Pts',(17.2817027995838,-68.2707813631761,
12.));
#128643=CARTESIAN_POINT('Ctrl Pts',(17.2810061574352,-68.2913778177258,
12.));
#128644=CARTESIAN_POINT('Ctrl Pts',(17.2802860705807,-68.3120245763884,
12.));
#128645=CARTESIAN_POINT('Ctrl Pts',(17.2795424631789,-68.3327214657533,
12.));
#128646=CARTESIAN_POINT('Ctrl Pts',(17.2787752592475,-68.353468311648,12.));
#128647=CARTESIAN_POINT('Ctrl Pts',(17.2779843829605,-68.374264939895,12.));
#128648=CARTESIAN_POINT('Ctrl Pts',(17.2771697589387,-68.3951111770498,
12.));
#128649=CARTESIAN_POINT('Ctrl Pts',(17.2763313126025,-68.4160068512781,
12.));
#128650=CARTESIAN_POINT('Ctrl Pts',(17.2754689703001,-68.4369517926803,
12.));
#128651=CARTESIAN_POINT('Ctrl Pts',(17.2745826591125,-68.4579458328208,
12.));
#128652=CARTESIAN_POINT('Ctrl Pts',(17.2736723067366,-68.4789888044357,
12.));
#128653=CARTESIAN_POINT('Ctrl Pts',(17.2727378413485,-68.5000805410896,
12.));
#128654=CARTESIAN_POINT('Ctrl Pts',(17.2717791914537,-68.5212208767835,
12.));
#128655=CARTESIAN_POINT('Ctrl Pts',(17.2707962858912,-68.5424096459746,
12.));
#128656=CARTESIAN_POINT('Ctrl Pts',(17.2697890538956,-68.5636466837502,
12.));
#128657=CARTESIAN_POINT('Ctrl Pts',(17.2687574251428,-68.5849318259449,
12.));
#128658=CARTESIAN_POINT('Ctrl Pts',(17.2677013298061,-68.606264909278,12.));
#128659=CARTESIAN_POINT('Ctrl Pts',(17.266620698609,-68.6276457714757,12.));
#128660=CARTESIAN_POINT('Ctrl Pts',(17.2655154627935,-68.6490742512085,
12.));
#128661=CARTESIAN_POINT('Ctrl Pts',(17.2643855540895,-68.6705501880263,
12.));
#128662=CARTESIAN_POINT('Ctrl Pts',(17.263230904689,-68.6920734222932,12.));
#128663=CARTESIAN_POINT('Ctrl Pts',(17.2620514472176,-68.7136437951074,
12.));
#128664=CARTESIAN_POINT('Ctrl Pts',(17.2608471147178,-68.7352611482519,
12.));
#128665=CARTESIAN_POINT('Ctrl Pts',(17.2596178406545,-68.7569253242312,
12.));
#128666=CARTESIAN_POINT('Ctrl Pts',(17.2583635589196,-68.7786361662876,
12.));
#128667=CARTESIAN_POINT('Ctrl Pts',(17.2570842038385,-68.8003935184193,
12.));
#128668=CARTESIAN_POINT('Ctrl Pts',(17.2557797101815,-68.8221972253954,
12.));
#128669=CARTESIAN_POINT('Ctrl Pts',(17.2544500131627,-68.8440471327563,
12.));
#128670=CARTESIAN_POINT('Ctrl Pts',(17.2530950484259,-68.8659430867977,
12.));
#128671=CARTESIAN_POINT('Ctrl Pts',(17.2517147520376,-68.8878849345557,
12.));
#128672=CARTESIAN_POINT('Ctrl Pts',(17.2503090604792,-68.9098725237868,
12.));
#128673=CARTESIAN_POINT('Ctrl Pts',(17.248877910643,-68.9319057029407,12.));
#128674=CARTESIAN_POINT('Ctrl Pts',(17.2474212398275,-68.9539843211618,
12.));
#128675=CARTESIAN_POINT('Ctrl Pts',(17.2459389857327,-68.9761082282922,
12.));
#128676=CARTESIAN_POINT('Ctrl Pts',(17.2444310864585,-68.9982772748694,
12.));
#128677=CARTESIAN_POINT('Ctrl Pts',(17.2428974805043,-69.0204913121226,
12.));
#128678=CARTESIAN_POINT('Ctrl Pts',(17.2413381067722,-69.0427501919636,
12.));
#128679=CARTESIAN_POINT('Ctrl Pts',(17.2397529045587,-69.0650537669859,
12.));
#128680=CARTESIAN_POINT('Ctrl Pts',(17.2381418135489,-69.0874018904598,
12.));
#128681=CARTESIAN_POINT('Ctrl Pts',(17.2365047738125,-69.1097944163244,
12.));
#128682=CARTESIAN_POINT('Ctrl Pts',(17.2348417258017,-69.1322311991759,
12.));
#128683=CARTESIAN_POINT('Ctrl Pts',(17.2331526103511,-69.1547120942542,
12.));
#128684=CARTESIAN_POINT('Ctrl Pts',(17.2314373686705,-69.1772369574462,
12.));
#128685=CARTESIAN_POINT('Ctrl Pts',(17.229695942341,-69.1998056452837,12.));
#128686=CARTESIAN_POINT('Ctrl Pts',(17.2279282733119,-69.2224180149377,
12.));
#128687=CARTESIAN_POINT('Ctrl Pts',(17.2261343039015,-69.2450739242092,
12.));
#128688=CARTESIAN_POINT('Ctrl Pts',(17.2243139767963,-69.2677732315199,
12.));
#128689=CARTESIAN_POINT('Ctrl Pts',(17.2224672350432,-69.2905157959141,
12.));
#128690=CARTESIAN_POINT('Ctrl Pts',(17.2205940220455,-69.3133014770542,
12.));
#128691=CARTESIAN_POINT('Ctrl Pts',(17.2186942815603,-69.3361301352149,
12.));
#128692=CARTESIAN_POINT('Ctrl Pts',(17.2167679576991,-69.359001631272,12.));
#128693=CARTESIAN_POINT('Ctrl Pts',(17.2148149949261,-69.3819158266955,
12.));
#128694=CARTESIAN_POINT('Ctrl Pts',(17.2128353380511,-69.4048725835516,
12.));
#128695=CARTESIAN_POINT('Ctrl Pts',(17.2108289322258,-69.4278717644989,
12.));
#128696=CARTESIAN_POINT('Ctrl Pts',(17.208795722942,-69.4509132327836,12.));
#128697=CARTESIAN_POINT('Ctrl Pts',(17.2067356560326,-69.4739968522271,
12.));
#128698=CARTESIAN_POINT('Ctrl Pts',(17.2046486776697,-69.497122487222,12.));
#128699=CARTESIAN_POINT('Ctrl Pts',(17.2025347343568,-69.5202900027329,
12.));
#128700=CARTESIAN_POINT('Ctrl Pts',(17.2003937729266,-69.5434992642932,
12.));
#128701=CARTESIAN_POINT('Ctrl Pts',(17.198225740538,-69.5667501379984,12.));
#128702=CARTESIAN_POINT('Ctrl Pts',(17.1960305846787,-69.5900424904954,
12.));
#128703=CARTESIAN_POINT('Ctrl Pts',(17.1938082531619,-69.6133761889787,
12.));
#128704=CARTESIAN_POINT('Ctrl Pts',(17.1915586941198,-69.6367511011927,
12.));
#128705=CARTESIAN_POINT('Ctrl Pts',(17.1892818560004,-69.6601670954277,
12.));
#128706=CARTESIAN_POINT('Ctrl Pts',(17.1869776875663,-69.6836240405151,
12.));
#128707=CARTESIAN_POINT('Ctrl Pts',(17.1846461378966,-69.7071218058149,
12.));
#128708=CARTESIAN_POINT('Ctrl Pts',(17.1822871563834,-69.7306602612125,
12.));
#128709=CARTESIAN_POINT('Ctrl Pts',(17.1799006927255,-69.7542392771216,
12.));
#128710=CARTESIAN_POINT('Ctrl Pts',(17.1774866969255,-69.7778587244788,
12.));
#128711=CARTESIAN_POINT('Ctrl Pts',(17.1750451192887,-69.8015184747404,
12.));
#128712=CARTESIAN_POINT('Ctrl Pts',(17.1725759104254,-69.8252183998713,
12.));
#128713=CARTESIAN_POINT('Ctrl Pts',(17.1700790212476,-69.8489583723417,
12.));
#128714=CARTESIAN_POINT('Ctrl Pts',(17.1675544029621,-69.8727382651292,
12.));
#128715=CARTESIAN_POINT('Ctrl Pts',(17.1650020070686,-69.8965579517147,
12.));
#128716=CARTESIAN_POINT('Ctrl Pts',(17.1624217853577,-69.9204173060779,
12.));
#128717=CARTESIAN_POINT('Ctrl Pts',(17.1598136899144,-69.9443162026865,
12.));
#128718=CARTESIAN_POINT('Ctrl Pts',(17.157177673114,-69.9682545164942,12.));
#128719=CARTESIAN_POINT('Ctrl Pts',(17.1545136876161,-69.9922321229428,
12.));
#128720=CARTESIAN_POINT('Ctrl Pts',(17.1518216863624,-70.0162488979586,
12.));
#128721=CARTESIAN_POINT('Ctrl Pts',(17.1491016225748,-70.040304717948,12.));
#128722=CARTESIAN_POINT('Ctrl Pts',(17.1463534497592,-70.0643994597865,
12.));
#128723=CARTESIAN_POINT('Ctrl Pts',(17.1435771217015,-70.0885330008169,
12.));
#128724=CARTESIAN_POINT('Ctrl Pts',(17.1407725924615,-70.1127052188515,
12.));
#128725=CARTESIAN_POINT('Ctrl Pts',(17.1379398163708,-70.1369159921686,
12.));
#128726=CARTESIAN_POINT('Ctrl Pts',(17.1350787480313,-70.1611651995085,
12.));
#128727=CARTESIAN_POINT('Ctrl Pts',(17.1321893423183,-70.1854527200636,
12.));
#128728=CARTESIAN_POINT('Ctrl Pts',(17.1292715543779,-70.2097784334749,
12.));
#128729=CARTESIAN_POINT('Ctrl Pts',(17.1263253396202,-70.2341422198362,
12.));
#128730=CARTESIAN_POINT('Ctrl Pts',(17.1233506537176,-70.2585439596899,
12.));
#128731=CARTESIAN_POINT('Ctrl Pts',(17.1203474526031,-70.2829835340239,
12.));
#128732=CARTESIAN_POINT('Ctrl Pts',(17.1173156924733,-70.3074608242613,
12.));
#128733=CARTESIAN_POINT('Ctrl Pts',(17.1142553297869,-70.3319757122576,
12.));
#128734=CARTESIAN_POINT('Ctrl Pts',(17.111166321257,-70.356528080303,12.));
#128735=CARTESIAN_POINT('Ctrl Pts',(17.1080486238499,-70.3811178111206,
12.));
#128736=CARTESIAN_POINT('Ctrl Pts',(17.1049021947833,-70.4057447878621,
12.));
#128737=CARTESIAN_POINT('Ctrl Pts',(17.1017269915289,-70.4304088940998,
12.));
#128738=CARTESIAN_POINT('Ctrl Pts',(17.098522971812,-70.4551100138221,12.));
#128739=CARTESIAN_POINT('Ctrl Pts',(17.0952900936044,-70.4798480314364,
12.));
#128740=CARTESIAN_POINT('Ctrl Pts',(17.0920283151217,-70.5046228317669,
12.));
#128741=CARTESIAN_POINT('Ctrl Pts',(17.0887375948221,-70.5294343000516,
12.));
#128742=CARTESIAN_POINT('Ctrl Pts',(17.085417891409,-70.5542823219346,12.));
#128743=CARTESIAN_POINT('Ctrl Pts',(17.0820691638314,-70.5791667834599,
12.));
#128744=CARTESIAN_POINT('Ctrl Pts',(17.0786913712766,-70.6040875710762,
12.));
#128745=CARTESIAN_POINT('Ctrl Pts',(17.0752844731679,-70.6290445716341,
12.));
#128746=CARTESIAN_POINT('Ctrl Pts',(17.0718484291623,-70.6540376723839,
12.));
#128747=CARTESIAN_POINT('Ctrl Pts',(17.0683831991532,-70.6790667609678,
12.));
#128748=CARTESIAN_POINT('Ctrl Pts',(17.0648887432714,-70.7041317254127,
12.));
#128749=CARTESIAN_POINT('Ctrl Pts',(17.0613650218788,-70.7292324541348,
12.));
#128750=CARTESIAN_POINT('Ctrl Pts',(17.0578119955651,-70.754368835938,12.));
#128751=CARTESIAN_POINT('Ctrl Pts',(17.0542296251462,-70.7795407600127,
12.));
#128752=CARTESIAN_POINT('Ctrl Pts',(17.0506178716661,-70.8047481159298,
12.));
#128753=CARTESIAN_POINT('Ctrl Pts',(17.0469766964001,-70.8299907936334,
12.));
#128754=CARTESIAN_POINT('Ctrl Pts',(17.0433060608474,-70.8552686834423,
12.));
#128755=CARTESIAN_POINT('Ctrl Pts',(17.0396059267277,-70.8805816760501,
12.));
#128756=CARTESIAN_POINT('Ctrl Pts',(17.0358762559786,-70.9059296625214,
12.));
#128757=CARTESIAN_POINT('Ctrl Pts',(17.0321170107564,-70.9313125342876,
12.));
#128758=CARTESIAN_POINT('Ctrl Pts',(17.0283281534392,-70.956730183136,12.));
#128759=CARTESIAN_POINT('Ctrl Pts',(17.0245096466229,-70.9821825012136,
12.));
#128760=CARTESIAN_POINT('Ctrl Pts',(17.0206614531166,-71.0076693810301,
12.));
#128761=CARTESIAN_POINT('Ctrl Pts',(17.0167835359419,-71.0331907154574,
12.));
#128762=CARTESIAN_POINT('Ctrl Pts',(17.0128758583334,-71.0587463977268,
12.));
#128763=CARTESIAN_POINT('Ctrl Pts',(17.0089383837437,-71.0843363214221,
12.));
#128764=CARTESIAN_POINT('Ctrl Pts',(17.0049710758393,-71.1099603804786,
12.));
#128765=CARTESIAN_POINT('Ctrl Pts',(17.0009738984935,-71.1356184691806,
12.));
#128766=CARTESIAN_POINT('Ctrl Pts',(16.9969468157824,-71.1613104821568,
12.));
#128767=CARTESIAN_POINT('Ctrl Pts',(16.9928897919828,-71.187036314374,12.));
#128768=CARTESIAN_POINT('Ctrl Pts',(16.9888027915742,-71.212795861124,12.));
#128769=CARTESIAN_POINT('Ctrl Pts',(16.9846857792383,-71.2385890180221,
12.));
#128770=CARTESIAN_POINT('Ctrl Pts',(16.9805387198571,-71.2644156810198,
12.));
#128771=CARTESIAN_POINT('Ctrl Pts',(16.9763615785136,-71.290275746412,12.));
#128772=CARTESIAN_POINT('Ctrl Pts',(16.9721543204951,-71.3161691108427,
12.));
#128773=CARTESIAN_POINT('Ctrl Pts',(16.9679169112994,-71.3420956713082,
12.));
#128774=CARTESIAN_POINT('Ctrl Pts',(16.9636493166397,-71.3680553251562,
12.));
#128775=CARTESIAN_POINT('Ctrl Pts',(16.9593515024276,-71.3940479700677,
12.));
#128776=CARTESIAN_POINT('Ctrl Pts',(16.955023434762,-71.4200735040384,12.));
#128777=CARTESIAN_POINT('Ctrl Pts',(16.9506650799188,-71.4461318253563,
12.));
#128778=CARTESIAN_POINT('Ctrl Pts',(16.9462764043443,-71.4722228325794,
12.));
#128779=CARTESIAN_POINT('Ctrl Pts',(16.9418573746488,-71.4983464245055,
12.));
#128780=CARTESIAN_POINT('Ctrl Pts',(16.9374079576201,-71.5245025002139,
12.));
#128781=CARTESIAN_POINT('Ctrl Pts',(16.9329281202377,-71.5506909591128,
12.));
#128782=CARTESIAN_POINT('Ctrl Pts',(16.9284178296933,-71.5769117009842,
12.));
#128783=CARTESIAN_POINT('Ctrl Pts',(16.9238770534071,-71.6031646260174,
12.));
#128784=CARTESIAN_POINT('Ctrl Pts',(16.9193057590607,-71.6294496348652,
12.));
#128785=CARTESIAN_POINT('Ctrl Pts',(16.9147039145717,-71.6557666285917,
12.));
#128786=CARTESIAN_POINT('Ctrl Pts',(16.9100714880368,-71.6821155085612,
12.));
#128787=CARTESIAN_POINT('Ctrl Pts',(16.9054084476847,-71.7084961763357,
12.));
#128788=CARTESIAN_POINT('Ctrl Pts',(16.9007147618344,-71.7349085335796,
12.));
#128789=CARTESIAN_POINT('Ctrl Pts',(16.8959903988409,-71.7613524819235,
12.));
#128790=CARTESIAN_POINT('Ctrl Pts',(16.8912353270942,-71.7878279229546,
12.));
#128791=CARTESIAN_POINT('Ctrl Pts',(16.8864495151344,-71.8143347584962,
12.));
#128792=CARTESIAN_POINT('Ctrl Pts',(16.881632931747,-71.8408728908258,12.));
#128793=CARTESIAN_POINT('Ctrl Pts',(16.87678554607,-71.8674422229149,12.));
#128794=CARTESIAN_POINT('Ctrl Pts',(16.871907327697,-71.8940426586534,12.));
#128795=CARTESIAN_POINT('Ctrl Pts',(16.866998246792,-71.9206741030887,12.));
#128796=CARTESIAN_POINT('Ctrl Pts',(16.8620582738437,-71.9473364618922,
12.));
#128797=CARTESIAN_POINT('Ctrl Pts',(16.8570873794269,-71.9740296408347,
12.));
#128798=CARTESIAN_POINT('Ctrl Pts',(16.8520855339445,-72.0007535452081,
12.));
#128799=CARTESIAN_POINT('Ctrl Pts',(16.8470527074275,-72.0275080793727,
12.));
#128800=CARTESIAN_POINT('Ctrl Pts',(16.8419888691976,-72.0542931459825,
12.));
#128801=CARTESIAN_POINT('Ctrl Pts',(16.8368939881446,-72.0811086466121,
12.));
#128802=CARTESIAN_POINT('Ctrl Pts',(16.8317680333404,-72.1079544831513,
12.));
#128803=CARTESIAN_POINT('Ctrl Pts',(16.8266109745795,-72.13483055902,12.));
#128804=CARTESIAN_POINT('Ctrl Pts',(16.8214227828942,-72.1617367803235,
12.));
#128805=CARTESIAN_POINT('Ctrl Pts',(16.8162034312269,-72.1886730573452,
12.));
#128806=CARTESIAN_POINT('Ctrl Pts',(16.8109528945896,-72.2156393048975,
12.));
#128807=CARTESIAN_POINT('Ctrl Pts',(16.8064254147775,-72.2387802230856,
12.));
#128808=CARTESIAN_POINT('Ctrl Pts',(16.8029374213794,-72.256538003526,12.));
#128809=CARTESIAN_POINT('Ctrl Pts',(16.8005027425862,-72.2688994295264,
12.));
#128810=CARTESIAN_POINT('Ctrl Pts',(16.7991305317749,-72.2758557891329,
12.));
#128811=CARTESIAN_POINT('Ctrl Pts',(16.7988252568748,-72.2774028393915,
12.));
#128812=CARTESIAN_POINT('',(17.2912529479484,-67.8307641965655,0.));
#128813=CARTESIAN_POINT('',(17.2912529479484,-67.8307641965655,0.));
#128814=CARTESIAN_POINT('Ctrl Pts',(16.7988252568748,-72.2774028393915,
0.));
#128815=CARTESIAN_POINT('Ctrl Pts',(16.7991305317749,-72.275855789133,0.));
#128816=CARTESIAN_POINT('Ctrl Pts',(16.8005027425862,-72.2688994295265,
0.));
#128817=CARTESIAN_POINT('Ctrl Pts',(16.8029374213794,-72.2565380035261,
0.));
#128818=CARTESIAN_POINT('Ctrl Pts',(16.8064254147775,-72.2387802230856,
0.));
#128819=CARTESIAN_POINT('Ctrl Pts',(16.8109528945896,-72.2156393048975,
0.));
#128820=CARTESIAN_POINT('Ctrl Pts',(16.8162034312269,-72.1886730573452,
0.));
#128821=CARTESIAN_POINT('Ctrl Pts',(16.8214227828942,-72.1617367803235,
0.));
#128822=CARTESIAN_POINT('Ctrl Pts',(16.8266109745795,-72.13483055902,0.));
#128823=CARTESIAN_POINT('Ctrl Pts',(16.8317680333404,-72.1079544831513,
0.));
#128824=CARTESIAN_POINT('Ctrl Pts',(16.8368939881446,-72.0811086466121,
0.));
#128825=CARTESIAN_POINT('Ctrl Pts',(16.8419888691976,-72.0542931459825,
0.));
#128826=CARTESIAN_POINT('Ctrl Pts',(16.8470527074275,-72.0275080793727,
0.));
#128827=CARTESIAN_POINT('Ctrl Pts',(16.8520855339445,-72.0007535452081,
0.));
#128828=CARTESIAN_POINT('Ctrl Pts',(16.8570873794269,-71.9740296408347,
0.));
#128829=CARTESIAN_POINT('Ctrl Pts',(16.8620582738437,-71.9473364618922,
0.));
#128830=CARTESIAN_POINT('Ctrl Pts',(16.866998246792,-71.9206741030887,0.));
#128831=CARTESIAN_POINT('Ctrl Pts',(16.871907327697,-71.8940426586534,0.));
#128832=CARTESIAN_POINT('Ctrl Pts',(16.87678554607,-71.8674422229149,0.));
#128833=CARTESIAN_POINT('Ctrl Pts',(16.881632931747,-71.8408728908258,0.));
#128834=CARTESIAN_POINT('Ctrl Pts',(16.8864495151344,-71.8143347584962,
0.));
#128835=CARTESIAN_POINT('Ctrl Pts',(16.8912353270942,-71.7878279229546,
0.));
#128836=CARTESIAN_POINT('Ctrl Pts',(16.8959903988409,-71.7613524819235,
0.));
#128837=CARTESIAN_POINT('Ctrl Pts',(16.9007147618344,-71.7349085335796,
0.));
#128838=CARTESIAN_POINT('Ctrl Pts',(16.9054084476847,-71.7084961763357,
0.));
#128839=CARTESIAN_POINT('Ctrl Pts',(16.9100714880368,-71.6821155085612,
0.));
#128840=CARTESIAN_POINT('Ctrl Pts',(16.9147039145717,-71.6557666285917,
0.));
#128841=CARTESIAN_POINT('Ctrl Pts',(16.9193057590607,-71.6294496348652,
0.));
#128842=CARTESIAN_POINT('Ctrl Pts',(16.9238770534071,-71.6031646260174,
0.));
#128843=CARTESIAN_POINT('Ctrl Pts',(16.9284178296933,-71.5769117009842,
0.));
#128844=CARTESIAN_POINT('Ctrl Pts',(16.9329281202377,-71.5506909591128,
0.));
#128845=CARTESIAN_POINT('Ctrl Pts',(16.9374079576201,-71.5245025002139,
0.));
#128846=CARTESIAN_POINT('Ctrl Pts',(16.9418573746488,-71.4983464245055,
0.));
#128847=CARTESIAN_POINT('Ctrl Pts',(16.9462764043443,-71.4722228325794,
0.));
#128848=CARTESIAN_POINT('Ctrl Pts',(16.9506650799188,-71.4461318253563,
0.));
#128849=CARTESIAN_POINT('Ctrl Pts',(16.955023434762,-71.4200735040384,0.));
#128850=CARTESIAN_POINT('Ctrl Pts',(16.9593515024276,-71.3940479700677,
0.));
#128851=CARTESIAN_POINT('Ctrl Pts',(16.9636493166397,-71.3680553251562,
0.));
#128852=CARTESIAN_POINT('Ctrl Pts',(16.9679169112994,-71.3420956713082,
0.));
#128853=CARTESIAN_POINT('Ctrl Pts',(16.9721543204951,-71.3161691108427,
0.));
#128854=CARTESIAN_POINT('Ctrl Pts',(16.9763615785136,-71.290275746412,0.));
#128855=CARTESIAN_POINT('Ctrl Pts',(16.9805387198571,-71.2644156810198,
0.));
#128856=CARTESIAN_POINT('Ctrl Pts',(16.9846857792383,-71.2385890180221,
0.));
#128857=CARTESIAN_POINT('Ctrl Pts',(16.9888027915742,-71.212795861124,0.));
#128858=CARTESIAN_POINT('Ctrl Pts',(16.9928897919828,-71.187036314374,0.));
#128859=CARTESIAN_POINT('Ctrl Pts',(16.9969468157824,-71.1613104821568,
0.));
#128860=CARTESIAN_POINT('Ctrl Pts',(17.0009738984935,-71.1356184691806,
0.));
#128861=CARTESIAN_POINT('Ctrl Pts',(17.0049710758393,-71.1099603804786,
0.));
#128862=CARTESIAN_POINT('Ctrl Pts',(17.0089383837437,-71.0843363214221,
0.));
#128863=CARTESIAN_POINT('Ctrl Pts',(17.0128758583334,-71.0587463977268,
0.));
#128864=CARTESIAN_POINT('Ctrl Pts',(17.0167835359419,-71.0331907154574,
0.));
#128865=CARTESIAN_POINT('Ctrl Pts',(17.0206614531166,-71.0076693810301,
0.));
#128866=CARTESIAN_POINT('Ctrl Pts',(17.0245096466229,-70.9821825012136,
0.));
#128867=CARTESIAN_POINT('Ctrl Pts',(17.0283281534392,-70.956730183136,0.));
#128868=CARTESIAN_POINT('Ctrl Pts',(17.0321170107564,-70.9313125342876,
0.));
#128869=CARTESIAN_POINT('Ctrl Pts',(17.0358762559786,-70.9059296625214,
0.));
#128870=CARTESIAN_POINT('Ctrl Pts',(17.0396059267277,-70.8805816760501,
0.));
#128871=CARTESIAN_POINT('Ctrl Pts',(17.0433060608474,-70.8552686834423,
0.));
#128872=CARTESIAN_POINT('Ctrl Pts',(17.0469766964001,-70.8299907936334,
0.));
#128873=CARTESIAN_POINT('Ctrl Pts',(17.0506178716661,-70.8047481159298,
0.));
#128874=CARTESIAN_POINT('Ctrl Pts',(17.0542296251462,-70.7795407600127,
0.));
#128875=CARTESIAN_POINT('Ctrl Pts',(17.0578119955651,-70.754368835938,0.));
#128876=CARTESIAN_POINT('Ctrl Pts',(17.0613650218788,-70.7292324541348,
0.));
#128877=CARTESIAN_POINT('Ctrl Pts',(17.0648887432714,-70.7041317254127,
0.));
#128878=CARTESIAN_POINT('Ctrl Pts',(17.0683831991532,-70.6790667609678,
0.));
#128879=CARTESIAN_POINT('Ctrl Pts',(17.0718484291623,-70.6540376723839,
0.));
#128880=CARTESIAN_POINT('Ctrl Pts',(17.0752844731679,-70.6290445716341,
0.));
#128881=CARTESIAN_POINT('Ctrl Pts',(17.0786913712766,-70.6040875710762,
0.));
#128882=CARTESIAN_POINT('Ctrl Pts',(17.0820691638314,-70.5791667834599,
0.));
#128883=CARTESIAN_POINT('Ctrl Pts',(17.085417891409,-70.5542823219346,0.));
#128884=CARTESIAN_POINT('Ctrl Pts',(17.0887375948221,-70.5294343000516,
0.));
#128885=CARTESIAN_POINT('Ctrl Pts',(17.0920283151217,-70.5046228317669,
0.));
#128886=CARTESIAN_POINT('Ctrl Pts',(17.0952900936044,-70.4798480314364,
0.));
#128887=CARTESIAN_POINT('Ctrl Pts',(17.098522971812,-70.4551100138221,0.));
#128888=CARTESIAN_POINT('Ctrl Pts',(17.1017269915289,-70.4304088940998,
0.));
#128889=CARTESIAN_POINT('Ctrl Pts',(17.1049021947833,-70.4057447878621,
0.));
#128890=CARTESIAN_POINT('Ctrl Pts',(17.1080486238499,-70.3811178111206,
0.));
#128891=CARTESIAN_POINT('Ctrl Pts',(17.111166321257,-70.356528080303,0.));
#128892=CARTESIAN_POINT('Ctrl Pts',(17.1142553297869,-70.3319757122576,
0.));
#128893=CARTESIAN_POINT('Ctrl Pts',(17.1173156924733,-70.3074608242613,
0.));
#128894=CARTESIAN_POINT('Ctrl Pts',(17.1203474526031,-70.2829835340239,
0.));
#128895=CARTESIAN_POINT('Ctrl Pts',(17.1233506537176,-70.2585439596899,
0.));
#128896=CARTESIAN_POINT('Ctrl Pts',(17.1263253396202,-70.2341422198362,
0.));
#128897=CARTESIAN_POINT('Ctrl Pts',(17.1292715543779,-70.2097784334749,
0.));
#128898=CARTESIAN_POINT('Ctrl Pts',(17.1321893423183,-70.1854527200636,
0.));
#128899=CARTESIAN_POINT('Ctrl Pts',(17.1350787480313,-70.1611651995085,
0.));
#128900=CARTESIAN_POINT('Ctrl Pts',(17.1379398163708,-70.1369159921686,
0.));
#128901=CARTESIAN_POINT('Ctrl Pts',(17.1407725924615,-70.1127052188515,
0.));
#128902=CARTESIAN_POINT('Ctrl Pts',(17.1435771217015,-70.0885330008169,
0.));
#128903=CARTESIAN_POINT('Ctrl Pts',(17.1463534497592,-70.0643994597865,
0.));
#128904=CARTESIAN_POINT('Ctrl Pts',(17.1491016225748,-70.040304717948,0.));
#128905=CARTESIAN_POINT('Ctrl Pts',(17.1518216863624,-70.0162488979586,
0.));
#128906=CARTESIAN_POINT('Ctrl Pts',(17.1545136876161,-69.9922321229428,
0.));
#128907=CARTESIAN_POINT('Ctrl Pts',(17.157177673114,-69.9682545164942,0.));
#128908=CARTESIAN_POINT('Ctrl Pts',(17.1598136899144,-69.9443162026865,
0.));
#128909=CARTESIAN_POINT('Ctrl Pts',(17.1624217853577,-69.9204173060779,
0.));
#128910=CARTESIAN_POINT('Ctrl Pts',(17.1650020070686,-69.8965579517147,
0.));
#128911=CARTESIAN_POINT('Ctrl Pts',(17.1675544029621,-69.8727382651292,
0.));
#128912=CARTESIAN_POINT('Ctrl Pts',(17.1700790212476,-69.8489583723417,
0.));
#128913=CARTESIAN_POINT('Ctrl Pts',(17.1725759104254,-69.8252183998713,
0.));
#128914=CARTESIAN_POINT('Ctrl Pts',(17.1750451192887,-69.8015184747404,
0.));
#128915=CARTESIAN_POINT('Ctrl Pts',(17.1774866969255,-69.7778587244788,
0.));
#128916=CARTESIAN_POINT('Ctrl Pts',(17.1799006927255,-69.7542392771216,
0.));
#128917=CARTESIAN_POINT('Ctrl Pts',(17.1822871563834,-69.7306602612125,
0.));
#128918=CARTESIAN_POINT('Ctrl Pts',(17.1846461378966,-69.7071218058149,
0.));
#128919=CARTESIAN_POINT('Ctrl Pts',(17.1869776875663,-69.6836240405151,
0.));
#128920=CARTESIAN_POINT('Ctrl Pts',(17.1892818560004,-69.6601670954277,
0.));
#128921=CARTESIAN_POINT('Ctrl Pts',(17.1915586941198,-69.6367511011927,
0.));
#128922=CARTESIAN_POINT('Ctrl Pts',(17.1938082531619,-69.6133761889787,
0.));
#128923=CARTESIAN_POINT('Ctrl Pts',(17.1960305846787,-69.5900424904954,
0.));
#128924=CARTESIAN_POINT('Ctrl Pts',(17.198225740538,-69.5667501379984,0.));
#128925=CARTESIAN_POINT('Ctrl Pts',(17.2003937729266,-69.5434992642932,
0.));
#128926=CARTESIAN_POINT('Ctrl Pts',(17.2025347343568,-69.5202900027329,
0.));
#128927=CARTESIAN_POINT('Ctrl Pts',(17.2046486776697,-69.497122487222,0.));
#128928=CARTESIAN_POINT('Ctrl Pts',(17.2067356560326,-69.4739968522271,
0.));
#128929=CARTESIAN_POINT('Ctrl Pts',(17.208795722942,-69.4509132327836,0.));
#128930=CARTESIAN_POINT('Ctrl Pts',(17.2108289322258,-69.4278717644989,
0.));
#128931=CARTESIAN_POINT('Ctrl Pts',(17.2128353380511,-69.4048725835516,
0.));
#128932=CARTESIAN_POINT('Ctrl Pts',(17.2148149949261,-69.3819158266955,
0.));
#128933=CARTESIAN_POINT('Ctrl Pts',(17.2167679576991,-69.359001631272,0.));
#128934=CARTESIAN_POINT('Ctrl Pts',(17.2186942815603,-69.3361301352149,
0.));
#128935=CARTESIAN_POINT('Ctrl Pts',(17.2205940220455,-69.3133014770542,
0.));
#128936=CARTESIAN_POINT('Ctrl Pts',(17.2224672350432,-69.2905157959141,
0.));
#128937=CARTESIAN_POINT('Ctrl Pts',(17.2243139767963,-69.2677732315199,
0.));
#128938=CARTESIAN_POINT('Ctrl Pts',(17.2261343039015,-69.2450739242092,
0.));
#128939=CARTESIAN_POINT('Ctrl Pts',(17.2279282733119,-69.2224180149377,
0.));
#128940=CARTESIAN_POINT('Ctrl Pts',(17.229695942341,-69.1998056452837,0.));
#128941=CARTESIAN_POINT('Ctrl Pts',(17.2314373686705,-69.1772369574462,
0.));
#128942=CARTESIAN_POINT('Ctrl Pts',(17.2331526103511,-69.1547120942542,
0.));
#128943=CARTESIAN_POINT('Ctrl Pts',(17.2348417258017,-69.1322311991759,
0.));
#128944=CARTESIAN_POINT('Ctrl Pts',(17.2365047738125,-69.1097944163244,
0.));
#128945=CARTESIAN_POINT('Ctrl Pts',(17.2381418135489,-69.0874018904598,
0.));
#128946=CARTESIAN_POINT('Ctrl Pts',(17.2397529045587,-69.0650537669859,
0.));
#128947=CARTESIAN_POINT('Ctrl Pts',(17.2413381067722,-69.0427501919636,
0.));
#128948=CARTESIAN_POINT('Ctrl Pts',(17.2428974805043,-69.0204913121226,
0.));
#128949=CARTESIAN_POINT('Ctrl Pts',(17.2444310864585,-68.9982772748694,
0.));
#128950=CARTESIAN_POINT('Ctrl Pts',(17.2459389857327,-68.9761082282922,
0.));
#128951=CARTESIAN_POINT('Ctrl Pts',(17.2474212398275,-68.9539843211618,
0.));
#128952=CARTESIAN_POINT('Ctrl Pts',(17.248877910643,-68.9319057029407,0.));
#128953=CARTESIAN_POINT('Ctrl Pts',(17.2503090604792,-68.9098725237868,
0.));
#128954=CARTESIAN_POINT('Ctrl Pts',(17.2517147520376,-68.8878849345557,
0.));
#128955=CARTESIAN_POINT('Ctrl Pts',(17.2530950484259,-68.8659430867977,
0.));
#128956=CARTESIAN_POINT('Ctrl Pts',(17.2544500131627,-68.8440471327563,
0.));
#128957=CARTESIAN_POINT('Ctrl Pts',(17.2557797101815,-68.8221972253954,
0.));
#128958=CARTESIAN_POINT('Ctrl Pts',(17.2570842038385,-68.8003935184193,
0.));
#128959=CARTESIAN_POINT('Ctrl Pts',(17.2583635589196,-68.7786361662876,
0.));
#128960=CARTESIAN_POINT('Ctrl Pts',(17.2596178406545,-68.7569253242312,
0.));
#128961=CARTESIAN_POINT('Ctrl Pts',(17.2608471147178,-68.7352611482519,
0.));
#128962=CARTESIAN_POINT('Ctrl Pts',(17.2620514472176,-68.7136437951074,
0.));
#128963=CARTESIAN_POINT('Ctrl Pts',(17.263230904689,-68.6920734222932,0.));
#128964=CARTESIAN_POINT('Ctrl Pts',(17.2643855540895,-68.6705501880263,
0.));
#128965=CARTESIAN_POINT('Ctrl Pts',(17.2655154627935,-68.6490742512085,
0.));
#128966=CARTESIAN_POINT('Ctrl Pts',(17.266620698609,-68.6276457714757,0.));
#128967=CARTESIAN_POINT('Ctrl Pts',(17.2677013298061,-68.606264909278,0.));
#128968=CARTESIAN_POINT('Ctrl Pts',(17.2687574251428,-68.5849318259449,
0.));
#128969=CARTESIAN_POINT('Ctrl Pts',(17.2697890538956,-68.5636466837502,
0.));
#128970=CARTESIAN_POINT('Ctrl Pts',(17.2707962858912,-68.5424096459746,
0.));
#128971=CARTESIAN_POINT('Ctrl Pts',(17.2717791914537,-68.5212208767835,
0.));
#128972=CARTESIAN_POINT('Ctrl Pts',(17.2727378413485,-68.5000805410896,
0.));
#128973=CARTESIAN_POINT('Ctrl Pts',(17.2736723067366,-68.4789888044357,
0.));
#128974=CARTESIAN_POINT('Ctrl Pts',(17.2745826591125,-68.4579458328208,
0.));
#128975=CARTESIAN_POINT('Ctrl Pts',(17.2754689703001,-68.4369517926803,
0.));
#128976=CARTESIAN_POINT('Ctrl Pts',(17.2763313126025,-68.4160068512781,
0.));
#128977=CARTESIAN_POINT('Ctrl Pts',(17.2771697589387,-68.3951111770498,
0.));
#128978=CARTESIAN_POINT('Ctrl Pts',(17.2779843829605,-68.374264939895,0.));
#128979=CARTESIAN_POINT('Ctrl Pts',(17.2787752592475,-68.353468311648,0.));
#128980=CARTESIAN_POINT('Ctrl Pts',(17.2795424631789,-68.3327214657533,
0.));
#128981=CARTESIAN_POINT('Ctrl Pts',(17.2802860705807,-68.3120245763884,
0.));
#128982=CARTESIAN_POINT('Ctrl Pts',(17.2810061574352,-68.2913778177258,
0.));
#128983=CARTESIAN_POINT('Ctrl Pts',(17.2817027995838,-68.2707813631761,
0.));
#128984=CARTESIAN_POINT('Ctrl Pts',(17.2823760723886,-68.250235384512,0.));
#128985=CARTESIAN_POINT('Ctrl Pts',(17.2830260513878,-68.2297400535339,
0.));
#128986=CARTESIAN_POINT('Ctrl Pts',(17.2836528130825,-68.2092955440591,
0.));
#128987=CARTESIAN_POINT('Ctrl Pts',(17.2842564355796,-68.1889020335418,
0.));
#128988=CARTESIAN_POINT('Ctrl Pts',(17.2848369995283,-68.1685597054193,
0.));
#128989=CARTESIAN_POINT('Ctrl Pts',(17.2853945882059,-68.1482687493176,
0.));
#128990=CARTESIAN_POINT('Ctrl Pts',(17.2859292855694,-68.1280293561473,
0.));
#128991=CARTESIAN_POINT('Ctrl Pts',(17.2864411745455,-68.1078417137865,
0.));
#128992=CARTESIAN_POINT('Ctrl Pts',(17.2869303355438,-68.0877060033229,
0.));
#128993=CARTESIAN_POINT('Ctrl Pts',(17.2873968440855,-68.0676223930469,
0.));
#128994=CARTESIAN_POINT('Ctrl Pts',(17.2878407730981,-68.0475910442494,
0.));
#128995=CARTESIAN_POINT('Ctrl Pts',(17.2882621974737,-68.027612122741,0.));
#128996=CARTESIAN_POINT('Ctrl Pts',(17.28866119774,-68.007685808115,0.));
#128997=CARTESIAN_POINT('Ctrl Pts',(17.2890378644843,-67.9878123049132,
0.));
#128998=CARTESIAN_POINT('Ctrl Pts',(17.2893923013852,-67.9679918502441,
0.));
#128999=CARTESIAN_POINT('Ctrl Pts',(17.2897246158895,-67.9482246901517,
0.));
#129000=CARTESIAN_POINT('Ctrl Pts',(17.2900349103956,-67.9285110571662,
0.));
#129001=CARTESIAN_POINT('Ctrl Pts',(17.2903232740717,-67.908851149676,0.));
#129002=CARTESIAN_POINT('Ctrl Pts',(17.2905897724029,-67.8892451049871,
0.));
#129003=CARTESIAN_POINT('Ctrl Pts',(17.2908344459816,-67.8696929979178,
0.));
#129004=CARTESIAN_POINT('Ctrl Pts',(17.2910127431203,-67.8540944890057,
0.));
#129005=CARTESIAN_POINT('Ctrl Pts',(17.2911366591419,-67.8424198971214,
0.));
#129006=CARTESIAN_POINT('Ctrl Pts',(17.2912149114145,-67.8346476309106,
0.));
#129007=CARTESIAN_POINT('Ctrl Pts',(17.2912529479484,-67.8307641965655,
0.));
#129008=CARTESIAN_POINT('Ctrl Pts',(10.343287191141,-73.778495580227,0.));
#129009=CARTESIAN_POINT('Ctrl Pts',(10.343287191141,-73.778495580227,12.));
#129010=CARTESIAN_POINT('Ctrl Pts',(10.3449014384453,-73.7731377048058,
0.));
#129011=CARTESIAN_POINT('Ctrl Pts',(10.3449014384453,-73.7731377048058,
12.));
#129012=CARTESIAN_POINT('Ctrl Pts',(10.3481265449342,-73.7624245587789,
0.));
#129013=CARTESIAN_POINT('Ctrl Pts',(10.3481265449342,-73.7624245587789,
12.));
#129014=CARTESIAN_POINT('Ctrl Pts',(10.3529540403092,-73.7463626541854,
0.));
#129015=CARTESIAN_POINT('Ctrl Pts',(10.3529540403092,-73.7463626541854,
12.));
#129016=CARTESIAN_POINT('Ctrl Pts',(10.359370371262,-73.7249624109173,0.));
#129017=CARTESIAN_POINT('Ctrl Pts',(10.359370371262,-73.7249624109173,12.));
#129018=CARTESIAN_POINT('Ctrl Pts',(10.3673568984582,-73.6982381645206,
0.));
#129019=CARTESIAN_POINT('Ctrl Pts',(10.3673568984582,-73.6982381645206,
12.));
#129020=CARTESIAN_POINT('Ctrl Pts',(10.3753095356342,-73.6715399947839,
0.));
#129021=CARTESIAN_POINT('Ctrl Pts',(10.3753095356342,-73.6715399947839,
12.));
#129022=CARTESIAN_POINT('Ctrl Pts',(10.3832282820371,-73.6448679350696,
0.));
#129023=CARTESIAN_POINT('Ctrl Pts',(10.3832282820371,-73.6448679350696,
12.));
#129024=CARTESIAN_POINT('Ctrl Pts',(10.3911131417463,-73.6182220363156,
0.));
#129025=CARTESIAN_POINT('Ctrl Pts',(10.3911131417463,-73.6182220363156,
12.));
#129026=CARTESIAN_POINT('Ctrl Pts',(10.3989641265285,-73.5916023719713,
0.));
#129027=CARTESIAN_POINT('Ctrl Pts',(10.3989641265285,-73.5916023719713,
12.));
#129028=CARTESIAN_POINT('Ctrl Pts',(10.406781255551,-73.5650090359839,0.));
#129029=CARTESIAN_POINT('Ctrl Pts',(10.406781255551,-73.5650090359839,12.));
#129030=CARTESIAN_POINT('Ctrl Pts',(10.414564552681,-73.5384421354543,0.));
#129031=CARTESIAN_POINT('Ctrl Pts',(10.414564552681,-73.5384421354543,12.));
#129032=CARTESIAN_POINT('Ctrl Pts',(10.4223140444605,-73.5119017847575,
0.));
#129033=CARTESIAN_POINT('Ctrl Pts',(10.4223140444605,-73.5119017847575,
12.));
#129034=CARTESIAN_POINT('Ctrl Pts',(10.430029757865,-73.485388099225,0.));
#129035=CARTESIAN_POINT('Ctrl Pts',(10.430029757865,-73.485388099225,12.));
#129036=CARTESIAN_POINT('Ctrl Pts',(10.4377117180222,-73.4589011886197,
0.));
#129037=CARTESIAN_POINT('Ctrl Pts',(10.4377117180222,-73.4589011886197,
12.));
#129038=CARTESIAN_POINT('Ctrl Pts',(10.4453599463547,-73.4324411518554,
0.));
#129039=CARTESIAN_POINT('Ctrl Pts',(10.4453599463547,-73.4324411518554,
12.));
#129040=CARTESIAN_POINT('Ctrl Pts',(10.452974461845,-73.4060080806686,0.));
#129041=CARTESIAN_POINT('Ctrl Pts',(10.452974461845,-73.4060080806686,12.));
#129042=CARTESIAN_POINT('Ctrl Pts',(10.4605552819397,-73.37960206225,0.));
#129043=CARTESIAN_POINT('Ctrl Pts',(10.4605552819397,-73.37960206225,12.));
#129044=CARTESIAN_POINT('Ctrl Pts',(10.4681024236289,-73.3532231823659,
0.));
#129045=CARTESIAN_POINT('Ctrl Pts',(10.4681024236289,-73.3532231823659,
12.));
#129046=CARTESIAN_POINT('Ctrl Pts',(10.4756159043806,-73.3268715280575,
0.));
#129047=CARTESIAN_POINT('Ctrl Pts',(10.4756159043806,-73.3268715280575,
12.));
#129048=CARTESIAN_POINT('Ctrl Pts',(10.4830957433305,-73.3005471910583,
0.));
#129049=CARTESIAN_POINT('Ctrl Pts',(10.4830957433305,-73.3005471910583,
12.));
#129050=CARTESIAN_POINT('Ctrl Pts',(10.4905419611523,-73.2742502674304,
0.));
#129051=CARTESIAN_POINT('Ctrl Pts',(10.4905419611523,-73.2742502674304,
12.));
#129052=CARTESIAN_POINT('Ctrl Pts',(10.4979545795192,-73.2479808560189,
0.));
#129053=CARTESIAN_POINT('Ctrl Pts',(10.4979545795192,-73.2479808560189,
12.));
#129054=CARTESIAN_POINT('Ctrl Pts',(10.5053336206908,-73.2217390572562,
0.));
#129055=CARTESIAN_POINT('Ctrl Pts',(10.5053336206908,-73.2217390572562,
12.));
#129056=CARTESIAN_POINT('Ctrl Pts',(10.5126791070805,-73.1955249719048,
0.));
#129057=CARTESIAN_POINT('Ctrl Pts',(10.5126791070805,-73.1955249719048,
12.));
#129058=CARTESIAN_POINT('Ctrl Pts',(10.5199910607654,-73.1693386996138,
0.));
#129059=CARTESIAN_POINT('Ctrl Pts',(10.5199910607654,-73.1693386996138,
12.));
#129060=CARTESIAN_POINT('Ctrl Pts',(10.5272695032653,-73.1431803382711,
0.));
#129061=CARTESIAN_POINT('Ctrl Pts',(10.5272695032653,-73.1431803382711,
12.));
#129062=CARTESIAN_POINT('Ctrl Pts',(10.53451445581,-73.1170499848039,0.));
#129063=CARTESIAN_POINT('Ctrl Pts',(10.53451445581,-73.1170499848039,12.));
#129064=CARTESIAN_POINT('Ctrl Pts',(10.5417259395002,-73.0909477356474,
0.));
#129065=CARTESIAN_POINT('Ctrl Pts',(10.5417259395002,-73.0909477356474,
12.));
#129066=CARTESIAN_POINT('Ctrl Pts',(10.5489039755138,-73.0648736873434,
0.));
#129067=CARTESIAN_POINT('Ctrl Pts',(10.5489039755138,-73.0648736873434,
12.));
#129068=CARTESIAN_POINT('Ctrl Pts',(10.5560485852974,-73.0388279370834,
0.));
#129069=CARTESIAN_POINT('Ctrl Pts',(10.5560485852974,-73.0388279370834,
12.));
#129070=CARTESIAN_POINT('Ctrl Pts',(10.5631597907651,-73.0128105832621,
0.));
#129071=CARTESIAN_POINT('Ctrl Pts',(10.5631597907651,-73.0128105832621,
12.));
#129072=CARTESIAN_POINT('Ctrl Pts',(10.570237614205,-72.9868217252283,0.));
#129073=CARTESIAN_POINT('Ctrl Pts',(10.570237614205,-72.9868217252283,12.));
#129074=CARTESIAN_POINT('Ctrl Pts',(10.5772820781958,-72.9608614630534,
0.));
#129075=CARTESIAN_POINT('Ctrl Pts',(10.5772820781958,-72.9608614630534,
12.));
#129076=CARTESIAN_POINT('Ctrl Pts',(10.5842932055209,-72.9349298972822,
0.));
#129077=CARTESIAN_POINT('Ctrl Pts',(10.5842932055209,-72.9349298972822,
12.));
#129078=CARTESIAN_POINT('Ctrl Pts',(10.5912710190928,-72.9090271287083,
0.));
#129079=CARTESIAN_POINT('Ctrl Pts',(10.5912710190928,-72.9090271287083,
12.));
#129080=CARTESIAN_POINT('Ctrl Pts',(10.5982155418626,-72.8831532580845,
0.));
#129081=CARTESIAN_POINT('Ctrl Pts',(10.5982155418626,-72.8831532580845,
12.));
#129082=CARTESIAN_POINT('Ctrl Pts',(10.6051267968203,-72.8573083861337,
0.));
#129083=CARTESIAN_POINT('Ctrl Pts',(10.6051267968203,-72.8573083861337,
12.));
#129084=CARTESIAN_POINT('Ctrl Pts',(10.6120048070367,-72.8314926136881,
0.));
#129085=CARTESIAN_POINT('Ctrl Pts',(10.6120048070367,-72.8314926136881,
12.));
#129086=CARTESIAN_POINT('Ctrl Pts',(10.6188495956973,-72.8057060417887,
0.));
#129087=CARTESIAN_POINT('Ctrl Pts',(10.6188495956973,-72.8057060417887,
12.));
#129088=CARTESIAN_POINT('Ctrl Pts',(10.6256611861394,-72.7799487717911,
0.));
#129089=CARTESIAN_POINT('Ctrl Pts',(10.6256611861394,-72.7799487717911,
12.));
#129090=CARTESIAN_POINT('Ctrl Pts',(10.6324396018998,-72.7542209054812,
0.));
#129091=CARTESIAN_POINT('Ctrl Pts',(10.6324396018998,-72.7542209054812,
12.));
#129092=CARTESIAN_POINT('Ctrl Pts',(10.6391848667352,-72.7285225451293,
0.));
#129093=CARTESIAN_POINT('Ctrl Pts',(10.6391848667352,-72.7285225451293,
12.));
#129094=CARTESIAN_POINT('Ctrl Pts',(10.6458970045946,-72.7028537934317,
0.));
#129095=CARTESIAN_POINT('Ctrl Pts',(10.6458970045946,-72.7028537934317,
12.));
#129096=CARTESIAN_POINT('Ctrl Pts',(10.6525760396054,-72.6772147534752,
0.));
#129097=CARTESIAN_POINT('Ctrl Pts',(10.6525760396054,-72.6772147534752,
12.));
#129098=CARTESIAN_POINT('Ctrl Pts',(10.659221996058,-72.651605528691,0.));
#129099=CARTESIAN_POINT('Ctrl Pts',(10.659221996058,-72.651605528691,12.));
#129100=CARTESIAN_POINT('Ctrl Pts',(10.6658348983944,-72.6260262228065,
0.));
#129101=CARTESIAN_POINT('Ctrl Pts',(10.6658348983944,-72.6260262228065,
12.));
#129102=CARTESIAN_POINT('Ctrl Pts',(10.6724147711995,-72.6004769398019,
0.));
#129103=CARTESIAN_POINT('Ctrl Pts',(10.6724147711995,-72.6004769398019,
12.));
#129104=CARTESIAN_POINT('Ctrl Pts',(10.6789616392042,-72.5749577839415,
0.));
#129105=CARTESIAN_POINT('Ctrl Pts',(10.6789616392042,-72.5749577839415,
12.));
#129106=CARTESIAN_POINT('Ctrl Pts',(10.6854755272904,-72.5494688597961,
0.));
#129107=CARTESIAN_POINT('Ctrl Pts',(10.6854755272904,-72.5494688597961,
12.));
#129108=CARTESIAN_POINT('Ctrl Pts',(10.691956460499,-72.5240102722664,0.));
#129109=CARTESIAN_POINT('Ctrl Pts',(10.691956460499,-72.5240102722664,12.));
#129110=CARTESIAN_POINT('Ctrl Pts',(10.6984044640398,-72.4985821266023,
0.));
#129111=CARTESIAN_POINT('Ctrl Pts',(10.6984044640398,-72.4985821266023,
12.));
#129112=CARTESIAN_POINT('Ctrl Pts',(10.7048195633061,-72.4731845284227,
0.));
#129113=CARTESIAN_POINT('Ctrl Pts',(10.7048195633061,-72.4731845284227,
12.));
#129114=CARTESIAN_POINT('Ctrl Pts',(10.7112017838706,-72.4478175837156,
0.));
#129115=CARTESIAN_POINT('Ctrl Pts',(10.7112017838706,-72.4478175837156,
12.));
#129116=CARTESIAN_POINT('Ctrl Pts',(10.7175511514788,-72.4224813988347,
0.));
#129117=CARTESIAN_POINT('Ctrl Pts',(10.7175511514788,-72.4224813988347,
12.));
#129118=CARTESIAN_POINT('Ctrl Pts',(10.7238676920469,-72.3971760804933,
0.));
#129119=CARTESIAN_POINT('Ctrl Pts',(10.7238676920469,-72.3971760804933,
12.));
#129120=CARTESIAN_POINT('Ctrl Pts',(10.7301514316607,-72.3719017357571,
0.));
#129121=CARTESIAN_POINT('Ctrl Pts',(10.7301514316607,-72.3719017357571,
12.));
#129122=CARTESIAN_POINT('Ctrl Pts',(10.73640239658,-72.3466584720318,0.));
#129123=CARTESIAN_POINT('Ctrl Pts',(10.73640239658,-72.3466584720318,12.));
#129124=CARTESIAN_POINT('Ctrl Pts',(10.7426206132375,-72.3214463970641,
0.));
#129125=CARTESIAN_POINT('Ctrl Pts',(10.7426206132375,-72.3214463970641,
12.));
#129126=CARTESIAN_POINT('Ctrl Pts',(10.7488061082367,-72.2962656189556,
0.));
#129127=CARTESIAN_POINT('Ctrl Pts',(10.7488061082367,-72.2962656189556,
12.));
#129128=CARTESIAN_POINT('Ctrl Pts',(10.7549589083535,-72.2711162461681,
0.));
#129129=CARTESIAN_POINT('Ctrl Pts',(10.7549589083535,-72.2711162461681,
12.));
#129130=CARTESIAN_POINT('Ctrl Pts',(10.7610790405385,-72.2459983875296,
0.));
#129131=CARTESIAN_POINT('Ctrl Pts',(10.7610790405385,-72.2459983875296,
12.));
#129132=CARTESIAN_POINT('Ctrl Pts',(10.7671665319255,-72.2209121522366,
0.));
#129133=CARTESIAN_POINT('Ctrl Pts',(10.7671665319255,-72.2209121522366,
12.));
#129134=CARTESIAN_POINT('Ctrl Pts',(10.7732214098344,-72.1958576498558,
0.));
#129135=CARTESIAN_POINT('Ctrl Pts',(10.7732214098344,-72.1958576498558,
12.));
#129136=CARTESIAN_POINT('Ctrl Pts',(10.7792437017662,-72.1708349903305,
0.));
#129137=CARTESIAN_POINT('Ctrl Pts',(10.7792437017662,-72.1708349903305,
12.));
#129138=CARTESIAN_POINT('Ctrl Pts',(10.7852334354016,-72.1458442839834,
0.));
#129139=CARTESIAN_POINT('Ctrl Pts',(10.7852334354016,-72.1458442839834,
12.));
#129140=CARTESIAN_POINT('Ctrl Pts',(10.7911906386027,-72.1208856415171,
0.));
#129141=CARTESIAN_POINT('Ctrl Pts',(10.7911906386027,-72.1208856415171,
12.));
#129142=CARTESIAN_POINT('Ctrl Pts',(10.7971153394166,-72.0959591740114,
0.));
#129143=CARTESIAN_POINT('Ctrl Pts',(10.7971153394166,-72.0959591740114,
12.));
#129144=CARTESIAN_POINT('Ctrl Pts',(10.8030075660808,-72.0710649929202,
0.));
#129145=CARTESIAN_POINT('Ctrl Pts',(10.8030075660808,-72.0710649929202,
12.));
#129146=CARTESIAN_POINT('Ctrl Pts',(10.8088673470184,-72.0462032100815,
0.));
#129147=CARTESIAN_POINT('Ctrl Pts',(10.8088673470184,-72.0462032100815,
12.));
#129148=CARTESIAN_POINT('Ctrl Pts',(10.8146947108375,-72.0213739377223,
0.));
#129149=CARTESIAN_POINT('Ctrl Pts',(10.8146947108375,-72.0213739377223,
12.));
#129150=CARTESIAN_POINT('Ctrl Pts',(10.8204896863328,-71.9965772884619,
0.));
#129151=CARTESIAN_POINT('Ctrl Pts',(10.8204896863328,-71.9965772884619,
12.));
#129152=CARTESIAN_POINT('Ctrl Pts',(10.8262523024897,-71.9718133753127,
0.));
#129153=CARTESIAN_POINT('Ctrl Pts',(10.8262523024897,-71.9718133753127,
12.));
#129154=CARTESIAN_POINT('Ctrl Pts',(10.8319825884918,-71.9470823116785,
0.));
#129155=CARTESIAN_POINT('Ctrl Pts',(10.8319825884918,-71.9470823116785,
12.));
#129156=CARTESIAN_POINT('Ctrl Pts',(10.8376805737159,-71.9223842113625,
0.));
#129157=CARTESIAN_POINT('Ctrl Pts',(10.8376805737159,-71.9223842113625,
12.));
#129158=CARTESIAN_POINT('Ctrl Pts',(10.8433462877311,-71.8977191885725,
0.));
#129159=CARTESIAN_POINT('Ctrl Pts',(10.8433462877311,-71.8977191885725,
12.));
#129160=CARTESIAN_POINT('Ctrl Pts',(10.8489797602997,-71.8730873579224,
0.));
#129161=CARTESIAN_POINT('Ctrl Pts',(10.8489797602997,-71.8730873579224,
12.));
#129162=CARTESIAN_POINT('Ctrl Pts',(10.8545810213799,-71.8484888344339,
0.));
#129163=CARTESIAN_POINT('Ctrl Pts',(10.8545810213799,-71.8484888344339,
12.));
#129164=CARTESIAN_POINT('Ctrl Pts',(10.8601501011332,-71.8239237335331,
0.));
#129165=CARTESIAN_POINT('Ctrl Pts',(10.8601501011332,-71.8239237335331,
12.));
#129166=CARTESIAN_POINT('Ctrl Pts',(10.865687029922,-71.7993921710564,0.));
#129167=CARTESIAN_POINT('Ctrl Pts',(10.865687029922,-71.7993921710564,12.));
#129168=CARTESIAN_POINT('Ctrl Pts',(10.8711918383073,-71.7748942632593,
0.));
#129169=CARTESIAN_POINT('Ctrl Pts',(10.8711918383073,-71.7748942632593,
12.));
#129170=CARTESIAN_POINT('Ctrl Pts',(10.8766645570497,-71.7504301268181,
0.));
#129171=CARTESIAN_POINT('Ctrl Pts',(10.8766645570497,-71.7504301268181,
12.));
#129172=CARTESIAN_POINT('Ctrl Pts',(10.882105217112,-71.7259998788328,0.));
#129173=CARTESIAN_POINT('Ctrl Pts',(10.882105217112,-71.7259998788328,12.));
#129174=CARTESIAN_POINT('Ctrl Pts',(10.8875138496671,-71.7016036368236,
0.));
#129175=CARTESIAN_POINT('Ctrl Pts',(10.8875138496671,-71.7016036368236,
12.));
#129176=CARTESIAN_POINT('Ctrl Pts',(10.8928904860964,-71.6772415187364,
0.));
#129177=CARTESIAN_POINT('Ctrl Pts',(10.8928904860964,-71.6772415187364,
12.));
#129178=CARTESIAN_POINT('Ctrl Pts',(10.898235157987,-71.6529136429504,0.));
#129179=CARTESIAN_POINT('Ctrl Pts',(10.898235157987,-71.6529136429504,12.));
#129180=CARTESIAN_POINT('Ctrl Pts',(10.9035478971328,-71.6286201282812,
0.));
#129181=CARTESIAN_POINT('Ctrl Pts',(10.9035478971328,-71.6286201282812,
12.));
#129182=CARTESIAN_POINT('Ctrl Pts',(10.9088287355365,-71.6043610939835,
0.));
#129183=CARTESIAN_POINT('Ctrl Pts',(10.9088287355365,-71.6043610939835,
12.));
#129184=CARTESIAN_POINT('Ctrl Pts',(10.914077705417,-71.5801366597488,0.));
#129185=CARTESIAN_POINT('Ctrl Pts',(10.914077705417,-71.5801366597488,12.));
#129186=CARTESIAN_POINT('Ctrl Pts',(10.91929483921,-71.5559469457091,0.));
#129187=CARTESIAN_POINT('Ctrl Pts',(10.91929483921,-71.5559469457091,12.));
#129188=CARTESIAN_POINT('Ctrl Pts',(10.9244801695642,-71.5317920724459,
0.));
#129189=CARTESIAN_POINT('Ctrl Pts',(10.9244801695642,-71.5317920724459,
12.));
#129190=CARTESIAN_POINT('Ctrl Pts',(10.9296337293424,-71.5076721609937,
0.));
#129191=CARTESIAN_POINT('Ctrl Pts',(10.9296337293424,-71.5076721609937,
12.));
#129192=CARTESIAN_POINT('Ctrl Pts',(10.9347555516235,-71.4835873328423,
0.));
#129193=CARTESIAN_POINT('Ctrl Pts',(10.9347555516235,-71.4835873328423,
12.));
#129194=CARTESIAN_POINT('Ctrl Pts',(10.9398456697095,-71.4595377099351,
0.));
#129195=CARTESIAN_POINT('Ctrl Pts',(10.9398456697095,-71.4595377099351,
12.));
#129196=CARTESIAN_POINT('Ctrl Pts',(10.944904117127,-71.435523414672,0.));
#129197=CARTESIAN_POINT('Ctrl Pts',(10.944904117127,-71.435523414672,12.));
#129198=CARTESIAN_POINT('Ctrl Pts',(10.9499309276236,-71.4115445699194,
0.));
#129199=CARTESIAN_POINT('Ctrl Pts',(10.9499309276236,-71.4115445699194,
12.));
#129200=CARTESIAN_POINT('Ctrl Pts',(10.954926135169,-71.3876012990138,0.));
#129201=CARTESIAN_POINT('Ctrl Pts',(10.954926135169,-71.3876012990138,12.));
#129202=CARTESIAN_POINT('Ctrl Pts',(10.9598897739564,-71.3636937257649,
0.));
#129203=CARTESIAN_POINT('Ctrl Pts',(10.9598897739564,-71.3636937257649,
12.));
#129204=CARTESIAN_POINT('Ctrl Pts',(10.9648218784098,-71.339821974454,0.));
#129205=CARTESIAN_POINT('Ctrl Pts',(10.9648218784098,-71.339821974454,12.));
#129206=CARTESIAN_POINT('Ctrl Pts',(10.969722483186,-71.3159861698358,0.));
#129207=CARTESIAN_POINT('Ctrl Pts',(10.969722483186,-71.3159861698358,12.));
#129208=CARTESIAN_POINT('Ctrl Pts',(10.9745916231709,-71.2921864371491,
0.));
#129209=CARTESIAN_POINT('Ctrl Pts',(10.9745916231709,-71.2921864371491,
12.));
#129210=CARTESIAN_POINT('Ctrl Pts',(10.9794293334805,-71.2684229021207,
0.));
#129211=CARTESIAN_POINT('Ctrl Pts',(10.9794293334805,-71.2684229021207,
12.));
#129212=CARTESIAN_POINT('Ctrl Pts',(10.9842356494627,-71.2446956909687,
0.));
#129213=CARTESIAN_POINT('Ctrl Pts',(10.9842356494627,-71.2446956909687,
12.));
#129214=CARTESIAN_POINT('Ctrl Pts',(10.9890106067039,-71.2210049304014,
0.));
#129215=CARTESIAN_POINT('Ctrl Pts',(10.9890106067039,-71.2210049304014,
12.));
#129216=CARTESIAN_POINT('Ctrl Pts',(10.993754241032,-71.1973507476191,0.));
#129217=CARTESIAN_POINT('Ctrl Pts',(10.993754241032,-71.1973507476191,12.));
#129218=CARTESIAN_POINT('Ctrl Pts',(10.9984665885127,-71.1737332703248,
0.));
#129219=CARTESIAN_POINT('Ctrl Pts',(10.9984665885127,-71.1737332703248,
12.));
#129220=CARTESIAN_POINT('Ctrl Pts',(11.0031476854502,-71.1501526267286,
0.));
#129221=CARTESIAN_POINT('Ctrl Pts',(11.0031476854502,-71.1501526267286,
12.));
#129222=CARTESIAN_POINT('Ctrl Pts',(11.0077975683895,-71.1266089455517,
0.));
#129223=CARTESIAN_POINT('Ctrl Pts',(11.0077975683895,-71.1266089455517,
12.));
#129224=CARTESIAN_POINT('Ctrl Pts',(11.0124162741224,-71.1031023560249,
0.));
#129225=CARTESIAN_POINT('Ctrl Pts',(11.0124162741224,-71.1031023560249,
12.));
#129226=CARTESIAN_POINT('Ctrl Pts',(11.0170038396915,-71.0796329878907,
0.));
#129227=CARTESIAN_POINT('Ctrl Pts',(11.0170038396915,-71.0796329878907,
12.));
#129228=CARTESIAN_POINT('Ctrl Pts',(11.0215603023856,-71.0562009714136,
0.));
#129229=CARTESIAN_POINT('Ctrl Pts',(11.0215603023856,-71.0562009714136,
12.));
#129230=CARTESIAN_POINT('Ctrl Pts',(11.0260856997415,-71.0328064373856,
0.));
#129231=CARTESIAN_POINT('Ctrl Pts',(11.0260856997415,-71.0328064373856,
12.));
#129232=CARTESIAN_POINT('Ctrl Pts',(11.0305800695456,-71.0094495171292,
0.));
#129233=CARTESIAN_POINT('Ctrl Pts',(11.0305800695456,-71.0094495171292,
12.));
#129234=CARTESIAN_POINT('Ctrl Pts',(11.0350434498405,-70.986130342497,0.));
#129235=CARTESIAN_POINT('Ctrl Pts',(11.0350434498405,-70.986130342497,12.));
#129236=CARTESIAN_POINT('Ctrl Pts',(11.0394758789285,-70.9628490458748,
0.));
#129237=CARTESIAN_POINT('Ctrl Pts',(11.0394758789285,-70.9628490458748,
12.));
#129238=CARTESIAN_POINT('Ctrl Pts',(11.0438773953681,-70.9396057601924,
0.));
#129239=CARTESIAN_POINT('Ctrl Pts',(11.0438773953681,-70.9396057601924,
12.));
#129240=CARTESIAN_POINT('Ctrl Pts',(11.048248037975,-70.916400618927,0.));
#129241=CARTESIAN_POINT('Ctrl Pts',(11.048248037975,-70.916400618927,12.));
#129242=CARTESIAN_POINT('Ctrl Pts',(11.0525878458243,-70.8932337561087,
0.));
#129243=CARTESIAN_POINT('Ctrl Pts',(11.0525878458243,-70.8932337561087,
12.));
#129244=CARTESIAN_POINT('Ctrl Pts',(11.0568968582569,-70.8701053063186,
0.));
#129245=CARTESIAN_POINT('Ctrl Pts',(11.0568968582569,-70.8701053063186,
12.));
#129246=CARTESIAN_POINT('Ctrl Pts',(11.0611751148834,-70.8470154046919,
0.));
#129247=CARTESIAN_POINT('Ctrl Pts',(11.0611751148834,-70.8470154046919,
12.));
#129248=CARTESIAN_POINT('Ctrl Pts',(11.0654226555802,-70.8239641869299,
0.));
#129249=CARTESIAN_POINT('Ctrl Pts',(11.0654226555802,-70.8239641869299,
12.));
#129250=CARTESIAN_POINT('Ctrl Pts',(11.0696395204909,-70.8009517893057,
0.));
#129251=CARTESIAN_POINT('Ctrl Pts',(11.0696395204909,-70.8009517893057,
12.));
#129252=CARTESIAN_POINT('Ctrl Pts',(11.073825750029,-70.7779783486677,0.));
#129253=CARTESIAN_POINT('Ctrl Pts',(11.073825750029,-70.7779783486677,12.));
#129254=CARTESIAN_POINT('Ctrl Pts',(11.0779813848846,-70.7550440024384,
0.));
#129255=CARTESIAN_POINT('Ctrl Pts',(11.0779813848846,-70.7550440024384,
12.));
#129256=CARTESIAN_POINT('Ctrl Pts',(11.0821064660269,-70.732148888618,0.));
#129257=CARTESIAN_POINT('Ctrl Pts',(11.0821064660269,-70.732148888618,12.));
#129258=CARTESIAN_POINT('Ctrl Pts',(11.0862010347016,-70.7092931457954,
0.));
#129259=CARTESIAN_POINT('Ctrl Pts',(11.0862010347016,-70.7092931457954,
12.));
#129260=CARTESIAN_POINT('Ctrl Pts',(11.0902651324323,-70.6864769131546,
0.));
#129261=CARTESIAN_POINT('Ctrl Pts',(11.0902651324323,-70.6864769131546,
12.));
#129262=CARTESIAN_POINT('Ctrl Pts',(11.0942988010233,-70.6637003304785,
0.));
#129263=CARTESIAN_POINT('Ctrl Pts',(11.0942988010233,-70.6637003304785,
12.));
#129264=CARTESIAN_POINT('Ctrl Pts',(11.0983020825667,-70.6409635381482,
0.));
#129265=CARTESIAN_POINT('Ctrl Pts',(11.0983020825667,-70.6409635381482,
12.));
#129266=CARTESIAN_POINT('Ctrl Pts',(11.1022750194445,-70.6182666771481,
0.));
#129267=CARTESIAN_POINT('Ctrl Pts',(11.1022750194445,-70.6182666771481,
12.));
#129268=CARTESIAN_POINT('Ctrl Pts',(11.1062176543262,-70.5956098890773,
0.));
#129269=CARTESIAN_POINT('Ctrl Pts',(11.1062176543262,-70.5956098890773,
12.));
#129270=CARTESIAN_POINT('Ctrl Pts',(11.1101300301701,-70.5729933161546,
0.));
#129271=CARTESIAN_POINT('Ctrl Pts',(11.1101300301701,-70.5729933161546,
12.));
#129272=CARTESIAN_POINT('Ctrl Pts',(11.1140121902271,-70.5504171012234,
0.));
#129273=CARTESIAN_POINT('Ctrl Pts',(11.1140121902271,-70.5504171012234,
12.));
#129274=CARTESIAN_POINT('Ctrl Pts',(11.1178641780476,-70.5278813877494,
0.));
#129275=CARTESIAN_POINT('Ctrl Pts',(11.1178641780476,-70.5278813877494,
12.));
#129276=CARTESIAN_POINT('Ctrl Pts',(11.1216860374826,-70.505386319828,0.));
#129277=CARTESIAN_POINT('Ctrl Pts',(11.1216860374826,-70.505386319828,12.));
#129278=CARTESIAN_POINT('Ctrl Pts',(11.1254778126821,-70.4829320421957,
0.));
#129279=CARTESIAN_POINT('Ctrl Pts',(11.1254778126821,-70.4829320421957,
12.));
#129280=CARTESIAN_POINT('Ctrl Pts',(11.1292395480974,-70.4605187002354,
0.));
#129281=CARTESIAN_POINT('Ctrl Pts',(11.1292395480974,-70.4605187002354,
12.));
#129282=CARTESIAN_POINT('Ctrl Pts',(11.1329712884846,-70.4381464399819,
0.));
#129283=CARTESIAN_POINT('Ctrl Pts',(11.1329712884846,-70.4381464399819,
12.));
#129284=CARTESIAN_POINT('Ctrl Pts',(11.1366730789125,-70.4158154081205,
0.));
#129285=CARTESIAN_POINT('Ctrl Pts',(11.1366730789125,-70.4158154081205,
12.));
#129286=CARTESIAN_POINT('Ctrl Pts',(11.1403449647625,-70.393525751996,0.));
#129287=CARTESIAN_POINT('Ctrl Pts',(11.1403449647625,-70.393525751996,12.));
#129288=CARTESIAN_POINT('Ctrl Pts',(11.143986991727,-70.3712776196223,0.));
#129289=CARTESIAN_POINT('Ctrl Pts',(11.143986991727,-70.3712776196223,12.));
#129290=CARTESIAN_POINT('Ctrl Pts',(11.1475992058124,-70.349071159688,0.));
#129291=CARTESIAN_POINT('Ctrl Pts',(11.1475992058124,-70.349071159688,12.));
#129292=CARTESIAN_POINT('Ctrl Pts',(11.1511816533421,-70.326906521559,0.));
#129293=CARTESIAN_POINT('Ctrl Pts',(11.1511816533421,-70.326906521559,12.));
#129294=CARTESIAN_POINT('Ctrl Pts',(11.1547343809646,-70.3047838552756,
0.));
#129295=CARTESIAN_POINT('Ctrl Pts',(11.1547343809646,-70.3047838552756,
12.));
#129296=CARTESIAN_POINT('Ctrl Pts',(11.158257435652,-70.2827033115662,0.));
#129297=CARTESIAN_POINT('Ctrl Pts',(11.158257435652,-70.2827033115662,12.));
#129298=CARTESIAN_POINT('Ctrl Pts',(11.1617508647016,-70.260665041859,0.));
#129299=CARTESIAN_POINT('Ctrl Pts',(11.1617508647016,-70.260665041859,12.));
#129300=CARTESIAN_POINT('Ctrl Pts',(11.1652147157383,-70.2386691982902,
0.));
#129301=CARTESIAN_POINT('Ctrl Pts',(11.1652147157383,-70.2386691982902,
12.));
#129302=CARTESIAN_POINT('Ctrl Pts',(11.168649036721,-70.2167159337094,0.));
#129303=CARTESIAN_POINT('Ctrl Pts',(11.168649036721,-70.2167159337094,12.));
#129304=CARTESIAN_POINT('Ctrl Pts',(11.1720538759499,-70.1948054016816,
0.));
#129305=CARTESIAN_POINT('Ctrl Pts',(11.1720538759499,-70.1948054016816,
12.));
#129306=CARTESIAN_POINT('Ctrl Pts',(11.1754292820631,-70.1729377564954,
0.));
#129307=CARTESIAN_POINT('Ctrl Pts',(11.1754292820631,-70.1729377564954,
12.));
#129308=CARTESIAN_POINT('Ctrl Pts',(11.1787753040363,-70.1511131531672,
0.));
#129309=CARTESIAN_POINT('Ctrl Pts',(11.1787753040363,-70.1511131531672,
12.));
#129310=CARTESIAN_POINT('Ctrl Pts',(11.1820919911846,-70.1293317474432,
0.));
#129311=CARTESIAN_POINT('Ctrl Pts',(11.1820919911846,-70.1293317474432,
12.));
#129312=CARTESIAN_POINT('Ctrl Pts',(11.185379393167,-70.1075936957973,0.));
#129313=CARTESIAN_POINT('Ctrl Pts',(11.185379393167,-70.1075936957973,12.));
#129314=CARTESIAN_POINT('Ctrl Pts',(11.1886375599916,-70.0858991554295,
0.));
#129315=CARTESIAN_POINT('Ctrl Pts',(11.1886375599916,-70.0858991554295,
12.));
#129316=CARTESIAN_POINT('Ctrl Pts',(11.1918665420168,-70.0642482842942,
0.));
#129317=CARTESIAN_POINT('Ctrl Pts',(11.1918665420168,-70.0642482842942,
12.));
#129318=CARTESIAN_POINT('Ctrl Pts',(11.1950663899578,-70.0426412411194,
0.));
#129319=CARTESIAN_POINT('Ctrl Pts',(11.1950663899578,-70.0426412411194,
12.));
#129320=CARTESIAN_POINT('Ctrl Pts',(11.1982371548918,-70.0210781854236,
0.));
#129321=CARTESIAN_POINT('Ctrl Pts',(11.1982371548918,-70.0210781854236,
12.));
#129322=CARTESIAN_POINT('Ctrl Pts',(11.2013788882711,-69.9995592775322,
0.));
#129323=CARTESIAN_POINT('Ctrl Pts',(11.2013788882711,-69.9995592775322,
12.));
#129324=CARTESIAN_POINT('Ctrl Pts',(11.2044916419239,-69.9780846785771,
0.));
#129325=CARTESIAN_POINT('Ctrl Pts',(11.2044916419239,-69.9780846785771,
12.));
#129326=CARTESIAN_POINT('Ctrl Pts',(11.2075754680445,-69.9566545504813,
0.));
#129327=CARTESIAN_POINT('Ctrl Pts',(11.2075754680445,-69.9566545504813,
12.));
#129328=CARTESIAN_POINT('Ctrl Pts',(11.2106304191881,-69.9352690559399,
0.));
#129329=CARTESIAN_POINT('Ctrl Pts',(11.2106304191881,-69.9352690559399,
12.));
#129330=CARTESIAN_POINT('Ctrl Pts',(11.2136565482679,-69.9139283584036,
0.));
#129331=CARTESIAN_POINT('Ctrl Pts',(11.2136565482679,-69.9139283584036,
12.));
#129332=CARTESIAN_POINT('Ctrl Pts',(11.2166539085527,-69.8926326220414,
0.));
#129333=CARTESIAN_POINT('Ctrl Pts',(11.2166539085527,-69.8926326220414,
12.));
#129334=CARTESIAN_POINT('Ctrl Pts',(11.2196225536794,-69.8713820117918,
0.));
#129335=CARTESIAN_POINT('Ctrl Pts',(11.2196225536794,-69.8713820117918,
12.));
#129336=CARTESIAN_POINT('Ctrl Pts',(11.2225625376739,-69.8501766934445,
0.));
#129337=CARTESIAN_POINT('Ctrl Pts',(11.2225625376739,-69.8501766934445,
12.));
#129338=CARTESIAN_POINT('Ctrl Pts',(11.225473914972,-69.8290168337076,0.));
#129339=CARTESIAN_POINT('Ctrl Pts',(11.225473914972,-69.8290168337076,12.));
#129340=CARTESIAN_POINT('Ctrl Pts',(11.2283567404434,-69.8079026002753,
0.));
#129341=CARTESIAN_POINT('Ctrl Pts',(11.2283567404434,-69.8079026002753,
12.));
#129342=CARTESIAN_POINT('Ctrl Pts',(11.2312110694183,-69.7868341618927,
0.));
#129343=CARTESIAN_POINT('Ctrl Pts',(11.2312110694183,-69.7868341618927,
12.));
#129344=CARTESIAN_POINT('Ctrl Pts',(11.2340369576452,-69.7658116882298,
0.));
#129345=CARTESIAN_POINT('Ctrl Pts',(11.2340369576452,-69.7658116882298,
12.));
#129346=CARTESIAN_POINT('Ctrl Pts',(11.236834461247,-69.7448353497394,0.));
#129347=CARTESIAN_POINT('Ctrl Pts',(11.236834461247,-69.7448353497394,12.));
#129348=CARTESIAN_POINT('Ctrl Pts',(11.2396036366861,-69.7239053175362,
0.));
#129349=CARTESIAN_POINT('Ctrl Pts',(11.2396036366861,-69.7239053175362,
12.));
#129350=CARTESIAN_POINT('Ctrl Pts',(11.242344540717,-69.7030217632187,0.));
#129351=CARTESIAN_POINT('Ctrl Pts',(11.242344540717,-69.7030217632187,12.));
#129352=CARTESIAN_POINT('Ctrl Pts',(11.2450572303847,-69.6821848588492,
0.));
#129353=CARTESIAN_POINT('Ctrl Pts',(11.2450572303847,-69.6821848588492,
12.));
#129354=CARTESIAN_POINT('Ctrl Pts',(11.247741763139,-69.6613947773563,0.));
#129355=CARTESIAN_POINT('Ctrl Pts',(11.247741763139,-69.6613947773563,12.));
#129356=CARTESIAN_POINT('Ctrl Pts',(11.2503981969413,-69.6406516928902,
0.));
#129357=CARTESIAN_POINT('Ctrl Pts',(11.2503981969413,-69.6406516928902,
12.));
#129358=CARTESIAN_POINT('Ctrl Pts',(11.2530265903555,-69.6199557811231,
0.));
#129359=CARTESIAN_POINT('Ctrl Pts',(11.2530265903555,-69.6199557811231,
12.));
#129360=CARTESIAN_POINT('Ctrl Pts',(11.255627002701,-69.5993072197355,0.));
#129361=CARTESIAN_POINT('Ctrl Pts',(11.255627002701,-69.5993072197355,12.));
#129362=CARTESIAN_POINT('Ctrl Pts',(11.2581994939534,-69.5787061880815,
0.));
#129363=CARTESIAN_POINT('Ctrl Pts',(11.2581994939534,-69.5787061880815,
12.));
#129364=CARTESIAN_POINT('Ctrl Pts',(11.2607441244697,-69.5581528662846,
0.));
#129365=CARTESIAN_POINT('Ctrl Pts',(11.2607441244697,-69.5581528662846,
12.));
#129366=CARTESIAN_POINT('Ctrl Pts',(11.2632609547629,-69.5376474344768,
0.));
#129367=CARTESIAN_POINT('Ctrl Pts',(11.2632609547629,-69.5376474344768,
12.));
#129368=CARTESIAN_POINT('Ctrl Pts',(11.265750045272,-69.5171900720188,0.));
#129369=CARTESIAN_POINT('Ctrl Pts',(11.265750045272,-69.5171900720188,12.));
#129370=CARTESIAN_POINT('Ctrl Pts',(11.2682114561015,-69.4967809565978,
0.));
#129371=CARTESIAN_POINT('Ctrl Pts',(11.2682114561015,-69.4967809565978,
12.));
#129372=CARTESIAN_POINT('Ctrl Pts',(11.2706452475287,-69.4764202659443,
0.));
#129373=CARTESIAN_POINT('Ctrl Pts',(11.2706452475287,-69.4764202659443,
12.));
#129374=CARTESIAN_POINT('Ctrl Pts',(11.2730514806143,-69.4561081798815,
0.));
#129375=CARTESIAN_POINT('Ctrl Pts',(11.2730514806143,-69.4561081798815,
12.));
#129376=CARTESIAN_POINT('Ctrl Pts',(11.2754302177019,-69.4358448819957,
0.));
#129377=CARTESIAN_POINT('Ctrl Pts',(11.2754302177019,-69.4358448819957,
12.));
#129378=CARTESIAN_POINT('Ctrl Pts',(11.2777815231462,-69.4156305620554,
0.));
#129379=CARTESIAN_POINT('Ctrl Pts',(11.2777815231462,-69.4156305620554,
12.));
#129380=CARTESIAN_POINT('Ctrl Pts',(11.2801054633807,-69.395465416223,0.));
#129381=CARTESIAN_POINT('Ctrl Pts',(11.2801054633807,-69.395465416223,12.));
#129382=CARTESIAN_POINT('Ctrl Pts',(11.2824021054038,-69.375349642,0.));
#129383=CARTESIAN_POINT('Ctrl Pts',(11.2824021054038,-69.375349642,12.));
#129384=CARTESIAN_POINT('Ctrl Pts',(11.2846715154521,-69.3552834337771,
0.));
#129385=CARTESIAN_POINT('Ctrl Pts',(11.2846715154521,-69.3552834337771,
12.));
#129386=CARTESIAN_POINT('Ctrl Pts',(11.2869137578463,-69.3352669789611,
0.));
#129387=CARTESIAN_POINT('Ctrl Pts',(11.2869137578463,-69.3352669789611,
12.));
#129388=CARTESIAN_POINT('Ctrl Pts',(11.2891288931528,-69.315300451784,0.));
#129389=CARTESIAN_POINT('Ctrl Pts',(11.2891288931528,-69.315300451784,12.));
#129390=CARTESIAN_POINT('Ctrl Pts',(11.2913169799642,-69.2953840192792,
0.));
#129391=CARTESIAN_POINT('Ctrl Pts',(11.2913169799642,-69.2953840192792,
12.));
#129392=CARTESIAN_POINT('Ctrl Pts',(11.2934780784361,-69.2755178531534,
0.));
#129393=CARTESIAN_POINT('Ctrl Pts',(11.2934780784361,-69.2755178531534,
12.));
#129394=CARTESIAN_POINT('Ctrl Pts',(11.2956122531375,-69.255702139335,0.));
#129395=CARTESIAN_POINT('Ctrl Pts',(11.2956122531375,-69.255702139335,12.));
#129396=CARTESIAN_POINT('Ctrl Pts',(11.2977195764836,-69.2359370894828,
0.));
#129397=CARTESIAN_POINT('Ctrl Pts',(11.2977195764836,-69.2359370894828,
12.));
#129398=CARTESIAN_POINT('Ctrl Pts',(11.2998001310934,-69.216222948839,0.));
#129399=CARTESIAN_POINT('Ctrl Pts',(11.2998001310934,-69.216222948839,12.));
#129400=CARTESIAN_POINT('Ctrl Pts',(11.3018540025605,-69.1965599718761,
0.));
#129401=CARTESIAN_POINT('Ctrl Pts',(11.3018540025605,-69.1965599718761,
12.));
#129402=CARTESIAN_POINT('Ctrl Pts',(11.3038812726275,-69.1769483991639,
0.));
#129403=CARTESIAN_POINT('Ctrl Pts',(11.3038812726275,-69.1769483991639,
12.));
#129404=CARTESIAN_POINT('Ctrl Pts',(11.3058820128323,-69.1573884361076,
0.));
#129405=CARTESIAN_POINT('Ctrl Pts',(11.3058820128323,-69.1573884361076,
12.));
#129406=CARTESIAN_POINT('Ctrl Pts',(11.3078562764442,-69.137880225198,0.));
#129407=CARTESIAN_POINT('Ctrl Pts',(11.3078562764442,-69.137880225198,12.));
#129408=CARTESIAN_POINT('Ctrl Pts',(11.3098040973799,-69.1184238445065,
0.));
#129409=CARTESIAN_POINT('Ctrl Pts',(11.3098040973799,-69.1184238445065,
12.));
#129410=CARTESIAN_POINT('Ctrl Pts',(11.3113412156741,-69.1029002322497,
0.));
#129411=CARTESIAN_POINT('Ctrl Pts',(11.3113412156741,-69.1029002322497,
12.));
#129412=CARTESIAN_POINT('Ctrl Pts',(11.3124821678849,-69.0912808657051,
0.));
#129413=CARTESIAN_POINT('Ctrl Pts',(11.3124821678849,-69.0912808657051,
12.));
#129414=CARTESIAN_POINT('Ctrl Pts',(11.3132375200184,-69.0835449954486,
0.));
#129415=CARTESIAN_POINT('Ctrl Pts',(11.3132375200184,-69.0835449954486,
12.));
#129416=CARTESIAN_POINT('Ctrl Pts',(11.3136138754165,-69.079679653846,0.));
#129417=CARTESIAN_POINT('Ctrl Pts',(11.3136138754165,-69.079679653846,12.));
#129418=CARTESIAN_POINT('',(11.3136138754165,-69.079679653846,12.));
#129419=CARTESIAN_POINT('Ctrl Pts',(11.3136138754165,-69.079679653846,12.));
#129420=CARTESIAN_POINT('Ctrl Pts',(11.3132375200184,-69.0835449954486,
12.));
#129421=CARTESIAN_POINT('Ctrl Pts',(11.3124821678849,-69.0912808657051,
12.));
#129422=CARTESIAN_POINT('Ctrl Pts',(11.3113412156741,-69.1029002322497,
12.));
#129423=CARTESIAN_POINT('Ctrl Pts',(11.3098040973799,-69.1184238445065,
12.));
#129424=CARTESIAN_POINT('Ctrl Pts',(11.3078562764442,-69.137880225198,12.));
#129425=CARTESIAN_POINT('Ctrl Pts',(11.3058820128323,-69.1573884361076,
12.));
#129426=CARTESIAN_POINT('Ctrl Pts',(11.3038812726275,-69.1769483991639,
12.));
#129427=CARTESIAN_POINT('Ctrl Pts',(11.3018540025605,-69.1965599718761,
12.));
#129428=CARTESIAN_POINT('Ctrl Pts',(11.2998001310934,-69.216222948839,12.));
#129429=CARTESIAN_POINT('Ctrl Pts',(11.2977195764836,-69.2359370894828,
12.));
#129430=CARTESIAN_POINT('Ctrl Pts',(11.2956122531375,-69.255702139335,12.));
#129431=CARTESIAN_POINT('Ctrl Pts',(11.2934780784361,-69.2755178531534,
12.));
#129432=CARTESIAN_POINT('Ctrl Pts',(11.2913169799642,-69.2953840192792,
12.));
#129433=CARTESIAN_POINT('Ctrl Pts',(11.2891288931528,-69.315300451784,12.));
#129434=CARTESIAN_POINT('Ctrl Pts',(11.2869137578463,-69.3352669789611,
12.));
#129435=CARTESIAN_POINT('Ctrl Pts',(11.2846715154521,-69.3552834337771,
12.));
#129436=CARTESIAN_POINT('Ctrl Pts',(11.2824021054038,-69.375349642,12.));
#129437=CARTESIAN_POINT('Ctrl Pts',(11.2801054633807,-69.395465416223,12.));
#129438=CARTESIAN_POINT('Ctrl Pts',(11.2777815231462,-69.4156305620554,
12.));
#129439=CARTESIAN_POINT('Ctrl Pts',(11.2754302177019,-69.4358448819957,
12.));
#129440=CARTESIAN_POINT('Ctrl Pts',(11.2730514806143,-69.4561081798815,
12.));
#129441=CARTESIAN_POINT('Ctrl Pts',(11.2706452475287,-69.4764202659443,
12.));
#129442=CARTESIAN_POINT('Ctrl Pts',(11.2682114561015,-69.4967809565978,
12.));
#129443=CARTESIAN_POINT('Ctrl Pts',(11.265750045272,-69.5171900720188,12.));
#129444=CARTESIAN_POINT('Ctrl Pts',(11.2632609547629,-69.5376474344768,
12.));
#129445=CARTESIAN_POINT('Ctrl Pts',(11.2607441244697,-69.5581528662846,
12.));
#129446=CARTESIAN_POINT('Ctrl Pts',(11.2581994939534,-69.5787061880815,
12.));
#129447=CARTESIAN_POINT('Ctrl Pts',(11.255627002701,-69.5993072197355,12.));
#129448=CARTESIAN_POINT('Ctrl Pts',(11.2530265903555,-69.6199557811231,
12.));
#129449=CARTESIAN_POINT('Ctrl Pts',(11.2503981969413,-69.6406516928902,
12.));
#129450=CARTESIAN_POINT('Ctrl Pts',(11.247741763139,-69.6613947773563,12.));
#129451=CARTESIAN_POINT('Ctrl Pts',(11.2450572303847,-69.6821848588492,
12.));
#129452=CARTESIAN_POINT('Ctrl Pts',(11.242344540717,-69.7030217632187,12.));
#129453=CARTESIAN_POINT('Ctrl Pts',(11.2396036366861,-69.7239053175362,
12.));
#129454=CARTESIAN_POINT('Ctrl Pts',(11.236834461247,-69.7448353497394,12.));
#129455=CARTESIAN_POINT('Ctrl Pts',(11.2340369576452,-69.7658116882298,
12.));
#129456=CARTESIAN_POINT('Ctrl Pts',(11.2312110694183,-69.7868341618927,
12.));
#129457=CARTESIAN_POINT('Ctrl Pts',(11.2283567404434,-69.8079026002753,
12.));
#129458=CARTESIAN_POINT('Ctrl Pts',(11.225473914972,-69.8290168337076,12.));
#129459=CARTESIAN_POINT('Ctrl Pts',(11.2225625376739,-69.8501766934445,
12.));
#129460=CARTESIAN_POINT('Ctrl Pts',(11.2196225536794,-69.8713820117918,
12.));
#129461=CARTESIAN_POINT('Ctrl Pts',(11.2166539085527,-69.8926326220414,
12.));
#129462=CARTESIAN_POINT('Ctrl Pts',(11.2136565482679,-69.9139283584036,
12.));
#129463=CARTESIAN_POINT('Ctrl Pts',(11.2106304191881,-69.9352690559399,
12.));
#129464=CARTESIAN_POINT('Ctrl Pts',(11.2075754680445,-69.9566545504813,
12.));
#129465=CARTESIAN_POINT('Ctrl Pts',(11.2044916419239,-69.9780846785771,
12.));
#129466=CARTESIAN_POINT('Ctrl Pts',(11.2013788882711,-69.9995592775322,
12.));
#129467=CARTESIAN_POINT('Ctrl Pts',(11.1982371548918,-70.0210781854236,
12.));
#129468=CARTESIAN_POINT('Ctrl Pts',(11.1950663899578,-70.0426412411194,
12.));
#129469=CARTESIAN_POINT('Ctrl Pts',(11.1918665420168,-70.0642482842942,
12.));
#129470=CARTESIAN_POINT('Ctrl Pts',(11.1886375599916,-70.0858991554295,
12.));
#129471=CARTESIAN_POINT('Ctrl Pts',(11.185379393167,-70.1075936957973,12.));
#129472=CARTESIAN_POINT('Ctrl Pts',(11.1820919911846,-70.1293317474432,
12.));
#129473=CARTESIAN_POINT('Ctrl Pts',(11.1787753040363,-70.1511131531672,
12.));
#129474=CARTESIAN_POINT('Ctrl Pts',(11.1754292820631,-70.1729377564954,
12.));
#129475=CARTESIAN_POINT('Ctrl Pts',(11.1720538759499,-70.1948054016816,
12.));
#129476=CARTESIAN_POINT('Ctrl Pts',(11.168649036721,-70.2167159337094,12.));
#129477=CARTESIAN_POINT('Ctrl Pts',(11.1652147157383,-70.2386691982902,
12.));
#129478=CARTESIAN_POINT('Ctrl Pts',(11.1617508647016,-70.260665041859,12.));
#129479=CARTESIAN_POINT('Ctrl Pts',(11.158257435652,-70.2827033115662,12.));
#129480=CARTESIAN_POINT('Ctrl Pts',(11.1547343809646,-70.3047838552756,
12.));
#129481=CARTESIAN_POINT('Ctrl Pts',(11.1511816533421,-70.326906521559,12.));
#129482=CARTESIAN_POINT('Ctrl Pts',(11.1475992058124,-70.349071159688,12.));
#129483=CARTESIAN_POINT('Ctrl Pts',(11.143986991727,-70.3712776196223,12.));
#129484=CARTESIAN_POINT('Ctrl Pts',(11.1403449647625,-70.393525751996,12.));
#129485=CARTESIAN_POINT('Ctrl Pts',(11.1366730789125,-70.4158154081205,
12.));
#129486=CARTESIAN_POINT('Ctrl Pts',(11.1329712884846,-70.4381464399819,
12.));
#129487=CARTESIAN_POINT('Ctrl Pts',(11.1292395480974,-70.4605187002354,
12.));
#129488=CARTESIAN_POINT('Ctrl Pts',(11.1254778126821,-70.4829320421957,
12.));
#129489=CARTESIAN_POINT('Ctrl Pts',(11.1216860374826,-70.505386319828,12.));
#129490=CARTESIAN_POINT('Ctrl Pts',(11.1178641780476,-70.5278813877494,
12.));
#129491=CARTESIAN_POINT('Ctrl Pts',(11.1140121902271,-70.5504171012234,
12.));
#129492=CARTESIAN_POINT('Ctrl Pts',(11.1101300301701,-70.5729933161546,
12.));
#129493=CARTESIAN_POINT('Ctrl Pts',(11.1062176543262,-70.5956098890773,
12.));
#129494=CARTESIAN_POINT('Ctrl Pts',(11.1022750194445,-70.6182666771481,
12.));
#129495=CARTESIAN_POINT('Ctrl Pts',(11.0983020825667,-70.6409635381482,
12.));
#129496=CARTESIAN_POINT('Ctrl Pts',(11.0942988010233,-70.6637003304785,
12.));
#129497=CARTESIAN_POINT('Ctrl Pts',(11.0902651324323,-70.6864769131546,
12.));
#129498=CARTESIAN_POINT('Ctrl Pts',(11.0862010347016,-70.7092931457954,
12.));
#129499=CARTESIAN_POINT('Ctrl Pts',(11.0821064660269,-70.732148888618,12.));
#129500=CARTESIAN_POINT('Ctrl Pts',(11.0779813848846,-70.7550440024384,
12.));
#129501=CARTESIAN_POINT('Ctrl Pts',(11.073825750029,-70.7779783486677,12.));
#129502=CARTESIAN_POINT('Ctrl Pts',(11.0696395204909,-70.8009517893057,
12.));
#129503=CARTESIAN_POINT('Ctrl Pts',(11.0654226555802,-70.8239641869299,
12.));
#129504=CARTESIAN_POINT('Ctrl Pts',(11.0611751148834,-70.8470154046919,
12.));
#129505=CARTESIAN_POINT('Ctrl Pts',(11.0568968582569,-70.8701053063186,
12.));
#129506=CARTESIAN_POINT('Ctrl Pts',(11.0525878458243,-70.8932337561087,
12.));
#129507=CARTESIAN_POINT('Ctrl Pts',(11.048248037975,-70.916400618927,12.));
#129508=CARTESIAN_POINT('Ctrl Pts',(11.0438773953681,-70.9396057601924,
12.));
#129509=CARTESIAN_POINT('Ctrl Pts',(11.0394758789285,-70.9628490458748,
12.));
#129510=CARTESIAN_POINT('Ctrl Pts',(11.0350434498405,-70.986130342497,12.));
#129511=CARTESIAN_POINT('Ctrl Pts',(11.0305800695456,-71.0094495171292,
12.));
#129512=CARTESIAN_POINT('Ctrl Pts',(11.0260856997415,-71.0328064373856,
12.));
#129513=CARTESIAN_POINT('Ctrl Pts',(11.0215603023856,-71.0562009714136,
12.));
#129514=CARTESIAN_POINT('Ctrl Pts',(11.0170038396915,-71.0796329878907,
12.));
#129515=CARTESIAN_POINT('Ctrl Pts',(11.0124162741224,-71.1031023560249,
12.));
#129516=CARTESIAN_POINT('Ctrl Pts',(11.0077975683895,-71.1266089455517,
12.));
#129517=CARTESIAN_POINT('Ctrl Pts',(11.0031476854502,-71.1501526267286,
12.));
#129518=CARTESIAN_POINT('Ctrl Pts',(10.9984665885127,-71.1737332703248,
12.));
#129519=CARTESIAN_POINT('Ctrl Pts',(10.993754241032,-71.1973507476191,12.));
#129520=CARTESIAN_POINT('Ctrl Pts',(10.9890106067039,-71.2210049304014,
12.));
#129521=CARTESIAN_POINT('Ctrl Pts',(10.9842356494627,-71.2446956909687,
12.));
#129522=CARTESIAN_POINT('Ctrl Pts',(10.9794293334805,-71.2684229021207,
12.));
#129523=CARTESIAN_POINT('Ctrl Pts',(10.9745916231709,-71.2921864371491,
12.));
#129524=CARTESIAN_POINT('Ctrl Pts',(10.969722483186,-71.3159861698358,12.));
#129525=CARTESIAN_POINT('Ctrl Pts',(10.9648218784098,-71.339821974454,12.));
#129526=CARTESIAN_POINT('Ctrl Pts',(10.9598897739564,-71.3636937257649,
12.));
#129527=CARTESIAN_POINT('Ctrl Pts',(10.954926135169,-71.3876012990138,12.));
#129528=CARTESIAN_POINT('Ctrl Pts',(10.9499309276236,-71.4115445699194,
12.));
#129529=CARTESIAN_POINT('Ctrl Pts',(10.944904117127,-71.435523414672,12.));
#129530=CARTESIAN_POINT('Ctrl Pts',(10.9398456697095,-71.4595377099351,
12.));
#129531=CARTESIAN_POINT('Ctrl Pts',(10.9347555516235,-71.4835873328423,
12.));
#129532=CARTESIAN_POINT('Ctrl Pts',(10.9296337293424,-71.5076721609937,
12.));
#129533=CARTESIAN_POINT('Ctrl Pts',(10.9244801695642,-71.5317920724459,
12.));
#129534=CARTESIAN_POINT('Ctrl Pts',(10.91929483921,-71.5559469457091,12.));
#129535=CARTESIAN_POINT('Ctrl Pts',(10.914077705417,-71.5801366597488,12.));
#129536=CARTESIAN_POINT('Ctrl Pts',(10.9088287355365,-71.6043610939835,
12.));
#129537=CARTESIAN_POINT('Ctrl Pts',(10.9035478971328,-71.6286201282812,
12.));
#129538=CARTESIAN_POINT('Ctrl Pts',(10.898235157987,-71.6529136429504,12.));
#129539=CARTESIAN_POINT('Ctrl Pts',(10.8928904860964,-71.6772415187364,
12.));
#129540=CARTESIAN_POINT('Ctrl Pts',(10.8875138496671,-71.7016036368236,
12.));
#129541=CARTESIAN_POINT('Ctrl Pts',(10.882105217112,-71.7259998788328,12.));
#129542=CARTESIAN_POINT('Ctrl Pts',(10.8766645570497,-71.7504301268181,
12.));
#129543=CARTESIAN_POINT('Ctrl Pts',(10.8711918383073,-71.7748942632593,
12.));
#129544=CARTESIAN_POINT('Ctrl Pts',(10.865687029922,-71.7993921710564,12.));
#129545=CARTESIAN_POINT('Ctrl Pts',(10.8601501011332,-71.8239237335331,
12.));
#129546=CARTESIAN_POINT('Ctrl Pts',(10.8545810213799,-71.8484888344339,
12.));
#129547=CARTESIAN_POINT('Ctrl Pts',(10.8489797602997,-71.8730873579224,
12.));
#129548=CARTESIAN_POINT('Ctrl Pts',(10.8433462877311,-71.8977191885725,
12.));
#129549=CARTESIAN_POINT('Ctrl Pts',(10.8376805737159,-71.9223842113625,
12.));
#129550=CARTESIAN_POINT('Ctrl Pts',(10.8319825884918,-71.9470823116785,
12.));
#129551=CARTESIAN_POINT('Ctrl Pts',(10.8262523024897,-71.9718133753127,
12.));
#129552=CARTESIAN_POINT('Ctrl Pts',(10.8204896863328,-71.9965772884619,
12.));
#129553=CARTESIAN_POINT('Ctrl Pts',(10.8146947108375,-72.0213739377223,
12.));
#129554=CARTESIAN_POINT('Ctrl Pts',(10.8088673470184,-72.0462032100815,
12.));
#129555=CARTESIAN_POINT('Ctrl Pts',(10.8030075660808,-72.0710649929202,
12.));
#129556=CARTESIAN_POINT('Ctrl Pts',(10.7971153394166,-72.0959591740114,
12.));
#129557=CARTESIAN_POINT('Ctrl Pts',(10.7911906386027,-72.1208856415171,
12.));
#129558=CARTESIAN_POINT('Ctrl Pts',(10.7852334354016,-72.1458442839834,
12.));
#129559=CARTESIAN_POINT('Ctrl Pts',(10.7792437017662,-72.1708349903305,
12.));
#129560=CARTESIAN_POINT('Ctrl Pts',(10.7732214098344,-72.1958576498558,
12.));
#129561=CARTESIAN_POINT('Ctrl Pts',(10.7671665319255,-72.2209121522366,
12.));
#129562=CARTESIAN_POINT('Ctrl Pts',(10.7610790405385,-72.2459983875296,
12.));
#129563=CARTESIAN_POINT('Ctrl Pts',(10.7549589083535,-72.2711162461681,
12.));
#129564=CARTESIAN_POINT('Ctrl Pts',(10.7488061082367,-72.2962656189556,
12.));
#129565=CARTESIAN_POINT('Ctrl Pts',(10.7426206132375,-72.3214463970641,
12.));
#129566=CARTESIAN_POINT('Ctrl Pts',(10.73640239658,-72.3466584720318,12.));
#129567=CARTESIAN_POINT('Ctrl Pts',(10.7301514316607,-72.3719017357571,
12.));
#129568=CARTESIAN_POINT('Ctrl Pts',(10.7238676920469,-72.3971760804933,
12.));
#129569=CARTESIAN_POINT('Ctrl Pts',(10.7175511514788,-72.4224813988347,
12.));
#129570=CARTESIAN_POINT('Ctrl Pts',(10.7112017838706,-72.4478175837156,
12.));
#129571=CARTESIAN_POINT('Ctrl Pts',(10.7048195633061,-72.4731845284227,
12.));
#129572=CARTESIAN_POINT('Ctrl Pts',(10.6984044640398,-72.4985821266023,
12.));
#129573=CARTESIAN_POINT('Ctrl Pts',(10.691956460499,-72.5240102722664,12.));
#129574=CARTESIAN_POINT('Ctrl Pts',(10.6854755272904,-72.5494688597961,
12.));
#129575=CARTESIAN_POINT('Ctrl Pts',(10.6789616392042,-72.5749577839415,
12.));
#129576=CARTESIAN_POINT('Ctrl Pts',(10.6724147711995,-72.6004769398019,
12.));
#129577=CARTESIAN_POINT('Ctrl Pts',(10.6658348983944,-72.6260262228065,
12.));
#129578=CARTESIAN_POINT('Ctrl Pts',(10.659221996058,-72.651605528691,12.));
#129579=CARTESIAN_POINT('Ctrl Pts',(10.6525760396054,-72.6772147534752,
12.));
#129580=CARTESIAN_POINT('Ctrl Pts',(10.6458970045946,-72.7028537934317,
12.));
#129581=CARTESIAN_POINT('Ctrl Pts',(10.6391848667352,-72.7285225451293,
12.));
#129582=CARTESIAN_POINT('Ctrl Pts',(10.6324396018998,-72.7542209054812,
12.));
#129583=CARTESIAN_POINT('Ctrl Pts',(10.6256611861394,-72.7799487717911,
12.));
#129584=CARTESIAN_POINT('Ctrl Pts',(10.6188495956973,-72.8057060417887,
12.));
#129585=CARTESIAN_POINT('Ctrl Pts',(10.6120048070367,-72.8314926136881,
12.));
#129586=CARTESIAN_POINT('Ctrl Pts',(10.6051267968203,-72.8573083861337,
12.));
#129587=CARTESIAN_POINT('Ctrl Pts',(10.5982155418626,-72.8831532580845,
12.));
#129588=CARTESIAN_POINT('Ctrl Pts',(10.5912710190928,-72.9090271287083,
12.));
#129589=CARTESIAN_POINT('Ctrl Pts',(10.5842932055209,-72.9349298972822,
12.));
#129590=CARTESIAN_POINT('Ctrl Pts',(10.5772820781958,-72.9608614630534,
12.));
#129591=CARTESIAN_POINT('Ctrl Pts',(10.570237614205,-72.9868217252283,12.));
#129592=CARTESIAN_POINT('Ctrl Pts',(10.5631597907651,-73.0128105832621,
12.));
#129593=CARTESIAN_POINT('Ctrl Pts',(10.5560485852974,-73.0388279370834,
12.));
#129594=CARTESIAN_POINT('Ctrl Pts',(10.5489039755138,-73.0648736873434,
12.));
#129595=CARTESIAN_POINT('Ctrl Pts',(10.5417259395002,-73.0909477356474,
12.));
#129596=CARTESIAN_POINT('Ctrl Pts',(10.53451445581,-73.1170499848039,12.));
#129597=CARTESIAN_POINT('Ctrl Pts',(10.5272695032653,-73.1431803382711,
12.));
#129598=CARTESIAN_POINT('Ctrl Pts',(10.5199910607654,-73.1693386996138,
12.));
#129599=CARTESIAN_POINT('Ctrl Pts',(10.5126791070805,-73.1955249719048,
12.));
#129600=CARTESIAN_POINT('Ctrl Pts',(10.5053336206908,-73.2217390572562,
12.));
#129601=CARTESIAN_POINT('Ctrl Pts',(10.4979545795192,-73.2479808560189,
12.));
#129602=CARTESIAN_POINT('Ctrl Pts',(10.4905419611523,-73.2742502674304,
12.));
#129603=CARTESIAN_POINT('Ctrl Pts',(10.4830957433305,-73.3005471910583,
12.));
#129604=CARTESIAN_POINT('Ctrl Pts',(10.4756159043806,-73.3268715280575,
12.));
#129605=CARTESIAN_POINT('Ctrl Pts',(10.4681024236289,-73.3532231823659,
12.));
#129606=CARTESIAN_POINT('Ctrl Pts',(10.4605552819397,-73.37960206225,12.));
#129607=CARTESIAN_POINT('Ctrl Pts',(10.452974461845,-73.4060080806686,12.));
#129608=CARTESIAN_POINT('Ctrl Pts',(10.4464473465479,-73.4286663448107,
12.));
#129609=CARTESIAN_POINT('Ctrl Pts',(10.4414249334739,-73.44605255288,12.));
#129610=CARTESIAN_POINT('Ctrl Pts',(10.4379221501041,-73.4581547436838,
12.));
#129611=CARTESIAN_POINT('Ctrl Pts',(10.4359488742809,-73.4649650361893,
12.));
#129612=CARTESIAN_POINT('Ctrl Pts',(10.4355099267296,-73.4664795929938,
12.));
#129613=CARTESIAN_POINT('',(11.3136138754165,-69.079679653846,0.));
#129614=CARTESIAN_POINT('',(11.3136138754165,-69.079679653846,0.));
#129615=CARTESIAN_POINT('Ctrl Pts',(10.4355099267296,-73.4664795929938,
0.));
#129616=CARTESIAN_POINT('Ctrl Pts',(10.4359488742809,-73.4649650361893,
0.));
#129617=CARTESIAN_POINT('Ctrl Pts',(10.4379221501041,-73.4581547436838,
0.));
#129618=CARTESIAN_POINT('Ctrl Pts',(10.4414249334739,-73.44605255288,0.));
#129619=CARTESIAN_POINT('Ctrl Pts',(10.4464473465479,-73.4286663448107,
0.));
#129620=CARTESIAN_POINT('Ctrl Pts',(10.452974461845,-73.4060080806686,0.));
#129621=CARTESIAN_POINT('Ctrl Pts',(10.4605552819397,-73.37960206225,0.));
#129622=CARTESIAN_POINT('Ctrl Pts',(10.4681024236289,-73.3532231823659,
0.));
#129623=CARTESIAN_POINT('Ctrl Pts',(10.4756159043806,-73.3268715280575,
0.));
#129624=CARTESIAN_POINT('Ctrl Pts',(10.4830957433305,-73.3005471910583,
0.));
#129625=CARTESIAN_POINT('Ctrl Pts',(10.4905419611523,-73.2742502674304,
0.));
#129626=CARTESIAN_POINT('Ctrl Pts',(10.4979545795192,-73.2479808560189,
0.));
#129627=CARTESIAN_POINT('Ctrl Pts',(10.5053336206908,-73.2217390572562,
0.));
#129628=CARTESIAN_POINT('Ctrl Pts',(10.5126791070805,-73.1955249719048,
0.));
#129629=CARTESIAN_POINT('Ctrl Pts',(10.5199910607654,-73.1693386996138,
0.));
#129630=CARTESIAN_POINT('Ctrl Pts',(10.5272695032653,-73.1431803382711,
0.));
#129631=CARTESIAN_POINT('Ctrl Pts',(10.53451445581,-73.1170499848039,0.));
#129632=CARTESIAN_POINT('Ctrl Pts',(10.5417259395002,-73.0909477356474,
0.));
#129633=CARTESIAN_POINT('Ctrl Pts',(10.5489039755138,-73.0648736873434,
0.));
#129634=CARTESIAN_POINT('Ctrl Pts',(10.5560485852974,-73.0388279370834,
0.));
#129635=CARTESIAN_POINT('Ctrl Pts',(10.5631597907651,-73.0128105832621,
0.));
#129636=CARTESIAN_POINT('Ctrl Pts',(10.570237614205,-72.9868217252283,0.));
#129637=CARTESIAN_POINT('Ctrl Pts',(10.5772820781958,-72.9608614630534,
0.));
#129638=CARTESIAN_POINT('Ctrl Pts',(10.5842932055209,-72.9349298972822,
0.));
#129639=CARTESIAN_POINT('Ctrl Pts',(10.5912710190928,-72.9090271287083,
0.));
#129640=CARTESIAN_POINT('Ctrl Pts',(10.5982155418626,-72.8831532580845,
0.));
#129641=CARTESIAN_POINT('Ctrl Pts',(10.6051267968203,-72.8573083861337,
0.));
#129642=CARTESIAN_POINT('Ctrl Pts',(10.6120048070367,-72.8314926136881,
0.));
#129643=CARTESIAN_POINT('Ctrl Pts',(10.6188495956973,-72.8057060417887,
0.));
#129644=CARTESIAN_POINT('Ctrl Pts',(10.6256611861394,-72.7799487717911,
0.));
#129645=CARTESIAN_POINT('Ctrl Pts',(10.6324396018998,-72.7542209054812,
0.));
#129646=CARTESIAN_POINT('Ctrl Pts',(10.6391848667352,-72.7285225451293,
0.));
#129647=CARTESIAN_POINT('Ctrl Pts',(10.6458970045946,-72.7028537934317,
0.));
#129648=CARTESIAN_POINT('Ctrl Pts',(10.6525760396054,-72.6772147534752,
0.));
#129649=CARTESIAN_POINT('Ctrl Pts',(10.659221996058,-72.651605528691,0.));
#129650=CARTESIAN_POINT('Ctrl Pts',(10.6658348983944,-72.6260262228065,
0.));
#129651=CARTESIAN_POINT('Ctrl Pts',(10.6724147711995,-72.6004769398019,
0.));
#129652=CARTESIAN_POINT('Ctrl Pts',(10.6789616392042,-72.5749577839415,
0.));
#129653=CARTESIAN_POINT('Ctrl Pts',(10.6854755272904,-72.5494688597961,
0.));
#129654=CARTESIAN_POINT('Ctrl Pts',(10.691956460499,-72.5240102722664,0.));
#129655=CARTESIAN_POINT('Ctrl Pts',(10.6984044640398,-72.4985821266023,
0.));
#129656=CARTESIAN_POINT('Ctrl Pts',(10.7048195633061,-72.4731845284227,
0.));
#129657=CARTESIAN_POINT('Ctrl Pts',(10.7112017838706,-72.4478175837156,
0.));
#129658=CARTESIAN_POINT('Ctrl Pts',(10.7175511514788,-72.4224813988347,
0.));
#129659=CARTESIAN_POINT('Ctrl Pts',(10.7238676920469,-72.3971760804933,
0.));
#129660=CARTESIAN_POINT('Ctrl Pts',(10.7301514316607,-72.3719017357571,
0.));
#129661=CARTESIAN_POINT('Ctrl Pts',(10.73640239658,-72.3466584720318,0.));
#129662=CARTESIAN_POINT('Ctrl Pts',(10.7426206132375,-72.3214463970641,
0.));
#129663=CARTESIAN_POINT('Ctrl Pts',(10.7488061082367,-72.2962656189556,
0.));
#129664=CARTESIAN_POINT('Ctrl Pts',(10.7549589083535,-72.2711162461681,
0.));
#129665=CARTESIAN_POINT('Ctrl Pts',(10.7610790405385,-72.2459983875296,
0.));
#129666=CARTESIAN_POINT('Ctrl Pts',(10.7671665319255,-72.2209121522366,
0.));
#129667=CARTESIAN_POINT('Ctrl Pts',(10.7732214098344,-72.1958576498558,
0.));
#129668=CARTESIAN_POINT('Ctrl Pts',(10.7792437017662,-72.1708349903305,
0.));
#129669=CARTESIAN_POINT('Ctrl Pts',(10.7852334354016,-72.1458442839834,
0.));
#129670=CARTESIAN_POINT('Ctrl Pts',(10.7911906386027,-72.1208856415171,
0.));
#129671=CARTESIAN_POINT('Ctrl Pts',(10.7971153394166,-72.0959591740114,
0.));
#129672=CARTESIAN_POINT('Ctrl Pts',(10.8030075660808,-72.0710649929202,
0.));
#129673=CARTESIAN_POINT('Ctrl Pts',(10.8088673470184,-72.0462032100815,
0.));
#129674=CARTESIAN_POINT('Ctrl Pts',(10.8146947108375,-72.0213739377223,
0.));
#129675=CARTESIAN_POINT('Ctrl Pts',(10.8204896863328,-71.9965772884619,
0.));
#129676=CARTESIAN_POINT('Ctrl Pts',(10.8262523024897,-71.9718133753127,
0.));
#129677=CARTESIAN_POINT('Ctrl Pts',(10.8319825884918,-71.9470823116785,
0.));
#129678=CARTESIAN_POINT('Ctrl Pts',(10.8376805737159,-71.9223842113625,
0.));
#129679=CARTESIAN_POINT('Ctrl Pts',(10.8433462877311,-71.8977191885725,
0.));
#129680=CARTESIAN_POINT('Ctrl Pts',(10.8489797602997,-71.8730873579224,
0.));
#129681=CARTESIAN_POINT('Ctrl Pts',(10.8545810213799,-71.8484888344339,
0.));
#129682=CARTESIAN_POINT('Ctrl Pts',(10.8601501011332,-71.8239237335331,
0.));
#129683=CARTESIAN_POINT('Ctrl Pts',(10.865687029922,-71.7993921710564,0.));
#129684=CARTESIAN_POINT('Ctrl Pts',(10.8711918383073,-71.7748942632593,
0.));
#129685=CARTESIAN_POINT('Ctrl Pts',(10.8766645570497,-71.7504301268181,
0.));
#129686=CARTESIAN_POINT('Ctrl Pts',(10.882105217112,-71.7259998788328,0.));
#129687=CARTESIAN_POINT('Ctrl Pts',(10.8875138496671,-71.7016036368236,
0.));
#129688=CARTESIAN_POINT('Ctrl Pts',(10.8928904860964,-71.6772415187364,
0.));
#129689=CARTESIAN_POINT('Ctrl Pts',(10.898235157987,-71.6529136429504,0.));
#129690=CARTESIAN_POINT('Ctrl Pts',(10.9035478971328,-71.6286201282812,
0.));
#129691=CARTESIAN_POINT('Ctrl Pts',(10.9088287355365,-71.6043610939835,
0.));
#129692=CARTESIAN_POINT('Ctrl Pts',(10.914077705417,-71.5801366597488,0.));
#129693=CARTESIAN_POINT('Ctrl Pts',(10.91929483921,-71.5559469457091,0.));
#129694=CARTESIAN_POINT('Ctrl Pts',(10.9244801695642,-71.5317920724459,
0.));
#129695=CARTESIAN_POINT('Ctrl Pts',(10.9296337293424,-71.5076721609937,
0.));
#129696=CARTESIAN_POINT('Ctrl Pts',(10.9347555516235,-71.4835873328423,
0.));
#129697=CARTESIAN_POINT('Ctrl Pts',(10.9398456697095,-71.4595377099351,
0.));
#129698=CARTESIAN_POINT('Ctrl Pts',(10.944904117127,-71.435523414672,0.));
#129699=CARTESIAN_POINT('Ctrl Pts',(10.9499309276236,-71.4115445699194,
0.));
#129700=CARTESIAN_POINT('Ctrl Pts',(10.954926135169,-71.3876012990138,0.));
#129701=CARTESIAN_POINT('Ctrl Pts',(10.9598897739564,-71.3636937257649,
0.));
#129702=CARTESIAN_POINT('Ctrl Pts',(10.9648218784098,-71.339821974454,0.));
#129703=CARTESIAN_POINT('Ctrl Pts',(10.969722483186,-71.3159861698358,0.));
#129704=CARTESIAN_POINT('Ctrl Pts',(10.9745916231709,-71.2921864371491,
0.));
#129705=CARTESIAN_POINT('Ctrl Pts',(10.9794293334805,-71.2684229021207,
0.));
#129706=CARTESIAN_POINT('Ctrl Pts',(10.9842356494627,-71.2446956909687,
0.));
#129707=CARTESIAN_POINT('Ctrl Pts',(10.9890106067039,-71.2210049304014,
0.));
#129708=CARTESIAN_POINT('Ctrl Pts',(10.993754241032,-71.1973507476191,0.));
#129709=CARTESIAN_POINT('Ctrl Pts',(10.9984665885127,-71.1737332703248,
0.));
#129710=CARTESIAN_POINT('Ctrl Pts',(11.0031476854502,-71.1501526267286,
0.));
#129711=CARTESIAN_POINT('Ctrl Pts',(11.0077975683895,-71.1266089455517,
0.));
#129712=CARTESIAN_POINT('Ctrl Pts',(11.0124162741224,-71.1031023560249,
0.));
#129713=CARTESIAN_POINT('Ctrl Pts',(11.0170038396915,-71.0796329878907,
0.));
#129714=CARTESIAN_POINT('Ctrl Pts',(11.0215603023856,-71.0562009714136,
0.));
#129715=CARTESIAN_POINT('Ctrl Pts',(11.0260856997415,-71.0328064373856,
0.));
#129716=CARTESIAN_POINT('Ctrl Pts',(11.0305800695456,-71.0094495171292,
0.));
#129717=CARTESIAN_POINT('Ctrl Pts',(11.0350434498405,-70.986130342497,0.));
#129718=CARTESIAN_POINT('Ctrl Pts',(11.0394758789285,-70.9628490458748,
0.));
#129719=CARTESIAN_POINT('Ctrl Pts',(11.0438773953681,-70.9396057601924,
0.));
#129720=CARTESIAN_POINT('Ctrl Pts',(11.048248037975,-70.916400618927,0.));
#129721=CARTESIAN_POINT('Ctrl Pts',(11.0525878458243,-70.8932337561087,
0.));
#129722=CARTESIAN_POINT('Ctrl Pts',(11.0568968582569,-70.8701053063186,
0.));
#129723=CARTESIAN_POINT('Ctrl Pts',(11.0611751148834,-70.8470154046919,
0.));
#129724=CARTESIAN_POINT('Ctrl Pts',(11.0654226555802,-70.8239641869299,
0.));
#129725=CARTESIAN_POINT('Ctrl Pts',(11.0696395204909,-70.8009517893057,
0.));
#129726=CARTESIAN_POINT('Ctrl Pts',(11.073825750029,-70.7779783486677,0.));
#129727=CARTESIAN_POINT('Ctrl Pts',(11.0779813848846,-70.7550440024384,
0.));
#129728=CARTESIAN_POINT('Ctrl Pts',(11.0821064660269,-70.732148888618,0.));
#129729=CARTESIAN_POINT('Ctrl Pts',(11.0862010347016,-70.7092931457954,
0.));
#129730=CARTESIAN_POINT('Ctrl Pts',(11.0902651324323,-70.6864769131546,
0.));
#129731=CARTESIAN_POINT('Ctrl Pts',(11.0942988010233,-70.6637003304785,
0.));
#129732=CARTESIAN_POINT('Ctrl Pts',(11.0983020825667,-70.6409635381482,
0.));
#129733=CARTESIAN_POINT('Ctrl Pts',(11.1022750194445,-70.6182666771481,
0.));
#129734=CARTESIAN_POINT('Ctrl Pts',(11.1062176543262,-70.5956098890773,
0.));
#129735=CARTESIAN_POINT('Ctrl Pts',(11.1101300301701,-70.5729933161546,
0.));
#129736=CARTESIAN_POINT('Ctrl Pts',(11.1140121902271,-70.5504171012234,
0.));
#129737=CARTESIAN_POINT('Ctrl Pts',(11.1178641780476,-70.5278813877494,
0.));
#129738=CARTESIAN_POINT('Ctrl Pts',(11.1216860374826,-70.505386319828,0.));
#129739=CARTESIAN_POINT('Ctrl Pts',(11.1254778126821,-70.4829320421957,
0.));
#129740=CARTESIAN_POINT('Ctrl Pts',(11.1292395480974,-70.4605187002354,
0.));
#129741=CARTESIAN_POINT('Ctrl Pts',(11.1329712884846,-70.4381464399819,
0.));
#129742=CARTESIAN_POINT('Ctrl Pts',(11.1366730789125,-70.4158154081205,
0.));
#129743=CARTESIAN_POINT('Ctrl Pts',(11.1403449647625,-70.393525751996,0.));
#129744=CARTESIAN_POINT('Ctrl Pts',(11.143986991727,-70.3712776196223,0.));
#129745=CARTESIAN_POINT('Ctrl Pts',(11.1475992058124,-70.349071159688,0.));
#129746=CARTESIAN_POINT('Ctrl Pts',(11.1511816533421,-70.326906521559,0.));
#129747=CARTESIAN_POINT('Ctrl Pts',(11.1547343809646,-70.3047838552756,
0.));
#129748=CARTESIAN_POINT('Ctrl Pts',(11.158257435652,-70.2827033115662,0.));
#129749=CARTESIAN_POINT('Ctrl Pts',(11.1617508647016,-70.260665041859,0.));
#129750=CARTESIAN_POINT('Ctrl Pts',(11.1652147157383,-70.2386691982902,
0.));
#129751=CARTESIAN_POINT('Ctrl Pts',(11.168649036721,-70.2167159337094,0.));
#129752=CARTESIAN_POINT('Ctrl Pts',(11.1720538759499,-70.1948054016816,
0.));
#129753=CARTESIAN_POINT('Ctrl Pts',(11.1754292820631,-70.1729377564954,
0.));
#129754=CARTESIAN_POINT('Ctrl Pts',(11.1787753040363,-70.1511131531672,
0.));
#129755=CARTESIAN_POINT('Ctrl Pts',(11.1820919911846,-70.1293317474432,
0.));
#129756=CARTESIAN_POINT('Ctrl Pts',(11.185379393167,-70.1075936957973,0.));
#129757=CARTESIAN_POINT('Ctrl Pts',(11.1886375599916,-70.0858991554295,
0.));
#129758=CARTESIAN_POINT('Ctrl Pts',(11.1918665420168,-70.0642482842942,
0.));
#129759=CARTESIAN_POINT('Ctrl Pts',(11.1950663899578,-70.0426412411194,
0.));
#129760=CARTESIAN_POINT('Ctrl Pts',(11.1982371548918,-70.0210781854236,
0.));
#129761=CARTESIAN_POINT('Ctrl Pts',(11.2013788882711,-69.9995592775322,
0.));
#129762=CARTESIAN_POINT('Ctrl Pts',(11.2044916419239,-69.9780846785771,
0.));
#129763=CARTESIAN_POINT('Ctrl Pts',(11.2075754680445,-69.9566545504813,
0.));
#129764=CARTESIAN_POINT('Ctrl Pts',(11.2106304191881,-69.9352690559399,
0.));
#129765=CARTESIAN_POINT('Ctrl Pts',(11.2136565482679,-69.9139283584036,
0.));
#129766=CARTESIAN_POINT('Ctrl Pts',(11.2166539085527,-69.8926326220414,
0.));
#129767=CARTESIAN_POINT('Ctrl Pts',(11.2196225536794,-69.8713820117918,
0.));
#129768=CARTESIAN_POINT('Ctrl Pts',(11.2225625376739,-69.8501766934445,
0.));
#129769=CARTESIAN_POINT('Ctrl Pts',(11.225473914972,-69.8290168337076,0.));
#129770=CARTESIAN_POINT('Ctrl Pts',(11.2283567404434,-69.8079026002753,
0.));
#129771=CARTESIAN_POINT('Ctrl Pts',(11.2312110694183,-69.7868341618927,
0.));
#129772=CARTESIAN_POINT('Ctrl Pts',(11.2340369576452,-69.7658116882298,
0.));
#129773=CARTESIAN_POINT('Ctrl Pts',(11.236834461247,-69.7448353497394,0.));
#129774=CARTESIAN_POINT('Ctrl Pts',(11.2396036366861,-69.7239053175362,
0.));
#129775=CARTESIAN_POINT('Ctrl Pts',(11.242344540717,-69.7030217632187,0.));
#129776=CARTESIAN_POINT('Ctrl Pts',(11.2450572303847,-69.6821848588492,
0.));
#129777=CARTESIAN_POINT('Ctrl Pts',(11.247741763139,-69.6613947773563,0.));
#129778=CARTESIAN_POINT('Ctrl Pts',(11.2503981969413,-69.6406516928902,
0.));
#129779=CARTESIAN_POINT('Ctrl Pts',(11.2530265903555,-69.6199557811231,
0.));
#129780=CARTESIAN_POINT('Ctrl Pts',(11.255627002701,-69.5993072197355,0.));
#129781=CARTESIAN_POINT('Ctrl Pts',(11.2581994939534,-69.5787061880815,
0.));
#129782=CARTESIAN_POINT('Ctrl Pts',(11.2607441244697,-69.5581528662846,
0.));
#129783=CARTESIAN_POINT('Ctrl Pts',(11.2632609547629,-69.5376474344768,
0.));
#129784=CARTESIAN_POINT('Ctrl Pts',(11.265750045272,-69.5171900720188,0.));
#129785=CARTESIAN_POINT('Ctrl Pts',(11.2682114561015,-69.4967809565978,
0.));
#129786=CARTESIAN_POINT('Ctrl Pts',(11.2706452475287,-69.4764202659443,
0.));
#129787=CARTESIAN_POINT('Ctrl Pts',(11.2730514806143,-69.4561081798815,
0.));
#129788=CARTESIAN_POINT('Ctrl Pts',(11.2754302177019,-69.4358448819957,
0.));
#129789=CARTESIAN_POINT('Ctrl Pts',(11.2777815231462,-69.4156305620554,
0.));
#129790=CARTESIAN_POINT('Ctrl Pts',(11.2801054633807,-69.395465416223,0.));
#129791=CARTESIAN_POINT('Ctrl Pts',(11.2824021054038,-69.375349642,0.));
#129792=CARTESIAN_POINT('Ctrl Pts',(11.2846715154521,-69.3552834337771,
0.));
#129793=CARTESIAN_POINT('Ctrl Pts',(11.2869137578463,-69.3352669789611,
0.));
#129794=CARTESIAN_POINT('Ctrl Pts',(11.2891288931528,-69.315300451784,0.));
#129795=CARTESIAN_POINT('Ctrl Pts',(11.2913169799642,-69.2953840192792,
0.));
#129796=CARTESIAN_POINT('Ctrl Pts',(11.2934780784361,-69.2755178531534,
0.));
#129797=CARTESIAN_POINT('Ctrl Pts',(11.2956122531375,-69.255702139335,0.));
#129798=CARTESIAN_POINT('Ctrl Pts',(11.2977195764836,-69.2359370894828,
0.));
#129799=CARTESIAN_POINT('Ctrl Pts',(11.2998001310934,-69.216222948839,0.));
#129800=CARTESIAN_POINT('Ctrl Pts',(11.3018540025605,-69.1965599718761,
0.));
#129801=CARTESIAN_POINT('Ctrl Pts',(11.3038812726275,-69.1769483991639,
0.));
#129802=CARTESIAN_POINT('Ctrl Pts',(11.3058820128323,-69.1573884361076,
0.));
#129803=CARTESIAN_POINT('Ctrl Pts',(11.3078562764442,-69.137880225198,0.));
#129804=CARTESIAN_POINT('Ctrl Pts',(11.3098040973799,-69.1184238445065,
0.));
#129805=CARTESIAN_POINT('Ctrl Pts',(11.3113412156741,-69.1029002322497,
0.));
#129806=CARTESIAN_POINT('Ctrl Pts',(11.3124821678849,-69.0912808657051,
0.));
#129807=CARTESIAN_POINT('Ctrl Pts',(11.3132375200184,-69.0835449954486,
0.));
#129808=CARTESIAN_POINT('Ctrl Pts',(11.3136138754165,-69.079679653846,0.));
#129809=CARTESIAN_POINT('Ctrl Pts',(3.87370827955543,-74.3992230078037,
0.));
#129810=CARTESIAN_POINT('Ctrl Pts',(3.87370827955543,-74.3992230078037,
12.));
#129811=CARTESIAN_POINT('Ctrl Pts',(3.87578335377324,-74.3940262116388,
0.));
#129812=CARTESIAN_POINT('Ctrl Pts',(3.87578335377324,-74.3940262116388,
12.));
#129813=CARTESIAN_POINT('Ctrl Pts',(3.87992989995746,-74.3836349189184,
0.));
#129814=CARTESIAN_POINT('Ctrl Pts',(3.87992989995746,-74.3836349189184,
12.));
#129815=CARTESIAN_POINT('Ctrl Pts',(3.88613891247983,-74.3680548786661,
0.));
#129816=CARTESIAN_POINT('Ctrl Pts',(3.88613891247983,-74.3680548786661,
12.));
#129817=CARTESIAN_POINT('Ctrl Pts',(3.89439598145328,-74.3472952898745,
0.));
#129818=CARTESIAN_POINT('Ctrl Pts',(3.89439598145328,-74.3472952898745,
12.));
#129819=CARTESIAN_POINT('Ctrl Pts',(3.90468128904633,-74.3213688090134,
0.));
#129820=CARTESIAN_POINT('Ctrl Pts',(3.90468128904633,-74.3213688090134,
12.));
#129821=CARTESIAN_POINT('Ctrl Pts',(3.9149305628503,-74.2954653518728,0.));
#129822=CARTESIAN_POINT('Ctrl Pts',(3.9149305628503,-74.2954653518728,12.));
#129823=CARTESIAN_POINT('Ctrl Pts',(3.92514379920743,-74.2695849516226,
0.));
#129824=CARTESIAN_POINT('Ctrl Pts',(3.92514379920743,-74.2695849516226,
12.));
#129825=CARTESIAN_POINT('Ctrl Pts',(3.93532099774203,-74.2437276593623,
0.));
#129826=CARTESIAN_POINT('Ctrl Pts',(3.93532099774203,-74.2437276593623,
12.));
#129827=CARTESIAN_POINT('Ctrl Pts',(3.9454621637745,-74.2178935492876,0.));
#129828=CARTESIAN_POINT('Ctrl Pts',(3.9454621637745,-74.2178935492876,12.));
#129829=CARTESIAN_POINT('Ctrl Pts',(3.9555673082111,-74.1920827166585,0.));
#129830=CARTESIAN_POINT('Ctrl Pts',(3.9555673082111,-74.1920827166585,12.));
#129831=CARTESIAN_POINT('Ctrl Pts',(3.96563644549385,-74.1662952702485,
0.));
#129832=CARTESIAN_POINT('Ctrl Pts',(3.96563644549385,-74.1662952702485,
12.));
#129833=CARTESIAN_POINT('Ctrl Pts',(3.97566959209528,-74.1405313263109,
0.));
#129834=CARTESIAN_POINT('Ctrl Pts',(3.97566959209528,-74.1405313263109,
12.));
#129835=CARTESIAN_POINT('Ctrl Pts',(3.98566676483641,-74.1147910020891,
0.));
#129836=CARTESIAN_POINT('Ctrl Pts',(3.98566676483641,-74.1147910020891,
12.));
#129837=CARTESIAN_POINT('Ctrl Pts',(3.99562797918286,-74.0890744091186,
0.));
#129838=CARTESIAN_POINT('Ctrl Pts',(3.99562797918286,-74.0890744091186,
12.));
#129839=CARTESIAN_POINT('Ctrl Pts',(4.00555324785479,-74.0633816478037,
0.));
#129840=CARTESIAN_POINT('Ctrl Pts',(4.00555324785479,-74.0633816478037,
12.));
#129841=CARTESIAN_POINT('Ctrl Pts',(4.0154425817671,-74.0377128111863,0.));
#129842=CARTESIAN_POINT('Ctrl Pts',(4.0154425817671,-74.0377128111863,12.));
#129843=CARTESIAN_POINT('Ctrl Pts',(4.02529599070094,-74.012067987646,0.));
#129844=CARTESIAN_POINT('Ctrl Pts',(4.02529599070094,-74.012067987646,12.));
#129845=CARTESIAN_POINT('Ctrl Pts',(4.03511348410659,-73.9864472641033,
0.));
#129846=CARTESIAN_POINT('Ctrl Pts',(4.03511348410659,-73.9864472641033,
12.));
#129847=CARTESIAN_POINT('Ctrl Pts',(4.04489507179957,-73.9608507287909,
0.));
#129848=CARTESIAN_POINT('Ctrl Pts',(4.04489507179957,-73.9608507287909,
12.));
#129849=CARTESIAN_POINT('Ctrl Pts',(4.05464076484751,-73.9352784747608,
0.));
#129850=CARTESIAN_POINT('Ctrl Pts',(4.05464076484751,-73.9352784747608,
12.));
#129851=CARTESIAN_POINT('Ctrl Pts',(4.06435057547324,-73.9097305995115,
0.));
#129852=CARTESIAN_POINT('Ctrl Pts',(4.06435057547324,-73.9097305995115,
12.));
#129853=CARTESIAN_POINT('Ctrl Pts',(4.07402451665244,-73.8842072034008,
0.));
#129854=CARTESIAN_POINT('Ctrl Pts',(4.07402451665244,-73.8842072034008,
12.));
#129855=CARTESIAN_POINT('Ctrl Pts',(4.08366260180674,-73.8587083884191,
0.));
#129856=CARTESIAN_POINT('Ctrl Pts',(4.08366260180674,-73.8587083884191,
12.));
#129857=CARTESIAN_POINT('Ctrl Pts',(4.09326484448232,-73.8332342568989,
0.));
#129858=CARTESIAN_POINT('Ctrl Pts',(4.09326484448232,-73.8332342568989,
12.));
#129859=CARTESIAN_POINT('Ctrl Pts',(4.10283125798728,-73.8077849100342,
0.));
#129860=CARTESIAN_POINT('Ctrl Pts',(4.10283125798728,-73.8077849100342,
12.));
#129861=CARTESIAN_POINT('Ctrl Pts',(4.11236185522786,-73.7823604472159,
0.));
#129862=CARTESIAN_POINT('Ctrl Pts',(4.11236185522786,-73.7823604472159,
12.));
#129863=CARTESIAN_POINT('Ctrl Pts',(4.12185664890556,-73.7569609668528,
0.));
#129864=CARTESIAN_POINT('Ctrl Pts',(4.12185664890556,-73.7569609668528,
12.));
#129865=CARTESIAN_POINT('Ctrl Pts',(4.13131565163577,-73.7315865668522,
0.));
#129866=CARTESIAN_POINT('Ctrl Pts',(4.13131565163577,-73.7315865668522,
12.));
#129867=CARTESIAN_POINT('Ctrl Pts',(4.14073887610152,-73.7062373452342,
0.));
#129868=CARTESIAN_POINT('Ctrl Pts',(4.14073887610152,-73.7062373452342,
12.));
#129869=CARTESIAN_POINT('Ctrl Pts',(4.15012633519722,-73.6809134006897,
0.));
#129870=CARTESIAN_POINT('Ctrl Pts',(4.15012633519722,-73.6809134006897,
12.));
#129871=CARTESIAN_POINT('Ctrl Pts',(4.15947804217783,-73.6556148331489,
0.));
#129872=CARTESIAN_POINT('Ctrl Pts',(4.15947804217783,-73.6556148331489,
12.));
#129873=CARTESIAN_POINT('Ctrl Pts',(4.1687940105878,-73.6303417435251,0.));
#129874=CARTESIAN_POINT('Ctrl Pts',(4.1687940105878,-73.6303417435251,12.));
#129875=CARTESIAN_POINT('Ctrl Pts',(4.17807425419812,-73.6050942334768,
0.));
#129876=CARTESIAN_POINT('Ctrl Pts',(4.17807425419812,-73.6050942334768,
12.));
#129877=CARTESIAN_POINT('Ctrl Pts',(4.18731878694235,-73.5798724051519,
0.));
#129878=CARTESIAN_POINT('Ctrl Pts',(4.18731878694235,-73.5798724051519,
12.));
#129879=CARTESIAN_POINT('Ctrl Pts',(4.19652762286126,-73.5546763609572,
0.));
#129880=CARTESIAN_POINT('Ctrl Pts',(4.19652762286126,-73.5546763609572,
12.));
#129881=CARTESIAN_POINT('Ctrl Pts',(4.20570077603729,-73.5295062032628,
0.));
#129882=CARTESIAN_POINT('Ctrl Pts',(4.20570077603729,-73.5295062032628,
12.));
#129883=CARTESIAN_POINT('Ctrl Pts',(4.2148382605944,-73.5043620344116,0.));
#129884=CARTESIAN_POINT('Ctrl Pts',(4.2148382605944,-73.5043620344116,12.));
#129885=CARTESIAN_POINT('Ctrl Pts',(4.22394009072755,-73.4792439568633,
0.));
#129886=CARTESIAN_POINT('Ctrl Pts',(4.22394009072755,-73.4792439568633,
12.));
#129887=CARTESIAN_POINT('Ctrl Pts',(4.23300628072757,-73.4541520732948,
0.));
#129888=CARTESIAN_POINT('Ctrl Pts',(4.23300628072757,-73.4541520732948,
12.));
#129889=CARTESIAN_POINT('Ctrl Pts',(4.24203684500938,-73.4290864867101,
0.));
#129890=CARTESIAN_POINT('Ctrl Pts',(4.24203684500938,-73.4290864867101,
12.));
#129891=CARTESIAN_POINT('Ctrl Pts',(4.25103179814886,-73.4040473005592,
0.));
#129892=CARTESIAN_POINT('Ctrl Pts',(4.25103179814886,-73.4040473005592,
12.));
#129893=CARTESIAN_POINT('Ctrl Pts',(4.25999115489898,-73.3790346187938,
0.));
#129894=CARTESIAN_POINT('Ctrl Pts',(4.25999115489898,-73.3790346187938,
12.));
#129895=CARTESIAN_POINT('Ctrl Pts',(4.26891493016699,-73.3540485458065,
0.));
#129896=CARTESIAN_POINT('Ctrl Pts',(4.26891493016699,-73.3540485458065,
12.));
#129897=CARTESIAN_POINT('Ctrl Pts',(4.27780313900389,-73.3290891863949,
0.));
#129898=CARTESIAN_POINT('Ctrl Pts',(4.27780313900389,-73.3290891863949,
12.));
#129899=CARTESIAN_POINT('Ctrl Pts',(4.286655796593,-73.3041566457135,0.));
#129900=CARTESIAN_POINT('Ctrl Pts',(4.286655796593,-73.3041566457135,12.));
#129901=CARTESIAN_POINT('Ctrl Pts',(4.29547291824286,-73.2792510292254,
0.));
#129902=CARTESIAN_POINT('Ctrl Pts',(4.29547291824286,-73.2792510292254,
12.));
#129903=CARTESIAN_POINT('Ctrl Pts',(4.30425451938229,-73.2543724426577,
0.));
#129904=CARTESIAN_POINT('Ctrl Pts',(4.30425451938229,-73.2543724426577,
12.));
#129905=CARTESIAN_POINT('Ctrl Pts',(4.31300061556097,-73.2295209920334,
0.));
#129906=CARTESIAN_POINT('Ctrl Pts',(4.31300061556097,-73.2295209920334,
12.));
#129907=CARTESIAN_POINT('Ctrl Pts',(4.32171122245213,-73.204696783694,0.));
#129908=CARTESIAN_POINT('Ctrl Pts',(4.32171122245213,-73.204696783694,12.));
#129909=CARTESIAN_POINT('Ctrl Pts',(4.33038635585876,-73.1798999243235,
0.));
#129910=CARTESIAN_POINT('Ctrl Pts',(4.33038635585876,-73.1798999243235,
12.));
#129911=CARTESIAN_POINT('Ctrl Pts',(4.3390260317214,-73.1551305209685,0.));
#129912=CARTESIAN_POINT('Ctrl Pts',(4.3390260317214,-73.1551305209685,12.));
#129913=CARTESIAN_POINT('Ctrl Pts',(4.34763026613157,-73.130388681059,0.));
#129914=CARTESIAN_POINT('Ctrl Pts',(4.34763026613157,-73.130388681059,12.));
#129915=CARTESIAN_POINT('Ctrl Pts',(4.35619907532719,-73.1056745124087,
0.));
#129916=CARTESIAN_POINT('Ctrl Pts',(4.35619907532719,-73.1056745124087,
12.));
#129917=CARTESIAN_POINT('Ctrl Pts',(4.3647324756864,-73.0809881232103,0.));
#129918=CARTESIAN_POINT('Ctrl Pts',(4.3647324756864,-73.0809881232103,12.));
#129919=CARTESIAN_POINT('Ctrl Pts',(4.37323048372606,-73.0563296220299,
0.));
#129920=CARTESIAN_POINT('Ctrl Pts',(4.37323048372606,-73.0563296220299,
12.));
#129921=CARTESIAN_POINT('Ctrl Pts',(4.3816931161015,-73.0316991177993,0.));
#129922=CARTESIAN_POINT('Ctrl Pts',(4.3816931161015,-73.0316991177993,12.));
#129923=CARTESIAN_POINT('Ctrl Pts',(4.39012038961138,-73.007096719804,0.));
#129924=CARTESIAN_POINT('Ctrl Pts',(4.39012038961138,-73.007096719804,12.));
#129925=CARTESIAN_POINT('Ctrl Pts',(4.39851232119721,-72.9825225376847,
0.));
#129926=CARTESIAN_POINT('Ctrl Pts',(4.39851232119721,-72.9825225376847,
12.));
#129927=CARTESIAN_POINT('Ctrl Pts',(4.40686892793957,-72.95797668145,0.));
#129928=CARTESIAN_POINT('Ctrl Pts',(4.40686892793957,-72.95797668145,12.));
#129929=CARTESIAN_POINT('Ctrl Pts',(4.41519022705921,-72.9334592614829,
0.));
#129930=CARTESIAN_POINT('Ctrl Pts',(4.41519022705921,-72.9334592614829,
12.));
#129931=CARTESIAN_POINT('Ctrl Pts',(4.42347623591941,-72.9089703885462,
0.));
#129932=CARTESIAN_POINT('Ctrl Pts',(4.42347623591941,-72.9089703885462,
12.));
#129933=CARTESIAN_POINT('Ctrl Pts',(4.43172697203349,-72.8845101737855,
0.));
#129934=CARTESIAN_POINT('Ctrl Pts',(4.43172697203349,-72.8845101737855,
12.));
#129935=CARTESIAN_POINT('Ctrl Pts',(4.43994245306817,-72.8600787287318,
0.));
#129936=CARTESIAN_POINT('Ctrl Pts',(4.43994245306817,-72.8600787287318,
12.));
#129937=CARTESIAN_POINT('Ctrl Pts',(4.44812269683737,-72.8356761653069,
0.));
#129938=CARTESIAN_POINT('Ctrl Pts',(4.44812269683737,-72.8356761653069,
12.));
#129939=CARTESIAN_POINT('Ctrl Pts',(4.45626772130145,-72.8113025958262,
0.));
#129940=CARTESIAN_POINT('Ctrl Pts',(4.45626772130145,-72.8113025958262,
12.));
#129941=CARTESIAN_POINT('Ctrl Pts',(4.46437754456792,-72.7869581329994,
0.));
#129942=CARTESIAN_POINT('Ctrl Pts',(4.46437754456792,-72.7869581329994,
12.));
#129943=CARTESIAN_POINT('Ctrl Pts',(4.47245218489609,-72.7626428899281,
0.));
#129944=CARTESIAN_POINT('Ctrl Pts',(4.47245218489609,-72.7626428899281,
12.));
#129945=CARTESIAN_POINT('Ctrl Pts',(4.48049166070205,-72.738356980103,0.));
#129946=CARTESIAN_POINT('Ctrl Pts',(4.48049166070205,-72.738356980103,12.));
#129947=CARTESIAN_POINT('Ctrl Pts',(4.48849599055337,-72.714100517414,0.));
#129948=CARTESIAN_POINT('Ctrl Pts',(4.48849599055337,-72.714100517414,12.));
#129949=CARTESIAN_POINT('Ctrl Pts',(4.49646519316812,-72.6898736161542,
0.));
#129950=CARTESIAN_POINT('Ctrl Pts',(4.49646519316812,-72.6898736161542,
12.));
#129951=CARTESIAN_POINT('Ctrl Pts',(4.50439928741603,-72.6656763910241,
0.));
#129952=CARTESIAN_POINT('Ctrl Pts',(4.50439928741603,-72.6656763910241,
12.));
#129953=CARTESIAN_POINT('Ctrl Pts',(4.51229829232263,-72.6415089571321,
0.));
#129954=CARTESIAN_POINT('Ctrl Pts',(4.51229829232263,-72.6415089571321,
12.));
#129955=CARTESIAN_POINT('Ctrl Pts',(4.52016222707637,-72.6173714299942,
0.));
#129956=CARTESIAN_POINT('Ctrl Pts',(4.52016222707637,-72.6173714299942,
12.));
#129957=CARTESIAN_POINT('Ctrl Pts',(4.52799111102391,-72.5932639255409,
0.));
#129958=CARTESIAN_POINT('Ctrl Pts',(4.52799111102391,-72.5932639255409,
12.));
#129959=CARTESIAN_POINT('Ctrl Pts',(4.53578496366799,-72.5691865601223,
0.));
#129960=CARTESIAN_POINT('Ctrl Pts',(4.53578496366799,-72.5691865601223,
12.));
#129961=CARTESIAN_POINT('Ctrl Pts',(4.54354380466821,-72.5451394505104,
0.));
#129962=CARTESIAN_POINT('Ctrl Pts',(4.54354380466821,-72.5451394505104,
12.));
#129963=CARTESIAN_POINT('Ctrl Pts',(4.55126765384403,-72.5211227139001,
0.));
#129964=CARTESIAN_POINT('Ctrl Pts',(4.55126765384403,-72.5211227139001,
12.));
#129965=CARTESIAN_POINT('Ctrl Pts',(4.5589565311822,-72.4971364679068,0.));
#129966=CARTESIAN_POINT('Ctrl Pts',(4.5589565311822,-72.4971364679068,12.));
#129967=CARTESIAN_POINT('Ctrl Pts',(4.56661045683375,-72.4731808305728,
0.));
#129968=CARTESIAN_POINT('Ctrl Pts',(4.56661045683375,-72.4731808305728,
12.));
#129969=CARTESIAN_POINT('Ctrl Pts',(4.57422945111101,-72.4492559203745,
0.));
#129970=CARTESIAN_POINT('Ctrl Pts',(4.57422945111101,-72.4492559203745,
12.));
#129971=CARTESIAN_POINT('Ctrl Pts',(4.58181353448851,-72.4253618562252,
0.));
#129972=CARTESIAN_POINT('Ctrl Pts',(4.58181353448851,-72.4253618562252,
12.));
#129973=CARTESIAN_POINT('Ctrl Pts',(4.58936272760543,-72.401498757478,0.));
#129974=CARTESIAN_POINT('Ctrl Pts',(4.58936272760543,-72.401498757478,12.));
#129975=CARTESIAN_POINT('Ctrl Pts',(4.59687705127329,-72.3776667439227,
0.));
#129976=CARTESIAN_POINT('Ctrl Pts',(4.59687705127329,-72.3776667439227,
12.));
#129977=CARTESIAN_POINT('Ctrl Pts',(4.60435652647452,-72.3538659357913,
0.));
#129978=CARTESIAN_POINT('Ctrl Pts',(4.60435652647452,-72.3538659357913,
12.));
#129979=CARTESIAN_POINT('Ctrl Pts',(4.61180117435862,-72.3300964537658,
0.));
#129980=CARTESIAN_POINT('Ctrl Pts',(4.61180117435862,-72.3300964537658,
12.));
#129981=CARTESIAN_POINT('Ctrl Pts',(4.61921101624291,-72.3063584189807,
0.));
#129982=CARTESIAN_POINT('Ctrl Pts',(4.61921101624291,-72.3063584189807,
12.));
#129983=CARTESIAN_POINT('Ctrl Pts',(4.62658607361465,-72.2826519530259,
0.));
#129984=CARTESIAN_POINT('Ctrl Pts',(4.62658607361465,-72.2826519530259,
12.));
#129985=CARTESIAN_POINT('Ctrl Pts',(4.63392636813843,-72.2589771779456,
0.));
#129986=CARTESIAN_POINT('Ctrl Pts',(4.63392636813843,-72.2589771779456,
12.));
#129987=CARTESIAN_POINT('Ctrl Pts',(4.64123192165627,-72.2353342162417,
0.));
#129988=CARTESIAN_POINT('Ctrl Pts',(4.64123192165627,-72.2353342162417,
12.));
#129989=CARTESIAN_POINT('Ctrl Pts',(4.64850275618323,-72.2117231908822,
0.));
#129990=CARTESIAN_POINT('Ctrl Pts',(4.64850275618323,-72.2117231908822,
12.));
#129991=CARTESIAN_POINT('Ctrl Pts',(4.65573889390821,-72.1881442253053,
0.));
#129992=CARTESIAN_POINT('Ctrl Pts',(4.65573889390821,-72.1881442253053,
12.));
#129993=CARTESIAN_POINT('Ctrl Pts',(4.66294035719569,-72.1645974434216,
0.));
#129994=CARTESIAN_POINT('Ctrl Pts',(4.66294035719569,-72.1645974434216,
12.));
#129995=CARTESIAN_POINT('Ctrl Pts',(4.67010716859284,-72.1410829696128,
0.));
#129996=CARTESIAN_POINT('Ctrl Pts',(4.67010716859284,-72.1410829696128,
12.));
#129997=CARTESIAN_POINT('Ctrl Pts',(4.67723935083094,-72.1176009287351,
0.));
#129998=CARTESIAN_POINT('Ctrl Pts',(4.67723935083094,-72.1176009287351,
12.));
#129999=CARTESIAN_POINT('Ctrl Pts',(4.68433692682068,-72.0941514461287,
0.));
#130000=CARTESIAN_POINT('Ctrl Pts',(4.68433692682068,-72.0941514461287,
12.));
#130001=CARTESIAN_POINT('Ctrl Pts',(4.69139991965283,-72.0707346476213,
0.));
#130002=CARTESIAN_POINT('Ctrl Pts',(4.69139991965283,-72.0707346476213,
12.));
#130003=CARTESIAN_POINT('Ctrl Pts',(4.69842835259991,-72.0473506595318,
0.));
#130004=CARTESIAN_POINT('Ctrl Pts',(4.69842835259991,-72.0473506595318,
12.));
#130005=CARTESIAN_POINT('Ctrl Pts',(4.705422249123,-72.0239996086686,0.));
#130006=CARTESIAN_POINT('Ctrl Pts',(4.705422249123,-72.0239996086686,12.));
#130007=CARTESIAN_POINT('Ctrl Pts',(4.71238163287396,-72.0006816223325,
0.));
#130008=CARTESIAN_POINT('Ctrl Pts',(4.71238163287396,-72.0006816223325,
12.));
#130009=CARTESIAN_POINT('Ctrl Pts',(4.7193065276907,-71.9773968283259,0.));
#130010=CARTESIAN_POINT('Ctrl Pts',(4.7193065276907,-71.9773968283259,12.));
#130011=CARTESIAN_POINT('Ctrl Pts',(4.72619695759773,-71.9541453549579,
0.));
#130012=CARTESIAN_POINT('Ctrl Pts',(4.72619695759773,-71.9541453549579,
12.));
#130013=CARTESIAN_POINT('Ctrl Pts',(4.73305294680785,-71.9309273310471,
0.));
#130014=CARTESIAN_POINT('Ctrl Pts',(4.73305294680785,-71.9309273310471,
12.));
#130015=CARTESIAN_POINT('Ctrl Pts',(4.73987451972863,-71.9077428859212,
0.));
#130016=CARTESIAN_POINT('Ctrl Pts',(4.73987451972863,-71.9077428859212,
12.));
#130017=CARTESIAN_POINT('Ctrl Pts',(4.74666170096546,-71.8845921494189,
0.));
#130018=CARTESIAN_POINT('Ctrl Pts',(4.74666170096546,-71.8845921494189,
12.));
#130019=CARTESIAN_POINT('Ctrl Pts',(4.75341451531669,-71.8614752519008,
0.));
#130020=CARTESIAN_POINT('Ctrl Pts',(4.75341451531669,-71.8614752519008,
12.));
#130021=CARTESIAN_POINT('Ctrl Pts',(4.76013298777419,-71.8383923242531,
0.));
#130022=CARTESIAN_POINT('Ctrl Pts',(4.76013298777419,-71.8383923242531,
12.));
#130023=CARTESIAN_POINT('Ctrl Pts',(4.76681714352501,-71.8153434978923,
0.));
#130024=CARTESIAN_POINT('Ctrl Pts',(4.76681714352501,-71.8153434978923,
12.));
#130025=CARTESIAN_POINT('Ctrl Pts',(4.77346700795791,-71.7923289047643,
0.));
#130026=CARTESIAN_POINT('Ctrl Pts',(4.77346700795791,-71.7923289047643,
12.));
#130027=CARTESIAN_POINT('Ctrl Pts',(4.78008260666649,-71.769348677346,0.));
#130028=CARTESIAN_POINT('Ctrl Pts',(4.78008260666649,-71.769348677346,12.));
#130029=CARTESIAN_POINT('Ctrl Pts',(4.78666396544457,-71.7464029486563,
0.));
#130030=CARTESIAN_POINT('Ctrl Pts',(4.78666396544457,-71.7464029486563,
12.));
#130031=CARTESIAN_POINT('Ctrl Pts',(4.79321111028675,-71.723491852261,0.));
#130032=CARTESIAN_POINT('Ctrl Pts',(4.79321111028675,-71.723491852261,12.));
#130033=CARTESIAN_POINT('Ctrl Pts',(4.7997240673901,-71.7006155222764,0.));
#130034=CARTESIAN_POINT('Ctrl Pts',(4.7997240673901,-71.7006155222764,12.));
#130035=CARTESIAN_POINT('Ctrl Pts',(4.80620286316074,-71.6777740933687,
0.));
#130036=CARTESIAN_POINT('Ctrl Pts',(4.80620286316074,-71.6777740933687,
12.));
#130037=CARTESIAN_POINT('Ctrl Pts',(4.81264752421712,-71.6549677007582,
0.));
#130038=CARTESIAN_POINT('Ctrl Pts',(4.81264752421712,-71.6549677007582,
12.));
#130039=CARTESIAN_POINT('Ctrl Pts',(4.81905807738541,-71.6321964802297,
0.));
#130040=CARTESIAN_POINT('Ctrl Pts',(4.81905807738541,-71.6321964802297,
12.));
#130041=CARTESIAN_POINT('Ctrl Pts',(4.8254345497002,-71.6094605681353,0.));
#130042=CARTESIAN_POINT('Ctrl Pts',(4.8254345497002,-71.6094605681353,12.));
#130043=CARTESIAN_POINT('Ctrl Pts',(4.83177696840639,-71.5867601014008,
0.));
#130044=CARTESIAN_POINT('Ctrl Pts',(4.83177696840639,-71.5867601014008,
12.));
#130045=CARTESIAN_POINT('Ctrl Pts',(4.83808536096589,-71.5640952175239,
0.));
#130046=CARTESIAN_POINT('Ctrl Pts',(4.83808536096589,-71.5640952175239,
12.));
#130047=CARTESIAN_POINT('Ctrl Pts',(4.84435975506055,-71.5414660545778,
0.));
#130048=CARTESIAN_POINT('Ctrl Pts',(4.84435975506055,-71.5414660545778,
12.));
#130049=CARTESIAN_POINT('Ctrl Pts',(4.85060017858786,-71.5188727512231,
0.));
#130050=CARTESIAN_POINT('Ctrl Pts',(4.85060017858786,-71.5188727512231,
12.));
#130051=CARTESIAN_POINT('Ctrl Pts',(4.85680665966184,-71.4963154467128,
0.));
#130052=CARTESIAN_POINT('Ctrl Pts',(4.85680665966184,-71.4963154467128,
12.));
#130053=CARTESIAN_POINT('Ctrl Pts',(4.86297922661498,-71.4737942808971,
0.));
#130054=CARTESIAN_POINT('Ctrl Pts',(4.86297922661498,-71.4737942808971,
12.));
#130055=CARTESIAN_POINT('Ctrl Pts',(4.86911790800533,-71.4513093942216,
0.));
#130056=CARTESIAN_POINT('Ctrl Pts',(4.86911790800533,-71.4513093942216,
12.));
#130057=CARTESIAN_POINT('Ctrl Pts',(4.8752227326188,-71.4288609277324,0.));
#130058=CARTESIAN_POINT('Ctrl Pts',(4.8752227326188,-71.4288609277324,12.));
#130059=CARTESIAN_POINT('Ctrl Pts',(4.88129372946524,-71.4064490230857,
0.));
#130060=CARTESIAN_POINT('Ctrl Pts',(4.88129372946524,-71.4064490230857,
12.));
#130061=CARTESIAN_POINT('Ctrl Pts',(4.88733092777963,-71.3840738225548,
0.));
#130062=CARTESIAN_POINT('Ctrl Pts',(4.88733092777963,-71.3840738225548,
12.));
#130063=CARTESIAN_POINT('Ctrl Pts',(4.89333435702423,-71.3617354690342,
0.));
#130064=CARTESIAN_POINT('Ctrl Pts',(4.89333435702423,-71.3617354690342,
12.));
#130065=CARTESIAN_POINT('Ctrl Pts',(4.89930404689598,-71.3394341060396,
0.));
#130066=CARTESIAN_POINT('Ctrl Pts',(4.89930404689598,-71.3394341060396,
12.));
#130067=CARTESIAN_POINT('Ctrl Pts',(4.90524002732805,-71.3171698777124,
0.));
#130068=CARTESIAN_POINT('Ctrl Pts',(4.90524002732805,-71.3171698777124,
12.));
#130069=CARTESIAN_POINT('Ctrl Pts',(4.91114232848622,-71.2949429288319,
0.));
#130070=CARTESIAN_POINT('Ctrl Pts',(4.91114232848622,-71.2949429288319,
12.));
#130071=CARTESIAN_POINT('Ctrl Pts',(4.91701098077041,-71.27275340482,0.));
#130072=CARTESIAN_POINT('Ctrl Pts',(4.91701098077041,-71.27275340482,12.));
#130073=CARTESIAN_POINT('Ctrl Pts',(4.92284601481709,-71.2506014517457,
0.));
#130074=CARTESIAN_POINT('Ctrl Pts',(4.92284601481709,-71.2506014517457,
12.));
#130075=CARTESIAN_POINT('Ctrl Pts',(4.9286474615071,-71.2284872163248,0.));
#130076=CARTESIAN_POINT('Ctrl Pts',(4.9286474615071,-71.2284872163248,12.));
#130077=CARTESIAN_POINT('Ctrl Pts',(4.93441535196593,-71.206410845926,0.));
#130078=CARTESIAN_POINT('Ctrl Pts',(4.93441535196593,-71.206410845926,12.));
#130079=CARTESIAN_POINT('Ctrl Pts',(4.94014971756096,-71.184372488583,0.));
#130080=CARTESIAN_POINT('Ctrl Pts',(4.94014971756096,-71.184372488583,12.));
#130081=CARTESIAN_POINT('Ctrl Pts',(4.94585058990336,-71.1623722929998,
0.));
#130082=CARTESIAN_POINT('Ctrl Pts',(4.94585058990336,-71.1623722929998,
12.));
#130083=CARTESIAN_POINT('Ctrl Pts',(4.9515180008511,-71.1404104085561,0.));
#130084=CARTESIAN_POINT('Ctrl Pts',(4.9515180008511,-71.1404104085561,12.));
#130085=CARTESIAN_POINT('Ctrl Pts',(4.95715198251703,-71.1184869853071,
0.));
#130086=CARTESIAN_POINT('Ctrl Pts',(4.95715198251703,-71.1184869853071,
12.));
#130087=CARTESIAN_POINT('Ctrl Pts',(4.96275256726786,-71.0966021739922,
0.));
#130088=CARTESIAN_POINT('Ctrl Pts',(4.96275256726786,-71.0966021739922,
12.));
#130089=CARTESIAN_POINT('Ctrl Pts',(4.96831978772201,-71.0747561260443,
0.));
#130090=CARTESIAN_POINT('Ctrl Pts',(4.96831978772201,-71.0747561260443,
12.));
#130091=CARTESIAN_POINT('Ctrl Pts',(4.97385367675156,-71.0529489935959,
0.));
#130092=CARTESIAN_POINT('Ctrl Pts',(4.97385367675156,-71.0529489935959,
12.));
#130093=CARTESIAN_POINT('Ctrl Pts',(4.97935426748576,-71.031180929482,0.));
#130094=CARTESIAN_POINT('Ctrl Pts',(4.97935426748576,-71.031180929482,12.));
#130095=CARTESIAN_POINT('Ctrl Pts',(4.9848215933185,-71.0094520872375,0.));
#130096=CARTESIAN_POINT('Ctrl Pts',(4.9848215933185,-71.0094520872375,12.));
#130097=CARTESIAN_POINT('Ctrl Pts',(4.99025568790652,-70.9877626211112,
0.));
#130098=CARTESIAN_POINT('Ctrl Pts',(4.99025568790652,-70.9877626211112,
12.));
#130099=CARTESIAN_POINT('Ctrl Pts',(4.99565658516905,-70.9661126860773,
0.));
#130100=CARTESIAN_POINT('Ctrl Pts',(4.99565658516905,-70.9661126860773,
12.));
#130101=CARTESIAN_POINT('Ctrl Pts',(5.00102431929038,-70.9445024378439,
0.));
#130102=CARTESIAN_POINT('Ctrl Pts',(5.00102431929038,-70.9445024378439,
12.));
#130103=CARTESIAN_POINT('Ctrl Pts',(5.00635892472517,-70.9229320328588,
0.));
#130104=CARTESIAN_POINT('Ctrl Pts',(5.00635892472517,-70.9229320328588,
12.));
#130105=CARTESIAN_POINT('Ctrl Pts',(5.01166043620572,-70.9014016283123,
0.));
#130106=CARTESIAN_POINT('Ctrl Pts',(5.01166043620572,-70.9014016283123,
12.));
#130107=CARTESIAN_POINT('Ctrl Pts',(5.01692888873792,-70.8799113821449,
0.));
#130108=CARTESIAN_POINT('Ctrl Pts',(5.01692888873792,-70.8799113821449,
12.));
#130109=CARTESIAN_POINT('Ctrl Pts',(5.02216431760059,-70.8584614530517,
0.));
#130110=CARTESIAN_POINT('Ctrl Pts',(5.02216431760059,-70.8584614530517,
12.));
#130111=CARTESIAN_POINT('Ctrl Pts',(5.0273667583469,-70.8370520004844,0.));
#130112=CARTESIAN_POINT('Ctrl Pts',(5.0273667583469,-70.8370520004844,12.));
#130113=CARTESIAN_POINT('Ctrl Pts',(5.0325362468094,-70.8156831846494,0.));
#130114=CARTESIAN_POINT('Ctrl Pts',(5.0325362468094,-70.8156831846494,12.));
#130115=CARTESIAN_POINT('Ctrl Pts',(5.03767281910483,-70.7943551665071,
0.));
#130116=CARTESIAN_POINT('Ctrl Pts',(5.03767281910483,-70.7943551665071,
12.));
#130117=CARTESIAN_POINT('Ctrl Pts',(5.04277651163356,-70.7730681077997,
0.));
#130118=CARTESIAN_POINT('Ctrl Pts',(5.04277651163356,-70.7730681077997,
12.));
#130119=CARTESIAN_POINT('Ctrl Pts',(5.0478473610835,-70.7518221710715,0.));
#130120=CARTESIAN_POINT('Ctrl Pts',(5.0478473610835,-70.7518221710715,12.));
#130121=CARTESIAN_POINT('Ctrl Pts',(5.05288540443477,-70.7306175196856,
0.));
#130122=CARTESIAN_POINT('Ctrl Pts',(5.05288540443477,-70.7306175196856,
12.));
#130123=CARTESIAN_POINT('Ctrl Pts',(5.0578906789704,-70.7094543178416,0.));
#130124=CARTESIAN_POINT('Ctrl Pts',(5.0578906789704,-70.7094543178416,12.));
#130125=CARTESIAN_POINT('Ctrl Pts',(5.06286322227796,-70.6883327305755,
0.));
#130126=CARTESIAN_POINT('Ctrl Pts',(5.06286322227796,-70.6883327305755,
12.));
#130127=CARTESIAN_POINT('Ctrl Pts',(5.06780307224052,-70.6672529237431,
0.));
#130128=CARTESIAN_POINT('Ctrl Pts',(5.06780307224052,-70.6672529237431,
12.));
#130129=CARTESIAN_POINT('Ctrl Pts',(5.07271026703349,-70.6462150640009,
0.));
#130130=CARTESIAN_POINT('Ctrl Pts',(5.07271026703349,-70.6462150640009,
12.));
#130131=CARTESIAN_POINT('Ctrl Pts',(5.07758484512309,-70.6252193187892,
0.));
#130132=CARTESIAN_POINT('Ctrl Pts',(5.07758484512309,-70.6252193187892,
12.));
#130133=CARTESIAN_POINT('Ctrl Pts',(5.08242684526703,-70.6042658562951,
0.));
#130134=CARTESIAN_POINT('Ctrl Pts',(5.08242684526703,-70.6042658562951,
12.));
#130135=CARTESIAN_POINT('Ctrl Pts',(5.0872363065229,-70.5833548455043,0.));
#130136=CARTESIAN_POINT('Ctrl Pts',(5.0872363065229,-70.5833548455043,12.));
#130137=CARTESIAN_POINT('Ctrl Pts',(5.09201326826145,-70.5624864562841,
0.));
#130138=CARTESIAN_POINT('Ctrl Pts',(5.09201326826145,-70.5624864562841,
12.));
#130139=CARTESIAN_POINT('Ctrl Pts',(5.09675777018181,-70.5416608594526,
0.));
#130140=CARTESIAN_POINT('Ctrl Pts',(5.09675777018181,-70.5416608594526,
12.));
#130141=CARTESIAN_POINT('Ctrl Pts',(5.10146985232927,-70.5208782268482,
0.));
#130142=CARTESIAN_POINT('Ctrl Pts',(5.10146985232927,-70.5208782268482,
12.));
#130143=CARTESIAN_POINT('Ctrl Pts',(5.10614955511642,-70.5001387313963,
0.));
#130144=CARTESIAN_POINT('Ctrl Pts',(5.10614955511642,-70.5001387313963,
12.));
#130145=CARTESIAN_POINT('Ctrl Pts',(5.11079691929192,-70.4794425469799,
0.));
#130146=CARTESIAN_POINT('Ctrl Pts',(5.11079691929192,-70.4794425469799,
12.));
#130147=CARTESIAN_POINT('Ctrl Pts',(5.11541198590919,-70.4587898482946,
0.));
#130148=CARTESIAN_POINT('Ctrl Pts',(5.11541198590919,-70.4587898482946,
12.));
#130149=CARTESIAN_POINT('Ctrl Pts',(5.11999479630214,-70.438180810725,0.));
#130150=CARTESIAN_POINT('Ctrl Pts',(5.11999479630214,-70.438180810725,12.));
#130151=CARTESIAN_POINT('Ctrl Pts',(5.12454539205346,-70.4176156101633,
0.));
#130152=CARTESIAN_POINT('Ctrl Pts',(5.12454539205346,-70.4176156101633,
12.));
#130153=CARTESIAN_POINT('Ctrl Pts',(5.12906381499485,-70.3970944229885,
0.));
#130154=CARTESIAN_POINT('Ctrl Pts',(5.12906381499485,-70.3970944229885,
12.));
#130155=CARTESIAN_POINT('Ctrl Pts',(5.1335501072859,-70.3766174264786,0.));
#130156=CARTESIAN_POINT('Ctrl Pts',(5.1335501072859,-70.3766174264786,12.));
#130157=CARTESIAN_POINT('Ctrl Pts',(5.1380043114891,-70.3561847991725,0.));
#130158=CARTESIAN_POINT('Ctrl Pts',(5.1380043114891,-70.3561847991725,12.));
#130159=CARTESIAN_POINT('Ctrl Pts',(5.14242647063466,-70.3357967211782,
0.));
#130160=CARTESIAN_POINT('Ctrl Pts',(5.14242647063466,-70.3357967211782,
12.));
#130161=CARTESIAN_POINT('Ctrl Pts',(5.14681662833053,-70.31545337467,0.));
#130162=CARTESIAN_POINT('Ctrl Pts',(5.14681662833053,-70.31545337467,12.));
#130163=CARTESIAN_POINT('Ctrl Pts',(5.15117482869224,-70.2951549435469,
0.));
#130164=CARTESIAN_POINT('Ctrl Pts',(5.15117482869224,-70.2951549435469,
12.));
#130165=CARTESIAN_POINT('Ctrl Pts',(5.15550111614837,-70.2749016125073,
0.));
#130166=CARTESIAN_POINT('Ctrl Pts',(5.15550111614837,-70.2749016125073,
12.));
#130167=CARTESIAN_POINT('Ctrl Pts',(5.159795535282,-70.2546935662719,0.));
#130168=CARTESIAN_POINT('Ctrl Pts',(5.159795535282,-70.2546935662719,12.));
#130169=CARTESIAN_POINT('Ctrl Pts',(5.16405813066993,-70.2345309887864,
0.));
#130170=CARTESIAN_POINT('Ctrl Pts',(5.16405813066993,-70.2345309887864,
12.));
#130171=CARTESIAN_POINT('Ctrl Pts',(5.16828894670139,-70.2144140623004,
0.));
#130172=CARTESIAN_POINT('Ctrl Pts',(5.16828894670139,-70.2144140623004,
12.));
#130173=CARTESIAN_POINT('Ctrl Pts',(5.17248802793419,-70.1943429691214,
0.));
#130174=CARTESIAN_POINT('Ctrl Pts',(5.17248802793419,-70.1943429691214,
12.));
#130175=CARTESIAN_POINT('Ctrl Pts',(5.17665541952399,-70.1743178937102,
0.));
#130176=CARTESIAN_POINT('Ctrl Pts',(5.17665541952399,-70.1743178937102,
12.));
#130177=CARTESIAN_POINT('Ctrl Pts',(5.18079116757658,-70.1543390243882,
0.));
#130178=CARTESIAN_POINT('Ctrl Pts',(5.18079116757658,-70.1543390243882,
12.));
#130179=CARTESIAN_POINT('Ctrl Pts',(5.18489531966234,-70.1344065558106,
0.));
#130180=CARTESIAN_POINT('Ctrl Pts',(5.18489531966234,-70.1344065558106,
12.));
#130181=CARTESIAN_POINT('Ctrl Pts',(5.18896792486522,-70.1145206891833,
0.));
#130182=CARTESIAN_POINT('Ctrl Pts',(5.18896792486522,-70.1145206891833,
12.));
#130183=CARTESIAN_POINT('Ctrl Pts',(5.19300903271543,-70.0946816270957,
0.));
#130184=CARTESIAN_POINT('Ctrl Pts',(5.19300903271543,-70.0946816270957,
12.));
#130185=CARTESIAN_POINT('Ctrl Pts',(5.19701869225514,-70.0748895689716,
0.));
#130186=CARTESIAN_POINT('Ctrl Pts',(5.19701869225514,-70.0748895689716,
12.));
#130187=CARTESIAN_POINT('Ctrl Pts',(5.20099695122676,-70.0551447071106,
0.));
#130188=CARTESIAN_POINT('Ctrl Pts',(5.20099695122676,-70.0551447071106,
12.));
#130189=CARTESIAN_POINT('Ctrl Pts',(5.20494385478083,-70.0354472203604,
0.));
#130190=CARTESIAN_POINT('Ctrl Pts',(5.20494385478083,-70.0354472203604,
12.));
#130191=CARTESIAN_POINT('Ctrl Pts',(5.20885944672914,-70.0157972802255,
0.));
#130192=CARTESIAN_POINT('Ctrl Pts',(5.20885944672914,-70.0157972802255,
12.));
#130193=CARTESIAN_POINT('Ctrl Pts',(5.2127437720332,-69.996195063002,0.));
#130194=CARTESIAN_POINT('Ctrl Pts',(5.2127437720332,-69.996195063002,12.));
#130195=CARTESIAN_POINT('Ctrl Pts',(5.21659687881138,-69.9766407595385,
0.));
#130196=CARTESIAN_POINT('Ctrl Pts',(5.21659687881138,-69.9766407595385,
12.));
#130197=CARTESIAN_POINT('Ctrl Pts',(5.22041882075626,-69.9571345869996,
0.));
#130198=CARTESIAN_POINT('Ctrl Pts',(5.22041882075626,-69.9571345869996,
12.));
#130199=CARTESIAN_POINT('Ctrl Pts',(5.22420965879807,-69.9376767968951,
0.));
#130200=CARTESIAN_POINT('Ctrl Pts',(5.22420965879807,-69.9376767968951,
12.));
#130201=CARTESIAN_POINT('Ctrl Pts',(5.22796945602602,-69.9182676501892,
0.));
#130202=CARTESIAN_POINT('Ctrl Pts',(5.22796945602602,-69.9182676501892,
12.));
#130203=CARTESIAN_POINT('Ctrl Pts',(5.23169827290451,-69.8989073936606,
0.));
#130204=CARTESIAN_POINT('Ctrl Pts',(5.23169827290451,-69.8989073936606,
12.));
#130205=CARTESIAN_POINT('Ctrl Pts',(5.23539616279714,-69.8795962381676,
0.));
#130206=CARTESIAN_POINT('Ctrl Pts',(5.23539616279714,-69.8795962381676,
12.));
#130207=CARTESIAN_POINT('Ctrl Pts',(5.2390631663514,-69.8603343303016,0.));
#130208=CARTESIAN_POINT('Ctrl Pts',(5.2390631663514,-69.8603343303016,12.));
#130209=CARTESIAN_POINT('Ctrl Pts',(5.24269931055074,-69.8411217507931,
0.));
#130210=CARTESIAN_POINT('Ctrl Pts',(5.24269931055074,-69.8411217507931,
12.));
#130211=CARTESIAN_POINT('Ctrl Pts',(5.24558355160219,-69.8257911792542,
0.));
#130212=CARTESIAN_POINT('Ctrl Pts',(5.24558355160219,-69.8257911792542,
12.));
#130213=CARTESIAN_POINT('Ctrl Pts',(5.24773285666673,-69.8143154684447,
0.));
#130214=CARTESIAN_POINT('Ctrl Pts',(5.24773285666673,-69.8143154684447,
12.));
#130215=CARTESIAN_POINT('Ctrl Pts',(5.24915955997536,-69.8066748687863,
0.));
#130216=CARTESIAN_POINT('Ctrl Pts',(5.24915955997536,-69.8066748687863,
12.));
#130217=CARTESIAN_POINT('Ctrl Pts',(5.2498713699459,-69.8028570375098,0.));
#130218=CARTESIAN_POINT('Ctrl Pts',(5.2498713699459,-69.8028570375098,12.));
#130219=CARTESIAN_POINT('',(5.2498713699459,-69.8028570375098,12.));
#130220=CARTESIAN_POINT('Ctrl Pts',(5.2498713699459,-69.8028570375098,12.));
#130221=CARTESIAN_POINT('Ctrl Pts',(5.24915955997536,-69.8066748687863,
12.));
#130222=CARTESIAN_POINT('Ctrl Pts',(5.24773285666673,-69.8143154684447,
12.));
#130223=CARTESIAN_POINT('Ctrl Pts',(5.24558355160219,-69.8257911792542,
12.));
#130224=CARTESIAN_POINT('Ctrl Pts',(5.24269931055074,-69.8411217507931,
12.));
#130225=CARTESIAN_POINT('Ctrl Pts',(5.2390631663514,-69.8603343303016,12.));
#130226=CARTESIAN_POINT('Ctrl Pts',(5.23539616279714,-69.8795962381676,
12.));
#130227=CARTESIAN_POINT('Ctrl Pts',(5.23169827290451,-69.8989073936606,
12.));
#130228=CARTESIAN_POINT('Ctrl Pts',(5.22796945602602,-69.9182676501892,
12.));
#130229=CARTESIAN_POINT('Ctrl Pts',(5.22420965879807,-69.9376767968951,
12.));
#130230=CARTESIAN_POINT('Ctrl Pts',(5.22041882075626,-69.9571345869996,
12.));
#130231=CARTESIAN_POINT('Ctrl Pts',(5.21659687881138,-69.9766407595385,
12.));
#130232=CARTESIAN_POINT('Ctrl Pts',(5.2127437720332,-69.996195063002,12.));
#130233=CARTESIAN_POINT('Ctrl Pts',(5.20885944672914,-70.0157972802255,
12.));
#130234=CARTESIAN_POINT('Ctrl Pts',(5.20494385478083,-70.0354472203604,
12.));
#130235=CARTESIAN_POINT('Ctrl Pts',(5.20099695122676,-70.0551447071106,
12.));
#130236=CARTESIAN_POINT('Ctrl Pts',(5.19701869225514,-70.0748895689716,
12.));
#130237=CARTESIAN_POINT('Ctrl Pts',(5.19300903271543,-70.0946816270957,
12.));
#130238=CARTESIAN_POINT('Ctrl Pts',(5.18896792486522,-70.1145206891833,
12.));
#130239=CARTESIAN_POINT('Ctrl Pts',(5.18489531966234,-70.1344065558106,
12.));
#130240=CARTESIAN_POINT('Ctrl Pts',(5.18079116757658,-70.1543390243882,
12.));
#130241=CARTESIAN_POINT('Ctrl Pts',(5.17665541952399,-70.1743178937102,
12.));
#130242=CARTESIAN_POINT('Ctrl Pts',(5.17248802793419,-70.1943429691214,
12.));
#130243=CARTESIAN_POINT('Ctrl Pts',(5.16828894670139,-70.2144140623004,
12.));
#130244=CARTESIAN_POINT('Ctrl Pts',(5.16405813066993,-70.2345309887864,
12.));
#130245=CARTESIAN_POINT('Ctrl Pts',(5.159795535282,-70.2546935662719,12.));
#130246=CARTESIAN_POINT('Ctrl Pts',(5.15550111614837,-70.2749016125073,
12.));
#130247=CARTESIAN_POINT('Ctrl Pts',(5.15117482869224,-70.2951549435469,
12.));
#130248=CARTESIAN_POINT('Ctrl Pts',(5.14681662833053,-70.31545337467,12.));
#130249=CARTESIAN_POINT('Ctrl Pts',(5.14242647063466,-70.3357967211782,
12.));
#130250=CARTESIAN_POINT('Ctrl Pts',(5.1380043114891,-70.3561847991725,12.));
#130251=CARTESIAN_POINT('Ctrl Pts',(5.1335501072859,-70.3766174264786,12.));
#130252=CARTESIAN_POINT('Ctrl Pts',(5.12906381499485,-70.3970944229885,
12.));
#130253=CARTESIAN_POINT('Ctrl Pts',(5.12454539205346,-70.4176156101633,
12.));
#130254=CARTESIAN_POINT('Ctrl Pts',(5.11999479630214,-70.438180810725,12.));
#130255=CARTESIAN_POINT('Ctrl Pts',(5.11541198590919,-70.4587898482946,
12.));
#130256=CARTESIAN_POINT('Ctrl Pts',(5.11079691929192,-70.4794425469799,
12.));
#130257=CARTESIAN_POINT('Ctrl Pts',(5.10614955511642,-70.5001387313963,
12.));
#130258=CARTESIAN_POINT('Ctrl Pts',(5.10146985232927,-70.5208782268482,
12.));
#130259=CARTESIAN_POINT('Ctrl Pts',(5.09675777018181,-70.5416608594526,
12.));
#130260=CARTESIAN_POINT('Ctrl Pts',(5.09201326826145,-70.5624864562841,
12.));
#130261=CARTESIAN_POINT('Ctrl Pts',(5.0872363065229,-70.5833548455043,12.));
#130262=CARTESIAN_POINT('Ctrl Pts',(5.08242684526703,-70.6042658562951,
12.));
#130263=CARTESIAN_POINT('Ctrl Pts',(5.07758484512309,-70.6252193187892,
12.));
#130264=CARTESIAN_POINT('Ctrl Pts',(5.07271026703349,-70.6462150640009,
12.));
#130265=CARTESIAN_POINT('Ctrl Pts',(5.06780307224052,-70.6672529237431,
12.));
#130266=CARTESIAN_POINT('Ctrl Pts',(5.06286322227796,-70.6883327305755,
12.));
#130267=CARTESIAN_POINT('Ctrl Pts',(5.0578906789704,-70.7094543178416,12.));
#130268=CARTESIAN_POINT('Ctrl Pts',(5.05288540443477,-70.7306175196856,
12.));
#130269=CARTESIAN_POINT('Ctrl Pts',(5.0478473610835,-70.7518221710715,12.));
#130270=CARTESIAN_POINT('Ctrl Pts',(5.04277651163356,-70.7730681077997,
12.));
#130271=CARTESIAN_POINT('Ctrl Pts',(5.03767281910483,-70.7943551665071,
12.));
#130272=CARTESIAN_POINT('Ctrl Pts',(5.0325362468094,-70.8156831846494,12.));
#130273=CARTESIAN_POINT('Ctrl Pts',(5.0273667583469,-70.8370520004844,12.));
#130274=CARTESIAN_POINT('Ctrl Pts',(5.02216431760059,-70.8584614530517,
12.));
#130275=CARTESIAN_POINT('Ctrl Pts',(5.01692888873792,-70.8799113821449,
12.));
#130276=CARTESIAN_POINT('Ctrl Pts',(5.01166043620572,-70.9014016283123,
12.));
#130277=CARTESIAN_POINT('Ctrl Pts',(5.00635892472517,-70.9229320328588,
12.));
#130278=CARTESIAN_POINT('Ctrl Pts',(5.00102431929038,-70.9445024378439,
12.));
#130279=CARTESIAN_POINT('Ctrl Pts',(4.99565658516905,-70.9661126860773,
12.));
#130280=CARTESIAN_POINT('Ctrl Pts',(4.99025568790652,-70.9877626211112,
12.));
#130281=CARTESIAN_POINT('Ctrl Pts',(4.9848215933185,-71.0094520872375,12.));
#130282=CARTESIAN_POINT('Ctrl Pts',(4.97935426748576,-71.031180929482,12.));
#130283=CARTESIAN_POINT('Ctrl Pts',(4.97385367675156,-71.0529489935959,
12.));
#130284=CARTESIAN_POINT('Ctrl Pts',(4.96831978772201,-71.0747561260443,
12.));
#130285=CARTESIAN_POINT('Ctrl Pts',(4.96275256726786,-71.0966021739922,
12.));
#130286=CARTESIAN_POINT('Ctrl Pts',(4.95715198251703,-71.1184869853071,
12.));
#130287=CARTESIAN_POINT('Ctrl Pts',(4.9515180008511,-71.1404104085561,12.));
#130288=CARTESIAN_POINT('Ctrl Pts',(4.94585058990336,-71.1623722929998,
12.));
#130289=CARTESIAN_POINT('Ctrl Pts',(4.94014971756096,-71.184372488583,12.));
#130290=CARTESIAN_POINT('Ctrl Pts',(4.93441535196593,-71.206410845926,12.));
#130291=CARTESIAN_POINT('Ctrl Pts',(4.9286474615071,-71.2284872163248,12.));
#130292=CARTESIAN_POINT('Ctrl Pts',(4.92284601481709,-71.2506014517457,
12.));
#130293=CARTESIAN_POINT('Ctrl Pts',(4.91701098077041,-71.27275340482,12.));
#130294=CARTESIAN_POINT('Ctrl Pts',(4.91114232848622,-71.2949429288319,
12.));
#130295=CARTESIAN_POINT('Ctrl Pts',(4.90524002732805,-71.3171698777124,
12.));
#130296=CARTESIAN_POINT('Ctrl Pts',(4.89930404689598,-71.3394341060396,
12.));
#130297=CARTESIAN_POINT('Ctrl Pts',(4.89333435702423,-71.3617354690342,
12.));
#130298=CARTESIAN_POINT('Ctrl Pts',(4.88733092777963,-71.3840738225548,
12.));
#130299=CARTESIAN_POINT('Ctrl Pts',(4.88129372946524,-71.4064490230857,
12.));
#130300=CARTESIAN_POINT('Ctrl Pts',(4.8752227326188,-71.4288609277324,12.));
#130301=CARTESIAN_POINT('Ctrl Pts',(4.86911790800533,-71.4513093942216,
12.));
#130302=CARTESIAN_POINT('Ctrl Pts',(4.86297922661498,-71.4737942808971,
12.));
#130303=CARTESIAN_POINT('Ctrl Pts',(4.85680665966184,-71.4963154467128,
12.));
#130304=CARTESIAN_POINT('Ctrl Pts',(4.85060017858786,-71.5188727512231,
12.));
#130305=CARTESIAN_POINT('Ctrl Pts',(4.84435975506055,-71.5414660545778,
12.));
#130306=CARTESIAN_POINT('Ctrl Pts',(4.83808536096589,-71.5640952175239,
12.));
#130307=CARTESIAN_POINT('Ctrl Pts',(4.83177696840639,-71.5867601014008,
12.));
#130308=CARTESIAN_POINT('Ctrl Pts',(4.8254345497002,-71.6094605681353,12.));
#130309=CARTESIAN_POINT('Ctrl Pts',(4.81905807738541,-71.6321964802297,
12.));
#130310=CARTESIAN_POINT('Ctrl Pts',(4.81264752421712,-71.6549677007582,
12.));
#130311=CARTESIAN_POINT('Ctrl Pts',(4.80620286316074,-71.6777740933687,
12.));
#130312=CARTESIAN_POINT('Ctrl Pts',(4.7997240673901,-71.7006155222764,12.));
#130313=CARTESIAN_POINT('Ctrl Pts',(4.79321111028675,-71.723491852261,12.));
#130314=CARTESIAN_POINT('Ctrl Pts',(4.78666396544457,-71.7464029486563,
12.));
#130315=CARTESIAN_POINT('Ctrl Pts',(4.78008260666649,-71.769348677346,12.));
#130316=CARTESIAN_POINT('Ctrl Pts',(4.77346700795791,-71.7923289047643,
12.));
#130317=CARTESIAN_POINT('Ctrl Pts',(4.76681714352501,-71.8153434978923,
12.));
#130318=CARTESIAN_POINT('Ctrl Pts',(4.76013298777419,-71.8383923242531,
12.));
#130319=CARTESIAN_POINT('Ctrl Pts',(4.75341451531669,-71.8614752519008,
12.));
#130320=CARTESIAN_POINT('Ctrl Pts',(4.74666170096546,-71.8845921494189,
12.));
#130321=CARTESIAN_POINT('Ctrl Pts',(4.73987451972863,-71.9077428859212,
12.));
#130322=CARTESIAN_POINT('Ctrl Pts',(4.73305294680785,-71.9309273310471,
12.));
#130323=CARTESIAN_POINT('Ctrl Pts',(4.72619695759773,-71.9541453549579,
12.));
#130324=CARTESIAN_POINT('Ctrl Pts',(4.7193065276907,-71.9773968283259,12.));
#130325=CARTESIAN_POINT('Ctrl Pts',(4.71238163287396,-72.0006816223325,
12.));
#130326=CARTESIAN_POINT('Ctrl Pts',(4.705422249123,-72.0239996086686,12.));
#130327=CARTESIAN_POINT('Ctrl Pts',(4.69842835259991,-72.0473506595318,
12.));
#130328=CARTESIAN_POINT('Ctrl Pts',(4.69139991965283,-72.0707346476213,
12.));
#130329=CARTESIAN_POINT('Ctrl Pts',(4.68433692682068,-72.0941514461287,
12.));
#130330=CARTESIAN_POINT('Ctrl Pts',(4.67723935083094,-72.1176009287351,
12.));
#130331=CARTESIAN_POINT('Ctrl Pts',(4.67010716859284,-72.1410829696128,
12.));
#130332=CARTESIAN_POINT('Ctrl Pts',(4.66294035719569,-72.1645974434216,
12.));
#130333=CARTESIAN_POINT('Ctrl Pts',(4.65573889390821,-72.1881442253053,
12.));
#130334=CARTESIAN_POINT('Ctrl Pts',(4.64850275618323,-72.2117231908822,
12.));
#130335=CARTESIAN_POINT('Ctrl Pts',(4.64123192165627,-72.2353342162417,
12.));
#130336=CARTESIAN_POINT('Ctrl Pts',(4.63392636813843,-72.2589771779456,
12.));
#130337=CARTESIAN_POINT('Ctrl Pts',(4.62658607361465,-72.2826519530259,
12.));
#130338=CARTESIAN_POINT('Ctrl Pts',(4.61921101624291,-72.3063584189807,
12.));
#130339=CARTESIAN_POINT('Ctrl Pts',(4.61180117435862,-72.3300964537658,
12.));
#130340=CARTESIAN_POINT('Ctrl Pts',(4.60435652647452,-72.3538659357913,
12.));
#130341=CARTESIAN_POINT('Ctrl Pts',(4.59687705127329,-72.3776667439227,
12.));
#130342=CARTESIAN_POINT('Ctrl Pts',(4.58936272760543,-72.401498757478,12.));
#130343=CARTESIAN_POINT('Ctrl Pts',(4.58181353448851,-72.4253618562252,
12.));
#130344=CARTESIAN_POINT('Ctrl Pts',(4.57422945111101,-72.4492559203745,
12.));
#130345=CARTESIAN_POINT('Ctrl Pts',(4.56661045683375,-72.4731808305728,
12.));
#130346=CARTESIAN_POINT('Ctrl Pts',(4.5589565311822,-72.4971364679068,12.));
#130347=CARTESIAN_POINT('Ctrl Pts',(4.55126765384403,-72.5211227139001,
12.));
#130348=CARTESIAN_POINT('Ctrl Pts',(4.54354380466821,-72.5451394505104,
12.));
#130349=CARTESIAN_POINT('Ctrl Pts',(4.53578496366799,-72.5691865601223,
12.));
#130350=CARTESIAN_POINT('Ctrl Pts',(4.52799111102391,-72.5932639255409,
12.));
#130351=CARTESIAN_POINT('Ctrl Pts',(4.52016222707637,-72.6173714299942,
12.));
#130352=CARTESIAN_POINT('Ctrl Pts',(4.51229829232263,-72.6415089571321,
12.));
#130353=CARTESIAN_POINT('Ctrl Pts',(4.50439928741603,-72.6656763910241,
12.));
#130354=CARTESIAN_POINT('Ctrl Pts',(4.49646519316812,-72.6898736161542,
12.));
#130355=CARTESIAN_POINT('Ctrl Pts',(4.48849599055337,-72.714100517414,12.));
#130356=CARTESIAN_POINT('Ctrl Pts',(4.48049166070205,-72.738356980103,12.));
#130357=CARTESIAN_POINT('Ctrl Pts',(4.47245218489609,-72.7626428899281,
12.));
#130358=CARTESIAN_POINT('Ctrl Pts',(4.46437754456792,-72.7869581329994,
12.));
#130359=CARTESIAN_POINT('Ctrl Pts',(4.45626772130145,-72.8113025958262,
12.));
#130360=CARTESIAN_POINT('Ctrl Pts',(4.44812269683737,-72.8356761653069,
12.));
#130361=CARTESIAN_POINT('Ctrl Pts',(4.43994245306817,-72.8600787287318,
12.));
#130362=CARTESIAN_POINT('Ctrl Pts',(4.43172697203349,-72.8845101737855,
12.));
#130363=CARTESIAN_POINT('Ctrl Pts',(4.42347623591941,-72.9089703885462,
12.));
#130364=CARTESIAN_POINT('Ctrl Pts',(4.41519022705921,-72.9334592614829,
12.));
#130365=CARTESIAN_POINT('Ctrl Pts',(4.40686892793957,-72.95797668145,12.));
#130366=CARTESIAN_POINT('Ctrl Pts',(4.39851232119721,-72.9825225376847,
12.));
#130367=CARTESIAN_POINT('Ctrl Pts',(4.39012038961138,-73.007096719804,12.));
#130368=CARTESIAN_POINT('Ctrl Pts',(4.3816931161015,-73.0316991177993,12.));
#130369=CARTESIAN_POINT('Ctrl Pts',(4.37323048372606,-73.0563296220299,
12.));
#130370=CARTESIAN_POINT('Ctrl Pts',(4.3647324756864,-73.0809881232103,12.));
#130371=CARTESIAN_POINT('Ctrl Pts',(4.35619907532719,-73.1056745124087,
12.));
#130372=CARTESIAN_POINT('Ctrl Pts',(4.34763026613157,-73.130388681059,12.));
#130373=CARTESIAN_POINT('Ctrl Pts',(4.3390260317214,-73.1551305209685,12.));
#130374=CARTESIAN_POINT('Ctrl Pts',(4.33038635585876,-73.1798999243235,
12.));
#130375=CARTESIAN_POINT('Ctrl Pts',(4.32171122245213,-73.204696783694,12.));
#130376=CARTESIAN_POINT('Ctrl Pts',(4.31300061556097,-73.2295209920334,
12.));
#130377=CARTESIAN_POINT('Ctrl Pts',(4.30425451938229,-73.2543724426577,
12.));
#130378=CARTESIAN_POINT('Ctrl Pts',(4.29547291824286,-73.2792510292254,
12.));
#130379=CARTESIAN_POINT('Ctrl Pts',(4.286655796593,-73.3041566457135,12.));
#130380=CARTESIAN_POINT('Ctrl Pts',(4.27780313900389,-73.3290891863949,
12.));
#130381=CARTESIAN_POINT('Ctrl Pts',(4.26891493016699,-73.3540485458065,
12.));
#130382=CARTESIAN_POINT('Ctrl Pts',(4.25999115489898,-73.3790346187938,
12.));
#130383=CARTESIAN_POINT('Ctrl Pts',(4.25103179814886,-73.4040473005592,
12.));
#130384=CARTESIAN_POINT('Ctrl Pts',(4.24203684500938,-73.4290864867101,
12.));
#130385=CARTESIAN_POINT('Ctrl Pts',(4.23300628072757,-73.4541520732948,
12.));
#130386=CARTESIAN_POINT('Ctrl Pts',(4.22394009072755,-73.4792439568633,
12.));
#130387=CARTESIAN_POINT('Ctrl Pts',(4.2148382605944,-73.5043620344116,12.));
#130388=CARTESIAN_POINT('Ctrl Pts',(4.20570077603729,-73.5295062032628,
12.));
#130389=CARTESIAN_POINT('Ctrl Pts',(4.19652762286126,-73.5546763609572,
12.));
#130390=CARTESIAN_POINT('Ctrl Pts',(4.18731878694235,-73.5798724051519,
12.));
#130391=CARTESIAN_POINT('Ctrl Pts',(4.17807425419812,-73.6050942334768,
12.));
#130392=CARTESIAN_POINT('Ctrl Pts',(4.1687940105878,-73.6303417435251,12.));
#130393=CARTESIAN_POINT('Ctrl Pts',(4.15947804217783,-73.6556148331489,
12.));
#130394=CARTESIAN_POINT('Ctrl Pts',(4.15012633519722,-73.6809134006897,
12.));
#130395=CARTESIAN_POINT('Ctrl Pts',(4.14073887610152,-73.7062373452342,
12.));
#130396=CARTESIAN_POINT('Ctrl Pts',(4.13131565163577,-73.7315865668522,
12.));
#130397=CARTESIAN_POINT('Ctrl Pts',(4.12185664890556,-73.7569609668528,
12.));
#130398=CARTESIAN_POINT('Ctrl Pts',(4.11236185522786,-73.7823604472159,
12.));
#130399=CARTESIAN_POINT('Ctrl Pts',(4.10283125798728,-73.8077849100342,
12.));
#130400=CARTESIAN_POINT('Ctrl Pts',(4.09326484448232,-73.8332342568989,
12.));
#130401=CARTESIAN_POINT('Ctrl Pts',(4.08366260180674,-73.8587083884191,
12.));
#130402=CARTESIAN_POINT('Ctrl Pts',(4.07402451665244,-73.8842072034008,
12.));
#130403=CARTESIAN_POINT('Ctrl Pts',(4.06435057547324,-73.9097305995115,
12.));
#130404=CARTESIAN_POINT('Ctrl Pts',(4.05464076484751,-73.9352784747608,
12.));
#130405=CARTESIAN_POINT('Ctrl Pts',(4.04489507179957,-73.9608507287909,
12.));
#130406=CARTESIAN_POINT('Ctrl Pts',(4.03511348410659,-73.9864472641033,
12.));
#130407=CARTESIAN_POINT('Ctrl Pts',(4.02529599070094,-74.012067987646,12.));
#130408=CARTESIAN_POINT('Ctrl Pts',(4.0154425817671,-74.0377128111863,12.));
#130409=CARTESIAN_POINT('Ctrl Pts',(4.00696550627364,-74.0597159782109,
12.));
#130410=CARTESIAN_POINT('Ctrl Pts',(4.00044689711983,-74.0765982943677,
12.));
#130411=CARTESIAN_POINT('Ctrl Pts',(3.99590266746991,-74.0883491449954,
12.));
#130412=CARTESIAN_POINT('Ctrl Pts',(3.99334334445528,-74.0949615399619,
12.));
#130413=CARTESIAN_POINT('Ctrl Pts',(3.99277406490872,-74.0964320766207,
12.));
#130414=CARTESIAN_POINT('',(5.2498713699459,-69.8028570375098,0.));
#130415=CARTESIAN_POINT('',(5.2498713699459,-69.8028570375097,0.));
#130416=CARTESIAN_POINT('Ctrl Pts',(3.99277406490873,-74.0964320766207,
0.));
#130417=CARTESIAN_POINT('Ctrl Pts',(3.9933433444553,-74.0949615399619,0.));
#130418=CARTESIAN_POINT('Ctrl Pts',(3.99590266746992,-74.0883491449954,
0.));
#130419=CARTESIAN_POINT('Ctrl Pts',(4.00044689711983,-74.0765982943676,
0.));
#130420=CARTESIAN_POINT('Ctrl Pts',(4.00696550627364,-74.0597159782109,
0.));
#130421=CARTESIAN_POINT('Ctrl Pts',(4.0154425817671,-74.0377128111863,0.));
#130422=CARTESIAN_POINT('Ctrl Pts',(4.02529599070094,-74.012067987646,0.));
#130423=CARTESIAN_POINT('Ctrl Pts',(4.03511348410659,-73.9864472641033,
0.));
#130424=CARTESIAN_POINT('Ctrl Pts',(4.04489507179957,-73.9608507287909,
0.));
#130425=CARTESIAN_POINT('Ctrl Pts',(4.05464076484751,-73.9352784747608,
0.));
#130426=CARTESIAN_POINT('Ctrl Pts',(4.06435057547324,-73.9097305995115,
0.));
#130427=CARTESIAN_POINT('Ctrl Pts',(4.07402451665244,-73.8842072034008,
0.));
#130428=CARTESIAN_POINT('Ctrl Pts',(4.08366260180674,-73.8587083884191,
0.));
#130429=CARTESIAN_POINT('Ctrl Pts',(4.09326484448232,-73.8332342568989,
0.));
#130430=CARTESIAN_POINT('Ctrl Pts',(4.10283125798728,-73.8077849100342,
0.));
#130431=CARTESIAN_POINT('Ctrl Pts',(4.11236185522786,-73.7823604472159,
0.));
#130432=CARTESIAN_POINT('Ctrl Pts',(4.12185664890556,-73.7569609668528,
0.));
#130433=CARTESIAN_POINT('Ctrl Pts',(4.13131565163577,-73.7315865668522,
0.));
#130434=CARTESIAN_POINT('Ctrl Pts',(4.14073887610152,-73.7062373452342,
0.));
#130435=CARTESIAN_POINT('Ctrl Pts',(4.15012633519722,-73.6809134006897,
0.));
#130436=CARTESIAN_POINT('Ctrl Pts',(4.15947804217783,-73.6556148331489,
0.));
#130437=CARTESIAN_POINT('Ctrl Pts',(4.1687940105878,-73.6303417435251,0.));
#130438=CARTESIAN_POINT('Ctrl Pts',(4.17807425419812,-73.6050942334768,
0.));
#130439=CARTESIAN_POINT('Ctrl Pts',(4.18731878694235,-73.5798724051519,
0.));
#130440=CARTESIAN_POINT('Ctrl Pts',(4.19652762286126,-73.5546763609572,
0.));
#130441=CARTESIAN_POINT('Ctrl Pts',(4.20570077603729,-73.5295062032628,
0.));
#130442=CARTESIAN_POINT('Ctrl Pts',(4.2148382605944,-73.5043620344116,0.));
#130443=CARTESIAN_POINT('Ctrl Pts',(4.22394009072755,-73.4792439568633,
0.));
#130444=CARTESIAN_POINT('Ctrl Pts',(4.23300628072757,-73.4541520732948,
0.));
#130445=CARTESIAN_POINT('Ctrl Pts',(4.24203684500938,-73.4290864867101,
0.));
#130446=CARTESIAN_POINT('Ctrl Pts',(4.25103179814886,-73.4040473005592,
0.));
#130447=CARTESIAN_POINT('Ctrl Pts',(4.25999115489898,-73.3790346187938,
0.));
#130448=CARTESIAN_POINT('Ctrl Pts',(4.26891493016699,-73.3540485458065,
0.));
#130449=CARTESIAN_POINT('Ctrl Pts',(4.27780313900389,-73.3290891863949,
0.));
#130450=CARTESIAN_POINT('Ctrl Pts',(4.286655796593,-73.3041566457135,0.));
#130451=CARTESIAN_POINT('Ctrl Pts',(4.29547291824286,-73.2792510292254,
0.));
#130452=CARTESIAN_POINT('Ctrl Pts',(4.30425451938229,-73.2543724426577,
0.));
#130453=CARTESIAN_POINT('Ctrl Pts',(4.31300061556097,-73.2295209920334,
0.));
#130454=CARTESIAN_POINT('Ctrl Pts',(4.32171122245213,-73.204696783694,0.));
#130455=CARTESIAN_POINT('Ctrl Pts',(4.33038635585876,-73.1798999243235,
0.));
#130456=CARTESIAN_POINT('Ctrl Pts',(4.3390260317214,-73.1551305209685,0.));
#130457=CARTESIAN_POINT('Ctrl Pts',(4.34763026613157,-73.130388681059,0.));
#130458=CARTESIAN_POINT('Ctrl Pts',(4.35619907532719,-73.1056745124087,
0.));
#130459=CARTESIAN_POINT('Ctrl Pts',(4.3647324756864,-73.0809881232103,0.));
#130460=CARTESIAN_POINT('Ctrl Pts',(4.37323048372606,-73.0563296220299,
0.));
#130461=CARTESIAN_POINT('Ctrl Pts',(4.3816931161015,-73.0316991177993,0.));
#130462=CARTESIAN_POINT('Ctrl Pts',(4.39012038961138,-73.007096719804,0.));
#130463=CARTESIAN_POINT('Ctrl Pts',(4.39851232119721,-72.9825225376847,
0.));
#130464=CARTESIAN_POINT('Ctrl Pts',(4.40686892793957,-72.95797668145,0.));
#130465=CARTESIAN_POINT('Ctrl Pts',(4.41519022705921,-72.9334592614829,
0.));
#130466=CARTESIAN_POINT('Ctrl Pts',(4.42347623591941,-72.9089703885462,
0.));
#130467=CARTESIAN_POINT('Ctrl Pts',(4.43172697203349,-72.8845101737855,
0.));
#130468=CARTESIAN_POINT('Ctrl Pts',(4.43994245306817,-72.8600787287318,
0.));
#130469=CARTESIAN_POINT('Ctrl Pts',(4.44812269683737,-72.8356761653069,
0.));
#130470=CARTESIAN_POINT('Ctrl Pts',(4.45626772130145,-72.8113025958262,
0.));
#130471=CARTESIAN_POINT('Ctrl Pts',(4.46437754456792,-72.7869581329994,
0.));
#130472=CARTESIAN_POINT('Ctrl Pts',(4.47245218489609,-72.7626428899281,
0.));
#130473=CARTESIAN_POINT('Ctrl Pts',(4.48049166070205,-72.738356980103,0.));
#130474=CARTESIAN_POINT('Ctrl Pts',(4.48849599055337,-72.714100517414,0.));
#130475=CARTESIAN_POINT('Ctrl Pts',(4.49646519316812,-72.6898736161542,
0.));
#130476=CARTESIAN_POINT('Ctrl Pts',(4.50439928741603,-72.6656763910241,
0.));
#130477=CARTESIAN_POINT('Ctrl Pts',(4.51229829232263,-72.6415089571321,
0.));
#130478=CARTESIAN_POINT('Ctrl Pts',(4.52016222707637,-72.6173714299942,
0.));
#130479=CARTESIAN_POINT('Ctrl Pts',(4.52799111102391,-72.5932639255409,
0.));
#130480=CARTESIAN_POINT('Ctrl Pts',(4.53578496366799,-72.5691865601223,
0.));
#130481=CARTESIAN_POINT('Ctrl Pts',(4.54354380466821,-72.5451394505104,
0.));
#130482=CARTESIAN_POINT('Ctrl Pts',(4.55126765384403,-72.5211227139001,
0.));
#130483=CARTESIAN_POINT('Ctrl Pts',(4.5589565311822,-72.4971364679068,0.));
#130484=CARTESIAN_POINT('Ctrl Pts',(4.56661045683375,-72.4731808305728,
0.));
#130485=CARTESIAN_POINT('Ctrl Pts',(4.57422945111101,-72.4492559203745,
0.));
#130486=CARTESIAN_POINT('Ctrl Pts',(4.58181353448851,-72.4253618562252,
0.));
#130487=CARTESIAN_POINT('Ctrl Pts',(4.58936272760543,-72.401498757478,0.));
#130488=CARTESIAN_POINT('Ctrl Pts',(4.59687705127329,-72.3776667439227,
0.));
#130489=CARTESIAN_POINT('Ctrl Pts',(4.60435652647452,-72.3538659357913,
0.));
#130490=CARTESIAN_POINT('Ctrl Pts',(4.61180117435862,-72.3300964537658,
0.));
#130491=CARTESIAN_POINT('Ctrl Pts',(4.61921101624291,-72.3063584189807,
0.));
#130492=CARTESIAN_POINT('Ctrl Pts',(4.62658607361465,-72.2826519530259,
0.));
#130493=CARTESIAN_POINT('Ctrl Pts',(4.63392636813843,-72.2589771779456,
0.));
#130494=CARTESIAN_POINT('Ctrl Pts',(4.64123192165627,-72.2353342162417,
0.));
#130495=CARTESIAN_POINT('Ctrl Pts',(4.64850275618323,-72.2117231908822,
0.));
#130496=CARTESIAN_POINT('Ctrl Pts',(4.65573889390821,-72.1881442253053,
0.));
#130497=CARTESIAN_POINT('Ctrl Pts',(4.66294035719569,-72.1645974434216,
0.));
#130498=CARTESIAN_POINT('Ctrl Pts',(4.67010716859284,-72.1410829696128,
0.));
#130499=CARTESIAN_POINT('Ctrl Pts',(4.67723935083094,-72.1176009287351,
0.));
#130500=CARTESIAN_POINT('Ctrl Pts',(4.68433692682068,-72.0941514461287,
0.));
#130501=CARTESIAN_POINT('Ctrl Pts',(4.69139991965283,-72.0707346476213,
0.));
#130502=CARTESIAN_POINT('Ctrl Pts',(4.69842835259991,-72.0473506595318,
0.));
#130503=CARTESIAN_POINT('Ctrl Pts',(4.705422249123,-72.0239996086686,0.));
#130504=CARTESIAN_POINT('Ctrl Pts',(4.71238163287396,-72.0006816223325,
0.));
#130505=CARTESIAN_POINT('Ctrl Pts',(4.7193065276907,-71.9773968283259,0.));
#130506=CARTESIAN_POINT('Ctrl Pts',(4.72619695759773,-71.9541453549579,
0.));
#130507=CARTESIAN_POINT('Ctrl Pts',(4.73305294680785,-71.9309273310471,
0.));
#130508=CARTESIAN_POINT('Ctrl Pts',(4.73987451972863,-71.9077428859212,
0.));
#130509=CARTESIAN_POINT('Ctrl Pts',(4.74666170096546,-71.8845921494189,
0.));
#130510=CARTESIAN_POINT('Ctrl Pts',(4.75341451531669,-71.8614752519008,
0.));
#130511=CARTESIAN_POINT('Ctrl Pts',(4.76013298777419,-71.8383923242531,
0.));
#130512=CARTESIAN_POINT('Ctrl Pts',(4.76681714352501,-71.8153434978923,
0.));
#130513=CARTESIAN_POINT('Ctrl Pts',(4.77346700795791,-71.7923289047643,
0.));
#130514=CARTESIAN_POINT('Ctrl Pts',(4.78008260666649,-71.769348677346,0.));
#130515=CARTESIAN_POINT('Ctrl Pts',(4.78666396544457,-71.7464029486563,
0.));
#130516=CARTESIAN_POINT('Ctrl Pts',(4.79321111028675,-71.723491852261,0.));
#130517=CARTESIAN_POINT('Ctrl Pts',(4.7997240673901,-71.7006155222764,0.));
#130518=CARTESIAN_POINT('Ctrl Pts',(4.80620286316074,-71.6777740933687,
0.));
#130519=CARTESIAN_POINT('Ctrl Pts',(4.81264752421712,-71.6549677007582,
0.));
#130520=CARTESIAN_POINT('Ctrl Pts',(4.81905807738541,-71.6321964802297,
0.));
#130521=CARTESIAN_POINT('Ctrl Pts',(4.8254345497002,-71.6094605681353,0.));
#130522=CARTESIAN_POINT('Ctrl Pts',(4.83177696840639,-71.5867601014008,
0.));
#130523=CARTESIAN_POINT('Ctrl Pts',(4.83808536096589,-71.5640952175239,
0.));
#130524=CARTESIAN_POINT('Ctrl Pts',(4.84435975506055,-71.5414660545778,
0.));
#130525=CARTESIAN_POINT('Ctrl Pts',(4.85060017858786,-71.5188727512231,
0.));
#130526=CARTESIAN_POINT('Ctrl Pts',(4.85680665966184,-71.4963154467128,
0.));
#130527=CARTESIAN_POINT('Ctrl Pts',(4.86297922661498,-71.4737942808971,
0.));
#130528=CARTESIAN_POINT('Ctrl Pts',(4.86911790800533,-71.4513093942216,
0.));
#130529=CARTESIAN_POINT('Ctrl Pts',(4.8752227326188,-71.4288609277324,0.));
#130530=CARTESIAN_POINT('Ctrl Pts',(4.88129372946524,-71.4064490230857,
0.));
#130531=CARTESIAN_POINT('Ctrl Pts',(4.88733092777963,-71.3840738225548,
0.));
#130532=CARTESIAN_POINT('Ctrl Pts',(4.89333435702423,-71.3617354690342,
0.));
#130533=CARTESIAN_POINT('Ctrl Pts',(4.89930404689598,-71.3394341060396,
0.));
#130534=CARTESIAN_POINT('Ctrl Pts',(4.90524002732805,-71.3171698777124,
0.));
#130535=CARTESIAN_POINT('Ctrl Pts',(4.91114232848622,-71.2949429288319,
0.));
#130536=CARTESIAN_POINT('Ctrl Pts',(4.91701098077041,-71.27275340482,0.));
#130537=CARTESIAN_POINT('Ctrl Pts',(4.92284601481709,-71.2506014517457,
0.));
#130538=CARTESIAN_POINT('Ctrl Pts',(4.9286474615071,-71.2284872163248,0.));
#130539=CARTESIAN_POINT('Ctrl Pts',(4.93441535196593,-71.206410845926,0.));
#130540=CARTESIAN_POINT('Ctrl Pts',(4.94014971756096,-71.184372488583,0.));
#130541=CARTESIAN_POINT('Ctrl Pts',(4.94585058990336,-71.1623722929998,
0.));
#130542=CARTESIAN_POINT('Ctrl Pts',(4.9515180008511,-71.1404104085561,0.));
#130543=CARTESIAN_POINT('Ctrl Pts',(4.95715198251703,-71.1184869853071,
0.));
#130544=CARTESIAN_POINT('Ctrl Pts',(4.96275256726786,-71.0966021739922,
0.));
#130545=CARTESIAN_POINT('Ctrl Pts',(4.96831978772201,-71.0747561260443,
0.));
#130546=CARTESIAN_POINT('Ctrl Pts',(4.97385367675156,-71.0529489935959,
0.));
#130547=CARTESIAN_POINT('Ctrl Pts',(4.97935426748576,-71.031180929482,0.));
#130548=CARTESIAN_POINT('Ctrl Pts',(4.9848215933185,-71.0094520872375,0.));
#130549=CARTESIAN_POINT('Ctrl Pts',(4.99025568790652,-70.9877626211112,
0.));
#130550=CARTESIAN_POINT('Ctrl Pts',(4.99565658516905,-70.9661126860773,
0.));
#130551=CARTESIAN_POINT('Ctrl Pts',(5.00102431929038,-70.9445024378439,
0.));
#130552=CARTESIAN_POINT('Ctrl Pts',(5.00635892472517,-70.9229320328588,
0.));
#130553=CARTESIAN_POINT('Ctrl Pts',(5.01166043620572,-70.9014016283123,
0.));
#130554=CARTESIAN_POINT('Ctrl Pts',(5.01692888873792,-70.8799113821449,
0.));
#130555=CARTESIAN_POINT('Ctrl Pts',(5.02216431760059,-70.8584614530517,
0.));
#130556=CARTESIAN_POINT('Ctrl Pts',(5.0273667583469,-70.8370520004844,0.));
#130557=CARTESIAN_POINT('Ctrl Pts',(5.0325362468094,-70.8156831846494,0.));
#130558=CARTESIAN_POINT('Ctrl Pts',(5.03767281910483,-70.7943551665071,
0.));
#130559=CARTESIAN_POINT('Ctrl Pts',(5.04277651163356,-70.7730681077997,
0.));
#130560=CARTESIAN_POINT('Ctrl Pts',(5.0478473610835,-70.7518221710715,0.));
#130561=CARTESIAN_POINT('Ctrl Pts',(5.05288540443477,-70.7306175196856,
0.));
#130562=CARTESIAN_POINT('Ctrl Pts',(5.0578906789704,-70.7094543178416,0.));
#130563=CARTESIAN_POINT('Ctrl Pts',(5.06286322227796,-70.6883327305755,
0.));
#130564=CARTESIAN_POINT('Ctrl Pts',(5.06780307224052,-70.6672529237431,
0.));
#130565=CARTESIAN_POINT('Ctrl Pts',(5.07271026703349,-70.6462150640009,
0.));
#130566=CARTESIAN_POINT('Ctrl Pts',(5.07758484512309,-70.6252193187892,
0.));
#130567=CARTESIAN_POINT('Ctrl Pts',(5.08242684526703,-70.6042658562951,
0.));
#130568=CARTESIAN_POINT('Ctrl Pts',(5.0872363065229,-70.5833548455043,0.));
#130569=CARTESIAN_POINT('Ctrl Pts',(5.09201326826145,-70.5624864562841,
0.));
#130570=CARTESIAN_POINT('Ctrl Pts',(5.09675777018181,-70.5416608594526,
0.));
#130571=CARTESIAN_POINT('Ctrl Pts',(5.10146985232927,-70.5208782268482,
0.));
#130572=CARTESIAN_POINT('Ctrl Pts',(5.10614955511642,-70.5001387313963,
0.));
#130573=CARTESIAN_POINT('Ctrl Pts',(5.11079691929192,-70.4794425469799,
0.));
#130574=CARTESIAN_POINT('Ctrl Pts',(5.11541198590919,-70.4587898482946,
0.));
#130575=CARTESIAN_POINT('Ctrl Pts',(5.11999479630214,-70.438180810725,0.));
#130576=CARTESIAN_POINT('Ctrl Pts',(5.12454539205346,-70.4176156101633,
0.));
#130577=CARTESIAN_POINT('Ctrl Pts',(5.12906381499485,-70.3970944229885,
0.));
#130578=CARTESIAN_POINT('Ctrl Pts',(5.1335501072859,-70.3766174264786,0.));
#130579=CARTESIAN_POINT('Ctrl Pts',(5.1380043114891,-70.3561847991725,0.));
#130580=CARTESIAN_POINT('Ctrl Pts',(5.14242647063466,-70.3357967211782,
0.));
#130581=CARTESIAN_POINT('Ctrl Pts',(5.14681662833053,-70.31545337467,0.));
#130582=CARTESIAN_POINT('Ctrl Pts',(5.15117482869224,-70.2951549435469,
0.));
#130583=CARTESIAN_POINT('Ctrl Pts',(5.15550111614837,-70.2749016125073,
0.));
#130584=CARTESIAN_POINT('Ctrl Pts',(5.159795535282,-70.2546935662719,0.));
#130585=CARTESIAN_POINT('Ctrl Pts',(5.16405813066993,-70.2345309887864,
0.));
#130586=CARTESIAN_POINT('Ctrl Pts',(5.16828894670139,-70.2144140623004,
0.));
#130587=CARTESIAN_POINT('Ctrl Pts',(5.17248802793419,-70.1943429691214,
0.));
#130588=CARTESIAN_POINT('Ctrl Pts',(5.17665541952399,-70.1743178937102,
0.));
#130589=CARTESIAN_POINT('Ctrl Pts',(5.18079116757658,-70.1543390243882,
0.));
#130590=CARTESIAN_POINT('Ctrl Pts',(5.18489531966234,-70.1344065558106,
0.));
#130591=CARTESIAN_POINT('Ctrl Pts',(5.18896792486522,-70.1145206891833,
0.));
#130592=CARTESIAN_POINT('Ctrl Pts',(5.19300903271543,-70.0946816270957,
0.));
#130593=CARTESIAN_POINT('Ctrl Pts',(5.19701869225514,-70.0748895689716,
0.));
#130594=CARTESIAN_POINT('Ctrl Pts',(5.20099695122676,-70.0551447071106,
0.));
#130595=CARTESIAN_POINT('Ctrl Pts',(5.20494385478083,-70.0354472203604,
0.));
#130596=CARTESIAN_POINT('Ctrl Pts',(5.20885944672914,-70.0157972802255,
0.));
#130597=CARTESIAN_POINT('Ctrl Pts',(5.2127437720332,-69.996195063002,0.));
#130598=CARTESIAN_POINT('Ctrl Pts',(5.21659687881138,-69.9766407595385,
0.));
#130599=CARTESIAN_POINT('Ctrl Pts',(5.22041882075626,-69.9571345869996,
0.));
#130600=CARTESIAN_POINT('Ctrl Pts',(5.22420965879807,-69.9376767968951,
0.));
#130601=CARTESIAN_POINT('Ctrl Pts',(5.22796945602602,-69.9182676501892,
0.));
#130602=CARTESIAN_POINT('Ctrl Pts',(5.23169827290451,-69.8989073936606,
0.));
#130603=CARTESIAN_POINT('Ctrl Pts',(5.23539616279714,-69.8795962381676,
0.));
#130604=CARTESIAN_POINT('Ctrl Pts',(5.2390631663514,-69.8603343303016,0.));
#130605=CARTESIAN_POINT('Ctrl Pts',(5.24269931055074,-69.8411217507931,
0.));
#130606=CARTESIAN_POINT('Ctrl Pts',(5.24558355160219,-69.8257911792542,
0.));
#130607=CARTESIAN_POINT('Ctrl Pts',(5.24773285666673,-69.8143154684447,
0.));
#130608=CARTESIAN_POINT('Ctrl Pts',(5.24915955997536,-69.8066748687863,
0.));
#130609=CARTESIAN_POINT('Ctrl Pts',(5.2498713699459,-69.8028570375098,0.));
#130610=CARTESIAN_POINT('Ctrl Pts',(-2.62535189104656,-74.4537274248118,
0.));
#130611=CARTESIAN_POINT('Ctrl Pts',(-2.62535189104656,-74.4537274248118,
12.));
#130612=CARTESIAN_POINT('Ctrl Pts',(-2.62283178248297,-74.4487312586601,
0.));
#130613=CARTESIAN_POINT('Ctrl Pts',(-2.62283178248297,-74.4487312586601,
12.));
#130614=CARTESIAN_POINT('Ctrl Pts',(-2.6177953543237,-74.4387409032582,
0.));
#130615=CARTESIAN_POINT('Ctrl Pts',(-2.6177953543237,-74.4387409032582,
12.));
#130616=CARTESIAN_POINT('Ctrl Pts',(-2.61025207898831,-74.4237613008609,
0.));
#130617=CARTESIAN_POINT('Ctrl Pts',(-2.61025207898831,-74.4237613008609,
12.));
#130618=CARTESIAN_POINT('Ctrl Pts',(-2.60021711327491,-74.4038003595514,
0.));
#130619=CARTESIAN_POINT('Ctrl Pts',(-2.60021711327491,-74.4038003595514,
12.));
#130620=CARTESIAN_POINT('Ctrl Pts',(-2.58771130268619,-74.3788689604,0.));
#130621=CARTESIAN_POINT('Ctrl Pts',(-2.58771130268619,-74.3788689604,12.));
#130622=CARTESIAN_POINT('Ctrl Pts',(-2.57524339541657,-74.3539573568054,
0.));
#130623=CARTESIAN_POINT('Ctrl Pts',(-2.57524339541657,-74.3539573568054,
12.));
#130624=CARTESIAN_POINT('Ctrl Pts',(-2.56281339800082,-74.3290655814922,
0.));
#130625=CARTESIAN_POINT('Ctrl Pts',(-2.56281339800082,-74.3290655814922,
12.));
#130626=CARTESIAN_POINT('Ctrl Pts',(-2.55042131526684,-74.3041936853329,
0.));
#130627=CARTESIAN_POINT('Ctrl Pts',(-2.55042131526684,-74.3041936853329,
12.));
#130628=CARTESIAN_POINT('Ctrl Pts',(-2.53806714838103,-74.2793417427044,
0.));
#130629=CARTESIAN_POINT('Ctrl Pts',(-2.53806714838103,-74.2793417427044,
12.));
#130630=CARTESIAN_POINT('Ctrl Pts',(-2.52575089478112,-74.2545098494549,
0.));
#130631=CARTESIAN_POINT('Ctrl Pts',(-2.52575089478112,-74.2545098494549,
12.));
#130632=CARTESIAN_POINT('Ctrl Pts',(-2.51347254956027,-74.2296981152027,
0.));
#130633=CARTESIAN_POINT('Ctrl Pts',(-2.51347254956027,-74.2296981152027,
12.));
#130634=CARTESIAN_POINT('Ctrl Pts',(-2.50123210644075,-74.2049066571942,
0.));
#130635=CARTESIAN_POINT('Ctrl Pts',(-2.50123210644075,-74.2049066571942,
12.));
#130636=CARTESIAN_POINT('Ctrl Pts',(-2.48902955888401,-74.180135593693,
0.));
#130637=CARTESIAN_POINT('Ctrl Pts',(-2.48902955888401,-74.180135593693,
12.));
#130638=CARTESIAN_POINT('Ctrl Pts',(-2.47686490120423,-74.1553850371577,
0.));
#130639=CARTESIAN_POINT('Ctrl Pts',(-2.47686490120423,-74.1553850371577,
12.));
#130640=CARTESIAN_POINT('Ctrl Pts',(-2.46473812948048,-74.1306550887196,
0.));
#130641=CARTESIAN_POINT('Ctrl Pts',(-2.46473812948048,-74.1306550887196,
12.));
#130642=CARTESIAN_POINT('Ctrl Pts',(-2.45264924094852,-74.1059458420175,
0.));
#130643=CARTESIAN_POINT('Ctrl Pts',(-2.45264924094852,-74.1059458420175,
12.));
#130644=CARTESIAN_POINT('Ctrl Pts',(-2.44059823356722,-74.0812573859474,
0.));
#130645=CARTESIAN_POINT('Ctrl Pts',(-2.44059823356722,-74.0812573859474,
12.));
#130646=CARTESIAN_POINT('Ctrl Pts',(-2.42858510549786,-74.0565898079227,
0.));
#130647=CARTESIAN_POINT('Ctrl Pts',(-2.42858510549786,-74.0565898079227,
12.));
#130648=CARTESIAN_POINT('Ctrl Pts',(-2.41660985465228,-74.0319431966956,
0.));
#130649=CARTESIAN_POINT('Ctrl Pts',(-2.41660985465228,-74.0319431966956,
12.));
#130650=CARTESIAN_POINT('Ctrl Pts',(-2.40467247811497,-74.0073176459287,
0.));
#130651=CARTESIAN_POINT('Ctrl Pts',(-2.40467247811497,-74.0073176459287,
12.));
#130652=CARTESIAN_POINT('Ctrl Pts',(-2.39277297220716,-73.9827132538149,
0.));
#130653=CARTESIAN_POINT('Ctrl Pts',(-2.39277297220716,-73.9827132538149,
12.));
#130654=CARTESIAN_POINT('Ctrl Pts',(-2.38091133274933,-73.9581301214609,
0.));
#130655=CARTESIAN_POINT('Ctrl Pts',(-2.38091133274933,-73.9581301214609,
12.));
#130656=CARTESIAN_POINT('Ctrl Pts',(-2.36908755525994,-73.9335683516388,
0.));
#130657=CARTESIAN_POINT('Ctrl Pts',(-2.36908755525994,-73.9335683516388,
12.));
#130658=CARTESIAN_POINT('Ctrl Pts',(-2.35730163516324,-73.9090280474723,
0.));
#130659=CARTESIAN_POINT('Ctrl Pts',(-2.35730163516324,-73.9090280474723,
12.));
#130660=CARTESIAN_POINT('Ctrl Pts',(-2.3455535680214,-73.8845093109302,
0.));
#130661=CARTESIAN_POINT('Ctrl Pts',(-2.3455535680214,-73.8845093109302,
12.));
#130662=CARTESIAN_POINT('Ctrl Pts',(-2.3338433496398,-73.8600122421502,
0.));
#130663=CARTESIAN_POINT('Ctrl Pts',(-2.3338433496398,-73.8600122421502,
12.));
#130664=CARTESIAN_POINT('Ctrl Pts',(-2.32217097594215,-73.8355369402733,
0.));
#130665=CARTESIAN_POINT('Ctrl Pts',(-2.32217097594215,-73.8355369402733,
12.));
#130666=CARTESIAN_POINT('Ctrl Pts',(-2.31053644289425,-73.8110835039341,
0.));
#130667=CARTESIAN_POINT('Ctrl Pts',(-2.31053644289425,-73.8110835039341,
12.));
#130668=CARTESIAN_POINT('Ctrl Pts',(-2.29893974640435,-73.7866520318849,
0.));
#130669=CARTESIAN_POINT('Ctrl Pts',(-2.29893974640435,-73.7866520318849,
12.));
#130670=CARTESIAN_POINT('Ctrl Pts',(-2.28738088222858,-73.7622426235648,
0.));
#130671=CARTESIAN_POINT('Ctrl Pts',(-2.28738088222858,-73.7622426235648,
12.));
#130672=CARTESIAN_POINT('Ctrl Pts',(-2.27585984587193,-73.7378553796792,
0.));
#130673=CARTESIAN_POINT('Ctrl Pts',(-2.27585984587193,-73.7378553796792,
12.));
#130674=CARTESIAN_POINT('Ctrl Pts',(-2.26437663263663,-73.7134904019378,
0.));
#130675=CARTESIAN_POINT('Ctrl Pts',(-2.26437663263663,-73.7134904019378,
12.));
#130676=CARTESIAN_POINT('Ctrl Pts',(-2.25293123766425,-73.6891477928124,
0.));
#130677=CARTESIAN_POINT('Ctrl Pts',(-2.25293123766425,-73.6891477928124,
12.));
#130678=CARTESIAN_POINT('Ctrl Pts',(-2.24152365597699,-73.6648276552766,
0.));
#130679=CARTESIAN_POINT('Ctrl Pts',(-2.24152365597699,-73.6648276552766,
12.));
#130680=CARTESIAN_POINT('Ctrl Pts',(-2.23015388251289,-73.6405300925714,
0.));
#130681=CARTESIAN_POINT('Ctrl Pts',(-2.23015388251289,-73.6405300925714,
12.));
#130682=CARTESIAN_POINT('Ctrl Pts',(-2.21882191216521,-73.6162552079044,
0.));
#130683=CARTESIAN_POINT('Ctrl Pts',(-2.21882191216521,-73.6162552079044,
12.));
#130684=CARTESIAN_POINT('Ctrl Pts',(-2.20752773978353,-73.5920031044604,
0.));
#130685=CARTESIAN_POINT('Ctrl Pts',(-2.20752773978353,-73.5920031044604,
12.));
#130686=CARTESIAN_POINT('Ctrl Pts',(-2.19627136015683,-73.5677738855461,
0.));
#130687=CARTESIAN_POINT('Ctrl Pts',(-2.19627136015683,-73.5677738855461,
12.));
#130688=CARTESIAN_POINT('Ctrl Pts',(-2.18505276799756,-73.5435676546934,
0.));
#130689=CARTESIAN_POINT('Ctrl Pts',(-2.18505276799756,-73.5435676546934,
12.));
#130690=CARTESIAN_POINT('Ctrl Pts',(-2.17387195792306,-73.5193845157705,
0.));
#130691=CARTESIAN_POINT('Ctrl Pts',(-2.17387195792306,-73.5193845157705,
12.));
#130692=CARTESIAN_POINT('Ctrl Pts',(-2.16272892442915,-73.4952245731044,
0.));
#130693=CARTESIAN_POINT('Ctrl Pts',(-2.16272892442915,-73.4952245731044,
12.));
#130694=CARTESIAN_POINT('Ctrl Pts',(-2.15162366187899,-73.4710879315367,
0.));
#130695=CARTESIAN_POINT('Ctrl Pts',(-2.15162366187899,-73.4710879315367,
12.));
#130696=CARTESIAN_POINT('Ctrl Pts',(-2.14055616452049,-73.4469746963622,
0.));
#130697=CARTESIAN_POINT('Ctrl Pts',(-2.14055616452049,-73.4469746963622,
12.));
#130698=CARTESIAN_POINT('Ctrl Pts',(-2.1295264264936,-73.4228849732914,
0.));
#130699=CARTESIAN_POINT('Ctrl Pts',(-2.1295264264936,-73.4228849732914,
12.));
#130700=CARTESIAN_POINT('Ctrl Pts',(-2.11853444183764,-73.3988188684022,
0.));
#130701=CARTESIAN_POINT('Ctrl Pts',(-2.11853444183764,-73.3988188684022,
12.));
#130702=CARTESIAN_POINT('Ctrl Pts',(-2.10758020449401,-73.3747764880903,
0.));
#130703=CARTESIAN_POINT('Ctrl Pts',(-2.10758020449401,-73.3747764880903,
12.));
#130704=CARTESIAN_POINT('Ctrl Pts',(-2.09666370830733,-73.3507579390254,
0.));
#130705=CARTESIAN_POINT('Ctrl Pts',(-2.09666370830733,-73.3507579390254,
12.));
#130706=CARTESIAN_POINT('Ctrl Pts',(-2.08578494702762,-73.3267633281822,
0.));
#130707=CARTESIAN_POINT('Ctrl Pts',(-2.08578494702762,-73.3267633281822,
12.));
#130708=CARTESIAN_POINT('Ctrl Pts',(-2.07494391430954,-73.3027927628636,
0.));
#130709=CARTESIAN_POINT('Ctrl Pts',(-2.07494391430954,-73.3027927628636,
12.));
#130710=CARTESIAN_POINT('Ctrl Pts',(-2.06414060370837,-73.2788463507248,
0.));
#130711=CARTESIAN_POINT('Ctrl Pts',(-2.06414060370837,-73.2788463507248,
12.));
#130712=CARTESIAN_POINT('Ctrl Pts',(-2.05337500867395,-73.2549241997946,
0.));
#130713=CARTESIAN_POINT('Ctrl Pts',(-2.05337500867395,-73.2549241997946,
12.));
#130714=CARTESIAN_POINT('Ctrl Pts',(-2.04264712253915,-73.2310264184965,
0.));
#130715=CARTESIAN_POINT('Ctrl Pts',(-2.04264712253915,-73.2310264184965,
12.));
#130716=CARTESIAN_POINT('Ctrl Pts',(-2.0319569385244,-73.2071531156492,
0.));
#130717=CARTESIAN_POINT('Ctrl Pts',(-2.0319569385244,-73.2071531156492,
12.));
#130718=CARTESIAN_POINT('Ctrl Pts',(-2.02130444974352,-73.1833044004612,
0.));
#130719=CARTESIAN_POINT('Ctrl Pts',(-2.02130444974352,-73.1833044004612,
12.));
#130720=CARTESIAN_POINT('Ctrl Pts',(-2.01068964920465,-73.159480382525,
0.));
#130721=CARTESIAN_POINT('Ctrl Pts',(-2.01068964920465,-73.159480382525,
12.));
#130722=CARTESIAN_POINT('Ctrl Pts',(-2.00011252980987,-73.1356811718094,
0.));
#130723=CARTESIAN_POINT('Ctrl Pts',(-2.00011252980987,-73.1356811718094,
12.));
#130724=CARTESIAN_POINT('Ctrl Pts',(-1.9895730843493,-73.1119068786482,
0.));
#130725=CARTESIAN_POINT('Ctrl Pts',(-1.9895730843493,-73.1119068786482,
12.));
#130726=CARTESIAN_POINT('Ctrl Pts',(-1.97907130550172,-73.0881576137415,
0.));
#130727=CARTESIAN_POINT('Ctrl Pts',(-1.97907130550172,-73.0881576137415,
12.));
#130728=CARTESIAN_POINT('Ctrl Pts',(-1.96860718583944,-73.0644334881679,
0.));
#130729=CARTESIAN_POINT('Ctrl Pts',(-1.96860718583944,-73.0644334881679,
12.));
#130730=CARTESIAN_POINT('Ctrl Pts',(-1.95818071782773,-73.0407346133912,
0.));
#130731=CARTESIAN_POINT('Ctrl Pts',(-1.95818071782773,-73.0407346133912,
12.));
#130732=CARTESIAN_POINT('Ctrl Pts',(-1.947791893823,-73.0170611012659,0.));
#130733=CARTESIAN_POINT('Ctrl Pts',(-1.947791893823,-73.0170611012659,12.));
#130734=CARTESIAN_POINT('Ctrl Pts',(-1.93744070606557,-72.9934130640414,
0.));
#130735=CARTESIAN_POINT('Ctrl Pts',(-1.93744070606557,-72.9934130640414,
12.));
#130736=CARTESIAN_POINT('Ctrl Pts',(-1.92712714667648,-72.9697906143638,
0.));
#130737=CARTESIAN_POINT('Ctrl Pts',(-1.92712714667648,-72.9697906143638,
12.));
#130738=CARTESIAN_POINT('Ctrl Pts',(-1.91685120766428,-72.9461938652816,
0.));
#130739=CARTESIAN_POINT('Ctrl Pts',(-1.91685120766428,-72.9461938652816,
12.));
#130740=CARTESIAN_POINT('Ctrl Pts',(-1.90661288092583,-72.9226229302483,
0.));
#130741=CARTESIAN_POINT('Ctrl Pts',(-1.90661288092583,-72.9226229302483,
12.));
#130742=CARTESIAN_POINT('Ctrl Pts',(-1.89641215824584,-72.8990779231226,
0.));
#130743=CARTESIAN_POINT('Ctrl Pts',(-1.89641215824584,-72.8990779231226,
12.));
#130744=CARTESIAN_POINT('Ctrl Pts',(-1.88624903129195,-72.8755589581674,
0.));
#130745=CARTESIAN_POINT('Ctrl Pts',(-1.88624903129195,-72.8755589581674,
12.));
#130746=CARTESIAN_POINT('Ctrl Pts',(-1.87612349160952,-72.8520661500465,
0.));
#130747=CARTESIAN_POINT('Ctrl Pts',(-1.87612349160952,-72.8520661500465,
12.));
#130748=CARTESIAN_POINT('Ctrl Pts',(-1.86603553062776,-72.8285996138346,
0.));
#130749=CARTESIAN_POINT('Ctrl Pts',(-1.86603553062776,-72.8285996138346,
12.));
#130750=CARTESIAN_POINT('Ctrl Pts',(-1.85598513966115,-72.8051594650214,
0.));
#130751=CARTESIAN_POINT('Ctrl Pts',(-1.85598513966115,-72.8051594650214,
12.));
#130752=CARTESIAN_POINT('Ctrl Pts',(-1.84597230990858,-72.7817458195155,
0.));
#130753=CARTESIAN_POINT('Ctrl Pts',(-1.84597230990858,-72.7817458195155,
12.));
#130754=CARTESIAN_POINT('Ctrl Pts',(-1.83599703244926,-72.7583587936454,
0.));
#130755=CARTESIAN_POINT('Ctrl Pts',(-1.83599703244926,-72.7583587936454,
12.));
#130756=CARTESIAN_POINT('Ctrl Pts',(-1.82605929823565,-72.73499850416,0.));
#130757=CARTESIAN_POINT('Ctrl Pts',(-1.82605929823565,-72.73499850416,12.));
#130758=CARTESIAN_POINT('Ctrl Pts',(-1.81615909809872,-72.7116650682347,
0.));
#130759=CARTESIAN_POINT('Ctrl Pts',(-1.81615909809872,-72.7116650682347,
12.));
#130760=CARTESIAN_POINT('Ctrl Pts',(-1.80629642275051,-72.6883586034768,
0.));
#130761=CARTESIAN_POINT('Ctrl Pts',(-1.80629642275051,-72.6883586034768,
12.));
#130762=CARTESIAN_POINT('Ctrl Pts',(-1.79647126278359,-72.6650792279271,
0.));
#130763=CARTESIAN_POINT('Ctrl Pts',(-1.79647126278359,-72.6650792279271,
12.));
#130764=CARTESIAN_POINT('Ctrl Pts',(-1.78668360866813,-72.6418270600623,
0.));
#130765=CARTESIAN_POINT('Ctrl Pts',(-1.78668360866813,-72.6418270600623,
12.));
#130766=CARTESIAN_POINT('Ctrl Pts',(-1.7769334507443,-72.618602218792,0.));
#130767=CARTESIAN_POINT('Ctrl Pts',(-1.7769334507443,-72.618602218792,12.));
#130768=CARTESIAN_POINT('Ctrl Pts',(-1.7672207792258,-72.5954048234655,
0.));
#130769=CARTESIAN_POINT('Ctrl Pts',(-1.7672207792258,-72.5954048234655,
12.));
#130770=CARTESIAN_POINT('Ctrl Pts',(-1.7575455842035,-72.5722349938789,
0.));
#130771=CARTESIAN_POINT('Ctrl Pts',(-1.7575455842035,-72.5722349938789,
12.));
#130772=CARTESIAN_POINT('Ctrl Pts',(-1.74790785564476,-72.5490928502773,
0.));
#130773=CARTESIAN_POINT('Ctrl Pts',(-1.74790785564476,-72.5490928502773,
12.));
#130774=CARTESIAN_POINT('Ctrl Pts',(-1.73830758339123,-72.5259785133586,
0.));
#130775=CARTESIAN_POINT('Ctrl Pts',(-1.73830758339123,-72.5259785133586,
12.));
#130776=CARTESIAN_POINT('Ctrl Pts',(-1.72874475715098,-72.5028921042704,
0.));
#130777=CARTESIAN_POINT('Ctrl Pts',(-1.72874475715098,-72.5028921042704,
12.));
#130778=CARTESIAN_POINT('Ctrl Pts',(-1.71921936650032,-72.4798337446162,
0.));
#130779=CARTESIAN_POINT('Ctrl Pts',(-1.71921936650032,-72.4798337446162,
12.));
#130780=CARTESIAN_POINT('Ctrl Pts',(-1.70973140088837,-72.4568035564618,
0.));
#130781=CARTESIAN_POINT('Ctrl Pts',(-1.70973140088837,-72.4568035564618,
12.));
#130782=CARTESIAN_POINT('Ctrl Pts',(-1.70028084963647,-72.4338016623388,
0.));
#130783=CARTESIAN_POINT('Ctrl Pts',(-1.70028084963647,-72.4338016623388,
12.));
#130784=CARTESIAN_POINT('Ctrl Pts',(-1.69086770193641,-72.4108281852473,
0.));
#130785=CARTESIAN_POINT('Ctrl Pts',(-1.69086770193641,-72.4108281852473,
12.));
#130786=CARTESIAN_POINT('Ctrl Pts',(-1.68149194684288,-72.3878832486549,
0.));
#130787=CARTESIAN_POINT('Ctrl Pts',(-1.68149194684288,-72.3878832486549,
12.));
#130788=CARTESIAN_POINT('Ctrl Pts',(-1.67215357327372,-72.3649669765013,
0.));
#130789=CARTESIAN_POINT('Ctrl Pts',(-1.67215357327372,-72.3649669765013,
12.));
#130790=CARTESIAN_POINT('Ctrl Pts',(-1.66285257001502,-72.3420794932052,
0.));
#130791=CARTESIAN_POINT('Ctrl Pts',(-1.66285257001502,-72.3420794932052,
12.));
#130792=CARTESIAN_POINT('Ctrl Pts',(-1.65358892572066,-72.3192209236691,
0.));
#130793=CARTESIAN_POINT('Ctrl Pts',(-1.65358892572066,-72.3192209236691,
12.));
#130794=CARTESIAN_POINT('Ctrl Pts',(-1.64436262891078,-72.2963913932811,
0.));
#130795=CARTESIAN_POINT('Ctrl Pts',(-1.64436262891078,-72.2963913932811,
12.));
#130796=CARTESIAN_POINT('Ctrl Pts',(-1.63517366796459,-72.2735910279149,
0.));
#130797=CARTESIAN_POINT('Ctrl Pts',(-1.63517366796459,-72.2735910279149,
12.));
#130798=CARTESIAN_POINT('Ctrl Pts',(-1.62602203111924,-72.2508199539325,
0.));
#130799=CARTESIAN_POINT('Ctrl Pts',(-1.62602203111924,-72.2508199539325,
12.));
#130800=CARTESIAN_POINT('Ctrl Pts',(-1.61690770647536,-72.2280782981941,
0.));
#130801=CARTESIAN_POINT('Ctrl Pts',(-1.61690770647536,-72.2280782981941,
12.));
#130802=CARTESIAN_POINT('Ctrl Pts',(-1.60783068199662,-72.2053661880611,
0.));
#130803=CARTESIAN_POINT('Ctrl Pts',(-1.60783068199662,-72.2053661880611,
12.));
#130804=CARTESIAN_POINT('Ctrl Pts',(-1.5987909455085,-72.1826837514,0.));
#130805=CARTESIAN_POINT('Ctrl Pts',(-1.5987909455085,-72.1826837514,12.));
#130806=CARTESIAN_POINT('Ctrl Pts',(-1.58978848469128,-72.1600311165813,
0.));
#130807=CARTESIAN_POINT('Ctrl Pts',(-1.58978848469128,-72.1600311165813,
12.));
#130808=CARTESIAN_POINT('Ctrl Pts',(-1.58082328707808,-72.1374084124829,
0.));
#130809=CARTESIAN_POINT('Ctrl Pts',(-1.58082328707808,-72.1374084124829,
12.));
#130810=CARTESIAN_POINT('Ctrl Pts',(-1.57189534006043,-72.1148157684987,
0.));
#130811=CARTESIAN_POINT('Ctrl Pts',(-1.57189534006043,-72.1148157684987,
12.));
#130812=CARTESIAN_POINT('Ctrl Pts',(-1.56300463088811,-72.092253314543,
0.));
#130813=CARTESIAN_POINT('Ctrl Pts',(-1.56300463088811,-72.092253314543,
12.));
#130814=CARTESIAN_POINT('Ctrl Pts',(-1.55415114666774,-72.0697211810548,
0.));
#130815=CARTESIAN_POINT('Ctrl Pts',(-1.55415114666774,-72.0697211810548,
12.));
#130816=CARTESIAN_POINT('Ctrl Pts',(-1.54533487435626,-72.0472194989968,
0.));
#130817=CARTESIAN_POINT('Ctrl Pts',(-1.54533487435626,-72.0472194989968,
12.));
#130818=CARTESIAN_POINT('Ctrl Pts',(-1.53655580075814,-72.0247483998582,
0.));
#130819=CARTESIAN_POINT('Ctrl Pts',(-1.53655580075814,-72.0247483998582,
12.));
#130820=CARTESIAN_POINT('Ctrl Pts',(-1.52781391253103,-72.0023080156647,
0.));
#130821=CARTESIAN_POINT('Ctrl Pts',(-1.52781391253103,-72.0023080156647,
12.));
#130822=CARTESIAN_POINT('Ctrl Pts',(-1.51910919618567,-71.9798984789828,
0.));
#130823=CARTESIAN_POINT('Ctrl Pts',(-1.51910919618567,-71.9798984789828,
12.));
#130824=CARTESIAN_POINT('Ctrl Pts',(-1.51044163808455,-71.9575199229241,
0.));
#130825=CARTESIAN_POINT('Ctrl Pts',(-1.51044163808455,-71.9575199229241,
12.));
#130826=CARTESIAN_POINT('Ctrl Pts',(-1.50181122443535,-71.935172481145,
0.));
#130827=CARTESIAN_POINT('Ctrl Pts',(-1.50181122443535,-71.935172481145,
12.));
#130828=CARTESIAN_POINT('Ctrl Pts',(-1.493217941288,-71.9128562878491,0.));
#130829=CARTESIAN_POINT('Ctrl Pts',(-1.493217941288,-71.9128562878491,12.));
#130830=CARTESIAN_POINT('Ctrl Pts',(-1.48466177454021,-71.8905714777972,
0.));
#130831=CARTESIAN_POINT('Ctrl Pts',(-1.48466177454021,-71.8905714777972,
12.));
#130832=CARTESIAN_POINT('Ctrl Pts',(-1.4761427099373,-71.8683181863123,
0.));
#130833=CARTESIAN_POINT('Ctrl Pts',(-1.4761427099373,-71.8683181863123,
12.));
#130834=CARTESIAN_POINT('Ctrl Pts',(-1.46766073307089,-71.8460965492836,
0.));
#130835=CARTESIAN_POINT('Ctrl Pts',(-1.46766073307089,-71.8460965492836,
12.));
#130836=CARTESIAN_POINT('Ctrl Pts',(-1.45921582937229,-71.8239067031664,
0.));
#130837=CARTESIAN_POINT('Ctrl Pts',(-1.45921582937229,-71.8239067031664,
12.));
#130838=CARTESIAN_POINT('Ctrl Pts',(-1.45080798410957,-71.8017487849865,
0.));
#130839=CARTESIAN_POINT('Ctrl Pts',(-1.45080798410957,-71.8017487849865,
12.));
#130840=CARTESIAN_POINT('Ctrl Pts',(-1.44243718239305,-71.7796229323496,
0.));
#130841=CARTESIAN_POINT('Ctrl Pts',(-1.44243718239305,-71.7796229323496,
12.));
#130842=CARTESIAN_POINT('Ctrl Pts',(-1.43410340917489,-71.7575292834456,
0.));
#130843=CARTESIAN_POINT('Ctrl Pts',(-1.43410340917489,-71.7575292834456,
12.));
#130844=CARTESIAN_POINT('Ctrl Pts',(-1.42580664924774,-71.7354679770537,
0.));
#130845=CARTESIAN_POINT('Ctrl Pts',(-1.42580664924774,-71.7354679770537,
12.));
#130846=CARTESIAN_POINT('Ctrl Pts',(-1.41754688723791,-71.7134391525417,
0.));
#130847=CARTESIAN_POINT('Ctrl Pts',(-1.41754688723791,-71.7134391525417,
12.));
#130848=CARTESIAN_POINT('Ctrl Pts',(-1.40932410760275,-71.6914429498702,
0.));
#130849=CARTESIAN_POINT('Ctrl Pts',(-1.40932410760275,-71.6914429498702,
12.));
#130850=CARTESIAN_POINT('Ctrl Pts',(-1.401138294636,-71.6694795096034,0.));
#130851=CARTESIAN_POINT('Ctrl Pts',(-1.401138294636,-71.6694795096034,12.));
#130852=CARTESIAN_POINT('Ctrl Pts',(-1.39298943246731,-71.6475489729149,
0.));
#130853=CARTESIAN_POINT('Ctrl Pts',(-1.39298943246731,-71.6475489729149,
12.));
#130854=CARTESIAN_POINT('Ctrl Pts',(-1.38487750506076,-71.6256514815918,
0.));
#130855=CARTESIAN_POINT('Ctrl Pts',(-1.38487750506076,-71.6256514815918,
12.));
#130856=CARTESIAN_POINT('Ctrl Pts',(-1.37680249620763,-71.6037871780347,
0.));
#130857=CARTESIAN_POINT('Ctrl Pts',(-1.37680249620763,-71.6037871780347,
12.));
#130858=CARTESIAN_POINT('Ctrl Pts',(-1.36876438952449,-71.5819562052613,
0.));
#130859=CARTESIAN_POINT('Ctrl Pts',(-1.36876438952449,-71.5819562052613,
12.));
#130860=CARTESIAN_POINT('Ctrl Pts',(-1.36076316845806,-71.5601587069175,
0.));
#130861=CARTESIAN_POINT('Ctrl Pts',(-1.36076316845806,-71.5601587069175,
12.));
#130862=CARTESIAN_POINT('Ctrl Pts',(-1.35279881628453,-71.538394827283,
0.));
#130863=CARTESIAN_POINT('Ctrl Pts',(-1.35279881628453,-71.538394827283,
12.));
#130864=CARTESIAN_POINT('Ctrl Pts',(-1.34487131610785,-71.5166647112766,
0.));
#130865=CARTESIAN_POINT('Ctrl Pts',(-1.34487131610785,-71.5166647112766,
12.));
#130866=CARTESIAN_POINT('Ctrl Pts',(-1.33698065085228,-71.4949685044559,
0.));
#130867=CARTESIAN_POINT('Ctrl Pts',(-1.33698065085228,-71.4949685044559,
12.));
#130868=CARTESIAN_POINT('Ctrl Pts',(-1.32912680326131,-71.4733063530227,
0.));
#130869=CARTESIAN_POINT('Ctrl Pts',(-1.32912680326131,-71.4733063530227,
12.));
#130870=CARTESIAN_POINT('Ctrl Pts',(-1.32130975590231,-71.4516784038346,
0.));
#130871=CARTESIAN_POINT('Ctrl Pts',(-1.32130975590231,-71.4516784038346,
12.));
#130872=CARTESIAN_POINT('Ctrl Pts',(-1.31352949116539,-71.4300848044095,
0.));
#130873=CARTESIAN_POINT('Ctrl Pts',(-1.31352949116539,-71.4300848044095,
12.));
#130874=CARTESIAN_POINT('Ctrl Pts',(-1.30578599126139,-71.4085257029308,
0.));
#130875=CARTESIAN_POINT('Ctrl Pts',(-1.30578599126139,-71.4085257029308,
12.));
#130876=CARTESIAN_POINT('Ctrl Pts',(-1.29807923821414,-71.3870012482474,
0.));
#130877=CARTESIAN_POINT('Ctrl Pts',(-1.29807923821414,-71.3870012482474,
12.));
#130878=CARTESIAN_POINT('Ctrl Pts',(-1.29040921386061,-71.3655115898801,
0.));
#130879=CARTESIAN_POINT('Ctrl Pts',(-1.29040921386061,-71.3655115898801,
12.));
#130880=CARTESIAN_POINT('Ctrl Pts',(-1.28277589985475,-71.344056878033,
0.));
#130881=CARTESIAN_POINT('Ctrl Pts',(-1.28277589985475,-71.344056878033,
12.));
#130882=CARTESIAN_POINT('Ctrl Pts',(-1.27517927766611,-71.3226372635993,
0.));
#130883=CARTESIAN_POINT('Ctrl Pts',(-1.27517927766611,-71.3226372635993,
12.));
#130884=CARTESIAN_POINT('Ctrl Pts',(-1.26761932857723,-71.301252898167,
0.));
#130885=CARTESIAN_POINT('Ctrl Pts',(-1.26761932857723,-71.301252898167,
12.));
#130886=CARTESIAN_POINT('Ctrl Pts',(-1.26009603367565,-71.2799039340191,
0.));
#130887=CARTESIAN_POINT('Ctrl Pts',(-1.26009603367565,-71.2799039340191,
12.));
#130888=CARTESIAN_POINT('Ctrl Pts',(-1.25260937385561,-71.2585905241422,
0.));
#130889=CARTESIAN_POINT('Ctrl Pts',(-1.25260937385561,-71.2585905241422,
12.));
#130890=CARTESIAN_POINT('Ctrl Pts',(-1.24515932982108,-71.2373128222359,
0.));
#130891=CARTESIAN_POINT('Ctrl Pts',(-1.24515932982108,-71.2373128222359,
12.));
#130892=CARTESIAN_POINT('Ctrl Pts',(-1.23774588208427,-71.2160709827189,
0.));
#130893=CARTESIAN_POINT('Ctrl Pts',(-1.23774588208427,-71.2160709827189,
12.));
#130894=CARTESIAN_POINT('Ctrl Pts',(-1.23036901096246,-71.1948651607319,
0.));
#130895=CARTESIAN_POINT('Ctrl Pts',(-1.23036901096246,-71.1948651607319,
12.));
#130896=CARTESIAN_POINT('Ctrl Pts',(-1.22302869657028,-71.1736955121361,
0.));
#130897=CARTESIAN_POINT('Ctrl Pts',(-1.22302869657028,-71.1736955121361,
12.));
#130898=CARTESIAN_POINT('Ctrl Pts',(-1.21572491882273,-71.1525621935266,
0.));
#130899=CARTESIAN_POINT('Ctrl Pts',(-1.21572491882273,-71.1525621935266,
12.));
#130900=CARTESIAN_POINT('Ctrl Pts',(-1.20845765743654,-71.1314653622442,
0.));
#130901=CARTESIAN_POINT('Ctrl Pts',(-1.20845765743654,-71.1314653622442,
12.));
#130902=CARTESIAN_POINT('Ctrl Pts',(-1.20122689192836,-71.1104051763839,
0.));
#130903=CARTESIAN_POINT('Ctrl Pts',(-1.20122689192836,-71.1104051763839,
12.));
#130904=CARTESIAN_POINT('Ctrl Pts',(-1.19403260160998,-71.089381794801,
0.));
#130905=CARTESIAN_POINT('Ctrl Pts',(-1.19403260160998,-71.089381794801,
12.));
#130906=CARTESIAN_POINT('Ctrl Pts',(-1.18687476558127,-71.0683953771147,
0.));
#130907=CARTESIAN_POINT('Ctrl Pts',(-1.18687476558127,-71.0683953771147,
12.));
#130908=CARTESIAN_POINT('Ctrl Pts',(-1.179753362735,-71.0474460837157,0.));
#130909=CARTESIAN_POINT('Ctrl Pts',(-1.179753362735,-71.0474460837157,12.));
#130910=CARTESIAN_POINT('Ctrl Pts',(-1.17266837175776,-71.0265340757697,
0.));
#130911=CARTESIAN_POINT('Ctrl Pts',(-1.17266837175776,-71.0265340757697,
12.));
#130912=CARTESIAN_POINT('Ctrl Pts',(-1.16561977112882,-71.0056595152204,
0.));
#130913=CARTESIAN_POINT('Ctrl Pts',(-1.16561977112882,-71.0056595152204,
12.));
#130914=CARTESIAN_POINT('Ctrl Pts',(-1.1586075391149,-70.9848225647876,
0.));
#130915=CARTESIAN_POINT('Ctrl Pts',(-1.1586075391149,-70.9848225647876,
12.));
#130916=CARTESIAN_POINT('Ctrl Pts',(-1.1516316537653,-70.9640233879671,
0.));
#130917=CARTESIAN_POINT('Ctrl Pts',(-1.1516316537653,-70.9640233879671,
12.));
#130918=CARTESIAN_POINT('Ctrl Pts',(-1.14469209291494,-70.943262149058,
0.));
#130919=CARTESIAN_POINT('Ctrl Pts',(-1.14469209291494,-70.943262149058,
12.));
#130920=CARTESIAN_POINT('Ctrl Pts',(-1.13778883418216,-70.9225390131835,
0.));
#130921=CARTESIAN_POINT('Ctrl Pts',(-1.13778883418216,-70.9225390131835,
12.));
#130922=CARTESIAN_POINT('Ctrl Pts',(-1.13092185496563,-70.9018541463083,
0.));
#130923=CARTESIAN_POINT('Ctrl Pts',(-1.13092185496563,-70.9018541463083,
12.));
#130924=CARTESIAN_POINT('Ctrl Pts',(-1.12409113243511,-70.8812077152564,
0.));
#130925=CARTESIAN_POINT('Ctrl Pts',(-1.12409113243511,-70.8812077152564,
12.));
#130926=CARTESIAN_POINT('Ctrl Pts',(-1.1172966435299,-70.860599887712,0.));
#130927=CARTESIAN_POINT('Ctrl Pts',(-1.1172966435299,-70.860599887712,12.));
#130928=CARTESIAN_POINT('Ctrl Pts',(-1.11053836496638,-70.8400308322013,
0.));
#130929=CARTESIAN_POINT('Ctrl Pts',(-1.11053836496638,-70.8400308322013,
12.));
#130930=CARTESIAN_POINT('Ctrl Pts',(-1.10381627323946,-70.8195007180739,
0.));
#130931=CARTESIAN_POINT('Ctrl Pts',(-1.10381627323946,-70.8195007180739,
12.));
#130932=CARTESIAN_POINT('Ctrl Pts',(-1.0971303446227,-70.7990097154855,
0.));
#130933=CARTESIAN_POINT('Ctrl Pts',(-1.0971303446227,-70.7990097154855,
12.));
#130934=CARTESIAN_POINT('Ctrl Pts',(-1.09048055516434,-70.7785579953611,
0.));
#130935=CARTESIAN_POINT('Ctrl Pts',(-1.09048055516434,-70.7785579953611,
12.));
#130936=CARTESIAN_POINT('Ctrl Pts',(-1.08386688068349,-70.7581457294475,
0.));
#130937=CARTESIAN_POINT('Ctrl Pts',(-1.08386688068349,-70.7581457294475,
12.));
#130938=CARTESIAN_POINT('Ctrl Pts',(-1.07728929676412,-70.737773090397,
0.));
#130939=CARTESIAN_POINT('Ctrl Pts',(-1.07728929676412,-70.737773090397,
12.));
#130940=CARTESIAN_POINT('Ctrl Pts',(-1.07074777874596,-70.7174402518378,
0.));
#130941=CARTESIAN_POINT('Ctrl Pts',(-1.07074777874596,-70.7174402518378,
12.));
#130942=CARTESIAN_POINT('Ctrl Pts',(-1.0642423017128,-70.6971473884443,
0.));
#130943=CARTESIAN_POINT('Ctrl Pts',(-1.0642423017128,-70.6971473884443,
12.));
#130944=CARTESIAN_POINT('Ctrl Pts',(-1.05777284047728,-70.6768946760063,
0.));
#130945=CARTESIAN_POINT('Ctrl Pts',(-1.05777284047728,-70.6768946760063,
12.));
#130946=CARTESIAN_POINT('Ctrl Pts',(-1.05133936960069,-70.6566822912965,
0.));
#130947=CARTESIAN_POINT('Ctrl Pts',(-1.05133936960069,-70.6566822912965,
12.));
#130948=CARTESIAN_POINT('Ctrl Pts',(-1.04494186341156,-70.6365104119238,
0.));
#130949=CARTESIAN_POINT('Ctrl Pts',(-1.04494186341156,-70.6365104119238,
12.));
#130950=CARTESIAN_POINT('Ctrl Pts',(-1.03858029601906,-70.6163792162079,
0.));
#130951=CARTESIAN_POINT('Ctrl Pts',(-1.03858029601906,-70.6163792162079,
12.));
#130952=CARTESIAN_POINT('Ctrl Pts',(-1.03225464132872,-70.5962888829958,
0.));
#130953=CARTESIAN_POINT('Ctrl Pts',(-1.03225464132872,-70.5962888829958,
12.));
#130954=CARTESIAN_POINT('Ctrl Pts',(-1.02596487304049,-70.5762395916412,
0.));
#130955=CARTESIAN_POINT('Ctrl Pts',(-1.02596487304049,-70.5762395916412,
12.));
#130956=CARTESIAN_POINT('Ctrl Pts',(-1.01971096460599,-70.5562315224219,
0.));
#130957=CARTESIAN_POINT('Ctrl Pts',(-1.01971096460599,-70.5562315224219,
12.));
#130958=CARTESIAN_POINT('Ctrl Pts',(-1.0134928891854,-70.5362648569072,
0.));
#130959=CARTESIAN_POINT('Ctrl Pts',(-1.0134928891854,-70.5362648569072,
12.));
#130960=CARTESIAN_POINT('Ctrl Pts',(-1.00731061960968,-70.5163397782699,
0.));
#130961=CARTESIAN_POINT('Ctrl Pts',(-1.00731061960968,-70.5163397782699,
12.));
#130962=CARTESIAN_POINT('Ctrl Pts',(-1.00116412831438,-70.4964564717917,
0.));
#130963=CARTESIAN_POINT('Ctrl Pts',(-1.00116412831438,-70.4964564717917,
12.));
#130964=CARTESIAN_POINT('Ctrl Pts',(-0.995053387379681,-70.476615124517,
0.));
#130965=CARTESIAN_POINT('Ctrl Pts',(-0.995053387379681,-70.476615124517,
12.));
#130966=CARTESIAN_POINT('Ctrl Pts',(-0.98897836864359,-70.4568159243131,
0.));
#130967=CARTESIAN_POINT('Ctrl Pts',(-0.98897836864359,-70.4568159243131,
12.));
#130968=CARTESIAN_POINT('Ctrl Pts',(-0.982939043792158,-70.4370590590839,
0.));
#130969=CARTESIAN_POINT('Ctrl Pts',(-0.982939043792158,-70.4370590590839,
12.));
#130970=CARTESIAN_POINT('Ctrl Pts',(-0.976935384450128,-70.41734471596,
0.));
#130971=CARTESIAN_POINT('Ctrl Pts',(-0.976935384450128,-70.41734471596,
12.));
#130972=CARTESIAN_POINT('Ctrl Pts',(-0.970967362281301,-70.3976730803664,
0.));
#130973=CARTESIAN_POINT('Ctrl Pts',(-0.970967362281301,-70.3976730803664,
12.));
#130974=CARTESIAN_POINT('Ctrl Pts',(-0.965034948786559,-70.3780443378003,
0.));
#130975=CARTESIAN_POINT('Ctrl Pts',(-0.965034948786559,-70.3780443378003,
12.));
#130976=CARTESIAN_POINT('Ctrl Pts',(-0.959138115058886,-70.3584586759561,
0.));
#130977=CARTESIAN_POINT('Ctrl Pts',(-0.959138115058886,-70.3584586759561,
12.));
#130978=CARTESIAN_POINT('Ctrl Pts',(-0.953276831581232,-70.338916286457,
0.));
#130979=CARTESIAN_POINT('Ctrl Pts',(-0.953276831581232,-70.338916286457,
12.));
#130980=CARTESIAN_POINT('Ctrl Pts',(-0.947451067929564,-70.3194173673635,
0.));
#130981=CARTESIAN_POINT('Ctrl Pts',(-0.947451067929564,-70.3194173673635,
12.));
#130982=CARTESIAN_POINT('Ctrl Pts',(-0.941660792742953,-70.2999621233938,
0.));
#130983=CARTESIAN_POINT('Ctrl Pts',(-0.941660792742953,-70.2999621233938,
12.));
#130984=CARTESIAN_POINT('Ctrl Pts',(-0.935905974336492,-70.2805507606832,
0.));
#130985=CARTESIAN_POINT('Ctrl Pts',(-0.935905974336492,-70.2805507606832,
12.));
#130986=CARTESIAN_POINT('Ctrl Pts',(-0.930186581235576,-70.2611834821711,
0.));
#130987=CARTESIAN_POINT('Ctrl Pts',(-0.930186581235576,-70.2611834821711,
12.));
#130988=CARTESIAN_POINT('Ctrl Pts',(-0.924502582639453,-70.241860483586,
0.));
#130989=CARTESIAN_POINT('Ctrl Pts',(-0.924502582639453,-70.241860483586,
12.));
#130990=CARTESIAN_POINT('Ctrl Pts',(-0.918853949157045,-70.2225819470306,
0.));
#130991=CARTESIAN_POINT('Ctrl Pts',(-0.918853949157045,-70.2225819470306,
12.));
#130992=CARTESIAN_POINT('Ctrl Pts',(-0.913240652090839,-70.2033480471749,
0.));
#130993=CARTESIAN_POINT('Ctrl Pts',(-0.913240652090839,-70.2033480471749,
12.));
#130994=CARTESIAN_POINT('Ctrl Pts',(-0.90766266201565,-70.184158963563,
0.));
#130995=CARTESIAN_POINT('Ctrl Pts',(-0.90766266201565,-70.184158963563,
12.));
#130996=CARTESIAN_POINT('Ctrl Pts',(-0.902119947629773,-70.1650148905109,
0.));
#130997=CARTESIAN_POINT('Ctrl Pts',(-0.902119947629773,-70.1650148905109,
12.));
#130998=CARTESIAN_POINT('Ctrl Pts',(-0.896612474372085,-70.1459160490366,
0.));
#130999=CARTESIAN_POINT('Ctrl Pts',(-0.896612474372085,-70.1459160490366,
12.));
#131000=CARTESIAN_POINT('Ctrl Pts',(-0.891140203464724,-70.1268626950031,
0.));
#131001=CARTESIAN_POINT('Ctrl Pts',(-0.891140203464724,-70.1268626950031,
12.));
#131002=CARTESIAN_POINT('Ctrl Pts',(-0.885703094803086,-70.1078550938801,
0.));
#131003=CARTESIAN_POINT('Ctrl Pts',(-0.885703094803086,-70.1078550938801,
12.));
#131004=CARTESIAN_POINT('Ctrl Pts',(-0.880301109661037,-70.0888934967772,
0.));
#131005=CARTESIAN_POINT('Ctrl Pts',(-0.880301109661037,-70.0888934967772,
12.));
#131006=CARTESIAN_POINT('Ctrl Pts',(-0.87493421325557,-70.0699781184013,
0.));
#131007=CARTESIAN_POINT('Ctrl Pts',(-0.87493421325557,-70.0699781184013,
12.));
#131008=CARTESIAN_POINT('Ctrl Pts',(-0.869602377870139,-70.0511091083285,
0.));
#131009=CARTESIAN_POINT('Ctrl Pts',(-0.869602377870139,-70.0511091083285,
12.));
#131010=CARTESIAN_POINT('Ctrl Pts',(-0.86430558366009,-70.0322865493339,
0.));
#131011=CARTESIAN_POINT('Ctrl Pts',(-0.86430558366009,-70.0322865493339,
12.));
#131012=CARTESIAN_POINT('Ctrl Pts',(-0.860096170667398,-70.0172656934192,
0.));
#131013=CARTESIAN_POINT('Ctrl Pts',(-0.860096170667398,-70.0172656934192,
12.));
#131014=CARTESIAN_POINT('Ctrl Pts',(-0.856954870258371,-70.0060209754332,
0.));
#131015=CARTESIAN_POINT('Ctrl Pts',(-0.856954870258371,-70.0060209754332,
12.));
#131016=CARTESIAN_POINT('Ctrl Pts',(-0.854867673848293,-69.9985337959499,
0.));
#131017=CARTESIAN_POINT('Ctrl Pts',(-0.854867673848293,-69.9985337959499,
12.));
#131018=CARTESIAN_POINT('Ctrl Pts',(-0.853825826608993,-69.9947925310006,
0.));
#131019=CARTESIAN_POINT('Ctrl Pts',(-0.853825826608993,-69.9947925310006,
12.));
#131020=CARTESIAN_POINT('',(-0.853825826608993,-69.9947925310006,12.));
#131021=CARTESIAN_POINT('Ctrl Pts',(-0.853825826608993,-69.9947925310006,
12.));
#131022=CARTESIAN_POINT('Ctrl Pts',(-0.854867673848293,-69.9985337959499,
12.));
#131023=CARTESIAN_POINT('Ctrl Pts',(-0.856954870258371,-70.0060209754332,
12.));
#131024=CARTESIAN_POINT('Ctrl Pts',(-0.860096170667398,-70.0172656934192,
12.));
#131025=CARTESIAN_POINT('Ctrl Pts',(-0.86430558366009,-70.0322865493339,
12.));
#131026=CARTESIAN_POINT('Ctrl Pts',(-0.869602377870139,-70.0511091083285,
12.));
#131027=CARTESIAN_POINT('Ctrl Pts',(-0.87493421325557,-70.0699781184013,
12.));
#131028=CARTESIAN_POINT('Ctrl Pts',(-0.880301109661037,-70.0888934967772,
12.));
#131029=CARTESIAN_POINT('Ctrl Pts',(-0.885703094803086,-70.1078550938801,
12.));
#131030=CARTESIAN_POINT('Ctrl Pts',(-0.891140203464724,-70.1268626950031,
12.));
#131031=CARTESIAN_POINT('Ctrl Pts',(-0.896612474372085,-70.1459160490366,
12.));
#131032=CARTESIAN_POINT('Ctrl Pts',(-0.902119947629773,-70.1650148905109,
12.));
#131033=CARTESIAN_POINT('Ctrl Pts',(-0.90766266201565,-70.184158963563,
12.));
#131034=CARTESIAN_POINT('Ctrl Pts',(-0.913240652090839,-70.2033480471749,
12.));
#131035=CARTESIAN_POINT('Ctrl Pts',(-0.918853949157045,-70.2225819470306,
12.));
#131036=CARTESIAN_POINT('Ctrl Pts',(-0.924502582639453,-70.241860483586,
12.));
#131037=CARTESIAN_POINT('Ctrl Pts',(-0.930186581235576,-70.2611834821711,
12.));
#131038=CARTESIAN_POINT('Ctrl Pts',(-0.935905974336492,-70.2805507606832,
12.));
#131039=CARTESIAN_POINT('Ctrl Pts',(-0.941660792742953,-70.2999621233938,
12.));
#131040=CARTESIAN_POINT('Ctrl Pts',(-0.947451067929564,-70.3194173673635,
12.));
#131041=CARTESIAN_POINT('Ctrl Pts',(-0.953276831581232,-70.338916286457,
12.));
#131042=CARTESIAN_POINT('Ctrl Pts',(-0.959138115058886,-70.3584586759561,
12.));
#131043=CARTESIAN_POINT('Ctrl Pts',(-0.965034948786559,-70.3780443378003,
12.));
#131044=CARTESIAN_POINT('Ctrl Pts',(-0.970967362281301,-70.3976730803664,
12.));
#131045=CARTESIAN_POINT('Ctrl Pts',(-0.976935384450128,-70.41734471596,
12.));
#131046=CARTESIAN_POINT('Ctrl Pts',(-0.982939043792158,-70.4370590590839,
12.));
#131047=CARTESIAN_POINT('Ctrl Pts',(-0.98897836864359,-70.4568159243131,
12.));
#131048=CARTESIAN_POINT('Ctrl Pts',(-0.995053387379681,-70.476615124517,
12.));
#131049=CARTESIAN_POINT('Ctrl Pts',(-1.00116412831438,-70.4964564717917,
12.));
#131050=CARTESIAN_POINT('Ctrl Pts',(-1.00731061960968,-70.5163397782699,
12.));
#131051=CARTESIAN_POINT('Ctrl Pts',(-1.0134928891854,-70.5362648569072,
12.));
#131052=CARTESIAN_POINT('Ctrl Pts',(-1.01971096460599,-70.5562315224219,
12.));
#131053=CARTESIAN_POINT('Ctrl Pts',(-1.02596487304049,-70.5762395916412,
12.));
#131054=CARTESIAN_POINT('Ctrl Pts',(-1.03225464132872,-70.5962888829958,
12.));
#131055=CARTESIAN_POINT('Ctrl Pts',(-1.03858029601906,-70.6163792162079,
12.));
#131056=CARTESIAN_POINT('Ctrl Pts',(-1.04494186341156,-70.6365104119238,
12.));
#131057=CARTESIAN_POINT('Ctrl Pts',(-1.05133936960069,-70.6566822912965,
12.));
#131058=CARTESIAN_POINT('Ctrl Pts',(-1.05777284047728,-70.6768946760063,
12.));
#131059=CARTESIAN_POINT('Ctrl Pts',(-1.0642423017128,-70.6971473884443,
12.));
#131060=CARTESIAN_POINT('Ctrl Pts',(-1.07074777874596,-70.7174402518378,
12.));
#131061=CARTESIAN_POINT('Ctrl Pts',(-1.07728929676412,-70.737773090397,
12.));
#131062=CARTESIAN_POINT('Ctrl Pts',(-1.08386688068349,-70.7581457294475,
12.));
#131063=CARTESIAN_POINT('Ctrl Pts',(-1.09048055516434,-70.7785579953611,
12.));
#131064=CARTESIAN_POINT('Ctrl Pts',(-1.0971303446227,-70.7990097154855,
12.));
#131065=CARTESIAN_POINT('Ctrl Pts',(-1.10381627323946,-70.8195007180739,
12.));
#131066=CARTESIAN_POINT('Ctrl Pts',(-1.11053836496638,-70.8400308322013,
12.));
#131067=CARTESIAN_POINT('Ctrl Pts',(-1.1172966435299,-70.860599887712,12.));
#131068=CARTESIAN_POINT('Ctrl Pts',(-1.12409113243511,-70.8812077152564,
12.));
#131069=CARTESIAN_POINT('Ctrl Pts',(-1.13092185496563,-70.9018541463083,
12.));
#131070=CARTESIAN_POINT('Ctrl Pts',(-1.13778883418216,-70.9225390131835,
12.));
#131071=CARTESIAN_POINT('Ctrl Pts',(-1.14469209291494,-70.943262149058,
12.));
#131072=CARTESIAN_POINT('Ctrl Pts',(-1.1516316537653,-70.9640233879671,
12.));
#131073=CARTESIAN_POINT('Ctrl Pts',(-1.1586075391149,-70.9848225647876,
12.));
#131074=CARTESIAN_POINT('Ctrl Pts',(-1.16561977112882,-71.0056595152204,
12.));
#131075=CARTESIAN_POINT('Ctrl Pts',(-1.17266837175776,-71.0265340757697,
12.));
#131076=CARTESIAN_POINT('Ctrl Pts',(-1.179753362735,-71.0474460837157,12.));
#131077=CARTESIAN_POINT('Ctrl Pts',(-1.18687476558127,-71.0683953771147,
12.));
#131078=CARTESIAN_POINT('Ctrl Pts',(-1.19403260160998,-71.089381794801,
12.));
#131079=CARTESIAN_POINT('Ctrl Pts',(-1.20122689192836,-71.1104051763839,
12.));
#131080=CARTESIAN_POINT('Ctrl Pts',(-1.20845765743654,-71.1314653622442,
12.));
#131081=CARTESIAN_POINT('Ctrl Pts',(-1.21572491882273,-71.1525621935266,
12.));
#131082=CARTESIAN_POINT('Ctrl Pts',(-1.22302869657028,-71.1736955121361,
12.));
#131083=CARTESIAN_POINT('Ctrl Pts',(-1.23036901096246,-71.1948651607319,
12.));
#131084=CARTESIAN_POINT('Ctrl Pts',(-1.23774588208427,-71.2160709827189,
12.));
#131085=CARTESIAN_POINT('Ctrl Pts',(-1.24515932982108,-71.2373128222359,
12.));
#131086=CARTESIAN_POINT('Ctrl Pts',(-1.25260937385561,-71.2585905241422,
12.));
#131087=CARTESIAN_POINT('Ctrl Pts',(-1.26009603367565,-71.2799039340191,
12.));
#131088=CARTESIAN_POINT('Ctrl Pts',(-1.26761932857723,-71.301252898167,
12.));
#131089=CARTESIAN_POINT('Ctrl Pts',(-1.27517927766611,-71.3226372635993,
12.));
#131090=CARTESIAN_POINT('Ctrl Pts',(-1.28277589985475,-71.344056878033,
12.));
#131091=CARTESIAN_POINT('Ctrl Pts',(-1.29040921386061,-71.3655115898801,
12.));
#131092=CARTESIAN_POINT('Ctrl Pts',(-1.29807923821414,-71.3870012482474,
12.));
#131093=CARTESIAN_POINT('Ctrl Pts',(-1.30578599126139,-71.4085257029308,
12.));
#131094=CARTESIAN_POINT('Ctrl Pts',(-1.31352949116539,-71.4300848044095,
12.));
#131095=CARTESIAN_POINT('Ctrl Pts',(-1.32130975590231,-71.4516784038346,
12.));
#131096=CARTESIAN_POINT('Ctrl Pts',(-1.32912680326131,-71.4733063530227,
12.));
#131097=CARTESIAN_POINT('Ctrl Pts',(-1.33698065085228,-71.4949685044559,
12.));
#131098=CARTESIAN_POINT('Ctrl Pts',(-1.34487131610785,-71.5166647112766,
12.));
#131099=CARTESIAN_POINT('Ctrl Pts',(-1.35279881628453,-71.538394827283,
12.));
#131100=CARTESIAN_POINT('Ctrl Pts',(-1.36076316845806,-71.5601587069175,
12.));
#131101=CARTESIAN_POINT('Ctrl Pts',(-1.36876438952449,-71.5819562052613,
12.));
#131102=CARTESIAN_POINT('Ctrl Pts',(-1.37680249620763,-71.6037871780347,
12.));
#131103=CARTESIAN_POINT('Ctrl Pts',(-1.38487750506076,-71.6256514815918,
12.));
#131104=CARTESIAN_POINT('Ctrl Pts',(-1.39298943246731,-71.6475489729149,
12.));
#131105=CARTESIAN_POINT('Ctrl Pts',(-1.401138294636,-71.6694795096034,12.));
#131106=CARTESIAN_POINT('Ctrl Pts',(-1.40932410760275,-71.6914429498702,
12.));
#131107=CARTESIAN_POINT('Ctrl Pts',(-1.41754688723791,-71.7134391525417,
12.));
#131108=CARTESIAN_POINT('Ctrl Pts',(-1.42580664924774,-71.7354679770537,
12.));
#131109=CARTESIAN_POINT('Ctrl Pts',(-1.43410340917489,-71.7575292834456,
12.));
#131110=CARTESIAN_POINT('Ctrl Pts',(-1.44243718239305,-71.7796229323496,
12.));
#131111=CARTESIAN_POINT('Ctrl Pts',(-1.45080798410957,-71.8017487849865,
12.));
#131112=CARTESIAN_POINT('Ctrl Pts',(-1.45921582937229,-71.8239067031664,
12.));
#131113=CARTESIAN_POINT('Ctrl Pts',(-1.46766073307089,-71.8460965492836,
12.));
#131114=CARTESIAN_POINT('Ctrl Pts',(-1.4761427099373,-71.8683181863123,
12.));
#131115=CARTESIAN_POINT('Ctrl Pts',(-1.48466177454021,-71.8905714777972,
12.));
#131116=CARTESIAN_POINT('Ctrl Pts',(-1.493217941288,-71.9128562878491,12.));
#131117=CARTESIAN_POINT('Ctrl Pts',(-1.50181122443535,-71.935172481145,
12.));
#131118=CARTESIAN_POINT('Ctrl Pts',(-1.51044163808455,-71.9575199229241,
12.));
#131119=CARTESIAN_POINT('Ctrl Pts',(-1.51910919618567,-71.9798984789828,
12.));
#131120=CARTESIAN_POINT('Ctrl Pts',(-1.52781391253103,-72.0023080156647,
12.));
#131121=CARTESIAN_POINT('Ctrl Pts',(-1.53655580075814,-72.0247483998582,
12.));
#131122=CARTESIAN_POINT('Ctrl Pts',(-1.54533487435626,-72.0472194989968,
12.));
#131123=CARTESIAN_POINT('Ctrl Pts',(-1.55415114666774,-72.0697211810548,
12.));
#131124=CARTESIAN_POINT('Ctrl Pts',(-1.56300463088811,-72.092253314543,
12.));
#131125=CARTESIAN_POINT('Ctrl Pts',(-1.57189534006043,-72.1148157684987,
12.));
#131126=CARTESIAN_POINT('Ctrl Pts',(-1.58082328707808,-72.1374084124829,
12.));
#131127=CARTESIAN_POINT('Ctrl Pts',(-1.58978848469128,-72.1600311165813,
12.));
#131128=CARTESIAN_POINT('Ctrl Pts',(-1.5987909455085,-72.1826837514,12.));
#131129=CARTESIAN_POINT('Ctrl Pts',(-1.60783068199662,-72.2053661880611,
12.));
#131130=CARTESIAN_POINT('Ctrl Pts',(-1.61690770647536,-72.2280782981941,
12.));
#131131=CARTESIAN_POINT('Ctrl Pts',(-1.62602203111924,-72.2508199539325,
12.));
#131132=CARTESIAN_POINT('Ctrl Pts',(-1.63517366796459,-72.2735910279149,
12.));
#131133=CARTESIAN_POINT('Ctrl Pts',(-1.64436262891078,-72.2963913932811,
12.));
#131134=CARTESIAN_POINT('Ctrl Pts',(-1.65358892572066,-72.3192209236691,
12.));
#131135=CARTESIAN_POINT('Ctrl Pts',(-1.66285257001502,-72.3420794932052,
12.));
#131136=CARTESIAN_POINT('Ctrl Pts',(-1.67215357327372,-72.3649669765013,
12.));
#131137=CARTESIAN_POINT('Ctrl Pts',(-1.68149194684288,-72.3878832486549,
12.));
#131138=CARTESIAN_POINT('Ctrl Pts',(-1.69086770193641,-72.4108281852473,
12.));
#131139=CARTESIAN_POINT('Ctrl Pts',(-1.70028084963647,-72.4338016623388,
12.));
#131140=CARTESIAN_POINT('Ctrl Pts',(-1.70973140088837,-72.4568035564618,
12.));
#131141=CARTESIAN_POINT('Ctrl Pts',(-1.71921936650032,-72.4798337446162,
12.));
#131142=CARTESIAN_POINT('Ctrl Pts',(-1.72874475715098,-72.5028921042704,
12.));
#131143=CARTESIAN_POINT('Ctrl Pts',(-1.73830758339123,-72.5259785133586,
12.));
#131144=CARTESIAN_POINT('Ctrl Pts',(-1.74790785564476,-72.5490928502773,
12.));
#131145=CARTESIAN_POINT('Ctrl Pts',(-1.7575455842035,-72.5722349938789,
12.));
#131146=CARTESIAN_POINT('Ctrl Pts',(-1.7672207792258,-72.5954048234655,
12.));
#131147=CARTESIAN_POINT('Ctrl Pts',(-1.7769334507443,-72.618602218792,12.));
#131148=CARTESIAN_POINT('Ctrl Pts',(-1.78668360866813,-72.6418270600623,
12.));
#131149=CARTESIAN_POINT('Ctrl Pts',(-1.79647126278359,-72.6650792279271,
12.));
#131150=CARTESIAN_POINT('Ctrl Pts',(-1.80629642275051,-72.6883586034768,
12.));
#131151=CARTESIAN_POINT('Ctrl Pts',(-1.81615909809872,-72.7116650682347,
12.));
#131152=CARTESIAN_POINT('Ctrl Pts',(-1.82605929823565,-72.73499850416,12.));
#131153=CARTESIAN_POINT('Ctrl Pts',(-1.83599703244926,-72.7583587936454,
12.));
#131154=CARTESIAN_POINT('Ctrl Pts',(-1.84597230990858,-72.7817458195155,
12.));
#131155=CARTESIAN_POINT('Ctrl Pts',(-1.85598513966115,-72.8051594650214,
12.));
#131156=CARTESIAN_POINT('Ctrl Pts',(-1.86603553062776,-72.8285996138346,
12.));
#131157=CARTESIAN_POINT('Ctrl Pts',(-1.87612349160952,-72.8520661500465,
12.));
#131158=CARTESIAN_POINT('Ctrl Pts',(-1.88624903129195,-72.8755589581674,
12.));
#131159=CARTESIAN_POINT('Ctrl Pts',(-1.89641215824584,-72.8990779231226,
12.));
#131160=CARTESIAN_POINT('Ctrl Pts',(-1.90661288092583,-72.9226229302483,
12.));
#131161=CARTESIAN_POINT('Ctrl Pts',(-1.91685120766428,-72.9461938652816,
12.));
#131162=CARTESIAN_POINT('Ctrl Pts',(-1.92712714667648,-72.9697906143638,
12.));
#131163=CARTESIAN_POINT('Ctrl Pts',(-1.93744070606557,-72.9934130640414,
12.));
#131164=CARTESIAN_POINT('Ctrl Pts',(-1.947791893823,-73.0170611012659,12.));
#131165=CARTESIAN_POINT('Ctrl Pts',(-1.95818071782773,-73.0407346133912,
12.));
#131166=CARTESIAN_POINT('Ctrl Pts',(-1.96860718583944,-73.0644334881679,
12.));
#131167=CARTESIAN_POINT('Ctrl Pts',(-1.97907130550172,-73.0881576137415,
12.));
#131168=CARTESIAN_POINT('Ctrl Pts',(-1.9895730843493,-73.1119068786482,
12.));
#131169=CARTESIAN_POINT('Ctrl Pts',(-2.00011252980987,-73.1356811718094,
12.));
#131170=CARTESIAN_POINT('Ctrl Pts',(-2.01068964920465,-73.159480382525,
12.));
#131171=CARTESIAN_POINT('Ctrl Pts',(-2.02130444974352,-73.1833044004612,
12.));
#131172=CARTESIAN_POINT('Ctrl Pts',(-2.0319569385244,-73.2071531156492,
12.));
#131173=CARTESIAN_POINT('Ctrl Pts',(-2.04264712253915,-73.2310264184965,
12.));
#131174=CARTESIAN_POINT('Ctrl Pts',(-2.05337500867395,-73.2549241997946,
12.));
#131175=CARTESIAN_POINT('Ctrl Pts',(-2.06414060370837,-73.2788463507248,
12.));
#131176=CARTESIAN_POINT('Ctrl Pts',(-2.07494391430954,-73.3027927628636,
12.));
#131177=CARTESIAN_POINT('Ctrl Pts',(-2.08578494702762,-73.3267633281822,
12.));
#131178=CARTESIAN_POINT('Ctrl Pts',(-2.09666370830733,-73.3507579390254,
12.));
#131179=CARTESIAN_POINT('Ctrl Pts',(-2.10758020449401,-73.3747764880903,
12.));
#131180=CARTESIAN_POINT('Ctrl Pts',(-2.11853444183764,-73.3988188684022,
12.));
#131181=CARTESIAN_POINT('Ctrl Pts',(-2.1295264264936,-73.4228849732914,
12.));
#131182=CARTESIAN_POINT('Ctrl Pts',(-2.14055616452049,-73.4469746963622,
12.));
#131183=CARTESIAN_POINT('Ctrl Pts',(-2.15162366187899,-73.4710879315367,
12.));
#131184=CARTESIAN_POINT('Ctrl Pts',(-2.16272892442915,-73.4952245731044,
12.));
#131185=CARTESIAN_POINT('Ctrl Pts',(-2.17387195792306,-73.5193845157705,
12.));
#131186=CARTESIAN_POINT('Ctrl Pts',(-2.18505276799756,-73.5435676546934,
12.));
#131187=CARTESIAN_POINT('Ctrl Pts',(-2.19627136015683,-73.5677738855461,
12.));
#131188=CARTESIAN_POINT('Ctrl Pts',(-2.20752773978353,-73.5920031044604,
12.));
#131189=CARTESIAN_POINT('Ctrl Pts',(-2.21882191216521,-73.6162552079044,
12.));
#131190=CARTESIAN_POINT('Ctrl Pts',(-2.23015388251289,-73.6405300925714,
12.));
#131191=CARTESIAN_POINT('Ctrl Pts',(-2.24152365597699,-73.6648276552766,
12.));
#131192=CARTESIAN_POINT('Ctrl Pts',(-2.25293123766425,-73.6891477928124,
12.));
#131193=CARTESIAN_POINT('Ctrl Pts',(-2.26437663263663,-73.7134904019378,
12.));
#131194=CARTESIAN_POINT('Ctrl Pts',(-2.27585984587193,-73.7378553796792,
12.));
#131195=CARTESIAN_POINT('Ctrl Pts',(-2.28738088222858,-73.7622426235648,
12.));
#131196=CARTESIAN_POINT('Ctrl Pts',(-2.29893974640435,-73.7866520318849,
12.));
#131197=CARTESIAN_POINT('Ctrl Pts',(-2.31053644289425,-73.8110835039341,
12.));
#131198=CARTESIAN_POINT('Ctrl Pts',(-2.32217097594215,-73.8355369402733,
12.));
#131199=CARTESIAN_POINT('Ctrl Pts',(-2.3338433496398,-73.8600122421502,
12.));
#131200=CARTESIAN_POINT('Ctrl Pts',(-2.3455535680214,-73.8845093109302,
12.));
#131201=CARTESIAN_POINT('Ctrl Pts',(-2.35730163516324,-73.9090280474723,
12.));
#131202=CARTESIAN_POINT('Ctrl Pts',(-2.36908755525994,-73.9335683516388,
12.));
#131203=CARTESIAN_POINT('Ctrl Pts',(-2.38091133274933,-73.9581301214609,
12.));
#131204=CARTESIAN_POINT('Ctrl Pts',(-2.39277297220716,-73.9827132538149,
12.));
#131205=CARTESIAN_POINT('Ctrl Pts',(-2.40467247811497,-74.0073176459287,
12.));
#131206=CARTESIAN_POINT('Ctrl Pts',(-2.41660985465228,-74.0319431966956,
12.));
#131207=CARTESIAN_POINT('Ctrl Pts',(-2.42858510549786,-74.0565898079227,
12.));
#131208=CARTESIAN_POINT('Ctrl Pts',(-2.44059823356722,-74.0812573859474,
12.));
#131209=CARTESIAN_POINT('Ctrl Pts',(-2.45264924094852,-74.1059458420175,
12.));
#131210=CARTESIAN_POINT('Ctrl Pts',(-2.46301176097527,-74.1271264545378,
12.));
#131211=CARTESIAN_POINT('Ctrl Pts',(-2.47097695565717,-74.1433763941622,
12.));
#131212=CARTESIAN_POINT('Ctrl Pts',(-2.47652804725572,-74.1546864735453,
12.));
#131213=CARTESIAN_POINT('Ctrl Pts',(-2.47965393946824,-74.1610506466543,
12.));
#131214=CARTESIAN_POINT('Ctrl Pts',(-2.480349218449,-74.1624659714954,12.));
#131215=CARTESIAN_POINT('',(-0.853825826608993,-69.9947925310006,0.));
#131216=CARTESIAN_POINT('',(-0.853825826608992,-69.9947925310006,0.));
#131217=CARTESIAN_POINT('Ctrl Pts',(-2.480349218449,-74.1624659714955,0.));
#131218=CARTESIAN_POINT('Ctrl Pts',(-2.47965393946824,-74.1610506466543,
0.));
#131219=CARTESIAN_POINT('Ctrl Pts',(-2.47652804725572,-74.1546864735453,
0.));
#131220=CARTESIAN_POINT('Ctrl Pts',(-2.47097695565718,-74.1433763941622,
0.));
#131221=CARTESIAN_POINT('Ctrl Pts',(-2.46301176097527,-74.1271264545378,
0.));
#131222=CARTESIAN_POINT('Ctrl Pts',(-2.45264924094852,-74.1059458420175,
0.));
#131223=CARTESIAN_POINT('Ctrl Pts',(-2.44059823356722,-74.0812573859474,
0.));
#131224=CARTESIAN_POINT('Ctrl Pts',(-2.42858510549786,-74.0565898079227,
0.));
#131225=CARTESIAN_POINT('Ctrl Pts',(-2.41660985465228,-74.0319431966956,
0.));
#131226=CARTESIAN_POINT('Ctrl Pts',(-2.40467247811497,-74.0073176459287,
0.));
#131227=CARTESIAN_POINT('Ctrl Pts',(-2.39277297220716,-73.9827132538149,
0.));
#131228=CARTESIAN_POINT('Ctrl Pts',(-2.38091133274933,-73.9581301214609,
0.));
#131229=CARTESIAN_POINT('Ctrl Pts',(-2.36908755525994,-73.9335683516388,
0.));
#131230=CARTESIAN_POINT('Ctrl Pts',(-2.35730163516324,-73.9090280474723,
0.));
#131231=CARTESIAN_POINT('Ctrl Pts',(-2.3455535680214,-73.8845093109302,
0.));
#131232=CARTESIAN_POINT('Ctrl Pts',(-2.3338433496398,-73.8600122421502,
0.));
#131233=CARTESIAN_POINT('Ctrl Pts',(-2.32217097594215,-73.8355369402733,
0.));
#131234=CARTESIAN_POINT('Ctrl Pts',(-2.31053644289425,-73.8110835039341,
0.));
#131235=CARTESIAN_POINT('Ctrl Pts',(-2.29893974640435,-73.7866520318849,
0.));
#131236=CARTESIAN_POINT('Ctrl Pts',(-2.28738088222858,-73.7622426235648,
0.));
#131237=CARTESIAN_POINT('Ctrl Pts',(-2.27585984587193,-73.7378553796792,
0.));
#131238=CARTESIAN_POINT('Ctrl Pts',(-2.26437663263663,-73.7134904019378,
0.));
#131239=CARTESIAN_POINT('Ctrl Pts',(-2.25293123766425,-73.6891477928124,
0.));
#131240=CARTESIAN_POINT('Ctrl Pts',(-2.24152365597699,-73.6648276552766,
0.));
#131241=CARTESIAN_POINT('Ctrl Pts',(-2.23015388251289,-73.6405300925714,
0.));
#131242=CARTESIAN_POINT('Ctrl Pts',(-2.21882191216521,-73.6162552079044,
0.));
#131243=CARTESIAN_POINT('Ctrl Pts',(-2.20752773978353,-73.5920031044604,
0.));
#131244=CARTESIAN_POINT('Ctrl Pts',(-2.19627136015683,-73.5677738855461,
0.));
#131245=CARTESIAN_POINT('Ctrl Pts',(-2.18505276799756,-73.5435676546934,
0.));
#131246=CARTESIAN_POINT('Ctrl Pts',(-2.17387195792306,-73.5193845157705,
0.));
#131247=CARTESIAN_POINT('Ctrl Pts',(-2.16272892442915,-73.4952245731044,
0.));
#131248=CARTESIAN_POINT('Ctrl Pts',(-2.15162366187899,-73.4710879315367,
0.));
#131249=CARTESIAN_POINT('Ctrl Pts',(-2.14055616452049,-73.4469746963622,
0.));
#131250=CARTESIAN_POINT('Ctrl Pts',(-2.1295264264936,-73.4228849732914,
0.));
#131251=CARTESIAN_POINT('Ctrl Pts',(-2.11853444183764,-73.3988188684022,
0.));
#131252=CARTESIAN_POINT('Ctrl Pts',(-2.10758020449401,-73.3747764880903,
0.));
#131253=CARTESIAN_POINT('Ctrl Pts',(-2.09666370830733,-73.3507579390254,
0.));
#131254=CARTESIAN_POINT('Ctrl Pts',(-2.08578494702762,-73.3267633281822,
0.));
#131255=CARTESIAN_POINT('Ctrl Pts',(-2.07494391430954,-73.3027927628636,
0.));
#131256=CARTESIAN_POINT('Ctrl Pts',(-2.06414060370837,-73.2788463507248,
0.));
#131257=CARTESIAN_POINT('Ctrl Pts',(-2.05337500867395,-73.2549241997946,
0.));
#131258=CARTESIAN_POINT('Ctrl Pts',(-2.04264712253915,-73.2310264184965,
0.));
#131259=CARTESIAN_POINT('Ctrl Pts',(-2.0319569385244,-73.2071531156492,
0.));
#131260=CARTESIAN_POINT('Ctrl Pts',(-2.02130444974352,-73.1833044004612,
0.));
#131261=CARTESIAN_POINT('Ctrl Pts',(-2.01068964920465,-73.159480382525,
0.));
#131262=CARTESIAN_POINT('Ctrl Pts',(-2.00011252980987,-73.1356811718094,
0.));
#131263=CARTESIAN_POINT('Ctrl Pts',(-1.9895730843493,-73.1119068786482,
0.));
#131264=CARTESIAN_POINT('Ctrl Pts',(-1.97907130550172,-73.0881576137415,
0.));
#131265=CARTESIAN_POINT('Ctrl Pts',(-1.96860718583944,-73.0644334881679,
0.));
#131266=CARTESIAN_POINT('Ctrl Pts',(-1.95818071782773,-73.0407346133912,
0.));
#131267=CARTESIAN_POINT('Ctrl Pts',(-1.947791893823,-73.0170611012659,0.));
#131268=CARTESIAN_POINT('Ctrl Pts',(-1.93744070606557,-72.9934130640414,
0.));
#131269=CARTESIAN_POINT('Ctrl Pts',(-1.92712714667648,-72.9697906143638,
0.));
#131270=CARTESIAN_POINT('Ctrl Pts',(-1.91685120766428,-72.9461938652816,
0.));
#131271=CARTESIAN_POINT('Ctrl Pts',(-1.90661288092583,-72.9226229302483,
0.));
#131272=CARTESIAN_POINT('Ctrl Pts',(-1.89641215824584,-72.8990779231226,
0.));
#131273=CARTESIAN_POINT('Ctrl Pts',(-1.88624903129195,-72.8755589581674,
0.));
#131274=CARTESIAN_POINT('Ctrl Pts',(-1.87612349160952,-72.8520661500465,
0.));
#131275=CARTESIAN_POINT('Ctrl Pts',(-1.86603553062776,-72.8285996138346,
0.));
#131276=CARTESIAN_POINT('Ctrl Pts',(-1.85598513966115,-72.8051594650214,
0.));
#131277=CARTESIAN_POINT('Ctrl Pts',(-1.84597230990858,-72.7817458195155,
0.));
#131278=CARTESIAN_POINT('Ctrl Pts',(-1.83599703244926,-72.7583587936454,
0.));
#131279=CARTESIAN_POINT('Ctrl Pts',(-1.82605929823565,-72.73499850416,0.));
#131280=CARTESIAN_POINT('Ctrl Pts',(-1.81615909809872,-72.7116650682347,
0.));
#131281=CARTESIAN_POINT('Ctrl Pts',(-1.80629642275051,-72.6883586034768,
0.));
#131282=CARTESIAN_POINT('Ctrl Pts',(-1.79647126278359,-72.6650792279271,
0.));
#131283=CARTESIAN_POINT('Ctrl Pts',(-1.78668360866813,-72.6418270600623,
0.));
#131284=CARTESIAN_POINT('Ctrl Pts',(-1.7769334507443,-72.618602218792,0.));
#131285=CARTESIAN_POINT('Ctrl Pts',(-1.7672207792258,-72.5954048234655,
0.));
#131286=CARTESIAN_POINT('Ctrl Pts',(-1.7575455842035,-72.5722349938789,
0.));
#131287=CARTESIAN_POINT('Ctrl Pts',(-1.74790785564476,-72.5490928502773,
0.));
#131288=CARTESIAN_POINT('Ctrl Pts',(-1.73830758339123,-72.5259785133586,
0.));
#131289=CARTESIAN_POINT('Ctrl Pts',(-1.72874475715098,-72.5028921042704,
0.));
#131290=CARTESIAN_POINT('Ctrl Pts',(-1.71921936650032,-72.4798337446162,
0.));
#131291=CARTESIAN_POINT('Ctrl Pts',(-1.70973140088837,-72.4568035564618,
0.));
#131292=CARTESIAN_POINT('Ctrl Pts',(-1.70028084963647,-72.4338016623388,
0.));
#131293=CARTESIAN_POINT('Ctrl Pts',(-1.69086770193641,-72.4108281852473,
0.));
#131294=CARTESIAN_POINT('Ctrl Pts',(-1.68149194684288,-72.3878832486549,
0.));
#131295=CARTESIAN_POINT('Ctrl Pts',(-1.67215357327372,-72.3649669765013,
0.));
#131296=CARTESIAN_POINT('Ctrl Pts',(-1.66285257001502,-72.3420794932052,
0.));
#131297=CARTESIAN_POINT('Ctrl Pts',(-1.65358892572066,-72.3192209236691,
0.));
#131298=CARTESIAN_POINT('Ctrl Pts',(-1.64436262891078,-72.2963913932811,
0.));
#131299=CARTESIAN_POINT('Ctrl Pts',(-1.63517366796459,-72.2735910279149,
0.));
#131300=CARTESIAN_POINT('Ctrl Pts',(-1.62602203111924,-72.2508199539325,
0.));
#131301=CARTESIAN_POINT('Ctrl Pts',(-1.61690770647536,-72.2280782981941,
0.));
#131302=CARTESIAN_POINT('Ctrl Pts',(-1.60783068199662,-72.2053661880611,
0.));
#131303=CARTESIAN_POINT('Ctrl Pts',(-1.5987909455085,-72.1826837514,0.));
#131304=CARTESIAN_POINT('Ctrl Pts',(-1.58978848469128,-72.1600311165813,
0.));
#131305=CARTESIAN_POINT('Ctrl Pts',(-1.58082328707808,-72.1374084124829,
0.));
#131306=CARTESIAN_POINT('Ctrl Pts',(-1.57189534006043,-72.1148157684987,
0.));
#131307=CARTESIAN_POINT('Ctrl Pts',(-1.56300463088811,-72.092253314543,
0.));
#131308=CARTESIAN_POINT('Ctrl Pts',(-1.55415114666774,-72.0697211810548,
0.));
#131309=CARTESIAN_POINT('Ctrl Pts',(-1.54533487435626,-72.0472194989968,
0.));
#131310=CARTESIAN_POINT('Ctrl Pts',(-1.53655580075814,-72.0247483998582,
0.));
#131311=CARTESIAN_POINT('Ctrl Pts',(-1.52781391253103,-72.0023080156647,
0.));
#131312=CARTESIAN_POINT('Ctrl Pts',(-1.51910919618567,-71.9798984789828,
0.));
#131313=CARTESIAN_POINT('Ctrl Pts',(-1.51044163808455,-71.9575199229241,
0.));
#131314=CARTESIAN_POINT('Ctrl Pts',(-1.50181122443535,-71.935172481145,
0.));
#131315=CARTESIAN_POINT('Ctrl Pts',(-1.493217941288,-71.9128562878491,0.));
#131316=CARTESIAN_POINT('Ctrl Pts',(-1.48466177454021,-71.8905714777972,
0.));
#131317=CARTESIAN_POINT('Ctrl Pts',(-1.4761427099373,-71.8683181863123,
0.));
#131318=CARTESIAN_POINT('Ctrl Pts',(-1.46766073307089,-71.8460965492836,
0.));
#131319=CARTESIAN_POINT('Ctrl Pts',(-1.45921582937229,-71.8239067031664,
0.));
#131320=CARTESIAN_POINT('Ctrl Pts',(-1.45080798410957,-71.8017487849865,
0.));
#131321=CARTESIAN_POINT('Ctrl Pts',(-1.44243718239305,-71.7796229323496,
0.));
#131322=CARTESIAN_POINT('Ctrl Pts',(-1.43410340917489,-71.7575292834456,
0.));
#131323=CARTESIAN_POINT('Ctrl Pts',(-1.42580664924774,-71.7354679770537,
0.));
#131324=CARTESIAN_POINT('Ctrl Pts',(-1.41754688723791,-71.7134391525417,
0.));
#131325=CARTESIAN_POINT('Ctrl Pts',(-1.40932410760275,-71.6914429498702,
0.));
#131326=CARTESIAN_POINT('Ctrl Pts',(-1.401138294636,-71.6694795096034,0.));
#131327=CARTESIAN_POINT('Ctrl Pts',(-1.39298943246731,-71.6475489729149,
0.));
#131328=CARTESIAN_POINT('Ctrl Pts',(-1.38487750506076,-71.6256514815918,
0.));
#131329=CARTESIAN_POINT('Ctrl Pts',(-1.37680249620763,-71.6037871780347,
0.));
#131330=CARTESIAN_POINT('Ctrl Pts',(-1.36876438952449,-71.5819562052613,
0.));
#131331=CARTESIAN_POINT('Ctrl Pts',(-1.36076316845806,-71.5601587069175,
0.));
#131332=CARTESIAN_POINT('Ctrl Pts',(-1.35279881628453,-71.538394827283,
0.));
#131333=CARTESIAN_POINT('Ctrl Pts',(-1.34487131610785,-71.5166647112766,
0.));
#131334=CARTESIAN_POINT('Ctrl Pts',(-1.33698065085228,-71.4949685044559,
0.));
#131335=CARTESIAN_POINT('Ctrl Pts',(-1.32912680326131,-71.4733063530227,
0.));
#131336=CARTESIAN_POINT('Ctrl Pts',(-1.32130975590231,-71.4516784038346,
0.));
#131337=CARTESIAN_POINT('Ctrl Pts',(-1.31352949116539,-71.4300848044095,
0.));
#131338=CARTESIAN_POINT('Ctrl Pts',(-1.30578599126139,-71.4085257029308,
0.));
#131339=CARTESIAN_POINT('Ctrl Pts',(-1.29807923821414,-71.3870012482474,
0.));
#131340=CARTESIAN_POINT('Ctrl Pts',(-1.29040921386061,-71.3655115898801,
0.));
#131341=CARTESIAN_POINT('Ctrl Pts',(-1.28277589985475,-71.344056878033,
0.));
#131342=CARTESIAN_POINT('Ctrl Pts',(-1.27517927766611,-71.3226372635993,
0.));
#131343=CARTESIAN_POINT('Ctrl Pts',(-1.26761932857723,-71.301252898167,
0.));
#131344=CARTESIAN_POINT('Ctrl Pts',(-1.26009603367565,-71.2799039340191,
0.));
#131345=CARTESIAN_POINT('Ctrl Pts',(-1.25260937385561,-71.2585905241422,
0.));
#131346=CARTESIAN_POINT('Ctrl Pts',(-1.24515932982108,-71.2373128222359,
0.));
#131347=CARTESIAN_POINT('Ctrl Pts',(-1.23774588208427,-71.2160709827189,
0.));
#131348=CARTESIAN_POINT('Ctrl Pts',(-1.23036901096246,-71.1948651607319,
0.));
#131349=CARTESIAN_POINT('Ctrl Pts',(-1.22302869657028,-71.1736955121361,
0.));
#131350=CARTESIAN_POINT('Ctrl Pts',(-1.21572491882273,-71.1525621935266,
0.));
#131351=CARTESIAN_POINT('Ctrl Pts',(-1.20845765743654,-71.1314653622442,
0.));
#131352=CARTESIAN_POINT('Ctrl Pts',(-1.20122689192836,-71.1104051763839,
0.));
#131353=CARTESIAN_POINT('Ctrl Pts',(-1.19403260160998,-71.089381794801,
0.));
#131354=CARTESIAN_POINT('Ctrl Pts',(-1.18687476558127,-71.0683953771147,
0.));
#131355=CARTESIAN_POINT('Ctrl Pts',(-1.179753362735,-71.0474460837157,0.));
#131356=CARTESIAN_POINT('Ctrl Pts',(-1.17266837175776,-71.0265340757697,
0.));
#131357=CARTESIAN_POINT('Ctrl Pts',(-1.16561977112882,-71.0056595152204,
0.));
#131358=CARTESIAN_POINT('Ctrl Pts',(-1.1586075391149,-70.9848225647876,
0.));
#131359=CARTESIAN_POINT('Ctrl Pts',(-1.1516316537653,-70.9640233879671,
0.));
#131360=CARTESIAN_POINT('Ctrl Pts',(-1.14469209291494,-70.943262149058,
0.));
#131361=CARTESIAN_POINT('Ctrl Pts',(-1.13778883418216,-70.9225390131835,
0.));
#131362=CARTESIAN_POINT('Ctrl Pts',(-1.13092185496563,-70.9018541463083,
0.));
#131363=CARTESIAN_POINT('Ctrl Pts',(-1.12409113243511,-70.8812077152564,
0.));
#131364=CARTESIAN_POINT('Ctrl Pts',(-1.1172966435299,-70.860599887712,0.));
#131365=CARTESIAN_POINT('Ctrl Pts',(-1.11053836496638,-70.8400308322013,
0.));
#131366=CARTESIAN_POINT('Ctrl Pts',(-1.10381627323946,-70.8195007180739,
0.));
#131367=CARTESIAN_POINT('Ctrl Pts',(-1.0971303446227,-70.7990097154855,
0.));
#131368=CARTESIAN_POINT('Ctrl Pts',(-1.09048055516434,-70.7785579953611,
0.));
#131369=CARTESIAN_POINT('Ctrl Pts',(-1.08386688068349,-70.7581457294475,
0.));
#131370=CARTESIAN_POINT('Ctrl Pts',(-1.07728929676412,-70.737773090397,
0.));
#131371=CARTESIAN_POINT('Ctrl Pts',(-1.07074777874596,-70.7174402518378,
0.));
#131372=CARTESIAN_POINT('Ctrl Pts',(-1.0642423017128,-70.6971473884443,
0.));
#131373=CARTESIAN_POINT('Ctrl Pts',(-1.05777284047728,-70.6768946760063,
0.));
#131374=CARTESIAN_POINT('Ctrl Pts',(-1.05133936960069,-70.6566822912965,
0.));
#131375=CARTESIAN_POINT('Ctrl Pts',(-1.04494186341156,-70.6365104119238,
0.));
#131376=CARTESIAN_POINT('Ctrl Pts',(-1.03858029601906,-70.6163792162079,
0.));
#131377=CARTESIAN_POINT('Ctrl Pts',(-1.03225464132872,-70.5962888829958,
0.));
#131378=CARTESIAN_POINT('Ctrl Pts',(-1.02596487304049,-70.5762395916412,
0.));
#131379=CARTESIAN_POINT('Ctrl Pts',(-1.01971096460599,-70.5562315224219,
0.));
#131380=CARTESIAN_POINT('Ctrl Pts',(-1.0134928891854,-70.5362648569072,
0.));
#131381=CARTESIAN_POINT('Ctrl Pts',(-1.00731061960968,-70.5163397782699,
0.));
#131382=CARTESIAN_POINT('Ctrl Pts',(-1.00116412831438,-70.4964564717917,
0.));
#131383=CARTESIAN_POINT('Ctrl Pts',(-0.995053387379681,-70.476615124517,
0.));
#131384=CARTESIAN_POINT('Ctrl Pts',(-0.98897836864359,-70.4568159243131,
0.));
#131385=CARTESIAN_POINT('Ctrl Pts',(-0.982939043792158,-70.4370590590839,
0.));
#131386=CARTESIAN_POINT('Ctrl Pts',(-0.976935384450128,-70.41734471596,
0.));
#131387=CARTESIAN_POINT('Ctrl Pts',(-0.970967362281301,-70.3976730803664,
0.));
#131388=CARTESIAN_POINT('Ctrl Pts',(-0.965034948786559,-70.3780443378003,
0.));
#131389=CARTESIAN_POINT('Ctrl Pts',(-0.959138115058886,-70.3584586759561,
0.));
#131390=CARTESIAN_POINT('Ctrl Pts',(-0.953276831581232,-70.338916286457,
0.));
#131391=CARTESIAN_POINT('Ctrl Pts',(-0.947451067929564,-70.3194173673635,
0.));
#131392=CARTESIAN_POINT('Ctrl Pts',(-0.941660792742953,-70.2999621233938,
0.));
#131393=CARTESIAN_POINT('Ctrl Pts',(-0.935905974336492,-70.2805507606832,
0.));
#131394=CARTESIAN_POINT('Ctrl Pts',(-0.930186581235576,-70.2611834821711,
0.));
#131395=CARTESIAN_POINT('Ctrl Pts',(-0.924502582639453,-70.241860483586,
0.));
#131396=CARTESIAN_POINT('Ctrl Pts',(-0.918853949157045,-70.2225819470306,
0.));
#131397=CARTESIAN_POINT('Ctrl Pts',(-0.913240652090839,-70.2033480471749,
0.));
#131398=CARTESIAN_POINT('Ctrl Pts',(-0.90766266201565,-70.184158963563,
0.));
#131399=CARTESIAN_POINT('Ctrl Pts',(-0.902119947629773,-70.1650148905109,
0.));
#131400=CARTESIAN_POINT('Ctrl Pts',(-0.896612474372085,-70.1459160490366,
0.));
#131401=CARTESIAN_POINT('Ctrl Pts',(-0.891140203464724,-70.1268626950031,
0.));
#131402=CARTESIAN_POINT('Ctrl Pts',(-0.885703094803086,-70.1078550938801,
0.));
#131403=CARTESIAN_POINT('Ctrl Pts',(-0.880301109661037,-70.0888934967772,
0.));
#131404=CARTESIAN_POINT('Ctrl Pts',(-0.87493421325557,-70.0699781184013,
0.));
#131405=CARTESIAN_POINT('Ctrl Pts',(-0.869602377870139,-70.0511091083285,
0.));
#131406=CARTESIAN_POINT('Ctrl Pts',(-0.86430558366009,-70.0322865493339,
0.));
#131407=CARTESIAN_POINT('Ctrl Pts',(-0.860096170667398,-70.0172656934192,
0.));
#131408=CARTESIAN_POINT('Ctrl Pts',(-0.856954870258371,-70.0060209754332,
0.));
#131409=CARTESIAN_POINT('Ctrl Pts',(-0.854867673848293,-69.9985337959499,
0.));
#131410=CARTESIAN_POINT('Ctrl Pts',(-0.853825826608993,-69.9947925310006,
0.));
#131411=CARTESIAN_POINT('Ctrl Pts',(-9.10443154852688,-73.9415940197274,
0.));
#131412=CARTESIAN_POINT('Ctrl Pts',(-9.10443154852688,-73.9415940197274,
12.));
#131413=CARTESIAN_POINT('Ctrl Pts',(-9.10148558516537,-73.9368365074299,
0.));
#131414=CARTESIAN_POINT('Ctrl Pts',(-9.10148558516537,-73.9368365074299,
12.));
#131415=CARTESIAN_POINT('Ctrl Pts',(-9.09559760529042,-73.9273231219835,
0.));
#131416=CARTESIAN_POINT('Ctrl Pts',(-9.09559760529042,-73.9273231219835,
12.));
#131417=CARTESIAN_POINT('Ctrl Pts',(-9.08677747602205,-73.9130579612604,
0.));
#131418=CARTESIAN_POINT('Ctrl Pts',(-9.08677747602205,-73.9130579612604,
12.));
#131419=CARTESIAN_POINT('Ctrl Pts',(-9.07504098571707,-73.8940475822492,
0.));
#131420=CARTESIAN_POINT('Ctrl Pts',(-9.07504098571707,-73.8940475822492,
12.));
#131421=CARTESIAN_POINT('Ctrl Pts',(-9.06040984890246,-73.8703010078091,
0.));
#131422=CARTESIAN_POINT('Ctrl Pts',(-9.06040984890246,-73.8703010078091,
12.));
#131423=CARTESIAN_POINT('Ctrl Pts',(-9.04581819646984,-73.8465708501057,
0.));
#131424=CARTESIAN_POINT('Ctrl Pts',(-9.04581819646984,-73.8465708501057,
12.));
#131425=CARTESIAN_POINT('Ctrl Pts',(-9.03126603778125,-73.8228571411697,
0.));
#131426=CARTESIAN_POINT('Ctrl Pts',(-9.03126603778125,-73.8228571411697,
12.));
#131427=CARTESIAN_POINT('Ctrl Pts',(-9.01675338208004,-73.7991599312592,
0.));
#131428=CARTESIAN_POINT('Ctrl Pts',(-9.01675338208004,-73.7991599312592,
12.));
#131429=CARTESIAN_POINT('Ctrl Pts',(-9.00228023701055,-73.7754792943665,
0.));
#131430=CARTESIAN_POINT('Ctrl Pts',(-9.00228023701055,-73.7754792943665,
12.));
#131431=CARTESIAN_POINT('Ctrl Pts',(-8.98784660837397,-73.7518153261981,
0.));
#131432=CARTESIAN_POINT('Ctrl Pts',(-8.98784660837397,-73.7518153261981,
12.));
#131433=CARTESIAN_POINT('Ctrl Pts',(-8.97345250083601,-73.728168136383,
0.));
#131434=CARTESIAN_POINT('Ctrl Pts',(-8.97345250083601,-73.728168136383,
12.));
#131435=CARTESIAN_POINT('Ctrl Pts',(-8.95909791836152,-73.7045378422686,
0.));
#131436=CARTESIAN_POINT('Ctrl Pts',(-8.95909791836152,-73.7045378422686,
12.));
#131437=CARTESIAN_POINT('Ctrl Pts',(-8.94478286474419,-73.6809245622383,
0.));
#131438=CARTESIAN_POINT('Ctrl Pts',(-8.94478286474419,-73.6809245622383,
12.));
#131439=CARTESIAN_POINT('Ctrl Pts',(-8.93050734412124,-73.6573284088184,
0.));
#131440=CARTESIAN_POINT('Ctrl Pts',(-8.93050734412124,-73.6573284088184,
12.));
#131441=CARTESIAN_POINT('Ctrl Pts',(-8.91627136140084,-73.633749483097,
0.));
#131442=CARTESIAN_POINT('Ctrl Pts',(-8.91627136140084,-73.633749483097,
12.));
#131443=CARTESIAN_POINT('Ctrl Pts',(-8.90207492199043,-73.6101878785976,
0.));
#131444=CARTESIAN_POINT('Ctrl Pts',(-8.90207492199043,-73.6101878785976,
12.));
#131445=CARTESIAN_POINT('Ctrl Pts',(-8.88791803160442,-73.5866436840556,
0.));
#131446=CARTESIAN_POINT('Ctrl Pts',(-8.88791803160442,-73.5866436840556,
12.));
#131447=CARTESIAN_POINT('Ctrl Pts',(-8.8738006960297,-73.5631169867122,
0.));
#131448=CARTESIAN_POINT('Ctrl Pts',(-8.8738006960297,-73.5631169867122,
12.));
#131449=CARTESIAN_POINT('Ctrl Pts',(-8.8597229209213,-73.5396078751639,
0.));
#131450=CARTESIAN_POINT('Ctrl Pts',(-8.8597229209213,-73.5396078751639,
12.));
#131451=CARTESIAN_POINT('Ctrl Pts',(-8.84568471153805,-73.5161164429709,
0.));
#131452=CARTESIAN_POINT('Ctrl Pts',(-8.84568471153805,-73.5161164429709,
12.));
#131453=CARTESIAN_POINT('Ctrl Pts',(-8.83168607277325,-73.492642788273,
0.));
#131454=CARTESIAN_POINT('Ctrl Pts',(-8.83168607277325,-73.492642788273,
12.));
#131455=CARTESIAN_POINT('Ctrl Pts',(-8.8177270092753,-73.4691870121567,
0.));
#131456=CARTESIAN_POINT('Ctrl Pts',(-8.8177270092753,-73.4691870121567,
12.));
#131457=CARTESIAN_POINT('Ctrl Pts',(-8.80380752553691,-73.4457492173933,
0.));
#131458=CARTESIAN_POINT('Ctrl Pts',(-8.80380752553691,-73.4457492173933,
12.));
#131459=CARTESIAN_POINT('Ctrl Pts',(-8.78992762598756,-73.422329507113,
0.));
#131460=CARTESIAN_POINT('Ctrl Pts',(-8.78992762598756,-73.422329507113,
12.));
#131461=CARTESIAN_POINT('Ctrl Pts',(-8.77608731509347,-73.3989279832835,
0.));
#131462=CARTESIAN_POINT('Ctrl Pts',(-8.77608731509347,-73.3989279832835,
12.));
#131463=CARTESIAN_POINT('Ctrl Pts',(-8.76228659740357,-73.3755447460269,
0.));
#131464=CARTESIAN_POINT('Ctrl Pts',(-8.76228659740357,-73.3755447460269,
12.));
#131465=CARTESIAN_POINT('Ctrl Pts',(-8.74852547749778,-73.3521798944622,
0.));
#131466=CARTESIAN_POINT('Ctrl Pts',(-8.74852547749778,-73.3521798944622,
12.));
#131467=CARTESIAN_POINT('Ctrl Pts',(-8.7348039599538,-73.3288335272002,
0.));
#131468=CARTESIAN_POINT('Ctrl Pts',(-8.7348039599538,-73.3288335272002,
12.));
#131469=CARTESIAN_POINT('Ctrl Pts',(-8.72112204930231,-73.3055057429742,
0.));
#131470=CARTESIAN_POINT('Ctrl Pts',(-8.72112204930231,-73.3055057429742,
12.));
#131471=CARTESIAN_POINT('Ctrl Pts',(-8.70747974998229,-73.2821966412148,
0.));
#131472=CARTESIAN_POINT('Ctrl Pts',(-8.70747974998229,-73.2821966412148,
12.));
#131473=CARTESIAN_POINT('Ctrl Pts',(-8.69387706629285,-73.2589063226358,
0.));
#131474=CARTESIAN_POINT('Ctrl Pts',(-8.69387706629285,-73.2589063226358,
12.));
#131475=CARTESIAN_POINT('Ctrl Pts',(-8.68031400241871,-73.2356348889693,
0.));
#131476=CARTESIAN_POINT('Ctrl Pts',(-8.68031400241871,-73.2356348889693,
12.));
#131477=CARTESIAN_POINT('Ctrl Pts',(-8.66679056245091,-73.2123824427208,
0.));
#131478=CARTESIAN_POINT('Ctrl Pts',(-8.66679056245091,-73.2123824427208,
12.));
#131479=CARTESIAN_POINT('Ctrl Pts',(-8.65330675040536,-73.1891490869056,
0.));
#131480=CARTESIAN_POINT('Ctrl Pts',(-8.65330675040536,-73.1891490869056,
12.));
#131481=CARTESIAN_POINT('Ctrl Pts',(-8.63986257023738,-73.1659349248132,
0.));
#131482=CARTESIAN_POINT('Ctrl Pts',(-8.63986257023738,-73.1659349248132,
12.));
#131483=CARTESIAN_POINT('Ctrl Pts',(-8.62645802585483,-73.1427400597037,
0.));
#131484=CARTESIAN_POINT('Ctrl Pts',(-8.62645802585483,-73.1427400597037,
12.));
#131485=CARTESIAN_POINT('Ctrl Pts',(-8.61309312112001,-73.1195645948178,
0.));
#131486=CARTESIAN_POINT('Ctrl Pts',(-8.61309312112001,-73.1195645948178,
12.));
#131487=CARTESIAN_POINT('Ctrl Pts',(-8.59976785984551,-73.0964086335235,
0.));
#131488=CARTESIAN_POINT('Ctrl Pts',(-8.59976785984551,-73.0964086335235,
12.));
#131489=CARTESIAN_POINT('Ctrl Pts',(-8.58648224578731,-73.0732722794195,
0.));
#131490=CARTESIAN_POINT('Ctrl Pts',(-8.58648224578731,-73.0732722794195,
12.));
#131491=CARTESIAN_POINT('Ctrl Pts',(-8.57323628263593,-73.0501556364479,
0.));
#131492=CARTESIAN_POINT('Ctrl Pts',(-8.57323628263593,-73.0501556364479,
12.));
#131493=CARTESIAN_POINT('Ctrl Pts',(-8.56002997400083,-73.0270588090183,
0.));
#131494=CARTESIAN_POINT('Ctrl Pts',(-8.56002997400083,-73.0270588090183,
12.));
#131495=CARTESIAN_POINT('Ctrl Pts',(-8.54686332340417,-73.0039819020648,
0.));
#131496=CARTESIAN_POINT('Ctrl Pts',(-8.54686332340417,-73.0039819020648,
12.));
#131497=CARTESIAN_POINT('Ctrl Pts',(-8.5337363342928,-72.9809250209828,
0.));
#131498=CARTESIAN_POINT('Ctrl Pts',(-8.5337363342928,-72.9809250209828,
12.));
#131499=CARTESIAN_POINT('Ctrl Pts',(-8.52064901004227,-72.9578882715912,
0.));
#131500=CARTESIAN_POINT('Ctrl Pts',(-8.52064901004227,-72.9578882715912,
12.));
#131501=CARTESIAN_POINT('Ctrl Pts',(-8.50760135395983,-72.9348717600838,
0.));
#131502=CARTESIAN_POINT('Ctrl Pts',(-8.50760135395983,-72.9348717600838,
12.));
#131503=CARTESIAN_POINT('Ctrl Pts',(-8.49459336928295,-72.9118755929795,
0.));
#131504=CARTESIAN_POINT('Ctrl Pts',(-8.49459336928295,-72.9118755929795,
12.));
#131505=CARTESIAN_POINT('Ctrl Pts',(-8.48162505917657,-72.8888998770785,
0.));
#131506=CARTESIAN_POINT('Ctrl Pts',(-8.48162505917657,-72.8888998770785,
12.));
#131507=CARTESIAN_POINT('Ctrl Pts',(-8.46869642673794,-72.8659447194933,
0.));
#131508=CARTESIAN_POINT('Ctrl Pts',(-8.46869642673794,-72.8659447194933,
12.));
#131509=CARTESIAN_POINT('Ctrl Pts',(-8.45580747499793,-72.8430102276713,
0.));
#131510=CARTESIAN_POINT('Ctrl Pts',(-8.45580747499793,-72.8430102276713,
12.));
#131511=CARTESIAN_POINT('Ctrl Pts',(-8.44295820691911,-72.8200965094199,
0.));
#131512=CARTESIAN_POINT('Ctrl Pts',(-8.44295820691911,-72.8200965094199,
12.));
#131513=CARTESIAN_POINT('Ctrl Pts',(-8.43014862539157,-72.7972036729276,
0.));
#131514=CARTESIAN_POINT('Ctrl Pts',(-8.43014862539157,-72.7972036729276,
12.));
#131515=CARTESIAN_POINT('Ctrl Pts',(-8.41737873322329,-72.7743318267865,
0.));
#131516=CARTESIAN_POINT('Ctrl Pts',(-8.41737873322329,-72.7743318267865,
12.));
#131517=CARTESIAN_POINT('Ctrl Pts',(-8.40464853314468,-72.751481079992,
0.));
#131518=CARTESIAN_POINT('Ctrl Pts',(-8.40464853314468,-72.751481079992,
12.));
#131519=CARTESIAN_POINT('Ctrl Pts',(-8.3919580278139,-72.7286515419373,
0.));
#131520=CARTESIAN_POINT('Ctrl Pts',(-8.3919580278139,-72.7286515419373,
12.));
#131521=CARTESIAN_POINT('Ctrl Pts',(-8.37930721981731,-72.705843322407,
0.));
#131522=CARTESIAN_POINT('Ctrl Pts',(-8.37930721981731,-72.705843322407,
12.));
#131523=CARTESIAN_POINT('Ctrl Pts',(-8.36669611166842,-72.6830565315703,
0.));
#131524=CARTESIAN_POINT('Ctrl Pts',(-8.36669611166842,-72.6830565315703,
12.));
#131525=CARTESIAN_POINT('Ctrl Pts',(-8.35412470580101,-72.6602912799696,
0.));
#131526=CARTESIAN_POINT('Ctrl Pts',(-8.35412470580101,-72.6602912799696,
12.));
#131527=CARTESIAN_POINT('Ctrl Pts',(-8.34159300456986,-72.6375476785215,
0.));
#131528=CARTESIAN_POINT('Ctrl Pts',(-8.34159300456986,-72.6375476785215,
12.));
#131529=CARTESIAN_POINT('Ctrl Pts',(-8.3291010102567,-72.6148258385296,
0.));
#131530=CARTESIAN_POINT('Ctrl Pts',(-8.3291010102567,-72.6148258385296,
12.));
#131531=CARTESIAN_POINT('Ctrl Pts',(-8.31664872507016,-72.5921258716901,
0.));
#131532=CARTESIAN_POINT('Ctrl Pts',(-8.31664872507016,-72.5921258716901,
12.));
#131533=CARTESIAN_POINT('Ctrl Pts',(-8.30423615114452,-72.5694478900982,
0.));
#131534=CARTESIAN_POINT('Ctrl Pts',(-8.30423615114452,-72.5694478900982,
12.));
#131535=CARTESIAN_POINT('Ctrl Pts',(-8.29186329053279,-72.5467920062521,
0.));
#131536=CARTESIAN_POINT('Ctrl Pts',(-8.29186329053279,-72.5467920062521,
12.));
#131537=CARTESIAN_POINT('Ctrl Pts',(-8.27953014520376,-72.5241583330562,
0.));
#131538=CARTESIAN_POINT('Ctrl Pts',(-8.27953014520376,-72.5241583330562,
12.));
#131539=CARTESIAN_POINT('Ctrl Pts',(-8.26723671704919,-72.5015469838254,
0.));
#131540=CARTESIAN_POINT('Ctrl Pts',(-8.26723671704919,-72.5015469838254,
12.));
#131541=CARTESIAN_POINT('Ctrl Pts',(-8.25498300788493,-72.4789580722875,
0.));
#131542=CARTESIAN_POINT('Ctrl Pts',(-8.25498300788493,-72.4789580722875,
12.));
#131543=CARTESIAN_POINT('Ctrl Pts',(-8.2427690194504,-72.4563917125842,
0.));
#131544=CARTESIAN_POINT('Ctrl Pts',(-8.2427690194504,-72.4563917125842,
12.));
#131545=CARTESIAN_POINT('Ctrl Pts',(-8.23059475340356,-72.4338480192695,
0.));
#131546=CARTESIAN_POINT('Ctrl Pts',(-8.23059475340356,-72.4338480192695,
12.));
#131547=CARTESIAN_POINT('Ctrl Pts',(-8.2184602113156,-72.4113271073079,
0.));
#131548=CARTESIAN_POINT('Ctrl Pts',(-8.2184602113156,-72.4113271073079,
12.));
#131549=CARTESIAN_POINT('Ctrl Pts',(-8.20636539467776,-72.3888290920832,
0.));
#131550=CARTESIAN_POINT('Ctrl Pts',(-8.20636539467776,-72.3888290920832,
12.));
#131551=CARTESIAN_POINT('Ctrl Pts',(-8.19431030490314,-72.3663540894026,
0.));
#131552=CARTESIAN_POINT('Ctrl Pts',(-8.19431030490314,-72.3663540894026,
12.));
#131553=CARTESIAN_POINT('Ctrl Pts',(-8.18229494332623,-72.3439022155007,
0.));
#131554=CARTESIAN_POINT('Ctrl Pts',(-8.18229494332623,-72.3439022155007,
12.));
#131555=CARTESIAN_POINT('Ctrl Pts',(-8.1703193111989,-72.3214735870409,
0.));
#131556=CARTESIAN_POINT('Ctrl Pts',(-8.1703193111989,-72.3214735870409,
12.));
#131557=CARTESIAN_POINT('Ctrl Pts',(-8.15838340968335,-72.2990683211162,
0.));
#131558=CARTESIAN_POINT('Ctrl Pts',(-8.15838340968335,-72.2990683211162,
12.));
#131559=CARTESIAN_POINT('Ctrl Pts',(-8.14648723985797,-72.2766865352555,
0.));
#131560=CARTESIAN_POINT('Ctrl Pts',(-8.14648723985797,-72.2766865352555,
12.));
#131561=CARTESIAN_POINT('Ctrl Pts',(-8.13463080272028,-72.2543283474278,
0.));
#131562=CARTESIAN_POINT('Ctrl Pts',(-8.13463080272028,-72.2543283474278,
12.));
#131563=CARTESIAN_POINT('Ctrl Pts',(-8.1228140991866,-72.2319938760449,
0.));
#131564=CARTESIAN_POINT('Ctrl Pts',(-8.1228140991866,-72.2319938760449,
12.));
#131565=CARTESIAN_POINT('Ctrl Pts',(-8.11103713008928,-72.209683239963,
0.));
#131566=CARTESIAN_POINT('Ctrl Pts',(-8.11103713008928,-72.209683239963,
12.));
#131567=CARTESIAN_POINT('Ctrl Pts',(-8.09929989616889,-72.1873965584813,
0.));
#131568=CARTESIAN_POINT('Ctrl Pts',(-8.09929989616889,-72.1873965584813,
12.));
#131569=CARTESIAN_POINT('Ctrl Pts',(-8.08760239807836,-72.1651339513477,
0.));
#131570=CARTESIAN_POINT('Ctrl Pts',(-8.08760239807836,-72.1651339513477,
12.));
#131571=CARTESIAN_POINT('Ctrl Pts',(-8.07594463638719,-72.1428955387663,
0.));
#131572=CARTESIAN_POINT('Ctrl Pts',(-8.07594463638719,-72.1428955387663,
12.));
#131573=CARTESIAN_POINT('Ctrl Pts',(-8.06432661158095,-72.1206814413988,
0.));
#131574=CARTESIAN_POINT('Ctrl Pts',(-8.06432661158095,-72.1206814413988,
12.));
#131575=CARTESIAN_POINT('Ctrl Pts',(-8.05274832405948,-72.0984917803693,
0.));
#131576=CARTESIAN_POINT('Ctrl Pts',(-8.05274832405948,-72.0984917803693,
12.));
#131577=CARTESIAN_POINT('Ctrl Pts',(-8.04120977412872,-72.0763266772615,
0.));
#131578=CARTESIAN_POINT('Ctrl Pts',(-8.04120977412872,-72.0763266772615,
12.));
#131579=CARTESIAN_POINT('Ctrl Pts',(-8.02971096200307,-72.0541862541243,
0.));
#131580=CARTESIAN_POINT('Ctrl Pts',(-8.02971096200307,-72.0541862541243,
12.));
#131581=CARTESIAN_POINT('Ctrl Pts',(-8.01825188781056,-72.032070633479,
0.));
#131582=CARTESIAN_POINT('Ctrl Pts',(-8.01825188781056,-72.032070633479,
12.));
#131583=CARTESIAN_POINT('Ctrl Pts',(-8.00683255159247,-72.0099799383213,
0.));
#131584=CARTESIAN_POINT('Ctrl Pts',(-8.00683255159247,-72.0099799383213,
12.));
#131585=CARTESIAN_POINT('Ctrl Pts',(-7.99545295330191,-71.9879142921254,
0.));
#131586=CARTESIAN_POINT('Ctrl Pts',(-7.99545295330191,-71.9879142921254,
12.));
#131587=CARTESIAN_POINT('Ctrl Pts',(-7.98411309279612,-71.965873818843,
0.));
#131588=CARTESIAN_POINT('Ctrl Pts',(-7.98411309279612,-71.965873818843,
12.));
#131589=CARTESIAN_POINT('Ctrl Pts',(-7.97281296983717,-71.9438586429081,
0.));
#131590=CARTESIAN_POINT('Ctrl Pts',(-7.97281296983717,-71.9438586429081,
12.));
#131591=CARTESIAN_POINT('Ctrl Pts',(-7.96155258409763,-71.9218688892431,
0.));
#131592=CARTESIAN_POINT('Ctrl Pts',(-7.96155258409763,-71.9218688892431,
12.));
#131593=CARTESIAN_POINT('Ctrl Pts',(-7.9503319351605,-71.8999046832643,
0.));
#131594=CARTESIAN_POINT('Ctrl Pts',(-7.9503319351605,-71.8999046832643,
12.));
#131595=CARTESIAN_POINT('Ctrl Pts',(-7.93915102251794,-71.8779661508832,
0.));
#131596=CARTESIAN_POINT('Ctrl Pts',(-7.93915102251794,-71.8779661508832,
12.));
#131597=CARTESIAN_POINT('Ctrl Pts',(-7.92800984556395,-71.8560534185071,
0.));
#131598=CARTESIAN_POINT('Ctrl Pts',(-7.92800984556395,-71.8560534185071,
12.));
#131599=CARTESIAN_POINT('Ctrl Pts',(-7.91690840359367,-71.8341666130426,
0.));
#131600=CARTESIAN_POINT('Ctrl Pts',(-7.91690840359367,-71.8341666130426,
12.));
#131601=CARTESIAN_POINT('Ctrl Pts',(-7.90584669580955,-71.8123058619042,
0.));
#131602=CARTESIAN_POINT('Ctrl Pts',(-7.90584669580955,-71.8123058619042,
12.));
#131603=CARTESIAN_POINT('Ctrl Pts',(-7.89482472132137,-71.7904712930175,
0.));
#131604=CARTESIAN_POINT('Ctrl Pts',(-7.89482472132137,-71.7904712930175,
12.));
#131605=CARTESIAN_POINT('Ctrl Pts',(-7.88384247914523,-71.7686630348238,
0.));
#131606=CARTESIAN_POINT('Ctrl Pts',(-7.88384247914523,-71.7686630348238,
12.));
#131607=CARTESIAN_POINT('Ctrl Pts',(-7.87289996819653,-71.7468812162788,
0.));
#131608=CARTESIAN_POINT('Ctrl Pts',(-7.87289996819653,-71.7468812162788,
12.));
#131609=CARTESIAN_POINT('Ctrl Pts',(-7.86199718728826,-71.7251259668563,
0.));
#131610=CARTESIAN_POINT('Ctrl Pts',(-7.86199718728826,-71.7251259668563,
12.));
#131611=CARTESIAN_POINT('Ctrl Pts',(-7.85113413513735,-71.7033974165568,
0.));
#131612=CARTESIAN_POINT('Ctrl Pts',(-7.85113413513735,-71.7033974165568,
12.));
#131613=CARTESIAN_POINT('Ctrl Pts',(-7.84031081036489,-71.6816956959117,
0.));
#131614=CARTESIAN_POINT('Ctrl Pts',(-7.84031081036489,-71.6816956959117,
12.));
#131615=CARTESIAN_POINT('Ctrl Pts',(-7.82952721149507,-71.6600209359872,
0.));
#131616=CARTESIAN_POINT('Ctrl Pts',(-7.82952721149507,-71.6600209359872,
12.));
#131617=CARTESIAN_POINT('Ctrl Pts',(-7.8187833369486,-71.6383732683844,
0.));
#131618=CARTESIAN_POINT('Ctrl Pts',(-7.8187833369486,-71.6383732683844,
12.));
#131619=CARTESIAN_POINT('Ctrl Pts',(-7.80807918504021,-71.6167528252423,
0.));
#131620=CARTESIAN_POINT('Ctrl Pts',(-7.80807918504021,-71.6167528252423,
12.));
#131621=CARTESIAN_POINT('Ctrl Pts',(-7.79741475398513,-71.5951597392471,
0.));
#131622=CARTESIAN_POINT('Ctrl Pts',(-7.79741475398513,-71.5951597392471,
12.));
#131623=CARTESIAN_POINT('Ctrl Pts',(-7.78679004189934,-71.5735941436364,
0.));
#131624=CARTESIAN_POINT('Ctrl Pts',(-7.78679004189934,-71.5735941436364,
12.));
#131625=CARTESIAN_POINT('Ctrl Pts',(-7.77620504679869,-71.5520561722039,
0.));
#131626=CARTESIAN_POINT('Ctrl Pts',(-7.77620504679869,-71.5520561722039,
12.));
#131627=CARTESIAN_POINT('Ctrl Pts',(-7.76565976659226,-71.5305459592994,
0.));
#131628=CARTESIAN_POINT('Ctrl Pts',(-7.76565976659226,-71.5305459592994,
12.));
#131629=CARTESIAN_POINT('Ctrl Pts',(-7.75515419907966,-71.5090636398318,
0.));
#131630=CARTESIAN_POINT('Ctrl Pts',(-7.75515419907966,-71.5090636398318,
12.));
#131631=CARTESIAN_POINT('Ctrl Pts',(-7.74468834195746,-71.4876093492781,
0.));
#131632=CARTESIAN_POINT('Ctrl Pts',(-7.74468834195746,-71.4876093492781,
12.));
#131633=CARTESIAN_POINT('Ctrl Pts',(-7.7342621928194,-71.4661832236888,
0.));
#131634=CARTESIAN_POINT('Ctrl Pts',(-7.7342621928194,-71.4661832236888,
12.));
#131635=CARTESIAN_POINT('Ctrl Pts',(-7.72387574915544,-71.4447853996916,
0.));
#131636=CARTESIAN_POINT('Ctrl Pts',(-7.72387574915544,-71.4447853996916,
12.));
#131637=CARTESIAN_POINT('Ctrl Pts',(-7.7135290083452,-71.4234160144925,
0.));
#131638=CARTESIAN_POINT('Ctrl Pts',(-7.7135290083452,-71.4234160144925,
12.));
#131639=CARTESIAN_POINT('Ctrl Pts',(-7.70322196765538,-71.4020752058796,
0.));
#131640=CARTESIAN_POINT('Ctrl Pts',(-7.70322196765538,-71.4020752058796,
12.));
#131641=CARTESIAN_POINT('Ctrl Pts',(-7.69295462424611,-71.3807631122331,
0.));
#131642=CARTESIAN_POINT('Ctrl Pts',(-7.69295462424611,-71.3807631122331,
12.));
#131643=CARTESIAN_POINT('Ctrl Pts',(-7.68272697517086,-71.3594798725281,
0.));
#131644=CARTESIAN_POINT('Ctrl Pts',(-7.68272697517086,-71.3594798725281,
12.));
#131645=CARTESIAN_POINT('Ctrl Pts',(-7.67253901737552,-71.3382256263414,
0.));
#131646=CARTESIAN_POINT('Ctrl Pts',(-7.67253901737552,-71.3382256263414,
12.));
#131647=CARTESIAN_POINT('Ctrl Pts',(-7.66239074769163,-71.3170005138502,
0.));
#131648=CARTESIAN_POINT('Ctrl Pts',(-7.66239074769163,-71.3170005138502,
12.));
#131649=CARTESIAN_POINT('Ctrl Pts',(-7.65228216283403,-71.2958046758372,
0.));
#131650=CARTESIAN_POINT('Ctrl Pts',(-7.65228216283403,-71.2958046758372,
12.));
#131651=CARTESIAN_POINT('Ctrl Pts',(-7.64221325940724,-71.2746382537007,
0.));
#131652=CARTESIAN_POINT('Ctrl Pts',(-7.64221325940724,-71.2746382537007,
12.));
#131653=CARTESIAN_POINT('Ctrl Pts',(-7.63218403390537,-71.2535013894602,
0.));
#131654=CARTESIAN_POINT('Ctrl Pts',(-7.63218403390537,-71.2535013894602,
12.));
#131655=CARTESIAN_POINT('Ctrl Pts',(-7.62219448271109,-71.2323942257609,
0.));
#131656=CARTESIAN_POINT('Ctrl Pts',(-7.62219448271109,-71.2323942257609,
12.));
#131657=CARTESIAN_POINT('Ctrl Pts',(-7.61224460208837,-71.211316905874,
0.));
#131658=CARTESIAN_POINT('Ctrl Pts',(-7.61224460208837,-71.211316905874,
12.));
#131659=CARTESIAN_POINT('Ctrl Pts',(-7.60233438818096,-71.1902695737013,
0.));
#131660=CARTESIAN_POINT('Ctrl Pts',(-7.60233438818096,-71.1902695737013,
12.));
#131661=CARTESIAN_POINT('Ctrl Pts',(-7.59246383701813,-71.1692523737844,
0.));
#131662=CARTESIAN_POINT('Ctrl Pts',(-7.59246383701813,-71.1692523737844,
12.));
#131663=CARTESIAN_POINT('Ctrl Pts',(-7.58263294451451,-71.1482654513119,
0.));
#131664=CARTESIAN_POINT('Ctrl Pts',(-7.58263294451451,-71.1482654513119,
12.));
#131665=CARTESIAN_POINT('Ctrl Pts',(-7.57284170646886,-71.1273089521234,
0.));
#131666=CARTESIAN_POINT('Ctrl Pts',(-7.57284170646886,-71.1273089521234,
12.));
#131667=CARTESIAN_POINT('Ctrl Pts',(-7.56309011855657,-71.106383022711,
0.));
#131668=CARTESIAN_POINT('Ctrl Pts',(-7.56309011855657,-71.106383022711,
12.));
#131669=CARTESIAN_POINT('Ctrl Pts',(-7.55337817632916,-71.0854878102243,
0.));
#131670=CARTESIAN_POINT('Ctrl Pts',(-7.55337817632916,-71.0854878102243,
12.));
#131671=CARTESIAN_POINT('Ctrl Pts',(-7.54370587521979,-71.0646234624811,
0.));
#131672=CARTESIAN_POINT('Ctrl Pts',(-7.54370587521979,-71.0646234624811,
12.));
#131673=CARTESIAN_POINT('Ctrl Pts',(-7.53407321054262,-71.043790127973,
0.));
#131674=CARTESIAN_POINT('Ctrl Pts',(-7.53407321054262,-71.043790127973,
12.));
#131675=CARTESIAN_POINT('Ctrl Pts',(-7.52448017749124,-71.0229879558699,
0.));
#131676=CARTESIAN_POINT('Ctrl Pts',(-7.52448017749124,-71.0229879558699,
12.));
#131677=CARTESIAN_POINT('Ctrl Pts',(-7.5149267711309,-71.002217096021,0.));
#131678=CARTESIAN_POINT('Ctrl Pts',(-7.5149267711309,-71.002217096021,12.));
#131679=CARTESIAN_POINT('Ctrl Pts',(-7.50541298639928,-70.9814776989612,
0.));
#131680=CARTESIAN_POINT('Ctrl Pts',(-7.50541298639928,-70.9814776989612,
12.));
#131681=CARTESIAN_POINT('Ctrl Pts',(-7.4959388181113,-70.9607699159218,
0.));
#131682=CARTESIAN_POINT('Ctrl Pts',(-7.4959388181113,-70.9607699159218,
12.));
#131683=CARTESIAN_POINT('Ctrl Pts',(-7.48650426095823,-70.940093898837,
0.));
#131684=CARTESIAN_POINT('Ctrl Pts',(-7.48650426095823,-70.940093898837,
12.));
#131685=CARTESIAN_POINT('Ctrl Pts',(-7.47710930950562,-70.9194498003493,
0.));
#131686=CARTESIAN_POINT('Ctrl Pts',(-7.47710930950562,-70.9194498003493,
12.));
#131687=CARTESIAN_POINT('Ctrl Pts',(-7.46775395818527,-70.8988377738104,
0.));
#131688=CARTESIAN_POINT('Ctrl Pts',(-7.46775395818527,-70.8988377738104,
12.));
#131689=CARTESIAN_POINT('Ctrl Pts',(-7.45843820129782,-70.87825797329,0.));
#131690=CARTESIAN_POINT('Ctrl Pts',(-7.45843820129782,-70.87825797329,12.));
#131691=CARTESIAN_POINT('Ctrl Pts',(-7.44916203301647,-70.8577105535848,
0.));
#131692=CARTESIAN_POINT('Ctrl Pts',(-7.44916203301647,-70.8577105535848,
12.));
#131693=CARTESIAN_POINT('Ctrl Pts',(-7.43992544738605,-70.8371956702241,
0.));
#131694=CARTESIAN_POINT('Ctrl Pts',(-7.43992544738605,-70.8371956702241,
12.));
#131695=CARTESIAN_POINT('Ctrl Pts',(-7.43072843832014,-70.8167134794737,
0.));
#131696=CARTESIAN_POINT('Ctrl Pts',(-7.43072843832014,-70.8167134794737,
12.));
#131697=CARTESIAN_POINT('Ctrl Pts',(-7.42157099959326,-70.796264138335,
0.));
#131698=CARTESIAN_POINT('Ctrl Pts',(-7.42157099959326,-70.796264138335,
12.));
#131699=CARTESIAN_POINT('Ctrl Pts',(-7.41245312484497,-70.7758478045576,
0.));
#131700=CARTESIAN_POINT('Ctrl Pts',(-7.41245312484497,-70.7758478045576,
12.));
#131701=CARTESIAN_POINT('Ctrl Pts',(-7.40337480758237,-70.7554646366514,
0.));
#131702=CARTESIAN_POINT('Ctrl Pts',(-7.40337480758237,-70.7554646366514,
12.));
#131703=CARTESIAN_POINT('Ctrl Pts',(-7.39433604117891,-70.735114793895,
0.));
#131704=CARTESIAN_POINT('Ctrl Pts',(-7.39433604117891,-70.735114793895,
12.));
#131705=CARTESIAN_POINT('Ctrl Pts',(-7.38533681887027,-70.7147984363423,
0.));
#131706=CARTESIAN_POINT('Ctrl Pts',(-7.38533681887027,-70.7147984363423,
12.));
#131707=CARTESIAN_POINT('Ctrl Pts',(-7.3763771337476,-70.6945157248269,
0.));
#131708=CARTESIAN_POINT('Ctrl Pts',(-7.3763771337476,-70.6945157248269,
12.));
#131709=CARTESIAN_POINT('Ctrl Pts',(-7.36745697876295,-70.6742668209685,
0.));
#131710=CARTESIAN_POINT('Ctrl Pts',(-7.36745697876295,-70.6742668209685,
12.));
#131711=CARTESIAN_POINT('Ctrl Pts',(-7.35857634673051,-70.6540518871772,
0.));
#131712=CARTESIAN_POINT('Ctrl Pts',(-7.35857634673051,-70.6540518871772,
12.));
#131713=CARTESIAN_POINT('Ctrl Pts',(-7.3497352303258,-70.6338710866562,
0.));
#131714=CARTESIAN_POINT('Ctrl Pts',(-7.3497352303258,-70.6338710866562,
12.));
#131715=CARTESIAN_POINT('Ctrl Pts',(-7.34093362208017,-70.6137245834002,
0.));
#131716=CARTESIAN_POINT('Ctrl Pts',(-7.34093362208017,-70.6137245834002,
12.));
#131717=CARTESIAN_POINT('Ctrl Pts',(-7.33217151437608,-70.5936125421958,
0.));
#131718=CARTESIAN_POINT('Ctrl Pts',(-7.33217151437608,-70.5936125421958,
12.));
#131719=CARTESIAN_POINT('Ctrl Pts',(-7.32344889945237,-70.573535128649,
0.));
#131720=CARTESIAN_POINT('Ctrl Pts',(-7.32344889945237,-70.573535128649,
12.));
#131721=CARTESIAN_POINT('Ctrl Pts',(-7.31476576940403,-70.5534925092053,
0.));
#131722=CARTESIAN_POINT('Ctrl Pts',(-7.31476576940403,-70.5534925092053,
12.));
#131723=CARTESIAN_POINT('Ctrl Pts',(-7.30612211618047,-70.5334848511675,
0.));
#131724=CARTESIAN_POINT('Ctrl Pts',(-7.30612211618047,-70.5334848511675,
12.));
#131725=CARTESIAN_POINT('Ctrl Pts',(-7.29751793157801,-70.5135123227147,
0.));
#131726=CARTESIAN_POINT('Ctrl Pts',(-7.29751793157801,-70.5135123227147,
12.));
#131727=CARTESIAN_POINT('Ctrl Pts',(-7.28895320723835,-70.4935750929029,
0.));
#131728=CARTESIAN_POINT('Ctrl Pts',(-7.28895320723835,-70.4935750929029,
12.));
#131729=CARTESIAN_POINT('Ctrl Pts',(-7.28042793465449,-70.4736733316463,
0.));
#131730=CARTESIAN_POINT('Ctrl Pts',(-7.28042793465449,-70.4736733316463,
12.));
#131731=CARTESIAN_POINT('Ctrl Pts',(-7.27194210517057,-70.4538072096986,
0.));
#131732=CARTESIAN_POINT('Ctrl Pts',(-7.27194210517057,-70.4538072096986,
12.));
#131733=CARTESIAN_POINT('Ctrl Pts',(-7.2634957099805,-70.433976898636,0.));
#131734=CARTESIAN_POINT('Ctrl Pts',(-7.2634957099805,-70.433976898636,12.));
#131735=CARTESIAN_POINT('Ctrl Pts',(-7.25508874012075,-70.4141825708207,
0.));
#131736=CARTESIAN_POINT('Ctrl Pts',(-7.25508874012075,-70.4141825708207,
12.));
#131737=CARTESIAN_POINT('Ctrl Pts',(-7.24672118647116,-70.3944243994532,
0.));
#131738=CARTESIAN_POINT('Ctrl Pts',(-7.24672118647116,-70.3944243994532,
12.));
#131739=CARTESIAN_POINT('Ctrl Pts',(-7.23839303975626,-70.3747025586569,
0.));
#131740=CARTESIAN_POINT('Ctrl Pts',(-7.23839303975626,-70.3747025586569,
12.));
#131741=CARTESIAN_POINT('Ctrl Pts',(-7.2301042905423,-70.3550172235486,
0.));
#131742=CARTESIAN_POINT('Ctrl Pts',(-7.2301042905423,-70.3550172235486,
12.));
#131743=CARTESIAN_POINT('Ctrl Pts',(-7.22185492923177,-70.3353685703097,
0.));
#131744=CARTESIAN_POINT('Ctrl Pts',(-7.22185492923177,-70.3353685703097,
12.));
#131745=CARTESIAN_POINT('Ctrl Pts',(-7.21364494605424,-70.3157567762561,
0.));
#131746=CARTESIAN_POINT('Ctrl Pts',(-7.21364494605424,-70.3157567762561,
12.));
#131747=CARTESIAN_POINT('Ctrl Pts',(-7.20547433107457,-70.2961820197051,
0.));
#131748=CARTESIAN_POINT('Ctrl Pts',(-7.20547433107457,-70.2961820197051,
12.));
#131749=CARTESIAN_POINT('Ctrl Pts',(-7.1973430741986,-70.276644479827,0.));
#131750=CARTESIAN_POINT('Ctrl Pts',(-7.1973430741986,-70.276644479827,12.));
#131751=CARTESIAN_POINT('Ctrl Pts',(-7.18925116517562,-70.2571443365198,
0.));
#131752=CARTESIAN_POINT('Ctrl Pts',(-7.18925116517562,-70.2571443365198,
12.));
#131753=CARTESIAN_POINT('Ctrl Pts',(-7.181198593598,-70.2376817702239,0.));
#131754=CARTESIAN_POINT('Ctrl Pts',(-7.181198593598,-70.2376817702239,12.));
#131755=CARTESIAN_POINT('Ctrl Pts',(-7.17318534889747,-70.2182569619028,
0.));
#131756=CARTESIAN_POINT('Ctrl Pts',(-7.17318534889747,-70.2182569619028,
12.));
#131757=CARTESIAN_POINT('Ctrl Pts',(-7.16521142033892,-70.1988700934622,
0.));
#131758=CARTESIAN_POINT('Ctrl Pts',(-7.16521142033892,-70.1988700934622,
12.));
#131759=CARTESIAN_POINT('Ctrl Pts',(-7.15727679700946,-70.1795213481196,
0.));
#131760=CARTESIAN_POINT('Ctrl Pts',(-7.15727679700946,-70.1795213481196,
12.));
#131761=CARTESIAN_POINT('Ctrl Pts',(-7.14938146780801,-70.1602109107188,
0.));
#131762=CARTESIAN_POINT('Ctrl Pts',(-7.14938146780801,-70.1602109107188,
12.));
#131763=CARTESIAN_POINT('Ctrl Pts',(-7.14152542142338,-70.1409389682389,
0.));
#131764=CARTESIAN_POINT('Ctrl Pts',(-7.14152542142338,-70.1409389682389,
12.));
#131765=CARTESIAN_POINT('Ctrl Pts',(-7.13370864634398,-70.1217057094456,
0.));
#131766=CARTESIAN_POINT('Ctrl Pts',(-7.13370864634398,-70.1217057094456,
12.));
#131767=CARTESIAN_POINT('Ctrl Pts',(-7.1259311308887,-70.1025113239463,
0.));
#131768=CARTESIAN_POINT('Ctrl Pts',(-7.1259311308887,-70.1025113239463,
12.));
#131769=CARTESIAN_POINT('Ctrl Pts',(-7.11819286322823,-70.0833560013971,
0.));
#131770=CARTESIAN_POINT('Ctrl Pts',(-7.11819286322823,-70.0833560013971,
12.));
#131771=CARTESIAN_POINT('Ctrl Pts',(-7.11049383140481,-70.06423993069,0.));
#131772=CARTESIAN_POINT('Ctrl Pts',(-7.11049383140481,-70.06423993069,12.));
#131773=CARTESIAN_POINT('Ctrl Pts',(-7.10283402335091,-70.0451632990137,
0.));
#131774=CARTESIAN_POINT('Ctrl Pts',(-7.10283402335091,-70.0451632990137,
12.));
#131775=CARTESIAN_POINT('Ctrl Pts',(-7.09521342684301,-70.0261262936435,
0.));
#131776=CARTESIAN_POINT('Ctrl Pts',(-7.09521342684301,-70.0261262936435,
12.));
#131777=CARTESIAN_POINT('Ctrl Pts',(-7.08763202944274,-70.0071291040791,
0.));
#131778=CARTESIAN_POINT('Ctrl Pts',(-7.08763202944274,-70.0071291040791,
12.));
#131779=CARTESIAN_POINT('Ctrl Pts',(-7.08008981844642,-69.988171923787,
0.));
#131780=CARTESIAN_POINT('Ctrl Pts',(-7.08008981844642,-69.988171923787,
12.));
#131781=CARTESIAN_POINT('Ctrl Pts',(-7.07258678080792,-69.9692549527256,
0.));
#131782=CARTESIAN_POINT('Ctrl Pts',(-7.07258678080792,-69.9692549527256,
12.));
#131783=CARTESIAN_POINT('Ctrl Pts',(-7.06512290312802,-69.9503783975676,
0.));
#131784=CARTESIAN_POINT('Ctrl Pts',(-7.06512290312802,-69.9503783975676,
12.));
#131785=CARTESIAN_POINT('Ctrl Pts',(-7.05769817180824,-69.9315424664252,
0.));
#131786=CARTESIAN_POINT('Ctrl Pts',(-7.05769817180824,-69.9315424664252,
12.));
#131787=CARTESIAN_POINT('Ctrl Pts',(-7.05031257318107,-69.9127473642087,
0.));
#131788=CARTESIAN_POINT('Ctrl Pts',(-7.05031257318107,-69.9127473642087,
12.));
#131789=CARTESIAN_POINT('Ctrl Pts',(-7.04296609362186,-69.8939932885864,
0.));
#131790=CARTESIAN_POINT('Ctrl Pts',(-7.04296609362186,-69.8939932885864,
12.));
#131791=CARTESIAN_POINT('Ctrl Pts',(-7.03565871972265,-69.8752804235296,
0.));
#131792=CARTESIAN_POINT('Ctrl Pts',(-7.03565871972265,-69.8752804235296,
12.));
#131793=CARTESIAN_POINT('Ctrl Pts',(-7.02839043811862,-69.8566089455448,
0.));
#131794=CARTESIAN_POINT('Ctrl Pts',(-7.02839043811862,-69.8566089455448,
12.));
#131795=CARTESIAN_POINT('Ctrl Pts',(-7.02116123514487,-69.8379790360574,
0.));
#131796=CARTESIAN_POINT('Ctrl Pts',(-7.02116123514487,-69.8379790360574,
12.));
#131797=CARTESIAN_POINT('Ctrl Pts',(-7.01397109655455,-69.8193908913722,
0.));
#131798=CARTESIAN_POINT('Ctrl Pts',(-7.01397109655455,-69.8193908913722,
12.));
#131799=CARTESIAN_POINT('Ctrl Pts',(-7.00682000718104,-69.8008447346782,
0.));
#131800=CARTESIAN_POINT('Ctrl Pts',(-7.00682000718104,-69.8008447346782,
12.));
#131801=CARTESIAN_POINT('Ctrl Pts',(-6.99970795069399,-69.7823408242446,
0.));
#131802=CARTESIAN_POINT('Ctrl Pts',(-6.99970795069399,-69.7823408242446,
12.));
#131803=CARTESIAN_POINT('Ctrl Pts',(-6.99263491027859,-69.7638794280263,
0.));
#131804=CARTESIAN_POINT('Ctrl Pts',(-6.99263491027859,-69.7638794280263,
12.));
#131805=CARTESIAN_POINT('Ctrl Pts',(-6.98560086924172,-69.7454607995524,
0.));
#131806=CARTESIAN_POINT('Ctrl Pts',(-6.98560086924172,-69.7454607995524,
12.));
#131807=CARTESIAN_POINT('Ctrl Pts',(-6.97860581164568,-69.7270851557443,
0.));
#131808=CARTESIAN_POINT('Ctrl Pts',(-6.97860581164568,-69.7270851557443,
12.));
#131809=CARTESIAN_POINT('Ctrl Pts',(-6.97164972291581,-69.7087526480249,
0.));
#131810=CARTESIAN_POINT('Ctrl Pts',(-6.97164972291581,-69.7087526480249,
12.));
#131811=CARTESIAN_POINT('Ctrl Pts',(-6.96473259049729,-69.6904633605834,
0.));
#131812=CARTESIAN_POINT('Ctrl Pts',(-6.96473259049729,-69.6904633605834,
12.));
#131813=CARTESIAN_POINT('Ctrl Pts',(-6.95923004173795,-69.6758665380764,
0.));
#131814=CARTESIAN_POINT('Ctrl Pts',(-6.95923004173795,-69.6758665380764,
12.));
#131815=CARTESIAN_POINT('Ctrl Pts',(-6.9551206531773,-69.6649383920075,
0.));
#131816=CARTESIAN_POINT('Ctrl Pts',(-6.9551206531773,-69.6649383920075,
12.));
#131817=CARTESIAN_POINT('Ctrl Pts',(-6.95238884849075,-69.6576616146559,
0.));
#131818=CARTESIAN_POINT('Ctrl Pts',(-6.95238884849075,-69.6576616146559,
12.));
#131819=CARTESIAN_POINT('Ctrl Pts',(-6.95102489306927,-69.6540253893193,
0.));
#131820=CARTESIAN_POINT('Ctrl Pts',(-6.95102489306927,-69.6540253893193,
12.));
#131821=CARTESIAN_POINT('',(-6.95102489306927,-69.6540253893193,12.));
#131822=CARTESIAN_POINT('Ctrl Pts',(-6.95102489306927,-69.6540253893193,
12.));
#131823=CARTESIAN_POINT('Ctrl Pts',(-6.95238884849075,-69.6576616146559,
12.));
#131824=CARTESIAN_POINT('Ctrl Pts',(-6.9551206531773,-69.6649383920075,
12.));
#131825=CARTESIAN_POINT('Ctrl Pts',(-6.95923004173795,-69.6758665380764,
12.));
#131826=CARTESIAN_POINT('Ctrl Pts',(-6.96473259049729,-69.6904633605834,
12.));
#131827=CARTESIAN_POINT('Ctrl Pts',(-6.97164972291581,-69.7087526480249,
12.));
#131828=CARTESIAN_POINT('Ctrl Pts',(-6.97860581164568,-69.7270851557443,
12.));
#131829=CARTESIAN_POINT('Ctrl Pts',(-6.98560086924172,-69.7454607995524,
12.));
#131830=CARTESIAN_POINT('Ctrl Pts',(-6.99263491027859,-69.7638794280263,
12.));
#131831=CARTESIAN_POINT('Ctrl Pts',(-6.99970795069399,-69.7823408242446,
12.));
#131832=CARTESIAN_POINT('Ctrl Pts',(-7.00682000718104,-69.8008447346782,
12.));
#131833=CARTESIAN_POINT('Ctrl Pts',(-7.01397109655455,-69.8193908913722,
12.));
#131834=CARTESIAN_POINT('Ctrl Pts',(-7.02116123514487,-69.8379790360574,
12.));
#131835=CARTESIAN_POINT('Ctrl Pts',(-7.02839043811862,-69.8566089455448,
12.));
#131836=CARTESIAN_POINT('Ctrl Pts',(-7.03565871972265,-69.8752804235296,
12.));
#131837=CARTESIAN_POINT('Ctrl Pts',(-7.04296609362186,-69.8939932885864,
12.));
#131838=CARTESIAN_POINT('Ctrl Pts',(-7.05031257318107,-69.9127473642087,
12.));
#131839=CARTESIAN_POINT('Ctrl Pts',(-7.05769817180824,-69.9315424664252,
12.));
#131840=CARTESIAN_POINT('Ctrl Pts',(-7.06512290312802,-69.9503783975676,
12.));
#131841=CARTESIAN_POINT('Ctrl Pts',(-7.07258678080792,-69.9692549527256,
12.));
#131842=CARTESIAN_POINT('Ctrl Pts',(-7.08008981844642,-69.988171923787,
12.));
#131843=CARTESIAN_POINT('Ctrl Pts',(-7.08763202944274,-70.0071291040791,
12.));
#131844=CARTESIAN_POINT('Ctrl Pts',(-7.09521342684301,-70.0261262936435,
12.));
#131845=CARTESIAN_POINT('Ctrl Pts',(-7.10283402335091,-70.0451632990137,
12.));
#131846=CARTESIAN_POINT('Ctrl Pts',(-7.11049383140481,-70.06423993069,12.));
#131847=CARTESIAN_POINT('Ctrl Pts',(-7.11819286322823,-70.0833560013971,
12.));
#131848=CARTESIAN_POINT('Ctrl Pts',(-7.1259311308887,-70.1025113239463,
12.));
#131849=CARTESIAN_POINT('Ctrl Pts',(-7.13370864634398,-70.1217057094456,
12.));
#131850=CARTESIAN_POINT('Ctrl Pts',(-7.14152542142338,-70.1409389682389,
12.));
#131851=CARTESIAN_POINT('Ctrl Pts',(-7.14938146780801,-70.1602109107188,
12.));
#131852=CARTESIAN_POINT('Ctrl Pts',(-7.15727679700946,-70.1795213481196,
12.));
#131853=CARTESIAN_POINT('Ctrl Pts',(-7.16521142033892,-70.1988700934622,
12.));
#131854=CARTESIAN_POINT('Ctrl Pts',(-7.17318534889747,-70.2182569619028,
12.));
#131855=CARTESIAN_POINT('Ctrl Pts',(-7.181198593598,-70.2376817702239,12.));
#131856=CARTESIAN_POINT('Ctrl Pts',(-7.18925116517562,-70.2571443365198,
12.));
#131857=CARTESIAN_POINT('Ctrl Pts',(-7.1973430741986,-70.276644479827,12.));
#131858=CARTESIAN_POINT('Ctrl Pts',(-7.20547433107457,-70.2961820197051,
12.));
#131859=CARTESIAN_POINT('Ctrl Pts',(-7.21364494605424,-70.3157567762561,
12.));
#131860=CARTESIAN_POINT('Ctrl Pts',(-7.22185492923177,-70.3353685703097,
12.));
#131861=CARTESIAN_POINT('Ctrl Pts',(-7.2301042905423,-70.3550172235486,
12.));
#131862=CARTESIAN_POINT('Ctrl Pts',(-7.23839303975626,-70.3747025586569,
12.));
#131863=CARTESIAN_POINT('Ctrl Pts',(-7.24672118647116,-70.3944243994532,
12.));
#131864=CARTESIAN_POINT('Ctrl Pts',(-7.25508874012075,-70.4141825708207,
12.));
#131865=CARTESIAN_POINT('Ctrl Pts',(-7.2634957099805,-70.433976898636,12.));
#131866=CARTESIAN_POINT('Ctrl Pts',(-7.27194210517057,-70.4538072096986,
12.));
#131867=CARTESIAN_POINT('Ctrl Pts',(-7.28042793465449,-70.4736733316463,
12.));
#131868=CARTESIAN_POINT('Ctrl Pts',(-7.28895320723835,-70.4935750929029,
12.));
#131869=CARTESIAN_POINT('Ctrl Pts',(-7.29751793157801,-70.5135123227147,
12.));
#131870=CARTESIAN_POINT('Ctrl Pts',(-7.30612211618047,-70.5334848511675,
12.));
#131871=CARTESIAN_POINT('Ctrl Pts',(-7.31476576940403,-70.5534925092053,
12.));
#131872=CARTESIAN_POINT('Ctrl Pts',(-7.32344889945237,-70.573535128649,
12.));
#131873=CARTESIAN_POINT('Ctrl Pts',(-7.33217151437608,-70.5936125421958,
12.));
#131874=CARTESIAN_POINT('Ctrl Pts',(-7.34093362208017,-70.6137245834002,
12.));
#131875=CARTESIAN_POINT('Ctrl Pts',(-7.3497352303258,-70.6338710866562,
12.));
#131876=CARTESIAN_POINT('Ctrl Pts',(-7.35857634673051,-70.6540518871772,
12.));
#131877=CARTESIAN_POINT('Ctrl Pts',(-7.36745697876295,-70.6742668209685,
12.));
#131878=CARTESIAN_POINT('Ctrl Pts',(-7.3763771337476,-70.6945157248269,
12.));
#131879=CARTESIAN_POINT('Ctrl Pts',(-7.38533681887027,-70.7147984363423,
12.));
#131880=CARTESIAN_POINT('Ctrl Pts',(-7.39433604117891,-70.735114793895,
12.));
#131881=CARTESIAN_POINT('Ctrl Pts',(-7.40337480758237,-70.7554646366514,
12.));
#131882=CARTESIAN_POINT('Ctrl Pts',(-7.41245312484497,-70.7758478045576,
12.));
#131883=CARTESIAN_POINT('Ctrl Pts',(-7.42157099959326,-70.796264138335,
12.));
#131884=CARTESIAN_POINT('Ctrl Pts',(-7.43072843832014,-70.8167134794737,
12.));
#131885=CARTESIAN_POINT('Ctrl Pts',(-7.43992544738605,-70.8371956702241,
12.));
#131886=CARTESIAN_POINT('Ctrl Pts',(-7.44916203301647,-70.8577105535848,
12.));
#131887=CARTESIAN_POINT('Ctrl Pts',(-7.45843820129782,-70.87825797329,12.));
#131888=CARTESIAN_POINT('Ctrl Pts',(-7.46775395818527,-70.8988377738104,
12.));
#131889=CARTESIAN_POINT('Ctrl Pts',(-7.47710930950562,-70.9194498003493,
12.));
#131890=CARTESIAN_POINT('Ctrl Pts',(-7.48650426095823,-70.940093898837,
12.));
#131891=CARTESIAN_POINT('Ctrl Pts',(-7.4959388181113,-70.9607699159218,
12.));
#131892=CARTESIAN_POINT('Ctrl Pts',(-7.50541298639928,-70.9814776989612,
12.));
#131893=CARTESIAN_POINT('Ctrl Pts',(-7.5149267711309,-71.002217096021,12.));
#131894=CARTESIAN_POINT('Ctrl Pts',(-7.52448017749124,-71.0229879558699,
12.));
#131895=CARTESIAN_POINT('Ctrl Pts',(-7.53407321054262,-71.043790127973,
12.));
#131896=CARTESIAN_POINT('Ctrl Pts',(-7.54370587521979,-71.0646234624811,
12.));
#131897=CARTESIAN_POINT('Ctrl Pts',(-7.55337817632916,-71.0854878102243,
12.));
#131898=CARTESIAN_POINT('Ctrl Pts',(-7.56309011855657,-71.106383022711,
12.));
#131899=CARTESIAN_POINT('Ctrl Pts',(-7.57284170646886,-71.1273089521234,
12.));
#131900=CARTESIAN_POINT('Ctrl Pts',(-7.58263294451451,-71.1482654513119,
12.));
#131901=CARTESIAN_POINT('Ctrl Pts',(-7.59246383701813,-71.1692523737844,
12.));
#131902=CARTESIAN_POINT('Ctrl Pts',(-7.60233438818096,-71.1902695737013,
12.));
#131903=CARTESIAN_POINT('Ctrl Pts',(-7.61224460208837,-71.211316905874,
12.));
#131904=CARTESIAN_POINT('Ctrl Pts',(-7.62219448271109,-71.2323942257609,
12.));
#131905=CARTESIAN_POINT('Ctrl Pts',(-7.63218403390537,-71.2535013894602,
12.));
#131906=CARTESIAN_POINT('Ctrl Pts',(-7.64221325940724,-71.2746382537007,
12.));
#131907=CARTESIAN_POINT('Ctrl Pts',(-7.65228216283403,-71.2958046758372,
12.));
#131908=CARTESIAN_POINT('Ctrl Pts',(-7.66239074769163,-71.3170005138502,
12.));
#131909=CARTESIAN_POINT('Ctrl Pts',(-7.67253901737552,-71.3382256263414,
12.));
#131910=CARTESIAN_POINT('Ctrl Pts',(-7.68272697517086,-71.3594798725281,
12.));
#131911=CARTESIAN_POINT('Ctrl Pts',(-7.69295462424611,-71.3807631122331,
12.));
#131912=CARTESIAN_POINT('Ctrl Pts',(-7.70322196765538,-71.4020752058796,
12.));
#131913=CARTESIAN_POINT('Ctrl Pts',(-7.7135290083452,-71.4234160144925,
12.));
#131914=CARTESIAN_POINT('Ctrl Pts',(-7.72387574915544,-71.4447853996916,
12.));
#131915=CARTESIAN_POINT('Ctrl Pts',(-7.7342621928194,-71.4661832236888,
12.));
#131916=CARTESIAN_POINT('Ctrl Pts',(-7.74468834195746,-71.4876093492781,
12.));
#131917=CARTESIAN_POINT('Ctrl Pts',(-7.75515419907966,-71.5090636398318,
12.));
#131918=CARTESIAN_POINT('Ctrl Pts',(-7.76565976659226,-71.5305459592994,
12.));
#131919=CARTESIAN_POINT('Ctrl Pts',(-7.77620504679869,-71.5520561722039,
12.));
#131920=CARTESIAN_POINT('Ctrl Pts',(-7.78679004189934,-71.5735941436364,
12.));
#131921=CARTESIAN_POINT('Ctrl Pts',(-7.79741475398513,-71.5951597392471,
12.));
#131922=CARTESIAN_POINT('Ctrl Pts',(-7.80807918504021,-71.6167528252423,
12.));
#131923=CARTESIAN_POINT('Ctrl Pts',(-7.8187833369486,-71.6383732683844,
12.));
#131924=CARTESIAN_POINT('Ctrl Pts',(-7.82952721149507,-71.6600209359872,
12.));
#131925=CARTESIAN_POINT('Ctrl Pts',(-7.84031081036489,-71.6816956959117,
12.));
#131926=CARTESIAN_POINT('Ctrl Pts',(-7.85113413513735,-71.7033974165568,
12.));
#131927=CARTESIAN_POINT('Ctrl Pts',(-7.86199718728826,-71.7251259668563,
12.));
#131928=CARTESIAN_POINT('Ctrl Pts',(-7.87289996819653,-71.7468812162788,
12.));
#131929=CARTESIAN_POINT('Ctrl Pts',(-7.88384247914523,-71.7686630348238,
12.));
#131930=CARTESIAN_POINT('Ctrl Pts',(-7.89482472132137,-71.7904712930175,
12.));
#131931=CARTESIAN_POINT('Ctrl Pts',(-7.90584669580955,-71.8123058619042,
12.));
#131932=CARTESIAN_POINT('Ctrl Pts',(-7.91690840359367,-71.8341666130426,
12.));
#131933=CARTESIAN_POINT('Ctrl Pts',(-7.92800984556395,-71.8560534185071,
12.));
#131934=CARTESIAN_POINT('Ctrl Pts',(-7.93915102251794,-71.8779661508832,
12.));
#131935=CARTESIAN_POINT('Ctrl Pts',(-7.9503319351605,-71.8999046832643,
12.));
#131936=CARTESIAN_POINT('Ctrl Pts',(-7.96155258409763,-71.9218688892431,
12.));
#131937=CARTESIAN_POINT('Ctrl Pts',(-7.97281296983717,-71.9438586429081,
12.));
#131938=CARTESIAN_POINT('Ctrl Pts',(-7.98411309279612,-71.965873818843,
12.));
#131939=CARTESIAN_POINT('Ctrl Pts',(-7.99545295330191,-71.9879142921254,
12.));
#131940=CARTESIAN_POINT('Ctrl Pts',(-8.00683255159247,-72.0099799383213,
12.));
#131941=CARTESIAN_POINT('Ctrl Pts',(-8.01825188781056,-72.032070633479,
12.));
#131942=CARTESIAN_POINT('Ctrl Pts',(-8.02971096200307,-72.0541862541243,
12.));
#131943=CARTESIAN_POINT('Ctrl Pts',(-8.04120977412872,-72.0763266772615,
12.));
#131944=CARTESIAN_POINT('Ctrl Pts',(-8.05274832405948,-72.0984917803693,
12.));
#131945=CARTESIAN_POINT('Ctrl Pts',(-8.06432661158095,-72.1206814413988,
12.));
#131946=CARTESIAN_POINT('Ctrl Pts',(-8.07594463638719,-72.1428955387663,
12.));
#131947=CARTESIAN_POINT('Ctrl Pts',(-8.08760239807836,-72.1651339513477,
12.));
#131948=CARTESIAN_POINT('Ctrl Pts',(-8.09929989616889,-72.1873965584813,
12.));
#131949=CARTESIAN_POINT('Ctrl Pts',(-8.11103713008928,-72.209683239963,
12.));
#131950=CARTESIAN_POINT('Ctrl Pts',(-8.1228140991866,-72.2319938760449,
12.));
#131951=CARTESIAN_POINT('Ctrl Pts',(-8.13463080272028,-72.2543283474278,
12.));
#131952=CARTESIAN_POINT('Ctrl Pts',(-8.14648723985797,-72.2766865352555,
12.));
#131953=CARTESIAN_POINT('Ctrl Pts',(-8.15838340968335,-72.2990683211162,
12.));
#131954=CARTESIAN_POINT('Ctrl Pts',(-8.1703193111989,-72.3214735870409,
12.));
#131955=CARTESIAN_POINT('Ctrl Pts',(-8.18229494332623,-72.3439022155007,
12.));
#131956=CARTESIAN_POINT('Ctrl Pts',(-8.19431030490314,-72.3663540894026,
12.));
#131957=CARTESIAN_POINT('Ctrl Pts',(-8.20636539467776,-72.3888290920832,
12.));
#131958=CARTESIAN_POINT('Ctrl Pts',(-8.2184602113156,-72.4113271073079,
12.));
#131959=CARTESIAN_POINT('Ctrl Pts',(-8.23059475340356,-72.4338480192695,
12.));
#131960=CARTESIAN_POINT('Ctrl Pts',(-8.2427690194504,-72.4563917125842,
12.));
#131961=CARTESIAN_POINT('Ctrl Pts',(-8.25498300788493,-72.4789580722875,
12.));
#131962=CARTESIAN_POINT('Ctrl Pts',(-8.26723671704919,-72.5015469838254,
12.));
#131963=CARTESIAN_POINT('Ctrl Pts',(-8.27953014520376,-72.5241583330562,
12.));
#131964=CARTESIAN_POINT('Ctrl Pts',(-8.29186329053279,-72.5467920062521,
12.));
#131965=CARTESIAN_POINT('Ctrl Pts',(-8.30423615114452,-72.5694478900982,
12.));
#131966=CARTESIAN_POINT('Ctrl Pts',(-8.31664872507016,-72.5921258716901,
12.));
#131967=CARTESIAN_POINT('Ctrl Pts',(-8.3291010102567,-72.6148258385296,
12.));
#131968=CARTESIAN_POINT('Ctrl Pts',(-8.34159300456986,-72.6375476785215,
12.));
#131969=CARTESIAN_POINT('Ctrl Pts',(-8.35412470580101,-72.6602912799696,
12.));
#131970=CARTESIAN_POINT('Ctrl Pts',(-8.36669611166842,-72.6830565315703,
12.));
#131971=CARTESIAN_POINT('Ctrl Pts',(-8.37930721981731,-72.705843322407,
12.));
#131972=CARTESIAN_POINT('Ctrl Pts',(-8.3919580278139,-72.7286515419373,
12.));
#131973=CARTESIAN_POINT('Ctrl Pts',(-8.40464853314468,-72.751481079992,
12.));
#131974=CARTESIAN_POINT('Ctrl Pts',(-8.41737873322329,-72.7743318267865,
12.));
#131975=CARTESIAN_POINT('Ctrl Pts',(-8.43014862539157,-72.7972036729276,
12.));
#131976=CARTESIAN_POINT('Ctrl Pts',(-8.44295820691911,-72.8200965094199,
12.));
#131977=CARTESIAN_POINT('Ctrl Pts',(-8.45580747499793,-72.8430102276713,
12.));
#131978=CARTESIAN_POINT('Ctrl Pts',(-8.46869642673794,-72.8659447194933,
12.));
#131979=CARTESIAN_POINT('Ctrl Pts',(-8.48162505917657,-72.8888998770785,
12.));
#131980=CARTESIAN_POINT('Ctrl Pts',(-8.49459336928295,-72.9118755929795,
12.));
#131981=CARTESIAN_POINT('Ctrl Pts',(-8.50760135395983,-72.9348717600838,
12.));
#131982=CARTESIAN_POINT('Ctrl Pts',(-8.52064901004227,-72.9578882715912,
12.));
#131983=CARTESIAN_POINT('Ctrl Pts',(-8.5337363342928,-72.9809250209828,
12.));
#131984=CARTESIAN_POINT('Ctrl Pts',(-8.54686332340417,-73.0039819020648,
12.));
#131985=CARTESIAN_POINT('Ctrl Pts',(-8.56002997400083,-73.0270588090183,
12.));
#131986=CARTESIAN_POINT('Ctrl Pts',(-8.57323628263593,-73.0501556364479,
12.));
#131987=CARTESIAN_POINT('Ctrl Pts',(-8.58648224578731,-73.0732722794195,
12.));
#131988=CARTESIAN_POINT('Ctrl Pts',(-8.59976785984551,-73.0964086335235,
12.));
#131989=CARTESIAN_POINT('Ctrl Pts',(-8.61309312112001,-73.1195645948178,
12.));
#131990=CARTESIAN_POINT('Ctrl Pts',(-8.62645802585483,-73.1427400597037,
12.));
#131991=CARTESIAN_POINT('Ctrl Pts',(-8.63986257023738,-73.1659349248132,
12.));
#131992=CARTESIAN_POINT('Ctrl Pts',(-8.65330675040536,-73.1891490869056,
12.));
#131993=CARTESIAN_POINT('Ctrl Pts',(-8.66679056245091,-73.2123824427208,
12.));
#131994=CARTESIAN_POINT('Ctrl Pts',(-8.68031400241871,-73.2356348889693,
12.));
#131995=CARTESIAN_POINT('Ctrl Pts',(-8.69387706629285,-73.2589063226358,
12.));
#131996=CARTESIAN_POINT('Ctrl Pts',(-8.70747974998229,-73.2821966412148,
12.));
#131997=CARTESIAN_POINT('Ctrl Pts',(-8.72112204930231,-73.3055057429742,
12.));
#131998=CARTESIAN_POINT('Ctrl Pts',(-8.7348039599538,-73.3288335272002,
12.));
#131999=CARTESIAN_POINT('Ctrl Pts',(-8.74852547749778,-73.3521798944622,
12.));
#132000=CARTESIAN_POINT('Ctrl Pts',(-8.76228659740357,-73.3755447460269,
12.));
#132001=CARTESIAN_POINT('Ctrl Pts',(-8.77608731509347,-73.3989279832835,
12.));
#132002=CARTESIAN_POINT('Ctrl Pts',(-8.78992762598756,-73.422329507113,
12.));
#132003=CARTESIAN_POINT('Ctrl Pts',(-8.80380752553691,-73.4457492173933,
12.));
#132004=CARTESIAN_POINT('Ctrl Pts',(-8.8177270092753,-73.4691870121567,
12.));
#132005=CARTESIAN_POINT('Ctrl Pts',(-8.83168607277325,-73.492642788273,
12.));
#132006=CARTESIAN_POINT('Ctrl Pts',(-8.84568471153805,-73.5161164429709,
12.));
#132007=CARTESIAN_POINT('Ctrl Pts',(-8.8597229209213,-73.5396078751639,
12.));
#132008=CARTESIAN_POINT('Ctrl Pts',(-8.8738006960297,-73.5631169867122,
12.));
#132009=CARTESIAN_POINT('Ctrl Pts',(-8.88791803160442,-73.5866436840556,
12.));
#132010=CARTESIAN_POINT('Ctrl Pts',(-8.90207492199043,-73.6101878785976,
12.));
#132011=CARTESIAN_POINT('Ctrl Pts',(-8.91424402151604,-73.630384739363,
12.));
#132012=CARTESIAN_POINT('Ctrl Pts',(-8.92359518178502,-73.6458786306025,
12.));
#132013=CARTESIAN_POINT('Ctrl Pts',(-8.93011088817333,-73.6566618622077,
12.));
#132014=CARTESIAN_POINT('Ctrl Pts',(-8.93377955965658,-73.6627293782592,
12.));
#132015=CARTESIAN_POINT('Ctrl Pts',(-8.93459554657871,-73.6640787198061,
12.));
#132016=CARTESIAN_POINT('',(-6.95102489306927,-69.6540253893193,0.));
#132017=CARTESIAN_POINT('',(-6.95102489306927,-69.6540253893193,0.));
#132018=CARTESIAN_POINT('Ctrl Pts',(-8.93459554657871,-73.6640787198061,
0.));
#132019=CARTESIAN_POINT('Ctrl Pts',(-8.93377955965658,-73.6627293782592,
0.));
#132020=CARTESIAN_POINT('Ctrl Pts',(-8.93011088817333,-73.6566618622077,
0.));
#132021=CARTESIAN_POINT('Ctrl Pts',(-8.92359518178502,-73.6458786306025,
0.));
#132022=CARTESIAN_POINT('Ctrl Pts',(-8.91424402151604,-73.630384739363,
0.));
#132023=CARTESIAN_POINT('Ctrl Pts',(-8.90207492199043,-73.6101878785976,
0.));
#132024=CARTESIAN_POINT('Ctrl Pts',(-8.88791803160442,-73.5866436840556,
0.));
#132025=CARTESIAN_POINT('Ctrl Pts',(-8.8738006960297,-73.5631169867122,
0.));
#132026=CARTESIAN_POINT('Ctrl Pts',(-8.8597229209213,-73.5396078751639,
0.));
#132027=CARTESIAN_POINT('Ctrl Pts',(-8.84568471153805,-73.5161164429709,
0.));
#132028=CARTESIAN_POINT('Ctrl Pts',(-8.83168607277325,-73.492642788273,
0.));
#132029=CARTESIAN_POINT('Ctrl Pts',(-8.8177270092753,-73.4691870121567,
0.));
#132030=CARTESIAN_POINT('Ctrl Pts',(-8.80380752553691,-73.4457492173933,
0.));
#132031=CARTESIAN_POINT('Ctrl Pts',(-8.78992762598756,-73.422329507113,
0.));
#132032=CARTESIAN_POINT('Ctrl Pts',(-8.77608731509347,-73.3989279832835,
0.));
#132033=CARTESIAN_POINT('Ctrl Pts',(-8.76228659740357,-73.3755447460269,
0.));
#132034=CARTESIAN_POINT('Ctrl Pts',(-8.74852547749778,-73.3521798944622,
0.));
#132035=CARTESIAN_POINT('Ctrl Pts',(-8.7348039599538,-73.3288335272002,
0.));
#132036=CARTESIAN_POINT('Ctrl Pts',(-8.72112204930231,-73.3055057429742,
0.));
#132037=CARTESIAN_POINT('Ctrl Pts',(-8.70747974998229,-73.2821966412148,
0.));
#132038=CARTESIAN_POINT('Ctrl Pts',(-8.69387706629285,-73.2589063226358,
0.));
#132039=CARTESIAN_POINT('Ctrl Pts',(-8.68031400241871,-73.2356348889693,
0.));
#132040=CARTESIAN_POINT('Ctrl Pts',(-8.66679056245091,-73.2123824427208,
0.));
#132041=CARTESIAN_POINT('Ctrl Pts',(-8.65330675040536,-73.1891490869056,
0.));
#132042=CARTESIAN_POINT('Ctrl Pts',(-8.63986257023738,-73.1659349248132,
0.));
#132043=CARTESIAN_POINT('Ctrl Pts',(-8.62645802585483,-73.1427400597037,
0.));
#132044=CARTESIAN_POINT('Ctrl Pts',(-8.61309312112001,-73.1195645948178,
0.));
#132045=CARTESIAN_POINT('Ctrl Pts',(-8.59976785984551,-73.0964086335235,
0.));
#132046=CARTESIAN_POINT('Ctrl Pts',(-8.58648224578731,-73.0732722794195,
0.));
#132047=CARTESIAN_POINT('Ctrl Pts',(-8.57323628263593,-73.0501556364479,
0.));
#132048=CARTESIAN_POINT('Ctrl Pts',(-8.56002997400083,-73.0270588090183,
0.));
#132049=CARTESIAN_POINT('Ctrl Pts',(-8.54686332340417,-73.0039819020648,
0.));
#132050=CARTESIAN_POINT('Ctrl Pts',(-8.5337363342928,-72.9809250209828,
0.));
#132051=CARTESIAN_POINT('Ctrl Pts',(-8.52064901004227,-72.9578882715912,
0.));
#132052=CARTESIAN_POINT('Ctrl Pts',(-8.50760135395983,-72.9348717600838,
0.));
#132053=CARTESIAN_POINT('Ctrl Pts',(-8.49459336928295,-72.9118755929795,
0.));
#132054=CARTESIAN_POINT('Ctrl Pts',(-8.48162505917657,-72.8888998770785,
0.));
#132055=CARTESIAN_POINT('Ctrl Pts',(-8.46869642673794,-72.8659447194933,
0.));
#132056=CARTESIAN_POINT('Ctrl Pts',(-8.45580747499793,-72.8430102276713,
0.));
#132057=CARTESIAN_POINT('Ctrl Pts',(-8.44295820691911,-72.8200965094199,
0.));
#132058=CARTESIAN_POINT('Ctrl Pts',(-8.43014862539157,-72.7972036729276,
0.));
#132059=CARTESIAN_POINT('Ctrl Pts',(-8.41737873322329,-72.7743318267865,
0.));
#132060=CARTESIAN_POINT('Ctrl Pts',(-8.40464853314468,-72.751481079992,
0.));
#132061=CARTESIAN_POINT('Ctrl Pts',(-8.3919580278139,-72.7286515419373,
0.));
#132062=CARTESIAN_POINT('Ctrl Pts',(-8.37930721981731,-72.705843322407,
0.));
#132063=CARTESIAN_POINT('Ctrl Pts',(-8.36669611166842,-72.6830565315703,
0.));
#132064=CARTESIAN_POINT('Ctrl Pts',(-8.35412470580101,-72.6602912799696,
0.));
#132065=CARTESIAN_POINT('Ctrl Pts',(-8.34159300456986,-72.6375476785215,
0.));
#132066=CARTESIAN_POINT('Ctrl Pts',(-8.3291010102567,-72.6148258385296,
0.));
#132067=CARTESIAN_POINT('Ctrl Pts',(-8.31664872507016,-72.5921258716901,
0.));
#132068=CARTESIAN_POINT('Ctrl Pts',(-8.30423615114452,-72.5694478900982,
0.));
#132069=CARTESIAN_POINT('Ctrl Pts',(-8.29186329053279,-72.5467920062521,
0.));
#132070=CARTESIAN_POINT('Ctrl Pts',(-8.27953014520376,-72.5241583330562,
0.));
#132071=CARTESIAN_POINT('Ctrl Pts',(-8.26723671704919,-72.5015469838254,
0.));
#132072=CARTESIAN_POINT('Ctrl Pts',(-8.25498300788493,-72.4789580722875,
0.));
#132073=CARTESIAN_POINT('Ctrl Pts',(-8.2427690194504,-72.4563917125842,
0.));
#132074=CARTESIAN_POINT('Ctrl Pts',(-8.23059475340356,-72.4338480192695,
0.));
#132075=CARTESIAN_POINT('Ctrl Pts',(-8.2184602113156,-72.4113271073079,
0.));
#132076=CARTESIAN_POINT('Ctrl Pts',(-8.20636539467776,-72.3888290920832,
0.));
#132077=CARTESIAN_POINT('Ctrl Pts',(-8.19431030490314,-72.3663540894026,
0.));
#132078=CARTESIAN_POINT('Ctrl Pts',(-8.18229494332623,-72.3439022155007,
0.));
#132079=CARTESIAN_POINT('Ctrl Pts',(-8.1703193111989,-72.3214735870409,
0.));
#132080=CARTESIAN_POINT('Ctrl Pts',(-8.15838340968335,-72.2990683211162,
0.));
#132081=CARTESIAN_POINT('Ctrl Pts',(-8.14648723985797,-72.2766865352555,
0.));
#132082=CARTESIAN_POINT('Ctrl Pts',(-8.13463080272028,-72.2543283474278,
0.));
#132083=CARTESIAN_POINT('Ctrl Pts',(-8.1228140991866,-72.2319938760449,
0.));
#132084=CARTESIAN_POINT('Ctrl Pts',(-8.11103713008928,-72.209683239963,
0.));
#132085=CARTESIAN_POINT('Ctrl Pts',(-8.09929989616889,-72.1873965584813,
0.));
#132086=CARTESIAN_POINT('Ctrl Pts',(-8.08760239807836,-72.1651339513477,
0.));
#132087=CARTESIAN_POINT('Ctrl Pts',(-8.07594463638719,-72.1428955387663,
0.));
#132088=CARTESIAN_POINT('Ctrl Pts',(-8.06432661158095,-72.1206814413988,
0.));
#132089=CARTESIAN_POINT('Ctrl Pts',(-8.05274832405948,-72.0984917803693,
0.));
#132090=CARTESIAN_POINT('Ctrl Pts',(-8.04120977412872,-72.0763266772615,
0.));
#132091=CARTESIAN_POINT('Ctrl Pts',(-8.02971096200307,-72.0541862541243,
0.));
#132092=CARTESIAN_POINT('Ctrl Pts',(-8.01825188781056,-72.032070633479,
0.));
#132093=CARTESIAN_POINT('Ctrl Pts',(-8.00683255159247,-72.0099799383213,
0.));
#132094=CARTESIAN_POINT('Ctrl Pts',(-7.99545295330191,-71.9879142921254,
0.));
#132095=CARTESIAN_POINT('Ctrl Pts',(-7.98411309279612,-71.965873818843,
0.));
#132096=CARTESIAN_POINT('Ctrl Pts',(-7.97281296983717,-71.9438586429081,
0.));
#132097=CARTESIAN_POINT('Ctrl Pts',(-7.96155258409763,-71.9218688892431,
0.));
#132098=CARTESIAN_POINT('Ctrl Pts',(-7.9503319351605,-71.8999046832643,
0.));
#132099=CARTESIAN_POINT('Ctrl Pts',(-7.93915102251794,-71.8779661508832,
0.));
#132100=CARTESIAN_POINT('Ctrl Pts',(-7.92800984556395,-71.8560534185071,
0.));
#132101=CARTESIAN_POINT('Ctrl Pts',(-7.91690840359367,-71.8341666130426,
0.));
#132102=CARTESIAN_POINT('Ctrl Pts',(-7.90584669580955,-71.8123058619042,
0.));
#132103=CARTESIAN_POINT('Ctrl Pts',(-7.89482472132137,-71.7904712930175,
0.));
#132104=CARTESIAN_POINT('Ctrl Pts',(-7.88384247914523,-71.7686630348238,
0.));
#132105=CARTESIAN_POINT('Ctrl Pts',(-7.87289996819653,-71.7468812162788,
0.));
#132106=CARTESIAN_POINT('Ctrl Pts',(-7.86199718728826,-71.7251259668563,
0.));
#132107=CARTESIAN_POINT('Ctrl Pts',(-7.85113413513735,-71.7033974165568,
0.));
#132108=CARTESIAN_POINT('Ctrl Pts',(-7.84031081036489,-71.6816956959117,
0.));
#132109=CARTESIAN_POINT('Ctrl Pts',(-7.82952721149507,-71.6600209359872,
0.));
#132110=CARTESIAN_POINT('Ctrl Pts',(-7.8187833369486,-71.6383732683844,
0.));
#132111=CARTESIAN_POINT('Ctrl Pts',(-7.80807918504021,-71.6167528252423,
0.));
#132112=CARTESIAN_POINT('Ctrl Pts',(-7.79741475398513,-71.5951597392471,
0.));
#132113=CARTESIAN_POINT('Ctrl Pts',(-7.78679004189934,-71.5735941436364,
0.));
#132114=CARTESIAN_POINT('Ctrl Pts',(-7.77620504679869,-71.5520561722039,
0.));
#132115=CARTESIAN_POINT('Ctrl Pts',(-7.76565976659226,-71.5305459592994,
0.));
#132116=CARTESIAN_POINT('Ctrl Pts',(-7.75515419907966,-71.5090636398318,
0.));
#132117=CARTESIAN_POINT('Ctrl Pts',(-7.74468834195746,-71.4876093492781,
0.));
#132118=CARTESIAN_POINT('Ctrl Pts',(-7.7342621928194,-71.4661832236888,
0.));
#132119=CARTESIAN_POINT('Ctrl Pts',(-7.72387574915544,-71.4447853996916,
0.));
#132120=CARTESIAN_POINT('Ctrl Pts',(-7.7135290083452,-71.4234160144925,
0.));
#132121=CARTESIAN_POINT('Ctrl Pts',(-7.70322196765538,-71.4020752058796,
0.));
#132122=CARTESIAN_POINT('Ctrl Pts',(-7.69295462424611,-71.3807631122331,
0.));
#132123=CARTESIAN_POINT('Ctrl Pts',(-7.68272697517086,-71.3594798725281,
0.));
#132124=CARTESIAN_POINT('Ctrl Pts',(-7.67253901737552,-71.3382256263414,
0.));
#132125=CARTESIAN_POINT('Ctrl Pts',(-7.66239074769163,-71.3170005138502,
0.));
#132126=CARTESIAN_POINT('Ctrl Pts',(-7.65228216283403,-71.2958046758372,
0.));
#132127=CARTESIAN_POINT('Ctrl Pts',(-7.64221325940724,-71.2746382537007,
0.));
#132128=CARTESIAN_POINT('Ctrl Pts',(-7.63218403390537,-71.2535013894602,
0.));
#132129=CARTESIAN_POINT('Ctrl Pts',(-7.62219448271109,-71.2323942257609,
0.));
#132130=CARTESIAN_POINT('Ctrl Pts',(-7.61224460208837,-71.211316905874,
0.));
#132131=CARTESIAN_POINT('Ctrl Pts',(-7.60233438818096,-71.1902695737013,
0.));
#132132=CARTESIAN_POINT('Ctrl Pts',(-7.59246383701813,-71.1692523737844,
0.));
#132133=CARTESIAN_POINT('Ctrl Pts',(-7.58263294451451,-71.1482654513119,
0.));
#132134=CARTESIAN_POINT('Ctrl Pts',(-7.57284170646886,-71.1273089521234,
0.));
#132135=CARTESIAN_POINT('Ctrl Pts',(-7.56309011855657,-71.106383022711,
0.));
#132136=CARTESIAN_POINT('Ctrl Pts',(-7.55337817632916,-71.0854878102243,
0.));
#132137=CARTESIAN_POINT('Ctrl Pts',(-7.54370587521979,-71.0646234624811,
0.));
#132138=CARTESIAN_POINT('Ctrl Pts',(-7.53407321054262,-71.043790127973,
0.));
#132139=CARTESIAN_POINT('Ctrl Pts',(-7.52448017749124,-71.0229879558699,
0.));
#132140=CARTESIAN_POINT('Ctrl Pts',(-7.5149267711309,-71.002217096021,0.));
#132141=CARTESIAN_POINT('Ctrl Pts',(-7.50541298639928,-70.9814776989612,
0.));
#132142=CARTESIAN_POINT('Ctrl Pts',(-7.4959388181113,-70.9607699159218,
0.));
#132143=CARTESIAN_POINT('Ctrl Pts',(-7.48650426095823,-70.940093898837,
0.));
#132144=CARTESIAN_POINT('Ctrl Pts',(-7.47710930950562,-70.9194498003493,
0.));
#132145=CARTESIAN_POINT('Ctrl Pts',(-7.46775395818527,-70.8988377738104,
0.));
#132146=CARTESIAN_POINT('Ctrl Pts',(-7.45843820129782,-70.87825797329,0.));
#132147=CARTESIAN_POINT('Ctrl Pts',(-7.44916203301647,-70.8577105535848,
0.));
#132148=CARTESIAN_POINT('Ctrl Pts',(-7.43992544738605,-70.8371956702241,
0.));
#132149=CARTESIAN_POINT('Ctrl Pts',(-7.43072843832014,-70.8167134794737,
0.));
#132150=CARTESIAN_POINT('Ctrl Pts',(-7.42157099959326,-70.796264138335,
0.));
#132151=CARTESIAN_POINT('Ctrl Pts',(-7.41245312484497,-70.7758478045576,
0.));
#132152=CARTESIAN_POINT('Ctrl Pts',(-7.40337480758237,-70.7554646366514,
0.));
#132153=CARTESIAN_POINT('Ctrl Pts',(-7.39433604117891,-70.735114793895,
0.));
#132154=CARTESIAN_POINT('Ctrl Pts',(-7.38533681887027,-70.7147984363423,
0.));
#132155=CARTESIAN_POINT('Ctrl Pts',(-7.3763771337476,-70.6945157248269,
0.));
#132156=CARTESIAN_POINT('Ctrl Pts',(-7.36745697876295,-70.6742668209685,
0.));
#132157=CARTESIAN_POINT('Ctrl Pts',(-7.35857634673051,-70.6540518871772,
0.));
#132158=CARTESIAN_POINT('Ctrl Pts',(-7.3497352303258,-70.6338710866562,
0.));
#132159=CARTESIAN_POINT('Ctrl Pts',(-7.34093362208017,-70.6137245834002,
0.));
#132160=CARTESIAN_POINT('Ctrl Pts',(-7.33217151437608,-70.5936125421958,
0.));
#132161=CARTESIAN_POINT('Ctrl Pts',(-7.32344889945237,-70.573535128649,
0.));
#132162=CARTESIAN_POINT('Ctrl Pts',(-7.31476576940403,-70.5534925092053,
0.));
#132163=CARTESIAN_POINT('Ctrl Pts',(-7.30612211618047,-70.5334848511675,
0.));
#132164=CARTESIAN_POINT('Ctrl Pts',(-7.29751793157801,-70.5135123227147,
0.));
#132165=CARTESIAN_POINT('Ctrl Pts',(-7.28895320723835,-70.4935750929029,
0.));
#132166=CARTESIAN_POINT('Ctrl Pts',(-7.28042793465449,-70.4736733316463,
0.));
#132167=CARTESIAN_POINT('Ctrl Pts',(-7.27194210517057,-70.4538072096986,
0.));
#132168=CARTESIAN_POINT('Ctrl Pts',(-7.2634957099805,-70.433976898636,0.));
#132169=CARTESIAN_POINT('Ctrl Pts',(-7.25508874012075,-70.4141825708207,
0.));
#132170=CARTESIAN_POINT('Ctrl Pts',(-7.24672118647116,-70.3944243994532,
0.));
#132171=CARTESIAN_POINT('Ctrl Pts',(-7.23839303975626,-70.3747025586569,
0.));
#132172=CARTESIAN_POINT('Ctrl Pts',(-7.2301042905423,-70.3550172235486,
0.));
#132173=CARTESIAN_POINT('Ctrl Pts',(-7.22185492923177,-70.3353685703097,
0.));
#132174=CARTESIAN_POINT('Ctrl Pts',(-7.21364494605424,-70.3157567762561,
0.));
#132175=CARTESIAN_POINT('Ctrl Pts',(-7.20547433107457,-70.2961820197051,
0.));
#132176=CARTESIAN_POINT('Ctrl Pts',(-7.1973430741986,-70.276644479827,0.));
#132177=CARTESIAN_POINT('Ctrl Pts',(-7.18925116517562,-70.2571443365198,
0.));
#132178=CARTESIAN_POINT('Ctrl Pts',(-7.181198593598,-70.2376817702239,0.));
#132179=CARTESIAN_POINT('Ctrl Pts',(-7.17318534889747,-70.2182569619028,
0.));
#132180=CARTESIAN_POINT('Ctrl Pts',(-7.16521142033892,-70.1988700934622,
0.));
#132181=CARTESIAN_POINT('Ctrl Pts',(-7.15727679700946,-70.1795213481196,
0.));
#132182=CARTESIAN_POINT('Ctrl Pts',(-7.14938146780801,-70.1602109107188,
0.));
#132183=CARTESIAN_POINT('Ctrl Pts',(-7.14152542142338,-70.1409389682389,
0.));
#132184=CARTESIAN_POINT('Ctrl Pts',(-7.13370864634398,-70.1217057094456,
0.));
#132185=CARTESIAN_POINT('Ctrl Pts',(-7.1259311308887,-70.1025113239463,
0.));
#132186=CARTESIAN_POINT('Ctrl Pts',(-7.11819286322823,-70.0833560013971,
0.));
#132187=CARTESIAN_POINT('Ctrl Pts',(-7.11049383140481,-70.06423993069,0.));
#132188=CARTESIAN_POINT('Ctrl Pts',(-7.10283402335091,-70.0451632990137,
0.));
#132189=CARTESIAN_POINT('Ctrl Pts',(-7.09521342684301,-70.0261262936435,
0.));
#132190=CARTESIAN_POINT('Ctrl Pts',(-7.08763202944274,-70.0071291040791,
0.));
#132191=CARTESIAN_POINT('Ctrl Pts',(-7.08008981844642,-69.988171923787,
0.));
#132192=CARTESIAN_POINT('Ctrl Pts',(-7.07258678080792,-69.9692549527256,
0.));
#132193=CARTESIAN_POINT('Ctrl Pts',(-7.06512290312802,-69.9503783975676,
0.));
#132194=CARTESIAN_POINT('Ctrl Pts',(-7.05769817180824,-69.9315424664252,
0.));
#132195=CARTESIAN_POINT('Ctrl Pts',(-7.05031257318107,-69.9127473642087,
0.));
#132196=CARTESIAN_POINT('Ctrl Pts',(-7.04296609362186,-69.8939932885864,
0.));
#132197=CARTESIAN_POINT('Ctrl Pts',(-7.03565871972265,-69.8752804235296,
0.));
#132198=CARTESIAN_POINT('Ctrl Pts',(-7.02839043811862,-69.8566089455448,
0.));
#132199=CARTESIAN_POINT('Ctrl Pts',(-7.02116123514487,-69.8379790360574,
0.));
#132200=CARTESIAN_POINT('Ctrl Pts',(-7.01397109655455,-69.8193908913722,
0.));
#132201=CARTESIAN_POINT('Ctrl Pts',(-7.00682000718104,-69.8008447346782,
0.));
#132202=CARTESIAN_POINT('Ctrl Pts',(-6.99970795069399,-69.7823408242446,
0.));
#132203=CARTESIAN_POINT('Ctrl Pts',(-6.99263491027859,-69.7638794280263,
0.));
#132204=CARTESIAN_POINT('Ctrl Pts',(-6.98560086924172,-69.7454607995524,
0.));
#132205=CARTESIAN_POINT('Ctrl Pts',(-6.97860581164568,-69.7270851557443,
0.));
#132206=CARTESIAN_POINT('Ctrl Pts',(-6.97164972291581,-69.7087526480249,
0.));
#132207=CARTESIAN_POINT('Ctrl Pts',(-6.96473259049729,-69.6904633605834,
0.));
#132208=CARTESIAN_POINT('Ctrl Pts',(-6.95923004173795,-69.6758665380764,
0.));
#132209=CARTESIAN_POINT('Ctrl Pts',(-6.9551206531773,-69.6649383920075,
0.));
#132210=CARTESIAN_POINT('Ctrl Pts',(-6.95238884849075,-69.6576616146559,
0.));
#132211=CARTESIAN_POINT('Ctrl Pts',(-6.95102489306927,-69.6540253893193,
0.));
#132212=CARTESIAN_POINT('Ctrl Pts',(-15.5142209845168,-72.8667204369977,
0.));
#132213=CARTESIAN_POINT('Ctrl Pts',(-15.5142209845168,-72.8667204369977,
12.));
#132214=CARTESIAN_POINT('Ctrl Pts',(-15.5108715869174,-72.8622377860957,
0.));
#132215=CARTESIAN_POINT('Ctrl Pts',(-15.5108715869174,-72.8622377860957,
12.));
#132216=CARTESIAN_POINT('Ctrl Pts',(-15.5041768664089,-72.8532737732124,
0.));
#132217=CARTESIAN_POINT('Ctrl Pts',(-15.5041768664089,-72.8532737732124,
12.));
#132218=CARTESIAN_POINT('Ctrl Pts',(-15.494147009717,-72.8398316206501,
0.));
#132219=CARTESIAN_POINT('Ctrl Pts',(-15.494147009717,-72.8398316206501,
12.));
#132220=CARTESIAN_POINT('Ctrl Pts',(-15.4807983165983,-72.8219164844002,
0.));
#132221=CARTESIAN_POINT('Ctrl Pts',(-15.4807983165983,-72.8219164844002,
12.));
#132222=CARTESIAN_POINT('Ctrl Pts',(-15.4641532053435,-72.7995354604414,
0.));
#132223=CARTESIAN_POINT('Ctrl Pts',(-15.4641532053435,-72.7995354604414,
12.));
#132224=CARTESIAN_POINT('Ctrl Pts',(-15.4475488590336,-72.7771673494582,
0.));
#132225=CARTESIAN_POINT('Ctrl Pts',(-15.4475488590336,-72.7771673494582,
12.));
#132226=CARTESIAN_POINT('Ctrl Pts',(-15.4309852897866,-72.7548121825431,
0.));
#132227=CARTESIAN_POINT('Ctrl Pts',(-15.4309852897866,-72.7548121825431,
12.));
#132228=CARTESIAN_POINT('Ctrl Pts',(-15.4144625111911,-72.7324700089576,
0.));
#132229=CARTESIAN_POINT('Ctrl Pts',(-15.4144625111911,-72.7324700089576,
12.));
#132230=CARTESIAN_POINT('Ctrl Pts',(-15.397980537311,-72.710140901746,0.));
#132231=CARTESIAN_POINT('Ctrl Pts',(-15.397980537311,-72.710140901746,12.));
#132232=CARTESIAN_POINT('Ctrl Pts',(-15.3815393822669,-72.6878249557452,
0.));
#132233=CARTESIAN_POINT('Ctrl Pts',(-15.3815393822669,-72.6878249557452,
12.));
#132234=CARTESIAN_POINT('Ctrl Pts',(-15.3651390602616,-72.6655222797603,
0.));
#132235=CARTESIAN_POINT('Ctrl Pts',(-15.3651390602616,-72.6655222797603,
12.));
#132236=CARTESIAN_POINT('Ctrl Pts',(-15.3487795854723,-72.6432329903466,
0.));
#132237=CARTESIAN_POINT('Ctrl Pts',(-15.3487795854723,-72.6432329903466,
12.));
#132238=CARTESIAN_POINT('Ctrl Pts',(-15.3324609719961,-72.6209572051064,
0.));
#132239=CARTESIAN_POINT('Ctrl Pts',(-15.3324609719961,-72.6209572051064,
12.));
#132240=CARTESIAN_POINT('Ctrl Pts',(-15.3161832337617,-72.5986950357771,
0.));
#132241=CARTESIAN_POINT('Ctrl Pts',(-15.3161832337617,-72.5986950357771,
12.));
#132242=CARTESIAN_POINT('Ctrl Pts',(-15.2999463844691,-72.5764465826345,
0.));
#132243=CARTESIAN_POINT('Ctrl Pts',(-15.2999463844691,-72.5764465826345,
12.));
#132244=CARTESIAN_POINT('Ctrl Pts',(-15.2837504376562,-72.5542119383748,
0.));
#132245=CARTESIAN_POINT('Ctrl Pts',(-15.2837504376562,-72.5542119383748,
12.));
#132246=CARTESIAN_POINT('Ctrl Pts',(-15.2675954067495,-72.5319911908978,
0.));
#132247=CARTESIAN_POINT('Ctrl Pts',(-15.2675954067495,-72.5319911908978,
12.));
#132248=CARTESIAN_POINT('Ctrl Pts',(-15.2514813051174,-72.5097844266083,
0.));
#132249=CARTESIAN_POINT('Ctrl Pts',(-15.2514813051174,-72.5097844266083,
12.));
#132250=CARTESIAN_POINT('Ctrl Pts',(-15.2354081461151,-72.4875917332729,
0.));
#132251=CARTESIAN_POINT('Ctrl Pts',(-15.2354081461151,-72.4875917332729,
12.));
#132252=CARTESIAN_POINT('Ctrl Pts',(-15.2193759431359,-72.4654132036373,
0.));
#132253=CARTESIAN_POINT('Ctrl Pts',(-15.2193759431359,-72.4654132036373,
12.));
#132254=CARTESIAN_POINT('Ctrl Pts',(-15.2033847096077,-72.4432489350415,
0.));
#132255=CARTESIAN_POINT('Ctrl Pts',(-15.2033847096077,-72.4432489350415,
12.));
#132256=CARTESIAN_POINT('Ctrl Pts',(-15.1874344589715,-72.4210990277819,
0.));
#132257=CARTESIAN_POINT('Ctrl Pts',(-15.1874344589715,-72.4210990277819,
12.));
#132258=CARTESIAN_POINT('Ctrl Pts',(-15.1715252046602,-72.3989635838476,
0.));
#132259=CARTESIAN_POINT('Ctrl Pts',(-15.1715252046602,-72.3989635838476,
12.));
#132260=CARTESIAN_POINT('Ctrl Pts',(-15.1556569600747,-72.37684270559,0.));
#132261=CARTESIAN_POINT('Ctrl Pts',(-15.1556569600747,-72.37684270559,12.));
#132262=CARTESIAN_POINT('Ctrl Pts',(-15.1398297385513,-72.3547364941996,
0.));
#132263=CARTESIAN_POINT('Ctrl Pts',(-15.1398297385513,-72.3547364941996,
12.));
#132264=CARTESIAN_POINT('Ctrl Pts',(-15.1240435533478,-72.332645049021,
0.));
#132265=CARTESIAN_POINT('Ctrl Pts',(-15.1240435533478,-72.332645049021,
12.));
#132266=CARTESIAN_POINT('Ctrl Pts',(-15.1082984176655,-72.3105684683971,
0.));
#132267=CARTESIAN_POINT('Ctrl Pts',(-15.1082984176655,-72.3105684683971,
12.));
#132268=CARTESIAN_POINT('Ctrl Pts',(-15.0925943446593,-72.2885068501641,
0.));
#132269=CARTESIAN_POINT('Ctrl Pts',(-15.0925943446593,-72.2885068501641,
12.));
#132270=CARTESIAN_POINT('Ctrl Pts',(-15.0769313474476,-72.266460292285,
0.));
#132271=CARTESIAN_POINT('Ctrl Pts',(-15.0769313474476,-72.266460292285,
12.));
#132272=CARTESIAN_POINT('Ctrl Pts',(-15.0613094391186,-72.244428893425,
0.));
#132273=CARTESIAN_POINT('Ctrl Pts',(-15.0613094391186,-72.244428893425,
12.));
#132274=CARTESIAN_POINT('Ctrl Pts',(-15.0457286327328,-72.2224127535401,
0.));
#132275=CARTESIAN_POINT('Ctrl Pts',(-15.0457286327328,-72.2224127535401,
12.));
#132276=CARTESIAN_POINT('Ctrl Pts',(-15.0301889413255,-72.2004119736104,
0.));
#132277=CARTESIAN_POINT('Ctrl Pts',(-15.0301889413255,-72.2004119736104,
12.));
#132278=CARTESIAN_POINT('Ctrl Pts',(-15.0146903779061,-72.1784266553948,
0.));
#132279=CARTESIAN_POINT('Ctrl Pts',(-15.0146903779061,-72.1784266553948,
12.));
#132280=CARTESIAN_POINT('Ctrl Pts',(-14.9992329554537,-72.1564569011668,
0.));
#132281=CARTESIAN_POINT('Ctrl Pts',(-14.9992329554537,-72.1564569011668,
12.));
#132282=CARTESIAN_POINT('Ctrl Pts',(-14.9838166869107,-72.1345028134779,
0.));
#132283=CARTESIAN_POINT('Ctrl Pts',(-14.9838166869107,-72.1345028134779,
12.));
#132284=CARTESIAN_POINT('Ctrl Pts',(-14.9684415851699,-72.1125644948547,
0.));
#132285=CARTESIAN_POINT('Ctrl Pts',(-14.9684415851699,-72.1125644948547,
12.));
#132286=CARTESIAN_POINT('Ctrl Pts',(-14.953107663077,-72.0906420478085,
0.));
#132287=CARTESIAN_POINT('Ctrl Pts',(-14.953107663077,-72.0906420478085,
12.));
#132288=CARTESIAN_POINT('Ctrl Pts',(-14.937814933439,-72.0687355749815,
0.));
#132289=CARTESIAN_POINT('Ctrl Pts',(-14.937814933439,-72.0687355749815,
12.));
#132290=CARTESIAN_POINT('Ctrl Pts',(-14.9225634090269,-72.046845179251,
0.));
#132291=CARTESIAN_POINT('Ctrl Pts',(-14.9225634090269,-72.046845179251,
12.));
#132292=CARTESIAN_POINT('Ctrl Pts',(-14.9073531025763,-72.0249709638419,
0.));
#132293=CARTESIAN_POINT('Ctrl Pts',(-14.9073531025763,-72.0249709638419,
12.));
#132294=CARTESIAN_POINT('Ctrl Pts',(-14.8921840267829,-72.0031130324519,
0.));
#132295=CARTESIAN_POINT('Ctrl Pts',(-14.8921840267829,-72.0031130324519,
12.));
#132296=CARTESIAN_POINT('Ctrl Pts',(-14.8770561943011,-71.9812714893087,
0.));
#132297=CARTESIAN_POINT('Ctrl Pts',(-14.8770561943011,-71.9812714893087,
12.));
#132298=CARTESIAN_POINT('Ctrl Pts',(-14.8619696177503,-71.9594464391063,
0.));
#132299=CARTESIAN_POINT('Ctrl Pts',(-14.8619696177503,-71.9594464391063,
12.));
#132300=CARTESIAN_POINT('Ctrl Pts',(-14.846924309716,-71.9376379869668,
0.));
#132301=CARTESIAN_POINT('Ctrl Pts',(-14.846924309716,-71.9376379869668,
12.));
#132302=CARTESIAN_POINT('Ctrl Pts',(-14.8319202827482,-71.9158462383915,
0.));
#132303=CARTESIAN_POINT('Ctrl Pts',(-14.8319202827482,-71.9158462383915,
12.));
#132304=CARTESIAN_POINT('Ctrl Pts',(-14.8169575493559,-71.8940712992119,
0.));
#132305=CARTESIAN_POINT('Ctrl Pts',(-14.8169575493559,-71.8940712992119,
12.));
#132306=CARTESIAN_POINT('Ctrl Pts',(-14.8020361220002,-71.872313275546,
0.));
#132307=CARTESIAN_POINT('Ctrl Pts',(-14.8020361220002,-71.872313275546,
12.));
#132308=CARTESIAN_POINT('Ctrl Pts',(-14.7871560131021,-71.8505722738286,
0.));
#132309=CARTESIAN_POINT('Ctrl Pts',(-14.7871560131021,-71.8505722738286,
12.));
#132310=CARTESIAN_POINT('Ctrl Pts',(-14.7723172350454,-71.8288484008343,
0.));
#132311=CARTESIAN_POINT('Ctrl Pts',(-14.7723172350454,-71.8288484008343,
12.));
#132312=CARTESIAN_POINT('Ctrl Pts',(-14.7575198001776,-71.8071417637019,
0.));
#132313=CARTESIAN_POINT('Ctrl Pts',(-14.7575198001776,-71.8071417637019,
12.));
#132314=CARTESIAN_POINT('Ctrl Pts',(-14.742763720807,-71.7854524699563,
0.));
#132315=CARTESIAN_POINT('Ctrl Pts',(-14.742763720807,-71.7854524699563,
12.));
#132316=CARTESIAN_POINT('Ctrl Pts',(-14.7280490091954,-71.7637806275316,
0.));
#132317=CARTESIAN_POINT('Ctrl Pts',(-14.7280490091954,-71.7637806275316,
12.));
#132318=CARTESIAN_POINT('Ctrl Pts',(-14.7133756775622,-71.7421263447707,
0.));
#132319=CARTESIAN_POINT('Ctrl Pts',(-14.7133756775622,-71.7421263447707,
12.));
#132320=CARTESIAN_POINT('Ctrl Pts',(-14.6987437380898,-71.7204897304186,
0.));
#132321=CARTESIAN_POINT('Ctrl Pts',(-14.6987437380898,-71.7204897304186,
12.));
#132322=CARTESIAN_POINT('Ctrl Pts',(-14.6841532029231,-71.698870893617,
0.));
#132323=CARTESIAN_POINT('Ctrl Pts',(-14.6841532029231,-71.698870893617,
12.));
#132324=CARTESIAN_POINT('Ctrl Pts',(-14.6696040841679,-71.6772699438966,
0.));
#132325=CARTESIAN_POINT('Ctrl Pts',(-14.6696040841679,-71.6772699438966,
12.));
#132326=CARTESIAN_POINT('Ctrl Pts',(-14.6550963938832,-71.6556869911669,
0.));
#132327=CARTESIAN_POINT('Ctrl Pts',(-14.6550963938832,-71.6556869911669,
12.));
#132328=CARTESIAN_POINT('Ctrl Pts',(-14.6406301440817,-71.6341221457175,
0.));
#132329=CARTESIAN_POINT('Ctrl Pts',(-14.6406301440817,-71.6341221457175,
12.));
#132330=CARTESIAN_POINT('Ctrl Pts',(-14.6262053467372,-71.6125755182295,
0.));
#132331=CARTESIAN_POINT('Ctrl Pts',(-14.6262053467372,-71.6125755182295,
12.));
#132332=CARTESIAN_POINT('Ctrl Pts',(-14.611822013785,-71.5910472197815,
0.));
#132333=CARTESIAN_POINT('Ctrl Pts',(-14.611822013785,-71.5910472197815,
12.));
#132334=CARTESIAN_POINT('Ctrl Pts',(-14.5974801571209,-71.569537361856,
0.));
#132335=CARTESIAN_POINT('Ctrl Pts',(-14.5974801571209,-71.569537361856,
12.));
#132336=CARTESIAN_POINT('Ctrl Pts',(-14.5831797885951,-71.5480460563445,
0.));
#132337=CARTESIAN_POINT('Ctrl Pts',(-14.5831797885951,-71.5480460563445,
12.));
#132338=CARTESIAN_POINT('Ctrl Pts',(-14.568920920009,-71.52657341555,0.));
#132339=CARTESIAN_POINT('Ctrl Pts',(-14.568920920009,-71.52657341555,12.));
#132340=CARTESIAN_POINT('Ctrl Pts',(-14.5547035631233,-71.5051195521914,
0.));
#132341=CARTESIAN_POINT('Ctrl Pts',(-14.5547035631233,-71.5051195521914,
12.));
#132342=CARTESIAN_POINT('Ctrl Pts',(-14.540527729659,-71.4836845794052,
0.));
#132343=CARTESIAN_POINT('Ctrl Pts',(-14.540527729659,-71.4836845794052,
12.));
#132344=CARTESIAN_POINT('Ctrl Pts',(-14.5263934312969,-71.4622686107475,
0.));
#132345=CARTESIAN_POINT('Ctrl Pts',(-14.5263934312969,-71.4622686107475,
12.));
#132346=CARTESIAN_POINT('Ctrl Pts',(-14.5123006796728,-71.4408717601917,
0.));
#132347=CARTESIAN_POINT('Ctrl Pts',(-14.5123006796728,-71.4408717601917,
12.));
#132348=CARTESIAN_POINT('Ctrl Pts',(-14.4982494863716,-71.4194941421279,
0.));
#132349=CARTESIAN_POINT('Ctrl Pts',(-14.4982494863716,-71.4194941421279,
12.));
#132350=CARTESIAN_POINT('Ctrl Pts',(-14.4842398629353,-71.398135871371,
0.));
#132351=CARTESIAN_POINT('Ctrl Pts',(-14.4842398629353,-71.398135871371,
12.));
#132352=CARTESIAN_POINT('Ctrl Pts',(-14.470271820865,-71.3767970631642,
0.));
#132353=CARTESIAN_POINT('Ctrl Pts',(-14.470271820865,-71.3767970631642,
12.));
#132354=CARTESIAN_POINT('Ctrl Pts',(-14.4563453716204,-71.3554778331835,
0.));
#132355=CARTESIAN_POINT('Ctrl Pts',(-14.4563453716204,-71.3554778331835,
12.));
#132356=CARTESIAN_POINT('Ctrl Pts',(-14.4424605266166,-71.3341782975393,
0.));
#132357=CARTESIAN_POINT('Ctrl Pts',(-14.4424605266166,-71.3341782975393,
12.));
#132358=CARTESIAN_POINT('Ctrl Pts',(-14.4286172972168,-71.3128985727777,
0.));
#132359=CARTESIAN_POINT('Ctrl Pts',(-14.4286172972168,-71.3128985727777,
12.));
#132360=CARTESIAN_POINT('Ctrl Pts',(-14.4148156947384,-71.2916387758864,
0.));
#132361=CARTESIAN_POINT('Ctrl Pts',(-14.4148156947384,-71.2916387758864,
12.));
#132362=CARTESIAN_POINT('Ctrl Pts',(-14.401055730457,-71.2703990242986,
0.));
#132363=CARTESIAN_POINT('Ctrl Pts',(-14.401055730457,-71.2703990242986,
12.));
#132364=CARTESIAN_POINT('Ctrl Pts',(-14.3873374156056,-71.2491794358956,
0.));
#132365=CARTESIAN_POINT('Ctrl Pts',(-14.3873374156056,-71.2491794358956,
12.));
#132366=CARTESIAN_POINT('Ctrl Pts',(-14.3736607613723,-71.2279801290088,
0.));
#132367=CARTESIAN_POINT('Ctrl Pts',(-14.3736607613723,-71.2279801290088,
12.));
#132368=CARTESIAN_POINT('Ctrl Pts',(-14.3600257788927,-71.2068012224187,
0.));
#132369=CARTESIAN_POINT('Ctrl Pts',(-14.3600257788927,-71.2068012224187,
12.));
#132370=CARTESIAN_POINT('Ctrl Pts',(-14.3464324792537,-71.185642835361,
0.));
#132371=CARTESIAN_POINT('Ctrl Pts',(-14.3464324792537,-71.185642835361,
12.));
#132372=CARTESIAN_POINT('Ctrl Pts',(-14.3328808734993,-71.1645050875323,
0.));
#132373=CARTESIAN_POINT('Ctrl Pts',(-14.3328808734993,-71.1645050875323,
12.));
#132374=CARTESIAN_POINT('Ctrl Pts',(-14.3193709726295,-71.1433880990932,
0.));
#132375=CARTESIAN_POINT('Ctrl Pts',(-14.3193709726295,-71.1433880990932,
12.));
#132376=CARTESIAN_POINT('Ctrl Pts',(-14.3059027875992,-71.1222919906718,
0.));
#132377=CARTESIAN_POINT('Ctrl Pts',(-14.3059027875992,-71.1222919906718,
12.));
#132378=CARTESIAN_POINT('Ctrl Pts',(-14.2924763293101,-71.1012168833626,
0.));
#132379=CARTESIAN_POINT('Ctrl Pts',(-14.2924763293101,-71.1012168833626,
12.));
#132380=CARTESIAN_POINT('Ctrl Pts',(-14.2790916086129,-71.0801628987314,
0.));
#132381=CARTESIAN_POINT('Ctrl Pts',(-14.2790916086129,-71.0801628987314,
12.));
#132382=CARTESIAN_POINT('Ctrl Pts',(-14.2657486363136,-71.059130158822,
0.));
#132383=CARTESIAN_POINT('Ctrl Pts',(-14.2657486363136,-71.059130158822,
12.));
#132384=CARTESIAN_POINT('Ctrl Pts',(-14.2524474231732,-71.0381187861585,
0.));
#132385=CARTESIAN_POINT('Ctrl Pts',(-14.2524474231732,-71.0381187861585,
12.));
#132386=CARTESIAN_POINT('Ctrl Pts',(-14.2391879799063,-71.0171289037493,
0.));
#132387=CARTESIAN_POINT('Ctrl Pts',(-14.2391879799063,-71.0171289037493,
12.));
#132388=CARTESIAN_POINT('Ctrl Pts',(-14.2259703171739,-70.996160635087,
0.));
#132389=CARTESIAN_POINT('Ctrl Pts',(-14.2259703171739,-70.996160635087,
12.));
#132390=CARTESIAN_POINT('Ctrl Pts',(-14.2127944455841,-70.9752141041527,
0.));
#132391=CARTESIAN_POINT('Ctrl Pts',(-14.2127944455841,-70.9752141041527,
12.));
#132392=CARTESIAN_POINT('Ctrl Pts',(-14.1996603756984,-70.9542894354221,
0.));
#132393=CARTESIAN_POINT('Ctrl Pts',(-14.1996603756984,-70.9542894354221,
12.));
#132394=CARTESIAN_POINT('Ctrl Pts',(-14.1865681180321,-70.9333867538705,
0.));
#132395=CARTESIAN_POINT('Ctrl Pts',(-14.1865681180321,-70.9333867538705,
12.));
#132396=CARTESIAN_POINT('Ctrl Pts',(-14.1735176830533,-70.9125061849744,
0.));
#132397=CARTESIAN_POINT('Ctrl Pts',(-14.1735176830533,-70.9125061849744,
12.));
#132398=CARTESIAN_POINT('Ctrl Pts',(-14.1605090811753,-70.8916478547131,
0.));
#132399=CARTESIAN_POINT('Ctrl Pts',(-14.1605090811753,-70.8916478547131,
12.));
#132400=CARTESIAN_POINT('Ctrl Pts',(-14.1475423227567,-70.8708118895718,
0.));
#132401=CARTESIAN_POINT('Ctrl Pts',(-14.1475423227567,-70.8708118895718,
12.));
#132402=CARTESIAN_POINT('Ctrl Pts',(-14.1346174181079,-70.8499984165493,
0.));
#132403=CARTESIAN_POINT('Ctrl Pts',(-14.1346174181079,-70.8499984165493,
12.));
#132404=CARTESIAN_POINT('Ctrl Pts',(-14.1217343774914,-70.8292075631624,
0.));
#132405=CARTESIAN_POINT('Ctrl Pts',(-14.1217343774914,-70.8292075631624,
12.));
#132406=CARTESIAN_POINT('Ctrl Pts',(-14.1088932111214,-70.8084394574491,
0.));
#132407=CARTESIAN_POINT('Ctrl Pts',(-14.1088932111214,-70.8084394574491,
12.));
#132408=CARTESIAN_POINT('Ctrl Pts',(-14.0960939291568,-70.787694227969,
0.));
#132409=CARTESIAN_POINT('Ctrl Pts',(-14.0960939291568,-70.787694227969,
12.));
#132410=CARTESIAN_POINT('Ctrl Pts',(-14.0833365416995,-70.7669720038067,
0.));
#132411=CARTESIAN_POINT('Ctrl Pts',(-14.0833365416995,-70.7669720038067,
12.));
#132412=CARTESIAN_POINT('Ctrl Pts',(-14.0706210588015,-70.7462729145799,
0.));
#132413=CARTESIAN_POINT('Ctrl Pts',(-14.0706210588015,-70.7462729145799,
12.));
#132414=CARTESIAN_POINT('Ctrl Pts',(-14.0579474904657,-70.7255970904433,
0.));
#132415=CARTESIAN_POINT('Ctrl Pts',(-14.0579474904657,-70.7255970904433,
12.));
#132416=CARTESIAN_POINT('Ctrl Pts',(-14.0453158466451,-70.7049446620931,
0.));
#132417=CARTESIAN_POINT('Ctrl Pts',(-14.0453158466451,-70.7049446620931,
12.));
#132418=CARTESIAN_POINT('Ctrl Pts',(-14.0327261372363,-70.6843157607672,
0.));
#132419=CARTESIAN_POINT('Ctrl Pts',(-14.0327261372363,-70.6843157607672,
12.));
#132420=CARTESIAN_POINT('Ctrl Pts',(-14.020178372077,-70.6637105182487,
0.));
#132421=CARTESIAN_POINT('Ctrl Pts',(-14.020178372077,-70.6637105182487,
12.));
#132422=CARTESIAN_POINT('Ctrl Pts',(-14.0076725609536,-70.6431290668744,
0.));
#132423=CARTESIAN_POINT('Ctrl Pts',(-14.0076725609536,-70.6431290668744,
12.));
#132424=CARTESIAN_POINT('Ctrl Pts',(-13.9952087136018,-70.6225715395392,
0.));
#132425=CARTESIAN_POINT('Ctrl Pts',(-13.9952087136018,-70.6225715395392,
12.));
#132426=CARTESIAN_POINT('Ctrl Pts',(-13.9827868397057,-70.6020380697004,
0.));
#132427=CARTESIAN_POINT('Ctrl Pts',(-13.9827868397057,-70.6020380697004,
12.));
#132428=CARTESIAN_POINT('Ctrl Pts',(-13.9704069488918,-70.5815287913791,
0.));
#132429=CARTESIAN_POINT('Ctrl Pts',(-13.9704069488918,-70.5815287913791,
12.));
#132430=CARTESIAN_POINT('Ctrl Pts',(-13.9580690507262,-70.5610438391622,
0.));
#132431=CARTESIAN_POINT('Ctrl Pts',(-13.9580690507262,-70.5610438391622,
12.));
#132432=CARTESIAN_POINT('Ctrl Pts',(-13.9457731547217,-70.5405833482123,
0.));
#132433=CARTESIAN_POINT('Ctrl Pts',(-13.9457731547217,-70.5405833482123,
12.));
#132434=CARTESIAN_POINT('Ctrl Pts',(-13.9335192703389,-70.5201474542717,
0.));
#132435=CARTESIAN_POINT('Ctrl Pts',(-13.9335192703389,-70.5201474542717,
12.));
#132436=CARTESIAN_POINT('Ctrl Pts',(-13.9213074069852,-70.4997362936671,
0.));
#132437=CARTESIAN_POINT('Ctrl Pts',(-13.9213074069852,-70.4997362936671,
12.));
#132438=CARTESIAN_POINT('Ctrl Pts',(-13.9091375740084,-70.4793500033106,
0.));
#132439=CARTESIAN_POINT('Ctrl Pts',(-13.9091375740084,-70.4793500033106,
12.));
#132440=CARTESIAN_POINT('Ctrl Pts',(-13.8970097806947,-70.4589887207043,
0.));
#132441=CARTESIAN_POINT('Ctrl Pts',(-13.8970097806947,-70.4589887207043,
12.));
#132442=CARTESIAN_POINT('Ctrl Pts',(-13.8849240362757,-70.4386525839492,
0.));
#132443=CARTESIAN_POINT('Ctrl Pts',(-13.8849240362757,-70.4386525839492,
12.));
#132444=CARTESIAN_POINT('Ctrl Pts',(-13.8728803499284,-70.4183417317486,
0.));
#132445=CARTESIAN_POINT('Ctrl Pts',(-13.8728803499284,-70.4183417317486,
12.));
#132446=CARTESIAN_POINT('Ctrl Pts',(-13.8608787307753,-70.3980563034142,
0.));
#132447=CARTESIAN_POINT('Ctrl Pts',(-13.8608787307753,-70.3980563034142,
12.));
#132448=CARTESIAN_POINT('Ctrl Pts',(-13.8489191878774,-70.377796438866,
0.));
#132449=CARTESIAN_POINT('Ctrl Pts',(-13.8489191878774,-70.377796438866,
12.));
#132450=CARTESIAN_POINT('Ctrl Pts',(-13.8370017302318,-70.3575622786373,
0.));
#132451=CARTESIAN_POINT('Ctrl Pts',(-13.8370017302318,-70.3575622786373,
12.));
#132452=CARTESIAN_POINT('Ctrl Pts',(-13.8251263667799,-70.3373539638841,
0.));
#132453=CARTESIAN_POINT('Ctrl Pts',(-13.8251263667799,-70.3373539638841,
12.));
#132454=CARTESIAN_POINT('Ctrl Pts',(-13.8132931064067,-70.3171716363912,
0.));
#132455=CARTESIAN_POINT('Ctrl Pts',(-13.8132931064067,-70.3171716363912,
12.));
#132456=CARTESIAN_POINT('Ctrl Pts',(-13.8015019579411,-70.2970154385763,
0.));
#132457=CARTESIAN_POINT('Ctrl Pts',(-13.8015019579411,-70.2970154385763,
12.));
#132458=CARTESIAN_POINT('Ctrl Pts',(-13.7897529301482,-70.2768855134909,
0.));
#132459=CARTESIAN_POINT('Ctrl Pts',(-13.7897529301482,-70.2768855134909,
12.));
#132460=CARTESIAN_POINT('Ctrl Pts',(-13.7780460317284,-70.2567820048253,
0.));
#132461=CARTESIAN_POINT('Ctrl Pts',(-13.7780460317284,-70.2567820048253,
12.));
#132462=CARTESIAN_POINT('Ctrl Pts',(-13.7663812713235,-70.2367050569174,
0.));
#132463=CARTESIAN_POINT('Ctrl Pts',(-13.7663812713235,-70.2367050569174,
12.));
#132464=CARTESIAN_POINT('Ctrl Pts',(-13.7547586575178,-70.216654814759,
0.));
#132465=CARTESIAN_POINT('Ctrl Pts',(-13.7547586575178,-70.216654814759,
12.));
#132466=CARTESIAN_POINT('Ctrl Pts',(-13.7431781988368,-70.1966314240012,
0.));
#132467=CARTESIAN_POINT('Ctrl Pts',(-13.7431781988368,-70.1966314240012,
12.));
#132468=CARTESIAN_POINT('Ctrl Pts',(-13.73163990374,-70.1766350309554,0.));
#132469=CARTESIAN_POINT('Ctrl Pts',(-13.73163990374,-70.1766350309554,12.));
#132470=CARTESIAN_POINT('Ctrl Pts',(-13.7201437806207,-70.1566657825989,
0.));
#132471=CARTESIAN_POINT('Ctrl Pts',(-13.7201437806207,-70.1566657825989,
12.));
#132472=CARTESIAN_POINT('Ctrl Pts',(-13.7086898378127,-70.1367238265853,
0.));
#132473=CARTESIAN_POINT('Ctrl Pts',(-13.7086898378127,-70.1367238265853,
12.));
#132474=CARTESIAN_POINT('Ctrl Pts',(-13.6972780835898,-70.1168093112493,
0.));
#132475=CARTESIAN_POINT('Ctrl Pts',(-13.6972780835898,-70.1168093112493,
12.));
#132476=CARTESIAN_POINT('Ctrl Pts',(-13.685908526165,-70.0969223856123,
0.));
#132477=CARTESIAN_POINT('Ctrl Pts',(-13.685908526165,-70.0969223856123,
12.));
#132478=CARTESIAN_POINT('Ctrl Pts',(-13.6745811736825,-70.0770631993831,
0.));
#132479=CARTESIAN_POINT('Ctrl Pts',(-13.6745811736825,-70.0770631993831,
12.));
#132480=CARTESIAN_POINT('Ctrl Pts',(-13.6632960342192,-70.057231902965,
0.));
#132481=CARTESIAN_POINT('Ctrl Pts',(-13.6632960342192,-70.057231902965,
12.));
#132482=CARTESIAN_POINT('Ctrl Pts',(-13.6520531157904,-70.037428647466,
0.));
#132483=CARTESIAN_POINT('Ctrl Pts',(-13.6520531157904,-70.037428647466,
12.));
#132484=CARTESIAN_POINT('Ctrl Pts',(-13.6408524263496,-70.0176535847047,
0.));
#132485=CARTESIAN_POINT('Ctrl Pts',(-13.6408524263496,-70.0176535847047,
12.));
#132486=CARTESIAN_POINT('Ctrl Pts',(-13.6296939737866,-69.9979068672163,
0.));
#132487=CARTESIAN_POINT('Ctrl Pts',(-13.6296939737866,-69.9979068672163,
12.));
#132488=CARTESIAN_POINT('Ctrl Pts',(-13.61857776592,-69.9781886482543,0.));
#132489=CARTESIAN_POINT('Ctrl Pts',(-13.61857776592,-69.9781886482543,12.));
#132490=CARTESIAN_POINT('Ctrl Pts',(-13.6075038105,-69.9584990817989,0.));
#132491=CARTESIAN_POINT('Ctrl Pts',(-13.6075038105,-69.9584990817989,12.));
#132492=CARTESIAN_POINT('Ctrl Pts',(-13.5964721152136,-69.9388383225655,
0.));
#132493=CARTESIAN_POINT('Ctrl Pts',(-13.5964721152136,-69.9388383225655,
12.));
#132494=CARTESIAN_POINT('Ctrl Pts',(-13.5854826876834,-69.9192065260107,
0.));
#132495=CARTESIAN_POINT('Ctrl Pts',(-13.5854826876834,-69.9192065260107,
12.));
#132496=CARTESIAN_POINT('Ctrl Pts',(-13.5745355354657,-69.899603848336,
0.));
#132497=CARTESIAN_POINT('Ctrl Pts',(-13.5745355354657,-69.899603848336,
12.));
#132498=CARTESIAN_POINT('Ctrl Pts',(-13.5636306660422,-69.880030446488,
0.));
#132499=CARTESIAN_POINT('Ctrl Pts',(-13.5636306660422,-69.880030446488,
12.));
#132500=CARTESIAN_POINT('Ctrl Pts',(-13.5527680868256,-69.8604864781705,
0.));
#132501=CARTESIAN_POINT('Ctrl Pts',(-13.5527680868256,-69.8604864781705,
12.));
#132502=CARTESIAN_POINT('Ctrl Pts',(-13.5419478051626,-69.840972101856,
0.));
#132503=CARTESIAN_POINT('Ctrl Pts',(-13.5419478051626,-69.840972101856,
12.));
#132504=CARTESIAN_POINT('Ctrl Pts',(-13.5311698283339,-69.8214874767944,
0.));
#132505=CARTESIAN_POINT('Ctrl Pts',(-13.5311698283339,-69.8214874767944,
12.));
#132506=CARTESIAN_POINT('Ctrl Pts',(-13.5204341635507,-69.8020327630204,
0.));
#132507=CARTESIAN_POINT('Ctrl Pts',(-13.5204341635507,-69.8020327630204,
12.));
#132508=CARTESIAN_POINT('Ctrl Pts',(-13.5097408179478,-69.7826081213575,
0.));
#132509=CARTESIAN_POINT('Ctrl Pts',(-13.5097408179478,-69.7826081213575,
12.));
#132510=CARTESIAN_POINT('Ctrl Pts',(-13.4990897985903,-69.7632137134247,
0.));
#132511=CARTESIAN_POINT('Ctrl Pts',(-13.4990897985903,-69.7632137134247,
12.));
#132512=CARTESIAN_POINT('Ctrl Pts',(-13.4884811124748,-69.7438497016404,
0.));
#132513=CARTESIAN_POINT('Ctrl Pts',(-13.4884811124748,-69.7438497016404,
12.));
#132514=CARTESIAN_POINT('Ctrl Pts',(-13.4779147665285,-69.7245162492251,
0.));
#132515=CARTESIAN_POINT('Ctrl Pts',(-13.4779147665285,-69.7245162492251,
12.));
#132516=CARTESIAN_POINT('Ctrl Pts',(-13.4673907676045,-69.7052135202003,
0.));
#132517=CARTESIAN_POINT('Ctrl Pts',(-13.4673907676045,-69.7052135202003,
12.));
#132518=CARTESIAN_POINT('Ctrl Pts',(-13.4569091224762,-69.6859416793898,
0.));
#132519=CARTESIAN_POINT('Ctrl Pts',(-13.4569091224762,-69.6859416793898,
12.));
#132520=CARTESIAN_POINT('Ctrl Pts',(-13.4464698378456,-69.6667008924454,
0.));
#132521=CARTESIAN_POINT('Ctrl Pts',(-13.4464698378456,-69.6667008924454,
12.));
#132522=CARTESIAN_POINT('Ctrl Pts',(-13.4360729203444,-69.6474913258684,
0.));
#132523=CARTESIAN_POINT('Ctrl Pts',(-13.4360729203444,-69.6474913258684,
12.));
#132524=CARTESIAN_POINT('Ctrl Pts',(-13.425718376534,-69.6283131470267,
0.));
#132525=CARTESIAN_POINT('Ctrl Pts',(-13.425718376534,-69.6283131470267,
12.));
#132526=CARTESIAN_POINT('Ctrl Pts',(-13.4154062128998,-69.6091665241743,
0.));
#132527=CARTESIAN_POINT('Ctrl Pts',(-13.4154062128998,-69.6091665241743,
12.));
#132528=CARTESIAN_POINT('Ctrl Pts',(-13.4051364358494,-69.5900516264524,
0.));
#132529=CARTESIAN_POINT('Ctrl Pts',(-13.4051364358494,-69.5900516264524,
12.));
#132530=CARTESIAN_POINT('Ctrl Pts',(-13.3949090517173,-69.5709686238701,
0.));
#132531=CARTESIAN_POINT('Ctrl Pts',(-13.3949090517173,-69.5709686238701,
12.));
#132532=CARTESIAN_POINT('Ctrl Pts',(-13.3847240667626,-69.5519176872857,
0.));
#132533=CARTESIAN_POINT('Ctrl Pts',(-13.3847240667626,-69.5519176872857,
12.));
#132534=CARTESIAN_POINT('Ctrl Pts',(-13.3745814871667,-69.5328989883899,
0.));
#132535=CARTESIAN_POINT('Ctrl Pts',(-13.3745814871667,-69.5328989883899,
12.));
#132536=CARTESIAN_POINT('Ctrl Pts',(-13.3644813190225,-69.5139126996703,
0.));
#132537=CARTESIAN_POINT('Ctrl Pts',(-13.3644813190225,-69.5139126996703,
12.));
#132538=CARTESIAN_POINT('Ctrl Pts',(-13.3544235683399,-69.4949589944633,
0.));
#132539=CARTESIAN_POINT('Ctrl Pts',(-13.3544235683399,-69.4949589944633,
12.));
#132540=CARTESIAN_POINT('Ctrl Pts',(-13.3444082410546,-69.4760380470382,
0.));
#132541=CARTESIAN_POINT('Ctrl Pts',(-13.3444082410546,-69.4760380470382,
12.));
#132542=CARTESIAN_POINT('Ctrl Pts',(-13.3344353430313,-69.4571500326673,
0.));
#132543=CARTESIAN_POINT('Ctrl Pts',(-13.3344353430313,-69.4571500326673,
12.));
#132544=CARTESIAN_POINT('Ctrl Pts',(-13.3245048800641,-69.4382951276983,
0.));
#132545=CARTESIAN_POINT('Ctrl Pts',(-13.3245048800641,-69.4382951276983,
12.));
#132546=CARTESIAN_POINT('Ctrl Pts',(-13.3146168578738,-69.4194735096238,
0.));
#132547=CARTESIAN_POINT('Ctrl Pts',(-13.3146168578738,-69.4194735096238,
12.));
#132548=CARTESIAN_POINT('Ctrl Pts',(-13.3047712821046,-69.4006853569485,
0.));
#132549=CARTESIAN_POINT('Ctrl Pts',(-13.3047712821046,-69.4006853569485,
12.));
#132550=CARTESIAN_POINT('Ctrl Pts',(-13.2949681583164,-69.3819308490408,
0.));
#132551=CARTESIAN_POINT('Ctrl Pts',(-13.2949681583164,-69.3819308490408,
12.));
#132552=CARTESIAN_POINT('Ctrl Pts',(-13.2852074919767,-69.3632101660072,
0.));
#132553=CARTESIAN_POINT('Ctrl Pts',(-13.2852074919767,-69.3632101660072,
12.));
#132554=CARTESIAN_POINT('Ctrl Pts',(-13.2754892884437,-69.3445234885088,
0.));
#132555=CARTESIAN_POINT('Ctrl Pts',(-13.2754892884437,-69.3445234885088,
12.));
#132556=CARTESIAN_POINT('Ctrl Pts',(-13.2658135529616,-69.3258709977416,
0.));
#132557=CARTESIAN_POINT('Ctrl Pts',(-13.2658135529616,-69.3258709977416,
12.));
#132558=CARTESIAN_POINT('Ctrl Pts',(-13.2561802906901,-69.3072528758546,
0.));
#132559=CARTESIAN_POINT('Ctrl Pts',(-13.2561802906901,-69.3072528758546,
12.));
#132560=CARTESIAN_POINT('Ctrl Pts',(-13.2465895067264,-69.2886693063193,
0.));
#132561=CARTESIAN_POINT('Ctrl Pts',(-13.2465895067264,-69.2886693063193,
12.));
#132562=CARTESIAN_POINT('Ctrl Pts',(-13.2370412061218,-69.2701204742436,
0.));
#132563=CARTESIAN_POINT('Ctrl Pts',(-13.2370412061218,-69.2701204742436,
12.));
#132564=CARTESIAN_POINT('Ctrl Pts',(-13.2275353939044,-69.2516065668809,
0.));
#132565=CARTESIAN_POINT('Ctrl Pts',(-13.2275353939044,-69.2516065668809,
12.));
#132566=CARTESIAN_POINT('Ctrl Pts',(-13.2180720750585,-69.2331277732819,
0.));
#132567=CARTESIAN_POINT('Ctrl Pts',(-13.2180720750585,-69.2331277732819,
12.));
#132568=CARTESIAN_POINT('Ctrl Pts',(-13.2086512544729,-69.2146842833506,
0.));
#132569=CARTESIAN_POINT('Ctrl Pts',(-13.2086512544729,-69.2146842833506,
12.));
#132570=CARTESIAN_POINT('Ctrl Pts',(-13.1992729368928,-69.1962762870524,
0.));
#132571=CARTESIAN_POINT('Ctrl Pts',(-13.1992729368928,-69.1962762870524,
12.));
#132572=CARTESIAN_POINT('Ctrl Pts',(-13.1899371268689,-69.1779039736026,
0.));
#132573=CARTESIAN_POINT('Ctrl Pts',(-13.1899371268689,-69.1779039736026,
12.));
#132574=CARTESIAN_POINT('Ctrl Pts',(-13.1806438286944,-69.1595675305294,
0.));
#132575=CARTESIAN_POINT('Ctrl Pts',(-13.1806438286944,-69.1595675305294,
12.));
#132576=CARTESIAN_POINT('Ctrl Pts',(-13.1713930465142,-69.141267145461,
0.));
#132577=CARTESIAN_POINT('Ctrl Pts',(-13.1713930465142,-69.141267145461,
12.));
#132578=CARTESIAN_POINT('Ctrl Pts',(-13.1621847844533,-69.1230030082597,
0.));
#132579=CARTESIAN_POINT('Ctrl Pts',(-13.1621847844533,-69.1230030082597,
12.));
#132580=CARTESIAN_POINT('Ctrl Pts',(-13.1530190467181,-69.1047753127633,
0.));
#132581=CARTESIAN_POINT('Ctrl Pts',(-13.1530190467181,-69.1047753127633,
12.));
#132582=CARTESIAN_POINT('Ctrl Pts',(-13.1438958377397,-69.0865842593063,
0.));
#132583=CARTESIAN_POINT('Ctrl Pts',(-13.1438958377397,-69.0865842593063,
12.));
#132584=CARTESIAN_POINT('Ctrl Pts',(-13.1348151621824,-69.0684300549426,
0.));
#132585=CARTESIAN_POINT('Ctrl Pts',(-13.1348151621824,-69.0684300549426,
12.));
#132586=CARTESIAN_POINT('Ctrl Pts',(-13.1257770246378,-69.0503129081778,
0.));
#132587=CARTESIAN_POINT('Ctrl Pts',(-13.1257770246378,-69.0503129081778,
12.));
#132588=CARTESIAN_POINT('Ctrl Pts',(-13.1167814293495,-69.0322330243336,
0.));
#132589=CARTESIAN_POINT('Ctrl Pts',(-13.1167814293495,-69.0322330243336,
12.));
#132590=CARTESIAN_POINT('Ctrl Pts',(-13.1078283799726,-69.0141906015137,
0.));
#132591=CARTESIAN_POINT('Ctrl Pts',(-13.1078283799726,-69.0141906015137,
12.));
#132592=CARTESIAN_POINT('Ctrl Pts',(-13.0989178791843,-68.9961858241577,
0.));
#132593=CARTESIAN_POINT('Ctrl Pts',(-13.0989178791843,-68.9961858241577,
12.));
#132594=CARTESIAN_POINT('Ctrl Pts',(-13.0900499290541,-68.9782188692654,
0.));
#132595=CARTESIAN_POINT('Ctrl Pts',(-13.0900499290541,-68.9782188692654,
12.));
#132596=CARTESIAN_POINT('Ctrl Pts',(-13.0812245317816,-68.9602899187628,
0.));
#132597=CARTESIAN_POINT('Ctrl Pts',(-13.0812245317816,-68.9602899187628,
12.));
#132598=CARTESIAN_POINT('Ctrl Pts',(-13.072441690283,-68.9423991694493,
0.));
#132599=CARTESIAN_POINT('Ctrl Pts',(-13.072441690283,-68.9423991694493,
12.));
#132600=CARTESIAN_POINT('Ctrl Pts',(-13.0637014089018,-68.9245468449865,
0.));
#132601=CARTESIAN_POINT('Ctrl Pts',(-13.0637014089018,-68.9245468449865,
12.));
#132602=CARTESIAN_POINT('Ctrl Pts',(-13.0550036938793,-68.9067332040842,
0.));
#132603=CARTESIAN_POINT('Ctrl Pts',(-13.0550036938793,-68.9067332040842,
12.));
#132604=CARTESIAN_POINT('Ctrl Pts',(-13.0463485518185,-68.8889585151431,
0.));
#132605=CARTESIAN_POINT('Ctrl Pts',(-13.0463485518185,-68.8889585151431,
12.));
#132606=CARTESIAN_POINT('Ctrl Pts',(-13.0377359881863,-68.8712230321823,
0.));
#132607=CARTESIAN_POINT('Ctrl Pts',(-13.0377359881863,-68.8712230321823,
12.));
#132608=CARTESIAN_POINT('Ctrl Pts',(-13.0291660060118,-68.8535269726871,
0.));
#132609=CARTESIAN_POINT('Ctrl Pts',(-13.0291660060118,-68.8535269726871,
12.));
#132610=CARTESIAN_POINT('Ctrl Pts',(-13.0206386039729,-68.835870488774,
0.));
#132611=CARTESIAN_POINT('Ctrl Pts',(-13.0206386039729,-68.835870488774,
12.));
#132612=CARTESIAN_POINT('Ctrl Pts',(-13.0121537769003,-68.8182536654067,
0.));
#132613=CARTESIAN_POINT('Ctrl Pts',(-13.0121537769003,-68.8182536654067,
12.));
#132614=CARTESIAN_POINT('Ctrl Pts',(-13.0053999700929,-68.8041919669403,
0.));
#132615=CARTESIAN_POINT('Ctrl Pts',(-13.0053999700929,-68.8041919669403,
12.));
#132616=CARTESIAN_POINT('Ctrl Pts',(-13.0003537683089,-68.7936635625788,
0.));
#132617=CARTESIAN_POINT('Ctrl Pts',(-13.0003537683089,-68.7936635625788,
12.));
#132618=CARTESIAN_POINT('Ctrl Pts',(-12.996998146029,-68.7866525680284,
0.));
#132619=CARTESIAN_POINT('Ctrl Pts',(-12.996998146029,-68.7866525680284,
12.));
#132620=CARTESIAN_POINT('Ctrl Pts',(-12.9953224629497,-68.7831490561748,
0.));
#132621=CARTESIAN_POINT('Ctrl Pts',(-12.9953224629497,-68.7831490561748,
12.));
#132622=CARTESIAN_POINT('',(-12.9953224629497,-68.7831490561748,12.));
#132623=CARTESIAN_POINT('Ctrl Pts',(-12.9953224629497,-68.7831490561748,
12.));
#132624=CARTESIAN_POINT('Ctrl Pts',(-12.996998146029,-68.7866525680284,
12.));
#132625=CARTESIAN_POINT('Ctrl Pts',(-13.0003537683089,-68.7936635625788,
12.));
#132626=CARTESIAN_POINT('Ctrl Pts',(-13.0053999700929,-68.8041919669403,
12.));
#132627=CARTESIAN_POINT('Ctrl Pts',(-13.0121537769003,-68.8182536654067,
12.));
#132628=CARTESIAN_POINT('Ctrl Pts',(-13.0206386039729,-68.835870488774,
12.));
#132629=CARTESIAN_POINT('Ctrl Pts',(-13.0291660060118,-68.8535269726871,
12.));
#132630=CARTESIAN_POINT('Ctrl Pts',(-13.0377359881863,-68.8712230321823,
12.));
#132631=CARTESIAN_POINT('Ctrl Pts',(-13.0463485518185,-68.8889585151431,
12.));
#132632=CARTESIAN_POINT('Ctrl Pts',(-13.0550036938793,-68.9067332040842,
12.));
#132633=CARTESIAN_POINT('Ctrl Pts',(-13.0637014089018,-68.9245468449865,
12.));
#132634=CARTESIAN_POINT('Ctrl Pts',(-13.072441690283,-68.9423991694493,
12.));
#132635=CARTESIAN_POINT('Ctrl Pts',(-13.0812245317816,-68.9602899187628,
12.));
#132636=CARTESIAN_POINT('Ctrl Pts',(-13.0900499290541,-68.9782188692654,
12.));
#132637=CARTESIAN_POINT('Ctrl Pts',(-13.0989178791843,-68.9961858241577,
12.));
#132638=CARTESIAN_POINT('Ctrl Pts',(-13.1078283799726,-69.0141906015137,
12.));
#132639=CARTESIAN_POINT('Ctrl Pts',(-13.1167814293495,-69.0322330243336,
12.));
#132640=CARTESIAN_POINT('Ctrl Pts',(-13.1257770246378,-69.0503129081778,
12.));
#132641=CARTESIAN_POINT('Ctrl Pts',(-13.1348151621824,-69.0684300549426,
12.));
#132642=CARTESIAN_POINT('Ctrl Pts',(-13.1438958377397,-69.0865842593063,
12.));
#132643=CARTESIAN_POINT('Ctrl Pts',(-13.1530190467181,-69.1047753127633,
12.));
#132644=CARTESIAN_POINT('Ctrl Pts',(-13.1621847844533,-69.1230030082597,
12.));
#132645=CARTESIAN_POINT('Ctrl Pts',(-13.1713930465142,-69.141267145461,
12.));
#132646=CARTESIAN_POINT('Ctrl Pts',(-13.1806438286944,-69.1595675305294,
12.));
#132647=CARTESIAN_POINT('Ctrl Pts',(-13.1899371268689,-69.1779039736026,
12.));
#132648=CARTESIAN_POINT('Ctrl Pts',(-13.1992729368928,-69.1962762870524,
12.));
#132649=CARTESIAN_POINT('Ctrl Pts',(-13.2086512544729,-69.2146842833506,
12.));
#132650=CARTESIAN_POINT('Ctrl Pts',(-13.2180720750585,-69.2331277732819,
12.));
#132651=CARTESIAN_POINT('Ctrl Pts',(-13.2275353939044,-69.2516065668809,
12.));
#132652=CARTESIAN_POINT('Ctrl Pts',(-13.2370412061218,-69.2701204742436,
12.));
#132653=CARTESIAN_POINT('Ctrl Pts',(-13.2465895067264,-69.2886693063193,
12.));
#132654=CARTESIAN_POINT('Ctrl Pts',(-13.2561802906901,-69.3072528758546,
12.));
#132655=CARTESIAN_POINT('Ctrl Pts',(-13.2658135529616,-69.3258709977416,
12.));
#132656=CARTESIAN_POINT('Ctrl Pts',(-13.2754892884437,-69.3445234885088,
12.));
#132657=CARTESIAN_POINT('Ctrl Pts',(-13.2852074919767,-69.3632101660072,
12.));
#132658=CARTESIAN_POINT('Ctrl Pts',(-13.2949681583164,-69.3819308490408,
12.));
#132659=CARTESIAN_POINT('Ctrl Pts',(-13.3047712821046,-69.4006853569485,
12.));
#132660=CARTESIAN_POINT('Ctrl Pts',(-13.3146168578738,-69.4194735096238,
12.));
#132661=CARTESIAN_POINT('Ctrl Pts',(-13.3245048800641,-69.4382951276983,
12.));
#132662=CARTESIAN_POINT('Ctrl Pts',(-13.3344353430313,-69.4571500326673,
12.));
#132663=CARTESIAN_POINT('Ctrl Pts',(-13.3444082410546,-69.4760380470382,
12.));
#132664=CARTESIAN_POINT('Ctrl Pts',(-13.3544235683399,-69.4949589944633,
12.));
#132665=CARTESIAN_POINT('Ctrl Pts',(-13.3644813190225,-69.5139126996703,
12.));
#132666=CARTESIAN_POINT('Ctrl Pts',(-13.3745814871667,-69.5328989883899,
12.));
#132667=CARTESIAN_POINT('Ctrl Pts',(-13.3847240667626,-69.5519176872857,
12.));
#132668=CARTESIAN_POINT('Ctrl Pts',(-13.3949090517173,-69.5709686238701,
12.));
#132669=CARTESIAN_POINT('Ctrl Pts',(-13.4051364358494,-69.5900516264524,
12.));
#132670=CARTESIAN_POINT('Ctrl Pts',(-13.4154062128998,-69.6091665241743,
12.));
#132671=CARTESIAN_POINT('Ctrl Pts',(-13.425718376534,-69.6283131470267,
12.));
#132672=CARTESIAN_POINT('Ctrl Pts',(-13.4360729203444,-69.6474913258684,
12.));
#132673=CARTESIAN_POINT('Ctrl Pts',(-13.4464698378456,-69.6667008924454,
12.));
#132674=CARTESIAN_POINT('Ctrl Pts',(-13.4569091224762,-69.6859416793898,
12.));
#132675=CARTESIAN_POINT('Ctrl Pts',(-13.4673907676045,-69.7052135202003,
12.));
#132676=CARTESIAN_POINT('Ctrl Pts',(-13.4779147665285,-69.7245162492251,
12.));
#132677=CARTESIAN_POINT('Ctrl Pts',(-13.4884811124748,-69.7438497016404,
12.));
#132678=CARTESIAN_POINT('Ctrl Pts',(-13.4990897985903,-69.7632137134247,
12.));
#132679=CARTESIAN_POINT('Ctrl Pts',(-13.5097408179478,-69.7826081213575,
12.));
#132680=CARTESIAN_POINT('Ctrl Pts',(-13.5204341635507,-69.8020327630204,
12.));
#132681=CARTESIAN_POINT('Ctrl Pts',(-13.5311698283339,-69.8214874767944,
12.));
#132682=CARTESIAN_POINT('Ctrl Pts',(-13.5419478051626,-69.840972101856,
12.));
#132683=CARTESIAN_POINT('Ctrl Pts',(-13.5527680868256,-69.8604864781705,
12.));
#132684=CARTESIAN_POINT('Ctrl Pts',(-13.5636306660422,-69.880030446488,
12.));
#132685=CARTESIAN_POINT('Ctrl Pts',(-13.5745355354657,-69.899603848336,
12.));
#132686=CARTESIAN_POINT('Ctrl Pts',(-13.5854826876834,-69.9192065260107,
12.));
#132687=CARTESIAN_POINT('Ctrl Pts',(-13.5964721152136,-69.9388383225655,
12.));
#132688=CARTESIAN_POINT('Ctrl Pts',(-13.6075038105,-69.9584990817989,12.));
#132689=CARTESIAN_POINT('Ctrl Pts',(-13.61857776592,-69.9781886482543,12.));
#132690=CARTESIAN_POINT('Ctrl Pts',(-13.6296939737866,-69.9979068672163,
12.));
#132691=CARTESIAN_POINT('Ctrl Pts',(-13.6408524263496,-70.0176535847047,
12.));
#132692=CARTESIAN_POINT('Ctrl Pts',(-13.6520531157904,-70.037428647466,
12.));
#132693=CARTESIAN_POINT('Ctrl Pts',(-13.6632960342192,-70.057231902965,
12.));
#132694=CARTESIAN_POINT('Ctrl Pts',(-13.6745811736825,-70.0770631993831,
12.));
#132695=CARTESIAN_POINT('Ctrl Pts',(-13.685908526165,-70.0969223856123,
12.));
#132696=CARTESIAN_POINT('Ctrl Pts',(-13.6972780835898,-70.1168093112493,
12.));
#132697=CARTESIAN_POINT('Ctrl Pts',(-13.7086898378127,-70.1367238265853,
12.));
#132698=CARTESIAN_POINT('Ctrl Pts',(-13.7201437806207,-70.1566657825989,
12.));
#132699=CARTESIAN_POINT('Ctrl Pts',(-13.73163990374,-70.1766350309554,12.));
#132700=CARTESIAN_POINT('Ctrl Pts',(-13.7431781988368,-70.1966314240012,
12.));
#132701=CARTESIAN_POINT('Ctrl Pts',(-13.7547586575178,-70.216654814759,
12.));
#132702=CARTESIAN_POINT('Ctrl Pts',(-13.7663812713235,-70.2367050569174,
12.));
#132703=CARTESIAN_POINT('Ctrl Pts',(-13.7780460317284,-70.2567820048253,
12.));
#132704=CARTESIAN_POINT('Ctrl Pts',(-13.7897529301482,-70.2768855134909,
12.));
#132705=CARTESIAN_POINT('Ctrl Pts',(-13.8015019579411,-70.2970154385763,
12.));
#132706=CARTESIAN_POINT('Ctrl Pts',(-13.8132931064067,-70.3171716363912,
12.));
#132707=CARTESIAN_POINT('Ctrl Pts',(-13.8251263667799,-70.3373539638841,
12.));
#132708=CARTESIAN_POINT('Ctrl Pts',(-13.8370017302318,-70.3575622786373,
12.));
#132709=CARTESIAN_POINT('Ctrl Pts',(-13.8489191878774,-70.377796438866,
12.));
#132710=CARTESIAN_POINT('Ctrl Pts',(-13.8608787307753,-70.3980563034142,
12.));
#132711=CARTESIAN_POINT('Ctrl Pts',(-13.8728803499284,-70.4183417317486,
12.));
#132712=CARTESIAN_POINT('Ctrl Pts',(-13.8849240362757,-70.4386525839492,
12.));
#132713=CARTESIAN_POINT('Ctrl Pts',(-13.8970097806947,-70.4589887207043,
12.));
#132714=CARTESIAN_POINT('Ctrl Pts',(-13.9091375740084,-70.4793500033106,
12.));
#132715=CARTESIAN_POINT('Ctrl Pts',(-13.9213074069852,-70.4997362936671,
12.));
#132716=CARTESIAN_POINT('Ctrl Pts',(-13.9335192703389,-70.5201474542717,
12.));
#132717=CARTESIAN_POINT('Ctrl Pts',(-13.9457731547217,-70.5405833482123,
12.));
#132718=CARTESIAN_POINT('Ctrl Pts',(-13.9580690507262,-70.5610438391622,
12.));
#132719=CARTESIAN_POINT('Ctrl Pts',(-13.9704069488918,-70.5815287913791,
12.));
#132720=CARTESIAN_POINT('Ctrl Pts',(-13.9827868397057,-70.6020380697004,
12.));
#132721=CARTESIAN_POINT('Ctrl Pts',(-13.9952087136018,-70.6225715395392,
12.));
#132722=CARTESIAN_POINT('Ctrl Pts',(-14.0076725609536,-70.6431290668744,
12.));
#132723=CARTESIAN_POINT('Ctrl Pts',(-14.020178372077,-70.6637105182487,
12.));
#132724=CARTESIAN_POINT('Ctrl Pts',(-14.0327261372363,-70.6843157607672,
12.));
#132725=CARTESIAN_POINT('Ctrl Pts',(-14.0453158466451,-70.7049446620931,
12.));
#132726=CARTESIAN_POINT('Ctrl Pts',(-14.0579474904657,-70.7255970904433,
12.));
#132727=CARTESIAN_POINT('Ctrl Pts',(-14.0706210588015,-70.7462729145799,
12.));
#132728=CARTESIAN_POINT('Ctrl Pts',(-14.0833365416995,-70.7669720038067,
12.));
#132729=CARTESIAN_POINT('Ctrl Pts',(-14.0960939291568,-70.787694227969,
12.));
#132730=CARTESIAN_POINT('Ctrl Pts',(-14.1088932111214,-70.8084394574491,
12.));
#132731=CARTESIAN_POINT('Ctrl Pts',(-14.1217343774914,-70.8292075631624,
12.));
#132732=CARTESIAN_POINT('Ctrl Pts',(-14.1346174181079,-70.8499984165493,
12.));
#132733=CARTESIAN_POINT('Ctrl Pts',(-14.1475423227567,-70.8708118895718,
12.));
#132734=CARTESIAN_POINT('Ctrl Pts',(-14.1605090811753,-70.8916478547131,
12.));
#132735=CARTESIAN_POINT('Ctrl Pts',(-14.1735176830533,-70.9125061849744,
12.));
#132736=CARTESIAN_POINT('Ctrl Pts',(-14.1865681180321,-70.9333867538705,
12.));
#132737=CARTESIAN_POINT('Ctrl Pts',(-14.1996603756984,-70.9542894354221,
12.));
#132738=CARTESIAN_POINT('Ctrl Pts',(-14.2127944455841,-70.9752141041527,
12.));
#132739=CARTESIAN_POINT('Ctrl Pts',(-14.2259703171739,-70.996160635087,
12.));
#132740=CARTESIAN_POINT('Ctrl Pts',(-14.2391879799063,-71.0171289037493,
12.));
#132741=CARTESIAN_POINT('Ctrl Pts',(-14.2524474231732,-71.0381187861585,
12.));
#132742=CARTESIAN_POINT('Ctrl Pts',(-14.2657486363136,-71.059130158822,
12.));
#132743=CARTESIAN_POINT('Ctrl Pts',(-14.2790916086129,-71.0801628987314,
12.));
#132744=CARTESIAN_POINT('Ctrl Pts',(-14.2924763293101,-71.1012168833626,
12.));
#132745=CARTESIAN_POINT('Ctrl Pts',(-14.3059027875992,-71.1222919906718,
12.));
#132746=CARTESIAN_POINT('Ctrl Pts',(-14.3193709726295,-71.1433880990932,
12.));
#132747=CARTESIAN_POINT('Ctrl Pts',(-14.3328808734993,-71.1645050875323,
12.));
#132748=CARTESIAN_POINT('Ctrl Pts',(-14.3464324792537,-71.185642835361,
12.));
#132749=CARTESIAN_POINT('Ctrl Pts',(-14.3600257788927,-71.2068012224187,
12.));
#132750=CARTESIAN_POINT('Ctrl Pts',(-14.3736607613723,-71.2279801290088,
12.));
#132751=CARTESIAN_POINT('Ctrl Pts',(-14.3873374156056,-71.2491794358956,
12.));
#132752=CARTESIAN_POINT('Ctrl Pts',(-14.401055730457,-71.2703990242986,
12.));
#132753=CARTESIAN_POINT('Ctrl Pts',(-14.4148156947384,-71.2916387758864,
12.));
#132754=CARTESIAN_POINT('Ctrl Pts',(-14.4286172972168,-71.3128985727777,
12.));
#132755=CARTESIAN_POINT('Ctrl Pts',(-14.4424605266166,-71.3341782975393,
12.));
#132756=CARTESIAN_POINT('Ctrl Pts',(-14.4563453716204,-71.3554778331835,
12.));
#132757=CARTESIAN_POINT('Ctrl Pts',(-14.470271820865,-71.3767970631642,
12.));
#132758=CARTESIAN_POINT('Ctrl Pts',(-14.4842398629353,-71.398135871371,
12.));
#132759=CARTESIAN_POINT('Ctrl Pts',(-14.4982494863716,-71.4194941421279,
12.));
#132760=CARTESIAN_POINT('Ctrl Pts',(-14.5123006796728,-71.4408717601917,
12.));
#132761=CARTESIAN_POINT('Ctrl Pts',(-14.5263934312969,-71.4622686107475,
12.));
#132762=CARTESIAN_POINT('Ctrl Pts',(-14.540527729659,-71.4836845794052,
12.));
#132763=CARTESIAN_POINT('Ctrl Pts',(-14.5547035631233,-71.5051195521914,
12.));
#132764=CARTESIAN_POINT('Ctrl Pts',(-14.568920920009,-71.52657341555,12.));
#132765=CARTESIAN_POINT('Ctrl Pts',(-14.5831797885951,-71.5480460563445,
12.));
#132766=CARTESIAN_POINT('Ctrl Pts',(-14.5974801571209,-71.569537361856,
12.));
#132767=CARTESIAN_POINT('Ctrl Pts',(-14.611822013785,-71.5910472197815,
12.));
#132768=CARTESIAN_POINT('Ctrl Pts',(-14.6262053467372,-71.6125755182295,
12.));
#132769=CARTESIAN_POINT('Ctrl Pts',(-14.6406301440817,-71.6341221457175,
12.));
#132770=CARTESIAN_POINT('Ctrl Pts',(-14.6550963938832,-71.6556869911669,
12.));
#132771=CARTESIAN_POINT('Ctrl Pts',(-14.6696040841679,-71.6772699438966,
12.));
#132772=CARTESIAN_POINT('Ctrl Pts',(-14.6841532029231,-71.698870893617,
12.));
#132773=CARTESIAN_POINT('Ctrl Pts',(-14.6987437380898,-71.7204897304186,
12.));
#132774=CARTESIAN_POINT('Ctrl Pts',(-14.7133756775622,-71.7421263447707,
12.));
#132775=CARTESIAN_POINT('Ctrl Pts',(-14.7280490091954,-71.7637806275316,
12.));
#132776=CARTESIAN_POINT('Ctrl Pts',(-14.742763720807,-71.7854524699563,
12.));
#132777=CARTESIAN_POINT('Ctrl Pts',(-14.7575198001776,-71.8071417637019,
12.));
#132778=CARTESIAN_POINT('Ctrl Pts',(-14.7723172350454,-71.8288484008343,
12.));
#132779=CARTESIAN_POINT('Ctrl Pts',(-14.7871560131021,-71.8505722738286,
12.));
#132780=CARTESIAN_POINT('Ctrl Pts',(-14.8020361220002,-71.872313275546,
12.));
#132781=CARTESIAN_POINT('Ctrl Pts',(-14.8169575493559,-71.8940712992119,
12.));
#132782=CARTESIAN_POINT('Ctrl Pts',(-14.8319202827482,-71.9158462383915,
12.));
#132783=CARTESIAN_POINT('Ctrl Pts',(-14.846924309716,-71.9376379869668,
12.));
#132784=CARTESIAN_POINT('Ctrl Pts',(-14.8619696177503,-71.9594464391063,
12.));
#132785=CARTESIAN_POINT('Ctrl Pts',(-14.8770561943011,-71.9812714893087,
12.));
#132786=CARTESIAN_POINT('Ctrl Pts',(-14.8921840267829,-72.0031130324519,
12.));
#132787=CARTESIAN_POINT('Ctrl Pts',(-14.9073531025763,-72.0249709638419,
12.));
#132788=CARTESIAN_POINT('Ctrl Pts',(-14.9225634090269,-72.046845179251,
12.));
#132789=CARTESIAN_POINT('Ctrl Pts',(-14.937814933439,-72.0687355749815,
12.));
#132790=CARTESIAN_POINT('Ctrl Pts',(-14.953107663077,-72.0906420478085,
12.));
#132791=CARTESIAN_POINT('Ctrl Pts',(-14.9684415851699,-72.1125644948547,
12.));
#132792=CARTESIAN_POINT('Ctrl Pts',(-14.9838166869107,-72.1345028134779,
12.));
#132793=CARTESIAN_POINT('Ctrl Pts',(-14.9992329554537,-72.1564569011668,
12.));
#132794=CARTESIAN_POINT('Ctrl Pts',(-15.0146903779061,-72.1784266553948,
12.));
#132795=CARTESIAN_POINT('Ctrl Pts',(-15.0301889413255,-72.2004119736104,
12.));
#132796=CARTESIAN_POINT('Ctrl Pts',(-15.0457286327328,-72.2224127535401,
12.));
#132797=CARTESIAN_POINT('Ctrl Pts',(-15.0613094391186,-72.244428893425,
12.));
#132798=CARTESIAN_POINT('Ctrl Pts',(-15.0769313474476,-72.266460292285,
12.));
#132799=CARTESIAN_POINT('Ctrl Pts',(-15.0925943446593,-72.2885068501641,
12.));
#132800=CARTESIAN_POINT('Ctrl Pts',(-15.1082984176655,-72.3105684683971,
12.));
#132801=CARTESIAN_POINT('Ctrl Pts',(-15.1240435533478,-72.332645049021,
12.));
#132802=CARTESIAN_POINT('Ctrl Pts',(-15.1398297385513,-72.3547364941996,
12.));
#132803=CARTESIAN_POINT('Ctrl Pts',(-15.1556569600747,-72.37684270559,12.));
#132804=CARTESIAN_POINT('Ctrl Pts',(-15.1715252046602,-72.3989635838476,
12.));
#132805=CARTESIAN_POINT('Ctrl Pts',(-15.1874344589715,-72.4210990277819,
12.));
#132806=CARTESIAN_POINT('Ctrl Pts',(-15.2033847096077,-72.4432489350415,
12.));
#132807=CARTESIAN_POINT('Ctrl Pts',(-15.2193759431359,-72.4654132036373,
12.));
#132808=CARTESIAN_POINT('Ctrl Pts',(-15.2354081461151,-72.4875917332729,
12.));
#132809=CARTESIAN_POINT('Ctrl Pts',(-15.2514813051174,-72.5097844266083,
12.));
#132810=CARTESIAN_POINT('Ctrl Pts',(-15.2675954067495,-72.5319911908978,
12.));
#132811=CARTESIAN_POINT('Ctrl Pts',(-15.2837504376562,-72.5542119383748,
12.));
#132812=CARTESIAN_POINT('Ctrl Pts',(-15.2976335024853,-72.5732713370796,
12.));
#132813=CARTESIAN_POINT('Ctrl Pts',(-15.3082994603652,-72.5878912620663,
12.));
#132814=CARTESIAN_POINT('Ctrl Pts',(-15.3157301930832,-72.5980655789898,
12.));
#132815=CARTESIAN_POINT('Ctrl Pts',(-15.3199137230319,-72.6037902605228,
12.));
#132816=CARTESIAN_POINT('Ctrl Pts',(-15.3208442077421,-72.6050633494713,
12.));
#132817=CARTESIAN_POINT('',(-12.9953224629497,-68.7831490561748,0.));
#132818=CARTESIAN_POINT('',(-12.9953224629497,-68.7831490561748,0.));
#132819=CARTESIAN_POINT('Ctrl Pts',(-15.3208442077421,-72.6050633494713,
0.));
#132820=CARTESIAN_POINT('Ctrl Pts',(-15.3199137230319,-72.6037902605228,
0.));
#132821=CARTESIAN_POINT('Ctrl Pts',(-15.3157301930832,-72.5980655789898,
0.));
#132822=CARTESIAN_POINT('Ctrl Pts',(-15.3082994603652,-72.5878912620663,
0.));
#132823=CARTESIAN_POINT('Ctrl Pts',(-15.2976335024853,-72.5732713370796,
0.));
#132824=CARTESIAN_POINT('Ctrl Pts',(-15.2837504376562,-72.5542119383748,
0.));
#132825=CARTESIAN_POINT('Ctrl Pts',(-15.2675954067495,-72.5319911908978,
0.));
#132826=CARTESIAN_POINT('Ctrl Pts',(-15.2514813051174,-72.5097844266083,
0.));
#132827=CARTESIAN_POINT('Ctrl Pts',(-15.2354081461151,-72.4875917332729,
0.));
#132828=CARTESIAN_POINT('Ctrl Pts',(-15.2193759431359,-72.4654132036373,
0.));
#132829=CARTESIAN_POINT('Ctrl Pts',(-15.2033847096077,-72.4432489350415,
0.));
#132830=CARTESIAN_POINT('Ctrl Pts',(-15.1874344589715,-72.4210990277819,
0.));
#132831=CARTESIAN_POINT('Ctrl Pts',(-15.1715252046602,-72.3989635838476,
0.));
#132832=CARTESIAN_POINT('Ctrl Pts',(-15.1556569600747,-72.37684270559,0.));
#132833=CARTESIAN_POINT('Ctrl Pts',(-15.1398297385513,-72.3547364941996,
0.));
#132834=CARTESIAN_POINT('Ctrl Pts',(-15.1240435533478,-72.332645049021,
0.));
#132835=CARTESIAN_POINT('Ctrl Pts',(-15.1082984176655,-72.3105684683971,
0.));
#132836=CARTESIAN_POINT('Ctrl Pts',(-15.0925943446593,-72.2885068501641,
0.));
#132837=CARTESIAN_POINT('Ctrl Pts',(-15.0769313474476,-72.266460292285,
0.));
#132838=CARTESIAN_POINT('Ctrl Pts',(-15.0613094391186,-72.244428893425,
0.));
#132839=CARTESIAN_POINT('Ctrl Pts',(-15.0457286327328,-72.2224127535401,
0.));
#132840=CARTESIAN_POINT('Ctrl Pts',(-15.0301889413255,-72.2004119736104,
0.));
#132841=CARTESIAN_POINT('Ctrl Pts',(-15.0146903779061,-72.1784266553948,
0.));
#132842=CARTESIAN_POINT('Ctrl Pts',(-14.9992329554537,-72.1564569011668,
0.));
#132843=CARTESIAN_POINT('Ctrl Pts',(-14.9838166869107,-72.1345028134779,
0.));
#132844=CARTESIAN_POINT('Ctrl Pts',(-14.9684415851699,-72.1125644948547,
0.));
#132845=CARTESIAN_POINT('Ctrl Pts',(-14.953107663077,-72.0906420478085,
0.));
#132846=CARTESIAN_POINT('Ctrl Pts',(-14.937814933439,-72.0687355749815,
0.));
#132847=CARTESIAN_POINT('Ctrl Pts',(-14.9225634090269,-72.046845179251,
0.));
#132848=CARTESIAN_POINT('Ctrl Pts',(-14.9073531025763,-72.0249709638419,
0.));
#132849=CARTESIAN_POINT('Ctrl Pts',(-14.8921840267829,-72.0031130324519,
0.));
#132850=CARTESIAN_POINT('Ctrl Pts',(-14.8770561943011,-71.9812714893087,
0.));
#132851=CARTESIAN_POINT('Ctrl Pts',(-14.8619696177503,-71.9594464391063,
0.));
#132852=CARTESIAN_POINT('Ctrl Pts',(-14.846924309716,-71.9376379869668,
0.));
#132853=CARTESIAN_POINT('Ctrl Pts',(-14.8319202827482,-71.9158462383915,
0.));
#132854=CARTESIAN_POINT('Ctrl Pts',(-14.8169575493559,-71.8940712992119,
0.));
#132855=CARTESIAN_POINT('Ctrl Pts',(-14.8020361220002,-71.872313275546,
0.));
#132856=CARTESIAN_POINT('Ctrl Pts',(-14.7871560131021,-71.8505722738286,
0.));
#132857=CARTESIAN_POINT('Ctrl Pts',(-14.7723172350454,-71.8288484008343,
0.));
#132858=CARTESIAN_POINT('Ctrl Pts',(-14.7575198001776,-71.8071417637019,
0.));
#132859=CARTESIAN_POINT('Ctrl Pts',(-14.742763720807,-71.7854524699563,
0.));
#132860=CARTESIAN_POINT('Ctrl Pts',(-14.7280490091954,-71.7637806275316,
0.));
#132861=CARTESIAN_POINT('Ctrl Pts',(-14.7133756775622,-71.7421263447707,
0.));
#132862=CARTESIAN_POINT('Ctrl Pts',(-14.6987437380898,-71.7204897304186,
0.));
#132863=CARTESIAN_POINT('Ctrl Pts',(-14.6841532029231,-71.698870893617,
0.));
#132864=CARTESIAN_POINT('Ctrl Pts',(-14.6696040841679,-71.6772699438966,
0.));
#132865=CARTESIAN_POINT('Ctrl Pts',(-14.6550963938832,-71.6556869911669,
0.));
#132866=CARTESIAN_POINT('Ctrl Pts',(-14.6406301440817,-71.6341221457175,
0.));
#132867=CARTESIAN_POINT('Ctrl Pts',(-14.6262053467372,-71.6125755182295,
0.));
#132868=CARTESIAN_POINT('Ctrl Pts',(-14.611822013785,-71.5910472197815,
0.));
#132869=CARTESIAN_POINT('Ctrl Pts',(-14.5974801571209,-71.569537361856,
0.));
#132870=CARTESIAN_POINT('Ctrl Pts',(-14.5831797885951,-71.5480460563445,
0.));
#132871=CARTESIAN_POINT('Ctrl Pts',(-14.568920920009,-71.52657341555,0.));
#132872=CARTESIAN_POINT('Ctrl Pts',(-14.5547035631233,-71.5051195521914,
0.));
#132873=CARTESIAN_POINT('Ctrl Pts',(-14.540527729659,-71.4836845794052,
0.));
#132874=CARTESIAN_POINT('Ctrl Pts',(-14.5263934312969,-71.4622686107475,
0.));
#132875=CARTESIAN_POINT('Ctrl Pts',(-14.5123006796728,-71.4408717601917,
0.));
#132876=CARTESIAN_POINT('Ctrl Pts',(-14.4982494863716,-71.4194941421279,
0.));
#132877=CARTESIAN_POINT('Ctrl Pts',(-14.4842398629353,-71.398135871371,
0.));
#132878=CARTESIAN_POINT('Ctrl Pts',(-14.470271820865,-71.3767970631642,
0.));
#132879=CARTESIAN_POINT('Ctrl Pts',(-14.4563453716204,-71.3554778331835,
0.));
#132880=CARTESIAN_POINT('Ctrl Pts',(-14.4424605266166,-71.3341782975393,
0.));
#132881=CARTESIAN_POINT('Ctrl Pts',(-14.4286172972168,-71.3128985727777,
0.));
#132882=CARTESIAN_POINT('Ctrl Pts',(-14.4148156947384,-71.2916387758864,
0.));
#132883=CARTESIAN_POINT('Ctrl Pts',(-14.401055730457,-71.2703990242986,
0.));
#132884=CARTESIAN_POINT('Ctrl Pts',(-14.3873374156056,-71.2491794358956,
0.));
#132885=CARTESIAN_POINT('Ctrl Pts',(-14.3736607613723,-71.2279801290088,
0.));
#132886=CARTESIAN_POINT('Ctrl Pts',(-14.3600257788927,-71.2068012224187,
0.));
#132887=CARTESIAN_POINT('Ctrl Pts',(-14.3464324792537,-71.185642835361,
0.));
#132888=CARTESIAN_POINT('Ctrl Pts',(-14.3328808734993,-71.1645050875323,
0.));
#132889=CARTESIAN_POINT('Ctrl Pts',(-14.3193709726295,-71.1433880990932,
0.));
#132890=CARTESIAN_POINT('Ctrl Pts',(-14.3059027875992,-71.1222919906718,
0.));
#132891=CARTESIAN_POINT('Ctrl Pts',(-14.2924763293101,-71.1012168833626,
0.));
#132892=CARTESIAN_POINT('Ctrl Pts',(-14.2790916086129,-71.0801628987314,
0.));
#132893=CARTESIAN_POINT('Ctrl Pts',(-14.2657486363136,-71.059130158822,
0.));
#132894=CARTESIAN_POINT('Ctrl Pts',(-14.2524474231732,-71.0381187861585,
0.));
#132895=CARTESIAN_POINT('Ctrl Pts',(-14.2391879799063,-71.0171289037493,
0.));
#132896=CARTESIAN_POINT('Ctrl Pts',(-14.2259703171739,-70.996160635087,
0.));
#132897=CARTESIAN_POINT('Ctrl Pts',(-14.2127944455841,-70.9752141041527,
0.));
#132898=CARTESIAN_POINT('Ctrl Pts',(-14.1996603756984,-70.9542894354221,
0.));
#132899=CARTESIAN_POINT('Ctrl Pts',(-14.1865681180321,-70.9333867538705,
0.));
#132900=CARTESIAN_POINT('Ctrl Pts',(-14.1735176830533,-70.9125061849744,
0.));
#132901=CARTESIAN_POINT('Ctrl Pts',(-14.1605090811753,-70.8916478547131,
0.));
#132902=CARTESIAN_POINT('Ctrl Pts',(-14.1475423227567,-70.8708118895718,
0.));
#132903=CARTESIAN_POINT('Ctrl Pts',(-14.1346174181079,-70.8499984165493,
0.));
#132904=CARTESIAN_POINT('Ctrl Pts',(-14.1217343774914,-70.8292075631624,
0.));
#132905=CARTESIAN_POINT('Ctrl Pts',(-14.1088932111214,-70.8084394574491,
0.));
#132906=CARTESIAN_POINT('Ctrl Pts',(-14.0960939291568,-70.787694227969,
0.));
#132907=CARTESIAN_POINT('Ctrl Pts',(-14.0833365416995,-70.7669720038067,
0.));
#132908=CARTESIAN_POINT('Ctrl Pts',(-14.0706210588015,-70.7462729145799,
0.));
#132909=CARTESIAN_POINT('Ctrl Pts',(-14.0579474904657,-70.7255970904433,
0.));
#132910=CARTESIAN_POINT('Ctrl Pts',(-14.0453158466451,-70.7049446620931,
0.));
#132911=CARTESIAN_POINT('Ctrl Pts',(-14.0327261372363,-70.6843157607672,
0.));
#132912=CARTESIAN_POINT('Ctrl Pts',(-14.020178372077,-70.6637105182487,
0.));
#132913=CARTESIAN_POINT('Ctrl Pts',(-14.0076725609536,-70.6431290668744,
0.));
#132914=CARTESIAN_POINT('Ctrl Pts',(-13.9952087136018,-70.6225715395392,
0.));
#132915=CARTESIAN_POINT('Ctrl Pts',(-13.9827868397057,-70.6020380697004,
0.));
#132916=CARTESIAN_POINT('Ctrl Pts',(-13.9704069488918,-70.5815287913791,
0.));
#132917=CARTESIAN_POINT('Ctrl Pts',(-13.9580690507262,-70.5610438391622,
0.));
#132918=CARTESIAN_POINT('Ctrl Pts',(-13.9457731547217,-70.5405833482123,
0.));
#132919=CARTESIAN_POINT('Ctrl Pts',(-13.9335192703389,-70.5201474542717,
0.));
#132920=CARTESIAN_POINT('Ctrl Pts',(-13.9213074069852,-70.4997362936671,
0.));
#132921=CARTESIAN_POINT('Ctrl Pts',(-13.9091375740084,-70.4793500033106,
0.));
#132922=CARTESIAN_POINT('Ctrl Pts',(-13.8970097806947,-70.4589887207043,
0.));
#132923=CARTESIAN_POINT('Ctrl Pts',(-13.8849240362757,-70.4386525839492,
0.));
#132924=CARTESIAN_POINT('Ctrl Pts',(-13.8728803499284,-70.4183417317486,
0.));
#132925=CARTESIAN_POINT('Ctrl Pts',(-13.8608787307753,-70.3980563034142,
0.));
#132926=CARTESIAN_POINT('Ctrl Pts',(-13.8489191878774,-70.377796438866,
0.));
#132927=CARTESIAN_POINT('Ctrl Pts',(-13.8370017302318,-70.3575622786373,
0.));
#132928=CARTESIAN_POINT('Ctrl Pts',(-13.8251263667799,-70.3373539638841,
0.));
#132929=CARTESIAN_POINT('Ctrl Pts',(-13.8132931064067,-70.3171716363912,
0.));
#132930=CARTESIAN_POINT('Ctrl Pts',(-13.8015019579411,-70.2970154385763,
0.));
#132931=CARTESIAN_POINT('Ctrl Pts',(-13.7897529301482,-70.2768855134909,
0.));
#132932=CARTESIAN_POINT('Ctrl Pts',(-13.7780460317284,-70.2567820048253,
0.));
#132933=CARTESIAN_POINT('Ctrl Pts',(-13.7663812713235,-70.2367050569174,
0.));
#132934=CARTESIAN_POINT('Ctrl Pts',(-13.7547586575178,-70.216654814759,
0.));
#132935=CARTESIAN_POINT('Ctrl Pts',(-13.7431781988368,-70.1966314240012,
0.));
#132936=CARTESIAN_POINT('Ctrl Pts',(-13.73163990374,-70.1766350309554,0.));
#132937=CARTESIAN_POINT('Ctrl Pts',(-13.7201437806207,-70.1566657825989,
0.));
#132938=CARTESIAN_POINT('Ctrl Pts',(-13.7086898378127,-70.1367238265853,
0.));
#132939=CARTESIAN_POINT('Ctrl Pts',(-13.6972780835898,-70.1168093112493,
0.));
#132940=CARTESIAN_POINT('Ctrl Pts',(-13.685908526165,-70.0969223856123,
0.));
#132941=CARTESIAN_POINT('Ctrl Pts',(-13.6745811736825,-70.0770631993831,
0.));
#132942=CARTESIAN_POINT('Ctrl Pts',(-13.6632960342192,-70.057231902965,
0.));
#132943=CARTESIAN_POINT('Ctrl Pts',(-13.6520531157904,-70.037428647466,
0.));
#132944=CARTESIAN_POINT('Ctrl Pts',(-13.6408524263496,-70.0176535847047,
0.));
#132945=CARTESIAN_POINT('Ctrl Pts',(-13.6296939737866,-69.9979068672163,
0.));
#132946=CARTESIAN_POINT('Ctrl Pts',(-13.61857776592,-69.9781886482543,0.));
#132947=CARTESIAN_POINT('Ctrl Pts',(-13.6075038105,-69.9584990817989,0.));
#132948=CARTESIAN_POINT('Ctrl Pts',(-13.5964721152136,-69.9388383225655,
0.));
#132949=CARTESIAN_POINT('Ctrl Pts',(-13.5854826876834,-69.9192065260107,
0.));
#132950=CARTESIAN_POINT('Ctrl Pts',(-13.5745355354657,-69.899603848336,
0.));
#132951=CARTESIAN_POINT('Ctrl Pts',(-13.5636306660422,-69.880030446488,
0.));
#132952=CARTESIAN_POINT('Ctrl Pts',(-13.5527680868256,-69.8604864781705,
0.));
#132953=CARTESIAN_POINT('Ctrl Pts',(-13.5419478051626,-69.840972101856,
0.));
#132954=CARTESIAN_POINT('Ctrl Pts',(-13.5311698283339,-69.8214874767944,
0.));
#132955=CARTESIAN_POINT('Ctrl Pts',(-13.5204341635507,-69.8020327630204,
0.));
#132956=CARTESIAN_POINT('Ctrl Pts',(-13.5097408179478,-69.7826081213575,
0.));
#132957=CARTESIAN_POINT('Ctrl Pts',(-13.4990897985903,-69.7632137134247,
0.));
#132958=CARTESIAN_POINT('Ctrl Pts',(-13.4884811124748,-69.7438497016404,
0.));
#132959=CARTESIAN_POINT('Ctrl Pts',(-13.4779147665285,-69.7245162492251,
0.));
#132960=CARTESIAN_POINT('Ctrl Pts',(-13.4673907676045,-69.7052135202003,
0.));
#132961=CARTESIAN_POINT('Ctrl Pts',(-13.4569091224762,-69.6859416793898,
0.));
#132962=CARTESIAN_POINT('Ctrl Pts',(-13.4464698378456,-69.6667008924454,
0.));
#132963=CARTESIAN_POINT('Ctrl Pts',(-13.4360729203444,-69.6474913258684,
0.));
#132964=CARTESIAN_POINT('Ctrl Pts',(-13.425718376534,-69.6283131470267,
0.));
#132965=CARTESIAN_POINT('Ctrl Pts',(-13.4154062128998,-69.6091665241743,
0.));
#132966=CARTESIAN_POINT('Ctrl Pts',(-13.4051364358494,-69.5900516264524,
0.));
#132967=CARTESIAN_POINT('Ctrl Pts',(-13.3949090517173,-69.5709686238701,
0.));
#132968=CARTESIAN_POINT('Ctrl Pts',(-13.3847240667626,-69.5519176872857,
0.));
#132969=CARTESIAN_POINT('Ctrl Pts',(-13.3745814871667,-69.5328989883899,
0.));
#132970=CARTESIAN_POINT('Ctrl Pts',(-13.3644813190225,-69.5139126996703,
0.));
#132971=CARTESIAN_POINT('Ctrl Pts',(-13.3544235683399,-69.4949589944633,
0.));
#132972=CARTESIAN_POINT('Ctrl Pts',(-13.3444082410546,-69.4760380470382,
0.));
#132973=CARTESIAN_POINT('Ctrl Pts',(-13.3344353430313,-69.4571500326673,
0.));
#132974=CARTESIAN_POINT('Ctrl Pts',(-13.3245048800641,-69.4382951276983,
0.));
#132975=CARTESIAN_POINT('Ctrl Pts',(-13.3146168578738,-69.4194735096238,
0.));
#132976=CARTESIAN_POINT('Ctrl Pts',(-13.3047712821046,-69.4006853569485,
0.));
#132977=CARTESIAN_POINT('Ctrl Pts',(-13.2949681583164,-69.3819308490408,
0.));
#132978=CARTESIAN_POINT('Ctrl Pts',(-13.2852074919767,-69.3632101660072,
0.));
#132979=CARTESIAN_POINT('Ctrl Pts',(-13.2754892884437,-69.3445234885088,
0.));
#132980=CARTESIAN_POINT('Ctrl Pts',(-13.2658135529616,-69.3258709977416,
0.));
#132981=CARTESIAN_POINT('Ctrl Pts',(-13.2561802906901,-69.3072528758546,
0.));
#132982=CARTESIAN_POINT('Ctrl Pts',(-13.2465895067264,-69.2886693063193,
0.));
#132983=CARTESIAN_POINT('Ctrl Pts',(-13.2370412061218,-69.2701204742436,
0.));
#132984=CARTESIAN_POINT('Ctrl Pts',(-13.2275353939044,-69.2516065668809,
0.));
#132985=CARTESIAN_POINT('Ctrl Pts',(-13.2180720750585,-69.2331277732819,
0.));
#132986=CARTESIAN_POINT('Ctrl Pts',(-13.2086512544729,-69.2146842833506,
0.));
#132987=CARTESIAN_POINT('Ctrl Pts',(-13.1992729368928,-69.1962762870524,
0.));
#132988=CARTESIAN_POINT('Ctrl Pts',(-13.1899371268689,-69.1779039736026,
0.));
#132989=CARTESIAN_POINT('Ctrl Pts',(-13.1806438286944,-69.1595675305294,
0.));
#132990=CARTESIAN_POINT('Ctrl Pts',(-13.1713930465142,-69.141267145461,
0.));
#132991=CARTESIAN_POINT('Ctrl Pts',(-13.1621847844533,-69.1230030082597,
0.));
#132992=CARTESIAN_POINT('Ctrl Pts',(-13.1530190467181,-69.1047753127633,
0.));
#132993=CARTESIAN_POINT('Ctrl Pts',(-13.1438958377397,-69.0865842593063,
0.));
#132994=CARTESIAN_POINT('Ctrl Pts',(-13.1348151621824,-69.0684300549426,
0.));
#132995=CARTESIAN_POINT('Ctrl Pts',(-13.1257770246378,-69.0503129081778,
0.));
#132996=CARTESIAN_POINT('Ctrl Pts',(-13.1167814293495,-69.0322330243336,
0.));
#132997=CARTESIAN_POINT('Ctrl Pts',(-13.1078283799726,-69.0141906015137,
0.));
#132998=CARTESIAN_POINT('Ctrl Pts',(-13.0989178791843,-68.9961858241577,
0.));
#132999=CARTESIAN_POINT('Ctrl Pts',(-13.0900499290541,-68.9782188692654,
0.));
#133000=CARTESIAN_POINT('Ctrl Pts',(-13.0812245317816,-68.9602899187628,
0.));
#133001=CARTESIAN_POINT('Ctrl Pts',(-13.072441690283,-68.9423991694493,
0.));
#133002=CARTESIAN_POINT('Ctrl Pts',(-13.0637014089018,-68.9245468449865,
0.));
#133003=CARTESIAN_POINT('Ctrl Pts',(-13.0550036938793,-68.9067332040842,
0.));
#133004=CARTESIAN_POINT('Ctrl Pts',(-13.0463485518185,-68.8889585151431,
0.));
#133005=CARTESIAN_POINT('Ctrl Pts',(-13.0377359881863,-68.8712230321823,
0.));
#133006=CARTESIAN_POINT('Ctrl Pts',(-13.0291660060118,-68.8535269726871,
0.));
#133007=CARTESIAN_POINT('Ctrl Pts',(-13.0206386039729,-68.835870488774,
0.));
#133008=CARTESIAN_POINT('Ctrl Pts',(-13.0121537769003,-68.8182536654067,
0.));
#133009=CARTESIAN_POINT('Ctrl Pts',(-13.0053999700929,-68.8041919669403,
0.));
#133010=CARTESIAN_POINT('Ctrl Pts',(-13.0003537683089,-68.7936635625788,
0.));
#133011=CARTESIAN_POINT('Ctrl Pts',(-12.996998146029,-68.7866525680284,
0.));
#133012=CARTESIAN_POINT('Ctrl Pts',(-12.9953224629497,-68.7831490561748,
0.));
#133013=CARTESIAN_POINT('Ctrl Pts',(-21.8059378310719,-71.2372871136136,
0.));
#133014=CARTESIAN_POINT('Ctrl Pts',(-21.8059378310719,-71.2372871136136,
12.));
#133015=CARTESIAN_POINT('Ctrl Pts',(-21.8022104901727,-71.2331134397872,
0.));
#133016=CARTESIAN_POINT('Ctrl Pts',(-21.8022104901727,-71.2331134397872,
12.));
#133017=CARTESIAN_POINT('Ctrl Pts',(-21.7947599798961,-71.2247670210176,
0.));
#133018=CARTESIAN_POINT('Ctrl Pts',(-21.7947599798961,-71.2247670210176,
12.));
#133019=CARTESIAN_POINT('Ctrl Pts',(-21.7835967290463,-71.2122501795138,
0.));
#133020=CARTESIAN_POINT('Ctrl Pts',(-21.7835967290463,-71.2122501795138,
12.));
#133021=CARTESIAN_POINT('Ctrl Pts',(-21.7687374247288,-71.1955666310295,
0.));
#133022=CARTESIAN_POINT('Ctrl Pts',(-21.7687374247288,-71.1955666310295,
12.));
#133023=CARTESIAN_POINT('Ctrl Pts',(-21.750205018381,-71.1747214906585,
0.));
#133024=CARTESIAN_POINT('Ctrl Pts',(-21.750205018381,-71.1747214906585,
12.));
#133025=CARTESIAN_POINT('Ctrl Pts',(-21.7317143472952,-71.1538856612261,
0.));
#133026=CARTESIAN_POINT('Ctrl Pts',(-21.7317143472952,-71.1538856612261,
12.));
#133027=CARTESIAN_POINT('Ctrl Pts',(-21.7132654262531,-71.1330591726506,
0.));
#133028=CARTESIAN_POINT('Ctrl Pts',(-21.7132654262531,-71.1330591726506,
12.));
#133029=CARTESIAN_POINT('Ctrl Pts',(-21.694858273085,-71.1122420728217,
0.));
#133030=CARTESIAN_POINT('Ctrl Pts',(-21.694858273085,-71.1122420728217,
12.));
#133031=CARTESIAN_POINT('Ctrl Pts',(-21.6764929081677,-71.0914344332798,
0.));
#133032=CARTESIAN_POINT('Ctrl Pts',(-21.6764929081677,-71.0914344332798,
12.));
#133033=CARTESIAN_POINT('Ctrl Pts',(-21.6581693538335,-71.0706363472704,
0.));
#133034=CARTESIAN_POINT('Ctrl Pts',(-21.6581693538335,-71.0706363472704,
12.));
#133035=CARTESIAN_POINT('Ctrl Pts',(-21.6398876337141,-71.0498479219467,
0.));
#133036=CARTESIAN_POINT('Ctrl Pts',(-21.6398876337141,-71.0498479219467,
12.));
#133037=CARTESIAN_POINT('Ctrl Pts',(-21.6216477720913,-71.0290692721847,
0.));
#133038=CARTESIAN_POINT('Ctrl Pts',(-21.6216477720913,-71.0290692721847,
12.));
#133039=CARTESIAN_POINT('Ctrl Pts',(-21.6034497932581,-71.0083005139107,
0.));
#133040=CARTESIAN_POINT('Ctrl Pts',(-21.6034497932581,-71.0083005139107,
12.));
#133041=CARTESIAN_POINT('Ctrl Pts',(-21.585293720829,-70.987541757223,0.));
#133042=CARTESIAN_POINT('Ctrl Pts',(-21.585293720829,-70.987541757223,12.));
#133043=CARTESIAN_POINT('Ctrl Pts',(-21.5671795771914,-70.9667931008215,
0.));
#133044=CARTESIAN_POINT('Ctrl Pts',(-21.5671795771914,-70.9667931008215,
12.));
#133045=CARTESIAN_POINT('Ctrl Pts',(-21.5491073839106,-70.94605463587,0.));
#133046=CARTESIAN_POINT('Ctrl Pts',(-21.5491073839106,-70.94605463587,12.));
#133047=CARTESIAN_POINT('Ctrl Pts',(-21.5310771620231,-70.9253264487636,
0.));
#133048=CARTESIAN_POINT('Ctrl Pts',(-21.5310771620231,-70.9253264487636,
12.));
#133049=CARTESIAN_POINT('Ctrl Pts',(-21.513088932377,-70.9046086244131,
0.));
#133050=CARTESIAN_POINT('Ctrl Pts',(-21.513088932377,-70.9046086244131,
12.));
#133051=CARTESIAN_POINT('Ctrl Pts',(-21.4951427159262,-70.8839012490871,
0.));
#133052=CARTESIAN_POINT('Ctrl Pts',(-21.4951427159262,-70.8839012490871,
12.));
#133053=CARTESIAN_POINT('Ctrl Pts',(-21.477238534096,-70.8632044140112,
0.));
#133054=CARTESIAN_POINT('Ctrl Pts',(-21.477238534096,-70.8632044140112,
12.));
#133055=CARTESIAN_POINT('Ctrl Pts',(-21.4593764087474,-70.8425182149846,
0.));
#133056=CARTESIAN_POINT('Ctrl Pts',(-21.4593764087474,-70.8425182149846,
12.));
#133057=CARTESIAN_POINT('Ctrl Pts',(-21.4415563620114,-70.8218427507506,
0.));
#133058=CARTESIAN_POINT('Ctrl Pts',(-21.4415563620114,-70.8218427507506,
12.));
#133059=CARTESIAN_POINT('Ctrl Pts',(-21.4237784161588,-70.8011781217394,
0.));
#133060=CARTESIAN_POINT('Ctrl Pts',(-21.4237784161588,-70.8011781217394,
12.));
#133061=CARTESIAN_POINT('Ctrl Pts',(-21.4060425934599,-70.780524428745,
0.));
#133062=CARTESIAN_POINT('Ctrl Pts',(-21.4060425934599,-70.780524428745,
12.));
#133063=CARTESIAN_POINT('Ctrl Pts',(-21.3883489160196,-70.7598817714105,
0.));
#133064=CARTESIAN_POINT('Ctrl Pts',(-21.3883489160196,-70.7598817714105,
12.));
#133065=CARTESIAN_POINT('Ctrl Pts',(-21.3706974057039,-70.7392502475469,
0.));
#133066=CARTESIAN_POINT('Ctrl Pts',(-21.3706974057039,-70.7392502475469,
12.));
#133067=CARTESIAN_POINT('Ctrl Pts',(-21.3530880842349,-70.7186299539724,
0.));
#133068=CARTESIAN_POINT('Ctrl Pts',(-21.3530880842349,-70.7186299539724,
12.));
#133069=CARTESIAN_POINT('Ctrl Pts',(-21.3355209732443,-70.6980209870045,
0.));
#133070=CARTESIAN_POINT('Ctrl Pts',(-21.3355209732443,-70.6980209870045,
12.));
#133071=CARTESIAN_POINT('Ctrl Pts',(-21.3179960943389,-70.6774234430897,
0.));
#133072=CARTESIAN_POINT('Ctrl Pts',(-21.3179960943389,-70.6774234430897,
12.));
#133073=CARTESIAN_POINT('Ctrl Pts',(-21.300513469156,-70.6568374193774,
0.));
#133074=CARTESIAN_POINT('Ctrl Pts',(-21.300513469156,-70.6568374193774,
12.));
#133075=CARTESIAN_POINT('Ctrl Pts',(-21.2830731194183,-70.6362630143047,
0.));
#133076=CARTESIAN_POINT('Ctrl Pts',(-21.2830731194183,-70.6362630143047,
12.));
#133077=CARTESIAN_POINT('Ctrl Pts',(-21.2656750669126,-70.6157003273316,
0.));
#133078=CARTESIAN_POINT('Ctrl Pts',(-21.2656750669126,-70.6157003273316,
12.));
#133079=CARTESIAN_POINT('Ctrl Pts',(-21.2483193334676,-70.5951494586957,
0.));
#133080=CARTESIAN_POINT('Ctrl Pts',(-21.2483193334676,-70.5951494586957,
12.));
#133081=CARTESIAN_POINT('Ctrl Pts',(-21.2310059409266,-70.5746105091502,
0.));
#133082=CARTESIAN_POINT('Ctrl Pts',(-21.2310059409266,-70.5746105091502,
12.));
#133083=CARTESIAN_POINT('Ctrl Pts',(-21.2137349111208,-70.5540835797283,
0.));
#133084=CARTESIAN_POINT('Ctrl Pts',(-21.2137349111208,-70.5540835797283,
12.));
#133085=CARTESIAN_POINT('Ctrl Pts',(-21.1965062658298,-70.5335687714428,
0.));
#133086=CARTESIAN_POINT('Ctrl Pts',(-21.1965062658298,-70.5335687714428,
12.));
#133087=CARTESIAN_POINT('Ctrl Pts',(-21.1793200267847,-70.5130661852955,
0.));
#133088=CARTESIAN_POINT('Ctrl Pts',(-21.1793200267847,-70.5130661852955,
12.));
#133089=CARTESIAN_POINT('Ctrl Pts',(-21.1621762156897,-70.4925759224216,
0.));
#133090=CARTESIAN_POINT('Ctrl Pts',(-21.1621762156897,-70.4925759224216,
12.));
#133091=CARTESIAN_POINT('Ctrl Pts',(-21.1450748542337,-70.4720980841939,
0.));
#133092=CARTESIAN_POINT('Ctrl Pts',(-21.1450748542337,-70.4720980841939,
12.));
#133093=CARTESIAN_POINT('Ctrl Pts',(-21.1280159641003,-70.4516327723346,
0.));
#133094=CARTESIAN_POINT('Ctrl Pts',(-21.1280159641003,-70.4516327723346,
12.));
#133095=CARTESIAN_POINT('Ctrl Pts',(-21.1109995669747,-70.4311800890401,
0.));
#133096=CARTESIAN_POINT('Ctrl Pts',(-21.1109995669747,-70.4311800890401,
12.));
#133097=CARTESIAN_POINT('Ctrl Pts',(-21.0940256845473,-70.4107401370389,
0.));
#133098=CARTESIAN_POINT('Ctrl Pts',(-21.0940256845473,-70.4107401370389,
12.));
#133099=CARTESIAN_POINT('Ctrl Pts',(-21.0770943385141,-70.3903130195265,
0.));
#133100=CARTESIAN_POINT('Ctrl Pts',(-21.0770943385141,-70.3903130195265,
12.));
#133101=CARTESIAN_POINT('Ctrl Pts',(-21.0602055505748,-70.3698988401281,
0.));
#133102=CARTESIAN_POINT('Ctrl Pts',(-21.0602055505748,-70.3698988401281,
12.));
#133103=CARTESIAN_POINT('Ctrl Pts',(-21.0433593424267,-70.3494977028498,
0.));
#133104=CARTESIAN_POINT('Ctrl Pts',(-21.0433593424267,-70.3494977028498,
12.));
#133105=CARTESIAN_POINT('Ctrl Pts',(-21.0265557357548,-70.3291097120302,
0.));
#133106=CARTESIAN_POINT('Ctrl Pts',(-21.0265557357548,-70.3291097120302,
12.));
#133107=CARTESIAN_POINT('Ctrl Pts',(-21.0097947522218,-70.3087349722973,
0.));
#133108=CARTESIAN_POINT('Ctrl Pts',(-21.0097947522218,-70.3087349722973,
12.));
#133109=CARTESIAN_POINT('Ctrl Pts',(-20.9930764134776,-70.2883735885984,
0.));
#133110=CARTESIAN_POINT('Ctrl Pts',(-20.9930764134776,-70.2883735885984,
12.));
#133111=CARTESIAN_POINT('Ctrl Pts',(-20.9764007411653,-70.2680256662224,
0.));
#133112=CARTESIAN_POINT('Ctrl Pts',(-20.9764007411653,-70.2680256662224,
12.));
#133113=CARTESIAN_POINT('Ctrl Pts',(-20.9597677569228,-70.2476913108244,
0.));
#133114=CARTESIAN_POINT('Ctrl Pts',(-20.9597677569228,-70.2476913108244,
12.));
#133115=CARTESIAN_POINT('Ctrl Pts',(-20.9431774823831,-70.2273706284472,
0.));
#133116=CARTESIAN_POINT('Ctrl Pts',(-20.9431774823831,-70.2273706284472,
12.));
#133117=CARTESIAN_POINT('Ctrl Pts',(-20.9266299391684,-70.2070637255458,
0.));
#133118=CARTESIAN_POINT('Ctrl Pts',(-20.9266299391684,-70.2070637255458,
12.));
#133119=CARTESIAN_POINT('Ctrl Pts',(-20.9101251488944,-70.1867707089854,
0.));
#133120=CARTESIAN_POINT('Ctrl Pts',(-20.9101251488944,-70.1867707089854,
12.));
#133121=CARTESIAN_POINT('Ctrl Pts',(-20.8936631331748,-70.1664916860358,
0.));
#133122=CARTESIAN_POINT('Ctrl Pts',(-20.8936631331748,-70.1664916860358,
12.));
#133123=CARTESIAN_POINT('Ctrl Pts',(-20.8772439136206,-70.1462267643646,
0.));
#133124=CARTESIAN_POINT('Ctrl Pts',(-20.8772439136206,-70.1462267643646,
12.));
#133125=CARTESIAN_POINT('Ctrl Pts',(-20.8608675118379,-70.1259760520309,
0.));
#133126=CARTESIAN_POINT('Ctrl Pts',(-20.8608675118379,-70.1259760520309,
12.));
#133127=CARTESIAN_POINT('Ctrl Pts',(-20.8445339494188,-70.1057396574747,
0.));
#133128=CARTESIAN_POINT('Ctrl Pts',(-20.8445339494188,-70.1057396574747,
12.));
#133129=CARTESIAN_POINT('Ctrl Pts',(-20.8282432479429,-70.0855176895191,
0.));
#133130=CARTESIAN_POINT('Ctrl Pts',(-20.8282432479429,-70.0855176895191,
12.));
#133131=CARTESIAN_POINT('Ctrl Pts',(-20.8119954289849,-70.0653102573803,
0.));
#133132=CARTESIAN_POINT('Ctrl Pts',(-20.8119954289849,-70.0653102573803,
12.));
#133133=CARTESIAN_POINT('Ctrl Pts',(-20.7957905141157,-70.0451174706741,
0.));
#133134=CARTESIAN_POINT('Ctrl Pts',(-20.7957905141157,-70.0451174706741,
12.));
#133135=CARTESIAN_POINT('Ctrl Pts',(-20.7796285249022,-70.024939439422,
0.));
#133136=CARTESIAN_POINT('Ctrl Pts',(-20.7796285249022,-70.024939439422,
12.));
#133137=CARTESIAN_POINT('Ctrl Pts',(-20.7635094829016,-70.0047762740568,
0.));
#133138=CARTESIAN_POINT('Ctrl Pts',(-20.7635094829016,-70.0047762740568,
12.));
#133139=CARTESIAN_POINT('Ctrl Pts',(-20.7474334096581,-69.9846280854257,
0.));
#133140=CARTESIAN_POINT('Ctrl Pts',(-20.7474334096581,-69.9846280854257,
12.));
#133141=CARTESIAN_POINT('Ctrl Pts',(-20.7314003267119,-69.9644949847934,
0.));
#133142=CARTESIAN_POINT('Ctrl Pts',(-20.7314003267119,-69.9644949847934,
12.));
#133143=CARTESIAN_POINT('Ctrl Pts',(-20.7154102555997,-69.9443770838448,
0.));
#133144=CARTESIAN_POINT('Ctrl Pts',(-20.7154102555997,-69.9443770838448,
12.));
#133145=CARTESIAN_POINT('Ctrl Pts',(-20.6994632178552,-69.9242744946854,
0.));
#133146=CARTESIAN_POINT('Ctrl Pts',(-20.6994632178552,-69.9242744946854,
12.));
#133147=CARTESIAN_POINT('Ctrl Pts',(-20.683559235003,-69.904187329841,0.));
#133148=CARTESIAN_POINT('Ctrl Pts',(-20.683559235003,-69.904187329841,12.));
#133149=CARTESIAN_POINT('Ctrl Pts',(-20.667698328554,-69.8841157022568,
0.));
#133150=CARTESIAN_POINT('Ctrl Pts',(-20.667698328554,-69.8841157022568,
12.));
#133151=CARTESIAN_POINT('Ctrl Pts',(-20.6518805200129,-69.8640597253045,
0.));
#133152=CARTESIAN_POINT('Ctrl Pts',(-20.6518805200129,-69.8640597253045,
12.));
#133153=CARTESIAN_POINT('Ctrl Pts',(-20.6361058308811,-69.8440195127866,
0.));
#133154=CARTESIAN_POINT('Ctrl Pts',(-20.6361058308811,-69.8440195127866,
12.));
#133155=CARTESIAN_POINT('Ctrl Pts',(-20.6203742826566,-69.8239951789402,
0.));
#133156=CARTESIAN_POINT('Ctrl Pts',(-20.6203742826566,-69.8239951789402,
12.));
#133157=CARTESIAN_POINT('Ctrl Pts',(-20.6046858968308,-69.8039868384389,
0.));
#133158=CARTESIAN_POINT('Ctrl Pts',(-20.6046858968308,-69.8039868384389,
12.));
#133159=CARTESIAN_POINT('Ctrl Pts',(-20.5890406948811,-69.7839946063949,
0.));
#133160=CARTESIAN_POINT('Ctrl Pts',(-20.5890406948811,-69.7839946063949,
12.));
#133161=CARTESIAN_POINT('Ctrl Pts',(-20.5734386982783,-69.7640185983644,
0.));
#133162=CARTESIAN_POINT('Ctrl Pts',(-20.5734386982783,-69.7640185983644,
12.));
#133163=CARTESIAN_POINT('Ctrl Pts',(-20.5578799284898,-69.744058930351,
0.));
#133164=CARTESIAN_POINT('Ctrl Pts',(-20.5578799284898,-69.744058930351,
12.));
#133165=CARTESIAN_POINT('Ctrl Pts',(-20.54236440698,-69.7241157188083,0.));
#133166=CARTESIAN_POINT('Ctrl Pts',(-20.54236440698,-69.7241157188083,12.));
#133167=CARTESIAN_POINT('Ctrl Pts',(-20.5268921552077,-69.7041890806425,
0.));
#133168=CARTESIAN_POINT('Ctrl Pts',(-20.5268921552077,-69.7041890806425,
12.));
#133169=CARTESIAN_POINT('Ctrl Pts',(-20.5114631946185,-69.6842791332115,
0.));
#133170=CARTESIAN_POINT('Ctrl Pts',(-20.5114631946185,-69.6842791332115,
12.));
#133171=CARTESIAN_POINT('Ctrl Pts',(-20.4960775466492,-69.6643859943308,
0.));
#133172=CARTESIAN_POINT('Ctrl Pts',(-20.4960775466492,-69.6643859943308,
12.));
#133173=CARTESIAN_POINT('Ctrl Pts',(-20.480735232734,-69.6445097822792,
0.));
#133174=CARTESIAN_POINT('Ctrl Pts',(-20.480735232734,-69.6445097822792,
12.));
#133175=CARTESIAN_POINT('Ctrl Pts',(-20.4654362743037,-69.6246506158013,
0.));
#133176=CARTESIAN_POINT('Ctrl Pts',(-20.4654362743037,-69.6246506158013,
12.));
#133177=CARTESIAN_POINT('Ctrl Pts',(-20.4501806927852,-69.6048086141113,
0.));
#133178=CARTESIAN_POINT('Ctrl Pts',(-20.4501806927852,-69.6048086141113,
12.));
#133179=CARTESIAN_POINT('Ctrl Pts',(-20.4349685095924,-69.5849838968928,
0.));
#133180=CARTESIAN_POINT('Ctrl Pts',(-20.4349685095924,-69.5849838968928,
12.));
#133181=CARTESIAN_POINT('Ctrl Pts',(-20.4197997461301,-69.5651765843033,
0.));
#133182=CARTESIAN_POINT('Ctrl Pts',(-20.4197997461301,-69.5651765843033,
12.));
#133183=CARTESIAN_POINT('Ctrl Pts',(-20.4046744237999,-69.5453867969804,
0.));
#133184=CARTESIAN_POINT('Ctrl Pts',(-20.4046744237999,-69.5453867969804,
12.));
#133185=CARTESIAN_POINT('Ctrl Pts',(-20.3895925640005,-69.5256146560441,
0.));
#133186=CARTESIAN_POINT('Ctrl Pts',(-20.3895925640005,-69.5256146560441,
12.));
#133187=CARTESIAN_POINT('Ctrl Pts',(-20.3745541881269,-69.5058602831008,
0.));
#133188=CARTESIAN_POINT('Ctrl Pts',(-20.3745541881269,-69.5058602831008,
12.));
#133189=CARTESIAN_POINT('Ctrl Pts',(-20.3595593175623,-69.4861238002441,
0.));
#133190=CARTESIAN_POINT('Ctrl Pts',(-20.3595593175623,-69.4861238002441,
12.));
#133191=CARTESIAN_POINT('Ctrl Pts',(-20.3446079736802,-69.4664053300587,
0.));
#133192=CARTESIAN_POINT('Ctrl Pts',(-20.3446079736802,-69.4664053300587,
12.));
#133193=CARTESIAN_POINT('Ctrl Pts',(-20.3297001778507,-69.4467049956262,
0.));
#133194=CARTESIAN_POINT('Ctrl Pts',(-20.3297001778507,-69.4467049956262,
12.));
#133195=CARTESIAN_POINT('Ctrl Pts',(-20.3148359514415,-69.4270229205297,
0.));
#133196=CARTESIAN_POINT('Ctrl Pts',(-20.3148359514415,-69.4270229205297,
12.));
#133197=CARTESIAN_POINT('Ctrl Pts',(-20.3000153158167,-69.407359228856,
0.));
#133198=CARTESIAN_POINT('Ctrl Pts',(-20.3000153158167,-69.407359228856,
12.));
#133199=CARTESIAN_POINT('Ctrl Pts',(-20.2852382923299,-69.3877140451975,
0.));
#133200=CARTESIAN_POINT('Ctrl Pts',(-20.2852382923299,-69.3877140451975,
12.));
#133201=CARTESIAN_POINT('Ctrl Pts',(-20.2705049023241,-69.368087494655,
0.));
#133202=CARTESIAN_POINT('Ctrl Pts',(-20.2705049023241,-69.368087494655,
12.));
#133203=CARTESIAN_POINT('Ctrl Pts',(-20.2558151671391,-69.3484797028458,
0.));
#133204=CARTESIAN_POINT('Ctrl Pts',(-20.2558151671391,-69.3484797028458,
12.));
#133205=CARTESIAN_POINT('Ctrl Pts',(-20.2411691081123,-69.3288907959067,
0.));
#133206=CARTESIAN_POINT('Ctrl Pts',(-20.2411691081123,-69.3288907959067,
12.));
#133207=CARTESIAN_POINT('Ctrl Pts',(-20.2265667465784,-69.3093209004984,
0.));
#133208=CARTESIAN_POINT('Ctrl Pts',(-20.2265667465784,-69.3093209004984,
12.));
#133209=CARTESIAN_POINT('Ctrl Pts',(-20.2120081038621,-69.2897701438059,
0.));
#133210=CARTESIAN_POINT('Ctrl Pts',(-20.2120081038621,-69.2897701438059,
12.));
#133211=CARTESIAN_POINT('Ctrl Pts',(-20.1974932012773,-69.2702386535422,
0.));
#133212=CARTESIAN_POINT('Ctrl Pts',(-20.1974932012773,-69.2702386535422,
12.));
#133213=CARTESIAN_POINT('Ctrl Pts',(-20.1830220601349,-69.2507265579554,
0.));
#133214=CARTESIAN_POINT('Ctrl Pts',(-20.1830220601349,-69.2507265579554,
12.));
#133215=CARTESIAN_POINT('Ctrl Pts',(-20.1685947017433,-69.2312339858335,
0.));
#133216=CARTESIAN_POINT('Ctrl Pts',(-20.1685947017433,-69.2312339858335,
12.));
#133217=CARTESIAN_POINT('Ctrl Pts',(-20.1542111474087,-69.2117610665076,
0.));
#133218=CARTESIAN_POINT('Ctrl Pts',(-20.1542111474087,-69.2117610665076,
12.));
#133219=CARTESIAN_POINT('Ctrl Pts',(-20.139871418428,-69.1923079298538,
0.));
#133220=CARTESIAN_POINT('Ctrl Pts',(-20.139871418428,-69.1923079298538,
12.));
#133221=CARTESIAN_POINT('Ctrl Pts',(-20.1255755360872,-69.1728747062963,
0.));
#133222=CARTESIAN_POINT('Ctrl Pts',(-20.1255755360872,-69.1728747062963,
12.));
#133223=CARTESIAN_POINT('Ctrl Pts',(-20.1113235216694,-69.1534615268152,
0.));
#133224=CARTESIAN_POINT('Ctrl Pts',(-20.1113235216694,-69.1534615268152,
12.));
#133225=CARTESIAN_POINT('Ctrl Pts',(-20.0971153964557,-69.1340685229514,
0.));
#133226=CARTESIAN_POINT('Ctrl Pts',(-20.0971153964557,-69.1340685229514,
12.));
#133227=CARTESIAN_POINT('Ctrl Pts',(-20.0829511817251,-69.1146958268104,
0.));
#133228=CARTESIAN_POINT('Ctrl Pts',(-20.0829511817251,-69.1146958268104,
12.));
#133229=CARTESIAN_POINT('Ctrl Pts',(-20.068830898748,-69.095343571064,0.));
#133230=CARTESIAN_POINT('Ctrl Pts',(-20.068830898748,-69.095343571064,12.));
#133231=CARTESIAN_POINT('Ctrl Pts',(-20.0547545687842,-69.0760118889535,
0.));
#133232=CARTESIAN_POINT('Ctrl Pts',(-20.0547545687842,-69.0760118889535,
12.));
#133233=CARTESIAN_POINT('Ctrl Pts',(-20.0407222130906,-69.0567009142978,
0.));
#133234=CARTESIAN_POINT('Ctrl Pts',(-20.0407222130906,-69.0567009142978,
12.));
#133235=CARTESIAN_POINT('Ctrl Pts',(-20.0267338529223,-69.0374107814984,
0.));
#133236=CARTESIAN_POINT('Ctrl Pts',(-20.0267338529223,-69.0374107814984,
12.));
#133237=CARTESIAN_POINT('Ctrl Pts',(-20.0127895095327,-69.0181416255431,
0.));
#133238=CARTESIAN_POINT('Ctrl Pts',(-20.0127895095327,-69.0181416255431,
12.));
#133239=CARTESIAN_POINT('Ctrl Pts',(-19.9988892041666,-68.9988935820084,
0.));
#133240=CARTESIAN_POINT('Ctrl Pts',(-19.9988892041666,-68.9988935820084,
12.));
#133241=CARTESIAN_POINT('Ctrl Pts',(-19.9850329580591,-68.9796667870638,
0.));
#133242=CARTESIAN_POINT('Ctrl Pts',(-19.9850329580591,-68.9796667870638,
12.));
#133243=CARTESIAN_POINT('Ctrl Pts',(-19.9712207924429,-68.9604613774802,
0.));
#133244=CARTESIAN_POINT('Ctrl Pts',(-19.9712207924429,-68.9604613774802,
12.));
#133245=CARTESIAN_POINT('Ctrl Pts',(-19.9574527285488,-68.9412774906333,
0.));
#133246=CARTESIAN_POINT('Ctrl Pts',(-19.9574527285488,-68.9412774906333,
12.));
#133247=CARTESIAN_POINT('Ctrl Pts',(-19.9437287876066,-68.9221152645095,
0.));
#133248=CARTESIAN_POINT('Ctrl Pts',(-19.9437287876066,-68.9221152645095,
12.));
#133249=CARTESIAN_POINT('Ctrl Pts',(-19.9300489908374,-68.9029748377067,
0.));
#133250=CARTESIAN_POINT('Ctrl Pts',(-19.9300489908374,-68.9029748377067,
12.));
#133251=CARTESIAN_POINT('Ctrl Pts',(-19.9164133594526,-68.8838563494393,
0.));
#133252=CARTESIAN_POINT('Ctrl Pts',(-19.9164133594526,-68.8838563494393,
12.));
#133253=CARTESIAN_POINT('Ctrl Pts',(-19.9028219146618,-68.8647599395469,
0.));
#133254=CARTESIAN_POINT('Ctrl Pts',(-19.9028219146618,-68.8647599395469,
12.));
#133255=CARTESIAN_POINT('Ctrl Pts',(-19.8892746776739,-68.8456857485002,
0.));
#133256=CARTESIAN_POINT('Ctrl Pts',(-19.8892746776739,-68.8456857485002,
12.));
#133257=CARTESIAN_POINT('Ctrl Pts',(-19.8757716696965,-68.8266339174056,
0.));
#133258=CARTESIAN_POINT('Ctrl Pts',(-19.8757716696965,-68.8266339174056,
12.));
#133259=CARTESIAN_POINT('Ctrl Pts',(-19.8623129119293,-68.8076045880065,
0.));
#133260=CARTESIAN_POINT('Ctrl Pts',(-19.8623129119293,-68.8076045880065,
12.));
#133261=CARTESIAN_POINT('Ctrl Pts',(-19.8488984255627,-68.7885979026878,
0.));
#133262=CARTESIAN_POINT('Ctrl Pts',(-19.8488984255627,-68.7885979026878,
12.));
#133263=CARTESIAN_POINT('Ctrl Pts',(-19.8355282317858,-68.7696140044851,
0.));
#133264=CARTESIAN_POINT('Ctrl Pts',(-19.8355282317858,-68.7696140044851,
12.));
#133265=CARTESIAN_POINT('Ctrl Pts',(-19.8222023517871,-68.7506530370904,
0.));
#133266=CARTESIAN_POINT('Ctrl Pts',(-19.8222023517871,-68.7506530370904,
12.));
#133267=CARTESIAN_POINT('Ctrl Pts',(-19.8089208067537,-68.7317151448573,
0.));
#133268=CARTESIAN_POINT('Ctrl Pts',(-19.8089208067537,-68.7317151448573,
12.));
#133269=CARTESIAN_POINT('Ctrl Pts',(-19.7956836178651,-68.7128004728033,
0.));
#133270=CARTESIAN_POINT('Ctrl Pts',(-19.7956836178651,-68.7128004728033,
12.));
#133271=CARTESIAN_POINT('Ctrl Pts',(-19.7824908062925,-68.6939091666149,
0.));
#133272=CARTESIAN_POINT('Ctrl Pts',(-19.7824908062925,-68.6939091666149,
12.));
#133273=CARTESIAN_POINT('Ctrl Pts',(-19.7693423932067,-68.6750413726574,
0.));
#133274=CARTESIAN_POINT('Ctrl Pts',(-19.7693423932067,-68.6750413726574,
12.));
#133275=CARTESIAN_POINT('Ctrl Pts',(-19.7562383997784,-68.65619723798,0.));
#133276=CARTESIAN_POINT('Ctrl Pts',(-19.7562383997784,-68.65619723798,12.));
#133277=CARTESIAN_POINT('Ctrl Pts',(-19.7431788471773,-68.6373769103211,
0.));
#133278=CARTESIAN_POINT('Ctrl Pts',(-19.7431788471773,-68.6373769103211,
12.));
#133279=CARTESIAN_POINT('Ctrl Pts',(-19.7301637565646,-68.6185805381102,
0.));
#133280=CARTESIAN_POINT('Ctrl Pts',(-19.7301637565646,-68.6185805381102,
12.));
#133281=CARTESIAN_POINT('Ctrl Pts',(-19.717193149095,-68.5998082704741,
0.));
#133282=CARTESIAN_POINT('Ctrl Pts',(-19.717193149095,-68.5998082704741,
12.));
#133283=CARTESIAN_POINT('Ctrl Pts',(-19.7042670459234,-68.5810602572474,
0.));
#133284=CARTESIAN_POINT('Ctrl Pts',(-19.7042670459234,-68.5810602572474,
12.));
#133285=CARTESIAN_POINT('Ctrl Pts',(-19.6913854682046,-68.5623366489776,
0.));
#133286=CARTESIAN_POINT('Ctrl Pts',(-19.6913854682046,-68.5623366489776,
12.));
#133287=CARTESIAN_POINT('Ctrl Pts',(-19.6785484370929,-68.543637596932,
0.));
#133288=CARTESIAN_POINT('Ctrl Pts',(-19.6785484370929,-68.543637596932,
12.));
#133289=CARTESIAN_POINT('Ctrl Pts',(-19.665755973734,-68.5249632530994,
0.));
#133290=CARTESIAN_POINT('Ctrl Pts',(-19.665755973734,-68.5249632530994,
12.));
#133291=CARTESIAN_POINT('Ctrl Pts',(-19.653008099269,-68.5063137701986,
0.));
#133292=CARTESIAN_POINT('Ctrl Pts',(-19.653008099269,-68.5063137701986,
12.));
#133293=CARTESIAN_POINT('Ctrl Pts',(-19.6403048348397,-68.4876893016863,
0.));
#133294=CARTESIAN_POINT('Ctrl Pts',(-19.6403048348397,-68.4876893016863,
12.));
#133295=CARTESIAN_POINT('Ctrl Pts',(-19.6276462015888,-68.4690900017631,
0.));
#133296=CARTESIAN_POINT('Ctrl Pts',(-19.6276462015888,-68.4690900017631,
12.));
#133297=CARTESIAN_POINT('Ctrl Pts',(-19.6150322206578,-68.4505160253777,
0.));
#133298=CARTESIAN_POINT('Ctrl Pts',(-19.6150322206578,-68.4505160253777,
12.));
#133299=CARTESIAN_POINT('Ctrl Pts',(-19.6024629131786,-68.4319675282273,
0.));
#133300=CARTESIAN_POINT('Ctrl Pts',(-19.6024629131786,-68.4319675282273,
12.));
#133301=CARTESIAN_POINT('Ctrl Pts',(-19.5899383002804,-68.4134446667695,
0.));
#133302=CARTESIAN_POINT('Ctrl Pts',(-19.5899383002804,-68.4134446667695,
12.));
#133303=CARTESIAN_POINT('Ctrl Pts',(-19.5774584030939,-68.3949475982334,
0.));
#133304=CARTESIAN_POINT('Ctrl Pts',(-19.5774584030939,-68.3949475982334,
12.));
#133305=CARTESIAN_POINT('Ctrl Pts',(-19.5650232427516,-68.3764764806287,
0.));
#133306=CARTESIAN_POINT('Ctrl Pts',(-19.5650232427516,-68.3764764806287,
12.));
#133307=CARTESIAN_POINT('Ctrl Pts',(-19.5526328403852,-68.3580314727522,
0.));
#133308=CARTESIAN_POINT('Ctrl Pts',(-19.5526328403852,-68.3580314727522,
12.));
#133309=CARTESIAN_POINT('Ctrl Pts',(-19.540287217119,-68.3396127341938,
0.));
#133310=CARTESIAN_POINT('Ctrl Pts',(-19.540287217119,-68.3396127341938,
12.));
#133311=CARTESIAN_POINT('Ctrl Pts',(-19.5279863940773,-68.3212204253415,
0.));
#133312=CARTESIAN_POINT('Ctrl Pts',(-19.5279863940773,-68.3212204253415,
12.));
#133313=CARTESIAN_POINT('Ctrl Pts',(-19.5157303923856,-68.3028547073862,
0.));
#133314=CARTESIAN_POINT('Ctrl Pts',(-19.5157303923856,-68.3028547073862,
12.));
#133315=CARTESIAN_POINT('Ctrl Pts',(-19.5035192331706,-68.2845157423234,
0.));
#133316=CARTESIAN_POINT('Ctrl Pts',(-19.5035192331706,-68.2845157423234,
12.));
#133317=CARTESIAN_POINT('Ctrl Pts',(-19.4913529375545,-68.2662036929531,
0.));
#133318=CARTESIAN_POINT('Ctrl Pts',(-19.4913529375545,-68.2662036929531,
12.));
#133319=CARTESIAN_POINT('Ctrl Pts',(-19.4792315266505,-68.2479187228815,
0.));
#133320=CARTESIAN_POINT('Ctrl Pts',(-19.4792315266505,-68.2479187228815,
12.));
#133321=CARTESIAN_POINT('Ctrl Pts',(-19.4671550215724,-68.2296609965461,
0.));
#133322=CARTESIAN_POINT('Ctrl Pts',(-19.4671550215724,-68.2296609965461,
12.));
#133323=CARTESIAN_POINT('Ctrl Pts',(-19.4551234434384,-68.2114306792366,
0.));
#133324=CARTESIAN_POINT('Ctrl Pts',(-19.4551234434384,-68.2114306792366,
12.));
#133325=CARTESIAN_POINT('Ctrl Pts',(-19.4431368133718,-68.1932279371121,
0.));
#133326=CARTESIAN_POINT('Ctrl Pts',(-19.4431368133718,-68.1932279371121,
12.));
#133327=CARTESIAN_POINT('Ctrl Pts',(-19.4311951524977,-68.1750529372211,
0.));
#133328=CARTESIAN_POINT('Ctrl Pts',(-19.4311951524977,-68.1750529372211,
12.));
#133329=CARTESIAN_POINT('Ctrl Pts',(-19.4192984819411,-68.1569058475026,
0.));
#133330=CARTESIAN_POINT('Ctrl Pts',(-19.4192984819411,-68.1569058475026,
12.));
#133331=CARTESIAN_POINT('Ctrl Pts',(-19.4074468228294,-68.1387868367668,
0.));
#133332=CARTESIAN_POINT('Ctrl Pts',(-19.4074468228294,-68.1387868367668,
12.));
#133333=CARTESIAN_POINT('Ctrl Pts',(-19.3956401962893,-68.1206960746763,
0.));
#133334=CARTESIAN_POINT('Ctrl Pts',(-19.3956401962893,-68.1206960746763,
12.));
#133335=CARTESIAN_POINT('Ctrl Pts',(-19.3838786234426,-68.1026337317298,
0.));
#133336=CARTESIAN_POINT('Ctrl Pts',(-19.3838786234426,-68.1026337317298,
12.));
#133337=CARTESIAN_POINT('Ctrl Pts',(-19.3721621253921,-68.0845999792274,
0.));
#133338=CARTESIAN_POINT('Ctrl Pts',(-19.3721621253921,-68.0845999792274,
12.));
#133339=CARTESIAN_POINT('Ctrl Pts',(-19.3604907232322,-68.0665949893222,
0.));
#133340=CARTESIAN_POINT('Ctrl Pts',(-19.3604907232322,-68.0665949893222,
12.));
#133341=CARTESIAN_POINT('Ctrl Pts',(-19.3488644380646,-68.0486189351027,
0.));
#133342=CARTESIAN_POINT('Ctrl Pts',(-19.3488644380646,-68.0486189351027,
12.));
#133343=CARTESIAN_POINT('Ctrl Pts',(-19.3372832910077,-68.0306719906636,
0.));
#133344=CARTESIAN_POINT('Ctrl Pts',(-19.3372832910077,-68.0306719906636,
12.));
#133345=CARTESIAN_POINT('Ctrl Pts',(-19.3257473032031,-68.0127543311761,
0.));
#133346=CARTESIAN_POINT('Ctrl Pts',(-19.3257473032031,-68.0127543311761,
12.));
#133347=CARTESIAN_POINT('Ctrl Pts',(-19.3142564958196,-67.9948661329591,
0.));
#133348=CARTESIAN_POINT('Ctrl Pts',(-19.3142564958196,-67.9948661329591,
12.));
#133349=CARTESIAN_POINT('Ctrl Pts',(-19.3028108900374,-67.977007573346,
0.));
#133350=CARTESIAN_POINT('Ctrl Pts',(-19.3028108900374,-67.977007573346,
12.));
#133351=CARTESIAN_POINT('Ctrl Pts',(-19.2914105070283,-67.959178830538,
0.));
#133352=CARTESIAN_POINT('Ctrl Pts',(-19.2914105070283,-67.959178830538,
12.));
#133353=CARTESIAN_POINT('Ctrl Pts',(-19.2800553679362,-67.9413800834798,
0.));
#133354=CARTESIAN_POINT('Ctrl Pts',(-19.2800553679362,-67.9413800834798,
12.));
#133355=CARTESIAN_POINT('Ctrl Pts',(-19.2687454938449,-67.9236115116781,
0.));
#133356=CARTESIAN_POINT('Ctrl Pts',(-19.2687454938449,-67.9236115116781,
12.));
#133357=CARTESIAN_POINT('Ctrl Pts',(-19.2574809057705,-67.9058732951822,
0.));
#133358=CARTESIAN_POINT('Ctrl Pts',(-19.2574809057705,-67.9058732951822,
12.));
#133359=CARTESIAN_POINT('Ctrl Pts',(-19.2462616247287,-67.8881656149983,
0.));
#133360=CARTESIAN_POINT('Ctrl Pts',(-19.2462616247287,-67.8881656149983,
12.));
#133361=CARTESIAN_POINT('Ctrl Pts',(-19.2350876717878,-67.8704886534555,
0.));
#133362=CARTESIAN_POINT('Ctrl Pts',(-19.2350876717878,-67.8704886534555,
12.));
#133363=CARTESIAN_POINT('Ctrl Pts',(-19.223959068113,-67.852842594517,0.));
#133364=CARTESIAN_POINT('Ctrl Pts',(-19.223959068113,-67.852842594517,12.));
#133365=CARTESIAN_POINT('Ctrl Pts',(-19.2128758350336,-67.8352276242856,
0.));
#133366=CARTESIAN_POINT('Ctrl Pts',(-19.2128758350336,-67.8352276242856,
12.));
#133367=CARTESIAN_POINT('Ctrl Pts',(-19.2018379939918,-67.817643930658,
0.));
#133368=CARTESIAN_POINT('Ctrl Pts',(-19.2018379939918,-67.817643930658,
12.));
#133369=CARTESIAN_POINT('Ctrl Pts',(-19.1908455664089,-67.8000917023896,
0.));
#133370=CARTESIAN_POINT('Ctrl Pts',(-19.1908455664089,-67.8000917023896,
12.));
#133371=CARTESIAN_POINT('Ctrl Pts',(-19.1798985735687,-67.7825711283092,
0.));
#133372=CARTESIAN_POINT('Ctrl Pts',(-19.1798985735687,-67.7825711283092,
12.));
#133373=CARTESIAN_POINT('Ctrl Pts',(-19.1689970364959,-67.7650823965156,
0.));
#133374=CARTESIAN_POINT('Ctrl Pts',(-19.1689970364959,-67.7650823965156,
12.));
#133375=CARTESIAN_POINT('Ctrl Pts',(-19.1581409758112,-67.7476256934492,
0.));
#133376=CARTESIAN_POINT('Ctrl Pts',(-19.1581409758112,-67.7476256934492,
12.));
#133377=CARTESIAN_POINT('Ctrl Pts',(-19.1473304119969,-67.7302012056629,
0.));
#133378=CARTESIAN_POINT('Ctrl Pts',(-19.1473304119969,-67.7302012056629,
12.));
#133379=CARTESIAN_POINT('Ctrl Pts',(-19.1365653657098,-67.7128091219372,
0.));
#133380=CARTESIAN_POINT('Ctrl Pts',(-19.1365653657098,-67.7128091219372,
12.));
#133381=CARTESIAN_POINT('Ctrl Pts',(-19.1258458580343,-67.6954496350053,
0.));
#133382=CARTESIAN_POINT('Ctrl Pts',(-19.1258458580343,-67.6954496350053,
12.));
#133383=CARTESIAN_POINT('Ctrl Pts',(-19.115171910845,-67.6781229440535,
0.));
#133384=CARTESIAN_POINT('Ctrl Pts',(-19.115171910845,-67.6781229440535,
12.));
#133385=CARTESIAN_POINT('Ctrl Pts',(-19.1045435468345,-67.6608292549412,
0.));
#133386=CARTESIAN_POINT('Ctrl Pts',(-19.1045435468345,-67.6608292549412,
12.));
#133387=CARTESIAN_POINT('Ctrl Pts',(-19.0939607887492,-67.6435687749803,
0.));
#133388=CARTESIAN_POINT('Ctrl Pts',(-19.0939607887492,-67.6435687749803,
12.));
#133389=CARTESIAN_POINT('Ctrl Pts',(-19.0834236587115,-67.6263417083414,
0.));
#133390=CARTESIAN_POINT('Ctrl Pts',(-19.0834236587115,-67.6263417083414,
12.));
#133391=CARTESIAN_POINT('Ctrl Pts',(-19.0729321776287,-67.6091482520557,
0.));
#133392=CARTESIAN_POINT('Ctrl Pts',(-19.0729321776287,-67.6091482520557,
12.));
#133393=CARTESIAN_POINT('Ctrl Pts',(-19.0624863642425,-67.5919885896278,
0.));
#133394=CARTESIAN_POINT('Ctrl Pts',(-19.0624863642425,-67.5919885896278,
12.));
#133395=CARTESIAN_POINT('Ctrl Pts',(-19.0520862360414,-67.5748628972035,
0.));
#133396=CARTESIAN_POINT('Ctrl Pts',(-19.0520862360414,-67.5748628972035,
12.));
#133397=CARTESIAN_POINT('Ctrl Pts',(-19.0417318110721,-67.5577713558248,
0.));
#133398=CARTESIAN_POINT('Ctrl Pts',(-19.0417318110721,-67.5577713558248,
12.));
#133399=CARTESIAN_POINT('Ctrl Pts',(-19.0314231093924,-67.540714161288,
0.));
#133400=CARTESIAN_POINT('Ctrl Pts',(-19.0314231093924,-67.540714161288,
12.));
#133401=CARTESIAN_POINT('Ctrl Pts',(-19.0211601548222,-67.5236915360253,
0.));
#133402=CARTESIAN_POINT('Ctrl Pts',(-19.0211601548222,-67.5236915360253,
12.));
#133403=CARTESIAN_POINT('Ctrl Pts',(-19.0109429761274,-67.5067037372177,
0.));
#133404=CARTESIAN_POINT('Ctrl Pts',(-19.0109429761274,-67.5067037372177,
12.));
#133405=CARTESIAN_POINT('Ctrl Pts',(-19.0007716032785,-67.4897510316692,
0.));
#133406=CARTESIAN_POINT('Ctrl Pts',(-19.0007716032785,-67.4897510316692,
12.));
#133407=CARTESIAN_POINT('Ctrl Pts',(-18.9906460638607,-67.4728336719558,
0.));
#133408=CARTESIAN_POINT('Ctrl Pts',(-18.9906460638607,-67.4728336719558,
12.));
#133409=CARTESIAN_POINT('Ctrl Pts',(-18.9805663798466,-67.4559518744714,
0.));
#133410=CARTESIAN_POINT('Ctrl Pts',(-18.9805663798466,-67.4559518744714,
12.));
#133411=CARTESIAN_POINT('Ctrl Pts',(-18.9705325631773,-67.4391057908687,
0.));
#133412=CARTESIAN_POINT('Ctrl Pts',(-18.9705325631773,-67.4391057908687,
12.));
#133413=CARTESIAN_POINT('Ctrl Pts',(-18.9605446161079,-67.4222955062385,
0.));
#133414=CARTESIAN_POINT('Ctrl Pts',(-18.9605446161079,-67.4222955062385,
12.));
#133415=CARTESIAN_POINT('Ctrl Pts',(-18.9525909518003,-67.4088759498287,
0.));
#133416=CARTESIAN_POINT('Ctrl Pts',(-18.9525909518003,-67.4088759498287,
12.));
#133417=CARTESIAN_POINT('Ctrl Pts',(-18.9466463414355,-67.398827414689,
0.));
#133418=CARTESIAN_POINT('Ctrl Pts',(-18.9466463414355,-67.398827414689,
12.));
#133419=CARTESIAN_POINT('Ctrl Pts',(-18.942692439874,-67.3921355608417,
0.));
#133420=CARTESIAN_POINT('Ctrl Pts',(-18.942692439874,-67.3921355608417,
12.));
#133421=CARTESIAN_POINT('Ctrl Pts',(-18.9407177820969,-67.3887914263118,
0.));
#133422=CARTESIAN_POINT('Ctrl Pts',(-18.9407177820969,-67.3887914263118,
12.));
#133423=CARTESIAN_POINT('',(-18.9407177820969,-67.3887914263118,12.));
#133424=CARTESIAN_POINT('Ctrl Pts',(-18.9407177820969,-67.3887914263118,
12.));
#133425=CARTESIAN_POINT('Ctrl Pts',(-18.942692439874,-67.3921355608417,
12.));
#133426=CARTESIAN_POINT('Ctrl Pts',(-18.9466463414355,-67.398827414689,
12.));
#133427=CARTESIAN_POINT('Ctrl Pts',(-18.9525909518003,-67.4088759498287,
12.));
#133428=CARTESIAN_POINT('Ctrl Pts',(-18.9605446161079,-67.4222955062385,
12.));
#133429=CARTESIAN_POINT('Ctrl Pts',(-18.9705325631773,-67.4391057908687,
12.));
#133430=CARTESIAN_POINT('Ctrl Pts',(-18.9805663798466,-67.4559518744714,
12.));
#133431=CARTESIAN_POINT('Ctrl Pts',(-18.9906460638607,-67.4728336719558,
12.));
#133432=CARTESIAN_POINT('Ctrl Pts',(-19.0007716032785,-67.4897510316692,
12.));
#133433=CARTESIAN_POINT('Ctrl Pts',(-19.0109429761274,-67.5067037372177,
12.));
#133434=CARTESIAN_POINT('Ctrl Pts',(-19.0211601548222,-67.5236915360253,
12.));
#133435=CARTESIAN_POINT('Ctrl Pts',(-19.0314231093924,-67.540714161288,
12.));
#133436=CARTESIAN_POINT('Ctrl Pts',(-19.0417318110721,-67.5577713558248,
12.));
#133437=CARTESIAN_POINT('Ctrl Pts',(-19.0520862360414,-67.5748628972035,
12.));
#133438=CARTESIAN_POINT('Ctrl Pts',(-19.0624863642425,-67.5919885896278,
12.));
#133439=CARTESIAN_POINT('Ctrl Pts',(-19.0729321776287,-67.6091482520557,
12.));
#133440=CARTESIAN_POINT('Ctrl Pts',(-19.0834236587115,-67.6263417083414,
12.));
#133441=CARTESIAN_POINT('Ctrl Pts',(-19.0939607887492,-67.6435687749803,
12.));
#133442=CARTESIAN_POINT('Ctrl Pts',(-19.1045435468345,-67.6608292549412,
12.));
#133443=CARTESIAN_POINT('Ctrl Pts',(-19.115171910845,-67.6781229440535,
12.));
#133444=CARTESIAN_POINT('Ctrl Pts',(-19.1258458580343,-67.6954496350053,
12.));
#133445=CARTESIAN_POINT('Ctrl Pts',(-19.1365653657098,-67.7128091219372,
12.));
#133446=CARTESIAN_POINT('Ctrl Pts',(-19.1473304119969,-67.7302012056629,
12.));
#133447=CARTESIAN_POINT('Ctrl Pts',(-19.1581409758112,-67.7476256934492,
12.));
#133448=CARTESIAN_POINT('Ctrl Pts',(-19.1689970364959,-67.7650823965156,
12.));
#133449=CARTESIAN_POINT('Ctrl Pts',(-19.1798985735687,-67.7825711283092,
12.));
#133450=CARTESIAN_POINT('Ctrl Pts',(-19.1908455664089,-67.8000917023896,
12.));
#133451=CARTESIAN_POINT('Ctrl Pts',(-19.2018379939918,-67.817643930658,
12.));
#133452=CARTESIAN_POINT('Ctrl Pts',(-19.2128758350336,-67.8352276242856,
12.));
#133453=CARTESIAN_POINT('Ctrl Pts',(-19.223959068113,-67.852842594517,12.));
#133454=CARTESIAN_POINT('Ctrl Pts',(-19.2350876717878,-67.8704886534555,
12.));
#133455=CARTESIAN_POINT('Ctrl Pts',(-19.2462616247287,-67.8881656149983,
12.));
#133456=CARTESIAN_POINT('Ctrl Pts',(-19.2574809057705,-67.9058732951822,
12.));
#133457=CARTESIAN_POINT('Ctrl Pts',(-19.2687454938449,-67.9236115116781,
12.));
#133458=CARTESIAN_POINT('Ctrl Pts',(-19.2800553679362,-67.9413800834798,
12.));
#133459=CARTESIAN_POINT('Ctrl Pts',(-19.2914105070283,-67.959178830538,
12.));
#133460=CARTESIAN_POINT('Ctrl Pts',(-19.3028108900374,-67.977007573346,
12.));
#133461=CARTESIAN_POINT('Ctrl Pts',(-19.3142564958196,-67.9948661329591,
12.));
#133462=CARTESIAN_POINT('Ctrl Pts',(-19.3257473032031,-68.0127543311761,
12.));
#133463=CARTESIAN_POINT('Ctrl Pts',(-19.3372832910077,-68.0306719906636,
12.));
#133464=CARTESIAN_POINT('Ctrl Pts',(-19.3488644380646,-68.0486189351027,
12.));
#133465=CARTESIAN_POINT('Ctrl Pts',(-19.3604907232322,-68.0665949893222,
12.));
#133466=CARTESIAN_POINT('Ctrl Pts',(-19.3721621253921,-68.0845999792274,
12.));
#133467=CARTESIAN_POINT('Ctrl Pts',(-19.3838786234426,-68.1026337317298,
12.));
#133468=CARTESIAN_POINT('Ctrl Pts',(-19.3956401962893,-68.1206960746763,
12.));
#133469=CARTESIAN_POINT('Ctrl Pts',(-19.4074468228294,-68.1387868367668,
12.));
#133470=CARTESIAN_POINT('Ctrl Pts',(-19.4192984819411,-68.1569058475026,
12.));
#133471=CARTESIAN_POINT('Ctrl Pts',(-19.4311951524977,-68.1750529372211,
12.));
#133472=CARTESIAN_POINT('Ctrl Pts',(-19.4431368133718,-68.1932279371121,
12.));
#133473=CARTESIAN_POINT('Ctrl Pts',(-19.4551234434384,-68.2114306792366,
12.));
#133474=CARTESIAN_POINT('Ctrl Pts',(-19.4671550215724,-68.2296609965461,
12.));
#133475=CARTESIAN_POINT('Ctrl Pts',(-19.4792315266505,-68.2479187228815,
12.));
#133476=CARTESIAN_POINT('Ctrl Pts',(-19.4913529375545,-68.2662036929531,
12.));
#133477=CARTESIAN_POINT('Ctrl Pts',(-19.5035192331706,-68.2845157423234,
12.));
#133478=CARTESIAN_POINT('Ctrl Pts',(-19.5157303923856,-68.3028547073862,
12.));
#133479=CARTESIAN_POINT('Ctrl Pts',(-19.5279863940773,-68.3212204253415,
12.));
#133480=CARTESIAN_POINT('Ctrl Pts',(-19.540287217119,-68.3396127341938,
12.));
#133481=CARTESIAN_POINT('Ctrl Pts',(-19.5526328403852,-68.3580314727522,
12.));
#133482=CARTESIAN_POINT('Ctrl Pts',(-19.5650232427516,-68.3764764806287,
12.));
#133483=CARTESIAN_POINT('Ctrl Pts',(-19.5774584030939,-68.3949475982334,
12.));
#133484=CARTESIAN_POINT('Ctrl Pts',(-19.5899383002804,-68.4134446667695,
12.));
#133485=CARTESIAN_POINT('Ctrl Pts',(-19.6024629131786,-68.4319675282273,
12.));
#133486=CARTESIAN_POINT('Ctrl Pts',(-19.6150322206578,-68.4505160253777,
12.));
#133487=CARTESIAN_POINT('Ctrl Pts',(-19.6276462015888,-68.4690900017631,
12.));
#133488=CARTESIAN_POINT('Ctrl Pts',(-19.6403048348397,-68.4876893016863,
12.));
#133489=CARTESIAN_POINT('Ctrl Pts',(-19.653008099269,-68.5063137701986,
12.));
#133490=CARTESIAN_POINT('Ctrl Pts',(-19.665755973734,-68.5249632530994,
12.));
#133491=CARTESIAN_POINT('Ctrl Pts',(-19.6785484370929,-68.543637596932,
12.));
#133492=CARTESIAN_POINT('Ctrl Pts',(-19.6913854682046,-68.5623366489776,
12.));
#133493=CARTESIAN_POINT('Ctrl Pts',(-19.7042670459234,-68.5810602572474,
12.));
#133494=CARTESIAN_POINT('Ctrl Pts',(-19.717193149095,-68.5998082704741,
12.));
#133495=CARTESIAN_POINT('Ctrl Pts',(-19.7301637565646,-68.6185805381102,
12.));
#133496=CARTESIAN_POINT('Ctrl Pts',(-19.7431788471773,-68.6373769103211,
12.));
#133497=CARTESIAN_POINT('Ctrl Pts',(-19.7562383997784,-68.65619723798,12.));
#133498=CARTESIAN_POINT('Ctrl Pts',(-19.7693423932067,-68.6750413726574,
12.));
#133499=CARTESIAN_POINT('Ctrl Pts',(-19.7824908062925,-68.6939091666149,
12.));
#133500=CARTESIAN_POINT('Ctrl Pts',(-19.7956836178651,-68.7128004728033,
12.));
#133501=CARTESIAN_POINT('Ctrl Pts',(-19.8089208067537,-68.7317151448573,
12.));
#133502=CARTESIAN_POINT('Ctrl Pts',(-19.8222023517871,-68.7506530370904,
12.));
#133503=CARTESIAN_POINT('Ctrl Pts',(-19.8355282317858,-68.7696140044851,
12.));
#133504=CARTESIAN_POINT('Ctrl Pts',(-19.8488984255627,-68.7885979026878,
12.));
#133505=CARTESIAN_POINT('Ctrl Pts',(-19.8623129119293,-68.8076045880065,
12.));
#133506=CARTESIAN_POINT('Ctrl Pts',(-19.8757716696965,-68.8266339174056,
12.));
#133507=CARTESIAN_POINT('Ctrl Pts',(-19.8892746776739,-68.8456857485002,
12.));
#133508=CARTESIAN_POINT('Ctrl Pts',(-19.9028219146618,-68.8647599395469,
12.));
#133509=CARTESIAN_POINT('Ctrl Pts',(-19.9164133594526,-68.8838563494393,
12.));
#133510=CARTESIAN_POINT('Ctrl Pts',(-19.9300489908374,-68.9029748377067,
12.));
#133511=CARTESIAN_POINT('Ctrl Pts',(-19.9437287876066,-68.9221152645095,
12.));
#133512=CARTESIAN_POINT('Ctrl Pts',(-19.9574527285488,-68.9412774906333,
12.));
#133513=CARTESIAN_POINT('Ctrl Pts',(-19.9712207924429,-68.9604613774802,
12.));
#133514=CARTESIAN_POINT('Ctrl Pts',(-19.9850329580591,-68.9796667870638,
12.));
#133515=CARTESIAN_POINT('Ctrl Pts',(-19.9988892041666,-68.9988935820084,
12.));
#133516=CARTESIAN_POINT('Ctrl Pts',(-20.0127895095327,-69.0181416255431,
12.));
#133517=CARTESIAN_POINT('Ctrl Pts',(-20.0267338529223,-69.0374107814984,
12.));
#133518=CARTESIAN_POINT('Ctrl Pts',(-20.0407222130906,-69.0567009142978,
12.));
#133519=CARTESIAN_POINT('Ctrl Pts',(-20.0547545687842,-69.0760118889535,
12.));
#133520=CARTESIAN_POINT('Ctrl Pts',(-20.068830898748,-69.095343571064,12.));
#133521=CARTESIAN_POINT('Ctrl Pts',(-20.0829511817251,-69.1146958268104,
12.));
#133522=CARTESIAN_POINT('Ctrl Pts',(-20.0971153964557,-69.1340685229514,
12.));
#133523=CARTESIAN_POINT('Ctrl Pts',(-20.1113235216694,-69.1534615268152,
12.));
#133524=CARTESIAN_POINT('Ctrl Pts',(-20.1255755360872,-69.1728747062963,
12.));
#133525=CARTESIAN_POINT('Ctrl Pts',(-20.139871418428,-69.1923079298538,
12.));
#133526=CARTESIAN_POINT('Ctrl Pts',(-20.1542111474087,-69.2117610665076,
12.));
#133527=CARTESIAN_POINT('Ctrl Pts',(-20.1685947017433,-69.2312339858335,
12.));
#133528=CARTESIAN_POINT('Ctrl Pts',(-20.1830220601349,-69.2507265579554,
12.));
#133529=CARTESIAN_POINT('Ctrl Pts',(-20.1974932012773,-69.2702386535422,
12.));
#133530=CARTESIAN_POINT('Ctrl Pts',(-20.2120081038621,-69.2897701438059,
12.));
#133531=CARTESIAN_POINT('Ctrl Pts',(-20.2265667465784,-69.3093209004984,
12.));
#133532=CARTESIAN_POINT('Ctrl Pts',(-20.2411691081123,-69.3288907959067,
12.));
#133533=CARTESIAN_POINT('Ctrl Pts',(-20.2558151671391,-69.3484797028458,
12.));
#133534=CARTESIAN_POINT('Ctrl Pts',(-20.2705049023241,-69.368087494655,
12.));
#133535=CARTESIAN_POINT('Ctrl Pts',(-20.2852382923299,-69.3877140451975,
12.));
#133536=CARTESIAN_POINT('Ctrl Pts',(-20.3000153158167,-69.407359228856,
12.));
#133537=CARTESIAN_POINT('Ctrl Pts',(-20.3148359514415,-69.4270229205297,
12.));
#133538=CARTESIAN_POINT('Ctrl Pts',(-20.3297001778507,-69.4467049956262,
12.));
#133539=CARTESIAN_POINT('Ctrl Pts',(-20.3446079736802,-69.4664053300587,
12.));
#133540=CARTESIAN_POINT('Ctrl Pts',(-20.3595593175623,-69.4861238002441,
12.));
#133541=CARTESIAN_POINT('Ctrl Pts',(-20.3745541881269,-69.5058602831008,
12.));
#133542=CARTESIAN_POINT('Ctrl Pts',(-20.3895925640005,-69.5256146560441,
12.));
#133543=CARTESIAN_POINT('Ctrl Pts',(-20.4046744237999,-69.5453867969804,
12.));
#133544=CARTESIAN_POINT('Ctrl Pts',(-20.4197997461301,-69.5651765843033,
12.));
#133545=CARTESIAN_POINT('Ctrl Pts',(-20.4349685095924,-69.5849838968928,
12.));
#133546=CARTESIAN_POINT('Ctrl Pts',(-20.4501806927852,-69.6048086141113,
12.));
#133547=CARTESIAN_POINT('Ctrl Pts',(-20.4654362743037,-69.6246506158013,
12.));
#133548=CARTESIAN_POINT('Ctrl Pts',(-20.480735232734,-69.6445097822792,
12.));
#133549=CARTESIAN_POINT('Ctrl Pts',(-20.4960775466492,-69.6643859943308,
12.));
#133550=CARTESIAN_POINT('Ctrl Pts',(-20.5114631946185,-69.6842791332115,
12.));
#133551=CARTESIAN_POINT('Ctrl Pts',(-20.5268921552077,-69.7041890806425,
12.));
#133552=CARTESIAN_POINT('Ctrl Pts',(-20.54236440698,-69.7241157188083,12.));
#133553=CARTESIAN_POINT('Ctrl Pts',(-20.5578799284898,-69.744058930351,
12.));
#133554=CARTESIAN_POINT('Ctrl Pts',(-20.5734386982783,-69.7640185983644,
12.));
#133555=CARTESIAN_POINT('Ctrl Pts',(-20.5890406948811,-69.7839946063949,
12.));
#133556=CARTESIAN_POINT('Ctrl Pts',(-20.6046858968308,-69.8039868384389,
12.));
#133557=CARTESIAN_POINT('Ctrl Pts',(-20.6203742826566,-69.8239951789402,
12.));
#133558=CARTESIAN_POINT('Ctrl Pts',(-20.6361058308811,-69.8440195127866,
12.));
#133559=CARTESIAN_POINT('Ctrl Pts',(-20.6518805200129,-69.8640597253045,
12.));
#133560=CARTESIAN_POINT('Ctrl Pts',(-20.667698328554,-69.8841157022568,
12.));
#133561=CARTESIAN_POINT('Ctrl Pts',(-20.683559235003,-69.904187329841,12.));
#133562=CARTESIAN_POINT('Ctrl Pts',(-20.6994632178552,-69.9242744946854,
12.));
#133563=CARTESIAN_POINT('Ctrl Pts',(-20.7154102555997,-69.9443770838448,
12.));
#133564=CARTESIAN_POINT('Ctrl Pts',(-20.7314003267119,-69.9644949847934,
12.));
#133565=CARTESIAN_POINT('Ctrl Pts',(-20.7474334096581,-69.9846280854257,
12.));
#133566=CARTESIAN_POINT('Ctrl Pts',(-20.7635094829016,-70.0047762740568,
12.));
#133567=CARTESIAN_POINT('Ctrl Pts',(-20.7796285249022,-70.024939439422,
12.));
#133568=CARTESIAN_POINT('Ctrl Pts',(-20.7957905141157,-70.0451174706741,
12.));
#133569=CARTESIAN_POINT('Ctrl Pts',(-20.8119954289849,-70.0653102573803,
12.));
#133570=CARTESIAN_POINT('Ctrl Pts',(-20.8282432479429,-70.0855176895191,
12.));
#133571=CARTESIAN_POINT('Ctrl Pts',(-20.8445339494188,-70.1057396574747,
12.));
#133572=CARTESIAN_POINT('Ctrl Pts',(-20.8608675118379,-70.1259760520309,
12.));
#133573=CARTESIAN_POINT('Ctrl Pts',(-20.8772439136206,-70.1462267643646,
12.));
#133574=CARTESIAN_POINT('Ctrl Pts',(-20.8936631331748,-70.1664916860358,
12.));
#133575=CARTESIAN_POINT('Ctrl Pts',(-20.9101251488944,-70.1867707089854,
12.));
#133576=CARTESIAN_POINT('Ctrl Pts',(-20.9266299391684,-70.2070637255458,
12.));
#133577=CARTESIAN_POINT('Ctrl Pts',(-20.9431774823831,-70.2273706284472,
12.));
#133578=CARTESIAN_POINT('Ctrl Pts',(-20.9597677569228,-70.2476913108244,
12.));
#133579=CARTESIAN_POINT('Ctrl Pts',(-20.9764007411653,-70.2680256662224,
12.));
#133580=CARTESIAN_POINT('Ctrl Pts',(-20.9930764134776,-70.2883735885984,
12.));
#133581=CARTESIAN_POINT('Ctrl Pts',(-21.0097947522218,-70.3087349722973,
12.));
#133582=CARTESIAN_POINT('Ctrl Pts',(-21.0265557357548,-70.3291097120302,
12.));
#133583=CARTESIAN_POINT('Ctrl Pts',(-21.0433593424267,-70.3494977028498,
12.));
#133584=CARTESIAN_POINT('Ctrl Pts',(-21.0602055505748,-70.3698988401281,
12.));
#133585=CARTESIAN_POINT('Ctrl Pts',(-21.0770943385141,-70.3903130195265,
12.));
#133586=CARTESIAN_POINT('Ctrl Pts',(-21.0940256845473,-70.4107401370389,
12.));
#133587=CARTESIAN_POINT('Ctrl Pts',(-21.1109995669747,-70.4311800890401,
12.));
#133588=CARTESIAN_POINT('Ctrl Pts',(-21.1280159641003,-70.4516327723346,
12.));
#133589=CARTESIAN_POINT('Ctrl Pts',(-21.1450748542337,-70.4720980841939,
12.));
#133590=CARTESIAN_POINT('Ctrl Pts',(-21.1621762156897,-70.4925759224216,
12.));
#133591=CARTESIAN_POINT('Ctrl Pts',(-21.1793200267847,-70.5130661852955,
12.));
#133592=CARTESIAN_POINT('Ctrl Pts',(-21.1965062658298,-70.5335687714428,
12.));
#133593=CARTESIAN_POINT('Ctrl Pts',(-21.2137349111208,-70.5540835797283,
12.));
#133594=CARTESIAN_POINT('Ctrl Pts',(-21.2310059409266,-70.5746105091502,
12.));
#133595=CARTESIAN_POINT('Ctrl Pts',(-21.2483193334676,-70.5951494586957,
12.));
#133596=CARTESIAN_POINT('Ctrl Pts',(-21.2656750669126,-70.6157003273316,
12.));
#133597=CARTESIAN_POINT('Ctrl Pts',(-21.2830731194183,-70.6362630143047,
12.));
#133598=CARTESIAN_POINT('Ctrl Pts',(-21.300513469156,-70.6568374193774,
12.));
#133599=CARTESIAN_POINT('Ctrl Pts',(-21.3179960943389,-70.6774234430897,
12.));
#133600=CARTESIAN_POINT('Ctrl Pts',(-21.3355209732443,-70.6980209870045,
12.));
#133601=CARTESIAN_POINT('Ctrl Pts',(-21.3530880842349,-70.7186299539724,
12.));
#133602=CARTESIAN_POINT('Ctrl Pts',(-21.3706974057039,-70.7392502475469,
12.));
#133603=CARTESIAN_POINT('Ctrl Pts',(-21.3883489160196,-70.7598817714105,
12.));
#133604=CARTESIAN_POINT('Ctrl Pts',(-21.4060425934599,-70.780524428745,
12.));
#133605=CARTESIAN_POINT('Ctrl Pts',(-21.4237784161588,-70.8011781217394,
12.));
#133606=CARTESIAN_POINT('Ctrl Pts',(-21.4415563620114,-70.8218427507506,
12.));
#133607=CARTESIAN_POINT('Ctrl Pts',(-21.4593764087474,-70.8425182149846,
12.));
#133608=CARTESIAN_POINT('Ctrl Pts',(-21.477238534096,-70.8632044140112,
12.));
#133609=CARTESIAN_POINT('Ctrl Pts',(-21.4951427159262,-70.8839012490871,
12.));
#133610=CARTESIAN_POINT('Ctrl Pts',(-21.513088932377,-70.9046086244131,
12.));
#133611=CARTESIAN_POINT('Ctrl Pts',(-21.5310771620231,-70.9253264487636,
12.));
#133612=CARTESIAN_POINT('Ctrl Pts',(-21.5491073839106,-70.94605463587,12.));
#133613=CARTESIAN_POINT('Ctrl Pts',(-21.5645987555371,-70.9638315189818,
12.));
#133614=CARTESIAN_POINT('Ctrl Pts',(-21.5764983366483,-70.977466211259,
12.));
#133615=CARTESIAN_POINT('Ctrl Pts',(-21.5847875433335,-70.9869541808058,
12.));
#133616=CARTESIAN_POINT('Ctrl Pts',(-21.5894540925587,-70.9922924595372,
12.));
#133617=CARTESIAN_POINT('Ctrl Pts',(-21.5904919935066,-70.993479606912,
12.));
#133618=CARTESIAN_POINT('',(-18.9407177820969,-67.3887914263118,0.));
#133619=CARTESIAN_POINT('',(-18.9407177820969,-67.3887914263118,0.));
#133620=CARTESIAN_POINT('Ctrl Pts',(-21.5904919935066,-70.993479606912,
0.));
#133621=CARTESIAN_POINT('Ctrl Pts',(-21.5894540925587,-70.9922924595372,
0.));
#133622=CARTESIAN_POINT('Ctrl Pts',(-21.5847875433335,-70.9869541808058,
0.));
#133623=CARTESIAN_POINT('Ctrl Pts',(-21.5764983366483,-70.977466211259,
0.));
#133624=CARTESIAN_POINT('Ctrl Pts',(-21.5645987555371,-70.9638315189818,
0.));
#133625=CARTESIAN_POINT('Ctrl Pts',(-21.5491073839106,-70.94605463587,0.));
#133626=CARTESIAN_POINT('Ctrl Pts',(-21.5310771620231,-70.9253264487636,
0.));
#133627=CARTESIAN_POINT('Ctrl Pts',(-21.513088932377,-70.9046086244131,
0.));
#133628=CARTESIAN_POINT('Ctrl Pts',(-21.4951427159262,-70.8839012490871,
0.));
#133629=CARTESIAN_POINT('Ctrl Pts',(-21.477238534096,-70.8632044140112,
0.));
#133630=CARTESIAN_POINT('Ctrl Pts',(-21.4593764087474,-70.8425182149846,
0.));
#133631=CARTESIAN_POINT('Ctrl Pts',(-21.4415563620114,-70.8218427507506,
0.));
#133632=CARTESIAN_POINT('Ctrl Pts',(-21.4237784161588,-70.8011781217394,
0.));
#133633=CARTESIAN_POINT('Ctrl Pts',(-21.4060425934599,-70.780524428745,
0.));
#133634=CARTESIAN_POINT('Ctrl Pts',(-21.3883489160196,-70.7598817714105,
0.));
#133635=CARTESIAN_POINT('Ctrl Pts',(-21.3706974057039,-70.7392502475469,
0.));
#133636=CARTESIAN_POINT('Ctrl Pts',(-21.3530880842349,-70.7186299539724,
0.));
#133637=CARTESIAN_POINT('Ctrl Pts',(-21.3355209732443,-70.6980209870045,
0.));
#133638=CARTESIAN_POINT('Ctrl Pts',(-21.3179960943389,-70.6774234430897,
0.));
#133639=CARTESIAN_POINT('Ctrl Pts',(-21.300513469156,-70.6568374193774,
0.));
#133640=CARTESIAN_POINT('Ctrl Pts',(-21.2830731194183,-70.6362630143047,
0.));
#133641=CARTESIAN_POINT('Ctrl Pts',(-21.2656750669126,-70.6157003273316,
0.));
#133642=CARTESIAN_POINT('Ctrl Pts',(-21.2483193334676,-70.5951494586957,
0.));
#133643=CARTESIAN_POINT('Ctrl Pts',(-21.2310059409266,-70.5746105091502,
0.));
#133644=CARTESIAN_POINT('Ctrl Pts',(-21.2137349111208,-70.5540835797283,
0.));
#133645=CARTESIAN_POINT('Ctrl Pts',(-21.1965062658298,-70.5335687714428,
0.));
#133646=CARTESIAN_POINT('Ctrl Pts',(-21.1793200267847,-70.5130661852955,
0.));
#133647=CARTESIAN_POINT('Ctrl Pts',(-21.1621762156897,-70.4925759224216,
0.));
#133648=CARTESIAN_POINT('Ctrl Pts',(-21.1450748542337,-70.4720980841939,
0.));
#133649=CARTESIAN_POINT('Ctrl Pts',(-21.1280159641003,-70.4516327723346,
0.));
#133650=CARTESIAN_POINT('Ctrl Pts',(-21.1109995669747,-70.4311800890401,
0.));
#133651=CARTESIAN_POINT('Ctrl Pts',(-21.0940256845473,-70.4107401370389,
0.));
#133652=CARTESIAN_POINT('Ctrl Pts',(-21.0770943385141,-70.3903130195265,
0.));
#133653=CARTESIAN_POINT('Ctrl Pts',(-21.0602055505748,-70.3698988401281,
0.));
#133654=CARTESIAN_POINT('Ctrl Pts',(-21.0433593424267,-70.3494977028498,
0.));
#133655=CARTESIAN_POINT('Ctrl Pts',(-21.0265557357548,-70.3291097120302,
0.));
#133656=CARTESIAN_POINT('Ctrl Pts',(-21.0097947522218,-70.3087349722973,
0.));
#133657=CARTESIAN_POINT('Ctrl Pts',(-20.9930764134776,-70.2883735885984,
0.));
#133658=CARTESIAN_POINT('Ctrl Pts',(-20.9764007411653,-70.2680256662224,
0.));
#133659=CARTESIAN_POINT('Ctrl Pts',(-20.9597677569228,-70.2476913108244,
0.));
#133660=CARTESIAN_POINT('Ctrl Pts',(-20.9431774823831,-70.2273706284472,
0.));
#133661=CARTESIAN_POINT('Ctrl Pts',(-20.9266299391684,-70.2070637255458,
0.));
#133662=CARTESIAN_POINT('Ctrl Pts',(-20.9101251488944,-70.1867707089854,
0.));
#133663=CARTESIAN_POINT('Ctrl Pts',(-20.8936631331748,-70.1664916860358,
0.));
#133664=CARTESIAN_POINT('Ctrl Pts',(-20.8772439136206,-70.1462267643646,
0.));
#133665=CARTESIAN_POINT('Ctrl Pts',(-20.8608675118379,-70.1259760520309,
0.));
#133666=CARTESIAN_POINT('Ctrl Pts',(-20.8445339494188,-70.1057396574747,
0.));
#133667=CARTESIAN_POINT('Ctrl Pts',(-20.8282432479429,-70.0855176895191,
0.));
#133668=CARTESIAN_POINT('Ctrl Pts',(-20.8119954289849,-70.0653102573803,
0.));
#133669=CARTESIAN_POINT('Ctrl Pts',(-20.7957905141157,-70.0451174706741,
0.));
#133670=CARTESIAN_POINT('Ctrl Pts',(-20.7796285249022,-70.024939439422,
0.));
#133671=CARTESIAN_POINT('Ctrl Pts',(-20.7635094829016,-70.0047762740568,
0.));
#133672=CARTESIAN_POINT('Ctrl Pts',(-20.7474334096581,-69.9846280854257,
0.));
#133673=CARTESIAN_POINT('Ctrl Pts',(-20.7314003267119,-69.9644949847934,
0.));
#133674=CARTESIAN_POINT('Ctrl Pts',(-20.7154102555997,-69.9443770838448,
0.));
#133675=CARTESIAN_POINT('Ctrl Pts',(-20.6994632178552,-69.9242744946854,
0.));
#133676=CARTESIAN_POINT('Ctrl Pts',(-20.683559235003,-69.904187329841,0.));
#133677=CARTESIAN_POINT('Ctrl Pts',(-20.667698328554,-69.8841157022568,
0.));
#133678=CARTESIAN_POINT('Ctrl Pts',(-20.6518805200129,-69.8640597253045,
0.));
#133679=CARTESIAN_POINT('Ctrl Pts',(-20.6361058308811,-69.8440195127866,
0.));
#133680=CARTESIAN_POINT('Ctrl Pts',(-20.6203742826566,-69.8239951789402,
0.));
#133681=CARTESIAN_POINT('Ctrl Pts',(-20.6046858968308,-69.8039868384389,
0.));
#133682=CARTESIAN_POINT('Ctrl Pts',(-20.5890406948811,-69.7839946063949,
0.));
#133683=CARTESIAN_POINT('Ctrl Pts',(-20.5734386982783,-69.7640185983644,
0.));
#133684=CARTESIAN_POINT('Ctrl Pts',(-20.5578799284898,-69.744058930351,
0.));
#133685=CARTESIAN_POINT('Ctrl Pts',(-20.54236440698,-69.7241157188083,0.));
#133686=CARTESIAN_POINT('Ctrl Pts',(-20.5268921552077,-69.7041890806425,
0.));
#133687=CARTESIAN_POINT('Ctrl Pts',(-20.5114631946185,-69.6842791332115,
0.));
#133688=CARTESIAN_POINT('Ctrl Pts',(-20.4960775466492,-69.6643859943308,
0.));
#133689=CARTESIAN_POINT('Ctrl Pts',(-20.480735232734,-69.6445097822792,
0.));
#133690=CARTESIAN_POINT('Ctrl Pts',(-20.4654362743037,-69.6246506158013,
0.));
#133691=CARTESIAN_POINT('Ctrl Pts',(-20.4501806927852,-69.6048086141113,
0.));
#133692=CARTESIAN_POINT('Ctrl Pts',(-20.4349685095924,-69.5849838968928,
0.));
#133693=CARTESIAN_POINT('Ctrl Pts',(-20.4197997461301,-69.5651765843033,
0.));
#133694=CARTESIAN_POINT('Ctrl Pts',(-20.4046744237999,-69.5453867969804,
0.));
#133695=CARTESIAN_POINT('Ctrl Pts',(-20.3895925640005,-69.5256146560441,
0.));
#133696=CARTESIAN_POINT('Ctrl Pts',(-20.3745541881269,-69.5058602831008,
0.));
#133697=CARTESIAN_POINT('Ctrl Pts',(-20.3595593175623,-69.4861238002441,
0.));
#133698=CARTESIAN_POINT('Ctrl Pts',(-20.3446079736802,-69.4664053300587,
0.));
#133699=CARTESIAN_POINT('Ctrl Pts',(-20.3297001778507,-69.4467049956262,
0.));
#133700=CARTESIAN_POINT('Ctrl Pts',(-20.3148359514415,-69.4270229205297,
0.));
#133701=CARTESIAN_POINT('Ctrl Pts',(-20.3000153158167,-69.407359228856,
0.));
#133702=CARTESIAN_POINT('Ctrl Pts',(-20.2852382923299,-69.3877140451975,
0.));
#133703=CARTESIAN_POINT('Ctrl Pts',(-20.2705049023241,-69.368087494655,
0.));
#133704=CARTESIAN_POINT('Ctrl Pts',(-20.2558151671391,-69.3484797028458,
0.));
#133705=CARTESIAN_POINT('Ctrl Pts',(-20.2411691081123,-69.3288907959067,
0.));
#133706=CARTESIAN_POINT('Ctrl Pts',(-20.2265667465784,-69.3093209004984,
0.));
#133707=CARTESIAN_POINT('Ctrl Pts',(-20.2120081038621,-69.2897701438059,
0.));
#133708=CARTESIAN_POINT('Ctrl Pts',(-20.1974932012773,-69.2702386535422,
0.));
#133709=CARTESIAN_POINT('Ctrl Pts',(-20.1830220601349,-69.2507265579554,
0.));
#133710=CARTESIAN_POINT('Ctrl Pts',(-20.1685947017433,-69.2312339858335,
0.));
#133711=CARTESIAN_POINT('Ctrl Pts',(-20.1542111474087,-69.2117610665076,
0.));
#133712=CARTESIAN_POINT('Ctrl Pts',(-20.139871418428,-69.1923079298538,
0.));
#133713=CARTESIAN_POINT('Ctrl Pts',(-20.1255755360872,-69.1728747062963,
0.));
#133714=CARTESIAN_POINT('Ctrl Pts',(-20.1113235216694,-69.1534615268152,
0.));
#133715=CARTESIAN_POINT('Ctrl Pts',(-20.0971153964557,-69.1340685229514,
0.));
#133716=CARTESIAN_POINT('Ctrl Pts',(-20.0829511817251,-69.1146958268104,
0.));
#133717=CARTESIAN_POINT('Ctrl Pts',(-20.068830898748,-69.095343571064,0.));
#133718=CARTESIAN_POINT('Ctrl Pts',(-20.0547545687842,-69.0760118889535,
0.));
#133719=CARTESIAN_POINT('Ctrl Pts',(-20.0407222130906,-69.0567009142978,
0.));
#133720=CARTESIAN_POINT('Ctrl Pts',(-20.0267338529223,-69.0374107814984,
0.));
#133721=CARTESIAN_POINT('Ctrl Pts',(-20.0127895095327,-69.0181416255431,
0.));
#133722=CARTESIAN_POINT('Ctrl Pts',(-19.9988892041666,-68.9988935820084,
0.));
#133723=CARTESIAN_POINT('Ctrl Pts',(-19.9850329580591,-68.9796667870638,
0.));
#133724=CARTESIAN_POINT('Ctrl Pts',(-19.9712207924429,-68.9604613774802,
0.));
#133725=CARTESIAN_POINT('Ctrl Pts',(-19.9574527285488,-68.9412774906333,
0.));
#133726=CARTESIAN_POINT('Ctrl Pts',(-19.9437287876066,-68.9221152645095,
0.));
#133727=CARTESIAN_POINT('Ctrl Pts',(-19.9300489908374,-68.9029748377067,
0.));
#133728=CARTESIAN_POINT('Ctrl Pts',(-19.9164133594526,-68.8838563494393,
0.));
#133729=CARTESIAN_POINT('Ctrl Pts',(-19.9028219146618,-68.8647599395469,
0.));
#133730=CARTESIAN_POINT('Ctrl Pts',(-19.8892746776739,-68.8456857485002,
0.));
#133731=CARTESIAN_POINT('Ctrl Pts',(-19.8757716696965,-68.8266339174056,
0.));
#133732=CARTESIAN_POINT('Ctrl Pts',(-19.8623129119293,-68.8076045880065,
0.));
#133733=CARTESIAN_POINT('Ctrl Pts',(-19.8488984255627,-68.7885979026878,
0.));
#133734=CARTESIAN_POINT('Ctrl Pts',(-19.8355282317858,-68.7696140044851,
0.));
#133735=CARTESIAN_POINT('Ctrl Pts',(-19.8222023517871,-68.7506530370904,
0.));
#133736=CARTESIAN_POINT('Ctrl Pts',(-19.8089208067537,-68.7317151448573,
0.));
#133737=CARTESIAN_POINT('Ctrl Pts',(-19.7956836178651,-68.7128004728033,
0.));
#133738=CARTESIAN_POINT('Ctrl Pts',(-19.7824908062925,-68.6939091666149,
0.));
#133739=CARTESIAN_POINT('Ctrl Pts',(-19.7693423932067,-68.6750413726574,
0.));
#133740=CARTESIAN_POINT('Ctrl Pts',(-19.7562383997784,-68.65619723798,0.));
#133741=CARTESIAN_POINT('Ctrl Pts',(-19.7431788471773,-68.6373769103211,
0.));
#133742=CARTESIAN_POINT('Ctrl Pts',(-19.7301637565646,-68.6185805381102,
0.));
#133743=CARTESIAN_POINT('Ctrl Pts',(-19.717193149095,-68.5998082704741,
0.));
#133744=CARTESIAN_POINT('Ctrl Pts',(-19.7042670459234,-68.5810602572474,
0.));
#133745=CARTESIAN_POINT('Ctrl Pts',(-19.6913854682046,-68.5623366489776,
0.));
#133746=CARTESIAN_POINT('Ctrl Pts',(-19.6785484370929,-68.543637596932,
0.));
#133747=CARTESIAN_POINT('Ctrl Pts',(-19.665755973734,-68.5249632530994,
0.));
#133748=CARTESIAN_POINT('Ctrl Pts',(-19.653008099269,-68.5063137701986,
0.));
#133749=CARTESIAN_POINT('Ctrl Pts',(-19.6403048348397,-68.4876893016863,
0.));
#133750=CARTESIAN_POINT('Ctrl Pts',(-19.6276462015888,-68.4690900017631,
0.));
#133751=CARTESIAN_POINT('Ctrl Pts',(-19.6150322206578,-68.4505160253777,
0.));
#133752=CARTESIAN_POINT('Ctrl Pts',(-19.6024629131786,-68.4319675282273,
0.));
#133753=CARTESIAN_POINT('Ctrl Pts',(-19.5899383002804,-68.4134446667695,
0.));
#133754=CARTESIAN_POINT('Ctrl Pts',(-19.5774584030939,-68.3949475982334,
0.));
#133755=CARTESIAN_POINT('Ctrl Pts',(-19.5650232427516,-68.3764764806287,
0.));
#133756=CARTESIAN_POINT('Ctrl Pts',(-19.5526328403852,-68.3580314727522,
0.));
#133757=CARTESIAN_POINT('Ctrl Pts',(-19.540287217119,-68.3396127341938,
0.));
#133758=CARTESIAN_POINT('Ctrl Pts',(-19.5279863940773,-68.3212204253415,
0.));
#133759=CARTESIAN_POINT('Ctrl Pts',(-19.5157303923856,-68.3028547073862,
0.));
#133760=CARTESIAN_POINT('Ctrl Pts',(-19.5035192331706,-68.2845157423234,
0.));
#133761=CARTESIAN_POINT('Ctrl Pts',(-19.4913529375545,-68.2662036929531,
0.));
#133762=CARTESIAN_POINT('Ctrl Pts',(-19.4792315266505,-68.2479187228815,
0.));
#133763=CARTESIAN_POINT('Ctrl Pts',(-19.4671550215724,-68.2296609965461,
0.));
#133764=CARTESIAN_POINT('Ctrl Pts',(-19.4551234434384,-68.2114306792366,
0.));
#133765=CARTESIAN_POINT('Ctrl Pts',(-19.4431368133718,-68.1932279371121,
0.));
#133766=CARTESIAN_POINT('Ctrl Pts',(-19.4311951524977,-68.1750529372211,
0.));
#133767=CARTESIAN_POINT('Ctrl Pts',(-19.4192984819411,-68.1569058475026,
0.));
#133768=CARTESIAN_POINT('Ctrl Pts',(-19.4074468228294,-68.1387868367668,
0.));
#133769=CARTESIAN_POINT('Ctrl Pts',(-19.3956401962893,-68.1206960746763,
0.));
#133770=CARTESIAN_POINT('Ctrl Pts',(-19.3838786234426,-68.1026337317298,
0.));
#133771=CARTESIAN_POINT('Ctrl Pts',(-19.3721621253921,-68.0845999792274,
0.));
#133772=CARTESIAN_POINT('Ctrl Pts',(-19.3604907232322,-68.0665949893222,
0.));
#133773=CARTESIAN_POINT('Ctrl Pts',(-19.3488644380646,-68.0486189351027,
0.));
#133774=CARTESIAN_POINT('Ctrl Pts',(-19.3372832910077,-68.0306719906636,
0.));
#133775=CARTESIAN_POINT('Ctrl Pts',(-19.3257473032031,-68.0127543311761,
0.));
#133776=CARTESIAN_POINT('Ctrl Pts',(-19.3142564958196,-67.9948661329591,
0.));
#133777=CARTESIAN_POINT('Ctrl Pts',(-19.3028108900374,-67.977007573346,
0.));
#133778=CARTESIAN_POINT('Ctrl Pts',(-19.2914105070283,-67.959178830538,
0.));
#133779=CARTESIAN_POINT('Ctrl Pts',(-19.2800553679362,-67.9413800834798,
0.));
#133780=CARTESIAN_POINT('Ctrl Pts',(-19.2687454938449,-67.9236115116781,
0.));
#133781=CARTESIAN_POINT('Ctrl Pts',(-19.2574809057705,-67.9058732951822,
0.));
#133782=CARTESIAN_POINT('Ctrl Pts',(-19.2462616247287,-67.8881656149983,
0.));
#133783=CARTESIAN_POINT('Ctrl Pts',(-19.2350876717878,-67.8704886534555,
0.));
#133784=CARTESIAN_POINT('Ctrl Pts',(-19.223959068113,-67.852842594517,0.));
#133785=CARTESIAN_POINT('Ctrl Pts',(-19.2128758350336,-67.8352276242856,
0.));
#133786=CARTESIAN_POINT('Ctrl Pts',(-19.2018379939918,-67.817643930658,
0.));
#133787=CARTESIAN_POINT('Ctrl Pts',(-19.1908455664089,-67.8000917023896,
0.));
#133788=CARTESIAN_POINT('Ctrl Pts',(-19.1798985735687,-67.7825711283092,
0.));
#133789=CARTESIAN_POINT('Ctrl Pts',(-19.1689970364959,-67.7650823965156,
0.));
#133790=CARTESIAN_POINT('Ctrl Pts',(-19.1581409758112,-67.7476256934492,
0.));
#133791=CARTESIAN_POINT('Ctrl Pts',(-19.1473304119969,-67.7302012056629,
0.));
#133792=CARTESIAN_POINT('Ctrl Pts',(-19.1365653657098,-67.7128091219372,
0.));
#133793=CARTESIAN_POINT('Ctrl Pts',(-19.1258458580343,-67.6954496350053,
0.));
#133794=CARTESIAN_POINT('Ctrl Pts',(-19.115171910845,-67.6781229440535,
0.));
#133795=CARTESIAN_POINT('Ctrl Pts',(-19.1045435468345,-67.6608292549412,
0.));
#133796=CARTESIAN_POINT('Ctrl Pts',(-19.0939607887492,-67.6435687749803,
0.));
#133797=CARTESIAN_POINT('Ctrl Pts',(-19.0834236587115,-67.6263417083414,
0.));
#133798=CARTESIAN_POINT('Ctrl Pts',(-19.0729321776287,-67.6091482520557,
0.));
#133799=CARTESIAN_POINT('Ctrl Pts',(-19.0624863642425,-67.5919885896278,
0.));
#133800=CARTESIAN_POINT('Ctrl Pts',(-19.0520862360414,-67.5748628972035,
0.));
#133801=CARTESIAN_POINT('Ctrl Pts',(-19.0417318110721,-67.5577713558248,
0.));
#133802=CARTESIAN_POINT('Ctrl Pts',(-19.0314231093924,-67.540714161288,
0.));
#133803=CARTESIAN_POINT('Ctrl Pts',(-19.0211601548222,-67.5236915360253,
0.));
#133804=CARTESIAN_POINT('Ctrl Pts',(-19.0109429761274,-67.5067037372177,
0.));
#133805=CARTESIAN_POINT('Ctrl Pts',(-19.0007716032785,-67.4897510316692,
0.));
#133806=CARTESIAN_POINT('Ctrl Pts',(-18.9906460638607,-67.4728336719558,
0.));
#133807=CARTESIAN_POINT('Ctrl Pts',(-18.9805663798466,-67.4559518744714,
0.));
#133808=CARTESIAN_POINT('Ctrl Pts',(-18.9705325631773,-67.4391057908687,
0.));
#133809=CARTESIAN_POINT('Ctrl Pts',(-18.9605446161079,-67.4222955062385,
0.));
#133810=CARTESIAN_POINT('Ctrl Pts',(-18.9525909518003,-67.4088759498287,
0.));
#133811=CARTESIAN_POINT('Ctrl Pts',(-18.9466463414355,-67.398827414689,
0.));
#133812=CARTESIAN_POINT('Ctrl Pts',(-18.942692439874,-67.3921355608417,
0.));
#133813=CARTESIAN_POINT('Ctrl Pts',(-18.9407177820969,-67.3887914263118,
0.));
#133814=CARTESIAN_POINT('Ctrl Pts',(-27.9316983239472,-69.065695021045,
0.));
#133815=CARTESIAN_POINT('Ctrl Pts',(-27.9316983239472,-69.065695021045,
12.));
#133816=CARTESIAN_POINT('Ctrl Pts',(-27.9276214070631,-69.0618620884721,
0.));
#133817=CARTESIAN_POINT('Ctrl Pts',(-27.9276214070631,-69.0618620884721,
12.));
#133818=CARTESIAN_POINT('Ctrl Pts',(-27.9194718099003,-69.0541967851028,
0.));
#133819=CARTESIAN_POINT('Ctrl Pts',(-27.9194718099003,-69.0541967851028,
12.));
#133820=CARTESIAN_POINT('Ctrl Pts',(-27.9072601239722,-69.0427005153791,
0.));
#133821=CARTESIAN_POINT('Ctrl Pts',(-27.9072601239722,-69.0427005153791,
12.));
#133822=CARTESIAN_POINT('Ctrl Pts',(-27.8910032967339,-69.0273755265382,
0.));
#133823=CARTESIAN_POINT('Ctrl Pts',(-27.8910032967339,-69.0273755265382,
12.));
#133824=CARTESIAN_POINT('Ctrl Pts',(-27.8707246380957,-69.0082249138598,
0.));
#133825=CARTESIAN_POINT('Ctrl Pts',(-27.8707246380957,-69.0082249138598,
12.));
#133826=CARTESIAN_POINT('Ctrl Pts',(-27.8504883674059,-68.9890799392213,
0.));
#133827=CARTESIAN_POINT('Ctrl Pts',(-27.8504883674059,-68.9890799392213,
12.));
#133828=CARTESIAN_POINT('Ctrl Pts',(-27.8302945019977,-68.9699406311389,
0.));
#133829=CARTESIAN_POINT('Ctrl Pts',(-27.8302945019977,-68.9699406311389,
12.));
#133830=CARTESIAN_POINT('Ctrl Pts',(-27.8101430638072,-68.9508070357658,
0.));
#133831=CARTESIAN_POINT('Ctrl Pts',(-27.8101430638072,-68.9508070357658,
12.));
#133832=CARTESIAN_POINT('Ctrl Pts',(-27.7900340793689,-68.9316792225946,
0.));
#133833=CARTESIAN_POINT('Ctrl Pts',(-27.7900340793689,-68.9316792225946,
12.));
#133834=CARTESIAN_POINT('Ctrl Pts',(-27.7699675790571,-68.9125572825693,
0.));
#133835=CARTESIAN_POINT('Ctrl Pts',(-27.7699675790571,-68.9125572825693,
12.));
#133836=CARTESIAN_POINT('Ctrl Pts',(-27.7499435957525,-68.8934413203759,
0.));
#133837=CARTESIAN_POINT('Ctrl Pts',(-27.7499435957525,-68.8934413203759,
12.));
#133838=CARTESIAN_POINT('Ctrl Pts',(-27.7299621636566,-68.8743314483369,
0.));
#133839=CARTESIAN_POINT('Ctrl Pts',(-27.7299621636566,-68.8743314483369,
12.));
#133840=CARTESIAN_POINT('Ctrl Pts',(-27.7100233170737,-68.85522777982,0.));
#133841=CARTESIAN_POINT('Ctrl Pts',(-27.7100233170737,-68.85522777982,12.));
#133842=CARTESIAN_POINT('Ctrl Pts',(-27.6901270891241,-68.8361304224467,
0.));
#133843=CARTESIAN_POINT('Ctrl Pts',(-27.6901270891241,-68.8361304224467,
12.));
#133844=CARTESIAN_POINT('Ctrl Pts',(-27.6702735107121,-68.81703947259,0.));
#133845=CARTESIAN_POINT('Ctrl Pts',(-27.6702735107121,-68.81703947259,12.));
#133846=CARTESIAN_POINT('Ctrl Pts',(-27.6504626112666,-68.7979550191872,
0.));
#133847=CARTESIAN_POINT('Ctrl Pts',(-27.6504626112666,-68.7979550191872,
12.));
#133848=CARTESIAN_POINT('Ctrl Pts',(-27.6306944192738,-68.7788771464713,
0.));
#133849=CARTESIAN_POINT('Ctrl Pts',(-27.6306944192738,-68.7788771464713,
12.));
#133850=CARTESIAN_POINT('Ctrl Pts',(-27.6109689629029,-68.7598059372129,
0.));
#133851=CARTESIAN_POINT('Ctrl Pts',(-27.6109689629029,-68.7598059372129,
12.));
#133852=CARTESIAN_POINT('Ctrl Pts',(-27.5912862705469,-68.7407414755259,
0.));
#133853=CARTESIAN_POINT('Ctrl Pts',(-27.5912862705469,-68.7407414755259,
12.));
#133854=CARTESIAN_POINT('Ctrl Pts',(-27.5716463715005,-68.7216838504218,
0.));
#133855=CARTESIAN_POINT('Ctrl Pts',(-27.5716463715005,-68.7216838504218,
12.));
#133856=CARTESIAN_POINT('Ctrl Pts',(-27.5520492958907,-68.7026331554296,
0.));
#133857=CARTESIAN_POINT('Ctrl Pts',(-27.5520492958907,-68.7026331554296,
12.));
#133858=CARTESIAN_POINT('Ctrl Pts',(-27.5324950743706,-68.6835894869882,
0.));
#133859=CARTESIAN_POINT('Ctrl Pts',(-27.5324950743706,-68.6835894869882,
12.));
#133860=CARTESIAN_POINT('Ctrl Pts',(-27.5129837378791,-68.6645529432045,
0.));
#133861=CARTESIAN_POINT('Ctrl Pts',(-27.5129837378791,-68.6645529432045,
12.));
#133862=CARTESIAN_POINT('Ctrl Pts',(-27.4935153173868,-68.645523622548,
0.));
#133863=CARTESIAN_POINT('Ctrl Pts',(-27.4935153173868,-68.645523622548,
12.));
#133864=CARTESIAN_POINT('Ctrl Pts',(-27.4740898435988,-68.6265016223561,
0.));
#133865=CARTESIAN_POINT('Ctrl Pts',(-27.4740898435988,-68.6265016223561,
12.));
#133866=CARTESIAN_POINT('Ctrl Pts',(-27.4547073468227,-68.6074870381619,
0.));
#133867=CARTESIAN_POINT('Ctrl Pts',(-27.4547073468227,-68.6074870381619,
12.));
#133868=CARTESIAN_POINT('Ctrl Pts',(-27.4353678571361,-68.5884799645218,
0.));
#133869=CARTESIAN_POINT('Ctrl Pts',(-27.4353678571361,-68.5884799645218,
12.));
#133870=CARTESIAN_POINT('Ctrl Pts',(-27.4160714044831,-68.5694804955014,
0.));
#133871=CARTESIAN_POINT('Ctrl Pts',(-27.4160714044831,-68.5694804955014,
12.));
#133872=CARTESIAN_POINT('Ctrl Pts',(-27.3968180187941,-68.5504887252975,
0.));
#133873=CARTESIAN_POINT('Ctrl Pts',(-27.3968180187941,-68.5504887252975,
12.));
#133874=CARTESIAN_POINT('Ctrl Pts',(-27.3776077300914,-68.5315047488035,
0.));
#133875=CARTESIAN_POINT('Ctrl Pts',(-27.3776077300914,-68.5315047488035,
12.));
#133876=CARTESIAN_POINT('Ctrl Pts',(-27.3584405685941,-68.5125286621888,
0.));
#133877=CARTESIAN_POINT('Ctrl Pts',(-27.3584405685941,-68.5125286621888,
12.));
#133878=CARTESIAN_POINT('Ctrl Pts',(-27.3393165646748,-68.4935605626361,
0.));
#133879=CARTESIAN_POINT('Ctrl Pts',(-27.3393165646748,-68.4935605626361,
12.));
#133880=CARTESIAN_POINT('Ctrl Pts',(-27.3202357488153,-68.4746005480992,
0.));
#133881=CARTESIAN_POINT('Ctrl Pts',(-27.3202357488153,-68.4746005480992,
12.));
#133882=CARTESIAN_POINT('Ctrl Pts',(-27.301198151557,-68.455648717044,0.));
#133883=CARTESIAN_POINT('Ctrl Pts',(-27.301198151557,-68.455648717044,12.));
#133884=CARTESIAN_POINT('Ctrl Pts',(-27.2822038034539,-68.4367051682166,
0.));
#133885=CARTESIAN_POINT('Ctrl Pts',(-27.2822038034539,-68.4367051682166,
12.));
#133886=CARTESIAN_POINT('Ctrl Pts',(-27.2632527350062,-68.4177700003471,
0.));
#133887=CARTESIAN_POINT('Ctrl Pts',(-27.2632527350062,-68.4177700003471,
12.));
#133888=CARTESIAN_POINT('Ctrl Pts',(-27.2443449766654,-68.3988433121589,
0.));
#133889=CARTESIAN_POINT('Ctrl Pts',(-27.2443449766654,-68.3988433121589,
12.));
#133890=CARTESIAN_POINT('Ctrl Pts',(-27.2254805588677,-68.379925202511,
0.));
#133891=CARTESIAN_POINT('Ctrl Pts',(-27.2254805588677,-68.379925202511,
12.));
#133892=CARTESIAN_POINT('Ctrl Pts',(-27.2066595120544,-68.3610157704999,
0.));
#133893=CARTESIAN_POINT('Ctrl Pts',(-27.2066595120544,-68.3610157704999,
12.));
#133894=CARTESIAN_POINT('Ctrl Pts',(-27.1878818666925,-68.3421151155708,
0.));
#133895=CARTESIAN_POINT('Ctrl Pts',(-27.1878818666925,-68.3421151155708,
12.));
#133896=CARTESIAN_POINT('Ctrl Pts',(-27.1691476532917,-68.3232233376415,
0.));
#133897=CARTESIAN_POINT('Ctrl Pts',(-27.1691476532917,-68.3232233376415,
12.));
#133898=CARTESIAN_POINT('Ctrl Pts',(-27.1504569024131,-68.3043405371589,
0.));
#133899=CARTESIAN_POINT('Ctrl Pts',(-27.1504569024131,-68.3043405371589,
12.));
#133900=CARTESIAN_POINT('Ctrl Pts',(-27.1318096446643,-68.285466815035,
0.));
#133901=CARTESIAN_POINT('Ctrl Pts',(-27.1318096446643,-68.285466815035,
12.));
#133902=CARTESIAN_POINT('Ctrl Pts',(-27.1132059106939,-68.2666022726094,
0.));
#133903=CARTESIAN_POINT('Ctrl Pts',(-27.1132059106939,-68.2666022726094,
12.));
#133904=CARTESIAN_POINT('Ctrl Pts',(-27.0946457311814,-68.2477470116014,
0.));
#133905=CARTESIAN_POINT('Ctrl Pts',(-27.0946457311814,-68.2477470116014,
12.));
#133906=CARTESIAN_POINT('Ctrl Pts',(-27.076129136823,-68.2289011340624,
0.));
#133907=CARTESIAN_POINT('Ctrl Pts',(-27.076129136823,-68.2289011340624,
12.));
#133908=CARTESIAN_POINT('Ctrl Pts',(-27.0576561583179,-68.2100647423345,
0.));
#133909=CARTESIAN_POINT('Ctrl Pts',(-27.0576561583179,-68.2100647423345,
12.));
#133910=CARTESIAN_POINT('Ctrl Pts',(-27.0392268263805,-68.1912379390786,
0.));
#133911=CARTESIAN_POINT('Ctrl Pts',(-27.0392268263805,-68.1912379390786,
12.));
#133912=CARTESIAN_POINT('Ctrl Pts',(-27.0208411717477,-68.1724208272967,
0.));
#133913=CARTESIAN_POINT('Ctrl Pts',(-27.0208411717477,-68.1724208272967,
12.));
#133914=CARTESIAN_POINT('Ctrl Pts',(-27.0024992251839,-68.1536135103558,
0.));
#133915=CARTESIAN_POINT('Ctrl Pts',(-27.0024992251839,-68.1536135103558,
12.));
#133916=CARTESIAN_POINT('Ctrl Pts',(-26.9842010174819,-68.13481609201,0.));
#133917=CARTESIAN_POINT('Ctrl Pts',(-26.9842010174819,-68.13481609201,12.));
#133918=CARTESIAN_POINT('Ctrl Pts',(-26.9659465794596,-68.1160286764244,
0.));
#133919=CARTESIAN_POINT('Ctrl Pts',(-26.9659465794596,-68.1160286764244,
12.));
#133920=CARTESIAN_POINT('Ctrl Pts',(-26.9477359419646,-68.0972513681739,
0.));
#133921=CARTESIAN_POINT('Ctrl Pts',(-26.9477359419646,-68.0972513681739,
12.));
#133922=CARTESIAN_POINT('Ctrl Pts',(-26.9295691358775,-68.0784842722362,
0.));
#133923=CARTESIAN_POINT('Ctrl Pts',(-26.9295691358775,-68.0784842722362,
12.));
#133924=CARTESIAN_POINT('Ctrl Pts',(-26.9114461921109,-68.0597274939857,
0.));
#133925=CARTESIAN_POINT('Ctrl Pts',(-26.9114461921109,-68.0597274939857,
12.));
#133926=CARTESIAN_POINT('Ctrl Pts',(-26.8933671416065,-68.0409811391871,
0.));
#133927=CARTESIAN_POINT('Ctrl Pts',(-26.8933671416065,-68.0409811391871,
12.));
#133928=CARTESIAN_POINT('Ctrl Pts',(-26.8753320153255,-68.0222453139862,
0.));
#133929=CARTESIAN_POINT('Ctrl Pts',(-26.8753320153255,-68.0222453139862,
12.));
#133930=CARTESIAN_POINT('Ctrl Pts',(-26.85734084425,-68.0035201249108,0.));
#133931=CARTESIAN_POINT('Ctrl Pts',(-26.85734084425,-68.0035201249108,12.));
#133932=CARTESIAN_POINT('Ctrl Pts',(-26.8393936593914,-67.9848056788814,
0.));
#133933=CARTESIAN_POINT('Ctrl Pts',(-26.8393936593914,-67.9848056788814,
12.));
#133934=CARTESIAN_POINT('Ctrl Pts',(-26.8214904917922,-67.9661020832165,
0.));
#133935=CARTESIAN_POINT('Ctrl Pts',(-26.8214904917922,-67.9661020832165,
12.));
#133936=CARTESIAN_POINT('Ctrl Pts',(-26.8036313725262,-67.9474094456395,
0.));
#133937=CARTESIAN_POINT('Ctrl Pts',(-26.8036313725262,-67.9474094456395,
12.));
#133938=CARTESIAN_POINT('Ctrl Pts',(-26.7858163326933,-67.9287278742839,
0.));
#133939=CARTESIAN_POINT('Ctrl Pts',(-26.7858163326933,-67.9287278742839,
12.));
#133940=CARTESIAN_POINT('Ctrl Pts',(-26.7680454034169,-67.9100574776974,
0.));
#133941=CARTESIAN_POINT('Ctrl Pts',(-26.7680454034169,-67.9100574776974,
12.));
#133942=CARTESIAN_POINT('Ctrl Pts',(-26.7503186158523,-67.8913983648441,
0.));
#133943=CARTESIAN_POINT('Ctrl Pts',(-26.7503186158523,-67.8913983648441,
12.));
#133944=CARTESIAN_POINT('Ctrl Pts',(-26.7326360011886,-67.8727506451067,
0.));
#133945=CARTESIAN_POINT('Ctrl Pts',(-26.7326360011886,-67.8727506451067,
12.));
#133946=CARTESIAN_POINT('Ctrl Pts',(-26.7149975906478,-67.8541144282875,
0.));
#133947=CARTESIAN_POINT('Ctrl Pts',(-26.7149975906478,-67.8541144282875,
12.));
#133948=CARTESIAN_POINT('Ctrl Pts',(-26.6974034154803,-67.8354898246079,
0.));
#133949=CARTESIAN_POINT('Ctrl Pts',(-26.6974034154803,-67.8354898246079,
12.));
#133950=CARTESIAN_POINT('Ctrl Pts',(-26.6798535069586,-67.8168769447086,
0.));
#133951=CARTESIAN_POINT('Ctrl Pts',(-26.6798535069586,-67.8168769447086,
12.));
#133952=CARTESIAN_POINT('Ctrl Pts',(-26.6623478963867,-67.7982758996557,
0.));
#133953=CARTESIAN_POINT('Ctrl Pts',(-26.6623478963867,-67.7982758996557,
12.));
#133954=CARTESIAN_POINT('Ctrl Pts',(-26.6448866151027,-67.7796868009447,
0.));
#133955=CARTESIAN_POINT('Ctrl Pts',(-26.6448866151027,-67.7796868009447,
12.));
#133956=CARTESIAN_POINT('Ctrl Pts',(-26.6274696944793,-67.7611097605042,
0.));
#133957=CARTESIAN_POINT('Ctrl Pts',(-26.6274696944793,-67.7611097605042,
12.));
#133958=CARTESIAN_POINT('Ctrl Pts',(-26.6100971659205,-67.7425448906983,
0.));
#133959=CARTESIAN_POINT('Ctrl Pts',(-26.6100971659205,-67.7425448906983,
12.));
#133960=CARTESIAN_POINT('Ctrl Pts',(-26.5927690608547,-67.7239923043295,
0.));
#133961=CARTESIAN_POINT('Ctrl Pts',(-26.5927690608547,-67.7239923043295,
12.));
#133962=CARTESIAN_POINT('Ctrl Pts',(-26.5754854107422,-67.7054521146427,
0.));
#133963=CARTESIAN_POINT('Ctrl Pts',(-26.5754854107422,-67.7054521146427,
12.));
#133964=CARTESIAN_POINT('Ctrl Pts',(-26.5582462470794,-67.6869244353292,
0.));
#133965=CARTESIAN_POINT('Ctrl Pts',(-26.5582462470794,-67.6869244353292,
12.));
#133966=CARTESIAN_POINT('Ctrl Pts',(-26.5410516013984,-67.6684093805288,
0.));
#133967=CARTESIAN_POINT('Ctrl Pts',(-26.5410516013984,-67.6684093805288,
12.));
#133968=CARTESIAN_POINT('Ctrl Pts',(-26.5239015052656,-67.6499070648323,
0.));
#133969=CARTESIAN_POINT('Ctrl Pts',(-26.5239015052656,-67.6499070648323,
12.));
#133970=CARTESIAN_POINT('Ctrl Pts',(-26.5067959902731,-67.6314176032823,
0.));
#133971=CARTESIAN_POINT('Ctrl Pts',(-26.5067959902731,-67.6314176032823,
12.));
#133972=CARTESIAN_POINT('Ctrl Pts',(-26.4897350880447,-67.6129411113774,
0.));
#133973=CARTESIAN_POINT('Ctrl Pts',(-26.4897350880447,-67.6129411113774,
12.));
#133974=CARTESIAN_POINT('Ctrl Pts',(-26.4727188302415,-67.5944777050782,
0.));
#133975=CARTESIAN_POINT('Ctrl Pts',(-26.4727188302415,-67.5944777050782,
12.));
#133976=CARTESIAN_POINT('Ctrl Pts',(-26.4557472485622,-67.5760275008096,
0.));
#133977=CARTESIAN_POINT('Ctrl Pts',(-26.4557472485622,-67.5760275008096,
12.));
#133978=CARTESIAN_POINT('Ctrl Pts',(-26.4388203747422,-67.5575906154648,
0.));
#133979=CARTESIAN_POINT('Ctrl Pts',(-26.4388203747422,-67.5575906154648,
12.));
#133980=CARTESIAN_POINT('Ctrl Pts',(-26.4219382405452,-67.5391671664055,
0.));
#133981=CARTESIAN_POINT('Ctrl Pts',(-26.4219382405452,-67.5391671664055,
12.));
#133982=CARTESIAN_POINT('Ctrl Pts',(-26.4051008777669,-67.5207572714666,
0.));
#133983=CARTESIAN_POINT('Ctrl Pts',(-26.4051008777669,-67.5207572714666,
12.));
#133984=CARTESIAN_POINT('Ctrl Pts',(-26.3883083182417,-67.5023610489611,
0.));
#133985=CARTESIAN_POINT('Ctrl Pts',(-26.3883083182417,-67.5023610489611,
12.));
#133986=CARTESIAN_POINT('Ctrl Pts',(-26.3715605938432,-67.4839786176833,
0.));
#133987=CARTESIAN_POINT('Ctrl Pts',(-26.3715605938432,-67.4839786176833,
12.));
#133988=CARTESIAN_POINT('Ctrl Pts',(-26.3548577364835,-67.4656100969121,
0.));
#133989=CARTESIAN_POINT('Ctrl Pts',(-26.3548577364835,-67.4656100969121,
12.));
#133990=CARTESIAN_POINT('Ctrl Pts',(-26.3381997781059,-67.4472556064127,
0.));
#133991=CARTESIAN_POINT('Ctrl Pts',(-26.3381997781059,-67.4472556064127,
12.));
#133992=CARTESIAN_POINT('Ctrl Pts',(-26.3215867506864,-67.4289152664406,
0.));
#133993=CARTESIAN_POINT('Ctrl Pts',(-26.3215867506864,-67.4289152664406,
12.));
#133994=CARTESIAN_POINT('Ctrl Pts',(-26.305018686241,-67.4105891977465,
0.));
#133995=CARTESIAN_POINT('Ctrl Pts',(-26.305018686241,-67.4105891977465,
12.));
#133996=CARTESIAN_POINT('Ctrl Pts',(-26.288495616827,-67.392277521581,0.));
#133997=CARTESIAN_POINT('Ctrl Pts',(-26.288495616827,-67.392277521581,12.));
#133998=CARTESIAN_POINT('Ctrl Pts',(-26.2720175745423,-67.3739803596967,
0.));
#133999=CARTESIAN_POINT('Ctrl Pts',(-26.2720175745423,-67.3739803596967,
12.));
#134000=CARTESIAN_POINT('Ctrl Pts',(-26.255584591518,-67.3556978343506,
0.));
#134001=CARTESIAN_POINT('Ctrl Pts',(-26.255584591518,-67.3556978343506,
12.));
#134002=CARTESIAN_POINT('Ctrl Pts',(-26.2391966999192,-67.3374300683075,
0.));
#134003=CARTESIAN_POINT('Ctrl Pts',(-26.2391966999192,-67.3374300683075,
12.));
#134004=CARTESIAN_POINT('Ctrl Pts',(-26.2228539319528,-67.3191771848468,
0.));
#134005=CARTESIAN_POINT('Ctrl Pts',(-26.2228539319528,-67.3191771848468,
12.));
#134006=CARTESIAN_POINT('Ctrl Pts',(-26.2065563198685,-67.3009393077654,
0.));
#134007=CARTESIAN_POINT('Ctrl Pts',(-26.2065563198685,-67.3009393077654,
12.));
#134008=CARTESIAN_POINT('Ctrl Pts',(-26.1903038959589,-67.2827165613828,
0.));
#134009=CARTESIAN_POINT('Ctrl Pts',(-26.1903038959589,-67.2827165613828,
12.));
#134010=CARTESIAN_POINT('Ctrl Pts',(-26.1740966925527,-67.2645090705414,
0.));
#134011=CARTESIAN_POINT('Ctrl Pts',(-26.1740966925527,-67.2645090705414,
12.));
#134012=CARTESIAN_POINT('Ctrl Pts',(-26.1579347420135,-67.2463169606105,
0.));
#134013=CARTESIAN_POINT('Ctrl Pts',(-26.1579347420135,-67.2463169606105,
12.));
#134014=CARTESIAN_POINT('Ctrl Pts',(-26.1418180767487,-67.228140357493,
0.));
#134015=CARTESIAN_POINT('Ctrl Pts',(-26.1418180767487,-67.228140357493,
12.));
#134016=CARTESIAN_POINT('Ctrl Pts',(-26.1257467292102,-67.2099793876295,
0.));
#134017=CARTESIAN_POINT('Ctrl Pts',(-26.1257467292102,-67.2099793876295,
12.));
#134018=CARTESIAN_POINT('Ctrl Pts',(-26.109720731895,-67.191834178002,0.));
#134019=CARTESIAN_POINT('Ctrl Pts',(-26.109720731895,-67.191834178002,12.));
#134020=CARTESIAN_POINT('Ctrl Pts',(-26.0937401173385,-67.1737048561364,
0.));
#134021=CARTESIAN_POINT('Ctrl Pts',(-26.0937401173385,-67.1737048561364,
12.));
#134022=CARTESIAN_POINT('Ctrl Pts',(-26.077804918113,-67.1555915501052,
0.));
#134023=CARTESIAN_POINT('Ctrl Pts',(-26.077804918113,-67.1555915501052,
12.));
#134024=CARTESIAN_POINT('Ctrl Pts',(-26.0619151668361,-67.1374943885353,
0.));
#134025=CARTESIAN_POINT('Ctrl Pts',(-26.0619151668361,-67.1374943885353,
12.));
#134026=CARTESIAN_POINT('Ctrl Pts',(-26.0460708961725,-67.1194135006121,
0.));
#134027=CARTESIAN_POINT('Ctrl Pts',(-26.0460708961725,-67.1194135006121,
12.));
#134028=CARTESIAN_POINT('Ctrl Pts',(-26.030272138834,-67.101349016084,0.));
#134029=CARTESIAN_POINT('Ctrl Pts',(-26.030272138834,-67.101349016084,12.));
#134030=CARTESIAN_POINT('Ctrl Pts',(-26.0145189275733,-67.083301065264,
0.));
#134031=CARTESIAN_POINT('Ctrl Pts',(-26.0145189275733,-67.083301065264,
12.));
#134032=CARTESIAN_POINT('Ctrl Pts',(-25.9988112951818,-67.0652697790335,
0.));
#134033=CARTESIAN_POINT('Ctrl Pts',(-25.9988112951818,-67.0652697790335,
12.));
#134034=CARTESIAN_POINT('Ctrl Pts',(-25.9831492744988,-67.0472552888495,
0.));
#134035=CARTESIAN_POINT('Ctrl Pts',(-25.9831492744988,-67.0472552888495,
12.));
#134036=CARTESIAN_POINT('Ctrl Pts',(-25.9675328984123,-67.0292577267495,
0.));
#134037=CARTESIAN_POINT('Ctrl Pts',(-25.9675328984123,-67.0292577267495,
12.));
#134038=CARTESIAN_POINT('Ctrl Pts',(-25.9519621998598,-67.0112772253553,
0.));
#134039=CARTESIAN_POINT('Ctrl Pts',(-25.9519621998598,-67.0112772253553,
12.));
#134040=CARTESIAN_POINT('Ctrl Pts',(-25.9364372118216,-66.993313917876,
0.));
#134041=CARTESIAN_POINT('Ctrl Pts',(-25.9364372118216,-66.993313917876,
12.));
#134042=CARTESIAN_POINT('Ctrl Pts',(-25.9209579673198,-66.9753679381122,
0.));
#134043=CARTESIAN_POINT('Ctrl Pts',(-25.9209579673198,-66.9753679381122,
12.));
#134044=CARTESIAN_POINT('Ctrl Pts',(-25.9055244994267,-66.9574394204635,
0.));
#134045=CARTESIAN_POINT('Ctrl Pts',(-25.9055244994267,-66.9574394204635,
12.));
#134046=CARTESIAN_POINT('Ctrl Pts',(-25.8901368412655,-66.9395284999327,
0.));
#134047=CARTESIAN_POINT('Ctrl Pts',(-25.8901368412655,-66.9395284999327,
12.));
#134048=CARTESIAN_POINT('Ctrl Pts',(-25.8747950260114,-66.9216353121308,
0.));
#134049=CARTESIAN_POINT('Ctrl Pts',(-25.8747950260114,-66.9216353121308,
12.));
#134050=CARTESIAN_POINT('Ctrl Pts',(-25.8594990868845,-66.9037599932787,
0.));
#134051=CARTESIAN_POINT('Ctrl Pts',(-25.8594990868845,-66.9037599932787,
12.));
#134052=CARTESIAN_POINT('Ctrl Pts',(-25.8442490571486,-66.8859026802123,
0.));
#134053=CARTESIAN_POINT('Ctrl Pts',(-25.8442490571486,-66.8859026802123,
12.));
#134054=CARTESIAN_POINT('Ctrl Pts',(-25.8290449701207,-66.8680635103907,
0.));
#134055=CARTESIAN_POINT('Ctrl Pts',(-25.8290449701207,-66.8680635103907,
12.));
#134056=CARTESIAN_POINT('Ctrl Pts',(-25.8138868591715,-66.8502426219015,
0.));
#134057=CARTESIAN_POINT('Ctrl Pts',(-25.8138868591715,-66.8502426219015,
12.));
#134058=CARTESIAN_POINT('Ctrl Pts',(-25.7987747577265,-66.8324401534657,
0.));
#134059=CARTESIAN_POINT('Ctrl Pts',(-25.7987747577265,-66.8324401534657,
12.));
#134060=CARTESIAN_POINT('Ctrl Pts',(-25.783708699258,-66.8146562444397,
0.));
#134061=CARTESIAN_POINT('Ctrl Pts',(-25.783708699258,-66.8146562444397,
12.));
#134062=CARTESIAN_POINT('Ctrl Pts',(-25.7686887172859,-66.7968910348199,
0.));
#134063=CARTESIAN_POINT('Ctrl Pts',(-25.7686887172859,-66.7968910348199,
12.));
#134064=CARTESIAN_POINT('Ctrl Pts',(-25.7537148453848,-66.7791446652505,
0.));
#134065=CARTESIAN_POINT('Ctrl Pts',(-25.7537148453848,-66.7791446652505,
12.));
#134066=CARTESIAN_POINT('Ctrl Pts',(-25.7387871171861,-66.7614172770302,
0.));
#134067=CARTESIAN_POINT('Ctrl Pts',(-25.7387871171861,-66.7614172770302,
12.));
#134068=CARTESIAN_POINT('Ctrl Pts',(-25.7239055663778,-66.7437090121168,
0.));
#134069=CARTESIAN_POINT('Ctrl Pts',(-25.7239055663778,-66.7437090121168,
12.));
#134070=CARTESIAN_POINT('Ctrl Pts',(-25.7090702266976,-66.72602001313,0.));
#134071=CARTESIAN_POINT('Ctrl Pts',(-25.7090702266976,-66.72602001313,12.));
#134072=CARTESIAN_POINT('Ctrl Pts',(-25.6942811319337,-66.7083504233566,
0.));
#134073=CARTESIAN_POINT('Ctrl Pts',(-25.6942811319337,-66.7083504233566,
12.));
#134074=CARTESIAN_POINT('Ctrl Pts',(-25.679538315933,-66.6907003867599,
0.));
#134075=CARTESIAN_POINT('Ctrl Pts',(-25.679538315933,-66.6907003867599,
12.));
#134076=CARTESIAN_POINT('Ctrl Pts',(-25.6648418126016,-66.6730700479843,
0.));
#134077=CARTESIAN_POINT('Ctrl Pts',(-25.6648418126016,-66.6730700479843,
12.));
#134078=CARTESIAN_POINT('Ctrl Pts',(-25.6501916559051,-66.6554595523611,
0.));
#134079=CARTESIAN_POINT('Ctrl Pts',(-25.6501916559051,-66.6554595523611,
12.));
#134080=CARTESIAN_POINT('Ctrl Pts',(-25.6355878798605,-66.6378690459105,
0.));
#134081=CARTESIAN_POINT('Ctrl Pts',(-25.6355878798605,-66.6378690459105,
12.));
#134082=CARTESIAN_POINT('Ctrl Pts',(-25.6210305185395,-66.6202986753482,
0.));
#134083=CARTESIAN_POINT('Ctrl Pts',(-25.6210305185395,-66.6202986753482,
12.));
#134084=CARTESIAN_POINT('Ctrl Pts',(-25.606519606075,-66.6027485880947,
0.));
#134085=CARTESIAN_POINT('Ctrl Pts',(-25.606519606075,-66.6027485880947,
12.));
#134086=CARTESIAN_POINT('Ctrl Pts',(-25.5920551766629,-66.585218932281,
0.));
#134087=CARTESIAN_POINT('Ctrl Pts',(-25.5920551766629,-66.585218932281,
12.));
#134088=CARTESIAN_POINT('Ctrl Pts',(-25.5776372645605,-66.567709856755,
0.));
#134089=CARTESIAN_POINT('Ctrl Pts',(-25.5776372645605,-66.567709856755,
12.));
#134090=CARTESIAN_POINT('Ctrl Pts',(-25.5632659040797,-66.5502215110843,
0.));
#134091=CARTESIAN_POINT('Ctrl Pts',(-25.5632659040797,-66.5502215110843,
12.));
#134092=CARTESIAN_POINT('Ctrl Pts',(-25.5489411295916,-66.5327540455638,
0.));
#134093=CARTESIAN_POINT('Ctrl Pts',(-25.5489411295916,-66.5327540455638,
12.));
#134094=CARTESIAN_POINT('Ctrl Pts',(-25.5346629755322,-66.5153076112237,
0.));
#134095=CARTESIAN_POINT('Ctrl Pts',(-25.5346629755322,-66.5153076112237,
12.));
#134096=CARTESIAN_POINT('Ctrl Pts',(-25.5204314764033,-66.4978823598352,
0.));
#134097=CARTESIAN_POINT('Ctrl Pts',(-25.5204314764033,-66.4978823598352,
12.));
#134098=CARTESIAN_POINT('Ctrl Pts',(-25.5062466667703,-66.4804784439146,
0.));
#134099=CARTESIAN_POINT('Ctrl Pts',(-25.5062466667703,-66.4804784439146,
12.));
#134100=CARTESIAN_POINT('Ctrl Pts',(-25.4921085812548,-66.463096016725,
0.));
#134101=CARTESIAN_POINT('Ctrl Pts',(-25.4921085812548,-66.463096016725,
12.));
#134102=CARTESIAN_POINT('Ctrl Pts',(-25.4780172545418,-66.445735232287,
0.));
#134103=CARTESIAN_POINT('Ctrl Pts',(-25.4780172545418,-66.445735232287,
12.));
#134104=CARTESIAN_POINT('Ctrl Pts',(-25.463972721385,-66.4283962453899,
0.));
#134105=CARTESIAN_POINT('Ctrl Pts',(-25.463972721385,-66.4283962453899,
12.));
#134106=CARTESIAN_POINT('Ctrl Pts',(-25.4499750166079,-66.4110792116,0.));
#134107=CARTESIAN_POINT('Ctrl Pts',(-25.4499750166079,-66.4110792116,12.));
#134108=CARTESIAN_POINT('Ctrl Pts',(-25.4360241751017,-66.3937842872684,
0.));
#134109=CARTESIAN_POINT('Ctrl Pts',(-25.4360241751017,-66.3937842872684,
12.));
#134110=CARTESIAN_POINT('Ctrl Pts',(-25.4221202318198,-66.3765116295363,
0.));
#134111=CARTESIAN_POINT('Ctrl Pts',(-25.4221202318198,-66.3765116295363,
12.));
#134112=CARTESIAN_POINT('Ctrl Pts',(-25.4082632217846,-66.3592613963407,
0.));
#134113=CARTESIAN_POINT('Ctrl Pts',(-25.4082632217846,-66.3592613963407,
12.));
#134114=CARTESIAN_POINT('Ctrl Pts',(-25.3944531800901,-66.3420337464176,
0.));
#134115=CARTESIAN_POINT('Ctrl Pts',(-25.3944531800901,-66.3420337464176,
12.));
#134116=CARTESIAN_POINT('Ctrl Pts',(-25.3806901419013,-66.3248288393046,
0.));
#134117=CARTESIAN_POINT('Ctrl Pts',(-25.3806901419013,-66.3248288393046,
12.));
#134118=CARTESIAN_POINT('Ctrl Pts',(-25.3669741424491,-66.3076468353417,
0.));
#134119=CARTESIAN_POINT('Ctrl Pts',(-25.3669741424491,-66.3076468353417,
12.));
#134120=CARTESIAN_POINT('Ctrl Pts',(-25.3533052170254,-66.2904878956721,
0.));
#134121=CARTESIAN_POINT('Ctrl Pts',(-25.3533052170254,-66.2904878956721,
12.));
#134122=CARTESIAN_POINT('Ctrl Pts',(-25.3396834009955,-66.2733521822675,
0.));
#134123=CARTESIAN_POINT('Ctrl Pts',(-25.3396834009955,-66.2733521822675,
12.));
#134124=CARTESIAN_POINT('Ctrl Pts',(-25.326108729803,-66.2562398579479,
0.));
#134125=CARTESIAN_POINT('Ctrl Pts',(-25.326108729803,-66.2562398579479,
12.));
#134126=CARTESIAN_POINT('Ctrl Pts',(-25.3125812389728,-66.2391510863992,
0.));
#134127=CARTESIAN_POINT('Ctrl Pts',(-25.3125812389728,-66.2391510863992,
12.));
#134128=CARTESIAN_POINT('Ctrl Pts',(-25.2991009641087,-66.222086032193,
0.));
#134129=CARTESIAN_POINT('Ctrl Pts',(-25.2991009641087,-66.222086032193,
12.));
#134130=CARTESIAN_POINT('Ctrl Pts',(-25.2856679408921,-66.2050448607883,
0.));
#134131=CARTESIAN_POINT('Ctrl Pts',(-25.2856679408921,-66.2050448607883,
12.));
#134132=CARTESIAN_POINT('Ctrl Pts',(-25.2722822050829,-66.1880277385113,
0.));
#134133=CARTESIAN_POINT('Ctrl Pts',(-25.2722822050829,-66.1880277385113,
12.));
#134134=CARTESIAN_POINT('Ctrl Pts',(-25.2589437925145,-66.1710348325378,
0.));
#134135=CARTESIAN_POINT('Ctrl Pts',(-25.2589437925145,-66.1710348325378,
12.));
#134136=CARTESIAN_POINT('Ctrl Pts',(-25.245652739088,-66.1540663108767,
0.));
#134137=CARTESIAN_POINT('Ctrl Pts',(-25.245652739088,-66.1540663108767,
12.));
#134138=CARTESIAN_POINT('Ctrl Pts',(-25.2324090807561,-66.1371223423371,
0.));
#134139=CARTESIAN_POINT('Ctrl Pts',(-25.2324090807561,-66.1371223423371,
12.));
#134140=CARTESIAN_POINT('Ctrl Pts',(-25.2192128535367,-66.1202030965784,
0.));
#134141=CARTESIAN_POINT('Ctrl Pts',(-25.2192128535367,-66.1202030965784,
12.));
#134142=CARTESIAN_POINT('Ctrl Pts',(-25.2060640935371,-66.1033087441916,
0.));
#134143=CARTESIAN_POINT('Ctrl Pts',(-25.2060640935371,-66.1033087441916,
12.));
#134144=CARTESIAN_POINT('Ctrl Pts',(-25.1929628369685,-66.086439456768,
0.));
#134145=CARTESIAN_POINT('Ctrl Pts',(-25.1929628369685,-66.086439456768,
12.));
#134146=CARTESIAN_POINT('Ctrl Pts',(-25.1799091201594,-66.0695954069698,
0.));
#134147=CARTESIAN_POINT('Ctrl Pts',(-25.1799091201594,-66.0695954069698,
12.));
#134148=CARTESIAN_POINT('Ctrl Pts',(-25.1669029795652,-66.0527767686,0.));
#134149=CARTESIAN_POINT('Ctrl Pts',(-25.1669029795652,-66.0527767686,12.));
#134150=CARTESIAN_POINT('Ctrl Pts',(-25.153944451741,-66.0359837164709,
0.));
#134151=CARTESIAN_POINT('Ctrl Pts',(-25.153944451741,-66.0359837164709,
12.));
#134152=CARTESIAN_POINT('Ctrl Pts',(-25.1410335733094,-66.0192164262607,
0.));
#134153=CARTESIAN_POINT('Ctrl Pts',(-25.1410335733094,-66.0192164262607,
12.));
#134154=CARTESIAN_POINT('Ctrl Pts',(-25.12817038093,-66.0024750743902,0.));
#134155=CARTESIAN_POINT('Ctrl Pts',(-25.12817038093,-66.0024750743902,12.));
#134156=CARTESIAN_POINT('Ctrl Pts',(-25.1153549112512,-65.9857598378455,
0.));
#134157=CARTESIAN_POINT('Ctrl Pts',(-25.1153549112512,-65.9857598378455,
12.));
#134158=CARTESIAN_POINT('Ctrl Pts',(-25.1025872009016,-65.9690708941591,
0.));
#134159=CARTESIAN_POINT('Ctrl Pts',(-25.1025872009016,-65.9690708941591,
12.));
#134160=CARTESIAN_POINT('Ctrl Pts',(-25.0898672865926,-65.9524084218167,
0.));
#134161=CARTESIAN_POINT('Ctrl Pts',(-25.0898672865926,-65.9524084218167,
12.));
#134162=CARTESIAN_POINT('Ctrl Pts',(-25.0771952052033,-65.9357726006174,
0.));
#134163=CARTESIAN_POINT('Ctrl Pts',(-25.0771952052033,-65.9357726006174,
12.));
#134164=CARTESIAN_POINT('Ctrl Pts',(-25.0645709938519,-65.9191636119796,
0.));
#134165=CARTESIAN_POINT('Ctrl Pts',(-25.0645709938519,-65.9191636119796,
12.));
#134166=CARTESIAN_POINT('Ctrl Pts',(-25.0519946900066,-65.9025816394391,
0.));
#134167=CARTESIAN_POINT('Ctrl Pts',(-25.0519946900066,-65.9025816394391,
12.));
#134168=CARTESIAN_POINT('Ctrl Pts',(-25.039466331404,-65.8860268683088,
0.));
#134169=CARTESIAN_POINT('Ctrl Pts',(-25.039466331404,-65.8860268683088,
12.));
#134170=CARTESIAN_POINT('Ctrl Pts',(-25.0269859558351,-65.8694994847586,
0.));
#134171=CARTESIAN_POINT('Ctrl Pts',(-25.0269859558351,-65.8694994847586,
12.));
#134172=CARTESIAN_POINT('Ctrl Pts',(-25.0145536009603,-65.8529996750441,
0.));
#134173=CARTESIAN_POINT('Ctrl Pts',(-25.0145536009603,-65.8529996750441,
12.));
#134174=CARTESIAN_POINT('Ctrl Pts',(-25.0021693041181,-65.8365276247157,
0.));
#134175=CARTESIAN_POINT('Ctrl Pts',(-25.0021693041181,-65.8365276247157,
12.));
#134176=CARTESIAN_POINT('Ctrl Pts',(-24.9898331021002,-65.8200835177071,
0.));
#134177=CARTESIAN_POINT('Ctrl Pts',(-24.9898331021002,-65.8200835177071,
12.));
#134178=CARTESIAN_POINT('Ctrl Pts',(-24.97754503157,-65.8036675380761,0.));
#134179=CARTESIAN_POINT('Ctrl Pts',(-24.97754503157,-65.8036675380761,12.));
#134180=CARTESIAN_POINT('Ctrl Pts',(-24.965305129559,-65.7872798720847,
0.));
#134181=CARTESIAN_POINT('Ctrl Pts',(-24.965305129559,-65.7872798720847,
12.));
#134182=CARTESIAN_POINT('Ctrl Pts',(-24.9531134338693,-65.7709207098949,
0.));
#134183=CARTESIAN_POINT('Ctrl Pts',(-24.9531134338693,-65.7709207098949,
12.));
#134184=CARTESIAN_POINT('Ctrl Pts',(-24.9409699836523,-65.7545902480286,
0.));
#134185=CARTESIAN_POINT('Ctrl Pts',(-24.9409699836523,-65.7545902480286,
12.));
#134186=CARTESIAN_POINT('Ctrl Pts',(-24.9288748194562,-65.7382886895839,
0.));
#134187=CARTESIAN_POINT('Ctrl Pts',(-24.9288748194562,-65.7382886895839,
12.));
#134188=CARTESIAN_POINT('Ctrl Pts',(-24.9168279820093,-65.7220162391016,
0.));
#134189=CARTESIAN_POINT('Ctrl Pts',(-24.9168279820093,-65.7220162391016,
12.));
#134190=CARTESIAN_POINT('Ctrl Pts',(-24.9048295111444,-65.7057730980471,
0.));
#134191=CARTESIAN_POINT('Ctrl Pts',(-24.9048295111444,-65.7057730980471,
12.));
#134192=CARTESIAN_POINT('Ctrl Pts',(-24.8928794448616,-65.6895594608798,
0.));
#134193=CARTESIAN_POINT('Ctrl Pts',(-24.8928794448616,-65.6895594608798,
12.));
#134194=CARTESIAN_POINT('Ctrl Pts',(-24.8809778178248,-65.6733755087723,
0.));
#134195=CARTESIAN_POINT('Ctrl Pts',(-24.8809778178248,-65.6733755087723,
12.));
#134196=CARTESIAN_POINT('Ctrl Pts',(-24.8691246628081,-65.6572214156761,
0.));
#134197=CARTESIAN_POINT('Ctrl Pts',(-24.8691246628081,-65.6572214156761,
12.));
#134198=CARTESIAN_POINT('Ctrl Pts',(-24.8573200135684,-65.6410973603713,
0.));
#134199=CARTESIAN_POINT('Ctrl Pts',(-24.8573200135684,-65.6410973603713,
12.));
#134200=CARTESIAN_POINT('Ctrl Pts',(-24.8455639071517,-65.6250035361612,
0.));
#134201=CARTESIAN_POINT('Ctrl Pts',(-24.8455639071517,-65.6250035361612,
12.));
#134202=CARTESIAN_POINT('Ctrl Pts',(-24.8338563866739,-65.6089401625551,
0.));
#134203=CARTESIAN_POINT('Ctrl Pts',(-24.8338563866739,-65.6089401625551,
12.));
#134204=CARTESIAN_POINT('Ctrl Pts',(-24.8221975032059,-65.5929074932487,
0.));
#134205=CARTESIAN_POINT('Ctrl Pts',(-24.8221975032059,-65.5929074932487,
12.));
#134206=CARTESIAN_POINT('Ctrl Pts',(-24.8105873098578,-65.5769057914184,
0.));
#134207=CARTESIAN_POINT('Ctrl Pts',(-24.8105873098578,-65.5769057914184,
12.));
#134208=CARTESIAN_POINT('Ctrl Pts',(-24.7990258561234,-65.5609353062749,
0.));
#134209=CARTESIAN_POINT('Ctrl Pts',(-24.7990258561234,-65.5609353062749,
12.));
#134210=CARTESIAN_POINT('Ctrl Pts',(-24.7875131827515,-65.5449962514735,
0.));
#134211=CARTESIAN_POINT('Ctrl Pts',(-24.7875131827515,-65.5449962514735,
12.));
#134212=CARTESIAN_POINT('Ctrl Pts',(-24.7760493148551,-65.5290887770493,
0.));
#134213=CARTESIAN_POINT('Ctrl Pts',(-24.7760493148551,-65.5290887770493,
12.));
#134214=CARTESIAN_POINT('Ctrl Pts',(-24.7646342620969,-65.5132129675727,
0.));
#134215=CARTESIAN_POINT('Ctrl Pts',(-24.7646342620969,-65.5132129675727,
12.));
#134216=CARTESIAN_POINT('Ctrl Pts',(-24.7555412724771,-65.5005376841469,
0.));
#134217=CARTESIAN_POINT('Ctrl Pts',(-24.7555412724771,-65.5005376841469,
12.));
#134218=CARTESIAN_POINT('Ctrl Pts',(-24.7487434956058,-65.4910454936487,
0.));
#134219=CARTESIAN_POINT('Ctrl Pts',(-24.7487434956058,-65.4910454936487,
12.));
#134220=CARTESIAN_POINT('Ctrl Pts',(-24.7442214063411,-65.484723709553,
0.));
#134221=CARTESIAN_POINT('Ctrl Pts',(-24.7442214063411,-65.484723709553,
12.));
#134222=CARTESIAN_POINT('Ctrl Pts',(-24.7419628022042,-65.4815644032299,
0.));
#134223=CARTESIAN_POINT('Ctrl Pts',(-24.7419628022042,-65.4815644032299,
12.));
#134224=CARTESIAN_POINT('',(-24.7419628022042,-65.4815644032299,12.));
#134225=CARTESIAN_POINT('Ctrl Pts',(-24.7419628022042,-65.4815644032299,
12.));
#134226=CARTESIAN_POINT('Ctrl Pts',(-24.7442214063411,-65.484723709553,
12.));
#134227=CARTESIAN_POINT('Ctrl Pts',(-24.7487434956058,-65.4910454936487,
12.));
#134228=CARTESIAN_POINT('Ctrl Pts',(-24.7555412724771,-65.5005376841469,
12.));
#134229=CARTESIAN_POINT('Ctrl Pts',(-24.7646342620969,-65.5132129675727,
12.));
#134230=CARTESIAN_POINT('Ctrl Pts',(-24.7760493148551,-65.5290887770493,
12.));
#134231=CARTESIAN_POINT('Ctrl Pts',(-24.7875131827515,-65.5449962514735,
12.));
#134232=CARTESIAN_POINT('Ctrl Pts',(-24.7990258561234,-65.5609353062749,
12.));
#134233=CARTESIAN_POINT('Ctrl Pts',(-24.8105873098578,-65.5769057914184,
12.));
#134234=CARTESIAN_POINT('Ctrl Pts',(-24.8221975032059,-65.5929074932487,
12.));
#134235=CARTESIAN_POINT('Ctrl Pts',(-24.8338563866739,-65.6089401625551,
12.));
#134236=CARTESIAN_POINT('Ctrl Pts',(-24.8455639071517,-65.6250035361612,
12.));
#134237=CARTESIAN_POINT('Ctrl Pts',(-24.8573200135684,-65.6410973603713,
12.));
#134238=CARTESIAN_POINT('Ctrl Pts',(-24.8691246628081,-65.6572214156761,
12.));
#134239=CARTESIAN_POINT('Ctrl Pts',(-24.8809778178248,-65.6733755087723,
12.));
#134240=CARTESIAN_POINT('Ctrl Pts',(-24.8928794448616,-65.6895594608798,
12.));
#134241=CARTESIAN_POINT('Ctrl Pts',(-24.9048295111444,-65.7057730980471,
12.));
#134242=CARTESIAN_POINT('Ctrl Pts',(-24.9168279820093,-65.7220162391016,
12.));
#134243=CARTESIAN_POINT('Ctrl Pts',(-24.9288748194562,-65.7382886895839,
12.));
#134244=CARTESIAN_POINT('Ctrl Pts',(-24.9409699836523,-65.7545902480286,
12.));
#134245=CARTESIAN_POINT('Ctrl Pts',(-24.9531134338693,-65.7709207098949,
12.));
#134246=CARTESIAN_POINT('Ctrl Pts',(-24.965305129559,-65.7872798720847,
12.));
#134247=CARTESIAN_POINT('Ctrl Pts',(-24.97754503157,-65.8036675380761,12.));
#134248=CARTESIAN_POINT('Ctrl Pts',(-24.9898331021002,-65.8200835177071,
12.));
#134249=CARTESIAN_POINT('Ctrl Pts',(-25.0021693041181,-65.8365276247157,
12.));
#134250=CARTESIAN_POINT('Ctrl Pts',(-25.0145536009603,-65.8529996750441,
12.));
#134251=CARTESIAN_POINT('Ctrl Pts',(-25.0269859558351,-65.8694994847586,
12.));
#134252=CARTESIAN_POINT('Ctrl Pts',(-25.039466331404,-65.8860268683088,
12.));
#134253=CARTESIAN_POINT('Ctrl Pts',(-25.0519946900066,-65.9025816394391,
12.));
#134254=CARTESIAN_POINT('Ctrl Pts',(-25.0645709938519,-65.9191636119796,
12.));
#134255=CARTESIAN_POINT('Ctrl Pts',(-25.0771952052033,-65.9357726006174,
12.));
#134256=CARTESIAN_POINT('Ctrl Pts',(-25.0898672865926,-65.9524084218167,
12.));
#134257=CARTESIAN_POINT('Ctrl Pts',(-25.1025872009016,-65.9690708941591,
12.));
#134258=CARTESIAN_POINT('Ctrl Pts',(-25.1153549112512,-65.9857598378455,
12.));
#134259=CARTESIAN_POINT('Ctrl Pts',(-25.12817038093,-66.0024750743902,12.));
#134260=CARTESIAN_POINT('Ctrl Pts',(-25.1410335733094,-66.0192164262607,
12.));
#134261=CARTESIAN_POINT('Ctrl Pts',(-25.153944451741,-66.0359837164709,
12.));
#134262=CARTESIAN_POINT('Ctrl Pts',(-25.1669029795652,-66.0527767686,12.));
#134263=CARTESIAN_POINT('Ctrl Pts',(-25.1799091201594,-66.0695954069698,
12.));
#134264=CARTESIAN_POINT('Ctrl Pts',(-25.1929628369685,-66.086439456768,
12.));
#134265=CARTESIAN_POINT('Ctrl Pts',(-25.2060640935371,-66.1033087441916,
12.));
#134266=CARTESIAN_POINT('Ctrl Pts',(-25.2192128535367,-66.1202030965784,
12.));
#134267=CARTESIAN_POINT('Ctrl Pts',(-25.2324090807561,-66.1371223423371,
12.));
#134268=CARTESIAN_POINT('Ctrl Pts',(-25.245652739088,-66.1540663108767,
12.));
#134269=CARTESIAN_POINT('Ctrl Pts',(-25.2589437925145,-66.1710348325378,
12.));
#134270=CARTESIAN_POINT('Ctrl Pts',(-25.2722822050829,-66.1880277385113,
12.));
#134271=CARTESIAN_POINT('Ctrl Pts',(-25.2856679408921,-66.2050448607883,
12.));
#134272=CARTESIAN_POINT('Ctrl Pts',(-25.2991009641087,-66.222086032193,
12.));
#134273=CARTESIAN_POINT('Ctrl Pts',(-25.3125812389728,-66.2391510863992,
12.));
#134274=CARTESIAN_POINT('Ctrl Pts',(-25.326108729803,-66.2562398579479,
12.));
#134275=CARTESIAN_POINT('Ctrl Pts',(-25.3396834009955,-66.2733521822675,
12.));
#134276=CARTESIAN_POINT('Ctrl Pts',(-25.3533052170254,-66.2904878956721,
12.));
#134277=CARTESIAN_POINT('Ctrl Pts',(-25.3669741424491,-66.3076468353417,
12.));
#134278=CARTESIAN_POINT('Ctrl Pts',(-25.3806901419013,-66.3248288393046,
12.));
#134279=CARTESIAN_POINT('Ctrl Pts',(-25.3944531800901,-66.3420337464176,
12.));
#134280=CARTESIAN_POINT('Ctrl Pts',(-25.4082632217846,-66.3592613963407,
12.));
#134281=CARTESIAN_POINT('Ctrl Pts',(-25.4221202318198,-66.3765116295363,
12.));
#134282=CARTESIAN_POINT('Ctrl Pts',(-25.4360241751017,-66.3937842872684,
12.));
#134283=CARTESIAN_POINT('Ctrl Pts',(-25.4499750166079,-66.4110792116,12.));
#134284=CARTESIAN_POINT('Ctrl Pts',(-25.463972721385,-66.4283962453899,
12.));
#134285=CARTESIAN_POINT('Ctrl Pts',(-25.4780172545418,-66.445735232287,
12.));
#134286=CARTESIAN_POINT('Ctrl Pts',(-25.4921085812548,-66.463096016725,
12.));
#134287=CARTESIAN_POINT('Ctrl Pts',(-25.5062466667703,-66.4804784439146,
12.));
#134288=CARTESIAN_POINT('Ctrl Pts',(-25.5204314764033,-66.4978823598352,
12.));
#134289=CARTESIAN_POINT('Ctrl Pts',(-25.5346629755322,-66.5153076112237,
12.));
#134290=CARTESIAN_POINT('Ctrl Pts',(-25.5489411295916,-66.5327540455638,
12.));
#134291=CARTESIAN_POINT('Ctrl Pts',(-25.5632659040797,-66.5502215110843,
12.));
#134292=CARTESIAN_POINT('Ctrl Pts',(-25.5776372645605,-66.567709856755,
12.));
#134293=CARTESIAN_POINT('Ctrl Pts',(-25.5920551766629,-66.585218932281,
12.));
#134294=CARTESIAN_POINT('Ctrl Pts',(-25.606519606075,-66.6027485880947,
12.));
#134295=CARTESIAN_POINT('Ctrl Pts',(-25.6210305185395,-66.6202986753482,
12.));
#134296=CARTESIAN_POINT('Ctrl Pts',(-25.6355878798605,-66.6378690459105,
12.));
#134297=CARTESIAN_POINT('Ctrl Pts',(-25.6501916559051,-66.6554595523611,
12.));
#134298=CARTESIAN_POINT('Ctrl Pts',(-25.6648418126016,-66.6730700479843,
12.));
#134299=CARTESIAN_POINT('Ctrl Pts',(-25.679538315933,-66.6907003867599,
12.));
#134300=CARTESIAN_POINT('Ctrl Pts',(-25.6942811319337,-66.7083504233566,
12.));
#134301=CARTESIAN_POINT('Ctrl Pts',(-25.7090702266976,-66.72602001313,12.));
#134302=CARTESIAN_POINT('Ctrl Pts',(-25.7239055663778,-66.7437090121168,
12.));
#134303=CARTESIAN_POINT('Ctrl Pts',(-25.7387871171861,-66.7614172770302,
12.));
#134304=CARTESIAN_POINT('Ctrl Pts',(-25.7537148453848,-66.7791446652505,
12.));
#134305=CARTESIAN_POINT('Ctrl Pts',(-25.7686887172859,-66.7968910348199,
12.));
#134306=CARTESIAN_POINT('Ctrl Pts',(-25.783708699258,-66.8146562444397,
12.));
#134307=CARTESIAN_POINT('Ctrl Pts',(-25.7987747577265,-66.8324401534657,
12.));
#134308=CARTESIAN_POINT('Ctrl Pts',(-25.8138868591715,-66.8502426219015,
12.));
#134309=CARTESIAN_POINT('Ctrl Pts',(-25.8290449701207,-66.8680635103907,
12.));
#134310=CARTESIAN_POINT('Ctrl Pts',(-25.8442490571486,-66.8859026802123,
12.));
#134311=CARTESIAN_POINT('Ctrl Pts',(-25.8594990868845,-66.9037599932787,
12.));
#134312=CARTESIAN_POINT('Ctrl Pts',(-25.8747950260114,-66.9216353121308,
12.));
#134313=CARTESIAN_POINT('Ctrl Pts',(-25.8901368412655,-66.9395284999327,
12.));
#134314=CARTESIAN_POINT('Ctrl Pts',(-25.9055244994267,-66.9574394204635,
12.));
#134315=CARTESIAN_POINT('Ctrl Pts',(-25.9209579673198,-66.9753679381122,
12.));
#134316=CARTESIAN_POINT('Ctrl Pts',(-25.9364372118216,-66.993313917876,
12.));
#134317=CARTESIAN_POINT('Ctrl Pts',(-25.9519621998598,-67.0112772253553,
12.));
#134318=CARTESIAN_POINT('Ctrl Pts',(-25.9675328984123,-67.0292577267495,
12.));
#134319=CARTESIAN_POINT('Ctrl Pts',(-25.9831492744988,-67.0472552888495,
12.));
#134320=CARTESIAN_POINT('Ctrl Pts',(-25.9988112951818,-67.0652697790335,
12.));
#134321=CARTESIAN_POINT('Ctrl Pts',(-26.0145189275733,-67.083301065264,
12.));
#134322=CARTESIAN_POINT('Ctrl Pts',(-26.030272138834,-67.101349016084,12.));
#134323=CARTESIAN_POINT('Ctrl Pts',(-26.0460708961725,-67.1194135006121,
12.));
#134324=CARTESIAN_POINT('Ctrl Pts',(-26.0619151668361,-67.1374943885353,
12.));
#134325=CARTESIAN_POINT('Ctrl Pts',(-26.077804918113,-67.1555915501052,
12.));
#134326=CARTESIAN_POINT('Ctrl Pts',(-26.0937401173385,-67.1737048561364,
12.));
#134327=CARTESIAN_POINT('Ctrl Pts',(-26.109720731895,-67.191834178002,12.));
#134328=CARTESIAN_POINT('Ctrl Pts',(-26.1257467292102,-67.2099793876295,
12.));
#134329=CARTESIAN_POINT('Ctrl Pts',(-26.1418180767487,-67.228140357493,
12.));
#134330=CARTESIAN_POINT('Ctrl Pts',(-26.1579347420135,-67.2463169606105,
12.));
#134331=CARTESIAN_POINT('Ctrl Pts',(-26.1740966925527,-67.2645090705414,
12.));
#134332=CARTESIAN_POINT('Ctrl Pts',(-26.1903038959589,-67.2827165613828,
12.));
#134333=CARTESIAN_POINT('Ctrl Pts',(-26.2065563198685,-67.3009393077654,
12.));
#134334=CARTESIAN_POINT('Ctrl Pts',(-26.2228539319528,-67.3191771848468,
12.));
#134335=CARTESIAN_POINT('Ctrl Pts',(-26.2391966999192,-67.3374300683075,
12.));
#134336=CARTESIAN_POINT('Ctrl Pts',(-26.255584591518,-67.3556978343506,
12.));
#134337=CARTESIAN_POINT('Ctrl Pts',(-26.2720175745423,-67.3739803596967,
12.));
#134338=CARTESIAN_POINT('Ctrl Pts',(-26.288495616827,-67.392277521581,12.));
#134339=CARTESIAN_POINT('Ctrl Pts',(-26.305018686241,-67.4105891977465,
12.));
#134340=CARTESIAN_POINT('Ctrl Pts',(-26.3215867506864,-67.4289152664406,
12.));
#134341=CARTESIAN_POINT('Ctrl Pts',(-26.3381997781059,-67.4472556064127,
12.));
#134342=CARTESIAN_POINT('Ctrl Pts',(-26.3548577364835,-67.4656100969121,
12.));
#134343=CARTESIAN_POINT('Ctrl Pts',(-26.3715605938432,-67.4839786176833,
12.));
#134344=CARTESIAN_POINT('Ctrl Pts',(-26.3883083182417,-67.5023610489611,
12.));
#134345=CARTESIAN_POINT('Ctrl Pts',(-26.4051008777669,-67.5207572714666,
12.));
#134346=CARTESIAN_POINT('Ctrl Pts',(-26.4219382405452,-67.5391671664055,
12.));
#134347=CARTESIAN_POINT('Ctrl Pts',(-26.4388203747422,-67.5575906154648,
12.));
#134348=CARTESIAN_POINT('Ctrl Pts',(-26.4557472485622,-67.5760275008096,
12.));
#134349=CARTESIAN_POINT('Ctrl Pts',(-26.4727188302415,-67.5944777050782,
12.));
#134350=CARTESIAN_POINT('Ctrl Pts',(-26.4897350880447,-67.6129411113774,
12.));
#134351=CARTESIAN_POINT('Ctrl Pts',(-26.5067959902731,-67.6314176032823,
12.));
#134352=CARTESIAN_POINT('Ctrl Pts',(-26.5239015052656,-67.6499070648323,
12.));
#134353=CARTESIAN_POINT('Ctrl Pts',(-26.5410516013984,-67.6684093805288,
12.));
#134354=CARTESIAN_POINT('Ctrl Pts',(-26.5582462470794,-67.6869244353292,
12.));
#134355=CARTESIAN_POINT('Ctrl Pts',(-26.5754854107422,-67.7054521146427,
12.));
#134356=CARTESIAN_POINT('Ctrl Pts',(-26.5927690608547,-67.7239923043295,
12.));
#134357=CARTESIAN_POINT('Ctrl Pts',(-26.6100971659205,-67.7425448906983,
12.));
#134358=CARTESIAN_POINT('Ctrl Pts',(-26.6274696944793,-67.7611097605042,
12.));
#134359=CARTESIAN_POINT('Ctrl Pts',(-26.6448866151027,-67.7796868009447,
12.));
#134360=CARTESIAN_POINT('Ctrl Pts',(-26.6623478963867,-67.7982758996557,
12.));
#134361=CARTESIAN_POINT('Ctrl Pts',(-26.6798535069586,-67.8168769447086,
12.));
#134362=CARTESIAN_POINT('Ctrl Pts',(-26.6974034154803,-67.8354898246079,
12.));
#134363=CARTESIAN_POINT('Ctrl Pts',(-26.7149975906478,-67.8541144282875,
12.));
#134364=CARTESIAN_POINT('Ctrl Pts',(-26.7326360011886,-67.8727506451067,
12.));
#134365=CARTESIAN_POINT('Ctrl Pts',(-26.7503186158523,-67.8913983648441,
12.));
#134366=CARTESIAN_POINT('Ctrl Pts',(-26.7680454034169,-67.9100574776974,
12.));
#134367=CARTESIAN_POINT('Ctrl Pts',(-26.7858163326933,-67.9287278742839,
12.));
#134368=CARTESIAN_POINT('Ctrl Pts',(-26.8036313725262,-67.9474094456395,
12.));
#134369=CARTESIAN_POINT('Ctrl Pts',(-26.8214904917922,-67.9661020832165,
12.));
#134370=CARTESIAN_POINT('Ctrl Pts',(-26.8393936593914,-67.9848056788814,
12.));
#134371=CARTESIAN_POINT('Ctrl Pts',(-26.85734084425,-68.0035201249108,12.));
#134372=CARTESIAN_POINT('Ctrl Pts',(-26.8753320153255,-68.0222453139862,
12.));
#134373=CARTESIAN_POINT('Ctrl Pts',(-26.8933671416065,-68.0409811391871,
12.));
#134374=CARTESIAN_POINT('Ctrl Pts',(-26.9114461921109,-68.0597274939857,
12.));
#134375=CARTESIAN_POINT('Ctrl Pts',(-26.9295691358775,-68.0784842722362,
12.));
#134376=CARTESIAN_POINT('Ctrl Pts',(-26.9477359419646,-68.0972513681739,
12.));
#134377=CARTESIAN_POINT('Ctrl Pts',(-26.9659465794596,-68.1160286764244,
12.));
#134378=CARTESIAN_POINT('Ctrl Pts',(-26.9842010174819,-68.13481609201,12.));
#134379=CARTESIAN_POINT('Ctrl Pts',(-27.0024992251839,-68.1536135103558,
12.));
#134380=CARTESIAN_POINT('Ctrl Pts',(-27.0208411717477,-68.1724208272967,
12.));
#134381=CARTESIAN_POINT('Ctrl Pts',(-27.0392268263805,-68.1912379390786,
12.));
#134382=CARTESIAN_POINT('Ctrl Pts',(-27.0576561583179,-68.2100647423345,
12.));
#134383=CARTESIAN_POINT('Ctrl Pts',(-27.076129136823,-68.2289011340624,
12.));
#134384=CARTESIAN_POINT('Ctrl Pts',(-27.0946457311814,-68.2477470116014,
12.));
#134385=CARTESIAN_POINT('Ctrl Pts',(-27.1132059106939,-68.2666022726094,
12.));
#134386=CARTESIAN_POINT('Ctrl Pts',(-27.1318096446643,-68.285466815035,
12.));
#134387=CARTESIAN_POINT('Ctrl Pts',(-27.1504569024131,-68.3043405371589,
12.));
#134388=CARTESIAN_POINT('Ctrl Pts',(-27.1691476532917,-68.3232233376415,
12.));
#134389=CARTESIAN_POINT('Ctrl Pts',(-27.1878818666925,-68.3421151155708,
12.));
#134390=CARTESIAN_POINT('Ctrl Pts',(-27.2066595120544,-68.3610157704999,
12.));
#134391=CARTESIAN_POINT('Ctrl Pts',(-27.2254805588677,-68.379925202511,
12.));
#134392=CARTESIAN_POINT('Ctrl Pts',(-27.2443449766654,-68.3988433121589,
12.));
#134393=CARTESIAN_POINT('Ctrl Pts',(-27.2632527350062,-68.4177700003471,
12.));
#134394=CARTESIAN_POINT('Ctrl Pts',(-27.2822038034539,-68.4367051682166,
12.));
#134395=CARTESIAN_POINT('Ctrl Pts',(-27.301198151557,-68.455648717044,12.));
#134396=CARTESIAN_POINT('Ctrl Pts',(-27.3202357488153,-68.4746005480992,
12.));
#134397=CARTESIAN_POINT('Ctrl Pts',(-27.3393165646748,-68.4935605626361,
12.));
#134398=CARTESIAN_POINT('Ctrl Pts',(-27.3584405685941,-68.5125286621888,
12.));
#134399=CARTESIAN_POINT('Ctrl Pts',(-27.3776077300914,-68.5315047488035,
12.));
#134400=CARTESIAN_POINT('Ctrl Pts',(-27.3968180187941,-68.5504887252975,
12.));
#134401=CARTESIAN_POINT('Ctrl Pts',(-27.4160714044831,-68.5694804955014,
12.));
#134402=CARTESIAN_POINT('Ctrl Pts',(-27.4353678571361,-68.5884799645218,
12.));
#134403=CARTESIAN_POINT('Ctrl Pts',(-27.4547073468227,-68.6074870381619,
12.));
#134404=CARTESIAN_POINT('Ctrl Pts',(-27.4740898435988,-68.6265016223561,
12.));
#134405=CARTESIAN_POINT('Ctrl Pts',(-27.4935153173868,-68.645523622548,
12.));
#134406=CARTESIAN_POINT('Ctrl Pts',(-27.5129837378791,-68.6645529432045,
12.));
#134407=CARTESIAN_POINT('Ctrl Pts',(-27.5324950743706,-68.6835894869882,
12.));
#134408=CARTESIAN_POINT('Ctrl Pts',(-27.5520492958907,-68.7026331554296,
12.));
#134409=CARTESIAN_POINT('Ctrl Pts',(-27.5716463715005,-68.7216838504218,
12.));
#134410=CARTESIAN_POINT('Ctrl Pts',(-27.5912862705469,-68.7407414755259,
12.));
#134411=CARTESIAN_POINT('Ctrl Pts',(-27.6109689629029,-68.7598059372129,
12.));
#134412=CARTESIAN_POINT('Ctrl Pts',(-27.6306944192738,-68.7788771464713,
12.));
#134413=CARTESIAN_POINT('Ctrl Pts',(-27.6504626112666,-68.7979550191872,
12.));
#134414=CARTESIAN_POINT('Ctrl Pts',(-27.6674443909984,-68.8143140938915,
12.));
#134415=CARTESIAN_POINT('Ctrl Pts',(-27.6804870323434,-68.8268597852179,
12.));
#134416=CARTESIAN_POINT('Ctrl Pts',(-27.6895716271275,-68.8355891982106,
12.));
#134417=CARTESIAN_POINT('Ctrl Pts',(-27.6946856803719,-68.840500446616,
12.));
#134418=CARTESIAN_POINT('Ctrl Pts',(-27.6958230985045,-68.8415926175086,
12.));
#134419=CARTESIAN_POINT('',(-24.7419628022042,-65.4815644032299,0.));
#134420=CARTESIAN_POINT('',(-24.7419628022042,-65.4815644032299,0.));
#134421=CARTESIAN_POINT('Ctrl Pts',(-27.6958230985045,-68.8415926175086,
0.));
#134422=CARTESIAN_POINT('Ctrl Pts',(-27.6946856803719,-68.840500446616,
0.));
#134423=CARTESIAN_POINT('Ctrl Pts',(-27.6895716271275,-68.8355891982106,
0.));
#134424=CARTESIAN_POINT('Ctrl Pts',(-27.6804870323434,-68.8268597852179,
0.));
#134425=CARTESIAN_POINT('Ctrl Pts',(-27.6674443909984,-68.8143140938915,
0.));
#134426=CARTESIAN_POINT('Ctrl Pts',(-27.6504626112666,-68.7979550191872,
0.));
#134427=CARTESIAN_POINT('Ctrl Pts',(-27.6306944192738,-68.7788771464713,
0.));
#134428=CARTESIAN_POINT('Ctrl Pts',(-27.6109689629029,-68.7598059372129,
0.));
#134429=CARTESIAN_POINT('Ctrl Pts',(-27.5912862705469,-68.7407414755259,
0.));
#134430=CARTESIAN_POINT('Ctrl Pts',(-27.5716463715005,-68.7216838504218,
0.));
#134431=CARTESIAN_POINT('Ctrl Pts',(-27.5520492958907,-68.7026331554296,
0.));
#134432=CARTESIAN_POINT('Ctrl Pts',(-27.5324950743706,-68.6835894869882,
0.));
#134433=CARTESIAN_POINT('Ctrl Pts',(-27.5129837378791,-68.6645529432045,
0.));
#134434=CARTESIAN_POINT('Ctrl Pts',(-27.4935153173868,-68.645523622548,
0.));
#134435=CARTESIAN_POINT('Ctrl Pts',(-27.4740898435988,-68.6265016223561,
0.));
#134436=CARTESIAN_POINT('Ctrl Pts',(-27.4547073468227,-68.6074870381619,
0.));
#134437=CARTESIAN_POINT('Ctrl Pts',(-27.4353678571361,-68.5884799645218,
0.));
#134438=CARTESIAN_POINT('Ctrl Pts',(-27.4160714044831,-68.5694804955014,
0.));
#134439=CARTESIAN_POINT('Ctrl Pts',(-27.3968180187941,-68.5504887252975,
0.));
#134440=CARTESIAN_POINT('Ctrl Pts',(-27.3776077300914,-68.5315047488035,
0.));
#134441=CARTESIAN_POINT('Ctrl Pts',(-27.3584405685941,-68.5125286621888,
0.));
#134442=CARTESIAN_POINT('Ctrl Pts',(-27.3393165646748,-68.4935605626361,
0.));
#134443=CARTESIAN_POINT('Ctrl Pts',(-27.3202357488153,-68.4746005480992,
0.));
#134444=CARTESIAN_POINT('Ctrl Pts',(-27.301198151557,-68.455648717044,0.));
#134445=CARTESIAN_POINT('Ctrl Pts',(-27.2822038034539,-68.4367051682166,
0.));
#134446=CARTESIAN_POINT('Ctrl Pts',(-27.2632527350062,-68.4177700003471,
0.));
#134447=CARTESIAN_POINT('Ctrl Pts',(-27.2443449766654,-68.3988433121589,
0.));
#134448=CARTESIAN_POINT('Ctrl Pts',(-27.2254805588677,-68.379925202511,
0.));
#134449=CARTESIAN_POINT('Ctrl Pts',(-27.2066595120544,-68.3610157704999,
0.));
#134450=CARTESIAN_POINT('Ctrl Pts',(-27.1878818666925,-68.3421151155708,
0.));
#134451=CARTESIAN_POINT('Ctrl Pts',(-27.1691476532917,-68.3232233376415,
0.));
#134452=CARTESIAN_POINT('Ctrl Pts',(-27.1504569024131,-68.3043405371589,
0.));
#134453=CARTESIAN_POINT('Ctrl Pts',(-27.1318096446643,-68.285466815035,
0.));
#134454=CARTESIAN_POINT('Ctrl Pts',(-27.1132059106939,-68.2666022726094,
0.));
#134455=CARTESIAN_POINT('Ctrl Pts',(-27.0946457311814,-68.2477470116014,
0.));
#134456=CARTESIAN_POINT('Ctrl Pts',(-27.076129136823,-68.2289011340624,
0.));
#134457=CARTESIAN_POINT('Ctrl Pts',(-27.0576561583179,-68.2100647423345,
0.));
#134458=CARTESIAN_POINT('Ctrl Pts',(-27.0392268263805,-68.1912379390786,
0.));
#134459=CARTESIAN_POINT('Ctrl Pts',(-27.0208411717477,-68.1724208272967,
0.));
#134460=CARTESIAN_POINT('Ctrl Pts',(-27.0024992251839,-68.1536135103558,
0.));
#134461=CARTESIAN_POINT('Ctrl Pts',(-26.9842010174819,-68.13481609201,0.));
#134462=CARTESIAN_POINT('Ctrl Pts',(-26.9659465794596,-68.1160286764244,
0.));
#134463=CARTESIAN_POINT('Ctrl Pts',(-26.9477359419646,-68.0972513681739,
0.));
#134464=CARTESIAN_POINT('Ctrl Pts',(-26.9295691358775,-68.0784842722362,
0.));
#134465=CARTESIAN_POINT('Ctrl Pts',(-26.9114461921109,-68.0597274939857,
0.));
#134466=CARTESIAN_POINT('Ctrl Pts',(-26.8933671416065,-68.0409811391871,
0.));
#134467=CARTESIAN_POINT('Ctrl Pts',(-26.8753320153255,-68.0222453139862,
0.));
#134468=CARTESIAN_POINT('Ctrl Pts',(-26.85734084425,-68.0035201249108,0.));
#134469=CARTESIAN_POINT('Ctrl Pts',(-26.8393936593914,-67.9848056788814,
0.));
#134470=CARTESIAN_POINT('Ctrl Pts',(-26.8214904917922,-67.9661020832165,
0.));
#134471=CARTESIAN_POINT('Ctrl Pts',(-26.8036313725262,-67.9474094456395,
0.));
#134472=CARTESIAN_POINT('Ctrl Pts',(-26.7858163326933,-67.9287278742839,
0.));
#134473=CARTESIAN_POINT('Ctrl Pts',(-26.7680454034169,-67.9100574776974,
0.));
#134474=CARTESIAN_POINT('Ctrl Pts',(-26.7503186158523,-67.8913983648441,
0.));
#134475=CARTESIAN_POINT('Ctrl Pts',(-26.7326360011886,-67.8727506451067,
0.));
#134476=CARTESIAN_POINT('Ctrl Pts',(-26.7149975906478,-67.8541144282875,
0.));
#134477=CARTESIAN_POINT('Ctrl Pts',(-26.6974034154803,-67.8354898246079,
0.));
#134478=CARTESIAN_POINT('Ctrl Pts',(-26.6798535069586,-67.8168769447086,
0.));
#134479=CARTESIAN_POINT('Ctrl Pts',(-26.6623478963867,-67.7982758996557,
0.));
#134480=CARTESIAN_POINT('Ctrl Pts',(-26.6448866151027,-67.7796868009447,
0.));
#134481=CARTESIAN_POINT('Ctrl Pts',(-26.6274696944793,-67.7611097605042,
0.));
#134482=CARTESIAN_POINT('Ctrl Pts',(-26.6100971659205,-67.7425448906983,
0.));
#134483=CARTESIAN_POINT('Ctrl Pts',(-26.5927690608547,-67.7239923043295,
0.));
#134484=CARTESIAN_POINT('Ctrl Pts',(-26.5754854107422,-67.7054521146427,
0.));
#134485=CARTESIAN_POINT('Ctrl Pts',(-26.5582462470794,-67.6869244353292,
0.));
#134486=CARTESIAN_POINT('Ctrl Pts',(-26.5410516013984,-67.6684093805288,
0.));
#134487=CARTESIAN_POINT('Ctrl Pts',(-26.5239015052656,-67.6499070648323,
0.));
#134488=CARTESIAN_POINT('Ctrl Pts',(-26.5067959902731,-67.6314176032823,
0.));
#134489=CARTESIAN_POINT('Ctrl Pts',(-26.4897350880447,-67.6129411113774,
0.));
#134490=CARTESIAN_POINT('Ctrl Pts',(-26.4727188302415,-67.5944777050782,
0.));
#134491=CARTESIAN_POINT('Ctrl Pts',(-26.4557472485622,-67.5760275008096,
0.));
#134492=CARTESIAN_POINT('Ctrl Pts',(-26.4388203747422,-67.5575906154648,
0.));
#134493=CARTESIAN_POINT('Ctrl Pts',(-26.4219382405452,-67.5391671664055,
0.));
#134494=CARTESIAN_POINT('Ctrl Pts',(-26.4051008777669,-67.5207572714666,
0.));
#134495=CARTESIAN_POINT('Ctrl Pts',(-26.3883083182417,-67.5023610489611,
0.));
#134496=CARTESIAN_POINT('Ctrl Pts',(-26.3715605938432,-67.4839786176833,
0.));
#134497=CARTESIAN_POINT('Ctrl Pts',(-26.3548577364835,-67.4656100969121,
0.));
#134498=CARTESIAN_POINT('Ctrl Pts',(-26.3381997781059,-67.4472556064127,
0.));
#134499=CARTESIAN_POINT('Ctrl Pts',(-26.3215867506864,-67.4289152664406,
0.));
#134500=CARTESIAN_POINT('Ctrl Pts',(-26.305018686241,-67.4105891977465,
0.));
#134501=CARTESIAN_POINT('Ctrl Pts',(-26.288495616827,-67.392277521581,0.));
#134502=CARTESIAN_POINT('Ctrl Pts',(-26.2720175745423,-67.3739803596967,
0.));
#134503=CARTESIAN_POINT('Ctrl Pts',(-26.255584591518,-67.3556978343506,
0.));
#134504=CARTESIAN_POINT('Ctrl Pts',(-26.2391966999192,-67.3374300683075,
0.));
#134505=CARTESIAN_POINT('Ctrl Pts',(-26.2228539319528,-67.3191771848468,
0.));
#134506=CARTESIAN_POINT('Ctrl Pts',(-26.2065563198685,-67.3009393077654,
0.));
#134507=CARTESIAN_POINT('Ctrl Pts',(-26.1903038959589,-67.2827165613828,
0.));
#134508=CARTESIAN_POINT('Ctrl Pts',(-26.1740966925527,-67.2645090705414,
0.));
#134509=CARTESIAN_POINT('Ctrl Pts',(-26.1579347420135,-67.2463169606105,
0.));
#134510=CARTESIAN_POINT('Ctrl Pts',(-26.1418180767487,-67.228140357493,
0.));
#134511=CARTESIAN_POINT('Ctrl Pts',(-26.1257467292102,-67.2099793876295,
0.));
#134512=CARTESIAN_POINT('Ctrl Pts',(-26.109720731895,-67.191834178002,0.));
#134513=CARTESIAN_POINT('Ctrl Pts',(-26.0937401173385,-67.1737048561364,
0.));
#134514=CARTESIAN_POINT('Ctrl Pts',(-26.077804918113,-67.1555915501052,
0.));
#134515=CARTESIAN_POINT('Ctrl Pts',(-26.0619151668361,-67.1374943885353,
0.));
#134516=CARTESIAN_POINT('Ctrl Pts',(-26.0460708961725,-67.1194135006121,
0.));
#134517=CARTESIAN_POINT('Ctrl Pts',(-26.030272138834,-67.101349016084,0.));
#134518=CARTESIAN_POINT('Ctrl Pts',(-26.0145189275733,-67.083301065264,
0.));
#134519=CARTESIAN_POINT('Ctrl Pts',(-25.9988112951818,-67.0652697790335,
0.));
#134520=CARTESIAN_POINT('Ctrl Pts',(-25.9831492744988,-67.0472552888495,
0.));
#134521=CARTESIAN_POINT('Ctrl Pts',(-25.9675328984123,-67.0292577267495,
0.));
#134522=CARTESIAN_POINT('Ctrl Pts',(-25.9519621998598,-67.0112772253553,
0.));
#134523=CARTESIAN_POINT('Ctrl Pts',(-25.9364372118216,-66.993313917876,
0.));
#134524=CARTESIAN_POINT('Ctrl Pts',(-25.9209579673198,-66.9753679381122,
0.));
#134525=CARTESIAN_POINT('Ctrl Pts',(-25.9055244994267,-66.9574394204635,
0.));
#134526=CARTESIAN_POINT('Ctrl Pts',(-25.8901368412655,-66.9395284999327,
0.));
#134527=CARTESIAN_POINT('Ctrl Pts',(-25.8747950260114,-66.9216353121308,
0.));
#134528=CARTESIAN_POINT('Ctrl Pts',(-25.8594990868845,-66.9037599932787,
0.));
#134529=CARTESIAN_POINT('Ctrl Pts',(-25.8442490571486,-66.8859026802123,
0.));
#134530=CARTESIAN_POINT('Ctrl Pts',(-25.8290449701207,-66.8680635103907,
0.));
#134531=CARTESIAN_POINT('Ctrl Pts',(-25.8138868591715,-66.8502426219015,
0.));
#134532=CARTESIAN_POINT('Ctrl Pts',(-25.7987747577265,-66.8324401534657,
0.));
#134533=CARTESIAN_POINT('Ctrl Pts',(-25.783708699258,-66.8146562444397,
0.));
#134534=CARTESIAN_POINT('Ctrl Pts',(-25.7686887172859,-66.7968910348199,
0.));
#134535=CARTESIAN_POINT('Ctrl Pts',(-25.7537148453848,-66.7791446652505,
0.));
#134536=CARTESIAN_POINT('Ctrl Pts',(-25.7387871171861,-66.7614172770302,
0.));
#134537=CARTESIAN_POINT('Ctrl Pts',(-25.7239055663778,-66.7437090121168,
0.));
#134538=CARTESIAN_POINT('Ctrl Pts',(-25.7090702266976,-66.72602001313,0.));
#134539=CARTESIAN_POINT('Ctrl Pts',(-25.6942811319337,-66.7083504233566,
0.));
#134540=CARTESIAN_POINT('Ctrl Pts',(-25.679538315933,-66.6907003867599,
0.));
#134541=CARTESIAN_POINT('Ctrl Pts',(-25.6648418126016,-66.6730700479843,
0.));
#134542=CARTESIAN_POINT('Ctrl Pts',(-25.6501916559051,-66.6554595523611,
0.));
#134543=CARTESIAN_POINT('Ctrl Pts',(-25.6355878798605,-66.6378690459105,
0.));
#134544=CARTESIAN_POINT('Ctrl Pts',(-25.6210305185395,-66.6202986753482,
0.));
#134545=CARTESIAN_POINT('Ctrl Pts',(-25.606519606075,-66.6027485880947,
0.));
#134546=CARTESIAN_POINT('Ctrl Pts',(-25.5920551766629,-66.585218932281,
0.));
#134547=CARTESIAN_POINT('Ctrl Pts',(-25.5776372645605,-66.567709856755,
0.));
#134548=CARTESIAN_POINT('Ctrl Pts',(-25.5632659040797,-66.5502215110843,
0.));
#134549=CARTESIAN_POINT('Ctrl Pts',(-25.5489411295916,-66.5327540455638,
0.));
#134550=CARTESIAN_POINT('Ctrl Pts',(-25.5346629755322,-66.5153076112237,
0.));
#134551=CARTESIAN_POINT('Ctrl Pts',(-25.5204314764033,-66.4978823598352,
0.));
#134552=CARTESIAN_POINT('Ctrl Pts',(-25.5062466667703,-66.4804784439146,
0.));
#134553=CARTESIAN_POINT('Ctrl Pts',(-25.4921085812548,-66.463096016725,
0.));
#134554=CARTESIAN_POINT('Ctrl Pts',(-25.4780172545418,-66.445735232287,
0.));
#134555=CARTESIAN_POINT('Ctrl Pts',(-25.463972721385,-66.4283962453899,
0.));
#134556=CARTESIAN_POINT('Ctrl Pts',(-25.4499750166079,-66.4110792116,0.));
#134557=CARTESIAN_POINT('Ctrl Pts',(-25.4360241751017,-66.3937842872684,
0.));
#134558=CARTESIAN_POINT('Ctrl Pts',(-25.4221202318198,-66.3765116295363,
0.));
#134559=CARTESIAN_POINT('Ctrl Pts',(-25.4082632217846,-66.3592613963407,
0.));
#134560=CARTESIAN_POINT('Ctrl Pts',(-25.3944531800901,-66.3420337464176,
0.));
#134561=CARTESIAN_POINT('Ctrl Pts',(-25.3806901419013,-66.3248288393046,
0.));
#134562=CARTESIAN_POINT('Ctrl Pts',(-25.3669741424491,-66.3076468353417,
0.));
#134563=CARTESIAN_POINT('Ctrl Pts',(-25.3533052170254,-66.2904878956721,
0.));
#134564=CARTESIAN_POINT('Ctrl Pts',(-25.3396834009955,-66.2733521822675,
0.));
#134565=CARTESIAN_POINT('Ctrl Pts',(-25.326108729803,-66.2562398579479,
0.));
#134566=CARTESIAN_POINT('Ctrl Pts',(-25.3125812389728,-66.2391510863992,
0.));
#134567=CARTESIAN_POINT('Ctrl Pts',(-25.2991009641087,-66.222086032193,
0.));
#134568=CARTESIAN_POINT('Ctrl Pts',(-25.2856679408921,-66.2050448607883,
0.));
#134569=CARTESIAN_POINT('Ctrl Pts',(-25.2722822050829,-66.1880277385113,
0.));
#134570=CARTESIAN_POINT('Ctrl Pts',(-25.2589437925145,-66.1710348325378,
0.));
#134571=CARTESIAN_POINT('Ctrl Pts',(-25.245652739088,-66.1540663108767,
0.));
#134572=CARTESIAN_POINT('Ctrl Pts',(-25.2324090807561,-66.1371223423371,
0.));
#134573=CARTESIAN_POINT('Ctrl Pts',(-25.2192128535367,-66.1202030965784,
0.));
#134574=CARTESIAN_POINT('Ctrl Pts',(-25.2060640935371,-66.1033087441916,
0.));
#134575=CARTESIAN_POINT('Ctrl Pts',(-25.1929628369685,-66.086439456768,
0.));
#134576=CARTESIAN_POINT('Ctrl Pts',(-25.1799091201594,-66.0695954069698,
0.));
#134577=CARTESIAN_POINT('Ctrl Pts',(-25.1669029795652,-66.0527767686,0.));
#134578=CARTESIAN_POINT('Ctrl Pts',(-25.153944451741,-66.0359837164709,
0.));
#134579=CARTESIAN_POINT('Ctrl Pts',(-25.1410335733094,-66.0192164262607,
0.));
#134580=CARTESIAN_POINT('Ctrl Pts',(-25.12817038093,-66.0024750743902,0.));
#134581=CARTESIAN_POINT('Ctrl Pts',(-25.1153549112512,-65.9857598378455,
0.));
#134582=CARTESIAN_POINT('Ctrl Pts',(-25.1025872009016,-65.9690708941591,
0.));
#134583=CARTESIAN_POINT('Ctrl Pts',(-25.0898672865926,-65.9524084218167,
0.));
#134584=CARTESIAN_POINT('Ctrl Pts',(-25.0771952052033,-65.9357726006174,
0.));
#134585=CARTESIAN_POINT('Ctrl Pts',(-25.0645709938519,-65.9191636119796,
0.));
#134586=CARTESIAN_POINT('Ctrl Pts',(-25.0519946900066,-65.9025816394391,
0.));
#134587=CARTESIAN_POINT('Ctrl Pts',(-25.039466331404,-65.8860268683088,
0.));
#134588=CARTESIAN_POINT('Ctrl Pts',(-25.0269859558351,-65.8694994847586,
0.));
#134589=CARTESIAN_POINT('Ctrl Pts',(-25.0145536009603,-65.8529996750441,
0.));
#134590=CARTESIAN_POINT('Ctrl Pts',(-25.0021693041181,-65.8365276247157,
0.));
#134591=CARTESIAN_POINT('Ctrl Pts',(-24.9898331021002,-65.8200835177071,
0.));
#134592=CARTESIAN_POINT('Ctrl Pts',(-24.97754503157,-65.8036675380761,0.));
#134593=CARTESIAN_POINT('Ctrl Pts',(-24.965305129559,-65.7872798720847,
0.));
#134594=CARTESIAN_POINT('Ctrl Pts',(-24.9531134338693,-65.7709207098949,
0.));
#134595=CARTESIAN_POINT('Ctrl Pts',(-24.9409699836523,-65.7545902480286,
0.));
#134596=CARTESIAN_POINT('Ctrl Pts',(-24.9288748194562,-65.7382886895839,
0.));
#134597=CARTESIAN_POINT('Ctrl Pts',(-24.9168279820093,-65.7220162391016,
0.));
#134598=CARTESIAN_POINT('Ctrl Pts',(-24.9048295111444,-65.7057730980471,
0.));
#134599=CARTESIAN_POINT('Ctrl Pts',(-24.8928794448616,-65.6895594608798,
0.));
#134600=CARTESIAN_POINT('Ctrl Pts',(-24.8809778178248,-65.6733755087723,
0.));
#134601=CARTESIAN_POINT('Ctrl Pts',(-24.8691246628081,-65.6572214156761,
0.));
#134602=CARTESIAN_POINT('Ctrl Pts',(-24.8573200135684,-65.6410973603713,
0.));
#134603=CARTESIAN_POINT('Ctrl Pts',(-24.8455639071517,-65.6250035361612,
0.));
#134604=CARTESIAN_POINT('Ctrl Pts',(-24.8338563866739,-65.6089401625551,
0.));
#134605=CARTESIAN_POINT('Ctrl Pts',(-24.8221975032059,-65.5929074932487,
0.));
#134606=CARTESIAN_POINT('Ctrl Pts',(-24.8105873098578,-65.5769057914184,
0.));
#134607=CARTESIAN_POINT('Ctrl Pts',(-24.7990258561234,-65.5609353062749,
0.));
#134608=CARTESIAN_POINT('Ctrl Pts',(-24.7875131827515,-65.5449962514735,
0.));
#134609=CARTESIAN_POINT('Ctrl Pts',(-24.7760493148551,-65.5290887770493,
0.));
#134610=CARTESIAN_POINT('Ctrl Pts',(-24.7646342620969,-65.5132129675727,
0.));
#134611=CARTESIAN_POINT('Ctrl Pts',(-24.7555412724771,-65.5005376841469,
0.));
#134612=CARTESIAN_POINT('Ctrl Pts',(-24.7487434956058,-65.4910454936487,
0.));
#134613=CARTESIAN_POINT('Ctrl Pts',(-24.7442214063411,-65.484723709553,
0.));
#134614=CARTESIAN_POINT('Ctrl Pts',(-24.7419628022042,-65.4815644032299,
0.));
#134615=CARTESIAN_POINT('Ctrl Pts',(-33.8448817269567,-66.3684712863594,
0.));
#134616=CARTESIAN_POINT('Ctrl Pts',(-33.8448817269567,-66.3684712863594,
12.));
#134617=CARTESIAN_POINT('Ctrl Pts',(-33.840486261887,-66.3650082659712,
0.));
#134618=CARTESIAN_POINT('Ctrl Pts',(-33.840486261887,-66.3650082659712,
12.));
#134619=CARTESIAN_POINT('Ctrl Pts',(-33.8316996011932,-66.3580824155893,
0.));
#134620=CARTESIAN_POINT('Ctrl Pts',(-33.8316996011932,-66.3580824155893,
12.));
#134621=CARTESIAN_POINT('Ctrl Pts',(-33.8185324184903,-66.3476942112,0.));
#134622=CARTESIAN_POINT('Ctrl Pts',(-33.8185324184903,-66.3476942112,12.));
#134623=CARTESIAN_POINT('Ctrl Pts',(-33.8010017926027,-66.3338444144211,
0.));
#134624=CARTESIAN_POINT('Ctrl Pts',(-33.8010017926027,-66.3338444144211,
12.));
#134625=CARTESIAN_POINT('Ctrl Pts',(-33.7791312145108,-66.3165340771611,
0.));
#134626=CARTESIAN_POINT('Ctrl Pts',(-33.7791312145108,-66.3165340771611,
12.));
#134627=CARTESIAN_POINT('Ctrl Pts',(-33.7573033544559,-66.2992256621336,
0.));
#134628=CARTESIAN_POINT('Ctrl Pts',(-33.7573033544559,-66.2992256621336,
12.));
#134629=CARTESIAN_POINT('Ctrl Pts',(-33.7355182321907,-66.2819191962353,
0.));
#134630=CARTESIAN_POINT('Ctrl Pts',(-33.7355182321907,-66.2819191962353,
12.));
#134631=CARTESIAN_POINT('Ctrl Pts',(-33.7137758735903,-66.2646147235321,
0.));
#134632=CARTESIAN_POINT('Ctrl Pts',(-33.7137758735903,-66.2646147235321,
12.));
#134633=CARTESIAN_POINT('Ctrl Pts',(-33.6920763111448,-66.2473123109395,
0.));
#134634=CARTESIAN_POINT('Ctrl Pts',(-33.6920763111448,-66.2473123109395,
12.));
#134635=CARTESIAN_POINT('Ctrl Pts',(-33.6704195830392,-66.2300120464082,
0.));
#134636=CARTESIAN_POINT('Ctrl Pts',(-33.6704195830392,-66.2300120464082,
12.));
#134637=CARTESIAN_POINT('Ctrl Pts',(-33.6488057311532,-66.2127140313598,
0.));
#134638=CARTESIAN_POINT('Ctrl Pts',(-33.6488057311532,-66.2127140313598,
12.));
#134639=CARTESIAN_POINT('Ctrl Pts',(-33.6272347993476,-66.1954183747088,
0.));
#134640=CARTESIAN_POINT('Ctrl Pts',(-33.6272347993476,-66.1954183747088,
12.));
#134641=CARTESIAN_POINT('Ctrl Pts',(-33.6057068316769,-66.1781251864017,
0.));
#134642=CARTESIAN_POINT('Ctrl Pts',(-33.6057068316769,-66.1781251864017,
12.));
#134643=CARTESIAN_POINT('Ctrl Pts',(-33.5842218705151,-66.1608345707636,
0.));
#134644=CARTESIAN_POINT('Ctrl Pts',(-33.5842218705151,-66.1608345707636,
12.));
#134645=CARTESIAN_POINT('Ctrl Pts',(-33.5627799550483,-66.1435466211076,
0.));
#134646=CARTESIAN_POINT('Ctrl Pts',(-33.5627799550483,-66.1435466211076,
12.));
#134647=CARTESIAN_POINT('Ctrl Pts',(-33.5413811223451,-66.1262614234674,
0.));
#134648=CARTESIAN_POINT('Ctrl Pts',(-33.5413811223451,-66.1262614234674,
12.));
#134649=CARTESIAN_POINT('Ctrl Pts',(-33.5200254081243,-66.1089790592729,
0.));
#134650=CARTESIAN_POINT('Ctrl Pts',(-33.5200254081243,-66.1089790592729,
12.));
#134651=CARTESIAN_POINT('Ctrl Pts',(-33.4987128476622,-66.0916996085244,
0.));
#134652=CARTESIAN_POINT('Ctrl Pts',(-33.4987128476622,-66.0916996085244,
12.));
#134653=CARTESIAN_POINT('Ctrl Pts',(-33.4774434765746,-66.0744231525415,
0.));
#134654=CARTESIAN_POINT('Ctrl Pts',(-33.4774434765746,-66.0744231525415,
12.));
#134655=CARTESIAN_POINT('Ctrl Pts',(-33.4562173318025,-66.0571497774434,
0.));
#134656=CARTESIAN_POINT('Ctrl Pts',(-33.4562173318025,-66.0571497774434,
12.));
#134657=CARTESIAN_POINT('Ctrl Pts',(-33.4350344515101,-66.0398795737777,
0.));
#134658=CARTESIAN_POINT('Ctrl Pts',(-33.4350344515101,-66.0398795737777,
12.));
#134659=CARTESIAN_POINT('Ctrl Pts',(-33.4138948746388,-66.0226126349446,
0.));
#134660=CARTESIAN_POINT('Ctrl Pts',(-33.4138948746388,-66.0226126349446,
12.));
#134661=CARTESIAN_POINT('Ctrl Pts',(-33.3927986405605,-66.0053490559812,
0.));
#134662=CARTESIAN_POINT('Ctrl Pts',(-33.3927986405605,-66.0053490559812,
12.));
#134663=CARTESIAN_POINT('Ctrl Pts',(-33.37174578871,-65.9880889322831,0.));
#134664=CARTESIAN_POINT('Ctrl Pts',(-33.37174578871,-65.9880889322831,12.));
#134665=CARTESIAN_POINT('Ctrl Pts',(-33.3507363581593,-65.970832358141,
0.));
#134666=CARTESIAN_POINT('Ctrl Pts',(-33.3507363581593,-65.970832358141,
12.));
#134667=CARTESIAN_POINT('Ctrl Pts',(-33.3297703874266,-65.9535794260831,
0.));
#134668=CARTESIAN_POINT('Ctrl Pts',(-33.3297703874266,-65.9535794260831,
12.));
#134669=CARTESIAN_POINT('Ctrl Pts',(-33.3088479147164,-65.9363302276846,
0.));
#134670=CARTESIAN_POINT('Ctrl Pts',(-33.3088479147164,-65.9363302276846,
12.));
#134671=CARTESIAN_POINT('Ctrl Pts',(-33.2879689780573,-65.9190848540433,
0.));
#134672=CARTESIAN_POINT('Ctrl Pts',(-33.2879689780573,-65.9190848540433,
12.));
#134673=CARTESIAN_POINT('Ctrl Pts',(-33.2671336154754,-65.9018433963889,
0.));
#134674=CARTESIAN_POINT('Ctrl Pts',(-33.2671336154754,-65.9018433963889,
12.));
#134675=CARTESIAN_POINT('Ctrl Pts',(-33.2463418651493,-65.8846059466371,
0.));
#134676=CARTESIAN_POINT('Ctrl Pts',(-33.2463418651493,-65.8846059466371,
12.));
#134677=CARTESIAN_POINT('Ctrl Pts',(-33.2255937655649,-65.8673725979577,
0.));
#134678=CARTESIAN_POINT('Ctrl Pts',(-33.2255937655649,-65.8673725979577,
12.));
#134679=CARTESIAN_POINT('Ctrl Pts',(-33.2048893554491,-65.8501434445164,
0.));
#134680=CARTESIAN_POINT('Ctrl Pts',(-33.2048893554491,-65.8501434445164,
12.));
#134681=CARTESIAN_POINT('Ctrl Pts',(-33.1842286737051,-65.8329185812375,
0.));
#134682=CARTESIAN_POINT('Ctrl Pts',(-33.1842286737051,-65.8329185812375,
12.));
#134683=CARTESIAN_POINT('Ctrl Pts',(-33.16361175934,-65.8156981035503,0.));
#134684=CARTESIAN_POINT('Ctrl Pts',(-33.16361175934,-65.8156981035503,12.));
#134685=CARTESIAN_POINT('Ctrl Pts',(-33.1430386513976,-65.7984821071623,
0.));
#134686=CARTESIAN_POINT('Ctrl Pts',(-33.1430386513976,-65.7984821071623,
12.));
#134687=CARTESIAN_POINT('Ctrl Pts',(-33.1225093888672,-65.7812706877696,
0.));
#134688=CARTESIAN_POINT('Ctrl Pts',(-33.1225093888672,-65.7812706877696,
12.));
#134689=CARTESIAN_POINT('Ctrl Pts',(-33.1020240106885,-65.7640639410661,
0.));
#134690=CARTESIAN_POINT('Ctrl Pts',(-33.1020240106885,-65.7640639410661,
12.));
#134691=CARTESIAN_POINT('Ctrl Pts',(-33.081582555798,-65.7468619628815,
0.));
#134692=CARTESIAN_POINT('Ctrl Pts',(-33.081582555798,-65.7468619628815,
12.));
#134693=CARTESIAN_POINT('Ctrl Pts',(-33.0611850631582,-65.7296648492824,
0.));
#134694=CARTESIAN_POINT('Ctrl Pts',(-33.0611850631582,-65.7296648492824,
12.));
#134695=CARTESIAN_POINT('Ctrl Pts',(-33.0408315717873,-65.7124726966802,
0.));
#134696=CARTESIAN_POINT('Ctrl Pts',(-33.0408315717873,-65.7124726966802,
12.));
#134697=CARTESIAN_POINT('Ctrl Pts',(-33.0205221207873,-65.6952856019533,
0.));
#134698=CARTESIAN_POINT('Ctrl Pts',(-33.0205221207873,-65.6952856019533,
12.));
#134699=CARTESIAN_POINT('Ctrl Pts',(-33.0002567493574,-65.6781036625027,
0.));
#134700=CARTESIAN_POINT('Ctrl Pts',(-33.0002567493574,-65.6781036625027,
12.));
#134701=CARTESIAN_POINT('Ctrl Pts',(-32.980035496784,-65.6609269761888,
0.));
#134702=CARTESIAN_POINT('Ctrl Pts',(-32.980035496784,-65.6609269761888,
12.));
#134703=CARTESIAN_POINT('Ctrl Pts',(-32.9598584024313,-65.6437556412946,
0.));
#134704=CARTESIAN_POINT('Ctrl Pts',(-32.9598584024313,-65.6437556412946,
12.));
#134705=CARTESIAN_POINT('Ctrl Pts',(-32.9397255057274,-65.6265897564783,
0.));
#134706=CARTESIAN_POINT('Ctrl Pts',(-32.9397255057274,-65.6265897564783,
12.));
#134707=CARTESIAN_POINT('Ctrl Pts',(-32.9196368461463,-65.6094294207276,
0.));
#134708=CARTESIAN_POINT('Ctrl Pts',(-32.9196368461463,-65.6094294207276,
12.));
#134709=CARTESIAN_POINT('Ctrl Pts',(-32.8995924631898,-65.5922747333194,
0.));
#134710=CARTESIAN_POINT('Ctrl Pts',(-32.8995924631898,-65.5922747333194,
12.));
#134711=CARTESIAN_POINT('Ctrl Pts',(-32.879592396403,-65.5751257938472,
0.));
#134712=CARTESIAN_POINT('Ctrl Pts',(-32.879592396403,-65.5751257938472,
12.));
#134713=CARTESIAN_POINT('Ctrl Pts',(-32.8596366853832,-65.5579827022421,
0.));
#134714=CARTESIAN_POINT('Ctrl Pts',(-32.8596366853832,-65.5579827022421,
12.));
#134715=CARTESIAN_POINT('Ctrl Pts',(-32.8397253697866,-65.5408455587964,
0.));
#134716=CARTESIAN_POINT('Ctrl Pts',(-32.8397253697866,-65.5408455587964,
12.));
#134717=CARTESIAN_POINT('Ctrl Pts',(-32.8198584893316,-65.5237144641857,
0.));
#134718=CARTESIAN_POINT('Ctrl Pts',(-32.8198584893316,-65.5237144641857,
12.));
#134719=CARTESIAN_POINT('Ctrl Pts',(-32.8000360837975,-65.5065895194928,
0.));
#134720=CARTESIAN_POINT('Ctrl Pts',(-32.8000360837975,-65.5065895194928,
12.));
#134721=CARTESIAN_POINT('Ctrl Pts',(-32.7802581930287,-65.489470826206,
0.));
#134722=CARTESIAN_POINT('Ctrl Pts',(-32.7802581930287,-65.489470826206,
12.));
#134723=CARTESIAN_POINT('Ctrl Pts',(-32.7605248569378,-65.4723584862122,
0.));
#134724=CARTESIAN_POINT('Ctrl Pts',(-32.7605248569378,-65.4723584862122,
12.));
#134725=CARTESIAN_POINT('Ctrl Pts',(-32.7408361155037,-65.4552526017905,
0.));
#134726=CARTESIAN_POINT('Ctrl Pts',(-32.7408361155037,-65.4552526017905,
12.));
#134727=CARTESIAN_POINT('Ctrl Pts',(-32.7211920087684,-65.4381532756065,
0.));
#134728=CARTESIAN_POINT('Ctrl Pts',(-32.7211920087684,-65.4381532756065,
12.));
#134729=CARTESIAN_POINT('Ctrl Pts',(-32.7015925768265,-65.4210606107035,
0.));
#134730=CARTESIAN_POINT('Ctrl Pts',(-32.7015925768265,-65.4210606107035,
12.));
#134731=CARTESIAN_POINT('Ctrl Pts',(-32.6820378598267,-65.4039747105038,
0.));
#134732=CARTESIAN_POINT('Ctrl Pts',(-32.6820378598267,-65.4039747105038,
12.));
#134733=CARTESIAN_POINT('Ctrl Pts',(-32.6625278979811,-65.3868956788182,
0.));
#134734=CARTESIAN_POINT('Ctrl Pts',(-32.6625278979811,-65.3868956788182,
12.));
#134735=CARTESIAN_POINT('Ctrl Pts',(-32.6430627315674,-65.3698236198512,
0.));
#134736=CARTESIAN_POINT('Ctrl Pts',(-32.6430627315674,-65.3698236198512,
12.));
#134737=CARTESIAN_POINT('Ctrl Pts',(-32.6236424009301,-65.3527586382081,
0.));
#134738=CARTESIAN_POINT('Ctrl Pts',(-32.6236424009301,-65.3527586382081,
12.));
#134739=CARTESIAN_POINT('Ctrl Pts',(-32.6042669464751,-65.3357008389003,
0.));
#134740=CARTESIAN_POINT('Ctrl Pts',(-32.6042669464751,-65.3357008389003,
12.));
#134741=CARTESIAN_POINT('Ctrl Pts',(-32.5849364086679,-65.31865032735,0.));
#134742=CARTESIAN_POINT('Ctrl Pts',(-32.5849364086679,-65.31865032735,12.));
#134743=CARTESIAN_POINT('Ctrl Pts',(-32.5656508280422,-65.3016072093912,
0.));
#134744=CARTESIAN_POINT('Ctrl Pts',(-32.5656508280422,-65.3016072093912,
12.));
#134745=CARTESIAN_POINT('Ctrl Pts',(-32.5464102452015,-65.2845715912721,
0.));
#134746=CARTESIAN_POINT('Ctrl Pts',(-32.5464102452015,-65.2845715912721,
12.));
#134747=CARTESIAN_POINT('Ctrl Pts',(-32.5272147008191,-65.2675435796558,
0.));
#134748=CARTESIAN_POINT('Ctrl Pts',(-32.5272147008191,-65.2675435796558,
12.));
#134749=CARTESIAN_POINT('Ctrl Pts',(-32.5080642356328,-65.2505232816209,
0.));
#134750=CARTESIAN_POINT('Ctrl Pts',(-32.5080642356328,-65.2505232816209,
12.));
#134751=CARTESIAN_POINT('Ctrl Pts',(-32.4889588904392,-65.2335108046614,
0.));
#134752=CARTESIAN_POINT('Ctrl Pts',(-32.4889588904392,-65.2335108046614,
12.));
#134753=CARTESIAN_POINT('Ctrl Pts',(-32.4698987061032,-65.2165062566924,
0.));
#134754=CARTESIAN_POINT('Ctrl Pts',(-32.4698987061032,-65.2165062566924,
12.));
#134755=CARTESIAN_POINT('Ctrl Pts',(-32.450883723561,-65.1995097460538,
0.));
#134756=CARTESIAN_POINT('Ctrl Pts',(-32.450883723561,-65.1995097460538,
12.));
#134757=CARTESIAN_POINT('Ctrl Pts',(-32.4319139838213,-65.182521381514,
0.));
#134758=CARTESIAN_POINT('Ctrl Pts',(-32.4319139838213,-65.182521381514,
12.));
#134759=CARTESIAN_POINT('Ctrl Pts',(-32.4129895279615,-65.1655412722725,
0.));
#134760=CARTESIAN_POINT('Ctrl Pts',(-32.4129895279615,-65.1655412722725,
12.));
#134761=CARTESIAN_POINT('Ctrl Pts',(-32.3941103971221,-65.1485695279635,
0.));
#134762=CARTESIAN_POINT('Ctrl Pts',(-32.3941103971221,-65.1485695279635,
12.));
#134763=CARTESIAN_POINT('Ctrl Pts',(-32.3752766325136,-65.1316062586588,
0.));
#134764=CARTESIAN_POINT('Ctrl Pts',(-32.3752766325136,-65.1316062586588,
12.));
#134765=CARTESIAN_POINT('Ctrl Pts',(-32.3564882754212,-65.1146515748722,
0.));
#134766=CARTESIAN_POINT('Ctrl Pts',(-32.3564882754212,-65.1146515748722,
12.));
#134767=CARTESIAN_POINT('Ctrl Pts',(-32.3377453672051,-65.0977055875607,
0.));
#134768=CARTESIAN_POINT('Ctrl Pts',(-32.3377453672051,-65.0977055875607,
12.));
#134769=CARTESIAN_POINT('Ctrl Pts',(-32.3190479492987,-65.0807684081281,
0.));
#134770=CARTESIAN_POINT('Ctrl Pts',(-32.3190479492987,-65.0807684081281,
12.));
#134771=CARTESIAN_POINT('Ctrl Pts',(-32.3003960632007,-65.0638401484257,
0.));
#134772=CARTESIAN_POINT('Ctrl Pts',(-32.3003960632007,-65.0638401484257,
12.));
#134773=CARTESIAN_POINT('Ctrl Pts',(-32.2817897504807,-65.0469209207563,
0.));
#134774=CARTESIAN_POINT('Ctrl Pts',(-32.2817897504807,-65.0469209207563,
12.));
#134775=CARTESIAN_POINT('Ctrl Pts',(-32.2632290527862,-65.03001083788,0.));
#134776=CARTESIAN_POINT('Ctrl Pts',(-32.2632290527862,-65.03001083788,12.));
#134777=CARTESIAN_POINT('Ctrl Pts',(-32.2447140118422,-65.0131100130157,
0.));
#134778=CARTESIAN_POINT('Ctrl Pts',(-32.2447140118422,-65.0131100130157,
12.));
#134779=CARTESIAN_POINT('Ctrl Pts',(-32.2262446694513,-64.9962185598461,
0.));
#134780=CARTESIAN_POINT('Ctrl Pts',(-32.2262446694513,-64.9962185598461,
12.));
#134781=CARTESIAN_POINT('Ctrl Pts',(-32.207821067485,-64.9793365925178,
0.));
#134782=CARTESIAN_POINT('Ctrl Pts',(-32.207821067485,-64.9793365925178,
12.));
#134783=CARTESIAN_POINT('Ctrl Pts',(-32.1894432478881,-64.9624642256461,
0.));
#134784=CARTESIAN_POINT('Ctrl Pts',(-32.1894432478881,-64.9624642256461,
12.));
#134785=CARTESIAN_POINT('Ctrl Pts',(-32.1711112526855,-64.9456015743192,
0.));
#134786=CARTESIAN_POINT('Ctrl Pts',(-32.1711112526855,-64.9456015743192,
12.));
#134787=CARTESIAN_POINT('Ctrl Pts',(-32.1528251239831,-64.9287487541015,
0.));
#134788=CARTESIAN_POINT('Ctrl Pts',(-32.1528251239831,-64.9287487541015,
12.));
#134789=CARTESIAN_POINT('Ctrl Pts',(-32.1345849039674,-64.9119058810366,
0.));
#134790=CARTESIAN_POINT('Ctrl Pts',(-32.1345849039674,-64.9119058810366,
12.));
#134791=CARTESIAN_POINT('Ctrl Pts',(-32.1163906348984,-64.8950730716501,
0.));
#134792=CARTESIAN_POINT('Ctrl Pts',(-32.1163906348984,-64.8950730716501,
12.));
#134793=CARTESIAN_POINT('Ctrl Pts',(-32.0982423591113,-64.8782504429527,
0.));
#134794=CARTESIAN_POINT('Ctrl Pts',(-32.0982423591113,-64.8782504429527,
12.));
#134795=CARTESIAN_POINT('Ctrl Pts',(-32.0801401190244,-64.8614381124454,
0.));
#134796=CARTESIAN_POINT('Ctrl Pts',(-32.0801401190244,-64.8614381124454,
12.));
#134797=CARTESIAN_POINT('Ctrl Pts',(-32.0620839571409,-64.8446361981234,
0.));
#134798=CARTESIAN_POINT('Ctrl Pts',(-32.0620839571409,-64.8446361981234,
12.));
#134799=CARTESIAN_POINT('Ctrl Pts',(-32.0440739160477,-64.8278448184785,
0.));
#134800=CARTESIAN_POINT('Ctrl Pts',(-32.0440739160477,-64.8278448184785,
12.));
#134801=CARTESIAN_POINT('Ctrl Pts',(-32.0261100384092,-64.811064092502,
0.));
#134802=CARTESIAN_POINT('Ctrl Pts',(-32.0261100384092,-64.811064092502,
12.));
#134803=CARTESIAN_POINT('Ctrl Pts',(-32.0081923669678,-64.7942941396883,
0.));
#134804=CARTESIAN_POINT('Ctrl Pts',(-32.0081923669678,-64.7942941396883,
12.));
#134805=CARTESIAN_POINT('Ctrl Pts',(-31.9903209445522,-64.7775350800404,
0.));
#134806=CARTESIAN_POINT('Ctrl Pts',(-31.9903209445522,-64.7775350800404,
12.));
#134807=CARTESIAN_POINT('Ctrl Pts',(-31.9724958140791,-64.7607870340738,
0.));
#134808=CARTESIAN_POINT('Ctrl Pts',(-31.9724958140791,-64.7607870340738,
12.));
#134809=CARTESIAN_POINT('Ctrl Pts',(-31.9547170185533,-64.74405012282,0.));
#134810=CARTESIAN_POINT('Ctrl Pts',(-31.9547170185533,-64.74405012282,12.));
#134811=CARTESIAN_POINT('Ctrl Pts',(-31.9369846010613,-64.727324467829,
0.));
#134812=CARTESIAN_POINT('Ctrl Pts',(-31.9369846010613,-64.727324467829,
12.));
#134813=CARTESIAN_POINT('Ctrl Pts',(-31.9192986047702,-64.7106101911722,
0.));
#134814=CARTESIAN_POINT('Ctrl Pts',(-31.9192986047702,-64.7106101911722,
12.));
#134815=CARTESIAN_POINT('Ctrl Pts',(-31.9016590729371,-64.693907415449,
0.));
#134816=CARTESIAN_POINT('Ctrl Pts',(-31.9016590729371,-64.693907415449,
12.));
#134817=CARTESIAN_POINT('Ctrl Pts',(-31.8840660489106,-64.6772162637904,
0.));
#134818=CARTESIAN_POINT('Ctrl Pts',(-31.8840660489106,-64.6772162637904,
12.));
#134819=CARTESIAN_POINT('Ctrl Pts',(-31.8665195761312,-64.6605368598631,
0.));
#134820=CARTESIAN_POINT('Ctrl Pts',(-31.8665195761312,-64.6605368598631,
12.));
#134821=CARTESIAN_POINT('Ctrl Pts',(-31.849019698125,-64.6438693278718,
0.));
#134822=CARTESIAN_POINT('Ctrl Pts',(-31.849019698125,-64.6438693278718,
12.));
#134823=CARTESIAN_POINT('Ctrl Pts',(-31.8315664585027,-64.6272137925629,
0.));
#134824=CARTESIAN_POINT('Ctrl Pts',(-31.8315664585027,-64.6272137925629,
12.));
#134825=CARTESIAN_POINT('Ctrl Pts',(-31.8141599009685,-64.6105703792311,
0.));
#134826=CARTESIAN_POINT('Ctrl Pts',(-31.8141599009685,-64.6105703792311,
12.));
#134827=CARTESIAN_POINT('Ctrl Pts',(-31.7968000693218,-64.5939392137233,
0.));
#134828=CARTESIAN_POINT('Ctrl Pts',(-31.7968000693218,-64.5939392137233,
12.));
#134829=CARTESIAN_POINT('Ctrl Pts',(-31.7794870074584,-64.5773204224429,
0.));
#134830=CARTESIAN_POINT('Ctrl Pts',(-31.7794870074584,-64.5773204224429,
12.));
#134831=CARTESIAN_POINT('Ctrl Pts',(-31.7622207593637,-64.5607141323527,
0.));
#134832=CARTESIAN_POINT('Ctrl Pts',(-31.7622207593637,-64.5607141323527,
12.));
#134833=CARTESIAN_POINT('Ctrl Pts',(-31.7450013691117,-64.5441204709779,
0.));
#134834=CARTESIAN_POINT('Ctrl Pts',(-31.7450013691117,-64.5441204709779,
12.));
#134835=CARTESIAN_POINT('Ctrl Pts',(-31.7278288808736,-64.5275395664134,
0.));
#134836=CARTESIAN_POINT('Ctrl Pts',(-31.7278288808736,-64.5275395664134,
12.));
#134837=CARTESIAN_POINT('Ctrl Pts',(-31.7107033389204,-64.5109715473276,
0.));
#134838=CARTESIAN_POINT('Ctrl Pts',(-31.7107033389204,-64.5109715473276,
12.));
#134839=CARTESIAN_POINT('Ctrl Pts',(-31.6936247876228,-64.4944165429672,
0.));
#134840=CARTESIAN_POINT('Ctrl Pts',(-31.6936247876228,-64.4944165429672,
12.));
#134841=CARTESIAN_POINT('Ctrl Pts',(-31.6765932714456,-64.4778746831597,
0.));
#134842=CARTESIAN_POINT('Ctrl Pts',(-31.6765932714456,-64.4778746831597,
12.));
#134843=CARTESIAN_POINT('Ctrl Pts',(-31.6596088349468,-64.4613460983186,
0.));
#134844=CARTESIAN_POINT('Ctrl Pts',(-31.6596088349468,-64.4613460983186,
12.));
#134845=CARTESIAN_POINT('Ctrl Pts',(-31.6426715227865,-64.4448309194498,
0.));
#134846=CARTESIAN_POINT('Ctrl Pts',(-31.6426715227865,-64.4448309194498,
12.));
#134847=CARTESIAN_POINT('Ctrl Pts',(-31.6257813797282,-64.4283292781553,
0.));
#134848=CARTESIAN_POINT('Ctrl Pts',(-31.6257813797282,-64.4283292781553,
12.));
#134849=CARTESIAN_POINT('Ctrl Pts',(-31.6089384506399,-64.4118413066386,
0.));
#134850=CARTESIAN_POINT('Ctrl Pts',(-31.6089384506399,-64.4118413066386,
12.));
#134851=CARTESIAN_POINT('Ctrl Pts',(-31.5921427804879,-64.3953671377071,
0.));
#134852=CARTESIAN_POINT('Ctrl Pts',(-31.5921427804879,-64.3953671377071,
12.));
#134853=CARTESIAN_POINT('Ctrl Pts',(-31.5753944143355,-64.3789069047768,
0.));
#134854=CARTESIAN_POINT('Ctrl Pts',(-31.5753944143355,-64.3789069047768,
12.));
#134855=CARTESIAN_POINT('Ctrl Pts',(-31.5586933973532,-64.3624607418798,
0.));
#134856=CARTESIAN_POINT('Ctrl Pts',(-31.5586933973532,-64.3624607418798,
12.));
#134857=CARTESIAN_POINT('Ctrl Pts',(-31.5420397748198,-64.34602878367,0.));
#134858=CARTESIAN_POINT('Ctrl Pts',(-31.5420397748198,-64.34602878367,12.));
#134859=CARTESIAN_POINT('Ctrl Pts',(-31.525433592124,-64.3296111654273,
0.));
#134860=CARTESIAN_POINT('Ctrl Pts',(-31.525433592124,-64.3296111654273,
12.));
#134861=CARTESIAN_POINT('Ctrl Pts',(-31.5088748947565,-64.3132080230603,
0.));
#134862=CARTESIAN_POINT('Ctrl Pts',(-31.5088748947565,-64.3132080230603,
12.));
#134863=CARTESIAN_POINT('Ctrl Pts',(-31.4923637283109,-64.2968194931113,
0.));
#134864=CARTESIAN_POINT('Ctrl Pts',(-31.4923637283109,-64.2968194931113,
12.));
#134865=CARTESIAN_POINT('Ctrl Pts',(-31.4759001384923,-64.2804457127633,
0.));
#134866=CARTESIAN_POINT('Ctrl Pts',(-31.4759001384923,-64.2804457127633,
12.));
#134867=CARTESIAN_POINT('Ctrl Pts',(-31.4594841711189,-64.264086819846,
0.));
#134868=CARTESIAN_POINT('Ctrl Pts',(-31.4594841711189,-64.264086819846,
12.));
#134869=CARTESIAN_POINT('Ctrl Pts',(-31.443115872123,-64.2477429528408,
0.));
#134870=CARTESIAN_POINT('Ctrl Pts',(-31.443115872123,-64.2477429528408,
12.));
#134871=CARTESIAN_POINT('Ctrl Pts',(-31.426795287544,-64.2314142508843,
0.));
#134872=CARTESIAN_POINT('Ctrl Pts',(-31.426795287544,-64.2314142508843,
12.));
#134873=CARTESIAN_POINT('Ctrl Pts',(-31.4105224635298,-64.2151008537733,
0.));
#134874=CARTESIAN_POINT('Ctrl Pts',(-31.4105224635298,-64.2151008537733,
12.));
#134875=CARTESIAN_POINT('Ctrl Pts',(-31.3942974463458,-64.1988029019733,
0.));
#134876=CARTESIAN_POINT('Ctrl Pts',(-31.3942974463458,-64.1988029019733,
12.));
#134877=CARTESIAN_POINT('Ctrl Pts',(-31.3781202823758,-64.1825205366231,
0.));
#134878=CARTESIAN_POINT('Ctrl Pts',(-31.3781202823758,-64.1825205366231,
12.));
#134879=CARTESIAN_POINT('Ctrl Pts',(-31.3619910181223,-64.1662538995407,
0.));
#134880=CARTESIAN_POINT('Ctrl Pts',(-31.3619910181223,-64.1662538995407,
12.));
#134881=CARTESIAN_POINT('Ctrl Pts',(-31.3459097001996,-64.150003133226,
0.));
#134882=CARTESIAN_POINT('Ctrl Pts',(-31.3459097001996,-64.150003133226,
12.));
#134883=CARTESIAN_POINT('Ctrl Pts',(-31.3298763753366,-64.1337683808667,
0.));
#134884=CARTESIAN_POINT('Ctrl Pts',(-31.3298763753366,-64.1337683808667,
12.));
#134885=CARTESIAN_POINT('Ctrl Pts',(-31.3138910903852,-64.1175497863475,
0.));
#134886=CARTESIAN_POINT('Ctrl Pts',(-31.3138910903852,-64.1175497863475,
12.));
#134887=CARTESIAN_POINT('Ctrl Pts',(-31.2979538923214,-64.1013474942554,
0.));
#134888=CARTESIAN_POINT('Ctrl Pts',(-31.2979538923214,-64.1013474942554,
12.));
#134889=CARTESIAN_POINT('Ctrl Pts',(-31.2820648282451,-64.0851616498861,
0.));
#134890=CARTESIAN_POINT('Ctrl Pts',(-31.2820648282451,-64.0851616498861,
12.));
#134891=CARTESIAN_POINT('Ctrl Pts',(-31.2662239453734,-64.0689923992474,
0.));
#134892=CARTESIAN_POINT('Ctrl Pts',(-31.2662239453734,-64.0689923992474,
12.));
#134893=CARTESIAN_POINT('Ctrl Pts',(-31.2504312910457,-64.0528398890671,
0.));
#134894=CARTESIAN_POINT('Ctrl Pts',(-31.2504312910457,-64.0528398890671,
12.));
#134895=CARTESIAN_POINT('Ctrl Pts',(-31.23468691273,-64.036704266799,0.));
#134896=CARTESIAN_POINT('Ctrl Pts',(-31.23468691273,-64.036704266799,12.));
#134897=CARTESIAN_POINT('Ctrl Pts',(-31.2189908580245,-64.0205856806298,
0.));
#134898=CARTESIAN_POINT('Ctrl Pts',(-31.2189908580245,-64.0205856806298,
12.));
#134899=CARTESIAN_POINT('Ctrl Pts',(-31.2033431746559,-64.004484279483,
0.));
#134900=CARTESIAN_POINT('Ctrl Pts',(-31.2033431746559,-64.004484279483,
12.));
#134901=CARTESIAN_POINT('Ctrl Pts',(-31.1877439104717,-63.9884002130209,
0.));
#134902=CARTESIAN_POINT('Ctrl Pts',(-31.1877439104717,-63.9884002130209,
12.));
#134903=CARTESIAN_POINT('Ctrl Pts',(-31.1721931134488,-63.972333631655,
0.));
#134904=CARTESIAN_POINT('Ctrl Pts',(-31.1721931134488,-63.972333631655,
12.));
#134905=CARTESIAN_POINT('Ctrl Pts',(-31.1566908316993,-63.9562846865566,
0.));
#134906=CARTESIAN_POINT('Ctrl Pts',(-31.1566908316993,-63.9562846865566,
12.));
#134907=CARTESIAN_POINT('Ctrl Pts',(-31.1412371134727,-63.940253529665,
0.));
#134908=CARTESIAN_POINT('Ctrl Pts',(-31.1412371134727,-63.940253529665,
12.));
#134909=CARTESIAN_POINT('Ctrl Pts',(-31.1258320071545,-63.9242403136954,
0.));
#134910=CARTESIAN_POINT('Ctrl Pts',(-31.1258320071545,-63.9242403136954,
12.));
#134911=CARTESIAN_POINT('Ctrl Pts',(-31.1104755612606,-63.9082451921447,
0.));
#134912=CARTESIAN_POINT('Ctrl Pts',(-31.1104755612606,-63.9082451921447,
12.));
#134913=CARTESIAN_POINT('Ctrl Pts',(-31.0951678244454,-63.8922683192962,
0.));
#134914=CARTESIAN_POINT('Ctrl Pts',(-31.0951678244454,-63.8922683192962,
12.));
#134915=CARTESIAN_POINT('Ctrl Pts',(-31.079908845504,-63.8763098502235,
0.));
#134916=CARTESIAN_POINT('Ctrl Pts',(-31.079908845504,-63.8763098502235,
12.));
#134917=CARTESIAN_POINT('Ctrl Pts',(-31.0646986733724,-63.8603699407922,
0.));
#134918=CARTESIAN_POINT('Ctrl Pts',(-31.0646986733724,-63.8603699407922,
12.));
#134919=CARTESIAN_POINT('Ctrl Pts',(-31.0495373571218,-63.8444487476615,
0.));
#134920=CARTESIAN_POINT('Ctrl Pts',(-31.0495373571218,-63.8444487476615,
12.));
#134921=CARTESIAN_POINT('Ctrl Pts',(-31.0344249459544,-63.8285464282857,
0.));
#134922=CARTESIAN_POINT('Ctrl Pts',(-31.0344249459544,-63.8285464282857,
12.));
#134923=CARTESIAN_POINT('Ctrl Pts',(-31.0193614892177,-63.8126631409376,
0.));
#134924=CARTESIAN_POINT('Ctrl Pts',(-31.0193614892177,-63.8126631409376,
12.));
#134925=CARTESIAN_POINT('Ctrl Pts',(-31.0043470364112,-63.7967990447287,
0.));
#134926=CARTESIAN_POINT('Ctrl Pts',(-31.0043470364112,-63.7967990447287,
12.));
#134927=CARTESIAN_POINT('Ctrl Pts',(-30.9893816371907,-63.7809542996258,
0.));
#134928=CARTESIAN_POINT('Ctrl Pts',(-30.9893816371907,-63.7809542996258,
12.));
#134929=CARTESIAN_POINT('Ctrl Pts',(-30.9744653413679,-63.7651290664713,
0.));
#134930=CARTESIAN_POINT('Ctrl Pts',(-30.9744653413679,-63.7651290664713,
12.));
#134931=CARTESIAN_POINT('Ctrl Pts',(-30.9595981989091,-63.7493235069844,
0.));
#134932=CARTESIAN_POINT('Ctrl Pts',(-30.9595981989091,-63.7493235069844,
12.));
#134933=CARTESIAN_POINT('Ctrl Pts',(-30.9447802599345,-63.733537783742,
0.));
#134934=CARTESIAN_POINT('Ctrl Pts',(-30.9447802599345,-63.733537783742,
12.));
#134935=CARTESIAN_POINT('Ctrl Pts',(-30.9300115747113,-63.7177720601604,
0.));
#134936=CARTESIAN_POINT('Ctrl Pts',(-30.9300115747113,-63.7177720601604,
12.));
#134937=CARTESIAN_POINT('Ctrl Pts',(-30.9152921936471,-63.7020265004805,
0.));
#134938=CARTESIAN_POINT('Ctrl Pts',(-30.9152921936471,-63.7020265004805,
12.));
#134939=CARTESIAN_POINT('Ctrl Pts',(-30.9006221672703,-63.6863012697353,
0.));
#134940=CARTESIAN_POINT('Ctrl Pts',(-30.9006221672703,-63.6863012697353,
12.));
#134941=CARTESIAN_POINT('Ctrl Pts',(-30.8860015462488,-63.6705965337996,
0.));
#134942=CARTESIAN_POINT('Ctrl Pts',(-30.8860015462488,-63.6705965337996,
12.));
#134943=CARTESIAN_POINT('Ctrl Pts',(-30.8714303814202,-63.6549124594681,
0.));
#134944=CARTESIAN_POINT('Ctrl Pts',(-30.8714303814202,-63.6549124594681,
12.));
#134945=CARTESIAN_POINT('Ctrl Pts',(-30.8569087238132,-63.6392492145233,
0.));
#134946=CARTESIAN_POINT('Ctrl Pts',(-30.8569087238132,-63.6392492145233,
12.));
#134947=CARTESIAN_POINT('Ctrl Pts',(-30.8424366246665,-63.6236069678041,
0.));
#134948=CARTESIAN_POINT('Ctrl Pts',(-30.8424366246665,-63.6236069678041,
12.));
#134949=CARTESIAN_POINT('Ctrl Pts',(-30.8280141354448,-63.6079858892746,
0.));
#134950=CARTESIAN_POINT('Ctrl Pts',(-30.8280141354448,-63.6079858892746,
12.));
#134951=CARTESIAN_POINT('Ctrl Pts',(-30.8136413077999,-63.5923861498963,
0.));
#134952=CARTESIAN_POINT('Ctrl Pts',(-30.8136413077999,-63.5923861498963,
12.));
#134953=CARTESIAN_POINT('Ctrl Pts',(-30.7993181935265,-63.5768079214868,
0.));
#134954=CARTESIAN_POINT('Ctrl Pts',(-30.7993181935265,-63.5768079214868,
12.));
#134955=CARTESIAN_POINT('Ctrl Pts',(-30.7850448445207,-63.5612513766005,
0.));
#134956=CARTESIAN_POINT('Ctrl Pts',(-30.7850448445207,-63.5612513766005,
12.));
#134957=CARTESIAN_POINT('Ctrl Pts',(-30.7708213127169,-63.5457166883558,
0.));
#134958=CARTESIAN_POINT('Ctrl Pts',(-30.7708213127169,-63.5457166883558,
12.));
#134959=CARTESIAN_POINT('Ctrl Pts',(-30.7566476500772,-63.5302040304173,
0.));
#134960=CARTESIAN_POINT('Ctrl Pts',(-30.7566476500772,-63.5302040304173,
12.));
#134961=CARTESIAN_POINT('Ctrl Pts',(-30.7425239087294,-63.514713577392,
0.));
#134962=CARTESIAN_POINT('Ctrl Pts',(-30.7425239087294,-63.514713577392,
12.));
#134963=CARTESIAN_POINT('Ctrl Pts',(-30.7284501410827,-63.4992455051805,
0.));
#134964=CARTESIAN_POINT('Ctrl Pts',(-30.7284501410827,-63.4992455051805,
12.));
#134965=CARTESIAN_POINT('Ctrl Pts',(-30.7144263999259,-63.4837999912758,
0.));
#134966=CARTESIAN_POINT('Ctrl Pts',(-30.7144263999259,-63.4837999912758,
12.));
#134967=CARTESIAN_POINT('Ctrl Pts',(-30.7004527385806,-63.4683772152497,
0.));
#134968=CARTESIAN_POINT('Ctrl Pts',(-30.7004527385806,-63.4683772152497,
12.));
#134969=CARTESIAN_POINT('Ctrl Pts',(-30.6865292107911,-63.452977358421,
0.));
#134970=CARTESIAN_POINT('Ctrl Pts',(-30.6865292107911,-63.452977358421,
12.));
#134971=CARTESIAN_POINT('Ctrl Pts',(-30.6726558704302,-63.4376006029575,
0.));
#134972=CARTESIAN_POINT('Ctrl Pts',(-30.6726558704302,-63.4376006029575,
12.));
#134973=CARTESIAN_POINT('Ctrl Pts',(-30.6588327712482,-63.4222471311236,
0.));
#134974=CARTESIAN_POINT('Ctrl Pts',(-30.6588327712482,-63.4222471311236,
12.));
#134975=CARTESIAN_POINT('Ctrl Pts',(-30.6450599666135,-63.4069171245093,
0.));
#134976=CARTESIAN_POINT('Ctrl Pts',(-30.6450599666135,-63.4069171245093,
12.));
#134977=CARTESIAN_POINT('Ctrl Pts',(-30.6313375092085,-63.3916107631421,
0.));
#134978=CARTESIAN_POINT('Ctrl Pts',(-30.6313375092085,-63.3916107631421,
12.));
#134979=CARTESIAN_POINT('Ctrl Pts',(-30.6176654515988,-63.3763282271838,
0.));
#134980=CARTESIAN_POINT('Ctrl Pts',(-30.6176654515988,-63.3763282271838,
12.));
#134981=CARTESIAN_POINT('Ctrl Pts',(-30.604043846909,-63.3610696989599,
0.));
#134982=CARTESIAN_POINT('Ctrl Pts',(-30.604043846909,-63.3610696989599,
12.));
#134983=CARTESIAN_POINT('Ctrl Pts',(-30.5904727493707,-63.3458353646144,
0.));
#134984=CARTESIAN_POINT('Ctrl Pts',(-30.5904727493707,-63.3458353646144,
12.));
#134985=CARTESIAN_POINT('Ctrl Pts',(-30.5769522151147,-63.330625416509,
0.));
#134986=CARTESIAN_POINT('Ctrl Pts',(-30.5769522151147,-63.330625416509,
12.));
#134987=CARTESIAN_POINT('Ctrl Pts',(-30.5634823022358,-63.315440053435,
0.));
#134988=CARTESIAN_POINT('Ctrl Pts',(-30.5634823022358,-63.315440053435,
12.));
#134989=CARTESIAN_POINT('Ctrl Pts',(-30.5500630691343,-63.3002794756049,
0.));
#134990=CARTESIAN_POINT('Ctrl Pts',(-30.5500630691343,-63.3002794756049,
12.));
#134991=CARTESIAN_POINT('Ctrl Pts',(-30.5366945730503,-63.2851438802462,
0.));
#134992=CARTESIAN_POINT('Ctrl Pts',(-30.5366945730503,-63.2851438802462,
12.));
#134993=CARTESIAN_POINT('Ctrl Pts',(-30.5233768687875,-63.2700334577661,
0.));
#134994=CARTESIAN_POINT('Ctrl Pts',(-30.5233768687875,-63.2700334577661,
12.));
#134995=CARTESIAN_POINT('Ctrl Pts',(-30.5101100066683,-63.2549483856268,
0.));
#134996=CARTESIAN_POINT('Ctrl Pts',(-30.5101100066683,-63.2549483856268,
12.));
#134997=CARTESIAN_POINT('Ctrl Pts',(-30.4968940345028,-63.2398888342612,
0.));
#134998=CARTESIAN_POINT('Ctrl Pts',(-30.4968940345028,-63.2398888342612,
12.));
#134999=CARTESIAN_POINT('Ctrl Pts',(-30.4837290015011,-63.2248549788272,
0.));
#135000=CARTESIAN_POINT('Ctrl Pts',(-30.4837290015011,-63.2248549788272,
12.));
#135001=CARTESIAN_POINT('Ctrl Pts',(-30.470614961416,-63.2098470086636,
0.));
#135002=CARTESIAN_POINT('Ctrl Pts',(-30.470614961416,-63.2098470086636,
12.));
#135003=CARTESIAN_POINT('Ctrl Pts',(-30.4575519763305,-63.1948651386868,
0.));
#135004=CARTESIAN_POINT('Ctrl Pts',(-30.4575519763305,-63.1948651386868,
12.));
#135005=CARTESIAN_POINT('Ctrl Pts',(-30.4445401192324,-63.1799096171757,
0.));
#135006=CARTESIAN_POINT('Ctrl Pts',(-30.4445401192324,-63.1799096171757,
12.));
#135007=CARTESIAN_POINT('Ctrl Pts',(-30.431579465967,-63.1649807016766,
0.));
#135008=CARTESIAN_POINT('Ctrl Pts',(-30.431579465967,-63.1649807016766,
12.));
#135009=CARTESIAN_POINT('Ctrl Pts',(-30.4186700875598,-63.1500786361382,
0.));
#135010=CARTESIAN_POINT('Ctrl Pts',(-30.4186700875598,-63.1500786361382,
12.));
#135011=CARTESIAN_POINT('Ctrl Pts',(-30.4058120432259,-63.1352036298512,
0.));
#135012=CARTESIAN_POINT('Ctrl Pts',(-30.4058120432259,-63.1352036298512,
12.));
#135013=CARTESIAN_POINT('Ctrl Pts',(-30.3930053710592,-63.1203558300911,
0.));
#135014=CARTESIAN_POINT('Ctrl Pts',(-30.3930053710592,-63.1203558300911,
12.));
#135015=CARTESIAN_POINT('Ctrl Pts',(-30.3802500880565,-63.1055353202641,
0.));
#135016=CARTESIAN_POINT('Ctrl Pts',(-30.3802500880565,-63.1055353202641,
12.));
#135017=CARTESIAN_POINT('Ctrl Pts',(-30.3700869762658,-63.0937007763826,
0.));
#135018=CARTESIAN_POINT('Ctrl Pts',(-30.3700869762658,-63.0937007763826,
12.));
#135019=CARTESIAN_POINT('Ctrl Pts',(-30.3624877680747,-63.0848371718274,
0.));
#135020=CARTESIAN_POINT('Ctrl Pts',(-30.3624877680747,-63.0848371718274,
12.));
#135021=CARTESIAN_POINT('Ctrl Pts',(-30.3574319069366,-63.0789335700774,
0.));
#135022=CARTESIAN_POINT('Ctrl Pts',(-30.3574319069366,-63.0789335700774,
12.));
#135023=CARTESIAN_POINT('Ctrl Pts',(-30.3549065457811,-63.0759831361898,
0.));
#135024=CARTESIAN_POINT('Ctrl Pts',(-30.3549065457811,-63.0759831361898,
12.));
#135025=CARTESIAN_POINT('',(-30.3549065457811,-63.0759831361898,12.));
#135026=CARTESIAN_POINT('Ctrl Pts',(-30.3549065457811,-63.0759831361898,
12.));
#135027=CARTESIAN_POINT('Ctrl Pts',(-30.3574319069366,-63.0789335700774,
12.));
#135028=CARTESIAN_POINT('Ctrl Pts',(-30.3624877680747,-63.0848371718274,
12.));
#135029=CARTESIAN_POINT('Ctrl Pts',(-30.3700869762658,-63.0937007763826,
12.));
#135030=CARTESIAN_POINT('Ctrl Pts',(-30.3802500880565,-63.1055353202641,
12.));
#135031=CARTESIAN_POINT('Ctrl Pts',(-30.3930053710592,-63.1203558300911,
12.));
#135032=CARTESIAN_POINT('Ctrl Pts',(-30.4058120432259,-63.1352036298512,
12.));
#135033=CARTESIAN_POINT('Ctrl Pts',(-30.4186700875598,-63.1500786361382,
12.));
#135034=CARTESIAN_POINT('Ctrl Pts',(-30.431579465967,-63.1649807016766,
12.));
#135035=CARTESIAN_POINT('Ctrl Pts',(-30.4445401192324,-63.1799096171757,
12.));
#135036=CARTESIAN_POINT('Ctrl Pts',(-30.4575519763305,-63.1948651386868,
12.));
#135037=CARTESIAN_POINT('Ctrl Pts',(-30.470614961416,-63.2098470086636,
12.));
#135038=CARTESIAN_POINT('Ctrl Pts',(-30.4837290015011,-63.2248549788272,
12.));
#135039=CARTESIAN_POINT('Ctrl Pts',(-30.4968940345028,-63.2398888342612,
12.));
#135040=CARTESIAN_POINT('Ctrl Pts',(-30.5101100066683,-63.2549483856268,
12.));
#135041=CARTESIAN_POINT('Ctrl Pts',(-30.5233768687875,-63.2700334577661,
12.));
#135042=CARTESIAN_POINT('Ctrl Pts',(-30.5366945730503,-63.2851438802462,
12.));
#135043=CARTESIAN_POINT('Ctrl Pts',(-30.5500630691343,-63.3002794756049,
12.));
#135044=CARTESIAN_POINT('Ctrl Pts',(-30.5634823022358,-63.315440053435,
12.));
#135045=CARTESIAN_POINT('Ctrl Pts',(-30.5769522151147,-63.330625416509,
12.));
#135046=CARTESIAN_POINT('Ctrl Pts',(-30.5904727493707,-63.3458353646144,
12.));
#135047=CARTESIAN_POINT('Ctrl Pts',(-30.604043846909,-63.3610696989599,
12.));
#135048=CARTESIAN_POINT('Ctrl Pts',(-30.6176654515988,-63.3763282271838,
12.));
#135049=CARTESIAN_POINT('Ctrl Pts',(-30.6313375092085,-63.3916107631421,
12.));
#135050=CARTESIAN_POINT('Ctrl Pts',(-30.6450599666135,-63.4069171245093,
12.));
#135051=CARTESIAN_POINT('Ctrl Pts',(-30.6588327712482,-63.4222471311236,
12.));
#135052=CARTESIAN_POINT('Ctrl Pts',(-30.6726558704302,-63.4376006029575,
12.));
#135053=CARTESIAN_POINT('Ctrl Pts',(-30.6865292107911,-63.452977358421,
12.));
#135054=CARTESIAN_POINT('Ctrl Pts',(-30.7004527385806,-63.4683772152497,
12.));
#135055=CARTESIAN_POINT('Ctrl Pts',(-30.7144263999259,-63.4837999912758,
12.));
#135056=CARTESIAN_POINT('Ctrl Pts',(-30.7284501410827,-63.4992455051805,
12.));
#135057=CARTESIAN_POINT('Ctrl Pts',(-30.7425239087294,-63.514713577392,
12.));
#135058=CARTESIAN_POINT('Ctrl Pts',(-30.7566476500772,-63.5302040304173,
12.));
#135059=CARTESIAN_POINT('Ctrl Pts',(-30.7708213127169,-63.5457166883558,
12.));
#135060=CARTESIAN_POINT('Ctrl Pts',(-30.7850448445207,-63.5612513766005,
12.));
#135061=CARTESIAN_POINT('Ctrl Pts',(-30.7993181935265,-63.5768079214868,
12.));
#135062=CARTESIAN_POINT('Ctrl Pts',(-30.8136413077999,-63.5923861498963,
12.));
#135063=CARTESIAN_POINT('Ctrl Pts',(-30.8280141354448,-63.6079858892746,
12.));
#135064=CARTESIAN_POINT('Ctrl Pts',(-30.8424366246665,-63.6236069678041,
12.));
#135065=CARTESIAN_POINT('Ctrl Pts',(-30.8569087238132,-63.6392492145233,
12.));
#135066=CARTESIAN_POINT('Ctrl Pts',(-30.8714303814202,-63.6549124594681,
12.));
#135067=CARTESIAN_POINT('Ctrl Pts',(-30.8860015462488,-63.6705965337996,
12.));
#135068=CARTESIAN_POINT('Ctrl Pts',(-30.9006221672703,-63.6863012697353,
12.));
#135069=CARTESIAN_POINT('Ctrl Pts',(-30.9152921936471,-63.7020265004805,
12.));
#135070=CARTESIAN_POINT('Ctrl Pts',(-30.9300115747113,-63.7177720601604,
12.));
#135071=CARTESIAN_POINT('Ctrl Pts',(-30.9447802599345,-63.733537783742,
12.));
#135072=CARTESIAN_POINT('Ctrl Pts',(-30.9595981989091,-63.7493235069844,
12.));
#135073=CARTESIAN_POINT('Ctrl Pts',(-30.9744653413679,-63.7651290664713,
12.));
#135074=CARTESIAN_POINT('Ctrl Pts',(-30.9893816371907,-63.7809542996258,
12.));
#135075=CARTESIAN_POINT('Ctrl Pts',(-31.0043470364112,-63.7967990447287,
12.));
#135076=CARTESIAN_POINT('Ctrl Pts',(-31.0193614892177,-63.8126631409376,
12.));
#135077=CARTESIAN_POINT('Ctrl Pts',(-31.0344249459544,-63.8285464282857,
12.));
#135078=CARTESIAN_POINT('Ctrl Pts',(-31.0495373571218,-63.8444487476615,
12.));
#135079=CARTESIAN_POINT('Ctrl Pts',(-31.0646986733724,-63.8603699407922,
12.));
#135080=CARTESIAN_POINT('Ctrl Pts',(-31.079908845504,-63.8763098502235,
12.));
#135081=CARTESIAN_POINT('Ctrl Pts',(-31.0951678244454,-63.8922683192962,
12.));
#135082=CARTESIAN_POINT('Ctrl Pts',(-31.1104755612606,-63.9082451921447,
12.));
#135083=CARTESIAN_POINT('Ctrl Pts',(-31.1258320071545,-63.9242403136954,
12.));
#135084=CARTESIAN_POINT('Ctrl Pts',(-31.1412371134727,-63.940253529665,
12.));
#135085=CARTESIAN_POINT('Ctrl Pts',(-31.1566908316993,-63.9562846865566,
12.));
#135086=CARTESIAN_POINT('Ctrl Pts',(-31.1721931134488,-63.972333631655,
12.));
#135087=CARTESIAN_POINT('Ctrl Pts',(-31.1877439104717,-63.9884002130209,
12.));
#135088=CARTESIAN_POINT('Ctrl Pts',(-31.2033431746559,-64.004484279483,
12.));
#135089=CARTESIAN_POINT('Ctrl Pts',(-31.2189908580245,-64.0205856806298,
12.));
#135090=CARTESIAN_POINT('Ctrl Pts',(-31.23468691273,-64.036704266799,12.));
#135091=CARTESIAN_POINT('Ctrl Pts',(-31.2504312910457,-64.0528398890671,
12.));
#135092=CARTESIAN_POINT('Ctrl Pts',(-31.2662239453734,-64.0689923992474,
12.));
#135093=CARTESIAN_POINT('Ctrl Pts',(-31.2820648282451,-64.0851616498861,
12.));
#135094=CARTESIAN_POINT('Ctrl Pts',(-31.2979538923214,-64.1013474942554,
12.));
#135095=CARTESIAN_POINT('Ctrl Pts',(-31.3138910903852,-64.1175497863475,
12.));
#135096=CARTESIAN_POINT('Ctrl Pts',(-31.3298763753366,-64.1337683808667,
12.));
#135097=CARTESIAN_POINT('Ctrl Pts',(-31.3459097001996,-64.150003133226,
12.));
#135098=CARTESIAN_POINT('Ctrl Pts',(-31.3619910181223,-64.1662538995407,
12.));
#135099=CARTESIAN_POINT('Ctrl Pts',(-31.3781202823758,-64.1825205366231,
12.));
#135100=CARTESIAN_POINT('Ctrl Pts',(-31.3942974463458,-64.1988029019733,
12.));
#135101=CARTESIAN_POINT('Ctrl Pts',(-31.4105224635298,-64.2151008537733,
12.));
#135102=CARTESIAN_POINT('Ctrl Pts',(-31.426795287544,-64.2314142508843,
12.));
#135103=CARTESIAN_POINT('Ctrl Pts',(-31.443115872123,-64.2477429528408,
12.));
#135104=CARTESIAN_POINT('Ctrl Pts',(-31.4594841711189,-64.264086819846,
12.));
#135105=CARTESIAN_POINT('Ctrl Pts',(-31.4759001384923,-64.2804457127633,
12.));
#135106=CARTESIAN_POINT('Ctrl Pts',(-31.4923637283109,-64.2968194931113,
12.));
#135107=CARTESIAN_POINT('Ctrl Pts',(-31.5088748947565,-64.3132080230603,
12.));
#135108=CARTESIAN_POINT('Ctrl Pts',(-31.525433592124,-64.3296111654273,
12.));
#135109=CARTESIAN_POINT('Ctrl Pts',(-31.5420397748198,-64.34602878367,12.));
#135110=CARTESIAN_POINT('Ctrl Pts',(-31.5586933973532,-64.3624607418798,
12.));
#135111=CARTESIAN_POINT('Ctrl Pts',(-31.5753944143355,-64.3789069047768,
12.));
#135112=CARTESIAN_POINT('Ctrl Pts',(-31.5921427804879,-64.3953671377071,
12.));
#135113=CARTESIAN_POINT('Ctrl Pts',(-31.6089384506399,-64.4118413066386,
12.));
#135114=CARTESIAN_POINT('Ctrl Pts',(-31.6257813797282,-64.4283292781553,
12.));
#135115=CARTESIAN_POINT('Ctrl Pts',(-31.6426715227865,-64.4448309194498,
12.));
#135116=CARTESIAN_POINT('Ctrl Pts',(-31.6596088349468,-64.4613460983186,
12.));
#135117=CARTESIAN_POINT('Ctrl Pts',(-31.6765932714456,-64.4778746831597,
12.));
#135118=CARTESIAN_POINT('Ctrl Pts',(-31.6936247876228,-64.4944165429672,
12.));
#135119=CARTESIAN_POINT('Ctrl Pts',(-31.7107033389204,-64.5109715473276,
12.));
#135120=CARTESIAN_POINT('Ctrl Pts',(-31.7278288808736,-64.5275395664134,
12.));
#135121=CARTESIAN_POINT('Ctrl Pts',(-31.7450013691117,-64.5441204709779,
12.));
#135122=CARTESIAN_POINT('Ctrl Pts',(-31.7622207593637,-64.5607141323527,
12.));
#135123=CARTESIAN_POINT('Ctrl Pts',(-31.7794870074584,-64.5773204224429,
12.));
#135124=CARTESIAN_POINT('Ctrl Pts',(-31.7968000693218,-64.5939392137233,
12.));
#135125=CARTESIAN_POINT('Ctrl Pts',(-31.8141599009685,-64.6105703792311,
12.));
#135126=CARTESIAN_POINT('Ctrl Pts',(-31.8315664585027,-64.6272137925629,
12.));
#135127=CARTESIAN_POINT('Ctrl Pts',(-31.849019698125,-64.6438693278718,
12.));
#135128=CARTESIAN_POINT('Ctrl Pts',(-31.8665195761312,-64.6605368598631,
12.));
#135129=CARTESIAN_POINT('Ctrl Pts',(-31.8840660489106,-64.6772162637904,
12.));
#135130=CARTESIAN_POINT('Ctrl Pts',(-31.9016590729371,-64.693907415449,
12.));
#135131=CARTESIAN_POINT('Ctrl Pts',(-31.9192986047702,-64.7106101911722,
12.));
#135132=CARTESIAN_POINT('Ctrl Pts',(-31.9369846010613,-64.727324467829,
12.));
#135133=CARTESIAN_POINT('Ctrl Pts',(-31.9547170185533,-64.74405012282,12.));
#135134=CARTESIAN_POINT('Ctrl Pts',(-31.9724958140791,-64.7607870340738,
12.));
#135135=CARTESIAN_POINT('Ctrl Pts',(-31.9903209445522,-64.7775350800404,
12.));
#135136=CARTESIAN_POINT('Ctrl Pts',(-32.0081923669678,-64.7942941396883,
12.));
#135137=CARTESIAN_POINT('Ctrl Pts',(-32.0261100384092,-64.811064092502,
12.));
#135138=CARTESIAN_POINT('Ctrl Pts',(-32.0440739160477,-64.8278448184785,
12.));
#135139=CARTESIAN_POINT('Ctrl Pts',(-32.0620839571409,-64.8446361981234,
12.));
#135140=CARTESIAN_POINT('Ctrl Pts',(-32.0801401190244,-64.8614381124454,
12.));
#135141=CARTESIAN_POINT('Ctrl Pts',(-32.0982423591113,-64.8782504429527,
12.));
#135142=CARTESIAN_POINT('Ctrl Pts',(-32.1163906348984,-64.8950730716501,
12.));
#135143=CARTESIAN_POINT('Ctrl Pts',(-32.1345849039674,-64.9119058810366,
12.));
#135144=CARTESIAN_POINT('Ctrl Pts',(-32.1528251239831,-64.9287487541015,
12.));
#135145=CARTESIAN_POINT('Ctrl Pts',(-32.1711112526855,-64.9456015743192,
12.));
#135146=CARTESIAN_POINT('Ctrl Pts',(-32.1894432478881,-64.9624642256461,
12.));
#135147=CARTESIAN_POINT('Ctrl Pts',(-32.207821067485,-64.9793365925178,
12.));
#135148=CARTESIAN_POINT('Ctrl Pts',(-32.2262446694513,-64.9962185598461,
12.));
#135149=CARTESIAN_POINT('Ctrl Pts',(-32.2447140118422,-65.0131100130157,
12.));
#135150=CARTESIAN_POINT('Ctrl Pts',(-32.2632290527862,-65.03001083788,12.));
#135151=CARTESIAN_POINT('Ctrl Pts',(-32.2817897504807,-65.0469209207563,
12.));
#135152=CARTESIAN_POINT('Ctrl Pts',(-32.3003960632007,-65.0638401484257,
12.));
#135153=CARTESIAN_POINT('Ctrl Pts',(-32.3190479492987,-65.0807684081281,
12.));
#135154=CARTESIAN_POINT('Ctrl Pts',(-32.3377453672051,-65.0977055875607,
12.));
#135155=CARTESIAN_POINT('Ctrl Pts',(-32.3564882754212,-65.1146515748722,
12.));
#135156=CARTESIAN_POINT('Ctrl Pts',(-32.3752766325136,-65.1316062586588,
12.));
#135157=CARTESIAN_POINT('Ctrl Pts',(-32.3941103971221,-65.1485695279635,
12.));
#135158=CARTESIAN_POINT('Ctrl Pts',(-32.4129895279615,-65.1655412722725,
12.));
#135159=CARTESIAN_POINT('Ctrl Pts',(-32.4319139838213,-65.182521381514,
12.));
#135160=CARTESIAN_POINT('Ctrl Pts',(-32.450883723561,-65.1995097460538,
12.));
#135161=CARTESIAN_POINT('Ctrl Pts',(-32.4698987061032,-65.2165062566924,
12.));
#135162=CARTESIAN_POINT('Ctrl Pts',(-32.4889588904392,-65.2335108046614,
12.));
#135163=CARTESIAN_POINT('Ctrl Pts',(-32.5080642356328,-65.2505232816209,
12.));
#135164=CARTESIAN_POINT('Ctrl Pts',(-32.5272147008191,-65.2675435796558,
12.));
#135165=CARTESIAN_POINT('Ctrl Pts',(-32.5464102452015,-65.2845715912721,
12.));
#135166=CARTESIAN_POINT('Ctrl Pts',(-32.5656508280422,-65.3016072093912,
12.));
#135167=CARTESIAN_POINT('Ctrl Pts',(-32.5849364086679,-65.31865032735,12.));
#135168=CARTESIAN_POINT('Ctrl Pts',(-32.6042669464751,-65.3357008389003,
12.));
#135169=CARTESIAN_POINT('Ctrl Pts',(-32.6236424009301,-65.3527586382081,
12.));
#135170=CARTESIAN_POINT('Ctrl Pts',(-32.6430627315674,-65.3698236198512,
12.));
#135171=CARTESIAN_POINT('Ctrl Pts',(-32.6625278979811,-65.3868956788182,
12.));
#135172=CARTESIAN_POINT('Ctrl Pts',(-32.6820378598267,-65.4039747105038,
12.));
#135173=CARTESIAN_POINT('Ctrl Pts',(-32.7015925768265,-65.4210606107035,
12.));
#135174=CARTESIAN_POINT('Ctrl Pts',(-32.7211920087684,-65.4381532756065,
12.));
#135175=CARTESIAN_POINT('Ctrl Pts',(-32.7408361155037,-65.4552526017905,
12.));
#135176=CARTESIAN_POINT('Ctrl Pts',(-32.7605248569378,-65.4723584862122,
12.));
#135177=CARTESIAN_POINT('Ctrl Pts',(-32.7802581930287,-65.489470826206,
12.));
#135178=CARTESIAN_POINT('Ctrl Pts',(-32.8000360837975,-65.5065895194928,
12.));
#135179=CARTESIAN_POINT('Ctrl Pts',(-32.8198584893316,-65.5237144641857,
12.));
#135180=CARTESIAN_POINT('Ctrl Pts',(-32.8397253697866,-65.5408455587964,
12.));
#135181=CARTESIAN_POINT('Ctrl Pts',(-32.8596366853832,-65.5579827022421,
12.));
#135182=CARTESIAN_POINT('Ctrl Pts',(-32.879592396403,-65.5751257938472,
12.));
#135183=CARTESIAN_POINT('Ctrl Pts',(-32.8995924631898,-65.5922747333194,
12.));
#135184=CARTESIAN_POINT('Ctrl Pts',(-32.9196368461463,-65.6094294207276,
12.));
#135185=CARTESIAN_POINT('Ctrl Pts',(-32.9397255057274,-65.6265897564783,
12.));
#135186=CARTESIAN_POINT('Ctrl Pts',(-32.9598584024313,-65.6437556412946,
12.));
#135187=CARTESIAN_POINT('Ctrl Pts',(-32.980035496784,-65.6609269761888,
12.));
#135188=CARTESIAN_POINT('Ctrl Pts',(-33.0002567493574,-65.6781036625027,
12.));
#135189=CARTESIAN_POINT('Ctrl Pts',(-33.0205221207873,-65.6952856019533,
12.));
#135190=CARTESIAN_POINT('Ctrl Pts',(-33.0408315717873,-65.7124726966802,
12.));
#135191=CARTESIAN_POINT('Ctrl Pts',(-33.0611850631582,-65.7296648492824,
12.));
#135192=CARTESIAN_POINT('Ctrl Pts',(-33.081582555798,-65.7468619628815,
12.));
#135193=CARTESIAN_POINT('Ctrl Pts',(-33.1020240106885,-65.7640639410661,
12.));
#135194=CARTESIAN_POINT('Ctrl Pts',(-33.1225093888672,-65.7812706877696,
12.));
#135195=CARTESIAN_POINT('Ctrl Pts',(-33.1430386513976,-65.7984821071623,
12.));
#135196=CARTESIAN_POINT('Ctrl Pts',(-33.16361175934,-65.8156981035503,12.));
#135197=CARTESIAN_POINT('Ctrl Pts',(-33.1842286737051,-65.8329185812375,
12.));
#135198=CARTESIAN_POINT('Ctrl Pts',(-33.2048893554491,-65.8501434445164,
12.));
#135199=CARTESIAN_POINT('Ctrl Pts',(-33.2255937655649,-65.8673725979577,
12.));
#135200=CARTESIAN_POINT('Ctrl Pts',(-33.2463418651493,-65.8846059466371,
12.));
#135201=CARTESIAN_POINT('Ctrl Pts',(-33.2671336154754,-65.9018433963889,
12.));
#135202=CARTESIAN_POINT('Ctrl Pts',(-33.2879689780573,-65.9190848540433,
12.));
#135203=CARTESIAN_POINT('Ctrl Pts',(-33.3088479147164,-65.9363302276846,
12.));
#135204=CARTESIAN_POINT('Ctrl Pts',(-33.3297703874266,-65.9535794260831,
12.));
#135205=CARTESIAN_POINT('Ctrl Pts',(-33.3507363581593,-65.970832358141,
12.));
#135206=CARTESIAN_POINT('Ctrl Pts',(-33.37174578871,-65.9880889322831,12.));
#135207=CARTESIAN_POINT('Ctrl Pts',(-33.3927986405605,-66.0053490559812,
12.));
#135208=CARTESIAN_POINT('Ctrl Pts',(-33.4138948746388,-66.0226126349446,
12.));
#135209=CARTESIAN_POINT('Ctrl Pts',(-33.4350344515101,-66.0398795737777,
12.));
#135210=CARTESIAN_POINT('Ctrl Pts',(-33.4562173318025,-66.0571497774434,
12.));
#135211=CARTESIAN_POINT('Ctrl Pts',(-33.4774434765746,-66.0744231525415,
12.));
#135212=CARTESIAN_POINT('Ctrl Pts',(-33.4987128476622,-66.0916996085244,
12.));
#135213=CARTESIAN_POINT('Ctrl Pts',(-33.5200254081243,-66.1089790592729,
12.));
#135214=CARTESIAN_POINT('Ctrl Pts',(-33.5413811223451,-66.1262614234674,
12.));
#135215=CARTESIAN_POINT('Ctrl Pts',(-33.5597240685846,-66.1410781873278,
12.));
#135216=CARTESIAN_POINT('Ctrl Pts',(-33.5738105077875,-66.1524393974174,
12.));
#135217=CARTESIAN_POINT('Ctrl Pts',(-33.5836213514189,-66.1603438177522,
12.));
#135218=CARTESIAN_POINT('Ctrl Pts',(-33.5891439876494,-66.1647906582657,
12.));
#135219=CARTESIAN_POINT('Ctrl Pts',(-33.590372266528,-66.1657795405962,
12.));
#135220=CARTESIAN_POINT('',(-30.3549065457811,-63.0759831361898,0.));
#135221=CARTESIAN_POINT('',(-30.3549065457811,-63.0759831361898,0.));
#135222=CARTESIAN_POINT('Ctrl Pts',(-33.590372266528,-66.1657795405962,
0.));
#135223=CARTESIAN_POINT('Ctrl Pts',(-33.5891439876494,-66.1647906582657,
0.));
#135224=CARTESIAN_POINT('Ctrl Pts',(-33.5836213514189,-66.1603438177522,
0.));
#135225=CARTESIAN_POINT('Ctrl Pts',(-33.5738105077875,-66.1524393974174,
0.));
#135226=CARTESIAN_POINT('Ctrl Pts',(-33.5597240685846,-66.1410781873278,
0.));
#135227=CARTESIAN_POINT('Ctrl Pts',(-33.5413811223451,-66.1262614234674,
0.));
#135228=CARTESIAN_POINT('Ctrl Pts',(-33.5200254081243,-66.1089790592729,
0.));
#135229=CARTESIAN_POINT('Ctrl Pts',(-33.4987128476622,-66.0916996085244,
0.));
#135230=CARTESIAN_POINT('Ctrl Pts',(-33.4774434765746,-66.0744231525415,
0.));
#135231=CARTESIAN_POINT('Ctrl Pts',(-33.4562173318025,-66.0571497774434,
0.));
#135232=CARTESIAN_POINT('Ctrl Pts',(-33.4350344515101,-66.0398795737777,
0.));
#135233=CARTESIAN_POINT('Ctrl Pts',(-33.4138948746388,-66.0226126349446,
0.));
#135234=CARTESIAN_POINT('Ctrl Pts',(-33.3927986405605,-66.0053490559812,
0.));
#135235=CARTESIAN_POINT('Ctrl Pts',(-33.37174578871,-65.9880889322831,0.));
#135236=CARTESIAN_POINT('Ctrl Pts',(-33.3507363581593,-65.970832358141,
0.));
#135237=CARTESIAN_POINT('Ctrl Pts',(-33.3297703874266,-65.9535794260831,
0.));
#135238=CARTESIAN_POINT('Ctrl Pts',(-33.3088479147164,-65.9363302276846,
0.));
#135239=CARTESIAN_POINT('Ctrl Pts',(-33.2879689780573,-65.9190848540433,
0.));
#135240=CARTESIAN_POINT('Ctrl Pts',(-33.2671336154754,-65.9018433963889,
0.));
#135241=CARTESIAN_POINT('Ctrl Pts',(-33.2463418651493,-65.8846059466371,
0.));
#135242=CARTESIAN_POINT('Ctrl Pts',(-33.2255937655649,-65.8673725979577,
0.));
#135243=CARTESIAN_POINT('Ctrl Pts',(-33.2048893554491,-65.8501434445164,
0.));
#135244=CARTESIAN_POINT('Ctrl Pts',(-33.1842286737051,-65.8329185812375,
0.));
#135245=CARTESIAN_POINT('Ctrl Pts',(-33.16361175934,-65.8156981035503,0.));
#135246=CARTESIAN_POINT('Ctrl Pts',(-33.1430386513976,-65.7984821071623,
0.));
#135247=CARTESIAN_POINT('Ctrl Pts',(-33.1225093888672,-65.7812706877696,
0.));
#135248=CARTESIAN_POINT('Ctrl Pts',(-33.1020240106885,-65.7640639410661,
0.));
#135249=CARTESIAN_POINT('Ctrl Pts',(-33.081582555798,-65.7468619628815,
0.));
#135250=CARTESIAN_POINT('Ctrl Pts',(-33.0611850631582,-65.7296648492824,
0.));
#135251=CARTESIAN_POINT('Ctrl Pts',(-33.0408315717873,-65.7124726966802,
0.));
#135252=CARTESIAN_POINT('Ctrl Pts',(-33.0205221207873,-65.6952856019533,
0.));
#135253=CARTESIAN_POINT('Ctrl Pts',(-33.0002567493574,-65.6781036625027,
0.));
#135254=CARTESIAN_POINT('Ctrl Pts',(-32.980035496784,-65.6609269761888,
0.));
#135255=CARTESIAN_POINT('Ctrl Pts',(-32.9598584024313,-65.6437556412946,
0.));
#135256=CARTESIAN_POINT('Ctrl Pts',(-32.9397255057274,-65.6265897564783,
0.));
#135257=CARTESIAN_POINT('Ctrl Pts',(-32.9196368461463,-65.6094294207276,
0.));
#135258=CARTESIAN_POINT('Ctrl Pts',(-32.8995924631898,-65.5922747333194,
0.));
#135259=CARTESIAN_POINT('Ctrl Pts',(-32.879592396403,-65.5751257938472,
0.));
#135260=CARTESIAN_POINT('Ctrl Pts',(-32.8596366853832,-65.5579827022421,
0.));
#135261=CARTESIAN_POINT('Ctrl Pts',(-32.8397253697866,-65.5408455587964,
0.));
#135262=CARTESIAN_POINT('Ctrl Pts',(-32.8198584893316,-65.5237144641857,
0.));
#135263=CARTESIAN_POINT('Ctrl Pts',(-32.8000360837975,-65.5065895194928,
0.));
#135264=CARTESIAN_POINT('Ctrl Pts',(-32.7802581930287,-65.489470826206,
0.));
#135265=CARTESIAN_POINT('Ctrl Pts',(-32.7605248569378,-65.4723584862122,
0.));
#135266=CARTESIAN_POINT('Ctrl Pts',(-32.7408361155037,-65.4552526017905,
0.));
#135267=CARTESIAN_POINT('Ctrl Pts',(-32.7211920087684,-65.4381532756065,
0.));
#135268=CARTESIAN_POINT('Ctrl Pts',(-32.7015925768265,-65.4210606107035,
0.));
#135269=CARTESIAN_POINT('Ctrl Pts',(-32.6820378598267,-65.4039747105038,
0.));
#135270=CARTESIAN_POINT('Ctrl Pts',(-32.6625278979811,-65.3868956788182,
0.));
#135271=CARTESIAN_POINT('Ctrl Pts',(-32.6430627315674,-65.3698236198512,
0.));
#135272=CARTESIAN_POINT('Ctrl Pts',(-32.6236424009301,-65.3527586382081,
0.));
#135273=CARTESIAN_POINT('Ctrl Pts',(-32.6042669464751,-65.3357008389003,
0.));
#135274=CARTESIAN_POINT('Ctrl Pts',(-32.5849364086679,-65.31865032735,0.));
#135275=CARTESIAN_POINT('Ctrl Pts',(-32.5656508280422,-65.3016072093912,
0.));
#135276=CARTESIAN_POINT('Ctrl Pts',(-32.5464102452015,-65.2845715912721,
0.));
#135277=CARTESIAN_POINT('Ctrl Pts',(-32.5272147008191,-65.2675435796558,
0.));
#135278=CARTESIAN_POINT('Ctrl Pts',(-32.5080642356328,-65.2505232816209,
0.));
#135279=CARTESIAN_POINT('Ctrl Pts',(-32.4889588904392,-65.2335108046614,
0.));
#135280=CARTESIAN_POINT('Ctrl Pts',(-32.4698987061032,-65.2165062566924,
0.));
#135281=CARTESIAN_POINT('Ctrl Pts',(-32.450883723561,-65.1995097460538,
0.));
#135282=CARTESIAN_POINT('Ctrl Pts',(-32.4319139838213,-65.182521381514,
0.));
#135283=CARTESIAN_POINT('Ctrl Pts',(-32.4129895279615,-65.1655412722725,
0.));
#135284=CARTESIAN_POINT('Ctrl Pts',(-32.3941103971221,-65.1485695279635,
0.));
#135285=CARTESIAN_POINT('Ctrl Pts',(-32.3752766325136,-65.1316062586588,
0.));
#135286=CARTESIAN_POINT('Ctrl Pts',(-32.3564882754212,-65.1146515748722,
0.));
#135287=CARTESIAN_POINT('Ctrl Pts',(-32.3377453672051,-65.0977055875607,
0.));
#135288=CARTESIAN_POINT('Ctrl Pts',(-32.3190479492987,-65.0807684081281,
0.));
#135289=CARTESIAN_POINT('Ctrl Pts',(-32.3003960632007,-65.0638401484257,
0.));
#135290=CARTESIAN_POINT('Ctrl Pts',(-32.2817897504807,-65.0469209207563,
0.));
#135291=CARTESIAN_POINT('Ctrl Pts',(-32.2632290527862,-65.03001083788,0.));
#135292=CARTESIAN_POINT('Ctrl Pts',(-32.2447140118422,-65.0131100130157,
0.));
#135293=CARTESIAN_POINT('Ctrl Pts',(-32.2262446694513,-64.9962185598461,
0.));
#135294=CARTESIAN_POINT('Ctrl Pts',(-32.207821067485,-64.9793365925178,
0.));
#135295=CARTESIAN_POINT('Ctrl Pts',(-32.1894432478881,-64.9624642256461,
0.));
#135296=CARTESIAN_POINT('Ctrl Pts',(-32.1711112526855,-64.9456015743192,
0.));
#135297=CARTESIAN_POINT('Ctrl Pts',(-32.1528251239831,-64.9287487541015,
0.));
#135298=CARTESIAN_POINT('Ctrl Pts',(-32.1345849039674,-64.9119058810366,
0.));
#135299=CARTESIAN_POINT('Ctrl Pts',(-32.1163906348984,-64.8950730716501,
0.));
#135300=CARTESIAN_POINT('Ctrl Pts',(-32.0982423591113,-64.8782504429527,
0.));
#135301=CARTESIAN_POINT('Ctrl Pts',(-32.0801401190244,-64.8614381124454,
0.));
#135302=CARTESIAN_POINT('Ctrl Pts',(-32.0620839571409,-64.8446361981234,
0.));
#135303=CARTESIAN_POINT('Ctrl Pts',(-32.0440739160477,-64.8278448184785,
0.));
#135304=CARTESIAN_POINT('Ctrl Pts',(-32.0261100384092,-64.811064092502,
0.));
#135305=CARTESIAN_POINT('Ctrl Pts',(-32.0081923669678,-64.7942941396883,
0.));
#135306=CARTESIAN_POINT('Ctrl Pts',(-31.9903209445522,-64.7775350800404,
0.));
#135307=CARTESIAN_POINT('Ctrl Pts',(-31.9724958140791,-64.7607870340738,
0.));
#135308=CARTESIAN_POINT('Ctrl Pts',(-31.9547170185533,-64.74405012282,0.));
#135309=CARTESIAN_POINT('Ctrl Pts',(-31.9369846010613,-64.727324467829,
0.));
#135310=CARTESIAN_POINT('Ctrl Pts',(-31.9192986047702,-64.7106101911722,
0.));
#135311=CARTESIAN_POINT('Ctrl Pts',(-31.9016590729371,-64.693907415449,
0.));
#135312=CARTESIAN_POINT('Ctrl Pts',(-31.8840660489106,-64.6772162637904,
0.));
#135313=CARTESIAN_POINT('Ctrl Pts',(-31.8665195761312,-64.6605368598631,
0.));
#135314=CARTESIAN_POINT('Ctrl Pts',(-31.849019698125,-64.6438693278718,
0.));
#135315=CARTESIAN_POINT('Ctrl Pts',(-31.8315664585027,-64.6272137925629,
0.));
#135316=CARTESIAN_POINT('Ctrl Pts',(-31.8141599009685,-64.6105703792311,
0.));
#135317=CARTESIAN_POINT('Ctrl Pts',(-31.7968000693218,-64.5939392137233,
0.));
#135318=CARTESIAN_POINT('Ctrl Pts',(-31.7794870074584,-64.5773204224429,
0.));
#135319=CARTESIAN_POINT('Ctrl Pts',(-31.7622207593637,-64.5607141323527,
0.));
#135320=CARTESIAN_POINT('Ctrl Pts',(-31.7450013691117,-64.5441204709779,
0.));
#135321=CARTESIAN_POINT('Ctrl Pts',(-31.7278288808736,-64.5275395664134,
0.));
#135322=CARTESIAN_POINT('Ctrl Pts',(-31.7107033389204,-64.5109715473276,
0.));
#135323=CARTESIAN_POINT('Ctrl Pts',(-31.6936247876228,-64.4944165429672,
0.));
#135324=CARTESIAN_POINT('Ctrl Pts',(-31.6765932714456,-64.4778746831597,
0.));
#135325=CARTESIAN_POINT('Ctrl Pts',(-31.6596088349468,-64.4613460983186,
0.));
#135326=CARTESIAN_POINT('Ctrl Pts',(-31.6426715227865,-64.4448309194498,
0.));
#135327=CARTESIAN_POINT('Ctrl Pts',(-31.6257813797282,-64.4283292781553,
0.));
#135328=CARTESIAN_POINT('Ctrl Pts',(-31.6089384506399,-64.4118413066386,
0.));
#135329=CARTESIAN_POINT('Ctrl Pts',(-31.5921427804879,-64.3953671377071,
0.));
#135330=CARTESIAN_POINT('Ctrl Pts',(-31.5753944143355,-64.3789069047768,
0.));
#135331=CARTESIAN_POINT('Ctrl Pts',(-31.5586933973532,-64.3624607418798,
0.));
#135332=CARTESIAN_POINT('Ctrl Pts',(-31.5420397748198,-64.34602878367,0.));
#135333=CARTESIAN_POINT('Ctrl Pts',(-31.525433592124,-64.3296111654273,
0.));
#135334=CARTESIAN_POINT('Ctrl Pts',(-31.5088748947565,-64.3132080230603,
0.));
#135335=CARTESIAN_POINT('Ctrl Pts',(-31.4923637283109,-64.2968194931113,
0.));
#135336=CARTESIAN_POINT('Ctrl Pts',(-31.4759001384923,-64.2804457127633,
0.));
#135337=CARTESIAN_POINT('Ctrl Pts',(-31.4594841711189,-64.264086819846,
0.));
#135338=CARTESIAN_POINT('Ctrl Pts',(-31.443115872123,-64.2477429528408,
0.));
#135339=CARTESIAN_POINT('Ctrl Pts',(-31.426795287544,-64.2314142508843,
0.));
#135340=CARTESIAN_POINT('Ctrl Pts',(-31.4105224635298,-64.2151008537733,
0.));
#135341=CARTESIAN_POINT('Ctrl Pts',(-31.3942974463458,-64.1988029019733,
0.));
#135342=CARTESIAN_POINT('Ctrl Pts',(-31.3781202823758,-64.1825205366231,
0.));
#135343=CARTESIAN_POINT('Ctrl Pts',(-31.3619910181223,-64.1662538995407,
0.));
#135344=CARTESIAN_POINT('Ctrl Pts',(-31.3459097001996,-64.150003133226,
0.));
#135345=CARTESIAN_POINT('Ctrl Pts',(-31.3298763753366,-64.1337683808667,
0.));
#135346=CARTESIAN_POINT('Ctrl Pts',(-31.3138910903852,-64.1175497863475,
0.));
#135347=CARTESIAN_POINT('Ctrl Pts',(-31.2979538923214,-64.1013474942554,
0.));
#135348=CARTESIAN_POINT('Ctrl Pts',(-31.2820648282451,-64.0851616498861,
0.));
#135349=CARTESIAN_POINT('Ctrl Pts',(-31.2662239453734,-64.0689923992474,
0.));
#135350=CARTESIAN_POINT('Ctrl Pts',(-31.2504312910457,-64.0528398890671,
0.));
#135351=CARTESIAN_POINT('Ctrl Pts',(-31.23468691273,-64.036704266799,0.));
#135352=CARTESIAN_POINT('Ctrl Pts',(-31.2189908580245,-64.0205856806298,
0.));
#135353=CARTESIAN_POINT('Ctrl Pts',(-31.2033431746559,-64.004484279483,
0.));
#135354=CARTESIAN_POINT('Ctrl Pts',(-31.1877439104717,-63.9884002130209,
0.));
#135355=CARTESIAN_POINT('Ctrl Pts',(-31.1721931134488,-63.972333631655,
0.));
#135356=CARTESIAN_POINT('Ctrl Pts',(-31.1566908316993,-63.9562846865566,
0.));
#135357=CARTESIAN_POINT('Ctrl Pts',(-31.1412371134727,-63.940253529665,
0.));
#135358=CARTESIAN_POINT('Ctrl Pts',(-31.1258320071545,-63.9242403136954,
0.));
#135359=CARTESIAN_POINT('Ctrl Pts',(-31.1104755612606,-63.9082451921447,
0.));
#135360=CARTESIAN_POINT('Ctrl Pts',(-31.0951678244454,-63.8922683192962,
0.));
#135361=CARTESIAN_POINT('Ctrl Pts',(-31.079908845504,-63.8763098502235,
0.));
#135362=CARTESIAN_POINT('Ctrl Pts',(-31.0646986733724,-63.8603699407922,
0.));
#135363=CARTESIAN_POINT('Ctrl Pts',(-31.0495373571218,-63.8444487476615,
0.));
#135364=CARTESIAN_POINT('Ctrl Pts',(-31.0344249459544,-63.8285464282857,
0.));
#135365=CARTESIAN_POINT('Ctrl Pts',(-31.0193614892177,-63.8126631409376,
0.));
#135366=CARTESIAN_POINT('Ctrl Pts',(-31.0043470364112,-63.7967990447287,
0.));
#135367=CARTESIAN_POINT('Ctrl Pts',(-30.9893816371907,-63.7809542996258,
0.));
#135368=CARTESIAN_POINT('Ctrl Pts',(-30.9744653413679,-63.7651290664713,
0.));
#135369=CARTESIAN_POINT('Ctrl Pts',(-30.9595981989091,-63.7493235069844,
0.));
#135370=CARTESIAN_POINT('Ctrl Pts',(-30.9447802599345,-63.733537783742,
0.));
#135371=CARTESIAN_POINT('Ctrl Pts',(-30.9300115747113,-63.7177720601604,
0.));
#135372=CARTESIAN_POINT('Ctrl Pts',(-30.9152921936471,-63.7020265004805,
0.));
#135373=CARTESIAN_POINT('Ctrl Pts',(-30.9006221672703,-63.6863012697353,
0.));
#135374=CARTESIAN_POINT('Ctrl Pts',(-30.8860015462488,-63.6705965337996,
0.));
#135375=CARTESIAN_POINT('Ctrl Pts',(-30.8714303814202,-63.6549124594681,
0.));
#135376=CARTESIAN_POINT('Ctrl Pts',(-30.8569087238132,-63.6392492145233,
0.));
#135377=CARTESIAN_POINT('Ctrl Pts',(-30.8424366246665,-63.6236069678041,
0.));
#135378=CARTESIAN_POINT('Ctrl Pts',(-30.8280141354448,-63.6079858892746,
0.));
#135379=CARTESIAN_POINT('Ctrl Pts',(-30.8136413077999,-63.5923861498963,
0.));
#135380=CARTESIAN_POINT('Ctrl Pts',(-30.7993181935265,-63.5768079214868,
0.));
#135381=CARTESIAN_POINT('Ctrl Pts',(-30.7850448445207,-63.5612513766005,
0.));
#135382=CARTESIAN_POINT('Ctrl Pts',(-30.7708213127169,-63.5457166883558,
0.));
#135383=CARTESIAN_POINT('Ctrl Pts',(-30.7566476500772,-63.5302040304173,
0.));
#135384=CARTESIAN_POINT('Ctrl Pts',(-30.7425239087294,-63.514713577392,
0.));
#135385=CARTESIAN_POINT('Ctrl Pts',(-30.7284501410827,-63.4992455051805,
0.));
#135386=CARTESIAN_POINT('Ctrl Pts',(-30.7144263999259,-63.4837999912758,
0.));
#135387=CARTESIAN_POINT('Ctrl Pts',(-30.7004527385806,-63.4683772152497,
0.));
#135388=CARTESIAN_POINT('Ctrl Pts',(-30.6865292107911,-63.452977358421,
0.));
#135389=CARTESIAN_POINT('Ctrl Pts',(-30.6726558704302,-63.4376006029575,
0.));
#135390=CARTESIAN_POINT('Ctrl Pts',(-30.6588327712482,-63.4222471311236,
0.));
#135391=CARTESIAN_POINT('Ctrl Pts',(-30.6450599666135,-63.4069171245093,
0.));
#135392=CARTESIAN_POINT('Ctrl Pts',(-30.6313375092085,-63.3916107631421,
0.));
#135393=CARTESIAN_POINT('Ctrl Pts',(-30.6176654515988,-63.3763282271838,
0.));
#135394=CARTESIAN_POINT('Ctrl Pts',(-30.604043846909,-63.3610696989599,
0.));
#135395=CARTESIAN_POINT('Ctrl Pts',(-30.5904727493707,-63.3458353646144,
0.));
#135396=CARTESIAN_POINT('Ctrl Pts',(-30.5769522151147,-63.330625416509,
0.));
#135397=CARTESIAN_POINT('Ctrl Pts',(-30.5634823022358,-63.315440053435,
0.));
#135398=CARTESIAN_POINT('Ctrl Pts',(-30.5500630691343,-63.3002794756049,
0.));
#135399=CARTESIAN_POINT('Ctrl Pts',(-30.5366945730503,-63.2851438802462,
0.));
#135400=CARTESIAN_POINT('Ctrl Pts',(-30.5233768687875,-63.2700334577661,
0.));
#135401=CARTESIAN_POINT('Ctrl Pts',(-30.5101100066683,-63.2549483856268,
0.));
#135402=CARTESIAN_POINT('Ctrl Pts',(-30.4968940345028,-63.2398888342612,
0.));
#135403=CARTESIAN_POINT('Ctrl Pts',(-30.4837290015011,-63.2248549788272,
0.));
#135404=CARTESIAN_POINT('Ctrl Pts',(-30.470614961416,-63.2098470086636,
0.));
#135405=CARTESIAN_POINT('Ctrl Pts',(-30.4575519763305,-63.1948651386868,
0.));
#135406=CARTESIAN_POINT('Ctrl Pts',(-30.4445401192324,-63.1799096171757,
0.));
#135407=CARTESIAN_POINT('Ctrl Pts',(-30.431579465967,-63.1649807016766,
0.));
#135408=CARTESIAN_POINT('Ctrl Pts',(-30.4186700875598,-63.1500786361382,
0.));
#135409=CARTESIAN_POINT('Ctrl Pts',(-30.4058120432259,-63.1352036298512,
0.));
#135410=CARTESIAN_POINT('Ctrl Pts',(-30.3930053710592,-63.1203558300911,
0.));
#135411=CARTESIAN_POINT('Ctrl Pts',(-30.3802500880565,-63.1055353202641,
0.));
#135412=CARTESIAN_POINT('Ctrl Pts',(-30.3700869762658,-63.0937007763826,
0.));
#135413=CARTESIAN_POINT('Ctrl Pts',(-30.3624877680747,-63.0848371718274,
0.));
#135414=CARTESIAN_POINT('Ctrl Pts',(-30.3574319069366,-63.0789335700774,
0.));
#135415=CARTESIAN_POINT('Ctrl Pts',(-30.3549065457811,-63.0759831361898,
0.));
#135416=CARTESIAN_POINT('Ctrl Pts',(-39.5004851439258,-63.1661434108059,
0.));
#135417=CARTESIAN_POINT('Ctrl Pts',(-39.5004851439258,-63.1661434108059,
12.));
#135418=CARTESIAN_POINT('Ctrl Pts',(-39.4958045828135,-63.1630766582787,
0.));
#135419=CARTESIAN_POINT('Ctrl Pts',(-39.4958045828135,-63.1630766582787,
12.));
#135420=CARTESIAN_POINT('Ctrl Pts',(-39.4864477303823,-63.1569429707875,
0.));
#135421=CARTESIAN_POINT('Ctrl Pts',(-39.4864477303823,-63.1569429707875,
12.));
#135422=CARTESIAN_POINT('Ctrl Pts',(-39.4724252611155,-63.1477418922405,
0.));
#135423=CARTESIAN_POINT('Ctrl Pts',(-39.4724252611155,-63.1477418922405,
12.));
#135424=CARTESIAN_POINT('Ctrl Pts',(-39.4537542552268,-63.1354726928398,
0.));
#135425=CARTESIAN_POINT('Ctrl Pts',(-39.4537542552268,-63.1354726928398,
12.));
#135426=CARTESIAN_POINT('Ctrl Pts',(-39.4304582059864,-63.1201343731172,
0.));
#135427=CARTESIAN_POINT('Ctrl Pts',(-39.4304582059864,-63.1201343731172,
12.));
#135428=CARTESIAN_POINT('Ctrl Pts',(-39.4072048797616,-63.10479424519,0.));
#135429=CARTESIAN_POINT('Ctrl Pts',(-39.4072048797616,-63.10479424519,12.));
#135430=CARTESIAN_POINT('Ctrl Pts',(-39.383994298574,-63.0894523341314,
0.));
#135431=CARTESIAN_POINT('Ctrl Pts',(-39.383994298574,-63.0894523341314,
12.));
#135432=CARTESIAN_POINT('Ctrl Pts',(-39.3608264920409,-63.0741086815841,
0.));
#135433=CARTESIAN_POINT('Ctrl Pts',(-39.3608264920409,-63.0741086815841,
12.));
#135434=CARTESIAN_POINT('Ctrl Pts',(-39.3377014983609,-63.0587633513774,
0.));
#135435=CARTESIAN_POINT('Ctrl Pts',(-39.3377014983609,-63.0587633513774,
12.));
#135436=CARTESIAN_POINT('Ctrl Pts',(-39.3146193632392,-63.0434164277992,
0.));
#135437=CARTESIAN_POINT('Ctrl Pts',(-39.3146193632392,-63.0434164277992,
12.));
#135438=CARTESIAN_POINT('Ctrl Pts',(-39.2915801372354,-63.0280680082352,
0.));
#135439=CARTESIAN_POINT('Ctrl Pts',(-39.2915801372354,-63.0280680082352,
12.));
#135440=CARTESIAN_POINT('Ctrl Pts',(-39.2685838735361,-63.0127181973628,
0.));
#135441=CARTESIAN_POINT('Ctrl Pts',(-39.2685838735361,-63.0127181973628,
12.));
#135442=CARTESIAN_POINT('Ctrl Pts',(-39.2456306256104,-62.9973671008703,
0.));
#135443=CARTESIAN_POINT('Ctrl Pts',(-39.2456306256104,-62.9973671008703,
12.));
#135444=CARTESIAN_POINT('Ctrl Pts',(-39.2227204447638,-62.9820148189929,
0.));
#135445=CARTESIAN_POINT('Ctrl Pts',(-39.2227204447638,-62.9820148189929,
12.));
#135446=CARTESIAN_POINT('Ctrl Pts',(-39.1998533781661,-62.9666614412731,
0.));
#135447=CARTESIAN_POINT('Ctrl Pts',(-39.1998533781661,-62.9666614412731,
12.));
#135448=CARTESIAN_POINT('Ctrl Pts',(-39.1770294702428,-62.9513070501867,
0.));
#135449=CARTESIAN_POINT('Ctrl Pts',(-39.1770294702428,-62.9513070501867,
12.));
#135450=CARTESIAN_POINT('Ctrl Pts',(-39.1542487636744,-62.9359517237404,
0.));
#135451=CARTESIAN_POINT('Ctrl Pts',(-39.1542487636744,-62.9359517237404,
12.));
#135452=CARTESIAN_POINT('Ctrl Pts',(-39.131511300575,-62.9205955385558,
0.));
#135453=CARTESIAN_POINT('Ctrl Pts',(-39.131511300575,-62.9205955385558,
12.));
#135454=CARTESIAN_POINT('Ctrl Pts',(-39.1088171235125,-62.9052385725387,
0.));
#135455=CARTESIAN_POINT('Ctrl Pts',(-39.1088171235125,-62.9052385725387,
12.));
#135456=CARTESIAN_POINT('Ctrl Pts',(-39.0861662767932,-62.8898809082611,
0.));
#135457=CARTESIAN_POINT('Ctrl Pts',(-39.0861662767932,-62.8898809082611,
12.));
#135458=CARTESIAN_POINT('Ctrl Pts',(-39.0635588063277,-62.8745226325998,
0.));
#135459=CARTESIAN_POINT('Ctrl Pts',(-39.0635588063277,-62.8745226325998,
12.));
#135460=CARTESIAN_POINT('Ctrl Pts',(-39.0409947590497,-62.8591638352055,
0.));
#135461=CARTESIAN_POINT('Ctrl Pts',(-39.0409947590497,-62.8591638352055,
12.));
#135462=CARTESIAN_POINT('Ctrl Pts',(-39.0184741824641,-62.8438046073224,
0.));
#135463=CARTESIAN_POINT('Ctrl Pts',(-39.0184741824641,-62.8438046073224,
12.));
#135464=CARTESIAN_POINT('Ctrl Pts',(-38.9959971241701,-62.8284450405459,
0.));
#135465=CARTESIAN_POINT('Ctrl Pts',(-38.9959971241701,-62.8284450405459,
12.));
#135466=CARTESIAN_POINT('Ctrl Pts',(-38.9735636313089,-62.8130852254027,
0.));
#135467=CARTESIAN_POINT('Ctrl Pts',(-38.9735636313089,-62.8130852254027,
12.));
#135468=CARTESIAN_POINT('Ctrl Pts',(-38.9511737503165,-62.7977252507117,
0.));
#135469=CARTESIAN_POINT('Ctrl Pts',(-38.9511737503165,-62.7977252507117,
12.));
#135470=CARTESIAN_POINT('Ctrl Pts',(-38.9288275272335,-62.78236520437,0.));
#135471=CARTESIAN_POINT('Ctrl Pts',(-38.9288275272335,-62.78236520437,12.));
#135472=CARTESIAN_POINT('Ctrl Pts',(-38.9065250078832,-62.7670051738143,
0.));
#135473=CARTESIAN_POINT('Ctrl Pts',(-38.9065250078832,-62.7670051738143,
12.));
#135474=CARTESIAN_POINT('Ctrl Pts',(-38.8842662380984,-62.7516452466128,
0.));
#135475=CARTESIAN_POINT('Ctrl Pts',(-38.8842662380984,-62.7516452466128,
12.));
#135476=CARTESIAN_POINT('Ctrl Pts',(-38.8620512639233,-62.7362855110042,
0.));
#135477=CARTESIAN_POINT('Ctrl Pts',(-38.8620512639233,-62.7362855110042,
12.));
#135478=CARTESIAN_POINT('Ctrl Pts',(-38.8398801318177,-62.7209260564493,
0.));
#135479=CARTESIAN_POINT('Ctrl Pts',(-38.8398801318177,-62.7209260564493,
12.));
#135480=CARTESIAN_POINT('Ctrl Pts',(-38.8177528885681,-62.7055669733802,
0.));
#135481=CARTESIAN_POINT('Ctrl Pts',(-38.8177528885681,-62.7055669733802,
12.));
#135482=CARTESIAN_POINT('Ctrl Pts',(-38.795669581203,-62.6902083529694,
0.));
#135483=CARTESIAN_POINT('Ctrl Pts',(-38.795669581203,-62.6902083529694,
12.));
#135484=CARTESIAN_POINT('Ctrl Pts',(-38.7736302568982,-62.6748502868835,
0.));
#135485=CARTESIAN_POINT('Ctrl Pts',(-38.7736302568982,-62.6748502868835,
12.));
#135486=CARTESIAN_POINT('Ctrl Pts',(-38.7516349628904,-62.6594928670628,
0.));
#135487=CARTESIAN_POINT('Ctrl Pts',(-38.7516349628904,-62.6594928670628,
12.));
#135488=CARTESIAN_POINT('Ctrl Pts',(-38.7296837463609,-62.6441361854411,
0.));
#135489=CARTESIAN_POINT('Ctrl Pts',(-38.7296837463609,-62.6441361854411,
12.));
#135490=CARTESIAN_POINT('Ctrl Pts',(-38.7077766544416,-62.6287803339542,
0.));
#135491=CARTESIAN_POINT('Ctrl Pts',(-38.7077766544416,-62.6287803339542,
12.));
#135492=CARTESIAN_POINT('Ctrl Pts',(-38.6859137342731,-62.6134254046739,
0.));
#135493=CARTESIAN_POINT('Ctrl Pts',(-38.6859137342731,-62.6134254046739,
12.));
#135494=CARTESIAN_POINT('Ctrl Pts',(-38.6640950330421,-62.5980714899052,
0.));
#135495=CARTESIAN_POINT('Ctrl Pts',(-38.6640950330421,-62.5980714899052,
12.));
#135496=CARTESIAN_POINT('Ctrl Pts',(-38.6423205980213,-62.582718682292,
0.));
#135497=CARTESIAN_POINT('Ctrl Pts',(-38.6423205980213,-62.582718682292,
12.));
#135498=CARTESIAN_POINT('Ctrl Pts',(-38.6205904766073,-62.5673670749361,
0.));
#135499=CARTESIAN_POINT('Ctrl Pts',(-38.6205904766073,-62.5673670749361,
12.));
#135500=CARTESIAN_POINT('Ctrl Pts',(-38.5989047163393,-62.5520167614516,
0.));
#135501=CARTESIAN_POINT('Ctrl Pts',(-38.5989047163393,-62.5520167614516,
12.));
#135502=CARTESIAN_POINT('Ctrl Pts',(-38.5772633648832,-62.5366678359023,
0.));
#135503=CARTESIAN_POINT('Ctrl Pts',(-38.5772633648832,-62.5366678359023,
12.));
#135504=CARTESIAN_POINT('Ctrl Pts',(-38.5556664700195,-62.5213203927663,
0.));
#135505=CARTESIAN_POINT('Ctrl Pts',(-38.5556664700195,-62.5213203927663,
12.));
#135506=CARTESIAN_POINT('Ctrl Pts',(-38.5341140796248,-62.5059745268901,
0.));
#135507=CARTESIAN_POINT('Ctrl Pts',(-38.5341140796248,-62.5059745268901,
12.));
#135508=CARTESIAN_POINT('Ctrl Pts',(-38.5126062416502,-62.4906303334443,
0.));
#135509=CARTESIAN_POINT('Ctrl Pts',(-38.5126062416502,-62.4906303334443,
12.));
#135510=CARTESIAN_POINT('Ctrl Pts',(-38.4911430040997,-62.4752879078854,
0.));
#135511=CARTESIAN_POINT('Ctrl Pts',(-38.4911430040997,-62.4752879078854,
12.));
#135512=CARTESIAN_POINT('Ctrl Pts',(-38.4697244150482,-62.4599473459811,
0.));
#135513=CARTESIAN_POINT('Ctrl Pts',(-38.4697244150482,-62.4599473459811,
12.));
#135514=CARTESIAN_POINT('Ctrl Pts',(-38.4483505226518,-62.4446087438312,
0.));
#135515=CARTESIAN_POINT('Ctrl Pts',(-38.4483505226518,-62.4446087438312,
12.));
#135516=CARTESIAN_POINT('Ctrl Pts',(-38.4270213751568,-62.4292721978901,
0.));
#135517=CARTESIAN_POINT('Ctrl Pts',(-38.4270213751568,-62.4292721978901,
12.));
#135518=CARTESIAN_POINT('Ctrl Pts',(-38.405737020905,-62.4139378049885,
0.));
#135519=CARTESIAN_POINT('Ctrl Pts',(-38.405737020905,-62.4139378049885,
12.));
#135520=CARTESIAN_POINT('Ctrl Pts',(-38.3844975083343,-62.3986056623577,
0.));
#135521=CARTESIAN_POINT('Ctrl Pts',(-38.3844975083343,-62.3986056623577,
12.));
#135522=CARTESIAN_POINT('Ctrl Pts',(-38.3633028859828,-62.3832758676271,
0.));
#135523=CARTESIAN_POINT('Ctrl Pts',(-38.3633028859828,-62.3832758676271,
12.));
#135524=CARTESIAN_POINT('Ctrl Pts',(-38.342153202491,-62.3679485188171,
0.));
#135525=CARTESIAN_POINT('Ctrl Pts',(-38.342153202491,-62.3679485188171,
12.));
#135526=CARTESIAN_POINT('Ctrl Pts',(-38.3210485066001,-62.3526237143336,
0.));
#135527=CARTESIAN_POINT('Ctrl Pts',(-38.3210485066001,-62.3526237143336,
12.));
#135528=CARTESIAN_POINT('Ctrl Pts',(-38.2999888471476,-62.3373015529613,
0.));
#135529=CARTESIAN_POINT('Ctrl Pts',(-38.2999888471476,-62.3373015529613,
12.));
#135530=CARTESIAN_POINT('Ctrl Pts',(-38.2789742730564,-62.3219821338569,
0.));
#135531=CARTESIAN_POINT('Ctrl Pts',(-38.2789742730564,-62.3219821338569,
12.));
#135532=CARTESIAN_POINT('Ctrl Pts',(-38.2580048333361,-62.3066655565503,
0.));
#135533=CARTESIAN_POINT('Ctrl Pts',(-38.2580048333361,-62.3066655565503,
12.));
#135534=CARTESIAN_POINT('Ctrl Pts',(-38.2370805770935,-62.2913519209521,
0.));
#135535=CARTESIAN_POINT('Ctrl Pts',(-38.2370805770935,-62.2913519209521,
12.));
#135536=CARTESIAN_POINT('Ctrl Pts',(-38.2162015535353,-62.2760413273602,
0.));
#135537=CARTESIAN_POINT('Ctrl Pts',(-38.2162015535353,-62.2760413273602,
12.));
#135538=CARTESIAN_POINT('Ctrl Pts',(-38.1953678119691,-62.2607338764654,
0.));
#135539=CARTESIAN_POINT('Ctrl Pts',(-38.1953678119691,-62.2607338764654,
12.));
#135540=CARTESIAN_POINT('Ctrl Pts',(-38.1745794017996,-62.245429669358,
0.));
#135541=CARTESIAN_POINT('Ctrl Pts',(-38.1745794017996,-62.245429669358,
12.));
#135542=CARTESIAN_POINT('Ctrl Pts',(-38.1538363725264,-62.2301288075321,
0.));
#135543=CARTESIAN_POINT('Ctrl Pts',(-38.1538363725264,-62.2301288075321,
12.));
#135544=CARTESIAN_POINT('Ctrl Pts',(-38.133138773753,-62.2148313928863,
0.));
#135545=CARTESIAN_POINT('Ctrl Pts',(-38.133138773753,-62.2148313928863,
12.));
#135546=CARTESIAN_POINT('Ctrl Pts',(-38.1124866551886,-62.1995375277257,
0.));
#135547=CARTESIAN_POINT('Ctrl Pts',(-38.1124866551886,-62.1995375277257,
12.));
#135548=CARTESIAN_POINT('Ctrl Pts',(-38.0918800666479,-62.1842473147626,
0.));
#135549=CARTESIAN_POINT('Ctrl Pts',(-38.0918800666479,-62.1842473147626,
12.));
#135550=CARTESIAN_POINT('Ctrl Pts',(-38.0713190580463,-62.1689608571176,
0.));
#135551=CARTESIAN_POINT('Ctrl Pts',(-38.0713190580463,-62.1689608571176,
12.));
#135552=CARTESIAN_POINT('Ctrl Pts',(-38.0508036793939,-62.1536782583199,
0.));
#135553=CARTESIAN_POINT('Ctrl Pts',(-38.0508036793939,-62.1536782583199,
12.));
#135554=CARTESIAN_POINT('Ctrl Pts',(-38.0303339808053,-62.1383996223124,
0.));
#135555=CARTESIAN_POINT('Ctrl Pts',(-38.0303339808053,-62.1383996223124,
12.));
#135556=CARTESIAN_POINT('Ctrl Pts',(-38.0099100125037,-62.123125053455,
0.));
#135557=CARTESIAN_POINT('Ctrl Pts',(-38.0099100125037,-62.123125053455,
12.));
#135558=CARTESIAN_POINT('Ctrl Pts',(-37.9895318248212,-62.107854656528,
0.));
#135559=CARTESIAN_POINT('Ctrl Pts',(-37.9895318248212,-62.107854656528,
12.));
#135560=CARTESIAN_POINT('Ctrl Pts',(-37.9691994681966,-62.0925885367352,
0.));
#135561=CARTESIAN_POINT('Ctrl Pts',(-37.9691994681966,-62.0925885367352,
12.));
#135562=CARTESIAN_POINT('Ctrl Pts',(-37.9489129931689,-62.0773267997078,
0.));
#135563=CARTESIAN_POINT('Ctrl Pts',(-37.9489129931689,-62.0773267997078,
12.));
#135564=CARTESIAN_POINT('Ctrl Pts',(-37.9286724503851,-62.0620695515074,
0.));
#135565=CARTESIAN_POINT('Ctrl Pts',(-37.9286724503851,-62.0620695515074,
12.));
#135566=CARTESIAN_POINT('Ctrl Pts',(-37.9084778906053,-62.0468168986288,
0.));
#135567=CARTESIAN_POINT('Ctrl Pts',(-37.9084778906053,-62.0468168986288,
12.));
#135568=CARTESIAN_POINT('Ctrl Pts',(-37.8883293647029,-62.031568948002,
0.));
#135569=CARTESIAN_POINT('Ctrl Pts',(-37.8883293647029,-62.031568948002,
12.));
#135570=CARTESIAN_POINT('Ctrl Pts',(-37.868226923663,-62.0163258069957,
0.));
#135571=CARTESIAN_POINT('Ctrl Pts',(-37.868226923663,-62.0163258069957,
12.));
#135572=CARTESIAN_POINT('Ctrl Pts',(-37.8481706185749,-62.0010875834187,
0.));
#135573=CARTESIAN_POINT('Ctrl Pts',(-37.8481706185749,-62.0010875834187,
12.));
#135574=CARTESIAN_POINT('Ctrl Pts',(-37.828160500638,-61.9858543855236,
0.));
#135575=CARTESIAN_POINT('Ctrl Pts',(-37.828160500638,-61.9858543855236,
12.));
#135576=CARTESIAN_POINT('Ctrl Pts',(-37.8081966211689,-61.9706263220114,
0.));
#135577=CARTESIAN_POINT('Ctrl Pts',(-37.8081966211689,-61.9706263220114,
12.));
#135578=CARTESIAN_POINT('Ctrl Pts',(-37.7882790316014,-61.9554035020338,
0.));
#135579=CARTESIAN_POINT('Ctrl Pts',(-37.7882790316014,-61.9554035020338,
12.));
#135580=CARTESIAN_POINT('Ctrl Pts',(-37.7684077834872,-61.9401860351972,
0.));
#135581=CARTESIAN_POINT('Ctrl Pts',(-37.7684077834872,-61.9401860351972,
12.));
#135582=CARTESIAN_POINT('Ctrl Pts',(-37.7485829284871,-61.9249740315649,
0.));
#135583=CARTESIAN_POINT('Ctrl Pts',(-37.7485829284871,-61.9249740315649,
12.));
#135584=CARTESIAN_POINT('Ctrl Pts',(-37.7288045183756,-61.9097676016601,
0.));
#135585=CARTESIAN_POINT('Ctrl Pts',(-37.7288045183756,-61.9097676016601,
12.));
#135586=CARTESIAN_POINT('Ctrl Pts',(-37.7090726050482,-61.8945668564704,
0.));
#135587=CARTESIAN_POINT('Ctrl Pts',(-37.7090726050482,-61.8945668564704,
12.));
#135588=CARTESIAN_POINT('Ctrl Pts',(-37.6893872405228,-61.8793719074507,
0.));
#135589=CARTESIAN_POINT('Ctrl Pts',(-37.6893872405228,-61.8793719074507,
12.));
#135590=CARTESIAN_POINT('Ctrl Pts',(-37.6697484769392,-61.8641828665261,
0.));
#135591=CARTESIAN_POINT('Ctrl Pts',(-37.6697484769392,-61.8641828665261,
12.));
#135592=CARTESIAN_POINT('Ctrl Pts',(-37.6501563665523,-61.8489998460957,
0.));
#135593=CARTESIAN_POINT('Ctrl Pts',(-37.6501563665523,-61.8489998460957,
12.));
#135594=CARTESIAN_POINT('Ctrl Pts',(-37.6306109617346,-61.8338229590352,
0.));
#135595=CARTESIAN_POINT('Ctrl Pts',(-37.6306109617346,-61.8338229590352,
12.));
#135596=CARTESIAN_POINT('Ctrl Pts',(-37.6111123149839,-61.8186523187015,
0.));
#135597=CARTESIAN_POINT('Ctrl Pts',(-37.6111123149839,-61.8186523187015,
12.));
#135598=CARTESIAN_POINT('Ctrl Pts',(-37.5916604789253,-61.8034880389362,
0.));
#135599=CARTESIAN_POINT('Ctrl Pts',(-37.5916604789253,-61.8034880389362,
12.));
#135600=CARTESIAN_POINT('Ctrl Pts',(-37.5722555063111,-61.7883302340687,
0.));
#135601=CARTESIAN_POINT('Ctrl Pts',(-37.5722555063111,-61.7883302340687,
12.));
#135602=CARTESIAN_POINT('Ctrl Pts',(-37.5528974500142,-61.773179018919,
0.));
#135603=CARTESIAN_POINT('Ctrl Pts',(-37.5528974500142,-61.773179018919,
12.));
#135604=CARTESIAN_POINT('Ctrl Pts',(-37.5335863630287,-61.7580345088016,
0.));
#135605=CARTESIAN_POINT('Ctrl Pts',(-37.5335863630287,-61.7580345088016,
12.));
#135606=CARTESIAN_POINT('Ctrl Pts',(-37.5143222984796,-61.7428968195299,
0.));
#135607=CARTESIAN_POINT('Ctrl Pts',(-37.5143222984796,-61.7428968195299,
12.));
#135608=CARTESIAN_POINT('Ctrl Pts',(-37.4951053096237,-61.7277660674205,
0.));
#135609=CARTESIAN_POINT('Ctrl Pts',(-37.4951053096237,-61.7277660674205,
12.));
#135610=CARTESIAN_POINT('Ctrl Pts',(-37.4759354498509,-61.7126423692963,
0.));
#135611=CARTESIAN_POINT('Ctrl Pts',(-37.4759354498509,-61.7126423692963,
12.));
#135612=CARTESIAN_POINT('Ctrl Pts',(-37.4568127726773,-61.6975258424894,
0.));
#135613=CARTESIAN_POINT('Ctrl Pts',(-37.4568127726773,-61.6975258424894,
12.));
#135614=CARTESIAN_POINT('Ctrl Pts',(-37.4377373317451,-61.6824166048444,
0.));
#135615=CARTESIAN_POINT('Ctrl Pts',(-37.4377373317451,-61.6824166048444,
12.));
#135616=CARTESIAN_POINT('Ctrl Pts',(-37.4187091808321,-61.6673147747242,
0.));
#135617=CARTESIAN_POINT('Ctrl Pts',(-37.4187091808321,-61.6673147747242,
12.));
#135618=CARTESIAN_POINT('Ctrl Pts',(-37.3997283738533,-61.6522204710131,
0.));
#135619=CARTESIAN_POINT('Ctrl Pts',(-37.3997283738533,-61.6522204710131,
12.));
#135620=CARTESIAN_POINT('Ctrl Pts',(-37.3807949648624,-61.637133813121,
0.));
#135621=CARTESIAN_POINT('Ctrl Pts',(-37.3807949648624,-61.637133813121,
12.));
#135622=CARTESIAN_POINT('Ctrl Pts',(-37.361909008045,-61.6220549209866,
0.));
#135623=CARTESIAN_POINT('Ctrl Pts',(-37.361909008045,-61.6220549209866,
12.));
#135624=CARTESIAN_POINT('Ctrl Pts',(-37.343070557718,-61.6069839150807,
0.));
#135625=CARTESIAN_POINT('Ctrl Pts',(-37.343070557718,-61.6069839150807,
12.));
#135626=CARTESIAN_POINT('Ctrl Pts',(-37.3242796683395,-61.591920916412,
0.));
#135627=CARTESIAN_POINT('Ctrl Pts',(-37.3242796683395,-61.591920916412,
12.));
#135628=CARTESIAN_POINT('Ctrl Pts',(-37.3055363945107,-61.5768660465311,
0.));
#135629=CARTESIAN_POINT('Ctrl Pts',(-37.3055363945107,-61.5768660465311,
12.));
#135630=CARTESIAN_POINT('Ctrl Pts',(-37.2868407909771,-61.5618194275348,
0.));
#135631=CARTESIAN_POINT('Ctrl Pts',(-37.2868407909771,-61.5618194275348,
12.));
#135632=CARTESIAN_POINT('Ctrl Pts',(-37.2681929126221,-61.5467811820691,
0.));
#135633=CARTESIAN_POINT('Ctrl Pts',(-37.2681929126221,-61.5467811820691,
12.));
#135634=CARTESIAN_POINT('Ctrl Pts',(-37.2495928144667,-61.5317514333328,
0.));
#135635=CARTESIAN_POINT('Ctrl Pts',(-37.2495928144667,-61.5317514333328,
12.));
#135636=CARTESIAN_POINT('Ctrl Pts',(-37.2310405516781,-61.5167303050832,
0.));
#135637=CARTESIAN_POINT('Ctrl Pts',(-37.2310405516781,-61.5167303050832,
12.));
#135638=CARTESIAN_POINT('Ctrl Pts',(-37.2125361795731,-61.501717921641,
0.));
#135639=CARTESIAN_POINT('Ctrl Pts',(-37.2125361795731,-61.501717921641,
12.));
#135640=CARTESIAN_POINT('Ctrl Pts',(-37.1940797536181,-61.4867144078936,
0.));
#135641=CARTESIAN_POINT('Ctrl Pts',(-37.1940797536181,-61.4867144078936,
12.));
#135642=CARTESIAN_POINT('Ctrl Pts',(-37.175671329424,-61.4717198892994,
0.));
#135643=CARTESIAN_POINT('Ctrl Pts',(-37.175671329424,-61.4717198892994,
12.));
#135644=CARTESIAN_POINT('Ctrl Pts',(-37.1573109627454,-61.4567344918919,
0.));
#135645=CARTESIAN_POINT('Ctrl Pts',(-37.1573109627454,-61.4567344918919,
12.));
#135646=CARTESIAN_POINT('Ctrl Pts',(-37.1389987094905,-61.4417583422863,
0.));
#135647=CARTESIAN_POINT('Ctrl Pts',(-37.1389987094905,-61.4417583422863,
12.));
#135648=CARTESIAN_POINT('Ctrl Pts',(-37.1207346257222,-61.4267915676822,
0.));
#135649=CARTESIAN_POINT('Ctrl Pts',(-37.1207346257222,-61.4267915676822,
12.));
#135650=CARTESIAN_POINT('Ctrl Pts',(-37.1025187676602,-61.4118342958697,
0.));
#135651=CARTESIAN_POINT('Ctrl Pts',(-37.1025187676602,-61.4118342958697,
12.));
#135652=CARTESIAN_POINT('Ctrl Pts',(-37.0843511916745,-61.3968866552317,
0.));
#135653=CARTESIAN_POINT('Ctrl Pts',(-37.0843511916745,-61.3968866552317,
12.));
#135654=CARTESIAN_POINT('Ctrl Pts',(-37.0662319542849,-61.381948774749,
0.));
#135655=CARTESIAN_POINT('Ctrl Pts',(-37.0662319542849,-61.381948774749,
12.));
#135656=CARTESIAN_POINT('Ctrl Pts',(-37.0481611121717,-61.3670207840068,
0.));
#135657=CARTESIAN_POINT('Ctrl Pts',(-37.0481611121717,-61.3670207840068,
12.));
#135658=CARTESIAN_POINT('Ctrl Pts',(-37.0301387221774,-61.3521028132003,
0.));
#135659=CARTESIAN_POINT('Ctrl Pts',(-37.0301387221774,-61.3521028132003,
12.));
#135660=CARTESIAN_POINT('Ctrl Pts',(-37.0121648413082,-61.3371949931387,
0.));
#135661=CARTESIAN_POINT('Ctrl Pts',(-37.0121648413082,-61.3371949931387,
12.));
#135662=CARTESIAN_POINT('Ctrl Pts',(-36.994239526727,-61.3222974552486,
0.));
#135663=CARTESIAN_POINT('Ctrl Pts',(-36.994239526727,-61.3222974552486,
12.));
#135664=CARTESIAN_POINT('Ctrl Pts',(-36.9763628357544,-61.3074103315791,
0.));
#135665=CARTESIAN_POINT('Ctrl Pts',(-36.9763628357544,-61.3074103315791,
12.));
#135666=CARTESIAN_POINT('Ctrl Pts',(-36.9585348258776,-61.2925337548077,
0.));
#135667=CARTESIAN_POINT('Ctrl Pts',(-36.9585348258776,-61.2925337548077,
12.));
#135668=CARTESIAN_POINT('Ctrl Pts',(-36.9407555547535,-61.2776678582461,
0.));
#135669=CARTESIAN_POINT('Ctrl Pts',(-36.9407555547535,-61.2776678582461,
12.));
#135670=CARTESIAN_POINT('Ctrl Pts',(-36.9230250802087,-61.2628127758457,
0.));
#135671=CARTESIAN_POINT('Ctrl Pts',(-36.9230250802087,-61.2628127758457,
12.));
#135672=CARTESIAN_POINT('Ctrl Pts',(-36.9053434602343,-61.247968642201,
0.));
#135673=CARTESIAN_POINT('Ctrl Pts',(-36.9053434602343,-61.247968642201,
12.));
#135674=CARTESIAN_POINT('Ctrl Pts',(-36.8877107529865,-61.2331355925547,
0.));
#135675=CARTESIAN_POINT('Ctrl Pts',(-36.8877107529865,-61.2331355925547,
12.));
#135676=CARTESIAN_POINT('Ctrl Pts',(-36.8701270167969,-61.2183137628056,
0.));
#135677=CARTESIAN_POINT('Ctrl Pts',(-36.8701270167969,-61.2183137628056,
12.));
#135678=CARTESIAN_POINT('Ctrl Pts',(-36.852592310174,-61.2035032895127,
0.));
#135679=CARTESIAN_POINT('Ctrl Pts',(-36.852592310174,-61.2035032895127,
12.));
#135680=CARTESIAN_POINT('Ctrl Pts',(-36.8351066918036,-61.1887043099014,
0.));
#135681=CARTESIAN_POINT('Ctrl Pts',(-36.8351066918036,-61.1887043099014,
12.));
#135682=CARTESIAN_POINT('Ctrl Pts',(-36.8176702205423,-61.1739169618666,
0.));
#135683=CARTESIAN_POINT('Ctrl Pts',(-36.8176702205423,-61.1739169618666,
12.));
#135684=CARTESIAN_POINT('Ctrl Pts',(-36.8002829554209,-61.1591413839787,
0.));
#135685=CARTESIAN_POINT('Ctrl Pts',(-36.8002829554209,-61.1591413839787,
12.));
#135686=CARTESIAN_POINT('Ctrl Pts',(-36.7829449556532,-61.1443777154911,
0.));
#135687=CARTESIAN_POINT('Ctrl Pts',(-36.7829449556532,-61.1443777154911,
12.));
#135688=CARTESIAN_POINT('Ctrl Pts',(-36.765656280638,-61.1296260963466,
0.));
#135689=CARTESIAN_POINT('Ctrl Pts',(-36.765656280638,-61.1296260963466,
12.));
#135690=CARTESIAN_POINT('Ctrl Pts',(-36.7484169899596,-61.1148866671829,
0.));
#135691=CARTESIAN_POINT('Ctrl Pts',(-36.7484169899596,-61.1148866671829,
12.));
#135692=CARTESIAN_POINT('Ctrl Pts',(-36.7312271433807,-61.100159569337,
0.));
#135693=CARTESIAN_POINT('Ctrl Pts',(-36.7312271433807,-61.100159569337,
12.));
#135694=CARTESIAN_POINT('Ctrl Pts',(-36.7140868008486,-61.0854449448524,
0.));
#135695=CARTESIAN_POINT('Ctrl Pts',(-36.7140868008486,-61.0854449448524,
12.));
#135696=CARTESIAN_POINT('Ctrl Pts',(-36.6969960225022,-61.0707429364847,
0.));
#135697=CARTESIAN_POINT('Ctrl Pts',(-36.6969960225022,-61.0707429364847,
12.));
#135698=CARTESIAN_POINT('Ctrl Pts',(-36.679954868674,-61.0560536877083,
0.));
#135699=CARTESIAN_POINT('Ctrl Pts',(-36.679954868674,-61.0560536877083,
12.));
#135700=CARTESIAN_POINT('Ctrl Pts',(-36.6629633998886,-61.0413773427203,
0.));
#135701=CARTESIAN_POINT('Ctrl Pts',(-36.6629633998886,-61.0413773427203,
12.));
#135702=CARTESIAN_POINT('Ctrl Pts',(-36.6460216768553,-61.0267140464432,
0.));
#135703=CARTESIAN_POINT('Ctrl Pts',(-36.6460216768553,-61.0267140464432,
12.));
#135704=CARTESIAN_POINT('Ctrl Pts',(-36.6291297604776,-61.0120639445349,
0.));
#135705=CARTESIAN_POINT('Ctrl Pts',(-36.6291297604776,-61.0120639445349,
12.));
#135706=CARTESIAN_POINT('Ctrl Pts',(-36.61228771186,-60.9974271833981,0.));
#135707=CARTESIAN_POINT('Ctrl Pts',(-36.61228771186,-60.9974271833981,12.));
#135708=CARTESIAN_POINT('Ctrl Pts',(-36.595495592311,-60.9828039101887,
0.));
#135709=CARTESIAN_POINT('Ctrl Pts',(-36.595495592311,-60.9828039101887,
12.));
#135710=CARTESIAN_POINT('Ctrl Pts',(-36.5787534633416,-60.9681942728236,
0.));
#135711=CARTESIAN_POINT('Ctrl Pts',(-36.5787534633416,-60.9681942728236,
12.));
#135712=CARTESIAN_POINT('Ctrl Pts',(-36.5620613866615,-60.9535984199873,
0.));
#135713=CARTESIAN_POINT('Ctrl Pts',(-36.5620613866615,-60.9535984199873,
12.));
#135714=CARTESIAN_POINT('Ctrl Pts',(-36.5454194241865,-60.9390165011355,
0.));
#135715=CARTESIAN_POINT('Ctrl Pts',(-36.5454194241865,-60.9390165011355,
12.));
#135716=CARTESIAN_POINT('Ctrl Pts',(-36.5288276380416,-60.9244486664987,
0.));
#135717=CARTESIAN_POINT('Ctrl Pts',(-36.5288276380416,-60.9244486664987,
12.));
#135718=CARTESIAN_POINT('Ctrl Pts',(-36.5122860905612,-60.9098950670847,
0.));
#135719=CARTESIAN_POINT('Ctrl Pts',(-36.5122860905612,-60.9098950670847,
12.));
#135720=CARTESIAN_POINT('Ctrl Pts',(-36.4957948442835,-60.8953558546795,
0.));
#135721=CARTESIAN_POINT('Ctrl Pts',(-36.4957948442835,-60.8953558546795,
12.));
#135722=CARTESIAN_POINT('Ctrl Pts',(-36.4793539619466,-60.8808311818499,
0.));
#135723=CARTESIAN_POINT('Ctrl Pts',(-36.4793539619466,-60.8808311818499,
12.));
#135724=CARTESIAN_POINT('Ctrl Pts',(-36.4629635065045,-60.8663212019657,
0.));
#135725=CARTESIAN_POINT('Ctrl Pts',(-36.4629635065045,-60.8663212019657,
12.));
#135726=CARTESIAN_POINT('Ctrl Pts',(-36.4466235411358,-60.8518260692188,
0.));
#135727=CARTESIAN_POINT('Ctrl Pts',(-36.4466235411358,-60.8518260692188,
12.));
#135728=CARTESIAN_POINT('Ctrl Pts',(-36.4303341292494,-60.8373459386392,
0.));
#135729=CARTESIAN_POINT('Ctrl Pts',(-36.4303341292494,-60.8373459386392,
12.));
#135730=CARTESIAN_POINT('Ctrl Pts',(-36.4140953344858,-60.822880966116,
0.));
#135731=CARTESIAN_POINT('Ctrl Pts',(-36.4140953344858,-60.822880966116,
12.));
#135732=CARTESIAN_POINT('Ctrl Pts',(-36.397907220716,-60.8084313083984,
0.));
#135733=CARTESIAN_POINT('Ctrl Pts',(-36.397907220716,-60.8084313083984,
12.));
#135734=CARTESIAN_POINT('Ctrl Pts',(-36.3817698520388,-60.793997123076,
0.));
#135735=CARTESIAN_POINT('Ctrl Pts',(-36.3817698520388,-60.793997123076,
12.));
#135736=CARTESIAN_POINT('Ctrl Pts',(-36.365683292773,-60.7795785685625,
0.));
#135737=CARTESIAN_POINT('Ctrl Pts',(-36.365683292773,-60.7795785685625,
12.));
#135738=CARTESIAN_POINT('Ctrl Pts',(-36.3496476074488,-60.7651758040803,
0.));
#135739=CARTESIAN_POINT('Ctrl Pts',(-36.3496476074488,-60.7651758040803,
12.));
#135740=CARTESIAN_POINT('Ctrl Pts',(-36.3336628607859,-60.7507889896308,
0.));
#135741=CARTESIAN_POINT('Ctrl Pts',(-36.3336628607859,-60.7507889896308,
12.));
#135742=CARTESIAN_POINT('Ctrl Pts',(-36.3177291177163,-60.7364182860412,
0.));
#135743=CARTESIAN_POINT('Ctrl Pts',(-36.3177291177163,-60.7364182860412,
12.));
#135744=CARTESIAN_POINT('Ctrl Pts',(-36.3018464434214,-60.722063855041,
0.));
#135745=CARTESIAN_POINT('Ctrl Pts',(-36.3018464434214,-60.722063855041,
12.));
#135746=CARTESIAN_POINT('Ctrl Pts',(-36.2860149033587,-60.7077258593268,
0.));
#135747=CARTESIAN_POINT('Ctrl Pts',(-36.2860149033587,-60.7077258593268,
12.));
#135748=CARTESIAN_POINT('Ctrl Pts',(-36.2702345632875,-60.6934044626291,
0.));
#135749=CARTESIAN_POINT('Ctrl Pts',(-36.2702345632875,-60.6934044626291,
12.));
#135750=CARTESIAN_POINT('Ctrl Pts',(-36.2545054892897,-60.67909982978,0.));
#135751=CARTESIAN_POINT('Ctrl Pts',(-36.2545054892897,-60.67909982978,12.));
#135752=CARTESIAN_POINT('Ctrl Pts',(-36.2388277477212,-60.6648121265885,
0.));
#135753=CARTESIAN_POINT('Ctrl Pts',(-36.2388277477212,-60.6648121265885,
12.));
#135754=CARTESIAN_POINT('Ctrl Pts',(-36.2232014051541,-60.6505415197042,
0.));
#135755=CARTESIAN_POINT('Ctrl Pts',(-36.2232014051541,-60.6505415197042,
12.));
#135756=CARTESIAN_POINT('Ctrl Pts',(-36.2076265283264,-60.6362881765019,
0.));
#135757=CARTESIAN_POINT('Ctrl Pts',(-36.2076265283264,-60.6362881765019,
12.));
#135758=CARTESIAN_POINT('Ctrl Pts',(-36.192103184063,-60.6220522649149,
0.));
#135759=CARTESIAN_POINT('Ctrl Pts',(-36.192103184063,-60.6220522649149,
12.));
#135760=CARTESIAN_POINT('Ctrl Pts',(-36.1766314392641,-60.6078339534181,
0.));
#135761=CARTESIAN_POINT('Ctrl Pts',(-36.1766314392641,-60.6078339534181,
12.));
#135762=CARTESIAN_POINT('Ctrl Pts',(-36.1612113610773,-60.5936334114108,
0.));
#135763=CARTESIAN_POINT('Ctrl Pts',(-36.1612113610773,-60.5936334114108,
12.));
#135764=CARTESIAN_POINT('Ctrl Pts',(-36.1458430170431,-60.5794508095564,
0.));
#135765=CARTESIAN_POINT('Ctrl Pts',(-36.1458430170431,-60.5794508095564,
12.));
#135766=CARTESIAN_POINT('Ctrl Pts',(-36.1305264752188,-60.565286320072,
0.));
#135767=CARTESIAN_POINT('Ctrl Pts',(-36.1305264752188,-60.565286320072,
12.));
#135768=CARTESIAN_POINT('Ctrl Pts',(-36.1152618043739,-60.5511401171984,
0.));
#135769=CARTESIAN_POINT('Ctrl Pts',(-36.1152618043739,-60.5511401171984,
12.));
#135770=CARTESIAN_POINT('Ctrl Pts',(-36.100049073851,-60.5370123768804,
0.));
#135771=CARTESIAN_POINT('Ctrl Pts',(-36.100049073851,-60.5370123768804,
12.));
#135772=CARTESIAN_POINT('Ctrl Pts',(-36.0848883531952,-60.5229032758973,
0.));
#135773=CARTESIAN_POINT('Ctrl Pts',(-36.0848883531952,-60.5229032758973,
12.));
#135774=CARTESIAN_POINT('Ctrl Pts',(-36.0697797118376,-60.5088129911354,
0.));
#135775=CARTESIAN_POINT('Ctrl Pts',(-36.0697797118376,-60.5088129911354,
12.));
#135776=CARTESIAN_POINT('Ctrl Pts',(-36.0547232187698,-60.4947416988422,
0.));
#135777=CARTESIAN_POINT('Ctrl Pts',(-36.0547232187698,-60.4947416988422,
12.));
#135778=CARTESIAN_POINT('Ctrl Pts',(-36.0397189421644,-60.4806895737686,
0.));
#135779=CARTESIAN_POINT('Ctrl Pts',(-36.0397189421644,-60.4806895737686,
12.));
#135780=CARTESIAN_POINT('Ctrl Pts',(-36.0247669500891,-60.4666567908093,
0.));
#135781=CARTESIAN_POINT('Ctrl Pts',(-36.0247669500891,-60.4666567908093,
12.));
#135782=CARTESIAN_POINT('Ctrl Pts',(-36.009867311357,-60.4526435269662,
0.));
#135783=CARTESIAN_POINT('Ctrl Pts',(-36.009867311357,-60.4526435269662,
12.));
#135784=CARTESIAN_POINT('Ctrl Pts',(-35.995020096217,-60.4386499629481,
0.));
#135785=CARTESIAN_POINT('Ctrl Pts',(-35.995020096217,-60.4386499629481,
12.));
#135786=CARTESIAN_POINT('Ctrl Pts',(-35.9802253773515,-60.4246762854926,
0.));
#135787=CARTESIAN_POINT('Ctrl Pts',(-35.9802253773515,-60.4246762854926,
12.));
#135788=CARTESIAN_POINT('Ctrl Pts',(-35.9654832299601,-60.4107226875714,
0.));
#135789=CARTESIAN_POINT('Ctrl Pts',(-35.9654832299601,-60.4107226875714,
12.));
#135790=CARTESIAN_POINT('Ctrl Pts',(-35.9507937296707,-60.3967893635452,
0.));
#135791=CARTESIAN_POINT('Ctrl Pts',(-35.9507937296707,-60.3967893635452,
12.));
#135792=CARTESIAN_POINT('Ctrl Pts',(-35.936156950695,-60.3828765049019,
0.));
#135793=CARTESIAN_POINT('Ctrl Pts',(-35.936156950695,-60.3828765049019,
12.));
#135794=CARTESIAN_POINT('Ctrl Pts',(-35.9215729642231,-60.3689842965481,
0.));
#135795=CARTESIAN_POINT('Ctrl Pts',(-35.9215729642231,-60.3689842965481,
12.));
#135796=CARTESIAN_POINT('Ctrl Pts',(-35.907041835853,-60.3551129108845,
0.));
#135797=CARTESIAN_POINT('Ctrl Pts',(-35.907041835853,-60.3551129108845,
12.));
#135798=CARTESIAN_POINT('Ctrl Pts',(-35.8925636280668,-60.3412625135287,
0.));
#135799=CARTESIAN_POINT('Ctrl Pts',(-35.8925636280668,-60.3412625135287,
12.));
#135800=CARTESIAN_POINT('Ctrl Pts',(-35.8781384051537,-60.327433274683,
0.));
#135801=CARTESIAN_POINT('Ctrl Pts',(-35.8781384051537,-60.327433274683,
12.));
#135802=CARTESIAN_POINT('Ctrl Pts',(-35.8637662371635,-60.3136253782809,
0.));
#135803=CARTESIAN_POINT('Ctrl Pts',(-35.8637662371635,-60.3136253782809,
12.));
#135804=CARTESIAN_POINT('Ctrl Pts',(-35.8494472046745,-60.2998390330102,
0.));
#135805=CARTESIAN_POINT('Ctrl Pts',(-35.8494472046745,-60.2998390330102,
12.));
#135806=CARTESIAN_POINT('Ctrl Pts',(-35.8351814020357,-60.2860744798436,
0.));
#135807=CARTESIAN_POINT('Ctrl Pts',(-35.8351814020357,-60.2860744798436,
12.));
#135808=CARTESIAN_POINT('Ctrl Pts',(-35.8209689272501,-60.2723319687369,
0.));
#135809=CARTESIAN_POINT('Ctrl Pts',(-35.8209689272501,-60.2723319687369,
12.));
#135810=CARTESIAN_POINT('Ctrl Pts',(-35.8068098723347,-60.2586117365205,
0.));
#135811=CARTESIAN_POINT('Ctrl Pts',(-35.8068098723347,-60.2586117365205,
12.));
#135812=CARTESIAN_POINT('Ctrl Pts',(-35.7927043145201,-60.2449139865274,
0.));
#135813=CARTESIAN_POINT('Ctrl Pts',(-35.7927043145201,-60.2449139865274,
12.));
#135814=CARTESIAN_POINT('Ctrl Pts',(-35.7786523045912,-60.2312388621529,
0.));
#135815=CARTESIAN_POINT('Ctrl Pts',(-35.7786523045912,-60.2312388621529,
12.));
#135816=CARTESIAN_POINT('Ctrl Pts',(-35.7646538667493,-60.2175864450043,
0.));
#135817=CARTESIAN_POINT('Ctrl Pts',(-35.7646538667493,-60.2175864450043,
12.));
#135818=CARTESIAN_POINT('Ctrl Pts',(-35.7534979802053,-60.206682708692,
0.));
#135819=CARTESIAN_POINT('Ctrl Pts',(-35.7534979802053,-60.206682708692,
12.));
#135820=CARTESIAN_POINT('Ctrl Pts',(-35.7451551752572,-60.1985151474623,
0.));
#135821=CARTESIAN_POINT('Ctrl Pts',(-35.7451551752572,-60.1985151474623,
12.));
#135822=CARTESIAN_POINT('Ctrl Pts',(-35.7396040204017,-60.193074658032,
0.));
#135823=CARTESIAN_POINT('Ctrl Pts',(-35.7396040204017,-60.193074658032,
12.));
#135824=CARTESIAN_POINT('Ctrl Pts',(-35.736831121751,-60.1903555511633,
0.));
#135825=CARTESIAN_POINT('Ctrl Pts',(-35.736831121751,-60.1903555511633,
12.));
#135826=CARTESIAN_POINT('',(-35.736831121751,-60.1903555511633,12.));
#135827=CARTESIAN_POINT('Ctrl Pts',(-35.736831121751,-60.1903555511633,
12.));
#135828=CARTESIAN_POINT('Ctrl Pts',(-35.7396040204017,-60.193074658032,
12.));
#135829=CARTESIAN_POINT('Ctrl Pts',(-35.7451551752572,-60.1985151474623,
12.));
#135830=CARTESIAN_POINT('Ctrl Pts',(-35.7534979802053,-60.206682708692,
12.));
#135831=CARTESIAN_POINT('Ctrl Pts',(-35.7646538667493,-60.2175864450043,
12.));
#135832=CARTESIAN_POINT('Ctrl Pts',(-35.7786523045912,-60.2312388621529,
12.));
#135833=CARTESIAN_POINT('Ctrl Pts',(-35.7927043145201,-60.2449139865274,
12.));
#135834=CARTESIAN_POINT('Ctrl Pts',(-35.8068098723347,-60.2586117365205,
12.));
#135835=CARTESIAN_POINT('Ctrl Pts',(-35.8209689272501,-60.2723319687369,
12.));
#135836=CARTESIAN_POINT('Ctrl Pts',(-35.8351814020357,-60.2860744798436,
12.));
#135837=CARTESIAN_POINT('Ctrl Pts',(-35.8494472046745,-60.2998390330102,
12.));
#135838=CARTESIAN_POINT('Ctrl Pts',(-35.8637662371635,-60.3136253782809,
12.));
#135839=CARTESIAN_POINT('Ctrl Pts',(-35.8781384051537,-60.327433274683,
12.));
#135840=CARTESIAN_POINT('Ctrl Pts',(-35.8925636280668,-60.3412625135287,
12.));
#135841=CARTESIAN_POINT('Ctrl Pts',(-35.907041835853,-60.3551129108845,
12.));
#135842=CARTESIAN_POINT('Ctrl Pts',(-35.9215729642231,-60.3689842965481,
12.));
#135843=CARTESIAN_POINT('Ctrl Pts',(-35.936156950695,-60.3828765049019,
12.));
#135844=CARTESIAN_POINT('Ctrl Pts',(-35.9507937296707,-60.3967893635452,
12.));
#135845=CARTESIAN_POINT('Ctrl Pts',(-35.9654832299601,-60.4107226875714,
12.));
#135846=CARTESIAN_POINT('Ctrl Pts',(-35.9802253773515,-60.4246762854926,
12.));
#135847=CARTESIAN_POINT('Ctrl Pts',(-35.995020096217,-60.4386499629481,
12.));
#135848=CARTESIAN_POINT('Ctrl Pts',(-36.009867311357,-60.4526435269662,
12.));
#135849=CARTESIAN_POINT('Ctrl Pts',(-36.0247669500891,-60.4666567908093,
12.));
#135850=CARTESIAN_POINT('Ctrl Pts',(-36.0397189421644,-60.4806895737686,
12.));
#135851=CARTESIAN_POINT('Ctrl Pts',(-36.0547232187698,-60.4947416988422,
12.));
#135852=CARTESIAN_POINT('Ctrl Pts',(-36.0697797118376,-60.5088129911354,
12.));
#135853=CARTESIAN_POINT('Ctrl Pts',(-36.0848883531952,-60.5229032758973,
12.));
#135854=CARTESIAN_POINT('Ctrl Pts',(-36.100049073851,-60.5370123768804,
12.));
#135855=CARTESIAN_POINT('Ctrl Pts',(-36.1152618043739,-60.5511401171984,
12.));
#135856=CARTESIAN_POINT('Ctrl Pts',(-36.1305264752188,-60.565286320072,
12.));
#135857=CARTESIAN_POINT('Ctrl Pts',(-36.1458430170431,-60.5794508095564,
12.));
#135858=CARTESIAN_POINT('Ctrl Pts',(-36.1612113610773,-60.5936334114108,
12.));
#135859=CARTESIAN_POINT('Ctrl Pts',(-36.1766314392641,-60.6078339534181,
12.));
#135860=CARTESIAN_POINT('Ctrl Pts',(-36.192103184063,-60.6220522649149,
12.));
#135861=CARTESIAN_POINT('Ctrl Pts',(-36.2076265283264,-60.6362881765019,
12.));
#135862=CARTESIAN_POINT('Ctrl Pts',(-36.2232014051541,-60.6505415197042,
12.));
#135863=CARTESIAN_POINT('Ctrl Pts',(-36.2388277477212,-60.6648121265885,
12.));
#135864=CARTESIAN_POINT('Ctrl Pts',(-36.2545054892897,-60.67909982978,12.));
#135865=CARTESIAN_POINT('Ctrl Pts',(-36.2702345632875,-60.6934044626291,
12.));
#135866=CARTESIAN_POINT('Ctrl Pts',(-36.2860149033587,-60.7077258593268,
12.));
#135867=CARTESIAN_POINT('Ctrl Pts',(-36.3018464434214,-60.722063855041,
12.));
#135868=CARTESIAN_POINT('Ctrl Pts',(-36.3177291177163,-60.7364182860412,
12.));
#135869=CARTESIAN_POINT('Ctrl Pts',(-36.3336628607859,-60.7507889896308,
12.));
#135870=CARTESIAN_POINT('Ctrl Pts',(-36.3496476074488,-60.7651758040803,
12.));
#135871=CARTESIAN_POINT('Ctrl Pts',(-36.365683292773,-60.7795785685625,
12.));
#135872=CARTESIAN_POINT('Ctrl Pts',(-36.3817698520388,-60.793997123076,
12.));
#135873=CARTESIAN_POINT('Ctrl Pts',(-36.397907220716,-60.8084313083984,
12.));
#135874=CARTESIAN_POINT('Ctrl Pts',(-36.4140953344858,-60.822880966116,
12.));
#135875=CARTESIAN_POINT('Ctrl Pts',(-36.4303341292494,-60.8373459386392,
12.));
#135876=CARTESIAN_POINT('Ctrl Pts',(-36.4466235411358,-60.8518260692188,
12.));
#135877=CARTESIAN_POINT('Ctrl Pts',(-36.4629635065045,-60.8663212019657,
12.));
#135878=CARTESIAN_POINT('Ctrl Pts',(-36.4793539619466,-60.8808311818499,
12.));
#135879=CARTESIAN_POINT('Ctrl Pts',(-36.4957948442835,-60.8953558546795,
12.));
#135880=CARTESIAN_POINT('Ctrl Pts',(-36.5122860905612,-60.9098950670847,
12.));
#135881=CARTESIAN_POINT('Ctrl Pts',(-36.5288276380416,-60.9244486664987,
12.));
#135882=CARTESIAN_POINT('Ctrl Pts',(-36.5454194241865,-60.9390165011355,
12.));
#135883=CARTESIAN_POINT('Ctrl Pts',(-36.5620613866615,-60.9535984199873,
12.));
#135884=CARTESIAN_POINT('Ctrl Pts',(-36.5787534633416,-60.9681942728236,
12.));
#135885=CARTESIAN_POINT('Ctrl Pts',(-36.595495592311,-60.9828039101887,
12.));
#135886=CARTESIAN_POINT('Ctrl Pts',(-36.61228771186,-60.9974271833981,12.));
#135887=CARTESIAN_POINT('Ctrl Pts',(-36.6291297604776,-61.0120639445349,
12.));
#135888=CARTESIAN_POINT('Ctrl Pts',(-36.6460216768553,-61.0267140464432,
12.));
#135889=CARTESIAN_POINT('Ctrl Pts',(-36.6629633998886,-61.0413773427203,
12.));
#135890=CARTESIAN_POINT('Ctrl Pts',(-36.679954868674,-61.0560536877083,
12.));
#135891=CARTESIAN_POINT('Ctrl Pts',(-36.6969960225022,-61.0707429364847,
12.));
#135892=CARTESIAN_POINT('Ctrl Pts',(-36.7140868008486,-61.0854449448524,
12.));
#135893=CARTESIAN_POINT('Ctrl Pts',(-36.7312271433807,-61.100159569337,
12.));
#135894=CARTESIAN_POINT('Ctrl Pts',(-36.7484169899596,-61.1148866671829,
12.));
#135895=CARTESIAN_POINT('Ctrl Pts',(-36.765656280638,-61.1296260963466,
12.));
#135896=CARTESIAN_POINT('Ctrl Pts',(-36.7829449556532,-61.1443777154911,
12.));
#135897=CARTESIAN_POINT('Ctrl Pts',(-36.8002829554209,-61.1591413839787,
12.));
#135898=CARTESIAN_POINT('Ctrl Pts',(-36.8176702205423,-61.1739169618666,
12.));
#135899=CARTESIAN_POINT('Ctrl Pts',(-36.8351066918036,-61.1887043099014,
12.));
#135900=CARTESIAN_POINT('Ctrl Pts',(-36.852592310174,-61.2035032895127,
12.));
#135901=CARTESIAN_POINT('Ctrl Pts',(-36.8701270167969,-61.2183137628056,
12.));
#135902=CARTESIAN_POINT('Ctrl Pts',(-36.8877107529865,-61.2331355925547,
12.));
#135903=CARTESIAN_POINT('Ctrl Pts',(-36.9053434602343,-61.247968642201,
12.));
#135904=CARTESIAN_POINT('Ctrl Pts',(-36.9230250802087,-61.2628127758457,
12.));
#135905=CARTESIAN_POINT('Ctrl Pts',(-36.9407555547535,-61.2776678582461,
12.));
#135906=CARTESIAN_POINT('Ctrl Pts',(-36.9585348258776,-61.2925337548077,
12.));
#135907=CARTESIAN_POINT('Ctrl Pts',(-36.9763628357544,-61.3074103315791,
12.));
#135908=CARTESIAN_POINT('Ctrl Pts',(-36.994239526727,-61.3222974552486,
12.));
#135909=CARTESIAN_POINT('Ctrl Pts',(-37.0121648413082,-61.3371949931387,
12.));
#135910=CARTESIAN_POINT('Ctrl Pts',(-37.0301387221774,-61.3521028132003,
12.));
#135911=CARTESIAN_POINT('Ctrl Pts',(-37.0481611121717,-61.3670207840068,
12.));
#135912=CARTESIAN_POINT('Ctrl Pts',(-37.0662319542849,-61.381948774749,
12.));
#135913=CARTESIAN_POINT('Ctrl Pts',(-37.0843511916745,-61.3968866552317,
12.));
#135914=CARTESIAN_POINT('Ctrl Pts',(-37.1025187676602,-61.4118342958697,
12.));
#135915=CARTESIAN_POINT('Ctrl Pts',(-37.1207346257222,-61.4267915676822,
12.));
#135916=CARTESIAN_POINT('Ctrl Pts',(-37.1389987094905,-61.4417583422863,
12.));
#135917=CARTESIAN_POINT('Ctrl Pts',(-37.1573109627454,-61.4567344918919,
12.));
#135918=CARTESIAN_POINT('Ctrl Pts',(-37.175671329424,-61.4717198892994,
12.));
#135919=CARTESIAN_POINT('Ctrl Pts',(-37.1940797536181,-61.4867144078936,
12.));
#135920=CARTESIAN_POINT('Ctrl Pts',(-37.2125361795731,-61.501717921641,
12.));
#135921=CARTESIAN_POINT('Ctrl Pts',(-37.2310405516781,-61.5167303050832,
12.));
#135922=CARTESIAN_POINT('Ctrl Pts',(-37.2495928144667,-61.5317514333328,
12.));
#135923=CARTESIAN_POINT('Ctrl Pts',(-37.2681929126221,-61.5467811820691,
12.));
#135924=CARTESIAN_POINT('Ctrl Pts',(-37.2868407909771,-61.5618194275348,
12.));
#135925=CARTESIAN_POINT('Ctrl Pts',(-37.3055363945107,-61.5768660465311,
12.));
#135926=CARTESIAN_POINT('Ctrl Pts',(-37.3242796683395,-61.591920916412,
12.));
#135927=CARTESIAN_POINT('Ctrl Pts',(-37.343070557718,-61.6069839150807,
12.));
#135928=CARTESIAN_POINT('Ctrl Pts',(-37.361909008045,-61.6220549209866,
12.));
#135929=CARTESIAN_POINT('Ctrl Pts',(-37.3807949648624,-61.637133813121,
12.));
#135930=CARTESIAN_POINT('Ctrl Pts',(-37.3997283738533,-61.6522204710131,
12.));
#135931=CARTESIAN_POINT('Ctrl Pts',(-37.4187091808321,-61.6673147747242,
12.));
#135932=CARTESIAN_POINT('Ctrl Pts',(-37.4377373317451,-61.6824166048444,
12.));
#135933=CARTESIAN_POINT('Ctrl Pts',(-37.4568127726773,-61.6975258424894,
12.));
#135934=CARTESIAN_POINT('Ctrl Pts',(-37.4759354498509,-61.7126423692963,
12.));
#135935=CARTESIAN_POINT('Ctrl Pts',(-37.4951053096237,-61.7277660674205,
12.));
#135936=CARTESIAN_POINT('Ctrl Pts',(-37.5143222984796,-61.7428968195299,
12.));
#135937=CARTESIAN_POINT('Ctrl Pts',(-37.5335863630287,-61.7580345088016,
12.));
#135938=CARTESIAN_POINT('Ctrl Pts',(-37.5528974500142,-61.773179018919,
12.));
#135939=CARTESIAN_POINT('Ctrl Pts',(-37.5722555063111,-61.7883302340687,
12.));
#135940=CARTESIAN_POINT('Ctrl Pts',(-37.5916604789253,-61.8034880389362,
12.));
#135941=CARTESIAN_POINT('Ctrl Pts',(-37.6111123149839,-61.8186523187015,
12.));
#135942=CARTESIAN_POINT('Ctrl Pts',(-37.6306109617346,-61.8338229590352,
12.));
#135943=CARTESIAN_POINT('Ctrl Pts',(-37.6501563665523,-61.8489998460957,
12.));
#135944=CARTESIAN_POINT('Ctrl Pts',(-37.6697484769392,-61.8641828665261,
12.));
#135945=CARTESIAN_POINT('Ctrl Pts',(-37.6893872405228,-61.8793719074507,
12.));
#135946=CARTESIAN_POINT('Ctrl Pts',(-37.7090726050482,-61.8945668564704,
12.));
#135947=CARTESIAN_POINT('Ctrl Pts',(-37.7288045183756,-61.9097676016601,
12.));
#135948=CARTESIAN_POINT('Ctrl Pts',(-37.7485829284871,-61.9249740315649,
12.));
#135949=CARTESIAN_POINT('Ctrl Pts',(-37.7684077834872,-61.9401860351972,
12.));
#135950=CARTESIAN_POINT('Ctrl Pts',(-37.7882790316014,-61.9554035020338,
12.));
#135951=CARTESIAN_POINT('Ctrl Pts',(-37.8081966211689,-61.9706263220114,
12.));
#135952=CARTESIAN_POINT('Ctrl Pts',(-37.828160500638,-61.9858543855236,
12.));
#135953=CARTESIAN_POINT('Ctrl Pts',(-37.8481706185749,-62.0010875834187,
12.));
#135954=CARTESIAN_POINT('Ctrl Pts',(-37.868226923663,-62.0163258069957,
12.));
#135955=CARTESIAN_POINT('Ctrl Pts',(-37.8883293647029,-62.031568948002,
12.));
#135956=CARTESIAN_POINT('Ctrl Pts',(-37.9084778906053,-62.0468168986288,
12.));
#135957=CARTESIAN_POINT('Ctrl Pts',(-37.9286724503851,-62.0620695515074,
12.));
#135958=CARTESIAN_POINT('Ctrl Pts',(-37.9489129931689,-62.0773267997078,
12.));
#135959=CARTESIAN_POINT('Ctrl Pts',(-37.9691994681966,-62.0925885367352,
12.));
#135960=CARTESIAN_POINT('Ctrl Pts',(-37.9895318248212,-62.107854656528,
12.));
#135961=CARTESIAN_POINT('Ctrl Pts',(-38.0099100125037,-62.123125053455,
12.));
#135962=CARTESIAN_POINT('Ctrl Pts',(-38.0303339808053,-62.1383996223124,
12.));
#135963=CARTESIAN_POINT('Ctrl Pts',(-38.0508036793939,-62.1536782583199,
12.));
#135964=CARTESIAN_POINT('Ctrl Pts',(-38.0713190580463,-62.1689608571176,
12.));
#135965=CARTESIAN_POINT('Ctrl Pts',(-38.0918800666479,-62.1842473147626,
12.));
#135966=CARTESIAN_POINT('Ctrl Pts',(-38.1124866551886,-62.1995375277257,
12.));
#135967=CARTESIAN_POINT('Ctrl Pts',(-38.133138773753,-62.2148313928863,
12.));
#135968=CARTESIAN_POINT('Ctrl Pts',(-38.1538363725264,-62.2301288075321,
12.));
#135969=CARTESIAN_POINT('Ctrl Pts',(-38.1745794017996,-62.245429669358,
12.));
#135970=CARTESIAN_POINT('Ctrl Pts',(-38.1953678119691,-62.2607338764654,
12.));
#135971=CARTESIAN_POINT('Ctrl Pts',(-38.2162015535353,-62.2760413273602,
12.));
#135972=CARTESIAN_POINT('Ctrl Pts',(-38.2370805770935,-62.2913519209521,
12.));
#135973=CARTESIAN_POINT('Ctrl Pts',(-38.2580048333361,-62.3066655565503,
12.));
#135974=CARTESIAN_POINT('Ctrl Pts',(-38.2789742730564,-62.3219821338569,
12.));
#135975=CARTESIAN_POINT('Ctrl Pts',(-38.2999888471476,-62.3373015529613,
12.));
#135976=CARTESIAN_POINT('Ctrl Pts',(-38.3210485066001,-62.3526237143336,
12.));
#135977=CARTESIAN_POINT('Ctrl Pts',(-38.342153202491,-62.3679485188171,
12.));
#135978=CARTESIAN_POINT('Ctrl Pts',(-38.3633028859828,-62.3832758676271,
12.));
#135979=CARTESIAN_POINT('Ctrl Pts',(-38.3844975083343,-62.3986056623577,
12.));
#135980=CARTESIAN_POINT('Ctrl Pts',(-38.405737020905,-62.4139378049885,
12.));
#135981=CARTESIAN_POINT('Ctrl Pts',(-38.4270213751568,-62.4292721978901,
12.));
#135982=CARTESIAN_POINT('Ctrl Pts',(-38.4483505226518,-62.4446087438312,
12.));
#135983=CARTESIAN_POINT('Ctrl Pts',(-38.4697244150482,-62.4599473459811,
12.));
#135984=CARTESIAN_POINT('Ctrl Pts',(-38.4911430040997,-62.4752879078854,
12.));
#135985=CARTESIAN_POINT('Ctrl Pts',(-38.5126062416502,-62.4906303334443,
12.));
#135986=CARTESIAN_POINT('Ctrl Pts',(-38.5341140796248,-62.5059745268901,
12.));
#135987=CARTESIAN_POINT('Ctrl Pts',(-38.5556664700195,-62.5213203927663,
12.));
#135988=CARTESIAN_POINT('Ctrl Pts',(-38.5772633648832,-62.5366678359023,
12.));
#135989=CARTESIAN_POINT('Ctrl Pts',(-38.5989047163393,-62.5520167614516,
12.));
#135990=CARTESIAN_POINT('Ctrl Pts',(-38.6205904766073,-62.5673670749361,
12.));
#135991=CARTESIAN_POINT('Ctrl Pts',(-38.6423205980213,-62.582718682292,
12.));
#135992=CARTESIAN_POINT('Ctrl Pts',(-38.6640950330421,-62.5980714899052,
12.));
#135993=CARTESIAN_POINT('Ctrl Pts',(-38.6859137342731,-62.6134254046739,
12.));
#135994=CARTESIAN_POINT('Ctrl Pts',(-38.7077766544416,-62.6287803339542,
12.));
#135995=CARTESIAN_POINT('Ctrl Pts',(-38.7296837463609,-62.6441361854411,
12.));
#135996=CARTESIAN_POINT('Ctrl Pts',(-38.7516349628904,-62.6594928670628,
12.));
#135997=CARTESIAN_POINT('Ctrl Pts',(-38.7736302568982,-62.6748502868835,
12.));
#135998=CARTESIAN_POINT('Ctrl Pts',(-38.795669581203,-62.6902083529694,
12.));
#135999=CARTESIAN_POINT('Ctrl Pts',(-38.8177528885681,-62.7055669733802,
12.));
#136000=CARTESIAN_POINT('Ctrl Pts',(-38.8398801318177,-62.7209260564493,
12.));
#136001=CARTESIAN_POINT('Ctrl Pts',(-38.8620512639233,-62.7362855110042,
12.));
#136002=CARTESIAN_POINT('Ctrl Pts',(-38.8842662380984,-62.7516452466128,
12.));
#136003=CARTESIAN_POINT('Ctrl Pts',(-38.9065250078832,-62.7670051738143,
12.));
#136004=CARTESIAN_POINT('Ctrl Pts',(-38.9288275272335,-62.78236520437,12.));
#136005=CARTESIAN_POINT('Ctrl Pts',(-38.9511737503165,-62.7977252507117,
12.));
#136006=CARTESIAN_POINT('Ctrl Pts',(-38.9735636313089,-62.8130852254027,
12.));
#136007=CARTESIAN_POINT('Ctrl Pts',(-38.9959971241701,-62.8284450405459,
12.));
#136008=CARTESIAN_POINT('Ctrl Pts',(-39.0184741824641,-62.8438046073224,
12.));
#136009=CARTESIAN_POINT('Ctrl Pts',(-39.0409947590497,-62.8591638352055,
12.));
#136010=CARTESIAN_POINT('Ctrl Pts',(-39.0635588063277,-62.8745226325998,
12.));
#136011=CARTESIAN_POINT('Ctrl Pts',(-39.0861662767932,-62.8898809082611,
12.));
#136012=CARTESIAN_POINT('Ctrl Pts',(-39.1088171235125,-62.9052385725387,
12.));
#136013=CARTESIAN_POINT('Ctrl Pts',(-39.131511300575,-62.9205955385558,
12.));
#136014=CARTESIAN_POINT('Ctrl Pts',(-39.1542487636744,-62.9359517237404,
12.));
#136015=CARTESIAN_POINT('Ctrl Pts',(-39.1770294702428,-62.9513070501867,
12.));
#136016=CARTESIAN_POINT('Ctrl Pts',(-39.1965939820934,-62.9644687386836,
12.));
#136017=CARTESIAN_POINT('Ctrl Pts',(-39.2116170128463,-62.9745590018674,
12.));
#136018=CARTESIAN_POINT('Ctrl Pts',(-39.222079438881,-62.9815782721328,
12.));
#136019=CARTESIAN_POINT('Ctrl Pts',(-39.2279686275011,-62.985526861613,
12.));
#136020=CARTESIAN_POINT('Ctrl Pts',(-39.2292784191818,-62.9864049293897,
12.));
#136021=CARTESIAN_POINT('',(-35.736831121751,-60.1903555511633,0.));
#136022=CARTESIAN_POINT('',(-35.736831121751,-60.1903555511633,0.));
#136023=CARTESIAN_POINT('Ctrl Pts',(-39.2292784191817,-62.9864049293896,
0.));
#136024=CARTESIAN_POINT('Ctrl Pts',(-39.227968627501,-62.985526861613,0.));
#136025=CARTESIAN_POINT('Ctrl Pts',(-39.2220794388809,-62.9815782721327,
0.));
#136026=CARTESIAN_POINT('Ctrl Pts',(-39.2116170128462,-62.9745590018674,
0.));
#136027=CARTESIAN_POINT('Ctrl Pts',(-39.1965939820934,-62.9644687386836,
0.));
#136028=CARTESIAN_POINT('Ctrl Pts',(-39.1770294702428,-62.9513070501867,
0.));
#136029=CARTESIAN_POINT('Ctrl Pts',(-39.1542487636744,-62.9359517237404,
0.));
#136030=CARTESIAN_POINT('Ctrl Pts',(-39.131511300575,-62.9205955385558,
0.));
#136031=CARTESIAN_POINT('Ctrl Pts',(-39.1088171235125,-62.9052385725387,
0.));
#136032=CARTESIAN_POINT('Ctrl Pts',(-39.0861662767932,-62.8898809082611,
0.));
#136033=CARTESIAN_POINT('Ctrl Pts',(-39.0635588063277,-62.8745226325998,
0.));
#136034=CARTESIAN_POINT('Ctrl Pts',(-39.0409947590497,-62.8591638352055,
0.));
#136035=CARTESIAN_POINT('Ctrl Pts',(-39.0184741824641,-62.8438046073224,
0.));
#136036=CARTESIAN_POINT('Ctrl Pts',(-38.9959971241701,-62.8284450405459,
0.));
#136037=CARTESIAN_POINT('Ctrl Pts',(-38.9735636313089,-62.8130852254027,
0.));
#136038=CARTESIAN_POINT('Ctrl Pts',(-38.9511737503165,-62.7977252507117,
0.));
#136039=CARTESIAN_POINT('Ctrl Pts',(-38.9288275272335,-62.78236520437,0.));
#136040=CARTESIAN_POINT('Ctrl Pts',(-38.9065250078832,-62.7670051738143,
0.));
#136041=CARTESIAN_POINT('Ctrl Pts',(-38.8842662380984,-62.7516452466128,
0.));
#136042=CARTESIAN_POINT('Ctrl Pts',(-38.8620512639233,-62.7362855110042,
0.));
#136043=CARTESIAN_POINT('Ctrl Pts',(-38.8398801318177,-62.7209260564493,
0.));
#136044=CARTESIAN_POINT('Ctrl Pts',(-38.8177528885681,-62.7055669733802,
0.));
#136045=CARTESIAN_POINT('Ctrl Pts',(-38.795669581203,-62.6902083529694,
0.));
#136046=CARTESIAN_POINT('Ctrl Pts',(-38.7736302568982,-62.6748502868835,
0.));
#136047=CARTESIAN_POINT('Ctrl Pts',(-38.7516349628904,-62.6594928670628,
0.));
#136048=CARTESIAN_POINT('Ctrl Pts',(-38.7296837463609,-62.6441361854411,
0.));
#136049=CARTESIAN_POINT('Ctrl Pts',(-38.7077766544416,-62.6287803339542,
0.));
#136050=CARTESIAN_POINT('Ctrl Pts',(-38.6859137342731,-62.6134254046739,
0.));
#136051=CARTESIAN_POINT('Ctrl Pts',(-38.6640950330421,-62.5980714899052,
0.));
#136052=CARTESIAN_POINT('Ctrl Pts',(-38.6423205980213,-62.582718682292,
0.));
#136053=CARTESIAN_POINT('Ctrl Pts',(-38.6205904766073,-62.5673670749361,
0.));
#136054=CARTESIAN_POINT('Ctrl Pts',(-38.5989047163393,-62.5520167614516,
0.));
#136055=CARTESIAN_POINT('Ctrl Pts',(-38.5772633648832,-62.5366678359023,
0.));
#136056=CARTESIAN_POINT('Ctrl Pts',(-38.5556664700195,-62.5213203927663,
0.));
#136057=CARTESIAN_POINT('Ctrl Pts',(-38.5341140796248,-62.5059745268901,
0.));
#136058=CARTESIAN_POINT('Ctrl Pts',(-38.5126062416502,-62.4906303334443,
0.));
#136059=CARTESIAN_POINT('Ctrl Pts',(-38.4911430040997,-62.4752879078854,
0.));
#136060=CARTESIAN_POINT('Ctrl Pts',(-38.4697244150482,-62.4599473459811,
0.));
#136061=CARTESIAN_POINT('Ctrl Pts',(-38.4483505226518,-62.4446087438312,
0.));
#136062=CARTESIAN_POINT('Ctrl Pts',(-38.4270213751568,-62.4292721978901,
0.));
#136063=CARTESIAN_POINT('Ctrl Pts',(-38.405737020905,-62.4139378049885,
0.));
#136064=CARTESIAN_POINT('Ctrl Pts',(-38.3844975083343,-62.3986056623577,
0.));
#136065=CARTESIAN_POINT('Ctrl Pts',(-38.3633028859828,-62.3832758676271,
0.));
#136066=CARTESIAN_POINT('Ctrl Pts',(-38.342153202491,-62.3679485188171,
0.));
#136067=CARTESIAN_POINT('Ctrl Pts',(-38.3210485066001,-62.3526237143336,
0.));
#136068=CARTESIAN_POINT('Ctrl Pts',(-38.2999888471476,-62.3373015529613,
0.));
#136069=CARTESIAN_POINT('Ctrl Pts',(-38.2789742730564,-62.3219821338569,
0.));
#136070=CARTESIAN_POINT('Ctrl Pts',(-38.2580048333361,-62.3066655565503,
0.));
#136071=CARTESIAN_POINT('Ctrl Pts',(-38.2370805770935,-62.2913519209521,
0.));
#136072=CARTESIAN_POINT('Ctrl Pts',(-38.2162015535353,-62.2760413273602,
0.));
#136073=CARTESIAN_POINT('Ctrl Pts',(-38.1953678119691,-62.2607338764654,
0.));
#136074=CARTESIAN_POINT('Ctrl Pts',(-38.1745794017996,-62.245429669358,
0.));
#136075=CARTESIAN_POINT('Ctrl Pts',(-38.1538363725264,-62.2301288075321,
0.));
#136076=CARTESIAN_POINT('Ctrl Pts',(-38.133138773753,-62.2148313928863,
0.));
#136077=CARTESIAN_POINT('Ctrl Pts',(-38.1124866551886,-62.1995375277257,
0.));
#136078=CARTESIAN_POINT('Ctrl Pts',(-38.0918800666479,-62.1842473147626,
0.));
#136079=CARTESIAN_POINT('Ctrl Pts',(-38.0713190580463,-62.1689608571176,
0.));
#136080=CARTESIAN_POINT('Ctrl Pts',(-38.0508036793939,-62.1536782583199,
0.));
#136081=CARTESIAN_POINT('Ctrl Pts',(-38.0303339808053,-62.1383996223124,
0.));
#136082=CARTESIAN_POINT('Ctrl Pts',(-38.0099100125037,-62.123125053455,
0.));
#136083=CARTESIAN_POINT('Ctrl Pts',(-37.9895318248212,-62.107854656528,
0.));
#136084=CARTESIAN_POINT('Ctrl Pts',(-37.9691994681966,-62.0925885367352,
0.));
#136085=CARTESIAN_POINT('Ctrl Pts',(-37.9489129931689,-62.0773267997078,
0.));
#136086=CARTESIAN_POINT('Ctrl Pts',(-37.9286724503851,-62.0620695515074,
0.));
#136087=CARTESIAN_POINT('Ctrl Pts',(-37.9084778906053,-62.0468168986288,
0.));
#136088=CARTESIAN_POINT('Ctrl Pts',(-37.8883293647029,-62.031568948002,
0.));
#136089=CARTESIAN_POINT('Ctrl Pts',(-37.868226923663,-62.0163258069957,
0.));
#136090=CARTESIAN_POINT('Ctrl Pts',(-37.8481706185749,-62.0010875834187,
0.));
#136091=CARTESIAN_POINT('Ctrl Pts',(-37.828160500638,-61.9858543855236,
0.));
#136092=CARTESIAN_POINT('Ctrl Pts',(-37.8081966211689,-61.9706263220114,
0.));
#136093=CARTESIAN_POINT('Ctrl Pts',(-37.7882790316014,-61.9554035020338,
0.));
#136094=CARTESIAN_POINT('Ctrl Pts',(-37.7684077834872,-61.9401860351972,
0.));
#136095=CARTESIAN_POINT('Ctrl Pts',(-37.7485829284871,-61.9249740315649,
0.));
#136096=CARTESIAN_POINT('Ctrl Pts',(-37.7288045183756,-61.9097676016601,
0.));
#136097=CARTESIAN_POINT('Ctrl Pts',(-37.7090726050482,-61.8945668564704,
0.));
#136098=CARTESIAN_POINT('Ctrl Pts',(-37.6893872405228,-61.8793719074507,
0.));
#136099=CARTESIAN_POINT('Ctrl Pts',(-37.6697484769392,-61.8641828665261,
0.));
#136100=CARTESIAN_POINT('Ctrl Pts',(-37.6501563665523,-61.8489998460957,
0.));
#136101=CARTESIAN_POINT('Ctrl Pts',(-37.6306109617346,-61.8338229590352,
0.));
#136102=CARTESIAN_POINT('Ctrl Pts',(-37.6111123149839,-61.8186523187015,
0.));
#136103=CARTESIAN_POINT('Ctrl Pts',(-37.5916604789253,-61.8034880389362,
0.));
#136104=CARTESIAN_POINT('Ctrl Pts',(-37.5722555063111,-61.7883302340687,
0.));
#136105=CARTESIAN_POINT('Ctrl Pts',(-37.5528974500142,-61.773179018919,
0.));
#136106=CARTESIAN_POINT('Ctrl Pts',(-37.5335863630287,-61.7580345088016,
0.));
#136107=CARTESIAN_POINT('Ctrl Pts',(-37.5143222984796,-61.7428968195299,
0.));
#136108=CARTESIAN_POINT('Ctrl Pts',(-37.4951053096237,-61.7277660674205,
0.));
#136109=CARTESIAN_POINT('Ctrl Pts',(-37.4759354498509,-61.7126423692963,
0.));
#136110=CARTESIAN_POINT('Ctrl Pts',(-37.4568127726773,-61.6975258424894,
0.));
#136111=CARTESIAN_POINT('Ctrl Pts',(-37.4377373317451,-61.6824166048444,
0.));
#136112=CARTESIAN_POINT('Ctrl Pts',(-37.4187091808321,-61.6673147747242,
0.));
#136113=CARTESIAN_POINT('Ctrl Pts',(-37.3997283738533,-61.6522204710131,
0.));
#136114=CARTESIAN_POINT('Ctrl Pts',(-37.3807949648624,-61.637133813121,
0.));
#136115=CARTESIAN_POINT('Ctrl Pts',(-37.361909008045,-61.6220549209866,
0.));
#136116=CARTESIAN_POINT('Ctrl Pts',(-37.343070557718,-61.6069839150807,
0.));
#136117=CARTESIAN_POINT('Ctrl Pts',(-37.3242796683395,-61.591920916412,
0.));
#136118=CARTESIAN_POINT('Ctrl Pts',(-37.3055363945107,-61.5768660465311,
0.));
#136119=CARTESIAN_POINT('Ctrl Pts',(-37.2868407909771,-61.5618194275348,
0.));
#136120=CARTESIAN_POINT('Ctrl Pts',(-37.2681929126221,-61.5467811820691,
0.));
#136121=CARTESIAN_POINT('Ctrl Pts',(-37.2495928144667,-61.5317514333328,
0.));
#136122=CARTESIAN_POINT('Ctrl Pts',(-37.2310405516781,-61.5167303050832,
0.));
#136123=CARTESIAN_POINT('Ctrl Pts',(-37.2125361795731,-61.501717921641,
0.));
#136124=CARTESIAN_POINT('Ctrl Pts',(-37.1940797536181,-61.4867144078936,
0.));
#136125=CARTESIAN_POINT('Ctrl Pts',(-37.175671329424,-61.4717198892994,
0.));
#136126=CARTESIAN_POINT('Ctrl Pts',(-37.1573109627454,-61.4567344918919,
0.));
#136127=CARTESIAN_POINT('Ctrl Pts',(-37.1389987094905,-61.4417583422863,
0.));
#136128=CARTESIAN_POINT('Ctrl Pts',(-37.1207346257222,-61.4267915676822,
0.));
#136129=CARTESIAN_POINT('Ctrl Pts',(-37.1025187676602,-61.4118342958697,
0.));
#136130=CARTESIAN_POINT('Ctrl Pts',(-37.0843511916745,-61.3968866552317,
0.));
#136131=CARTESIAN_POINT('Ctrl Pts',(-37.0662319542849,-61.381948774749,
0.));
#136132=CARTESIAN_POINT('Ctrl Pts',(-37.0481611121717,-61.3670207840068,
0.));
#136133=CARTESIAN_POINT('Ctrl Pts',(-37.0301387221774,-61.3521028132003,
0.));
#136134=CARTESIAN_POINT('Ctrl Pts',(-37.0121648413082,-61.3371949931387,
0.));
#136135=CARTESIAN_POINT('Ctrl Pts',(-36.994239526727,-61.3222974552486,
0.));
#136136=CARTESIAN_POINT('Ctrl Pts',(-36.9763628357544,-61.3074103315791,
0.));
#136137=CARTESIAN_POINT('Ctrl Pts',(-36.9585348258776,-61.2925337548077,
0.));
#136138=CARTESIAN_POINT('Ctrl Pts',(-36.9407555547535,-61.2776678582461,
0.));
#136139=CARTESIAN_POINT('Ctrl Pts',(-36.9230250802087,-61.2628127758457,
0.));
#136140=CARTESIAN_POINT('Ctrl Pts',(-36.9053434602343,-61.247968642201,
0.));
#136141=CARTESIAN_POINT('Ctrl Pts',(-36.8877107529865,-61.2331355925547,
0.));
#136142=CARTESIAN_POINT('Ctrl Pts',(-36.8701270167969,-61.2183137628056,
0.));
#136143=CARTESIAN_POINT('Ctrl Pts',(-36.852592310174,-61.2035032895127,
0.));
#136144=CARTESIAN_POINT('Ctrl Pts',(-36.8351066918036,-61.1887043099014,
0.));
#136145=CARTESIAN_POINT('Ctrl Pts',(-36.8176702205423,-61.1739169618666,
0.));
#136146=CARTESIAN_POINT('Ctrl Pts',(-36.8002829554209,-61.1591413839787,
0.));
#136147=CARTESIAN_POINT('Ctrl Pts',(-36.7829449556532,-61.1443777154911,
0.));
#136148=CARTESIAN_POINT('Ctrl Pts',(-36.765656280638,-61.1296260963466,
0.));
#136149=CARTESIAN_POINT('Ctrl Pts',(-36.7484169899596,-61.1148866671829,
0.));
#136150=CARTESIAN_POINT('Ctrl Pts',(-36.7312271433807,-61.100159569337,
0.));
#136151=CARTESIAN_POINT('Ctrl Pts',(-36.7140868008486,-61.0854449448524,
0.));
#136152=CARTESIAN_POINT('Ctrl Pts',(-36.6969960225022,-61.0707429364847,
0.));
#136153=CARTESIAN_POINT('Ctrl Pts',(-36.679954868674,-61.0560536877083,
0.));
#136154=CARTESIAN_POINT('Ctrl Pts',(-36.6629633998886,-61.0413773427203,
0.));
#136155=CARTESIAN_POINT('Ctrl Pts',(-36.6460216768553,-61.0267140464432,
0.));
#136156=CARTESIAN_POINT('Ctrl Pts',(-36.6291297604776,-61.0120639445349,
0.));
#136157=CARTESIAN_POINT('Ctrl Pts',(-36.61228771186,-60.9974271833981,0.));
#136158=CARTESIAN_POINT('Ctrl Pts',(-36.595495592311,-60.9828039101887,
0.));
#136159=CARTESIAN_POINT('Ctrl Pts',(-36.5787534633416,-60.9681942728236,
0.));
#136160=CARTESIAN_POINT('Ctrl Pts',(-36.5620613866615,-60.9535984199873,
0.));
#136161=CARTESIAN_POINT('Ctrl Pts',(-36.5454194241865,-60.9390165011355,
0.));
#136162=CARTESIAN_POINT('Ctrl Pts',(-36.5288276380416,-60.9244486664987,
0.));
#136163=CARTESIAN_POINT('Ctrl Pts',(-36.5122860905612,-60.9098950670847,
0.));
#136164=CARTESIAN_POINT('Ctrl Pts',(-36.4957948442835,-60.8953558546795,
0.));
#136165=CARTESIAN_POINT('Ctrl Pts',(-36.4793539619466,-60.8808311818499,
0.));
#136166=CARTESIAN_POINT('Ctrl Pts',(-36.4629635065045,-60.8663212019657,
0.));
#136167=CARTESIAN_POINT('Ctrl Pts',(-36.4466235411358,-60.8518260692188,
0.));
#136168=CARTESIAN_POINT('Ctrl Pts',(-36.4303341292494,-60.8373459386392,
0.));
#136169=CARTESIAN_POINT('Ctrl Pts',(-36.4140953344858,-60.822880966116,
0.));
#136170=CARTESIAN_POINT('Ctrl Pts',(-36.397907220716,-60.8084313083984,
0.));
#136171=CARTESIAN_POINT('Ctrl Pts',(-36.3817698520388,-60.793997123076,
0.));
#136172=CARTESIAN_POINT('Ctrl Pts',(-36.365683292773,-60.7795785685625,
0.));
#136173=CARTESIAN_POINT('Ctrl Pts',(-36.3496476074488,-60.7651758040803,
0.));
#136174=CARTESIAN_POINT('Ctrl Pts',(-36.3336628607859,-60.7507889896308,
0.));
#136175=CARTESIAN_POINT('Ctrl Pts',(-36.3177291177163,-60.7364182860412,
0.));
#136176=CARTESIAN_POINT('Ctrl Pts',(-36.3018464434214,-60.722063855041,
0.));
#136177=CARTESIAN_POINT('Ctrl Pts',(-36.2860149033587,-60.7077258593268,
0.));
#136178=CARTESIAN_POINT('Ctrl Pts',(-36.2702345632875,-60.6934044626291,
0.));
#136179=CARTESIAN_POINT('Ctrl Pts',(-36.2545054892897,-60.67909982978,0.));
#136180=CARTESIAN_POINT('Ctrl Pts',(-36.2388277477212,-60.6648121265885,
0.));
#136181=CARTESIAN_POINT('Ctrl Pts',(-36.2232014051541,-60.6505415197042,
0.));
#136182=CARTESIAN_POINT('Ctrl Pts',(-36.2076265283264,-60.6362881765019,
0.));
#136183=CARTESIAN_POINT('Ctrl Pts',(-36.192103184063,-60.6220522649149,
0.));
#136184=CARTESIAN_POINT('Ctrl Pts',(-36.1766314392641,-60.6078339534181,
0.));
#136185=CARTESIAN_POINT('Ctrl Pts',(-36.1612113610773,-60.5936334114108,
0.));
#136186=CARTESIAN_POINT('Ctrl Pts',(-36.1458430170431,-60.5794508095564,
0.));
#136187=CARTESIAN_POINT('Ctrl Pts',(-36.1305264752188,-60.565286320072,
0.));
#136188=CARTESIAN_POINT('Ctrl Pts',(-36.1152618043739,-60.5511401171984,
0.));
#136189=CARTESIAN_POINT('Ctrl Pts',(-36.100049073851,-60.5370123768804,
0.));
#136190=CARTESIAN_POINT('Ctrl Pts',(-36.0848883531952,-60.5229032758973,
0.));
#136191=CARTESIAN_POINT('Ctrl Pts',(-36.0697797118376,-60.5088129911354,
0.));
#136192=CARTESIAN_POINT('Ctrl Pts',(-36.0547232187698,-60.4947416988422,
0.));
#136193=CARTESIAN_POINT('Ctrl Pts',(-36.0397189421644,-60.4806895737686,
0.));
#136194=CARTESIAN_POINT('Ctrl Pts',(-36.0247669500891,-60.4666567908093,
0.));
#136195=CARTESIAN_POINT('Ctrl Pts',(-36.009867311357,-60.4526435269662,
0.));
#136196=CARTESIAN_POINT('Ctrl Pts',(-35.995020096217,-60.4386499629481,
0.));
#136197=CARTESIAN_POINT('Ctrl Pts',(-35.9802253773515,-60.4246762854926,
0.));
#136198=CARTESIAN_POINT('Ctrl Pts',(-35.9654832299601,-60.4107226875714,
0.));
#136199=CARTESIAN_POINT('Ctrl Pts',(-35.9507937296707,-60.3967893635452,
0.));
#136200=CARTESIAN_POINT('Ctrl Pts',(-35.936156950695,-60.3828765049019,
0.));
#136201=CARTESIAN_POINT('Ctrl Pts',(-35.9215729642231,-60.3689842965481,
0.));
#136202=CARTESIAN_POINT('Ctrl Pts',(-35.907041835853,-60.3551129108845,
0.));
#136203=CARTESIAN_POINT('Ctrl Pts',(-35.8925636280668,-60.3412625135287,
0.));
#136204=CARTESIAN_POINT('Ctrl Pts',(-35.8781384051537,-60.327433274683,
0.));
#136205=CARTESIAN_POINT('Ctrl Pts',(-35.8637662371635,-60.3136253782809,
0.));
#136206=CARTESIAN_POINT('Ctrl Pts',(-35.8494472046745,-60.2998390330102,
0.));
#136207=CARTESIAN_POINT('Ctrl Pts',(-35.8351814020357,-60.2860744798436,
0.));
#136208=CARTESIAN_POINT('Ctrl Pts',(-35.8209689272501,-60.2723319687369,
0.));
#136209=CARTESIAN_POINT('Ctrl Pts',(-35.8068098723347,-60.2586117365205,
0.));
#136210=CARTESIAN_POINT('Ctrl Pts',(-35.7927043145201,-60.2449139865274,
0.));
#136211=CARTESIAN_POINT('Ctrl Pts',(-35.7786523045912,-60.2312388621529,
0.));
#136212=CARTESIAN_POINT('Ctrl Pts',(-35.7646538667493,-60.2175864450043,
0.));
#136213=CARTESIAN_POINT('Ctrl Pts',(-35.7534979802053,-60.206682708692,
0.));
#136214=CARTESIAN_POINT('Ctrl Pts',(-35.7451551752572,-60.1985151474623,
0.));
#136215=CARTESIAN_POINT('Ctrl Pts',(-35.7396040204017,-60.193074658032,
0.));
#136216=CARTESIAN_POINT('Ctrl Pts',(-35.736831121751,-60.1903555511633,
0.));
#136217=CARTESIAN_POINT('Ctrl Pts',(-44.8554660179045,-59.483083043136,
0.));
#136218=CARTESIAN_POINT('Ctrl Pts',(-44.8554660179045,-59.483083043136,
12.));
#136219=CARTESIAN_POINT('Ctrl Pts',(-44.8505359826461,-59.4804358983083,
0.));
#136220=CARTESIAN_POINT('Ctrl Pts',(-44.8505359826461,-59.4804358983083,
12.));
#136221=CARTESIAN_POINT('Ctrl Pts',(-44.8406801497742,-59.4751410547732,
0.));
#136222=CARTESIAN_POINT('Ctrl Pts',(-44.8406801497742,-59.4751410547732,
12.));
#136223=CARTESIAN_POINT('Ctrl Pts',(-44.8259091134016,-59.4671971278321,
0.));
#136224=CARTESIAN_POINT('Ctrl Pts',(-44.8259091134016,-59.4671971278321,
12.));
#136225=CARTESIAN_POINT('Ctrl Pts',(-44.8062398251406,-59.4566019018254,
0.));
#136226=CARTESIAN_POINT('Ctrl Pts',(-44.8062398251406,-59.4566019018254,
12.));
#136227=CARTESIAN_POINT('Ctrl Pts',(-44.7816956017528,-59.4433523335147,
0.));
#136228=CARTESIAN_POINT('Ctrl Pts',(-44.7816956017528,-59.4433523335147,
12.));
#136229=CARTESIAN_POINT('Ctrl Pts',(-44.7571937812113,-59.430097240324,
0.));
#136230=CARTESIAN_POINT('Ctrl Pts',(-44.7571937812113,-59.430097240324,
12.));
#136231=CARTESIAN_POINT('Ctrl Pts',(-44.7327343876391,-59.4168366453118,
0.));
#136232=CARTESIAN_POINT('Ctrl Pts',(-44.7327343876391,-59.4168366453118,
12.));
#136233=CARTESIAN_POINT('Ctrl Pts',(-44.7083174541702,-59.4035705873811,
0.));
#136234=CARTESIAN_POINT('Ctrl Pts',(-44.7083174541702,-59.4035705873811,
12.));
#136235=CARTESIAN_POINT('Ctrl Pts',(-44.683943024421,-59.3902991267889,
0.));
#136236=CARTESIAN_POINT('Ctrl Pts',(-44.683943024421,-59.3902991267889,
12.));
#136237=CARTESIAN_POINT('Ctrl Pts',(-44.6596111512687,-59.377022343519,
0.));
#136238=CARTESIAN_POINT('Ctrl Pts',(-44.6596111512687,-59.377022343519,
12.));
#136239=CARTESIAN_POINT('Ctrl Pts',(-44.6353218935685,-59.3637403301801,
0.));
#136240=CARTESIAN_POINT('Ctrl Pts',(-44.6353218935685,-59.3637403301801,
12.));
#136241=CARTESIAN_POINT('Ctrl Pts',(-44.6110753134277,-59.3504531864154,
0.));
#136242=CARTESIAN_POINT('Ctrl Pts',(-44.6110753134277,-59.3504531864154,
12.));
#136243=CARTESIAN_POINT('Ctrl Pts',(-44.5868714733234,-59.3371610128511,
0.));
#136244=CARTESIAN_POINT('Ctrl Pts',(-44.5868714733234,-59.3371610128511,
12.));
#136245=CARTESIAN_POINT('Ctrl Pts',(-44.5627104331017,-59.3238639048694,
0.));
#136246=CARTESIAN_POINT('Ctrl Pts',(-44.5627104331017,-59.3238639048694,
12.));
#136247=CARTESIAN_POINT('Ctrl Pts',(-44.5385922475573,-59.3105619475609,
0.));
#136248=CARTESIAN_POINT('Ctrl Pts',(-44.5385922475573,-59.3105619475609,
12.));
#136249=CARTESIAN_POINT('Ctrl Pts',(-44.5145169681349,-59.2972552192156,
0.));
#136250=CARTESIAN_POINT('Ctrl Pts',(-44.5145169681349,-59.2972552192156,
12.));
#136251=CARTESIAN_POINT('Ctrl Pts',(-44.490484644151,-59.2839437938237,
0.));
#136252=CARTESIAN_POINT('Ctrl Pts',(-44.490484644151,-59.2839437938237,
12.));
#136253=CARTESIAN_POINT('Ctrl Pts',(-44.4664953242379,-59.2706277440445,
0.));
#136254=CARTESIAN_POINT('Ctrl Pts',(-44.4664953242379,-59.2706277440445,
12.));
#136255=CARTESIAN_POINT('Ctrl Pts',(-44.4425490575911,-59.2573071437774,
0.));
#136256=CARTESIAN_POINT('Ctrl Pts',(-44.4425490575911,-59.2573071437774,
12.));
#136257=CARTESIAN_POINT('Ctrl Pts',(-44.4186458955451,-59.2439820714187,
0.));
#136258=CARTESIAN_POINT('Ctrl Pts',(-44.4186458955451,-59.2439820714187,
12.));
#136259=CARTESIAN_POINT('Ctrl Pts',(-44.3947858914074,-59.2306526095131,
0.));
#136260=CARTESIAN_POINT('Ctrl Pts',(-44.3947858914074,-59.2306526095131,
12.));
#136261=CARTESIAN_POINT('Ctrl Pts',(-44.3709690997469,-59.2173188432798,
0.));
#136262=CARTESIAN_POINT('Ctrl Pts',(-44.3709690997469,-59.2173188432798,
12.));
#136263=CARTESIAN_POINT('Ctrl Pts',(-44.3471955758403,-59.2039808594752,
0.));
#136264=CARTESIAN_POINT('Ctrl Pts',(-44.3471955758403,-59.2039808594752,
12.));
#136265=CARTESIAN_POINT('Ctrl Pts',(-44.3234653750884,-59.1906387451979,
0.));
#136266=CARTESIAN_POINT('Ctrl Pts',(-44.3234653750884,-59.1906387451979,
12.));
#136267=CARTESIAN_POINT('Ctrl Pts',(-44.2997785523431,-59.1772925865213,
0.));
#136268=CARTESIAN_POINT('Ctrl Pts',(-44.2997785523431,-59.1772925865213,
12.));
#136269=CARTESIAN_POINT('Ctrl Pts',(-44.2761351616048,-59.1639424678793,
0.));
#136270=CARTESIAN_POINT('Ctrl Pts',(-44.2761351616048,-59.1639424678793,
12.));
#136271=CARTESIAN_POINT('Ctrl Pts',(-44.2525352563996,-59.1505884728215,
0.));
#136272=CARTESIAN_POINT('Ctrl Pts',(-44.2525352563996,-59.1505884728215,
12.));
#136273=CARTESIAN_POINT('Ctrl Pts',(-44.228978889997,-59.1372306844586,
0.));
#136274=CARTESIAN_POINT('Ctrl Pts',(-44.228978889997,-59.1372306844586,
12.));
#136275=CARTESIAN_POINT('Ctrl Pts',(-44.2054661156875,-59.1238691860306,
0.));
#136276=CARTESIAN_POINT('Ctrl Pts',(-44.2054661156875,-59.1238691860306,
12.));
#136277=CARTESIAN_POINT('Ctrl Pts',(-44.1819969870307,-59.1105040614276,
0.));
#136278=CARTESIAN_POINT('Ctrl Pts',(-44.1819969870307,-59.1105040614276,
12.));
#136279=CARTESIAN_POINT('Ctrl Pts',(-44.1585715581064,-59.0971353957206,
0.));
#136280=CARTESIAN_POINT('Ctrl Pts',(-44.1585715581064,-59.0971353957206,
12.));
#136281=CARTESIAN_POINT('Ctrl Pts',(-44.1351898834051,-59.08376327492,0.));
#136282=CARTESIAN_POINT('Ctrl Pts',(-44.1351898834051,-59.08376327492,12.));
#136283=CARTESIAN_POINT('Ctrl Pts',(-44.1118520177221,-59.0703877857526,
0.));
#136284=CARTESIAN_POINT('Ctrl Pts',(-44.1118520177221,-59.0703877857526,
12.));
#136285=CARTESIAN_POINT('Ctrl Pts',(-44.0885580160432,-59.0570090154243,
0.));
#136286=CARTESIAN_POINT('Ctrl Pts',(-44.0885580160432,-59.0570090154243,
12.));
#136287=CARTESIAN_POINT('Ctrl Pts',(-44.0653079334385,-59.0436270514087,
0.));
#136288=CARTESIAN_POINT('Ctrl Pts',(-44.0653079334385,-59.0436270514087,
12.));
#136289=CARTESIAN_POINT('Ctrl Pts',(-44.0421018249223,-59.0302419811777,
0.));
#136290=CARTESIAN_POINT('Ctrl Pts',(-44.0421018249223,-59.0302419811777,
12.));
#136291=CARTESIAN_POINT('Ctrl Pts',(-44.0189397454599,-59.0168538922095,
0.));
#136292=CARTESIAN_POINT('Ctrl Pts',(-44.0189397454599,-59.0168538922095,
12.));
#136293=CARTESIAN_POINT('Ctrl Pts',(-43.9958217500369,-59.0034628721168,
0.));
#136294=CARTESIAN_POINT('Ctrl Pts',(-43.9958217500369,-59.0034628721168,
12.));
#136295=CARTESIAN_POINT('Ctrl Pts',(-43.9727478937056,-58.9900690087408,
0.));
#136296=CARTESIAN_POINT('Ctrl Pts',(-43.9727478937056,-58.9900690087408,
12.));
#136297=CARTESIAN_POINT('Ctrl Pts',(-43.9497182316331,-58.9766723902529,
0.));
#136298=CARTESIAN_POINT('Ctrl Pts',(-43.9497182316331,-58.9766723902529,
12.));
#136299=CARTESIAN_POINT('Ctrl Pts',(-43.9267328191501,-58.9632731052696,
0.));
#136300=CARTESIAN_POINT('Ctrl Pts',(-43.9267328191501,-58.9632731052696,
12.));
#136301=CARTESIAN_POINT('Ctrl Pts',(-43.9037917117739,-58.9498712429054,
0.));
#136302=CARTESIAN_POINT('Ctrl Pts',(-43.9037917117739,-58.9498712429054,
12.));
#136303=CARTESIAN_POINT('Ctrl Pts',(-43.8808949651873,-58.936466892712,
0.));
#136304=CARTESIAN_POINT('Ctrl Pts',(-43.8808949651873,-58.936466892712,
12.));
#136305=CARTESIAN_POINT('Ctrl Pts',(-43.858042635223,-58.9230601446436,
0.));
#136306=CARTESIAN_POINT('Ctrl Pts',(-43.858042635223,-58.9230601446436,
12.));
#136307=CARTESIAN_POINT('Ctrl Pts',(-43.835234777842,-58.9096510890129,
0.));
#136308=CARTESIAN_POINT('Ctrl Pts',(-43.835234777842,-58.9096510890129,
12.));
#136309=CARTESIAN_POINT('Ctrl Pts',(-43.8124714491076,-58.8962398164493,
0.));
#136310=CARTESIAN_POINT('Ctrl Pts',(-43.8124714491076,-58.8962398164493,
12.));
#136311=CARTESIAN_POINT('Ctrl Pts',(-43.7897527051609,-58.8828264178621,
0.));
#136312=CARTESIAN_POINT('Ctrl Pts',(-43.7897527051609,-58.8828264178621,
12.));
#136313=CARTESIAN_POINT('Ctrl Pts',(-43.7670786022402,-58.8694109844648,
0.));
#136314=CARTESIAN_POINT('Ctrl Pts',(-43.7670786022402,-58.8694109844648,
12.));
#136315=CARTESIAN_POINT('Ctrl Pts',(-43.7444491966942,-58.855993607794,
0.));
#136316=CARTESIAN_POINT('Ctrl Pts',(-43.7444491966942,-58.855993607794,
12.));
#136317=CARTESIAN_POINT('Ctrl Pts',(-43.7218645449922,-58.8425743797326,
0.));
#136318=CARTESIAN_POINT('Ctrl Pts',(-43.7218645449922,-58.8425743797326,
12.));
#136319=CARTESIAN_POINT('Ctrl Pts',(-43.6993247037314,-58.8291533925293,
0.));
#136320=CARTESIAN_POINT('Ctrl Pts',(-43.6993247037314,-58.8291533925293,
12.));
#136321=CARTESIAN_POINT('Ctrl Pts',(-43.6768297296395,-58.8157307388238,
0.));
#136322=CARTESIAN_POINT('Ctrl Pts',(-43.6768297296395,-58.8157307388238,
12.));
#136323=CARTESIAN_POINT('Ctrl Pts',(-43.6543796795789,-58.8023065116436,
0.));
#136324=CARTESIAN_POINT('Ctrl Pts',(-43.6543796795789,-58.8023065116436,
12.));
#136325=CARTESIAN_POINT('Ctrl Pts',(-43.6319746105482,-58.788880804397,
0.));
#136326=CARTESIAN_POINT('Ctrl Pts',(-43.6319746105482,-58.788880804397,
12.));
#136327=CARTESIAN_POINT('Ctrl Pts',(-43.6096145796797,-58.775453710867,
0.));
#136328=CARTESIAN_POINT('Ctrl Pts',(-43.6096145796797,-58.775453710867,
12.));
#136329=CARTESIAN_POINT('Ctrl Pts',(-43.5872996442345,-58.7620253252062,
0.));
#136330=CARTESIAN_POINT('Ctrl Pts',(-43.5872996442345,-58.7620253252062,
12.));
#136331=CARTESIAN_POINT('Ctrl Pts',(-43.5650298615917,-58.74859574193,0.));
#136332=CARTESIAN_POINT('Ctrl Pts',(-43.5650298615917,-58.74859574193,12.));
#136333=CARTESIAN_POINT('Ctrl Pts',(-43.5428052892488,-58.735165055918,
0.));
#136334=CARTESIAN_POINT('Ctrl Pts',(-43.5428052892488,-58.735165055918,
12.));
#136335=CARTESIAN_POINT('Ctrl Pts',(-43.5206259848337,-58.7217333624209,
0.));
#136336=CARTESIAN_POINT('Ctrl Pts',(-43.5206259848337,-58.7217333624209,
12.));
#136337=CARTESIAN_POINT('Ctrl Pts',(-43.4984920061073,-58.7083007570661,
0.));
#136338=CARTESIAN_POINT('Ctrl Pts',(-43.4984920061073,-58.7083007570661,
12.));
#136339=CARTESIAN_POINT('Ctrl Pts',(-43.4764034109654,-58.6948673358638,
0.));
#136340=CARTESIAN_POINT('Ctrl Pts',(-43.4764034109654,-58.6948673358638,
12.));
#136341=CARTESIAN_POINT('Ctrl Pts',(-43.4543602574351,-58.6814331952138,
0.));
#136342=CARTESIAN_POINT('Ctrl Pts',(-43.4543602574351,-58.6814331952138,
12.));
#136343=CARTESIAN_POINT('Ctrl Pts',(-43.4323626036737,-58.6679984319097,
0.));
#136344=CARTESIAN_POINT('Ctrl Pts',(-43.4323626036737,-58.6679984319097,
12.));
#136345=CARTESIAN_POINT('Ctrl Pts',(-43.4104105079768,-58.6545631431393,
0.));
#136346=CARTESIAN_POINT('Ctrl Pts',(-43.4104105079768,-58.6545631431393,
12.));
#136347=CARTESIAN_POINT('Ctrl Pts',(-43.388504028781,-58.6411274264857,
0.));
#136348=CARTESIAN_POINT('Ctrl Pts',(-43.388504028781,-58.6411274264857,
12.));
#136349=CARTESIAN_POINT('Ctrl Pts',(-43.3666432246635,-58.627691379929,
0.));
#136350=CARTESIAN_POINT('Ctrl Pts',(-43.3666432246635,-58.627691379929,
12.));
#136351=CARTESIAN_POINT('Ctrl Pts',(-43.3448281543371,-58.6142551018467,
0.));
#136352=CARTESIAN_POINT('Ctrl Pts',(-43.3448281543371,-58.6142551018467,
12.));
#136353=CARTESIAN_POINT('Ctrl Pts',(-43.3230588766449,-58.6008186910156,
0.));
#136354=CARTESIAN_POINT('Ctrl Pts',(-43.3230588766449,-58.6008186910156,
12.));
#136355=CARTESIAN_POINT('Ctrl Pts',(-43.3013354505701,-58.5873822466152,
0.));
#136356=CARTESIAN_POINT('Ctrl Pts',(-43.3013354505701,-58.5873822466152,
12.));
#136357=CARTESIAN_POINT('Ctrl Pts',(-43.27965793524,-58.573945868231,0.));
#136358=CARTESIAN_POINT('Ctrl Pts',(-43.27965793524,-58.573945868231,12.));
#136359=CARTESIAN_POINT('Ctrl Pts',(-43.2580263899278,-58.5605096558578,
0.));
#136360=CARTESIAN_POINT('Ctrl Pts',(-43.2580263899278,-58.5605096558578,
12.));
#136361=CARTESIAN_POINT('Ctrl Pts',(-43.2364408740493,-58.5470737099032,
0.));
#136362=CARTESIAN_POINT('Ctrl Pts',(-43.2364408740493,-58.5470737099032,
12.));
#136363=CARTESIAN_POINT('Ctrl Pts',(-43.2149014471574,-58.5336381311917,
0.));
#136364=CARTESIAN_POINT('Ctrl Pts',(-43.2149014471574,-58.5336381311917,
12.));
#136365=CARTESIAN_POINT('Ctrl Pts',(-43.1934081689505,-58.5202030209669,
0.));
#136366=CARTESIAN_POINT('Ctrl Pts',(-43.1934081689505,-58.5202030209669,
12.));
#136367=CARTESIAN_POINT('Ctrl Pts',(-43.1719610992771,-58.5067684808944,
0.));
#136368=CARTESIAN_POINT('Ctrl Pts',(-43.1719610992771,-58.5067684808944,
12.));
#136369=CARTESIAN_POINT('Ctrl Pts',(-43.1505602981365,-58.4933346130636,
0.));
#136370=CARTESIAN_POINT('Ctrl Pts',(-43.1505602981365,-58.4933346130636,
12.));
#136371=CARTESIAN_POINT('Ctrl Pts',(-43.1292058256777,-58.4799015199907,
0.));
#136372=CARTESIAN_POINT('Ctrl Pts',(-43.1292058256777,-58.4799015199907,
12.));
#136373=CARTESIAN_POINT('Ctrl Pts',(-43.1078977421916,-58.4664693046217,
0.));
#136374=CARTESIAN_POINT('Ctrl Pts',(-43.1078977421916,-58.4664693046217,
12.));
#136375=CARTESIAN_POINT('Ctrl Pts',(-43.0866361081177,-58.4530380703348,
0.));
#136376=CARTESIAN_POINT('Ctrl Pts',(-43.0866361081177,-58.4530380703348,
12.));
#136377=CARTESIAN_POINT('Ctrl Pts',(-43.0654209840511,-58.439607920945,
0.));
#136378=CARTESIAN_POINT('Ctrl Pts',(-43.0654209840511,-58.439607920945,
12.));
#136379=CARTESIAN_POINT('Ctrl Pts',(-43.0442524307434,-58.4261789607058,
0.));
#136380=CARTESIAN_POINT('Ctrl Pts',(-43.0442524307434,-58.4261789607058,
12.));
#136381=CARTESIAN_POINT('Ctrl Pts',(-43.0231305091027,-58.4127512943136,
0.));
#136382=CARTESIAN_POINT('Ctrl Pts',(-43.0231305091027,-58.4127512943136,
12.));
#136383=CARTESIAN_POINT('Ctrl Pts',(-43.0020552801859,-58.3993250269101,
0.));
#136384=CARTESIAN_POINT('Ctrl Pts',(-43.0020552801859,-58.3993250269101,
12.));
#136385=CARTESIAN_POINT('Ctrl Pts',(-42.9810268052032,-58.3859002640856,
0.));
#136386=CARTESIAN_POINT('Ctrl Pts',(-42.9810268052032,-58.3859002640856,
12.));
#136387=CARTESIAN_POINT('Ctrl Pts',(-42.960045145526,-58.3724771118826,
0.));
#136388=CARTESIAN_POINT('Ctrl Pts',(-42.960045145526,-58.3724771118826,
12.));
#136389=CARTESIAN_POINT('Ctrl Pts',(-42.9391103626879,-58.3590556767978,
0.));
#136390=CARTESIAN_POINT('Ctrl Pts',(-42.9391103626879,-58.3590556767978,
12.));
#136391=CARTESIAN_POINT('Ctrl Pts',(-42.9182225183855,-58.3456360657865,
0.));
#136392=CARTESIAN_POINT('Ctrl Pts',(-42.9182225183855,-58.3456360657865,
12.));
#136393=CARTESIAN_POINT('Ctrl Pts',(-42.8973816744709,-58.3322183862654,
0.));
#136394=CARTESIAN_POINT('Ctrl Pts',(-42.8973816744709,-58.3322183862654,
12.));
#136395=CARTESIAN_POINT('Ctrl Pts',(-42.8765878929551,-58.3188027461164,
0.));
#136396=CARTESIAN_POINT('Ctrl Pts',(-42.8765878929551,-58.3188027461164,
12.));
#136397=CARTESIAN_POINT('Ctrl Pts',(-42.8558412360158,-58.3053892536894,
0.));
#136398=CARTESIAN_POINT('Ctrl Pts',(-42.8558412360158,-58.3053892536894,
12.));
#136399=CARTESIAN_POINT('Ctrl Pts',(-42.8351417659999,-58.2919780178064,
0.));
#136400=CARTESIAN_POINT('Ctrl Pts',(-42.8351417659999,-58.2919780178064,
12.));
#136401=CARTESIAN_POINT('Ctrl Pts',(-42.8144895454233,-58.2785691477638,
0.));
#136402=CARTESIAN_POINT('Ctrl Pts',(-42.8144895454233,-58.2785691477638,
12.));
#136403=CARTESIAN_POINT('Ctrl Pts',(-42.7938846369651,-58.2651627533368,
0.));
#136404=CARTESIAN_POINT('Ctrl Pts',(-42.7938846369651,-58.2651627533368,
12.));
#136405=CARTESIAN_POINT('Ctrl Pts',(-42.7733271034679,-58.251758944782,
0.));
#136406=CARTESIAN_POINT('Ctrl Pts',(-42.7733271034679,-58.251758944782,
12.));
#136407=CARTESIAN_POINT('Ctrl Pts',(-42.7528170079484,-58.2383578328424,
0.));
#136408=CARTESIAN_POINT('Ctrl Pts',(-42.7528170079484,-58.2383578328424,
12.));
#136409=CARTESIAN_POINT('Ctrl Pts',(-42.7323544135985,-58.22495952875,0.));
#136410=CARTESIAN_POINT('Ctrl Pts',(-42.7323544135985,-58.22495952875,12.));
#136411=CARTESIAN_POINT('Ctrl Pts',(-42.7119393837866,-58.21156414423,0.));
#136412=CARTESIAN_POINT('Ctrl Pts',(-42.7119393837866,-58.21156414423,12.));
#136413=CARTESIAN_POINT('Ctrl Pts',(-42.6915719820513,-58.1981717915037,
0.));
#136414=CARTESIAN_POINT('Ctrl Pts',(-42.6915719820513,-58.1981717915037,
12.));
#136415=CARTESIAN_POINT('Ctrl Pts',(-42.6712522721016,-58.1847825832923,
0.));
#136416=CARTESIAN_POINT('Ctrl Pts',(-42.6712522721016,-58.1847825832923,
12.));
#136417=CARTESIAN_POINT('Ctrl Pts',(-42.6509803178265,-58.171396632821,
0.));
#136418=CARTESIAN_POINT('Ctrl Pts',(-42.6509803178265,-58.171396632821,
12.));
#136419=CARTESIAN_POINT('Ctrl Pts',(-42.6307561832976,-58.1580140538228,
0.));
#136420=CARTESIAN_POINT('Ctrl Pts',(-42.6307561832976,-58.1580140538228,
12.));
#136421=CARTESIAN_POINT('Ctrl Pts',(-42.6105799327699,-58.1446349605421,
0.));
#136422=CARTESIAN_POINT('Ctrl Pts',(-42.6105799327699,-58.1446349605421,
12.));
#136423=CARTESIAN_POINT('Ctrl Pts',(-42.5904516306762,-58.1312594677386,
0.));
#136424=CARTESIAN_POINT('Ctrl Pts',(-42.5904516306762,-58.1312594677386,
12.));
#136425=CARTESIAN_POINT('Ctrl Pts',(-42.5703713416265,-58.1178876906907,
0.));
#136426=CARTESIAN_POINT('Ctrl Pts',(-42.5703713416265,-58.1178876906907,
12.));
#136427=CARTESIAN_POINT('Ctrl Pts',(-42.5503391304183,-58.1045197452002,
0.));
#136428=CARTESIAN_POINT('Ctrl Pts',(-42.5503391304183,-58.1045197452002,
12.));
#136429=CARTESIAN_POINT('Ctrl Pts',(-42.5303550620387,-58.0911557475965,
0.));
#136430=CARTESIAN_POINT('Ctrl Pts',(-42.5303550620387,-58.0911557475965,
12.));
#136431=CARTESIAN_POINT('Ctrl Pts',(-42.5104192016664,-58.0777958147403,
0.));
#136432=CARTESIAN_POINT('Ctrl Pts',(-42.5104192016664,-58.0777958147403,
12.));
#136433=CARTESIAN_POINT('Ctrl Pts',(-42.4905316146653,-58.0644400640275,
0.));
#136434=CARTESIAN_POINT('Ctrl Pts',(-42.4905316146653,-58.0644400640275,
12.));
#136435=CARTESIAN_POINT('Ctrl Pts',(-42.4706923665845,-58.0510886133926,
0.));
#136436=CARTESIAN_POINT('Ctrl Pts',(-42.4706923665845,-58.0510886133926,
12.));
#136437=CARTESIAN_POINT('Ctrl Pts',(-42.4509015231674,-58.037741581314,
0.));
#136438=CARTESIAN_POINT('Ctrl Pts',(-42.4509015231674,-58.037741581314,
12.));
#136439=CARTESIAN_POINT('Ctrl Pts',(-42.4311591503555,-58.0243990868181,
0.));
#136440=CARTESIAN_POINT('Ctrl Pts',(-42.4311591503555,-58.0243990868181,
12.));
#136441=CARTESIAN_POINT('Ctrl Pts',(-42.411465314289,-58.0110612494828,
0.));
#136442=CARTESIAN_POINT('Ctrl Pts',(-42.411465314289,-58.0110612494828,
12.));
#136443=CARTESIAN_POINT('Ctrl Pts',(-42.3918200813014,-57.9977281894422,
0.));
#136444=CARTESIAN_POINT('Ctrl Pts',(-42.3918200813014,-57.9977281894422,
12.));
#136445=CARTESIAN_POINT('Ctrl Pts',(-42.3722235179197,-57.9844000273911,
0.));
#136446=CARTESIAN_POINT('Ctrl Pts',(-42.3722235179197,-57.9844000273911,
12.));
#136447=CARTESIAN_POINT('Ctrl Pts',(-42.3526756908746,-57.9710768845899,
0.));
#136448=CARTESIAN_POINT('Ctrl Pts',(-42.3526756908746,-57.9710768845899,
12.));
#136449=CARTESIAN_POINT('Ctrl Pts',(-42.333176667102,-57.9577588828682,
0.));
#136450=CARTESIAN_POINT('Ctrl Pts',(-42.333176667102,-57.9577588828682,
12.));
#136451=CARTESIAN_POINT('Ctrl Pts',(-42.3137265137452,-57.9444461446299,
0.));
#136452=CARTESIAN_POINT('Ctrl Pts',(-42.3137265137452,-57.9444461446299,
12.));
#136453=CARTESIAN_POINT('Ctrl Pts',(-42.2943252981489,-57.9311387928563,
0.));
#136454=CARTESIAN_POINT('Ctrl Pts',(-42.2943252981489,-57.9311387928563,
12.));
#136455=CARTESIAN_POINT('Ctrl Pts',(-42.2749730878594,-57.9178369511114,
0.));
#136456=CARTESIAN_POINT('Ctrl Pts',(-42.2749730878594,-57.9178369511114,
12.));
#136457=CARTESIAN_POINT('Ctrl Pts',(-42.2556699506353,-57.9045407435474,
0.));
#136458=CARTESIAN_POINT('Ctrl Pts',(-42.2556699506353,-57.9045407435474,
12.));
#136459=CARTESIAN_POINT('Ctrl Pts',(-42.2364159544501,-57.8912502949096,
0.));
#136460=CARTESIAN_POINT('Ctrl Pts',(-42.2364159544501,-57.8912502949096,
12.));
#136461=CARTESIAN_POINT('Ctrl Pts',(-42.2172111674938,-57.8779657305413,
0.));
#136462=CARTESIAN_POINT('Ctrl Pts',(-42.2172111674938,-57.8779657305413,
12.));
#136463=CARTESIAN_POINT('Ctrl Pts',(-42.1980556581665,-57.864687176387,
0.));
#136464=CARTESIAN_POINT('Ctrl Pts',(-42.1980556581665,-57.864687176387,
12.));
#136465=CARTESIAN_POINT('Ctrl Pts',(-42.1789494950794,-57.8514147589972,
0.));
#136466=CARTESIAN_POINT('Ctrl Pts',(-42.1789494950794,-57.8514147589972,
12.));
#136467=CARTESIAN_POINT('Ctrl Pts',(-42.1598927470646,-57.8381486055342,
0.));
#136468=CARTESIAN_POINT('Ctrl Pts',(-42.1598927470646,-57.8381486055342,
12.));
#136469=CARTESIAN_POINT('Ctrl Pts',(-42.1408854831783,-57.8248888437775,
0.));
#136470=CARTESIAN_POINT('Ctrl Pts',(-42.1408854831783,-57.8248888437775,
12.));
#136471=CARTESIAN_POINT('Ctrl Pts',(-42.1219277727021,-57.8116356021288,
0.));
#136472=CARTESIAN_POINT('Ctrl Pts',(-42.1219277727021,-57.8116356021288,
12.));
#136473=CARTESIAN_POINT('Ctrl Pts',(-42.1030196851366,-57.798389009616,
0.));
#136474=CARTESIAN_POINT('Ctrl Pts',(-42.1030196851366,-57.798389009616,
12.));
#136475=CARTESIAN_POINT('Ctrl Pts',(-42.0841612902042,-57.7851491958987,
0.));
#136476=CARTESIAN_POINT('Ctrl Pts',(-42.0841612902042,-57.7851491958987,
12.));
#136477=CARTESIAN_POINT('Ctrl Pts',(-42.0653526578588,-57.7719162912744,
0.));
#136478=CARTESIAN_POINT('Ctrl Pts',(-42.0653526578588,-57.7719162912744,
12.));
#136479=CARTESIAN_POINT('Ctrl Pts',(-42.0465938582882,-57.7586904266834,
0.));
#136480=CARTESIAN_POINT('Ctrl Pts',(-42.0465938582882,-57.7586904266834,
12.));
#136481=CARTESIAN_POINT('Ctrl Pts',(-42.0278849619148,-57.745471733714,
0.));
#136482=CARTESIAN_POINT('Ctrl Pts',(-42.0278849619148,-57.745471733714,
12.));
#136483=CARTESIAN_POINT('Ctrl Pts',(-42.0092260393897,-57.7322603446066,
0.));
#136484=CARTESIAN_POINT('Ctrl Pts',(-42.0092260393897,-57.7322603446066,
12.));
#136485=CARTESIAN_POINT('Ctrl Pts',(-41.990617161596,-57.7190563922593,
0.));
#136486=CARTESIAN_POINT('Ctrl Pts',(-41.990617161596,-57.7190563922593,
12.));
#136487=CARTESIAN_POINT('Ctrl Pts',(-41.9720583996592,-57.7058600102351,
0.));
#136488=CARTESIAN_POINT('Ctrl Pts',(-41.9720583996592,-57.7058600102351,
12.));
#136489=CARTESIAN_POINT('Ctrl Pts',(-41.9535498249488,-57.6926713327672,
0.));
#136490=CARTESIAN_POINT('Ctrl Pts',(-41.9535498249488,-57.6926713327672,
12.));
#136491=CARTESIAN_POINT('Ctrl Pts',(-41.9350915090796,-57.6794904947649,
0.));
#136492=CARTESIAN_POINT('Ctrl Pts',(-41.9350915090796,-57.6794904947649,
12.));
#136493=CARTESIAN_POINT('Ctrl Pts',(-41.9166835239054,-57.6663176318189,
0.));
#136494=CARTESIAN_POINT('Ctrl Pts',(-41.9166835239054,-57.6663176318189,
12.));
#136495=CARTESIAN_POINT('Ctrl Pts',(-41.8983259415253,-57.6531528802072,
0.));
#136496=CARTESIAN_POINT('Ctrl Pts',(-41.8983259415253,-57.6531528802072,
12.));
#136497=CARTESIAN_POINT('Ctrl Pts',(-41.8800188342912,-57.6399963769009,
0.));
#136498=CARTESIAN_POINT('Ctrl Pts',(-41.8800188342912,-57.6399963769009,
12.));
#136499=CARTESIAN_POINT('Ctrl Pts',(-41.8617622748107,-57.6268482595701,
0.));
#136500=CARTESIAN_POINT('Ctrl Pts',(-41.8617622748107,-57.6268482595701,
12.));
#136501=CARTESIAN_POINT('Ctrl Pts',(-41.8435563359456,-57.613708666588,
0.));
#136502=CARTESIAN_POINT('Ctrl Pts',(-41.8435563359456,-57.613708666588,
12.));
#136503=CARTESIAN_POINT('Ctrl Pts',(-41.8254010908051,-57.6005777370347,
0.));
#136504=CARTESIAN_POINT('Ctrl Pts',(-41.8254010908051,-57.6005777370347,
12.));
#136505=CARTESIAN_POINT('Ctrl Pts',(-41.8072966127559,-57.5874556107054,
0.));
#136506=CARTESIAN_POINT('Ctrl Pts',(-41.8072966127559,-57.5874556107054,
12.));
#136507=CARTESIAN_POINT('Ctrl Pts',(-41.7892429754298,-57.5743424281204,
0.));
#136508=CARTESIAN_POINT('Ctrl Pts',(-41.7892429754298,-57.5743424281204,
12.));
#136509=CARTESIAN_POINT('Ctrl Pts',(-41.7712402527273,-57.561238330532,
0.));
#136510=CARTESIAN_POINT('Ctrl Pts',(-41.7712402527273,-57.561238330532,
12.));
#136511=CARTESIAN_POINT('Ctrl Pts',(-41.7532885188174,-57.5481434599334,
0.));
#136512=CARTESIAN_POINT('Ctrl Pts',(-41.7532885188174,-57.5481434599334,
12.));
#136513=CARTESIAN_POINT('Ctrl Pts',(-41.7353878481336,-57.5350579590648,
0.));
#136514=CARTESIAN_POINT('Ctrl Pts',(-41.7353878481336,-57.5350579590648,
12.));
#136515=CARTESIAN_POINT('Ctrl Pts',(-41.7175383153819,-57.5219819714169,
0.));
#136516=CARTESIAN_POINT('Ctrl Pts',(-41.7175383153819,-57.5219819714169,
12.));
#136517=CARTESIAN_POINT('Ctrl Pts',(-41.6997399955445,-57.5089156412341,
0.));
#136518=CARTESIAN_POINT('Ctrl Pts',(-41.6997399955445,-57.5089156412341,
12.));
#136519=CARTESIAN_POINT('Ctrl Pts',(-41.6819929638797,-57.4958591135165,
0.));
#136520=CARTESIAN_POINT('Ctrl Pts',(-41.6819929638797,-57.4958591135165,
12.));
#136521=CARTESIAN_POINT('Ctrl Pts',(-41.6642972959168,-57.4828125340222,
0.));
#136522=CARTESIAN_POINT('Ctrl Pts',(-41.6642972959168,-57.4828125340222,
12.));
#136523=CARTESIAN_POINT('Ctrl Pts',(-41.6466530674522,-57.4697760492693,
0.));
#136524=CARTESIAN_POINT('Ctrl Pts',(-41.6466530674522,-57.4697760492693,
12.));
#136525=CARTESIAN_POINT('Ctrl Pts',(-41.6290603545674,-57.4567498065573,
0.));
#136526=CARTESIAN_POINT('Ctrl Pts',(-41.6290603545674,-57.4567498065573,
12.));
#136527=CARTESIAN_POINT('Ctrl Pts',(-41.6115192336393,-57.4437339539848,
0.));
#136528=CARTESIAN_POINT('Ctrl Pts',(-41.6115192336393,-57.4437339539848,
12.));
#136529=CARTESIAN_POINT('Ctrl Pts',(-41.5940297813474,-57.4307286404656,
0.));
#136530=CARTESIAN_POINT('Ctrl Pts',(-41.5940297813474,-57.4307286404656,
12.));
#136531=CARTESIAN_POINT('Ctrl Pts',(-41.5765920746764,-57.417734015749,
0.));
#136532=CARTESIAN_POINT('Ctrl Pts',(-41.5765920746764,-57.417734015749,
12.));
#136533=CARTESIAN_POINT('Ctrl Pts',(-41.5592061909159,-57.4047502304207,
0.));
#136534=CARTESIAN_POINT('Ctrl Pts',(-41.5592061909159,-57.4047502304207,
12.));
#136535=CARTESIAN_POINT('Ctrl Pts',(-41.5418722076558,-57.3917774358844,
0.));
#136536=CARTESIAN_POINT('Ctrl Pts',(-41.5418722076558,-57.3917774358844,
12.));
#136537=CARTESIAN_POINT('Ctrl Pts',(-41.5245902027767,-57.378815784345,
0.));
#136538=CARTESIAN_POINT('Ctrl Pts',(-41.5245902027767,-57.378815784345,
12.));
#136539=CARTESIAN_POINT('Ctrl Pts',(-41.5073602544404,-57.3658654287948,
0.));
#136540=CARTESIAN_POINT('Ctrl Pts',(-41.5073602544404,-57.3658654287948,
12.));
#136541=CARTESIAN_POINT('Ctrl Pts',(-41.4901824410654,-57.3529265229858,
0.));
#136542=CARTESIAN_POINT('Ctrl Pts',(-41.4901824410654,-57.3529265229858,
12.));
#136543=CARTESIAN_POINT('Ctrl Pts',(-41.4730568413535,-57.339999221474,
0.));
#136544=CARTESIAN_POINT('Ctrl Pts',(-41.4730568413535,-57.339999221474,
12.));
#136545=CARTESIAN_POINT('Ctrl Pts',(-41.4559835343338,-57.3270836796925,
0.));
#136546=CARTESIAN_POINT('Ctrl Pts',(-41.4559835343338,-57.3270836796925,
12.));
#136547=CARTESIAN_POINT('Ctrl Pts',(-41.4389625993948,-57.3141800540137,
0.));
#136548=CARTESIAN_POINT('Ctrl Pts',(-41.4389625993948,-57.3141800540137,
12.));
#136549=CARTESIAN_POINT('Ctrl Pts',(-41.4219941163154,-57.3012885018139,
0.));
#136550=CARTESIAN_POINT('Ctrl Pts',(-41.4219941163154,-57.3012885018139,
12.));
#136551=CARTESIAN_POINT('Ctrl Pts',(-41.4050781652923,-57.2884091815385,
0.));
#136552=CARTESIAN_POINT('Ctrl Pts',(-41.4050781652923,-57.2884091815385,
12.));
#136553=CARTESIAN_POINT('Ctrl Pts',(-41.3882148268798,-57.2755422525822,
0.));
#136554=CARTESIAN_POINT('Ctrl Pts',(-41.3882148268798,-57.2755422525822,
12.));
#136555=CARTESIAN_POINT('Ctrl Pts',(-41.3714041819215,-57.2626878751584,
0.));
#136556=CARTESIAN_POINT('Ctrl Pts',(-41.3714041819215,-57.2626878751584,
12.));
#136557=CARTESIAN_POINT('Ctrl Pts',(-41.3546463114889,-57.2498462101883,
0.));
#136558=CARTESIAN_POINT('Ctrl Pts',(-41.3546463114889,-57.2498462101883,
12.));
#136559=CARTESIAN_POINT('Ctrl Pts',(-41.3379412967889,-57.237017419142,
0.));
#136560=CARTESIAN_POINT('Ctrl Pts',(-41.3379412967889,-57.237017419142,
12.));
#136561=CARTESIAN_POINT('Ctrl Pts',(-41.321289219151,-57.2242016640226,
0.));
#136562=CARTESIAN_POINT('Ctrl Pts',(-41.321289219151,-57.2242016640226,
12.));
#136563=CARTESIAN_POINT('Ctrl Pts',(-41.304690160231,-57.2113991077325,
0.));
#136564=CARTESIAN_POINT('Ctrl Pts',(-41.304690160231,-57.2113991077325,
12.));
#136565=CARTESIAN_POINT('Ctrl Pts',(-41.2881442021869,-57.1986099143992,
0.));
#136566=CARTESIAN_POINT('Ctrl Pts',(-41.2881442021869,-57.1986099143992,
12.));
#136567=CARTESIAN_POINT('Ctrl Pts',(-41.2716514278268,-57.1858342496526,
0.));
#136568=CARTESIAN_POINT('Ctrl Pts',(-41.2716514278268,-57.1858342496526,
12.));
#136569=CARTESIAN_POINT('Ctrl Pts',(-41.2552119208445,-57.1730722810771,
0.));
#136570=CARTESIAN_POINT('Ctrl Pts',(-41.2552119208445,-57.1730722810771,
12.));
#136571=CARTESIAN_POINT('Ctrl Pts',(-41.2388257656534,-57.1603241779042,
0.));
#136572=CARTESIAN_POINT('Ctrl Pts',(-41.2388257656534,-57.1603241779042,
12.));
#136573=CARTESIAN_POINT('Ctrl Pts',(-41.2224930469412,-57.1475901101795,
0.));
#136574=CARTESIAN_POINT('Ctrl Pts',(-41.2224930469412,-57.1475901101795,
12.));
#136575=CARTESIAN_POINT('Ctrl Pts',(-41.2062138492913,-57.1348702480644,
0.));
#136576=CARTESIAN_POINT('Ctrl Pts',(-41.2062138492913,-57.1348702480644,
12.));
#136577=CARTESIAN_POINT('Ctrl Pts',(-41.1899882567941,-57.1221647611231,
0.));
#136578=CARTESIAN_POINT('Ctrl Pts',(-41.1899882567941,-57.1221647611231,
12.));
#136579=CARTESIAN_POINT('Ctrl Pts',(-41.1738163525931,-57.1094738174998,
0.));
#136580=CARTESIAN_POINT('Ctrl Pts',(-41.1738163525931,-57.1094738174998,
12.));
#136581=CARTESIAN_POINT('Ctrl Pts',(-41.1576982197402,-57.0967975854912,
0.));
#136582=CARTESIAN_POINT('Ctrl Pts',(-41.1576982197402,-57.0967975854912,
12.));
#136583=CARTESIAN_POINT('Ctrl Pts',(-41.1416339422132,-57.0841362354281,
0.));
#136584=CARTESIAN_POINT('Ctrl Pts',(-41.1416339422132,-57.0841362354281,
12.));
#136585=CARTESIAN_POINT('Ctrl Pts',(-41.1256236057436,-57.0714899412091,
0.));
#136586=CARTESIAN_POINT('Ctrl Pts',(-41.1256236057436,-57.0714899412091,
12.));
#136587=CARTESIAN_POINT('Ctrl Pts',(-41.1096672990125,-57.0588588825266,
0.));
#136588=CARTESIAN_POINT('Ctrl Pts',(-41.1096672990125,-57.0588588825266,
12.));
#136589=CARTESIAN_POINT('Ctrl Pts',(-41.0937651137519,-57.0462432450637,
0.));
#136590=CARTESIAN_POINT('Ctrl Pts',(-41.0937651137519,-57.0462432450637,
12.));
#136591=CARTESIAN_POINT('Ctrl Pts',(-41.0779171422415,-57.0336432158503,
0.));
#136592=CARTESIAN_POINT('Ctrl Pts',(-41.0779171422415,-57.0336432158503,
12.));
#136593=CARTESIAN_POINT('Ctrl Pts',(-41.0621234751,-57.0210589791777,0.));
#136594=CARTESIAN_POINT('Ctrl Pts',(-41.0621234751,-57.0210589791777,12.));
#136595=CARTESIAN_POINT('Ctrl Pts',(-41.0463841993622,-57.008490713044,
0.));
#136596=CARTESIAN_POINT('Ctrl Pts',(-41.0463841993622,-57.008490713044,
12.));
#136597=CARTESIAN_POINT('Ctrl Pts',(-41.0306993954021,-56.9959385834768,
0.));
#136598=CARTESIAN_POINT('Ctrl Pts',(-41.0306993954021,-56.9959385834768,
12.));
#136599=CARTESIAN_POINT('Ctrl Pts',(-41.0150691398988,-56.9834027500178,
0.));
#136600=CARTESIAN_POINT('Ctrl Pts',(-41.0150691398988,-56.9834027500178,
12.));
#136601=CARTESIAN_POINT('Ctrl Pts',(-40.9994935117307,-56.9708833766183,
0.));
#136602=CARTESIAN_POINT('Ctrl Pts',(-40.9994935117307,-56.9708833766183,
12.));
#136603=CARTESIAN_POINT('Ctrl Pts',(-40.9839725967121,-56.9583806404069,
0.));
#136604=CARTESIAN_POINT('Ctrl Pts',(-40.9839725967121,-56.9583806404069,
12.));
#136605=CARTESIAN_POINT('Ctrl Pts',(-40.968506493303,-56.9458947422541,
0.));
#136606=CARTESIAN_POINT('Ctrl Pts',(-40.968506493303,-56.9458947422541,
12.));
#136607=CARTESIAN_POINT('Ctrl Pts',(-40.9530953164952,-56.9334259139928,
0.));
#136608=CARTESIAN_POINT('Ctrl Pts',(-40.9530953164952,-56.9334259139928,
12.));
#136609=CARTESIAN_POINT('Ctrl Pts',(-40.9377391857044,-56.9209743960861,
0.));
#136610=CARTESIAN_POINT('Ctrl Pts',(-40.9377391857044,-56.9209743960861,
12.));
#136611=CARTESIAN_POINT('Ctrl Pts',(-40.9224382132382,-56.9085404164432,
0.));
#136612=CARTESIAN_POINT('Ctrl Pts',(-40.9224382132382,-56.9085404164432,
12.));
#136613=CARTESIAN_POINT('Ctrl Pts',(-40.9071924937551,-56.8961241708926,
0.));
#136614=CARTESIAN_POINT('Ctrl Pts',(-40.9071924937551,-56.8961241708926,
12.));
#136615=CARTESIAN_POINT('Ctrl Pts',(-40.8920020903443,-56.8837257978574,
0.));
#136616=CARTESIAN_POINT('Ctrl Pts',(-40.8920020903443,-56.8837257978574,
12.));
#136617=CARTESIAN_POINT('Ctrl Pts',(-40.8768670342278,-56.8713453765252,
0.));
#136618=CARTESIAN_POINT('Ctrl Pts',(-40.8768670342278,-56.8713453765252,
12.));
#136619=CARTESIAN_POINT('Ctrl Pts',(-40.8648032759631,-56.8614554317993,
0.));
#136620=CARTESIAN_POINT('Ctrl Pts',(-40.8648032759631,-56.8614554317993,
12.));
#136621=CARTESIAN_POINT('Ctrl Pts',(-40.8557803680411,-56.8540460739677,
0.));
#136622=CARTESIAN_POINT('Ctrl Pts',(-40.8557803680411,-56.8540460739677,
12.));
#136623=CARTESIAN_POINT('Ctrl Pts',(-40.8497761671086,-56.8491101022668,
0.));
#136624=CARTESIAN_POINT('Ctrl Pts',(-40.8497761671086,-56.8491101022668,
12.));
#136625=CARTESIAN_POINT('Ctrl Pts',(-40.8467768343956,-56.8466430164621,
0.));
#136626=CARTESIAN_POINT('Ctrl Pts',(-40.8467768343956,-56.8466430164621,
12.));
#136627=CARTESIAN_POINT('',(-40.8467768343956,-56.8466430164621,12.));
#136628=CARTESIAN_POINT('Ctrl Pts',(-40.8467768343956,-56.8466430164621,
12.));
#136629=CARTESIAN_POINT('Ctrl Pts',(-40.8497761671086,-56.8491101022668,
12.));
#136630=CARTESIAN_POINT('Ctrl Pts',(-40.8557803680411,-56.8540460739677,
12.));
#136631=CARTESIAN_POINT('Ctrl Pts',(-40.8648032759631,-56.8614554317993,
12.));
#136632=CARTESIAN_POINT('Ctrl Pts',(-40.8768670342278,-56.8713453765252,
12.));
#136633=CARTESIAN_POINT('Ctrl Pts',(-40.8920020903443,-56.8837257978574,
12.));
#136634=CARTESIAN_POINT('Ctrl Pts',(-40.9071924937551,-56.8961241708926,
12.));
#136635=CARTESIAN_POINT('Ctrl Pts',(-40.9224382132382,-56.9085404164432,
12.));
#136636=CARTESIAN_POINT('Ctrl Pts',(-40.9377391857044,-56.9209743960861,
12.));
#136637=CARTESIAN_POINT('Ctrl Pts',(-40.9530953164952,-56.9334259139928,
12.));
#136638=CARTESIAN_POINT('Ctrl Pts',(-40.968506493303,-56.9458947422541,
12.));
#136639=CARTESIAN_POINT('Ctrl Pts',(-40.9839725967121,-56.9583806404069,
12.));
#136640=CARTESIAN_POINT('Ctrl Pts',(-40.9994935117307,-56.9708833766183,
12.));
#136641=CARTESIAN_POINT('Ctrl Pts',(-41.0150691398988,-56.9834027500178,
12.));
#136642=CARTESIAN_POINT('Ctrl Pts',(-41.0306993954021,-56.9959385834768,
12.));
#136643=CARTESIAN_POINT('Ctrl Pts',(-41.0463841993622,-57.008490713044,
12.));
#136644=CARTESIAN_POINT('Ctrl Pts',(-41.0621234751,-57.0210589791777,12.));
#136645=CARTESIAN_POINT('Ctrl Pts',(-41.0779171422415,-57.0336432158503,
12.));
#136646=CARTESIAN_POINT('Ctrl Pts',(-41.0937651137519,-57.0462432450637,
12.));
#136647=CARTESIAN_POINT('Ctrl Pts',(-41.1096672990125,-57.0588588825266,
12.));
#136648=CARTESIAN_POINT('Ctrl Pts',(-41.1256236057436,-57.0714899412091,
12.));
#136649=CARTESIAN_POINT('Ctrl Pts',(-41.1416339422132,-57.0841362354281,
12.));
#136650=CARTESIAN_POINT('Ctrl Pts',(-41.1576982197402,-57.0967975854912,
12.));
#136651=CARTESIAN_POINT('Ctrl Pts',(-41.1738163525931,-57.1094738174998,
12.));
#136652=CARTESIAN_POINT('Ctrl Pts',(-41.1899882567941,-57.1221647611231,
12.));
#136653=CARTESIAN_POINT('Ctrl Pts',(-41.2062138492913,-57.1348702480644,
12.));
#136654=CARTESIAN_POINT('Ctrl Pts',(-41.2224930469412,-57.1475901101795,
12.));
#136655=CARTESIAN_POINT('Ctrl Pts',(-41.2388257656534,-57.1603241779042,
12.));
#136656=CARTESIAN_POINT('Ctrl Pts',(-41.2552119208445,-57.1730722810771,
12.));
#136657=CARTESIAN_POINT('Ctrl Pts',(-41.2716514278268,-57.1858342496526,
12.));
#136658=CARTESIAN_POINT('Ctrl Pts',(-41.2881442021869,-57.1986099143992,
12.));
#136659=CARTESIAN_POINT('Ctrl Pts',(-41.304690160231,-57.2113991077325,
12.));
#136660=CARTESIAN_POINT('Ctrl Pts',(-41.321289219151,-57.2242016640226,
12.));
#136661=CARTESIAN_POINT('Ctrl Pts',(-41.3379412967889,-57.237017419142,
12.));
#136662=CARTESIAN_POINT('Ctrl Pts',(-41.3546463114889,-57.2498462101883,
12.));
#136663=CARTESIAN_POINT('Ctrl Pts',(-41.3714041819215,-57.2626878751584,
12.));
#136664=CARTESIAN_POINT('Ctrl Pts',(-41.3882148268798,-57.2755422525822,
12.));
#136665=CARTESIAN_POINT('Ctrl Pts',(-41.4050781652923,-57.2884091815385,
12.));
#136666=CARTESIAN_POINT('Ctrl Pts',(-41.4219941163154,-57.3012885018139,
12.));
#136667=CARTESIAN_POINT('Ctrl Pts',(-41.4389625993948,-57.3141800540137,
12.));
#136668=CARTESIAN_POINT('Ctrl Pts',(-41.4559835343338,-57.3270836796925,
12.));
#136669=CARTESIAN_POINT('Ctrl Pts',(-41.4730568413535,-57.339999221474,
12.));
#136670=CARTESIAN_POINT('Ctrl Pts',(-41.4901824410654,-57.3529265229858,
12.));
#136671=CARTESIAN_POINT('Ctrl Pts',(-41.5073602544404,-57.3658654287948,
12.));
#136672=CARTESIAN_POINT('Ctrl Pts',(-41.5245902027767,-57.378815784345,
12.));
#136673=CARTESIAN_POINT('Ctrl Pts',(-41.5418722076558,-57.3917774358844,
12.));
#136674=CARTESIAN_POINT('Ctrl Pts',(-41.5592061909159,-57.4047502304207,
12.));
#136675=CARTESIAN_POINT('Ctrl Pts',(-41.5765920746764,-57.417734015749,
12.));
#136676=CARTESIAN_POINT('Ctrl Pts',(-41.5940297813474,-57.4307286404656,
12.));
#136677=CARTESIAN_POINT('Ctrl Pts',(-41.6115192336393,-57.4437339539848,
12.));
#136678=CARTESIAN_POINT('Ctrl Pts',(-41.6290603545674,-57.4567498065573,
12.));
#136679=CARTESIAN_POINT('Ctrl Pts',(-41.6466530674522,-57.4697760492693,
12.));
#136680=CARTESIAN_POINT('Ctrl Pts',(-41.6642972959168,-57.4828125340222,
12.));
#136681=CARTESIAN_POINT('Ctrl Pts',(-41.6819929638797,-57.4958591135165,
12.));
#136682=CARTESIAN_POINT('Ctrl Pts',(-41.6997399955445,-57.5089156412341,
12.));
#136683=CARTESIAN_POINT('Ctrl Pts',(-41.7175383153819,-57.5219819714169,
12.));
#136684=CARTESIAN_POINT('Ctrl Pts',(-41.7353878481336,-57.5350579590648,
12.));
#136685=CARTESIAN_POINT('Ctrl Pts',(-41.7532885188174,-57.5481434599334,
12.));
#136686=CARTESIAN_POINT('Ctrl Pts',(-41.7712402527273,-57.561238330532,
12.));
#136687=CARTESIAN_POINT('Ctrl Pts',(-41.7892429754298,-57.5743424281204,
12.));
#136688=CARTESIAN_POINT('Ctrl Pts',(-41.8072966127559,-57.5874556107054,
12.));
#136689=CARTESIAN_POINT('Ctrl Pts',(-41.8254010908051,-57.6005777370347,
12.));
#136690=CARTESIAN_POINT('Ctrl Pts',(-41.8435563359456,-57.613708666588,
12.));
#136691=CARTESIAN_POINT('Ctrl Pts',(-41.8617622748107,-57.6268482595701,
12.));
#136692=CARTESIAN_POINT('Ctrl Pts',(-41.8800188342912,-57.6399963769009,
12.));
#136693=CARTESIAN_POINT('Ctrl Pts',(-41.8983259415253,-57.6531528802072,
12.));
#136694=CARTESIAN_POINT('Ctrl Pts',(-41.9166835239054,-57.6663176318189,
12.));
#136695=CARTESIAN_POINT('Ctrl Pts',(-41.9350915090796,-57.6794904947649,
12.));
#136696=CARTESIAN_POINT('Ctrl Pts',(-41.9535498249488,-57.6926713327672,
12.));
#136697=CARTESIAN_POINT('Ctrl Pts',(-41.9720583996592,-57.7058600102351,
12.));
#136698=CARTESIAN_POINT('Ctrl Pts',(-41.990617161596,-57.7190563922593,
12.));
#136699=CARTESIAN_POINT('Ctrl Pts',(-42.0092260393897,-57.7322603446066,
12.));
#136700=CARTESIAN_POINT('Ctrl Pts',(-42.0278849619148,-57.745471733714,
12.));
#136701=CARTESIAN_POINT('Ctrl Pts',(-42.0465938582882,-57.7586904266834,
12.));
#136702=CARTESIAN_POINT('Ctrl Pts',(-42.0653526578588,-57.7719162912744,
12.));
#136703=CARTESIAN_POINT('Ctrl Pts',(-42.0841612902042,-57.7851491958987,
12.));
#136704=CARTESIAN_POINT('Ctrl Pts',(-42.1030196851366,-57.798389009616,
12.));
#136705=CARTESIAN_POINT('Ctrl Pts',(-42.1219277727021,-57.8116356021288,
12.));
#136706=CARTESIAN_POINT('Ctrl Pts',(-42.1408854831783,-57.8248888437775,
12.));
#136707=CARTESIAN_POINT('Ctrl Pts',(-42.1598927470646,-57.8381486055342,
12.));
#136708=CARTESIAN_POINT('Ctrl Pts',(-42.1789494950794,-57.8514147589972,
12.));
#136709=CARTESIAN_POINT('Ctrl Pts',(-42.1980556581665,-57.864687176387,
12.));
#136710=CARTESIAN_POINT('Ctrl Pts',(-42.2172111674938,-57.8779657305413,
12.));
#136711=CARTESIAN_POINT('Ctrl Pts',(-42.2364159544501,-57.8912502949096,
12.));
#136712=CARTESIAN_POINT('Ctrl Pts',(-42.2556699506353,-57.9045407435474,
12.));
#136713=CARTESIAN_POINT('Ctrl Pts',(-42.2749730878594,-57.9178369511114,
12.));
#136714=CARTESIAN_POINT('Ctrl Pts',(-42.2943252981489,-57.9311387928563,
12.));
#136715=CARTESIAN_POINT('Ctrl Pts',(-42.3137265137452,-57.9444461446299,
12.));
#136716=CARTESIAN_POINT('Ctrl Pts',(-42.333176667102,-57.9577588828682,
12.));
#136717=CARTESIAN_POINT('Ctrl Pts',(-42.3526756908746,-57.9710768845899,
12.));
#136718=CARTESIAN_POINT('Ctrl Pts',(-42.3722235179197,-57.9844000273911,
12.));
#136719=CARTESIAN_POINT('Ctrl Pts',(-42.3918200813014,-57.9977281894422,
12.));
#136720=CARTESIAN_POINT('Ctrl Pts',(-42.411465314289,-58.0110612494828,
12.));
#136721=CARTESIAN_POINT('Ctrl Pts',(-42.4311591503555,-58.0243990868181,
12.));
#136722=CARTESIAN_POINT('Ctrl Pts',(-42.4509015231674,-58.037741581314,
12.));
#136723=CARTESIAN_POINT('Ctrl Pts',(-42.4706923665845,-58.0510886133926,
12.));
#136724=CARTESIAN_POINT('Ctrl Pts',(-42.4905316146653,-58.0644400640275,
12.));
#136725=CARTESIAN_POINT('Ctrl Pts',(-42.5104192016664,-58.0777958147403,
12.));
#136726=CARTESIAN_POINT('Ctrl Pts',(-42.5303550620387,-58.0911557475965,
12.));
#136727=CARTESIAN_POINT('Ctrl Pts',(-42.5503391304183,-58.1045197452002,
12.));
#136728=CARTESIAN_POINT('Ctrl Pts',(-42.5703713416265,-58.1178876906907,
12.));
#136729=CARTESIAN_POINT('Ctrl Pts',(-42.5904516306762,-58.1312594677386,
12.));
#136730=CARTESIAN_POINT('Ctrl Pts',(-42.6105799327699,-58.1446349605421,
12.));
#136731=CARTESIAN_POINT('Ctrl Pts',(-42.6307561832976,-58.1580140538228,
12.));
#136732=CARTESIAN_POINT('Ctrl Pts',(-42.6509803178265,-58.171396632821,
12.));
#136733=CARTESIAN_POINT('Ctrl Pts',(-42.6712522721016,-58.1847825832923,
12.));
#136734=CARTESIAN_POINT('Ctrl Pts',(-42.6915719820513,-58.1981717915037,
12.));
#136735=CARTESIAN_POINT('Ctrl Pts',(-42.7119393837866,-58.21156414423,12.));
#136736=CARTESIAN_POINT('Ctrl Pts',(-42.7323544135985,-58.22495952875,12.));
#136737=CARTESIAN_POINT('Ctrl Pts',(-42.7528170079484,-58.2383578328424,
12.));
#136738=CARTESIAN_POINT('Ctrl Pts',(-42.7733271034679,-58.251758944782,
12.));
#136739=CARTESIAN_POINT('Ctrl Pts',(-42.7938846369651,-58.2651627533368,
12.));
#136740=CARTESIAN_POINT('Ctrl Pts',(-42.8144895454233,-58.2785691477638,
12.));
#136741=CARTESIAN_POINT('Ctrl Pts',(-42.8351417659999,-58.2919780178064,
12.));
#136742=CARTESIAN_POINT('Ctrl Pts',(-42.8558412360158,-58.3053892536894,
12.));
#136743=CARTESIAN_POINT('Ctrl Pts',(-42.8765878929551,-58.3188027461164,
12.));
#136744=CARTESIAN_POINT('Ctrl Pts',(-42.8973816744709,-58.3322183862654,
12.));
#136745=CARTESIAN_POINT('Ctrl Pts',(-42.9182225183855,-58.3456360657865,
12.));
#136746=CARTESIAN_POINT('Ctrl Pts',(-42.9391103626879,-58.3590556767978,
12.));
#136747=CARTESIAN_POINT('Ctrl Pts',(-42.960045145526,-58.3724771118826,
12.));
#136748=CARTESIAN_POINT('Ctrl Pts',(-42.9810268052032,-58.3859002640856,
12.));
#136749=CARTESIAN_POINT('Ctrl Pts',(-43.0020552801859,-58.3993250269101,
12.));
#136750=CARTESIAN_POINT('Ctrl Pts',(-43.0231305091027,-58.4127512943136,
12.));
#136751=CARTESIAN_POINT('Ctrl Pts',(-43.0442524307434,-58.4261789607058,
12.));
#136752=CARTESIAN_POINT('Ctrl Pts',(-43.0654209840511,-58.439607920945,
12.));
#136753=CARTESIAN_POINT('Ctrl Pts',(-43.0866361081177,-58.4530380703348,
12.));
#136754=CARTESIAN_POINT('Ctrl Pts',(-43.1078977421916,-58.4664693046217,
12.));
#136755=CARTESIAN_POINT('Ctrl Pts',(-43.1292058256777,-58.4799015199907,
12.));
#136756=CARTESIAN_POINT('Ctrl Pts',(-43.1505602981365,-58.4933346130636,
12.));
#136757=CARTESIAN_POINT('Ctrl Pts',(-43.1719610992771,-58.5067684808944,
12.));
#136758=CARTESIAN_POINT('Ctrl Pts',(-43.1934081689505,-58.5202030209669,
12.));
#136759=CARTESIAN_POINT('Ctrl Pts',(-43.2149014471574,-58.5336381311917,
12.));
#136760=CARTESIAN_POINT('Ctrl Pts',(-43.2364408740493,-58.5470737099032,
12.));
#136761=CARTESIAN_POINT('Ctrl Pts',(-43.2580263899278,-58.5605096558578,
12.));
#136762=CARTESIAN_POINT('Ctrl Pts',(-43.27965793524,-58.573945868231,12.));
#136763=CARTESIAN_POINT('Ctrl Pts',(-43.3013354505701,-58.5873822466152,
12.));
#136764=CARTESIAN_POINT('Ctrl Pts',(-43.3230588766449,-58.6008186910156,
12.));
#136765=CARTESIAN_POINT('Ctrl Pts',(-43.3448281543371,-58.6142551018467,
12.));
#136766=CARTESIAN_POINT('Ctrl Pts',(-43.3666432246635,-58.627691379929,
12.));
#136767=CARTESIAN_POINT('Ctrl Pts',(-43.388504028781,-58.6411274264857,
12.));
#136768=CARTESIAN_POINT('Ctrl Pts',(-43.4104105079768,-58.6545631431393,
12.));
#136769=CARTESIAN_POINT('Ctrl Pts',(-43.4323626036737,-58.6679984319097,
12.));
#136770=CARTESIAN_POINT('Ctrl Pts',(-43.4543602574351,-58.6814331952138,
12.));
#136771=CARTESIAN_POINT('Ctrl Pts',(-43.4764034109654,-58.6948673358638,
12.));
#136772=CARTESIAN_POINT('Ctrl Pts',(-43.4984920061073,-58.7083007570661,
12.));
#136773=CARTESIAN_POINT('Ctrl Pts',(-43.5206259848337,-58.7217333624209,
12.));
#136774=CARTESIAN_POINT('Ctrl Pts',(-43.5428052892488,-58.735165055918,
12.));
#136775=CARTESIAN_POINT('Ctrl Pts',(-43.5650298615917,-58.74859574193,12.));
#136776=CARTESIAN_POINT('Ctrl Pts',(-43.5872996442345,-58.7620253252062,
12.));
#136777=CARTESIAN_POINT('Ctrl Pts',(-43.6096145796797,-58.775453710867,
12.));
#136778=CARTESIAN_POINT('Ctrl Pts',(-43.6319746105482,-58.788880804397,
12.));
#136779=CARTESIAN_POINT('Ctrl Pts',(-43.6543796795789,-58.8023065116436,
12.));
#136780=CARTESIAN_POINT('Ctrl Pts',(-43.6768297296395,-58.8157307388238,
12.));
#136781=CARTESIAN_POINT('Ctrl Pts',(-43.6993247037314,-58.8291533925293,
12.));
#136782=CARTESIAN_POINT('Ctrl Pts',(-43.7218645449922,-58.8425743797326,
12.));
#136783=CARTESIAN_POINT('Ctrl Pts',(-43.7444491966942,-58.855993607794,
12.));
#136784=CARTESIAN_POINT('Ctrl Pts',(-43.7670786022402,-58.8694109844648,
12.));
#136785=CARTESIAN_POINT('Ctrl Pts',(-43.7897527051609,-58.8828264178621,
12.));
#136786=CARTESIAN_POINT('Ctrl Pts',(-43.8124714491076,-58.8962398164493,
12.));
#136787=CARTESIAN_POINT('Ctrl Pts',(-43.835234777842,-58.9096510890129,
12.));
#136788=CARTESIAN_POINT('Ctrl Pts',(-43.858042635223,-58.9230601446436,
12.));
#136789=CARTESIAN_POINT('Ctrl Pts',(-43.8808949651873,-58.936466892712,
12.));
#136790=CARTESIAN_POINT('Ctrl Pts',(-43.9037917117739,-58.9498712429054,
12.));
#136791=CARTESIAN_POINT('Ctrl Pts',(-43.9267328191501,-58.9632731052696,
12.));
#136792=CARTESIAN_POINT('Ctrl Pts',(-43.9497182316331,-58.9766723902529,
12.));
#136793=CARTESIAN_POINT('Ctrl Pts',(-43.9727478937056,-58.9900690087408,
12.));
#136794=CARTESIAN_POINT('Ctrl Pts',(-43.9958217500369,-59.0034628721168,
12.));
#136795=CARTESIAN_POINT('Ctrl Pts',(-44.0189397454599,-59.0168538922095,
12.));
#136796=CARTESIAN_POINT('Ctrl Pts',(-44.0421018249223,-59.0302419811777,
12.));
#136797=CARTESIAN_POINT('Ctrl Pts',(-44.0653079334385,-59.0436270514087,
12.));
#136798=CARTESIAN_POINT('Ctrl Pts',(-44.0885580160432,-59.0570090154243,
12.));
#136799=CARTESIAN_POINT('Ctrl Pts',(-44.1118520177221,-59.0703877857526,
12.));
#136800=CARTESIAN_POINT('Ctrl Pts',(-44.1351898834051,-59.08376327492,12.));
#136801=CARTESIAN_POINT('Ctrl Pts',(-44.1585715581064,-59.0971353957206,
12.));
#136802=CARTESIAN_POINT('Ctrl Pts',(-44.1819969870307,-59.1105040614276,
12.));
#136803=CARTESIAN_POINT('Ctrl Pts',(-44.2054661156875,-59.1238691860306,
12.));
#136804=CARTESIAN_POINT('Ctrl Pts',(-44.228978889997,-59.1372306844586,
12.));
#136805=CARTESIAN_POINT('Ctrl Pts',(-44.2525352563996,-59.1505884728215,
12.));
#136806=CARTESIAN_POINT('Ctrl Pts',(-44.2761351616048,-59.1639424678793,
12.));
#136807=CARTESIAN_POINT('Ctrl Pts',(-44.2997785523431,-59.1772925865213,
12.));
#136808=CARTESIAN_POINT('Ctrl Pts',(-44.3234653750884,-59.1906387451979,
12.));
#136809=CARTESIAN_POINT('Ctrl Pts',(-44.3471955758403,-59.2039808594752,
12.));
#136810=CARTESIAN_POINT('Ctrl Pts',(-44.3709690997469,-59.2173188432798,
12.));
#136811=CARTESIAN_POINT('Ctrl Pts',(-44.3947858914074,-59.2306526095131,
12.));
#136812=CARTESIAN_POINT('Ctrl Pts',(-44.4186458955451,-59.2439820714187,
12.));
#136813=CARTESIAN_POINT('Ctrl Pts',(-44.4425490575911,-59.2573071437774,
12.));
#136814=CARTESIAN_POINT('Ctrl Pts',(-44.4664953242379,-59.2706277440445,
12.));
#136815=CARTESIAN_POINT('Ctrl Pts',(-44.490484644151,-59.2839437938237,
12.));
#136816=CARTESIAN_POINT('Ctrl Pts',(-44.5145169681349,-59.2972552192156,
12.));
#136817=CARTESIAN_POINT('Ctrl Pts',(-44.5351541478479,-59.3086616639523,
12.));
#136818=CARTESIAN_POINT('Ctrl Pts',(-44.5509994358154,-59.3174041872347,
12.));
#136819=CARTESIAN_POINT('Ctrl Pts',(-44.5620338188738,-59.3234848865455,
12.));
#136820=CARTESIAN_POINT('Ctrl Pts',(-44.5682447396021,-59.3269051738423,
12.));
#136821=CARTESIAN_POINT('Ctrl Pts',(-44.5696260757792,-59.3276657444392,
12.));
#136822=CARTESIAN_POINT('',(-40.8467768343956,-56.8466430164621,0.));
#136823=CARTESIAN_POINT('',(-40.8467768343956,-56.8466430164621,0.));
#136824=CARTESIAN_POINT('Ctrl Pts',(-44.5696260757791,-59.3276657444392,
0.));
#136825=CARTESIAN_POINT('Ctrl Pts',(-44.5682447396021,-59.3269051738423,
0.));
#136826=CARTESIAN_POINT('Ctrl Pts',(-44.5620338188738,-59.3234848865455,
0.));
#136827=CARTESIAN_POINT('Ctrl Pts',(-44.5509994358154,-59.3174041872347,
0.));
#136828=CARTESIAN_POINT('Ctrl Pts',(-44.5351541478479,-59.3086616639523,
0.));
#136829=CARTESIAN_POINT('Ctrl Pts',(-44.5145169681349,-59.2972552192156,
0.));
#136830=CARTESIAN_POINT('Ctrl Pts',(-44.490484644151,-59.2839437938237,
0.));
#136831=CARTESIAN_POINT('Ctrl Pts',(-44.4664953242379,-59.2706277440445,
0.));
#136832=CARTESIAN_POINT('Ctrl Pts',(-44.4425490575911,-59.2573071437774,
0.));
#136833=CARTESIAN_POINT('Ctrl Pts',(-44.4186458955451,-59.2439820714187,
0.));
#136834=CARTESIAN_POINT('Ctrl Pts',(-44.3947858914074,-59.2306526095131,
0.));
#136835=CARTESIAN_POINT('Ctrl Pts',(-44.3709690997469,-59.2173188432798,
0.));
#136836=CARTESIAN_POINT('Ctrl Pts',(-44.3471955758403,-59.2039808594752,
0.));
#136837=CARTESIAN_POINT('Ctrl Pts',(-44.3234653750884,-59.1906387451979,
0.));
#136838=CARTESIAN_POINT('Ctrl Pts',(-44.2997785523431,-59.1772925865213,
0.));
#136839=CARTESIAN_POINT('Ctrl Pts',(-44.2761351616048,-59.1639424678793,
0.));
#136840=CARTESIAN_POINT('Ctrl Pts',(-44.2525352563996,-59.1505884728215,
0.));
#136841=CARTESIAN_POINT('Ctrl Pts',(-44.228978889997,-59.1372306844586,
0.));
#136842=CARTESIAN_POINT('Ctrl Pts',(-44.2054661156875,-59.1238691860306,
0.));
#136843=CARTESIAN_POINT('Ctrl Pts',(-44.1819969870307,-59.1105040614276,
0.));
#136844=CARTESIAN_POINT('Ctrl Pts',(-44.1585715581064,-59.0971353957206,
0.));
#136845=CARTESIAN_POINT('Ctrl Pts',(-44.1351898834051,-59.08376327492,0.));
#136846=CARTESIAN_POINT('Ctrl Pts',(-44.1118520177221,-59.0703877857526,
0.));
#136847=CARTESIAN_POINT('Ctrl Pts',(-44.0885580160432,-59.0570090154243,
0.));
#136848=CARTESIAN_POINT('Ctrl Pts',(-44.0653079334385,-59.0436270514087,
0.));
#136849=CARTESIAN_POINT('Ctrl Pts',(-44.0421018249223,-59.0302419811777,
0.));
#136850=CARTESIAN_POINT('Ctrl Pts',(-44.0189397454599,-59.0168538922095,
0.));
#136851=CARTESIAN_POINT('Ctrl Pts',(-43.9958217500369,-59.0034628721168,
0.));
#136852=CARTESIAN_POINT('Ctrl Pts',(-43.9727478937056,-58.9900690087408,
0.));
#136853=CARTESIAN_POINT('Ctrl Pts',(-43.9497182316331,-58.9766723902529,
0.));
#136854=CARTESIAN_POINT('Ctrl Pts',(-43.9267328191501,-58.9632731052696,
0.));
#136855=CARTESIAN_POINT('Ctrl Pts',(-43.9037917117739,-58.9498712429054,
0.));
#136856=CARTESIAN_POINT('Ctrl Pts',(-43.8808949651873,-58.936466892712,
0.));
#136857=CARTESIAN_POINT('Ctrl Pts',(-43.858042635223,-58.9230601446436,
0.));
#136858=CARTESIAN_POINT('Ctrl Pts',(-43.835234777842,-58.9096510890129,
0.));
#136859=CARTESIAN_POINT('Ctrl Pts',(-43.8124714491076,-58.8962398164493,
0.));
#136860=CARTESIAN_POINT('Ctrl Pts',(-43.7897527051609,-58.8828264178621,
0.));
#136861=CARTESIAN_POINT('Ctrl Pts',(-43.7670786022402,-58.8694109844648,
0.));
#136862=CARTESIAN_POINT('Ctrl Pts',(-43.7444491966942,-58.855993607794,
0.));
#136863=CARTESIAN_POINT('Ctrl Pts',(-43.7218645449922,-58.8425743797326,
0.));
#136864=CARTESIAN_POINT('Ctrl Pts',(-43.6993247037314,-58.8291533925293,
0.));
#136865=CARTESIAN_POINT('Ctrl Pts',(-43.6768297296395,-58.8157307388238,
0.));
#136866=CARTESIAN_POINT('Ctrl Pts',(-43.6543796795789,-58.8023065116436,
0.));
#136867=CARTESIAN_POINT('Ctrl Pts',(-43.6319746105482,-58.788880804397,
0.));
#136868=CARTESIAN_POINT('Ctrl Pts',(-43.6096145796797,-58.775453710867,
0.));
#136869=CARTESIAN_POINT('Ctrl Pts',(-43.5872996442345,-58.7620253252062,
0.));
#136870=CARTESIAN_POINT('Ctrl Pts',(-43.5650298615917,-58.74859574193,0.));
#136871=CARTESIAN_POINT('Ctrl Pts',(-43.5428052892488,-58.735165055918,
0.));
#136872=CARTESIAN_POINT('Ctrl Pts',(-43.5206259848337,-58.7217333624209,
0.));
#136873=CARTESIAN_POINT('Ctrl Pts',(-43.4984920061073,-58.7083007570661,
0.));
#136874=CARTESIAN_POINT('Ctrl Pts',(-43.4764034109654,-58.6948673358638,
0.));
#136875=CARTESIAN_POINT('Ctrl Pts',(-43.4543602574351,-58.6814331952138,
0.));
#136876=CARTESIAN_POINT('Ctrl Pts',(-43.4323626036737,-58.6679984319097,
0.));
#136877=CARTESIAN_POINT('Ctrl Pts',(-43.4104105079768,-58.6545631431393,
0.));
#136878=CARTESIAN_POINT('Ctrl Pts',(-43.388504028781,-58.6411274264857,
0.));
#136879=CARTESIAN_POINT('Ctrl Pts',(-43.3666432246635,-58.627691379929,
0.));
#136880=CARTESIAN_POINT('Ctrl Pts',(-43.3448281543371,-58.6142551018467,
0.));
#136881=CARTESIAN_POINT('Ctrl Pts',(-43.3230588766449,-58.6008186910156,
0.));
#136882=CARTESIAN_POINT('Ctrl Pts',(-43.3013354505701,-58.5873822466152,
0.));
#136883=CARTESIAN_POINT('Ctrl Pts',(-43.27965793524,-58.573945868231,0.));
#136884=CARTESIAN_POINT('Ctrl Pts',(-43.2580263899278,-58.5605096558578,
0.));
#136885=CARTESIAN_POINT('Ctrl Pts',(-43.2364408740493,-58.5470737099032,
0.));
#136886=CARTESIAN_POINT('Ctrl Pts',(-43.2149014471574,-58.5336381311917,
0.));
#136887=CARTESIAN_POINT('Ctrl Pts',(-43.1934081689505,-58.5202030209669,
0.));
#136888=CARTESIAN_POINT('Ctrl Pts',(-43.1719610992771,-58.5067684808944,
0.));
#136889=CARTESIAN_POINT('Ctrl Pts',(-43.1505602981365,-58.4933346130636,
0.));
#136890=CARTESIAN_POINT('Ctrl Pts',(-43.1292058256777,-58.4799015199907,
0.));
#136891=CARTESIAN_POINT('Ctrl Pts',(-43.1078977421916,-58.4664693046217,
0.));
#136892=CARTESIAN_POINT('Ctrl Pts',(-43.0866361081177,-58.4530380703348,
0.));
#136893=CARTESIAN_POINT('Ctrl Pts',(-43.0654209840511,-58.439607920945,
0.));
#136894=CARTESIAN_POINT('Ctrl Pts',(-43.0442524307434,-58.4261789607058,
0.));
#136895=CARTESIAN_POINT('Ctrl Pts',(-43.0231305091027,-58.4127512943136,
0.));
#136896=CARTESIAN_POINT('Ctrl Pts',(-43.0020552801859,-58.3993250269101,
0.));
#136897=CARTESIAN_POINT('Ctrl Pts',(-42.9810268052032,-58.3859002640856,
0.));
#136898=CARTESIAN_POINT('Ctrl Pts',(-42.960045145526,-58.3724771118826,
0.));
#136899=CARTESIAN_POINT('Ctrl Pts',(-42.9391103626879,-58.3590556767978,
0.));
#136900=CARTESIAN_POINT('Ctrl Pts',(-42.9182225183855,-58.3456360657865,
0.));
#136901=CARTESIAN_POINT('Ctrl Pts',(-42.8973816744709,-58.3322183862654,
0.));
#136902=CARTESIAN_POINT('Ctrl Pts',(-42.8765878929551,-58.3188027461164,
0.));
#136903=CARTESIAN_POINT('Ctrl Pts',(-42.8558412360158,-58.3053892536894,
0.));
#136904=CARTESIAN_POINT('Ctrl Pts',(-42.8351417659999,-58.2919780178064,
0.));
#136905=CARTESIAN_POINT('Ctrl Pts',(-42.8144895454233,-58.2785691477638,
0.));
#136906=CARTESIAN_POINT('Ctrl Pts',(-42.7938846369651,-58.2651627533368,
0.));
#136907=CARTESIAN_POINT('Ctrl Pts',(-42.7733271034679,-58.251758944782,
0.));
#136908=CARTESIAN_POINT('Ctrl Pts',(-42.7528170079484,-58.2383578328424,
0.));
#136909=CARTESIAN_POINT('Ctrl Pts',(-42.7323544135985,-58.22495952875,0.));
#136910=CARTESIAN_POINT('Ctrl Pts',(-42.7119393837866,-58.21156414423,0.));
#136911=CARTESIAN_POINT('Ctrl Pts',(-42.6915719820513,-58.1981717915037,
0.));
#136912=CARTESIAN_POINT('Ctrl Pts',(-42.6712522721016,-58.1847825832923,
0.));
#136913=CARTESIAN_POINT('Ctrl Pts',(-42.6509803178265,-58.171396632821,
0.));
#136914=CARTESIAN_POINT('Ctrl Pts',(-42.6307561832976,-58.1580140538228,
0.));
#136915=CARTESIAN_POINT('Ctrl Pts',(-42.6105799327699,-58.1446349605421,
0.));
#136916=CARTESIAN_POINT('Ctrl Pts',(-42.5904516306762,-58.1312594677386,
0.));
#136917=CARTESIAN_POINT('Ctrl Pts',(-42.5703713416265,-58.1178876906907,
0.));
#136918=CARTESIAN_POINT('Ctrl Pts',(-42.5503391304183,-58.1045197452002,
0.));
#136919=CARTESIAN_POINT('Ctrl Pts',(-42.5303550620387,-58.0911557475965,
0.));
#136920=CARTESIAN_POINT('Ctrl Pts',(-42.5104192016664,-58.0777958147403,
0.));
#136921=CARTESIAN_POINT('Ctrl Pts',(-42.4905316146653,-58.0644400640275,
0.));
#136922=CARTESIAN_POINT('Ctrl Pts',(-42.4706923665845,-58.0510886133926,
0.));
#136923=CARTESIAN_POINT('Ctrl Pts',(-42.4509015231674,-58.037741581314,
0.));
#136924=CARTESIAN_POINT('Ctrl Pts',(-42.4311591503555,-58.0243990868181,
0.));
#136925=CARTESIAN_POINT('Ctrl Pts',(-42.411465314289,-58.0110612494828,
0.));
#136926=CARTESIAN_POINT('Ctrl Pts',(-42.3918200813014,-57.9977281894422,
0.));
#136927=CARTESIAN_POINT('Ctrl Pts',(-42.3722235179197,-57.9844000273911,
0.));
#136928=CARTESIAN_POINT('Ctrl Pts',(-42.3526756908746,-57.9710768845899,
0.));
#136929=CARTESIAN_POINT('Ctrl Pts',(-42.333176667102,-57.9577588828682,
0.));
#136930=CARTESIAN_POINT('Ctrl Pts',(-42.3137265137452,-57.9444461446299,
0.));
#136931=CARTESIAN_POINT('Ctrl Pts',(-42.2943252981489,-57.9311387928563,
0.));
#136932=CARTESIAN_POINT('Ctrl Pts',(-42.2749730878594,-57.9178369511114,
0.));
#136933=CARTESIAN_POINT('Ctrl Pts',(-42.2556699506353,-57.9045407435474,
0.));
#136934=CARTESIAN_POINT('Ctrl Pts',(-42.2364159544501,-57.8912502949096,
0.));
#136935=CARTESIAN_POINT('Ctrl Pts',(-42.2172111674938,-57.8779657305413,
0.));
#136936=CARTESIAN_POINT('Ctrl Pts',(-42.1980556581665,-57.864687176387,
0.));
#136937=CARTESIAN_POINT('Ctrl Pts',(-42.1789494950794,-57.8514147589972,
0.));
#136938=CARTESIAN_POINT('Ctrl Pts',(-42.1598927470646,-57.8381486055342,
0.));
#136939=CARTESIAN_POINT('Ctrl Pts',(-42.1408854831783,-57.8248888437775,
0.));
#136940=CARTESIAN_POINT('Ctrl Pts',(-42.1219277727021,-57.8116356021288,
0.));
#136941=CARTESIAN_POINT('Ctrl Pts',(-42.1030196851366,-57.798389009616,
0.));
#136942=CARTESIAN_POINT('Ctrl Pts',(-42.0841612902042,-57.7851491958987,
0.));
#136943=CARTESIAN_POINT('Ctrl Pts',(-42.0653526578588,-57.7719162912744,
0.));
#136944=CARTESIAN_POINT('Ctrl Pts',(-42.0465938582882,-57.7586904266834,
0.));
#136945=CARTESIAN_POINT('Ctrl Pts',(-42.0278849619148,-57.745471733714,
0.));
#136946=CARTESIAN_POINT('Ctrl Pts',(-42.0092260393897,-57.7322603446066,
0.));
#136947=CARTESIAN_POINT('Ctrl Pts',(-41.990617161596,-57.7190563922593,
0.));
#136948=CARTESIAN_POINT('Ctrl Pts',(-41.9720583996592,-57.7058600102351,
0.));
#136949=CARTESIAN_POINT('Ctrl Pts',(-41.9535498249488,-57.6926713327672,
0.));
#136950=CARTESIAN_POINT('Ctrl Pts',(-41.9350915090796,-57.6794904947649,
0.));
#136951=CARTESIAN_POINT('Ctrl Pts',(-41.9166835239054,-57.6663176318189,
0.));
#136952=CARTESIAN_POINT('Ctrl Pts',(-41.8983259415253,-57.6531528802072,
0.));
#136953=CARTESIAN_POINT('Ctrl Pts',(-41.8800188342912,-57.6399963769009,
0.));
#136954=CARTESIAN_POINT('Ctrl Pts',(-41.8617622748107,-57.6268482595701,
0.));
#136955=CARTESIAN_POINT('Ctrl Pts',(-41.8435563359456,-57.613708666588,
0.));
#136956=CARTESIAN_POINT('Ctrl Pts',(-41.8254010908051,-57.6005777370347,
0.));
#136957=CARTESIAN_POINT('Ctrl Pts',(-41.8072966127559,-57.5874556107054,
0.));
#136958=CARTESIAN_POINT('Ctrl Pts',(-41.7892429754298,-57.5743424281204,
0.));
#136959=CARTESIAN_POINT('Ctrl Pts',(-41.7712402527273,-57.561238330532,
0.));
#136960=CARTESIAN_POINT('Ctrl Pts',(-41.7532885188174,-57.5481434599334,
0.));
#136961=CARTESIAN_POINT('Ctrl Pts',(-41.7353878481336,-57.5350579590648,
0.));
#136962=CARTESIAN_POINT('Ctrl Pts',(-41.7175383153819,-57.5219819714169,
0.));
#136963=CARTESIAN_POINT('Ctrl Pts',(-41.6997399955445,-57.5089156412341,
0.));
#136964=CARTESIAN_POINT('Ctrl Pts',(-41.6819929638797,-57.4958591135165,
0.));
#136965=CARTESIAN_POINT('Ctrl Pts',(-41.6642972959168,-57.4828125340222,
0.));
#136966=CARTESIAN_POINT('Ctrl Pts',(-41.6466530674522,-57.4697760492693,
0.));
#136967=CARTESIAN_POINT('Ctrl Pts',(-41.6290603545674,-57.4567498065573,
0.));
#136968=CARTESIAN_POINT('Ctrl Pts',(-41.6115192336393,-57.4437339539848,
0.));
#136969=CARTESIAN_POINT('Ctrl Pts',(-41.5940297813474,-57.4307286404656,
0.));
#136970=CARTESIAN_POINT('Ctrl Pts',(-41.5765920746764,-57.417734015749,
0.));
#136971=CARTESIAN_POINT('Ctrl Pts',(-41.5592061909159,-57.4047502304207,
0.));
#136972=CARTESIAN_POINT('Ctrl Pts',(-41.5418722076558,-57.3917774358844,
0.));
#136973=CARTESIAN_POINT('Ctrl Pts',(-41.5245902027767,-57.378815784345,
0.));
#136974=CARTESIAN_POINT('Ctrl Pts',(-41.5073602544404,-57.3658654287948,
0.));
#136975=CARTESIAN_POINT('Ctrl Pts',(-41.4901824410654,-57.3529265229858,
0.));
#136976=CARTESIAN_POINT('Ctrl Pts',(-41.4730568413535,-57.339999221474,
0.));
#136977=CARTESIAN_POINT('Ctrl Pts',(-41.4559835343338,-57.3270836796925,
0.));
#136978=CARTESIAN_POINT('Ctrl Pts',(-41.4389625993948,-57.3141800540137,
0.));
#136979=CARTESIAN_POINT('Ctrl Pts',(-41.4219941163154,-57.3012885018139,
0.));
#136980=CARTESIAN_POINT('Ctrl Pts',(-41.4050781652923,-57.2884091815385,
0.));
#136981=CARTESIAN_POINT('Ctrl Pts',(-41.3882148268798,-57.2755422525822,
0.));
#136982=CARTESIAN_POINT('Ctrl Pts',(-41.3714041819215,-57.2626878751584,
0.));
#136983=CARTESIAN_POINT('Ctrl Pts',(-41.3546463114889,-57.2498462101883,
0.));
#136984=CARTESIAN_POINT('Ctrl Pts',(-41.3379412967889,-57.237017419142,
0.));
#136985=CARTESIAN_POINT('Ctrl Pts',(-41.321289219151,-57.2242016640226,
0.));
#136986=CARTESIAN_POINT('Ctrl Pts',(-41.304690160231,-57.2113991077325,
0.));
#136987=CARTESIAN_POINT('Ctrl Pts',(-41.2881442021869,-57.1986099143992,
0.));
#136988=CARTESIAN_POINT('Ctrl Pts',(-41.2716514278268,-57.1858342496526,
0.));
#136989=CARTESIAN_POINT('Ctrl Pts',(-41.2552119208445,-57.1730722810771,
0.));
#136990=CARTESIAN_POINT('Ctrl Pts',(-41.2388257656534,-57.1603241779042,
0.));
#136991=CARTESIAN_POINT('Ctrl Pts',(-41.2224930469412,-57.1475901101795,
0.));
#136992=CARTESIAN_POINT('Ctrl Pts',(-41.2062138492913,-57.1348702480644,
0.));
#136993=CARTESIAN_POINT('Ctrl Pts',(-41.1899882567941,-57.1221647611231,
0.));
#136994=CARTESIAN_POINT('Ctrl Pts',(-41.1738163525931,-57.1094738174998,
0.));
#136995=CARTESIAN_POINT('Ctrl Pts',(-41.1576982197402,-57.0967975854912,
0.));
#136996=CARTESIAN_POINT('Ctrl Pts',(-41.1416339422132,-57.0841362354281,
0.));
#136997=CARTESIAN_POINT('Ctrl Pts',(-41.1256236057436,-57.0714899412091,
0.));
#136998=CARTESIAN_POINT('Ctrl Pts',(-41.1096672990125,-57.0588588825266,
0.));
#136999=CARTESIAN_POINT('Ctrl Pts',(-41.0937651137519,-57.0462432450637,
0.));
#137000=CARTESIAN_POINT('Ctrl Pts',(-41.0779171422415,-57.0336432158503,
0.));
#137001=CARTESIAN_POINT('Ctrl Pts',(-41.0621234751,-57.0210589791777,0.));
#137002=CARTESIAN_POINT('Ctrl Pts',(-41.0463841993622,-57.008490713044,
0.));
#137003=CARTESIAN_POINT('Ctrl Pts',(-41.0306993954021,-56.9959385834768,
0.));
#137004=CARTESIAN_POINT('Ctrl Pts',(-41.0150691398988,-56.9834027500178,
0.));
#137005=CARTESIAN_POINT('Ctrl Pts',(-40.9994935117307,-56.9708833766183,
0.));
#137006=CARTESIAN_POINT('Ctrl Pts',(-40.9839725967121,-56.9583806404069,
0.));
#137007=CARTESIAN_POINT('Ctrl Pts',(-40.968506493303,-56.9458947422541,
0.));
#137008=CARTESIAN_POINT('Ctrl Pts',(-40.9530953164952,-56.9334259139928,
0.));
#137009=CARTESIAN_POINT('Ctrl Pts',(-40.9377391857044,-56.9209743960861,
0.));
#137010=CARTESIAN_POINT('Ctrl Pts',(-40.9224382132382,-56.9085404164432,
0.));
#137011=CARTESIAN_POINT('Ctrl Pts',(-40.9071924937551,-56.8961241708926,
0.));
#137012=CARTESIAN_POINT('Ctrl Pts',(-40.8920020903443,-56.8837257978574,
0.));
#137013=CARTESIAN_POINT('Ctrl Pts',(-40.8768670342278,-56.8713453765252,
0.));
#137014=CARTESIAN_POINT('Ctrl Pts',(-40.8648032759631,-56.8614554317993,
0.));
#137015=CARTESIAN_POINT('Ctrl Pts',(-40.8557803680411,-56.8540460739677,
0.));
#137016=CARTESIAN_POINT('Ctrl Pts',(-40.8497761671086,-56.8491101022668,
0.));
#137017=CARTESIAN_POINT('Ctrl Pts',(-40.8467768343956,-56.8466430164621,
0.));
#137018=CARTESIAN_POINT('Ctrl Pts',(-49.8690697110161,-55.3473204966403,
0.));
#137019=CARTESIAN_POINT('Ctrl Pts',(-49.8690697110161,-55.3473204966403,
12.));
#137020=CARTESIAN_POINT('Ctrl Pts',(-49.8639277221566,-55.3451131058826,
0.));
#137021=CARTESIAN_POINT('Ctrl Pts',(-49.8639277221566,-55.3451131058826,
12.));
#137022=CARTESIAN_POINT('Ctrl Pts',(-49.8536479176833,-55.34069740326,0.));
#137023=CARTESIAN_POINT('Ctrl Pts',(-49.8536479176833,-55.34069740326,12.));
#137024=CARTESIAN_POINT('Ctrl Pts',(-49.8382407307107,-55.3340710860055,
0.));
#137025=CARTESIAN_POINT('Ctrl Pts',(-49.8382407307107,-55.3340710860055,
12.));
#137026=CARTESIAN_POINT('Ctrl Pts',(-49.8177228552377,-55.3252304694602,
0.));
#137027=CARTESIAN_POINT('Ctrl Pts',(-49.8177228552377,-55.3252304694602,
12.));
#137028=CARTESIAN_POINT('Ctrl Pts',(-49.7921172540628,-55.3141704897766,
0.));
#137029=CARTESIAN_POINT('Ctrl Pts',(-49.7921172540628,-55.3141704897766,
12.));
#137030=CARTESIAN_POINT('Ctrl Pts',(-49.7665534128535,-55.3031013105853,
0.));
#137031=CARTESIAN_POINT('Ctrl Pts',(-49.7665534128535,-55.3031013105853,
12.));
#137032=CARTESIAN_POINT('Ctrl Pts',(-49.7410313576508,-55.2920229527546,
0.));
#137033=CARTESIAN_POINT('Ctrl Pts',(-49.7410313576508,-55.2920229527546,
12.));
#137034=CARTESIAN_POINT('Ctrl Pts',(-49.7155511248531,-55.2809354521515,
0.));
#137035=CARTESIAN_POINT('Ctrl Pts',(-49.7155511248531,-55.2809354521515,
12.));
#137036=CARTESIAN_POINT('Ctrl Pts',(-49.6901127631627,-55.2698388650025,
0.));
#137037=CARTESIAN_POINT('Ctrl Pts',(-49.6901127631627,-55.2698388650025,
12.));
#137038=CARTESIAN_POINT('Ctrl Pts',(-49.6647163322266,-55.2587332663783,
0.));
#137039=CARTESIAN_POINT('Ctrl Pts',(-49.6647163322266,-55.2587332663783,
12.));
#137040=CARTESIAN_POINT('Ctrl Pts',(-49.6393618987473,-55.2476187434057,
0.));
#137041=CARTESIAN_POINT('Ctrl Pts',(-49.6393618987473,-55.2476187434057,
12.));
#137042=CARTESIAN_POINT('Ctrl Pts',(-49.6140495332804,-55.2364953899358,
0.));
#137043=CARTESIAN_POINT('Ctrl Pts',(-49.6140495332804,-55.2364953899358,
12.));
#137044=CARTESIAN_POINT('Ctrl Pts',(-49.5887793068352,-55.2253633007666,
0.));
#137045=CARTESIAN_POINT('Ctrl Pts',(-49.5887793068352,-55.2253633007666,
12.));
#137046=CARTESIAN_POINT('Ctrl Pts',(-49.5635512873435,-55.2142225657013,
0.));
#137047=CARTESIAN_POINT('Ctrl Pts',(-49.5635512873435,-55.2142225657013,
12.));
#137048=CARTESIAN_POINT('Ctrl Pts',(-49.5383655368074,-55.2030732647312,
0.));
#137049=CARTESIAN_POINT('Ctrl Pts',(-49.5383655368074,-55.2030732647312,
12.));
#137050=CARTESIAN_POINT('Ctrl Pts',(-49.5132221132992,-55.1919154713647,
0.));
#137051=CARTESIAN_POINT('Ctrl Pts',(-49.5132221132992,-55.1919154713647,
12.));
#137052=CARTESIAN_POINT('Ctrl Pts',(-49.4881210723966,-55.1807492550119,
0.));
#137053=CARTESIAN_POINT('Ctrl Pts',(-49.4881210723966,-55.1807492550119,
12.));
#137054=CARTESIAN_POINT('Ctrl Pts',(-49.4630624688793,-55.1695746838174,
0.));
#137055=CARTESIAN_POINT('Ctrl Pts',(-49.4630624688793,-55.1695746838174,
12.));
#137056=CARTESIAN_POINT('Ctrl Pts',(-49.4380463581965,-55.1583918271116,
0.));
#137057=CARTESIAN_POINT('Ctrl Pts',(-49.4380463581965,-55.1583918271116,
12.));
#137058=CARTESIAN_POINT('Ctrl Pts',(-49.4130727983201,-55.1472007585183,
0.));
#137059=CARTESIAN_POINT('Ctrl Pts',(-49.4130727983201,-55.1472007585183,
12.));
#137060=CARTESIAN_POINT('Ctrl Pts',(-49.3881418495489,-55.1360015556221,
0.));
#137061=CARTESIAN_POINT('Ctrl Pts',(-49.3881418495489,-55.1360015556221,
12.));
#137062=CARTESIAN_POINT('Ctrl Pts',(-49.3632535736715,-55.1247942985619,
0.));
#137063=CARTESIAN_POINT('Ctrl Pts',(-49.3632535736715,-55.1247942985619,
12.));
#137064=CARTESIAN_POINT('Ctrl Pts',(-49.3384080333155,-55.1135790689464,
0.));
#137065=CARTESIAN_POINT('Ctrl Pts',(-49.3384080333155,-55.1135790689464,
12.));
#137066=CARTESIAN_POINT('Ctrl Pts',(-49.3136052912622,-55.102355948714,
0.));
#137067=CARTESIAN_POINT('Ctrl Pts',(-49.3136052912622,-55.102355948714,
12.));
#137068=CARTESIAN_POINT('Ctrl Pts',(-49.2888454096563,-55.0911250188302,
0.));
#137069=CARTESIAN_POINT('Ctrl Pts',(-49.2888454096563,-55.0911250188302,
12.));
#137070=CARTESIAN_POINT('Ctrl Pts',(-49.264128449652,-55.079886358701,0.));
#137071=CARTESIAN_POINT('Ctrl Pts',(-49.264128449652,-55.079886358701,12.));
#137072=CARTESIAN_POINT('Ctrl Pts',(-49.2394544718531,-55.0686400468931,
0.));
#137073=CARTESIAN_POINT('Ctrl Pts',(-49.2394544718531,-55.0686400468931,
12.));
#137074=CARTESIAN_POINT('Ctrl Pts',(-49.2148235365704,-55.0573861615579,
0.));
#137075=CARTESIAN_POINT('Ctrl Pts',(-49.2148235365704,-55.0573861615579,
12.));
#137076=CARTESIAN_POINT('Ctrl Pts',(-49.1902357041461,-55.0461247809744,
0.));
#137077=CARTESIAN_POINT('Ctrl Pts',(-49.1902357041461,-55.0461247809744,
12.));
#137078=CARTESIAN_POINT('Ctrl Pts',(-49.1656910352476,-55.0348559840453,
0.));
#137079=CARTESIAN_POINT('Ctrl Pts',(-49.1656910352476,-55.0348559840453,
12.));
#137080=CARTESIAN_POINT('Ctrl Pts',(-49.1411895911635,-55.0235798508045,
0.));
#137081=CARTESIAN_POINT('Ctrl Pts',(-49.1411895911635,-55.0235798508045,
12.));
#137082=CARTESIAN_POINT('Ctrl Pts',(-49.116731433673,-55.012296462186,0.));
#137083=CARTESIAN_POINT('Ctrl Pts',(-49.116731433673,-55.012296462186,12.));
#137084=CARTESIAN_POINT('Ctrl Pts',(-49.0923166249219,-55.0010058998107,
0.));
#137085=CARTESIAN_POINT('Ctrl Pts',(-49.0923166249219,-55.0010058998107,
12.));
#137086=CARTESIAN_POINT('Ctrl Pts',(-49.067945227287,-54.9897082457606,
0.));
#137087=CARTESIAN_POINT('Ctrl Pts',(-49.067945227287,-54.9897082457606,
12.));
#137088=CARTESIAN_POINT('Ctrl Pts',(-49.0436173032528,-54.9784035823766,
0.));
#137089=CARTESIAN_POINT('Ctrl Pts',(-49.0436173032528,-54.9784035823766,
12.));
#137090=CARTESIAN_POINT('Ctrl Pts',(-49.0193329152479,-54.9670919920029,
0.));
#137091=CARTESIAN_POINT('Ctrl Pts',(-49.0193329152479,-54.9670919920029,
12.));
#137092=CARTESIAN_POINT('Ctrl Pts',(-48.9950921256527,-54.9557735569943,
0.));
#137093=CARTESIAN_POINT('Ctrl Pts',(-48.9950921256527,-54.9557735569943,
12.));
#137094=CARTESIAN_POINT('Ctrl Pts',(-48.9708949968795,-54.9444483598378,
0.));
#137095=CARTESIAN_POINT('Ctrl Pts',(-48.9708949968795,-54.9444483598378,
12.));
#137096=CARTESIAN_POINT('Ctrl Pts',(-48.9467415914269,-54.9331164832424,
0.));
#137097=CARTESIAN_POINT('Ctrl Pts',(-48.9467415914269,-54.9331164832424,
12.));
#137098=CARTESIAN_POINT('Ctrl Pts',(-48.9226319719369,-54.9217780102355,
0.));
#137099=CARTESIAN_POINT('Ctrl Pts',(-48.9226319719369,-54.9217780102355,
12.));
#137100=CARTESIAN_POINT('Ctrl Pts',(-48.8985662012528,-54.9104330242742,
0.));
#137101=CARTESIAN_POINT('Ctrl Pts',(-48.8985662012528,-54.9104330242742,
12.));
#137102=CARTESIAN_POINT('Ctrl Pts',(-48.8745443424477,-54.8990816092953,
0.));
#137103=CARTESIAN_POINT('Ctrl Pts',(-48.8745443424477,-54.8990816092953,
12.));
#137104=CARTESIAN_POINT('Ctrl Pts',(-48.8505664587974,-54.8877238496566,
0.));
#137105=CARTESIAN_POINT('Ctrl Pts',(-48.8505664587974,-54.8877238496566,
12.));
#137106=CARTESIAN_POINT('Ctrl Pts',(-48.8266326137622,-54.8763598301037,
0.));
#137107=CARTESIAN_POINT('Ctrl Pts',(-48.8266326137622,-54.8763598301037,
12.));
#137108=CARTESIAN_POINT('Ctrl Pts',(-48.8027428709614,-54.8649896357285,
0.));
#137109=CARTESIAN_POINT('Ctrl Pts',(-48.8027428709614,-54.8649896357285,
12.));
#137110=CARTESIAN_POINT('Ctrl Pts',(-48.7788972941438,-54.8536133519292,
0.));
#137111=CARTESIAN_POINT('Ctrl Pts',(-48.7788972941438,-54.8536133519292,
12.));
#137112=CARTESIAN_POINT('Ctrl Pts',(-48.7550959471601,-54.8422310643763,
0.));
#137113=CARTESIAN_POINT('Ctrl Pts',(-48.7550959471601,-54.8422310643763,
12.));
#137114=CARTESIAN_POINT('Ctrl Pts',(-48.7313388939845,-54.8308428590344,
0.));
#137115=CARTESIAN_POINT('Ctrl Pts',(-48.7313388939845,-54.8308428590344,
12.));
#137116=CARTESIAN_POINT('Ctrl Pts',(-48.7076261987292,-54.819448822181,
0.));
#137117=CARTESIAN_POINT('Ctrl Pts',(-48.7076261987292,-54.819448822181,
12.));
#137118=CARTESIAN_POINT('Ctrl Pts',(-48.6839579256566,-54.8080490404275,
0.));
#137119=CARTESIAN_POINT('Ctrl Pts',(-48.6839579256566,-54.8080490404275,
12.));
#137120=CARTESIAN_POINT('Ctrl Pts',(-48.6603341391886,-54.796643600739,
0.));
#137121=CARTESIAN_POINT('Ctrl Pts',(-48.6603341391886,-54.796643600739,
12.));
#137122=CARTESIAN_POINT('Ctrl Pts',(-48.6367549039112,-54.7852325904583,
0.));
#137123=CARTESIAN_POINT('Ctrl Pts',(-48.6367549039112,-54.7852325904583,
12.));
#137124=CARTESIAN_POINT('Ctrl Pts',(-48.6132202845783,-54.7738160973032,
0.));
#137125=CARTESIAN_POINT('Ctrl Pts',(-48.6132202845783,-54.7738160973032,
12.));
#137126=CARTESIAN_POINT('Ctrl Pts',(-48.5897303461125,-54.7623942093586,
0.));
#137127=CARTESIAN_POINT('Ctrl Pts',(-48.5897303461125,-54.7623942093586,
12.));
#137128=CARTESIAN_POINT('Ctrl Pts',(-48.5662851536026,-54.7509670150714,
0.));
#137129=CARTESIAN_POINT('Ctrl Pts',(-48.5662851536026,-54.7509670150714,
12.));
#137130=CARTESIAN_POINT('Ctrl Pts',(-48.5428847722977,-54.7395346032453,
0.));
#137131=CARTESIAN_POINT('Ctrl Pts',(-48.5428847722977,-54.7395346032453,
12.));
#137132=CARTESIAN_POINT('Ctrl Pts',(-48.519529267596,-54.7280970630351,
0.));
#137133=CARTESIAN_POINT('Ctrl Pts',(-48.519529267596,-54.7280970630351,
12.));
#137134=CARTESIAN_POINT('Ctrl Pts',(-48.4962187050457,-54.716654483948,
0.));
#137135=CARTESIAN_POINT('Ctrl Pts',(-48.4962187050457,-54.716654483948,
12.));
#137136=CARTESIAN_POINT('Ctrl Pts',(-48.472953150357,-54.7052069558497,
0.));
#137137=CARTESIAN_POINT('Ctrl Pts',(-48.472953150357,-54.7052069558497,
12.));
#137138=CARTESIAN_POINT('Ctrl Pts',(-48.4497326694052,-54.6937545689695,
0.));
#137139=CARTESIAN_POINT('Ctrl Pts',(-48.4497326694052,-54.6937545689695,
12.));
#137140=CARTESIAN_POINT('Ctrl Pts',(-48.426557328234,-54.6822974139064,
0.));
#137141=CARTESIAN_POINT('Ctrl Pts',(-48.426557328234,-54.6822974139064,
12.));
#137142=CARTESIAN_POINT('Ctrl Pts',(-48.4034271930514,-54.6708355816358,
0.));
#137143=CARTESIAN_POINT('Ctrl Pts',(-48.4034271930514,-54.6708355816358,
12.));
#137144=CARTESIAN_POINT('Ctrl Pts',(-48.3803423302294,-54.6593691635145,
0.));
#137145=CARTESIAN_POINT('Ctrl Pts',(-48.3803423302294,-54.6593691635145,
12.));
#137146=CARTESIAN_POINT('Ctrl Pts',(-48.3573028063124,-54.6478982512794,
0.));
#137147=CARTESIAN_POINT('Ctrl Pts',(-48.3573028063124,-54.6478982512794,
12.));
#137148=CARTESIAN_POINT('Ctrl Pts',(-48.3343086880194,-54.6364229370494,
0.));
#137149=CARTESIAN_POINT('Ctrl Pts',(-48.3343086880194,-54.6364229370494,
12.));
#137150=CARTESIAN_POINT('Ctrl Pts',(-48.3113600422443,-54.6249433133261,
0.));
#137151=CARTESIAN_POINT('Ctrl Pts',(-48.3113600422443,-54.6249433133261,
12.));
#137152=CARTESIAN_POINT('Ctrl Pts',(-48.2884569360506,-54.6134594729959,
0.));
#137153=CARTESIAN_POINT('Ctrl Pts',(-48.2884569360506,-54.6134594729959,
12.));
#137154=CARTESIAN_POINT('Ctrl Pts',(-48.2655994366665,-54.6019715093309,
0.));
#137155=CARTESIAN_POINT('Ctrl Pts',(-48.2655994366665,-54.6019715093309,
12.));
#137156=CARTESIAN_POINT('Ctrl Pts',(-48.2427876114947,-54.5904795159926,
0.));
#137157=CARTESIAN_POINT('Ctrl Pts',(-48.2427876114947,-54.5904795159926,
12.));
#137158=CARTESIAN_POINT('Ctrl Pts',(-48.2200215281173,-54.5789835870342,
0.));
#137159=CARTESIAN_POINT('Ctrl Pts',(-48.2200215281173,-54.5789835870342,
12.));
#137160=CARTESIAN_POINT('Ctrl Pts',(-48.1973012542966,-54.5674838169041,
0.));
#137161=CARTESIAN_POINT('Ctrl Pts',(-48.1973012542966,-54.5674838169041,
12.));
#137162=CARTESIAN_POINT('Ctrl Pts',(-48.1746268579736,-54.5559803004492,
0.));
#137163=CARTESIAN_POINT('Ctrl Pts',(-48.1746268579736,-54.5559803004492,
12.));
#137164=CARTESIAN_POINT('Ctrl Pts',(-48.1519984072622,-54.5444731329201,
0.));
#137165=CARTESIAN_POINT('Ctrl Pts',(-48.1519984072622,-54.5444731329201,
12.));
#137166=CARTESIAN_POINT('Ctrl Pts',(-48.1294159704573,-54.5329624099721,
0.));
#137167=CARTESIAN_POINT('Ctrl Pts',(-48.1294159704573,-54.5329624099721,
12.));
#137168=CARTESIAN_POINT('Ctrl Pts',(-48.1068796160405,-54.5214482276678,
0.));
#137169=CARTESIAN_POINT('Ctrl Pts',(-48.1068796160405,-54.5214482276678,
12.));
#137170=CARTESIAN_POINT('Ctrl Pts',(-48.0843894126806,-54.5099306824786,
0.));
#137171=CARTESIAN_POINT('Ctrl Pts',(-48.0843894126806,-54.5099306824786,
12.));
#137172=CARTESIAN_POINT('Ctrl Pts',(-48.0619454292324,-54.4984098712886,
0.));
#137173=CARTESIAN_POINT('Ctrl Pts',(-48.0619454292324,-54.4984098712886,
12.));
#137174=CARTESIAN_POINT('Ctrl Pts',(-48.0395477347298,-54.4868858913971,
0.));
#137175=CARTESIAN_POINT('Ctrl Pts',(-48.0395477347298,-54.4868858913971,
12.));
#137176=CARTESIAN_POINT('Ctrl Pts',(-48.0171963983924,-54.4753588405215,
0.));
#137177=CARTESIAN_POINT('Ctrl Pts',(-48.0171963983924,-54.4753588405215,
12.));
#137178=CARTESIAN_POINT('Ctrl Pts',(-47.9948914896326,-54.4638288168003,
0.));
#137179=CARTESIAN_POINT('Ctrl Pts',(-47.9948914896326,-54.4638288168003,
12.));
#137180=CARTESIAN_POINT('Ctrl Pts',(-47.9726330780572,-54.4522959187955,
0.));
#137181=CARTESIAN_POINT('Ctrl Pts',(-47.9726330780572,-54.4522959187955,
12.));
#137182=CARTESIAN_POINT('Ctrl Pts',(-47.9504212334675,-54.4407602454967,
0.));
#137183=CARTESIAN_POINT('Ctrl Pts',(-47.9504212334675,-54.4407602454967,
12.));
#137184=CARTESIAN_POINT('Ctrl Pts',(-47.9282560258516,-54.429221896324,
0.));
#137185=CARTESIAN_POINT('Ctrl Pts',(-47.9282560258516,-54.429221896324,
12.));
#137186=CARTESIAN_POINT('Ctrl Pts',(-47.9061375253897,-54.4176809711311,
0.));
#137187=CARTESIAN_POINT('Ctrl Pts',(-47.9061375253897,-54.4176809711311,
12.));
#137188=CARTESIAN_POINT('Ctrl Pts',(-47.8840658024618,-54.4061375702079,
0.));
#137189=CARTESIAN_POINT('Ctrl Pts',(-47.8840658024618,-54.4061375702079,
12.));
#137190=CARTESIAN_POINT('Ctrl Pts',(-47.8620409276493,-54.3945917942832,
0.));
#137191=CARTESIAN_POINT('Ctrl Pts',(-47.8620409276493,-54.3945917942832,
12.));
#137192=CARTESIAN_POINT('Ctrl Pts',(-47.8400629717355,-54.3830437445279,
0.));
#137193=CARTESIAN_POINT('Ctrl Pts',(-47.8400629717355,-54.3830437445279,
12.));
#137194=CARTESIAN_POINT('Ctrl Pts',(-47.8181320056995,-54.3714935225591,
0.));
#137195=CARTESIAN_POINT('Ctrl Pts',(-47.8181320056995,-54.3714935225591,
12.));
#137196=CARTESIAN_POINT('Ctrl Pts',(-47.7962481007185,-54.3599412304438,
0.));
#137197=CARTESIAN_POINT('Ctrl Pts',(-47.7962481007185,-54.3599412304438,
12.));
#137198=CARTESIAN_POINT('Ctrl Pts',(-47.7744113281771,-54.3483869707002,
0.));
#137199=CARTESIAN_POINT('Ctrl Pts',(-47.7744113281771,-54.3483869707002,
12.));
#137200=CARTESIAN_POINT('Ctrl Pts',(-47.7526217596694,-54.3368308463023,
0.));
#137201=CARTESIAN_POINT('Ctrl Pts',(-47.7526217596694,-54.3368308463023,
12.));
#137202=CARTESIAN_POINT('Ctrl Pts',(-47.7308794669993,-54.3252729606823,
0.));
#137203=CARTESIAN_POINT('Ctrl Pts',(-47.7308794669993,-54.3252729606823,
12.));
#137204=CARTESIAN_POINT('Ctrl Pts',(-47.7091845221747,-54.3137134177345,
0.));
#137205=CARTESIAN_POINT('Ctrl Pts',(-47.7091845221747,-54.3137134177345,
12.));
#137206=CARTESIAN_POINT('Ctrl Pts',(-47.6875369974087,-54.302152321819,
0.));
#137207=CARTESIAN_POINT('Ctrl Pts',(-47.6875369974087,-54.302152321819,
12.));
#137208=CARTESIAN_POINT('Ctrl Pts',(-47.6659369651301,-54.290589777765,
0.));
#137209=CARTESIAN_POINT('Ctrl Pts',(-47.6659369651301,-54.290589777765,
12.));
#137210=CARTESIAN_POINT('Ctrl Pts',(-47.6443844979848,-54.2790258908738,
0.));
#137211=CARTESIAN_POINT('Ctrl Pts',(-47.6443844979848,-54.2790258908738,
12.));
#137212=CARTESIAN_POINT('Ctrl Pts',(-47.6228796688375,-54.2674607669226,
0.));
#137213=CARTESIAN_POINT('Ctrl Pts',(-47.6228796688375,-54.2674607669226,
12.));
#137214=CARTESIAN_POINT('Ctrl Pts',(-47.6014225507659,-54.2558945121678,
0.));
#137215=CARTESIAN_POINT('Ctrl Pts',(-47.6014225507659,-54.2558945121678,
12.));
#137216=CARTESIAN_POINT('Ctrl Pts',(-47.5800132170608,-54.244327233349,
0.));
#137217=CARTESIAN_POINT('Ctrl Pts',(-47.5800132170608,-54.244327233349,
12.));
#137218=CARTESIAN_POINT('Ctrl Pts',(-47.5586517412363,-54.2327590376924,
0.));
#137219=CARTESIAN_POINT('Ctrl Pts',(-47.5586517412363,-54.2327590376924,
12.));
#137220=CARTESIAN_POINT('Ctrl Pts',(-47.5373381970326,-54.2211900329138,
0.));
#137221=CARTESIAN_POINT('Ctrl Pts',(-47.5373381970326,-54.2211900329138,
12.));
#137222=CARTESIAN_POINT('Ctrl Pts',(-47.5160726584174,-54.209620327223,
0.));
#137223=CARTESIAN_POINT('Ctrl Pts',(-47.5160726584174,-54.209620327223,
12.));
#137224=CARTESIAN_POINT('Ctrl Pts',(-47.4948551995801,-54.198050029327,
0.));
#137225=CARTESIAN_POINT('Ctrl Pts',(-47.4948551995801,-54.198050029327,
12.));
#137226=CARTESIAN_POINT('Ctrl Pts',(-47.4736858949322,-54.1864792484345,
0.));
#137227=CARTESIAN_POINT('Ctrl Pts',(-47.4736858949322,-54.1864792484345,
12.));
#137228=CARTESIAN_POINT('Ctrl Pts',(-47.4525648191173,-54.1749080942593,
0.));
#137229=CARTESIAN_POINT('Ctrl Pts',(-47.4525648191173,-54.1749080942593,
12.));
#137230=CARTESIAN_POINT('Ctrl Pts',(-47.4314920470141,-54.1633366770239,
0.));
#137231=CARTESIAN_POINT('Ctrl Pts',(-47.4314920470141,-54.1633366770239,
12.));
#137232=CARTESIAN_POINT('Ctrl Pts',(-47.4104676537381,-54.1517651074637,
0.));
#137233=CARTESIAN_POINT('Ctrl Pts',(-47.4104676537381,-54.1517651074637,
12.));
#137234=CARTESIAN_POINT('Ctrl Pts',(-47.3894917146365,-54.1401934968311,
0.));
#137235=CARTESIAN_POINT('Ctrl Pts',(-47.3894917146365,-54.1401934968311,
12.));
#137236=CARTESIAN_POINT('Ctrl Pts',(-47.3685643052874,-54.1286219568989,
0.));
#137237=CARTESIAN_POINT('Ctrl Pts',(-47.3685643052874,-54.1286219568989,
12.));
#137238=CARTESIAN_POINT('Ctrl Pts',(-47.3476855015102,-54.1170505999645,
0.));
#137239=CARTESIAN_POINT('Ctrl Pts',(-47.3476855015102,-54.1170505999645,
12.));
#137240=CARTESIAN_POINT('Ctrl Pts',(-47.3268553793694,-54.1054795388543,
0.));
#137241=CARTESIAN_POINT('Ctrl Pts',(-47.3268553793694,-54.1054795388543,
12.));
#137242=CARTESIAN_POINT('Ctrl Pts',(-47.3060740151752,-54.0939088869269,
0.));
#137243=CARTESIAN_POINT('Ctrl Pts',(-47.3060740151752,-54.0939088869269,
12.));
#137244=CARTESIAN_POINT('Ctrl Pts',(-47.2853414854793,-54.0823387580776,
0.));
#137245=CARTESIAN_POINT('Ctrl Pts',(-47.2853414854793,-54.0823387580776,
12.));
#137246=CARTESIAN_POINT('Ctrl Pts',(-47.2646578670746,-54.0707692667438,
0.));
#137247=CARTESIAN_POINT('Ctrl Pts',(-47.2646578670746,-54.0707692667438,
12.));
#137248=CARTESIAN_POINT('Ctrl Pts',(-47.2440232370065,-54.0592005279086,
0.));
#137249=CARTESIAN_POINT('Ctrl Pts',(-47.2440232370065,-54.0592005279086,
12.));
#137250=CARTESIAN_POINT('Ctrl Pts',(-47.2234376725743,-54.047632657104,
0.));
#137251=CARTESIAN_POINT('Ctrl Pts',(-47.2234376725743,-54.047632657104,
12.));
#137252=CARTESIAN_POINT('Ctrl Pts',(-47.202901251334,-54.0360657704163,
0.));
#137253=CARTESIAN_POINT('Ctrl Pts',(-47.202901251334,-54.0360657704163,
12.));
#137254=CARTESIAN_POINT('Ctrl Pts',(-47.1824140510926,-54.0244999844893,
0.));
#137255=CARTESIAN_POINT('Ctrl Pts',(-47.1824140510926,-54.0244999844893,
12.));
#137256=CARTESIAN_POINT('Ctrl Pts',(-47.1619761499087,-54.0129354165297,
0.));
#137257=CARTESIAN_POINT('Ctrl Pts',(-47.1619761499087,-54.0129354165297,
12.));
#137258=CARTESIAN_POINT('Ctrl Pts',(-47.1415876261035,-54.0013721843118,
0.));
#137259=CARTESIAN_POINT('Ctrl Pts',(-47.1415876261035,-54.0013721843118,
12.));
#137260=CARTESIAN_POINT('Ctrl Pts',(-47.1212485582643,-53.989810406182,
0.));
#137261=CARTESIAN_POINT('Ctrl Pts',(-47.1212485582643,-53.989810406182,
12.));
#137262=CARTESIAN_POINT('Ctrl Pts',(-47.1009590252458,-53.9782502010634,
0.));
#137263=CARTESIAN_POINT('Ctrl Pts',(-47.1009590252458,-53.9782502010634,
12.));
#137264=CARTESIAN_POINT('Ctrl Pts',(-47.0807191061648,-53.9666916884596,
0.));
#137265=CARTESIAN_POINT('Ctrl Pts',(-47.0807191061648,-53.9666916884596,
12.));
#137266=CARTESIAN_POINT('Ctrl Pts',(-47.0605288804008,-53.95513498846,0.));
#137267=CARTESIAN_POINT('Ctrl Pts',(-47.0605288804008,-53.95513498846,12.));
#137268=CARTESIAN_POINT('Ctrl Pts',(-47.0403884276072,-53.9435802217436,
0.));
#137269=CARTESIAN_POINT('Ctrl Pts',(-47.0403884276072,-53.9435802217436,
12.));
#137270=CARTESIAN_POINT('Ctrl Pts',(-47.0202978277138,-53.9320275095853,
0.));
#137271=CARTESIAN_POINT('Ctrl Pts',(-47.0202978277138,-53.9320275095853,
12.));
#137272=CARTESIAN_POINT('Ctrl Pts',(-47.0002571609297,-53.9204769738596,
0.));
#137273=CARTESIAN_POINT('Ctrl Pts',(-47.0002571609297,-53.9204769738596,
12.));
#137274=CARTESIAN_POINT('Ctrl Pts',(-46.9802665077366,-53.9089287370463,
0.));
#137275=CARTESIAN_POINT('Ctrl Pts',(-46.9802665077366,-53.9089287370463,
12.));
#137276=CARTESIAN_POINT('Ctrl Pts',(-46.9603259488921,-53.8973829222348,
0.));
#137277=CARTESIAN_POINT('Ctrl Pts',(-46.9603259488921,-53.8973829222348,
12.));
#137278=CARTESIAN_POINT('Ctrl Pts',(-46.94043556544,-53.8858396531298,0.));
#137279=CARTESIAN_POINT('Ctrl Pts',(-46.94043556544,-53.8858396531298,12.));
#137280=CARTESIAN_POINT('Ctrl Pts',(-46.9205954387133,-53.8742990540563,
0.));
#137281=CARTESIAN_POINT('Ctrl Pts',(-46.9205954387133,-53.8742990540563,
12.));
#137282=CARTESIAN_POINT('Ctrl Pts',(-46.9008056503351,-53.8627612499638,
0.));
#137283=CARTESIAN_POINT('Ctrl Pts',(-46.9008056503351,-53.8627612499638,
12.));
#137284=CARTESIAN_POINT('Ctrl Pts',(-46.881066282213,-53.8512263664321,
0.));
#137285=CARTESIAN_POINT('Ctrl Pts',(-46.881066282213,-53.8512263664321,
12.));
#137286=CARTESIAN_POINT('Ctrl Pts',(-46.8613774165435,-53.8396945296757,
0.));
#137287=CARTESIAN_POINT('Ctrl Pts',(-46.8613774165435,-53.8396945296757,
12.));
#137288=CARTESIAN_POINT('Ctrl Pts',(-46.841739135822,-53.8281658665503,
0.));
#137289=CARTESIAN_POINT('Ctrl Pts',(-46.841739135822,-53.8281658665503,
12.));
#137290=CARTESIAN_POINT('Ctrl Pts',(-46.8221515228457,-53.816640504558,
0.));
#137291=CARTESIAN_POINT('Ctrl Pts',(-46.8221515228457,-53.816640504558,
12.));
#137292=CARTESIAN_POINT('Ctrl Pts',(-46.802614660715,-53.8051185718532,
0.));
#137293=CARTESIAN_POINT('Ctrl Pts',(-46.802614660715,-53.8051185718532,
12.));
#137294=CARTESIAN_POINT('Ctrl Pts',(-46.7831286328278,-53.793600197248,
0.));
#137295=CARTESIAN_POINT('Ctrl Pts',(-46.7831286328278,-53.793600197248,
12.));
#137296=CARTESIAN_POINT('Ctrl Pts',(-46.763693522886,-53.7820855102182,
0.));
#137297=CARTESIAN_POINT('Ctrl Pts',(-46.763693522886,-53.7820855102182,
12.));
#137298=CARTESIAN_POINT('Ctrl Pts',(-46.7443094149045,-53.7705746409076,
0.));
#137299=CARTESIAN_POINT('Ctrl Pts',(-46.7443094149045,-53.7705746409076,
12.));
#137300=CARTESIAN_POINT('Ctrl Pts',(-46.7249763932129,-53.7590677201342,
0.));
#137301=CARTESIAN_POINT('Ctrl Pts',(-46.7249763932129,-53.7590677201342,
12.));
#137302=CARTESIAN_POINT('Ctrl Pts',(-46.7056945424559,-53.7475648793946,
0.));
#137303=CARTESIAN_POINT('Ctrl Pts',(-46.7056945424559,-53.7475648793946,
12.));
#137304=CARTESIAN_POINT('Ctrl Pts',(-46.6864639475862,-53.7360662508675,
0.));
#137305=CARTESIAN_POINT('Ctrl Pts',(-46.6864639475862,-53.7360662508675,
12.));
#137306=CARTESIAN_POINT('Ctrl Pts',(-46.6672846938752,-53.7245719674221,
0.));
#137307=CARTESIAN_POINT('Ctrl Pts',(-46.6672846938752,-53.7245719674221,
12.));
#137308=CARTESIAN_POINT('Ctrl Pts',(-46.6481568669217,-53.7130821626262,
0.));
#137309=CARTESIAN_POINT('Ctrl Pts',(-46.6481568669217,-53.7130821626262,
12.));
#137310=CARTESIAN_POINT('Ctrl Pts',(-46.6290805526559,-53.7015969707541,
0.));
#137311=CARTESIAN_POINT('Ctrl Pts',(-46.6290805526559,-53.7015969707541,
12.));
#137312=CARTESIAN_POINT('Ctrl Pts',(-46.6100558373401,-53.690116526794,
0.));
#137313=CARTESIAN_POINT('Ctrl Pts',(-46.6100558373401,-53.690116526794,
12.));
#137314=CARTESIAN_POINT('Ctrl Pts',(-46.5910828075652,-53.678640966456,
0.));
#137315=CARTESIAN_POINT('Ctrl Pts',(-46.5910828075652,-53.678640966456,
12.));
#137316=CARTESIAN_POINT('Ctrl Pts',(-46.572161550259,-53.6671704261735,
0.));
#137317=CARTESIAN_POINT('Ctrl Pts',(-46.572161550259,-53.6671704261735,
12.));
#137318=CARTESIAN_POINT('Ctrl Pts',(-46.5532921526899,-53.6557050431069,
0.));
#137319=CARTESIAN_POINT('Ctrl Pts',(-46.5532921526899,-53.6557050431069,
12.));
#137320=CARTESIAN_POINT('Ctrl Pts',(-46.5344747024677,-53.6442449551455,
0.));
#137321=CARTESIAN_POINT('Ctrl Pts',(-46.5344747024677,-53.6442449551455,
12.));
#137322=CARTESIAN_POINT('Ctrl Pts',(-46.5157092875377,-53.6327903009098,
0.));
#137323=CARTESIAN_POINT('Ctrl Pts',(-46.5157092875377,-53.6327903009098,
12.));
#137324=CARTESIAN_POINT('Ctrl Pts',(-46.4969959961779,-53.6213412197542,
0.));
#137325=CARTESIAN_POINT('Ctrl Pts',(-46.4969959961779,-53.6213412197542,
12.));
#137326=CARTESIAN_POINT('Ctrl Pts',(-46.4783349170182,-53.6098978517869,
0.));
#137327=CARTESIAN_POINT('Ctrl Pts',(-46.4783349170182,-53.6098978517869,
12.));
#137328=CARTESIAN_POINT('Ctrl Pts',(-46.4597261390526,-53.5984603378862,
0.));
#137329=CARTESIAN_POINT('Ctrl Pts',(-46.4597261390526,-53.5984603378862,
12.));
#137330=CARTESIAN_POINT('Ctrl Pts',(-46.4411697516474,-53.5870288197161,
0.));
#137331=CARTESIAN_POINT('Ctrl Pts',(-46.4411697516474,-53.5870288197161,
12.));
#137332=CARTESIAN_POINT('Ctrl Pts',(-46.422665844546,-53.5756034397464,
0.));
#137333=CARTESIAN_POINT('Ctrl Pts',(-46.422665844546,-53.5756034397464,
12.));
#137334=CARTESIAN_POINT('Ctrl Pts',(-46.4042145078682,-53.5641843412537,
0.));
#137335=CARTESIAN_POINT('Ctrl Pts',(-46.4042145078682,-53.5641843412537,
12.));
#137336=CARTESIAN_POINT('Ctrl Pts',(-46.3858158321044,-53.552771668303,
0.));
#137337=CARTESIAN_POINT('Ctrl Pts',(-46.3858158321044,-53.552771668303,
12.));
#137338=CARTESIAN_POINT('Ctrl Pts',(-46.3674699081043,-53.5413655657323,
0.));
#137339=CARTESIAN_POINT('Ctrl Pts',(-46.3674699081043,-53.5413655657323,
12.));
#137340=CARTESIAN_POINT('Ctrl Pts',(-46.3491768270664,-53.5299661791396,
0.));
#137341=CARTESIAN_POINT('Ctrl Pts',(-46.3491768270664,-53.5299661791396,
12.));
#137342=CARTESIAN_POINT('Ctrl Pts',(-46.3309366805112,-53.518573654857,
0.));
#137343=CARTESIAN_POINT('Ctrl Pts',(-46.3309366805112,-53.518573654857,
12.));
#137344=CARTESIAN_POINT('Ctrl Pts',(-46.3127495603117,-53.5071881399932,
0.));
#137345=CARTESIAN_POINT('Ctrl Pts',(-46.3127495603117,-53.5071881399932,
12.));
#137346=CARTESIAN_POINT('Ctrl Pts',(-46.2946155587428,-53.4958097825019,
0.));
#137347=CARTESIAN_POINT('Ctrl Pts',(-46.2946155587428,-53.4958097825019,
12.));
#137348=CARTESIAN_POINT('Ctrl Pts',(-46.2765347685198,-53.4844387312414,
0.));
#137349=CARTESIAN_POINT('Ctrl Pts',(-46.2765347685198,-53.4844387312414,
12.));
#137350=CARTESIAN_POINT('Ctrl Pts',(-46.2585072828343,-53.4730751360359,
0.));
#137351=CARTESIAN_POINT('Ctrl Pts',(-46.2585072828343,-53.4730751360359,
12.));
#137352=CARTESIAN_POINT('Ctrl Pts',(-46.2405331953872,-53.4617191477382,
0.));
#137353=CARTESIAN_POINT('Ctrl Pts',(-46.2405331953872,-53.4617191477382,
12.));
#137354=CARTESIAN_POINT('Ctrl Pts',(-46.2226126003185,-53.4503709181158,
0.));
#137355=CARTESIAN_POINT('Ctrl Pts',(-46.2226126003185,-53.4503709181158,
12.));
#137356=CARTESIAN_POINT('Ctrl Pts',(-46.2047455921276,-53.4390305997263,
0.));
#137357=CARTESIAN_POINT('Ctrl Pts',(-46.2047455921276,-53.4390305997263,
12.));
#137358=CARTESIAN_POINT('Ctrl Pts',(-46.1869322656027,-53.4276983458129,
0.));
#137359=CARTESIAN_POINT('Ctrl Pts',(-46.1869322656027,-53.4276983458129,
12.));
#137360=CARTESIAN_POINT('Ctrl Pts',(-46.1691727157149,-53.4163743101535,
0.));
#137361=CARTESIAN_POINT('Ctrl Pts',(-46.1691727157149,-53.4163743101535,
12.));
#137362=CARTESIAN_POINT('Ctrl Pts',(-46.1514670376035,-53.4050586470463,
0.));
#137363=CARTESIAN_POINT('Ctrl Pts',(-46.1514670376035,-53.4050586470463,
12.));
#137364=CARTESIAN_POINT('Ctrl Pts',(-46.1338153268116,-53.3937515116572,
0.));
#137365=CARTESIAN_POINT('Ctrl Pts',(-46.1338153268116,-53.3937515116572,
12.));
#137366=CARTESIAN_POINT('Ctrl Pts',(-46.1162176794891,-53.3824530603284,
0.));
#137367=CARTESIAN_POINT('Ctrl Pts',(-46.1162176794891,-53.3824530603284,
12.));
#137368=CARTESIAN_POINT('Ctrl Pts',(-46.0986741925646,-53.3711634508426,
0.));
#137369=CARTESIAN_POINT('Ctrl Pts',(-46.0986741925646,-53.3711634508426,
12.));
#137370=CARTESIAN_POINT('Ctrl Pts',(-46.0811849640195,-53.3598828428519,
0.));
#137371=CARTESIAN_POINT('Ctrl Pts',(-46.0811849640195,-53.3598828428519,
12.));
#137372=CARTESIAN_POINT('Ctrl Pts',(-46.0637500926954,-53.3486113975868,
0.));
#137373=CARTESIAN_POINT('Ctrl Pts',(-46.0637500926954,-53.3486113975868,
12.));
#137374=CARTESIAN_POINT('Ctrl Pts',(-46.046369677778,-53.3373492770647,
0.));
#137375=CARTESIAN_POINT('Ctrl Pts',(-46.046369677778,-53.3373492770647,
12.));
#137376=CARTESIAN_POINT('Ctrl Pts',(-46.0290438183598,-53.3260966434277,
0.));
#137377=CARTESIAN_POINT('Ctrl Pts',(-46.0290438183598,-53.3260966434277,
12.));
#137378=CARTESIAN_POINT('Ctrl Pts',(-46.0117726129893,-53.3148536582658,
0.));
#137379=CARTESIAN_POINT('Ctrl Pts',(-46.0117726129893,-53.3148536582658,
12.));
#137380=CARTESIAN_POINT('Ctrl Pts',(-45.9945561591486,-53.3036204818367,
0.));
#137381=CARTESIAN_POINT('Ctrl Pts',(-45.9945561591486,-53.3036204818367,
12.));
#137382=CARTESIAN_POINT('Ctrl Pts',(-45.9773945542415,-53.2923972745585,
0.));
#137383=CARTESIAN_POINT('Ctrl Pts',(-45.9773945542415,-53.2923972745585,
12.));
#137384=CARTESIAN_POINT('Ctrl Pts',(-45.9602878967715,-53.2811841987945,
0.));
#137385=CARTESIAN_POINT('Ctrl Pts',(-45.9602878967715,-53.2811841987945,
12.));
#137386=CARTESIAN_POINT('Ctrl Pts',(-45.9432362873001,-53.2699814203097,
0.));
#137387=CARTESIAN_POINT('Ctrl Pts',(-45.9432362873001,-53.2699814203097,
12.));
#137388=CARTESIAN_POINT('Ctrl Pts',(-45.9262398298323,-53.2587891103835,
0.));
#137389=CARTESIAN_POINT('Ctrl Pts',(-45.9262398298323,-53.2587891103835,
12.));
#137390=CARTESIAN_POINT('Ctrl Pts',(-45.9092986319343,-53.2476074459977,
0.));
#137391=CARTESIAN_POINT('Ctrl Pts',(-45.9092986319343,-53.2476074459977,
12.));
#137392=CARTESIAN_POINT('Ctrl Pts',(-45.8924128018354,-53.2364366054276,
0.));
#137393=CARTESIAN_POINT('Ctrl Pts',(-45.8924128018354,-53.2364366054276,
12.));
#137394=CARTESIAN_POINT('Ctrl Pts',(-45.8755824458715,-53.2252767643652,
0.));
#137395=CARTESIAN_POINT('Ctrl Pts',(-45.8755824458715,-53.2252767643652,
12.));
#137396=CARTESIAN_POINT('Ctrl Pts',(-45.8588076662598,-53.2141280925458,
0.));
#137397=CARTESIAN_POINT('Ctrl Pts',(-45.8588076662598,-53.2141280925458,
12.));
#137398=CARTESIAN_POINT('Ctrl Pts',(-45.8420885575386,-53.2029907483602,
0.));
#137399=CARTESIAN_POINT('Ctrl Pts',(-45.8420885575386,-53.2029907483602,
12.));
#137400=CARTESIAN_POINT('Ctrl Pts',(-45.8254252100003,-53.1918648840598,
0.));
#137401=CARTESIAN_POINT('Ctrl Pts',(-45.8254252100003,-53.1918648840598,
12.));
#137402=CARTESIAN_POINT('Ctrl Pts',(-45.8088177165124,-53.1807506560977,
0.));
#137403=CARTESIAN_POINT('Ctrl Pts',(-45.8088177165124,-53.1807506560977,
12.));
#137404=CARTESIAN_POINT('Ctrl Pts',(-45.7922661780005,-53.1696482334487,
0.));
#137405=CARTESIAN_POINT('Ctrl Pts',(-45.7922661780005,-53.1696482334487,
12.));
#137406=CARTESIAN_POINT('Ctrl Pts',(-45.7757707100568,-53.158557807638,
0.));
#137407=CARTESIAN_POINT('Ctrl Pts',(-45.7757707100568,-53.158557807638,
12.));
#137408=CARTESIAN_POINT('Ctrl Pts',(-45.7593314474413,-53.147479599594,
0.));
#137409=CARTESIAN_POINT('Ctrl Pts',(-45.7593314474413,-53.147479599594,
12.));
#137410=CARTESIAN_POINT('Ctrl Pts',(-45.7429485300727,-53.136413838457,
0.));
#137411=CARTESIAN_POINT('Ctrl Pts',(-45.7429485300727,-53.136413838457,
12.));
#137412=CARTESIAN_POINT('Ctrl Pts',(-45.7266220896951,-53.1253607414806,
0.));
#137413=CARTESIAN_POINT('Ctrl Pts',(-45.7266220896951,-53.1253607414806,
12.));
#137414=CARTESIAN_POINT('Ctrl Pts',(-45.7103522376744,-53.1143204954981,
0.));
#137415=CARTESIAN_POINT('Ctrl Pts',(-45.7103522376744,-53.1143204954981,
12.));
#137416=CARTESIAN_POINT('Ctrl Pts',(-45.6941390489239,-53.1032932329074,
0.));
#137417=CARTESIAN_POINT('Ctrl Pts',(-45.6941390489239,-53.1032932329074,
12.));
#137418=CARTESIAN_POINT('Ctrl Pts',(-45.6779825614486,-53.0922790298736,
0.));
#137419=CARTESIAN_POINT('Ctrl Pts',(-45.6779825614486,-53.0922790298736,
12.));
#137420=CARTESIAN_POINT('Ctrl Pts',(-45.6651027439479,-53.083478145185,
0.));
#137421=CARTESIAN_POINT('Ctrl Pts',(-45.6651027439479,-53.083478145185,
12.));
#137422=CARTESIAN_POINT('Ctrl Pts',(-45.6554684028296,-53.0768833804386,
0.));
#137423=CARTESIAN_POINT('Ctrl Pts',(-45.6554684028296,-53.0768833804386,
12.));
#137424=CARTESIAN_POINT('Ctrl Pts',(-45.6490568514146,-53.0724894921921,
0.));
#137425=CARTESIAN_POINT('Ctrl Pts',(-45.6490568514146,-53.0724894921921,
12.));
#137426=CARTESIAN_POINT('Ctrl Pts',(-45.6458539113724,-53.0702932034641,
0.));
#137427=CARTESIAN_POINT('Ctrl Pts',(-45.6458539113724,-53.0702932034641,
12.));
#137428=CARTESIAN_POINT('',(-45.6458539113724,-53.0702932034641,12.));
#137429=CARTESIAN_POINT('Ctrl Pts',(-45.6458539113724,-53.0702932034641,
12.));
#137430=CARTESIAN_POINT('Ctrl Pts',(-45.6490568514146,-53.0724894921921,
12.));
#137431=CARTESIAN_POINT('Ctrl Pts',(-45.6554684028296,-53.0768833804386,
12.));
#137432=CARTESIAN_POINT('Ctrl Pts',(-45.6651027439479,-53.083478145185,
12.));
#137433=CARTESIAN_POINT('Ctrl Pts',(-45.6779825614486,-53.0922790298736,
12.));
#137434=CARTESIAN_POINT('Ctrl Pts',(-45.6941390489239,-53.1032932329074,
12.));
#137435=CARTESIAN_POINT('Ctrl Pts',(-45.7103522376744,-53.1143204954981,
12.));
#137436=CARTESIAN_POINT('Ctrl Pts',(-45.7266220896951,-53.1253607414806,
12.));
#137437=CARTESIAN_POINT('Ctrl Pts',(-45.7429485300727,-53.136413838457,
12.));
#137438=CARTESIAN_POINT('Ctrl Pts',(-45.7593314474413,-53.147479599594,
12.));
#137439=CARTESIAN_POINT('Ctrl Pts',(-45.7757707100568,-53.158557807638,
12.));
#137440=CARTESIAN_POINT('Ctrl Pts',(-45.7922661780005,-53.1696482334487,
12.));
#137441=CARTESIAN_POINT('Ctrl Pts',(-45.8088177165124,-53.1807506560977,
12.));
#137442=CARTESIAN_POINT('Ctrl Pts',(-45.8254252100003,-53.1918648840598,
12.));
#137443=CARTESIAN_POINT('Ctrl Pts',(-45.8420885575386,-53.2029907483602,
12.));
#137444=CARTESIAN_POINT('Ctrl Pts',(-45.8588076662598,-53.2141280925458,
12.));
#137445=CARTESIAN_POINT('Ctrl Pts',(-45.8755824458715,-53.2252767643652,
12.));
#137446=CARTESIAN_POINT('Ctrl Pts',(-45.8924128018354,-53.2364366054276,
12.));
#137447=CARTESIAN_POINT('Ctrl Pts',(-45.9092986319343,-53.2476074459977,
12.));
#137448=CARTESIAN_POINT('Ctrl Pts',(-45.9262398298323,-53.2587891103835,
12.));
#137449=CARTESIAN_POINT('Ctrl Pts',(-45.9432362873001,-53.2699814203097,
12.));
#137450=CARTESIAN_POINT('Ctrl Pts',(-45.9602878967715,-53.2811841987945,
12.));
#137451=CARTESIAN_POINT('Ctrl Pts',(-45.9773945542415,-53.2923972745585,
12.));
#137452=CARTESIAN_POINT('Ctrl Pts',(-45.9945561591486,-53.3036204818367,
12.));
#137453=CARTESIAN_POINT('Ctrl Pts',(-46.0117726129893,-53.3148536582658,
12.));
#137454=CARTESIAN_POINT('Ctrl Pts',(-46.0290438183598,-53.3260966434277,
12.));
#137455=CARTESIAN_POINT('Ctrl Pts',(-46.046369677778,-53.3373492770647,
12.));
#137456=CARTESIAN_POINT('Ctrl Pts',(-46.0637500926954,-53.3486113975868,
12.));
#137457=CARTESIAN_POINT('Ctrl Pts',(-46.0811849640195,-53.3598828428519,
12.));
#137458=CARTESIAN_POINT('Ctrl Pts',(-46.0986741925646,-53.3711634508426,
12.));
#137459=CARTESIAN_POINT('Ctrl Pts',(-46.1162176794891,-53.3824530603284,
12.));
#137460=CARTESIAN_POINT('Ctrl Pts',(-46.1338153268116,-53.3937515116572,
12.));
#137461=CARTESIAN_POINT('Ctrl Pts',(-46.1514670376035,-53.4050586470463,
12.));
#137462=CARTESIAN_POINT('Ctrl Pts',(-46.1691727157149,-53.4163743101535,
12.));
#137463=CARTESIAN_POINT('Ctrl Pts',(-46.1869322656027,-53.4276983458129,
12.));
#137464=CARTESIAN_POINT('Ctrl Pts',(-46.2047455921276,-53.4390305997263,
12.));
#137465=CARTESIAN_POINT('Ctrl Pts',(-46.2226126003185,-53.4503709181158,
12.));
#137466=CARTESIAN_POINT('Ctrl Pts',(-46.2405331953872,-53.4617191477382,
12.));
#137467=CARTESIAN_POINT('Ctrl Pts',(-46.2585072828343,-53.4730751360359,
12.));
#137468=CARTESIAN_POINT('Ctrl Pts',(-46.2765347685198,-53.4844387312414,
12.));
#137469=CARTESIAN_POINT('Ctrl Pts',(-46.2946155587428,-53.4958097825019,
12.));
#137470=CARTESIAN_POINT('Ctrl Pts',(-46.3127495603117,-53.5071881399932,
12.));
#137471=CARTESIAN_POINT('Ctrl Pts',(-46.3309366805112,-53.518573654857,
12.));
#137472=CARTESIAN_POINT('Ctrl Pts',(-46.3491768270664,-53.5299661791396,
12.));
#137473=CARTESIAN_POINT('Ctrl Pts',(-46.3674699081043,-53.5413655657323,
12.));
#137474=CARTESIAN_POINT('Ctrl Pts',(-46.3858158321044,-53.552771668303,
12.));
#137475=CARTESIAN_POINT('Ctrl Pts',(-46.4042145078682,-53.5641843412537,
12.));
#137476=CARTESIAN_POINT('Ctrl Pts',(-46.422665844546,-53.5756034397464,
12.));
#137477=CARTESIAN_POINT('Ctrl Pts',(-46.4411697516474,-53.5870288197161,
12.));
#137478=CARTESIAN_POINT('Ctrl Pts',(-46.4597261390526,-53.5984603378862,
12.));
#137479=CARTESIAN_POINT('Ctrl Pts',(-46.4783349170182,-53.6098978517869,
12.));
#137480=CARTESIAN_POINT('Ctrl Pts',(-46.4969959961779,-53.6213412197542,
12.));
#137481=CARTESIAN_POINT('Ctrl Pts',(-46.5157092875377,-53.6327903009098,
12.));
#137482=CARTESIAN_POINT('Ctrl Pts',(-46.5344747024677,-53.6442449551455,
12.));
#137483=CARTESIAN_POINT('Ctrl Pts',(-46.5532921526899,-53.6557050431069,
12.));
#137484=CARTESIAN_POINT('Ctrl Pts',(-46.572161550259,-53.6671704261735,
12.));
#137485=CARTESIAN_POINT('Ctrl Pts',(-46.5910828075652,-53.678640966456,
12.));
#137486=CARTESIAN_POINT('Ctrl Pts',(-46.6100558373401,-53.690116526794,
12.));
#137487=CARTESIAN_POINT('Ctrl Pts',(-46.6290805526559,-53.7015969707541,
12.));
#137488=CARTESIAN_POINT('Ctrl Pts',(-46.6481568669217,-53.7130821626262,
12.));
#137489=CARTESIAN_POINT('Ctrl Pts',(-46.6672846938752,-53.7245719674221,
12.));
#137490=CARTESIAN_POINT('Ctrl Pts',(-46.6864639475862,-53.7360662508675,
12.));
#137491=CARTESIAN_POINT('Ctrl Pts',(-46.7056945424559,-53.7475648793946,
12.));
#137492=CARTESIAN_POINT('Ctrl Pts',(-46.7249763932129,-53.7590677201342,
12.));
#137493=CARTESIAN_POINT('Ctrl Pts',(-46.7443094149045,-53.7705746409076,
12.));
#137494=CARTESIAN_POINT('Ctrl Pts',(-46.763693522886,-53.7820855102182,
12.));
#137495=CARTESIAN_POINT('Ctrl Pts',(-46.7831286328278,-53.793600197248,
12.));
#137496=CARTESIAN_POINT('Ctrl Pts',(-46.802614660715,-53.8051185718532,
12.));
#137497=CARTESIAN_POINT('Ctrl Pts',(-46.8221515228457,-53.816640504558,
12.));
#137498=CARTESIAN_POINT('Ctrl Pts',(-46.841739135822,-53.8281658665503,
12.));
#137499=CARTESIAN_POINT('Ctrl Pts',(-46.8613774165435,-53.8396945296757,
12.));
#137500=CARTESIAN_POINT('Ctrl Pts',(-46.881066282213,-53.8512263664321,
12.));
#137501=CARTESIAN_POINT('Ctrl Pts',(-46.9008056503351,-53.8627612499638,
12.));
#137502=CARTESIAN_POINT('Ctrl Pts',(-46.9205954387133,-53.8742990540563,
12.));
#137503=CARTESIAN_POINT('Ctrl Pts',(-46.94043556544,-53.8858396531298,12.));
#137504=CARTESIAN_POINT('Ctrl Pts',(-46.9603259488921,-53.8973829222348,
12.));
#137505=CARTESIAN_POINT('Ctrl Pts',(-46.9802665077366,-53.9089287370463,
12.));
#137506=CARTESIAN_POINT('Ctrl Pts',(-47.0002571609297,-53.9204769738596,
12.));
#137507=CARTESIAN_POINT('Ctrl Pts',(-47.0202978277138,-53.9320275095853,
12.));
#137508=CARTESIAN_POINT('Ctrl Pts',(-47.0403884276072,-53.9435802217436,
12.));
#137509=CARTESIAN_POINT('Ctrl Pts',(-47.0605288804008,-53.95513498846,12.));
#137510=CARTESIAN_POINT('Ctrl Pts',(-47.0807191061648,-53.9666916884596,
12.));
#137511=CARTESIAN_POINT('Ctrl Pts',(-47.1009590252458,-53.9782502010634,
12.));
#137512=CARTESIAN_POINT('Ctrl Pts',(-47.1212485582643,-53.989810406182,
12.));
#137513=CARTESIAN_POINT('Ctrl Pts',(-47.1415876261035,-54.0013721843118,
12.));
#137514=CARTESIAN_POINT('Ctrl Pts',(-47.1619761499087,-54.0129354165297,
12.));
#137515=CARTESIAN_POINT('Ctrl Pts',(-47.1824140510926,-54.0244999844893,
12.));
#137516=CARTESIAN_POINT('Ctrl Pts',(-47.202901251334,-54.0360657704163,
12.));
#137517=CARTESIAN_POINT('Ctrl Pts',(-47.2234376725743,-54.047632657104,
12.));
#137518=CARTESIAN_POINT('Ctrl Pts',(-47.2440232370065,-54.0592005279086,
12.));
#137519=CARTESIAN_POINT('Ctrl Pts',(-47.2646578670746,-54.0707692667438,
12.));
#137520=CARTESIAN_POINT('Ctrl Pts',(-47.2853414854793,-54.0823387580776,
12.));
#137521=CARTESIAN_POINT('Ctrl Pts',(-47.3060740151752,-54.0939088869269,
12.));
#137522=CARTESIAN_POINT('Ctrl Pts',(-47.3268553793694,-54.1054795388543,
12.));
#137523=CARTESIAN_POINT('Ctrl Pts',(-47.3476855015102,-54.1170505999645,
12.));
#137524=CARTESIAN_POINT('Ctrl Pts',(-47.3685643052874,-54.1286219568989,
12.));
#137525=CARTESIAN_POINT('Ctrl Pts',(-47.3894917146365,-54.1401934968311,
12.));
#137526=CARTESIAN_POINT('Ctrl Pts',(-47.4104676537381,-54.1517651074637,
12.));
#137527=CARTESIAN_POINT('Ctrl Pts',(-47.4314920470141,-54.1633366770239,
12.));
#137528=CARTESIAN_POINT('Ctrl Pts',(-47.4525648191173,-54.1749080942593,
12.));
#137529=CARTESIAN_POINT('Ctrl Pts',(-47.4736858949322,-54.1864792484345,
12.));
#137530=CARTESIAN_POINT('Ctrl Pts',(-47.4948551995801,-54.198050029327,
12.));
#137531=CARTESIAN_POINT('Ctrl Pts',(-47.5160726584174,-54.209620327223,
12.));
#137532=CARTESIAN_POINT('Ctrl Pts',(-47.5373381970326,-54.2211900329138,
12.));
#137533=CARTESIAN_POINT('Ctrl Pts',(-47.5586517412363,-54.2327590376924,
12.));
#137534=CARTESIAN_POINT('Ctrl Pts',(-47.5800132170608,-54.244327233349,
12.));
#137535=CARTESIAN_POINT('Ctrl Pts',(-47.6014225507659,-54.2558945121678,
12.));
#137536=CARTESIAN_POINT('Ctrl Pts',(-47.6228796688375,-54.2674607669226,
12.));
#137537=CARTESIAN_POINT('Ctrl Pts',(-47.6443844979848,-54.2790258908738,
12.));
#137538=CARTESIAN_POINT('Ctrl Pts',(-47.6659369651301,-54.290589777765,
12.));
#137539=CARTESIAN_POINT('Ctrl Pts',(-47.6875369974087,-54.302152321819,
12.));
#137540=CARTESIAN_POINT('Ctrl Pts',(-47.7091845221747,-54.3137134177345,
12.));
#137541=CARTESIAN_POINT('Ctrl Pts',(-47.7308794669993,-54.3252729606823,
12.));
#137542=CARTESIAN_POINT('Ctrl Pts',(-47.7526217596694,-54.3368308463023,
12.));
#137543=CARTESIAN_POINT('Ctrl Pts',(-47.7744113281771,-54.3483869707002,
12.));
#137544=CARTESIAN_POINT('Ctrl Pts',(-47.7962481007185,-54.3599412304438,
12.));
#137545=CARTESIAN_POINT('Ctrl Pts',(-47.8181320056995,-54.3714935225591,
12.));
#137546=CARTESIAN_POINT('Ctrl Pts',(-47.8400629717355,-54.3830437445279,
12.));
#137547=CARTESIAN_POINT('Ctrl Pts',(-47.8620409276493,-54.3945917942832,
12.));
#137548=CARTESIAN_POINT('Ctrl Pts',(-47.8840658024618,-54.4061375702079,
12.));
#137549=CARTESIAN_POINT('Ctrl Pts',(-47.9061375253897,-54.4176809711311,
12.));
#137550=CARTESIAN_POINT('Ctrl Pts',(-47.9282560258516,-54.429221896324,
12.));
#137551=CARTESIAN_POINT('Ctrl Pts',(-47.9504212334675,-54.4407602454967,
12.));
#137552=CARTESIAN_POINT('Ctrl Pts',(-47.9726330780572,-54.4522959187955,
12.));
#137553=CARTESIAN_POINT('Ctrl Pts',(-47.9948914896326,-54.4638288168003,
12.));
#137554=CARTESIAN_POINT('Ctrl Pts',(-48.0171963983924,-54.4753588405215,
12.));
#137555=CARTESIAN_POINT('Ctrl Pts',(-48.0395477347298,-54.4868858913971,
12.));
#137556=CARTESIAN_POINT('Ctrl Pts',(-48.0619454292324,-54.4984098712886,
12.));
#137557=CARTESIAN_POINT('Ctrl Pts',(-48.0843894126806,-54.5099306824786,
12.));
#137558=CARTESIAN_POINT('Ctrl Pts',(-48.1068796160405,-54.5214482276678,
12.));
#137559=CARTESIAN_POINT('Ctrl Pts',(-48.1294159704573,-54.5329624099721,
12.));
#137560=CARTESIAN_POINT('Ctrl Pts',(-48.1519984072622,-54.5444731329201,
12.));
#137561=CARTESIAN_POINT('Ctrl Pts',(-48.1746268579736,-54.5559803004492,
12.));
#137562=CARTESIAN_POINT('Ctrl Pts',(-48.1973012542966,-54.5674838169041,
12.));
#137563=CARTESIAN_POINT('Ctrl Pts',(-48.2200215281173,-54.5789835870342,
12.));
#137564=CARTESIAN_POINT('Ctrl Pts',(-48.2427876114947,-54.5904795159926,
12.));
#137565=CARTESIAN_POINT('Ctrl Pts',(-48.2655994366665,-54.6019715093309,
12.));
#137566=CARTESIAN_POINT('Ctrl Pts',(-48.2884569360506,-54.6134594729959,
12.));
#137567=CARTESIAN_POINT('Ctrl Pts',(-48.3113600422443,-54.6249433133261,
12.));
#137568=CARTESIAN_POINT('Ctrl Pts',(-48.3343086880194,-54.6364229370494,
12.));
#137569=CARTESIAN_POINT('Ctrl Pts',(-48.3573028063124,-54.6478982512794,
12.));
#137570=CARTESIAN_POINT('Ctrl Pts',(-48.3803423302294,-54.6593691635145,
12.));
#137571=CARTESIAN_POINT('Ctrl Pts',(-48.4034271930514,-54.6708355816358,
12.));
#137572=CARTESIAN_POINT('Ctrl Pts',(-48.426557328234,-54.6822974139064,
12.));
#137573=CARTESIAN_POINT('Ctrl Pts',(-48.4497326694052,-54.6937545689695,
12.));
#137574=CARTESIAN_POINT('Ctrl Pts',(-48.472953150357,-54.7052069558497,
12.));
#137575=CARTESIAN_POINT('Ctrl Pts',(-48.4962187050457,-54.716654483948,
12.));
#137576=CARTESIAN_POINT('Ctrl Pts',(-48.519529267596,-54.7280970630351,
12.));
#137577=CARTESIAN_POINT('Ctrl Pts',(-48.5428847722977,-54.7395346032453,
12.));
#137578=CARTESIAN_POINT('Ctrl Pts',(-48.5662851536026,-54.7509670150714,
12.));
#137579=CARTESIAN_POINT('Ctrl Pts',(-48.5897303461125,-54.7623942093586,
12.));
#137580=CARTESIAN_POINT('Ctrl Pts',(-48.6132202845783,-54.7738160973032,
12.));
#137581=CARTESIAN_POINT('Ctrl Pts',(-48.6367549039112,-54.7852325904583,
12.));
#137582=CARTESIAN_POINT('Ctrl Pts',(-48.6603341391886,-54.796643600739,
12.));
#137583=CARTESIAN_POINT('Ctrl Pts',(-48.6839579256566,-54.8080490404275,
12.));
#137584=CARTESIAN_POINT('Ctrl Pts',(-48.7076261987292,-54.819448822181,
12.));
#137585=CARTESIAN_POINT('Ctrl Pts',(-48.7313388939845,-54.8308428590344,
12.));
#137586=CARTESIAN_POINT('Ctrl Pts',(-48.7550959471601,-54.8422310643763,
12.));
#137587=CARTESIAN_POINT('Ctrl Pts',(-48.7788972941438,-54.8536133519292,
12.));
#137588=CARTESIAN_POINT('Ctrl Pts',(-48.8027428709614,-54.8649896357285,
12.));
#137589=CARTESIAN_POINT('Ctrl Pts',(-48.8266326137622,-54.8763598301037,
12.));
#137590=CARTESIAN_POINT('Ctrl Pts',(-48.8505664587974,-54.8877238496566,
12.));
#137591=CARTESIAN_POINT('Ctrl Pts',(-48.8745443424477,-54.8990816092953,
12.));
#137592=CARTESIAN_POINT('Ctrl Pts',(-48.8985662012528,-54.9104330242742,
12.));
#137593=CARTESIAN_POINT('Ctrl Pts',(-48.9226319719369,-54.9217780102355,
12.));
#137594=CARTESIAN_POINT('Ctrl Pts',(-48.9467415914269,-54.9331164832424,
12.));
#137595=CARTESIAN_POINT('Ctrl Pts',(-48.9708949968795,-54.9444483598378,
12.));
#137596=CARTESIAN_POINT('Ctrl Pts',(-48.9950921256527,-54.9557735569943,
12.));
#137597=CARTESIAN_POINT('Ctrl Pts',(-49.0193329152479,-54.9670919920029,
12.));
#137598=CARTESIAN_POINT('Ctrl Pts',(-49.0436173032528,-54.9784035823766,
12.));
#137599=CARTESIAN_POINT('Ctrl Pts',(-49.067945227287,-54.9897082457606,
12.));
#137600=CARTESIAN_POINT('Ctrl Pts',(-49.0923166249219,-55.0010058998107,
12.));
#137601=CARTESIAN_POINT('Ctrl Pts',(-49.116731433673,-55.012296462186,12.));
#137602=CARTESIAN_POINT('Ctrl Pts',(-49.1411895911635,-55.0235798508045,
12.));
#137603=CARTESIAN_POINT('Ctrl Pts',(-49.1656910352476,-55.0348559840453,
12.));
#137604=CARTESIAN_POINT('Ctrl Pts',(-49.1902357041461,-55.0461247809744,
12.));
#137605=CARTESIAN_POINT('Ctrl Pts',(-49.2148235365704,-55.0573861615579,
12.));
#137606=CARTESIAN_POINT('Ctrl Pts',(-49.2394544718531,-55.0686400468931,
12.));
#137607=CARTESIAN_POINT('Ctrl Pts',(-49.264128449652,-55.079886358701,12.));
#137608=CARTESIAN_POINT('Ctrl Pts',(-49.2888454096563,-55.0911250188302,
12.));
#137609=CARTESIAN_POINT('Ctrl Pts',(-49.3136052912622,-55.102355948714,
12.));
#137610=CARTESIAN_POINT('Ctrl Pts',(-49.3384080333155,-55.1135790689464,
12.));
#137611=CARTESIAN_POINT('Ctrl Pts',(-49.3632535736715,-55.1247942985619,
12.));
#137612=CARTESIAN_POINT('Ctrl Pts',(-49.3881418495489,-55.1360015556221,
12.));
#137613=CARTESIAN_POINT('Ctrl Pts',(-49.4130727983201,-55.1472007585183,
12.));
#137614=CARTESIAN_POINT('Ctrl Pts',(-49.4380463581965,-55.1583918271116,
12.));
#137615=CARTESIAN_POINT('Ctrl Pts',(-49.4630624688793,-55.1695746838174,
12.));
#137616=CARTESIAN_POINT('Ctrl Pts',(-49.4881210723966,-55.1807492550119,
12.));
#137617=CARTESIAN_POINT('Ctrl Pts',(-49.5132221132992,-55.1919154713647,
12.));
#137618=CARTESIAN_POINT('Ctrl Pts',(-49.5347748994759,-55.2014798624093,
12.));
#137619=CARTESIAN_POINT('Ctrl Pts',(-49.551321852449,-55.2088081099093,
12.));
#137620=CARTESIAN_POINT('Ctrl Pts',(-49.5628442142132,-55.2139039604721,
12.));
#137621=CARTESIAN_POINT('Ctrl Pts',(-49.5693295981927,-55.2167699151339,
12.));
#137622=CARTESIAN_POINT('Ctrl Pts',(-49.5707719660638,-55.2174072001495,
12.));
#137623=CARTESIAN_POINT('',(-45.6458539113724,-53.0702932034641,0.));
#137624=CARTESIAN_POINT('',(-45.6458539113724,-53.0702932034641,0.));
#137625=CARTESIAN_POINT('Ctrl Pts',(-49.5707719660638,-55.2174072001495,
0.));
#137626=CARTESIAN_POINT('Ctrl Pts',(-49.5693295981927,-55.2167699151339,
0.));
#137627=CARTESIAN_POINT('Ctrl Pts',(-49.5628442142132,-55.2139039604721,
0.));
#137628=CARTESIAN_POINT('Ctrl Pts',(-49.551321852449,-55.2088081099093,
0.));
#137629=CARTESIAN_POINT('Ctrl Pts',(-49.5347748994759,-55.2014798624093,
0.));
#137630=CARTESIAN_POINT('Ctrl Pts',(-49.5132221132992,-55.1919154713647,
0.));
#137631=CARTESIAN_POINT('Ctrl Pts',(-49.4881210723966,-55.1807492550119,
0.));
#137632=CARTESIAN_POINT('Ctrl Pts',(-49.4630624688793,-55.1695746838174,
0.));
#137633=CARTESIAN_POINT('Ctrl Pts',(-49.4380463581965,-55.1583918271116,
0.));
#137634=CARTESIAN_POINT('Ctrl Pts',(-49.4130727983201,-55.1472007585183,
0.));
#137635=CARTESIAN_POINT('Ctrl Pts',(-49.3881418495489,-55.1360015556221,
0.));
#137636=CARTESIAN_POINT('Ctrl Pts',(-49.3632535736715,-55.1247942985619,
0.));
#137637=CARTESIAN_POINT('Ctrl Pts',(-49.3384080333155,-55.1135790689464,
0.));
#137638=CARTESIAN_POINT('Ctrl Pts',(-49.3136052912622,-55.102355948714,
0.));
#137639=CARTESIAN_POINT('Ctrl Pts',(-49.2888454096563,-55.0911250188302,
0.));
#137640=CARTESIAN_POINT('Ctrl Pts',(-49.264128449652,-55.079886358701,0.));
#137641=CARTESIAN_POINT('Ctrl Pts',(-49.2394544718531,-55.0686400468931,
0.));
#137642=CARTESIAN_POINT('Ctrl Pts',(-49.2148235365704,-55.0573861615579,
0.));
#137643=CARTESIAN_POINT('Ctrl Pts',(-49.1902357041461,-55.0461247809744,
0.));
#137644=CARTESIAN_POINT('Ctrl Pts',(-49.1656910352476,-55.0348559840453,
0.));
#137645=CARTESIAN_POINT('Ctrl Pts',(-49.1411895911635,-55.0235798508045,
0.));
#137646=CARTESIAN_POINT('Ctrl Pts',(-49.116731433673,-55.012296462186,0.));
#137647=CARTESIAN_POINT('Ctrl Pts',(-49.0923166249219,-55.0010058998107,
0.));
#137648=CARTESIAN_POINT('Ctrl Pts',(-49.067945227287,-54.9897082457606,
0.));
#137649=CARTESIAN_POINT('Ctrl Pts',(-49.0436173032528,-54.9784035823766,
0.));
#137650=CARTESIAN_POINT('Ctrl Pts',(-49.0193329152479,-54.9670919920029,
0.));
#137651=CARTESIAN_POINT('Ctrl Pts',(-48.9950921256527,-54.9557735569943,
0.));
#137652=CARTESIAN_POINT('Ctrl Pts',(-48.9708949968795,-54.9444483598378,
0.));
#137653=CARTESIAN_POINT('Ctrl Pts',(-48.9467415914269,-54.9331164832424,
0.));
#137654=CARTESIAN_POINT('Ctrl Pts',(-48.9226319719369,-54.9217780102355,
0.));
#137655=CARTESIAN_POINT('Ctrl Pts',(-48.8985662012528,-54.9104330242742,
0.));
#137656=CARTESIAN_POINT('Ctrl Pts',(-48.8745443424477,-54.8990816092953,
0.));
#137657=CARTESIAN_POINT('Ctrl Pts',(-48.8505664587974,-54.8877238496566,
0.));
#137658=CARTESIAN_POINT('Ctrl Pts',(-48.8266326137622,-54.8763598301037,
0.));
#137659=CARTESIAN_POINT('Ctrl Pts',(-48.8027428709614,-54.8649896357285,
0.));
#137660=CARTESIAN_POINT('Ctrl Pts',(-48.7788972941438,-54.8536133519292,
0.));
#137661=CARTESIAN_POINT('Ctrl Pts',(-48.7550959471601,-54.8422310643763,
0.));
#137662=CARTESIAN_POINT('Ctrl Pts',(-48.7313388939845,-54.8308428590344,
0.));
#137663=CARTESIAN_POINT('Ctrl Pts',(-48.7076261987292,-54.819448822181,
0.));
#137664=CARTESIAN_POINT('Ctrl Pts',(-48.6839579256566,-54.8080490404275,
0.));
#137665=CARTESIAN_POINT('Ctrl Pts',(-48.6603341391886,-54.796643600739,
0.));
#137666=CARTESIAN_POINT('Ctrl Pts',(-48.6367549039112,-54.7852325904583,
0.));
#137667=CARTESIAN_POINT('Ctrl Pts',(-48.6132202845783,-54.7738160973032,
0.));
#137668=CARTESIAN_POINT('Ctrl Pts',(-48.5897303461125,-54.7623942093586,
0.));
#137669=CARTESIAN_POINT('Ctrl Pts',(-48.5662851536026,-54.7509670150714,
0.));
#137670=CARTESIAN_POINT('Ctrl Pts',(-48.5428847722977,-54.7395346032453,
0.));
#137671=CARTESIAN_POINT('Ctrl Pts',(-48.519529267596,-54.7280970630351,
0.));
#137672=CARTESIAN_POINT('Ctrl Pts',(-48.4962187050457,-54.716654483948,
0.));
#137673=CARTESIAN_POINT('Ctrl Pts',(-48.472953150357,-54.7052069558497,
0.));
#137674=CARTESIAN_POINT('Ctrl Pts',(-48.4497326694052,-54.6937545689695,
0.));
#137675=CARTESIAN_POINT('Ctrl Pts',(-48.426557328234,-54.6822974139064,
0.));
#137676=CARTESIAN_POINT('Ctrl Pts',(-48.4034271930514,-54.6708355816358,
0.));
#137677=CARTESIAN_POINT('Ctrl Pts',(-48.3803423302294,-54.6593691635145,
0.));
#137678=CARTESIAN_POINT('Ctrl Pts',(-48.3573028063124,-54.6478982512794,
0.));
#137679=CARTESIAN_POINT('Ctrl Pts',(-48.3343086880194,-54.6364229370494,
0.));
#137680=CARTESIAN_POINT('Ctrl Pts',(-48.3113600422443,-54.6249433133261,
0.));
#137681=CARTESIAN_POINT('Ctrl Pts',(-48.2884569360506,-54.6134594729959,
0.));
#137682=CARTESIAN_POINT('Ctrl Pts',(-48.2655994366665,-54.6019715093309,
0.));
#137683=CARTESIAN_POINT('Ctrl Pts',(-48.2427876114947,-54.5904795159926,
0.));
#137684=CARTESIAN_POINT('Ctrl Pts',(-48.2200215281173,-54.5789835870342,
0.));
#137685=CARTESIAN_POINT('Ctrl Pts',(-48.1973012542966,-54.5674838169041,
0.));
#137686=CARTESIAN_POINT('Ctrl Pts',(-48.1746268579736,-54.5559803004492,
0.));
#137687=CARTESIAN_POINT('Ctrl Pts',(-48.1519984072622,-54.5444731329201,
0.));
#137688=CARTESIAN_POINT('Ctrl Pts',(-48.1294159704573,-54.5329624099721,
0.));
#137689=CARTESIAN_POINT('Ctrl Pts',(-48.1068796160405,-54.5214482276678,
0.));
#137690=CARTESIAN_POINT('Ctrl Pts',(-48.0843894126806,-54.5099306824786,
0.));
#137691=CARTESIAN_POINT('Ctrl Pts',(-48.0619454292324,-54.4984098712886,
0.));
#137692=CARTESIAN_POINT('Ctrl Pts',(-48.0395477347298,-54.4868858913971,
0.));
#137693=CARTESIAN_POINT('Ctrl Pts',(-48.0171963983924,-54.4753588405215,
0.));
#137694=CARTESIAN_POINT('Ctrl Pts',(-47.9948914896326,-54.4638288168003,
0.));
#137695=CARTESIAN_POINT('Ctrl Pts',(-47.9726330780572,-54.4522959187955,
0.));
#137696=CARTESIAN_POINT('Ctrl Pts',(-47.9504212334675,-54.4407602454967,
0.));
#137697=CARTESIAN_POINT('Ctrl Pts',(-47.9282560258516,-54.429221896324,
0.));
#137698=CARTESIAN_POINT('Ctrl Pts',(-47.9061375253897,-54.4176809711311,
0.));
#137699=CARTESIAN_POINT('Ctrl Pts',(-47.8840658024618,-54.4061375702079,
0.));
#137700=CARTESIAN_POINT('Ctrl Pts',(-47.8620409276493,-54.3945917942832,
0.));
#137701=CARTESIAN_POINT('Ctrl Pts',(-47.8400629717355,-54.3830437445279,
0.));
#137702=CARTESIAN_POINT('Ctrl Pts',(-47.8181320056995,-54.3714935225591,
0.));
#137703=CARTESIAN_POINT('Ctrl Pts',(-47.7962481007185,-54.3599412304438,
0.));
#137704=CARTESIAN_POINT('Ctrl Pts',(-47.7744113281771,-54.3483869707002,
0.));
#137705=CARTESIAN_POINT('Ctrl Pts',(-47.7526217596694,-54.3368308463023,
0.));
#137706=CARTESIAN_POINT('Ctrl Pts',(-47.7308794669993,-54.3252729606823,
0.));
#137707=CARTESIAN_POINT('Ctrl Pts',(-47.7091845221747,-54.3137134177345,
0.));
#137708=CARTESIAN_POINT('Ctrl Pts',(-47.6875369974087,-54.302152321819,
0.));
#137709=CARTESIAN_POINT('Ctrl Pts',(-47.6659369651301,-54.290589777765,
0.));
#137710=CARTESIAN_POINT('Ctrl Pts',(-47.6443844979848,-54.2790258908738,
0.));
#137711=CARTESIAN_POINT('Ctrl Pts',(-47.6228796688375,-54.2674607669226,
0.));
#137712=CARTESIAN_POINT('Ctrl Pts',(-47.6014225507659,-54.2558945121678,
0.));
#137713=CARTESIAN_POINT('Ctrl Pts',(-47.5800132170608,-54.244327233349,
0.));
#137714=CARTESIAN_POINT('Ctrl Pts',(-47.5586517412363,-54.2327590376924,
0.));
#137715=CARTESIAN_POINT('Ctrl Pts',(-47.5373381970326,-54.2211900329138,
0.));
#137716=CARTESIAN_POINT('Ctrl Pts',(-47.5160726584174,-54.209620327223,
0.));
#137717=CARTESIAN_POINT('Ctrl Pts',(-47.4948551995801,-54.198050029327,
0.));
#137718=CARTESIAN_POINT('Ctrl Pts',(-47.4736858949322,-54.1864792484345,
0.));
#137719=CARTESIAN_POINT('Ctrl Pts',(-47.4525648191173,-54.1749080942593,
0.));
#137720=CARTESIAN_POINT('Ctrl Pts',(-47.4314920470141,-54.1633366770239,
0.));
#137721=CARTESIAN_POINT('Ctrl Pts',(-47.4104676537381,-54.1517651074637,
0.));
#137722=CARTESIAN_POINT('Ctrl Pts',(-47.3894917146365,-54.1401934968311,
0.));
#137723=CARTESIAN_POINT('Ctrl Pts',(-47.3685643052874,-54.1286219568989,
0.));
#137724=CARTESIAN_POINT('Ctrl Pts',(-47.3476855015102,-54.1170505999645,
0.));
#137725=CARTESIAN_POINT('Ctrl Pts',(-47.3268553793694,-54.1054795388543,
0.));
#137726=CARTESIAN_POINT('Ctrl Pts',(-47.3060740151752,-54.0939088869269,
0.));
#137727=CARTESIAN_POINT('Ctrl Pts',(-47.2853414854793,-54.0823387580776,
0.));
#137728=CARTESIAN_POINT('Ctrl Pts',(-47.2646578670746,-54.0707692667438,
0.));
#137729=CARTESIAN_POINT('Ctrl Pts',(-47.2440232370065,-54.0592005279086,
0.));
#137730=CARTESIAN_POINT('Ctrl Pts',(-47.2234376725743,-54.047632657104,
0.));
#137731=CARTESIAN_POINT('Ctrl Pts',(-47.202901251334,-54.0360657704163,
0.));
#137732=CARTESIAN_POINT('Ctrl Pts',(-47.1824140510926,-54.0244999844893,
0.));
#137733=CARTESIAN_POINT('Ctrl Pts',(-47.1619761499087,-54.0129354165297,
0.));
#137734=CARTESIAN_POINT('Ctrl Pts',(-47.1415876261035,-54.0013721843118,
0.));
#137735=CARTESIAN_POINT('Ctrl Pts',(-47.1212485582643,-53.989810406182,
0.));
#137736=CARTESIAN_POINT('Ctrl Pts',(-47.1009590252458,-53.9782502010634,
0.));
#137737=CARTESIAN_POINT('Ctrl Pts',(-47.0807191061648,-53.9666916884596,
0.));
#137738=CARTESIAN_POINT('Ctrl Pts',(-47.0605288804008,-53.95513498846,0.));
#137739=CARTESIAN_POINT('Ctrl Pts',(-47.0403884276072,-53.9435802217436,
0.));
#137740=CARTESIAN_POINT('Ctrl Pts',(-47.0202978277138,-53.9320275095853,
0.));
#137741=CARTESIAN_POINT('Ctrl Pts',(-47.0002571609297,-53.9204769738596,
0.));
#137742=CARTESIAN_POINT('Ctrl Pts',(-46.9802665077366,-53.9089287370463,
0.));
#137743=CARTESIAN_POINT('Ctrl Pts',(-46.9603259488921,-53.8973829222348,
0.));
#137744=CARTESIAN_POINT('Ctrl Pts',(-46.94043556544,-53.8858396531298,0.));
#137745=CARTESIAN_POINT('Ctrl Pts',(-46.9205954387133,-53.8742990540563,
0.));
#137746=CARTESIAN_POINT('Ctrl Pts',(-46.9008056503351,-53.8627612499638,
0.));
#137747=CARTESIAN_POINT('Ctrl Pts',(-46.881066282213,-53.8512263664321,
0.));
#137748=CARTESIAN_POINT('Ctrl Pts',(-46.8613774165435,-53.8396945296757,
0.));
#137749=CARTESIAN_POINT('Ctrl Pts',(-46.841739135822,-53.8281658665503,
0.));
#137750=CARTESIAN_POINT('Ctrl Pts',(-46.8221515228457,-53.816640504558,
0.));
#137751=CARTESIAN_POINT('Ctrl Pts',(-46.802614660715,-53.8051185718532,
0.));
#137752=CARTESIAN_POINT('Ctrl Pts',(-46.7831286328278,-53.793600197248,
0.));
#137753=CARTESIAN_POINT('Ctrl Pts',(-46.763693522886,-53.7820855102182,
0.));
#137754=CARTESIAN_POINT('Ctrl Pts',(-46.7443094149045,-53.7705746409076,
0.));
#137755=CARTESIAN_POINT('Ctrl Pts',(-46.7249763932129,-53.7590677201342,
0.));
#137756=CARTESIAN_POINT('Ctrl Pts',(-46.7056945424559,-53.7475648793946,
0.));
#137757=CARTESIAN_POINT('Ctrl Pts',(-46.6864639475862,-53.7360662508675,
0.));
#137758=CARTESIAN_POINT('Ctrl Pts',(-46.6672846938752,-53.7245719674221,
0.));
#137759=CARTESIAN_POINT('Ctrl Pts',(-46.6481568669217,-53.7130821626262,
0.));
#137760=CARTESIAN_POINT('Ctrl Pts',(-46.6290805526559,-53.7015969707541,
0.));
#137761=CARTESIAN_POINT('Ctrl Pts',(-46.6100558373401,-53.690116526794,
0.));
#137762=CARTESIAN_POINT('Ctrl Pts',(-46.5910828075652,-53.678640966456,
0.));
#137763=CARTESIAN_POINT('Ctrl Pts',(-46.572161550259,-53.6671704261735,
0.));
#137764=CARTESIAN_POINT('Ctrl Pts',(-46.5532921526899,-53.6557050431069,
0.));
#137765=CARTESIAN_POINT('Ctrl Pts',(-46.5344747024677,-53.6442449551455,
0.));
#137766=CARTESIAN_POINT('Ctrl Pts',(-46.5157092875377,-53.6327903009098,
0.));
#137767=CARTESIAN_POINT('Ctrl Pts',(-46.4969959961779,-53.6213412197542,
0.));
#137768=CARTESIAN_POINT('Ctrl Pts',(-46.4783349170182,-53.6098978517869,
0.));
#137769=CARTESIAN_POINT('Ctrl Pts',(-46.4597261390526,-53.5984603378862,
0.));
#137770=CARTESIAN_POINT('Ctrl Pts',(-46.4411697516474,-53.5870288197161,
0.));
#137771=CARTESIAN_POINT('Ctrl Pts',(-46.422665844546,-53.5756034397464,
0.));
#137772=CARTESIAN_POINT('Ctrl Pts',(-46.4042145078682,-53.5641843412537,
0.));
#137773=CARTESIAN_POINT('Ctrl Pts',(-46.3858158321044,-53.552771668303,
0.));
#137774=CARTESIAN_POINT('Ctrl Pts',(-46.3674699081043,-53.5413655657323,
0.));
#137775=CARTESIAN_POINT('Ctrl Pts',(-46.3491768270664,-53.5299661791396,
0.));
#137776=CARTESIAN_POINT('Ctrl Pts',(-46.3309366805112,-53.518573654857,
0.));
#137777=CARTESIAN_POINT('Ctrl Pts',(-46.3127495603117,-53.5071881399932,
0.));
#137778=CARTESIAN_POINT('Ctrl Pts',(-46.2946155587428,-53.4958097825019,
0.));
#137779=CARTESIAN_POINT('Ctrl Pts',(-46.2765347685198,-53.4844387312414,
0.));
#137780=CARTESIAN_POINT('Ctrl Pts',(-46.2585072828343,-53.4730751360359,
0.));
#137781=CARTESIAN_POINT('Ctrl Pts',(-46.2405331953872,-53.4617191477382,
0.));
#137782=CARTESIAN_POINT('Ctrl Pts',(-46.2226126003185,-53.4503709181158,
0.));
#137783=CARTESIAN_POINT('Ctrl Pts',(-46.2047455921276,-53.4390305997263,
0.));
#137784=CARTESIAN_POINT('Ctrl Pts',(-46.1869322656027,-53.4276983458129,
0.));
#137785=CARTESIAN_POINT('Ctrl Pts',(-46.1691727157149,-53.4163743101535,
0.));
#137786=CARTESIAN_POINT('Ctrl Pts',(-46.1514670376035,-53.4050586470463,
0.));
#137787=CARTESIAN_POINT('Ctrl Pts',(-46.1338153268116,-53.3937515116572,
0.));
#137788=CARTESIAN_POINT('Ctrl Pts',(-46.1162176794891,-53.3824530603284,
0.));
#137789=CARTESIAN_POINT('Ctrl Pts',(-46.0986741925646,-53.3711634508426,
0.));
#137790=CARTESIAN_POINT('Ctrl Pts',(-46.0811849640195,-53.3598828428519,
0.));
#137791=CARTESIAN_POINT('Ctrl Pts',(-46.0637500926954,-53.3486113975868,
0.));
#137792=CARTESIAN_POINT('Ctrl Pts',(-46.046369677778,-53.3373492770647,
0.));
#137793=CARTESIAN_POINT('Ctrl Pts',(-46.0290438183598,-53.3260966434277,
0.));
#137794=CARTESIAN_POINT('Ctrl Pts',(-46.0117726129893,-53.3148536582658,
0.));
#137795=CARTESIAN_POINT('Ctrl Pts',(-45.9945561591486,-53.3036204818367,
0.));
#137796=CARTESIAN_POINT('Ctrl Pts',(-45.9773945542415,-53.2923972745585,
0.));
#137797=CARTESIAN_POINT('Ctrl Pts',(-45.9602878967715,-53.2811841987945,
0.));
#137798=CARTESIAN_POINT('Ctrl Pts',(-45.9432362873001,-53.2699814203097,
0.));
#137799=CARTESIAN_POINT('Ctrl Pts',(-45.9262398298323,-53.2587891103835,
0.));
#137800=CARTESIAN_POINT('Ctrl Pts',(-45.9092986319343,-53.2476074459977,
0.));
#137801=CARTESIAN_POINT('Ctrl Pts',(-45.8924128018354,-53.2364366054276,
0.));
#137802=CARTESIAN_POINT('Ctrl Pts',(-45.8755824458715,-53.2252767643652,
0.));
#137803=CARTESIAN_POINT('Ctrl Pts',(-45.8588076662598,-53.2141280925458,
0.));
#137804=CARTESIAN_POINT('Ctrl Pts',(-45.8420885575386,-53.2029907483602,
0.));
#137805=CARTESIAN_POINT('Ctrl Pts',(-45.8254252100003,-53.1918648840598,
0.));
#137806=CARTESIAN_POINT('Ctrl Pts',(-45.8088177165124,-53.1807506560977,
0.));
#137807=CARTESIAN_POINT('Ctrl Pts',(-45.7922661780005,-53.1696482334487,
0.));
#137808=CARTESIAN_POINT('Ctrl Pts',(-45.7757707100568,-53.158557807638,
0.));
#137809=CARTESIAN_POINT('Ctrl Pts',(-45.7593314474413,-53.147479599594,
0.));
#137810=CARTESIAN_POINT('Ctrl Pts',(-45.7429485300727,-53.136413838457,
0.));
#137811=CARTESIAN_POINT('Ctrl Pts',(-45.7266220896951,-53.1253607414806,
0.));
#137812=CARTESIAN_POINT('Ctrl Pts',(-45.7103522376744,-53.1143204954981,
0.));
#137813=CARTESIAN_POINT('Ctrl Pts',(-45.6941390489239,-53.1032932329074,
0.));
#137814=CARTESIAN_POINT('Ctrl Pts',(-45.6779825614486,-53.0922790298736,
0.));
#137815=CARTESIAN_POINT('Ctrl Pts',(-45.6651027439479,-53.083478145185,
0.));
#137816=CARTESIAN_POINT('Ctrl Pts',(-45.6554684028296,-53.0768833804386,
0.));
#137817=CARTESIAN_POINT('Ctrl Pts',(-45.6490568514146,-53.0724894921921,
0.));
#137818=CARTESIAN_POINT('Ctrl Pts',(-45.6458539113724,-53.0702932034641,
0.));
#137819=CARTESIAN_POINT('Ctrl Pts',(-54.5031396718592,-50.7903314215393,
0.));
#137820=CARTESIAN_POINT('Ctrl Pts',(-54.5031396718592,-50.7903314215393,
12.));
#137821=CARTESIAN_POINT('Ctrl Pts',(-54.4978248630387,-50.7885805844281,
0.));
#137822=CARTESIAN_POINT('Ctrl Pts',(-54.4978248630387,-50.7885805844281,
12.));
#137823=CARTESIAN_POINT('Ctrl Pts',(-54.4871993224832,-50.7850776288814,
0.));
#137824=CARTESIAN_POINT('Ctrl Pts',(-54.4871993224832,-50.7850776288814,
12.));
#137825=CARTESIAN_POINT('Ctrl Pts',(-54.4712732429066,-50.7798193515888,
0.));
#137826=CARTESIAN_POINT('Ctrl Pts',(-54.4712732429066,-50.7798193515888,
12.));
#137827=CARTESIAN_POINT('Ctrl Pts',(-54.4500629336429,-50.7728006269349,
0.));
#137828=CARTESIAN_POINT('Ctrl Pts',(-54.4500629336429,-50.7728006269349,
12.));
#137829=CARTESIAN_POINT('Ctrl Pts',(-54.423590828767,-50.764014409002,0.));
#137830=CARTESIAN_POINT('Ctrl Pts',(-54.423590828767,-50.764014409002,12.));
#137831=CARTESIAN_POINT('Ctrl Pts',(-54.3971595231574,-50.7552153869475,
0.));
#137832=CARTESIAN_POINT('Ctrl Pts',(-54.3971595231574,-50.7552153869475,
12.));
#137833=CARTESIAN_POINT('Ctrl Pts',(-54.3707690445749,-50.7464035792906,
0.));
#137834=CARTESIAN_POINT('Ctrl Pts',(-54.3707690445749,-50.7464035792906,
12.));
#137835=CARTESIAN_POINT('Ctrl Pts',(-54.3444194324054,-50.7375790185896,
0.));
#137836=CARTESIAN_POINT('Ctrl Pts',(-54.3444194324054,-50.7375790185896,
12.));
#137837=CARTESIAN_POINT('Ctrl Pts',(-54.3181107400663,-50.7287417566123,
0.));
#137838=CARTESIAN_POINT('Ctrl Pts',(-54.3181107400663,-50.7287417566123,
12.));
#137839=CARTESIAN_POINT('Ctrl Pts',(-54.2918430335206,-50.7198918629451,
0.));
#137840=CARTESIAN_POINT('Ctrl Pts',(-54.2918430335206,-50.7198918629451,
12.));
#137841=CARTESIAN_POINT('Ctrl Pts',(-54.2656163868104,-50.7110294185698,
0.));
#137842=CARTESIAN_POINT('Ctrl Pts',(-54.2656163868104,-50.7110294185698,
12.));
#137843=CARTESIAN_POINT('Ctrl Pts',(-54.2394308784026,-50.7021545108311,
0.));
#137844=CARTESIAN_POINT('Ctrl Pts',(-54.2394308784026,-50.7021545108311,
12.));
#137845=CARTESIAN_POINT('Ctrl Pts',(-54.2132865872985,-50.6932672279772,
0.));
#137846=CARTESIAN_POINT('Ctrl Pts',(-54.2132865872985,-50.6932672279772,
12.));
#137847=CARTESIAN_POINT('Ctrl Pts',(-54.1871835889981,-50.6843676535492,
0.));
#137848=CARTESIAN_POINT('Ctrl Pts',(-54.1871835889981,-50.6843676535492,
12.));
#137849=CARTESIAN_POINT('Ctrl Pts',(-54.1611219522394,-50.67545586183,0.));
#137850=CARTESIAN_POINT('Ctrl Pts',(-54.1611219522394,-50.67545586183,12.));
#137851=CARTESIAN_POINT('Ctrl Pts',(-54.1351017412804,-50.6665319209869,
0.));
#137852=CARTESIAN_POINT('Ctrl Pts',(-54.1351017412804,-50.6665319209869,
12.));
#137853=CARTESIAN_POINT('Ctrl Pts',(-54.1091230175367,-50.6575958953221,
0.));
#137854=CARTESIAN_POINT('Ctrl Pts',(-54.1091230175367,-50.6575958953221,
12.));
#137855=CARTESIAN_POINT('Ctrl Pts',(-54.0831858415189,-50.6486478479465,
0.));
#137856=CARTESIAN_POINT('Ctrl Pts',(-54.0831858415189,-50.6486478479465,
12.));
#137857=CARTESIAN_POINT('Ctrl Pts',(-54.0572902745076,-50.6396878430939,
0.));
#137858=CARTESIAN_POINT('Ctrl Pts',(-54.0572902745076,-50.6396878430939,
12.));
#137859=CARTESIAN_POINT('Ctrl Pts',(-54.0314363806708,-50.6307159490553,
0.));
#137860=CARTESIAN_POINT('Ctrl Pts',(-54.0314363806708,-50.6307159490553,
12.));
#137861=CARTESIAN_POINT('Ctrl Pts',(-54.0056242268399,-50.6217322378648,
0.));
#137862=CARTESIAN_POINT('Ctrl Pts',(-54.0056242268399,-50.6217322378648,
12.));
#137863=CARTESIAN_POINT('Ctrl Pts',(-53.979853881553,-50.6127367839711,
0.));
#137864=CARTESIAN_POINT('Ctrl Pts',(-53.979853881553,-50.6127367839711,
12.));
#137865=CARTESIAN_POINT('Ctrl Pts',(-53.9541254143119,-50.603729663214,
0.));
#137866=CARTESIAN_POINT('Ctrl Pts',(-53.9541254143119,-50.603729663214,
12.));
#137867=CARTESIAN_POINT('Ctrl Pts',(-53.9284388948004,-50.5947109517483,
0.));
#137868=CARTESIAN_POINT('Ctrl Pts',(-53.9284388948004,-50.5947109517483,
12.));
#137869=CARTESIAN_POINT('Ctrl Pts',(-53.9027943919836,-50.5856807248151,
0.));
#137870=CARTESIAN_POINT('Ctrl Pts',(-53.9027943919836,-50.5856807248151,
12.));
#137871=CARTESIAN_POINT('Ctrl Pts',(-53.8771919737032,-50.5766390561884,
0.));
#137872=CARTESIAN_POINT('Ctrl Pts',(-53.8771919737032,-50.5766390561884,
12.));
#137873=CARTESIAN_POINT('Ctrl Pts',(-53.8516317071804,-50.5675860188538,
0.));
#137874=CARTESIAN_POINT('Ctrl Pts',(-53.8516317071804,-50.5675860188538,
12.));
#137875=CARTESIAN_POINT('Ctrl Pts',(-53.8261136593075,-50.5585216854091,
0.));
#137876=CARTESIAN_POINT('Ctrl Pts',(-53.8261136593075,-50.5585216854091,
12.));
#137877=CARTESIAN_POINT('Ctrl Pts',(-53.8006378970197,-50.5494461285761,
0.));
#137878=CARTESIAN_POINT('Ctrl Pts',(-53.8006378970197,-50.5494461285761,
12.));
#137879=CARTESIAN_POINT('Ctrl Pts',(-53.7752044876304,-50.5403594216698,
0.));
#137880=CARTESIAN_POINT('Ctrl Pts',(-53.7752044876304,-50.5403594216698,
12.));
#137881=CARTESIAN_POINT('Ctrl Pts',(-53.7498134991703,-50.5312616390779,
0.));
#137882=CARTESIAN_POINT('Ctrl Pts',(-53.7498134991703,-50.5312616390779,
12.));
#137883=CARTESIAN_POINT('Ctrl Pts',(-53.7244650002374,-50.522152856042,
0.));
#137884=CARTESIAN_POINT('Ctrl Pts',(-53.7244650002374,-50.522152856042,
12.));
#137885=CARTESIAN_POINT('Ctrl Pts',(-53.6991590598548,-50.513033148456,
0.));
#137886=CARTESIAN_POINT('Ctrl Pts',(-53.6991590598548,-50.513033148456,
12.));
#137887=CARTESIAN_POINT('Ctrl Pts',(-53.6738957473158,-50.503902592653,
0.));
#137888=CARTESIAN_POINT('Ctrl Pts',(-53.6738957473158,-50.503902592653,
12.));
#137889=CARTESIAN_POINT('Ctrl Pts',(-53.6486751320436,-50.4947612652149,
0.));
#137890=CARTESIAN_POINT('Ctrl Pts',(-53.6486751320436,-50.4947612652149,
12.));
#137891=CARTESIAN_POINT('Ctrl Pts',(-53.623497283406,-50.4856092427314,
0.));
#137892=CARTESIAN_POINT('Ctrl Pts',(-53.623497283406,-50.4856092427314,
12.));
#137893=CARTESIAN_POINT('Ctrl Pts',(-53.5983622707238,-50.4764466018071,
0.));
#137894=CARTESIAN_POINT('Ctrl Pts',(-53.5983622707238,-50.4764466018071,
12.));
#137895=CARTESIAN_POINT('Ctrl Pts',(-53.5732701633609,-50.4672734191756,
0.));
#137896=CARTESIAN_POINT('Ctrl Pts',(-53.5732701633609,-50.4672734191756,
12.));
#137897=CARTESIAN_POINT('Ctrl Pts',(-53.5482210307868,-50.4580897717838,
0.));
#137898=CARTESIAN_POINT('Ctrl Pts',(-53.5482210307868,-50.4580897717838,
12.));
#137899=CARTESIAN_POINT('Ctrl Pts',(-53.5232149426413,-50.4488957368839,
0.));
#137900=CARTESIAN_POINT('Ctrl Pts',(-53.5232149426413,-50.4488957368839,
12.));
#137901=CARTESIAN_POINT('Ctrl Pts',(-53.4982519688024,-50.4396913921382,
0.));
#137902=CARTESIAN_POINT('Ctrl Pts',(-53.4982519688024,-50.4396913921382,
12.));
#137903=CARTESIAN_POINT('Ctrl Pts',(-53.4733321794188,-50.4304768156667,
0.));
#137904=CARTESIAN_POINT('Ctrl Pts',(-53.4733321794188,-50.4304768156667,
12.));
#137905=CARTESIAN_POINT('Ctrl Pts',(-53.4484556448776,-50.4212520859914,
0.));
#137906=CARTESIAN_POINT('Ctrl Pts',(-53.4484556448776,-50.4212520859914,
12.));
#137907=CARTESIAN_POINT('Ctrl Pts',(-53.4236224357838,-50.4120172820047,
0.));
#137908=CARTESIAN_POINT('Ctrl Pts',(-53.4236224357838,-50.4120172820047,
12.));
#137909=CARTESIAN_POINT('Ctrl Pts',(-53.398832622931,-50.4027724829297,
0.));
#137910=CARTESIAN_POINT('Ctrl Pts',(-53.398832622931,-50.4027724829297,
12.));
#137911=CARTESIAN_POINT('Ctrl Pts',(-53.3740862772681,-50.3935177682837,
0.));
#137912=CARTESIAN_POINT('Ctrl Pts',(-53.3740862772681,-50.3935177682837,
12.));
#137913=CARTESIAN_POINT('Ctrl Pts',(-53.3493834698697,-50.384253217846,
0.));
#137914=CARTESIAN_POINT('Ctrl Pts',(-53.3493834698697,-50.384253217846,
12.));
#137915=CARTESIAN_POINT('Ctrl Pts',(-53.3247242719587,-50.3749789116786,
0.));
#137916=CARTESIAN_POINT('Ctrl Pts',(-53.3247242719587,-50.3749789116786,
12.));
#137917=CARTESIAN_POINT('Ctrl Pts',(-53.300108754923,-50.365694930143,0.));
#137918=CARTESIAN_POINT('Ctrl Pts',(-53.300108754923,-50.365694930143,12.));
#137919=CARTESIAN_POINT('Ctrl Pts',(-53.2755369903293,-50.3564013539199,
0.));
#137920=CARTESIAN_POINT('Ctrl Pts',(-53.2755369903293,-50.3564013539199,
12.));
#137921=CARTESIAN_POINT('Ctrl Pts',(-53.2510090499336,-50.3470982640289,
0.));
#137922=CARTESIAN_POINT('Ctrl Pts',(-53.2510090499336,-50.3470982640289,
12.));
#137923=CARTESIAN_POINT('Ctrl Pts',(-53.2265250056887,-50.3377857418515,
0.));
#137924=CARTESIAN_POINT('Ctrl Pts',(-53.2265250056887,-50.3377857418515,
12.));
#137925=CARTESIAN_POINT('Ctrl Pts',(-53.2020849297471,-50.3284638691278,
0.));
#137926=CARTESIAN_POINT('Ctrl Pts',(-53.2020849297471,-50.3284638691278,
12.));
#137927=CARTESIAN_POINT('Ctrl Pts',(-53.1776888944616,-50.3191327279493,
0.));
#137928=CARTESIAN_POINT('Ctrl Pts',(-53.1776888944616,-50.3191327279493,
12.));
#137929=CARTESIAN_POINT('Ctrl Pts',(-53.1533369723818,-50.3097924007534,
0.));
#137930=CARTESIAN_POINT('Ctrl Pts',(-53.1533369723818,-50.3097924007534,
12.));
#137931=CARTESIAN_POINT('Ctrl Pts',(-53.1290292362485,-50.300442970319,
0.));
#137932=CARTESIAN_POINT('Ctrl Pts',(-53.1290292362485,-50.300442970319,
12.));
#137933=CARTESIAN_POINT('Ctrl Pts',(-53.1047657589812,-50.2910845197619,
0.));
#137934=CARTESIAN_POINT('Ctrl Pts',(-53.1047657589812,-50.2910845197619,
12.));
#137935=CARTESIAN_POINT('Ctrl Pts',(-53.0805466136798,-50.2817171325358,
0.));
#137936=CARTESIAN_POINT('Ctrl Pts',(-53.0805466136798,-50.2817171325358,
12.));
#137937=CARTESIAN_POINT('Ctrl Pts',(-53.0563718736366,-50.2723408924373,
0.));
#137938=CARTESIAN_POINT('Ctrl Pts',(-53.0563718736366,-50.2723408924373,
12.));
#137939=CARTESIAN_POINT('Ctrl Pts',(-53.0322416123406,-50.2629558836111,
0.));
#137940=CARTESIAN_POINT('Ctrl Pts',(-53.0322416123406,-50.2629558836111,
12.));
#137941=CARTESIAN_POINT('Ctrl Pts',(-53.0081559034801,-50.2535621905552,
0.));
#137942=CARTESIAN_POINT('Ctrl Pts',(-53.0081559034801,-50.2535621905552,
12.));
#137943=CARTESIAN_POINT('Ctrl Pts',(-52.9841148209402,-50.2441598981286,
0.));
#137944=CARTESIAN_POINT('Ctrl Pts',(-52.9841148209402,-50.2441598981286,
12.));
#137945=CARTESIAN_POINT('Ctrl Pts',(-52.9601184388028,-50.2347490915555,
0.));
#137946=CARTESIAN_POINT('Ctrl Pts',(-52.9601184388028,-50.2347490915555,
12.));
#137947=CARTESIAN_POINT('Ctrl Pts',(-52.9361668313542,-50.2253298564241,
0.));
#137948=CARTESIAN_POINT('Ctrl Pts',(-52.9361668313542,-50.2253298564241,
12.));
#137949=CARTESIAN_POINT('Ctrl Pts',(-52.9122600730884,-50.2159022786879,
0.));
#137950=CARTESIAN_POINT('Ctrl Pts',(-52.9122600730884,-50.2159022786879,
12.));
#137951=CARTESIAN_POINT('Ctrl Pts',(-52.8883982387068,-50.2064664446663,
0.));
#137952=CARTESIAN_POINT('Ctrl Pts',(-52.8883982387068,-50.2064664446663,
12.));
#137953=CARTESIAN_POINT('Ctrl Pts',(-52.8645814031133,-50.1970224410471,
0.));
#137954=CARTESIAN_POINT('Ctrl Pts',(-52.8645814031133,-50.1970224410471,
12.));
#137955=CARTESIAN_POINT('Ctrl Pts',(-52.8408096414093,-50.1875703548884,
0.));
#137956=CARTESIAN_POINT('Ctrl Pts',(-52.8408096414093,-50.1875703548884,
12.));
#137957=CARTESIAN_POINT('Ctrl Pts',(-52.8170830289044,-50.1781102736205,
0.));
#137958=CARTESIAN_POINT('Ctrl Pts',(-52.8170830289044,-50.1781102736205,
12.));
#137959=CARTESIAN_POINT('Ctrl Pts',(-52.7934016411205,-50.1686422850488,
0.));
#137960=CARTESIAN_POINT('Ctrl Pts',(-52.7934016411205,-50.1686422850488,
12.));
#137961=CARTESIAN_POINT('Ctrl Pts',(-52.769765553794,-50.1591664773561,
0.));
#137962=CARTESIAN_POINT('Ctrl Pts',(-52.769765553794,-50.1591664773561,
12.));
#137963=CARTESIAN_POINT('Ctrl Pts',(-52.7461748428738,-50.1496829391073,
0.));
#137964=CARTESIAN_POINT('Ctrl Pts',(-52.7461748428738,-50.1496829391073,
12.));
#137965=CARTESIAN_POINT('Ctrl Pts',(-52.7226295845161,-50.1401917592537,
0.));
#137966=CARTESIAN_POINT('Ctrl Pts',(-52.7226295845161,-50.1401917592537,
12.));
#137967=CARTESIAN_POINT('Ctrl Pts',(-52.699129855093,-50.1306930271345,
0.));
#137968=CARTESIAN_POINT('Ctrl Pts',(-52.699129855093,-50.1306930271345,
12.));
#137969=CARTESIAN_POINT('Ctrl Pts',(-52.6756757311978,-50.1211868324781,
0.));
#137970=CARTESIAN_POINT('Ctrl Pts',(-52.6756757311978,-50.1211868324781,
12.));
#137971=CARTESIAN_POINT('Ctrl Pts',(-52.652267289646,-50.111673265404,0.));
#137972=CARTESIAN_POINT('Ctrl Pts',(-52.652267289646,-50.111673265404,12.));
#137973=CARTESIAN_POINT('Ctrl Pts',(-52.6289046074746,-50.1021524164264,
0.));
#137974=CARTESIAN_POINT('Ctrl Pts',(-52.6289046074746,-50.1021524164264,
12.));
#137975=CARTESIAN_POINT('Ctrl Pts',(-52.6055877619348,-50.0926243764578,
0.));
#137976=CARTESIAN_POINT('Ctrl Pts',(-52.6055877619348,-50.0926243764578,
12.));
#137977=CARTESIAN_POINT('Ctrl Pts',(-52.5823168304994,-50.0830892368107,
0.));
#137978=CARTESIAN_POINT('Ctrl Pts',(-52.5823168304994,-50.0830892368107,
12.));
#137979=CARTESIAN_POINT('Ctrl Pts',(-52.5590918908702,-50.0735470892007,
0.));
#137980=CARTESIAN_POINT('Ctrl Pts',(-52.5590918908702,-50.0735470892007,
12.));
#137981=CARTESIAN_POINT('Ctrl Pts',(-52.5359130209792,-50.0639980257479,
0.));
#137982=CARTESIAN_POINT('Ctrl Pts',(-52.5359130209792,-50.0639980257479,
12.));
#137983=CARTESIAN_POINT('Ctrl Pts',(-52.5127802989896,-50.0544421389818,
0.));
#137984=CARTESIAN_POINT('Ctrl Pts',(-52.5127802989896,-50.0544421389818,
12.));
#137985=CARTESIAN_POINT('Ctrl Pts',(-52.4896938032884,-50.0448795218441,
0.));
#137986=CARTESIAN_POINT('Ctrl Pts',(-52.4896938032884,-50.0448795218441,
12.));
#137987=CARTESIAN_POINT('Ctrl Pts',(-52.4666536124913,-50.0353102676921,
0.));
#137988=CARTESIAN_POINT('Ctrl Pts',(-52.4666536124913,-50.0353102676921,
12.));
#137989=CARTESIAN_POINT('Ctrl Pts',(-52.4436598054515,-50.0257344703,0.));
#137990=CARTESIAN_POINT('Ctrl Pts',(-52.4436598054515,-50.0257344703,12.));
#137991=CARTESIAN_POINT('Ctrl Pts',(-52.4207124612608,-50.0161522238616,
0.));
#137992=CARTESIAN_POINT('Ctrl Pts',(-52.4207124612608,-50.0161522238616,
12.));
#137993=CARTESIAN_POINT('Ctrl Pts',(-52.3978116592509,-50.0065636229938,
0.));
#137994=CARTESIAN_POINT('Ctrl Pts',(-52.3978116592509,-50.0065636229938,
12.));
#137995=CARTESIAN_POINT('Ctrl Pts',(-52.3749574789871,-49.9969687627408,
0.));
#137996=CARTESIAN_POINT('Ctrl Pts',(-52.3749574789871,-49.9969687627408,
12.));
#137997=CARTESIAN_POINT('Ctrl Pts',(-52.3521500002718,-49.9873677385775,
0.));
#137998=CARTESIAN_POINT('Ctrl Pts',(-52.3521500002718,-49.9873677385775,
12.));
#137999=CARTESIAN_POINT('Ctrl Pts',(-52.3293893031528,-49.9777606464106,
0.));
#138000=CARTESIAN_POINT('Ctrl Pts',(-52.3293893031528,-49.9777606464106,
12.));
#138001=CARTESIAN_POINT('Ctrl Pts',(-52.3066754679265,-49.9681475825824,
0.));
#138002=CARTESIAN_POINT('Ctrl Pts',(-52.3066754679265,-49.9681475825824,
12.));
#138003=CARTESIAN_POINT('Ctrl Pts',(-52.2840085751384,-49.9585286438733,
0.));
#138004=CARTESIAN_POINT('Ctrl Pts',(-52.2840085751384,-49.9585286438733,
12.));
#138005=CARTESIAN_POINT('Ctrl Pts',(-52.2613887055773,-49.9489039275064,
0.));
#138006=CARTESIAN_POINT('Ctrl Pts',(-52.2613887055773,-49.9489039275064,
12.));
#138007=CARTESIAN_POINT('Ctrl Pts',(-52.2388159402771,-49.9392735311509,
0.));
#138008=CARTESIAN_POINT('Ctrl Pts',(-52.2388159402771,-49.9392735311509,
12.));
#138009=CARTESIAN_POINT('Ctrl Pts',(-52.2162903605275,-49.9296375529245,
0.));
#138010=CARTESIAN_POINT('Ctrl Pts',(-52.2162903605275,-49.9296375529245,
12.));
#138011=CARTESIAN_POINT('Ctrl Pts',(-52.1938120478754,-49.9199960913962,
0.));
#138012=CARTESIAN_POINT('Ctrl Pts',(-52.1938120478754,-49.9199960913962,
12.));
#138013=CARTESIAN_POINT('Ctrl Pts',(-52.1713810841276,-49.9103492455902,
0.));
#138014=CARTESIAN_POINT('Ctrl Pts',(-52.1713810841276,-49.9103492455902,
12.));
#138015=CARTESIAN_POINT('Ctrl Pts',(-52.1489975513445,-49.9006971149895,
0.));
#138016=CARTESIAN_POINT('Ctrl Pts',(-52.1489975513445,-49.9006971149895,
12.));
#138017=CARTESIAN_POINT('Ctrl Pts',(-52.1266615318407,-49.8910397995397,
0.));
#138018=CARTESIAN_POINT('Ctrl Pts',(-52.1266615318407,-49.8910397995397,
12.));
#138019=CARTESIAN_POINT('Ctrl Pts',(-52.1043731081962,-49.8813773996517,
0.));
#138020=CARTESIAN_POINT('Ctrl Pts',(-52.1043731081962,-49.8813773996517,
12.));
#138021=CARTESIAN_POINT('Ctrl Pts',(-52.0821323632587,-49.8717100162048,
0.));
#138022=CARTESIAN_POINT('Ctrl Pts',(-52.0821323632587,-49.8717100162048,
12.));
#138023=CARTESIAN_POINT('Ctrl Pts',(-52.0599393801452,-49.86203775055,0.));
#138024=CARTESIAN_POINT('Ctrl Pts',(-52.0599393801452,-49.86203775055,12.));
#138025=CARTESIAN_POINT('Ctrl Pts',(-52.0377942422376,-49.8523607045149,
0.));
#138026=CARTESIAN_POINT('Ctrl Pts',(-52.0377942422376,-49.8523607045149,
12.));
#138027=CARTESIAN_POINT('Ctrl Pts',(-52.0156970331823,-49.8426789804071,
0.));
#138028=CARTESIAN_POINT('Ctrl Pts',(-52.0156970331823,-49.8426789804071,
12.));
#138029=CARTESIAN_POINT('Ctrl Pts',(-51.9936478369008,-49.8329926810172,
0.));
#138030=CARTESIAN_POINT('Ctrl Pts',(-51.9936478369008,-49.8329926810172,
12.));
#138031=CARTESIAN_POINT('Ctrl Pts',(-51.9716467375937,-49.8233019096222,
0.));
#138032=CARTESIAN_POINT('Ctrl Pts',(-51.9716467375937,-49.8233019096222,
12.));
#138033=CARTESIAN_POINT('Ctrl Pts',(-51.9496938197418,-49.8136067699896,
0.));
#138034=CARTESIAN_POINT('Ctrl Pts',(-51.9496938197418,-49.8136067699896,
12.));
#138035=CARTESIAN_POINT('Ctrl Pts',(-51.9277891681018,-49.8039073663812,
0.));
#138036=CARTESIAN_POINT('Ctrl Pts',(-51.9277891681018,-49.8039073663812,
12.));
#138037=CARTESIAN_POINT('Ctrl Pts',(-51.9059328677059,-49.7942038035576,
0.));
#138038=CARTESIAN_POINT('Ctrl Pts',(-51.9059328677059,-49.7942038035576,
12.));
#138039=CARTESIAN_POINT('Ctrl Pts',(-51.8841250038724,-49.7844961867808,
0.));
#138040=CARTESIAN_POINT('Ctrl Pts',(-51.8841250038724,-49.7844961867808,
12.));
#138041=CARTESIAN_POINT('Ctrl Pts',(-51.8623656622097,-49.7747846218182,
0.));
#138042=CARTESIAN_POINT('Ctrl Pts',(-51.8623656622097,-49.7747846218182,
12.));
#138043=CARTESIAN_POINT('Ctrl Pts',(-51.8406549286175,-49.7650692149462,
0.));
#138044=CARTESIAN_POINT('Ctrl Pts',(-51.8406549286175,-49.7650692149462,
12.));
#138045=CARTESIAN_POINT('Ctrl Pts',(-51.8189928892828,-49.755350072955,
0.));
#138046=CARTESIAN_POINT('Ctrl Pts',(-51.8189928892828,-49.755350072955,
12.));
#138047=CARTESIAN_POINT('Ctrl Pts',(-51.7973796306803,-49.7456273031534,
0.));
#138048=CARTESIAN_POINT('Ctrl Pts',(-51.7973796306803,-49.7456273031534,
12.));
#138049=CARTESIAN_POINT('Ctrl Pts',(-51.7758152395836,-49.7359010133721,
0.));
#138050=CARTESIAN_POINT('Ctrl Pts',(-51.7758152395836,-49.7359010133721,
12.));
#138051=CARTESIAN_POINT('Ctrl Pts',(-51.754299803067,-49.7261713119663,
0.));
#138052=CARTESIAN_POINT('Ctrl Pts',(-51.754299803067,-49.7261713119663,
12.));
#138053=CARTESIAN_POINT('Ctrl Pts',(-51.7328334085091,-49.7164383078212,
0.));
#138054=CARTESIAN_POINT('Ctrl Pts',(-51.7328334085091,-49.7164383078212,
12.));
#138055=CARTESIAN_POINT('Ctrl Pts',(-51.7114161435869,-49.7067021103553,
0.));
#138056=CARTESIAN_POINT('Ctrl Pts',(-51.7114161435869,-49.7067021103553,
12.));
#138057=CARTESIAN_POINT('Ctrl Pts',(-51.6900480962773,-49.6969628295262,
0.));
#138058=CARTESIAN_POINT('Ctrl Pts',(-51.6900480962773,-49.6969628295262,
12.));
#138059=CARTESIAN_POINT('Ctrl Pts',(-51.6687293548682,-49.6872205758336,
0.));
#138060=CARTESIAN_POINT('Ctrl Pts',(-51.6687293548682,-49.6872205758336,
12.));
#138061=CARTESIAN_POINT('Ctrl Pts',(-51.6474600079622,-49.6774754603245,
0.));
#138062=CARTESIAN_POINT('Ctrl Pts',(-51.6474600079622,-49.6774754603245,
12.));
#138063=CARTESIAN_POINT('Ctrl Pts',(-51.626240144479,-49.6677275945967,
0.));
#138064=CARTESIAN_POINT('Ctrl Pts',(-51.626240144479,-49.6677275945967,
12.));
#138065=CARTESIAN_POINT('Ctrl Pts',(-51.6050698536496,-49.6579770908037,
0.));
#138066=CARTESIAN_POINT('Ctrl Pts',(-51.6050698536496,-49.6579770908037,
12.));
#138067=CARTESIAN_POINT('Ctrl Pts',(-51.5839492250181,-49.6482240616593,
0.));
#138068=CARTESIAN_POINT('Ctrl Pts',(-51.5839492250181,-49.6482240616593,
12.));
#138069=CARTESIAN_POINT('Ctrl Pts',(-51.5628783484525,-49.6384686204413,
0.));
#138070=CARTESIAN_POINT('Ctrl Pts',(-51.5628783484525,-49.6384686204413,
12.));
#138071=CARTESIAN_POINT('Ctrl Pts',(-51.5418573141484,-49.6287108809966,
0.));
#138072=CARTESIAN_POINT('Ctrl Pts',(-51.5418573141484,-49.6287108809966,
12.));
#138073=CARTESIAN_POINT('Ctrl Pts',(-51.5208862126315,-49.6189509577452,
0.));
#138074=CARTESIAN_POINT('Ctrl Pts',(-51.5208862126315,-49.6189509577452,
12.));
#138075=CARTESIAN_POINT('Ctrl Pts',(-51.4999651347523,-49.6091889656866,
0.));
#138076=CARTESIAN_POINT('Ctrl Pts',(-51.4999651347523,-49.6091889656866,
12.));
#138077=CARTESIAN_POINT('Ctrl Pts',(-51.4790941716888,-49.5994250204031,
0.));
#138078=CARTESIAN_POINT('Ctrl Pts',(-51.4790941716888,-49.5994250204031,
12.));
#138079=CARTESIAN_POINT('Ctrl Pts',(-51.4582734149583,-49.5896592380654,
0.));
#138080=CARTESIAN_POINT('Ctrl Pts',(-51.4582734149583,-49.5896592380654,
12.));
#138081=CARTESIAN_POINT('Ctrl Pts',(-51.4375029564197,-49.5798917354366,
0.));
#138082=CARTESIAN_POINT('Ctrl Pts',(-51.4375029564197,-49.5798917354366,
12.));
#138083=CARTESIAN_POINT('Ctrl Pts',(-51.4167828882756,-49.5701226298769,
0.));
#138084=CARTESIAN_POINT('Ctrl Pts',(-51.4167828882756,-49.5701226298769,
12.));
#138085=CARTESIAN_POINT('Ctrl Pts',(-51.396113303067,-49.5603520393496,
0.));
#138086=CARTESIAN_POINT('Ctrl Pts',(-51.396113303067,-49.5603520393496,
12.));
#138087=CARTESIAN_POINT('Ctrl Pts',(-51.3754942936778,-49.550580082425,
0.));
#138088=CARTESIAN_POINT('Ctrl Pts',(-51.3754942936778,-49.550580082425,
12.));
#138089=CARTESIAN_POINT('Ctrl Pts',(-51.3549259533458,-49.5408068782859,
0.));
#138090=CARTESIAN_POINT('Ctrl Pts',(-51.3549259533458,-49.5408068782859,
12.));
#138091=CARTESIAN_POINT('Ctrl Pts',(-51.3344083756657,-49.5310325467332,
0.));
#138092=CARTESIAN_POINT('Ctrl Pts',(-51.3344083756657,-49.5310325467332,
12.));
#138093=CARTESIAN_POINT('Ctrl Pts',(-51.313941654591,-49.5212572081908,
0.));
#138094=CARTESIAN_POINT('Ctrl Pts',(-51.313941654591,-49.5212572081908,
12.));
#138095=CARTESIAN_POINT('Ctrl Pts',(-51.2935258844289,-49.5114809837122,
0.));
#138096=CARTESIAN_POINT('Ctrl Pts',(-51.2935258844289,-49.5114809837122,
12.));
#138097=CARTESIAN_POINT('Ctrl Pts',(-51.2731611598475,-49.5017039949852,
0.));
#138098=CARTESIAN_POINT('Ctrl Pts',(-51.2731611598475,-49.5017039949852,
12.));
#138099=CARTESIAN_POINT('Ctrl Pts',(-51.2528475758846,-49.4919263643362,
0.));
#138100=CARTESIAN_POINT('Ctrl Pts',(-51.2528475758846,-49.4919263643362,
12.));
#138101=CARTESIAN_POINT('Ctrl Pts',(-51.2325852279506,-49.4821482147356,
0.));
#138102=CARTESIAN_POINT('Ctrl Pts',(-51.2325852279506,-49.4821482147356,
12.));
#138103=CARTESIAN_POINT('Ctrl Pts',(-51.2123742118287,-49.4723696698021,
0.));
#138104=CARTESIAN_POINT('Ctrl Pts',(-51.2123742118287,-49.4723696698021,
12.));
#138105=CARTESIAN_POINT('Ctrl Pts',(-51.1922146236686,-49.4625908538074,
0.));
#138106=CARTESIAN_POINT('Ctrl Pts',(-51.1922146236686,-49.4625908538074,
12.));
#138107=CARTESIAN_POINT('Ctrl Pts',(-51.1721065599973,-49.4528118916832,
0.));
#138108=CARTESIAN_POINT('Ctrl Pts',(-51.1721065599973,-49.4528118916832,
12.));
#138109=CARTESIAN_POINT('Ctrl Pts',(-51.1520501177291,-49.4430329090287,
0.));
#138110=CARTESIAN_POINT('Ctrl Pts',(-51.1520501177291,-49.4430329090287,
12.));
#138111=CARTESIAN_POINT('Ctrl Pts',(-51.1320453941702,-49.4332540321178,
0.));
#138112=CARTESIAN_POINT('Ctrl Pts',(-51.1320453941702,-49.4332540321178,
12.));
#138113=CARTESIAN_POINT('Ctrl Pts',(-51.1120924870195,-49.423475387907,
0.));
#138114=CARTESIAN_POINT('Ctrl Pts',(-51.1120924870195,-49.423475387907,
12.));
#138115=CARTESIAN_POINT('Ctrl Pts',(-51.0921914943662,-49.4136971040428,
0.));
#138116=CARTESIAN_POINT('Ctrl Pts',(-51.0921914943662,-49.4136971040428,
12.));
#138117=CARTESIAN_POINT('Ctrl Pts',(-51.0723425146985,-49.4039193088634,
0.));
#138118=CARTESIAN_POINT('Ctrl Pts',(-51.0723425146985,-49.4039193088634,
12.));
#138119=CARTESIAN_POINT('Ctrl Pts',(-51.052545646907,-49.3941421314013,
0.));
#138120=CARTESIAN_POINT('Ctrl Pts',(-51.052545646907,-49.3941421314013,
12.));
#138121=CARTESIAN_POINT('Ctrl Pts',(-51.0328009902858,-49.3843657013852,
0.));
#138122=CARTESIAN_POINT('Ctrl Pts',(-51.0328009902858,-49.3843657013852,
12.));
#138123=CARTESIAN_POINT('Ctrl Pts',(-51.0131086445272,-49.3745901492432,
0.));
#138124=CARTESIAN_POINT('Ctrl Pts',(-51.0131086445272,-49.3745901492432,
12.));
#138125=CARTESIAN_POINT('Ctrl Pts',(-50.9934687097188,-49.3648156061058,
0.));
#138126=CARTESIAN_POINT('Ctrl Pts',(-50.9934687097188,-49.3648156061058,
12.));
#138127=CARTESIAN_POINT('Ctrl Pts',(-50.9738812863646,-49.355042203823,
0.));
#138128=CARTESIAN_POINT('Ctrl Pts',(-50.9738812863646,-49.355042203823,
12.));
#138129=CARTESIAN_POINT('Ctrl Pts',(-50.9543464753981,-49.345270074981,
0.));
#138130=CARTESIAN_POINT('Ctrl Pts',(-50.9543464753981,-49.345270074981,
12.));
#138131=CARTESIAN_POINT('Ctrl Pts',(-50.9348643781924,-49.3354993529159,
0.));
#138132=CARTESIAN_POINT('Ctrl Pts',(-50.9348643781924,-49.3354993529159,
12.));
#138133=CARTESIAN_POINT('Ctrl Pts',(-50.9154350965666,-49.3257301717335,
0.));
#138134=CARTESIAN_POINT('Ctrl Pts',(-50.9154350965666,-49.3257301717335,
12.));
#138135=CARTESIAN_POINT('Ctrl Pts',(-50.8960587327848,-49.3159626663109,
0.));
#138136=CARTESIAN_POINT('Ctrl Pts',(-50.8960587327848,-49.3159626663109,
12.));
#138137=CARTESIAN_POINT('Ctrl Pts',(-50.8767353895492,-49.3061969722781,
0.));
#138138=CARTESIAN_POINT('Ctrl Pts',(-50.8767353895492,-49.3061969722781,
12.));
#138139=CARTESIAN_POINT('Ctrl Pts',(-50.8574651699873,-49.2964332260039,
0.));
#138140=CARTESIAN_POINT('Ctrl Pts',(-50.8574651699873,-49.2964332260039,
12.));
#138141=CARTESIAN_POINT('Ctrl Pts',(-50.8382481776403,-49.2866715645838,
0.));
#138142=CARTESIAN_POINT('Ctrl Pts',(-50.8382481776403,-49.2866715645838,
12.));
#138143=CARTESIAN_POINT('Ctrl Pts',(-50.819084516434,-49.2769121258164,
0.));
#138144=CARTESIAN_POINT('Ctrl Pts',(-50.819084516434,-49.2769121258164,
12.));
#138145=CARTESIAN_POINT('Ctrl Pts',(-50.7999742907131,-49.2671550482435,
0.));
#138146=CARTESIAN_POINT('Ctrl Pts',(-50.7999742907131,-49.2671550482435,
12.));
#138147=CARTESIAN_POINT('Ctrl Pts',(-50.7809176052966,-49.2574004712134,
0.));
#138148=CARTESIAN_POINT('Ctrl Pts',(-50.7809176052966,-49.2574004712134,
12.));
#138149=CARTESIAN_POINT('Ctrl Pts',(-50.7619145655207,-49.2476485349373,
0.));
#138150=CARTESIAN_POINT('Ctrl Pts',(-50.7619145655207,-49.2476485349373,
12.));
#138151=CARTESIAN_POINT('Ctrl Pts',(-50.7429652772805,-49.2378993805471,
0.));
#138152=CARTESIAN_POINT('Ctrl Pts',(-50.7429652772805,-49.2378993805471,
12.));
#138153=CARTESIAN_POINT('Ctrl Pts',(-50.7240698470679,-49.228153150155,
0.));
#138154=CARTESIAN_POINT('Ctrl Pts',(-50.7240698470679,-49.228153150155,
12.));
#138155=CARTESIAN_POINT('Ctrl Pts',(-50.7052283818922,-49.2184099867461,
0.));
#138156=CARTESIAN_POINT('Ctrl Pts',(-50.7052283818922,-49.2184099867461,
12.));
#138157=CARTESIAN_POINT('Ctrl Pts',(-50.6864409891895,-49.2086700340614,
0.));
#138158=CARTESIAN_POINT('Ctrl Pts',(-50.6864409891895,-49.2086700340614,
12.));
#138159=CARTESIAN_POINT('Ctrl Pts',(-50.6677077767432,-49.1989334364996,
0.));
#138160=CARTESIAN_POINT('Ctrl Pts',(-50.6677077767432,-49.1989334364996,
12.));
#138161=CARTESIAN_POINT('Ctrl Pts',(-50.6490288525656,-49.189200338976,
0.));
#138162=CARTESIAN_POINT('Ctrl Pts',(-50.6490288525656,-49.189200338976,
12.));
#138163=CARTESIAN_POINT('Ctrl Pts',(-50.6304043248821,-49.1794708869099,
0.));
#138164=CARTESIAN_POINT('Ctrl Pts',(-50.6304043248821,-49.1794708869099,
12.));
#138165=CARTESIAN_POINT('Ctrl Pts',(-50.6118343023958,-49.1697452265494,
0.));
#138166=CARTESIAN_POINT('Ctrl Pts',(-50.6118343023958,-49.1697452265494,
12.));
#138167=CARTESIAN_POINT('Ctrl Pts',(-50.5933188945168,-49.1600235052621,
0.));
#138168=CARTESIAN_POINT('Ctrl Pts',(-50.5933188945168,-49.1600235052621,
12.));
#138169=CARTESIAN_POINT('Ctrl Pts',(-50.5748582115565,-49.1503058717821,
0.));
#138170=CARTESIAN_POINT('Ctrl Pts',(-50.5748582115565,-49.1503058717821,
12.));
#138171=CARTESIAN_POINT('Ctrl Pts',(-50.556452365038,-49.1405924766144,
0.));
#138172=CARTESIAN_POINT('Ctrl Pts',(-50.556452365038,-49.1405924766144,
12.));
#138173=CARTESIAN_POINT('Ctrl Pts',(-50.5381014674791,-49.1308834717615,
0.));
#138174=CARTESIAN_POINT('Ctrl Pts',(-50.5381014674791,-49.1308834717615,
12.));
#138175=CARTESIAN_POINT('Ctrl Pts',(-50.5198056318089,-49.1211790099795,
0.));
#138176=CARTESIAN_POINT('Ctrl Pts',(-50.5198056318089,-49.1211790099795,
12.));
#138177=CARTESIAN_POINT('Ctrl Pts',(-50.501564970874,-49.1114792441571,
0.));
#138178=CARTESIAN_POINT('Ctrl Pts',(-50.501564970874,-49.1114792441571,
12.));
#138179=CARTESIAN_POINT('Ctrl Pts',(-50.4833795969318,-49.1017843266803,
0.));
#138180=CARTESIAN_POINT('Ctrl Pts',(-50.4833795969318,-49.1017843266803,
12.));
#138181=CARTESIAN_POINT('Ctrl Pts',(-50.4652496210607,-49.0920944087008,
0.));
#138182=CARTESIAN_POINT('Ctrl Pts',(-50.4652496210607,-49.0920944087008,
12.));
#138183=CARTESIAN_POINT('Ctrl Pts',(-50.4471751542751,-49.0824096415371,
0.));
#138184=CARTESIAN_POINT('Ctrl Pts',(-50.4471751542751,-49.0824096415371,
12.));
#138185=CARTESIAN_POINT('Ctrl Pts',(-50.4291563088547,-49.0727301783494,
0.));
#138186=CARTESIAN_POINT('Ctrl Pts',(-50.4291563088547,-49.0727301783494,
12.));
#138187=CARTESIAN_POINT('Ctrl Pts',(-50.4111931994257,-49.0630561755075,
0.));
#138188=CARTESIAN_POINT('Ctrl Pts',(-50.4111931994257,-49.0630561755075,
12.));
#138189=CARTESIAN_POINT('Ctrl Pts',(-50.3932859445252,-49.0533877945744,
0.));
#138190=CARTESIAN_POINT('Ctrl Pts',(-50.3932859445252,-49.0533877945744,
12.));
#138191=CARTESIAN_POINT('Ctrl Pts',(-50.3754346667353,-49.0437252024832,
0.));
#138192=CARTESIAN_POINT('Ctrl Pts',(-50.3754346667353,-49.0437252024832,
12.));
#138193=CARTESIAN_POINT('Ctrl Pts',(-50.3576394894108,-49.0340685673982,
0.));
#138194=CARTESIAN_POINT('Ctrl Pts',(-50.3576394894108,-49.0340685673982,
12.));
#138195=CARTESIAN_POINT('Ctrl Pts',(-50.3399005337958,-49.024418055075,
0.));
#138196=CARTESIAN_POINT('Ctrl Pts',(-50.3399005337958,-49.024418055075,
12.));
#138197=CARTESIAN_POINT('Ctrl Pts',(-50.3222179165119,-49.0147738256942,
0.));
#138198=CARTESIAN_POINT('Ctrl Pts',(-50.3222179165119,-49.0147738256942,
12.));
#138199=CARTESIAN_POINT('Ctrl Pts',(-50.3045917455424,-49.0051360288044,
0.));
#138200=CARTESIAN_POINT('Ctrl Pts',(-50.3045917455424,-49.0051360288044,
12.));
#138201=CARTESIAN_POINT('Ctrl Pts',(-50.2870221241054,-48.9955048082081,
0.));
#138202=CARTESIAN_POINT('Ctrl Pts',(-50.2870221241054,-48.9955048082081,
12.));
#138203=CARTESIAN_POINT('Ctrl Pts',(-50.2695091583511,-48.9858803116689,
0.));
#138204=CARTESIAN_POINT('Ctrl Pts',(-50.2695091583511,-48.9858803116689,
12.));
#138205=CARTESIAN_POINT('Ctrl Pts',(-50.252052963548,-48.9762626987227,
0.));
#138206=CARTESIAN_POINT('Ctrl Pts',(-50.252052963548,-48.9762626987227,
12.));
#138207=CARTESIAN_POINT('Ctrl Pts',(-50.234653671541,-48.9666521500911,
0.));
#138208=CARTESIAN_POINT('Ctrl Pts',(-50.234653671541,-48.9666521500911,
12.));
#138209=CARTESIAN_POINT('Ctrl Pts',(-50.2173114358325,-48.9570488741167,
0.));
#138210=CARTESIAN_POINT('Ctrl Pts',(-50.2173114358325,-48.9570488741167,
12.));
#138211=CARTESIAN_POINT('Ctrl Pts',(-50.2000264157797,-48.9474530868733,
0.));
#138212=CARTESIAN_POINT('Ctrl Pts',(-50.2000264157797,-48.9474530868733,
12.));
#138213=CARTESIAN_POINT('Ctrl Pts',(-50.1827987615602,-48.9378649933055,
0.));
#138214=CARTESIAN_POINT('Ctrl Pts',(-50.1827987615602,-48.9378649933055,
12.));
#138215=CARTESIAN_POINT('Ctrl Pts',(-50.1656286003997,-48.9282847698294,
0.));
#138216=CARTESIAN_POINT('Ctrl Pts',(-50.1656286003997,-48.9282847698294,
12.));
#138217=CARTESIAN_POINT('Ctrl Pts',(-50.1485160184657,-48.9187125418099,
0.));
#138218=CARTESIAN_POINT('Ctrl Pts',(-50.1485160184657,-48.9187125418099,
12.));
#138219=CARTESIAN_POINT('Ctrl Pts',(-50.1314610602569,-48.90914838181,0.));
#138220=CARTESIAN_POINT('Ctrl Pts',(-50.1314610602569,-48.90914838181,12.));
#138221=CARTESIAN_POINT('Ctrl Pts',(-50.1178632067084,-48.9015035372055,
0.));
#138222=CARTESIAN_POINT('Ctrl Pts',(-50.1178632067084,-48.9015035372055,
12.));
#138223=CARTESIAN_POINT('Ctrl Pts',(-50.1076907555471,-48.895773555686,
0.));
#138224=CARTESIAN_POINT('Ctrl Pts',(-50.1076907555471,-48.895773555686,
12.));
#138225=CARTESIAN_POINT('Ctrl Pts',(-50.1009206494272,-48.8919551910366,
0.));
#138226=CARTESIAN_POINT('Ctrl Pts',(-50.1009206494272,-48.8919551910366,
12.));
#138227=CARTESIAN_POINT('Ctrl Pts',(-50.0975384783635,-48.8900464144686,
0.));
#138228=CARTESIAN_POINT('Ctrl Pts',(-50.0975384783635,-48.8900464144686,
12.));
#138229=CARTESIAN_POINT('',(-50.0975384783635,-48.8900464144686,12.));
#138230=CARTESIAN_POINT('Ctrl Pts',(-50.0975384783635,-48.8900464144686,
12.));
#138231=CARTESIAN_POINT('Ctrl Pts',(-50.1009206494272,-48.8919551910366,
12.));
#138232=CARTESIAN_POINT('Ctrl Pts',(-50.1076907555471,-48.895773555686,
12.));
#138233=CARTESIAN_POINT('Ctrl Pts',(-50.1178632067084,-48.9015035372055,
12.));
#138234=CARTESIAN_POINT('Ctrl Pts',(-50.1314610602569,-48.90914838181,12.));
#138235=CARTESIAN_POINT('Ctrl Pts',(-50.1485160184657,-48.9187125418099,
12.));
#138236=CARTESIAN_POINT('Ctrl Pts',(-50.1656286003997,-48.9282847698294,
12.));
#138237=CARTESIAN_POINT('Ctrl Pts',(-50.1827987615602,-48.9378649933055,
12.));
#138238=CARTESIAN_POINT('Ctrl Pts',(-50.2000264157797,-48.9474530868733,
12.));
#138239=CARTESIAN_POINT('Ctrl Pts',(-50.2173114358325,-48.9570488741167,
12.));
#138240=CARTESIAN_POINT('Ctrl Pts',(-50.234653671541,-48.9666521500911,
12.));
#138241=CARTESIAN_POINT('Ctrl Pts',(-50.252052963548,-48.9762626987227,
12.));
#138242=CARTESIAN_POINT('Ctrl Pts',(-50.2695091583511,-48.9858803116689,
12.));
#138243=CARTESIAN_POINT('Ctrl Pts',(-50.2870221241054,-48.9955048082081,
12.));
#138244=CARTESIAN_POINT('Ctrl Pts',(-50.3045917455424,-49.0051360288044,
12.));
#138245=CARTESIAN_POINT('Ctrl Pts',(-50.3222179165119,-49.0147738256942,
12.));
#138246=CARTESIAN_POINT('Ctrl Pts',(-50.3399005337958,-49.024418055075,
12.));
#138247=CARTESIAN_POINT('Ctrl Pts',(-50.3576394894108,-49.0340685673982,
12.));
#138248=CARTESIAN_POINT('Ctrl Pts',(-50.3754346667353,-49.0437252024832,
12.));
#138249=CARTESIAN_POINT('Ctrl Pts',(-50.3932859445252,-49.0533877945744,
12.));
#138250=CARTESIAN_POINT('Ctrl Pts',(-50.4111931994257,-49.0630561755075,
12.));
#138251=CARTESIAN_POINT('Ctrl Pts',(-50.4291563088547,-49.0727301783494,
12.));
#138252=CARTESIAN_POINT('Ctrl Pts',(-50.4471751542751,-49.0824096415371,
12.));
#138253=CARTESIAN_POINT('Ctrl Pts',(-50.4652496210607,-49.0920944087008,
12.));
#138254=CARTESIAN_POINT('Ctrl Pts',(-50.4833795969318,-49.1017843266803,
12.));
#138255=CARTESIAN_POINT('Ctrl Pts',(-50.501564970874,-49.1114792441571,
12.));
#138256=CARTESIAN_POINT('Ctrl Pts',(-50.5198056318089,-49.1211790099795,
12.));
#138257=CARTESIAN_POINT('Ctrl Pts',(-50.5381014674791,-49.1308834717615,
12.));
#138258=CARTESIAN_POINT('Ctrl Pts',(-50.556452365038,-49.1405924766144,
12.));
#138259=CARTESIAN_POINT('Ctrl Pts',(-50.5748582115565,-49.1503058717821,
12.));
#138260=CARTESIAN_POINT('Ctrl Pts',(-50.5933188945168,-49.1600235052621,
12.));
#138261=CARTESIAN_POINT('Ctrl Pts',(-50.6118343023958,-49.1697452265494,
12.));
#138262=CARTESIAN_POINT('Ctrl Pts',(-50.6304043248821,-49.1794708869099,
12.));
#138263=CARTESIAN_POINT('Ctrl Pts',(-50.6490288525656,-49.189200338976,
12.));
#138264=CARTESIAN_POINT('Ctrl Pts',(-50.6677077767432,-49.1989334364996,
12.));
#138265=CARTESIAN_POINT('Ctrl Pts',(-50.6864409891895,-49.2086700340614,
12.));
#138266=CARTESIAN_POINT('Ctrl Pts',(-50.7052283818922,-49.2184099867461,
12.));
#138267=CARTESIAN_POINT('Ctrl Pts',(-50.7240698470679,-49.228153150155,
12.));
#138268=CARTESIAN_POINT('Ctrl Pts',(-50.7429652772805,-49.2378993805471,
12.));
#138269=CARTESIAN_POINT('Ctrl Pts',(-50.7619145655207,-49.2476485349373,
12.));
#138270=CARTESIAN_POINT('Ctrl Pts',(-50.7809176052966,-49.2574004712134,
12.));
#138271=CARTESIAN_POINT('Ctrl Pts',(-50.7999742907131,-49.2671550482435,
12.));
#138272=CARTESIAN_POINT('Ctrl Pts',(-50.819084516434,-49.2769121258164,
12.));
#138273=CARTESIAN_POINT('Ctrl Pts',(-50.8382481776403,-49.2866715645838,
12.));
#138274=CARTESIAN_POINT('Ctrl Pts',(-50.8574651699873,-49.2964332260039,
12.));
#138275=CARTESIAN_POINT('Ctrl Pts',(-50.8767353895492,-49.3061969722781,
12.));
#138276=CARTESIAN_POINT('Ctrl Pts',(-50.8960587327848,-49.3159626663109,
12.));
#138277=CARTESIAN_POINT('Ctrl Pts',(-50.9154350965666,-49.3257301717335,
12.));
#138278=CARTESIAN_POINT('Ctrl Pts',(-50.9348643781924,-49.3354993529159,
12.));
#138279=CARTESIAN_POINT('Ctrl Pts',(-50.9543464753981,-49.345270074981,
12.));
#138280=CARTESIAN_POINT('Ctrl Pts',(-50.9738812863646,-49.355042203823,
12.));
#138281=CARTESIAN_POINT('Ctrl Pts',(-50.9934687097188,-49.3648156061058,
12.));
#138282=CARTESIAN_POINT('Ctrl Pts',(-51.0131086445272,-49.3745901492432,
12.));
#138283=CARTESIAN_POINT('Ctrl Pts',(-51.0328009902858,-49.3843657013852,
12.));
#138284=CARTESIAN_POINT('Ctrl Pts',(-51.052545646907,-49.3941421314013,
12.));
#138285=CARTESIAN_POINT('Ctrl Pts',(-51.0723425146985,-49.4039193088634,
12.));
#138286=CARTESIAN_POINT('Ctrl Pts',(-51.0921914943662,-49.4136971040428,
12.));
#138287=CARTESIAN_POINT('Ctrl Pts',(-51.1120924870195,-49.423475387907,
12.));
#138288=CARTESIAN_POINT('Ctrl Pts',(-51.1320453941702,-49.4332540321178,
12.));
#138289=CARTESIAN_POINT('Ctrl Pts',(-51.1520501177291,-49.4430329090287,
12.));
#138290=CARTESIAN_POINT('Ctrl Pts',(-51.1721065599973,-49.4528118916832,
12.));
#138291=CARTESIAN_POINT('Ctrl Pts',(-51.1922146236686,-49.4625908538074,
12.));
#138292=CARTESIAN_POINT('Ctrl Pts',(-51.2123742118287,-49.4723696698021,
12.));
#138293=CARTESIAN_POINT('Ctrl Pts',(-51.2325852279506,-49.4821482147356,
12.));
#138294=CARTESIAN_POINT('Ctrl Pts',(-51.2528475758846,-49.4919263643362,
12.));
#138295=CARTESIAN_POINT('Ctrl Pts',(-51.2731611598475,-49.5017039949852,
12.));
#138296=CARTESIAN_POINT('Ctrl Pts',(-51.2935258844289,-49.5114809837122,
12.));
#138297=CARTESIAN_POINT('Ctrl Pts',(-51.313941654591,-49.5212572081908,
12.));
#138298=CARTESIAN_POINT('Ctrl Pts',(-51.3344083756657,-49.5310325467332,
12.));
#138299=CARTESIAN_POINT('Ctrl Pts',(-51.3549259533458,-49.5408068782859,
12.));
#138300=CARTESIAN_POINT('Ctrl Pts',(-51.3754942936778,-49.550580082425,
12.));
#138301=CARTESIAN_POINT('Ctrl Pts',(-51.396113303067,-49.5603520393496,
12.));
#138302=CARTESIAN_POINT('Ctrl Pts',(-51.4167828882756,-49.5701226298769,
12.));
#138303=CARTESIAN_POINT('Ctrl Pts',(-51.4375029564197,-49.5798917354366,
12.));
#138304=CARTESIAN_POINT('Ctrl Pts',(-51.4582734149583,-49.5896592380654,
12.));
#138305=CARTESIAN_POINT('Ctrl Pts',(-51.4790941716888,-49.5994250204031,
12.));
#138306=CARTESIAN_POINT('Ctrl Pts',(-51.4999651347523,-49.6091889656866,
12.));
#138307=CARTESIAN_POINT('Ctrl Pts',(-51.5208862126315,-49.6189509577452,
12.));
#138308=CARTESIAN_POINT('Ctrl Pts',(-51.5418573141484,-49.6287108809966,
12.));
#138309=CARTESIAN_POINT('Ctrl Pts',(-51.5628783484525,-49.6384686204413,
12.));
#138310=CARTESIAN_POINT('Ctrl Pts',(-51.5839492250181,-49.6482240616593,
12.));
#138311=CARTESIAN_POINT('Ctrl Pts',(-51.6050698536496,-49.6579770908037,
12.));
#138312=CARTESIAN_POINT('Ctrl Pts',(-51.626240144479,-49.6677275945967,
12.));
#138313=CARTESIAN_POINT('Ctrl Pts',(-51.6474600079622,-49.6774754603245,
12.));
#138314=CARTESIAN_POINT('Ctrl Pts',(-51.6687293548682,-49.6872205758336,
12.));
#138315=CARTESIAN_POINT('Ctrl Pts',(-51.6900480962773,-49.6969628295262,
12.));
#138316=CARTESIAN_POINT('Ctrl Pts',(-51.7114161435869,-49.7067021103553,
12.));
#138317=CARTESIAN_POINT('Ctrl Pts',(-51.7328334085091,-49.7164383078212,
12.));
#138318=CARTESIAN_POINT('Ctrl Pts',(-51.754299803067,-49.7261713119663,
12.));
#138319=CARTESIAN_POINT('Ctrl Pts',(-51.7758152395836,-49.7359010133721,
12.));
#138320=CARTESIAN_POINT('Ctrl Pts',(-51.7973796306803,-49.7456273031534,
12.));
#138321=CARTESIAN_POINT('Ctrl Pts',(-51.8189928892828,-49.755350072955,
12.));
#138322=CARTESIAN_POINT('Ctrl Pts',(-51.8406549286175,-49.7650692149462,
12.));
#138323=CARTESIAN_POINT('Ctrl Pts',(-51.8623656622097,-49.7747846218182,
12.));
#138324=CARTESIAN_POINT('Ctrl Pts',(-51.8841250038724,-49.7844961867808,
12.));
#138325=CARTESIAN_POINT('Ctrl Pts',(-51.9059328677059,-49.7942038035576,
12.));
#138326=CARTESIAN_POINT('Ctrl Pts',(-51.9277891681018,-49.8039073663812,
12.));
#138327=CARTESIAN_POINT('Ctrl Pts',(-51.9496938197418,-49.8136067699896,
12.));
#138328=CARTESIAN_POINT('Ctrl Pts',(-51.9716467375937,-49.8233019096222,
12.));
#138329=CARTESIAN_POINT('Ctrl Pts',(-51.9936478369008,-49.8329926810172,
12.));
#138330=CARTESIAN_POINT('Ctrl Pts',(-52.0156970331823,-49.8426789804071,
12.));
#138331=CARTESIAN_POINT('Ctrl Pts',(-52.0377942422376,-49.8523607045149,
12.));
#138332=CARTESIAN_POINT('Ctrl Pts',(-52.0599393801452,-49.86203775055,12.));
#138333=CARTESIAN_POINT('Ctrl Pts',(-52.0821323632587,-49.8717100162048,
12.));
#138334=CARTESIAN_POINT('Ctrl Pts',(-52.1043731081962,-49.8813773996517,
12.));
#138335=CARTESIAN_POINT('Ctrl Pts',(-52.1266615318407,-49.8910397995397,
12.));
#138336=CARTESIAN_POINT('Ctrl Pts',(-52.1489975513445,-49.9006971149895,
12.));
#138337=CARTESIAN_POINT('Ctrl Pts',(-52.1713810841276,-49.9103492455902,
12.));
#138338=CARTESIAN_POINT('Ctrl Pts',(-52.1938120478754,-49.9199960913962,
12.));
#138339=CARTESIAN_POINT('Ctrl Pts',(-52.2162903605275,-49.9296375529245,
12.));
#138340=CARTESIAN_POINT('Ctrl Pts',(-52.2388159402771,-49.9392735311509,
12.));
#138341=CARTESIAN_POINT('Ctrl Pts',(-52.2613887055773,-49.9489039275064,
12.));
#138342=CARTESIAN_POINT('Ctrl Pts',(-52.2840085751384,-49.9585286438733,
12.));
#138343=CARTESIAN_POINT('Ctrl Pts',(-52.3066754679265,-49.9681475825824,
12.));
#138344=CARTESIAN_POINT('Ctrl Pts',(-52.3293893031528,-49.9777606464106,
12.));
#138345=CARTESIAN_POINT('Ctrl Pts',(-52.3521500002718,-49.9873677385775,
12.));
#138346=CARTESIAN_POINT('Ctrl Pts',(-52.3749574789871,-49.9969687627408,
12.));
#138347=CARTESIAN_POINT('Ctrl Pts',(-52.3978116592509,-50.0065636229938,
12.));
#138348=CARTESIAN_POINT('Ctrl Pts',(-52.4207124612608,-50.0161522238616,
12.));
#138349=CARTESIAN_POINT('Ctrl Pts',(-52.4436598054515,-50.0257344703,12.));
#138350=CARTESIAN_POINT('Ctrl Pts',(-52.4666536124913,-50.0353102676921,
12.));
#138351=CARTESIAN_POINT('Ctrl Pts',(-52.4896938032884,-50.0448795218441,
12.));
#138352=CARTESIAN_POINT('Ctrl Pts',(-52.5127802989896,-50.0544421389818,
12.));
#138353=CARTESIAN_POINT('Ctrl Pts',(-52.5359130209792,-50.0639980257479,
12.));
#138354=CARTESIAN_POINT('Ctrl Pts',(-52.5590918908702,-50.0735470892007,
12.));
#138355=CARTESIAN_POINT('Ctrl Pts',(-52.5823168304994,-50.0830892368107,
12.));
#138356=CARTESIAN_POINT('Ctrl Pts',(-52.6055877619348,-50.0926243764578,
12.));
#138357=CARTESIAN_POINT('Ctrl Pts',(-52.6289046074746,-50.1021524164264,
12.));
#138358=CARTESIAN_POINT('Ctrl Pts',(-52.652267289646,-50.111673265404,12.));
#138359=CARTESIAN_POINT('Ctrl Pts',(-52.6756757311978,-50.1211868324781,
12.));
#138360=CARTESIAN_POINT('Ctrl Pts',(-52.699129855093,-50.1306930271345,
12.));
#138361=CARTESIAN_POINT('Ctrl Pts',(-52.7226295845161,-50.1401917592537,
12.));
#138362=CARTESIAN_POINT('Ctrl Pts',(-52.7461748428738,-50.1496829391073,
12.));
#138363=CARTESIAN_POINT('Ctrl Pts',(-52.769765553794,-50.1591664773561,
12.));
#138364=CARTESIAN_POINT('Ctrl Pts',(-52.7934016411205,-50.1686422850488,
12.));
#138365=CARTESIAN_POINT('Ctrl Pts',(-52.8170830289044,-50.1781102736205,
12.));
#138366=CARTESIAN_POINT('Ctrl Pts',(-52.8408096414093,-50.1875703548884,
12.));
#138367=CARTESIAN_POINT('Ctrl Pts',(-52.8645814031133,-50.1970224410471,
12.));
#138368=CARTESIAN_POINT('Ctrl Pts',(-52.8883982387068,-50.2064664446663,
12.));
#138369=CARTESIAN_POINT('Ctrl Pts',(-52.9122600730884,-50.2159022786879,
12.));
#138370=CARTESIAN_POINT('Ctrl Pts',(-52.9361668313542,-50.2253298564241,
12.));
#138371=CARTESIAN_POINT('Ctrl Pts',(-52.9601184388028,-50.2347490915555,
12.));
#138372=CARTESIAN_POINT('Ctrl Pts',(-52.9841148209402,-50.2441598981286,
12.));
#138373=CARTESIAN_POINT('Ctrl Pts',(-53.0081559034801,-50.2535621905552,
12.));
#138374=CARTESIAN_POINT('Ctrl Pts',(-53.0322416123406,-50.2629558836111,
12.));
#138375=CARTESIAN_POINT('Ctrl Pts',(-53.0563718736366,-50.2723408924373,
12.));
#138376=CARTESIAN_POINT('Ctrl Pts',(-53.0805466136798,-50.2817171325358,
12.));
#138377=CARTESIAN_POINT('Ctrl Pts',(-53.1047657589812,-50.2910845197619,
12.));
#138378=CARTESIAN_POINT('Ctrl Pts',(-53.1290292362485,-50.300442970319,
12.));
#138379=CARTESIAN_POINT('Ctrl Pts',(-53.1533369723818,-50.3097924007534,
12.));
#138380=CARTESIAN_POINT('Ctrl Pts',(-53.1776888944616,-50.3191327279493,
12.));
#138381=CARTESIAN_POINT('Ctrl Pts',(-53.2020849297471,-50.3284638691278,
12.));
#138382=CARTESIAN_POINT('Ctrl Pts',(-53.2265250056887,-50.3377857418515,
12.));
#138383=CARTESIAN_POINT('Ctrl Pts',(-53.2510090499336,-50.3470982640289,
12.));
#138384=CARTESIAN_POINT('Ctrl Pts',(-53.2755369903293,-50.3564013539199,
12.));
#138385=CARTESIAN_POINT('Ctrl Pts',(-53.300108754923,-50.365694930143,12.));
#138386=CARTESIAN_POINT('Ctrl Pts',(-53.3247242719587,-50.3749789116786,
12.));
#138387=CARTESIAN_POINT('Ctrl Pts',(-53.3493834698697,-50.384253217846,
12.));
#138388=CARTESIAN_POINT('Ctrl Pts',(-53.3740862772681,-50.3935177682837,
12.));
#138389=CARTESIAN_POINT('Ctrl Pts',(-53.398832622931,-50.4027724829297,
12.));
#138390=CARTESIAN_POINT('Ctrl Pts',(-53.4236224357838,-50.4120172820047,
12.));
#138391=CARTESIAN_POINT('Ctrl Pts',(-53.4484556448776,-50.4212520859914,
12.));
#138392=CARTESIAN_POINT('Ctrl Pts',(-53.4733321794188,-50.4304768156667,
12.));
#138393=CARTESIAN_POINT('Ctrl Pts',(-53.4982519688024,-50.4396913921382,
12.));
#138394=CARTESIAN_POINT('Ctrl Pts',(-53.5232149426413,-50.4488957368839,
12.));
#138395=CARTESIAN_POINT('Ctrl Pts',(-53.5482210307868,-50.4580897717838,
12.));
#138396=CARTESIAN_POINT('Ctrl Pts',(-53.5732701633609,-50.4672734191756,
12.));
#138397=CARTESIAN_POINT('Ctrl Pts',(-53.5983622707238,-50.4764466018071,
12.));
#138398=CARTESIAN_POINT('Ctrl Pts',(-53.623497283406,-50.4856092427314,
12.));
#138399=CARTESIAN_POINT('Ctrl Pts',(-53.6486751320436,-50.4947612652149,
12.));
#138400=CARTESIAN_POINT('Ctrl Pts',(-53.6738957473158,-50.503902592653,
12.));
#138401=CARTESIAN_POINT('Ctrl Pts',(-53.6991590598548,-50.513033148456,
12.));
#138402=CARTESIAN_POINT('Ctrl Pts',(-53.7244650002374,-50.522152856042,
12.));
#138403=CARTESIAN_POINT('Ctrl Pts',(-53.7498134991703,-50.5312616390779,
12.));
#138404=CARTESIAN_POINT('Ctrl Pts',(-53.7752044876304,-50.5403594216698,
12.));
#138405=CARTESIAN_POINT('Ctrl Pts',(-53.8006378970197,-50.5494461285761,
12.));
#138406=CARTESIAN_POINT('Ctrl Pts',(-53.8261136593075,-50.5585216854091,
12.));
#138407=CARTESIAN_POINT('Ctrl Pts',(-53.8516317071804,-50.5675860188538,
12.));
#138408=CARTESIAN_POINT('Ctrl Pts',(-53.8771919737032,-50.5766390561884,
12.));
#138409=CARTESIAN_POINT('Ctrl Pts',(-53.9027943919836,-50.5856807248151,
12.));
#138410=CARTESIAN_POINT('Ctrl Pts',(-53.9284388948004,-50.5947109517483,
12.));
#138411=CARTESIAN_POINT('Ctrl Pts',(-53.9541254143119,-50.603729663214,
12.));
#138412=CARTESIAN_POINT('Ctrl Pts',(-53.979853881553,-50.6127367839711,
12.));
#138413=CARTESIAN_POINT('Ctrl Pts',(-54.0056242268399,-50.6217322378648,
12.));
#138414=CARTESIAN_POINT('Ctrl Pts',(-54.0314363806708,-50.6307159490553,
12.));
#138415=CARTESIAN_POINT('Ctrl Pts',(-54.0572902745076,-50.6396878430939,
12.));
#138416=CARTESIAN_POINT('Ctrl Pts',(-54.0831858415189,-50.6486478479465,
12.));
#138417=CARTESIAN_POINT('Ctrl Pts',(-54.1091230175367,-50.6575958953221,
12.));
#138418=CARTESIAN_POINT('Ctrl Pts',(-54.1351017412804,-50.6665319209869,
12.));
#138419=CARTESIAN_POINT('Ctrl Pts',(-54.1574061042043,-50.6741814675486,
12.));
#138420=CARTESIAN_POINT('Ctrl Pts',(-54.1745287898797,-50.6800396668778,
12.));
#138421=CARTESIAN_POINT('Ctrl Pts',(-54.1864514382196,-50.6841118861931,
12.));
#138422=CARTESIAN_POINT('Ctrl Pts',(-54.1931619277624,-50.6864016965744,
12.));
#138423=CARTESIAN_POINT('Ctrl Pts',(-54.1946543500373,-50.6869108458851,
12.));
#138424=CARTESIAN_POINT('',(-50.0975384783635,-48.8900464144686,0.));
#138425=CARTESIAN_POINT('',(-50.0975384783634,-48.8900464144686,0.));
#138426=CARTESIAN_POINT('Ctrl Pts',(-54.1946543500373,-50.6869108458851,
0.));
#138427=CARTESIAN_POINT('Ctrl Pts',(-54.1931619277624,-50.6864016965744,
0.));
#138428=CARTESIAN_POINT('Ctrl Pts',(-54.1864514382196,-50.6841118861931,
0.));
#138429=CARTESIAN_POINT('Ctrl Pts',(-54.1745287898797,-50.6800396668778,
0.));
#138430=CARTESIAN_POINT('Ctrl Pts',(-54.1574061042043,-50.6741814675486,
0.));
#138431=CARTESIAN_POINT('Ctrl Pts',(-54.1351017412804,-50.6665319209869,
0.));
#138432=CARTESIAN_POINT('Ctrl Pts',(-54.1091230175367,-50.6575958953221,
0.));
#138433=CARTESIAN_POINT('Ctrl Pts',(-54.0831858415189,-50.6486478479465,
0.));
#138434=CARTESIAN_POINT('Ctrl Pts',(-54.0572902745076,-50.6396878430939,
0.));
#138435=CARTESIAN_POINT('Ctrl Pts',(-54.0314363806708,-50.6307159490553,
0.));
#138436=CARTESIAN_POINT('Ctrl Pts',(-54.0056242268399,-50.6217322378648,
0.));
#138437=CARTESIAN_POINT('Ctrl Pts',(-53.979853881553,-50.6127367839711,
0.));
#138438=CARTESIAN_POINT('Ctrl Pts',(-53.9541254143119,-50.603729663214,
0.));
#138439=CARTESIAN_POINT('Ctrl Pts',(-53.9284388948004,-50.5947109517483,
0.));
#138440=CARTESIAN_POINT('Ctrl Pts',(-53.9027943919836,-50.5856807248151,
0.));
#138441=CARTESIAN_POINT('Ctrl Pts',(-53.8771919737032,-50.5766390561884,
0.));
#138442=CARTESIAN_POINT('Ctrl Pts',(-53.8516317071804,-50.5675860188538,
0.));
#138443=CARTESIAN_POINT('Ctrl Pts',(-53.8261136593075,-50.5585216854091,
0.));
#138444=CARTESIAN_POINT('Ctrl Pts',(-53.8006378970197,-50.5494461285761,
0.));
#138445=CARTESIAN_POINT('Ctrl Pts',(-53.7752044876304,-50.5403594216698,
0.));
#138446=CARTESIAN_POINT('Ctrl Pts',(-53.7498134991703,-50.5312616390779,
0.));
#138447=CARTESIAN_POINT('Ctrl Pts',(-53.7244650002374,-50.522152856042,
0.));
#138448=CARTESIAN_POINT('Ctrl Pts',(-53.6991590598548,-50.513033148456,
0.));
#138449=CARTESIAN_POINT('Ctrl Pts',(-53.6738957473158,-50.503902592653,
0.));
#138450=CARTESIAN_POINT('Ctrl Pts',(-53.6486751320436,-50.4947612652149,
0.));
#138451=CARTESIAN_POINT('Ctrl Pts',(-53.623497283406,-50.4856092427314,
0.));
#138452=CARTESIAN_POINT('Ctrl Pts',(-53.5983622707238,-50.4764466018071,
0.));
#138453=CARTESIAN_POINT('Ctrl Pts',(-53.5732701633609,-50.4672734191756,
0.));
#138454=CARTESIAN_POINT('Ctrl Pts',(-53.5482210307868,-50.4580897717838,
0.));
#138455=CARTESIAN_POINT('Ctrl Pts',(-53.5232149426413,-50.4488957368839,
0.));
#138456=CARTESIAN_POINT('Ctrl Pts',(-53.4982519688024,-50.4396913921382,
0.));
#138457=CARTESIAN_POINT('Ctrl Pts',(-53.4733321794188,-50.4304768156667,
0.));
#138458=CARTESIAN_POINT('Ctrl Pts',(-53.4484556448776,-50.4212520859914,
0.));
#138459=CARTESIAN_POINT('Ctrl Pts',(-53.4236224357838,-50.4120172820047,
0.));
#138460=CARTESIAN_POINT('Ctrl Pts',(-53.398832622931,-50.4027724829297,
0.));
#138461=CARTESIAN_POINT('Ctrl Pts',(-53.3740862772681,-50.3935177682837,
0.));
#138462=CARTESIAN_POINT('Ctrl Pts',(-53.3493834698697,-50.384253217846,
0.));
#138463=CARTESIAN_POINT('Ctrl Pts',(-53.3247242719587,-50.3749789116786,
0.));
#138464=CARTESIAN_POINT('Ctrl Pts',(-53.300108754923,-50.365694930143,0.));
#138465=CARTESIAN_POINT('Ctrl Pts',(-53.2755369903293,-50.3564013539199,
0.));
#138466=CARTESIAN_POINT('Ctrl Pts',(-53.2510090499336,-50.3470982640289,
0.));
#138467=CARTESIAN_POINT('Ctrl Pts',(-53.2265250056887,-50.3377857418515,
0.));
#138468=CARTESIAN_POINT('Ctrl Pts',(-53.2020849297471,-50.3284638691278,
0.));
#138469=CARTESIAN_POINT('Ctrl Pts',(-53.1776888944616,-50.3191327279493,
0.));
#138470=CARTESIAN_POINT('Ctrl Pts',(-53.1533369723818,-50.3097924007534,
0.));
#138471=CARTESIAN_POINT('Ctrl Pts',(-53.1290292362485,-50.300442970319,
0.));
#138472=CARTESIAN_POINT('Ctrl Pts',(-53.1047657589812,-50.2910845197619,
0.));
#138473=CARTESIAN_POINT('Ctrl Pts',(-53.0805466136798,-50.2817171325358,
0.));
#138474=CARTESIAN_POINT('Ctrl Pts',(-53.0563718736366,-50.2723408924373,
0.));
#138475=CARTESIAN_POINT('Ctrl Pts',(-53.0322416123406,-50.2629558836111,
0.));
#138476=CARTESIAN_POINT('Ctrl Pts',(-53.0081559034801,-50.2535621905552,
0.));
#138477=CARTESIAN_POINT('Ctrl Pts',(-52.9841148209402,-50.2441598981286,
0.));
#138478=CARTESIAN_POINT('Ctrl Pts',(-52.9601184388028,-50.2347490915555,
0.));
#138479=CARTESIAN_POINT('Ctrl Pts',(-52.9361668313542,-50.2253298564241,
0.));
#138480=CARTESIAN_POINT('Ctrl Pts',(-52.9122600730884,-50.2159022786879,
0.));
#138481=CARTESIAN_POINT('Ctrl Pts',(-52.8883982387068,-50.2064664446663,
0.));
#138482=CARTESIAN_POINT('Ctrl Pts',(-52.8645814031133,-50.1970224410471,
0.));
#138483=CARTESIAN_POINT('Ctrl Pts',(-52.8408096414093,-50.1875703548884,
0.));
#138484=CARTESIAN_POINT('Ctrl Pts',(-52.8170830289044,-50.1781102736205,
0.));
#138485=CARTESIAN_POINT('Ctrl Pts',(-52.7934016411205,-50.1686422850488,
0.));
#138486=CARTESIAN_POINT('Ctrl Pts',(-52.769765553794,-50.1591664773561,
0.));
#138487=CARTESIAN_POINT('Ctrl Pts',(-52.7461748428738,-50.1496829391073,
0.));
#138488=CARTESIAN_POINT('Ctrl Pts',(-52.7226295845161,-50.1401917592537,
0.));
#138489=CARTESIAN_POINT('Ctrl Pts',(-52.699129855093,-50.1306930271345,
0.));
#138490=CARTESIAN_POINT('Ctrl Pts',(-52.6756757311978,-50.1211868324781,
0.));
#138491=CARTESIAN_POINT('Ctrl Pts',(-52.652267289646,-50.111673265404,0.));
#138492=CARTESIAN_POINT('Ctrl Pts',(-52.6289046074746,-50.1021524164264,
0.));
#138493=CARTESIAN_POINT('Ctrl Pts',(-52.6055877619348,-50.0926243764578,
0.));
#138494=CARTESIAN_POINT('Ctrl Pts',(-52.5823168304994,-50.0830892368107,
0.));
#138495=CARTESIAN_POINT('Ctrl Pts',(-52.5590918908702,-50.0735470892007,
0.));
#138496=CARTESIAN_POINT('Ctrl Pts',(-52.5359130209792,-50.0639980257479,
0.));
#138497=CARTESIAN_POINT('Ctrl Pts',(-52.5127802989896,-50.0544421389818,
0.));
#138498=CARTESIAN_POINT('Ctrl Pts',(-52.4896938032884,-50.0448795218441,
0.));
#138499=CARTESIAN_POINT('Ctrl Pts',(-52.4666536124913,-50.0353102676921,
0.));
#138500=CARTESIAN_POINT('Ctrl Pts',(-52.4436598054515,-50.0257344703,0.));
#138501=CARTESIAN_POINT('Ctrl Pts',(-52.4207124612608,-50.0161522238616,
0.));
#138502=CARTESIAN_POINT('Ctrl Pts',(-52.3978116592509,-50.0065636229938,
0.));
#138503=CARTESIAN_POINT('Ctrl Pts',(-52.3749574789871,-49.9969687627408,
0.));
#138504=CARTESIAN_POINT('Ctrl Pts',(-52.3521500002718,-49.9873677385775,
0.));
#138505=CARTESIAN_POINT('Ctrl Pts',(-52.3293893031528,-49.9777606464106,
0.));
#138506=CARTESIAN_POINT('Ctrl Pts',(-52.3066754679265,-49.9681475825824,
0.));
#138507=CARTESIAN_POINT('Ctrl Pts',(-52.2840085751384,-49.9585286438733,
0.));
#138508=CARTESIAN_POINT('Ctrl Pts',(-52.2613887055773,-49.9489039275064,
0.));
#138509=CARTESIAN_POINT('Ctrl Pts',(-52.2388159402771,-49.9392735311509,
0.));
#138510=CARTESIAN_POINT('Ctrl Pts',(-52.2162903605275,-49.9296375529245,
0.));
#138511=CARTESIAN_POINT('Ctrl Pts',(-52.1938120478754,-49.9199960913962,
0.));
#138512=CARTESIAN_POINT('Ctrl Pts',(-52.1713810841276,-49.9103492455902,
0.));
#138513=CARTESIAN_POINT('Ctrl Pts',(-52.1489975513445,-49.9006971149895,
0.));
#138514=CARTESIAN_POINT('Ctrl Pts',(-52.1266615318407,-49.8910397995397,
0.));
#138515=CARTESIAN_POINT('Ctrl Pts',(-52.1043731081962,-49.8813773996517,
0.));
#138516=CARTESIAN_POINT('Ctrl Pts',(-52.0821323632587,-49.8717100162048,
0.));
#138517=CARTESIAN_POINT('Ctrl Pts',(-52.0599393801452,-49.86203775055,0.));
#138518=CARTESIAN_POINT('Ctrl Pts',(-52.0377942422376,-49.8523607045149,
0.));
#138519=CARTESIAN_POINT('Ctrl Pts',(-52.0156970331823,-49.8426789804071,
0.));
#138520=CARTESIAN_POINT('Ctrl Pts',(-51.9936478369008,-49.8329926810172,
0.));
#138521=CARTESIAN_POINT('Ctrl Pts',(-51.9716467375937,-49.8233019096222,
0.));
#138522=CARTESIAN_POINT('Ctrl Pts',(-51.9496938197418,-49.8136067699896,
0.));
#138523=CARTESIAN_POINT('Ctrl Pts',(-51.9277891681018,-49.8039073663812,
0.));
#138524=CARTESIAN_POINT('Ctrl Pts',(-51.9059328677059,-49.7942038035576,
0.));
#138525=CARTESIAN_POINT('Ctrl Pts',(-51.8841250038724,-49.7844961867808,
0.));
#138526=CARTESIAN_POINT('Ctrl Pts',(-51.8623656622097,-49.7747846218182,
0.));
#138527=CARTESIAN_POINT('Ctrl Pts',(-51.8406549286175,-49.7650692149462,
0.));
#138528=CARTESIAN_POINT('Ctrl Pts',(-51.8189928892828,-49.755350072955,
0.));
#138529=CARTESIAN_POINT('Ctrl Pts',(-51.7973796306803,-49.7456273031534,
0.));
#138530=CARTESIAN_POINT('Ctrl Pts',(-51.7758152395836,-49.7359010133721,
0.));
#138531=CARTESIAN_POINT('Ctrl Pts',(-51.754299803067,-49.7261713119663,
0.));
#138532=CARTESIAN_POINT('Ctrl Pts',(-51.7328334085091,-49.7164383078212,
0.));
#138533=CARTESIAN_POINT('Ctrl Pts',(-51.7114161435869,-49.7067021103553,
0.));
#138534=CARTESIAN_POINT('Ctrl Pts',(-51.6900480962773,-49.6969628295262,
0.));
#138535=CARTESIAN_POINT('Ctrl Pts',(-51.6687293548682,-49.6872205758336,
0.));
#138536=CARTESIAN_POINT('Ctrl Pts',(-51.6474600079622,-49.6774754603245,
0.));
#138537=CARTESIAN_POINT('Ctrl Pts',(-51.626240144479,-49.6677275945967,
0.));
#138538=CARTESIAN_POINT('Ctrl Pts',(-51.6050698536496,-49.6579770908037,
0.));
#138539=CARTESIAN_POINT('Ctrl Pts',(-51.5839492250181,-49.6482240616593,
0.));
#138540=CARTESIAN_POINT('Ctrl Pts',(-51.5628783484525,-49.6384686204413,
0.));
#138541=CARTESIAN_POINT('Ctrl Pts',(-51.5418573141484,-49.6287108809966,
0.));
#138542=CARTESIAN_POINT('Ctrl Pts',(-51.5208862126315,-49.6189509577452,
0.));
#138543=CARTESIAN_POINT('Ctrl Pts',(-51.4999651347523,-49.6091889656866,
0.));
#138544=CARTESIAN_POINT('Ctrl Pts',(-51.4790941716888,-49.5994250204031,
0.));
#138545=CARTESIAN_POINT('Ctrl Pts',(-51.4582734149583,-49.5896592380654,
0.));
#138546=CARTESIAN_POINT('Ctrl Pts',(-51.4375029564197,-49.5798917354366,
0.));
#138547=CARTESIAN_POINT('Ctrl Pts',(-51.4167828882756,-49.5701226298769,
0.));
#138548=CARTESIAN_POINT('Ctrl Pts',(-51.396113303067,-49.5603520393496,
0.));
#138549=CARTESIAN_POINT('Ctrl Pts',(-51.3754942936778,-49.550580082425,
0.));
#138550=CARTESIAN_POINT('Ctrl Pts',(-51.3549259533458,-49.5408068782859,
0.));
#138551=CARTESIAN_POINT('Ctrl Pts',(-51.3344083756657,-49.5310325467332,
0.));
#138552=CARTESIAN_POINT('Ctrl Pts',(-51.313941654591,-49.5212572081908,
0.));
#138553=CARTESIAN_POINT('Ctrl Pts',(-51.2935258844289,-49.5114809837122,
0.));
#138554=CARTESIAN_POINT('Ctrl Pts',(-51.2731611598475,-49.5017039949852,
0.));
#138555=CARTESIAN_POINT('Ctrl Pts',(-51.2528475758846,-49.4919263643362,
0.));
#138556=CARTESIAN_POINT('Ctrl Pts',(-51.2325852279506,-49.4821482147356,
0.));
#138557=CARTESIAN_POINT('Ctrl Pts',(-51.2123742118287,-49.4723696698021,
0.));
#138558=CARTESIAN_POINT('Ctrl Pts',(-51.1922146236686,-49.4625908538074,
0.));
#138559=CARTESIAN_POINT('Ctrl Pts',(-51.1721065599973,-49.4528118916832,
0.));
#138560=CARTESIAN_POINT('Ctrl Pts',(-51.1520501177291,-49.4430329090287,
0.));
#138561=CARTESIAN_POINT('Ctrl Pts',(-51.1320453941702,-49.4332540321178,
0.));
#138562=CARTESIAN_POINT('Ctrl Pts',(-51.1120924870195,-49.423475387907,
0.));
#138563=CARTESIAN_POINT('Ctrl Pts',(-51.0921914943662,-49.4136971040428,
0.));
#138564=CARTESIAN_POINT('Ctrl Pts',(-51.0723425146985,-49.4039193088634,
0.));
#138565=CARTESIAN_POINT('Ctrl Pts',(-51.052545646907,-49.3941421314013,
0.));
#138566=CARTESIAN_POINT('Ctrl Pts',(-51.0328009902858,-49.3843657013852,
0.));
#138567=CARTESIAN_POINT('Ctrl Pts',(-51.0131086445272,-49.3745901492432,
0.));
#138568=CARTESIAN_POINT('Ctrl Pts',(-50.9934687097188,-49.3648156061058,
0.));
#138569=CARTESIAN_POINT('Ctrl Pts',(-50.9738812863646,-49.355042203823,
0.));
#138570=CARTESIAN_POINT('Ctrl Pts',(-50.9543464753981,-49.345270074981,
0.));
#138571=CARTESIAN_POINT('Ctrl Pts',(-50.9348643781924,-49.3354993529159,
0.));
#138572=CARTESIAN_POINT('Ctrl Pts',(-50.9154350965666,-49.3257301717335,
0.));
#138573=CARTESIAN_POINT('Ctrl Pts',(-50.8960587327848,-49.3159626663109,
0.));
#138574=CARTESIAN_POINT('Ctrl Pts',(-50.8767353895492,-49.3061969722781,
0.));
#138575=CARTESIAN_POINT('Ctrl Pts',(-50.8574651699873,-49.2964332260039,
0.));
#138576=CARTESIAN_POINT('Ctrl Pts',(-50.8382481776403,-49.2866715645838,
0.));
#138577=CARTESIAN_POINT('Ctrl Pts',(-50.819084516434,-49.2769121258164,
0.));
#138578=CARTESIAN_POINT('Ctrl Pts',(-50.7999742907131,-49.2671550482435,
0.));
#138579=CARTESIAN_POINT('Ctrl Pts',(-50.7809176052966,-49.2574004712134,
0.));
#138580=CARTESIAN_POINT('Ctrl Pts',(-50.7619145655207,-49.2476485349373,
0.));
#138581=CARTESIAN_POINT('Ctrl Pts',(-50.7429652772805,-49.2378993805471,
0.));
#138582=CARTESIAN_POINT('Ctrl Pts',(-50.7240698470679,-49.228153150155,
0.));
#138583=CARTESIAN_POINT('Ctrl Pts',(-50.7052283818922,-49.2184099867461,
0.));
#138584=CARTESIAN_POINT('Ctrl Pts',(-50.6864409891895,-49.2086700340614,
0.));
#138585=CARTESIAN_POINT('Ctrl Pts',(-50.6677077767432,-49.1989334364996,
0.));
#138586=CARTESIAN_POINT('Ctrl Pts',(-50.6490288525656,-49.189200338976,
0.));
#138587=CARTESIAN_POINT('Ctrl Pts',(-50.6304043248821,-49.1794708869099,
0.));
#138588=CARTESIAN_POINT('Ctrl Pts',(-50.6118343023958,-49.1697452265494,
0.));
#138589=CARTESIAN_POINT('Ctrl Pts',(-50.5933188945168,-49.1600235052621,
0.));
#138590=CARTESIAN_POINT('Ctrl Pts',(-50.5748582115565,-49.1503058717821,
0.));
#138591=CARTESIAN_POINT('Ctrl Pts',(-50.556452365038,-49.1405924766144,
0.));
#138592=CARTESIAN_POINT('Ctrl Pts',(-50.5381014674791,-49.1308834717615,
0.));
#138593=CARTESIAN_POINT('Ctrl Pts',(-50.5198056318089,-49.1211790099795,
0.));
#138594=CARTESIAN_POINT('Ctrl Pts',(-50.501564970874,-49.1114792441571,
0.));
#138595=CARTESIAN_POINT('Ctrl Pts',(-50.4833795969318,-49.1017843266803,
0.));
#138596=CARTESIAN_POINT('Ctrl Pts',(-50.4652496210607,-49.0920944087008,
0.));
#138597=CARTESIAN_POINT('Ctrl Pts',(-50.4471751542751,-49.0824096415371,
0.));
#138598=CARTESIAN_POINT('Ctrl Pts',(-50.4291563088547,-49.0727301783494,
0.));
#138599=CARTESIAN_POINT('Ctrl Pts',(-50.4111931994257,-49.0630561755075,
0.));
#138600=CARTESIAN_POINT('Ctrl Pts',(-50.3932859445252,-49.0533877945744,
0.));
#138601=CARTESIAN_POINT('Ctrl Pts',(-50.3754346667353,-49.0437252024832,
0.));
#138602=CARTESIAN_POINT('Ctrl Pts',(-50.3576394894108,-49.0340685673982,
0.));
#138603=CARTESIAN_POINT('Ctrl Pts',(-50.3399005337958,-49.024418055075,
0.));
#138604=CARTESIAN_POINT('Ctrl Pts',(-50.3222179165119,-49.0147738256942,
0.));
#138605=CARTESIAN_POINT('Ctrl Pts',(-50.3045917455424,-49.0051360288044,
0.));
#138606=CARTESIAN_POINT('Ctrl Pts',(-50.2870221241054,-48.9955048082081,
0.));
#138607=CARTESIAN_POINT('Ctrl Pts',(-50.2695091583511,-48.9858803116689,
0.));
#138608=CARTESIAN_POINT('Ctrl Pts',(-50.252052963548,-48.9762626987227,
0.));
#138609=CARTESIAN_POINT('Ctrl Pts',(-50.234653671541,-48.9666521500911,
0.));
#138610=CARTESIAN_POINT('Ctrl Pts',(-50.2173114358325,-48.9570488741167,
0.));
#138611=CARTESIAN_POINT('Ctrl Pts',(-50.2000264157797,-48.9474530868733,
0.));
#138612=CARTESIAN_POINT('Ctrl Pts',(-50.1827987615602,-48.9378649933055,
0.));
#138613=CARTESIAN_POINT('Ctrl Pts',(-50.1656286003997,-48.9282847698294,
0.));
#138614=CARTESIAN_POINT('Ctrl Pts',(-50.1485160184657,-48.9187125418099,
0.));
#138615=CARTESIAN_POINT('Ctrl Pts',(-50.1314610602569,-48.90914838181,0.));
#138616=CARTESIAN_POINT('Ctrl Pts',(-50.1178632067084,-48.9015035372055,
0.));
#138617=CARTESIAN_POINT('Ctrl Pts',(-50.1076907555471,-48.895773555686,
0.));
#138618=CARTESIAN_POINT('Ctrl Pts',(-50.1009206494272,-48.8919551910366,
0.));
#138619=CARTESIAN_POINT('Ctrl Pts',(-50.0975384783635,-48.8900464144686,
0.));
#138620=CARTESIAN_POINT('Ctrl Pts',(-58.722407829904,-45.8467972562798,
0.));
#138621=CARTESIAN_POINT('Ctrl Pts',(-58.722407829904,-45.8467972562798,
12.));
#138622=CARTESIAN_POINT('Ctrl Pts',(-58.7169606500268,-45.8455162977427,
0.));
#138623=CARTESIAN_POINT('Ctrl Pts',(-58.7169606500268,-45.8455162977427,
12.));
#138624=CARTESIAN_POINT('Ctrl Pts',(-58.7060702401686,-45.8429527488786,
0.));
#138625=CARTESIAN_POINT('Ctrl Pts',(-58.7060702401686,-45.8429527488786,
12.));
#138626=CARTESIAN_POINT('Ctrl Pts',(-58.68974647507,-45.8391025302132,0.));
#138627=CARTESIAN_POINT('Ctrl Pts',(-58.68974647507,-45.8391025302132,12.));
#138628=CARTESIAN_POINT('Ctrl Pts',(-58.6680051552762,-45.8339591141834,
0.));
#138629=CARTESIAN_POINT('Ctrl Pts',(-58.6680051552762,-45.8339591141834,
12.));
#138630=CARTESIAN_POINT('Ctrl Pts',(-58.6408680154016,-45.8275135264249,
0.));
#138631=CARTESIAN_POINT('Ctrl Pts',(-58.6408680154016,-45.8275135264249,
12.));
#138632=CARTESIAN_POINT('Ctrl Pts',(-58.6137704035871,-45.8210516273781,
0.));
#138633=CARTESIAN_POINT('Ctrl Pts',(-58.6137704035871,-45.8210516273781,
12.));
#138634=CARTESIAN_POINT('Ctrl Pts',(-58.5867123491018,-45.814573433072,
0.));
#138635=CARTESIAN_POINT('Ctrl Pts',(-58.5867123491018,-45.814573433072,
12.));
#138636=CARTESIAN_POINT('Ctrl Pts',(-58.5596938940195,-45.8080789725084,
0.));
#138637=CARTESIAN_POINT('Ctrl Pts',(-58.5596938940195,-45.8080789725084,
12.));
#138638=CARTESIAN_POINT('Ctrl Pts',(-58.5327150960661,-45.8015682926024,
0.));
#138639=CARTESIAN_POINT('Ctrl Pts',(-58.5327150960661,-45.8015682926024,
12.));
#138640=CARTESIAN_POINT('Ctrl Pts',(-58.5057760270184,-45.7950414569268,
0.));
#138641=CARTESIAN_POINT('Ctrl Pts',(-58.5057760270184,-45.7950414569268,
12.));
#138642=CARTESIAN_POINT('Ctrl Pts',(-58.4788767676949,-45.7884985397018,
0.));
#138643=CARTESIAN_POINT('Ctrl Pts',(-58.4788767676949,-45.7884985397018,
12.));
#138644=CARTESIAN_POINT('Ctrl Pts',(-58.4520174038764,-45.7819396211009,
0.));
#138645=CARTESIAN_POINT('Ctrl Pts',(-58.4520174038764,-45.7819396211009,
12.));
#138646=CARTESIAN_POINT('Ctrl Pts',(-58.425198021955,-45.7753647821513,
0.));
#138647=CARTESIAN_POINT('Ctrl Pts',(-58.425198021955,-45.7753647821513,
12.));
#138648=CARTESIAN_POINT('Ctrl Pts',(-58.3984187044245,-45.7687740994956,
0.));
#138649=CARTESIAN_POINT('Ctrl Pts',(-58.3984187044245,-45.7687740994956,
12.));
#138650=CARTESIAN_POINT('Ctrl Pts',(-58.3716795262353,-45.7621676411434,
0.));
#138651=CARTESIAN_POINT('Ctrl Pts',(-58.3716795262353,-45.7621676411434,
12.));
#138652=CARTESIAN_POINT('Ctrl Pts',(-58.3449805573423,-45.755545469402,
0.));
#138653=CARTESIAN_POINT('Ctrl Pts',(-58.3449805573423,-45.755545469402,
12.));
#138654=CARTESIAN_POINT('Ctrl Pts',(-58.3183218645317,-45.7489076429763,
0.));
#138655=CARTESIAN_POINT('Ctrl Pts',(-58.3183218645317,-45.7489076429763,
12.));
#138656=CARTESIAN_POINT('Ctrl Pts',(-58.291703513584,-45.742254219463,0.));
#138657=CARTESIAN_POINT('Ctrl Pts',(-58.291703513584,-45.742254219463,12.));
#138658=CARTESIAN_POINT('Ctrl Pts',(-58.2651255711453,-45.7355852575106,
0.));
#138659=CARTESIAN_POINT('Ctrl Pts',(-58.2651255711453,-45.7355852575106,
12.));
#138660=CARTESIAN_POINT('Ctrl Pts',(-58.2385881070913,-45.7289008195578,
0.));
#138661=CARTESIAN_POINT('Ctrl Pts',(-58.2385881070913,-45.7289008195578,
12.));
#138662=CARTESIAN_POINT('Ctrl Pts',(-58.2120911942772,-45.7222009715397,
0.));
#138663=CARTESIAN_POINT('Ctrl Pts',(-58.2120911942772,-45.7222009715397,
12.));
#138664=CARTESIAN_POINT('Ctrl Pts',(-58.185634907469,-45.7154857816483,
0.));
#138665=CARTESIAN_POINT('Ctrl Pts',(-58.185634907469,-45.7154857816483,
12.));
#138666=CARTESIAN_POINT('Ctrl Pts',(-58.1592193225137,-45.7087553193771,
0.));
#138667=CARTESIAN_POINT('Ctrl Pts',(-58.1592193225137,-45.7087553193771,
12.));
#138668=CARTESIAN_POINT('Ctrl Pts',(-58.1328445154676,-45.702009654518,
0.));
#138669=CARTESIAN_POINT('Ctrl Pts',(-58.1328445154676,-45.702009654518,
12.));
#138670=CARTESIAN_POINT('Ctrl Pts',(-58.1065105615907,-45.695248856015,
0.));
#138671=CARTESIAN_POINT('Ctrl Pts',(-58.1065105615907,-45.695248856015,
12.));
#138672=CARTESIAN_POINT('Ctrl Pts',(-58.0802175348966,-45.6884729914485,
0.));
#138673=CARTESIAN_POINT('Ctrl Pts',(-58.0802175348966,-45.6884729914485,
12.));
#138674=CARTESIAN_POINT('Ctrl Pts',(-58.0539655087117,-45.6816821276678,
0.));
#138675=CARTESIAN_POINT('Ctrl Pts',(-58.0539655087117,-45.6816821276678,
12.));
#138676=CARTESIAN_POINT('Ctrl Pts',(-58.0277545560012,-45.6748763311643,
0.));
#138677=CARTESIAN_POINT('Ctrl Pts',(-58.0277545560012,-45.6748763311643,
12.));
#138678=CARTESIAN_POINT('Ctrl Pts',(-58.0015847497837,-45.6680556685493,
0.));
#138679=CARTESIAN_POINT('Ctrl Pts',(-58.0015847497837,-45.6680556685493,
12.));
#138680=CARTESIAN_POINT('Ctrl Pts',(-57.9754561635061,-45.661220206992,
0.));
#138681=CARTESIAN_POINT('Ctrl Pts',(-57.9754561635061,-45.661220206992,
12.));
#138682=CARTESIAN_POINT('Ctrl Pts',(-57.9493688714237,-45.6543700146679,
0.));
#138683=CARTESIAN_POINT('Ctrl Pts',(-57.9493688714237,-45.6543700146679,
12.));
#138684=CARTESIAN_POINT('Ctrl Pts',(-57.9233229484311,-45.6475051605535,
0.));
#138685=CARTESIAN_POINT('Ctrl Pts',(-57.9233229484311,-45.6475051605535,
12.));
#138686=CARTESIAN_POINT('Ctrl Pts',(-57.8973184699034,-45.6406257142381,
0.));
#138687=CARTESIAN_POINT('Ctrl Pts',(-57.8973184699034,-45.6406257142381,
12.));
#138688=CARTESIAN_POINT('Ctrl Pts',(-57.8713555115232,-45.6337317457252,
0.));
#138689=CARTESIAN_POINT('Ctrl Pts',(-57.8713555115232,-45.6337317457252,
12.));
#138690=CARTESIAN_POINT('Ctrl Pts',(-57.8454341491238,-45.6268233252544,
0.));
#138691=CARTESIAN_POINT('Ctrl Pts',(-57.8454341491238,-45.6268233252544,
12.));
#138692=CARTESIAN_POINT('Ctrl Pts',(-57.8195544584845,-45.6199005230783,
0.));
#138693=CARTESIAN_POINT('Ctrl Pts',(-57.8195544584845,-45.6199005230783,
12.));
#138694=CARTESIAN_POINT('Ctrl Pts',(-57.7937165153387,-45.6129634094683,
0.));
#138695=CARTESIAN_POINT('Ctrl Pts',(-57.7937165153387,-45.6129634094683,
12.));
#138696=CARTESIAN_POINT('Ctrl Pts',(-57.7679203954742,-45.6060120548205,
0.));
#138697=CARTESIAN_POINT('Ctrl Pts',(-57.7679203954742,-45.6060120548205,
12.));
#138698=CARTESIAN_POINT('Ctrl Pts',(-57.7421661748026,-45.5990465297343,
0.));
#138699=CARTESIAN_POINT('Ctrl Pts',(-57.7421661748026,-45.5990465297343,
12.));
#138700=CARTESIAN_POINT('Ctrl Pts',(-57.7164539294314,-45.5920669050986,
0.));
#138701=CARTESIAN_POINT('Ctrl Pts',(-57.7164539294314,-45.5920669050986,
12.));
#138702=CARTESIAN_POINT('Ctrl Pts',(-57.6907837357418,-45.5850732521895,
0.));
#138703=CARTESIAN_POINT('Ctrl Pts',(-57.6907837357418,-45.5850732521895,
12.));
#138704=CARTESIAN_POINT('Ctrl Pts',(-57.6651556704237,-45.5780656427163,
0.));
#138705=CARTESIAN_POINT('Ctrl Pts',(-57.6651556704237,-45.5780656427163,
12.));
#138706=CARTESIAN_POINT('Ctrl Pts',(-57.6395698104404,-45.5710441487674,
0.));
#138707=CARTESIAN_POINT('Ctrl Pts',(-57.6395698104404,-45.5710441487674,
12.));
#138708=CARTESIAN_POINT('Ctrl Pts',(-57.614026233004,-45.5640088427813,
0.));
#138709=CARTESIAN_POINT('Ctrl Pts',(-57.614026233004,-45.5640088427813,
12.));
#138710=CARTESIAN_POINT('Ctrl Pts',(-57.5885250155433,-45.5569597975096,
0.));
#138711=CARTESIAN_POINT('Ctrl Pts',(-57.5885250155433,-45.5569597975096,
12.));
#138712=CARTESIAN_POINT('Ctrl Pts',(-57.563066235668,-45.5498970859834,
0.));
#138713=CARTESIAN_POINT('Ctrl Pts',(-57.563066235668,-45.5498970859834,
12.));
#138714=CARTESIAN_POINT('Ctrl Pts',(-57.537649971135,-45.542820781484,0.));
#138715=CARTESIAN_POINT('Ctrl Pts',(-57.537649971135,-45.542820781484,12.));
#138716=CARTESIAN_POINT('Ctrl Pts',(-57.5122762998745,-45.5357309575611,
0.));
#138717=CARTESIAN_POINT('Ctrl Pts',(-57.5122762998745,-45.5357309575611,
12.));
#138718=CARTESIAN_POINT('Ctrl Pts',(-57.4869453000063,-45.5286276880484,
0.));
#138719=CARTESIAN_POINT('Ctrl Pts',(-57.4869453000063,-45.5286276880484,
12.));
#138720=CARTESIAN_POINT('Ctrl Pts',(-57.4616570498568,-45.5215110470825,
0.));
#138721=CARTESIAN_POINT('Ctrl Pts',(-57.4616570498568,-45.5215110470825,
12.));
#138722=CARTESIAN_POINT('Ctrl Pts',(-57.4364116279702,-45.5143811091205,
0.));
#138723=CARTESIAN_POINT('Ctrl Pts',(-57.4364116279702,-45.5143811091205,
12.));
#138724=CARTESIAN_POINT('Ctrl Pts',(-57.4112091131183,-45.5072379489631,
0.));
#138725=CARTESIAN_POINT('Ctrl Pts',(-57.4112091131183,-45.5072379489631,
12.));
#138726=CARTESIAN_POINT('Ctrl Pts',(-57.3860495843033,-45.5000816417509,
0.));
#138727=CARTESIAN_POINT('Ctrl Pts',(-57.3860495843033,-45.5000816417509,
12.));
#138728=CARTESIAN_POINT('Ctrl Pts',(-57.3609331207574,-45.4929122629572,
0.));
#138729=CARTESIAN_POINT('Ctrl Pts',(-57.3609331207574,-45.4929122629572,
12.));
#138730=CARTESIAN_POINT('Ctrl Pts',(-57.3358598019389,-45.4857298883824,
0.));
#138731=CARTESIAN_POINT('Ctrl Pts',(-57.3358598019389,-45.4857298883824,
12.));
#138732=CARTESIAN_POINT('Ctrl Pts',(-57.3108297075265,-45.4785345941507,
0.));
#138733=CARTESIAN_POINT('Ctrl Pts',(-57.3108297075265,-45.4785345941507,
12.));
#138734=CARTESIAN_POINT('Ctrl Pts',(-57.2858429174062,-45.4713264567063,
0.));
#138735=CARTESIAN_POINT('Ctrl Pts',(-57.2858429174062,-45.4713264567063,
12.));
#138736=CARTESIAN_POINT('Ctrl Pts',(-57.2608995116733,-45.4641055528141,
0.));
#138737=CARTESIAN_POINT('Ctrl Pts',(-57.2608995116733,-45.4641055528141,
12.));
#138738=CARTESIAN_POINT('Ctrl Pts',(-57.2359995706447,-45.4568719595641,
0.));
#138739=CARTESIAN_POINT('Ctrl Pts',(-57.2359995706447,-45.4568719595641,
12.));
#138740=CARTESIAN_POINT('Ctrl Pts',(-57.2111431748631,-45.4496257543759,
0.));
#138741=CARTESIAN_POINT('Ctrl Pts',(-57.2111431748631,-45.4496257543759,
12.));
#138742=CARTESIAN_POINT('Ctrl Pts',(-57.186330405101,-45.4423670150034,
0.));
#138743=CARTESIAN_POINT('Ctrl Pts',(-57.186330405101,-45.4423670150034,
12.));
#138744=CARTESIAN_POINT('Ctrl Pts',(-57.1615613423584,-45.4350958195433,
0.));
#138745=CARTESIAN_POINT('Ctrl Pts',(-57.1615613423584,-45.4350958195433,
12.));
#138746=CARTESIAN_POINT('Ctrl Pts',(-57.136836067863,-45.4278122464389,
0.));
#138747=CARTESIAN_POINT('Ctrl Pts',(-57.136836067863,-45.4278122464389,
12.));
#138748=CARTESIAN_POINT('Ctrl Pts',(-57.112154663078,-45.4205163744781,
0.));
#138749=CARTESIAN_POINT('Ctrl Pts',(-57.112154663078,-45.4205163744781,
12.));
#138750=CARTESIAN_POINT('Ctrl Pts',(-57.0875172097051,-45.4132082827948,
0.));
#138751=CARTESIAN_POINT('Ctrl Pts',(-57.0875172097051,-45.4132082827948,
12.));
#138752=CARTESIAN_POINT('Ctrl Pts',(-57.0629237896848,-45.4058880508693,
0.));
#138753=CARTESIAN_POINT('Ctrl Pts',(-57.0629237896848,-45.4058880508693,
12.));
#138754=CARTESIAN_POINT('Ctrl Pts',(-57.0383744851913,-45.3985557585311,
0.));
#138755=CARTESIAN_POINT('Ctrl Pts',(-57.0383744851913,-45.3985557585311,
12.));
#138756=CARTESIAN_POINT('Ctrl Pts',(-57.0138693786278,-45.3912114859616,
0.));
#138757=CARTESIAN_POINT('Ctrl Pts',(-57.0138693786278,-45.3912114859616,
12.));
#138758=CARTESIAN_POINT('Ctrl Pts',(-56.9894085526373,-45.3838553136948,
0.));
#138759=CARTESIAN_POINT('Ctrl Pts',(-56.9894085526373,-45.3838553136948,
12.));
#138760=CARTESIAN_POINT('Ctrl Pts',(-56.9649920901073,-45.3764873226196,
0.));
#138761=CARTESIAN_POINT('Ctrl Pts',(-56.9649920901073,-45.3764873226196,
12.));
#138762=CARTESIAN_POINT('Ctrl Pts',(-56.9406200741714,-45.3691075939826,
0.));
#138763=CARTESIAN_POINT('Ctrl Pts',(-56.9406200741714,-45.3691075939826,
12.));
#138764=CARTESIAN_POINT('Ctrl Pts',(-56.9162925882085,-45.3617162093922,
0.));
#138765=CARTESIAN_POINT('Ctrl Pts',(-56.9162925882085,-45.3617162093922,
12.));
#138766=CARTESIAN_POINT('Ctrl Pts',(-56.8920097158377,-45.3543132508238,
0.));
#138767=CARTESIAN_POINT('Ctrl Pts',(-56.8920097158377,-45.3543132508238,
12.));
#138768=CARTESIAN_POINT('Ctrl Pts',(-56.8677715409268,-45.3468988006203,
0.));
#138769=CARTESIAN_POINT('Ctrl Pts',(-56.8677715409268,-45.3468988006203,
12.));
#138770=CARTESIAN_POINT('Ctrl Pts',(-56.8435781475981,-45.3394729414931,
0.));
#138771=CARTESIAN_POINT('Ctrl Pts',(-56.8435781475981,-45.3394729414931,
12.));
#138772=CARTESIAN_POINT('Ctrl Pts',(-56.8194296202291,-45.332035756524,
0.));
#138773=CARTESIAN_POINT('Ctrl Pts',(-56.8194296202291,-45.332035756524,
12.));
#138774=CARTESIAN_POINT('Ctrl Pts',(-56.7953260434524,-45.3245873291684,
0.));
#138775=CARTESIAN_POINT('Ctrl Pts',(-56.7953260434524,-45.3245873291684,
12.));
#138776=CARTESIAN_POINT('Ctrl Pts',(-56.7712675021491,-45.31712774326,0.));
#138777=CARTESIAN_POINT('Ctrl Pts',(-56.7712675021491,-45.31712774326,12.));
#138778=CARTESIAN_POINT('Ctrl Pts',(-56.7472540814554,-45.3096570830117,
0.));
#138779=CARTESIAN_POINT('Ctrl Pts',(-56.7472540814554,-45.3096570830117,
12.));
#138780=CARTESIAN_POINT('Ctrl Pts',(-56.7232858667709,-45.3021754330178,
0.));
#138781=CARTESIAN_POINT('Ctrl Pts',(-56.7232858667709,-45.3021754330178,
12.));
#138782=CARTESIAN_POINT('Ctrl Pts',(-56.69936294376,-45.2946828782559,0.));
#138783=CARTESIAN_POINT('Ctrl Pts',(-56.69936294376,-45.2946828782559,12.));
#138784=CARTESIAN_POINT('Ctrl Pts',(-56.6754853983528,-45.2871795040906,
0.));
#138785=CARTESIAN_POINT('Ctrl Pts',(-56.6754853983528,-45.2871795040906,
12.));
#138786=CARTESIAN_POINT('Ctrl Pts',(-56.6516533167384,-45.2796653962785,
0.));
#138787=CARTESIAN_POINT('Ctrl Pts',(-56.6516533167384,-45.2796653962785,
12.));
#138788=CARTESIAN_POINT('Ctrl Pts',(-56.6278667853702,-45.2721406409695,
0.));
#138789=CARTESIAN_POINT('Ctrl Pts',(-56.6278667853702,-45.2721406409695,
12.));
#138790=CARTESIAN_POINT('Ctrl Pts',(-56.6041258909741,-45.2646053247087,
0.));
#138791=CARTESIAN_POINT('Ctrl Pts',(-56.6041258909741,-45.2646053247087,
12.));
#138792=CARTESIAN_POINT('Ctrl Pts',(-56.5804307205505,-45.257059534438,
0.));
#138793=CARTESIAN_POINT('Ctrl Pts',(-56.5804307205505,-45.257059534438,
12.));
#138794=CARTESIAN_POINT('Ctrl Pts',(-56.5567813613756,-45.2495033575,0.));
#138795=CARTESIAN_POINT('Ctrl Pts',(-56.5567813613756,-45.2495033575,12.));
#138796=CARTESIAN_POINT('Ctrl Pts',(-56.5331779009958,-45.2419368816428,
0.));
#138797=CARTESIAN_POINT('Ctrl Pts',(-56.5331779009958,-45.2419368816428,
12.));
#138798=CARTESIAN_POINT('Ctrl Pts',(-56.5096204272306,-45.2343601950227,
0.));
#138799=CARTESIAN_POINT('Ctrl Pts',(-56.5096204272306,-45.2343601950227,
12.));
#138800=CARTESIAN_POINT('Ctrl Pts',(-56.4861090281823,-45.2267733862049,
0.));
#138801=CARTESIAN_POINT('Ctrl Pts',(-56.4861090281823,-45.2267733862049,
12.));
#138802=CARTESIAN_POINT('Ctrl Pts',(-56.4626437922386,-45.2191765441666,
0.));
#138803=CARTESIAN_POINT('Ctrl Pts',(-56.4626437922386,-45.2191765441666,
12.));
#138804=CARTESIAN_POINT('Ctrl Pts',(-56.4392248080732,-45.2115697583,0.));
#138805=CARTESIAN_POINT('Ctrl Pts',(-56.4392248080732,-45.2115697583,12.));
#138806=CARTESIAN_POINT('Ctrl Pts',(-56.4158521646411,-45.2039531184171,
0.));
#138807=CARTESIAN_POINT('Ctrl Pts',(-56.4158521646411,-45.2039531184171,
12.));
#138808=CARTESIAN_POINT('Ctrl Pts',(-56.3925259511806,-45.1963267147529,
0.));
#138809=CARTESIAN_POINT('Ctrl Pts',(-56.3925259511806,-45.1963267147529,
12.));
#138810=CARTESIAN_POINT('Ctrl Pts',(-56.3692462572231,-45.1886906379667,
0.));
#138811=CARTESIAN_POINT('Ctrl Pts',(-56.3692462572231,-45.1886906379667,
12.));
#138812=CARTESIAN_POINT('Ctrl Pts',(-56.3460131725964,-45.1810449791453,
0.));
#138813=CARTESIAN_POINT('Ctrl Pts',(-56.3460131725964,-45.1810449791453,
12.));
#138814=CARTESIAN_POINT('Ctrl Pts',(-56.3228267874264,-45.173389829806,
0.));
#138815=CARTESIAN_POINT('Ctrl Pts',(-56.3228267874264,-45.173389829806,
12.));
#138816=CARTESIAN_POINT('Ctrl Pts',(-56.2996871921316,-45.1657252819013,
0.));
#138817=CARTESIAN_POINT('Ctrl Pts',(-56.2996871921316,-45.1657252819013,
12.));
#138818=CARTESIAN_POINT('Ctrl Pts',(-56.2765944774245,-45.1580514278223,
0.));
#138819=CARTESIAN_POINT('Ctrl Pts',(-56.2765944774245,-45.1580514278223,
12.));
#138820=CARTESIAN_POINT('Ctrl Pts',(-56.2535487343221,-45.1503683604005,
0.));
#138821=CARTESIAN_POINT('Ctrl Pts',(-56.2535487343221,-45.1503683604005,
12.));
#138822=CARTESIAN_POINT('Ctrl Pts',(-56.230550054149,-45.1426761729105,
0.));
#138823=CARTESIAN_POINT('Ctrl Pts',(-56.230550054149,-45.1426761729105,
12.));
#138824=CARTESIAN_POINT('Ctrl Pts',(-56.2075985285393,-45.1349749590737,
0.));
#138825=CARTESIAN_POINT('Ctrl Pts',(-56.2075985285393,-45.1349749590737,
12.));
#138826=CARTESIAN_POINT('Ctrl Pts',(-56.1846942494325,-45.127264813063,
0.));
#138827=CARTESIAN_POINT('Ctrl Pts',(-56.1846942494325,-45.127264813063,
12.));
#138828=CARTESIAN_POINT('Ctrl Pts',(-56.1618373090732,-45.1195458295062,
0.));
#138829=CARTESIAN_POINT('Ctrl Pts',(-56.1618373090732,-45.1195458295062,
12.));
#138830=CARTESIAN_POINT('Ctrl Pts',(-56.1390278000226,-45.1118181034888,
0.));
#138831=CARTESIAN_POINT('Ctrl Pts',(-56.1390278000226,-45.1118181034888,
12.));
#138832=CARTESIAN_POINT('Ctrl Pts',(-56.116265815162,-45.1040817305561,
0.));
#138833=CARTESIAN_POINT('Ctrl Pts',(-56.116265815162,-45.1040817305561,
12.));
#138834=CARTESIAN_POINT('Ctrl Pts',(-56.0935514476945,-45.0963368067177,
0.));
#138835=CARTESIAN_POINT('Ctrl Pts',(-56.0935514476945,-45.0963368067177,
12.));
#138836=CARTESIAN_POINT('Ctrl Pts',(-56.0708847911416,-45.0885834284517,
0.));
#138837=CARTESIAN_POINT('Ctrl Pts',(-56.0708847911416,-45.0885834284517,
12.));
#138838=CARTESIAN_POINT('Ctrl Pts',(-56.048265939342,-45.0808216927089,
0.));
#138839=CARTESIAN_POINT('Ctrl Pts',(-56.048265939342,-45.0808216927089,
12.));
#138840=CARTESIAN_POINT('Ctrl Pts',(-56.0256949864639,-45.0730516969148,
0.));
#138841=CARTESIAN_POINT('Ctrl Pts',(-56.0256949864639,-45.0730516969148,
12.));
#138842=CARTESIAN_POINT('Ctrl Pts',(-56.003172027008,-45.0652735389733,
0.));
#138843=CARTESIAN_POINT('Ctrl Pts',(-56.003172027008,-45.0652735389733,
12.));
#138844=CARTESIAN_POINT('Ctrl Pts',(-55.9806971558097,-45.0574873172694,
0.));
#138845=CARTESIAN_POINT('Ctrl Pts',(-55.9806971558097,-45.0574873172694,
12.));
#138846=CARTESIAN_POINT('Ctrl Pts',(-55.9582704680356,-45.0496931306755,
0.));
#138847=CARTESIAN_POINT('Ctrl Pts',(-55.9582704680356,-45.0496931306755,
12.));
#138848=CARTESIAN_POINT('Ctrl Pts',(-55.9358920591837,-45.041891078555,
0.));
#138849=CARTESIAN_POINT('Ctrl Pts',(-55.9358920591837,-45.041891078555,
12.));
#138850=CARTESIAN_POINT('Ctrl Pts',(-55.9135620250954,-45.0340812607657,
0.));
#138851=CARTESIAN_POINT('Ctrl Pts',(-55.9135620250954,-45.0340812607657,
12.));
#138852=CARTESIAN_POINT('Ctrl Pts',(-55.8912804619577,-45.0262637776614,
0.));
#138853=CARTESIAN_POINT('Ctrl Pts',(-55.8912804619577,-45.0262637776614,
12.));
#138854=CARTESIAN_POINT('Ctrl Pts',(-55.8690474663065,-45.0184387300973,
0.));
#138855=CARTESIAN_POINT('Ctrl Pts',(-55.8690474663065,-45.0184387300973,
12.));
#138856=CARTESIAN_POINT('Ctrl Pts',(-55.8468631350218,-45.0106062194342,
0.));
#138857=CARTESIAN_POINT('Ctrl Pts',(-55.8468631350218,-45.0106062194342,
12.));
#138858=CARTESIAN_POINT('Ctrl Pts',(-55.8247275653289,-45.0027663475433,
0.));
#138859=CARTESIAN_POINT('Ctrl Pts',(-55.8247275653289,-45.0027663475433,
12.));
#138860=CARTESIAN_POINT('Ctrl Pts',(-55.8026408548105,-44.9949192168093,
0.));
#138861=CARTESIAN_POINT('Ctrl Pts',(-55.8026408548105,-44.9949192168093,
12.));
#138862=CARTESIAN_POINT('Ctrl Pts',(-55.7806031014106,-44.9870649301342,
0.));
#138863=CARTESIAN_POINT('Ctrl Pts',(-55.7806031014106,-44.9870649301342,
12.));
#138864=CARTESIAN_POINT('Ctrl Pts',(-55.7586144034367,-44.9792035909413,
0.));
#138865=CARTESIAN_POINT('Ctrl Pts',(-55.7586144034367,-44.9792035909413,
12.));
#138866=CARTESIAN_POINT('Ctrl Pts',(-55.7366748595552,-44.9713353031804,
0.));
#138867=CARTESIAN_POINT('Ctrl Pts',(-55.7366748595552,-44.9713353031804,
12.));
#138868=CARTESIAN_POINT('Ctrl Pts',(-55.714784568793,-44.9634601713321,
0.));
#138869=CARTESIAN_POINT('Ctrl Pts',(-55.714784568793,-44.9634601713321,
12.));
#138870=CARTESIAN_POINT('Ctrl Pts',(-55.6929436305489,-44.9555783004106,
0.));
#138871=CARTESIAN_POINT('Ctrl Pts',(-55.6929436305489,-44.9555783004106,
12.));
#138872=CARTESIAN_POINT('Ctrl Pts',(-55.6711521445979,-44.9476897959684,
0.));
#138873=CARTESIAN_POINT('Ctrl Pts',(-55.6711521445979,-44.9476897959684,
12.));
#138874=CARTESIAN_POINT('Ctrl Pts',(-55.6494102110935,-44.9397947641006,
0.));
#138875=CARTESIAN_POINT('Ctrl Pts',(-55.6494102110935,-44.9397947641006,
12.));
#138876=CARTESIAN_POINT('Ctrl Pts',(-55.6277179305633,-44.9318933114506,
0.));
#138877=CARTESIAN_POINT('Ctrl Pts',(-55.6277179305633,-44.9318933114506,
12.));
#138878=CARTESIAN_POINT('Ctrl Pts',(-55.6060754039121,-44.9239855452144,
0.));
#138879=CARTESIAN_POINT('Ctrl Pts',(-55.6060754039121,-44.9239855452144,
12.));
#138880=CARTESIAN_POINT('Ctrl Pts',(-55.5844827324338,-44.9160715731443,
0.));
#138881=CARTESIAN_POINT('Ctrl Pts',(-55.5844827324338,-44.9160715731443,
12.));
#138882=CARTESIAN_POINT('Ctrl Pts',(-55.5629400178142,-44.908151503553,
0.));
#138883=CARTESIAN_POINT('Ctrl Pts',(-55.5629400178142,-44.908151503553,
12.));
#138884=CARTESIAN_POINT('Ctrl Pts',(-55.541447362134,-44.9002254453183,
0.));
#138885=CARTESIAN_POINT('Ctrl Pts',(-55.541447362134,-44.9002254453183,
12.));
#138886=CARTESIAN_POINT('Ctrl Pts',(-55.5200048678629,-44.8922935078889,
0.));
#138887=CARTESIAN_POINT('Ctrl Pts',(-55.5200048678629,-44.8922935078889,
12.));
#138888=CARTESIAN_POINT('Ctrl Pts',(-55.4986126378656,-44.8843558012886,
0.));
#138889=CARTESIAN_POINT('Ctrl Pts',(-55.4986126378656,-44.8843558012886,
12.));
#138890=CARTESIAN_POINT('Ctrl Pts',(-55.4772707754126,-44.8764124361206,
0.));
#138891=CARTESIAN_POINT('Ctrl Pts',(-55.4772707754126,-44.8764124361206,
12.));
#138892=CARTESIAN_POINT('Ctrl Pts',(-55.4559793841836,-44.8684635235725,
0.));
#138893=CARTESIAN_POINT('Ctrl Pts',(-55.4559793841836,-44.8684635235725,
12.));
#138894=CARTESIAN_POINT('Ctrl Pts',(-55.4347385682704,-44.8605091754214,
0.));
#138895=CARTESIAN_POINT('Ctrl Pts',(-55.4347385682704,-44.8605091754214,
12.));
#138896=CARTESIAN_POINT('Ctrl Pts',(-55.4135484321718,-44.8525495040408,
0.));
#138897=CARTESIAN_POINT('Ctrl Pts',(-55.4135484321718,-44.8525495040408,
12.));
#138898=CARTESIAN_POINT('Ctrl Pts',(-55.3924090808014,-44.8445846224044,
0.));
#138899=CARTESIAN_POINT('Ctrl Pts',(-55.3924090808014,-44.8445846224044,
12.));
#138900=CARTESIAN_POINT('Ctrl Pts',(-55.3713206194967,-44.8366146440901,
0.));
#138901=CARTESIAN_POINT('Ctrl Pts',(-55.3713206194967,-44.8366146440901,
12.));
#138902=CARTESIAN_POINT('Ctrl Pts',(-55.3502831540228,-44.8286396832847,
0.));
#138903=CARTESIAN_POINT('Ctrl Pts',(-55.3502831540228,-44.8286396832847,
12.));
#138904=CARTESIAN_POINT('Ctrl Pts',(-55.3292967905725,-44.8206598547887,
0.));
#138905=CARTESIAN_POINT('Ctrl Pts',(-55.3292967905725,-44.8206598547887,
12.));
#138906=CARTESIAN_POINT('Ctrl Pts',(-55.3083616357605,-44.8126752740208,
0.));
#138907=CARTESIAN_POINT('Ctrl Pts',(-55.3083616357605,-44.8126752740208,
12.));
#138908=CARTESIAN_POINT('Ctrl Pts',(-55.287477796635,-44.8046860570244,
0.));
#138909=CARTESIAN_POINT('Ctrl Pts',(-55.287477796635,-44.8046860570244,
12.));
#138910=CARTESIAN_POINT('Ctrl Pts',(-55.2666453806883,-44.796692320474,
0.));
#138911=CARTESIAN_POINT('Ctrl Pts',(-55.2666453806883,-44.796692320474,
12.));
#138912=CARTESIAN_POINT('Ctrl Pts',(-55.2458644958617,-44.7886941816823,
0.));
#138913=CARTESIAN_POINT('Ctrl Pts',(-55.2458644958617,-44.7886941816823,
12.));
#138914=CARTESIAN_POINT('Ctrl Pts',(-55.2251352505474,-44.7806917586077,
0.));
#138915=CARTESIAN_POINT('Ctrl Pts',(-55.2251352505474,-44.7806917586077,
12.));
#138916=CARTESIAN_POINT('Ctrl Pts',(-55.2044577535865,-44.7726851698618,
0.));
#138917=CARTESIAN_POINT('Ctrl Pts',(-55.2044577535865,-44.7726851698618,
12.));
#138918=CARTESIAN_POINT('Ctrl Pts',(-55.1838321142777,-44.7646745347108,
0.));
#138919=CARTESIAN_POINT('Ctrl Pts',(-55.1838321142777,-44.7646745347108,
12.));
#138920=CARTESIAN_POINT('Ctrl Pts',(-55.1632584423813,-44.7566599730771,
0.));
#138921=CARTESIAN_POINT('Ctrl Pts',(-55.1632584423813,-44.7566599730771,
12.));
#138922=CARTESIAN_POINT('Ctrl Pts',(-55.1427368481201,-44.7486416055419,
0.));
#138923=CARTESIAN_POINT('Ctrl Pts',(-55.1427368481201,-44.7486416055419,
12.));
#138924=CARTESIAN_POINT('Ctrl Pts',(-55.1222674421747,-44.7406195533482,
0.));
#138925=CARTESIAN_POINT('Ctrl Pts',(-55.1222674421747,-44.7406195533482,
12.));
#138926=CARTESIAN_POINT('Ctrl Pts',(-55.1018503356806,-44.7325939384042,
0.));
#138927=CARTESIAN_POINT('Ctrl Pts',(-55.1018503356806,-44.7325939384042,
12.));
#138928=CARTESIAN_POINT('Ctrl Pts',(-55.0814856402507,-44.7245648832988,
0.));
#138929=CARTESIAN_POINT('Ctrl Pts',(-55.0814856402507,-44.7245648832988,
12.));
#138930=CARTESIAN_POINT('Ctrl Pts',(-55.0611734679902,-44.7165325113165,
0.));
#138931=CARTESIAN_POINT('Ctrl Pts',(-55.0611734679902,-44.7165325113165,
12.));
#138932=CARTESIAN_POINT('Ctrl Pts',(-55.0409139315074,-44.7084969464509,
0.));
#138933=CARTESIAN_POINT('Ctrl Pts',(-55.0409139315074,-44.7084969464509,
12.));
#138934=CARTESIAN_POINT('Ctrl Pts',(-55.020707143922,-44.7004583134235,
0.));
#138935=CARTESIAN_POINT('Ctrl Pts',(-55.020707143922,-44.7004583134235,
12.));
#138936=CARTESIAN_POINT('Ctrl Pts',(-55.0005532188644,-44.6924167376851,
0.));
#138937=CARTESIAN_POINT('Ctrl Pts',(-55.0005532188644,-44.6924167376851,
12.));
#138938=CARTESIAN_POINT('Ctrl Pts',(-54.9804522704668,-44.6843723453985,
0.));
#138939=CARTESIAN_POINT('Ctrl Pts',(-54.9804522704668,-44.6843723453985,
12.));
#138940=CARTESIAN_POINT('Ctrl Pts',(-54.9604044133497,-44.6763252634255,
0.));
#138941=CARTESIAN_POINT('Ctrl Pts',(-54.9604044133497,-44.6763252634255,
12.));
#138942=CARTESIAN_POINT('Ctrl Pts',(-54.9404097626088,-44.6682756193155,
0.));
#138943=CARTESIAN_POINT('Ctrl Pts',(-54.9404097626088,-44.6682756193155,
12.));
#138944=CARTESIAN_POINT('Ctrl Pts',(-54.9204684337845,-44.6602235412853,
0.));
#138945=CARTESIAN_POINT('Ctrl Pts',(-54.9204684337845,-44.6602235412853,
12.));
#138946=CARTESIAN_POINT('Ctrl Pts',(-54.9005805428991,-44.6521691582551,
0.));
#138947=CARTESIAN_POINT('Ctrl Pts',(-54.9005805428991,-44.6521691582551,
12.));
#138948=CARTESIAN_POINT('Ctrl Pts',(-54.8807462065177,-44.6441125999074,
0.));
#138949=CARTESIAN_POINT('Ctrl Pts',(-54.8807462065177,-44.6441125999074,
12.));
#138950=CARTESIAN_POINT('Ctrl Pts',(-54.860965541796,-44.6360539967392,
0.));
#138951=CARTESIAN_POINT('Ctrl Pts',(-54.860965541796,-44.6360539967392,
12.));
#138952=CARTESIAN_POINT('Ctrl Pts',(-54.8412386665264,-44.6279934801159,
0.));
#138953=CARTESIAN_POINT('Ctrl Pts',(-54.8412386665264,-44.6279934801159,
12.));
#138954=CARTESIAN_POINT('Ctrl Pts',(-54.8215656991817,-44.6199311823276,
0.));
#138955=CARTESIAN_POINT('Ctrl Pts',(-54.8215656991817,-44.6199311823276,
12.));
#138956=CARTESIAN_POINT('Ctrl Pts',(-54.8019467588258,-44.6118672364889,
0.));
#138957=CARTESIAN_POINT('Ctrl Pts',(-54.8019467588258,-44.6118672364889,
12.));
#138958=CARTESIAN_POINT('Ctrl Pts',(-54.7823819650137,-44.60380177643,0.));
#138959=CARTESIAN_POINT('Ctrl Pts',(-54.7823819650137,-44.60380177643,12.));
#138960=CARTESIAN_POINT('Ctrl Pts',(-54.7628714377042,-44.5957349366062,
0.));
#138961=CARTESIAN_POINT('Ctrl Pts',(-54.7628714377042,-44.5957349366062,
12.));
#138962=CARTESIAN_POINT('Ctrl Pts',(-54.7434152971285,-44.5876668519676,
0.));
#138963=CARTESIAN_POINT('Ctrl Pts',(-54.7434152971285,-44.5876668519676,
12.));
#138964=CARTESIAN_POINT('Ctrl Pts',(-54.7240136637744,-44.5795976579476,
0.));
#138965=CARTESIAN_POINT('Ctrl Pts',(-54.7240136637744,-44.5795976579476,
12.));
#138966=CARTESIAN_POINT('Ctrl Pts',(-54.7046666586777,-44.5715274907637,
0.));
#138967=CARTESIAN_POINT('Ctrl Pts',(-54.7046666586777,-44.5715274907637,
12.));
#138968=CARTESIAN_POINT('Ctrl Pts',(-54.685374403676,-44.5634564876869,
0.));
#138969=CARTESIAN_POINT('Ctrl Pts',(-54.685374403676,-44.5634564876869,
12.));
#138970=CARTESIAN_POINT('Ctrl Pts',(-54.6661370216242,-44.5553847872712,
0.));
#138971=CARTESIAN_POINT('Ctrl Pts',(-54.6661370216242,-44.5553847872712,
12.));
#138972=CARTESIAN_POINT('Ctrl Pts',(-54.6469546367381,-44.5473125297289,
0.));
#138973=CARTESIAN_POINT('Ctrl Pts',(-54.6469546367381,-44.5473125297289,
12.));
#138974=CARTESIAN_POINT('Ctrl Pts',(-54.6278273743554,-44.5392398566775,
0.));
#138975=CARTESIAN_POINT('Ctrl Pts',(-54.6278273743554,-44.5392398566775,
12.));
#138976=CARTESIAN_POINT('Ctrl Pts',(-54.6087553602889,-44.5311669104494,
0.));
#138977=CARTESIAN_POINT('Ctrl Pts',(-54.6087553602889,-44.5311669104494,
12.));
#138978=CARTESIAN_POINT('Ctrl Pts',(-54.5897387202812,-44.5230938335165,
0.));
#138979=CARTESIAN_POINT('Ctrl Pts',(-54.5897387202812,-44.5230938335165,
12.));
#138980=CARTESIAN_POINT('Ctrl Pts',(-54.5707775794436,-44.5150207679007,
0.));
#138981=CARTESIAN_POINT('Ctrl Pts',(-54.5707775794436,-44.5150207679007,
12.));
#138982=CARTESIAN_POINT('Ctrl Pts',(-54.5518720616056,-44.5069478544977,
0.));
#138983=CARTESIAN_POINT('Ctrl Pts',(-54.5518720616056,-44.5069478544977,
12.));
#138984=CARTESIAN_POINT('Ctrl Pts',(-54.5330222905475,-44.4988752343744,
0.));
#138985=CARTESIAN_POINT('Ctrl Pts',(-54.5330222905475,-44.4988752343744,
12.));
#138986=CARTESIAN_POINT('Ctrl Pts',(-54.5142283914704,-44.4908030503225,
0.));
#138987=CARTESIAN_POINT('Ctrl Pts',(-54.5142283914704,-44.4908030503225,
12.));
#138988=CARTESIAN_POINT('Ctrl Pts',(-54.495490492193,-44.4827314481264,
0.));
#138989=CARTESIAN_POINT('Ctrl Pts',(-54.495490492193,-44.4827314481264,
12.));
#138990=CARTESIAN_POINT('Ctrl Pts',(-54.4768087248824,-44.4746605784031,
0.));
#138991=CARTESIAN_POINT('Ctrl Pts',(-54.4768087248824,-44.4746605784031,
12.));
#138992=CARTESIAN_POINT('Ctrl Pts',(-54.4581832262033,-44.4665905967668,
0.));
#138993=CARTESIAN_POINT('Ctrl Pts',(-54.4581832262033,-44.4665905967668,
12.));
#138994=CARTESIAN_POINT('Ctrl Pts',(-54.4396141336978,-44.4585216599907,
0.));
#138995=CARTESIAN_POINT('Ctrl Pts',(-54.4396141336978,-44.4585216599907,
12.));
#138996=CARTESIAN_POINT('Ctrl Pts',(-54.421101582595,-44.4504539226327,
0.));
#138997=CARTESIAN_POINT('Ctrl Pts',(-54.421101582595,-44.4504539226327,
12.));
#138998=CARTESIAN_POINT('Ctrl Pts',(-54.4026457030335,-44.4423875340995,
0.));
#138999=CARTESIAN_POINT('Ctrl Pts',(-54.4026457030335,-44.4423875340995,
12.));
#139000=CARTESIAN_POINT('Ctrl Pts',(-54.3842466156196,-44.4343226339592,
0.));
#139001=CARTESIAN_POINT('Ctrl Pts',(-54.3842466156196,-44.4343226339592,
12.));
#139002=CARTESIAN_POINT('Ctrl Pts',(-54.3659044357119,-44.4262593564712,
0.));
#139003=CARTESIAN_POINT('Ctrl Pts',(-54.3659044357119,-44.4262593564712,
12.));
#139004=CARTESIAN_POINT('Ctrl Pts',(-54.3476192819352,-44.4181978395851,
0.));
#139005=CARTESIAN_POINT('Ctrl Pts',(-54.3476192819352,-44.4181978395851,
12.));
#139006=CARTESIAN_POINT('Ctrl Pts',(-54.3293912830237,-44.4101382321834,
0.));
#139007=CARTESIAN_POINT('Ctrl Pts',(-54.3293912830237,-44.4101382321834,
12.));
#139008=CARTESIAN_POINT('Ctrl Pts',(-54.3112205860716,-44.402080702809,
0.));
#139009=CARTESIAN_POINT('Ctrl Pts',(-54.3112205860716,-44.402080702809,
12.));
#139010=CARTESIAN_POINT('Ctrl Pts',(-54.2931073621553,-44.3940254456331,
0.));
#139011=CARTESIAN_POINT('Ctrl Pts',(-54.2931073621553,-44.3940254456331,
12.));
#139012=CARTESIAN_POINT('Ctrl Pts',(-54.2750517888579,-44.3859726620183,
0.));
#139013=CARTESIAN_POINT('Ctrl Pts',(-54.2750517888579,-44.3859726620183,
12.));
#139014=CARTESIAN_POINT('Ctrl Pts',(-54.2570540336475,-44.3779225430405,
0.));
#139015=CARTESIAN_POINT('Ctrl Pts',(-54.2570540336475,-44.3779225430405,
12.));
#139016=CARTESIAN_POINT('Ctrl Pts',(-54.2391142386412,-44.3698752533561,
0.));
#139017=CARTESIAN_POINT('Ctrl Pts',(-54.2391142386412,-44.3698752533561,
12.));
#139018=CARTESIAN_POINT('Ctrl Pts',(-54.2212325006052,-44.361830910343,
0.));
#139019=CARTESIAN_POINT('Ctrl Pts',(-54.2212325006052,-44.361830910343,
12.));
#139020=CARTESIAN_POINT('Ctrl Pts',(-54.2034088701928,-44.3537895824096,
0.));
#139021=CARTESIAN_POINT('Ctrl Pts',(-54.2034088701928,-44.3537895824096,
12.));
#139022=CARTESIAN_POINT('Ctrl Pts',(-54.1891964684727,-44.3473589597726,
0.));
#139023=CARTESIAN_POINT('Ctrl Pts',(-54.1891964684727,-44.3473589597726,
12.));
#139024=CARTESIAN_POINT('Ctrl Pts',(-54.1785633257639,-44.3425373700993,
0.));
#139025=CARTESIAN_POINT('Ctrl Pts',(-54.1785633257639,-44.3425373700993,
12.));
#139026=CARTESIAN_POINT('Ctrl Pts',(-54.1714861895346,-44.3393235891075,
0.));
#139027=CARTESIAN_POINT('Ctrl Pts',(-54.1714861895346,-44.3393235891075,
12.));
#139028=CARTESIAN_POINT('Ctrl Pts',(-54.1679505278134,-44.3377168516418,
0.));
#139029=CARTESIAN_POINT('Ctrl Pts',(-54.1679505278134,-44.3377168516418,
12.));
#139030=CARTESIAN_POINT('',(-54.1679505278134,-44.3377168516418,12.));
#139031=CARTESIAN_POINT('Ctrl Pts',(-54.1679505278134,-44.3377168516418,
12.));
#139032=CARTESIAN_POINT('Ctrl Pts',(-54.1714861895346,-44.3393235891075,
12.));
#139033=CARTESIAN_POINT('Ctrl Pts',(-54.1785633257639,-44.3425373700993,
12.));
#139034=CARTESIAN_POINT('Ctrl Pts',(-54.1891964684727,-44.3473589597726,
12.));
#139035=CARTESIAN_POINT('Ctrl Pts',(-54.2034088701928,-44.3537895824096,
12.));
#139036=CARTESIAN_POINT('Ctrl Pts',(-54.2212325006052,-44.361830910343,
12.));
#139037=CARTESIAN_POINT('Ctrl Pts',(-54.2391142386412,-44.3698752533561,
12.));
#139038=CARTESIAN_POINT('Ctrl Pts',(-54.2570540336475,-44.3779225430405,
12.));
#139039=CARTESIAN_POINT('Ctrl Pts',(-54.2750517888579,-44.3859726620183,
12.));
#139040=CARTESIAN_POINT('Ctrl Pts',(-54.2931073621553,-44.3940254456331,
12.));
#139041=CARTESIAN_POINT('Ctrl Pts',(-54.3112205860716,-44.402080702809,
12.));
#139042=CARTESIAN_POINT('Ctrl Pts',(-54.3293912830237,-44.4101382321834,
12.));
#139043=CARTESIAN_POINT('Ctrl Pts',(-54.3476192819352,-44.4181978395851,
12.));
#139044=CARTESIAN_POINT('Ctrl Pts',(-54.3659044357119,-44.4262593564712,
12.));
#139045=CARTESIAN_POINT('Ctrl Pts',(-54.3842466156196,-44.4343226339592,
12.));
#139046=CARTESIAN_POINT('Ctrl Pts',(-54.4026457030335,-44.4423875340995,
12.));
#139047=CARTESIAN_POINT('Ctrl Pts',(-54.421101582595,-44.4504539226327,
12.));
#139048=CARTESIAN_POINT('Ctrl Pts',(-54.4396141336978,-44.4585216599907,
12.));
#139049=CARTESIAN_POINT('Ctrl Pts',(-54.4581832262033,-44.4665905967668,
12.));
#139050=CARTESIAN_POINT('Ctrl Pts',(-54.4768087248824,-44.4746605784031,
12.));
#139051=CARTESIAN_POINT('Ctrl Pts',(-54.495490492193,-44.4827314481264,
12.));
#139052=CARTESIAN_POINT('Ctrl Pts',(-54.5142283914704,-44.4908030503225,
12.));
#139053=CARTESIAN_POINT('Ctrl Pts',(-54.5330222905475,-44.4988752343744,
12.));
#139054=CARTESIAN_POINT('Ctrl Pts',(-54.5518720616056,-44.5069478544977,
12.));
#139055=CARTESIAN_POINT('Ctrl Pts',(-54.5707775794436,-44.5150207679007,
12.));
#139056=CARTESIAN_POINT('Ctrl Pts',(-54.5897387202812,-44.5230938335165,
12.));
#139057=CARTESIAN_POINT('Ctrl Pts',(-54.6087553602889,-44.5311669104494,
12.));
#139058=CARTESIAN_POINT('Ctrl Pts',(-54.6278273743554,-44.5392398566775,
12.));
#139059=CARTESIAN_POINT('Ctrl Pts',(-54.6469546367381,-44.5473125297289,
12.));
#139060=CARTESIAN_POINT('Ctrl Pts',(-54.6661370216242,-44.5553847872712,
12.));
#139061=CARTESIAN_POINT('Ctrl Pts',(-54.685374403676,-44.5634564876869,
12.));
#139062=CARTESIAN_POINT('Ctrl Pts',(-54.7046666586777,-44.5715274907637,
12.));
#139063=CARTESIAN_POINT('Ctrl Pts',(-54.7240136637744,-44.5795976579476,
12.));
#139064=CARTESIAN_POINT('Ctrl Pts',(-54.7434152971285,-44.5876668519676,
12.));
#139065=CARTESIAN_POINT('Ctrl Pts',(-54.7628714377042,-44.5957349366062,
12.));
#139066=CARTESIAN_POINT('Ctrl Pts',(-54.7823819650137,-44.60380177643,12.));
#139067=CARTESIAN_POINT('Ctrl Pts',(-54.8019467588258,-44.6118672364889,
12.));
#139068=CARTESIAN_POINT('Ctrl Pts',(-54.8215656991817,-44.6199311823276,
12.));
#139069=CARTESIAN_POINT('Ctrl Pts',(-54.8412386665264,-44.6279934801159,
12.));
#139070=CARTESIAN_POINT('Ctrl Pts',(-54.860965541796,-44.6360539967392,
12.));
#139071=CARTESIAN_POINT('Ctrl Pts',(-54.8807462065177,-44.6441125999074,
12.));
#139072=CARTESIAN_POINT('Ctrl Pts',(-54.9005805428991,-44.6521691582551,
12.));
#139073=CARTESIAN_POINT('Ctrl Pts',(-54.9204684337845,-44.6602235412853,
12.));
#139074=CARTESIAN_POINT('Ctrl Pts',(-54.9404097626088,-44.6682756193155,
12.));
#139075=CARTESIAN_POINT('Ctrl Pts',(-54.9604044133497,-44.6763252634255,
12.));
#139076=CARTESIAN_POINT('Ctrl Pts',(-54.9804522704668,-44.6843723453985,
12.));
#139077=CARTESIAN_POINT('Ctrl Pts',(-55.0005532188644,-44.6924167376851,
12.));
#139078=CARTESIAN_POINT('Ctrl Pts',(-55.020707143922,-44.7004583134235,
12.));
#139079=CARTESIAN_POINT('Ctrl Pts',(-55.0409139315074,-44.7084969464509,
12.));
#139080=CARTESIAN_POINT('Ctrl Pts',(-55.0611734679902,-44.7165325113165,
12.));
#139081=CARTESIAN_POINT('Ctrl Pts',(-55.0814856402507,-44.7245648832988,
12.));
#139082=CARTESIAN_POINT('Ctrl Pts',(-55.1018503356806,-44.7325939384042,
12.));
#139083=CARTESIAN_POINT('Ctrl Pts',(-55.1222674421747,-44.7406195533482,
12.));
#139084=CARTESIAN_POINT('Ctrl Pts',(-55.1427368481201,-44.7486416055419,
12.));
#139085=CARTESIAN_POINT('Ctrl Pts',(-55.1632584423813,-44.7566599730771,
12.));
#139086=CARTESIAN_POINT('Ctrl Pts',(-55.1838321142777,-44.7646745347108,
12.));
#139087=CARTESIAN_POINT('Ctrl Pts',(-55.2044577535865,-44.7726851698618,
12.));
#139088=CARTESIAN_POINT('Ctrl Pts',(-55.2251352505474,-44.7806917586077,
12.));
#139089=CARTESIAN_POINT('Ctrl Pts',(-55.2458644958617,-44.7886941816823,
12.));
#139090=CARTESIAN_POINT('Ctrl Pts',(-55.2666453806883,-44.796692320474,
12.));
#139091=CARTESIAN_POINT('Ctrl Pts',(-55.287477796635,-44.8046860570244,
12.));
#139092=CARTESIAN_POINT('Ctrl Pts',(-55.3083616357605,-44.8126752740208,
12.));
#139093=CARTESIAN_POINT('Ctrl Pts',(-55.3292967905725,-44.8206598547887,
12.));
#139094=CARTESIAN_POINT('Ctrl Pts',(-55.3502831540228,-44.8286396832847,
12.));
#139095=CARTESIAN_POINT('Ctrl Pts',(-55.3713206194967,-44.8366146440901,
12.));
#139096=CARTESIAN_POINT('Ctrl Pts',(-55.3924090808014,-44.8445846224044,
12.));
#139097=CARTESIAN_POINT('Ctrl Pts',(-55.4135484321718,-44.8525495040408,
12.));
#139098=CARTESIAN_POINT('Ctrl Pts',(-55.4347385682704,-44.8605091754214,
12.));
#139099=CARTESIAN_POINT('Ctrl Pts',(-55.4559793841836,-44.8684635235725,
12.));
#139100=CARTESIAN_POINT('Ctrl Pts',(-55.4772707754126,-44.8764124361206,
12.));
#139101=CARTESIAN_POINT('Ctrl Pts',(-55.4986126378656,-44.8843558012886,
12.));
#139102=CARTESIAN_POINT('Ctrl Pts',(-55.5200048678629,-44.8922935078889,
12.));
#139103=CARTESIAN_POINT('Ctrl Pts',(-55.541447362134,-44.9002254453183,
12.));
#139104=CARTESIAN_POINT('Ctrl Pts',(-55.5629400178142,-44.908151503553,
12.));
#139105=CARTESIAN_POINT('Ctrl Pts',(-55.5844827324338,-44.9160715731443,
12.));
#139106=CARTESIAN_POINT('Ctrl Pts',(-55.6060754039121,-44.9239855452144,
12.));
#139107=CARTESIAN_POINT('Ctrl Pts',(-55.6277179305633,-44.9318933114506,
12.));
#139108=CARTESIAN_POINT('Ctrl Pts',(-55.6494102110935,-44.9397947641006,
12.));
#139109=CARTESIAN_POINT('Ctrl Pts',(-55.6711521445979,-44.9476897959684,
12.));
#139110=CARTESIAN_POINT('Ctrl Pts',(-55.6929436305489,-44.9555783004106,
12.));
#139111=CARTESIAN_POINT('Ctrl Pts',(-55.714784568793,-44.9634601713321,
12.));
#139112=CARTESIAN_POINT('Ctrl Pts',(-55.7366748595552,-44.9713353031804,
12.));
#139113=CARTESIAN_POINT('Ctrl Pts',(-55.7586144034367,-44.9792035909413,
12.));
#139114=CARTESIAN_POINT('Ctrl Pts',(-55.7806031014106,-44.9870649301342,
12.));
#139115=CARTESIAN_POINT('Ctrl Pts',(-55.8026408548105,-44.9949192168093,
12.));
#139116=CARTESIAN_POINT('Ctrl Pts',(-55.8247275653289,-45.0027663475433,
12.));
#139117=CARTESIAN_POINT('Ctrl Pts',(-55.8468631350218,-45.0106062194342,
12.));
#139118=CARTESIAN_POINT('Ctrl Pts',(-55.8690474663065,-45.0184387300973,
12.));
#139119=CARTESIAN_POINT('Ctrl Pts',(-55.8912804619577,-45.0262637776614,
12.));
#139120=CARTESIAN_POINT('Ctrl Pts',(-55.9135620250954,-45.0340812607657,
12.));
#139121=CARTESIAN_POINT('Ctrl Pts',(-55.9358920591837,-45.041891078555,
12.));
#139122=CARTESIAN_POINT('Ctrl Pts',(-55.9582704680356,-45.0496931306755,
12.));
#139123=CARTESIAN_POINT('Ctrl Pts',(-55.9806971558097,-45.0574873172694,
12.));
#139124=CARTESIAN_POINT('Ctrl Pts',(-56.003172027008,-45.0652735389733,
12.));
#139125=CARTESIAN_POINT('Ctrl Pts',(-56.0256949864639,-45.0730516969148,
12.));
#139126=CARTESIAN_POINT('Ctrl Pts',(-56.048265939342,-45.0808216927089,
12.));
#139127=CARTESIAN_POINT('Ctrl Pts',(-56.0708847911416,-45.0885834284517,
12.));
#139128=CARTESIAN_POINT('Ctrl Pts',(-56.0935514476945,-45.0963368067177,
12.));
#139129=CARTESIAN_POINT('Ctrl Pts',(-56.116265815162,-45.1040817305561,
12.));
#139130=CARTESIAN_POINT('Ctrl Pts',(-56.1390278000226,-45.1118181034888,
12.));
#139131=CARTESIAN_POINT('Ctrl Pts',(-56.1618373090732,-45.1195458295062,
12.));
#139132=CARTESIAN_POINT('Ctrl Pts',(-56.1846942494325,-45.127264813063,
12.));
#139133=CARTESIAN_POINT('Ctrl Pts',(-56.2075985285393,-45.1349749590737,
12.));
#139134=CARTESIAN_POINT('Ctrl Pts',(-56.230550054149,-45.1426761729105,
12.));
#139135=CARTESIAN_POINT('Ctrl Pts',(-56.2535487343221,-45.1503683604005,
12.));
#139136=CARTESIAN_POINT('Ctrl Pts',(-56.2765944774245,-45.1580514278223,
12.));
#139137=CARTESIAN_POINT('Ctrl Pts',(-56.2996871921316,-45.1657252819013,
12.));
#139138=CARTESIAN_POINT('Ctrl Pts',(-56.3228267874264,-45.173389829806,
12.));
#139139=CARTESIAN_POINT('Ctrl Pts',(-56.3460131725964,-45.1810449791453,
12.));
#139140=CARTESIAN_POINT('Ctrl Pts',(-56.3692462572231,-45.1886906379667,
12.));
#139141=CARTESIAN_POINT('Ctrl Pts',(-56.3925259511806,-45.1963267147529,
12.));
#139142=CARTESIAN_POINT('Ctrl Pts',(-56.4158521646411,-45.2039531184171,
12.));
#139143=CARTESIAN_POINT('Ctrl Pts',(-56.4392248080732,-45.2115697583,12.));
#139144=CARTESIAN_POINT('Ctrl Pts',(-56.4626437922386,-45.2191765441666,
12.));
#139145=CARTESIAN_POINT('Ctrl Pts',(-56.4861090281823,-45.2267733862049,
12.));
#139146=CARTESIAN_POINT('Ctrl Pts',(-56.5096204272306,-45.2343601950227,
12.));
#139147=CARTESIAN_POINT('Ctrl Pts',(-56.5331779009958,-45.2419368816428,
12.));
#139148=CARTESIAN_POINT('Ctrl Pts',(-56.5567813613756,-45.2495033575,12.));
#139149=CARTESIAN_POINT('Ctrl Pts',(-56.5804307205505,-45.257059534438,
12.));
#139150=CARTESIAN_POINT('Ctrl Pts',(-56.6041258909741,-45.2646053247087,
12.));
#139151=CARTESIAN_POINT('Ctrl Pts',(-56.6278667853702,-45.2721406409695,
12.));
#139152=CARTESIAN_POINT('Ctrl Pts',(-56.6516533167384,-45.2796653962785,
12.));
#139153=CARTESIAN_POINT('Ctrl Pts',(-56.6754853983528,-45.2871795040906,
12.));
#139154=CARTESIAN_POINT('Ctrl Pts',(-56.69936294376,-45.2946828782559,12.));
#139155=CARTESIAN_POINT('Ctrl Pts',(-56.7232858667709,-45.3021754330178,
12.));
#139156=CARTESIAN_POINT('Ctrl Pts',(-56.7472540814554,-45.3096570830117,
12.));
#139157=CARTESIAN_POINT('Ctrl Pts',(-56.7712675021491,-45.31712774326,12.));
#139158=CARTESIAN_POINT('Ctrl Pts',(-56.7953260434524,-45.3245873291684,
12.));
#139159=CARTESIAN_POINT('Ctrl Pts',(-56.8194296202291,-45.332035756524,
12.));
#139160=CARTESIAN_POINT('Ctrl Pts',(-56.8435781475981,-45.3394729414931,
12.));
#139161=CARTESIAN_POINT('Ctrl Pts',(-56.8677715409268,-45.3468988006203,
12.));
#139162=CARTESIAN_POINT('Ctrl Pts',(-56.8920097158377,-45.3543132508238,
12.));
#139163=CARTESIAN_POINT('Ctrl Pts',(-56.9162925882085,-45.3617162093922,
12.));
#139164=CARTESIAN_POINT('Ctrl Pts',(-56.9406200741714,-45.3691075939826,
12.));
#139165=CARTESIAN_POINT('Ctrl Pts',(-56.9649920901073,-45.3764873226196,
12.));
#139166=CARTESIAN_POINT('Ctrl Pts',(-56.9894085526373,-45.3838553136948,
12.));
#139167=CARTESIAN_POINT('Ctrl Pts',(-57.0138693786278,-45.3912114859616,
12.));
#139168=CARTESIAN_POINT('Ctrl Pts',(-57.0383744851913,-45.3985557585311,
12.));
#139169=CARTESIAN_POINT('Ctrl Pts',(-57.0629237896848,-45.4058880508693,
12.));
#139170=CARTESIAN_POINT('Ctrl Pts',(-57.0875172097051,-45.4132082827948,
12.));
#139171=CARTESIAN_POINT('Ctrl Pts',(-57.112154663078,-45.4205163744781,
12.));
#139172=CARTESIAN_POINT('Ctrl Pts',(-57.136836067863,-45.4278122464389,
12.));
#139173=CARTESIAN_POINT('Ctrl Pts',(-57.1615613423584,-45.4350958195433,
12.));
#139174=CARTESIAN_POINT('Ctrl Pts',(-57.186330405101,-45.4423670150034,
12.));
#139175=CARTESIAN_POINT('Ctrl Pts',(-57.2111431748631,-45.4496257543759,
12.));
#139176=CARTESIAN_POINT('Ctrl Pts',(-57.2359995706447,-45.4568719595641,
12.));
#139177=CARTESIAN_POINT('Ctrl Pts',(-57.2608995116733,-45.4641055528141,
12.));
#139178=CARTESIAN_POINT('Ctrl Pts',(-57.2858429174062,-45.4713264567063,
12.));
#139179=CARTESIAN_POINT('Ctrl Pts',(-57.3108297075265,-45.4785345941507,
12.));
#139180=CARTESIAN_POINT('Ctrl Pts',(-57.3358598019389,-45.4857298883824,
12.));
#139181=CARTESIAN_POINT('Ctrl Pts',(-57.3609331207574,-45.4929122629572,
12.));
#139182=CARTESIAN_POINT('Ctrl Pts',(-57.3860495843033,-45.5000816417509,
12.));
#139183=CARTESIAN_POINT('Ctrl Pts',(-57.4112091131183,-45.5072379489631,
12.));
#139184=CARTESIAN_POINT('Ctrl Pts',(-57.4364116279702,-45.5143811091205,
12.));
#139185=CARTESIAN_POINT('Ctrl Pts',(-57.4616570498568,-45.5215110470825,
12.));
#139186=CARTESIAN_POINT('Ctrl Pts',(-57.4869453000063,-45.5286276880484,
12.));
#139187=CARTESIAN_POINT('Ctrl Pts',(-57.5122762998745,-45.5357309575611,
12.));
#139188=CARTESIAN_POINT('Ctrl Pts',(-57.537649971135,-45.542820781484,12.));
#139189=CARTESIAN_POINT('Ctrl Pts',(-57.563066235668,-45.5498970859834,
12.));
#139190=CARTESIAN_POINT('Ctrl Pts',(-57.5885250155433,-45.5569597975096,
12.));
#139191=CARTESIAN_POINT('Ctrl Pts',(-57.614026233004,-45.5640088427813,
12.));
#139192=CARTESIAN_POINT('Ctrl Pts',(-57.6395698104404,-45.5710441487674,
12.));
#139193=CARTESIAN_POINT('Ctrl Pts',(-57.6651556704237,-45.5780656427163,
12.));
#139194=CARTESIAN_POINT('Ctrl Pts',(-57.6907837357418,-45.5850732521895,
12.));
#139195=CARTESIAN_POINT('Ctrl Pts',(-57.7164539294314,-45.5920669050986,
12.));
#139196=CARTESIAN_POINT('Ctrl Pts',(-57.7421661748026,-45.5990465297343,
12.));
#139197=CARTESIAN_POINT('Ctrl Pts',(-57.7679203954742,-45.6060120548205,
12.));
#139198=CARTESIAN_POINT('Ctrl Pts',(-57.7937165153387,-45.6129634094683,
12.));
#139199=CARTESIAN_POINT('Ctrl Pts',(-57.8195544584845,-45.6199005230783,
12.));
#139200=CARTESIAN_POINT('Ctrl Pts',(-57.8454341491238,-45.6268233252544,
12.));
#139201=CARTESIAN_POINT('Ctrl Pts',(-57.8713555115232,-45.6337317457252,
12.));
#139202=CARTESIAN_POINT('Ctrl Pts',(-57.8973184699034,-45.6406257142381,
12.));
#139203=CARTESIAN_POINT('Ctrl Pts',(-57.9233229484311,-45.6475051605535,
12.));
#139204=CARTESIAN_POINT('Ctrl Pts',(-57.9493688714237,-45.6543700146679,
12.));
#139205=CARTESIAN_POINT('Ctrl Pts',(-57.9754561635061,-45.661220206992,
12.));
#139206=CARTESIAN_POINT('Ctrl Pts',(-58.0015847497837,-45.6680556685493,
12.));
#139207=CARTESIAN_POINT('Ctrl Pts',(-58.0277545560012,-45.6748763311643,
12.));
#139208=CARTESIAN_POINT('Ctrl Pts',(-58.0539655087117,-45.6816821276678,
12.));
#139209=CARTESIAN_POINT('Ctrl Pts',(-58.0802175348966,-45.6884729914485,
12.));
#139210=CARTESIAN_POINT('Ctrl Pts',(-58.1065105615907,-45.695248856015,
12.));
#139211=CARTESIAN_POINT('Ctrl Pts',(-58.1328445154676,-45.702009654518,
12.));
#139212=CARTESIAN_POINT('Ctrl Pts',(-58.1592193225137,-45.7087553193771,
12.));
#139213=CARTESIAN_POINT('Ctrl Pts',(-58.185634907469,-45.7154857816483,
12.));
#139214=CARTESIAN_POINT('Ctrl Pts',(-58.2120911942772,-45.7222009715397,
12.));
#139215=CARTESIAN_POINT('Ctrl Pts',(-58.2385881070913,-45.7289008195578,
12.));
#139216=CARTESIAN_POINT('Ctrl Pts',(-58.2651255711453,-45.7355852575106,
12.));
#139217=CARTESIAN_POINT('Ctrl Pts',(-58.291703513584,-45.742254219463,12.));
#139218=CARTESIAN_POINT('Ctrl Pts',(-58.3183218645317,-45.7489076429763,
12.));
#139219=CARTESIAN_POINT('Ctrl Pts',(-58.3449805573423,-45.755545469402,
12.));
#139220=CARTESIAN_POINT('Ctrl Pts',(-58.3678667473438,-45.7612219538124,
12.));
#139221=CARTESIAN_POINT('Ctrl Pts',(-58.3854348517444,-45.7655655205367,
12.));
#139222=CARTESIAN_POINT('Ctrl Pts',(-58.397667048107,-45.7685831165565,
12.));
#139223=CARTESIAN_POINT('Ctrl Pts',(-58.4045515723357,-45.7702793558177,
12.));
#139224=CARTESIAN_POINT('Ctrl Pts',(-58.4060826907797,-45.7706564944896,
12.));
#139225=CARTESIAN_POINT('',(-54.1679505278134,-44.3377168516418,0.));
#139226=CARTESIAN_POINT('',(-54.1679505278134,-44.3377168516418,0.));
#139227=CARTESIAN_POINT('Ctrl Pts',(-58.4060826907797,-45.7706564944896,
0.));
#139228=CARTESIAN_POINT('Ctrl Pts',(-58.4045515723357,-45.7702793558177,
0.));
#139229=CARTESIAN_POINT('Ctrl Pts',(-58.397667048107,-45.7685831165565,
0.));
#139230=CARTESIAN_POINT('Ctrl Pts',(-58.3854348517444,-45.7655655205367,
0.));
#139231=CARTESIAN_POINT('Ctrl Pts',(-58.3678667473437,-45.7612219538124,
0.));
#139232=CARTESIAN_POINT('Ctrl Pts',(-58.3449805573423,-45.755545469402,
0.));
#139233=CARTESIAN_POINT('Ctrl Pts',(-58.3183218645317,-45.7489076429763,
0.));
#139234=CARTESIAN_POINT('Ctrl Pts',(-58.291703513584,-45.742254219463,0.));
#139235=CARTESIAN_POINT('Ctrl Pts',(-58.2651255711453,-45.7355852575106,
0.));
#139236=CARTESIAN_POINT('Ctrl Pts',(-58.2385881070913,-45.7289008195578,
0.));
#139237=CARTESIAN_POINT('Ctrl Pts',(-58.2120911942772,-45.7222009715397,
0.));
#139238=CARTESIAN_POINT('Ctrl Pts',(-58.185634907469,-45.7154857816483,
0.));
#139239=CARTESIAN_POINT('Ctrl Pts',(-58.1592193225137,-45.7087553193771,
0.));
#139240=CARTESIAN_POINT('Ctrl Pts',(-58.1328445154676,-45.702009654518,
0.));
#139241=CARTESIAN_POINT('Ctrl Pts',(-58.1065105615907,-45.695248856015,
0.));
#139242=CARTESIAN_POINT('Ctrl Pts',(-58.0802175348966,-45.6884729914485,
0.));
#139243=CARTESIAN_POINT('Ctrl Pts',(-58.0539655087117,-45.6816821276678,
0.));
#139244=CARTESIAN_POINT('Ctrl Pts',(-58.0277545560012,-45.6748763311643,
0.));
#139245=CARTESIAN_POINT('Ctrl Pts',(-58.0015847497837,-45.6680556685493,
0.));
#139246=CARTESIAN_POINT('Ctrl Pts',(-57.9754561635061,-45.661220206992,
0.));
#139247=CARTESIAN_POINT('Ctrl Pts',(-57.9493688714237,-45.6543700146679,
0.));
#139248=CARTESIAN_POINT('Ctrl Pts',(-57.9233229484311,-45.6475051605535,
0.));
#139249=CARTESIAN_POINT('Ctrl Pts',(-57.8973184699034,-45.6406257142381,
0.));
#139250=CARTESIAN_POINT('Ctrl Pts',(-57.8713555115232,-45.6337317457252,
0.));
#139251=CARTESIAN_POINT('Ctrl Pts',(-57.8454341491238,-45.6268233252544,
0.));
#139252=CARTESIAN_POINT('Ctrl Pts',(-57.8195544584845,-45.6199005230783,
0.));
#139253=CARTESIAN_POINT('Ctrl Pts',(-57.7937165153387,-45.6129634094683,
0.));
#139254=CARTESIAN_POINT('Ctrl Pts',(-57.7679203954742,-45.6060120548205,
0.));
#139255=CARTESIAN_POINT('Ctrl Pts',(-57.7421661748026,-45.5990465297343,
0.));
#139256=CARTESIAN_POINT('Ctrl Pts',(-57.7164539294314,-45.5920669050986,
0.));
#139257=CARTESIAN_POINT('Ctrl Pts',(-57.6907837357418,-45.5850732521895,
0.));
#139258=CARTESIAN_POINT('Ctrl Pts',(-57.6651556704237,-45.5780656427163,
0.));
#139259=CARTESIAN_POINT('Ctrl Pts',(-57.6395698104404,-45.5710441487674,
0.));
#139260=CARTESIAN_POINT('Ctrl Pts',(-57.614026233004,-45.5640088427813,
0.));
#139261=CARTESIAN_POINT('Ctrl Pts',(-57.5885250155433,-45.5569597975096,
0.));
#139262=CARTESIAN_POINT('Ctrl Pts',(-57.563066235668,-45.5498970859834,
0.));
#139263=CARTESIAN_POINT('Ctrl Pts',(-57.537649971135,-45.542820781484,0.));
#139264=CARTESIAN_POINT('Ctrl Pts',(-57.5122762998745,-45.5357309575611,
0.));
#139265=CARTESIAN_POINT('Ctrl Pts',(-57.4869453000063,-45.5286276880484,
0.));
#139266=CARTESIAN_POINT('Ctrl Pts',(-57.4616570498568,-45.5215110470825,
0.));
#139267=CARTESIAN_POINT('Ctrl Pts',(-57.4364116279702,-45.5143811091205,
0.));
#139268=CARTESIAN_POINT('Ctrl Pts',(-57.4112091131183,-45.5072379489631,
0.));
#139269=CARTESIAN_POINT('Ctrl Pts',(-57.3860495843033,-45.5000816417509,
0.));
#139270=CARTESIAN_POINT('Ctrl Pts',(-57.3609331207574,-45.4929122629572,
0.));
#139271=CARTESIAN_POINT('Ctrl Pts',(-57.3358598019389,-45.4857298883824,
0.));
#139272=CARTESIAN_POINT('Ctrl Pts',(-57.3108297075265,-45.4785345941507,
0.));
#139273=CARTESIAN_POINT('Ctrl Pts',(-57.2858429174062,-45.4713264567063,
0.));
#139274=CARTESIAN_POINT('Ctrl Pts',(-57.2608995116733,-45.4641055528141,
0.));
#139275=CARTESIAN_POINT('Ctrl Pts',(-57.2359995706447,-45.4568719595641,
0.));
#139276=CARTESIAN_POINT('Ctrl Pts',(-57.2111431748631,-45.4496257543759,
0.));
#139277=CARTESIAN_POINT('Ctrl Pts',(-57.186330405101,-45.4423670150034,
0.));
#139278=CARTESIAN_POINT('Ctrl Pts',(-57.1615613423584,-45.4350958195433,
0.));
#139279=CARTESIAN_POINT('Ctrl Pts',(-57.136836067863,-45.4278122464389,
0.));
#139280=CARTESIAN_POINT('Ctrl Pts',(-57.112154663078,-45.4205163744781,
0.));
#139281=CARTESIAN_POINT('Ctrl Pts',(-57.0875172097051,-45.4132082827948,
0.));
#139282=CARTESIAN_POINT('Ctrl Pts',(-57.0629237896848,-45.4058880508693,
0.));
#139283=CARTESIAN_POINT('Ctrl Pts',(-57.0383744851913,-45.3985557585311,
0.));
#139284=CARTESIAN_POINT('Ctrl Pts',(-57.0138693786278,-45.3912114859616,
0.));
#139285=CARTESIAN_POINT('Ctrl Pts',(-56.9894085526373,-45.3838553136948,
0.));
#139286=CARTESIAN_POINT('Ctrl Pts',(-56.9649920901073,-45.3764873226196,
0.));
#139287=CARTESIAN_POINT('Ctrl Pts',(-56.9406200741714,-45.3691075939826,
0.));
#139288=CARTESIAN_POINT('Ctrl Pts',(-56.9162925882085,-45.3617162093922,
0.));
#139289=CARTESIAN_POINT('Ctrl Pts',(-56.8920097158377,-45.3543132508238,
0.));
#139290=CARTESIAN_POINT('Ctrl Pts',(-56.8677715409268,-45.3468988006203,
0.));
#139291=CARTESIAN_POINT('Ctrl Pts',(-56.8435781475981,-45.3394729414931,
0.));
#139292=CARTESIAN_POINT('Ctrl Pts',(-56.8194296202291,-45.332035756524,
0.));
#139293=CARTESIAN_POINT('Ctrl Pts',(-56.7953260434524,-45.3245873291684,
0.));
#139294=CARTESIAN_POINT('Ctrl Pts',(-56.7712675021491,-45.31712774326,0.));
#139295=CARTESIAN_POINT('Ctrl Pts',(-56.7472540814554,-45.3096570830117,
0.));
#139296=CARTESIAN_POINT('Ctrl Pts',(-56.7232858667709,-45.3021754330178,
0.));
#139297=CARTESIAN_POINT('Ctrl Pts',(-56.69936294376,-45.2946828782559,0.));
#139298=CARTESIAN_POINT('Ctrl Pts',(-56.6754853983528,-45.2871795040906,
0.));
#139299=CARTESIAN_POINT('Ctrl Pts',(-56.6516533167384,-45.2796653962785,
0.));
#139300=CARTESIAN_POINT('Ctrl Pts',(-56.6278667853702,-45.2721406409695,
0.));
#139301=CARTESIAN_POINT('Ctrl Pts',(-56.6041258909741,-45.2646053247087,
0.));
#139302=CARTESIAN_POINT('Ctrl Pts',(-56.5804307205505,-45.257059534438,
0.));
#139303=CARTESIAN_POINT('Ctrl Pts',(-56.5567813613756,-45.2495033575,0.));
#139304=CARTESIAN_POINT('Ctrl Pts',(-56.5331779009958,-45.2419368816428,
0.));
#139305=CARTESIAN_POINT('Ctrl Pts',(-56.5096204272306,-45.2343601950227,
0.));
#139306=CARTESIAN_POINT('Ctrl Pts',(-56.4861090281823,-45.2267733862049,
0.));
#139307=CARTESIAN_POINT('Ctrl Pts',(-56.4626437922386,-45.2191765441666,
0.));
#139308=CARTESIAN_POINT('Ctrl Pts',(-56.4392248080732,-45.2115697583,0.));
#139309=CARTESIAN_POINT('Ctrl Pts',(-56.4158521646411,-45.2039531184171,
0.));
#139310=CARTESIAN_POINT('Ctrl Pts',(-56.3925259511806,-45.1963267147529,
0.));
#139311=CARTESIAN_POINT('Ctrl Pts',(-56.3692462572231,-45.1886906379667,
0.));
#139312=CARTESIAN_POINT('Ctrl Pts',(-56.3460131725964,-45.1810449791453,
0.));
#139313=CARTESIAN_POINT('Ctrl Pts',(-56.3228267874264,-45.173389829806,
0.));
#139314=CARTESIAN_POINT('Ctrl Pts',(-56.2996871921316,-45.1657252819013,
0.));
#139315=CARTESIAN_POINT('Ctrl Pts',(-56.2765944774245,-45.1580514278223,
0.));
#139316=CARTESIAN_POINT('Ctrl Pts',(-56.2535487343221,-45.1503683604005,
0.));
#139317=CARTESIAN_POINT('Ctrl Pts',(-56.230550054149,-45.1426761729105,
0.));
#139318=CARTESIAN_POINT('Ctrl Pts',(-56.2075985285393,-45.1349749590737,
0.));
#139319=CARTESIAN_POINT('Ctrl Pts',(-56.1846942494325,-45.127264813063,
0.));
#139320=CARTESIAN_POINT('Ctrl Pts',(-56.1618373090732,-45.1195458295062,
0.));
#139321=CARTESIAN_POINT('Ctrl Pts',(-56.1390278000226,-45.1118181034888,
0.));
#139322=CARTESIAN_POINT('Ctrl Pts',(-56.116265815162,-45.1040817305561,
0.));
#139323=CARTESIAN_POINT('Ctrl Pts',(-56.0935514476945,-45.0963368067177,
0.));
#139324=CARTESIAN_POINT('Ctrl Pts',(-56.0708847911416,-45.0885834284517,
0.));
#139325=CARTESIAN_POINT('Ctrl Pts',(-56.048265939342,-45.0808216927089,
0.));
#139326=CARTESIAN_POINT('Ctrl Pts',(-56.0256949864639,-45.0730516969148,
0.));
#139327=CARTESIAN_POINT('Ctrl Pts',(-56.003172027008,-45.0652735389733,
0.));
#139328=CARTESIAN_POINT('Ctrl Pts',(-55.9806971558097,-45.0574873172694,
0.));
#139329=CARTESIAN_POINT('Ctrl Pts',(-55.9582704680356,-45.0496931306755,
0.));
#139330=CARTESIAN_POINT('Ctrl Pts',(-55.9358920591837,-45.041891078555,
0.));
#139331=CARTESIAN_POINT('Ctrl Pts',(-55.9135620250954,-45.0340812607657,
0.));
#139332=CARTESIAN_POINT('Ctrl Pts',(-55.8912804619577,-45.0262637776614,
0.));
#139333=CARTESIAN_POINT('Ctrl Pts',(-55.8690474663065,-45.0184387300973,
0.));
#139334=CARTESIAN_POINT('Ctrl Pts',(-55.8468631350218,-45.0106062194342,
0.));
#139335=CARTESIAN_POINT('Ctrl Pts',(-55.8247275653289,-45.0027663475433,
0.));
#139336=CARTESIAN_POINT('Ctrl Pts',(-55.8026408548105,-44.9949192168093,
0.));
#139337=CARTESIAN_POINT('Ctrl Pts',(-55.7806031014106,-44.9870649301342,
0.));
#139338=CARTESIAN_POINT('Ctrl Pts',(-55.7586144034367,-44.9792035909413,
0.));
#139339=CARTESIAN_POINT('Ctrl Pts',(-55.7366748595552,-44.9713353031804,
0.));
#139340=CARTESIAN_POINT('Ctrl Pts',(-55.714784568793,-44.9634601713321,
0.));
#139341=CARTESIAN_POINT('Ctrl Pts',(-55.6929436305489,-44.9555783004106,
0.));
#139342=CARTESIAN_POINT('Ctrl Pts',(-55.6711521445979,-44.9476897959684,
0.));
#139343=CARTESIAN_POINT('Ctrl Pts',(-55.6494102110935,-44.9397947641006,
0.));
#139344=CARTESIAN_POINT('Ctrl Pts',(-55.6277179305633,-44.9318933114506,
0.));
#139345=CARTESIAN_POINT('Ctrl Pts',(-55.6060754039121,-44.9239855452144,
0.));
#139346=CARTESIAN_POINT('Ctrl Pts',(-55.5844827324338,-44.9160715731443,
0.));
#139347=CARTESIAN_POINT('Ctrl Pts',(-55.5629400178142,-44.908151503553,
0.));
#139348=CARTESIAN_POINT('Ctrl Pts',(-55.541447362134,-44.9002254453183,
0.));
#139349=CARTESIAN_POINT('Ctrl Pts',(-55.5200048678629,-44.8922935078889,
0.));
#139350=CARTESIAN_POINT('Ctrl Pts',(-55.4986126378656,-44.8843558012886,
0.));
#139351=CARTESIAN_POINT('Ctrl Pts',(-55.4772707754126,-44.8764124361206,
0.));
#139352=CARTESIAN_POINT('Ctrl Pts',(-55.4559793841836,-44.8684635235725,
0.));
#139353=CARTESIAN_POINT('Ctrl Pts',(-55.4347385682704,-44.8605091754214,
0.));
#139354=CARTESIAN_POINT('Ctrl Pts',(-55.4135484321718,-44.8525495040408,
0.));
#139355=CARTESIAN_POINT('Ctrl Pts',(-55.3924090808014,-44.8445846224044,
0.));
#139356=CARTESIAN_POINT('Ctrl Pts',(-55.3713206194967,-44.8366146440901,
0.));
#139357=CARTESIAN_POINT('Ctrl Pts',(-55.3502831540228,-44.8286396832847,
0.));
#139358=CARTESIAN_POINT('Ctrl Pts',(-55.3292967905725,-44.8206598547887,
0.));
#139359=CARTESIAN_POINT('Ctrl Pts',(-55.3083616357605,-44.8126752740208,
0.));
#139360=CARTESIAN_POINT('Ctrl Pts',(-55.287477796635,-44.8046860570244,
0.));
#139361=CARTESIAN_POINT('Ctrl Pts',(-55.2666453806883,-44.796692320474,
0.));
#139362=CARTESIAN_POINT('Ctrl Pts',(-55.2458644958617,-44.7886941816823,
0.));
#139363=CARTESIAN_POINT('Ctrl Pts',(-55.2251352505474,-44.7806917586077,
0.));
#139364=CARTESIAN_POINT('Ctrl Pts',(-55.2044577535865,-44.7726851698618,
0.));
#139365=CARTESIAN_POINT('Ctrl Pts',(-55.1838321142777,-44.7646745347108,
0.));
#139366=CARTESIAN_POINT('Ctrl Pts',(-55.1632584423813,-44.7566599730771,
0.));
#139367=CARTESIAN_POINT('Ctrl Pts',(-55.1427368481201,-44.7486416055419,
0.));
#139368=CARTESIAN_POINT('Ctrl Pts',(-55.1222674421747,-44.7406195533482,
0.));
#139369=CARTESIAN_POINT('Ctrl Pts',(-55.1018503356806,-44.7325939384042,
0.));
#139370=CARTESIAN_POINT('Ctrl Pts',(-55.0814856402507,-44.7245648832988,
0.));
#139371=CARTESIAN_POINT('Ctrl Pts',(-55.0611734679902,-44.7165325113165,
0.));
#139372=CARTESIAN_POINT('Ctrl Pts',(-55.0409139315074,-44.7084969464509,
0.));
#139373=CARTESIAN_POINT('Ctrl Pts',(-55.020707143922,-44.7004583134235,
0.));
#139374=CARTESIAN_POINT('Ctrl Pts',(-55.0005532188644,-44.6924167376851,
0.));
#139375=CARTESIAN_POINT('Ctrl Pts',(-54.9804522704668,-44.6843723453985,
0.));
#139376=CARTESIAN_POINT('Ctrl Pts',(-54.9604044133497,-44.6763252634255,
0.));
#139377=CARTESIAN_POINT('Ctrl Pts',(-54.9404097626088,-44.6682756193155,
0.));
#139378=CARTESIAN_POINT('Ctrl Pts',(-54.9204684337845,-44.6602235412853,
0.));
#139379=CARTESIAN_POINT('Ctrl Pts',(-54.9005805428991,-44.6521691582551,
0.));
#139380=CARTESIAN_POINT('Ctrl Pts',(-54.8807462065177,-44.6441125999074,
0.));
#139381=CARTESIAN_POINT('Ctrl Pts',(-54.860965541796,-44.6360539967392,
0.));
#139382=CARTESIAN_POINT('Ctrl Pts',(-54.8412386665264,-44.6279934801159,
0.));
#139383=CARTESIAN_POINT('Ctrl Pts',(-54.8215656991817,-44.6199311823276,
0.));
#139384=CARTESIAN_POINT('Ctrl Pts',(-54.8019467588258,-44.6118672364889,
0.));
#139385=CARTESIAN_POINT('Ctrl Pts',(-54.7823819650137,-44.60380177643,0.));
#139386=CARTESIAN_POINT('Ctrl Pts',(-54.7628714377042,-44.5957349366062,
0.));
#139387=CARTESIAN_POINT('Ctrl Pts',(-54.7434152971285,-44.5876668519676,
0.));
#139388=CARTESIAN_POINT('Ctrl Pts',(-54.7240136637744,-44.5795976579476,
0.));
#139389=CARTESIAN_POINT('Ctrl Pts',(-54.7046666586777,-44.5715274907637,
0.));
#139390=CARTESIAN_POINT('Ctrl Pts',(-54.685374403676,-44.5634564876869,
0.));
#139391=CARTESIAN_POINT('Ctrl Pts',(-54.6661370216242,-44.5553847872712,
0.));
#139392=CARTESIAN_POINT('Ctrl Pts',(-54.6469546367381,-44.5473125297289,
0.));
#139393=CARTESIAN_POINT('Ctrl Pts',(-54.6278273743554,-44.5392398566775,
0.));
#139394=CARTESIAN_POINT('Ctrl Pts',(-54.6087553602889,-44.5311669104494,
0.));
#139395=CARTESIAN_POINT('Ctrl Pts',(-54.5897387202812,-44.5230938335165,
0.));
#139396=CARTESIAN_POINT('Ctrl Pts',(-54.5707775794436,-44.5150207679007,
0.));
#139397=CARTESIAN_POINT('Ctrl Pts',(-54.5518720616056,-44.5069478544977,
0.));
#139398=CARTESIAN_POINT('Ctrl Pts',(-54.5330222905475,-44.4988752343744,
0.));
#139399=CARTESIAN_POINT('Ctrl Pts',(-54.5142283914704,-44.4908030503225,
0.));
#139400=CARTESIAN_POINT('Ctrl Pts',(-54.495490492193,-44.4827314481264,
0.));
#139401=CARTESIAN_POINT('Ctrl Pts',(-54.4768087248824,-44.4746605784031,
0.));
#139402=CARTESIAN_POINT('Ctrl Pts',(-54.4581832262033,-44.4665905967668,
0.));
#139403=CARTESIAN_POINT('Ctrl Pts',(-54.4396141336978,-44.4585216599907,
0.));
#139404=CARTESIAN_POINT('Ctrl Pts',(-54.421101582595,-44.4504539226327,
0.));
#139405=CARTESIAN_POINT('Ctrl Pts',(-54.4026457030335,-44.4423875340995,
0.));
#139406=CARTESIAN_POINT('Ctrl Pts',(-54.3842466156196,-44.4343226339592,
0.));
#139407=CARTESIAN_POINT('Ctrl Pts',(-54.3659044357119,-44.4262593564712,
0.));
#139408=CARTESIAN_POINT('Ctrl Pts',(-54.3476192819352,-44.4181978395851,
0.));
#139409=CARTESIAN_POINT('Ctrl Pts',(-54.3293912830237,-44.4101382321834,
0.));
#139410=CARTESIAN_POINT('Ctrl Pts',(-54.3112205860716,-44.402080702809,
0.));
#139411=CARTESIAN_POINT('Ctrl Pts',(-54.2931073621553,-44.3940254456331,
0.));
#139412=CARTESIAN_POINT('Ctrl Pts',(-54.2750517888579,-44.3859726620183,
0.));
#139413=CARTESIAN_POINT('Ctrl Pts',(-54.2570540336475,-44.3779225430405,
0.));
#139414=CARTESIAN_POINT('Ctrl Pts',(-54.2391142386412,-44.3698752533561,
0.));
#139415=CARTESIAN_POINT('Ctrl Pts',(-54.2212325006052,-44.361830910343,
0.));
#139416=CARTESIAN_POINT('Ctrl Pts',(-54.2034088701928,-44.3537895824096,
0.));
#139417=CARTESIAN_POINT('Ctrl Pts',(-54.1891964684727,-44.3473589597726,
0.));
#139418=CARTESIAN_POINT('Ctrl Pts',(-54.1785633257639,-44.3425373700993,
0.));
#139419=CARTESIAN_POINT('Ctrl Pts',(-54.1714861895346,-44.3393235891075,
0.));
#139420=CARTESIAN_POINT('Ctrl Pts',(-54.1679505278134,-44.3377168516418,
0.));
#139421=CARTESIAN_POINT('Ctrl Pts',(-62.494763006804,-40.5543412808469,
0.));
#139422=CARTESIAN_POINT('Ctrl Pts',(-62.494763006804,-40.5543412808469,
12.));
#139423=CARTESIAN_POINT('Ctrl Pts',(-62.489224912198,-40.5535399497519,
0.));
#139424=CARTESIAN_POINT('Ctrl Pts',(-62.489224912198,-40.5535399497519,
12.));
#139425=CARTESIAN_POINT('Ctrl Pts',(-62.4781525156318,-40.5519353177252,
0.));
#139426=CARTESIAN_POINT('Ctrl Pts',(-62.4781525156318,-40.5519353177252,
12.));
#139427=CARTESIAN_POINT('Ctrl Pts',(-62.4615552987202,-40.5495224601758,
0.));
#139428=CARTESIAN_POINT('Ctrl Pts',(-62.4615552987202,-40.5495224601758,
12.));
#139429=CARTESIAN_POINT('Ctrl Pts',(-62.4394484329678,-40.5462934972718,
0.));
#139430=CARTESIAN_POINT('Ctrl Pts',(-62.4394484329678,-40.5462934972718,
12.));
#139431=CARTESIAN_POINT('Ctrl Pts',(-62.4118527881148,-40.5422375945026,
0.));
#139432=CARTESIAN_POINT('Ctrl Pts',(-62.4118527881148,-40.5422375945026,
12.));
#139433=CARTESIAN_POINT('Ctrl Pts',(-62.3842950992833,-40.5381619974169,
0.));
#139434=CARTESIAN_POINT('Ctrl Pts',(-62.3842950992833,-40.5381619974169,
12.));
#139435=CARTESIAN_POINT('Ctrl Pts',(-62.3567753970279,-40.5340667194319,
0.));
#139436=CARTESIAN_POINT('Ctrl Pts',(-62.3567753970279,-40.5340667194319,
12.));
#139437=CARTESIAN_POINT('Ctrl Pts',(-62.3292937257902,-40.5299517857721,
0.));
#139438=CARTESIAN_POINT('Ctrl Pts',(-62.3292937257902,-40.5299517857721,
12.));
#139439=CARTESIAN_POINT('Ctrl Pts',(-62.301850147165,-40.5258172381428,
0.));
#139440=CARTESIAN_POINT('Ctrl Pts',(-62.301850147165,-40.5258172381428,
12.));
#139441=CARTESIAN_POINT('Ctrl Pts',(-62.2744447381971,-40.5216631336193,
0.));
#139442=CARTESIAN_POINT('Ctrl Pts',(-62.2744447381971,-40.5216631336193,
12.));
#139443=CARTESIAN_POINT('Ctrl Pts',(-62.247077585866,-40.5174895390954,
0.));
#139444=CARTESIAN_POINT('Ctrl Pts',(-62.247077585866,-40.5174895390954,
12.));
#139445=CARTESIAN_POINT('Ctrl Pts',(-62.2197487826136,-40.5132965269633,
0.));
#139446=CARTESIAN_POINT('Ctrl Pts',(-62.2197487826136,-40.5132965269633,
12.));
#139447=CARTESIAN_POINT('Ctrl Pts',(-62.1924584215653,-40.5090841704122,
0.));
#139448=CARTESIAN_POINT('Ctrl Pts',(-62.1924584215653,-40.5090841704122,
12.));
#139449=CARTESIAN_POINT('Ctrl Pts',(-62.1652065915808,-40.5048525386035,
0.));
#139450=CARTESIAN_POINT('Ctrl Pts',(-62.1652065915808,-40.5048525386035,
12.));
#139451=CARTESIAN_POINT('Ctrl Pts',(-62.1379933732528,-40.5006016927554,
0.));
#139452=CARTESIAN_POINT('Ctrl Pts',(-62.1379933732528,-40.5006016927554,
12.));
#139453=CARTESIAN_POINT('Ctrl Pts',(-62.1108188417004,-40.4963316888412,
0.));
#139454=CARTESIAN_POINT('Ctrl Pts',(-62.1108188417004,-40.4963316888412,
12.));
#139455=CARTESIAN_POINT('Ctrl Pts',(-62.083683068572,-40.4920425795216,
0.));
#139456=CARTESIAN_POINT('Ctrl Pts',(-62.083683068572,-40.4920425795216,
12.));
#139457=CARTESIAN_POINT('Ctrl Pts',(-62.0565861244179,-40.4877344164411,
0.));
#139458=CARTESIAN_POINT('Ctrl Pts',(-62.0565861244179,-40.4877344164411,
12.));
#139459=CARTESIAN_POINT('Ctrl Pts',(-62.029528080742,-40.4834072522164,
0.));
#139460=CARTESIAN_POINT('Ctrl Pts',(-62.029528080742,-40.4834072522164,
12.));
#139461=CARTESIAN_POINT('Ctrl Pts',(-62.0025090125959,-40.4790611429583,
0.));
#139462=CARTESIAN_POINT('Ctrl Pts',(-62.0025090125959,-40.4790611429583,
12.));
#139463=CARTESIAN_POINT('Ctrl Pts',(-61.9755289983044,-40.4746961480015,
0.));
#139464=CARTESIAN_POINT('Ctrl Pts',(-61.9755289983044,-40.4746961480015,
12.));
#139465=CARTESIAN_POINT('Ctrl Pts',(-61.9485881182921,-40.470312328762,
0.));
#139466=CARTESIAN_POINT('Ctrl Pts',(-61.9485881182921,-40.470312328762,
12.));
#139467=CARTESIAN_POINT('Ctrl Pts',(-61.9216864541744,-40.4659097478587,
0.));
#139468=CARTESIAN_POINT('Ctrl Pts',(-61.9216864541744,-40.4659097478587,
12.));
#139469=CARTESIAN_POINT('Ctrl Pts',(-61.8948240878008,-40.4614884681889,
0.));
#139470=CARTESIAN_POINT('Ctrl Pts',(-61.8948240878008,-40.4614884681889,
12.));
#139471=CARTESIAN_POINT('Ctrl Pts',(-61.8680011001537,-40.4570485518749,
0.));
#139472=CARTESIAN_POINT('Ctrl Pts',(-61.8680011001537,-40.4570485518749,
12.));
#139473=CARTESIAN_POINT('Ctrl Pts',(-61.8412175708553,-40.4525900597894,
0.));
#139474=CARTESIAN_POINT('Ctrl Pts',(-61.8412175708553,-40.4525900597894,
12.));
#139475=CARTESIAN_POINT('Ctrl Pts',(-61.814473578779,-40.4481130521364,
0.));
#139476=CARTESIAN_POINT('Ctrl Pts',(-61.814473578779,-40.4481130521364,
12.));
#139477=CARTESIAN_POINT('Ctrl Pts',(-61.7877692024076,-40.4436175887949,
0.));
#139478=CARTESIAN_POINT('Ctrl Pts',(-61.7877692024076,-40.4436175887949,
12.));
#139479=CARTESIAN_POINT('Ctrl Pts',(-61.7611045202874,-40.4391037297588,
0.));
#139480=CARTESIAN_POINT('Ctrl Pts',(-61.7611045202874,-40.4391037297588,
12.));
#139481=CARTESIAN_POINT('Ctrl Pts',(-61.7344796114399,-40.4345715355404,
0.));
#139482=CARTESIAN_POINT('Ctrl Pts',(-61.7344796114399,-40.4345715355404,
12.));
#139483=CARTESIAN_POINT('Ctrl Pts',(-61.7078945557799,-40.430021067584,
0.));
#139484=CARTESIAN_POINT('Ctrl Pts',(-61.7078945557799,-40.430021067584,
12.));
#139485=CARTESIAN_POINT('Ctrl Pts',(-61.6813494339286,-40.425452388076,
0.));
#139486=CARTESIAN_POINT('Ctrl Pts',(-61.6813494339286,-40.425452388076,
12.));
#139487=CARTESIAN_POINT('Ctrl Pts',(-61.6548443270394,-40.4208655597717,
0.));
#139488=CARTESIAN_POINT('Ctrl Pts',(-61.6548443270394,-40.4208655597717,
12.));
#139489=CARTESIAN_POINT('Ctrl Pts',(-61.628379316608,-40.4162606458118,
0.));
#139490=CARTESIAN_POINT('Ctrl Pts',(-61.628379316608,-40.4162606458118,
12.));
#139491=CARTESIAN_POINT('Ctrl Pts',(-61.6019544843011,-40.4116377095596,
0.));
#139492=CARTESIAN_POINT('Ctrl Pts',(-61.6019544843011,-40.4116377095596,
12.));
#139493=CARTESIAN_POINT('Ctrl Pts',(-61.5755699117324,-40.4069968143956,
0.));
#139494=CARTESIAN_POINT('Ctrl Pts',(-61.5755699117324,-40.4069968143956,
12.));
#139495=CARTESIAN_POINT('Ctrl Pts',(-61.5492256804717,-40.4023380237232,
0.));
#139496=CARTESIAN_POINT('Ctrl Pts',(-61.5492256804717,-40.4023380237232,
12.));
#139497=CARTESIAN_POINT('Ctrl Pts',(-61.522921872154,-40.3976614010652,
0.));
#139498=CARTESIAN_POINT('Ctrl Pts',(-61.522921872154,-40.3976614010652,
12.));
#139499=CARTESIAN_POINT('Ctrl Pts',(-61.4966585685549,-40.3929670101365,
0.));
#139500=CARTESIAN_POINT('Ctrl Pts',(-61.4966585685549,-40.3929670101365,
12.));
#139501=CARTESIAN_POINT('Ctrl Pts',(-61.4704358516709,-40.3882549149227,
0.));
#139502=CARTESIAN_POINT('Ctrl Pts',(-61.4704358516709,-40.3882549149227,
12.));
#139503=CARTESIAN_POINT('Ctrl Pts',(-61.4442538038044,-40.383525179772,
0.));
#139504=CARTESIAN_POINT('Ctrl Pts',(-61.4442538038044,-40.383525179772,
12.));
#139505=CARTESIAN_POINT('Ctrl Pts',(-61.4181125076037,-40.3787778694364,
0.));
#139506=CARTESIAN_POINT('Ctrl Pts',(-61.4181125076037,-40.3787778694364,
12.));
#139507=CARTESIAN_POINT('Ctrl Pts',(-61.3920120460219,-40.3740130490225,
0.));
#139508=CARTESIAN_POINT('Ctrl Pts',(-61.3920120460219,-40.3740130490225,
12.));
#139509=CARTESIAN_POINT('Ctrl Pts',(-61.3659525022908,-40.3692307839636,
0.));
#139510=CARTESIAN_POINT('Ctrl Pts',(-61.3659525022908,-40.3692307839636,
12.));
#139511=CARTESIAN_POINT('Ctrl Pts',(-61.3399339598853,-40.3644311399861,
0.));
#139512=CARTESIAN_POINT('Ctrl Pts',(-61.3399339598853,-40.3644311399861,
12.));
#139513=CARTESIAN_POINT('Ctrl Pts',(-61.3139565024847,-40.3596141830791,
0.));
#139514=CARTESIAN_POINT('Ctrl Pts',(-61.3139565024847,-40.3596141830791,
12.));
#139515=CARTESIAN_POINT('Ctrl Pts',(-61.2880202139371,-40.3547799794679,
0.));
#139516=CARTESIAN_POINT('Ctrl Pts',(-61.2880202139371,-40.3547799794679,
12.));
#139517=CARTESIAN_POINT('Ctrl Pts',(-61.2621251782863,-40.3499285956304,
0.));
#139518=CARTESIAN_POINT('Ctrl Pts',(-61.2621251782863,-40.3499285956304,
12.));
#139519=CARTESIAN_POINT('Ctrl Pts',(-61.23627147979,-40.3450600983109,0.));
#139520=CARTESIAN_POINT('Ctrl Pts',(-61.23627147979,-40.3450600983109,12.));
#139521=CARTESIAN_POINT('Ctrl Pts',(-61.2104592029377,-40.340174554537,
0.));
#139522=CARTESIAN_POINT('Ctrl Pts',(-61.2104592029377,-40.340174554537,
12.));
#139523=CARTESIAN_POINT('Ctrl Pts',(-61.1846884324644,-40.335272031637,
0.));
#139524=CARTESIAN_POINT('Ctrl Pts',(-61.1846884324644,-40.335272031637,
12.));
#139525=CARTESIAN_POINT('Ctrl Pts',(-61.1589592533613,-40.3303525972615,
0.));
#139526=CARTESIAN_POINT('Ctrl Pts',(-61.1589592533613,-40.3303525972615,
12.));
#139527=CARTESIAN_POINT('Ctrl Pts',(-61.1332717508789,-40.32541631938,0.));
#139528=CARTESIAN_POINT('Ctrl Pts',(-61.1332717508789,-40.32541631938,12.));
#139529=CARTESIAN_POINT('Ctrl Pts',(-61.1076260105258,-40.3204632662725,
0.));
#139530=CARTESIAN_POINT('Ctrl Pts',(-61.1076260105258,-40.3204632662725,
12.));
#139531=CARTESIAN_POINT('Ctrl Pts',(-61.0820221180645,-40.3154935065262,
0.));
#139532=CARTESIAN_POINT('Ctrl Pts',(-61.0820221180645,-40.3154935065262,
12.));
#139533=CARTESIAN_POINT('Ctrl Pts',(-61.056460159505,-40.3105071090309,
0.));
#139534=CARTESIAN_POINT('Ctrl Pts',(-61.056460159505,-40.3105071090309,
12.));
#139535=CARTESIAN_POINT('Ctrl Pts',(-61.0309402210921,-40.3055041429775,
0.));
#139536=CARTESIAN_POINT('Ctrl Pts',(-61.0309402210921,-40.3055041429775,
12.));
#139537=CARTESIAN_POINT('Ctrl Pts',(-61.0054623893066,-40.300484677858,
0.));
#139538=CARTESIAN_POINT('Ctrl Pts',(-61.0054623893066,-40.300484677858,
12.));
#139539=CARTESIAN_POINT('Ctrl Pts',(-60.9800267508787,-40.295448783469,
0.));
#139540=CARTESIAN_POINT('Ctrl Pts',(-60.9800267508787,-40.295448783469,
12.));
#139541=CARTESIAN_POINT('Ctrl Pts',(-60.9546333927921,-40.2903965299155,
0.));
#139542=CARTESIAN_POINT('Ctrl Pts',(-60.9546333927921,-40.2903965299155,
12.));
#139543=CARTESIAN_POINT('Ctrl Pts',(-60.9292824022887,-40.2853279876161,
0.));
#139544=CARTESIAN_POINT('Ctrl Pts',(-60.9292824022887,-40.2853279876161,
12.));
#139545=CARTESIAN_POINT('Ctrl Pts',(-60.9039738668669,-40.2802432273104,
0.));
#139546=CARTESIAN_POINT('Ctrl Pts',(-60.9039738668669,-40.2802432273104,
12.));
#139547=CARTESIAN_POINT('Ctrl Pts',(-60.8787078742818,-40.2751423200639,
0.));
#139548=CARTESIAN_POINT('Ctrl Pts',(-60.8787078742818,-40.2751423200639,
12.));
#139549=CARTESIAN_POINT('Ctrl Pts',(-60.8534845125538,-40.2700253372647,
0.));
#139550=CARTESIAN_POINT('Ctrl Pts',(-60.8534845125538,-40.2700253372647,
12.));
#139551=CARTESIAN_POINT('Ctrl Pts',(-60.8283038699706,-40.2648923506248,
0.));
#139552=CARTESIAN_POINT('Ctrl Pts',(-60.8283038699706,-40.2648923506248,
12.));
#139553=CARTESIAN_POINT('Ctrl Pts',(-60.8031660350879,-40.2597434321803,
0.));
#139554=CARTESIAN_POINT('Ctrl Pts',(-60.8031660350879,-40.2597434321803,
12.));
#139555=CARTESIAN_POINT('Ctrl Pts',(-60.7780710967248,-40.2545786542953,
0.));
#139556=CARTESIAN_POINT('Ctrl Pts',(-60.7780710967248,-40.2545786542953,
12.));
#139557=CARTESIAN_POINT('Ctrl Pts',(-60.7530191439593,-40.2493980896638,
0.));
#139558=CARTESIAN_POINT('Ctrl Pts',(-60.7530191439593,-40.2493980896638,
12.));
#139559=CARTESIAN_POINT('Ctrl Pts',(-60.728010266139,-40.2442018113108,
0.));
#139560=CARTESIAN_POINT('Ctrl Pts',(-60.728010266139,-40.2442018113108,
12.));
#139561=CARTESIAN_POINT('Ctrl Pts',(-60.7030445528857,-40.2389898925932,
0.));
#139562=CARTESIAN_POINT('Ctrl Pts',(-60.7030445528857,-40.2389898925932,
12.));
#139563=CARTESIAN_POINT('Ctrl Pts',(-60.678122094098,-40.2337624072028,
0.));
#139564=CARTESIAN_POINT('Ctrl Pts',(-60.678122094098,-40.2337624072028,
12.));
#139565=CARTESIAN_POINT('Ctrl Pts',(-60.6532429799499,-40.2285194291706,
0.));
#139566=CARTESIAN_POINT('Ctrl Pts',(-60.6532429799499,-40.2285194291706,
12.));
#139567=CARTESIAN_POINT('Ctrl Pts',(-60.6284073008871,-40.2232610328721,
0.));
#139568=CARTESIAN_POINT('Ctrl Pts',(-60.6284073008871,-40.2232610328721,
12.));
#139569=CARTESIAN_POINT('Ctrl Pts',(-60.6036151476349,-40.2179872930273,
0.));
#139570=CARTESIAN_POINT('Ctrl Pts',(-60.6036151476349,-40.2179872930273,
12.));
#139571=CARTESIAN_POINT('Ctrl Pts',(-60.5788666112042,-40.2126982847011,
0.));
#139572=CARTESIAN_POINT('Ctrl Pts',(-60.5788666112042,-40.2126982847011,
12.));
#139573=CARTESIAN_POINT('Ctrl Pts',(-60.5541617828925,-40.2073940833052,
0.));
#139574=CARTESIAN_POINT('Ctrl Pts',(-60.5541617828925,-40.2073940833052,
12.));
#139575=CARTESIAN_POINT('Ctrl Pts',(-60.5295007542841,-40.2020747646014,
0.));
#139576=CARTESIAN_POINT('Ctrl Pts',(-60.5295007542841,-40.2020747646014,
12.));
#139577=CARTESIAN_POINT('Ctrl Pts',(-60.5048836172435,-40.1967404047062,
0.));
#139578=CARTESIAN_POINT('Ctrl Pts',(-60.5048836172435,-40.1967404047062,
12.));
#139579=CARTESIAN_POINT('Ctrl Pts',(-60.4803104639226,-40.1913910800921,
0.));
#139580=CARTESIAN_POINT('Ctrl Pts',(-60.4803104639226,-40.1913910800921,
12.));
#139581=CARTESIAN_POINT('Ctrl Pts',(-60.455781386769,-40.1860268675883,
0.));
#139582=CARTESIAN_POINT('Ctrl Pts',(-60.455781386769,-40.1860268675883,
12.));
#139583=CARTESIAN_POINT('Ctrl Pts',(-60.4312964785273,-40.180647844383,
0.));
#139584=CARTESIAN_POINT('Ctrl Pts',(-60.4312964785273,-40.180647844383,
12.));
#139585=CARTESIAN_POINT('Ctrl Pts',(-60.4068558322407,-40.1752540880268,
0.));
#139586=CARTESIAN_POINT('Ctrl Pts',(-60.4068558322407,-40.1752540880268,
12.));
#139587=CARTESIAN_POINT('Ctrl Pts',(-60.3824595412446,-40.1698456764377,
0.));
#139588=CARTESIAN_POINT('Ctrl Pts',(-60.3824595412446,-40.1698456764377,
12.));
#139589=CARTESIAN_POINT('Ctrl Pts',(-60.3581076991716,-40.1644226879033,
0.));
#139590=CARTESIAN_POINT('Ctrl Pts',(-60.3581076991716,-40.1644226879033,
12.));
#139591=CARTESIAN_POINT('Ctrl Pts',(-60.3338003999607,-40.1589852010804,
0.));
#139592=CARTESIAN_POINT('Ctrl Pts',(-60.3338003999607,-40.1589852010804,
12.));
#139593=CARTESIAN_POINT('Ctrl Pts',(-60.3095377378586,-40.1535332949976,
0.));
#139594=CARTESIAN_POINT('Ctrl Pts',(-60.3095377378586,-40.1535332949976,
12.));
#139595=CARTESIAN_POINT('Ctrl Pts',(-60.285319807422,-40.1480670490585,
0.));
#139596=CARTESIAN_POINT('Ctrl Pts',(-60.285319807422,-40.1480670490585,
12.));
#139597=CARTESIAN_POINT('Ctrl Pts',(-60.2611467035117,-40.1425865430472,
0.));
#139598=CARTESIAN_POINT('Ctrl Pts',(-60.2611467035117,-40.1425865430472,
12.));
#139599=CARTESIAN_POINT('Ctrl Pts',(-60.2370185212965,-40.1370918571304,
0.));
#139600=CARTESIAN_POINT('Ctrl Pts',(-60.2370185212965,-40.1370918571304,
12.));
#139601=CARTESIAN_POINT('Ctrl Pts',(-60.2129353562622,-40.1315830718577,
0.));
#139602=CARTESIAN_POINT('Ctrl Pts',(-60.2129353562622,-40.1315830718577,
12.));
#139603=CARTESIAN_POINT('Ctrl Pts',(-60.1888973042152,-40.1260602681644,
0.));
#139604=CARTESIAN_POINT('Ctrl Pts',(-60.1888973042152,-40.1260602681644,
12.));
#139605=CARTESIAN_POINT('Ctrl Pts',(-60.1649044612828,-40.1205235273739,
0.));
#139606=CARTESIAN_POINT('Ctrl Pts',(-60.1649044612828,-40.1205235273739,
12.));
#139607=CARTESIAN_POINT('Ctrl Pts',(-60.1409569239092,-40.1149729312036,
0.));
#139608=CARTESIAN_POINT('Ctrl Pts',(-60.1409569239092,-40.1149729312036,
12.));
#139609=CARTESIAN_POINT('Ctrl Pts',(-60.1170547888574,-40.1094085617674,
0.));
#139610=CARTESIAN_POINT('Ctrl Pts',(-60.1170547888574,-40.1094085617674,
12.));
#139611=CARTESIAN_POINT('Ctrl Pts',(-60.0931981532198,-40.1038305015766,
0.));
#139612=CARTESIAN_POINT('Ctrl Pts',(-60.0931981532198,-40.1038305015766,
12.));
#139613=CARTESIAN_POINT('Ctrl Pts',(-60.069387114421,-40.0982388335423,
0.));
#139614=CARTESIAN_POINT('Ctrl Pts',(-60.069387114421,-40.0982388335423,
12.));
#139615=CARTESIAN_POINT('Ctrl Pts',(-60.0456217702202,-40.0926336409785,
0.));
#139616=CARTESIAN_POINT('Ctrl Pts',(-60.0456217702202,-40.0926336409785,
12.));
#139617=CARTESIAN_POINT('Ctrl Pts',(-60.021902218706,-40.0870150076073,
0.));
#139618=CARTESIAN_POINT('Ctrl Pts',(-60.021902218706,-40.0870150076073,
12.));
#139619=CARTESIAN_POINT('Ctrl Pts',(-59.9982285582983,-40.0813830175623,
0.));
#139620=CARTESIAN_POINT('Ctrl Pts',(-59.9982285582983,-40.0813830175623,
12.));
#139621=CARTESIAN_POINT('Ctrl Pts',(-59.9746008877584,-40.0757377553888,
0.));
#139622=CARTESIAN_POINT('Ctrl Pts',(-59.9746008877584,-40.0757377553888,
12.));
#139623=CARTESIAN_POINT('Ctrl Pts',(-59.9510193061927,-40.0700793060473,
0.));
#139624=CARTESIAN_POINT('Ctrl Pts',(-59.9510193061927,-40.0700793060473,
12.));
#139625=CARTESIAN_POINT('Ctrl Pts',(-59.9274839130553,-40.0644077549159,
0.));
#139626=CARTESIAN_POINT('Ctrl Pts',(-59.9274839130553,-40.0644077549159,
12.));
#139627=CARTESIAN_POINT('Ctrl Pts',(-59.9039948081432,-40.0587231877961,
0.));
#139628=CARTESIAN_POINT('Ctrl Pts',(-59.9039948081432,-40.0587231877961,
12.));
#139629=CARTESIAN_POINT('Ctrl Pts',(-59.8805520915975,-40.0530256909162,
0.));
#139630=CARTESIAN_POINT('Ctrl Pts',(-59.8805520915975,-40.0530256909162,
12.));
#139631=CARTESIAN_POINT('Ctrl Pts',(-59.8571558639145,-40.0473153509323,
0.));
#139632=CARTESIAN_POINT('Ctrl Pts',(-59.8571558639145,-40.0473153509323,
12.));
#139633=CARTESIAN_POINT('Ctrl Pts',(-59.8338062259491,-40.0415922549313,
0.));
#139634=CARTESIAN_POINT('Ctrl Pts',(-59.8338062259491,-40.0415922549313,
12.));
#139635=CARTESIAN_POINT('Ctrl Pts',(-59.8105032789179,-40.035856490434,
0.));
#139636=CARTESIAN_POINT('Ctrl Pts',(-59.8105032789179,-40.035856490434,
12.));
#139637=CARTESIAN_POINT('Ctrl Pts',(-59.7872471243948,-40.0301081454006,
0.));
#139638=CARTESIAN_POINT('Ctrl Pts',(-59.7872471243948,-40.0301081454006,
12.));
#139639=CARTESIAN_POINT('Ctrl Pts',(-59.7640378643115,-40.0243473082343,
0.));
#139640=CARTESIAN_POINT('Ctrl Pts',(-59.7640378643115,-40.0243473082343,
12.));
#139641=CARTESIAN_POINT('Ctrl Pts',(-59.7408756009688,-40.0185740677827,
0.));
#139642=CARTESIAN_POINT('Ctrl Pts',(-59.7408756009688,-40.0185740677827,
12.));
#139643=CARTESIAN_POINT('Ctrl Pts',(-59.7177604370409,-40.0127885133407,
0.));
#139644=CARTESIAN_POINT('Ctrl Pts',(-59.7177604370409,-40.0127885133407,
12.));
#139645=CARTESIAN_POINT('Ctrl Pts',(-59.6946924755771,-40.0069907346536,
0.));
#139646=CARTESIAN_POINT('Ctrl Pts',(-59.6946924755771,-40.0069907346536,
12.));
#139647=CARTESIAN_POINT('Ctrl Pts',(-59.671671819999,-40.001180821923,0.));
#139648=CARTESIAN_POINT('Ctrl Pts',(-59.671671819999,-40.001180821923,12.));
#139649=CARTESIAN_POINT('Ctrl Pts',(-59.6486985741015,-39.9953588658114,
0.));
#139650=CARTESIAN_POINT('Ctrl Pts',(-59.6486985741015,-39.9953588658114,
12.));
#139651=CARTESIAN_POINT('Ctrl Pts',(-59.6257728420644,-39.9895249574432,
0.));
#139652=CARTESIAN_POINT('Ctrl Pts',(-59.6257728420644,-39.9895249574432,
12.));
#139653=CARTESIAN_POINT('Ctrl Pts',(-59.6028947284551,-39.9836791884071,
0.));
#139654=CARTESIAN_POINT('Ctrl Pts',(-59.6028947284551,-39.9836791884071,
12.));
#139655=CARTESIAN_POINT('Ctrl Pts',(-59.5800643382322,-39.9778216507609,
0.));
#139656=CARTESIAN_POINT('Ctrl Pts',(-59.5800643382322,-39.9778216507609,
12.));
#139657=CARTESIAN_POINT('Ctrl Pts',(-59.5572817767412,-39.971952437036,
0.));
#139658=CARTESIAN_POINT('Ctrl Pts',(-59.5572817767412,-39.971952437036,
12.));
#139659=CARTESIAN_POINT('Ctrl Pts',(-59.5345471497162,-39.9660716402423,
0.));
#139660=CARTESIAN_POINT('Ctrl Pts',(-59.5345471497162,-39.9660716402423,
12.));
#139661=CARTESIAN_POINT('Ctrl Pts',(-59.511860563292,-39.96017935387,0.));
#139662=CARTESIAN_POINT('Ctrl Pts',(-59.511860563292,-39.96017935387,12.));
#139663=CARTESIAN_POINT('Ctrl Pts',(-59.4892221240082,-39.954275671893,
0.));
#139664=CARTESIAN_POINT('Ctrl Pts',(-59.4892221240082,-39.954275671893,
12.));
#139665=CARTESIAN_POINT('Ctrl Pts',(-59.4666319388123,-39.9483606887731,
0.));
#139666=CARTESIAN_POINT('Ctrl Pts',(-59.4666319388123,-39.9483606887731,
12.));
#139667=CARTESIAN_POINT('Ctrl Pts',(-59.444090115055,-39.9424344994652,
0.));
#139668=CARTESIAN_POINT('Ctrl Pts',(-59.444090115055,-39.9424344994652,
12.));
#139669=CARTESIAN_POINT('Ctrl Pts',(-59.4215967604925,-39.9364971994215,
0.));
#139670=CARTESIAN_POINT('Ctrl Pts',(-59.4215967604925,-39.9364971994215,
12.));
#139671=CARTESIAN_POINT('Ctrl Pts',(-59.3991519832981,-39.9305488845934,
0.));
#139672=CARTESIAN_POINT('Ctrl Pts',(-59.3991519832981,-39.9305488845934,
12.));
#139673=CARTESIAN_POINT('Ctrl Pts',(-59.3767558920663,-39.9245896514359,
0.));
#139674=CARTESIAN_POINT('Ctrl Pts',(-59.3767558920663,-39.9245896514359,
12.));
#139675=CARTESIAN_POINT('Ctrl Pts',(-59.3544085958165,-39.9186195969113,
0.));
#139676=CARTESIAN_POINT('Ctrl Pts',(-59.3544085958165,-39.9186195969113,
12.));
#139677=CARTESIAN_POINT('Ctrl Pts',(-59.3321102039883,-39.9126388184956,
0.));
#139678=CARTESIAN_POINT('Ctrl Pts',(-59.3321102039883,-39.9126388184956,
12.));
#139679=CARTESIAN_POINT('Ctrl Pts',(-59.3098608264452,-39.9066474141826,
0.));
#139680=CARTESIAN_POINT('Ctrl Pts',(-59.3098608264452,-39.9066474141826,
12.));
#139681=CARTESIAN_POINT('Ctrl Pts',(-59.2876605734871,-39.9006454824861,
0.));
#139682=CARTESIAN_POINT('Ctrl Pts',(-59.2876605734871,-39.9006454824861,
12.));
#139683=CARTESIAN_POINT('Ctrl Pts',(-59.2655095558527,-39.8946331224442,
0.));
#139684=CARTESIAN_POINT('Ctrl Pts',(-59.2655095558527,-39.8946331224442,
12.));
#139685=CARTESIAN_POINT('Ctrl Pts',(-59.2434078847236,-39.8886104336234,
0.));
#139686=CARTESIAN_POINT('Ctrl Pts',(-59.2434078847236,-39.8886104336234,
12.));
#139687=CARTESIAN_POINT('Ctrl Pts',(-59.2213556717189,-39.8825775161252,
0.));
#139688=CARTESIAN_POINT('Ctrl Pts',(-59.2213556717189,-39.8825775161252,
12.));
#139689=CARTESIAN_POINT('Ctrl Pts',(-59.1993530289008,-39.8765344705894,
0.));
#139690=CARTESIAN_POINT('Ctrl Pts',(-59.1993530289008,-39.8765344705894,
12.));
#139691=CARTESIAN_POINT('Ctrl Pts',(-59.1774000687865,-39.8704813981978,
0.));
#139692=CARTESIAN_POINT('Ctrl Pts',(-59.1774000687865,-39.8704813981978,
12.));
#139693=CARTESIAN_POINT('Ctrl Pts',(-59.155496904352,-39.8644184006785,
0.));
#139694=CARTESIAN_POINT('Ctrl Pts',(-59.155496904352,-39.8644184006785,
12.));
#139695=CARTESIAN_POINT('Ctrl Pts',(-59.133643649035,-39.8583455803111,
0.));
#139696=CARTESIAN_POINT('Ctrl Pts',(-59.133643649035,-39.8583455803111,
12.));
#139697=CARTESIAN_POINT('Ctrl Pts',(-59.1118404167304,-39.8522630399337,
0.));
#139698=CARTESIAN_POINT('Ctrl Pts',(-59.1118404167304,-39.8522630399337,
12.));
#139699=CARTESIAN_POINT('Ctrl Pts',(-59.0900873217993,-39.8461708829465,
0.));
#139700=CARTESIAN_POINT('Ctrl Pts',(-59.0900873217993,-39.8461708829465,
12.));
#139701=CARTESIAN_POINT('Ctrl Pts',(-59.068384479077,-39.8400692133143,
0.));
#139702=CARTESIAN_POINT('Ctrl Pts',(-59.068384479077,-39.8400692133143,
12.));
#139703=CARTESIAN_POINT('Ctrl Pts',(-59.0467320038783,-39.8339581355714,
0.));
#139704=CARTESIAN_POINT('Ctrl Pts',(-59.0467320038783,-39.8339581355714,
12.));
#139705=CARTESIAN_POINT('Ctrl Pts',(-59.0251300119973,-39.8278377548261,
0.));
#139706=CARTESIAN_POINT('Ctrl Pts',(-59.0251300119973,-39.8278377548261,
12.));
#139707=CARTESIAN_POINT('Ctrl Pts',(-59.0035786197024,-39.8217081767658,
0.));
#139708=CARTESIAN_POINT('Ctrl Pts',(-59.0035786197024,-39.8217081767658,
12.));
#139709=CARTESIAN_POINT('Ctrl Pts',(-58.9820779437485,-39.8155695076624,
0.));
#139710=CARTESIAN_POINT('Ctrl Pts',(-58.9820779437485,-39.8155695076624,
12.));
#139711=CARTESIAN_POINT('Ctrl Pts',(-58.9606281013876,-39.8094218543781,
0.));
#139712=CARTESIAN_POINT('Ctrl Pts',(-58.9606281013876,-39.8094218543781,
12.));
#139713=CARTESIAN_POINT('Ctrl Pts',(-58.9392292103747,-39.8032653243712,
0.));
#139714=CARTESIAN_POINT('Ctrl Pts',(-58.9392292103747,-39.8032653243712,
12.));
#139715=CARTESIAN_POINT('Ctrl Pts',(-58.9178813889703,-39.7971000257044,
0.));
#139716=CARTESIAN_POINT('Ctrl Pts',(-58.9178813889703,-39.7971000257044,
12.));
#139717=CARTESIAN_POINT('Ctrl Pts',(-58.896584755939,-39.7909260670517,
0.));
#139718=CARTESIAN_POINT('Ctrl Pts',(-58.896584755939,-39.7909260670517,
12.));
#139719=CARTESIAN_POINT('Ctrl Pts',(-58.8753394305583,-39.7847435576995,
0.));
#139720=CARTESIAN_POINT('Ctrl Pts',(-58.8753394305583,-39.7847435576995,
12.));
#139721=CARTESIAN_POINT('Ctrl Pts',(-58.8541455326229,-39.7785526075477,
0.));
#139722=CARTESIAN_POINT('Ctrl Pts',(-58.8541455326229,-39.7785526075477,
12.));
#139723=CARTESIAN_POINT('Ctrl Pts',(-58.8330031824453,-39.772353327112,
0.));
#139724=CARTESIAN_POINT('Ctrl Pts',(-58.8330031824453,-39.772353327112,
12.));
#139725=CARTESIAN_POINT('Ctrl Pts',(-58.8119125008521,-39.7661458275276,
0.));
#139726=CARTESIAN_POINT('Ctrl Pts',(-58.8119125008521,-39.7661458275276,
12.));
#139727=CARTESIAN_POINT('Ctrl Pts',(-58.7908736091808,-39.7599302205527,
0.));
#139728=CARTESIAN_POINT('Ctrl Pts',(-58.7908736091808,-39.7599302205527,
12.));
#139729=CARTESIAN_POINT('Ctrl Pts',(-58.7698866293041,-39.753706618582,
0.));
#139730=CARTESIAN_POINT('Ctrl Pts',(-58.7698866293041,-39.753706618582,
12.));
#139731=CARTESIAN_POINT('Ctrl Pts',(-58.7489516836453,-39.7474751346603,
0.));
#139732=CARTESIAN_POINT('Ctrl Pts',(-58.7489516836453,-39.7474751346603,
12.));
#139733=CARTESIAN_POINT('Ctrl Pts',(-58.7280688951911,-39.7412358824949,
0.));
#139734=CARTESIAN_POINT('Ctrl Pts',(-58.7280688951911,-39.7412358824949,
12.));
#139735=CARTESIAN_POINT('Ctrl Pts',(-58.7072383875009,-39.7349889764737,
0.));
#139736=CARTESIAN_POINT('Ctrl Pts',(-58.7072383875009,-39.7349889764737,
12.));
#139737=CARTESIAN_POINT('Ctrl Pts',(-58.6864602847065,-39.7287345316664,
0.));
#139738=CARTESIAN_POINT('Ctrl Pts',(-58.6864602847065,-39.7287345316664,
12.));
#139739=CARTESIAN_POINT('Ctrl Pts',(-58.6657347115015,-39.7224726638087,
0.));
#139740=CARTESIAN_POINT('Ctrl Pts',(-58.6657347115015,-39.7224726638087,
12.));
#139741=CARTESIAN_POINT('Ctrl Pts',(-58.6450617931269,-39.7162034892896,
0.));
#139742=CARTESIAN_POINT('Ctrl Pts',(-58.6450617931269,-39.7162034892896,
12.));
#139743=CARTESIAN_POINT('Ctrl Pts',(-58.6244416553574,-39.7099271251421,
0.));
#139744=CARTESIAN_POINT('Ctrl Pts',(-58.6244416553574,-39.7099271251421,
12.));
#139745=CARTESIAN_POINT('Ctrl Pts',(-58.6038744244683,-39.7036436890248,
0.));
#139746=CARTESIAN_POINT('Ctrl Pts',(-58.6038744244683,-39.7036436890248,
12.));
#139747=CARTESIAN_POINT('Ctrl Pts',(-58.5833602272767,-39.6973532992555,
0.));
#139748=CARTESIAN_POINT('Ctrl Pts',(-58.5833602272767,-39.6973532992555,
12.));
#139749=CARTESIAN_POINT('Ctrl Pts',(-58.5628991912067,-39.6910560748639,
0.));
#139750=CARTESIAN_POINT('Ctrl Pts',(-58.5628991912067,-39.6910560748639,
12.));
#139751=CARTESIAN_POINT('Ctrl Pts',(-58.5424914443415,-39.6847521356395,
0.));
#139752=CARTESIAN_POINT('Ctrl Pts',(-58.5424914443415,-39.6847521356395,
12.));
#139753=CARTESIAN_POINT('Ctrl Pts',(-58.5221371154748,-39.6784416021817,
0.));
#139754=CARTESIAN_POINT('Ctrl Pts',(-58.5221371154748,-39.6784416021817,
12.));
#139755=CARTESIAN_POINT('Ctrl Pts',(-58.5018363341582,-39.6721245959516,
0.));
#139756=CARTESIAN_POINT('Ctrl Pts',(-58.5018363341582,-39.6721245959516,
12.));
#139757=CARTESIAN_POINT('Ctrl Pts',(-58.4815892306044,-39.66580123918,0.));
#139758=CARTESIAN_POINT('Ctrl Pts',(-58.4815892306044,-39.66580123918,12.));
#139759=CARTESIAN_POINT('Ctrl Pts',(-58.4613959355776,-39.659471654768,
0.));
#139760=CARTESIAN_POINT('Ctrl Pts',(-58.4613959355776,-39.659471654768,
12.));
#139761=CARTESIAN_POINT('Ctrl Pts',(-58.4412565802984,-39.6531359662043,
0.));
#139762=CARTESIAN_POINT('Ctrl Pts',(-58.4412565802984,-39.6531359662043,
12.));
#139763=CARTESIAN_POINT('Ctrl Pts',(-58.4211712963024,-39.6467942974464,
0.));
#139764=CARTESIAN_POINT('Ctrl Pts',(-58.4211712963024,-39.6467942974464,
12.));
#139765=CARTESIAN_POINT('Ctrl Pts',(-58.4011402154225,-39.6404467729113,
0.));
#139766=CARTESIAN_POINT('Ctrl Pts',(-58.4011402154225,-39.6404467729113,
12.));
#139767=CARTESIAN_POINT('Ctrl Pts',(-58.3811634701061,-39.6340935177492,
0.));
#139768=CARTESIAN_POINT('Ctrl Pts',(-58.3811634701061,-39.6340935177492,
12.));
#139769=CARTESIAN_POINT('Ctrl Pts',(-58.3612411936914,-39.6277346580898,
0.));
#139770=CARTESIAN_POINT('Ctrl Pts',(-58.3612411936914,-39.6277346580898,
12.));
#139771=CARTESIAN_POINT('Ctrl Pts',(-58.3413735206412,-39.6213703212522,
0.));
#139772=CARTESIAN_POINT('Ctrl Pts',(-58.3413735206412,-39.6213703212522,
12.));
#139773=CARTESIAN_POINT('Ctrl Pts',(-58.3215605869192,-39.6150006360894,
0.));
#139774=CARTESIAN_POINT('Ctrl Pts',(-58.3215605869192,-39.6150006360894,
12.));
#139775=CARTESIAN_POINT('Ctrl Pts',(-58.3018025297288,-39.6086257327559,
0.));
#139776=CARTESIAN_POINT('Ctrl Pts',(-58.3018025297288,-39.6086257327559,
12.));
#139777=CARTESIAN_POINT('Ctrl Pts',(-58.2820994868092,-39.6022457420772,
0.));
#139778=CARTESIAN_POINT('Ctrl Pts',(-58.2820994868092,-39.6022457420772,
12.));
#139779=CARTESIAN_POINT('Ctrl Pts',(-58.2624515958416,-39.5958607950237,
0.));
#139780=CARTESIAN_POINT('Ctrl Pts',(-58.2624515958416,-39.5958607950237,
12.));
#139781=CARTESIAN_POINT('Ctrl Pts',(-58.2428589938395,-39.5894710221729,
0.));
#139782=CARTESIAN_POINT('Ctrl Pts',(-58.2428589938395,-39.5894710221729,
12.));
#139783=CARTESIAN_POINT('Ctrl Pts',(-58.2233218164408,-39.5830765530919,
0.));
#139784=CARTESIAN_POINT('Ctrl Pts',(-58.2233218164408,-39.5830765530919,
12.));
#139785=CARTESIAN_POINT('Ctrl Pts',(-58.2038401992496,-39.5766775175226,
0.));
#139786=CARTESIAN_POINT('Ctrl Pts',(-58.2038401992496,-39.5766775175226,
12.));
#139787=CARTESIAN_POINT('Ctrl Pts',(-58.1844142794359,-39.5702740468013,
0.));
#139788=CARTESIAN_POINT('Ctrl Pts',(-58.1844142794359,-39.5702740468013,
12.));
#139789=CARTESIAN_POINT('Ctrl Pts',(-58.1650441970379,-39.5638662750174,
0.));
#139790=CARTESIAN_POINT('Ctrl Pts',(-58.1650441970379,-39.5638662750174,
12.));
#139791=CARTESIAN_POINT('Ctrl Pts',(-58.1457300968467,-39.5574543406959,
0.));
#139792=CARTESIAN_POINT('Ctrl Pts',(-58.1457300968467,-39.5574543406959,
12.));
#139793=CARTESIAN_POINT('Ctrl Pts',(-58.1264721285698,-39.5510383869476,
0.));
#139794=CARTESIAN_POINT('Ctrl Pts',(-58.1264721285698,-39.5510383869476,
12.));
#139795=CARTESIAN_POINT('Ctrl Pts',(-58.1072704428895,-39.5446185579615,
0.));
#139796=CARTESIAN_POINT('Ctrl Pts',(-58.1072704428895,-39.5446185579615,
12.));
#139797=CARTESIAN_POINT('Ctrl Pts',(-58.0881251879911,-39.5381949959214,
0.));
#139798=CARTESIAN_POINT('Ctrl Pts',(-58.0881251879911,-39.5381949959214,
12.));
#139799=CARTESIAN_POINT('Ctrl Pts',(-58.0690365065393,-39.5317678383231,
0.));
#139800=CARTESIAN_POINT('Ctrl Pts',(-58.0690365065393,-39.5317678383231,
12.));
#139801=CARTESIAN_POINT('Ctrl Pts',(-58.050004530846,-39.5253372136921,
0.));
#139802=CARTESIAN_POINT('Ctrl Pts',(-58.050004530846,-39.5253372136921,
12.));
#139803=CARTESIAN_POINT('Ctrl Pts',(-58.0310293875321,-39.5189032457227,
0.));
#139804=CARTESIAN_POINT('Ctrl Pts',(-58.0310293875321,-39.5189032457227,
12.));
#139805=CARTESIAN_POINT('Ctrl Pts',(-58.012111206794,-39.5124660615009,
0.));
#139806=CARTESIAN_POINT('Ctrl Pts',(-58.012111206794,-39.5124660615009,
12.));
#139807=CARTESIAN_POINT('Ctrl Pts',(-57.9932501298522,-39.5060257981225,
0.));
#139808=CARTESIAN_POINT('Ctrl Pts',(-57.9932501298522,-39.5060257981225,
12.));
#139809=CARTESIAN_POINT('Ctrl Pts',(-57.9744463179305,-39.4995826106691,
0.));
#139810=CARTESIAN_POINT('Ctrl Pts',(-57.9744463179305,-39.4995826106691,
12.));
#139811=CARTESIAN_POINT('Ctrl Pts',(-57.9556999583777,-39.4931366776627,
0.));
#139812=CARTESIAN_POINT('Ctrl Pts',(-57.9556999583777,-39.4931366776627,
12.));
#139813=CARTESIAN_POINT('Ctrl Pts',(-57.9370112456506,-39.4866881842223,
0.));
#139814=CARTESIAN_POINT('Ctrl Pts',(-57.9370112456506,-39.4866881842223,
12.));
#139815=CARTESIAN_POINT('Ctrl Pts',(-57.9183803632337,-39.4802373061008,
0.));
#139816=CARTESIAN_POINT('Ctrl Pts',(-57.9183803632337,-39.4802373061008,
12.));
#139817=CARTESIAN_POINT('Ctrl Pts',(-57.8998074670541,-39.4737841949417,
0.));
#139818=CARTESIAN_POINT('Ctrl Pts',(-57.8998074670541,-39.4737841949417,
12.));
#139819=CARTESIAN_POINT('Ctrl Pts',(-57.8812926637397,-39.4673289592425,
0.));
#139820=CARTESIAN_POINT('Ctrl Pts',(-57.8812926637397,-39.4673289592425,
12.));
#139821=CARTESIAN_POINT('Ctrl Pts',(-57.8628360097134,-39.4608716627367,
0.));
#139822=CARTESIAN_POINT('Ctrl Pts',(-57.8628360097134,-39.4608716627367,
12.));
#139823=CARTESIAN_POINT('Ctrl Pts',(-57.8481172247805,-39.4557042029884,
0.));
#139824=CARTESIAN_POINT('Ctrl Pts',(-57.8481172247805,-39.4557042029884,
12.));
#139825=CARTESIAN_POINT('Ctrl Pts',(-57.8371043151607,-39.45182770037,0.));
#139826=CARTESIAN_POINT('Ctrl Pts',(-57.8371043151607,-39.45182770037,12.));
#139827=CARTESIAN_POINT('Ctrl Pts',(-57.829774010102,-39.4492429618498,
0.));
#139828=CARTESIAN_POINT('Ctrl Pts',(-57.829774010102,-39.4492429618498,
12.));
#139829=CARTESIAN_POINT('Ctrl Pts',(-57.8261117662439,-39.4479504917286,
0.));
#139830=CARTESIAN_POINT('Ctrl Pts',(-57.8261117662439,-39.4479504917286,
12.));
#139831=CARTESIAN_POINT('',(-57.8261117662439,-39.4479504917286,12.));
#139832=CARTESIAN_POINT('Ctrl Pts',(-57.8261117662439,-39.4479504917286,
12.));
#139833=CARTESIAN_POINT('Ctrl Pts',(-57.829774010102,-39.4492429618498,
12.));
#139834=CARTESIAN_POINT('Ctrl Pts',(-57.8371043151607,-39.45182770037,12.));
#139835=CARTESIAN_POINT('Ctrl Pts',(-57.8481172247805,-39.4557042029884,
12.));
#139836=CARTESIAN_POINT('Ctrl Pts',(-57.8628360097134,-39.4608716627367,
12.));
#139837=CARTESIAN_POINT('Ctrl Pts',(-57.8812926637397,-39.4673289592425,
12.));
#139838=CARTESIAN_POINT('Ctrl Pts',(-57.8998074670541,-39.4737841949417,
12.));
#139839=CARTESIAN_POINT('Ctrl Pts',(-57.9183803632337,-39.4802373061008,
12.));
#139840=CARTESIAN_POINT('Ctrl Pts',(-57.9370112456506,-39.4866881842223,
12.));
#139841=CARTESIAN_POINT('Ctrl Pts',(-57.9556999583777,-39.4931366776627,
12.));
#139842=CARTESIAN_POINT('Ctrl Pts',(-57.9744463179305,-39.4995826106691,
12.));
#139843=CARTESIAN_POINT('Ctrl Pts',(-57.9932501298522,-39.5060257981225,
12.));
#139844=CARTESIAN_POINT('Ctrl Pts',(-58.012111206794,-39.5124660615009,
12.));
#139845=CARTESIAN_POINT('Ctrl Pts',(-58.0310293875321,-39.5189032457227,
12.));
#139846=CARTESIAN_POINT('Ctrl Pts',(-58.050004530846,-39.5253372136921,
12.));
#139847=CARTESIAN_POINT('Ctrl Pts',(-58.0690365065393,-39.5317678383231,
12.));
#139848=CARTESIAN_POINT('Ctrl Pts',(-58.0881251879911,-39.5381949959214,
12.));
#139849=CARTESIAN_POINT('Ctrl Pts',(-58.1072704428895,-39.5446185579615,
12.));
#139850=CARTESIAN_POINT('Ctrl Pts',(-58.1264721285698,-39.5510383869476,
12.));
#139851=CARTESIAN_POINT('Ctrl Pts',(-58.1457300968467,-39.5574543406959,
12.));
#139852=CARTESIAN_POINT('Ctrl Pts',(-58.1650441970379,-39.5638662750174,
12.));
#139853=CARTESIAN_POINT('Ctrl Pts',(-58.1844142794359,-39.5702740468013,
12.));
#139854=CARTESIAN_POINT('Ctrl Pts',(-58.2038401992496,-39.5766775175226,
12.));
#139855=CARTESIAN_POINT('Ctrl Pts',(-58.2233218164408,-39.5830765530919,
12.));
#139856=CARTESIAN_POINT('Ctrl Pts',(-58.2428589938395,-39.5894710221729,
12.));
#139857=CARTESIAN_POINT('Ctrl Pts',(-58.2624515958416,-39.5958607950237,
12.));
#139858=CARTESIAN_POINT('Ctrl Pts',(-58.2820994868092,-39.6022457420772,
12.));
#139859=CARTESIAN_POINT('Ctrl Pts',(-58.3018025297288,-39.6086257327559,
12.));
#139860=CARTESIAN_POINT('Ctrl Pts',(-58.3215605869192,-39.6150006360894,
12.));
#139861=CARTESIAN_POINT('Ctrl Pts',(-58.3413735206412,-39.6213703212522,
12.));
#139862=CARTESIAN_POINT('Ctrl Pts',(-58.3612411936914,-39.6277346580898,
12.));
#139863=CARTESIAN_POINT('Ctrl Pts',(-58.3811634701061,-39.6340935177492,
12.));
#139864=CARTESIAN_POINT('Ctrl Pts',(-58.4011402154225,-39.6404467729113,
12.));
#139865=CARTESIAN_POINT('Ctrl Pts',(-58.4211712963024,-39.6467942974464,
12.));
#139866=CARTESIAN_POINT('Ctrl Pts',(-58.4412565802984,-39.6531359662043,
12.));
#139867=CARTESIAN_POINT('Ctrl Pts',(-58.4613959355776,-39.659471654768,
12.));
#139868=CARTESIAN_POINT('Ctrl Pts',(-58.4815892306044,-39.66580123918,12.));
#139869=CARTESIAN_POINT('Ctrl Pts',(-58.5018363341582,-39.6721245959516,
12.));
#139870=CARTESIAN_POINT('Ctrl Pts',(-58.5221371154748,-39.6784416021817,
12.));
#139871=CARTESIAN_POINT('Ctrl Pts',(-58.5424914443415,-39.6847521356395,
12.));
#139872=CARTESIAN_POINT('Ctrl Pts',(-58.5628991912067,-39.6910560748639,
12.));
#139873=CARTESIAN_POINT('Ctrl Pts',(-58.5833602272767,-39.6973532992555,
12.));
#139874=CARTESIAN_POINT('Ctrl Pts',(-58.6038744244683,-39.7036436890248,
12.));
#139875=CARTESIAN_POINT('Ctrl Pts',(-58.6244416553574,-39.7099271251421,
12.));
#139876=CARTESIAN_POINT('Ctrl Pts',(-58.6450617931269,-39.7162034892896,
12.));
#139877=CARTESIAN_POINT('Ctrl Pts',(-58.6657347115015,-39.7224726638087,
12.));
#139878=CARTESIAN_POINT('Ctrl Pts',(-58.6864602847065,-39.7287345316664,
12.));
#139879=CARTESIAN_POINT('Ctrl Pts',(-58.7072383875009,-39.7349889764737,
12.));
#139880=CARTESIAN_POINT('Ctrl Pts',(-58.7280688951911,-39.7412358824949,
12.));
#139881=CARTESIAN_POINT('Ctrl Pts',(-58.7489516836453,-39.7474751346603,
12.));
#139882=CARTESIAN_POINT('Ctrl Pts',(-58.7698866293041,-39.753706618582,
12.));
#139883=CARTESIAN_POINT('Ctrl Pts',(-58.7908736091808,-39.7599302205527,
12.));
#139884=CARTESIAN_POINT('Ctrl Pts',(-58.8119125008521,-39.7661458275276,
12.));
#139885=CARTESIAN_POINT('Ctrl Pts',(-58.8330031824453,-39.772353327112,
12.));
#139886=CARTESIAN_POINT('Ctrl Pts',(-58.8541455326229,-39.7785526075477,
12.));
#139887=CARTESIAN_POINT('Ctrl Pts',(-58.8753394305583,-39.7847435576995,
12.));
#139888=CARTESIAN_POINT('Ctrl Pts',(-58.896584755939,-39.7909260670517,
12.));
#139889=CARTESIAN_POINT('Ctrl Pts',(-58.9178813889703,-39.7971000257044,
12.));
#139890=CARTESIAN_POINT('Ctrl Pts',(-58.9392292103747,-39.8032653243712,
12.));
#139891=CARTESIAN_POINT('Ctrl Pts',(-58.9606281013876,-39.8094218543781,
12.));
#139892=CARTESIAN_POINT('Ctrl Pts',(-58.9820779437485,-39.8155695076624,
12.));
#139893=CARTESIAN_POINT('Ctrl Pts',(-59.0035786197024,-39.8217081767658,
12.));
#139894=CARTESIAN_POINT('Ctrl Pts',(-59.0251300119973,-39.8278377548261,
12.));
#139895=CARTESIAN_POINT('Ctrl Pts',(-59.0467320038783,-39.8339581355714,
12.));
#139896=CARTESIAN_POINT('Ctrl Pts',(-59.068384479077,-39.8400692133143,
12.));
#139897=CARTESIAN_POINT('Ctrl Pts',(-59.0900873217993,-39.8461708829465,
12.));
#139898=CARTESIAN_POINT('Ctrl Pts',(-59.1118404167304,-39.8522630399337,
12.));
#139899=CARTESIAN_POINT('Ctrl Pts',(-59.133643649035,-39.8583455803111,
12.));
#139900=CARTESIAN_POINT('Ctrl Pts',(-59.155496904352,-39.8644184006785,
12.));
#139901=CARTESIAN_POINT('Ctrl Pts',(-59.1774000687865,-39.8704813981978,
12.));
#139902=CARTESIAN_POINT('Ctrl Pts',(-59.1993530289008,-39.8765344705894,
12.));
#139903=CARTESIAN_POINT('Ctrl Pts',(-59.2213556717189,-39.8825775161252,
12.));
#139904=CARTESIAN_POINT('Ctrl Pts',(-59.2434078847236,-39.8886104336234,
12.));
#139905=CARTESIAN_POINT('Ctrl Pts',(-59.2655095558527,-39.8946331224442,
12.));
#139906=CARTESIAN_POINT('Ctrl Pts',(-59.2876605734871,-39.9006454824861,
12.));
#139907=CARTESIAN_POINT('Ctrl Pts',(-59.3098608264452,-39.9066474141826,
12.));
#139908=CARTESIAN_POINT('Ctrl Pts',(-59.3321102039883,-39.9126388184956,
12.));
#139909=CARTESIAN_POINT('Ctrl Pts',(-59.3544085958165,-39.9186195969113,
12.));
#139910=CARTESIAN_POINT('Ctrl Pts',(-59.3767558920663,-39.9245896514359,
12.));
#139911=CARTESIAN_POINT('Ctrl Pts',(-59.3991519832981,-39.9305488845934,
12.));
#139912=CARTESIAN_POINT('Ctrl Pts',(-59.4215967604925,-39.9364971994215,
12.));
#139913=CARTESIAN_POINT('Ctrl Pts',(-59.444090115055,-39.9424344994652,
12.));
#139914=CARTESIAN_POINT('Ctrl Pts',(-59.4666319388123,-39.9483606887731,
12.));
#139915=CARTESIAN_POINT('Ctrl Pts',(-59.4892221240082,-39.954275671893,
12.));
#139916=CARTESIAN_POINT('Ctrl Pts',(-59.511860563292,-39.96017935387,12.));
#139917=CARTESIAN_POINT('Ctrl Pts',(-59.5345471497162,-39.9660716402423,
12.));
#139918=CARTESIAN_POINT('Ctrl Pts',(-59.5572817767412,-39.971952437036,
12.));
#139919=CARTESIAN_POINT('Ctrl Pts',(-59.5800643382322,-39.9778216507609,
12.));
#139920=CARTESIAN_POINT('Ctrl Pts',(-59.6028947284551,-39.9836791884071,
12.));
#139921=CARTESIAN_POINT('Ctrl Pts',(-59.6257728420644,-39.9895249574432,
12.));
#139922=CARTESIAN_POINT('Ctrl Pts',(-59.6486985741015,-39.9953588658114,
12.));
#139923=CARTESIAN_POINT('Ctrl Pts',(-59.671671819999,-40.001180821923,12.));
#139924=CARTESIAN_POINT('Ctrl Pts',(-59.6946924755771,-40.0069907346536,
12.));
#139925=CARTESIAN_POINT('Ctrl Pts',(-59.7177604370409,-40.0127885133407,
12.));
#139926=CARTESIAN_POINT('Ctrl Pts',(-59.7408756009688,-40.0185740677827,
12.));
#139927=CARTESIAN_POINT('Ctrl Pts',(-59.7640378643115,-40.0243473082343,
12.));
#139928=CARTESIAN_POINT('Ctrl Pts',(-59.7872471243948,-40.0301081454006,
12.));
#139929=CARTESIAN_POINT('Ctrl Pts',(-59.8105032789179,-40.035856490434,
12.));
#139930=CARTESIAN_POINT('Ctrl Pts',(-59.8338062259491,-40.0415922549313,
12.));
#139931=CARTESIAN_POINT('Ctrl Pts',(-59.8571558639145,-40.0473153509323,
12.));
#139932=CARTESIAN_POINT('Ctrl Pts',(-59.8805520915975,-40.0530256909162,
12.));
#139933=CARTESIAN_POINT('Ctrl Pts',(-59.9039948081432,-40.0587231877961,
12.));
#139934=CARTESIAN_POINT('Ctrl Pts',(-59.9274839130553,-40.0644077549159,
12.));
#139935=CARTESIAN_POINT('Ctrl Pts',(-59.9510193061927,-40.0700793060473,
12.));
#139936=CARTESIAN_POINT('Ctrl Pts',(-59.9746008877584,-40.0757377553888,
12.));
#139937=CARTESIAN_POINT('Ctrl Pts',(-59.9982285582983,-40.0813830175623,
12.));
#139938=CARTESIAN_POINT('Ctrl Pts',(-60.021902218706,-40.0870150076073,
12.));
#139939=CARTESIAN_POINT('Ctrl Pts',(-60.0456217702202,-40.0926336409785,
12.));
#139940=CARTESIAN_POINT('Ctrl Pts',(-60.069387114421,-40.0982388335423,
12.));
#139941=CARTESIAN_POINT('Ctrl Pts',(-60.0931981532198,-40.1038305015766,
12.));
#139942=CARTESIAN_POINT('Ctrl Pts',(-60.1170547888574,-40.1094085617674,
12.));
#139943=CARTESIAN_POINT('Ctrl Pts',(-60.1409569239092,-40.1149729312036,
12.));
#139944=CARTESIAN_POINT('Ctrl Pts',(-60.1649044612828,-40.1205235273739,
12.));
#139945=CARTESIAN_POINT('Ctrl Pts',(-60.1888973042152,-40.1260602681644,
12.));
#139946=CARTESIAN_POINT('Ctrl Pts',(-60.2129353562622,-40.1315830718577,
12.));
#139947=CARTESIAN_POINT('Ctrl Pts',(-60.2370185212965,-40.1370918571304,
12.));
#139948=CARTESIAN_POINT('Ctrl Pts',(-60.2611467035117,-40.1425865430472,
12.));
#139949=CARTESIAN_POINT('Ctrl Pts',(-60.285319807422,-40.1480670490585,
12.));
#139950=CARTESIAN_POINT('Ctrl Pts',(-60.3095377378586,-40.1535332949976,
12.));
#139951=CARTESIAN_POINT('Ctrl Pts',(-60.3338003999607,-40.1589852010804,
12.));
#139952=CARTESIAN_POINT('Ctrl Pts',(-60.3581076991716,-40.1644226879033,
12.));
#139953=CARTESIAN_POINT('Ctrl Pts',(-60.3824595412446,-40.1698456764377,
12.));
#139954=CARTESIAN_POINT('Ctrl Pts',(-60.4068558322407,-40.1752540880268,
12.));
#139955=CARTESIAN_POINT('Ctrl Pts',(-60.4312964785273,-40.180647844383,
12.));
#139956=CARTESIAN_POINT('Ctrl Pts',(-60.455781386769,-40.1860268675883,
12.));
#139957=CARTESIAN_POINT('Ctrl Pts',(-60.4803104639226,-40.1913910800921,
12.));
#139958=CARTESIAN_POINT('Ctrl Pts',(-60.5048836172435,-40.1967404047062,
12.));
#139959=CARTESIAN_POINT('Ctrl Pts',(-60.5295007542841,-40.2020747646014,
12.));
#139960=CARTESIAN_POINT('Ctrl Pts',(-60.5541617828925,-40.2073940833052,
12.));
#139961=CARTESIAN_POINT('Ctrl Pts',(-60.5788666112042,-40.2126982847011,
12.));
#139962=CARTESIAN_POINT('Ctrl Pts',(-60.6036151476349,-40.2179872930273,
12.));
#139963=CARTESIAN_POINT('Ctrl Pts',(-60.6284073008871,-40.2232610328721,
12.));
#139964=CARTESIAN_POINT('Ctrl Pts',(-60.6532429799499,-40.2285194291706,
12.));
#139965=CARTESIAN_POINT('Ctrl Pts',(-60.678122094098,-40.2337624072028,
12.));
#139966=CARTESIAN_POINT('Ctrl Pts',(-60.7030445528857,-40.2389898925932,
12.));
#139967=CARTESIAN_POINT('Ctrl Pts',(-60.728010266139,-40.2442018113108,
12.));
#139968=CARTESIAN_POINT('Ctrl Pts',(-60.7530191439593,-40.2493980896638,
12.));
#139969=CARTESIAN_POINT('Ctrl Pts',(-60.7780710967248,-40.2545786542953,
12.));
#139970=CARTESIAN_POINT('Ctrl Pts',(-60.8031660350879,-40.2597434321803,
12.));
#139971=CARTESIAN_POINT('Ctrl Pts',(-60.8283038699706,-40.2648923506248,
12.));
#139972=CARTESIAN_POINT('Ctrl Pts',(-60.8534845125538,-40.2700253372647,
12.));
#139973=CARTESIAN_POINT('Ctrl Pts',(-60.8787078742818,-40.2751423200639,
12.));
#139974=CARTESIAN_POINT('Ctrl Pts',(-60.9039738668669,-40.2802432273104,
12.));
#139975=CARTESIAN_POINT('Ctrl Pts',(-60.9292824022887,-40.2853279876161,
12.));
#139976=CARTESIAN_POINT('Ctrl Pts',(-60.9546333927921,-40.2903965299155,
12.));
#139977=CARTESIAN_POINT('Ctrl Pts',(-60.9800267508787,-40.295448783469,
12.));
#139978=CARTESIAN_POINT('Ctrl Pts',(-61.0054623893066,-40.300484677858,
12.));
#139979=CARTESIAN_POINT('Ctrl Pts',(-61.0309402210921,-40.3055041429775,
12.));
#139980=CARTESIAN_POINT('Ctrl Pts',(-61.056460159505,-40.3105071090309,
12.));
#139981=CARTESIAN_POINT('Ctrl Pts',(-61.0820221180645,-40.3154935065262,
12.));
#139982=CARTESIAN_POINT('Ctrl Pts',(-61.1076260105258,-40.3204632662725,
12.));
#139983=CARTESIAN_POINT('Ctrl Pts',(-61.1332717508789,-40.32541631938,12.));
#139984=CARTESIAN_POINT('Ctrl Pts',(-61.1589592533613,-40.3303525972615,
12.));
#139985=CARTESIAN_POINT('Ctrl Pts',(-61.1846884324644,-40.335272031637,
12.));
#139986=CARTESIAN_POINT('Ctrl Pts',(-61.2104592029377,-40.340174554537,
12.));
#139987=CARTESIAN_POINT('Ctrl Pts',(-61.23627147979,-40.3450600983109,12.));
#139988=CARTESIAN_POINT('Ctrl Pts',(-61.2621251782863,-40.3499285956304,
12.));
#139989=CARTESIAN_POINT('Ctrl Pts',(-61.2880202139371,-40.3547799794679,
12.));
#139990=CARTESIAN_POINT('Ctrl Pts',(-61.3139565024847,-40.3596141830791,
12.));
#139991=CARTESIAN_POINT('Ctrl Pts',(-61.3399339598853,-40.3644311399861,
12.));
#139992=CARTESIAN_POINT('Ctrl Pts',(-61.3659525022908,-40.3692307839636,
12.));
#139993=CARTESIAN_POINT('Ctrl Pts',(-61.3920120460219,-40.3740130490225,
12.));
#139994=CARTESIAN_POINT('Ctrl Pts',(-61.4181125076037,-40.3787778694364,
12.));
#139995=CARTESIAN_POINT('Ctrl Pts',(-61.4442538038044,-40.383525179772,
12.));
#139996=CARTESIAN_POINT('Ctrl Pts',(-61.4704358516709,-40.3882549149227,
12.));
#139997=CARTESIAN_POINT('Ctrl Pts',(-61.4966585685549,-40.3929670101365,
12.));
#139998=CARTESIAN_POINT('Ctrl Pts',(-61.522921872154,-40.3976614010652,
12.));
#139999=CARTESIAN_POINT('Ctrl Pts',(-61.5492256804717,-40.4023380237232,
12.));
#140000=CARTESIAN_POINT('Ctrl Pts',(-61.5755699117324,-40.4069968143956,
12.));
#140001=CARTESIAN_POINT('Ctrl Pts',(-61.6019544843011,-40.4116377095596,
12.));
#140002=CARTESIAN_POINT('Ctrl Pts',(-61.628379316608,-40.4162606458118,
12.));
#140003=CARTESIAN_POINT('Ctrl Pts',(-61.6548443270394,-40.4208655597717,
12.));
#140004=CARTESIAN_POINT('Ctrl Pts',(-61.6813494339286,-40.425452388076,
12.));
#140005=CARTESIAN_POINT('Ctrl Pts',(-61.7078945557799,-40.430021067584,
12.));
#140006=CARTESIAN_POINT('Ctrl Pts',(-61.7344796114399,-40.4345715355404,
12.));
#140007=CARTESIAN_POINT('Ctrl Pts',(-61.7611045202874,-40.4391037297588,
12.));
#140008=CARTESIAN_POINT('Ctrl Pts',(-61.7877692024076,-40.4436175887949,
12.));
#140009=CARTESIAN_POINT('Ctrl Pts',(-61.814473578779,-40.4481130521364,
12.));
#140010=CARTESIAN_POINT('Ctrl Pts',(-61.8412175708553,-40.4525900597894,
12.));
#140011=CARTESIAN_POINT('Ctrl Pts',(-61.8680011001537,-40.4570485518749,
12.));
#140012=CARTESIAN_POINT('Ctrl Pts',(-61.8948240878008,-40.4614884681889,
12.));
#140013=CARTESIAN_POINT('Ctrl Pts',(-61.9216864541744,-40.4659097478587,
12.));
#140014=CARTESIAN_POINT('Ctrl Pts',(-61.9485881182921,-40.470312328762,
12.));
#140015=CARTESIAN_POINT('Ctrl Pts',(-61.9755289983044,-40.4746961480015,
12.));
#140016=CARTESIAN_POINT('Ctrl Pts',(-62.0025090125959,-40.4790611429583,
12.));
#140017=CARTESIAN_POINT('Ctrl Pts',(-62.029528080742,-40.4834072522164,
12.));
#140018=CARTESIAN_POINT('Ctrl Pts',(-62.0565861244179,-40.4877344164411,
12.));
#140019=CARTESIAN_POINT('Ctrl Pts',(-62.083683068572,-40.4920425795216,
12.));
#140020=CARTESIAN_POINT('Ctrl Pts',(-62.1108188417004,-40.4963316888412,
12.));
#140021=CARTESIAN_POINT('Ctrl Pts',(-62.1341126810543,-40.4999919096264,
12.));
#140022=CARTESIAN_POINT('Ctrl Pts',(-62.1519925002978,-40.5027877865803,
12.));
#140023=CARTESIAN_POINT('Ctrl Pts',(-62.1644411502826,-40.5047277935767,
12.));
#140024=CARTESIAN_POINT('Ctrl Pts',(-62.1714473138108,-40.5058175523128,
12.));
#140025=CARTESIAN_POINT('Ctrl Pts',(-62.1730054756879,-40.506059810093,
12.));
#140026=CARTESIAN_POINT('',(-57.8261117662439,-39.4479504917286,0.));
#140027=CARTESIAN_POINT('',(-57.8261117662439,-39.4479504917286,0.));
#140028=CARTESIAN_POINT('Ctrl Pts',(-62.1730054756878,-40.506059810093,
0.));
#140029=CARTESIAN_POINT('Ctrl Pts',(-62.1714473138107,-40.5058175523128,
0.));
#140030=CARTESIAN_POINT('Ctrl Pts',(-62.1644411502825,-40.5047277935767,
0.));
#140031=CARTESIAN_POINT('Ctrl Pts',(-62.1519925002977,-40.5027877865803,
0.));
#140032=CARTESIAN_POINT('Ctrl Pts',(-62.1341126810543,-40.4999919096264,
0.));
#140033=CARTESIAN_POINT('Ctrl Pts',(-62.1108188417004,-40.4963316888412,
0.));
#140034=CARTESIAN_POINT('Ctrl Pts',(-62.083683068572,-40.4920425795216,
0.));
#140035=CARTESIAN_POINT('Ctrl Pts',(-62.0565861244179,-40.4877344164411,
0.));
#140036=CARTESIAN_POINT('Ctrl Pts',(-62.029528080742,-40.4834072522164,
0.));
#140037=CARTESIAN_POINT('Ctrl Pts',(-62.0025090125959,-40.4790611429583,
0.));
#140038=CARTESIAN_POINT('Ctrl Pts',(-61.9755289983044,-40.4746961480015,
0.));
#140039=CARTESIAN_POINT('Ctrl Pts',(-61.9485881182921,-40.470312328762,
0.));
#140040=CARTESIAN_POINT('Ctrl Pts',(-61.9216864541744,-40.4659097478587,
0.));
#140041=CARTESIAN_POINT('Ctrl Pts',(-61.8948240878008,-40.4614884681889,
0.));
#140042=CARTESIAN_POINT('Ctrl Pts',(-61.8680011001537,-40.4570485518749,
0.));
#140043=CARTESIAN_POINT('Ctrl Pts',(-61.8412175708553,-40.4525900597894,
0.));
#140044=CARTESIAN_POINT('Ctrl Pts',(-61.814473578779,-40.4481130521364,
0.));
#140045=CARTESIAN_POINT('Ctrl Pts',(-61.7877692024076,-40.4436175887949,
0.));
#140046=CARTESIAN_POINT('Ctrl Pts',(-61.7611045202874,-40.4391037297588,
0.));
#140047=CARTESIAN_POINT('Ctrl Pts',(-61.7344796114399,-40.4345715355404,
0.));
#140048=CARTESIAN_POINT('Ctrl Pts',(-61.7078945557799,-40.430021067584,
0.));
#140049=CARTESIAN_POINT('Ctrl Pts',(-61.6813494339286,-40.425452388076,
0.));
#140050=CARTESIAN_POINT('Ctrl Pts',(-61.6548443270394,-40.4208655597717,
0.));
#140051=CARTESIAN_POINT('Ctrl Pts',(-61.628379316608,-40.4162606458118,
0.));
#140052=CARTESIAN_POINT('Ctrl Pts',(-61.6019544843011,-40.4116377095596,
0.));
#140053=CARTESIAN_POINT('Ctrl Pts',(-61.5755699117324,-40.4069968143956,
0.));
#140054=CARTESIAN_POINT('Ctrl Pts',(-61.5492256804717,-40.4023380237232,
0.));
#140055=CARTESIAN_POINT('Ctrl Pts',(-61.522921872154,-40.3976614010652,
0.));
#140056=CARTESIAN_POINT('Ctrl Pts',(-61.4966585685549,-40.3929670101365,
0.));
#140057=CARTESIAN_POINT('Ctrl Pts',(-61.4704358516709,-40.3882549149227,
0.));
#140058=CARTESIAN_POINT('Ctrl Pts',(-61.4442538038044,-40.383525179772,
0.));
#140059=CARTESIAN_POINT('Ctrl Pts',(-61.4181125076037,-40.3787778694364,
0.));
#140060=CARTESIAN_POINT('Ctrl Pts',(-61.3920120460219,-40.3740130490225,
0.));
#140061=CARTESIAN_POINT('Ctrl Pts',(-61.3659525022908,-40.3692307839636,
0.));
#140062=CARTESIAN_POINT('Ctrl Pts',(-61.3399339598853,-40.3644311399861,
0.));
#140063=CARTESIAN_POINT('Ctrl Pts',(-61.3139565024847,-40.3596141830791,
0.));
#140064=CARTESIAN_POINT('Ctrl Pts',(-61.2880202139371,-40.3547799794679,
0.));
#140065=CARTESIAN_POINT('Ctrl Pts',(-61.2621251782863,-40.3499285956304,
0.));
#140066=CARTESIAN_POINT('Ctrl Pts',(-61.23627147979,-40.3450600983109,0.));
#140067=CARTESIAN_POINT('Ctrl Pts',(-61.2104592029377,-40.340174554537,
0.));
#140068=CARTESIAN_POINT('Ctrl Pts',(-61.1846884324644,-40.335272031637,
0.));
#140069=CARTESIAN_POINT('Ctrl Pts',(-61.1589592533613,-40.3303525972615,
0.));
#140070=CARTESIAN_POINT('Ctrl Pts',(-61.1332717508789,-40.32541631938,0.));
#140071=CARTESIAN_POINT('Ctrl Pts',(-61.1076260105258,-40.3204632662725,
0.));
#140072=CARTESIAN_POINT('Ctrl Pts',(-61.0820221180645,-40.3154935065262,
0.));
#140073=CARTESIAN_POINT('Ctrl Pts',(-61.056460159505,-40.3105071090309,
0.));
#140074=CARTESIAN_POINT('Ctrl Pts',(-61.0309402210921,-40.3055041429775,
0.));
#140075=CARTESIAN_POINT('Ctrl Pts',(-61.0054623893066,-40.300484677858,
0.));
#140076=CARTESIAN_POINT('Ctrl Pts',(-60.9800267508787,-40.295448783469,
0.));
#140077=CARTESIAN_POINT('Ctrl Pts',(-60.9546333927921,-40.2903965299155,
0.));
#140078=CARTESIAN_POINT('Ctrl Pts',(-60.9292824022887,-40.2853279876161,
0.));
#140079=CARTESIAN_POINT('Ctrl Pts',(-60.9039738668669,-40.2802432273104,
0.));
#140080=CARTESIAN_POINT('Ctrl Pts',(-60.8787078742818,-40.2751423200639,
0.));
#140081=CARTESIAN_POINT('Ctrl Pts',(-60.8534845125538,-40.2700253372647,
0.));
#140082=CARTESIAN_POINT('Ctrl Pts',(-60.8283038699706,-40.2648923506248,
0.));
#140083=CARTESIAN_POINT('Ctrl Pts',(-60.8031660350879,-40.2597434321803,
0.));
#140084=CARTESIAN_POINT('Ctrl Pts',(-60.7780710967248,-40.2545786542953,
0.));
#140085=CARTESIAN_POINT('Ctrl Pts',(-60.7530191439593,-40.2493980896638,
0.));
#140086=CARTESIAN_POINT('Ctrl Pts',(-60.728010266139,-40.2442018113108,
0.));
#140087=CARTESIAN_POINT('Ctrl Pts',(-60.7030445528857,-40.2389898925932,
0.));
#140088=CARTESIAN_POINT('Ctrl Pts',(-60.678122094098,-40.2337624072028,
0.));
#140089=CARTESIAN_POINT('Ctrl Pts',(-60.6532429799499,-40.2285194291706,
0.));
#140090=CARTESIAN_POINT('Ctrl Pts',(-60.6284073008871,-40.2232610328721,
0.));
#140091=CARTESIAN_POINT('Ctrl Pts',(-60.6036151476349,-40.2179872930273,
0.));
#140092=CARTESIAN_POINT('Ctrl Pts',(-60.5788666112042,-40.2126982847011,
0.));
#140093=CARTESIAN_POINT('Ctrl Pts',(-60.5541617828925,-40.2073940833052,
0.));
#140094=CARTESIAN_POINT('Ctrl Pts',(-60.5295007542841,-40.2020747646014,
0.));
#140095=CARTESIAN_POINT('Ctrl Pts',(-60.5048836172435,-40.1967404047062,
0.));
#140096=CARTESIAN_POINT('Ctrl Pts',(-60.4803104639226,-40.1913910800921,
0.));
#140097=CARTESIAN_POINT('Ctrl Pts',(-60.455781386769,-40.1860268675883,
0.));
#140098=CARTESIAN_POINT('Ctrl Pts',(-60.4312964785273,-40.180647844383,
0.));
#140099=CARTESIAN_POINT('Ctrl Pts',(-60.4068558322407,-40.1752540880268,
0.));
#140100=CARTESIAN_POINT('Ctrl Pts',(-60.3824595412446,-40.1698456764377,
0.));
#140101=CARTESIAN_POINT('Ctrl Pts',(-60.3581076991716,-40.1644226879033,
0.));
#140102=CARTESIAN_POINT('Ctrl Pts',(-60.3338003999607,-40.1589852010804,
0.));
#140103=CARTESIAN_POINT('Ctrl Pts',(-60.3095377378586,-40.1535332949976,
0.));
#140104=CARTESIAN_POINT('Ctrl Pts',(-60.285319807422,-40.1480670490585,
0.));
#140105=CARTESIAN_POINT('Ctrl Pts',(-60.2611467035117,-40.1425865430472,
0.));
#140106=CARTESIAN_POINT('Ctrl Pts',(-60.2370185212965,-40.1370918571304,
0.));
#140107=CARTESIAN_POINT('Ctrl Pts',(-60.2129353562622,-40.1315830718577,
0.));
#140108=CARTESIAN_POINT('Ctrl Pts',(-60.1888973042152,-40.1260602681644,
0.));
#140109=CARTESIAN_POINT('Ctrl Pts',(-60.1649044612828,-40.1205235273739,
0.));
#140110=CARTESIAN_POINT('Ctrl Pts',(-60.1409569239092,-40.1149729312036,
0.));
#140111=CARTESIAN_POINT('Ctrl Pts',(-60.1170547888574,-40.1094085617674,
0.));
#140112=CARTESIAN_POINT('Ctrl Pts',(-60.0931981532198,-40.1038305015766,
0.));
#140113=CARTESIAN_POINT('Ctrl Pts',(-60.069387114421,-40.0982388335423,
0.));
#140114=CARTESIAN_POINT('Ctrl Pts',(-60.0456217702202,-40.0926336409785,
0.));
#140115=CARTESIAN_POINT('Ctrl Pts',(-60.021902218706,-40.0870150076073,
0.));
#140116=CARTESIAN_POINT('Ctrl Pts',(-59.9982285582983,-40.0813830175623,
0.));
#140117=CARTESIAN_POINT('Ctrl Pts',(-59.9746008877584,-40.0757377553888,
0.));
#140118=CARTESIAN_POINT('Ctrl Pts',(-59.9510193061927,-40.0700793060473,
0.));
#140119=CARTESIAN_POINT('Ctrl Pts',(-59.9274839130553,-40.0644077549159,
0.));
#140120=CARTESIAN_POINT('Ctrl Pts',(-59.9039948081432,-40.0587231877961,
0.));
#140121=CARTESIAN_POINT('Ctrl Pts',(-59.8805520915975,-40.0530256909162,
0.));
#140122=CARTESIAN_POINT('Ctrl Pts',(-59.8571558639145,-40.0473153509323,
0.));
#140123=CARTESIAN_POINT('Ctrl Pts',(-59.8338062259491,-40.0415922549313,
0.));
#140124=CARTESIAN_POINT('Ctrl Pts',(-59.8105032789179,-40.035856490434,
0.));
#140125=CARTESIAN_POINT('Ctrl Pts',(-59.7872471243948,-40.0301081454006,
0.));
#140126=CARTESIAN_POINT('Ctrl Pts',(-59.7640378643115,-40.0243473082343,
0.));
#140127=CARTESIAN_POINT('Ctrl Pts',(-59.7408756009688,-40.0185740677827,
0.));
#140128=CARTESIAN_POINT('Ctrl Pts',(-59.7177604370409,-40.0127885133407,
0.));
#140129=CARTESIAN_POINT('Ctrl Pts',(-59.6946924755771,-40.0069907346536,
0.));
#140130=CARTESIAN_POINT('Ctrl Pts',(-59.671671819999,-40.001180821923,0.));
#140131=CARTESIAN_POINT('Ctrl Pts',(-59.6486985741015,-39.9953588658114,
0.));
#140132=CARTESIAN_POINT('Ctrl Pts',(-59.6257728420644,-39.9895249574432,
0.));
#140133=CARTESIAN_POINT('Ctrl Pts',(-59.6028947284551,-39.9836791884071,
0.));
#140134=CARTESIAN_POINT('Ctrl Pts',(-59.5800643382322,-39.9778216507609,
0.));
#140135=CARTESIAN_POINT('Ctrl Pts',(-59.5572817767412,-39.971952437036,
0.));
#140136=CARTESIAN_POINT('Ctrl Pts',(-59.5345471497162,-39.9660716402423,
0.));
#140137=CARTESIAN_POINT('Ctrl Pts',(-59.511860563292,-39.96017935387,0.));
#140138=CARTESIAN_POINT('Ctrl Pts',(-59.4892221240082,-39.954275671893,
0.));
#140139=CARTESIAN_POINT('Ctrl Pts',(-59.4666319388123,-39.9483606887731,
0.));
#140140=CARTESIAN_POINT('Ctrl Pts',(-59.444090115055,-39.9424344994652,
0.));
#140141=CARTESIAN_POINT('Ctrl Pts',(-59.4215967604925,-39.9364971994215,
0.));
#140142=CARTESIAN_POINT('Ctrl Pts',(-59.3991519832981,-39.9305488845934,
0.));
#140143=CARTESIAN_POINT('Ctrl Pts',(-59.3767558920663,-39.9245896514359,
0.));
#140144=CARTESIAN_POINT('Ctrl Pts',(-59.3544085958165,-39.9186195969113,
0.));
#140145=CARTESIAN_POINT('Ctrl Pts',(-59.3321102039883,-39.9126388184956,
0.));
#140146=CARTESIAN_POINT('Ctrl Pts',(-59.3098608264452,-39.9066474141826,
0.));
#140147=CARTESIAN_POINT('Ctrl Pts',(-59.2876605734871,-39.9006454824861,
0.));
#140148=CARTESIAN_POINT('Ctrl Pts',(-59.2655095558527,-39.8946331224442,
0.));
#140149=CARTESIAN_POINT('Ctrl Pts',(-59.2434078847236,-39.8886104336234,
0.));
#140150=CARTESIAN_POINT('Ctrl Pts',(-59.2213556717189,-39.8825775161252,
0.));
#140151=CARTESIAN_POINT('Ctrl Pts',(-59.1993530289008,-39.8765344705894,
0.));
#140152=CARTESIAN_POINT('Ctrl Pts',(-59.1774000687865,-39.8704813981978,
0.));
#140153=CARTESIAN_POINT('Ctrl Pts',(-59.155496904352,-39.8644184006785,
0.));
#140154=CARTESIAN_POINT('Ctrl Pts',(-59.133643649035,-39.8583455803111,
0.));
#140155=CARTESIAN_POINT('Ctrl Pts',(-59.1118404167304,-39.8522630399337,
0.));
#140156=CARTESIAN_POINT('Ctrl Pts',(-59.0900873217993,-39.8461708829465,
0.));
#140157=CARTESIAN_POINT('Ctrl Pts',(-59.068384479077,-39.8400692133143,
0.));
#140158=CARTESIAN_POINT('Ctrl Pts',(-59.0467320038783,-39.8339581355714,
0.));
#140159=CARTESIAN_POINT('Ctrl Pts',(-59.0251300119973,-39.8278377548261,
0.));
#140160=CARTESIAN_POINT('Ctrl Pts',(-59.0035786197024,-39.8217081767658,
0.));
#140161=CARTESIAN_POINT('Ctrl Pts',(-58.9820779437485,-39.8155695076624,
0.));
#140162=CARTESIAN_POINT('Ctrl Pts',(-58.9606281013876,-39.8094218543781,
0.));
#140163=CARTESIAN_POINT('Ctrl Pts',(-58.9392292103747,-39.8032653243712,
0.));
#140164=CARTESIAN_POINT('Ctrl Pts',(-58.9178813889703,-39.7971000257044,
0.));
#140165=CARTESIAN_POINT('Ctrl Pts',(-58.896584755939,-39.7909260670517,
0.));
#140166=CARTESIAN_POINT('Ctrl Pts',(-58.8753394305583,-39.7847435576995,
0.));
#140167=CARTESIAN_POINT('Ctrl Pts',(-58.8541455326229,-39.7785526075477,
0.));
#140168=CARTESIAN_POINT('Ctrl Pts',(-58.8330031824453,-39.772353327112,
0.));
#140169=CARTESIAN_POINT('Ctrl Pts',(-58.8119125008521,-39.7661458275276,
0.));
#140170=CARTESIAN_POINT('Ctrl Pts',(-58.7908736091808,-39.7599302205527,
0.));
#140171=CARTESIAN_POINT('Ctrl Pts',(-58.7698866293041,-39.753706618582,
0.));
#140172=CARTESIAN_POINT('Ctrl Pts',(-58.7489516836453,-39.7474751346603,
0.));
#140173=CARTESIAN_POINT('Ctrl Pts',(-58.7280688951911,-39.7412358824949,
0.));
#140174=CARTESIAN_POINT('Ctrl Pts',(-58.7072383875009,-39.7349889764737,
0.));
#140175=CARTESIAN_POINT('Ctrl Pts',(-58.6864602847065,-39.7287345316664,
0.));
#140176=CARTESIAN_POINT('Ctrl Pts',(-58.6657347115015,-39.7224726638087,
0.));
#140177=CARTESIAN_POINT('Ctrl Pts',(-58.6450617931269,-39.7162034892896,
0.));
#140178=CARTESIAN_POINT('Ctrl Pts',(-58.6244416553574,-39.7099271251421,
0.));
#140179=CARTESIAN_POINT('Ctrl Pts',(-58.6038744244683,-39.7036436890248,
0.));
#140180=CARTESIAN_POINT('Ctrl Pts',(-58.5833602272767,-39.6973532992555,
0.));
#140181=CARTESIAN_POINT('Ctrl Pts',(-58.5628991912067,-39.6910560748639,
0.));
#140182=CARTESIAN_POINT('Ctrl Pts',(-58.5424914443415,-39.6847521356395,
0.));
#140183=CARTESIAN_POINT('Ctrl Pts',(-58.5221371154748,-39.6784416021817,
0.));
#140184=CARTESIAN_POINT('Ctrl Pts',(-58.5018363341582,-39.6721245959516,
0.));
#140185=CARTESIAN_POINT('Ctrl Pts',(-58.4815892306044,-39.66580123918,0.));
#140186=CARTESIAN_POINT('Ctrl Pts',(-58.4613959355776,-39.659471654768,
0.));
#140187=CARTESIAN_POINT('Ctrl Pts',(-58.4412565802984,-39.6531359662043,
0.));
#140188=CARTESIAN_POINT('Ctrl Pts',(-58.4211712963024,-39.6467942974464,
0.));
#140189=CARTESIAN_POINT('Ctrl Pts',(-58.4011402154225,-39.6404467729113,
0.));
#140190=CARTESIAN_POINT('Ctrl Pts',(-58.3811634701061,-39.6340935177492,
0.));
#140191=CARTESIAN_POINT('Ctrl Pts',(-58.3612411936914,-39.6277346580898,
0.));
#140192=CARTESIAN_POINT('Ctrl Pts',(-58.3413735206412,-39.6213703212522,
0.));
#140193=CARTESIAN_POINT('Ctrl Pts',(-58.3215605869192,-39.6150006360894,
0.));
#140194=CARTESIAN_POINT('Ctrl Pts',(-58.3018025297288,-39.6086257327559,
0.));
#140195=CARTESIAN_POINT('Ctrl Pts',(-58.2820994868092,-39.6022457420772,
0.));
#140196=CARTESIAN_POINT('Ctrl Pts',(-58.2624515958416,-39.5958607950237,
0.));
#140197=CARTESIAN_POINT('Ctrl Pts',(-58.2428589938395,-39.5894710221729,
0.));
#140198=CARTESIAN_POINT('Ctrl Pts',(-58.2233218164408,-39.5830765530919,
0.));
#140199=CARTESIAN_POINT('Ctrl Pts',(-58.2038401992496,-39.5766775175226,
0.));
#140200=CARTESIAN_POINT('Ctrl Pts',(-58.1844142794359,-39.5702740468013,
0.));
#140201=CARTESIAN_POINT('Ctrl Pts',(-58.1650441970379,-39.5638662750174,
0.));
#140202=CARTESIAN_POINT('Ctrl Pts',(-58.1457300968467,-39.5574543406959,
0.));
#140203=CARTESIAN_POINT('Ctrl Pts',(-58.1264721285698,-39.5510383869476,
0.));
#140204=CARTESIAN_POINT('Ctrl Pts',(-58.1072704428895,-39.5446185579615,
0.));
#140205=CARTESIAN_POINT('Ctrl Pts',(-58.0881251879911,-39.5381949959214,
0.));
#140206=CARTESIAN_POINT('Ctrl Pts',(-58.0690365065393,-39.5317678383231,
0.));
#140207=CARTESIAN_POINT('Ctrl Pts',(-58.050004530846,-39.5253372136921,
0.));
#140208=CARTESIAN_POINT('Ctrl Pts',(-58.0310293875321,-39.5189032457227,
0.));
#140209=CARTESIAN_POINT('Ctrl Pts',(-58.012111206794,-39.5124660615009,
0.));
#140210=CARTESIAN_POINT('Ctrl Pts',(-57.9932501298522,-39.5060257981225,
0.));
#140211=CARTESIAN_POINT('Ctrl Pts',(-57.9744463179305,-39.4995826106691,
0.));
#140212=CARTESIAN_POINT('Ctrl Pts',(-57.9556999583777,-39.4931366776627,
0.));
#140213=CARTESIAN_POINT('Ctrl Pts',(-57.9370112456506,-39.4866881842223,
0.));
#140214=CARTESIAN_POINT('Ctrl Pts',(-57.9183803632337,-39.4802373061008,
0.));
#140215=CARTESIAN_POINT('Ctrl Pts',(-57.8998074670541,-39.4737841949417,
0.));
#140216=CARTESIAN_POINT('Ctrl Pts',(-57.8812926637397,-39.4673289592425,
0.));
#140217=CARTESIAN_POINT('Ctrl Pts',(-57.8628360097134,-39.4608716627367,
0.));
#140218=CARTESIAN_POINT('Ctrl Pts',(-57.8481172247805,-39.4557042029884,
0.));
#140219=CARTESIAN_POINT('Ctrl Pts',(-57.8371043151607,-39.45182770037,0.));
#140220=CARTESIAN_POINT('Ctrl Pts',(-57.829774010102,-39.4492429618498,
0.));
#140221=CARTESIAN_POINT('Ctrl Pts',(-57.8261117662439,-39.4479504917286,
0.));
#140222=CARTESIAN_POINT('Ctrl Pts',(-65.7914953018525,-34.9532422808861,
0.));
#140223=CARTESIAN_POINT('Ctrl Pts',(-65.7914953018525,-34.9532422808861,
12.));
#140224=CARTESIAN_POINT('Ctrl Pts',(-65.7859084407617,-34.9529266758465,
0.));
#140225=CARTESIAN_POINT('Ctrl Pts',(-65.7859084407617,-34.9529266758465,
12.));
#140226=CARTESIAN_POINT('Ctrl Pts',(-65.7747383251112,-34.9522931728759,
0.));
#140227=CARTESIAN_POINT('Ctrl Pts',(-65.7747383251112,-34.9522931728759,
12.));
#140228=CARTESIAN_POINT('Ctrl Pts',(-65.7579939712289,-34.9513360397454,
0.));
#140229=CARTESIAN_POINT('Ctrl Pts',(-65.7579939712289,-34.9513360397454,
12.));
#140230=CARTESIAN_POINT('Ctrl Pts',(-65.7356898061147,-34.9500461043246,
0.));
#140231=CARTESIAN_POINT('Ctrl Pts',(-65.7356898061147,-34.9500461043246,
12.));
#140232=CARTESIAN_POINT('Ctrl Pts',(-65.7078456758034,-34.9484107544137,
0.));
#140233=CARTESIAN_POINT('Ctrl Pts',(-65.7078456758034,-34.9484107544137,
12.));
#140234=CARTESIAN_POINT('Ctrl Pts',(-65.6800376406066,-34.9467524770438,
0.));
#140235=CARTESIAN_POINT('Ctrl Pts',(-65.6800376406066,-34.9467524770438,
12.));
#140236=CARTESIAN_POINT('Ctrl Pts',(-65.6522657321322,-34.9450712829182,
0.));
#140237=CARTESIAN_POINT('Ctrl Pts',(-65.6522657321322,-34.9450712829182,
12.));
#140238=CARTESIAN_POINT('Ctrl Pts',(-65.624529996851,-34.943367193292,0.));
#140239=CARTESIAN_POINT('Ctrl Pts',(-65.624529996851,-34.943367193292,12.));
#140240=CARTESIAN_POINT('Ctrl Pts',(-65.5968304997584,-34.9416402443435,
0.));
#140241=CARTESIAN_POINT('Ctrl Pts',(-65.5968304997584,-34.9416402443435,
12.));
#140242=CARTESIAN_POINT('Ctrl Pts',(-65.5691673225803,-34.9398904862157,
0.));
#140243=CARTESIAN_POINT('Ctrl Pts',(-65.5691673225803,-34.9398904862157,
12.));
#140244=CARTESIAN_POINT('Ctrl Pts',(-65.5415405577955,-34.9381179779673,
0.));
#140245=CARTESIAN_POINT('Ctrl Pts',(-65.5415405577955,-34.9381179779673,
12.));
#140246=CARTESIAN_POINT('Ctrl Pts',(-65.5139503038036,-34.9363227836582,
0.));
#140247=CARTESIAN_POINT('Ctrl Pts',(-65.5139503038036,-34.9363227836582,
12.));
#140248=CARTESIAN_POINT('Ctrl Pts',(-65.4863966597544,-34.9345049680825,
0.));
#140249=CARTESIAN_POINT('Ctrl Pts',(-65.4863966597544,-34.9345049680825,
12.));
#140250=CARTESIAN_POINT('Ctrl Pts',(-65.4588797201972,-34.932664592394,
0.));
#140251=CARTESIAN_POINT('Ctrl Pts',(-65.4588797201972,-34.932664592394,
12.));
#140252=CARTESIAN_POINT('Ctrl Pts',(-65.4313995707536,-34.9308017105536,
0.));
#140253=CARTESIAN_POINT('Ctrl Pts',(-65.4313995707536,-34.9308017105536,
12.));
#140254=CARTESIAN_POINT('Ctrl Pts',(-65.4039562911352,-34.9289163717747,
0.));
#140255=CARTESIAN_POINT('Ctrl Pts',(-65.4039562911352,-34.9289163717747,
12.));
#140256=CARTESIAN_POINT('Ctrl Pts',(-65.3765499573077,-34.9270086222731,
0.));
#140257=CARTESIAN_POINT('Ctrl Pts',(-65.3765499573077,-34.9270086222731,
12.));
#140258=CARTESIAN_POINT('Ctrl Pts',(-65.3491806440537,-34.9250785073477,
0.));
#140259=CARTESIAN_POINT('Ctrl Pts',(-65.3491806440537,-34.9250785073477,
12.));
#140260=CARTESIAN_POINT('Ctrl Pts',(-65.321848427191,-34.9231260731831,
0.));
#140261=CARTESIAN_POINT('Ctrl Pts',(-65.321848427191,-34.9231260731831,
12.));
#140262=CARTESIAN_POINT('Ctrl Pts',(-65.2945533863761,-34.9211513691355,
0.));
#140263=CARTESIAN_POINT('Ctrl Pts',(-65.2945533863761,-34.9211513691355,
12.));
#140264=CARTESIAN_POINT('Ctrl Pts',(-65.2672956048069,-34.9191544474872,
0.));
#140265=CARTESIAN_POINT('Ctrl Pts',(-65.2672956048069,-34.9191544474872,
12.));
#140266=CARTESIAN_POINT('Ctrl Pts',(-65.2400751679549,-34.9171353624113,
0.));
#140267=CARTESIAN_POINT('Ctrl Pts',(-65.2400751679549,-34.9171353624113,
12.));
#140268=CARTESIAN_POINT('Ctrl Pts',(-65.2128921625823,-34.9150941691747,
0.));
#140269=CARTESIAN_POINT('Ctrl Pts',(-65.2128921625823,-34.9150941691747,
12.));
#140270=CARTESIAN_POINT('Ctrl Pts',(-65.1857466757092,-34.9130309233022,
0.));
#140271=CARTESIAN_POINT('Ctrl Pts',(-65.1857466757092,-34.9130309233022,
12.));
#140272=CARTESIAN_POINT('Ctrl Pts',(-65.1586387934241,-34.9109456796213,
0.));
#140273=CARTESIAN_POINT('Ctrl Pts',(-65.1586387934241,-34.9109456796213,
12.));
#140274=CARTESIAN_POINT('Ctrl Pts',(-65.1315686003516,-34.9088384918336,
0.));
#140275=CARTESIAN_POINT('Ctrl Pts',(-65.1315686003516,-34.9088384918336,
12.));
#140276=CARTESIAN_POINT('Ctrl Pts',(-65.1045361803121,-34.9067094130399,
0.));
#140277=CARTESIAN_POINT('Ctrl Pts',(-65.1045361803121,-34.9067094130399,
12.));
#140278=CARTESIAN_POINT('Ctrl Pts',(-65.0775416167085,-34.9045584960509,
0.));
#140279=CARTESIAN_POINT('Ctrl Pts',(-65.0775416167085,-34.9045584960509,
12.));
#140280=CARTESIAN_POINT('Ctrl Pts',(-65.0505849930171,-34.9023857937865,
0.));
#140281=CARTESIAN_POINT('Ctrl Pts',(-65.0505849930171,-34.9023857937865,
12.));
#140282=CARTESIAN_POINT('Ctrl Pts',(-65.0236663932328,-34.9001913596416,
0.));
#140283=CARTESIAN_POINT('Ctrl Pts',(-65.0236663932328,-34.9001913596416,
12.));
#140284=CARTESIAN_POINT('Ctrl Pts',(-64.9967859023212,-34.8979752478616,
0.));
#140285=CARTESIAN_POINT('Ctrl Pts',(-64.9967859023212,-34.8979752478616,
12.));
#140286=CARTESIAN_POINT('Ctrl Pts',(-64.9699436060169,-34.8957375133697,
0.));
#140287=CARTESIAN_POINT('Ctrl Pts',(-64.9699436060169,-34.8957375133697,
12.));
#140288=CARTESIAN_POINT('Ctrl Pts',(-64.9431395906337,-34.8934782116095,
0.));
#140289=CARTESIAN_POINT('Ctrl Pts',(-64.9431395906337,-34.8934782116095,
12.));
#140290=CARTESIAN_POINT('Ctrl Pts',(-64.9163739428605,-34.8911973983785,
0.));
#140291=CARTESIAN_POINT('Ctrl Pts',(-64.9163739428605,-34.8911973983785,
12.));
#140292=CARTESIAN_POINT('Ctrl Pts',(-64.8896467495757,-34.888895129681,
0.));
#140293=CARTESIAN_POINT('Ctrl Pts',(-64.8896467495757,-34.888895129681,
12.));
#140294=CARTESIAN_POINT('Ctrl Pts',(-64.8629580976063,-34.8865714615436,
0.));
#140295=CARTESIAN_POINT('Ctrl Pts',(-64.8629580976063,-34.8865714615436,
12.));
#140296=CARTESIAN_POINT('Ctrl Pts',(-64.8363080737377,-34.8842264500188,
0.));
#140297=CARTESIAN_POINT('Ctrl Pts',(-64.8363080737377,-34.8842264500188,
12.));
#140298=CARTESIAN_POINT('Ctrl Pts',(-64.8096967648307,-34.881860151273,
0.));
#140299=CARTESIAN_POINT('Ctrl Pts',(-64.8096967648307,-34.881860151273,
12.));
#140300=CARTESIAN_POINT('Ctrl Pts',(-64.7831242579028,-34.8794726216513,
0.));
#140301=CARTESIAN_POINT('Ctrl Pts',(-64.7831242579028,-34.8794726216513,
12.));
#140302=CARTESIAN_POINT('Ctrl Pts',(-64.7565906402151,-34.8770639177493,
0.));
#140303=CARTESIAN_POINT('Ctrl Pts',(-64.7565906402151,-34.8770639177493,
12.));
#140304=CARTESIAN_POINT('Ctrl Pts',(-64.7300959993653,-34.8746340964971,
0.));
#140305=CARTESIAN_POINT('Ctrl Pts',(-64.7300959993653,-34.8746340964971,
12.));
#140306=CARTESIAN_POINT('Ctrl Pts',(-64.7036404233306,-34.8721832151974,
0.));
#140307=CARTESIAN_POINT('Ctrl Pts',(-64.7036404233306,-34.8721832151974,
12.));
#140308=CARTESIAN_POINT('Ctrl Pts',(-64.6772240004228,-34.869711331479,
0.));
#140309=CARTESIAN_POINT('Ctrl Pts',(-64.6772240004228,-34.869711331479,
12.));
#140310=CARTESIAN_POINT('Ctrl Pts',(-64.6508468192599,-34.867218503272,
0.));
#140311=CARTESIAN_POINT('Ctrl Pts',(-64.6508468192599,-34.867218503272,
12.));
#140312=CARTESIAN_POINT('Ctrl Pts',(-64.6245089687277,-34.8647047887774,
0.));
#140313=CARTESIAN_POINT('Ctrl Pts',(-64.6245089687277,-34.8647047887774,
12.));
#140314=CARTESIAN_POINT('Ctrl Pts',(-64.5982105379383,-34.8621702464401,
0.));
#140315=CARTESIAN_POINT('Ctrl Pts',(-64.5982105379383,-34.8621702464401,
12.));
#140316=CARTESIAN_POINT('Ctrl Pts',(-64.5719516161927,-34.8596149349256,
0.));
#140317=CARTESIAN_POINT('Ctrl Pts',(-64.5719516161927,-34.8596149349256,
12.));
#140318=CARTESIAN_POINT('Ctrl Pts',(-64.5457322930088,-34.857038913134,
0.));
#140319=CARTESIAN_POINT('Ctrl Pts',(-64.5457322930088,-34.857038913134,
12.));
#140320=CARTESIAN_POINT('Ctrl Pts',(-64.5195526581407,-34.8544422402118,
0.));
#140321=CARTESIAN_POINT('Ctrl Pts',(-64.5195526581407,-34.8544422402118,
12.));
#140322=CARTESIAN_POINT('Ctrl Pts',(-64.4934128015985,-34.851824975568,
0.));
#140323=CARTESIAN_POINT('Ctrl Pts',(-64.4934128015985,-34.851824975568,
12.));
#140324=CARTESIAN_POINT('Ctrl Pts',(-64.4673128136625,-34.8491871788895,
0.));
#140325=CARTESIAN_POINT('Ctrl Pts',(-64.4673128136625,-34.8491871788895,
12.));
#140326=CARTESIAN_POINT('Ctrl Pts',(-64.4412527848969,-34.8465289101621,
0.));
#140327=CARTESIAN_POINT('Ctrl Pts',(-64.4412527848969,-34.8465289101621,
12.));
#140328=CARTESIAN_POINT('Ctrl Pts',(-64.4152328061515,-34.8438502296664,
0.));
#140329=CARTESIAN_POINT('Ctrl Pts',(-64.4152328061515,-34.8438502296664,
12.));
#140330=CARTESIAN_POINT('Ctrl Pts',(-64.3892529685607,-34.8411511979702,
0.));
#140331=CARTESIAN_POINT('Ctrl Pts',(-64.3892529685607,-34.8411511979702,
12.));
#140332=CARTESIAN_POINT('Ctrl Pts',(-64.3633133635382,-34.8384318759248,
0.));
#140333=CARTESIAN_POINT('Ctrl Pts',(-64.3633133635382,-34.8384318759248,
12.));
#140334=CARTESIAN_POINT('Ctrl Pts',(-64.3374140827711,-34.8356923246618,
0.));
#140335=CARTESIAN_POINT('Ctrl Pts',(-64.3374140827711,-34.8356923246618,
12.));
#140336=CARTESIAN_POINT('Ctrl Pts',(-64.3115552182062,-34.8329326055919,
0.));
#140337=CARTESIAN_POINT('Ctrl Pts',(-64.3115552182062,-34.8329326055919,
12.));
#140338=CARTESIAN_POINT('Ctrl Pts',(-64.285736862052,-34.8301527804054,
0.));
#140339=CARTESIAN_POINT('Ctrl Pts',(-64.285736862052,-34.8301527804054,
12.));
#140340=CARTESIAN_POINT('Ctrl Pts',(-64.2599591067916,-34.8273529110744,
0.));
#140341=CARTESIAN_POINT('Ctrl Pts',(-64.2599591067916,-34.8273529110744,
12.));
#140342=CARTESIAN_POINT('Ctrl Pts',(-64.234222045188,-34.8245330598559,
0.));
#140343=CARTESIAN_POINT('Ctrl Pts',(-64.234222045188,-34.8245330598559,
12.));
#140344=CARTESIAN_POINT('Ctrl Pts',(-64.2085257702884,-34.8216932892968,
0.));
#140345=CARTESIAN_POINT('Ctrl Pts',(-64.2085257702884,-34.8216932892968,
12.));
#140346=CARTESIAN_POINT('Ctrl Pts',(-64.1828703754236,-34.8188336622419,
0.));
#140347=CARTESIAN_POINT('Ctrl Pts',(-64.1828703754236,-34.8188336622419,
12.));
#140348=CARTESIAN_POINT('Ctrl Pts',(-64.1572559542086,-34.8159542418374,
0.));
#140349=CARTESIAN_POINT('Ctrl Pts',(-64.1572559542086,-34.8159542418374,
12.));
#140350=CARTESIAN_POINT('Ctrl Pts',(-64.1316826005506,-34.8130550915287,
0.));
#140351=CARTESIAN_POINT('Ctrl Pts',(-64.1316826005506,-34.8130550915287,
12.));
#140352=CARTESIAN_POINT('Ctrl Pts',(-64.1061504086515,-34.8101362750597,
0.));
#140353=CARTESIAN_POINT('Ctrl Pts',(-64.1061504086515,-34.8101362750597,
12.));
#140354=CARTESIAN_POINT('Ctrl Pts',(-64.0806594730085,-34.8071978564747,
0.));
#140355=CARTESIAN_POINT('Ctrl Pts',(-64.0806594730085,-34.8071978564747,
12.));
#140356=CARTESIAN_POINT('Ctrl Pts',(-64.0552098884095,-34.8042399001211,
0.));
#140357=CARTESIAN_POINT('Ctrl Pts',(-64.0552098884095,-34.8042399001211,
12.));
#140358=CARTESIAN_POINT('Ctrl Pts',(-64.0298017499294,-34.8012624706526,
0.));
#140359=CARTESIAN_POINT('Ctrl Pts',(-64.0298017499294,-34.8012624706526,
12.));
#140360=CARTESIAN_POINT('Ctrl Pts',(-64.0044351529402,-34.7982656330293,
0.));
#140361=CARTESIAN_POINT('Ctrl Pts',(-64.0044351529402,-34.7982656330293,
12.));
#140362=CARTESIAN_POINT('Ctrl Pts',(-63.9791101931162,-34.7952494525177,
0.));
#140363=CARTESIAN_POINT('Ctrl Pts',(-63.9791101931162,-34.7952494525177,
12.));
#140364=CARTESIAN_POINT('Ctrl Pts',(-63.9538269664366,-34.7922139946943,
0.));
#140365=CARTESIAN_POINT('Ctrl Pts',(-63.9538269664366,-34.7922139946943,
12.));
#140366=CARTESIAN_POINT('Ctrl Pts',(-63.9285855691845,-34.7891593254488,
0.));
#140367=CARTESIAN_POINT('Ctrl Pts',(-63.9285855691845,-34.7891593254488,
12.));
#140368=CARTESIAN_POINT('Ctrl Pts',(-63.9033860979435,-34.7860855109911,
0.));
#140369=CARTESIAN_POINT('Ctrl Pts',(-63.9033860979435,-34.7860855109911,
12.));
#140370=CARTESIAN_POINT('Ctrl Pts',(-63.8782286496062,-34.7829926178496,
0.));
#140371=CARTESIAN_POINT('Ctrl Pts',(-63.8782286496062,-34.7829926178496,
12.));
#140372=CARTESIAN_POINT('Ctrl Pts',(-63.8531133213793,-34.7798807128715,
0.));
#140373=CARTESIAN_POINT('Ctrl Pts',(-63.8531133213793,-34.7798807128715,
12.));
#140374=CARTESIAN_POINT('Ctrl Pts',(-63.8280402107856,-34.7767498632243,
0.));
#140375=CARTESIAN_POINT('Ctrl Pts',(-63.8280402107856,-34.7767498632243,
12.));
#140376=CARTESIAN_POINT('Ctrl Pts',(-63.8030094156639,-34.7736001363993,
0.));
#140377=CARTESIAN_POINT('Ctrl Pts',(-63.8030094156639,-34.7736001363993,
12.));
#140378=CARTESIAN_POINT('Ctrl Pts',(-63.778021034163,-34.7704316002171,
0.));
#140379=CARTESIAN_POINT('Ctrl Pts',(-63.778021034163,-34.7704316002171,
12.));
#140380=CARTESIAN_POINT('Ctrl Pts',(-63.7530751647494,-34.7672443228275,
0.));
#140381=CARTESIAN_POINT('Ctrl Pts',(-63.7530751647494,-34.7672443228275,
12.));
#140382=CARTESIAN_POINT('Ctrl Pts',(-63.7281719062149,-34.76403837271,0.));
#140383=CARTESIAN_POINT('Ctrl Pts',(-63.7281719062149,-34.76403837271,12.));
#140384=CARTESIAN_POINT('Ctrl Pts',(-63.7033113576785,-34.7608138186759,
0.));
#140385=CARTESIAN_POINT('Ctrl Pts',(-63.7033113576785,-34.7608138186759,
12.));
#140386=CARTESIAN_POINT('Ctrl Pts',(-63.6784936185885,-34.7575707298713,
0.));
#140387=CARTESIAN_POINT('Ctrl Pts',(-63.6784936185885,-34.7575707298713,
12.));
#140388=CARTESIAN_POINT('Ctrl Pts',(-63.6537187887159,-34.7543091757833,
0.));
#140389=CARTESIAN_POINT('Ctrl Pts',(-63.6537187887159,-34.7543091757833,
12.));
#140390=CARTESIAN_POINT('Ctrl Pts',(-63.6289869681604,-34.7510292262406,
0.));
#140391=CARTESIAN_POINT('Ctrl Pts',(-63.6289869681604,-34.7510292262406,
12.));
#140392=CARTESIAN_POINT('Ctrl Pts',(-63.6042982573588,-34.7477309514136,
0.));
#140393=CARTESIAN_POINT('Ctrl Pts',(-63.6042982573588,-34.7477309514136,
12.));
#140394=CARTESIAN_POINT('Ctrl Pts',(-63.5796527570871,-34.744414421816,
0.));
#140395=CARTESIAN_POINT('Ctrl Pts',(-63.5796527570871,-34.744414421816,
12.));
#140396=CARTESIAN_POINT('Ctrl Pts',(-63.5550505684626,-34.7410797083081,
0.));
#140397=CARTESIAN_POINT('Ctrl Pts',(-63.5550505684626,-34.7410797083081,
12.));
#140398=CARTESIAN_POINT('Ctrl Pts',(-63.5304917929386,-34.7377268821025,
0.));
#140399=CARTESIAN_POINT('Ctrl Pts',(-63.5304917929386,-34.7377268821025,
12.));
#140400=CARTESIAN_POINT('Ctrl Pts',(-63.505976532309,-34.7343560147667,
0.));
#140401=CARTESIAN_POINT('Ctrl Pts',(-63.505976532309,-34.7343560147667,
12.));
#140402=CARTESIAN_POINT('Ctrl Pts',(-63.4815048887165,-34.7309671782214,
0.));
#140403=CARTESIAN_POINT('Ctrl Pts',(-63.4815048887165,-34.7309671782214,
12.));
#140404=CARTESIAN_POINT('Ctrl Pts',(-63.4570769646569,-34.7275604447438,
0.));
#140405=CARTESIAN_POINT('Ctrl Pts',(-63.4570769646569,-34.7275604447438,
12.));
#140406=CARTESIAN_POINT('Ctrl Pts',(-63.4326928629795,-34.7241358869701,
0.));
#140407=CARTESIAN_POINT('Ctrl Pts',(-63.4326928629795,-34.7241358869701,
12.));
#140408=CARTESIAN_POINT('Ctrl Pts',(-63.4083526868836,-34.7206935779007,
0.));
#140409=CARTESIAN_POINT('Ctrl Pts',(-63.4083526868836,-34.7206935779007,
12.));
#140410=CARTESIAN_POINT('Ctrl Pts',(-63.3840565399208,-34.7172335909038,
0.));
#140411=CARTESIAN_POINT('Ctrl Pts',(-63.3840565399208,-34.7172335909038,
12.));
#140412=CARTESIAN_POINT('Ctrl Pts',(-63.3598045260053,-34.7137559997146,
0.));
#140413=CARTESIAN_POINT('Ctrl Pts',(-63.3598045260053,-34.7137559997146,
12.));
#140414=CARTESIAN_POINT('Ctrl Pts',(-63.3355967494171,-34.7102608784374,
0.));
#140415=CARTESIAN_POINT('Ctrl Pts',(-63.3355967494171,-34.7102608784374,
12.));
#140416=CARTESIAN_POINT('Ctrl Pts',(-63.3114333148048,-34.7067483015491,
0.));
#140417=CARTESIAN_POINT('Ctrl Pts',(-63.3114333148048,-34.7067483015491,
12.));
#140418=CARTESIAN_POINT('Ctrl Pts',(-63.2873143271807,-34.703218343904,
0.));
#140419=CARTESIAN_POINT('Ctrl Pts',(-63.2873143271807,-34.703218343904,
12.));
#140420=CARTESIAN_POINT('Ctrl Pts',(-63.2632398919225,-34.6996710807378,
0.));
#140421=CARTESIAN_POINT('Ctrl Pts',(-63.2632398919225,-34.6996710807378,
12.));
#140422=CARTESIAN_POINT('Ctrl Pts',(-63.2392101147847,-34.6961065876666,
0.));
#140423=CARTESIAN_POINT('Ctrl Pts',(-63.2392101147847,-34.6961065876666,
12.));
#140424=CARTESIAN_POINT('Ctrl Pts',(-63.2152251019012,-34.6925249406897,
0.));
#140425=CARTESIAN_POINT('Ctrl Pts',(-63.2152251019012,-34.6925249406897,
12.));
#140426=CARTESIAN_POINT('Ctrl Pts',(-63.1912849597887,-34.6889262161924,
0.));
#140427=CARTESIAN_POINT('Ctrl Pts',(-63.1912849597887,-34.6889262161924,
12.));
#140428=CARTESIAN_POINT('Ctrl Pts',(-63.1673897953429,-34.6853104909518,
0.));
#140429=CARTESIAN_POINT('Ctrl Pts',(-63.1673897953429,-34.6853104909518,
12.));
#140430=CARTESIAN_POINT('Ctrl Pts',(-63.1435397158388,-34.6816778421402,
0.));
#140431=CARTESIAN_POINT('Ctrl Pts',(-63.1435397158388,-34.6816778421402,
12.));
#140432=CARTESIAN_POINT('Ctrl Pts',(-63.119734828943,-34.6780283473252,
0.));
#140433=CARTESIAN_POINT('Ctrl Pts',(-63.119734828943,-34.6780283473252,
12.));
#140434=CARTESIAN_POINT('Ctrl Pts',(-63.0959752427168,-34.674362084472,
0.));
#140435=CARTESIAN_POINT('Ctrl Pts',(-63.0959752427168,-34.674362084472,
12.));
#140436=CARTESIAN_POINT('Ctrl Pts',(-63.0722610656194,-34.670679131947,
0.));
#140437=CARTESIAN_POINT('Ctrl Pts',(-63.0722610656194,-34.670679131947,
12.));
#140438=CARTESIAN_POINT('Ctrl Pts',(-63.0485924065045,-34.6669795685228,
0.));
#140439=CARTESIAN_POINT('Ctrl Pts',(-63.0485924065045,-34.6669795685228,
12.));
#140440=CARTESIAN_POINT('Ctrl Pts',(-63.0249693746208,-34.6632634733824,
0.));
#140441=CARTESIAN_POINT('Ctrl Pts',(-63.0249693746208,-34.6632634733824,
12.));
#140442=CARTESIAN_POINT('Ctrl Pts',(-63.0013920796235,-34.6595309261191,
0.));
#140443=CARTESIAN_POINT('Ctrl Pts',(-63.0013920796235,-34.6595309261191,
12.));
#140444=CARTESIAN_POINT('Ctrl Pts',(-62.9778606315783,-34.6557820067393,
0.));
#140445=CARTESIAN_POINT('Ctrl Pts',(-62.9778606315783,-34.6557820067393,
12.));
#140446=CARTESIAN_POINT('Ctrl Pts',(-62.9543751409646,-34.6520167956655,
0.));
#140447=CARTESIAN_POINT('Ctrl Pts',(-62.9543751409646,-34.6520167956655,
12.));
#140448=CARTESIAN_POINT('Ctrl Pts',(-62.9309357186717,-34.6482353737424,
0.));
#140449=CARTESIAN_POINT('Ctrl Pts',(-62.9309357186717,-34.6482353737424,
12.));
#140450=CARTESIAN_POINT('Ctrl Pts',(-62.9075424760015,-34.644437822241,
0.));
#140451=CARTESIAN_POINT('Ctrl Pts',(-62.9075424760015,-34.644437822241,
12.));
#140452=CARTESIAN_POINT('Ctrl Pts',(-62.8841955246794,-34.6406242228592,
0.));
#140453=CARTESIAN_POINT('Ctrl Pts',(-62.8841955246794,-34.6406242228592,
12.));
#140454=CARTESIAN_POINT('Ctrl Pts',(-62.8608949768571,-34.6367946577235,
0.));
#140455=CARTESIAN_POINT('Ctrl Pts',(-62.8608949768571,-34.6367946577235,
12.));
#140456=CARTESIAN_POINT('Ctrl Pts',(-62.8376409451175,-34.6329492093935,
0.));
#140457=CARTESIAN_POINT('Ctrl Pts',(-62.8376409451175,-34.6329492093935,
12.));
#140458=CARTESIAN_POINT('Ctrl Pts',(-62.8144335424697,-34.6290879608673,
0.));
#140459=CARTESIAN_POINT('Ctrl Pts',(-62.8144335424697,-34.6290879608673,
12.));
#140460=CARTESIAN_POINT('Ctrl Pts',(-62.7912728823518,-34.6252109955853,
0.));
#140461=CARTESIAN_POINT('Ctrl Pts',(-62.7912728823518,-34.6252109955853,
12.));
#140462=CARTESIAN_POINT('Ctrl Pts',(-62.7681590786429,-34.6213183974317,
0.));
#140463=CARTESIAN_POINT('Ctrl Pts',(-62.7681590786429,-34.6213183974317,
12.));
#140464=CARTESIAN_POINT('Ctrl Pts',(-62.7450922456676,-34.6174102507375,
0.));
#140465=CARTESIAN_POINT('Ctrl Pts',(-62.7450922456676,-34.6174102507375,
12.));
#140466=CARTESIAN_POINT('Ctrl Pts',(-62.7220724981994,-34.6134866402837,
0.));
#140467=CARTESIAN_POINT('Ctrl Pts',(-62.7220724981994,-34.6134866402837,
12.));
#140468=CARTESIAN_POINT('Ctrl Pts',(-62.6990999514563,-34.6095476513077,
0.));
#140469=CARTESIAN_POINT('Ctrl Pts',(-62.6990999514563,-34.6095476513077,
12.));
#140470=CARTESIAN_POINT('Ctrl Pts',(-62.6761747211037,-34.6055933695069,
0.));
#140471=CARTESIAN_POINT('Ctrl Pts',(-62.6761747211037,-34.6055933695069,
12.));
#140472=CARTESIAN_POINT('Ctrl Pts',(-62.6532969232657,-34.6016238810398,
0.));
#140473=CARTESIAN_POINT('Ctrl Pts',(-62.6532969232657,-34.6016238810398,
12.));
#140474=CARTESIAN_POINT('Ctrl Pts',(-62.6304666745306,-34.5976392725296,
0.));
#140475=CARTESIAN_POINT('Ctrl Pts',(-62.6304666745306,-34.5976392725296,
12.));
#140476=CARTESIAN_POINT('Ctrl Pts',(-62.6076840919536,-34.5936396310679,
0.));
#140477=CARTESIAN_POINT('Ctrl Pts',(-62.6076840919536,-34.5936396310679,
12.));
#140478=CARTESIAN_POINT('Ctrl Pts',(-62.5849492930533,-34.5896250442216,
0.));
#140479=CARTESIAN_POINT('Ctrl Pts',(-62.5849492930533,-34.5896250442216,
12.));
#140480=CARTESIAN_POINT('Ctrl Pts',(-62.562262395816,-34.5855956000363,
0.));
#140481=CARTESIAN_POINT('Ctrl Pts',(-62.562262395816,-34.5855956000363,
12.));
#140482=CARTESIAN_POINT('Ctrl Pts',(-62.5396235187079,-34.5815513870377,
0.));
#140483=CARTESIAN_POINT('Ctrl Pts',(-62.5396235187079,-34.5815513870377,
12.));
#140484=CARTESIAN_POINT('Ctrl Pts',(-62.5170327806781,-34.5774924942355,
0.));
#140485=CARTESIAN_POINT('Ctrl Pts',(-62.5170327806781,-34.5774924942355,
12.));
#140486=CARTESIAN_POINT('Ctrl Pts',(-62.4944903011628,-34.5734190111272,
0.));
#140487=CARTESIAN_POINT('Ctrl Pts',(-62.4944903011628,-34.5734190111272,
12.));
#140488=CARTESIAN_POINT('Ctrl Pts',(-62.4719962000808,-34.5693310277051,
0.));
#140489=CARTESIAN_POINT('Ctrl Pts',(-62.4719962000808,-34.5693310277051,
12.));
#140490=CARTESIAN_POINT('Ctrl Pts',(-62.4495505978393,-34.5652286344593,
0.));
#140491=CARTESIAN_POINT('Ctrl Pts',(-62.4495505978393,-34.5652286344593,
12.));
#140492=CARTESIAN_POINT('Ctrl Pts',(-62.4271536153459,-34.5611119223798,
0.));
#140493=CARTESIAN_POINT('Ctrl Pts',(-62.4271536153459,-34.5611119223798,
12.));
#140494=CARTESIAN_POINT('Ctrl Pts',(-62.4048053740127,-34.5569809829613,
0.));
#140495=CARTESIAN_POINT('Ctrl Pts',(-62.4048053740127,-34.5569809829613,
12.));
#140496=CARTESIAN_POINT('Ctrl Pts',(-62.3825059957601,-34.5528359082075,
0.));
#140497=CARTESIAN_POINT('Ctrl Pts',(-62.3825059957601,-34.5528359082075,
12.));
#140498=CARTESIAN_POINT('Ctrl Pts',(-62.3602556030127,-34.5486767906384,
0.));
#140499=CARTESIAN_POINT('Ctrl Pts',(-62.3602556030127,-34.5486767906384,
12.));
#140500=CARTESIAN_POINT('Ctrl Pts',(-62.338054318708,-34.5445037232936,
0.));
#140501=CARTESIAN_POINT('Ctrl Pts',(-62.338054318708,-34.5445037232936,
12.));
#140502=CARTESIAN_POINT('Ctrl Pts',(-62.3159022663058,-34.5403167997337,
0.));
#140503=CARTESIAN_POINT('Ctrl Pts',(-62.3159022663058,-34.5403167997337,
12.));
#140504=CARTESIAN_POINT('Ctrl Pts',(-62.2937995697925,-34.5361161140449,
0.));
#140505=CARTESIAN_POINT('Ctrl Pts',(-62.2937995697925,-34.5361161140449,
12.));
#140506=CARTESIAN_POINT('Ctrl Pts',(-62.2717463536827,-34.5319017608433,
0.));
#140507=CARTESIAN_POINT('Ctrl Pts',(-62.2717463536827,-34.5319017608433,
12.));
#140508=CARTESIAN_POINT('Ctrl Pts',(-62.2497427430135,-34.5276738352808,
0.));
#140509=CARTESIAN_POINT('Ctrl Pts',(-62.2497427430135,-34.5276738352808,
12.));
#140510=CARTESIAN_POINT('Ctrl Pts',(-62.2277888633576,-34.523432433049,
0.));
#140511=CARTESIAN_POINT('Ctrl Pts',(-62.2277888633576,-34.523432433049,
12.));
#140512=CARTESIAN_POINT('Ctrl Pts',(-62.2058848408347,-34.5191776503842,
0.));
#140513=CARTESIAN_POINT('Ctrl Pts',(-62.2058848408347,-34.5191776503842,
12.));
#140514=CARTESIAN_POINT('Ctrl Pts',(-62.1840308021171,-34.5149095840729,
0.));
#140515=CARTESIAN_POINT('Ctrl Pts',(-62.1840308021171,-34.5149095840729,
12.));
#140516=CARTESIAN_POINT('Ctrl Pts',(-62.1622268744336,-34.5106283314594,
0.));
#140517=CARTESIAN_POINT('Ctrl Pts',(-62.1622268744336,-34.5106283314594,
12.));
#140518=CARTESIAN_POINT('Ctrl Pts',(-62.1404731855686,-34.5063339904533,
0.));
#140519=CARTESIAN_POINT('Ctrl Pts',(-62.1404731855686,-34.5063339904533,
12.));
#140520=CARTESIAN_POINT('Ctrl Pts',(-62.1187698638705,-34.5020266595292,
0.));
#140521=CARTESIAN_POINT('Ctrl Pts',(-62.1187698638705,-34.5020266595292,
12.));
#140522=CARTESIAN_POINT('Ctrl Pts',(-62.0971170382565,-34.4977064377281,
0.));
#140523=CARTESIAN_POINT('Ctrl Pts',(-62.0971170382565,-34.4977064377281,
12.));
#140524=CARTESIAN_POINT('Ctrl Pts',(-62.0755148382136,-34.4933734246592,
0.));
#140525=CARTESIAN_POINT('Ctrl Pts',(-62.0755148382136,-34.4933734246592,
12.));
#140526=CARTESIAN_POINT('Ctrl Pts',(-62.0539633937944,-34.4890277205041,
0.));
#140527=CARTESIAN_POINT('Ctrl Pts',(-62.0539633937944,-34.4890277205041,
12.));
#140528=CARTESIAN_POINT('Ctrl Pts',(-62.0324628356152,-34.4846694260205,
0.));
#140529=CARTESIAN_POINT('Ctrl Pts',(-62.0324628356152,-34.4846694260205,
12.));
#140530=CARTESIAN_POINT('Ctrl Pts',(-62.0110132948807,-34.4802986425535,
0.));
#140531=CARTESIAN_POINT('Ctrl Pts',(-62.0110132948807,-34.4802986425535,
12.));
#140532=CARTESIAN_POINT('Ctrl Pts',(-61.9896149034009,-34.4759154720477,
0.));
#140533=CARTESIAN_POINT('Ctrl Pts',(-61.9896149034009,-34.4759154720477,
12.));
#140534=CARTESIAN_POINT('Ctrl Pts',(-61.9682677936048,-34.4715200170589,
0.));
#140535=CARTESIAN_POINT('Ctrl Pts',(-61.9682677936048,-34.4715200170589,
12.));
#140536=CARTESIAN_POINT('Ctrl Pts',(-61.9469720985512,-34.4671123807706,
0.));
#140537=CARTESIAN_POINT('Ctrl Pts',(-61.9469720985512,-34.4671123807706,
12.));
#140538=CARTESIAN_POINT('Ctrl Pts',(-61.9257279519283,-34.462692666996,
0.));
#140539=CARTESIAN_POINT('Ctrl Pts',(-61.9257279519283,-34.462692666996,
12.));
#140540=CARTESIAN_POINT('Ctrl Pts',(-61.9045354880424,-34.4582609801625,
0.));
#140541=CARTESIAN_POINT('Ctrl Pts',(-61.9045354880424,-34.4582609801625,
12.));
#140542=CARTESIAN_POINT('Ctrl Pts',(-61.883394841802,-34.4538174253009,
0.));
#140543=CARTESIAN_POINT('Ctrl Pts',(-61.883394841802,-34.4538174253009,
12.));
#140544=CARTESIAN_POINT('Ctrl Pts',(-61.862306148703,-34.4493621080367,
0.));
#140545=CARTESIAN_POINT('Ctrl Pts',(-61.862306148703,-34.4493621080367,
12.));
#140546=CARTESIAN_POINT('Ctrl Pts',(-61.8412695447951,-34.4448951345753,
0.));
#140547=CARTESIAN_POINT('Ctrl Pts',(-61.8412695447951,-34.4448951345753,
12.));
#140548=CARTESIAN_POINT('Ctrl Pts',(-61.8202851667247,-34.4404166117313,
0.));
#140549=CARTESIAN_POINT('Ctrl Pts',(-61.8202851667247,-34.4404166117313,
12.));
#140550=CARTESIAN_POINT('Ctrl Pts',(-61.7993531518052,-34.4359266469757,
0.));
#140551=CARTESIAN_POINT('Ctrl Pts',(-61.7993531518052,-34.4359266469757,
12.));
#140552=CARTESIAN_POINT('Ctrl Pts',(-61.7784736380727,-34.4314253484791,
0.));
#140553=CARTESIAN_POINT('Ctrl Pts',(-61.7784736380727,-34.4314253484791,
12.));
#140554=CARTESIAN_POINT('Ctrl Pts',(-61.7576467643419,-34.4269128251569,
0.));
#140555=CARTESIAN_POINT('Ctrl Pts',(-61.7576467643419,-34.4269128251569,
12.));
#140556=CARTESIAN_POINT('Ctrl Pts',(-61.7368726702573,-34.4223891867166,
0.));
#140557=CARTESIAN_POINT('Ctrl Pts',(-61.7368726702573,-34.4223891867166,
12.));
#140558=CARTESIAN_POINT('Ctrl Pts',(-61.7161514961892,-34.4178545435753,
0.));
#140559=CARTESIAN_POINT('Ctrl Pts',(-61.7161514961892,-34.4178545435753,
12.));
#140560=CARTESIAN_POINT('Ctrl Pts',(-61.6954833831157,-34.4133090067696,
0.));
#140561=CARTESIAN_POINT('Ctrl Pts',(-61.6954833831157,-34.4133090067696,
12.));
#140562=CARTESIAN_POINT('Ctrl Pts',(-61.674868472521,-34.4087526878815,
0.));
#140563=CARTESIAN_POINT('Ctrl Pts',(-61.674868472521,-34.4087526878815,
12.));
#140564=CARTESIAN_POINT('Ctrl Pts',(-61.6543069062436,-34.4041856989328,
0.));
#140565=CARTESIAN_POINT('Ctrl Pts',(-61.6543069062436,-34.4041856989328,
12.));
#140566=CARTESIAN_POINT('Ctrl Pts',(-61.6337988264586,-34.399608152377,
0.));
#140567=CARTESIAN_POINT('Ctrl Pts',(-61.6337988264586,-34.399608152377,
12.));
#140568=CARTESIAN_POINT('Ctrl Pts',(-61.6133443760168,-34.3950201613446,
0.));
#140569=CARTESIAN_POINT('Ctrl Pts',(-61.6133443760168,-34.3950201613446,
12.));
#140570=CARTESIAN_POINT('Ctrl Pts',(-61.5929436987419,-34.3904218398642,
0.));
#140571=CARTESIAN_POINT('Ctrl Pts',(-61.5929436987419,-34.3904218398642,
12.));
#140572=CARTESIAN_POINT('Ctrl Pts',(-61.5725969396817,-34.3858133030511,
0.));
#140573=CARTESIAN_POINT('Ctrl Pts',(-61.5725969396817,-34.3858133030511,
12.));
#140574=CARTESIAN_POINT('Ctrl Pts',(-61.5523042455127,-34.3811946674179,
0.));
#140575=CARTESIAN_POINT('Ctrl Pts',(-61.5523042455127,-34.3811946674179,
12.));
#140576=CARTESIAN_POINT('Ctrl Pts',(-61.5320657642601,-34.3765660506659,
0.));
#140577=CARTESIAN_POINT('Ctrl Pts',(-61.5320657642601,-34.3765660506659,
12.));
#140578=CARTESIAN_POINT('Ctrl Pts',(-61.511881644541,-34.3719275711179,
0.));
#140579=CARTESIAN_POINT('Ctrl Pts',(-61.511881644541,-34.3719275711179,
12.));
#140580=CARTESIAN_POINT('Ctrl Pts',(-61.4917520349276,-34.3672793472463,
0.));
#140581=CARTESIAN_POINT('Ctrl Pts',(-61.4917520349276,-34.3672793472463,
12.));
#140582=CARTESIAN_POINT('Ctrl Pts',(-61.4716770832924,-34.3626214971903,
0.));
#140583=CARTESIAN_POINT('Ctrl Pts',(-61.4716770832924,-34.3626214971903,
12.));
#140584=CARTESIAN_POINT('Ctrl Pts',(-61.4516569360499,-34.357954138202,
0.));
#140585=CARTESIAN_POINT('Ctrl Pts',(-61.4516569360499,-34.357954138202,
12.));
#140586=CARTESIAN_POINT('Ctrl Pts',(-61.4316917395959,-34.3532773877112,
0.));
#140587=CARTESIAN_POINT('Ctrl Pts',(-61.4316917395959,-34.3532773877112,
12.));
#140588=CARTESIAN_POINT('Ctrl Pts',(-61.4117816420251,-34.3485913645991,
0.));
#140589=CARTESIAN_POINT('Ctrl Pts',(-61.4117816420251,-34.3485913645991,
12.));
#140590=CARTESIAN_POINT('Ctrl Pts',(-61.3919267945293,-34.34389619024,0.));
#140591=CARTESIAN_POINT('Ctrl Pts',(-61.3919267945293,-34.34389619024,12.));
#140592=CARTESIAN_POINT('Ctrl Pts',(-61.3721273534222,-34.339191990012,
0.));
#140593=CARTESIAN_POINT('Ctrl Pts',(-61.3721273534222,-34.339191990012,
12.));
#140594=CARTESIAN_POINT('Ctrl Pts',(-61.3523834803144,-34.3344788934337,
0.));
#140595=CARTESIAN_POINT('Ctrl Pts',(-61.3523834803144,-34.3344788934337,
12.));
#140596=CARTESIAN_POINT('Ctrl Pts',(-61.3326953378817,-34.3297570310126,
0.));
#140597=CARTESIAN_POINT('Ctrl Pts',(-61.3326953378817,-34.3297570310126,
12.));
#140598=CARTESIAN_POINT('Ctrl Pts',(-61.3130630861375,-34.3250265314761,
0.));
#140599=CARTESIAN_POINT('Ctrl Pts',(-61.3130630861375,-34.3250265314761,
12.));
#140600=CARTESIAN_POINT('Ctrl Pts',(-61.2934868791875,-34.3202875193629,
0.));
#140601=CARTESIAN_POINT('Ctrl Pts',(-61.2934868791875,-34.3202875193629,
12.));
#140602=CARTESIAN_POINT('Ctrl Pts',(-61.2739668600415,-34.3155401111776,
0.));
#140603=CARTESIAN_POINT('Ctrl Pts',(-61.2739668600415,-34.3155401111776,
12.));
#140604=CARTESIAN_POINT('Ctrl Pts',(-61.2545031656196,-34.3107844191081,
0.));
#140605=CARTESIAN_POINT('Ctrl Pts',(-61.2545031656196,-34.3107844191081,
12.));
#140606=CARTESIAN_POINT('Ctrl Pts',(-61.2350959366987,-34.3060205584093,
0.));
#140607=CARTESIAN_POINT('Ctrl Pts',(-61.2350959366987,-34.3060205584093,
12.));
#140608=CARTESIAN_POINT('Ctrl Pts',(-61.2157453259107,-34.3012486533474,
0.));
#140609=CARTESIAN_POINT('Ctrl Pts',(-61.2157453259107,-34.3012486533474,
12.));
#140610=CARTESIAN_POINT('Ctrl Pts',(-61.1964515073823,-34.296468844362,
0.));
#140611=CARTESIAN_POINT('Ctrl Pts',(-61.1964515073823,-34.296468844362,
12.));
#140612=CARTESIAN_POINT('Ctrl Pts',(-61.1772146833083,-34.2916812929675,
0.));
#140613=CARTESIAN_POINT('Ctrl Pts',(-61.1772146833083,-34.2916812929675,
12.));
#140614=CARTESIAN_POINT('Ctrl Pts',(-61.15803506354,-34.2868861666301,0.));
#140615=CARTESIAN_POINT('Ctrl Pts',(-61.15803506354,-34.2868861666301,12.));
#140616=CARTESIAN_POINT('Ctrl Pts',(-61.1389128461815,-34.2820836244425,
0.));
#140617=CARTESIAN_POINT('Ctrl Pts',(-61.1389128461815,-34.2820836244425,
12.));
#140618=CARTESIAN_POINT('Ctrl Pts',(-61.119848199783,-34.2772738038811,
0.));
#140619=CARTESIAN_POINT('Ctrl Pts',(-61.119848199783,-34.2772738038811,
12.));
#140620=CARTESIAN_POINT('Ctrl Pts',(-61.100841240023,-34.2724568037374,
0.));
#140621=CARTESIAN_POINT('Ctrl Pts',(-61.100841240023,-34.2724568037374,
12.));
#140622=CARTESIAN_POINT('Ctrl Pts',(-61.0818920286644,-34.2676326825846,
0.));
#140623=CARTESIAN_POINT('Ctrl Pts',(-61.0818920286644,-34.2676326825846,
12.));
#140624=CARTESIAN_POINT('Ctrl Pts',(-61.0667788793594,-34.2637677132139,
0.));
#140625=CARTESIAN_POINT('Ctrl Pts',(-61.0667788793594,-34.2637677132139,
12.));
#140626=CARTESIAN_POINT('Ctrl Pts',(-61.0554700177206,-34.2608658001761,
0.));
#140627=CARTESIAN_POINT('Ctrl Pts',(-61.0554700177206,-34.2608658001761,
12.));
#140628=CARTESIAN_POINT('Ctrl Pts',(-61.0479423318803,-34.2589297755482,
0.));
#140629=CARTESIAN_POINT('Ctrl Pts',(-61.0479423318803,-34.2589297755482,
12.));
#140630=CARTESIAN_POINT('Ctrl Pts',(-61.0441813777723,-34.2579614092497,
0.));
#140631=CARTESIAN_POINT('Ctrl Pts',(-61.0441813777723,-34.2579614092497,
12.));
#140632=CARTESIAN_POINT('',(-61.0441813777723,-34.2579614092497,12.));
#140633=CARTESIAN_POINT('Ctrl Pts',(-61.0441813777723,-34.2579614092497,
12.));
#140634=CARTESIAN_POINT('Ctrl Pts',(-61.0479423318803,-34.2589297755482,
12.));
#140635=CARTESIAN_POINT('Ctrl Pts',(-61.0554700177206,-34.2608658001761,
12.));
#140636=CARTESIAN_POINT('Ctrl Pts',(-61.0667788793594,-34.2637677132139,
12.));
#140637=CARTESIAN_POINT('Ctrl Pts',(-61.0818920286644,-34.2676326825846,
12.));
#140638=CARTESIAN_POINT('Ctrl Pts',(-61.100841240023,-34.2724568037374,
12.));
#140639=CARTESIAN_POINT('Ctrl Pts',(-61.119848199783,-34.2772738038811,
12.));
#140640=CARTESIAN_POINT('Ctrl Pts',(-61.1389128461815,-34.2820836244425,
12.));
#140641=CARTESIAN_POINT('Ctrl Pts',(-61.15803506354,-34.2868861666301,12.));
#140642=CARTESIAN_POINT('Ctrl Pts',(-61.1772146833083,-34.2916812929675,
12.));
#140643=CARTESIAN_POINT('Ctrl Pts',(-61.1964515073823,-34.296468844362,
12.));
#140644=CARTESIAN_POINT('Ctrl Pts',(-61.2157453259107,-34.3012486533474,
12.));
#140645=CARTESIAN_POINT('Ctrl Pts',(-61.2350959366987,-34.3060205584093,
12.));
#140646=CARTESIAN_POINT('Ctrl Pts',(-61.2545031656196,-34.3107844191081,
12.));
#140647=CARTESIAN_POINT('Ctrl Pts',(-61.2739668600415,-34.3155401111776,
12.));
#140648=CARTESIAN_POINT('Ctrl Pts',(-61.2934868791875,-34.3202875193629,
12.));
#140649=CARTESIAN_POINT('Ctrl Pts',(-61.3130630861375,-34.3250265314761,
12.));
#140650=CARTESIAN_POINT('Ctrl Pts',(-61.3326953378817,-34.3297570310126,
12.));
#140651=CARTESIAN_POINT('Ctrl Pts',(-61.3523834803144,-34.3344788934337,
12.));
#140652=CARTESIAN_POINT('Ctrl Pts',(-61.3721273534222,-34.339191990012,
12.));
#140653=CARTESIAN_POINT('Ctrl Pts',(-61.3919267945293,-34.34389619024,12.));
#140654=CARTESIAN_POINT('Ctrl Pts',(-61.4117816420251,-34.3485913645991,
12.));
#140655=CARTESIAN_POINT('Ctrl Pts',(-61.4316917395959,-34.3532773877112,
12.));
#140656=CARTESIAN_POINT('Ctrl Pts',(-61.4516569360499,-34.357954138202,
12.));
#140657=CARTESIAN_POINT('Ctrl Pts',(-61.4716770832924,-34.3626214971903,
12.));
#140658=CARTESIAN_POINT('Ctrl Pts',(-61.4917520349276,-34.3672793472463,
12.));
#140659=CARTESIAN_POINT('Ctrl Pts',(-61.511881644541,-34.3719275711179,
12.));
#140660=CARTESIAN_POINT('Ctrl Pts',(-61.5320657642601,-34.3765660506659,
12.));
#140661=CARTESIAN_POINT('Ctrl Pts',(-61.5523042455127,-34.3811946674179,
12.));
#140662=CARTESIAN_POINT('Ctrl Pts',(-61.5725969396817,-34.3858133030511,
12.));
#140663=CARTESIAN_POINT('Ctrl Pts',(-61.5929436987419,-34.3904218398642,
12.));
#140664=CARTESIAN_POINT('Ctrl Pts',(-61.6133443760168,-34.3950201613446,
12.));
#140665=CARTESIAN_POINT('Ctrl Pts',(-61.6337988264586,-34.399608152377,
12.));
#140666=CARTESIAN_POINT('Ctrl Pts',(-61.6543069062436,-34.4041856989328,
12.));
#140667=CARTESIAN_POINT('Ctrl Pts',(-61.674868472521,-34.4087526878815,
12.));
#140668=CARTESIAN_POINT('Ctrl Pts',(-61.6954833831157,-34.4133090067696,
12.));
#140669=CARTESIAN_POINT('Ctrl Pts',(-61.7161514961892,-34.4178545435753,
12.));
#140670=CARTESIAN_POINT('Ctrl Pts',(-61.7368726702573,-34.4223891867166,
12.));
#140671=CARTESIAN_POINT('Ctrl Pts',(-61.7576467643419,-34.4269128251569,
12.));
#140672=CARTESIAN_POINT('Ctrl Pts',(-61.7784736380727,-34.4314253484791,
12.));
#140673=CARTESIAN_POINT('Ctrl Pts',(-61.7993531518052,-34.4359266469757,
12.));
#140674=CARTESIAN_POINT('Ctrl Pts',(-61.8202851667247,-34.4404166117313,
12.));
#140675=CARTESIAN_POINT('Ctrl Pts',(-61.8412695447951,-34.4448951345753,
12.));
#140676=CARTESIAN_POINT('Ctrl Pts',(-61.862306148703,-34.4493621080367,
12.));
#140677=CARTESIAN_POINT('Ctrl Pts',(-61.883394841802,-34.4538174253009,
12.));
#140678=CARTESIAN_POINT('Ctrl Pts',(-61.9045354880424,-34.4582609801625,
12.));
#140679=CARTESIAN_POINT('Ctrl Pts',(-61.9257279519283,-34.462692666996,
12.));
#140680=CARTESIAN_POINT('Ctrl Pts',(-61.9469720985512,-34.4671123807706,
12.));
#140681=CARTESIAN_POINT('Ctrl Pts',(-61.9682677936048,-34.4715200170589,
12.));
#140682=CARTESIAN_POINT('Ctrl Pts',(-61.9896149034009,-34.4759154720477,
12.));
#140683=CARTESIAN_POINT('Ctrl Pts',(-62.0110132948807,-34.4802986425535,
12.));
#140684=CARTESIAN_POINT('Ctrl Pts',(-62.0324628356152,-34.4846694260205,
12.));
#140685=CARTESIAN_POINT('Ctrl Pts',(-62.0539633937944,-34.4890277205041,
12.));
#140686=CARTESIAN_POINT('Ctrl Pts',(-62.0755148382136,-34.4933734246592,
12.));
#140687=CARTESIAN_POINT('Ctrl Pts',(-62.0971170382565,-34.4977064377281,
12.));
#140688=CARTESIAN_POINT('Ctrl Pts',(-62.1187698638705,-34.5020266595292,
12.));
#140689=CARTESIAN_POINT('Ctrl Pts',(-62.1404731855686,-34.5063339904533,
12.));
#140690=CARTESIAN_POINT('Ctrl Pts',(-62.1622268744336,-34.5106283314594,
12.));
#140691=CARTESIAN_POINT('Ctrl Pts',(-62.1840308021171,-34.5149095840729,
12.));
#140692=CARTESIAN_POINT('Ctrl Pts',(-62.2058848408347,-34.5191776503842,
12.));
#140693=CARTESIAN_POINT('Ctrl Pts',(-62.2277888633576,-34.523432433049,
12.));
#140694=CARTESIAN_POINT('Ctrl Pts',(-62.2497427430135,-34.5276738352808,
12.));
#140695=CARTESIAN_POINT('Ctrl Pts',(-62.2717463536827,-34.5319017608433,
12.));
#140696=CARTESIAN_POINT('Ctrl Pts',(-62.2937995697925,-34.5361161140449,
12.));
#140697=CARTESIAN_POINT('Ctrl Pts',(-62.3159022663058,-34.5403167997337,
12.));
#140698=CARTESIAN_POINT('Ctrl Pts',(-62.338054318708,-34.5445037232936,
12.));
#140699=CARTESIAN_POINT('Ctrl Pts',(-62.3602556030127,-34.5486767906384,
12.));
#140700=CARTESIAN_POINT('Ctrl Pts',(-62.3825059957601,-34.5528359082075,
12.));
#140701=CARTESIAN_POINT('Ctrl Pts',(-62.4048053740127,-34.5569809829613,
12.));
#140702=CARTESIAN_POINT('Ctrl Pts',(-62.4271536153459,-34.5611119223798,
12.));
#140703=CARTESIAN_POINT('Ctrl Pts',(-62.4495505978393,-34.5652286344593,
12.));
#140704=CARTESIAN_POINT('Ctrl Pts',(-62.4719962000808,-34.5693310277051,
12.));
#140705=CARTESIAN_POINT('Ctrl Pts',(-62.4944903011628,-34.5734190111272,
12.));
#140706=CARTESIAN_POINT('Ctrl Pts',(-62.5170327806781,-34.5774924942355,
12.));
#140707=CARTESIAN_POINT('Ctrl Pts',(-62.5396235187079,-34.5815513870377,
12.));
#140708=CARTESIAN_POINT('Ctrl Pts',(-62.562262395816,-34.5855956000363,
12.));
#140709=CARTESIAN_POINT('Ctrl Pts',(-62.5849492930533,-34.5896250442216,
12.));
#140710=CARTESIAN_POINT('Ctrl Pts',(-62.6076840919536,-34.5936396310679,
12.));
#140711=CARTESIAN_POINT('Ctrl Pts',(-62.6304666745306,-34.5976392725296,
12.));
#140712=CARTESIAN_POINT('Ctrl Pts',(-62.6532969232657,-34.6016238810398,
12.));
#140713=CARTESIAN_POINT('Ctrl Pts',(-62.6761747211037,-34.6055933695069,
12.));
#140714=CARTESIAN_POINT('Ctrl Pts',(-62.6990999514563,-34.6095476513077,
12.));
#140715=CARTESIAN_POINT('Ctrl Pts',(-62.7220724981994,-34.6134866402837,
12.));
#140716=CARTESIAN_POINT('Ctrl Pts',(-62.7450922456676,-34.6174102507375,
12.));
#140717=CARTESIAN_POINT('Ctrl Pts',(-62.7681590786429,-34.6213183974317,
12.));
#140718=CARTESIAN_POINT('Ctrl Pts',(-62.7912728823518,-34.6252109955853,
12.));
#140719=CARTESIAN_POINT('Ctrl Pts',(-62.8144335424697,-34.6290879608673,
12.));
#140720=CARTESIAN_POINT('Ctrl Pts',(-62.8376409451175,-34.6329492093935,
12.));
#140721=CARTESIAN_POINT('Ctrl Pts',(-62.8608949768571,-34.6367946577235,
12.));
#140722=CARTESIAN_POINT('Ctrl Pts',(-62.8841955246794,-34.6406242228592,
12.));
#140723=CARTESIAN_POINT('Ctrl Pts',(-62.9075424760015,-34.644437822241,
12.));
#140724=CARTESIAN_POINT('Ctrl Pts',(-62.9309357186717,-34.6482353737424,
12.));
#140725=CARTESIAN_POINT('Ctrl Pts',(-62.9543751409646,-34.6520167956655,
12.));
#140726=CARTESIAN_POINT('Ctrl Pts',(-62.9778606315783,-34.6557820067393,
12.));
#140727=CARTESIAN_POINT('Ctrl Pts',(-63.0013920796235,-34.6595309261191,
12.));
#140728=CARTESIAN_POINT('Ctrl Pts',(-63.0249693746208,-34.6632634733824,
12.));
#140729=CARTESIAN_POINT('Ctrl Pts',(-63.0485924065045,-34.6669795685228,
12.));
#140730=CARTESIAN_POINT('Ctrl Pts',(-63.0722610656194,-34.670679131947,
12.));
#140731=CARTESIAN_POINT('Ctrl Pts',(-63.0959752427168,-34.674362084472,
12.));
#140732=CARTESIAN_POINT('Ctrl Pts',(-63.119734828943,-34.6780283473252,
12.));
#140733=CARTESIAN_POINT('Ctrl Pts',(-63.1435397158388,-34.6816778421402,
12.));
#140734=CARTESIAN_POINT('Ctrl Pts',(-63.1673897953429,-34.6853104909518,
12.));
#140735=CARTESIAN_POINT('Ctrl Pts',(-63.1912849597887,-34.6889262161924,
12.));
#140736=CARTESIAN_POINT('Ctrl Pts',(-63.2152251019012,-34.6925249406897,
12.));
#140737=CARTESIAN_POINT('Ctrl Pts',(-63.2392101147847,-34.6961065876666,
12.));
#140738=CARTESIAN_POINT('Ctrl Pts',(-63.2632398919225,-34.6996710807378,
12.));
#140739=CARTESIAN_POINT('Ctrl Pts',(-63.2873143271807,-34.703218343904,
12.));
#140740=CARTESIAN_POINT('Ctrl Pts',(-63.3114333148048,-34.7067483015491,
12.));
#140741=CARTESIAN_POINT('Ctrl Pts',(-63.3355967494171,-34.7102608784374,
12.));
#140742=CARTESIAN_POINT('Ctrl Pts',(-63.3598045260053,-34.7137559997146,
12.));
#140743=CARTESIAN_POINT('Ctrl Pts',(-63.3840565399208,-34.7172335909038,
12.));
#140744=CARTESIAN_POINT('Ctrl Pts',(-63.4083526868836,-34.7206935779007,
12.));
#140745=CARTESIAN_POINT('Ctrl Pts',(-63.4326928629795,-34.7241358869701,
12.));
#140746=CARTESIAN_POINT('Ctrl Pts',(-63.4570769646569,-34.7275604447438,
12.));
#140747=CARTESIAN_POINT('Ctrl Pts',(-63.4815048887165,-34.7309671782214,
12.));
#140748=CARTESIAN_POINT('Ctrl Pts',(-63.505976532309,-34.7343560147667,
12.));
#140749=CARTESIAN_POINT('Ctrl Pts',(-63.5304917929386,-34.7377268821025,
12.));
#140750=CARTESIAN_POINT('Ctrl Pts',(-63.5550505684626,-34.7410797083081,
12.));
#140751=CARTESIAN_POINT('Ctrl Pts',(-63.5796527570871,-34.744414421816,
12.));
#140752=CARTESIAN_POINT('Ctrl Pts',(-63.6042982573588,-34.7477309514136,
12.));
#140753=CARTESIAN_POINT('Ctrl Pts',(-63.6289869681604,-34.7510292262406,
12.));
#140754=CARTESIAN_POINT('Ctrl Pts',(-63.6537187887159,-34.7543091757833,
12.));
#140755=CARTESIAN_POINT('Ctrl Pts',(-63.6784936185885,-34.7575707298713,
12.));
#140756=CARTESIAN_POINT('Ctrl Pts',(-63.7033113576785,-34.7608138186759,
12.));
#140757=CARTESIAN_POINT('Ctrl Pts',(-63.7281719062149,-34.76403837271,12.));
#140758=CARTESIAN_POINT('Ctrl Pts',(-63.7530751647494,-34.7672443228275,
12.));
#140759=CARTESIAN_POINT('Ctrl Pts',(-63.778021034163,-34.7704316002171,
12.));
#140760=CARTESIAN_POINT('Ctrl Pts',(-63.8030094156639,-34.7736001363993,
12.));
#140761=CARTESIAN_POINT('Ctrl Pts',(-63.8280402107856,-34.7767498632243,
12.));
#140762=CARTESIAN_POINT('Ctrl Pts',(-63.8531133213793,-34.7798807128715,
12.));
#140763=CARTESIAN_POINT('Ctrl Pts',(-63.8782286496062,-34.7829926178496,
12.));
#140764=CARTESIAN_POINT('Ctrl Pts',(-63.9033860979435,-34.7860855109911,
12.));
#140765=CARTESIAN_POINT('Ctrl Pts',(-63.9285855691845,-34.7891593254488,
12.));
#140766=CARTESIAN_POINT('Ctrl Pts',(-63.9538269664366,-34.7922139946943,
12.));
#140767=CARTESIAN_POINT('Ctrl Pts',(-63.9791101931162,-34.7952494525177,
12.));
#140768=CARTESIAN_POINT('Ctrl Pts',(-64.0044351529402,-34.7982656330293,
12.));
#140769=CARTESIAN_POINT('Ctrl Pts',(-64.0298017499294,-34.8012624706526,
12.));
#140770=CARTESIAN_POINT('Ctrl Pts',(-64.0552098884095,-34.8042399001211,
12.));
#140771=CARTESIAN_POINT('Ctrl Pts',(-64.0806594730085,-34.8071978564747,
12.));
#140772=CARTESIAN_POINT('Ctrl Pts',(-64.1061504086515,-34.8101362750597,
12.));
#140773=CARTESIAN_POINT('Ctrl Pts',(-64.1316826005506,-34.8130550915287,
12.));
#140774=CARTESIAN_POINT('Ctrl Pts',(-64.1572559542086,-34.8159542418374,
12.));
#140775=CARTESIAN_POINT('Ctrl Pts',(-64.1828703754236,-34.8188336622419,
12.));
#140776=CARTESIAN_POINT('Ctrl Pts',(-64.2085257702884,-34.8216932892968,
12.));
#140777=CARTESIAN_POINT('Ctrl Pts',(-64.234222045188,-34.8245330598559,
12.));
#140778=CARTESIAN_POINT('Ctrl Pts',(-64.2599591067916,-34.8273529110744,
12.));
#140779=CARTESIAN_POINT('Ctrl Pts',(-64.285736862052,-34.8301527804054,
12.));
#140780=CARTESIAN_POINT('Ctrl Pts',(-64.3115552182062,-34.8329326055919,
12.));
#140781=CARTESIAN_POINT('Ctrl Pts',(-64.3374140827711,-34.8356923246618,
12.));
#140782=CARTESIAN_POINT('Ctrl Pts',(-64.3633133635382,-34.8384318759248,
12.));
#140783=CARTESIAN_POINT('Ctrl Pts',(-64.3892529685607,-34.8411511979702,
12.));
#140784=CARTESIAN_POINT('Ctrl Pts',(-64.4152328061515,-34.8438502296664,
12.));
#140785=CARTESIAN_POINT('Ctrl Pts',(-64.4412527848969,-34.8465289101621,
12.));
#140786=CARTESIAN_POINT('Ctrl Pts',(-64.4673128136625,-34.8491871788895,
12.));
#140787=CARTESIAN_POINT('Ctrl Pts',(-64.4934128015985,-34.851824975568,
12.));
#140788=CARTESIAN_POINT('Ctrl Pts',(-64.5195526581407,-34.8544422402118,
12.));
#140789=CARTESIAN_POINT('Ctrl Pts',(-64.5457322930088,-34.857038913134,
12.));
#140790=CARTESIAN_POINT('Ctrl Pts',(-64.5719516161927,-34.8596149349256,
12.));
#140791=CARTESIAN_POINT('Ctrl Pts',(-64.5982105379383,-34.8621702464401,
12.));
#140792=CARTESIAN_POINT('Ctrl Pts',(-64.6245089687277,-34.8647047887774,
12.));
#140793=CARTESIAN_POINT('Ctrl Pts',(-64.6508468192599,-34.867218503272,
12.));
#140794=CARTESIAN_POINT('Ctrl Pts',(-64.6772240004228,-34.869711331479,
12.));
#140795=CARTESIAN_POINT('Ctrl Pts',(-64.7036404233306,-34.8721832151974,
12.));
#140796=CARTESIAN_POINT('Ctrl Pts',(-64.7300959993653,-34.8746340964971,
12.));
#140797=CARTESIAN_POINT('Ctrl Pts',(-64.7565906402151,-34.8770639177493,
12.));
#140798=CARTESIAN_POINT('Ctrl Pts',(-64.7831242579028,-34.8794726216513,
12.));
#140799=CARTESIAN_POINT('Ctrl Pts',(-64.8096967648307,-34.881860151273,
12.));
#140800=CARTESIAN_POINT('Ctrl Pts',(-64.8363080737377,-34.8842264500188,
12.));
#140801=CARTESIAN_POINT('Ctrl Pts',(-64.8629580976063,-34.8865714615436,
12.));
#140802=CARTESIAN_POINT('Ctrl Pts',(-64.8896467495757,-34.888895129681,
12.));
#140803=CARTESIAN_POINT('Ctrl Pts',(-64.9163739428605,-34.8911973983785,
12.));
#140804=CARTESIAN_POINT('Ctrl Pts',(-64.9431395906337,-34.8934782116095,
12.));
#140805=CARTESIAN_POINT('Ctrl Pts',(-64.9699436060169,-34.8957375133697,
12.));
#140806=CARTESIAN_POINT('Ctrl Pts',(-64.9967859023212,-34.8979752478616,
12.));
#140807=CARTESIAN_POINT('Ctrl Pts',(-65.0236663932328,-34.9001913596416,
12.));
#140808=CARTESIAN_POINT('Ctrl Pts',(-65.0505849930171,-34.9023857937865,
12.));
#140809=CARTESIAN_POINT('Ctrl Pts',(-65.0775416167085,-34.9045584960509,
12.));
#140810=CARTESIAN_POINT('Ctrl Pts',(-65.1045361803121,-34.9067094130399,
12.));
#140811=CARTESIAN_POINT('Ctrl Pts',(-65.1315686003516,-34.9088384918336,
12.));
#140812=CARTESIAN_POINT('Ctrl Pts',(-65.1586387934241,-34.9109456796213,
12.));
#140813=CARTESIAN_POINT('Ctrl Pts',(-65.1857466757092,-34.9130309233022,
12.));
#140814=CARTESIAN_POINT('Ctrl Pts',(-65.2128921625823,-34.9150941691747,
12.));
#140815=CARTESIAN_POINT('Ctrl Pts',(-65.2400751679549,-34.9171353624113,
12.));
#140816=CARTESIAN_POINT('Ctrl Pts',(-65.2672956048069,-34.9191544474872,
12.));
#140817=CARTESIAN_POINT('Ctrl Pts',(-65.2945533863761,-34.9211513691355,
12.));
#140818=CARTESIAN_POINT('Ctrl Pts',(-65.321848427191,-34.9231260731831,
12.));
#140819=CARTESIAN_POINT('Ctrl Pts',(-65.3491806440537,-34.9250785073477,
12.));
#140820=CARTESIAN_POINT('Ctrl Pts',(-65.3765499573077,-34.9270086222731,
12.));
#140821=CARTESIAN_POINT('Ctrl Pts',(-65.4039562911352,-34.9289163717747,
12.));
#140822=CARTESIAN_POINT('Ctrl Pts',(-65.4274804996589,-34.9305324724445,
12.));
#140823=CARTESIAN_POINT('Ctrl Pts',(-65.4455359575245,-34.931759381316,
12.));
#140824=CARTESIAN_POINT('Ctrl Pts',(-65.4581063193883,-34.9326070346645,
12.));
#140825=CARTESIAN_POINT('Ctrl Pts',(-65.4651808010811,-34.9330820191535,
12.));
#140826=CARTESIAN_POINT('Ctrl Pts',(-65.4667541478385,-34.933187552314,
12.));
#140827=CARTESIAN_POINT('',(-61.0441813777723,-34.2579614092497,0.));
#140828=CARTESIAN_POINT('',(-61.0441813777723,-34.2579614092497,0.));
#140829=CARTESIAN_POINT('Ctrl Pts',(-65.4667541478385,-34.933187552314,
0.));
#140830=CARTESIAN_POINT('Ctrl Pts',(-65.465180801081,-34.9330820191535,
0.));
#140831=CARTESIAN_POINT('Ctrl Pts',(-65.4581063193883,-34.9326070346645,
0.));
#140832=CARTESIAN_POINT('Ctrl Pts',(-65.4455359575245,-34.931759381316,
0.));
#140833=CARTESIAN_POINT('Ctrl Pts',(-65.4274804996589,-34.9305324724445,
0.));
#140834=CARTESIAN_POINT('Ctrl Pts',(-65.4039562911352,-34.9289163717747,
0.));
#140835=CARTESIAN_POINT('Ctrl Pts',(-65.3765499573077,-34.9270086222731,
0.));
#140836=CARTESIAN_POINT('Ctrl Pts',(-65.3491806440537,-34.9250785073477,
0.));
#140837=CARTESIAN_POINT('Ctrl Pts',(-65.321848427191,-34.9231260731831,
0.));
#140838=CARTESIAN_POINT('Ctrl Pts',(-65.2945533863761,-34.9211513691355,
0.));
#140839=CARTESIAN_POINT('Ctrl Pts',(-65.2672956048069,-34.9191544474872,
0.));
#140840=CARTESIAN_POINT('Ctrl Pts',(-65.2400751679549,-34.9171353624113,
0.));
#140841=CARTESIAN_POINT('Ctrl Pts',(-65.2128921625823,-34.9150941691747,
0.));
#140842=CARTESIAN_POINT('Ctrl Pts',(-65.1857466757092,-34.9130309233022,
0.));
#140843=CARTESIAN_POINT('Ctrl Pts',(-65.1586387934241,-34.9109456796213,
0.));
#140844=CARTESIAN_POINT('Ctrl Pts',(-65.1315686003516,-34.9088384918336,
0.));
#140845=CARTESIAN_POINT('Ctrl Pts',(-65.1045361803121,-34.9067094130399,
0.));
#140846=CARTESIAN_POINT('Ctrl Pts',(-65.0775416167085,-34.9045584960509,
0.));
#140847=CARTESIAN_POINT('Ctrl Pts',(-65.0505849930171,-34.9023857937865,
0.));
#140848=CARTESIAN_POINT('Ctrl Pts',(-65.0236663932328,-34.9001913596416,
0.));
#140849=CARTESIAN_POINT('Ctrl Pts',(-64.9967859023212,-34.8979752478616,
0.));
#140850=CARTESIAN_POINT('Ctrl Pts',(-64.9699436060169,-34.8957375133697,
0.));
#140851=CARTESIAN_POINT('Ctrl Pts',(-64.9431395906337,-34.8934782116095,
0.));
#140852=CARTESIAN_POINT('Ctrl Pts',(-64.9163739428605,-34.8911973983785,
0.));
#140853=CARTESIAN_POINT('Ctrl Pts',(-64.8896467495757,-34.888895129681,
0.));
#140854=CARTESIAN_POINT('Ctrl Pts',(-64.8629580976063,-34.8865714615436,
0.));
#140855=CARTESIAN_POINT('Ctrl Pts',(-64.8363080737377,-34.8842264500188,
0.));
#140856=CARTESIAN_POINT('Ctrl Pts',(-64.8096967648307,-34.881860151273,
0.));
#140857=CARTESIAN_POINT('Ctrl Pts',(-64.7831242579028,-34.8794726216513,
0.));
#140858=CARTESIAN_POINT('Ctrl Pts',(-64.7565906402151,-34.8770639177493,
0.));
#140859=CARTESIAN_POINT('Ctrl Pts',(-64.7300959993653,-34.8746340964971,
0.));
#140860=CARTESIAN_POINT('Ctrl Pts',(-64.7036404233306,-34.8721832151974,
0.));
#140861=CARTESIAN_POINT('Ctrl Pts',(-64.6772240004228,-34.869711331479,
0.));
#140862=CARTESIAN_POINT('Ctrl Pts',(-64.6508468192599,-34.867218503272,
0.));
#140863=CARTESIAN_POINT('Ctrl Pts',(-64.6245089687277,-34.8647047887774,
0.));
#140864=CARTESIAN_POINT('Ctrl Pts',(-64.5982105379383,-34.8621702464401,
0.));
#140865=CARTESIAN_POINT('Ctrl Pts',(-64.5719516161927,-34.8596149349256,
0.));
#140866=CARTESIAN_POINT('Ctrl Pts',(-64.5457322930088,-34.857038913134,
0.));
#140867=CARTESIAN_POINT('Ctrl Pts',(-64.5195526581407,-34.8544422402118,
0.));
#140868=CARTESIAN_POINT('Ctrl Pts',(-64.4934128015985,-34.851824975568,
0.));
#140869=CARTESIAN_POINT('Ctrl Pts',(-64.4673128136625,-34.8491871788895,
0.));
#140870=CARTESIAN_POINT('Ctrl Pts',(-64.4412527848969,-34.8465289101621,
0.));
#140871=CARTESIAN_POINT('Ctrl Pts',(-64.4152328061515,-34.8438502296664,
0.));
#140872=CARTESIAN_POINT('Ctrl Pts',(-64.3892529685607,-34.8411511979702,
0.));
#140873=CARTESIAN_POINT('Ctrl Pts',(-64.3633133635382,-34.8384318759248,
0.));
#140874=CARTESIAN_POINT('Ctrl Pts',(-64.3374140827711,-34.8356923246618,
0.));
#140875=CARTESIAN_POINT('Ctrl Pts',(-64.3115552182062,-34.8329326055919,
0.));
#140876=CARTESIAN_POINT('Ctrl Pts',(-64.285736862052,-34.8301527804054,
0.));
#140877=CARTESIAN_POINT('Ctrl Pts',(-64.2599591067916,-34.8273529110744,
0.));
#140878=CARTESIAN_POINT('Ctrl Pts',(-64.234222045188,-34.8245330598559,
0.));
#140879=CARTESIAN_POINT('Ctrl Pts',(-64.2085257702884,-34.8216932892968,
0.));
#140880=CARTESIAN_POINT('Ctrl Pts',(-64.1828703754236,-34.8188336622419,
0.));
#140881=CARTESIAN_POINT('Ctrl Pts',(-64.1572559542086,-34.8159542418374,
0.));
#140882=CARTESIAN_POINT('Ctrl Pts',(-64.1316826005506,-34.8130550915287,
0.));
#140883=CARTESIAN_POINT('Ctrl Pts',(-64.1061504086515,-34.8101362750597,
0.));
#140884=CARTESIAN_POINT('Ctrl Pts',(-64.0806594730085,-34.8071978564747,
0.));
#140885=CARTESIAN_POINT('Ctrl Pts',(-64.0552098884095,-34.8042399001211,
0.));
#140886=CARTESIAN_POINT('Ctrl Pts',(-64.0298017499294,-34.8012624706526,
0.));
#140887=CARTESIAN_POINT('Ctrl Pts',(-64.0044351529402,-34.7982656330293,
0.));
#140888=CARTESIAN_POINT('Ctrl Pts',(-63.9791101931162,-34.7952494525177,
0.));
#140889=CARTESIAN_POINT('Ctrl Pts',(-63.9538269664366,-34.7922139946943,
0.));
#140890=CARTESIAN_POINT('Ctrl Pts',(-63.9285855691845,-34.7891593254488,
0.));
#140891=CARTESIAN_POINT('Ctrl Pts',(-63.9033860979435,-34.7860855109911,
0.));
#140892=CARTESIAN_POINT('Ctrl Pts',(-63.8782286496062,-34.7829926178496,
0.));
#140893=CARTESIAN_POINT('Ctrl Pts',(-63.8531133213793,-34.7798807128715,
0.));
#140894=CARTESIAN_POINT('Ctrl Pts',(-63.8280402107856,-34.7767498632243,
0.));
#140895=CARTESIAN_POINT('Ctrl Pts',(-63.8030094156639,-34.7736001363993,
0.));
#140896=CARTESIAN_POINT('Ctrl Pts',(-63.778021034163,-34.7704316002171,
0.));
#140897=CARTESIAN_POINT('Ctrl Pts',(-63.7530751647494,-34.7672443228275,
0.));
#140898=CARTESIAN_POINT('Ctrl Pts',(-63.7281719062149,-34.76403837271,0.));
#140899=CARTESIAN_POINT('Ctrl Pts',(-63.7033113576785,-34.7608138186759,
0.));
#140900=CARTESIAN_POINT('Ctrl Pts',(-63.6784936185885,-34.7575707298713,
0.));
#140901=CARTESIAN_POINT('Ctrl Pts',(-63.6537187887159,-34.7543091757833,
0.));
#140902=CARTESIAN_POINT('Ctrl Pts',(-63.6289869681604,-34.7510292262406,
0.));
#140903=CARTESIAN_POINT('Ctrl Pts',(-63.6042982573588,-34.7477309514136,
0.));
#140904=CARTESIAN_POINT('Ctrl Pts',(-63.5796527570871,-34.744414421816,
0.));
#140905=CARTESIAN_POINT('Ctrl Pts',(-63.5550505684626,-34.7410797083081,
0.));
#140906=CARTESIAN_POINT('Ctrl Pts',(-63.5304917929386,-34.7377268821025,
0.));
#140907=CARTESIAN_POINT('Ctrl Pts',(-63.505976532309,-34.7343560147667,
0.));
#140908=CARTESIAN_POINT('Ctrl Pts',(-63.4815048887165,-34.7309671782214,
0.));
#140909=CARTESIAN_POINT('Ctrl Pts',(-63.4570769646569,-34.7275604447438,
0.));
#140910=CARTESIAN_POINT('Ctrl Pts',(-63.4326928629795,-34.7241358869701,
0.));
#140911=CARTESIAN_POINT('Ctrl Pts',(-63.4083526868836,-34.7206935779007,
0.));
#140912=CARTESIAN_POINT('Ctrl Pts',(-63.3840565399208,-34.7172335909038,
0.));
#140913=CARTESIAN_POINT('Ctrl Pts',(-63.3598045260053,-34.7137559997146,
0.));
#140914=CARTESIAN_POINT('Ctrl Pts',(-63.3355967494171,-34.7102608784374,
0.));
#140915=CARTESIAN_POINT('Ctrl Pts',(-63.3114333148048,-34.7067483015491,
0.));
#140916=CARTESIAN_POINT('Ctrl Pts',(-63.2873143271807,-34.703218343904,
0.));
#140917=CARTESIAN_POINT('Ctrl Pts',(-63.2632398919225,-34.6996710807378,
0.));
#140918=CARTESIAN_POINT('Ctrl Pts',(-63.2392101147847,-34.6961065876666,
0.));
#140919=CARTESIAN_POINT('Ctrl Pts',(-63.2152251019012,-34.6925249406897,
0.));
#140920=CARTESIAN_POINT('Ctrl Pts',(-63.1912849597887,-34.6889262161924,
0.));
#140921=CARTESIAN_POINT('Ctrl Pts',(-63.1673897953429,-34.6853104909518,
0.));
#140922=CARTESIAN_POINT('Ctrl Pts',(-63.1435397158388,-34.6816778421402,
0.));
#140923=CARTESIAN_POINT('Ctrl Pts',(-63.119734828943,-34.6780283473252,
0.));
#140924=CARTESIAN_POINT('Ctrl Pts',(-63.0959752427168,-34.674362084472,
0.));
#140925=CARTESIAN_POINT('Ctrl Pts',(-63.0722610656194,-34.670679131947,
0.));
#140926=CARTESIAN_POINT('Ctrl Pts',(-63.0485924065045,-34.6669795685228,
0.));
#140927=CARTESIAN_POINT('Ctrl Pts',(-63.0249693746208,-34.6632634733824,
0.));
#140928=CARTESIAN_POINT('Ctrl Pts',(-63.0013920796235,-34.6595309261191,
0.));
#140929=CARTESIAN_POINT('Ctrl Pts',(-62.9778606315783,-34.6557820067393,
0.));
#140930=CARTESIAN_POINT('Ctrl Pts',(-62.9543751409646,-34.6520167956655,
0.));
#140931=CARTESIAN_POINT('Ctrl Pts',(-62.9309357186717,-34.6482353737424,
0.));
#140932=CARTESIAN_POINT('Ctrl Pts',(-62.9075424760015,-34.644437822241,
0.));
#140933=CARTESIAN_POINT('Ctrl Pts',(-62.8841955246794,-34.6406242228592,
0.));
#140934=CARTESIAN_POINT('Ctrl Pts',(-62.8608949768571,-34.6367946577235,
0.));
#140935=CARTESIAN_POINT('Ctrl Pts',(-62.8376409451175,-34.6329492093935,
0.));
#140936=CARTESIAN_POINT('Ctrl Pts',(-62.8144335424697,-34.6290879608673,
0.));
#140937=CARTESIAN_POINT('Ctrl Pts',(-62.7912728823518,-34.6252109955853,
0.));
#140938=CARTESIAN_POINT('Ctrl Pts',(-62.7681590786429,-34.6213183974317,
0.));
#140939=CARTESIAN_POINT('Ctrl Pts',(-62.7450922456676,-34.6174102507375,
0.));
#140940=CARTESIAN_POINT('Ctrl Pts',(-62.7220724981994,-34.6134866402837,
0.));
#140941=CARTESIAN_POINT('Ctrl Pts',(-62.6990999514563,-34.6095476513077,
0.));
#140942=CARTESIAN_POINT('Ctrl Pts',(-62.6761747211037,-34.6055933695069,
0.));
#140943=CARTESIAN_POINT('Ctrl Pts',(-62.6532969232657,-34.6016238810398,
0.));
#140944=CARTESIAN_POINT('Ctrl Pts',(-62.6304666745306,-34.5976392725296,
0.));
#140945=CARTESIAN_POINT('Ctrl Pts',(-62.6076840919536,-34.5936396310679,
0.));
#140946=CARTESIAN_POINT('Ctrl Pts',(-62.5849492930533,-34.5896250442216,
0.));
#140947=CARTESIAN_POINT('Ctrl Pts',(-62.562262395816,-34.5855956000363,
0.));
#140948=CARTESIAN_POINT('Ctrl Pts',(-62.5396235187079,-34.5815513870377,
0.));
#140949=CARTESIAN_POINT('Ctrl Pts',(-62.5170327806781,-34.5774924942355,
0.));
#140950=CARTESIAN_POINT('Ctrl Pts',(-62.4944903011628,-34.5734190111272,
0.));
#140951=CARTESIAN_POINT('Ctrl Pts',(-62.4719962000808,-34.5693310277051,
0.));
#140952=CARTESIAN_POINT('Ctrl Pts',(-62.4495505978393,-34.5652286344593,
0.));
#140953=CARTESIAN_POINT('Ctrl Pts',(-62.4271536153459,-34.5611119223798,
0.));
#140954=CARTESIAN_POINT('Ctrl Pts',(-62.4048053740127,-34.5569809829613,
0.));
#140955=CARTESIAN_POINT('Ctrl Pts',(-62.3825059957601,-34.5528359082075,
0.));
#140956=CARTESIAN_POINT('Ctrl Pts',(-62.3602556030127,-34.5486767906384,
0.));
#140957=CARTESIAN_POINT('Ctrl Pts',(-62.338054318708,-34.5445037232936,
0.));
#140958=CARTESIAN_POINT('Ctrl Pts',(-62.3159022663058,-34.5403167997337,
0.));
#140959=CARTESIAN_POINT('Ctrl Pts',(-62.2937995697925,-34.5361161140449,
0.));
#140960=CARTESIAN_POINT('Ctrl Pts',(-62.2717463536827,-34.5319017608433,
0.));
#140961=CARTESIAN_POINT('Ctrl Pts',(-62.2497427430135,-34.5276738352808,
0.));
#140962=CARTESIAN_POINT('Ctrl Pts',(-62.2277888633576,-34.523432433049,
0.));
#140963=CARTESIAN_POINT('Ctrl Pts',(-62.2058848408347,-34.5191776503842,
0.));
#140964=CARTESIAN_POINT('Ctrl Pts',(-62.1840308021171,-34.5149095840729,
0.));
#140965=CARTESIAN_POINT('Ctrl Pts',(-62.1622268744336,-34.5106283314594,
0.));
#140966=CARTESIAN_POINT('Ctrl Pts',(-62.1404731855686,-34.5063339904533,
0.));
#140967=CARTESIAN_POINT('Ctrl Pts',(-62.1187698638705,-34.5020266595292,
0.));
#140968=CARTESIAN_POINT('Ctrl Pts',(-62.0971170382565,-34.4977064377281,
0.));
#140969=CARTESIAN_POINT('Ctrl Pts',(-62.0755148382136,-34.4933734246592,
0.));
#140970=CARTESIAN_POINT('Ctrl Pts',(-62.0539633937944,-34.4890277205041,
0.));
#140971=CARTESIAN_POINT('Ctrl Pts',(-62.0324628356152,-34.4846694260205,
0.));
#140972=CARTESIAN_POINT('Ctrl Pts',(-62.0110132948807,-34.4802986425535,
0.));
#140973=CARTESIAN_POINT('Ctrl Pts',(-61.9896149034009,-34.4759154720477,
0.));
#140974=CARTESIAN_POINT('Ctrl Pts',(-61.9682677936048,-34.4715200170589,
0.));
#140975=CARTESIAN_POINT('Ctrl Pts',(-61.9469720985512,-34.4671123807706,
0.));
#140976=CARTESIAN_POINT('Ctrl Pts',(-61.9257279519283,-34.462692666996,
0.));
#140977=CARTESIAN_POINT('Ctrl Pts',(-61.9045354880424,-34.4582609801625,
0.));
#140978=CARTESIAN_POINT('Ctrl Pts',(-61.883394841802,-34.4538174253009,
0.));
#140979=CARTESIAN_POINT('Ctrl Pts',(-61.862306148703,-34.4493621080367,
0.));
#140980=CARTESIAN_POINT('Ctrl Pts',(-61.8412695447951,-34.4448951345753,
0.));
#140981=CARTESIAN_POINT('Ctrl Pts',(-61.8202851667247,-34.4404166117313,
0.));
#140982=CARTESIAN_POINT('Ctrl Pts',(-61.7993531518052,-34.4359266469757,
0.));
#140983=CARTESIAN_POINT('Ctrl Pts',(-61.7784736380727,-34.4314253484791,
0.));
#140984=CARTESIAN_POINT('Ctrl Pts',(-61.7576467643419,-34.4269128251569,
0.));
#140985=CARTESIAN_POINT('Ctrl Pts',(-61.7368726702573,-34.4223891867166,
0.));
#140986=CARTESIAN_POINT('Ctrl Pts',(-61.7161514961892,-34.4178545435753,
0.));
#140987=CARTESIAN_POINT('Ctrl Pts',(-61.6954833831157,-34.4133090067696,
0.));
#140988=CARTESIAN_POINT('Ctrl Pts',(-61.674868472521,-34.4087526878815,
0.));
#140989=CARTESIAN_POINT('Ctrl Pts',(-61.6543069062436,-34.4041856989328,
0.));
#140990=CARTESIAN_POINT('Ctrl Pts',(-61.6337988264586,-34.399608152377,
0.));
#140991=CARTESIAN_POINT('Ctrl Pts',(-61.6133443760168,-34.3950201613446,
0.));
#140992=CARTESIAN_POINT('Ctrl Pts',(-61.5929436987419,-34.3904218398642,
0.));
#140993=CARTESIAN_POINT('Ctrl Pts',(-61.5725969396817,-34.3858133030511,
0.));
#140994=CARTESIAN_POINT('Ctrl Pts',(-61.5523042455127,-34.3811946674179,
0.));
#140995=CARTESIAN_POINT('Ctrl Pts',(-61.5320657642601,-34.3765660506659,
0.));
#140996=CARTESIAN_POINT('Ctrl Pts',(-61.511881644541,-34.3719275711179,
0.));
#140997=CARTESIAN_POINT('Ctrl Pts',(-61.4917520349276,-34.3672793472463,
0.));
#140998=CARTESIAN_POINT('Ctrl Pts',(-61.4716770832924,-34.3626214971903,
0.));
#140999=CARTESIAN_POINT('Ctrl Pts',(-61.4516569360499,-34.357954138202,
0.));
#141000=CARTESIAN_POINT('Ctrl Pts',(-61.4316917395959,-34.3532773877112,
0.));
#141001=CARTESIAN_POINT('Ctrl Pts',(-61.4117816420251,-34.3485913645991,
0.));
#141002=CARTESIAN_POINT('Ctrl Pts',(-61.3919267945293,-34.34389619024,0.));
#141003=CARTESIAN_POINT('Ctrl Pts',(-61.3721273534222,-34.339191990012,
0.));
#141004=CARTESIAN_POINT('Ctrl Pts',(-61.3523834803144,-34.3344788934337,
0.));
#141005=CARTESIAN_POINT('Ctrl Pts',(-61.3326953378817,-34.3297570310126,
0.));
#141006=CARTESIAN_POINT('Ctrl Pts',(-61.3130630861375,-34.3250265314761,
0.));
#141007=CARTESIAN_POINT('Ctrl Pts',(-61.2934868791875,-34.3202875193629,
0.));
#141008=CARTESIAN_POINT('Ctrl Pts',(-61.2739668600415,-34.3155401111776,
0.));
#141009=CARTESIAN_POINT('Ctrl Pts',(-61.2545031656196,-34.3107844191081,
0.));
#141010=CARTESIAN_POINT('Ctrl Pts',(-61.2350959366987,-34.3060205584093,
0.));
#141011=CARTESIAN_POINT('Ctrl Pts',(-61.2157453259107,-34.3012486533474,
0.));
#141012=CARTESIAN_POINT('Ctrl Pts',(-61.1964515073823,-34.296468844362,
0.));
#141013=CARTESIAN_POINT('Ctrl Pts',(-61.1772146833083,-34.2916812929675,
0.));
#141014=CARTESIAN_POINT('Ctrl Pts',(-61.15803506354,-34.2868861666301,0.));
#141015=CARTESIAN_POINT('Ctrl Pts',(-61.1389128461815,-34.2820836244425,
0.));
#141016=CARTESIAN_POINT('Ctrl Pts',(-61.119848199783,-34.2772738038811,
0.));
#141017=CARTESIAN_POINT('Ctrl Pts',(-61.100841240023,-34.2724568037374,
0.));
#141018=CARTESIAN_POINT('Ctrl Pts',(-61.0818920286644,-34.2676326825846,
0.));
#141019=CARTESIAN_POINT('Ctrl Pts',(-61.0667788793594,-34.2637677132139,
0.));
#141020=CARTESIAN_POINT('Ctrl Pts',(-61.0554700177206,-34.2608658001761,
0.));
#141021=CARTESIAN_POINT('Ctrl Pts',(-61.0479423318803,-34.2589297755482,
0.));
#141022=CARTESIAN_POINT('Ctrl Pts',(-61.0441813777723,-34.2579614092497,
0.));
#141023=CARTESIAN_POINT('Ctrl Pts',(-68.5875145916629,-29.0861280018229,
0.));
#141024=CARTESIAN_POINT('Ctrl Pts',(-68.5875145916629,-29.0861280018229,
12.));
#141025=CARTESIAN_POINT('Ctrl Pts',(-68.5819214834737,-29.0863005247839,
0.));
#141026=CARTESIAN_POINT('Ctrl Pts',(-68.5819214834737,-29.0863005247839,
12.));
#141027=CARTESIAN_POINT('Ctrl Pts',(-68.5707386600636,-29.0866429722093,
0.));
#141028=CARTESIAN_POINT('Ctrl Pts',(-68.5707386600636,-29.0866429722093,
12.));
#141029=CARTESIAN_POINT('Ctrl Pts',(-68.5539746038542,-29.0871488478588,
0.));
#141030=CARTESIAN_POINT('Ctrl Pts',(-68.5539746038542,-29.0871488478588,
12.));
#141031=CARTESIAN_POINT('Ctrl Pts',(-68.5316428875424,-29.0878077571086,
0.));
#141032=CARTESIAN_POINT('Ctrl Pts',(-68.5316428875424,-29.0878077571086,
12.));
#141033=CARTESIAN_POINT('Ctrl Pts',(-68.5037621824171,-29.0886054060563,
0.));
#141034=CARTESIAN_POINT('Ctrl Pts',(-68.5037621824171,-29.0886054060563,
12.));
#141035=CARTESIAN_POINT('Ctrl Pts',(-68.4759154367939,-29.0893770688944,
0.));
#141036=CARTESIAN_POINT('Ctrl Pts',(-68.4759154367939,-29.0893770688944,
12.));
#141037=CARTESIAN_POINT('Ctrl Pts',(-68.4481026830931,-29.0901227535307,
0.));
#141038=CARTESIAN_POINT('Ctrl Pts',(-68.4481026830931,-29.0901227535307,
12.));
#141039=CARTESIAN_POINT('Ctrl Pts',(-68.4203239694612,-29.090842477089,
0.));
#141040=CARTESIAN_POINT('Ctrl Pts',(-68.4203239694612,-29.090842477089,
12.));
#141041=CARTESIAN_POINT('Ctrl Pts',(-68.3925793637995,-29.0915362699455,
0.));
#141042=CARTESIAN_POINT('Ctrl Pts',(-68.3925793637995,-29.0915362699455,
12.));
#141043=CARTESIAN_POINT('Ctrl Pts',(-68.364868951893,-29.0922041749294,
0.));
#141044=CARTESIAN_POINT('Ctrl Pts',(-68.364868951893,-29.0922041749294,
12.));
#141045=CARTESIAN_POINT('Ctrl Pts',(-68.3371928310161,-29.0928462428145,
0.));
#141046=CARTESIAN_POINT('Ctrl Pts',(-68.3371928310161,-29.0928462428145,
12.));
#141047=CARTESIAN_POINT('Ctrl Pts',(-68.3095511047769,-29.0934625288409,
0.));
#141048=CARTESIAN_POINT('Ctrl Pts',(-68.3095511047769,-29.0934625288409,
12.));
#141049=CARTESIAN_POINT('Ctrl Pts',(-68.2819438775953,-29.0940530889149,
0.));
#141050=CARTESIAN_POINT('Ctrl Pts',(-68.2819438775953,-29.0940530889149,
12.));
#141051=CARTESIAN_POINT('Ctrl Pts',(-68.2543712489906,-29.0946179757167,
0.));
#141052=CARTESIAN_POINT('Ctrl Pts',(-68.2543712489906,-29.0946179757167,
12.));
#141053=CARTESIAN_POINT('Ctrl Pts',(-68.2268333089617,-29.0951572355397,
0.));
#141054=CARTESIAN_POINT('Ctrl Pts',(-68.2268333089617,-29.0951572355397,
12.));
#141055=CARTESIAN_POINT('Ctrl Pts',(-68.1993301412061,-29.0956709104627,
0.));
#141056=CARTESIAN_POINT('Ctrl Pts',(-68.1993301412061,-29.0956709104627,
12.));
#141057=CARTESIAN_POINT('Ctrl Pts',(-68.1718618254281,-29.0961590399046,
0.));
#141058=CARTESIAN_POINT('Ctrl Pts',(-68.1718618254281,-29.0961590399046,
12.));
#141059=CARTESIAN_POINT('Ctrl Pts',(-68.1444284400742,-29.0966216624743,
0.));
#141060=CARTESIAN_POINT('Ctrl Pts',(-68.1444284400742,-29.0966216624743,
12.));
#141061=CARTESIAN_POINT('Ctrl Pts',(-68.1170300646987,-29.0970588175728,
0.));
#141062=CARTESIAN_POINT('Ctrl Pts',(-68.1170300646987,-29.0970588175728,
12.));
#141063=CARTESIAN_POINT('Ctrl Pts',(-68.0896667829567,-29.0974705474259,
0.));
#141064=CARTESIAN_POINT('Ctrl Pts',(-68.0896667829567,-29.0974705474259,
12.));
#141065=CARTESIAN_POINT('Ctrl Pts',(-68.0623386822863,-29.0978568968657,
0.));
#141066=CARTESIAN_POINT('Ctrl Pts',(-68.0623386822863,-29.0978568968657,
12.));
#141067=CARTESIAN_POINT('Ctrl Pts',(-68.0350458525551,-29.0982179124097,
0.));
#141068=CARTESIAN_POINT('Ctrl Pts',(-68.0350458525551,-29.0982179124097,
12.));
#141069=CARTESIAN_POINT('Ctrl Pts',(-68.0077883850121,-29.0985536415531,
0.));
#141070=CARTESIAN_POINT('Ctrl Pts',(-68.0077883850121,-29.0985536415531,
12.));
#141071=CARTESIAN_POINT('Ctrl Pts',(-67.9805663711855,-29.0988641320247,
0.));
#141072=CARTESIAN_POINT('Ctrl Pts',(-67.9805663711855,-29.0988641320247,
12.));
#141073=CARTESIAN_POINT('Ctrl Pts',(-67.9533799016148,-29.0991494309404,
0.));
#141074=CARTESIAN_POINT('Ctrl Pts',(-67.9533799016148,-29.0991494309404,
12.));
#141075=CARTESIAN_POINT('Ctrl Pts',(-67.9262290652829,-29.099409584422,
0.));
#141076=CARTESIAN_POINT('Ctrl Pts',(-67.9262290652829,-29.099409584422,
12.));
#141077=CARTESIAN_POINT('Ctrl Pts',(-67.8991139503193,-29.0996446380626,
0.));
#141078=CARTESIAN_POINT('Ctrl Pts',(-67.8991139503193,-29.0996446380626,
12.));
#141079=CARTESIAN_POINT('Ctrl Pts',(-67.8720346444124,-29.0998546372032,
0.));
#141080=CARTESIAN_POINT('Ctrl Pts',(-67.8720346444124,-29.0998546372032,
12.));
#141081=CARTESIAN_POINT('Ctrl Pts',(-67.8449912353329,-29.1000396272867,
0.));
#141082=CARTESIAN_POINT('Ctrl Pts',(-67.8449912353329,-29.1000396272867,
12.));
#141083=CARTESIAN_POINT('Ctrl Pts',(-67.8179838114099,-29.1001996541842,
0.));
#141084=CARTESIAN_POINT('Ctrl Pts',(-67.8179838114099,-29.1001996541842,
12.));
#141085=CARTESIAN_POINT('Ctrl Pts',(-67.7910124620135,-29.1003347645294,
0.));
#141086=CARTESIAN_POINT('Ctrl Pts',(-67.7910124620135,-29.1003347645294,
12.));
#141087=CARTESIAN_POINT('Ctrl Pts',(-67.7640772773388,-29.1004450055643,
0.));
#141088=CARTESIAN_POINT('Ctrl Pts',(-67.7640772773388,-29.1004450055643,
12.));
#141089=CARTESIAN_POINT('Ctrl Pts',(-67.7371783482035,-29.1005304249987,
0.));
#141090=CARTESIAN_POINT('Ctrl Pts',(-67.7371783482035,-29.1005304249987,
12.));
#141091=CARTESIAN_POINT('Ctrl Pts',(-67.7103157658296,-29.1005910708624,
0.));
#141092=CARTESIAN_POINT('Ctrl Pts',(-67.7103157658296,-29.1005910708624,
12.));
#141093=CARTESIAN_POINT('Ctrl Pts',(-67.6834896216461,-29.1006269913747,
0.));
#141094=CARTESIAN_POINT('Ctrl Pts',(-67.6834896216461,-29.1006269913747,
12.));
#141095=CARTESIAN_POINT('Ctrl Pts',(-67.6567000070326,-29.1006382347814,
0.));
#141096=CARTESIAN_POINT('Ctrl Pts',(-67.6567000070326,-29.1006382347814,
12.));
#141097=CARTESIAN_POINT('Ctrl Pts',(-67.6299470133295,-29.100624849358,
0.));
#141098=CARTESIAN_POINT('Ctrl Pts',(-67.6299470133295,-29.100624849358,
12.));
#141099=CARTESIAN_POINT('Ctrl Pts',(-67.6032307319623,-29.1005868834866,
0.));
#141100=CARTESIAN_POINT('Ctrl Pts',(-67.6032307319623,-29.1005868834866,
12.));
#141101=CARTESIAN_POINT('Ctrl Pts',(-67.5765512545281,-29.1005243857139,
0.));
#141102=CARTESIAN_POINT('Ctrl Pts',(-67.5765512545281,-29.1005243857139,
12.));
#141103=CARTESIAN_POINT('Ctrl Pts',(-67.5499086728888,-29.1004374048148,
0.));
#141104=CARTESIAN_POINT('Ctrl Pts',(-67.5499086728888,-29.1004374048148,
12.));
#141105=CARTESIAN_POINT('Ctrl Pts',(-67.5233030792704,-29.1003259898682,
0.));
#141106=CARTESIAN_POINT('Ctrl Pts',(-67.5233030792704,-29.1003259898682,
12.));
#141107=CARTESIAN_POINT('Ctrl Pts',(-67.4967345663096,-29.1001901902909,
0.));
#141108=CARTESIAN_POINT('Ctrl Pts',(-67.4967345663096,-29.1001901902909,
12.));
#141109=CARTESIAN_POINT('Ctrl Pts',(-67.4702032270048,-29.1000300557955,
0.));
#141110=CARTESIAN_POINT('Ctrl Pts',(-67.4702032270048,-29.1000300557955,
12.));
#141111=CARTESIAN_POINT('Ctrl Pts',(-67.4437091546859,-29.0998456363683,
0.));
#141112=CARTESIAN_POINT('Ctrl Pts',(-67.4437091546859,-29.0998456363683,
12.));
#141113=CARTESIAN_POINT('Ctrl Pts',(-67.4172524429727,-29.0996369822418,
0.));
#141114=CARTESIAN_POINT('Ctrl Pts',(-67.4172524429727,-29.0996369822418,
12.));
#141115=CARTESIAN_POINT('Ctrl Pts',(-67.3908331857323,-29.0994041438719,
0.));
#141116=CARTESIAN_POINT('Ctrl Pts',(-67.3908331857323,-29.0994041438719,
12.));
#141117=CARTESIAN_POINT('Ctrl Pts',(-67.3644514770387,-29.0991471719176,
0.));
#141118=CARTESIAN_POINT('Ctrl Pts',(-67.3644514770387,-29.0991471719176,
12.));
#141119=CARTESIAN_POINT('Ctrl Pts',(-67.3381074112027,-29.0988661172531,
0.));
#141120=CARTESIAN_POINT('Ctrl Pts',(-67.3381074112027,-29.0988661172531,
12.));
#141121=CARTESIAN_POINT('Ctrl Pts',(-67.311801082792,-29.0985610309771,
0.));
#141122=CARTESIAN_POINT('Ctrl Pts',(-67.311801082792,-29.0985610309771,
12.));
#141123=CARTESIAN_POINT('Ctrl Pts',(-67.2855325866517,-29.0982319644277,
0.));
#141124=CARTESIAN_POINT('Ctrl Pts',(-67.2855325866517,-29.0982319644277,
12.));
#141125=CARTESIAN_POINT('Ctrl Pts',(-67.2593020179209,-29.0978789691962,
0.));
#141126=CARTESIAN_POINT('Ctrl Pts',(-67.2593020179209,-29.0978789691962,
12.));
#141127=CARTESIAN_POINT('Ctrl Pts',(-67.2331094720471,-29.097502097147,
0.));
#141128=CARTESIAN_POINT('Ctrl Pts',(-67.2331094720471,-29.097502097147,
12.));
#141129=CARTESIAN_POINT('Ctrl Pts',(-67.2069550447883,-29.0971014004131,
0.));
#141130=CARTESIAN_POINT('Ctrl Pts',(-67.2069550447883,-29.0971014004131,
12.));
#141131=CARTESIAN_POINT('Ctrl Pts',(-67.1808388322109,-29.096676931389,
0.));
#141132=CARTESIAN_POINT('Ctrl Pts',(-67.1808388322109,-29.096676931389,
12.));
#141133=CARTESIAN_POINT('Ctrl Pts',(-67.1547609306843,-29.0962287427273,
0.));
#141134=CARTESIAN_POINT('Ctrl Pts',(-67.1547609306843,-29.0962287427273,
12.));
#141135=CARTESIAN_POINT('Ctrl Pts',(-67.1287214368746,-29.0957568873358,
0.));
#141136=CARTESIAN_POINT('Ctrl Pts',(-67.1287214368746,-29.0957568873358,
12.));
#141137=CARTESIAN_POINT('Ctrl Pts',(-67.1027204477311,-29.0952614183779,
0.));
#141138=CARTESIAN_POINT('Ctrl Pts',(-67.1027204477311,-29.0952614183779,
12.));
#141139=CARTESIAN_POINT('Ctrl Pts',(-67.0767580604879,-29.0947423892727,
0.));
#141140=CARTESIAN_POINT('Ctrl Pts',(-67.0767580604879,-29.0947423892727,
12.));
#141141=CARTESIAN_POINT('Ctrl Pts',(-67.0508343726776,-29.0941998536959,
0.));
#141142=CARTESIAN_POINT('Ctrl Pts',(-67.0508343726776,-29.0941998536959,
12.));
#141143=CARTESIAN_POINT('Ctrl Pts',(-67.0249494821363,-29.0936338655828,
0.));
#141144=CARTESIAN_POINT('Ctrl Pts',(-67.0249494821363,-29.0936338655828,
12.));
#141145=CARTESIAN_POINT('Ctrl Pts',(-66.9991034870083,-29.0930444791328,
0.));
#141146=CARTESIAN_POINT('Ctrl Pts',(-66.9991034870083,-29.0930444791328,
12.));
#141147=CARTESIAN_POINT('Ctrl Pts',(-66.9732964857466,-29.092431748817,
0.));
#141148=CARTESIAN_POINT('Ctrl Pts',(-66.9732964857466,-29.092431748817,
12.));
#141149=CARTESIAN_POINT('Ctrl Pts',(-66.9475285771135,-29.0917957293826,
0.));
#141150=CARTESIAN_POINT('Ctrl Pts',(-66.9475285771135,-29.0917957293826,
12.));
#141151=CARTESIAN_POINT('Ctrl Pts',(-66.9217998601885,-29.0911364758487,
0.));
#141152=CARTESIAN_POINT('Ctrl Pts',(-66.9217998601885,-29.0911364758487,
12.));
#141153=CARTESIAN_POINT('Ctrl Pts',(-66.8961104343707,-29.0904540435065,
0.));
#141154=CARTESIAN_POINT('Ctrl Pts',(-66.8961104343707,-29.0904540435065,
12.));
#141155=CARTESIAN_POINT('Ctrl Pts',(-66.8704603993794,-29.0897484879207,
0.));
#141156=CARTESIAN_POINT('Ctrl Pts',(-66.8704603993794,-29.0897484879207,
12.));
#141157=CARTESIAN_POINT('Ctrl Pts',(-66.8448498552503,-29.0890198649323,
0.));
#141158=CARTESIAN_POINT('Ctrl Pts',(-66.8448498552503,-29.0890198649323,
12.));
#141159=CARTESIAN_POINT('Ctrl Pts',(-66.8192789023312,-29.088268230663,
0.));
#141160=CARTESIAN_POINT('Ctrl Pts',(-66.8192789023312,-29.088268230663,
12.));
#141161=CARTESIAN_POINT('Ctrl Pts',(-66.793747641293,-29.0874936415132,
0.));
#141162=CARTESIAN_POINT('Ctrl Pts',(-66.793747641293,-29.0874936415132,
12.));
#141163=CARTESIAN_POINT('Ctrl Pts',(-66.7682561731341,-29.0866961541626,
0.));
#141164=CARTESIAN_POINT('Ctrl Pts',(-66.7682561731341,-29.0866961541626,
12.));
#141165=CARTESIAN_POINT('Ctrl Pts',(-66.7428045991841,-29.0858758255729,
0.));
#141166=CARTESIAN_POINT('Ctrl Pts',(-66.7428045991841,-29.0858758255729,
12.));
#141167=CARTESIAN_POINT('Ctrl Pts',(-66.7173930211022,-29.0850327129916,
0.));
#141168=CARTESIAN_POINT('Ctrl Pts',(-66.7173930211022,-29.0850327129916,
12.));
#141169=CARTESIAN_POINT('Ctrl Pts',(-66.6920215408751,-29.0841668739588,
0.));
#141170=CARTESIAN_POINT('Ctrl Pts',(-66.6920215408751,-29.0841668739588,
12.));
#141171=CARTESIAN_POINT('Ctrl Pts',(-66.6666902608249,-29.0832783663049,
0.));
#141172=CARTESIAN_POINT('Ctrl Pts',(-66.6666902608249,-29.0832783663049,
12.));
#141173=CARTESIAN_POINT('Ctrl Pts',(-66.6413992836147,-29.0823672481507,
0.));
#141174=CARTESIAN_POINT('Ctrl Pts',(-66.6413992836147,-29.0823672481507,
12.));
#141175=CARTESIAN_POINT('Ctrl Pts',(-66.6161487122502,-29.0814335779084,
0.));
#141176=CARTESIAN_POINT('Ctrl Pts',(-66.6161487122502,-29.0814335779084,
12.));
#141177=CARTESIAN_POINT('Ctrl Pts',(-66.59093865008,-29.0804774142854,0.));
#141178=CARTESIAN_POINT('Ctrl Pts',(-66.59093865008,-29.0804774142854,12.));
#141179=CARTESIAN_POINT('Ctrl Pts',(-66.5657692007906,-29.0794988162897,
0.));
#141180=CARTESIAN_POINT('Ctrl Pts',(-66.5657692007906,-29.0794988162897,
12.));
#141181=CARTESIAN_POINT('Ctrl Pts',(-66.5406404684132,-29.0784978432301,
0.));
#141182=CARTESIAN_POINT('Ctrl Pts',(-66.5406404684132,-29.0784978432301,
12.));
#141183=CARTESIAN_POINT('Ctrl Pts',(-66.5155525573323,-29.0774745547151,
0.));
#141184=CARTESIAN_POINT('Ctrl Pts',(-66.5155525573323,-29.0774745547151,
12.));
#141185=CARTESIAN_POINT('Ctrl Pts',(-66.4905055722868,-29.0764290106554,
0.));
#141186=CARTESIAN_POINT('Ctrl Pts',(-66.4905055722868,-29.0764290106554,
12.));
#141187=CARTESIAN_POINT('Ctrl Pts',(-66.4654996183731,-29.0753612712666,
0.));
#141188=CARTESIAN_POINT('Ctrl Pts',(-66.4654996183731,-29.0753612712666,
12.));
#141189=CARTESIAN_POINT('Ctrl Pts',(-66.4405348010388,-29.0742713970755,
0.));
#141190=CARTESIAN_POINT('Ctrl Pts',(-66.4405348010388,-29.0742713970755,
12.));
#141191=CARTESIAN_POINT('Ctrl Pts',(-66.4156112260887,-29.0731594489211,
0.));
#141192=CARTESIAN_POINT('Ctrl Pts',(-66.4156112260887,-29.0731594489211,
12.));
#141193=CARTESIAN_POINT('Ctrl Pts',(-66.3907289996932,-29.072025487953,
0.));
#141194=CARTESIAN_POINT('Ctrl Pts',(-66.3907289996932,-29.072025487953,
12.));
#141195=CARTESIAN_POINT('Ctrl Pts',(-66.3658882283903,-29.0708695756334,
0.));
#141196=CARTESIAN_POINT('Ctrl Pts',(-66.3658882283903,-29.0708695756334,
12.));
#141197=CARTESIAN_POINT('Ctrl Pts',(-66.3410890190884,-29.0696917737399,
0.));
#141198=CARTESIAN_POINT('Ctrl Pts',(-66.3410890190884,-29.0696917737399,
12.));
#141199=CARTESIAN_POINT('Ctrl Pts',(-66.3163314790615,-29.0684921443721,
0.));
#141200=CARTESIAN_POINT('Ctrl Pts',(-66.3163314790615,-29.0684921443721,
12.));
#141201=CARTESIAN_POINT('Ctrl Pts',(-66.2916157159536,-29.067270749953,
0.));
#141202=CARTESIAN_POINT('Ctrl Pts',(-66.2916157159536,-29.067270749953,
12.));
#141203=CARTESIAN_POINT('Ctrl Pts',(-66.2669418377871,-29.0660276532274,
0.));
#141204=CARTESIAN_POINT('Ctrl Pts',(-66.2669418377871,-29.0660276532274,
12.));
#141205=CARTESIAN_POINT('Ctrl Pts',(-66.2423099529669,-29.0647629172645,
0.));
#141206=CARTESIAN_POINT('Ctrl Pts',(-66.2423099529669,-29.0647629172645,
12.));
#141207=CARTESIAN_POINT('Ctrl Pts',(-66.2177201702818,-29.0634766054598,
0.));
#141208=CARTESIAN_POINT('Ctrl Pts',(-66.2177201702818,-29.0634766054598,
12.));
#141209=CARTESIAN_POINT('Ctrl Pts',(-66.1931725989008,-29.062168781542,
0.));
#141210=CARTESIAN_POINT('Ctrl Pts',(-66.1931725989008,-29.062168781542,
12.));
#141211=CARTESIAN_POINT('Ctrl Pts',(-66.1686673483757,-29.0608395095747,
0.));
#141212=CARTESIAN_POINT('Ctrl Pts',(-66.1686673483757,-29.0608395095747,
12.));
#141213=CARTESIAN_POINT('Ctrl Pts',(-66.144204528652,-29.0594888539558,
0.));
#141214=CARTESIAN_POINT('Ctrl Pts',(-66.144204528652,-29.0594888539558,
12.));
#141215=CARTESIAN_POINT('Ctrl Pts',(-66.1197842500714,-29.0581168794191,
0.));
#141216=CARTESIAN_POINT('Ctrl Pts',(-66.1197842500714,-29.0581168794191,
12.));
#141217=CARTESIAN_POINT('Ctrl Pts',(-66.0954066233752,-29.0567236510372,
0.));
#141218=CARTESIAN_POINT('Ctrl Pts',(-66.0954066233752,-29.0567236510372,
12.));
#141219=CARTESIAN_POINT('Ctrl Pts',(-66.0710717597003,-29.0553092342275,
0.));
#141220=CARTESIAN_POINT('Ctrl Pts',(-66.0710717597003,-29.0553092342275,
12.));
#141221=CARTESIAN_POINT('Ctrl Pts',(-66.0467797705806,-29.0538736947547,
0.));
#141222=CARTESIAN_POINT('Ctrl Pts',(-66.0467797705806,-29.0538736947547,
12.));
#141223=CARTESIAN_POINT('Ctrl Pts',(-66.0225307679584,-29.0524170987303,
0.));
#141224=CARTESIAN_POINT('Ctrl Pts',(-66.0225307679584,-29.0524170987303,
12.));
#141225=CARTESIAN_POINT('Ctrl Pts',(-65.9983248641877,-29.0509395126141,
0.));
#141226=CARTESIAN_POINT('Ctrl Pts',(-65.9983248641877,-29.0509395126141,
12.));
#141227=CARTESIAN_POINT('Ctrl Pts',(-65.9741621720372,-29.0494410032173,
0.));
#141228=CARTESIAN_POINT('Ctrl Pts',(-65.9741621720372,-29.0494410032173,
12.));
#141229=CARTESIAN_POINT('Ctrl Pts',(-65.9500428046873,-29.0479216377082,
0.));
#141230=CARTESIAN_POINT('Ctrl Pts',(-65.9500428046873,-29.0479216377082,
12.));
#141231=CARTESIAN_POINT('Ctrl Pts',(-65.9259668757309,-29.0463814836158,
0.));
#141232=CARTESIAN_POINT('Ctrl Pts',(-65.9259668757309,-29.0463814836158,
12.));
#141233=CARTESIAN_POINT('Ctrl Pts',(-65.9019344991854,-29.0448206088288,
0.));
#141234=CARTESIAN_POINT('Ctrl Pts',(-65.9019344991854,-29.0448206088288,
12.));
#141235=CARTESIAN_POINT('Ctrl Pts',(-65.8779457894959,-29.0432390815977,
0.));
#141236=CARTESIAN_POINT('Ctrl Pts',(-65.8779457894959,-29.0432390815977,
12.));
#141237=CARTESIAN_POINT('Ctrl Pts',(-65.854000861539,-29.0416369705375,
0.));
#141238=CARTESIAN_POINT('Ctrl Pts',(-65.854000861539,-29.0416369705375,
12.));
#141239=CARTESIAN_POINT('Ctrl Pts',(-65.8300998306198,-29.0400143446341,
0.));
#141240=CARTESIAN_POINT('Ctrl Pts',(-65.8300998306198,-29.0400143446341,
12.));
#141241=CARTESIAN_POINT('Ctrl Pts',(-65.8062428124723,-29.0383712732473,
0.));
#141242=CARTESIAN_POINT('Ctrl Pts',(-65.8062428124723,-29.0383712732473,
12.));
#141243=CARTESIAN_POINT('Ctrl Pts',(-65.7824299232715,-29.0367078261107,
0.));
#141244=CARTESIAN_POINT('Ctrl Pts',(-65.7824299232715,-29.0367078261107,
12.));
#141245=CARTESIAN_POINT('Ctrl Pts',(-65.7586612796375,-29.0350240733333,
0.));
#141246=CARTESIAN_POINT('Ctrl Pts',(-65.7586612796375,-29.0350240733333,
12.));
#141247=CARTESIAN_POINT('Ctrl Pts',(-65.7349369986382,-29.0333200854026,
0.));
#141248=CARTESIAN_POINT('Ctrl Pts',(-65.7349369986382,-29.0333200854026,
12.));
#141249=CARTESIAN_POINT('Ctrl Pts',(-65.7112571977874,-29.0315959331911,
0.));
#141250=CARTESIAN_POINT('Ctrl Pts',(-65.7112571977874,-29.0315959331911,
12.));
#141251=CARTESIAN_POINT('Ctrl Pts',(-65.6876219950465,-29.0298516879599,
0.));
#141252=CARTESIAN_POINT('Ctrl Pts',(-65.6876219950465,-29.0298516879599,
12.));
#141253=CARTESIAN_POINT('Ctrl Pts',(-65.664031508836,-29.0280874213584,
0.));
#141254=CARTESIAN_POINT('Ctrl Pts',(-65.664031508836,-29.0280874213584,
12.));
#141255=CARTESIAN_POINT('Ctrl Pts',(-65.6404858580391,-29.0263032054261,
0.));
#141256=CARTESIAN_POINT('Ctrl Pts',(-65.6404858580391,-29.0263032054261,
12.));
#141257=CARTESIAN_POINT('Ctrl Pts',(-65.6169851620054,-29.0244991125962,
0.));
#141258=CARTESIAN_POINT('Ctrl Pts',(-65.6169851620054,-29.0244991125962,
12.));
#141259=CARTESIAN_POINT('Ctrl Pts',(-65.593529540548,-29.0226752157013,
0.));
#141260=CARTESIAN_POINT('Ctrl Pts',(-65.593529540548,-29.0226752157013,
12.));
#141261=CARTESIAN_POINT('Ctrl Pts',(-65.5701191139455,-29.0208315879778,
0.));
#141262=CARTESIAN_POINT('Ctrl Pts',(-65.5701191139455,-29.0208315879778,
12.));
#141263=CARTESIAN_POINT('Ctrl Pts',(-65.5467540029546,-29.0189683030654,
0.));
#141264=CARTESIAN_POINT('Ctrl Pts',(-65.5467540029546,-29.0189683030654,
12.));
#141265=CARTESIAN_POINT('Ctrl Pts',(-65.523434328815,-29.01708543501,0.));
#141266=CARTESIAN_POINT('Ctrl Pts',(-65.523434328815,-29.01708543501,12.));
#141267=CARTESIAN_POINT('Ctrl Pts',(-65.5001602132524,-29.015183058267,
0.));
#141268=CARTESIAN_POINT('Ctrl Pts',(-65.5001602132524,-29.015183058267,
12.));
#141269=CARTESIAN_POINT('Ctrl Pts',(-65.4769317784754,-29.0132612477075,
0.));
#141270=CARTESIAN_POINT('Ctrl Pts',(-65.4769317784754,-29.0132612477075,
12.));
#141271=CARTESIAN_POINT('Ctrl Pts',(-65.4537491471782,-29.0113200786219,
0.));
#141272=CARTESIAN_POINT('Ctrl Pts',(-65.4537491471782,-29.0113200786219,
12.));
#141273=CARTESIAN_POINT('Ctrl Pts',(-65.4306124425524,-29.0093596267198,
0.));
#141274=CARTESIAN_POINT('Ctrl Pts',(-65.4306124425524,-29.0093596267198,
12.));
#141275=CARTESIAN_POINT('Ctrl Pts',(-65.4075217882921,-29.0073799681336,
0.));
#141276=CARTESIAN_POINT('Ctrl Pts',(-65.4075217882921,-29.0073799681336,
12.));
#141277=CARTESIAN_POINT('Ctrl Pts',(-65.3844773085976,-29.0053811794214,
0.));
#141278=CARTESIAN_POINT('Ctrl Pts',(-65.3844773085976,-29.0053811794214,
12.));
#141279=CARTESIAN_POINT('Ctrl Pts',(-65.3614791281726,-29.0033633375745,
0.));
#141280=CARTESIAN_POINT('Ctrl Pts',(-65.3614791281726,-29.0033633375745,
12.));
#141281=CARTESIAN_POINT('Ctrl Pts',(-65.3385273722278,-29.0013265200201,
0.));
#141282=CARTESIAN_POINT('Ctrl Pts',(-65.3385273722278,-29.0013265200201,
12.));
#141283=CARTESIAN_POINT('Ctrl Pts',(-65.3156221664942,-28.9992708046223,
0.));
#141284=CARTESIAN_POINT('Ctrl Pts',(-65.3156221664942,-28.9992708046223,
12.));
#141285=CARTESIAN_POINT('Ctrl Pts',(-65.2927636372261,-28.9971962696848,
0.));
#141286=CARTESIAN_POINT('Ctrl Pts',(-65.2927636372261,-28.9971962696848,
12.));
#141287=CARTESIAN_POINT('Ctrl Pts',(-65.2699519112052,-28.9951029939551,
0.));
#141288=CARTESIAN_POINT('Ctrl Pts',(-65.2699519112052,-28.9951029939551,
12.));
#141289=CARTESIAN_POINT('Ctrl Pts',(-65.2471871157375,-28.9929910566314,
0.));
#141290=CARTESIAN_POINT('Ctrl Pts',(-65.2471871157375,-28.9929910566314,
12.));
#141291=CARTESIAN_POINT('Ctrl Pts',(-65.2244693786586,-28.9908605373652,
0.));
#141292=CARTESIAN_POINT('Ctrl Pts',(-65.2244693786586,-28.9908605373652,
12.));
#141293=CARTESIAN_POINT('Ctrl Pts',(-65.2017988283465,-28.9887115162626,
0.));
#141294=CARTESIAN_POINT('Ctrl Pts',(-65.2017988283465,-28.9887115162626,
12.));
#141295=CARTESIAN_POINT('Ctrl Pts',(-65.1791755937254,-28.9865440738882,
0.));
#141296=CARTESIAN_POINT('Ctrl Pts',(-65.1791755937254,-28.9865440738882,
12.));
#141297=CARTESIAN_POINT('Ctrl Pts',(-65.1565998042705,-28.9843582912697,
0.));
#141298=CARTESIAN_POINT('Ctrl Pts',(-65.1565998042705,-28.9843582912697,
12.));
#141299=CARTESIAN_POINT('Ctrl Pts',(-65.1340715900042,-28.9821542499049,
0.));
#141300=CARTESIAN_POINT('Ctrl Pts',(-65.1340715900042,-28.9821542499049,
12.));
#141301=CARTESIAN_POINT('Ctrl Pts',(-65.111591081505,-28.9799320317648,
0.));
#141302=CARTESIAN_POINT('Ctrl Pts',(-65.111591081505,-28.9799320317648,
12.));
#141303=CARTESIAN_POINT('Ctrl Pts',(-65.0891584099174,-28.9776917192936,
0.));
#141304=CARTESIAN_POINT('Ctrl Pts',(-65.0891584099174,-28.9776917192936,
12.));
#141305=CARTESIAN_POINT('Ctrl Pts',(-65.0667737069562,-28.9754333954134,
0.));
#141306=CARTESIAN_POINT('Ctrl Pts',(-65.0667737069562,-28.9754333954134,
12.));
#141307=CARTESIAN_POINT('Ctrl Pts',(-65.0444371049082,-28.9731571435281,
0.));
#141308=CARTESIAN_POINT('Ctrl Pts',(-65.0444371049082,-28.9731571435281,
12.));
#141309=CARTESIAN_POINT('Ctrl Pts',(-65.0221487366279,-28.9708630475298,
0.));
#141310=CARTESIAN_POINT('Ctrl Pts',(-65.0221487366279,-28.9708630475298,
12.));
#141311=CARTESIAN_POINT('Ctrl Pts',(-64.9999087355504,-28.9685511918017,
0.));
#141312=CARTESIAN_POINT('Ctrl Pts',(-64.9999087355504,-28.9685511918017,
12.));
#141313=CARTESIAN_POINT('Ctrl Pts',(-64.9777172357028,-28.9662216612216,
0.));
#141314=CARTESIAN_POINT('Ctrl Pts',(-64.9777172357028,-28.9662216612216,
12.));
#141315=CARTESIAN_POINT('Ctrl Pts',(-64.955574371711,-28.9638745411677,
0.));
#141316=CARTESIAN_POINT('Ctrl Pts',(-64.955574371711,-28.9638745411677,
12.));
#141317=CARTESIAN_POINT('Ctrl Pts',(-64.9334802788037,-28.961509917525,
0.));
#141318=CARTESIAN_POINT('Ctrl Pts',(-64.9334802788037,-28.961509917525,
12.));
#141319=CARTESIAN_POINT('Ctrl Pts',(-64.9114350928124,-28.9591278766934,
0.));
#141320=CARTESIAN_POINT('Ctrl Pts',(-64.9114350928124,-28.9591278766934,
12.));
#141321=CARTESIAN_POINT('Ctrl Pts',(-64.8894389501799,-28.9567285055866,
0.));
#141322=CARTESIAN_POINT('Ctrl Pts',(-64.8894389501799,-28.9567285055866,
12.));
#141323=CARTESIAN_POINT('Ctrl Pts',(-64.8674919879646,-28.9543118916327,
0.));
#141324=CARTESIAN_POINT('Ctrl Pts',(-64.8674919879646,-28.9543118916327,
12.));
#141325=CARTESIAN_POINT('Ctrl Pts',(-64.8455943438423,-28.9518781227765,
0.));
#141326=CARTESIAN_POINT('Ctrl Pts',(-64.8455943438423,-28.9518781227765,
12.));
#141327=CARTESIAN_POINT('Ctrl Pts',(-64.8237461561024,-28.9494272874833,
0.));
#141328=CARTESIAN_POINT('Ctrl Pts',(-64.8237461561024,-28.9494272874833,
12.));
#141329=CARTESIAN_POINT('Ctrl Pts',(-64.8019475636454,-28.9469594747436,
0.));
#141330=CARTESIAN_POINT('Ctrl Pts',(-64.8019475636454,-28.9469594747436,
12.));
#141331=CARTESIAN_POINT('Ctrl Pts',(-64.7801987060097,-28.9444747740815,
0.));
#141332=CARTESIAN_POINT('Ctrl Pts',(-64.7801987060097,-28.9444747740815,
12.));
#141333=CARTESIAN_POINT('Ctrl Pts',(-64.7584997233889,-28.9419732755659,
0.));
#141334=CARTESIAN_POINT('Ctrl Pts',(-64.7584997233889,-28.9419732755659,
12.));
#141335=CARTESIAN_POINT('Ctrl Pts',(-64.7368507566461,-28.9394550698201,
0.));
#141336=CARTESIAN_POINT('Ctrl Pts',(-64.7368507566461,-28.9394550698201,
12.));
#141337=CARTESIAN_POINT('Ctrl Pts',(-64.715251947327,-28.9369202480383,
0.));
#141338=CARTESIAN_POINT('Ctrl Pts',(-64.715251947327,-28.9369202480383,
12.));
#141339=CARTESIAN_POINT('Ctrl Pts',(-64.6937034376591,-28.934368901987,
0.));
#141340=CARTESIAN_POINT('Ctrl Pts',(-64.6937034376591,-28.934368901987,
12.));
#141341=CARTESIAN_POINT('Ctrl Pts',(-64.6722053705389,-28.9318011239905,
0.));
#141342=CARTESIAN_POINT('Ctrl Pts',(-64.6722053705389,-28.9318011239905,
12.));
#141343=CARTESIAN_POINT('Ctrl Pts',(-64.6507578895155,-28.9292170069219,
0.));
#141344=CARTESIAN_POINT('Ctrl Pts',(-64.6507578895155,-28.9292170069219,
12.));
#141345=CARTESIAN_POINT('Ctrl Pts',(-64.6293611387753,-28.9266166441956,
0.));
#141346=CARTESIAN_POINT('Ctrl Pts',(-64.6293611387753,-28.9266166441956,
12.));
#141347=CARTESIAN_POINT('Ctrl Pts',(-64.6080152631065,-28.9240001297553,
0.));
#141348=CARTESIAN_POINT('Ctrl Pts',(-64.6080152631065,-28.9240001297553,
12.));
#141349=CARTESIAN_POINT('Ctrl Pts',(-64.5867204079452,-28.9213675580996,
0.));
#141350=CARTESIAN_POINT('Ctrl Pts',(-64.5867204079452,-28.9213675580996,
12.));
#141351=CARTESIAN_POINT('Ctrl Pts',(-64.5654767194487,-28.9187190243231,
0.));
#141352=CARTESIAN_POINT('Ctrl Pts',(-64.5654767194487,-28.9187190243231,
12.));
#141353=CARTESIAN_POINT('Ctrl Pts',(-64.544284344556,-28.9160546241538,
0.));
#141354=CARTESIAN_POINT('Ctrl Pts',(-64.544284344556,-28.9160546241538,
12.));
#141355=CARTESIAN_POINT('Ctrl Pts',(-64.5231434310457,-28.9133744539943,
0.));
#141356=CARTESIAN_POINT('Ctrl Pts',(-64.5231434310457,-28.9133744539943,
12.));
#141357=CARTESIAN_POINT('Ctrl Pts',(-64.5020541275927,-28.9106786109639,
0.));
#141358=CARTESIAN_POINT('Ctrl Pts',(-64.5020541275927,-28.9106786109639,
12.));
#141359=CARTESIAN_POINT('Ctrl Pts',(-64.4810165836568,-28.9079671928253,
0.));
#141360=CARTESIAN_POINT('Ctrl Pts',(-64.4810165836568,-28.9079671928253,
12.));
#141361=CARTESIAN_POINT('Ctrl Pts',(-64.460030949357,-28.9052402979055,
0.));
#141362=CARTESIAN_POINT('Ctrl Pts',(-64.460030949357,-28.9052402979055,
12.));
#141363=CARTESIAN_POINT('Ctrl Pts',(-64.439097375364,-28.9024980250309,
0.));
#141364=CARTESIAN_POINT('Ctrl Pts',(-64.439097375364,-28.9024980250309,
12.));
#141365=CARTESIAN_POINT('Ctrl Pts',(-64.4182160127401,-28.899740473435,
0.));
#141366=CARTESIAN_POINT('Ctrl Pts',(-64.4182160127401,-28.899740473435,
12.));
#141367=CARTESIAN_POINT('Ctrl Pts',(-64.3973870129201,-28.8969677427519,
0.));
#141368=CARTESIAN_POINT('Ctrl Pts',(-64.3973870129201,-28.8969677427519,
12.));
#141369=CARTESIAN_POINT('Ctrl Pts',(-64.3766105280715,-28.8941799332312,
0.));
#141370=CARTESIAN_POINT('Ctrl Pts',(-64.3766105280715,-28.8941799332312,
12.));
#141371=CARTESIAN_POINT('Ctrl Pts',(-64.3558867114087,-28.8913771459327,
0.));
#141372=CARTESIAN_POINT('Ctrl Pts',(-64.3558867114087,-28.8913771459327,
12.));
#141373=CARTESIAN_POINT('Ctrl Pts',(-64.3352157174606,-28.888559482892,
0.));
#141374=CARTESIAN_POINT('Ctrl Pts',(-64.3352157174606,-28.888559482892,
12.));
#141375=CARTESIAN_POINT('Ctrl Pts',(-64.3145977025005,-28.8857270473944,
0.));
#141376=CARTESIAN_POINT('Ctrl Pts',(-64.3145977025005,-28.8857270473944,
12.));
#141377=CARTESIAN_POINT('Ctrl Pts',(-64.2940328242482,-28.8828799437922,
0.));
#141378=CARTESIAN_POINT('Ctrl Pts',(-64.2940328242482,-28.8828799437922,
12.));
#141379=CARTESIAN_POINT('Ctrl Pts',(-64.2735212410682,-28.8800182770052,
0.));
#141380=CARTESIAN_POINT('Ctrl Pts',(-64.2735212410682,-28.8800182770052,
12.));
#141381=CARTESIAN_POINT('Ctrl Pts',(-64.2530631112926,-28.8771421521058,
0.));
#141382=CARTESIAN_POINT('Ctrl Pts',(-64.2530631112926,-28.8771421521058,
12.));
#141383=CARTESIAN_POINT('Ctrl Pts',(-64.232658592528,-28.8742516738959,
0.));
#141384=CARTESIAN_POINT('Ctrl Pts',(-64.232658592528,-28.8742516738959,
12.));
#141385=CARTESIAN_POINT('Ctrl Pts',(-64.2123078408507,-28.8713469464205,
0.));
#141386=CARTESIAN_POINT('Ctrl Pts',(-64.2123078408507,-28.8713469464205,
12.));
#141387=CARTESIAN_POINT('Ctrl Pts',(-64.1920110123342,-28.8684280739033,
0.));
#141388=CARTESIAN_POINT('Ctrl Pts',(-64.1920110123342,-28.8684280739033,
12.));
#141389=CARTESIAN_POINT('Ctrl Pts',(-64.1717682648708,-28.8654951618659,
0.));
#141390=CARTESIAN_POINT('Ctrl Pts',(-64.1717682648708,-28.8654951618659,
12.));
#141391=CARTESIAN_POINT('Ctrl Pts',(-64.1515797596555,-28.8625483180433,
0.));
#141392=CARTESIAN_POINT('Ctrl Pts',(-64.1515797596555,-28.8625483180433,
12.));
#141393=CARTESIAN_POINT('Ctrl Pts',(-64.1314456633345,-28.8595876537132,
0.));
#141394=CARTESIAN_POINT('Ctrl Pts',(-64.1314456633345,-28.8595876537132,
12.));
#141395=CARTESIAN_POINT('Ctrl Pts',(-64.1113661481918,-28.8566132838157,
0.));
#141396=CARTESIAN_POINT('Ctrl Pts',(-64.1113661481918,-28.8566132838157,
12.));
#141397=CARTESIAN_POINT('Ctrl Pts',(-64.0913413876586,-28.8536253241837,
0.));
#141398=CARTESIAN_POINT('Ctrl Pts',(-64.0913413876586,-28.8536253241837,
12.));
#141399=CARTESIAN_POINT('Ctrl Pts',(-64.0713715523588,-28.8506238891087,
0.));
#141400=CARTESIAN_POINT('Ctrl Pts',(-64.0713715523588,-28.8506238891087,
12.));
#141401=CARTESIAN_POINT('Ctrl Pts',(-64.0514568066659,-28.8476090892242,
0.));
#141402=CARTESIAN_POINT('Ctrl Pts',(-64.0514568066659,-28.8476090892242,
12.));
#141403=CARTESIAN_POINT('Ctrl Pts',(-64.0315973031994,-28.8445810281275,
0.));
#141404=CARTESIAN_POINT('Ctrl Pts',(-64.0315973031994,-28.8445810281275,
12.));
#141405=CARTESIAN_POINT('Ctrl Pts',(-64.0117931881364,-28.841539805646,
0.));
#141406=CARTESIAN_POINT('Ctrl Pts',(-64.0117931881364,-28.841539805646,
12.));
#141407=CARTESIAN_POINT('Ctrl Pts',(-63.9920446117632,-28.8384855243267,
0.));
#141408=CARTESIAN_POINT('Ctrl Pts',(-63.9920446117632,-28.8384855243267,
12.));
#141409=CARTESIAN_POINT('Ctrl Pts',(-63.9723517369614,-28.8354182946601,
0.));
#141410=CARTESIAN_POINT('Ctrl Pts',(-63.9723517369614,-28.8354182946601,
12.));
#141411=CARTESIAN_POINT('Ctrl Pts',(-63.9527147494351,-28.8323382413752,
0.));
#141412=CARTESIAN_POINT('Ctrl Pts',(-63.9527147494351,-28.8323382413752,
12.));
#141413=CARTESIAN_POINT('Ctrl Pts',(-63.9331338646868,-28.8292455077494,
0.));
#141414=CARTESIAN_POINT('Ctrl Pts',(-63.9331338646868,-28.8292455077494,
12.));
#141415=CARTESIAN_POINT('Ctrl Pts',(-63.9136093063647,-28.826140242322,
0.));
#141416=CARTESIAN_POINT('Ctrl Pts',(-63.9136093063647,-28.826140242322,
12.));
#141417=CARTESIAN_POINT('Ctrl Pts',(-63.894141285685,-28.8230225863142,
0.));
#141418=CARTESIAN_POINT('Ctrl Pts',(-63.894141285685,-28.8230225863142,
12.));
#141419=CARTESIAN_POINT('Ctrl Pts',(-63.8747299825383,-28.8198926619893,
0.));
#141420=CARTESIAN_POINT('Ctrl Pts',(-63.8747299825383,-28.8198926619893,
12.));
#141421=CARTESIAN_POINT('Ctrl Pts',(-63.8553755207732,-28.8167505576806,
0.));
#141422=CARTESIAN_POINT('Ctrl Pts',(-63.8553755207732,-28.8167505576806,
12.));
#141423=CARTESIAN_POINT('Ctrl Pts',(-63.8360779670226,-28.8135963263557,
0.));
#141424=CARTESIAN_POINT('Ctrl Pts',(-63.8360779670226,-28.8135963263557,
12.));
#141425=CARTESIAN_POINT('Ctrl Pts',(-63.8206854735372,-28.8110632621133,
0.));
#141426=CARTESIAN_POINT('Ctrl Pts',(-63.8206854735372,-28.8110632621133,
12.));
#141427=CARTESIAN_POINT('Ctrl Pts',(-63.809166727145,-28.8091580239664,
0.));
#141428=CARTESIAN_POINT('Ctrl Pts',(-63.809166727145,-28.8091580239664,
12.));
#141429=CARTESIAN_POINT('Ctrl Pts',(-63.8014989507575,-28.8078854475473,
0.));
#141430=CARTESIAN_POINT('Ctrl Pts',(-63.8014989507575,-28.8078854475473,
12.));
#141431=CARTESIAN_POINT('Ctrl Pts',(-63.7976679095314,-28.8072485549236,
0.));
#141432=CARTESIAN_POINT('Ctrl Pts',(-63.7976679095314,-28.8072485549236,
12.));
#141433=CARTESIAN_POINT('',(-63.7976679095314,-28.8072485549236,12.));
#141434=CARTESIAN_POINT('Ctrl Pts',(-63.7976679095314,-28.8072485549236,
12.));
#141435=CARTESIAN_POINT('Ctrl Pts',(-63.8014989507575,-28.8078854475473,
12.));
#141436=CARTESIAN_POINT('Ctrl Pts',(-63.809166727145,-28.8091580239664,
12.));
#141437=CARTESIAN_POINT('Ctrl Pts',(-63.8206854735372,-28.8110632621133,
12.));
#141438=CARTESIAN_POINT('Ctrl Pts',(-63.8360779670226,-28.8135963263557,
12.));
#141439=CARTESIAN_POINT('Ctrl Pts',(-63.8553755207732,-28.8167505576806,
12.));
#141440=CARTESIAN_POINT('Ctrl Pts',(-63.8747299825383,-28.8198926619893,
12.));
#141441=CARTESIAN_POINT('Ctrl Pts',(-63.894141285685,-28.8230225863142,
12.));
#141442=CARTESIAN_POINT('Ctrl Pts',(-63.9136093063647,-28.826140242322,
12.));
#141443=CARTESIAN_POINT('Ctrl Pts',(-63.9331338646868,-28.8292455077494,
12.));
#141444=CARTESIAN_POINT('Ctrl Pts',(-63.9527147494351,-28.8323382413752,
12.));
#141445=CARTESIAN_POINT('Ctrl Pts',(-63.9723517369614,-28.8354182946601,
12.));
#141446=CARTESIAN_POINT('Ctrl Pts',(-63.9920446117632,-28.8384855243267,
12.));
#141447=CARTESIAN_POINT('Ctrl Pts',(-64.0117931881364,-28.841539805646,
12.));
#141448=CARTESIAN_POINT('Ctrl Pts',(-64.0315973031994,-28.8445810281275,
12.));
#141449=CARTESIAN_POINT('Ctrl Pts',(-64.0514568066659,-28.8476090892242,
12.));
#141450=CARTESIAN_POINT('Ctrl Pts',(-64.0713715523588,-28.8506238891087,
12.));
#141451=CARTESIAN_POINT('Ctrl Pts',(-64.0913413876586,-28.8536253241837,
12.));
#141452=CARTESIAN_POINT('Ctrl Pts',(-64.1113661481918,-28.8566132838157,
12.));
#141453=CARTESIAN_POINT('Ctrl Pts',(-64.1314456633345,-28.8595876537132,
12.));
#141454=CARTESIAN_POINT('Ctrl Pts',(-64.1515797596555,-28.8625483180433,
12.));
#141455=CARTESIAN_POINT('Ctrl Pts',(-64.1717682648708,-28.8654951618659,
12.));
#141456=CARTESIAN_POINT('Ctrl Pts',(-64.1920110123342,-28.8684280739033,
12.));
#141457=CARTESIAN_POINT('Ctrl Pts',(-64.2123078408507,-28.8713469464205,
12.));
#141458=CARTESIAN_POINT('Ctrl Pts',(-64.232658592528,-28.8742516738959,
12.));
#141459=CARTESIAN_POINT('Ctrl Pts',(-64.2530631112926,-28.8771421521058,
12.));
#141460=CARTESIAN_POINT('Ctrl Pts',(-64.2735212410682,-28.8800182770052,
12.));
#141461=CARTESIAN_POINT('Ctrl Pts',(-64.2940328242482,-28.8828799437922,
12.));
#141462=CARTESIAN_POINT('Ctrl Pts',(-64.3145977025005,-28.8857270473944,
12.));
#141463=CARTESIAN_POINT('Ctrl Pts',(-64.3352157174606,-28.888559482892,
12.));
#141464=CARTESIAN_POINT('Ctrl Pts',(-64.3558867114087,-28.8913771459327,
12.));
#141465=CARTESIAN_POINT('Ctrl Pts',(-64.3766105280715,-28.8941799332312,
12.));
#141466=CARTESIAN_POINT('Ctrl Pts',(-64.3973870129201,-28.8969677427519,
12.));
#141467=CARTESIAN_POINT('Ctrl Pts',(-64.4182160127401,-28.899740473435,
12.));
#141468=CARTESIAN_POINT('Ctrl Pts',(-64.439097375364,-28.9024980250309,
12.));
#141469=CARTESIAN_POINT('Ctrl Pts',(-64.460030949357,-28.9052402979055,
12.));
#141470=CARTESIAN_POINT('Ctrl Pts',(-64.4810165836568,-28.9079671928253,
12.));
#141471=CARTESIAN_POINT('Ctrl Pts',(-64.5020541275927,-28.9106786109639,
12.));
#141472=CARTESIAN_POINT('Ctrl Pts',(-64.5231434310457,-28.9133744539943,
12.));
#141473=CARTESIAN_POINT('Ctrl Pts',(-64.544284344556,-28.9160546241538,
12.));
#141474=CARTESIAN_POINT('Ctrl Pts',(-64.5654767194487,-28.9187190243231,
12.));
#141475=CARTESIAN_POINT('Ctrl Pts',(-64.5867204079452,-28.9213675580996,
12.));
#141476=CARTESIAN_POINT('Ctrl Pts',(-64.6080152631065,-28.9240001297553,
12.));
#141477=CARTESIAN_POINT('Ctrl Pts',(-64.6293611387753,-28.9266166441956,
12.));
#141478=CARTESIAN_POINT('Ctrl Pts',(-64.6507578895155,-28.9292170069219,
12.));
#141479=CARTESIAN_POINT('Ctrl Pts',(-64.6722053705389,-28.9318011239905,
12.));
#141480=CARTESIAN_POINT('Ctrl Pts',(-64.6937034376591,-28.934368901987,
12.));
#141481=CARTESIAN_POINT('Ctrl Pts',(-64.715251947327,-28.9369202480383,
12.));
#141482=CARTESIAN_POINT('Ctrl Pts',(-64.7368507566461,-28.9394550698201,
12.));
#141483=CARTESIAN_POINT('Ctrl Pts',(-64.7584997233889,-28.9419732755659,
12.));
#141484=CARTESIAN_POINT('Ctrl Pts',(-64.7801987060097,-28.9444747740815,
12.));
#141485=CARTESIAN_POINT('Ctrl Pts',(-64.8019475636454,-28.9469594747436,
12.));
#141486=CARTESIAN_POINT('Ctrl Pts',(-64.8237461561024,-28.9494272874833,
12.));
#141487=CARTESIAN_POINT('Ctrl Pts',(-64.8455943438423,-28.9518781227765,
12.));
#141488=CARTESIAN_POINT('Ctrl Pts',(-64.8674919879646,-28.9543118916327,
12.));
#141489=CARTESIAN_POINT('Ctrl Pts',(-64.8894389501799,-28.9567285055866,
12.));
#141490=CARTESIAN_POINT('Ctrl Pts',(-64.9114350928124,-28.9591278766934,
12.));
#141491=CARTESIAN_POINT('Ctrl Pts',(-64.9334802788037,-28.961509917525,
12.));
#141492=CARTESIAN_POINT('Ctrl Pts',(-64.955574371711,-28.9638745411677,
12.));
#141493=CARTESIAN_POINT('Ctrl Pts',(-64.9777172357028,-28.9662216612216,
12.));
#141494=CARTESIAN_POINT('Ctrl Pts',(-64.9999087355504,-28.9685511918017,
12.));
#141495=CARTESIAN_POINT('Ctrl Pts',(-65.0221487366279,-28.9708630475298,
12.));
#141496=CARTESIAN_POINT('Ctrl Pts',(-65.0444371049082,-28.9731571435281,
12.));
#141497=CARTESIAN_POINT('Ctrl Pts',(-65.0667737069562,-28.9754333954134,
12.));
#141498=CARTESIAN_POINT('Ctrl Pts',(-65.0891584099174,-28.9776917192936,
12.));
#141499=CARTESIAN_POINT('Ctrl Pts',(-65.111591081505,-28.9799320317648,
12.));
#141500=CARTESIAN_POINT('Ctrl Pts',(-65.1340715900042,-28.9821542499049,
12.));
#141501=CARTESIAN_POINT('Ctrl Pts',(-65.1565998042705,-28.9843582912697,
12.));
#141502=CARTESIAN_POINT('Ctrl Pts',(-65.1791755937254,-28.9865440738882,
12.));
#141503=CARTESIAN_POINT('Ctrl Pts',(-65.2017988283465,-28.9887115162626,
12.));
#141504=CARTESIAN_POINT('Ctrl Pts',(-65.2244693786586,-28.9908605373652,
12.));
#141505=CARTESIAN_POINT('Ctrl Pts',(-65.2471871157375,-28.9929910566314,
12.));
#141506=CARTESIAN_POINT('Ctrl Pts',(-65.2699519112052,-28.9951029939551,
12.));
#141507=CARTESIAN_POINT('Ctrl Pts',(-65.2927636372261,-28.9971962696848,
12.));
#141508=CARTESIAN_POINT('Ctrl Pts',(-65.3156221664942,-28.9992708046223,
12.));
#141509=CARTESIAN_POINT('Ctrl Pts',(-65.3385273722278,-29.0013265200201,
12.));
#141510=CARTESIAN_POINT('Ctrl Pts',(-65.3614791281726,-29.0033633375745,
12.));
#141511=CARTESIAN_POINT('Ctrl Pts',(-65.3844773085976,-29.0053811794214,
12.));
#141512=CARTESIAN_POINT('Ctrl Pts',(-65.4075217882921,-29.0073799681336,
12.));
#141513=CARTESIAN_POINT('Ctrl Pts',(-65.4306124425524,-29.0093596267198,
12.));
#141514=CARTESIAN_POINT('Ctrl Pts',(-65.4537491471782,-29.0113200786219,
12.));
#141515=CARTESIAN_POINT('Ctrl Pts',(-65.4769317784754,-29.0132612477075,
12.));
#141516=CARTESIAN_POINT('Ctrl Pts',(-65.5001602132524,-29.015183058267,
12.));
#141517=CARTESIAN_POINT('Ctrl Pts',(-65.523434328815,-29.01708543501,12.));
#141518=CARTESIAN_POINT('Ctrl Pts',(-65.5467540029546,-29.0189683030654,
12.));
#141519=CARTESIAN_POINT('Ctrl Pts',(-65.5701191139455,-29.0208315879778,
12.));
#141520=CARTESIAN_POINT('Ctrl Pts',(-65.593529540548,-29.0226752157013,
12.));
#141521=CARTESIAN_POINT('Ctrl Pts',(-65.6169851620054,-29.0244991125962,
12.));
#141522=CARTESIAN_POINT('Ctrl Pts',(-65.6404858580391,-29.0263032054261,
12.));
#141523=CARTESIAN_POINT('Ctrl Pts',(-65.664031508836,-29.0280874213584,
12.));
#141524=CARTESIAN_POINT('Ctrl Pts',(-65.6876219950465,-29.0298516879599,
12.));
#141525=CARTESIAN_POINT('Ctrl Pts',(-65.7112571977874,-29.0315959331911,
12.));
#141526=CARTESIAN_POINT('Ctrl Pts',(-65.7349369986382,-29.0333200854026,
12.));
#141527=CARTESIAN_POINT('Ctrl Pts',(-65.7586612796375,-29.0350240733333,
12.));
#141528=CARTESIAN_POINT('Ctrl Pts',(-65.7824299232715,-29.0367078261107,
12.));
#141529=CARTESIAN_POINT('Ctrl Pts',(-65.8062428124723,-29.0383712732473,
12.));
#141530=CARTESIAN_POINT('Ctrl Pts',(-65.8300998306198,-29.0400143446341,
12.));
#141531=CARTESIAN_POINT('Ctrl Pts',(-65.854000861539,-29.0416369705375,
12.));
#141532=CARTESIAN_POINT('Ctrl Pts',(-65.8779457894959,-29.0432390815977,
12.));
#141533=CARTESIAN_POINT('Ctrl Pts',(-65.9019344991854,-29.0448206088288,
12.));
#141534=CARTESIAN_POINT('Ctrl Pts',(-65.9259668757309,-29.0463814836158,
12.));
#141535=CARTESIAN_POINT('Ctrl Pts',(-65.9500428046873,-29.0479216377082,
12.));
#141536=CARTESIAN_POINT('Ctrl Pts',(-65.9741621720372,-29.0494410032173,
12.));
#141537=CARTESIAN_POINT('Ctrl Pts',(-65.9983248641877,-29.0509395126141,
12.));
#141538=CARTESIAN_POINT('Ctrl Pts',(-66.0225307679584,-29.0524170987303,
12.));
#141539=CARTESIAN_POINT('Ctrl Pts',(-66.0467797705806,-29.0538736947547,
12.));
#141540=CARTESIAN_POINT('Ctrl Pts',(-66.0710717597003,-29.0553092342275,
12.));
#141541=CARTESIAN_POINT('Ctrl Pts',(-66.0954066233752,-29.0567236510372,
12.));
#141542=CARTESIAN_POINT('Ctrl Pts',(-66.1197842500714,-29.0581168794191,
12.));
#141543=CARTESIAN_POINT('Ctrl Pts',(-66.144204528652,-29.0594888539558,
12.));
#141544=CARTESIAN_POINT('Ctrl Pts',(-66.1686673483757,-29.0608395095747,
12.));
#141545=CARTESIAN_POINT('Ctrl Pts',(-66.1931725989008,-29.062168781542,
12.));
#141546=CARTESIAN_POINT('Ctrl Pts',(-66.2177201702818,-29.0634766054598,
12.));
#141547=CARTESIAN_POINT('Ctrl Pts',(-66.2423099529669,-29.0647629172645,
12.));
#141548=CARTESIAN_POINT('Ctrl Pts',(-66.2669418377871,-29.0660276532274,
12.));
#141549=CARTESIAN_POINT('Ctrl Pts',(-66.2916157159536,-29.067270749953,
12.));
#141550=CARTESIAN_POINT('Ctrl Pts',(-66.3163314790615,-29.0684921443721,
12.));
#141551=CARTESIAN_POINT('Ctrl Pts',(-66.3410890190884,-29.0696917737399,
12.));
#141552=CARTESIAN_POINT('Ctrl Pts',(-66.3658882283903,-29.0708695756334,
12.));
#141553=CARTESIAN_POINT('Ctrl Pts',(-66.3907289996932,-29.072025487953,
12.));
#141554=CARTESIAN_POINT('Ctrl Pts',(-66.4156112260887,-29.0731594489211,
12.));
#141555=CARTESIAN_POINT('Ctrl Pts',(-66.4405348010388,-29.0742713970755,
12.));
#141556=CARTESIAN_POINT('Ctrl Pts',(-66.4654996183731,-29.0753612712666,
12.));
#141557=CARTESIAN_POINT('Ctrl Pts',(-66.4905055722868,-29.0764290106554,
12.));
#141558=CARTESIAN_POINT('Ctrl Pts',(-66.5155525573323,-29.0774745547151,
12.));
#141559=CARTESIAN_POINT('Ctrl Pts',(-66.5406404684132,-29.0784978432301,
12.));
#141560=CARTESIAN_POINT('Ctrl Pts',(-66.5657692007906,-29.0794988162897,
12.));
#141561=CARTESIAN_POINT('Ctrl Pts',(-66.59093865008,-29.0804774142854,12.));
#141562=CARTESIAN_POINT('Ctrl Pts',(-66.6161487122502,-29.0814335779084,
12.));
#141563=CARTESIAN_POINT('Ctrl Pts',(-66.6413992836147,-29.0823672481507,
12.));
#141564=CARTESIAN_POINT('Ctrl Pts',(-66.6666902608249,-29.0832783663049,
12.));
#141565=CARTESIAN_POINT('Ctrl Pts',(-66.6920215408751,-29.0841668739588,
12.));
#141566=CARTESIAN_POINT('Ctrl Pts',(-66.7173930211022,-29.0850327129916,
12.));
#141567=CARTESIAN_POINT('Ctrl Pts',(-66.7428045991841,-29.0858758255729,
12.));
#141568=CARTESIAN_POINT('Ctrl Pts',(-66.7682561731341,-29.0866961541626,
12.));
#141569=CARTESIAN_POINT('Ctrl Pts',(-66.793747641293,-29.0874936415132,
12.));
#141570=CARTESIAN_POINT('Ctrl Pts',(-66.8192789023312,-29.088268230663,
12.));
#141571=CARTESIAN_POINT('Ctrl Pts',(-66.8448498552503,-29.0890198649323,
12.));
#141572=CARTESIAN_POINT('Ctrl Pts',(-66.8704603993794,-29.0897484879207,
12.));
#141573=CARTESIAN_POINT('Ctrl Pts',(-66.8961104343707,-29.0904540435065,
12.));
#141574=CARTESIAN_POINT('Ctrl Pts',(-66.9217998601885,-29.0911364758487,
12.));
#141575=CARTESIAN_POINT('Ctrl Pts',(-66.9475285771135,-29.0917957293826,
12.));
#141576=CARTESIAN_POINT('Ctrl Pts',(-66.9732964857466,-29.092431748817,
12.));
#141577=CARTESIAN_POINT('Ctrl Pts',(-66.9991034870083,-29.0930444791328,
12.));
#141578=CARTESIAN_POINT('Ctrl Pts',(-67.0249494821363,-29.0936338655828,
12.));
#141579=CARTESIAN_POINT('Ctrl Pts',(-67.0508343726776,-29.0941998536959,
12.));
#141580=CARTESIAN_POINT('Ctrl Pts',(-67.0767580604879,-29.0947423892727,
12.));
#141581=CARTESIAN_POINT('Ctrl Pts',(-67.1027204477311,-29.0952614183779,
12.));
#141582=CARTESIAN_POINT('Ctrl Pts',(-67.1287214368746,-29.0957568873358,
12.));
#141583=CARTESIAN_POINT('Ctrl Pts',(-67.1547609306843,-29.0962287427273,
12.));
#141584=CARTESIAN_POINT('Ctrl Pts',(-67.1808388322109,-29.096676931389,
12.));
#141585=CARTESIAN_POINT('Ctrl Pts',(-67.2069550447883,-29.0971014004131,
12.));
#141586=CARTESIAN_POINT('Ctrl Pts',(-67.2331094720471,-29.097502097147,
12.));
#141587=CARTESIAN_POINT('Ctrl Pts',(-67.2593020179209,-29.0978789691962,
12.));
#141588=CARTESIAN_POINT('Ctrl Pts',(-67.2855325866517,-29.0982319644277,
12.));
#141589=CARTESIAN_POINT('Ctrl Pts',(-67.311801082792,-29.0985610309771,
12.));
#141590=CARTESIAN_POINT('Ctrl Pts',(-67.3381074112027,-29.0988661172531,
12.));
#141591=CARTESIAN_POINT('Ctrl Pts',(-67.3644514770387,-29.0991471719176,
12.));
#141592=CARTESIAN_POINT('Ctrl Pts',(-67.3908331857323,-29.0994041438719,
12.));
#141593=CARTESIAN_POINT('Ctrl Pts',(-67.4172524429727,-29.0996369822418,
12.));
#141594=CARTESIAN_POINT('Ctrl Pts',(-67.4437091546859,-29.0998456363683,
12.));
#141595=CARTESIAN_POINT('Ctrl Pts',(-67.4702032270048,-29.1000300557955,
12.));
#141596=CARTESIAN_POINT('Ctrl Pts',(-67.4967345663096,-29.1001901902909,
12.));
#141597=CARTESIAN_POINT('Ctrl Pts',(-67.5233030792704,-29.1003259898682,
12.));
#141598=CARTESIAN_POINT('Ctrl Pts',(-67.5499086728888,-29.1004374048148,
12.));
#141599=CARTESIAN_POINT('Ctrl Pts',(-67.5765512545281,-29.1005243857139,
12.));
#141600=CARTESIAN_POINT('Ctrl Pts',(-67.6032307319623,-29.1005868834866,
12.));
#141601=CARTESIAN_POINT('Ctrl Pts',(-67.6299470133295,-29.100624849358,
12.));
#141602=CARTESIAN_POINT('Ctrl Pts',(-67.6567000070326,-29.1006382347814,
12.));
#141603=CARTESIAN_POINT('Ctrl Pts',(-67.6834896216461,-29.1006269913747,
12.));
#141604=CARTESIAN_POINT('Ctrl Pts',(-67.7103157658296,-29.1005910708624,
12.));
#141605=CARTESIAN_POINT('Ctrl Pts',(-67.7371783482035,-29.1005304249987,
12.));
#141606=CARTESIAN_POINT('Ctrl Pts',(-67.7640772773388,-29.1004450055643,
12.));
#141607=CARTESIAN_POINT('Ctrl Pts',(-67.7910124620135,-29.1003347645294,
12.));
#141608=CARTESIAN_POINT('Ctrl Pts',(-67.8179838114099,-29.1001996541842,
12.));
#141609=CARTESIAN_POINT('Ctrl Pts',(-67.8449912353329,-29.1000396272867,
12.));
#141610=CARTESIAN_POINT('Ctrl Pts',(-67.8720346444124,-29.0998546372032,
12.));
#141611=CARTESIAN_POINT('Ctrl Pts',(-67.8991139503193,-29.0996446380626,
12.));
#141612=CARTESIAN_POINT('Ctrl Pts',(-67.9262290652829,-29.099409584422,
12.));
#141613=CARTESIAN_POINT('Ctrl Pts',(-67.9533799016148,-29.0991494309404,
12.));
#141614=CARTESIAN_POINT('Ctrl Pts',(-67.9805663711855,-29.0988641320247,
12.));
#141615=CARTESIAN_POINT('Ctrl Pts',(-68.0077883850121,-29.0985536415531,
12.));
#141616=CARTESIAN_POINT('Ctrl Pts',(-68.0350458525551,-29.0982179124097,
12.));
#141617=CARTESIAN_POINT('Ctrl Pts',(-68.0623386822863,-29.0978568968657,
12.));
#141618=CARTESIAN_POINT('Ctrl Pts',(-68.0896667829567,-29.0974705474259,
12.));
#141619=CARTESIAN_POINT('Ctrl Pts',(-68.1170300646987,-29.0970588175728,
12.));
#141620=CARTESIAN_POINT('Ctrl Pts',(-68.1444284400742,-29.0966216624743,
12.));
#141621=CARTESIAN_POINT('Ctrl Pts',(-68.1718618254281,-29.0961590399046,
12.));
#141622=CARTESIAN_POINT('Ctrl Pts',(-68.1993301412061,-29.0956709104627,
12.));
#141623=CARTESIAN_POINT('Ctrl Pts',(-68.2229056854683,-29.095230591515,
12.));
#141624=CARTESIAN_POINT('Ctrl Pts',(-68.2409993690196,-29.094879194787,
12.));
#141625=CARTESIAN_POINT('Ctrl Pts',(-68.2535957747187,-29.0946280433337,
12.));
#141626=CARTESIAN_POINT('Ctrl Pts',(-68.2606847334987,-29.0944846386568,
12.));
#141627=CARTESIAN_POINT('Ctrl Pts',(-68.2622612910177,-29.0944526440266,
12.));
#141628=CARTESIAN_POINT('',(-63.7976679095314,-28.8072485549236,0.));
#141629=CARTESIAN_POINT('',(-63.7976679095314,-28.8072485549236,0.));
#141630=CARTESIAN_POINT('Ctrl Pts',(-68.2622612910177,-29.0944526440266,
0.));
#141631=CARTESIAN_POINT('Ctrl Pts',(-68.2606847334987,-29.0944846386568,
0.));
#141632=CARTESIAN_POINT('Ctrl Pts',(-68.2535957747187,-29.0946280433337,
0.));
#141633=CARTESIAN_POINT('Ctrl Pts',(-68.2409993690197,-29.094879194787,
0.));
#141634=CARTESIAN_POINT('Ctrl Pts',(-68.2229056854683,-29.095230591515,
0.));
#141635=CARTESIAN_POINT('Ctrl Pts',(-68.1993301412061,-29.0956709104627,
0.));
#141636=CARTESIAN_POINT('Ctrl Pts',(-68.1718618254281,-29.0961590399046,
0.));
#141637=CARTESIAN_POINT('Ctrl Pts',(-68.1444284400742,-29.0966216624743,
0.));
#141638=CARTESIAN_POINT('Ctrl Pts',(-68.1170300646987,-29.0970588175728,
0.));
#141639=CARTESIAN_POINT('Ctrl Pts',(-68.0896667829567,-29.0974705474259,
0.));
#141640=CARTESIAN_POINT('Ctrl Pts',(-68.0623386822863,-29.0978568968657,
0.));
#141641=CARTESIAN_POINT('Ctrl Pts',(-68.0350458525551,-29.0982179124097,
0.));
#141642=CARTESIAN_POINT('Ctrl Pts',(-68.0077883850121,-29.0985536415531,
0.));
#141643=CARTESIAN_POINT('Ctrl Pts',(-67.9805663711855,-29.0988641320247,
0.));
#141644=CARTESIAN_POINT('Ctrl Pts',(-67.9533799016148,-29.0991494309404,
0.));
#141645=CARTESIAN_POINT('Ctrl Pts',(-67.9262290652829,-29.099409584422,
0.));
#141646=CARTESIAN_POINT('Ctrl Pts',(-67.8991139503193,-29.0996446380626,
0.));
#141647=CARTESIAN_POINT('Ctrl Pts',(-67.8720346444124,-29.0998546372032,
0.));
#141648=CARTESIAN_POINT('Ctrl Pts',(-67.8449912353329,-29.1000396272867,
0.));
#141649=CARTESIAN_POINT('Ctrl Pts',(-67.8179838114099,-29.1001996541842,
0.));
#141650=CARTESIAN_POINT('Ctrl Pts',(-67.7910124620135,-29.1003347645294,
0.));
#141651=CARTESIAN_POINT('Ctrl Pts',(-67.7640772773388,-29.1004450055643,
0.));
#141652=CARTESIAN_POINT('Ctrl Pts',(-67.7371783482035,-29.1005304249987,
0.));
#141653=CARTESIAN_POINT('Ctrl Pts',(-67.7103157658296,-29.1005910708624,
0.));
#141654=CARTESIAN_POINT('Ctrl Pts',(-67.6834896216461,-29.1006269913747,
0.));
#141655=CARTESIAN_POINT('Ctrl Pts',(-67.6567000070326,-29.1006382347814,
0.));
#141656=CARTESIAN_POINT('Ctrl Pts',(-67.6299470133295,-29.100624849358,
0.));
#141657=CARTESIAN_POINT('Ctrl Pts',(-67.6032307319623,-29.1005868834866,
0.));
#141658=CARTESIAN_POINT('Ctrl Pts',(-67.5765512545281,-29.1005243857139,
0.));
#141659=CARTESIAN_POINT('Ctrl Pts',(-67.5499086728888,-29.1004374048148,
0.));
#141660=CARTESIAN_POINT('Ctrl Pts',(-67.5233030792704,-29.1003259898682,
0.));
#141661=CARTESIAN_POINT('Ctrl Pts',(-67.4967345663096,-29.1001901902909,
0.));
#141662=CARTESIAN_POINT('Ctrl Pts',(-67.4702032270048,-29.1000300557955,
0.));
#141663=CARTESIAN_POINT('Ctrl Pts',(-67.4437091546859,-29.0998456363683,
0.));
#141664=CARTESIAN_POINT('Ctrl Pts',(-67.4172524429727,-29.0996369822418,
0.));
#141665=CARTESIAN_POINT('Ctrl Pts',(-67.3908331857323,-29.0994041438719,
0.));
#141666=CARTESIAN_POINT('Ctrl Pts',(-67.3644514770387,-29.0991471719176,
0.));
#141667=CARTESIAN_POINT('Ctrl Pts',(-67.3381074112027,-29.0988661172531,
0.));
#141668=CARTESIAN_POINT('Ctrl Pts',(-67.311801082792,-29.0985610309771,
0.));
#141669=CARTESIAN_POINT('Ctrl Pts',(-67.2855325866517,-29.0982319644277,
0.));
#141670=CARTESIAN_POINT('Ctrl Pts',(-67.2593020179209,-29.0978789691962,
0.));
#141671=CARTESIAN_POINT('Ctrl Pts',(-67.2331094720471,-29.097502097147,
0.));
#141672=CARTESIAN_POINT('Ctrl Pts',(-67.2069550447883,-29.0971014004131,
0.));
#141673=CARTESIAN_POINT('Ctrl Pts',(-67.1808388322109,-29.096676931389,
0.));
#141674=CARTESIAN_POINT('Ctrl Pts',(-67.1547609306843,-29.0962287427273,
0.));
#141675=CARTESIAN_POINT('Ctrl Pts',(-67.1287214368746,-29.0957568873358,
0.));
#141676=CARTESIAN_POINT('Ctrl Pts',(-67.1027204477311,-29.0952614183779,
0.));
#141677=CARTESIAN_POINT('Ctrl Pts',(-67.0767580604879,-29.0947423892727,
0.));
#141678=CARTESIAN_POINT('Ctrl Pts',(-67.0508343726776,-29.0941998536959,
0.));
#141679=CARTESIAN_POINT('Ctrl Pts',(-67.0249494821363,-29.0936338655828,
0.));
#141680=CARTESIAN_POINT('Ctrl Pts',(-66.9991034870083,-29.0930444791328,
0.));
#141681=CARTESIAN_POINT('Ctrl Pts',(-66.9732964857466,-29.092431748817,
0.));
#141682=CARTESIAN_POINT('Ctrl Pts',(-66.9475285771135,-29.0917957293826,
0.));
#141683=CARTESIAN_POINT('Ctrl Pts',(-66.9217998601885,-29.0911364758487,
0.));
#141684=CARTESIAN_POINT('Ctrl Pts',(-66.8961104343707,-29.0904540435065,
0.));
#141685=CARTESIAN_POINT('Ctrl Pts',(-66.8704603993794,-29.0897484879207,
0.));
#141686=CARTESIAN_POINT('Ctrl Pts',(-66.8448498552503,-29.0890198649323,
0.));
#141687=CARTESIAN_POINT('Ctrl Pts',(-66.8192789023312,-29.088268230663,
0.));
#141688=CARTESIAN_POINT('Ctrl Pts',(-66.793747641293,-29.0874936415132,
0.));
#141689=CARTESIAN_POINT('Ctrl Pts',(-66.7682561731341,-29.0866961541626,
0.));
#141690=CARTESIAN_POINT('Ctrl Pts',(-66.7428045991841,-29.0858758255729,
0.));
#141691=CARTESIAN_POINT('Ctrl Pts',(-66.7173930211022,-29.0850327129916,
0.));
#141692=CARTESIAN_POINT('Ctrl Pts',(-66.6920215408751,-29.0841668739588,
0.));
#141693=CARTESIAN_POINT('Ctrl Pts',(-66.6666902608249,-29.0832783663049,
0.));
#141694=CARTESIAN_POINT('Ctrl Pts',(-66.6413992836147,-29.0823672481507,
0.));
#141695=CARTESIAN_POINT('Ctrl Pts',(-66.6161487122502,-29.0814335779084,
0.));
#141696=CARTESIAN_POINT('Ctrl Pts',(-66.59093865008,-29.0804774142854,0.));
#141697=CARTESIAN_POINT('Ctrl Pts',(-66.5657692007906,-29.0794988162897,
0.));
#141698=CARTESIAN_POINT('Ctrl Pts',(-66.5406404684132,-29.0784978432301,
0.));
#141699=CARTESIAN_POINT('Ctrl Pts',(-66.5155525573323,-29.0774745547151,
0.));
#141700=CARTESIAN_POINT('Ctrl Pts',(-66.4905055722868,-29.0764290106554,
0.));
#141701=CARTESIAN_POINT('Ctrl Pts',(-66.4654996183731,-29.0753612712666,
0.));
#141702=CARTESIAN_POINT('Ctrl Pts',(-66.4405348010388,-29.0742713970755,
0.));
#141703=CARTESIAN_POINT('Ctrl Pts',(-66.4156112260887,-29.0731594489211,
0.));
#141704=CARTESIAN_POINT('Ctrl Pts',(-66.3907289996932,-29.072025487953,
0.));
#141705=CARTESIAN_POINT('Ctrl Pts',(-66.3658882283903,-29.0708695756334,
0.));
#141706=CARTESIAN_POINT('Ctrl Pts',(-66.3410890190884,-29.0696917737399,
0.));
#141707=CARTESIAN_POINT('Ctrl Pts',(-66.3163314790615,-29.0684921443721,
0.));
#141708=CARTESIAN_POINT('Ctrl Pts',(-66.2916157159536,-29.067270749953,
0.));
#141709=CARTESIAN_POINT('Ctrl Pts',(-66.2669418377871,-29.0660276532274,
0.));
#141710=CARTESIAN_POINT('Ctrl Pts',(-66.2423099529669,-29.0647629172645,
0.));
#141711=CARTESIAN_POINT('Ctrl Pts',(-66.2177201702818,-29.0634766054598,
0.));
#141712=CARTESIAN_POINT('Ctrl Pts',(-66.1931725989008,-29.062168781542,
0.));
#141713=CARTESIAN_POINT('Ctrl Pts',(-66.1686673483757,-29.0608395095747,
0.));
#141714=CARTESIAN_POINT('Ctrl Pts',(-66.144204528652,-29.0594888539558,
0.));
#141715=CARTESIAN_POINT('Ctrl Pts',(-66.1197842500714,-29.0581168794191,
0.));
#141716=CARTESIAN_POINT('Ctrl Pts',(-66.0954066233752,-29.0567236510372,
0.));
#141717=CARTESIAN_POINT('Ctrl Pts',(-66.0710717597003,-29.0553092342275,
0.));
#141718=CARTESIAN_POINT('Ctrl Pts',(-66.0467797705806,-29.0538736947547,
0.));
#141719=CARTESIAN_POINT('Ctrl Pts',(-66.0225307679584,-29.0524170987303,
0.));
#141720=CARTESIAN_POINT('Ctrl Pts',(-65.9983248641877,-29.0509395126141,
0.));
#141721=CARTESIAN_POINT('Ctrl Pts',(-65.9741621720372,-29.0494410032173,
0.));
#141722=CARTESIAN_POINT('Ctrl Pts',(-65.9500428046873,-29.0479216377082,
0.));
#141723=CARTESIAN_POINT('Ctrl Pts',(-65.9259668757309,-29.0463814836158,
0.));
#141724=CARTESIAN_POINT('Ctrl Pts',(-65.9019344991854,-29.0448206088288,
0.));
#141725=CARTESIAN_POINT('Ctrl Pts',(-65.8779457894959,-29.0432390815977,
0.));
#141726=CARTESIAN_POINT('Ctrl Pts',(-65.854000861539,-29.0416369705375,
0.));
#141727=CARTESIAN_POINT('Ctrl Pts',(-65.8300998306198,-29.0400143446341,
0.));
#141728=CARTESIAN_POINT('Ctrl Pts',(-65.8062428124723,-29.0383712732473,
0.));
#141729=CARTESIAN_POINT('Ctrl Pts',(-65.7824299232715,-29.0367078261107,
0.));
#141730=CARTESIAN_POINT('Ctrl Pts',(-65.7586612796375,-29.0350240733333,
0.));
#141731=CARTESIAN_POINT('Ctrl Pts',(-65.7349369986382,-29.0333200854026,
0.));
#141732=CARTESIAN_POINT('Ctrl Pts',(-65.7112571977874,-29.0315959331911,
0.));
#141733=CARTESIAN_POINT('Ctrl Pts',(-65.6876219950465,-29.0298516879599,
0.));
#141734=CARTESIAN_POINT('Ctrl Pts',(-65.664031508836,-29.0280874213584,
0.));
#141735=CARTESIAN_POINT('Ctrl Pts',(-65.6404858580391,-29.0263032054261,
0.));
#141736=CARTESIAN_POINT('Ctrl Pts',(-65.6169851620054,-29.0244991125962,
0.));
#141737=CARTESIAN_POINT('Ctrl Pts',(-65.593529540548,-29.0226752157013,
0.));
#141738=CARTESIAN_POINT('Ctrl Pts',(-65.5701191139455,-29.0208315879778,
0.));
#141739=CARTESIAN_POINT('Ctrl Pts',(-65.5467540029546,-29.0189683030654,
0.));
#141740=CARTESIAN_POINT('Ctrl Pts',(-65.523434328815,-29.01708543501,0.));
#141741=CARTESIAN_POINT('Ctrl Pts',(-65.5001602132524,-29.015183058267,
0.));
#141742=CARTESIAN_POINT('Ctrl Pts',(-65.4769317784754,-29.0132612477075,
0.));
#141743=CARTESIAN_POINT('Ctrl Pts',(-65.4537491471782,-29.0113200786219,
0.));
#141744=CARTESIAN_POINT('Ctrl Pts',(-65.4306124425524,-29.0093596267198,
0.));
#141745=CARTESIAN_POINT('Ctrl Pts',(-65.4075217882921,-29.0073799681336,
0.));
#141746=CARTESIAN_POINT('Ctrl Pts',(-65.3844773085976,-29.0053811794214,
0.));
#141747=CARTESIAN_POINT('Ctrl Pts',(-65.3614791281726,-29.0033633375745,
0.));
#141748=CARTESIAN_POINT('Ctrl Pts',(-65.3385273722278,-29.0013265200201,
0.));
#141749=CARTESIAN_POINT('Ctrl Pts',(-65.3156221664942,-28.9992708046223,
0.));
#141750=CARTESIAN_POINT('Ctrl Pts',(-65.2927636372261,-28.9971962696848,
0.));
#141751=CARTESIAN_POINT('Ctrl Pts',(-65.2699519112052,-28.9951029939551,
0.));
#141752=CARTESIAN_POINT('Ctrl Pts',(-65.2471871157375,-28.9929910566314,
0.));
#141753=CARTESIAN_POINT('Ctrl Pts',(-65.2244693786586,-28.9908605373652,
0.));
#141754=CARTESIAN_POINT('Ctrl Pts',(-65.2017988283465,-28.9887115162626,
0.));
#141755=CARTESIAN_POINT('Ctrl Pts',(-65.1791755937254,-28.9865440738882,
0.));
#141756=CARTESIAN_POINT('Ctrl Pts',(-65.1565998042705,-28.9843582912697,
0.));
#141757=CARTESIAN_POINT('Ctrl Pts',(-65.1340715900042,-28.9821542499049,
0.));
#141758=CARTESIAN_POINT('Ctrl Pts',(-65.111591081505,-28.9799320317648,
0.));
#141759=CARTESIAN_POINT('Ctrl Pts',(-65.0891584099174,-28.9776917192936,
0.));
#141760=CARTESIAN_POINT('Ctrl Pts',(-65.0667737069562,-28.9754333954134,
0.));
#141761=CARTESIAN_POINT('Ctrl Pts',(-65.0444371049082,-28.9731571435281,
0.));
#141762=CARTESIAN_POINT('Ctrl Pts',(-65.0221487366279,-28.9708630475298,
0.));
#141763=CARTESIAN_POINT('Ctrl Pts',(-64.9999087355504,-28.9685511918017,
0.));
#141764=CARTESIAN_POINT('Ctrl Pts',(-64.9777172357028,-28.9662216612216,
0.));
#141765=CARTESIAN_POINT('Ctrl Pts',(-64.955574371711,-28.9638745411677,
0.));
#141766=CARTESIAN_POINT('Ctrl Pts',(-64.9334802788037,-28.961509917525,
0.));
#141767=CARTESIAN_POINT('Ctrl Pts',(-64.9114350928124,-28.9591278766934,
0.));
#141768=CARTESIAN_POINT('Ctrl Pts',(-64.8894389501799,-28.9567285055866,
0.));
#141769=CARTESIAN_POINT('Ctrl Pts',(-64.8674919879646,-28.9543118916327,
0.));
#141770=CARTESIAN_POINT('Ctrl Pts',(-64.8455943438423,-28.9518781227765,
0.));
#141771=CARTESIAN_POINT('Ctrl Pts',(-64.8237461561024,-28.9494272874833,
0.));
#141772=CARTESIAN_POINT('Ctrl Pts',(-64.8019475636454,-28.9469594747436,
0.));
#141773=CARTESIAN_POINT('Ctrl Pts',(-64.7801987060097,-28.9444747740815,
0.));
#141774=CARTESIAN_POINT('Ctrl Pts',(-64.7584997233889,-28.9419732755659,
0.));
#141775=CARTESIAN_POINT('Ctrl Pts',(-64.7368507566461,-28.9394550698201,
0.));
#141776=CARTESIAN_POINT('Ctrl Pts',(-64.715251947327,-28.9369202480383,
0.));
#141777=CARTESIAN_POINT('Ctrl Pts',(-64.6937034376591,-28.934368901987,
0.));
#141778=CARTESIAN_POINT('Ctrl Pts',(-64.6722053705389,-28.9318011239905,
0.));
#141779=CARTESIAN_POINT('Ctrl Pts',(-64.6507578895155,-28.9292170069219,
0.));
#141780=CARTESIAN_POINT('Ctrl Pts',(-64.6293611387753,-28.9266166441956,
0.));
#141781=CARTESIAN_POINT('Ctrl Pts',(-64.6080152631065,-28.9240001297553,
0.));
#141782=CARTESIAN_POINT('Ctrl Pts',(-64.5867204079452,-28.9213675580996,
0.));
#141783=CARTESIAN_POINT('Ctrl Pts',(-64.5654767194487,-28.9187190243231,
0.));
#141784=CARTESIAN_POINT('Ctrl Pts',(-64.544284344556,-28.9160546241538,
0.));
#141785=CARTESIAN_POINT('Ctrl Pts',(-64.5231434310457,-28.9133744539943,
0.));
#141786=CARTESIAN_POINT('Ctrl Pts',(-64.5020541275927,-28.9106786109639,
0.));
#141787=CARTESIAN_POINT('Ctrl Pts',(-64.4810165836568,-28.9079671928253,
0.));
#141788=CARTESIAN_POINT('Ctrl Pts',(-64.460030949357,-28.9052402979055,
0.));
#141789=CARTESIAN_POINT('Ctrl Pts',(-64.439097375364,-28.9024980250309,
0.));
#141790=CARTESIAN_POINT('Ctrl Pts',(-64.4182160127401,-28.899740473435,
0.));
#141791=CARTESIAN_POINT('Ctrl Pts',(-64.3973870129201,-28.8969677427519,
0.));
#141792=CARTESIAN_POINT('Ctrl Pts',(-64.3766105280715,-28.8941799332312,
0.));
#141793=CARTESIAN_POINT('Ctrl Pts',(-64.3558867114087,-28.8913771459327,
0.));
#141794=CARTESIAN_POINT('Ctrl Pts',(-64.3352157174606,-28.888559482892,
0.));
#141795=CARTESIAN_POINT('Ctrl Pts',(-64.3145977025005,-28.8857270473944,
0.));
#141796=CARTESIAN_POINT('Ctrl Pts',(-64.2940328242482,-28.8828799437922,
0.));
#141797=CARTESIAN_POINT('Ctrl Pts',(-64.2735212410682,-28.8800182770052,
0.));
#141798=CARTESIAN_POINT('Ctrl Pts',(-64.2530631112926,-28.8771421521058,
0.));
#141799=CARTESIAN_POINT('Ctrl Pts',(-64.232658592528,-28.8742516738959,
0.));
#141800=CARTESIAN_POINT('Ctrl Pts',(-64.2123078408507,-28.8713469464205,
0.));
#141801=CARTESIAN_POINT('Ctrl Pts',(-64.1920110123342,-28.8684280739033,
0.));
#141802=CARTESIAN_POINT('Ctrl Pts',(-64.1717682648708,-28.8654951618659,
0.));
#141803=CARTESIAN_POINT('Ctrl Pts',(-64.1515797596555,-28.8625483180433,
0.));
#141804=CARTESIAN_POINT('Ctrl Pts',(-64.1314456633345,-28.8595876537132,
0.));
#141805=CARTESIAN_POINT('Ctrl Pts',(-64.1113661481918,-28.8566132838157,
0.));
#141806=CARTESIAN_POINT('Ctrl Pts',(-64.0913413876586,-28.8536253241837,
0.));
#141807=CARTESIAN_POINT('Ctrl Pts',(-64.0713715523588,-28.8506238891087,
0.));
#141808=CARTESIAN_POINT('Ctrl Pts',(-64.0514568066659,-28.8476090892242,
0.));
#141809=CARTESIAN_POINT('Ctrl Pts',(-64.0315973031994,-28.8445810281275,
0.));
#141810=CARTESIAN_POINT('Ctrl Pts',(-64.0117931881364,-28.841539805646,
0.));
#141811=CARTESIAN_POINT('Ctrl Pts',(-63.9920446117632,-28.8384855243267,
0.));
#141812=CARTESIAN_POINT('Ctrl Pts',(-63.9723517369614,-28.8354182946601,
0.));
#141813=CARTESIAN_POINT('Ctrl Pts',(-63.9527147494351,-28.8323382413752,
0.));
#141814=CARTESIAN_POINT('Ctrl Pts',(-63.9331338646868,-28.8292455077494,
0.));
#141815=CARTESIAN_POINT('Ctrl Pts',(-63.9136093063647,-28.826140242322,
0.));
#141816=CARTESIAN_POINT('Ctrl Pts',(-63.894141285685,-28.8230225863142,
0.));
#141817=CARTESIAN_POINT('Ctrl Pts',(-63.8747299825383,-28.8198926619893,
0.));
#141818=CARTESIAN_POINT('Ctrl Pts',(-63.8553755207732,-28.8167505576806,
0.));
#141819=CARTESIAN_POINT('Ctrl Pts',(-63.8360779670226,-28.8135963263557,
0.));
#141820=CARTESIAN_POINT('Ctrl Pts',(-63.8206854735372,-28.8110632621133,
0.));
#141821=CARTESIAN_POINT('Ctrl Pts',(-63.809166727145,-28.8091580239664,
0.));
#141822=CARTESIAN_POINT('Ctrl Pts',(-63.8014989507575,-28.8078854475473,
0.));
#141823=CARTESIAN_POINT('Ctrl Pts',(-63.7976679095314,-28.8072485549236,
0.));
#141824=CARTESIAN_POINT('Ctrl Pts',(-70.8615414811571,-22.9976507259816,
0.));
#141825=CARTESIAN_POINT('Ctrl Pts',(-70.8615414811571,-22.9976507259816,
12.));
#141826=CARTESIAN_POINT('Ctrl Pts',(-70.8559846928,-22.9983100639391,0.));
#141827=CARTESIAN_POINT('Ctrl Pts',(-70.8559846928,-22.9983100639391,12.));
#141828=CARTESIAN_POINT('Ctrl Pts',(-70.8448742696689,-22.9996258555291,
0.));
#141829=CARTESIAN_POINT('Ctrl Pts',(-70.8448742696689,-22.9996258555291,
12.));
#141830=CARTESIAN_POINT('Ctrl Pts',(-70.8282180957225,-23.0015908899394,
0.));
#141831=CARTESIAN_POINT('Ctrl Pts',(-70.8282180957225,-23.0015908899394,
12.));
#141832=CARTESIAN_POINT('Ctrl Pts',(-70.8060287860585,-23.0041936291626,
0.));
#141833=CARTESIAN_POINT('Ctrl Pts',(-70.8060287860585,-23.0041936291626,
12.));
#141834=CARTESIAN_POINT('Ctrl Pts',(-70.7783236951202,-23.0074182063787,
0.));
#141835=CARTESIAN_POINT('Ctrl Pts',(-70.7783236951202,-23.0074182063787,
12.));
#141836=CARTESIAN_POINT('Ctrl Pts',(-70.750650169619,-23.0106139366046,
0.));
#141837=CARTESIAN_POINT('Ctrl Pts',(-70.750650169619,-23.0106139366046,
12.));
#141838=CARTESIAN_POINT('Ctrl Pts',(-70.7230082425412,-23.0137808248924,
0.));
#141839=CARTESIAN_POINT('Ctrl Pts',(-70.7230082425412,-23.0137808248924,
12.));
#141840=CARTESIAN_POINT('Ctrl Pts',(-70.6953979633426,-23.0169188841045,
0.));
#141841=CARTESIAN_POINT('Ctrl Pts',(-70.6953979633426,-23.0169188841045,
12.));
#141842=CARTESIAN_POINT('Ctrl Pts',(-70.6678194023135,-23.0200281385833,
0.));
#141843=CARTESIAN_POINT('Ctrl Pts',(-70.6678194023135,-23.0200281385833,
12.));
#141844=CARTESIAN_POINT('Ctrl Pts',(-70.6402726486453,-23.0231086235186,
0.));
#141845=CARTESIAN_POINT('Ctrl Pts',(-70.6402726486453,-23.0231086235186,
12.));
#141846=CARTESIAN_POINT('Ctrl Pts',(-70.6127578036673,-23.026160381013,
0.));
#141847=CARTESIAN_POINT('Ctrl Pts',(-70.6127578036673,-23.026160381013,
12.));
#141848=CARTESIAN_POINT('Ctrl Pts',(-70.5852749754082,-23.0291834570663,
0.));
#141849=CARTESIAN_POINT('Ctrl Pts',(-70.5852749754082,-23.0291834570663,
12.));
#141850=CARTESIAN_POINT('Ctrl Pts',(-70.5578242727627,-23.0321778982711,
0.));
#141851=CARTESIAN_POINT('Ctrl Pts',(-70.5578242727627,-23.0321778982711,
12.));
#141852=CARTESIAN_POINT('Ctrl Pts',(-70.5304057994631,-23.0351437484336,
0.));
#141853=CARTESIAN_POINT('Ctrl Pts',(-70.5304057994631,-23.0351437484336,
12.));
#141854=CARTESIAN_POINT('Ctrl Pts',(-70.5030196492003,-23.0380810458271,
0.));
#141855=CARTESIAN_POINT('Ctrl Pts',(-70.5030196492003,-23.0380810458271,
12.));
#141856=CARTESIAN_POINT('Ctrl Pts',(-70.4756659090209,-23.0409898250756,
0.));
#141857=CARTESIAN_POINT('Ctrl Pts',(-70.4756659090209,-23.0409898250756,
12.));
#141858=CARTESIAN_POINT('Ctrl Pts',(-70.4483446617614,-23.0438701185013,
0.));
#141859=CARTESIAN_POINT('Ctrl Pts',(-70.4483446617614,-23.0438701185013,
12.));
#141860=CARTESIAN_POINT('Ctrl Pts',(-70.4210559889348,-23.0467219577291,
0.));
#141861=CARTESIAN_POINT('Ctrl Pts',(-70.4210559889348,-23.0467219577291,
12.));
#141862=CARTESIAN_POINT('Ctrl Pts',(-70.3937999732267,-23.0495453750763,
0.));
#141863=CARTESIAN_POINT('Ctrl Pts',(-70.3937999732267,-23.0495453750763,
12.));
#141864=CARTESIAN_POINT('Ctrl Pts',(-70.3665767016542,-23.0523404053172,
0.));
#141865=CARTESIAN_POINT('Ctrl Pts',(-70.3665767016542,-23.0523404053172,
12.));
#141866=CARTESIAN_POINT('Ctrl Pts',(-70.3393862652297,-23.0551070854926,
0.));
#141867=CARTESIAN_POINT('Ctrl Pts',(-70.3393862652297,-23.0551070854926,
12.));
#141868=CARTESIAN_POINT('Ctrl Pts',(-70.3122287575335,-23.0578454541104,
0.));
#141869=CARTESIAN_POINT('Ctrl Pts',(-70.3122287575335,-23.0578454541104,
12.));
#141870=CARTESIAN_POINT('Ctrl Pts',(-70.2851042736066,-23.0605555505321,
0.));
#141871=CARTESIAN_POINT('Ctrl Pts',(-70.2851042736066,-23.0605555505321,
12.));
#141872=CARTESIAN_POINT('Ctrl Pts',(-70.2580129087888,-23.0632374143279,
0.));
#141873=CARTESIAN_POINT('Ctrl Pts',(-70.2580129087888,-23.0632374143279,
12.));
#141874=CARTESIAN_POINT('Ctrl Pts',(-70.2309547573815,-23.0658910845433,
0.));
#141875=CARTESIAN_POINT('Ctrl Pts',(-70.2309547573815,-23.0658910845433,
12.));
#141876=CARTESIAN_POINT('Ctrl Pts',(-70.2039299120488,-23.0685165993691,
0.));
#141877=CARTESIAN_POINT('Ctrl Pts',(-70.2039299120488,-23.0685165993691,
12.));
#141878=CARTESIAN_POINT('Ctrl Pts',(-70.1769384645586,-23.071113996544,
0.));
#141879=CARTESIAN_POINT('Ctrl Pts',(-70.1769384645586,-23.071113996544,
12.));
#141880=CARTESIAN_POINT('Ctrl Pts',(-70.1499805062172,-23.0736833135938,
0.));
#141881=CARTESIAN_POINT('Ctrl Pts',(-70.1499805062172,-23.0736833135938,
12.));
#141882=CARTESIAN_POINT('Ctrl Pts',(-70.123056128422,-23.0762245881389,
0.));
#141883=CARTESIAN_POINT('Ctrl Pts',(-70.123056128422,-23.0762245881389,
12.));
#141884=CARTESIAN_POINT('Ctrl Pts',(-70.0961654231639,-23.0787378581774,
0.));
#141885=CARTESIAN_POINT('Ctrl Pts',(-70.0961654231639,-23.0787378581774,
12.));
#141886=CARTESIAN_POINT('Ctrl Pts',(-70.0693084835373,-23.0812231623765,
0.));
#141887=CARTESIAN_POINT('Ctrl Pts',(-70.0693084835373,-23.0812231623765,
12.));
#141888=CARTESIAN_POINT('Ctrl Pts',(-70.0424854035115,-23.0836805399374,
0.));
#141889=CARTESIAN_POINT('Ctrl Pts',(-70.0424854035115,-23.0836805399374,
12.));
#141890=CARTESIAN_POINT('Ctrl Pts',(-70.0156962777169,-23.0861100304729,
0.));
#141891=CARTESIAN_POINT('Ctrl Pts',(-70.0156962777169,-23.0861100304729,
12.));
#141892=CARTESIAN_POINT('Ctrl Pts',(-69.9889412012143,-23.0885116738798,
0.));
#141893=CARTESIAN_POINT('Ctrl Pts',(-69.9889412012143,-23.0885116738798,
12.));
#141894=CARTESIAN_POINT('Ctrl Pts',(-69.9622202692873,-23.0908855102251,
0.));
#141895=CARTESIAN_POINT('Ctrl Pts',(-69.9622202692873,-23.0908855102251,
12.));
#141896=CARTESIAN_POINT('Ctrl Pts',(-69.9355335771729,-23.0932315796068,
0.));
#141897=CARTESIAN_POINT('Ctrl Pts',(-69.9355335771729,-23.0932315796068,
12.));
#141898=CARTESIAN_POINT('Ctrl Pts',(-69.9088812200713,-23.0955499221558,
0.));
#141899=CARTESIAN_POINT('Ctrl Pts',(-69.9088812200713,-23.0955499221558,
12.));
#141900=CARTESIAN_POINT('Ctrl Pts',(-69.8822632932768,-23.0978405781021,
0.));
#141901=CARTESIAN_POINT('Ctrl Pts',(-69.8822632932768,-23.0978405781021,
12.));
#141902=CARTESIAN_POINT('Ctrl Pts',(-69.8556798922693,-23.1001035878241,
0.));
#141903=CARTESIAN_POINT('Ctrl Pts',(-69.8556798922693,-23.1001035878241,
12.));
#141904=CARTESIAN_POINT('Ctrl Pts',(-69.8291311128118,-23.1023389919051,
0.));
#141905=CARTESIAN_POINT('Ctrl Pts',(-69.8291311128118,-23.1023389919051,
12.));
#141906=CARTESIAN_POINT('Ctrl Pts',(-69.8026170510572,-23.1045468311991,
0.));
#141907=CARTESIAN_POINT('Ctrl Pts',(-69.8026170510572,-23.1045468311991,
12.));
#141908=CARTESIAN_POINT('Ctrl Pts',(-69.7761378035964,-23.106727146861,
0.));
#141909=CARTESIAN_POINT('Ctrl Pts',(-69.7761378035964,-23.106727146861,
12.));
#141910=CARTESIAN_POINT('Ctrl Pts',(-69.7496934674069,-23.1088799803089,
0.));
#141911=CARTESIAN_POINT('Ctrl Pts',(-69.7496934674069,-23.1088799803089,
12.));
#141912=CARTESIAN_POINT('Ctrl Pts',(-69.7232841398197,-23.1110053732046,
0.));
#141913=CARTESIAN_POINT('Ctrl Pts',(-69.7232841398197,-23.1110053732046,
12.));
#141914=CARTESIAN_POINT('Ctrl Pts',(-69.6969099184767,-23.1131033674301,
0.));
#141915=CARTESIAN_POINT('Ctrl Pts',(-69.6969099184767,-23.1131033674301,
12.));
#141916=CARTESIAN_POINT('Ctrl Pts',(-69.6705709012852,-23.1151740050681,
0.));
#141917=CARTESIAN_POINT('Ctrl Pts',(-69.6705709012852,-23.1151740050681,
12.));
#141918=CARTESIAN_POINT('Ctrl Pts',(-69.6442671863765,-23.1172173283859,
0.));
#141919=CARTESIAN_POINT('Ctrl Pts',(-69.6442671863765,-23.1172173283859,
12.));
#141920=CARTESIAN_POINT('Ctrl Pts',(-69.6179988721365,-23.1192333798441,
0.));
#141921=CARTESIAN_POINT('Ctrl Pts',(-69.6179988721365,-23.1192333798441,
12.));
#141922=CARTESIAN_POINT('Ctrl Pts',(-69.5917660572265,-23.1212222021051,
0.));
#141923=CARTESIAN_POINT('Ctrl Pts',(-69.5917660572265,-23.1212222021051,
12.));
#141924=CARTESIAN_POINT('Ctrl Pts',(-69.5655688406052,-23.1231838380452,
0.));
#141925=CARTESIAN_POINT('Ctrl Pts',(-69.5655688406052,-23.1231838380452,
12.));
#141926=CARTESIAN_POINT('Ctrl Pts',(-69.539407321546,-23.1251183307676,
0.));
#141927=CARTESIAN_POINT('Ctrl Pts',(-69.539407321546,-23.1251183307676,
12.));
#141928=CARTESIAN_POINT('Ctrl Pts',(-69.5132815996537,-23.1270257236204,
0.));
#141929=CARTESIAN_POINT('Ctrl Pts',(-69.5132815996537,-23.1270257236204,
12.));
#141930=CARTESIAN_POINT('Ctrl Pts',(-69.4871917748654,-23.1289060601924,
0.));
#141931=CARTESIAN_POINT('Ctrl Pts',(-69.4871917748654,-23.1289060601924,
12.));
#141932=CARTESIAN_POINT('Ctrl Pts',(-69.4611379474484,-23.1307593843061,
0.));
#141933=CARTESIAN_POINT('Ctrl Pts',(-69.4611379474484,-23.1307593843061,
12.));
#141934=CARTESIAN_POINT('Ctrl Pts',(-69.4351202179946,-23.1325857400144,
0.));
#141935=CARTESIAN_POINT('Ctrl Pts',(-69.4351202179946,-23.1325857400144,
12.));
#141936=CARTESIAN_POINT('Ctrl Pts',(-69.4091386874132,-23.1343851715989,
0.));
#141937=CARTESIAN_POINT('Ctrl Pts',(-69.4091386874132,-23.1343851715989,
12.));
#141938=CARTESIAN_POINT('Ctrl Pts',(-69.3831934569182,-23.1361577235709,
0.));
#141939=CARTESIAN_POINT('Ctrl Pts',(-69.3831934569182,-23.1361577235709,
12.));
#141940=CARTESIAN_POINT('Ctrl Pts',(-69.3572846280296,-23.1379034406718,
0.));
#141941=CARTESIAN_POINT('Ctrl Pts',(-69.3572846280296,-23.1379034406718,
12.));
#141942=CARTESIAN_POINT('Ctrl Pts',(-69.3314123025869,-23.1396223678725,
0.));
#141943=CARTESIAN_POINT('Ctrl Pts',(-69.3314123025869,-23.1396223678725,
12.));
#141944=CARTESIAN_POINT('Ctrl Pts',(-69.3055765827546,-23.1413145503762,
0.));
#141945=CARTESIAN_POINT('Ctrl Pts',(-69.3055765827546,-23.1413145503762,
12.));
#141946=CARTESIAN_POINT('Ctrl Pts',(-69.2797775710273,-23.142980033622,
0.));
#141947=CARTESIAN_POINT('Ctrl Pts',(-69.2797775710273,-23.142980033622,
12.));
#141948=CARTESIAN_POINT('Ctrl Pts',(-69.254015370231,-23.1446188632931,
0.));
#141949=CARTESIAN_POINT('Ctrl Pts',(-69.254015370231,-23.1446188632931,
12.));
#141950=CARTESIAN_POINT('Ctrl Pts',(-69.2282900835235,-23.1462310853206,
0.));
#141951=CARTESIAN_POINT('Ctrl Pts',(-69.2282900835235,-23.1462310853206,
12.));
#141952=CARTESIAN_POINT('Ctrl Pts',(-69.2026018144028,-23.147816745879,
0.));
#141953=CARTESIAN_POINT('Ctrl Pts',(-69.2026018144028,-23.147816745879,
12.));
#141954=CARTESIAN_POINT('Ctrl Pts',(-69.1769506667084,-23.1493758913859,
0.));
#141955=CARTESIAN_POINT('Ctrl Pts',(-69.1769506667084,-23.1493758913859,
12.));
#141956=CARTESIAN_POINT('Ctrl Pts',(-69.1513367446231,-23.1509085685032,
0.));
#141957=CARTESIAN_POINT('Ctrl Pts',(-69.1513367446231,-23.1509085685032,
12.));
#141958=CARTESIAN_POINT('Ctrl Pts',(-69.1257601526687,-23.152414824141,
0.));
#141959=CARTESIAN_POINT('Ctrl Pts',(-69.1257601526687,-23.152414824141,
12.));
#141960=CARTESIAN_POINT('Ctrl Pts',(-69.1002209957025,-23.1538947054615,
0.));
#141961=CARTESIAN_POINT('Ctrl Pts',(-69.1002209957025,-23.1538947054615,
12.));
#141962=CARTESIAN_POINT('Ctrl Pts',(-69.074719378928,-23.1553482598762,
0.));
#141963=CARTESIAN_POINT('Ctrl Pts',(-69.074719378928,-23.1553482598762,
12.));
#141964=CARTESIAN_POINT('Ctrl Pts',(-69.0492554078992,-23.1567755350469,
0.));
#141965=CARTESIAN_POINT('Ctrl Pts',(-69.0492554078992,-23.1567755350469,
12.));
#141966=CARTESIAN_POINT('Ctrl Pts',(-69.0238291885245,-23.1581765788869,
0.));
#141967=CARTESIAN_POINT('Ctrl Pts',(-69.0238291885245,-23.1581765788869,
12.));
#141968=CARTESIAN_POINT('Ctrl Pts',(-68.9984408270659,-23.1595514395656,
0.));
#141969=CARTESIAN_POINT('Ctrl Pts',(-68.9984408270659,-23.1595514395656,
12.));
#141970=CARTESIAN_POINT('Ctrl Pts',(-68.9730904301369,-23.1609001655156,
0.));
#141971=CARTESIAN_POINT('Ctrl Pts',(-68.9730904301369,-23.1609001655156,
12.));
#141972=CARTESIAN_POINT('Ctrl Pts',(-68.9477781047106,-23.1622228054291,
0.));
#141973=CARTESIAN_POINT('Ctrl Pts',(-68.9477781047106,-23.1622228054291,
12.));
#141974=CARTESIAN_POINT('Ctrl Pts',(-68.9225039581248,-23.1635194082581,
0.));
#141975=CARTESIAN_POINT('Ctrl Pts',(-68.9225039581248,-23.1635194082581,
12.));
#141976=CARTESIAN_POINT('Ctrl Pts',(-68.8972680980842,-23.164790023215,
0.));
#141977=CARTESIAN_POINT('Ctrl Pts',(-68.8972680980842,-23.164790023215,
12.));
#141978=CARTESIAN_POINT('Ctrl Pts',(-68.8720706326609,-23.1660346997764,
0.));
#141979=CARTESIAN_POINT('Ctrl Pts',(-68.8720706326609,-23.1660346997764,
12.));
#141980=CARTESIAN_POINT('Ctrl Pts',(-68.8469116702898,-23.1672534876889,
0.));
#141981=CARTESIAN_POINT('Ctrl Pts',(-68.8469116702898,-23.1672534876889,
12.));
#141982=CARTESIAN_POINT('Ctrl Pts',(-68.8217913197752,-23.1684464369686,
0.));
#141983=CARTESIAN_POINT('Ctrl Pts',(-68.8217913197752,-23.1684464369686,
12.));
#141984=CARTESIAN_POINT('Ctrl Pts',(-68.7967096902996,-23.1696135978997,
0.));
#141985=CARTESIAN_POINT('Ctrl Pts',(-68.7967096902996,-23.1696135978997,
12.));
#141986=CARTESIAN_POINT('Ctrl Pts',(-68.771666891425,-23.170755021036,0.));
#141987=CARTESIAN_POINT('Ctrl Pts',(-68.771666891425,-23.170755021036,12.));
#141988=CARTESIAN_POINT('Ctrl Pts',(-68.746663033096,-23.1718707572043,
0.));
#141989=CARTESIAN_POINT('Ctrl Pts',(-68.746663033096,-23.1718707572043,
12.));
#141990=CARTESIAN_POINT('Ctrl Pts',(-68.7216982256341,-23.172960857511,
0.));
#141991=CARTESIAN_POINT('Ctrl Pts',(-68.7216982256341,-23.172960857511,
12.));
#141992=CARTESIAN_POINT('Ctrl Pts',(-68.696772579744,-23.1740253733417,
0.));
#141993=CARTESIAN_POINT('Ctrl Pts',(-68.696772579744,-23.1740253733417,
12.));
#141994=CARTESIAN_POINT('Ctrl Pts',(-68.6718862065216,-23.1750643563602,
0.));
#141995=CARTESIAN_POINT('Ctrl Pts',(-68.6718862065216,-23.1750643563602,
12.));
#141996=CARTESIAN_POINT('Ctrl Pts',(-68.6470392174564,-23.1760778585092,
0.));
#141997=CARTESIAN_POINT('Ctrl Pts',(-68.6470392174564,-23.1760778585092,
12.));
#141998=CARTESIAN_POINT('Ctrl Pts',(-68.6222317244341,-23.1770659320138,
0.));
#141999=CARTESIAN_POINT('Ctrl Pts',(-68.6222317244341,-23.1770659320138,
12.));
#142000=CARTESIAN_POINT('Ctrl Pts',(-68.597463839733,-23.1780286293875,
0.));
#142001=CARTESIAN_POINT('Ctrl Pts',(-68.597463839733,-23.1780286293875,
12.));
#142002=CARTESIAN_POINT('Ctrl Pts',(-68.5727356760278,-23.1789660034342,
0.));
#142003=CARTESIAN_POINT('Ctrl Pts',(-68.5727356760278,-23.1789660034342,
12.));
#142004=CARTESIAN_POINT('Ctrl Pts',(-68.5480473463985,-23.179878107245,
0.));
#142005=CARTESIAN_POINT('Ctrl Pts',(-68.5480473463985,-23.179878107245,
12.));
#142006=CARTESIAN_POINT('Ctrl Pts',(-68.5233989643345,-23.180764994201,
0.));
#142007=CARTESIAN_POINT('Ctrl Pts',(-68.5233989643345,-23.180764994201,
12.));
#142008=CARTESIAN_POINT('Ctrl Pts',(-68.4987906437356,-23.1816267179751,
0.));
#142009=CARTESIAN_POINT('Ctrl Pts',(-68.4987906437356,-23.1816267179751,
12.));
#142010=CARTESIAN_POINT('Ctrl Pts',(-68.4742224989098,-23.1824633325385,
0.));
#142011=CARTESIAN_POINT('Ctrl Pts',(-68.4742224989098,-23.1824633325385,
12.));
#142012=CARTESIAN_POINT('Ctrl Pts',(-68.4496946445758,-23.183274892163,
0.));
#142013=CARTESIAN_POINT('Ctrl Pts',(-68.4496946445758,-23.183274892163,
12.));
#142014=CARTESIAN_POINT('Ctrl Pts',(-68.4252071958729,-23.1840614514192,
0.));
#142015=CARTESIAN_POINT('Ctrl Pts',(-68.4252071958729,-23.1840614514192,
12.));
#142016=CARTESIAN_POINT('Ctrl Pts',(-68.4007602683652,-23.1848230651777,
0.));
#142017=CARTESIAN_POINT('Ctrl Pts',(-68.4007602683652,-23.1848230651777,
12.));
#142018=CARTESIAN_POINT('Ctrl Pts',(-68.376353978044,-23.1855597886116,
0.));
#142019=CARTESIAN_POINT('Ctrl Pts',(-68.376353978044,-23.1855597886116,
12.));
#142020=CARTESIAN_POINT('Ctrl Pts',(-68.3519884413246,-23.1862716772031,
0.));
#142021=CARTESIAN_POINT('Ctrl Pts',(-68.3519884413246,-23.1862716772031,
12.));
#142022=CARTESIAN_POINT('Ctrl Pts',(-68.3276637750485,-23.1869587867459,
0.));
#142023=CARTESIAN_POINT('Ctrl Pts',(-68.3276637750485,-23.1869587867459,
12.));
#142024=CARTESIAN_POINT('Ctrl Pts',(-68.3033800964939,-23.1876211733436,
0.));
#142025=CARTESIAN_POINT('Ctrl Pts',(-68.3033800964939,-23.1876211733436,
12.));
#142026=CARTESIAN_POINT('Ctrl Pts',(-68.2791375233795,-23.1882588934107,
0.));
#142027=CARTESIAN_POINT('Ctrl Pts',(-68.2791375233795,-23.1882588934107,
12.));
#142028=CARTESIAN_POINT('Ctrl Pts',(-68.2549361738681,-23.1888720036757,
0.));
#142029=CARTESIAN_POINT('Ctrl Pts',(-68.2549361738681,-23.1888720036757,
12.));
#142030=CARTESIAN_POINT('Ctrl Pts',(-68.2307761665633,-23.1894605611871,
0.));
#142031=CARTESIAN_POINT('Ctrl Pts',(-68.2307761665633,-23.1894605611871,
12.));
#142032=CARTESIAN_POINT('Ctrl Pts',(-68.2066576205116,-23.1900246233165,
0.));
#142033=CARTESIAN_POINT('Ctrl Pts',(-68.2066576205116,-23.1900246233165,
12.));
#142034=CARTESIAN_POINT('Ctrl Pts',(-68.1825806552129,-23.1905642477571,
0.));
#142035=CARTESIAN_POINT('Ctrl Pts',(-68.1825806552129,-23.1905642477571,
12.));
#142036=CARTESIAN_POINT('Ctrl Pts',(-68.1585453906257,-23.1910794925251,
0.));
#142037=CARTESIAN_POINT('Ctrl Pts',(-68.1585453906257,-23.1910794925251,
12.));
#142038=CARTESIAN_POINT('Ctrl Pts',(-68.1345519471695,-23.1915704159623,
0.));
#142039=CARTESIAN_POINT('Ctrl Pts',(-68.1345519471695,-23.1915704159623,
12.));
#142040=CARTESIAN_POINT('Ctrl Pts',(-68.110600445723,-23.1920370767426,
0.));
#142041=CARTESIAN_POINT('Ctrl Pts',(-68.110600445723,-23.1920370767426,
12.));
#142042=CARTESIAN_POINT('Ctrl Pts',(-68.0866910076251,-23.1924795338749,
0.));
#142043=CARTESIAN_POINT('Ctrl Pts',(-68.0866910076251,-23.1924795338749,
12.));
#142044=CARTESIAN_POINT('Ctrl Pts',(-68.0628237546863,-23.1928978467021,
0.));
#142045=CARTESIAN_POINT('Ctrl Pts',(-68.0628237546863,-23.1928978467021,
12.));
#142046=CARTESIAN_POINT('Ctrl Pts',(-68.0389988091933,-23.1932920749023,
0.));
#142047=CARTESIAN_POINT('Ctrl Pts',(-68.0389988091933,-23.1932920749023,
12.));
#142048=CARTESIAN_POINT('Ctrl Pts',(-68.0152162939121,-23.1936622784919,
0.));
#142049=CARTESIAN_POINT('Ctrl Pts',(-68.0152162939121,-23.1936622784919,
12.));
#142050=CARTESIAN_POINT('Ctrl Pts',(-67.991476332086,-23.1940085178313,
0.));
#142051=CARTESIAN_POINT('Ctrl Pts',(-67.991476332086,-23.1940085178313,
12.));
#142052=CARTESIAN_POINT('Ctrl Pts',(-67.9677790474385,-23.1943308536297,
0.));
#142053=CARTESIAN_POINT('Ctrl Pts',(-67.9677790474385,-23.1943308536297,
12.));
#142054=CARTESIAN_POINT('Ctrl Pts',(-67.9441245641842,-23.1946293469427,
0.));
#142055=CARTESIAN_POINT('Ctrl Pts',(-67.9441245641842,-23.1946293469427,
12.));
#142056=CARTESIAN_POINT('Ctrl Pts',(-67.9205130070324,-23.1949040591744,
0.));
#142057=CARTESIAN_POINT('Ctrl Pts',(-67.9205130070324,-23.1949040591744,
12.));
#142058=CARTESIAN_POINT('Ctrl Pts',(-67.8969445011916,-23.1951550520802,
0.));
#142059=CARTESIAN_POINT('Ctrl Pts',(-67.8969445011916,-23.1951550520802,
12.));
#142060=CARTESIAN_POINT('Ctrl Pts',(-67.8734191723667,-23.1953823877734,
0.));
#142061=CARTESIAN_POINT('Ctrl Pts',(-67.8734191723667,-23.1953823877734,
12.));
#142062=CARTESIAN_POINT('Ctrl Pts',(-67.8499371467616,-23.1955861287286,
0.));
#142063=CARTESIAN_POINT('Ctrl Pts',(-67.8499371467616,-23.1955861287286,
12.));
#142064=CARTESIAN_POINT('Ctrl Pts',(-67.8264985510917,-23.1957663377807,
0.));
#142065=CARTESIAN_POINT('Ctrl Pts',(-67.8264985510917,-23.1957663377807,
12.));
#142066=CARTESIAN_POINT('Ctrl Pts',(-67.8031035125887,-23.1959230781269,
0.));
#142067=CARTESIAN_POINT('Ctrl Pts',(-67.8031035125887,-23.1959230781269,
12.));
#142068=CARTESIAN_POINT('Ctrl Pts',(-67.7797521590045,-23.1960564133304,
0.));
#142069=CARTESIAN_POINT('Ctrl Pts',(-67.7797521590045,-23.1960564133304,
12.));
#142070=CARTESIAN_POINT('Ctrl Pts',(-67.7564446186079,-23.1961664073262,
0.));
#142071=CARTESIAN_POINT('Ctrl Pts',(-67.7564446186079,-23.1961664073262,
12.));
#142072=CARTESIAN_POINT('Ctrl Pts',(-67.7331810201883,-23.1962531244245,
0.));
#142073=CARTESIAN_POINT('Ctrl Pts',(-67.7331810201883,-23.1962531244245,
12.));
#142074=CARTESIAN_POINT('Ctrl Pts',(-67.7099614930671,-23.1963166293102,
0.));
#142075=CARTESIAN_POINT('Ctrl Pts',(-67.7099614930671,-23.1963166293102,
12.));
#142076=CARTESIAN_POINT('Ctrl Pts',(-67.6867861671031,-23.1963569870451,
0.));
#142077=CARTESIAN_POINT('Ctrl Pts',(-67.6867861671031,-23.1963569870451,
12.));
#142078=CARTESIAN_POINT('Ctrl Pts',(-67.6636551726964,-23.1963742630715,
0.));
#142079=CARTESIAN_POINT('Ctrl Pts',(-67.6636551726964,-23.1963742630715,
12.));
#142080=CARTESIAN_POINT('Ctrl Pts',(-67.6405686407863,-23.1963685232188,
0.));
#142081=CARTESIAN_POINT('Ctrl Pts',(-67.6405686407863,-23.1963685232188,
12.));
#142082=CARTESIAN_POINT('Ctrl Pts',(-67.6175267028555,-23.1963398337069,
0.));
#142083=CARTESIAN_POINT('Ctrl Pts',(-67.6175267028555,-23.1963398337069,
12.));
#142084=CARTESIAN_POINT('Ctrl Pts',(-67.5945294909426,-23.1962882611453,
0.));
#142085=CARTESIAN_POINT('Ctrl Pts',(-67.5945294909426,-23.1962882611453,
12.));
#142086=CARTESIAN_POINT('Ctrl Pts',(-67.5715771376461,-23.196213872536,
0.));
#142087=CARTESIAN_POINT('Ctrl Pts',(-67.5715771376461,-23.196213872536,
12.));
#142088=CARTESIAN_POINT('Ctrl Pts',(-67.5486697761288,-23.1961167352772,
0.));
#142089=CARTESIAN_POINT('Ctrl Pts',(-67.5486697761288,-23.1961167352772,
12.));
#142090=CARTESIAN_POINT('Ctrl Pts',(-67.5258075401146,-23.1959969171701,
0.));
#142091=CARTESIAN_POINT('Ctrl Pts',(-67.5258075401146,-23.1959969171701,
12.));
#142092=CARTESIAN_POINT('Ctrl Pts',(-67.5029905638949,-23.1958544864215,
0.));
#142093=CARTESIAN_POINT('Ctrl Pts',(-67.5029905638949,-23.1958544864215,
12.));
#142094=CARTESIAN_POINT('Ctrl Pts',(-67.4802189823408,-23.195689511644,
0.));
#142095=CARTESIAN_POINT('Ctrl Pts',(-67.4802189823408,-23.195689511644,
12.));
#142096=CARTESIAN_POINT('Ctrl Pts',(-67.4574929309076,-23.195502061859,
0.));
#142097=CARTESIAN_POINT('Ctrl Pts',(-67.4574929309076,-23.195502061859,
12.));
#142098=CARTESIAN_POINT('Ctrl Pts',(-67.4348125456398,-23.1952922065012,
0.));
#142099=CARTESIAN_POINT('Ctrl Pts',(-67.4348125456398,-23.1952922065012,
12.));
#142100=CARTESIAN_POINT('Ctrl Pts',(-67.412177963168,-23.1950600154265,
0.));
#142101=CARTESIAN_POINT('Ctrl Pts',(-67.412177963168,-23.1950600154265,
12.));
#142102=CARTESIAN_POINT('Ctrl Pts',(-67.3895893207182,-23.1948055589129,
0.));
#142103=CARTESIAN_POINT('Ctrl Pts',(-67.3895893207182,-23.1948055589129,
12.));
#142104=CARTESIAN_POINT('Ctrl Pts',(-67.3670467561212,-23.194528907661,
0.));
#142105=CARTESIAN_POINT('Ctrl Pts',(-67.3670467561212,-23.194528907661,
12.));
#142106=CARTESIAN_POINT('Ctrl Pts',(-67.3445504078176,-23.1942301327978,
0.));
#142107=CARTESIAN_POINT('Ctrl Pts',(-67.3445504078176,-23.1942301327978,
12.));
#142108=CARTESIAN_POINT('Ctrl Pts',(-67.3221004148603,-23.1939093058801,
0.));
#142109=CARTESIAN_POINT('Ctrl Pts',(-67.3221004148603,-23.1939093058801,
12.));
#142110=CARTESIAN_POINT('Ctrl Pts',(-67.2996969169098,-23.1935664989018,
0.));
#142111=CARTESIAN_POINT('Ctrl Pts',(-67.2996969169098,-23.1935664989018,
12.));
#142112=CARTESIAN_POINT('Ctrl Pts',(-67.2773400542477,-23.1932017842953,
0.));
#142113=CARTESIAN_POINT('Ctrl Pts',(-67.2773400542477,-23.1932017842953,
12.));
#142114=CARTESIAN_POINT('Ctrl Pts',(-67.2550299677888,-23.1928152349343,
0.));
#142115=CARTESIAN_POINT('Ctrl Pts',(-67.2550299677888,-23.1928152349343,
12.));
#142116=CARTESIAN_POINT('Ctrl Pts',(-67.232766799088,-23.1924069241385,
0.));
#142117=CARTESIAN_POINT('Ctrl Pts',(-67.232766799088,-23.1924069241385,
12.));
#142118=CARTESIAN_POINT('Ctrl Pts',(-67.2105506903447,-23.1919769256803,
0.));
#142119=CARTESIAN_POINT('Ctrl Pts',(-67.2105506903447,-23.1919769256803,
12.));
#142120=CARTESIAN_POINT('Ctrl Pts',(-67.1883817844038,-23.1915253137924,
0.));
#142121=CARTESIAN_POINT('Ctrl Pts',(-67.1883817844038,-23.1915253137924,
12.));
#142122=CARTESIAN_POINT('Ctrl Pts',(-67.1662602247639,-23.1910521631657,
0.));
#142123=CARTESIAN_POINT('Ctrl Pts',(-67.1662602247639,-23.1910521631657,
12.));
#142124=CARTESIAN_POINT('Ctrl Pts',(-67.1441861555817,-23.1905575489505,
0.));
#142125=CARTESIAN_POINT('Ctrl Pts',(-67.1441861555817,-23.1905575489505,
12.));
#142126=CARTESIAN_POINT('Ctrl Pts',(-67.1221597216741,-23.1900415467574,
0.));
#142127=CARTESIAN_POINT('Ctrl Pts',(-67.1221597216741,-23.1900415467574,
12.));
#142128=CARTESIAN_POINT('Ctrl Pts',(-67.1001810685143,-23.1895042326627,
0.));
#142129=CARTESIAN_POINT('Ctrl Pts',(-67.1001810685143,-23.1895042326627,
12.));
#142130=CARTESIAN_POINT('Ctrl Pts',(-67.0782503422305,-23.1889456832119,
0.));
#142131=CARTESIAN_POINT('Ctrl Pts',(-67.0782503422305,-23.1889456832119,
12.));
#142132=CARTESIAN_POINT('Ctrl Pts',(-67.0563676896325,-23.1883659754271,
0.));
#142133=CARTESIAN_POINT('Ctrl Pts',(-67.0563676896325,-23.1883659754271,
12.));
#142134=CARTESIAN_POINT('Ctrl Pts',(-67.0345332582306,-23.1877651868158,
0.));
#142135=CARTESIAN_POINT('Ctrl Pts',(-67.0345332582306,-23.1877651868158,
12.));
#142136=CARTESIAN_POINT('Ctrl Pts',(-67.0127471962501,-23.1871433953793,
0.));
#142137=CARTESIAN_POINT('Ctrl Pts',(-67.0127471962501,-23.1871433953793,
12.));
#142138=CARTESIAN_POINT('Ctrl Pts',(-66.9910096526462,-23.1865006796284,
0.));
#142139=CARTESIAN_POINT('Ctrl Pts',(-66.9910096526462,-23.1865006796284,
12.));
#142140=CARTESIAN_POINT('Ctrl Pts',(-66.9693207771031,-23.1858371185842,
0.));
#142141=CARTESIAN_POINT('Ctrl Pts',(-66.9693207771031,-23.1858371185842,
12.));
#142142=CARTESIAN_POINT('Ctrl Pts',(-66.9476807200203,-23.1851527917657,
0.));
#142143=CARTESIAN_POINT('Ctrl Pts',(-66.9476807200203,-23.1851527917657,
12.));
#142144=CARTESIAN_POINT('Ctrl Pts',(-66.9260896324949,-23.1844477791814,
0.));
#142145=CARTESIAN_POINT('Ctrl Pts',(-66.9260896324949,-23.1844477791814,
12.));
#142146=CARTESIAN_POINT('Ctrl Pts',(-66.9045476663063,-23.1837221613235,
0.));
#142147=CARTESIAN_POINT('Ctrl Pts',(-66.9045476663063,-23.1837221613235,
12.));
#142148=CARTESIAN_POINT('Ctrl Pts',(-66.8830549738795,-23.1829760191591,
0.));
#142149=CARTESIAN_POINT('Ctrl Pts',(-66.8830549738795,-23.1829760191591,
12.));
#142150=CARTESIAN_POINT('Ctrl Pts',(-66.8616117083331,-23.1822094341517,
0.));
#142151=CARTESIAN_POINT('Ctrl Pts',(-66.8616117083331,-23.1822094341517,
12.));
#142152=CARTESIAN_POINT('Ctrl Pts',(-66.8402180235566,-23.1814224882954,
0.));
#142153=CARTESIAN_POINT('Ctrl Pts',(-66.8402180235566,-23.1814224882954,
12.));
#142154=CARTESIAN_POINT('Ctrl Pts',(-66.8188740742727,-23.1806152641475,
0.));
#142155=CARTESIAN_POINT('Ctrl Pts',(-66.8188740742727,-23.1806152641475,
12.));
#142156=CARTESIAN_POINT('Ctrl Pts',(-66.7975800161,-23.1797878448639,0.));
#142157=CARTESIAN_POINT('Ctrl Pts',(-66.7975800161,-23.1797878448639,12.));
#142158=CARTESIAN_POINT('Ctrl Pts',(-66.776336005612,-23.1789403142366,
0.));
#142159=CARTESIAN_POINT('Ctrl Pts',(-66.776336005612,-23.1789403142366,
12.));
#142160=CARTESIAN_POINT('Ctrl Pts',(-66.7551422002204,-23.17807275663,0.));
#142161=CARTESIAN_POINT('Ctrl Pts',(-66.7551422002204,-23.17807275663,12.));
#142162=CARTESIAN_POINT('Ctrl Pts',(-66.7339987580427,-23.1771852569131,
0.));
#142163=CARTESIAN_POINT('Ctrl Pts',(-66.7339987580427,-23.1771852569131,
12.));
#142164=CARTESIAN_POINT('Ctrl Pts',(-66.7129058377896,-23.1762779004044,
0.));
#142165=CARTESIAN_POINT('Ctrl Pts',(-66.7129058377896,-23.1762779004044,
12.));
#142166=CARTESIAN_POINT('Ctrl Pts',(-66.6918635985972,-23.1753507727939,
0.));
#142167=CARTESIAN_POINT('Ctrl Pts',(-66.6918635985972,-23.1753507727939,
12.));
#142168=CARTESIAN_POINT('Ctrl Pts',(-66.6708722000079,-23.1744039601382,
0.));
#142169=CARTESIAN_POINT('Ctrl Pts',(-66.6708722000079,-23.1744039601382,
12.));
#142170=CARTESIAN_POINT('Ctrl Pts',(-66.6499318023473,-23.1734375490431,
0.));
#142171=CARTESIAN_POINT('Ctrl Pts',(-66.6499318023473,-23.1734375490431,
12.));
#142172=CARTESIAN_POINT('Ctrl Pts',(-66.6290425670548,-23.1724516268302,
0.));
#142173=CARTESIAN_POINT('Ctrl Pts',(-66.6290425670548,-23.1724516268302,
12.));
#142174=CARTESIAN_POINT('Ctrl Pts',(-66.6082046569644,-23.1714462816789,
0.));
#142175=CARTESIAN_POINT('Ctrl Pts',(-66.6082046569644,-23.1714462816789,
12.));
#142176=CARTESIAN_POINT('Ctrl Pts',(-66.5874182367563,-23.1704216028614,
0.));
#142177=CARTESIAN_POINT('Ctrl Pts',(-66.5874182367563,-23.1704216028614,
12.));
#142178=CARTESIAN_POINT('Ctrl Pts',(-66.5666834726454,-23.1693776805866,
0.));
#142179=CARTESIAN_POINT('Ctrl Pts',(-66.5666834726454,-23.1693776805866,
12.));
#142180=CARTESIAN_POINT('Ctrl Pts',(-66.5460005315376,-23.1683146055726,
0.));
#142181=CARTESIAN_POINT('Ctrl Pts',(-66.5460005315376,-23.1683146055726,
12.));
#142182=CARTESIAN_POINT('Ctrl Pts',(-66.5253695803205,-23.1672324686926,
0.));
#142183=CARTESIAN_POINT('Ctrl Pts',(-66.5253695803205,-23.1672324686926,
12.));
#142184=CARTESIAN_POINT('Ctrl Pts',(-66.5047907851348,-23.1661313606132,
0.));
#142185=CARTESIAN_POINT('Ctrl Pts',(-66.5047907851348,-23.1661313606132,
12.));
#142186=CARTESIAN_POINT('Ctrl Pts',(-66.4842643105311,-23.1650113713808,
0.));
#142187=CARTESIAN_POINT('Ctrl Pts',(-66.4842643105311,-23.1650113713808,
12.));
#142188=CARTESIAN_POINT('Ctrl Pts',(-66.4637903210727,-23.1638725912195,
0.));
#142189=CARTESIAN_POINT('Ctrl Pts',(-66.4637903210727,-23.1638725912195,
12.));
#142190=CARTESIAN_POINT('Ctrl Pts',(-66.4433689832478,-23.1627151114883,
0.));
#142191=CARTESIAN_POINT('Ctrl Pts',(-66.4433689832478,-23.1627151114883,
12.));
#142192=CARTESIAN_POINT('Ctrl Pts',(-66.4230004670278,-23.1615390254632,
0.));
#142193=CARTESIAN_POINT('Ctrl Pts',(-66.4230004670278,-23.1615390254632,
12.));
#142194=CARTESIAN_POINT('Ctrl Pts',(-66.4026849481232,-23.160344429474,
0.));
#142195=CARTESIAN_POINT('Ctrl Pts',(-66.4026849481232,-23.160344429474,
12.));
#142196=CARTESIAN_POINT('Ctrl Pts',(-66.3824226081801,-23.1591314230083,
0.));
#142197=CARTESIAN_POINT('Ctrl Pts',(-66.3824226081801,-23.1591314230083,
12.));
#142198=CARTESIAN_POINT('Ctrl Pts',(-66.3622136300654,-23.1579001063424,
0.));
#142199=CARTESIAN_POINT('Ctrl Pts',(-66.3622136300654,-23.1579001063424,
12.));
#142200=CARTESIAN_POINT('Ctrl Pts',(-66.3420581937147,-23.1566505784621,
0.));
#142201=CARTESIAN_POINT('Ctrl Pts',(-66.3420581937147,-23.1566505784621,
12.));
#142202=CARTESIAN_POINT('Ctrl Pts',(-66.3219564725184,-23.1553829352539,
0.));
#142203=CARTESIAN_POINT('Ctrl Pts',(-66.3219564725184,-23.1553829352539,
12.));
#142204=CARTESIAN_POINT('Ctrl Pts',(-66.3019086275444,-23.1540972666191,
0.));
#142205=CARTESIAN_POINT('Ctrl Pts',(-66.3019086275444,-23.1540972666191,
12.));
#142206=CARTESIAN_POINT('Ctrl Pts',(-66.281914813114,-23.1527936592651,
0.));
#142207=CARTESIAN_POINT('Ctrl Pts',(-66.281914813114,-23.1527936592651,
12.));
#142208=CARTESIAN_POINT('Ctrl Pts',(-66.2619751878793,-23.1514722022503,
0.));
#142209=CARTESIAN_POINT('Ctrl Pts',(-66.2619751878793,-23.1514722022503,
12.));
#142210=CARTESIAN_POINT('Ctrl Pts',(-66.2420899237318,-23.1501329914488,
0.));
#142211=CARTESIAN_POINT('Ctrl Pts',(-66.2420899237318,-23.1501329914488,
12.));
#142212=CARTESIAN_POINT('Ctrl Pts',(-66.2222592165398,-23.1487761349298,
0.));
#142213=CARTESIAN_POINT('Ctrl Pts',(-66.2222592165398,-23.1487761349298,
12.));
#142214=CARTESIAN_POINT('Ctrl Pts',(-66.2024832934733,-23.147401756643,
0.));
#142215=CARTESIAN_POINT('Ctrl Pts',(-66.2024832934733,-23.147401756643,
12.));
#142216=CARTESIAN_POINT('Ctrl Pts',(-66.1827623902755,-23.1460099850704,
0.));
#142217=CARTESIAN_POINT('Ctrl Pts',(-66.1827623902755,-23.1460099850704,
12.));
#142218=CARTESIAN_POINT('Ctrl Pts',(-66.163096729667,-23.1446009424872,
0.));
#142219=CARTESIAN_POINT('Ctrl Pts',(-66.163096729667,-23.1446009424872,
12.));
#142220=CARTESIAN_POINT('Ctrl Pts',(-66.14348650151,-23.1431747350127,0.));
#142221=CARTESIAN_POINT('Ctrl Pts',(-66.14348650151,-23.1431747350127,12.));
#142222=CARTESIAN_POINT('Ctrl Pts',(-66.1239318368803,-23.1417314398501,
0.));
#142223=CARTESIAN_POINT('Ctrl Pts',(-66.1239318368803,-23.1417314398501,
12.));
#142224=CARTESIAN_POINT('Ctrl Pts',(-66.1044328067739,-23.140271103958,
0.));
#142225=CARTESIAN_POINT('Ctrl Pts',(-66.1044328067739,-23.140271103958,
12.));
#142226=CARTESIAN_POINT('Ctrl Pts',(-66.0888781152779,-23.1390892229923,
0.));
#142227=CARTESIAN_POINT('Ctrl Pts',(-66.0888781152779,-23.1390892229923,
12.));
#142228=CARTESIAN_POINT('Ctrl Pts',(-66.0772371487475,-23.1381951597491,
0.));
#142229=CARTESIAN_POINT('Ctrl Pts',(-66.0772371487475,-23.1381951597491,
12.));
#142230=CARTESIAN_POINT('Ctrl Pts',(-66.0694876382212,-23.1375957166138,
0.));
#142231=CARTESIAN_POINT('Ctrl Pts',(-66.0694876382212,-23.1375957166138,
12.));
#142232=CARTESIAN_POINT('Ctrl Pts',(-66.0656156664138,-23.1372951448024,
0.));
#142233=CARTESIAN_POINT('Ctrl Pts',(-66.0656156664138,-23.1372951448024,
12.));
#142234=CARTESIAN_POINT('',(-66.0656156664138,-23.1372951448024,12.));
#142235=CARTESIAN_POINT('Ctrl Pts',(-66.0656156664138,-23.1372951448024,
12.));
#142236=CARTESIAN_POINT('Ctrl Pts',(-66.0694876382212,-23.1375957166138,
12.));
#142237=CARTESIAN_POINT('Ctrl Pts',(-66.0772371487475,-23.1381951597491,
12.));
#142238=CARTESIAN_POINT('Ctrl Pts',(-66.0888781152779,-23.1390892229923,
12.));
#142239=CARTESIAN_POINT('Ctrl Pts',(-66.1044328067739,-23.140271103958,
12.));
#142240=CARTESIAN_POINT('Ctrl Pts',(-66.1239318368803,-23.1417314398501,
12.));
#142241=CARTESIAN_POINT('Ctrl Pts',(-66.14348650151,-23.1431747350127,12.));
#142242=CARTESIAN_POINT('Ctrl Pts',(-66.163096729667,-23.1446009424872,
12.));
#142243=CARTESIAN_POINT('Ctrl Pts',(-66.1827623902755,-23.1460099850704,
12.));
#142244=CARTESIAN_POINT('Ctrl Pts',(-66.2024832934733,-23.147401756643,
12.));
#142245=CARTESIAN_POINT('Ctrl Pts',(-66.2222592165398,-23.1487761349298,
12.));
#142246=CARTESIAN_POINT('Ctrl Pts',(-66.2420899237318,-23.1501329914488,
12.));
#142247=CARTESIAN_POINT('Ctrl Pts',(-66.2619751878793,-23.1514722022503,
12.));
#142248=CARTESIAN_POINT('Ctrl Pts',(-66.281914813114,-23.1527936592651,
12.));
#142249=CARTESIAN_POINT('Ctrl Pts',(-66.3019086275444,-23.1540972666191,
12.));
#142250=CARTESIAN_POINT('Ctrl Pts',(-66.3219564725184,-23.1553829352539,
12.));
#142251=CARTESIAN_POINT('Ctrl Pts',(-66.3420581937147,-23.1566505784621,
12.));
#142252=CARTESIAN_POINT('Ctrl Pts',(-66.3622136300654,-23.1579001063424,
12.));
#142253=CARTESIAN_POINT('Ctrl Pts',(-66.3824226081801,-23.1591314230083,
12.));
#142254=CARTESIAN_POINT('Ctrl Pts',(-66.4026849481232,-23.160344429474,
12.));
#142255=CARTESIAN_POINT('Ctrl Pts',(-66.4230004670278,-23.1615390254632,
12.));
#142256=CARTESIAN_POINT('Ctrl Pts',(-66.4433689832478,-23.1627151114883,
12.));
#142257=CARTESIAN_POINT('Ctrl Pts',(-66.4637903210727,-23.1638725912195,
12.));
#142258=CARTESIAN_POINT('Ctrl Pts',(-66.4842643105311,-23.1650113713808,
12.));
#142259=CARTESIAN_POINT('Ctrl Pts',(-66.5047907851348,-23.1661313606132,
12.));
#142260=CARTESIAN_POINT('Ctrl Pts',(-66.5253695803205,-23.1672324686926,
12.));
#142261=CARTESIAN_POINT('Ctrl Pts',(-66.5460005315376,-23.1683146055726,
12.));
#142262=CARTESIAN_POINT('Ctrl Pts',(-66.5666834726454,-23.1693776805866,
12.));
#142263=CARTESIAN_POINT('Ctrl Pts',(-66.5874182367563,-23.1704216028614,
12.));
#142264=CARTESIAN_POINT('Ctrl Pts',(-66.6082046569644,-23.1714462816789,
12.));
#142265=CARTESIAN_POINT('Ctrl Pts',(-66.6290425670548,-23.1724516268302,
12.));
#142266=CARTESIAN_POINT('Ctrl Pts',(-66.6499318023473,-23.1734375490431,
12.));
#142267=CARTESIAN_POINT('Ctrl Pts',(-66.6708722000079,-23.1744039601382,
12.));
#142268=CARTESIAN_POINT('Ctrl Pts',(-66.6918635985972,-23.1753507727939,
12.));
#142269=CARTESIAN_POINT('Ctrl Pts',(-66.7129058377896,-23.1762779004044,
12.));
#142270=CARTESIAN_POINT('Ctrl Pts',(-66.7339987580427,-23.1771852569131,
12.));
#142271=CARTESIAN_POINT('Ctrl Pts',(-66.7551422002204,-23.17807275663,12.));
#142272=CARTESIAN_POINT('Ctrl Pts',(-66.776336005612,-23.1789403142366,
12.));
#142273=CARTESIAN_POINT('Ctrl Pts',(-66.7975800161,-23.1797878448639,12.));
#142274=CARTESIAN_POINT('Ctrl Pts',(-66.8188740742727,-23.1806152641475,
12.));
#142275=CARTESIAN_POINT('Ctrl Pts',(-66.8402180235566,-23.1814224882954,
12.));
#142276=CARTESIAN_POINT('Ctrl Pts',(-66.8616117083331,-23.1822094341517,
12.));
#142277=CARTESIAN_POINT('Ctrl Pts',(-66.8830549738795,-23.1829760191591,
12.));
#142278=CARTESIAN_POINT('Ctrl Pts',(-66.9045476663063,-23.1837221613235,
12.));
#142279=CARTESIAN_POINT('Ctrl Pts',(-66.9260896324949,-23.1844477791814,
12.));
#142280=CARTESIAN_POINT('Ctrl Pts',(-66.9476807200203,-23.1851527917657,
12.));
#142281=CARTESIAN_POINT('Ctrl Pts',(-66.9693207771031,-23.1858371185842,
12.));
#142282=CARTESIAN_POINT('Ctrl Pts',(-66.9910096526462,-23.1865006796284,
12.));
#142283=CARTESIAN_POINT('Ctrl Pts',(-67.0127471962501,-23.1871433953793,
12.));
#142284=CARTESIAN_POINT('Ctrl Pts',(-67.0345332582306,-23.1877651868158,
12.));
#142285=CARTESIAN_POINT('Ctrl Pts',(-67.0563676896325,-23.1883659754271,
12.));
#142286=CARTESIAN_POINT('Ctrl Pts',(-67.0782503422305,-23.1889456832119,
12.));
#142287=CARTESIAN_POINT('Ctrl Pts',(-67.1001810685143,-23.1895042326627,
12.));
#142288=CARTESIAN_POINT('Ctrl Pts',(-67.1221597216741,-23.1900415467574,
12.));
#142289=CARTESIAN_POINT('Ctrl Pts',(-67.1441861555817,-23.1905575489505,
12.));
#142290=CARTESIAN_POINT('Ctrl Pts',(-67.1662602247639,-23.1910521631657,
12.));
#142291=CARTESIAN_POINT('Ctrl Pts',(-67.1883817844038,-23.1915253137924,
12.));
#142292=CARTESIAN_POINT('Ctrl Pts',(-67.2105506903447,-23.1919769256803,
12.));
#142293=CARTESIAN_POINT('Ctrl Pts',(-67.232766799088,-23.1924069241385,
12.));
#142294=CARTESIAN_POINT('Ctrl Pts',(-67.2550299677888,-23.1928152349343,
12.));
#142295=CARTESIAN_POINT('Ctrl Pts',(-67.2773400542477,-23.1932017842953,
12.));
#142296=CARTESIAN_POINT('Ctrl Pts',(-67.2996969169098,-23.1935664989018,
12.));
#142297=CARTESIAN_POINT('Ctrl Pts',(-67.3221004148603,-23.1939093058801,
12.));
#142298=CARTESIAN_POINT('Ctrl Pts',(-67.3445504078176,-23.1942301327978,
12.));
#142299=CARTESIAN_POINT('Ctrl Pts',(-67.3670467561212,-23.194528907661,
12.));
#142300=CARTESIAN_POINT('Ctrl Pts',(-67.3895893207182,-23.1948055589129,
12.));
#142301=CARTESIAN_POINT('Ctrl Pts',(-67.412177963168,-23.1950600154265,
12.));
#142302=CARTESIAN_POINT('Ctrl Pts',(-67.4348125456398,-23.1952922065012,
12.));
#142303=CARTESIAN_POINT('Ctrl Pts',(-67.4574929309076,-23.195502061859,
12.));
#142304=CARTESIAN_POINT('Ctrl Pts',(-67.4802189823408,-23.195689511644,
12.));
#142305=CARTESIAN_POINT('Ctrl Pts',(-67.5029905638949,-23.1958544864215,
12.));
#142306=CARTESIAN_POINT('Ctrl Pts',(-67.5258075401146,-23.1959969171701,
12.));
#142307=CARTESIAN_POINT('Ctrl Pts',(-67.5486697761288,-23.1961167352772,
12.));
#142308=CARTESIAN_POINT('Ctrl Pts',(-67.5715771376461,-23.196213872536,
12.));
#142309=CARTESIAN_POINT('Ctrl Pts',(-67.5945294909426,-23.1962882611453,
12.));
#142310=CARTESIAN_POINT('Ctrl Pts',(-67.6175267028555,-23.1963398337069,
12.));
#142311=CARTESIAN_POINT('Ctrl Pts',(-67.6405686407863,-23.1963685232188,
12.));
#142312=CARTESIAN_POINT('Ctrl Pts',(-67.6636551726964,-23.1963742630715,
12.));
#142313=CARTESIAN_POINT('Ctrl Pts',(-67.6867861671031,-23.1963569870451,
12.));
#142314=CARTESIAN_POINT('Ctrl Pts',(-67.7099614930671,-23.1963166293102,
12.));
#142315=CARTESIAN_POINT('Ctrl Pts',(-67.7331810201883,-23.1962531244245,
12.));
#142316=CARTESIAN_POINT('Ctrl Pts',(-67.7564446186079,-23.1961664073262,
12.));
#142317=CARTESIAN_POINT('Ctrl Pts',(-67.7797521590045,-23.1960564133304,
12.));
#142318=CARTESIAN_POINT('Ctrl Pts',(-67.8031035125887,-23.1959230781269,
12.));
#142319=CARTESIAN_POINT('Ctrl Pts',(-67.8264985510917,-23.1957663377807,
12.));
#142320=CARTESIAN_POINT('Ctrl Pts',(-67.8499371467616,-23.1955861287286,
12.));
#142321=CARTESIAN_POINT('Ctrl Pts',(-67.8734191723667,-23.1953823877734,
12.));
#142322=CARTESIAN_POINT('Ctrl Pts',(-67.8969445011916,-23.1951550520802,
12.));
#142323=CARTESIAN_POINT('Ctrl Pts',(-67.9205130070324,-23.1949040591744,
12.));
#142324=CARTESIAN_POINT('Ctrl Pts',(-67.9441245641842,-23.1946293469427,
12.));
#142325=CARTESIAN_POINT('Ctrl Pts',(-67.9677790474385,-23.1943308536297,
12.));
#142326=CARTESIAN_POINT('Ctrl Pts',(-67.991476332086,-23.1940085178313,
12.));
#142327=CARTESIAN_POINT('Ctrl Pts',(-68.0152162939121,-23.1936622784919,
12.));
#142328=CARTESIAN_POINT('Ctrl Pts',(-68.0389988091933,-23.1932920749023,
12.));
#142329=CARTESIAN_POINT('Ctrl Pts',(-68.0628237546863,-23.1928978467021,
12.));
#142330=CARTESIAN_POINT('Ctrl Pts',(-68.0866910076251,-23.1924795338749,
12.));
#142331=CARTESIAN_POINT('Ctrl Pts',(-68.110600445723,-23.1920370767426,
12.));
#142332=CARTESIAN_POINT('Ctrl Pts',(-68.1345519471695,-23.1915704159623,
12.));
#142333=CARTESIAN_POINT('Ctrl Pts',(-68.1585453906257,-23.1910794925251,
12.));
#142334=CARTESIAN_POINT('Ctrl Pts',(-68.1825806552129,-23.1905642477571,
12.));
#142335=CARTESIAN_POINT('Ctrl Pts',(-68.2066576205116,-23.1900246233165,
12.));
#142336=CARTESIAN_POINT('Ctrl Pts',(-68.2307761665633,-23.1894605611871,
12.));
#142337=CARTESIAN_POINT('Ctrl Pts',(-68.2549361738681,-23.1888720036757,
12.));
#142338=CARTESIAN_POINT('Ctrl Pts',(-68.2791375233795,-23.1882588934107,
12.));
#142339=CARTESIAN_POINT('Ctrl Pts',(-68.3033800964939,-23.1876211733436,
12.));
#142340=CARTESIAN_POINT('Ctrl Pts',(-68.3276637750485,-23.1869587867459,
12.));
#142341=CARTESIAN_POINT('Ctrl Pts',(-68.3519884413246,-23.1862716772031,
12.));
#142342=CARTESIAN_POINT('Ctrl Pts',(-68.376353978044,-23.1855597886116,
12.));
#142343=CARTESIAN_POINT('Ctrl Pts',(-68.4007602683652,-23.1848230651777,
12.));
#142344=CARTESIAN_POINT('Ctrl Pts',(-68.4252071958729,-23.1840614514192,
12.));
#142345=CARTESIAN_POINT('Ctrl Pts',(-68.4496946445758,-23.183274892163,
12.));
#142346=CARTESIAN_POINT('Ctrl Pts',(-68.4742224989098,-23.1824633325385,
12.));
#142347=CARTESIAN_POINT('Ctrl Pts',(-68.4987906437356,-23.1816267179751,
12.));
#142348=CARTESIAN_POINT('Ctrl Pts',(-68.5233989643345,-23.180764994201,
12.));
#142349=CARTESIAN_POINT('Ctrl Pts',(-68.5480473463985,-23.179878107245,
12.));
#142350=CARTESIAN_POINT('Ctrl Pts',(-68.5727356760278,-23.1789660034342,
12.));
#142351=CARTESIAN_POINT('Ctrl Pts',(-68.597463839733,-23.1780286293875,
12.));
#142352=CARTESIAN_POINT('Ctrl Pts',(-68.6222317244341,-23.1770659320138,
12.));
#142353=CARTESIAN_POINT('Ctrl Pts',(-68.6470392174564,-23.1760778585092,
12.));
#142354=CARTESIAN_POINT('Ctrl Pts',(-68.6718862065216,-23.1750643563602,
12.));
#142355=CARTESIAN_POINT('Ctrl Pts',(-68.696772579744,-23.1740253733417,
12.));
#142356=CARTESIAN_POINT('Ctrl Pts',(-68.7216982256341,-23.172960857511,
12.));
#142357=CARTESIAN_POINT('Ctrl Pts',(-68.746663033096,-23.1718707572043,
12.));
#142358=CARTESIAN_POINT('Ctrl Pts',(-68.771666891425,-23.170755021036,12.));
#142359=CARTESIAN_POINT('Ctrl Pts',(-68.7967096902996,-23.1696135978997,
12.));
#142360=CARTESIAN_POINT('Ctrl Pts',(-68.8217913197752,-23.1684464369686,
12.));
#142361=CARTESIAN_POINT('Ctrl Pts',(-68.8469116702898,-23.1672534876889,
12.));
#142362=CARTESIAN_POINT('Ctrl Pts',(-68.8720706326609,-23.1660346997764,
12.));
#142363=CARTESIAN_POINT('Ctrl Pts',(-68.8972680980842,-23.164790023215,
12.));
#142364=CARTESIAN_POINT('Ctrl Pts',(-68.9225039581248,-23.1635194082581,
12.));
#142365=CARTESIAN_POINT('Ctrl Pts',(-68.9477781047106,-23.1622228054291,
12.));
#142366=CARTESIAN_POINT('Ctrl Pts',(-68.9730904301369,-23.1609001655156,
12.));
#142367=CARTESIAN_POINT('Ctrl Pts',(-68.9984408270659,-23.1595514395656,
12.));
#142368=CARTESIAN_POINT('Ctrl Pts',(-69.0238291885245,-23.1581765788869,
12.));
#142369=CARTESIAN_POINT('Ctrl Pts',(-69.0492554078992,-23.1567755350469,
12.));
#142370=CARTESIAN_POINT('Ctrl Pts',(-69.074719378928,-23.1553482598762,
12.));
#142371=CARTESIAN_POINT('Ctrl Pts',(-69.1002209957025,-23.1538947054615,
12.));
#142372=CARTESIAN_POINT('Ctrl Pts',(-69.1257601526687,-23.152414824141,
12.));
#142373=CARTESIAN_POINT('Ctrl Pts',(-69.1513367446231,-23.1509085685032,
12.));
#142374=CARTESIAN_POINT('Ctrl Pts',(-69.1769506667084,-23.1493758913859,
12.));
#142375=CARTESIAN_POINT('Ctrl Pts',(-69.2026018144028,-23.147816745879,
12.));
#142376=CARTESIAN_POINT('Ctrl Pts',(-69.2282900835235,-23.1462310853206,
12.));
#142377=CARTESIAN_POINT('Ctrl Pts',(-69.254015370231,-23.1446188632931,
12.));
#142378=CARTESIAN_POINT('Ctrl Pts',(-69.2797775710273,-23.142980033622,
12.));
#142379=CARTESIAN_POINT('Ctrl Pts',(-69.3055765827546,-23.1413145503762,
12.));
#142380=CARTESIAN_POINT('Ctrl Pts',(-69.3314123025869,-23.1396223678725,
12.));
#142381=CARTESIAN_POINT('Ctrl Pts',(-69.3572846280296,-23.1379034406718,
12.));
#142382=CARTESIAN_POINT('Ctrl Pts',(-69.3831934569182,-23.1361577235709,
12.));
#142383=CARTESIAN_POINT('Ctrl Pts',(-69.4091386874132,-23.1343851715989,
12.));
#142384=CARTESIAN_POINT('Ctrl Pts',(-69.4351202179946,-23.1325857400144,
12.));
#142385=CARTESIAN_POINT('Ctrl Pts',(-69.4611379474484,-23.1307593843061,
12.));
#142386=CARTESIAN_POINT('Ctrl Pts',(-69.4871917748654,-23.1289060601924,
12.));
#142387=CARTESIAN_POINT('Ctrl Pts',(-69.5132815996537,-23.1270257236204,
12.));
#142388=CARTESIAN_POINT('Ctrl Pts',(-69.539407321546,-23.1251183307676,
12.));
#142389=CARTESIAN_POINT('Ctrl Pts',(-69.5655688406052,-23.1231838380452,
12.));
#142390=CARTESIAN_POINT('Ctrl Pts',(-69.5917660572265,-23.1212222021051,
12.));
#142391=CARTESIAN_POINT('Ctrl Pts',(-69.6179988721365,-23.1192333798441,
12.));
#142392=CARTESIAN_POINT('Ctrl Pts',(-69.6442671863765,-23.1172173283859,
12.));
#142393=CARTESIAN_POINT('Ctrl Pts',(-69.6705709012852,-23.1151740050681,
12.));
#142394=CARTESIAN_POINT('Ctrl Pts',(-69.6969099184767,-23.1131033674301,
12.));
#142395=CARTESIAN_POINT('Ctrl Pts',(-69.7232841398197,-23.1110053732046,
12.));
#142396=CARTESIAN_POINT('Ctrl Pts',(-69.7496934674069,-23.1088799803089,
12.));
#142397=CARTESIAN_POINT('Ctrl Pts',(-69.7761378035964,-23.106727146861,
12.));
#142398=CARTESIAN_POINT('Ctrl Pts',(-69.8026170510572,-23.1045468311991,
12.));
#142399=CARTESIAN_POINT('Ctrl Pts',(-69.8291311128118,-23.1023389919051,
12.));
#142400=CARTESIAN_POINT('Ctrl Pts',(-69.8556798922693,-23.1001035878241,
12.));
#142401=CARTESIAN_POINT('Ctrl Pts',(-69.8822632932768,-23.0978405781021,
12.));
#142402=CARTESIAN_POINT('Ctrl Pts',(-69.9088812200713,-23.0955499221558,
12.));
#142403=CARTESIAN_POINT('Ctrl Pts',(-69.9355335771729,-23.0932315796068,
12.));
#142404=CARTESIAN_POINT('Ctrl Pts',(-69.9622202692873,-23.0908855102251,
12.));
#142405=CARTESIAN_POINT('Ctrl Pts',(-69.9889412012143,-23.0885116738798,
12.));
#142406=CARTESIAN_POINT('Ctrl Pts',(-70.0156962777169,-23.0861100304729,
12.));
#142407=CARTESIAN_POINT('Ctrl Pts',(-70.0424854035115,-23.0836805399374,
12.));
#142408=CARTESIAN_POINT('Ctrl Pts',(-70.0693084835373,-23.0812231623765,
12.));
#142409=CARTESIAN_POINT('Ctrl Pts',(-70.0961654231639,-23.0787378581774,
12.));
#142410=CARTESIAN_POINT('Ctrl Pts',(-70.123056128422,-23.0762245881389,
12.));
#142411=CARTESIAN_POINT('Ctrl Pts',(-70.1499805062172,-23.0736833135938,
12.));
#142412=CARTESIAN_POINT('Ctrl Pts',(-70.1769384645586,-23.071113996544,
12.));
#142413=CARTESIAN_POINT('Ctrl Pts',(-70.2039299120488,-23.0685165993691,
12.));
#142414=CARTESIAN_POINT('Ctrl Pts',(-70.2309547573815,-23.0658910845433,
12.));
#142415=CARTESIAN_POINT('Ctrl Pts',(-70.2580129087888,-23.0632374143279,
12.));
#142416=CARTESIAN_POINT('Ctrl Pts',(-70.2851042736066,-23.0605555505321,
12.));
#142417=CARTESIAN_POINT('Ctrl Pts',(-70.3122287575335,-23.0578454541104,
12.));
#142418=CARTESIAN_POINT('Ctrl Pts',(-70.3393862652297,-23.0551070854926,
12.));
#142419=CARTESIAN_POINT('Ctrl Pts',(-70.3665767016542,-23.0523404053172,
12.));
#142420=CARTESIAN_POINT('Ctrl Pts',(-70.3937999732267,-23.0495453750763,
12.));
#142421=CARTESIAN_POINT('Ctrl Pts',(-70.4210559889348,-23.0467219577291,
12.));
#142422=CARTESIAN_POINT('Ctrl Pts',(-70.4483446617614,-23.0438701185013,
12.));
#142423=CARTESIAN_POINT('Ctrl Pts',(-70.4756659090209,-23.0409898250756,
12.));
#142424=CARTESIAN_POINT('Ctrl Pts',(-70.4991133648947,-23.0384964376036,
12.));
#142425=CARTESIAN_POINT('Ctrl Pts',(-70.5171075702746,-23.0365694096173,
12.));
#142426=CARTESIAN_POINT('Ctrl Pts',(-70.5296341535556,-23.0352213647765,
12.));
#142427=CARTESIAN_POINT('Ctrl Pts',(-70.5366836381661,-23.0344606623299,
12.));
#142428=CARTESIAN_POINT('Ctrl Pts',(-70.538251407892,-23.0342913834073,
12.));
#142429=CARTESIAN_POINT('',(-66.0656156664138,-23.1372951448024,0.));
#142430=CARTESIAN_POINT('',(-66.0656156664138,-23.1372951448024,0.));
#142431=CARTESIAN_POINT('Ctrl Pts',(-70.538251407892,-23.0342913834073,
0.));
#142432=CARTESIAN_POINT('Ctrl Pts',(-70.5366836381661,-23.0344606623299,
0.));
#142433=CARTESIAN_POINT('Ctrl Pts',(-70.5296341535556,-23.0352213647765,
0.));
#142434=CARTESIAN_POINT('Ctrl Pts',(-70.5171075702746,-23.0365694096173,
0.));
#142435=CARTESIAN_POINT('Ctrl Pts',(-70.4991133648947,-23.0384964376036,
0.));
#142436=CARTESIAN_POINT('Ctrl Pts',(-70.4756659090209,-23.0409898250756,
0.));
#142437=CARTESIAN_POINT('Ctrl Pts',(-70.4483446617614,-23.0438701185013,
0.));
#142438=CARTESIAN_POINT('Ctrl Pts',(-70.4210559889348,-23.0467219577291,
0.));
#142439=CARTESIAN_POINT('Ctrl Pts',(-70.3937999732267,-23.0495453750763,
0.));
#142440=CARTESIAN_POINT('Ctrl Pts',(-70.3665767016542,-23.0523404053172,
0.));
#142441=CARTESIAN_POINT('Ctrl Pts',(-70.3393862652297,-23.0551070854926,
0.));
#142442=CARTESIAN_POINT('Ctrl Pts',(-70.3122287575335,-23.0578454541104,
0.));
#142443=CARTESIAN_POINT('Ctrl Pts',(-70.2851042736066,-23.0605555505321,
0.));
#142444=CARTESIAN_POINT('Ctrl Pts',(-70.2580129087888,-23.0632374143279,
0.));
#142445=CARTESIAN_POINT('Ctrl Pts',(-70.2309547573815,-23.0658910845433,
0.));
#142446=CARTESIAN_POINT('Ctrl Pts',(-70.2039299120488,-23.0685165993691,
0.));
#142447=CARTESIAN_POINT('Ctrl Pts',(-70.1769384645586,-23.071113996544,
0.));
#142448=CARTESIAN_POINT('Ctrl Pts',(-70.1499805062172,-23.0736833135938,
0.));
#142449=CARTESIAN_POINT('Ctrl Pts',(-70.123056128422,-23.0762245881389,
0.));
#142450=CARTESIAN_POINT('Ctrl Pts',(-70.0961654231639,-23.0787378581774,
0.));
#142451=CARTESIAN_POINT('Ctrl Pts',(-70.0693084835373,-23.0812231623765,
0.));
#142452=CARTESIAN_POINT('Ctrl Pts',(-70.0424854035115,-23.0836805399374,
0.));
#142453=CARTESIAN_POINT('Ctrl Pts',(-70.0156962777169,-23.0861100304729,
0.));
#142454=CARTESIAN_POINT('Ctrl Pts',(-69.9889412012143,-23.0885116738798,
0.));
#142455=CARTESIAN_POINT('Ctrl Pts',(-69.9622202692873,-23.0908855102251,
0.));
#142456=CARTESIAN_POINT('Ctrl Pts',(-69.9355335771729,-23.0932315796068,
0.));
#142457=CARTESIAN_POINT('Ctrl Pts',(-69.9088812200713,-23.0955499221558,
0.));
#142458=CARTESIAN_POINT('Ctrl Pts',(-69.8822632932768,-23.0978405781021,
0.));
#142459=CARTESIAN_POINT('Ctrl Pts',(-69.8556798922693,-23.1001035878241,
0.));
#142460=CARTESIAN_POINT('Ctrl Pts',(-69.8291311128118,-23.1023389919051,
0.));
#142461=CARTESIAN_POINT('Ctrl Pts',(-69.8026170510572,-23.1045468311991,
0.));
#142462=CARTESIAN_POINT('Ctrl Pts',(-69.7761378035964,-23.106727146861,
0.));
#142463=CARTESIAN_POINT('Ctrl Pts',(-69.7496934674069,-23.1088799803089,
0.));
#142464=CARTESIAN_POINT('Ctrl Pts',(-69.7232841398197,-23.1110053732046,
0.));
#142465=CARTESIAN_POINT('Ctrl Pts',(-69.6969099184767,-23.1131033674301,
0.));
#142466=CARTESIAN_POINT('Ctrl Pts',(-69.6705709012852,-23.1151740050681,
0.));
#142467=CARTESIAN_POINT('Ctrl Pts',(-69.6442671863765,-23.1172173283859,
0.));
#142468=CARTESIAN_POINT('Ctrl Pts',(-69.6179988721365,-23.1192333798441,
0.));
#142469=CARTESIAN_POINT('Ctrl Pts',(-69.5917660572265,-23.1212222021051,
0.));
#142470=CARTESIAN_POINT('Ctrl Pts',(-69.5655688406052,-23.1231838380452,
0.));
#142471=CARTESIAN_POINT('Ctrl Pts',(-69.539407321546,-23.1251183307676,
0.));
#142472=CARTESIAN_POINT('Ctrl Pts',(-69.5132815996537,-23.1270257236204,
0.));
#142473=CARTESIAN_POINT('Ctrl Pts',(-69.4871917748654,-23.1289060601924,
0.));
#142474=CARTESIAN_POINT('Ctrl Pts',(-69.4611379474484,-23.1307593843061,
0.));
#142475=CARTESIAN_POINT('Ctrl Pts',(-69.4351202179946,-23.1325857400144,
0.));
#142476=CARTESIAN_POINT('Ctrl Pts',(-69.4091386874132,-23.1343851715989,
0.));
#142477=CARTESIAN_POINT('Ctrl Pts',(-69.3831934569182,-23.1361577235709,
0.));
#142478=CARTESIAN_POINT('Ctrl Pts',(-69.3572846280296,-23.1379034406718,
0.));
#142479=CARTESIAN_POINT('Ctrl Pts',(-69.3314123025869,-23.1396223678725,
0.));
#142480=CARTESIAN_POINT('Ctrl Pts',(-69.3055765827546,-23.1413145503762,
0.));
#142481=CARTESIAN_POINT('Ctrl Pts',(-69.2797775710273,-23.142980033622,
0.));
#142482=CARTESIAN_POINT('Ctrl Pts',(-69.254015370231,-23.1446188632931,
0.));
#142483=CARTESIAN_POINT('Ctrl Pts',(-69.2282900835235,-23.1462310853206,
0.));
#142484=CARTESIAN_POINT('Ctrl Pts',(-69.2026018144028,-23.147816745879,
0.));
#142485=CARTESIAN_POINT('Ctrl Pts',(-69.1769506667084,-23.1493758913859,
0.));
#142486=CARTESIAN_POINT('Ctrl Pts',(-69.1513367446231,-23.1509085685032,
0.));
#142487=CARTESIAN_POINT('Ctrl Pts',(-69.1257601526687,-23.152414824141,
0.));
#142488=CARTESIAN_POINT('Ctrl Pts',(-69.1002209957025,-23.1538947054615,
0.));
#142489=CARTESIAN_POINT('Ctrl Pts',(-69.074719378928,-23.1553482598762,
0.));
#142490=CARTESIAN_POINT('Ctrl Pts',(-69.0492554078992,-23.1567755350469,
0.));
#142491=CARTESIAN_POINT('Ctrl Pts',(-69.0238291885245,-23.1581765788869,
0.));
#142492=CARTESIAN_POINT('Ctrl Pts',(-68.9984408270659,-23.1595514395656,
0.));
#142493=CARTESIAN_POINT('Ctrl Pts',(-68.9730904301369,-23.1609001655156,
0.));
#142494=CARTESIAN_POINT('Ctrl Pts',(-68.9477781047106,-23.1622228054291,
0.));
#142495=CARTESIAN_POINT('Ctrl Pts',(-68.9225039581248,-23.1635194082581,
0.));
#142496=CARTESIAN_POINT('Ctrl Pts',(-68.8972680980842,-23.164790023215,
0.));
#142497=CARTESIAN_POINT('Ctrl Pts',(-68.8720706326609,-23.1660346997764,
0.));
#142498=CARTESIAN_POINT('Ctrl Pts',(-68.8469116702898,-23.1672534876889,
0.));
#142499=CARTESIAN_POINT('Ctrl Pts',(-68.8217913197752,-23.1684464369686,
0.));
#142500=CARTESIAN_POINT('Ctrl Pts',(-68.7967096902996,-23.1696135978997,
0.));
#142501=CARTESIAN_POINT('Ctrl Pts',(-68.771666891425,-23.170755021036,0.));
#142502=CARTESIAN_POINT('Ctrl Pts',(-68.746663033096,-23.1718707572043,
0.));
#142503=CARTESIAN_POINT('Ctrl Pts',(-68.7216982256341,-23.172960857511,
0.));
#142504=CARTESIAN_POINT('Ctrl Pts',(-68.696772579744,-23.1740253733417,
0.));
#142505=CARTESIAN_POINT('Ctrl Pts',(-68.6718862065216,-23.1750643563602,
0.));
#142506=CARTESIAN_POINT('Ctrl Pts',(-68.6470392174564,-23.1760778585092,
0.));
#142507=CARTESIAN_POINT('Ctrl Pts',(-68.6222317244341,-23.1770659320138,
0.));
#142508=CARTESIAN_POINT('Ctrl Pts',(-68.597463839733,-23.1780286293875,
0.));
#142509=CARTESIAN_POINT('Ctrl Pts',(-68.5727356760278,-23.1789660034342,
0.));
#142510=CARTESIAN_POINT('Ctrl Pts',(-68.5480473463985,-23.179878107245,
0.));
#142511=CARTESIAN_POINT('Ctrl Pts',(-68.5233989643345,-23.180764994201,
0.));
#142512=CARTESIAN_POINT('Ctrl Pts',(-68.4987906437356,-23.1816267179751,
0.));
#142513=CARTESIAN_POINT('Ctrl Pts',(-68.4742224989098,-23.1824633325385,
0.));
#142514=CARTESIAN_POINT('Ctrl Pts',(-68.4496946445758,-23.183274892163,
0.));
#142515=CARTESIAN_POINT('Ctrl Pts',(-68.4252071958729,-23.1840614514192,
0.));
#142516=CARTESIAN_POINT('Ctrl Pts',(-68.4007602683652,-23.1848230651777,
0.));
#142517=CARTESIAN_POINT('Ctrl Pts',(-68.376353978044,-23.1855597886116,
0.));
#142518=CARTESIAN_POINT('Ctrl Pts',(-68.3519884413246,-23.1862716772031,
0.));
#142519=CARTESIAN_POINT('Ctrl Pts',(-68.3276637750485,-23.1869587867459,
0.));
#142520=CARTESIAN_POINT('Ctrl Pts',(-68.3033800964939,-23.1876211733436,
0.));
#142521=CARTESIAN_POINT('Ctrl Pts',(-68.2791375233795,-23.1882588934107,
0.));
#142522=CARTESIAN_POINT('Ctrl Pts',(-68.2549361738681,-23.1888720036757,
0.));
#142523=CARTESIAN_POINT('Ctrl Pts',(-68.2307761665633,-23.1894605611871,
0.));
#142524=CARTESIAN_POINT('Ctrl Pts',(-68.2066576205116,-23.1900246233165,
0.));
#142525=CARTESIAN_POINT('Ctrl Pts',(-68.1825806552129,-23.1905642477571,
0.));
#142526=CARTESIAN_POINT('Ctrl Pts',(-68.1585453906257,-23.1910794925251,
0.));
#142527=CARTESIAN_POINT('Ctrl Pts',(-68.1345519471695,-23.1915704159623,
0.));
#142528=CARTESIAN_POINT('Ctrl Pts',(-68.110600445723,-23.1920370767426,
0.));
#142529=CARTESIAN_POINT('Ctrl Pts',(-68.0866910076251,-23.1924795338749,
0.));
#142530=CARTESIAN_POINT('Ctrl Pts',(-68.0628237546863,-23.1928978467021,
0.));
#142531=CARTESIAN_POINT('Ctrl Pts',(-68.0389988091933,-23.1932920749023,
0.));
#142532=CARTESIAN_POINT('Ctrl Pts',(-68.0152162939121,-23.1936622784919,
0.));
#142533=CARTESIAN_POINT('Ctrl Pts',(-67.991476332086,-23.1940085178313,
0.));
#142534=CARTESIAN_POINT('Ctrl Pts',(-67.9677790474385,-23.1943308536297,
0.));
#142535=CARTESIAN_POINT('Ctrl Pts',(-67.9441245641842,-23.1946293469427,
0.));
#142536=CARTESIAN_POINT('Ctrl Pts',(-67.9205130070324,-23.1949040591744,
0.));
#142537=CARTESIAN_POINT('Ctrl Pts',(-67.8969445011916,-23.1951550520802,
0.));
#142538=CARTESIAN_POINT('Ctrl Pts',(-67.8734191723667,-23.1953823877734,
0.));
#142539=CARTESIAN_POINT('Ctrl Pts',(-67.8499371467616,-23.1955861287286,
0.));
#142540=CARTESIAN_POINT('Ctrl Pts',(-67.8264985510917,-23.1957663377807,
0.));
#142541=CARTESIAN_POINT('Ctrl Pts',(-67.8031035125887,-23.1959230781269,
0.));
#142542=CARTESIAN_POINT('Ctrl Pts',(-67.7797521590045,-23.1960564133304,
0.));
#142543=CARTESIAN_POINT('Ctrl Pts',(-67.7564446186079,-23.1961664073262,
0.));
#142544=CARTESIAN_POINT('Ctrl Pts',(-67.7331810201883,-23.1962531244245,
0.));
#142545=CARTESIAN_POINT('Ctrl Pts',(-67.7099614930671,-23.1963166293102,
0.));
#142546=CARTESIAN_POINT('Ctrl Pts',(-67.6867861671031,-23.1963569870451,
0.));
#142547=CARTESIAN_POINT('Ctrl Pts',(-67.6636551726964,-23.1963742630715,
0.));
#142548=CARTESIAN_POINT('Ctrl Pts',(-67.6405686407863,-23.1963685232188,
0.));
#142549=CARTESIAN_POINT('Ctrl Pts',(-67.6175267028555,-23.1963398337069,
0.));
#142550=CARTESIAN_POINT('Ctrl Pts',(-67.5945294909426,-23.1962882611453,
0.));
#142551=CARTESIAN_POINT('Ctrl Pts',(-67.5715771376461,-23.196213872536,
0.));
#142552=CARTESIAN_POINT('Ctrl Pts',(-67.5486697761288,-23.1961167352772,
0.));
#142553=CARTESIAN_POINT('Ctrl Pts',(-67.5258075401146,-23.1959969171701,
0.));
#142554=CARTESIAN_POINT('Ctrl Pts',(-67.5029905638949,-23.1958544864215,
0.));
#142555=CARTESIAN_POINT('Ctrl Pts',(-67.4802189823408,-23.195689511644,
0.));
#142556=CARTESIAN_POINT('Ctrl Pts',(-67.4574929309076,-23.195502061859,
0.));
#142557=CARTESIAN_POINT('Ctrl Pts',(-67.4348125456398,-23.1952922065012,
0.));
#142558=CARTESIAN_POINT('Ctrl Pts',(-67.412177963168,-23.1950600154265,
0.));
#142559=CARTESIAN_POINT('Ctrl Pts',(-67.3895893207182,-23.1948055589129,
0.));
#142560=CARTESIAN_POINT('Ctrl Pts',(-67.3670467561212,-23.194528907661,
0.));
#142561=CARTESIAN_POINT('Ctrl Pts',(-67.3445504078176,-23.1942301327978,
0.));
#142562=CARTESIAN_POINT('Ctrl Pts',(-67.3221004148603,-23.1939093058801,
0.));
#142563=CARTESIAN_POINT('Ctrl Pts',(-67.2996969169098,-23.1935664989018,
0.));
#142564=CARTESIAN_POINT('Ctrl Pts',(-67.2773400542477,-23.1932017842953,
0.));
#142565=CARTESIAN_POINT('Ctrl Pts',(-67.2550299677888,-23.1928152349343,
0.));
#142566=CARTESIAN_POINT('Ctrl Pts',(-67.232766799088,-23.1924069241385,
0.));
#142567=CARTESIAN_POINT('Ctrl Pts',(-67.2105506903447,-23.1919769256803,
0.));
#142568=CARTESIAN_POINT('Ctrl Pts',(-67.1883817844038,-23.1915253137924,
0.));
#142569=CARTESIAN_POINT('Ctrl Pts',(-67.1662602247639,-23.1910521631657,
0.));
#142570=CARTESIAN_POINT('Ctrl Pts',(-67.1441861555817,-23.1905575489505,
0.));
#142571=CARTESIAN_POINT('Ctrl Pts',(-67.1221597216741,-23.1900415467574,
0.));
#142572=CARTESIAN_POINT('Ctrl Pts',(-67.1001810685143,-23.1895042326627,
0.));
#142573=CARTESIAN_POINT('Ctrl Pts',(-67.0782503422305,-23.1889456832119,
0.));
#142574=CARTESIAN_POINT('Ctrl Pts',(-67.0563676896325,-23.1883659754271,
0.));
#142575=CARTESIAN_POINT('Ctrl Pts',(-67.0345332582306,-23.1877651868158,
0.));
#142576=CARTESIAN_POINT('Ctrl Pts',(-67.0127471962501,-23.1871433953793,
0.));
#142577=CARTESIAN_POINT('Ctrl Pts',(-66.9910096526462,-23.1865006796284,
0.));
#142578=CARTESIAN_POINT('Ctrl Pts',(-66.9693207771031,-23.1858371185842,
0.));
#142579=CARTESIAN_POINT('Ctrl Pts',(-66.9476807200203,-23.1851527917657,
0.));
#142580=CARTESIAN_POINT('Ctrl Pts',(-66.9260896324949,-23.1844477791814,
0.));
#142581=CARTESIAN_POINT('Ctrl Pts',(-66.9045476663063,-23.1837221613235,
0.));
#142582=CARTESIAN_POINT('Ctrl Pts',(-66.8830549738795,-23.1829760191591,
0.));
#142583=CARTESIAN_POINT('Ctrl Pts',(-66.8616117083331,-23.1822094341517,
0.));
#142584=CARTESIAN_POINT('Ctrl Pts',(-66.8402180235566,-23.1814224882954,
0.));
#142585=CARTESIAN_POINT('Ctrl Pts',(-66.8188740742727,-23.1806152641475,
0.));
#142586=CARTESIAN_POINT('Ctrl Pts',(-66.7975800161,-23.1797878448639,0.));
#142587=CARTESIAN_POINT('Ctrl Pts',(-66.776336005612,-23.1789403142366,
0.));
#142588=CARTESIAN_POINT('Ctrl Pts',(-66.7551422002204,-23.17807275663,0.));
#142589=CARTESIAN_POINT('Ctrl Pts',(-66.7339987580427,-23.1771852569131,
0.));
#142590=CARTESIAN_POINT('Ctrl Pts',(-66.7129058377896,-23.1762779004044,
0.));
#142591=CARTESIAN_POINT('Ctrl Pts',(-66.6918635985972,-23.1753507727939,
0.));
#142592=CARTESIAN_POINT('Ctrl Pts',(-66.6708722000079,-23.1744039601382,
0.));
#142593=CARTESIAN_POINT('Ctrl Pts',(-66.6499318023473,-23.1734375490431,
0.));
#142594=CARTESIAN_POINT('Ctrl Pts',(-66.6290425670548,-23.1724516268302,
0.));
#142595=CARTESIAN_POINT('Ctrl Pts',(-66.6082046569644,-23.1714462816789,
0.));
#142596=CARTESIAN_POINT('Ctrl Pts',(-66.5874182367563,-23.1704216028614,
0.));
#142597=CARTESIAN_POINT('Ctrl Pts',(-66.5666834726454,-23.1693776805866,
0.));
#142598=CARTESIAN_POINT('Ctrl Pts',(-66.5460005315376,-23.1683146055726,
0.));
#142599=CARTESIAN_POINT('Ctrl Pts',(-66.5253695803205,-23.1672324686926,
0.));
#142600=CARTESIAN_POINT('Ctrl Pts',(-66.5047907851348,-23.1661313606132,
0.));
#142601=CARTESIAN_POINT('Ctrl Pts',(-66.4842643105311,-23.1650113713808,
0.));
#142602=CARTESIAN_POINT('Ctrl Pts',(-66.4637903210727,-23.1638725912195,
0.));
#142603=CARTESIAN_POINT('Ctrl Pts',(-66.4433689832478,-23.1627151114883,
0.));
#142604=CARTESIAN_POINT('Ctrl Pts',(-66.4230004670278,-23.1615390254632,
0.));
#142605=CARTESIAN_POINT('Ctrl Pts',(-66.4026849481232,-23.160344429474,
0.));
#142606=CARTESIAN_POINT('Ctrl Pts',(-66.3824226081801,-23.1591314230083,
0.));
#142607=CARTESIAN_POINT('Ctrl Pts',(-66.3622136300654,-23.1579001063424,
0.));
#142608=CARTESIAN_POINT('Ctrl Pts',(-66.3420581937147,-23.1566505784621,
0.));
#142609=CARTESIAN_POINT('Ctrl Pts',(-66.3219564725184,-23.1553829352539,
0.));
#142610=CARTESIAN_POINT('Ctrl Pts',(-66.3019086275444,-23.1540972666191,
0.));
#142611=CARTESIAN_POINT('Ctrl Pts',(-66.281914813114,-23.1527936592651,
0.));
#142612=CARTESIAN_POINT('Ctrl Pts',(-66.2619751878793,-23.1514722022503,
0.));
#142613=CARTESIAN_POINT('Ctrl Pts',(-66.2420899237318,-23.1501329914488,
0.));
#142614=CARTESIAN_POINT('Ctrl Pts',(-66.2222592165398,-23.1487761349298,
0.));
#142615=CARTESIAN_POINT('Ctrl Pts',(-66.2024832934733,-23.147401756643,
0.));
#142616=CARTESIAN_POINT('Ctrl Pts',(-66.1827623902755,-23.1460099850704,
0.));
#142617=CARTESIAN_POINT('Ctrl Pts',(-66.163096729667,-23.1446009424872,
0.));
#142618=CARTESIAN_POINT('Ctrl Pts',(-66.14348650151,-23.1431747350127,0.));
#142619=CARTESIAN_POINT('Ctrl Pts',(-66.1239318368803,-23.1417314398501,
0.));
#142620=CARTESIAN_POINT('Ctrl Pts',(-66.1044328067739,-23.140271103958,
0.));
#142621=CARTESIAN_POINT('Ctrl Pts',(-66.0888781152779,-23.1390892229923,
0.));
#142622=CARTESIAN_POINT('Ctrl Pts',(-66.0772371487475,-23.1381951597491,
0.));
#142623=CARTESIAN_POINT('Ctrl Pts',(-66.0694876382212,-23.1375957166138,
0.));
#142624=CARTESIAN_POINT('Ctrl Pts',(-66.0656156664138,-23.1372951448024,
0.));
#142625=CARTESIAN_POINT('Ctrl Pts',(-72.5962692526112,-16.7341474417544,
0.));
#142626=CARTESIAN_POINT('Ctrl Pts',(-72.5962692526112,-16.7341474417544,
12.));
#142627=CARTESIAN_POINT('Ctrl Pts',(-72.5907910746008,-16.7352885767485,
0.));
#142628=CARTESIAN_POINT('Ctrl Pts',(-72.5907910746008,-16.7352885767485,
12.));
#142629=CARTESIAN_POINT('Ctrl Pts',(-72.5798376087774,-16.7375676985344,
0.));
#142630=CARTESIAN_POINT('Ctrl Pts',(-72.5798376087774,-16.7375676985344,
12.));
#142631=CARTESIAN_POINT('Ctrl Pts',(-72.5634160806351,-16.7409769366072,
0.));
#142632=CARTESIAN_POINT('Ctrl Pts',(-72.5634160806351,-16.7409769366072,
12.));
#142633=CARTESIAN_POINT('Ctrl Pts',(-72.5415380516636,-16.7455036973866,
0.));
#142634=CARTESIAN_POINT('Ctrl Pts',(-72.5415380516636,-16.7455036973866,
12.));
#142635=CARTESIAN_POINT('Ctrl Pts',(-72.514219427383,-16.7511306618915,
0.));
#142636=CARTESIAN_POINT('Ctrl Pts',(-72.514219427383,-16.7511306618915,
12.));
#142637=CARTESIAN_POINT('Ctrl Pts',(-72.4869297342427,-16.7567261380687,
0.));
#142638=CARTESIAN_POINT('Ctrl Pts',(-72.4869297342427,-16.7567261380687,
12.));
#142639=CARTESIAN_POINT('Ctrl Pts',(-72.4596690055437,-16.7622901280758,
0.));
#142640=CARTESIAN_POINT('Ctrl Pts',(-72.4596690055437,-16.7622901280758,
12.));
#142641=CARTESIAN_POINT('Ctrl Pts',(-72.4324372916746,-16.7678226404162,
0.));
#142642=CARTESIAN_POINT('Ctrl Pts',(-72.4324372916746,-16.7678226404162,
12.));
#142643=CARTESIAN_POINT('Ctrl Pts',(-72.4052346647799,-16.7733236932135,
0.));
#142644=CARTESIAN_POINT('Ctrl Pts',(-72.4052346647799,-16.7733236932135,
12.));
#142645=CARTESIAN_POINT('Ctrl Pts',(-72.3780612167786,-16.7787933137498,
0.));
#142646=CARTESIAN_POINT('Ctrl Pts',(-72.3780612167786,-16.7787933137498,
12.));
#142647=CARTESIAN_POINT('Ctrl Pts',(-72.3509170522838,-16.7842315351362,
0.));
#142648=CARTESIAN_POINT('Ctrl Pts',(-72.3509170522838,-16.7842315351362,
12.));
#142649=CARTESIAN_POINT('Ctrl Pts',(-72.3238022829223,-16.7896383937822,
0.));
#142650=CARTESIAN_POINT('Ctrl Pts',(-72.3238022829223,-16.7896383937822,
12.));
#142651=CARTESIAN_POINT('Ctrl Pts',(-72.2967170212353,-16.7950139266121,
0.));
#142652=CARTESIAN_POINT('Ctrl Pts',(-72.2967170212353,-16.7950139266121,
12.));
#142653=CARTESIAN_POINT('Ctrl Pts',(-72.2696613743782,-16.8003581682248,
0.));
#142654=CARTESIAN_POINT('Ctrl Pts',(-72.2696613743782,-16.8003581682248,
12.));
#142655=CARTESIAN_POINT('Ctrl Pts',(-72.2426354390213,-16.8056711485821,
0.));
#142656=CARTESIAN_POINT('Ctrl Pts',(-72.2426354390213,-16.8056711485821,
12.));
#142657=CARTESIAN_POINT('Ctrl Pts',(-72.2156393048975,-16.8109528945896,
0.));
#142658=CARTESIAN_POINT('Ctrl Pts',(-72.2156393048975,-16.8109528945896,
12.));
#142659=CARTESIAN_POINT('Ctrl Pts',(-72.1886730573452,-16.8162034312269,
0.));
#142660=CARTESIAN_POINT('Ctrl Pts',(-72.1886730573452,-16.8162034312269,
12.));
#142661=CARTESIAN_POINT('Ctrl Pts',(-72.1617367803235,-16.8214227828942,
0.));
#142662=CARTESIAN_POINT('Ctrl Pts',(-72.1617367803235,-16.8214227828942,
12.));
#142663=CARTESIAN_POINT('Ctrl Pts',(-72.13483055902,-16.8266109745795,0.));
#142664=CARTESIAN_POINT('Ctrl Pts',(-72.13483055902,-16.8266109745795,12.));
#142665=CARTESIAN_POINT('Ctrl Pts',(-72.1079544831513,-16.8317680333404,
0.));
#142666=CARTESIAN_POINT('Ctrl Pts',(-72.1079544831513,-16.8317680333404,
12.));
#142667=CARTESIAN_POINT('Ctrl Pts',(-72.0811086466121,-16.8368939881446,
0.));
#142668=CARTESIAN_POINT('Ctrl Pts',(-72.0811086466121,-16.8368939881446,
12.));
#142669=CARTESIAN_POINT('Ctrl Pts',(-72.0542931459825,-16.8419888691976,
0.));
#142670=CARTESIAN_POINT('Ctrl Pts',(-72.0542931459825,-16.8419888691976,
12.));
#142671=CARTESIAN_POINT('Ctrl Pts',(-72.0275080793727,-16.8470527074275,
0.));
#142672=CARTESIAN_POINT('Ctrl Pts',(-72.0275080793727,-16.8470527074275,
12.));
#142673=CARTESIAN_POINT('Ctrl Pts',(-72.0007535452081,-16.8520855339446,
0.));
#142674=CARTESIAN_POINT('Ctrl Pts',(-72.0007535452081,-16.8520855339446,
12.));
#142675=CARTESIAN_POINT('Ctrl Pts',(-71.9740296408347,-16.8570873794269,
0.));
#142676=CARTESIAN_POINT('Ctrl Pts',(-71.9740296408347,-16.8570873794269,
12.));
#142677=CARTESIAN_POINT('Ctrl Pts',(-71.9473364618922,-16.8620582738437,
0.));
#142678=CARTESIAN_POINT('Ctrl Pts',(-71.9473364618922,-16.8620582738437,
12.));
#142679=CARTESIAN_POINT('Ctrl Pts',(-71.9206741030887,-16.866998246792,
0.));
#142680=CARTESIAN_POINT('Ctrl Pts',(-71.9206741030887,-16.866998246792,
12.));
#142681=CARTESIAN_POINT('Ctrl Pts',(-71.8940426586534,-16.871907327697,
0.));
#142682=CARTESIAN_POINT('Ctrl Pts',(-71.8940426586534,-16.871907327697,
12.));
#142683=CARTESIAN_POINT('Ctrl Pts',(-71.8674422229149,-16.87678554607,0.));
#142684=CARTESIAN_POINT('Ctrl Pts',(-71.8674422229149,-16.87678554607,12.));
#142685=CARTESIAN_POINT('Ctrl Pts',(-71.8408728908258,-16.881632931747,
0.));
#142686=CARTESIAN_POINT('Ctrl Pts',(-71.8408728908258,-16.881632931747,
12.));
#142687=CARTESIAN_POINT('Ctrl Pts',(-71.8143347584962,-16.8864495151344,
0.));
#142688=CARTESIAN_POINT('Ctrl Pts',(-71.8143347584962,-16.8864495151344,
12.));
#142689=CARTESIAN_POINT('Ctrl Pts',(-71.7878279229546,-16.8912353270942,
0.));
#142690=CARTESIAN_POINT('Ctrl Pts',(-71.7878279229546,-16.8912353270942,
12.));
#142691=CARTESIAN_POINT('Ctrl Pts',(-71.7613524819235,-16.8959903988409,
0.));
#142692=CARTESIAN_POINT('Ctrl Pts',(-71.7613524819235,-16.8959903988409,
12.));
#142693=CARTESIAN_POINT('Ctrl Pts',(-71.7349085335796,-16.9007147618344,
0.));
#142694=CARTESIAN_POINT('Ctrl Pts',(-71.7349085335796,-16.9007147618344,
12.));
#142695=CARTESIAN_POINT('Ctrl Pts',(-71.7084961763357,-16.9054084476847,
0.));
#142696=CARTESIAN_POINT('Ctrl Pts',(-71.7084961763357,-16.9054084476847,
12.));
#142697=CARTESIAN_POINT('Ctrl Pts',(-71.6821155085612,-16.9100714880368,
0.));
#142698=CARTESIAN_POINT('Ctrl Pts',(-71.6821155085612,-16.9100714880368,
12.));
#142699=CARTESIAN_POINT('Ctrl Pts',(-71.6557666285917,-16.9147039145717,
0.));
#142700=CARTESIAN_POINT('Ctrl Pts',(-71.6557666285917,-16.9147039145717,
12.));
#142701=CARTESIAN_POINT('Ctrl Pts',(-71.6294496348652,-16.9193057590607,
0.));
#142702=CARTESIAN_POINT('Ctrl Pts',(-71.6294496348652,-16.9193057590607,
12.));
#142703=CARTESIAN_POINT('Ctrl Pts',(-71.6031646260174,-16.9238770534071,
0.));
#142704=CARTESIAN_POINT('Ctrl Pts',(-71.6031646260174,-16.9238770534071,
12.));
#142705=CARTESIAN_POINT('Ctrl Pts',(-71.5769117009842,-16.9284178296933,
0.));
#142706=CARTESIAN_POINT('Ctrl Pts',(-71.5769117009842,-16.9284178296933,
12.));
#142707=CARTESIAN_POINT('Ctrl Pts',(-71.5506909591128,-16.9329281202377,
0.));
#142708=CARTESIAN_POINT('Ctrl Pts',(-71.5506909591128,-16.9329281202377,
12.));
#142709=CARTESIAN_POINT('Ctrl Pts',(-71.5245025002139,-16.9374079576201,
0.));
#142710=CARTESIAN_POINT('Ctrl Pts',(-71.5245025002139,-16.9374079576201,
12.));
#142711=CARTESIAN_POINT('Ctrl Pts',(-71.4983464245055,-16.9418573746488,
0.));
#142712=CARTESIAN_POINT('Ctrl Pts',(-71.4983464245055,-16.9418573746488,
12.));
#142713=CARTESIAN_POINT('Ctrl Pts',(-71.4722228325794,-16.9462764043443,
0.));
#142714=CARTESIAN_POINT('Ctrl Pts',(-71.4722228325794,-16.9462764043443,
12.));
#142715=CARTESIAN_POINT('Ctrl Pts',(-71.4461318253563,-16.9506650799189,
0.));
#142716=CARTESIAN_POINT('Ctrl Pts',(-71.4461318253563,-16.9506650799189,
12.));
#142717=CARTESIAN_POINT('Ctrl Pts',(-71.4200735040384,-16.955023434762,
0.));
#142718=CARTESIAN_POINT('Ctrl Pts',(-71.4200735040384,-16.955023434762,
12.));
#142719=CARTESIAN_POINT('Ctrl Pts',(-71.3940479700677,-16.9593515024276,
0.));
#142720=CARTESIAN_POINT('Ctrl Pts',(-71.3940479700677,-16.9593515024276,
12.));
#142721=CARTESIAN_POINT('Ctrl Pts',(-71.3680553251562,-16.9636493166397,
0.));
#142722=CARTESIAN_POINT('Ctrl Pts',(-71.3680553251562,-16.9636493166397,
12.));
#142723=CARTESIAN_POINT('Ctrl Pts',(-71.3420956713082,-16.9679169112994,
0.));
#142724=CARTESIAN_POINT('Ctrl Pts',(-71.3420956713082,-16.9679169112994,
12.));
#142725=CARTESIAN_POINT('Ctrl Pts',(-71.3161691108427,-16.9721543204951,
0.));
#142726=CARTESIAN_POINT('Ctrl Pts',(-71.3161691108427,-16.9721543204951,
12.));
#142727=CARTESIAN_POINT('Ctrl Pts',(-71.290275746412,-16.9763615785136,
0.));
#142728=CARTESIAN_POINT('Ctrl Pts',(-71.290275746412,-16.9763615785136,
12.));
#142729=CARTESIAN_POINT('Ctrl Pts',(-71.2644156810198,-16.9805387198571,
0.));
#142730=CARTESIAN_POINT('Ctrl Pts',(-71.2644156810198,-16.9805387198571,
12.));
#142731=CARTESIAN_POINT('Ctrl Pts',(-71.2385890180221,-16.9846857792383,
0.));
#142732=CARTESIAN_POINT('Ctrl Pts',(-71.2385890180221,-16.9846857792383,
12.));
#142733=CARTESIAN_POINT('Ctrl Pts',(-71.212795861124,-16.9888027915742,
0.));
#142734=CARTESIAN_POINT('Ctrl Pts',(-71.212795861124,-16.9888027915742,
12.));
#142735=CARTESIAN_POINT('Ctrl Pts',(-71.187036314374,-16.9928897919828,
0.));
#142736=CARTESIAN_POINT('Ctrl Pts',(-71.187036314374,-16.9928897919828,
12.));
#142737=CARTESIAN_POINT('Ctrl Pts',(-71.1613104821568,-16.9969468157824,
0.));
#142738=CARTESIAN_POINT('Ctrl Pts',(-71.1613104821568,-16.9969468157824,
12.));
#142739=CARTESIAN_POINT('Ctrl Pts',(-71.1356184691806,-17.0009738984935,
0.));
#142740=CARTESIAN_POINT('Ctrl Pts',(-71.1356184691806,-17.0009738984935,
12.));
#142741=CARTESIAN_POINT('Ctrl Pts',(-71.1099603804786,-17.0049710758393,
0.));
#142742=CARTESIAN_POINT('Ctrl Pts',(-71.1099603804786,-17.0049710758393,
12.));
#142743=CARTESIAN_POINT('Ctrl Pts',(-71.0843363214221,-17.0089383837437,
0.));
#142744=CARTESIAN_POINT('Ctrl Pts',(-71.0843363214221,-17.0089383837437,
12.));
#142745=CARTESIAN_POINT('Ctrl Pts',(-71.0587463977268,-17.0128758583334,
0.));
#142746=CARTESIAN_POINT('Ctrl Pts',(-71.0587463977268,-17.0128758583334,
12.));
#142747=CARTESIAN_POINT('Ctrl Pts',(-71.0331907154574,-17.0167835359419,
0.));
#142748=CARTESIAN_POINT('Ctrl Pts',(-71.0331907154574,-17.0167835359419,
12.));
#142749=CARTESIAN_POINT('Ctrl Pts',(-71.0076693810301,-17.0206614531166,
0.));
#142750=CARTESIAN_POINT('Ctrl Pts',(-71.0076693810301,-17.0206614531166,
12.));
#142751=CARTESIAN_POINT('Ctrl Pts',(-70.9821825012136,-17.0245096466229,
0.));
#142752=CARTESIAN_POINT('Ctrl Pts',(-70.9821825012136,-17.0245096466229,
12.));
#142753=CARTESIAN_POINT('Ctrl Pts',(-70.956730183136,-17.0283281534392,
0.));
#142754=CARTESIAN_POINT('Ctrl Pts',(-70.956730183136,-17.0283281534392,
12.));
#142755=CARTESIAN_POINT('Ctrl Pts',(-70.9313125342876,-17.0321170107564,
0.));
#142756=CARTESIAN_POINT('Ctrl Pts',(-70.9313125342876,-17.0321170107564,
12.));
#142757=CARTESIAN_POINT('Ctrl Pts',(-70.9059296625214,-17.0358762559786,
0.));
#142758=CARTESIAN_POINT('Ctrl Pts',(-70.9059296625214,-17.0358762559786,
12.));
#142759=CARTESIAN_POINT('Ctrl Pts',(-70.8805816760501,-17.0396059267277,
0.));
#142760=CARTESIAN_POINT('Ctrl Pts',(-70.8805816760501,-17.0396059267277,
12.));
#142761=CARTESIAN_POINT('Ctrl Pts',(-70.8552686834423,-17.0433060608474,
0.));
#142762=CARTESIAN_POINT('Ctrl Pts',(-70.8552686834423,-17.0433060608474,
12.));
#142763=CARTESIAN_POINT('Ctrl Pts',(-70.8299907936334,-17.0469766964001,
0.));
#142764=CARTESIAN_POINT('Ctrl Pts',(-70.8299907936334,-17.0469766964001,
12.));
#142765=CARTESIAN_POINT('Ctrl Pts',(-70.8047481159298,-17.0506178716661,
0.));
#142766=CARTESIAN_POINT('Ctrl Pts',(-70.8047481159298,-17.0506178716661,
12.));
#142767=CARTESIAN_POINT('Ctrl Pts',(-70.7795407600127,-17.0542296251462,
0.));
#142768=CARTESIAN_POINT('Ctrl Pts',(-70.7795407600127,-17.0542296251462,
12.));
#142769=CARTESIAN_POINT('Ctrl Pts',(-70.754368835938,-17.0578119955651,
0.));
#142770=CARTESIAN_POINT('Ctrl Pts',(-70.754368835938,-17.0578119955651,
12.));
#142771=CARTESIAN_POINT('Ctrl Pts',(-70.7292324541348,-17.0613650218788,
0.));
#142772=CARTESIAN_POINT('Ctrl Pts',(-70.7292324541348,-17.0613650218788,
12.));
#142773=CARTESIAN_POINT('Ctrl Pts',(-70.7041317254127,-17.0648887432714,
0.));
#142774=CARTESIAN_POINT('Ctrl Pts',(-70.7041317254127,-17.0648887432714,
12.));
#142775=CARTESIAN_POINT('Ctrl Pts',(-70.6790667609678,-17.0683831991532,
0.));
#142776=CARTESIAN_POINT('Ctrl Pts',(-70.6790667609678,-17.0683831991532,
12.));
#142777=CARTESIAN_POINT('Ctrl Pts',(-70.6540376723839,-17.0718484291623,
0.));
#142778=CARTESIAN_POINT('Ctrl Pts',(-70.6540376723839,-17.0718484291623,
12.));
#142779=CARTESIAN_POINT('Ctrl Pts',(-70.6290445716341,-17.0752844731679,
0.));
#142780=CARTESIAN_POINT('Ctrl Pts',(-70.6290445716341,-17.0752844731679,
12.));
#142781=CARTESIAN_POINT('Ctrl Pts',(-70.6040875710762,-17.0786913712766,
0.));
#142782=CARTESIAN_POINT('Ctrl Pts',(-70.6040875710762,-17.0786913712766,
12.));
#142783=CARTESIAN_POINT('Ctrl Pts',(-70.5791667834599,-17.0820691638314,
0.));
#142784=CARTESIAN_POINT('Ctrl Pts',(-70.5791667834599,-17.0820691638314,
12.));
#142785=CARTESIAN_POINT('Ctrl Pts',(-70.5542823219346,-17.085417891409,
0.));
#142786=CARTESIAN_POINT('Ctrl Pts',(-70.5542823219346,-17.085417891409,
12.));
#142787=CARTESIAN_POINT('Ctrl Pts',(-70.5294343000516,-17.0887375948221,
0.));
#142788=CARTESIAN_POINT('Ctrl Pts',(-70.5294343000516,-17.0887375948221,
12.));
#142789=CARTESIAN_POINT('Ctrl Pts',(-70.5046228317669,-17.0920283151217,
0.));
#142790=CARTESIAN_POINT('Ctrl Pts',(-70.5046228317669,-17.0920283151217,
12.));
#142791=CARTESIAN_POINT('Ctrl Pts',(-70.4798480314364,-17.0952900936044,
0.));
#142792=CARTESIAN_POINT('Ctrl Pts',(-70.4798480314364,-17.0952900936044,
12.));
#142793=CARTESIAN_POINT('Ctrl Pts',(-70.4551100138221,-17.098522971812,
0.));
#142794=CARTESIAN_POINT('Ctrl Pts',(-70.4551100138221,-17.098522971812,
12.));
#142795=CARTESIAN_POINT('Ctrl Pts',(-70.4304088940998,-17.1017269915289,
0.));
#142796=CARTESIAN_POINT('Ctrl Pts',(-70.4304088940998,-17.1017269915289,
12.));
#142797=CARTESIAN_POINT('Ctrl Pts',(-70.4057447878621,-17.1049021947833,
0.));
#142798=CARTESIAN_POINT('Ctrl Pts',(-70.4057447878621,-17.1049021947833,
12.));
#142799=CARTESIAN_POINT('Ctrl Pts',(-70.3811178111206,-17.1080486238499,
0.));
#142800=CARTESIAN_POINT('Ctrl Pts',(-70.3811178111206,-17.1080486238499,
12.));
#142801=CARTESIAN_POINT('Ctrl Pts',(-70.356528080303,-17.111166321257,0.));
#142802=CARTESIAN_POINT('Ctrl Pts',(-70.356528080303,-17.111166321257,12.));
#142803=CARTESIAN_POINT('Ctrl Pts',(-70.3319757122576,-17.1142553297869,
0.));
#142804=CARTESIAN_POINT('Ctrl Pts',(-70.3319757122576,-17.1142553297869,
12.));
#142805=CARTESIAN_POINT('Ctrl Pts',(-70.3074608242613,-17.1173156924733,
0.));
#142806=CARTESIAN_POINT('Ctrl Pts',(-70.3074608242613,-17.1173156924733,
12.));
#142807=CARTESIAN_POINT('Ctrl Pts',(-70.2829835340239,-17.1203474526031,
0.));
#142808=CARTESIAN_POINT('Ctrl Pts',(-70.2829835340239,-17.1203474526031,
12.));
#142809=CARTESIAN_POINT('Ctrl Pts',(-70.2585439596899,-17.1233506537176,
0.));
#142810=CARTESIAN_POINT('Ctrl Pts',(-70.2585439596899,-17.1233506537176,
12.));
#142811=CARTESIAN_POINT('Ctrl Pts',(-70.2341422198362,-17.1263253396202,
0.));
#142812=CARTESIAN_POINT('Ctrl Pts',(-70.2341422198362,-17.1263253396202,
12.));
#142813=CARTESIAN_POINT('Ctrl Pts',(-70.2097784334749,-17.1292715543779,
0.));
#142814=CARTESIAN_POINT('Ctrl Pts',(-70.2097784334749,-17.1292715543779,
12.));
#142815=CARTESIAN_POINT('Ctrl Pts',(-70.1854527200636,-17.1321893423183,
0.));
#142816=CARTESIAN_POINT('Ctrl Pts',(-70.1854527200636,-17.1321893423183,
12.));
#142817=CARTESIAN_POINT('Ctrl Pts',(-70.1611651995085,-17.1350787480313,
0.));
#142818=CARTESIAN_POINT('Ctrl Pts',(-70.1611651995085,-17.1350787480313,
12.));
#142819=CARTESIAN_POINT('Ctrl Pts',(-70.1369159921686,-17.1379398163708,
0.));
#142820=CARTESIAN_POINT('Ctrl Pts',(-70.1369159921686,-17.1379398163708,
12.));
#142821=CARTESIAN_POINT('Ctrl Pts',(-70.1127052188515,-17.1407725924615,
0.));
#142822=CARTESIAN_POINT('Ctrl Pts',(-70.1127052188515,-17.1407725924615,
12.));
#142823=CARTESIAN_POINT('Ctrl Pts',(-70.0885330008169,-17.1435771217015,
0.));
#142824=CARTESIAN_POINT('Ctrl Pts',(-70.0885330008169,-17.1435771217015,
12.));
#142825=CARTESIAN_POINT('Ctrl Pts',(-70.0643994597865,-17.1463534497592,
0.));
#142826=CARTESIAN_POINT('Ctrl Pts',(-70.0643994597865,-17.1463534497592,
12.));
#142827=CARTESIAN_POINT('Ctrl Pts',(-70.040304717948,-17.1491016225748,
0.));
#142828=CARTESIAN_POINT('Ctrl Pts',(-70.040304717948,-17.1491016225748,
12.));
#142829=CARTESIAN_POINT('Ctrl Pts',(-70.0162488979586,-17.1518216863624,
0.));
#142830=CARTESIAN_POINT('Ctrl Pts',(-70.0162488979586,-17.1518216863624,
12.));
#142831=CARTESIAN_POINT('Ctrl Pts',(-69.9922321229428,-17.1545136876161,
0.));
#142832=CARTESIAN_POINT('Ctrl Pts',(-69.9922321229428,-17.1545136876161,
12.));
#142833=CARTESIAN_POINT('Ctrl Pts',(-69.9682545164942,-17.157177673114,
0.));
#142834=CARTESIAN_POINT('Ctrl Pts',(-69.9682545164942,-17.157177673114,
12.));
#142835=CARTESIAN_POINT('Ctrl Pts',(-69.9443162026865,-17.1598136899144,
0.));
#142836=CARTESIAN_POINT('Ctrl Pts',(-69.9443162026865,-17.1598136899144,
12.));
#142837=CARTESIAN_POINT('Ctrl Pts',(-69.9204173060779,-17.1624217853577,
0.));
#142838=CARTESIAN_POINT('Ctrl Pts',(-69.9204173060779,-17.1624217853577,
12.));
#142839=CARTESIAN_POINT('Ctrl Pts',(-69.8965579517147,-17.1650020070686,
0.));
#142840=CARTESIAN_POINT('Ctrl Pts',(-69.8965579517147,-17.1650020070686,
12.));
#142841=CARTESIAN_POINT('Ctrl Pts',(-69.8727382651292,-17.1675544029621,
0.));
#142842=CARTESIAN_POINT('Ctrl Pts',(-69.8727382651292,-17.1675544029621,
12.));
#142843=CARTESIAN_POINT('Ctrl Pts',(-69.8489583723417,-17.1700790212476,
0.));
#142844=CARTESIAN_POINT('Ctrl Pts',(-69.8489583723417,-17.1700790212476,
12.));
#142845=CARTESIAN_POINT('Ctrl Pts',(-69.8252183998713,-17.1725759104254,
0.));
#142846=CARTESIAN_POINT('Ctrl Pts',(-69.8252183998713,-17.1725759104254,
12.));
#142847=CARTESIAN_POINT('Ctrl Pts',(-69.8015184747404,-17.1750451192887,
0.));
#142848=CARTESIAN_POINT('Ctrl Pts',(-69.8015184747404,-17.1750451192887,
12.));
#142849=CARTESIAN_POINT('Ctrl Pts',(-69.7778587244788,-17.1774866969256,
0.));
#142850=CARTESIAN_POINT('Ctrl Pts',(-69.7778587244788,-17.1774866969256,
12.));
#142851=CARTESIAN_POINT('Ctrl Pts',(-69.7542392771216,-17.1799006927255,
0.));
#142852=CARTESIAN_POINT('Ctrl Pts',(-69.7542392771216,-17.1799006927255,
12.));
#142853=CARTESIAN_POINT('Ctrl Pts',(-69.7306602612125,-17.1822871563834,
0.));
#142854=CARTESIAN_POINT('Ctrl Pts',(-69.7306602612125,-17.1822871563834,
12.));
#142855=CARTESIAN_POINT('Ctrl Pts',(-69.7071218058149,-17.1846461378966,
0.));
#142856=CARTESIAN_POINT('Ctrl Pts',(-69.7071218058149,-17.1846461378966,
12.));
#142857=CARTESIAN_POINT('Ctrl Pts',(-69.6836240405151,-17.1869776875663,
0.));
#142858=CARTESIAN_POINT('Ctrl Pts',(-69.6836240405151,-17.1869776875663,
12.));
#142859=CARTESIAN_POINT('Ctrl Pts',(-69.6601670954277,-17.1892818560004,
0.));
#142860=CARTESIAN_POINT('Ctrl Pts',(-69.6601670954277,-17.1892818560004,
12.));
#142861=CARTESIAN_POINT('Ctrl Pts',(-69.6367511011927,-17.1915586941198,
0.));
#142862=CARTESIAN_POINT('Ctrl Pts',(-69.6367511011927,-17.1915586941198,
12.));
#142863=CARTESIAN_POINT('Ctrl Pts',(-69.6133761889787,-17.1938082531619,
0.));
#142864=CARTESIAN_POINT('Ctrl Pts',(-69.6133761889787,-17.1938082531619,
12.));
#142865=CARTESIAN_POINT('Ctrl Pts',(-69.5900424904954,-17.1960305846787,
0.));
#142866=CARTESIAN_POINT('Ctrl Pts',(-69.5900424904954,-17.1960305846787,
12.));
#142867=CARTESIAN_POINT('Ctrl Pts',(-69.5667501379984,-17.198225740538,
0.));
#142868=CARTESIAN_POINT('Ctrl Pts',(-69.5667501379984,-17.198225740538,
12.));
#142869=CARTESIAN_POINT('Ctrl Pts',(-69.5434992642932,-17.2003937729266,
0.));
#142870=CARTESIAN_POINT('Ctrl Pts',(-69.5434992642932,-17.2003937729266,
12.));
#142871=CARTESIAN_POINT('Ctrl Pts',(-69.5202900027329,-17.2025347343568,
0.));
#142872=CARTESIAN_POINT('Ctrl Pts',(-69.5202900027329,-17.2025347343568,
12.));
#142873=CARTESIAN_POINT('Ctrl Pts',(-69.497122487222,-17.2046486776697,
0.));
#142874=CARTESIAN_POINT('Ctrl Pts',(-69.497122487222,-17.2046486776697,
12.));
#142875=CARTESIAN_POINT('Ctrl Pts',(-69.4739968522271,-17.2067356560326,
0.));
#142876=CARTESIAN_POINT('Ctrl Pts',(-69.4739968522271,-17.2067356560326,
12.));
#142877=CARTESIAN_POINT('Ctrl Pts',(-69.4509132327836,-17.208795722942,
0.));
#142878=CARTESIAN_POINT('Ctrl Pts',(-69.4509132327836,-17.208795722942,
12.));
#142879=CARTESIAN_POINT('Ctrl Pts',(-69.4278717644989,-17.2108289322258,
0.));
#142880=CARTESIAN_POINT('Ctrl Pts',(-69.4278717644989,-17.2108289322258,
12.));
#142881=CARTESIAN_POINT('Ctrl Pts',(-69.4048725835516,-17.2128353380511,
0.));
#142882=CARTESIAN_POINT('Ctrl Pts',(-69.4048725835516,-17.2128353380511,
12.));
#142883=CARTESIAN_POINT('Ctrl Pts',(-69.3819158266955,-17.2148149949261,
0.));
#142884=CARTESIAN_POINT('Ctrl Pts',(-69.3819158266955,-17.2148149949261,
12.));
#142885=CARTESIAN_POINT('Ctrl Pts',(-69.359001631272,-17.2167679576991,
0.));
#142886=CARTESIAN_POINT('Ctrl Pts',(-69.359001631272,-17.2167679576991,
12.));
#142887=CARTESIAN_POINT('Ctrl Pts',(-69.3361301352149,-17.2186942815603,
0.));
#142888=CARTESIAN_POINT('Ctrl Pts',(-69.3361301352149,-17.2186942815603,
12.));
#142889=CARTESIAN_POINT('Ctrl Pts',(-69.3133014770542,-17.2205940220455,
0.));
#142890=CARTESIAN_POINT('Ctrl Pts',(-69.3133014770542,-17.2205940220455,
12.));
#142891=CARTESIAN_POINT('Ctrl Pts',(-69.2905157959141,-17.2224672350432,
0.));
#142892=CARTESIAN_POINT('Ctrl Pts',(-69.2905157959141,-17.2224672350432,
12.));
#142893=CARTESIAN_POINT('Ctrl Pts',(-69.2677732315199,-17.2243139767963,
0.));
#142894=CARTESIAN_POINT('Ctrl Pts',(-69.2677732315199,-17.2243139767963,
12.));
#142895=CARTESIAN_POINT('Ctrl Pts',(-69.2450739242092,-17.2261343039015,
0.));
#142896=CARTESIAN_POINT('Ctrl Pts',(-69.2450739242092,-17.2261343039015,
12.));
#142897=CARTESIAN_POINT('Ctrl Pts',(-69.2224180149377,-17.2279282733119,
0.));
#142898=CARTESIAN_POINT('Ctrl Pts',(-69.2224180149377,-17.2279282733119,
12.));
#142899=CARTESIAN_POINT('Ctrl Pts',(-69.1998056452837,-17.229695942341,
0.));
#142900=CARTESIAN_POINT('Ctrl Pts',(-69.1998056452837,-17.229695942341,
12.));
#142901=CARTESIAN_POINT('Ctrl Pts',(-69.1772369574462,-17.2314373686705,
0.));
#142902=CARTESIAN_POINT('Ctrl Pts',(-69.1772369574462,-17.2314373686705,
12.));
#142903=CARTESIAN_POINT('Ctrl Pts',(-69.1547120942542,-17.2331526103511,
0.));
#142904=CARTESIAN_POINT('Ctrl Pts',(-69.1547120942542,-17.2331526103511,
12.));
#142905=CARTESIAN_POINT('Ctrl Pts',(-69.1322311991759,-17.2348417258017,
0.));
#142906=CARTESIAN_POINT('Ctrl Pts',(-69.1322311991759,-17.2348417258017,
12.));
#142907=CARTESIAN_POINT('Ctrl Pts',(-69.1097944163244,-17.2365047738125,
0.));
#142908=CARTESIAN_POINT('Ctrl Pts',(-69.1097944163244,-17.2365047738125,
12.));
#142909=CARTESIAN_POINT('Ctrl Pts',(-69.0874018904598,-17.238141813549,
0.));
#142910=CARTESIAN_POINT('Ctrl Pts',(-69.0874018904598,-17.238141813549,
12.));
#142911=CARTESIAN_POINT('Ctrl Pts',(-69.0650537669859,-17.2397529045587,
0.));
#142912=CARTESIAN_POINT('Ctrl Pts',(-69.0650537669859,-17.2397529045587,
12.));
#142913=CARTESIAN_POINT('Ctrl Pts',(-69.0427501919636,-17.2413381067722,
0.));
#142914=CARTESIAN_POINT('Ctrl Pts',(-69.0427501919636,-17.2413381067722,
12.));
#142915=CARTESIAN_POINT('Ctrl Pts',(-69.0204913121226,-17.2428974805043,
0.));
#142916=CARTESIAN_POINT('Ctrl Pts',(-69.0204913121226,-17.2428974805043,
12.));
#142917=CARTESIAN_POINT('Ctrl Pts',(-68.9982772748694,-17.2444310864585,
0.));
#142918=CARTESIAN_POINT('Ctrl Pts',(-68.9982772748694,-17.2444310864585,
12.));
#142919=CARTESIAN_POINT('Ctrl Pts',(-68.9761082282922,-17.2459389857327,
0.));
#142920=CARTESIAN_POINT('Ctrl Pts',(-68.9761082282922,-17.2459389857327,
12.));
#142921=CARTESIAN_POINT('Ctrl Pts',(-68.9539843211618,-17.2474212398275,
0.));
#142922=CARTESIAN_POINT('Ctrl Pts',(-68.9539843211618,-17.2474212398275,
12.));
#142923=CARTESIAN_POINT('Ctrl Pts',(-68.9319057029407,-17.248877910643,
0.));
#142924=CARTESIAN_POINT('Ctrl Pts',(-68.9319057029407,-17.248877910643,
12.));
#142925=CARTESIAN_POINT('Ctrl Pts',(-68.9098725237868,-17.2503090604792,
0.));
#142926=CARTESIAN_POINT('Ctrl Pts',(-68.9098725237868,-17.2503090604792,
12.));
#142927=CARTESIAN_POINT('Ctrl Pts',(-68.8878849345557,-17.2517147520376,
0.));
#142928=CARTESIAN_POINT('Ctrl Pts',(-68.8878849345557,-17.2517147520376,
12.));
#142929=CARTESIAN_POINT('Ctrl Pts',(-68.8659430867977,-17.2530950484259,
0.));
#142930=CARTESIAN_POINT('Ctrl Pts',(-68.8659430867977,-17.2530950484259,
12.));
#142931=CARTESIAN_POINT('Ctrl Pts',(-68.8440471327563,-17.2544500131627,
0.));
#142932=CARTESIAN_POINT('Ctrl Pts',(-68.8440471327563,-17.2544500131627,
12.));
#142933=CARTESIAN_POINT('Ctrl Pts',(-68.8221972253954,-17.2557797101815,
0.));
#142934=CARTESIAN_POINT('Ctrl Pts',(-68.8221972253954,-17.2557797101815,
12.));
#142935=CARTESIAN_POINT('Ctrl Pts',(-68.8003935184193,-17.2570842038385,
0.));
#142936=CARTESIAN_POINT('Ctrl Pts',(-68.8003935184193,-17.2570842038385,
12.));
#142937=CARTESIAN_POINT('Ctrl Pts',(-68.7786361662876,-17.2583635589196,
0.));
#142938=CARTESIAN_POINT('Ctrl Pts',(-68.7786361662876,-17.2583635589196,
12.));
#142939=CARTESIAN_POINT('Ctrl Pts',(-68.7569253242312,-17.2596178406545,
0.));
#142940=CARTESIAN_POINT('Ctrl Pts',(-68.7569253242312,-17.2596178406545,
12.));
#142941=CARTESIAN_POINT('Ctrl Pts',(-68.7352611482519,-17.2608471147178,
0.));
#142942=CARTESIAN_POINT('Ctrl Pts',(-68.7352611482519,-17.2608471147178,
12.));
#142943=CARTESIAN_POINT('Ctrl Pts',(-68.7136437951074,-17.2620514472176,
0.));
#142944=CARTESIAN_POINT('Ctrl Pts',(-68.7136437951074,-17.2620514472176,
12.));
#142945=CARTESIAN_POINT('Ctrl Pts',(-68.6920734222932,-17.263230904689,
0.));
#142946=CARTESIAN_POINT('Ctrl Pts',(-68.6920734222932,-17.263230904689,
12.));
#142947=CARTESIAN_POINT('Ctrl Pts',(-68.6705501880263,-17.2643855540895,
0.));
#142948=CARTESIAN_POINT('Ctrl Pts',(-68.6705501880263,-17.2643855540895,
12.));
#142949=CARTESIAN_POINT('Ctrl Pts',(-68.6490742512085,-17.2655154627935,
0.));
#142950=CARTESIAN_POINT('Ctrl Pts',(-68.6490742512085,-17.2655154627935,
12.));
#142951=CARTESIAN_POINT('Ctrl Pts',(-68.6276457714757,-17.266620698609,
0.));
#142952=CARTESIAN_POINT('Ctrl Pts',(-68.6276457714757,-17.266620698609,
12.));
#142953=CARTESIAN_POINT('Ctrl Pts',(-68.606264909278,-17.2677013298061,
0.));
#142954=CARTESIAN_POINT('Ctrl Pts',(-68.606264909278,-17.2677013298061,
12.));
#142955=CARTESIAN_POINT('Ctrl Pts',(-68.5849318259449,-17.2687574251428,
0.));
#142956=CARTESIAN_POINT('Ctrl Pts',(-68.5849318259449,-17.2687574251428,
12.));
#142957=CARTESIAN_POINT('Ctrl Pts',(-68.5636466837502,-17.2697890538956,
0.));
#142958=CARTESIAN_POINT('Ctrl Pts',(-68.5636466837502,-17.2697890538956,
12.));
#142959=CARTESIAN_POINT('Ctrl Pts',(-68.5424096459746,-17.2707962858912,
0.));
#142960=CARTESIAN_POINT('Ctrl Pts',(-68.5424096459746,-17.2707962858912,
12.));
#142961=CARTESIAN_POINT('Ctrl Pts',(-68.5212208767835,-17.2717791914538,
0.));
#142962=CARTESIAN_POINT('Ctrl Pts',(-68.5212208767835,-17.2717791914538,
12.));
#142963=CARTESIAN_POINT('Ctrl Pts',(-68.5000805410896,-17.2727378413485,
0.));
#142964=CARTESIAN_POINT('Ctrl Pts',(-68.5000805410896,-17.2727378413485,
12.));
#142965=CARTESIAN_POINT('Ctrl Pts',(-68.4789888044357,-17.2736723067366,
0.));
#142966=CARTESIAN_POINT('Ctrl Pts',(-68.4789888044357,-17.2736723067366,
12.));
#142967=CARTESIAN_POINT('Ctrl Pts',(-68.4579458328208,-17.2745826591125,
0.));
#142968=CARTESIAN_POINT('Ctrl Pts',(-68.4579458328208,-17.2745826591125,
12.));
#142969=CARTESIAN_POINT('Ctrl Pts',(-68.4369517926803,-17.2754689703001,
0.));
#142970=CARTESIAN_POINT('Ctrl Pts',(-68.4369517926803,-17.2754689703001,
12.));
#142971=CARTESIAN_POINT('Ctrl Pts',(-68.4160068512781,-17.2763313126025,
0.));
#142972=CARTESIAN_POINT('Ctrl Pts',(-68.4160068512781,-17.2763313126025,
12.));
#142973=CARTESIAN_POINT('Ctrl Pts',(-68.3951111770498,-17.2771697589387,
0.));
#142974=CARTESIAN_POINT('Ctrl Pts',(-68.3951111770498,-17.2771697589387,
12.));
#142975=CARTESIAN_POINT('Ctrl Pts',(-68.374264939895,-17.2779843829605,
0.));
#142976=CARTESIAN_POINT('Ctrl Pts',(-68.374264939895,-17.2779843829605,
12.));
#142977=CARTESIAN_POINT('Ctrl Pts',(-68.353468311648,-17.2787752592475,
0.));
#142978=CARTESIAN_POINT('Ctrl Pts',(-68.353468311648,-17.2787752592475,
12.));
#142979=CARTESIAN_POINT('Ctrl Pts',(-68.3327214657533,-17.2795424631789,
0.));
#142980=CARTESIAN_POINT('Ctrl Pts',(-68.3327214657533,-17.2795424631789,
12.));
#142981=CARTESIAN_POINT('Ctrl Pts',(-68.3120245763884,-17.2802860705807,
0.));
#142982=CARTESIAN_POINT('Ctrl Pts',(-68.3120245763884,-17.2802860705807,
12.));
#142983=CARTESIAN_POINT('Ctrl Pts',(-68.2913778177258,-17.2810061574352,
0.));
#142984=CARTESIAN_POINT('Ctrl Pts',(-68.2913778177258,-17.2810061574352,
12.));
#142985=CARTESIAN_POINT('Ctrl Pts',(-68.2707813631761,-17.2817027995838,
0.));
#142986=CARTESIAN_POINT('Ctrl Pts',(-68.2707813631761,-17.2817027995838,
12.));
#142987=CARTESIAN_POINT('Ctrl Pts',(-68.250235384512,-17.2823760723886,
0.));
#142988=CARTESIAN_POINT('Ctrl Pts',(-68.250235384512,-17.2823760723886,
12.));
#142989=CARTESIAN_POINT('Ctrl Pts',(-68.2297400535339,-17.2830260513878,
0.));
#142990=CARTESIAN_POINT('Ctrl Pts',(-68.2297400535339,-17.2830260513878,
12.));
#142991=CARTESIAN_POINT('Ctrl Pts',(-68.2092955440591,-17.2836528130825,
0.));
#142992=CARTESIAN_POINT('Ctrl Pts',(-68.2092955440591,-17.2836528130825,
12.));
#142993=CARTESIAN_POINT('Ctrl Pts',(-68.1889020335418,-17.2842564355796,
0.));
#142994=CARTESIAN_POINT('Ctrl Pts',(-68.1889020335418,-17.2842564355796,
12.));
#142995=CARTESIAN_POINT('Ctrl Pts',(-68.1685597054193,-17.2848369995283,
0.));
#142996=CARTESIAN_POINT('Ctrl Pts',(-68.1685597054193,-17.2848369995283,
12.));
#142997=CARTESIAN_POINT('Ctrl Pts',(-68.1482687493176,-17.2853945882059,
0.));
#142998=CARTESIAN_POINT('Ctrl Pts',(-68.1482687493176,-17.2853945882059,
12.));
#142999=CARTESIAN_POINT('Ctrl Pts',(-68.1280293561473,-17.2859292855694,
0.));
#143000=CARTESIAN_POINT('Ctrl Pts',(-68.1280293561473,-17.2859292855694,
12.));
#143001=CARTESIAN_POINT('Ctrl Pts',(-68.1078417137865,-17.2864411745455,
0.));
#143002=CARTESIAN_POINT('Ctrl Pts',(-68.1078417137865,-17.2864411745455,
12.));
#143003=CARTESIAN_POINT('Ctrl Pts',(-68.0877060033229,-17.2869303355438,
0.));
#143004=CARTESIAN_POINT('Ctrl Pts',(-68.0877060033229,-17.2869303355438,
12.));
#143005=CARTESIAN_POINT('Ctrl Pts',(-68.0676223930469,-17.2873968440855,
0.));
#143006=CARTESIAN_POINT('Ctrl Pts',(-68.0676223930469,-17.2873968440855,
12.));
#143007=CARTESIAN_POINT('Ctrl Pts',(-68.0475910442494,-17.2878407730981,
0.));
#143008=CARTESIAN_POINT('Ctrl Pts',(-68.0475910442494,-17.2878407730981,
12.));
#143009=CARTESIAN_POINT('Ctrl Pts',(-68.027612122741,-17.2882621974737,
0.));
#143010=CARTESIAN_POINT('Ctrl Pts',(-68.027612122741,-17.2882621974737,
12.));
#143011=CARTESIAN_POINT('Ctrl Pts',(-68.007685808115,-17.28866119774,0.));
#143012=CARTESIAN_POINT('Ctrl Pts',(-68.007685808115,-17.28866119774,12.));
#143013=CARTESIAN_POINT('Ctrl Pts',(-67.9878123049132,-17.2890378644843,
0.));
#143014=CARTESIAN_POINT('Ctrl Pts',(-67.9878123049132,-17.2890378644843,
12.));
#143015=CARTESIAN_POINT('Ctrl Pts',(-67.9679918502441,-17.2893923013852,
0.));
#143016=CARTESIAN_POINT('Ctrl Pts',(-67.9679918502441,-17.2893923013852,
12.));
#143017=CARTESIAN_POINT('Ctrl Pts',(-67.9482246901517,-17.2897246158895,
0.));
#143018=CARTESIAN_POINT('Ctrl Pts',(-67.9482246901517,-17.2897246158895,
12.));
#143019=CARTESIAN_POINT('Ctrl Pts',(-67.9285110571662,-17.2900349103956,
0.));
#143020=CARTESIAN_POINT('Ctrl Pts',(-67.9285110571662,-17.2900349103956,
12.));
#143021=CARTESIAN_POINT('Ctrl Pts',(-67.908851149676,-17.2903232740717,
0.));
#143022=CARTESIAN_POINT('Ctrl Pts',(-67.908851149676,-17.2903232740717,
12.));
#143023=CARTESIAN_POINT('Ctrl Pts',(-67.8892451049871,-17.2905897724029,
0.));
#143024=CARTESIAN_POINT('Ctrl Pts',(-67.8892451049871,-17.2905897724029,
12.));
#143025=CARTESIAN_POINT('Ctrl Pts',(-67.8696929979178,-17.2908344459816,
0.));
#143026=CARTESIAN_POINT('Ctrl Pts',(-67.8696929979178,-17.2908344459816,
12.));
#143027=CARTESIAN_POINT('Ctrl Pts',(-67.8540944890057,-17.2910127431203,
0.));
#143028=CARTESIAN_POINT('Ctrl Pts',(-67.8540944890057,-17.2910127431203,
12.));
#143029=CARTESIAN_POINT('Ctrl Pts',(-67.8424198971214,-17.2911366591419,
0.));
#143030=CARTESIAN_POINT('Ctrl Pts',(-67.8424198971214,-17.2911366591419,
12.));
#143031=CARTESIAN_POINT('Ctrl Pts',(-67.8346476309106,-17.2912149114145,
0.));
#143032=CARTESIAN_POINT('Ctrl Pts',(-67.8346476309106,-17.2912149114145,
12.));
#143033=CARTESIAN_POINT('Ctrl Pts',(-67.8307641965655,-17.2912529479484,
0.));
#143034=CARTESIAN_POINT('Ctrl Pts',(-67.8307641965655,-17.2912529479484,
12.));
#143035=CARTESIAN_POINT('',(-67.8307641965655,-17.2912529479484,12.));
#143036=CARTESIAN_POINT('Ctrl Pts',(-67.8307641965655,-17.2912529479484,
12.));
#143037=CARTESIAN_POINT('Ctrl Pts',(-67.8346476309106,-17.2912149114145,
12.));
#143038=CARTESIAN_POINT('Ctrl Pts',(-67.8424198971214,-17.2911366591419,
12.));
#143039=CARTESIAN_POINT('Ctrl Pts',(-67.8540944890057,-17.2910127431203,
12.));
#143040=CARTESIAN_POINT('Ctrl Pts',(-67.8696929979178,-17.2908344459816,
12.));
#143041=CARTESIAN_POINT('Ctrl Pts',(-67.8892451049871,-17.2905897724029,
12.));
#143042=CARTESIAN_POINT('Ctrl Pts',(-67.908851149676,-17.2903232740717,
12.));
#143043=CARTESIAN_POINT('Ctrl Pts',(-67.9285110571662,-17.2900349103956,
12.));
#143044=CARTESIAN_POINT('Ctrl Pts',(-67.9482246901517,-17.2897246158895,
12.));
#143045=CARTESIAN_POINT('Ctrl Pts',(-67.9679918502441,-17.2893923013852,
12.));
#143046=CARTESIAN_POINT('Ctrl Pts',(-67.9878123049132,-17.2890378644843,
12.));
#143047=CARTESIAN_POINT('Ctrl Pts',(-68.007685808115,-17.28866119774,12.));
#143048=CARTESIAN_POINT('Ctrl Pts',(-68.027612122741,-17.2882621974737,
12.));
#143049=CARTESIAN_POINT('Ctrl Pts',(-68.0475910442494,-17.2878407730981,
12.));
#143050=CARTESIAN_POINT('Ctrl Pts',(-68.0676223930469,-17.2873968440855,
12.));
#143051=CARTESIAN_POINT('Ctrl Pts',(-68.0877060033229,-17.2869303355438,
12.));
#143052=CARTESIAN_POINT('Ctrl Pts',(-68.1078417137865,-17.2864411745455,
12.));
#143053=CARTESIAN_POINT('Ctrl Pts',(-68.1280293561473,-17.2859292855694,
12.));
#143054=CARTESIAN_POINT('Ctrl Pts',(-68.1482687493176,-17.2853945882059,
12.));
#143055=CARTESIAN_POINT('Ctrl Pts',(-68.1685597054193,-17.2848369995283,
12.));
#143056=CARTESIAN_POINT('Ctrl Pts',(-68.1889020335418,-17.2842564355796,
12.));
#143057=CARTESIAN_POINT('Ctrl Pts',(-68.2092955440591,-17.2836528130825,
12.));
#143058=CARTESIAN_POINT('Ctrl Pts',(-68.2297400535339,-17.2830260513878,
12.));
#143059=CARTESIAN_POINT('Ctrl Pts',(-68.250235384512,-17.2823760723886,
12.));
#143060=CARTESIAN_POINT('Ctrl Pts',(-68.2707813631761,-17.2817027995838,
12.));
#143061=CARTESIAN_POINT('Ctrl Pts',(-68.2913778177258,-17.2810061574352,
12.));
#143062=CARTESIAN_POINT('Ctrl Pts',(-68.3120245763884,-17.2802860705807,
12.));
#143063=CARTESIAN_POINT('Ctrl Pts',(-68.3327214657533,-17.2795424631789,
12.));
#143064=CARTESIAN_POINT('Ctrl Pts',(-68.353468311648,-17.2787752592475,
12.));
#143065=CARTESIAN_POINT('Ctrl Pts',(-68.374264939895,-17.2779843829605,
12.));
#143066=CARTESIAN_POINT('Ctrl Pts',(-68.3951111770498,-17.2771697589387,
12.));
#143067=CARTESIAN_POINT('Ctrl Pts',(-68.4160068512781,-17.2763313126025,
12.));
#143068=CARTESIAN_POINT('Ctrl Pts',(-68.4369517926803,-17.2754689703001,
12.));
#143069=CARTESIAN_POINT('Ctrl Pts',(-68.4579458328208,-17.2745826591125,
12.));
#143070=CARTESIAN_POINT('Ctrl Pts',(-68.4789888044357,-17.2736723067366,
12.));
#143071=CARTESIAN_POINT('Ctrl Pts',(-68.5000805410896,-17.2727378413485,
12.));
#143072=CARTESIAN_POINT('Ctrl Pts',(-68.5212208767835,-17.2717791914538,
12.));
#143073=CARTESIAN_POINT('Ctrl Pts',(-68.5424096459746,-17.2707962858912,
12.));
#143074=CARTESIAN_POINT('Ctrl Pts',(-68.5636466837502,-17.2697890538956,
12.));
#143075=CARTESIAN_POINT('Ctrl Pts',(-68.5849318259449,-17.2687574251428,
12.));
#143076=CARTESIAN_POINT('Ctrl Pts',(-68.606264909278,-17.2677013298061,
12.));
#143077=CARTESIAN_POINT('Ctrl Pts',(-68.6276457714757,-17.266620698609,
12.));
#143078=CARTESIAN_POINT('Ctrl Pts',(-68.6490742512085,-17.2655154627935,
12.));
#143079=CARTESIAN_POINT('Ctrl Pts',(-68.6705501880263,-17.2643855540895,
12.));
#143080=CARTESIAN_POINT('Ctrl Pts',(-68.6920734222932,-17.263230904689,
12.));
#143081=CARTESIAN_POINT('Ctrl Pts',(-68.7136437951074,-17.2620514472176,
12.));
#143082=CARTESIAN_POINT('Ctrl Pts',(-68.7352611482519,-17.2608471147178,
12.));
#143083=CARTESIAN_POINT('Ctrl Pts',(-68.7569253242312,-17.2596178406545,
12.));
#143084=CARTESIAN_POINT('Ctrl Pts',(-68.7786361662876,-17.2583635589196,
12.));
#143085=CARTESIAN_POINT('Ctrl Pts',(-68.8003935184193,-17.2570842038385,
12.));
#143086=CARTESIAN_POINT('Ctrl Pts',(-68.8221972253954,-17.2557797101815,
12.));
#143087=CARTESIAN_POINT('Ctrl Pts',(-68.8440471327563,-17.2544500131627,
12.));
#143088=CARTESIAN_POINT('Ctrl Pts',(-68.8659430867977,-17.2530950484259,
12.));
#143089=CARTESIAN_POINT('Ctrl Pts',(-68.8878849345557,-17.2517147520376,
12.));
#143090=CARTESIAN_POINT('Ctrl Pts',(-68.9098725237868,-17.2503090604792,
12.));
#143091=CARTESIAN_POINT('Ctrl Pts',(-68.9319057029407,-17.248877910643,
12.));
#143092=CARTESIAN_POINT('Ctrl Pts',(-68.9539843211618,-17.2474212398275,
12.));
#143093=CARTESIAN_POINT('Ctrl Pts',(-68.9761082282922,-17.2459389857327,
12.));
#143094=CARTESIAN_POINT('Ctrl Pts',(-68.9982772748694,-17.2444310864585,
12.));
#143095=CARTESIAN_POINT('Ctrl Pts',(-69.0204913121226,-17.2428974805043,
12.));
#143096=CARTESIAN_POINT('Ctrl Pts',(-69.0427501919636,-17.2413381067722,
12.));
#143097=CARTESIAN_POINT('Ctrl Pts',(-69.0650537669859,-17.2397529045587,
12.));
#143098=CARTESIAN_POINT('Ctrl Pts',(-69.0874018904598,-17.238141813549,
12.));
#143099=CARTESIAN_POINT('Ctrl Pts',(-69.1097944163244,-17.2365047738125,
12.));
#143100=CARTESIAN_POINT('Ctrl Pts',(-69.1322311991759,-17.2348417258017,
12.));
#143101=CARTESIAN_POINT('Ctrl Pts',(-69.1547120942542,-17.2331526103511,
12.));
#143102=CARTESIAN_POINT('Ctrl Pts',(-69.1772369574462,-17.2314373686705,
12.));
#143103=CARTESIAN_POINT('Ctrl Pts',(-69.1998056452837,-17.229695942341,
12.));
#143104=CARTESIAN_POINT('Ctrl Pts',(-69.2224180149377,-17.2279282733119,
12.));
#143105=CARTESIAN_POINT('Ctrl Pts',(-69.2450739242092,-17.2261343039015,
12.));
#143106=CARTESIAN_POINT('Ctrl Pts',(-69.2677732315199,-17.2243139767963,
12.));
#143107=CARTESIAN_POINT('Ctrl Pts',(-69.2905157959141,-17.2224672350432,
12.));
#143108=CARTESIAN_POINT('Ctrl Pts',(-69.3133014770542,-17.2205940220455,
12.));
#143109=CARTESIAN_POINT('Ctrl Pts',(-69.3361301352149,-17.2186942815603,
12.));
#143110=CARTESIAN_POINT('Ctrl Pts',(-69.359001631272,-17.2167679576991,
12.));
#143111=CARTESIAN_POINT('Ctrl Pts',(-69.3819158266955,-17.2148149949261,
12.));
#143112=CARTESIAN_POINT('Ctrl Pts',(-69.4048725835516,-17.2128353380511,
12.));
#143113=CARTESIAN_POINT('Ctrl Pts',(-69.4278717644989,-17.2108289322258,
12.));
#143114=CARTESIAN_POINT('Ctrl Pts',(-69.4509132327836,-17.208795722942,
12.));
#143115=CARTESIAN_POINT('Ctrl Pts',(-69.4739968522271,-17.2067356560326,
12.));
#143116=CARTESIAN_POINT('Ctrl Pts',(-69.497122487222,-17.2046486776697,
12.));
#143117=CARTESIAN_POINT('Ctrl Pts',(-69.5202900027329,-17.2025347343568,
12.));
#143118=CARTESIAN_POINT('Ctrl Pts',(-69.5434992642932,-17.2003937729266,
12.));
#143119=CARTESIAN_POINT('Ctrl Pts',(-69.5667501379984,-17.198225740538,
12.));
#143120=CARTESIAN_POINT('Ctrl Pts',(-69.5900424904954,-17.1960305846787,
12.));
#143121=CARTESIAN_POINT('Ctrl Pts',(-69.6133761889787,-17.1938082531619,
12.));
#143122=CARTESIAN_POINT('Ctrl Pts',(-69.6367511011927,-17.1915586941198,
12.));
#143123=CARTESIAN_POINT('Ctrl Pts',(-69.6601670954277,-17.1892818560004,
12.));
#143124=CARTESIAN_POINT('Ctrl Pts',(-69.6836240405151,-17.1869776875663,
12.));
#143125=CARTESIAN_POINT('Ctrl Pts',(-69.7071218058149,-17.1846461378966,
12.));
#143126=CARTESIAN_POINT('Ctrl Pts',(-69.7306602612125,-17.1822871563834,
12.));
#143127=CARTESIAN_POINT('Ctrl Pts',(-69.7542392771216,-17.1799006927255,
12.));
#143128=CARTESIAN_POINT('Ctrl Pts',(-69.7778587244788,-17.1774866969256,
12.));
#143129=CARTESIAN_POINT('Ctrl Pts',(-69.8015184747404,-17.1750451192887,
12.));
#143130=CARTESIAN_POINT('Ctrl Pts',(-69.8252183998713,-17.1725759104254,
12.));
#143131=CARTESIAN_POINT('Ctrl Pts',(-69.8489583723417,-17.1700790212476,
12.));
#143132=CARTESIAN_POINT('Ctrl Pts',(-69.8727382651292,-17.1675544029621,
12.));
#143133=CARTESIAN_POINT('Ctrl Pts',(-69.8965579517147,-17.1650020070686,
12.));
#143134=CARTESIAN_POINT('Ctrl Pts',(-69.9204173060779,-17.1624217853577,
12.));
#143135=CARTESIAN_POINT('Ctrl Pts',(-69.9443162026865,-17.1598136899144,
12.));
#143136=CARTESIAN_POINT('Ctrl Pts',(-69.9682545164942,-17.157177673114,
12.));
#143137=CARTESIAN_POINT('Ctrl Pts',(-69.9922321229428,-17.1545136876161,
12.));
#143138=CARTESIAN_POINT('Ctrl Pts',(-70.0162488979586,-17.1518216863624,
12.));
#143139=CARTESIAN_POINT('Ctrl Pts',(-70.040304717948,-17.1491016225748,
12.));
#143140=CARTESIAN_POINT('Ctrl Pts',(-70.0643994597865,-17.1463534497592,
12.));
#143141=CARTESIAN_POINT('Ctrl Pts',(-70.0885330008169,-17.1435771217015,
12.));
#143142=CARTESIAN_POINT('Ctrl Pts',(-70.1127052188515,-17.1407725924615,
12.));
#143143=CARTESIAN_POINT('Ctrl Pts',(-70.1369159921686,-17.1379398163708,
12.));
#143144=CARTESIAN_POINT('Ctrl Pts',(-70.1611651995085,-17.1350787480313,
12.));
#143145=CARTESIAN_POINT('Ctrl Pts',(-70.1854527200636,-17.1321893423183,
12.));
#143146=CARTESIAN_POINT('Ctrl Pts',(-70.2097784334749,-17.1292715543779,
12.));
#143147=CARTESIAN_POINT('Ctrl Pts',(-70.2341422198362,-17.1263253396202,
12.));
#143148=CARTESIAN_POINT('Ctrl Pts',(-70.2585439596899,-17.1233506537176,
12.));
#143149=CARTESIAN_POINT('Ctrl Pts',(-70.2829835340239,-17.1203474526031,
12.));
#143150=CARTESIAN_POINT('Ctrl Pts',(-70.3074608242613,-17.1173156924733,
12.));
#143151=CARTESIAN_POINT('Ctrl Pts',(-70.3319757122576,-17.1142553297869,
12.));
#143152=CARTESIAN_POINT('Ctrl Pts',(-70.356528080303,-17.111166321257,12.));
#143153=CARTESIAN_POINT('Ctrl Pts',(-70.3811178111206,-17.1080486238499,
12.));
#143154=CARTESIAN_POINT('Ctrl Pts',(-70.4057447878621,-17.1049021947833,
12.));
#143155=CARTESIAN_POINT('Ctrl Pts',(-70.4304088940998,-17.1017269915289,
12.));
#143156=CARTESIAN_POINT('Ctrl Pts',(-70.4551100138221,-17.098522971812,
12.));
#143157=CARTESIAN_POINT('Ctrl Pts',(-70.4798480314364,-17.0952900936044,
12.));
#143158=CARTESIAN_POINT('Ctrl Pts',(-70.5046228317669,-17.0920283151217,
12.));
#143159=CARTESIAN_POINT('Ctrl Pts',(-70.5294343000516,-17.0887375948221,
12.));
#143160=CARTESIAN_POINT('Ctrl Pts',(-70.5542823219346,-17.085417891409,
12.));
#143161=CARTESIAN_POINT('Ctrl Pts',(-70.5791667834599,-17.0820691638314,
12.));
#143162=CARTESIAN_POINT('Ctrl Pts',(-70.6040875710762,-17.0786913712766,
12.));
#143163=CARTESIAN_POINT('Ctrl Pts',(-70.6290445716341,-17.0752844731679,
12.));
#143164=CARTESIAN_POINT('Ctrl Pts',(-70.6540376723839,-17.0718484291623,
12.));
#143165=CARTESIAN_POINT('Ctrl Pts',(-70.6790667609678,-17.0683831991532,
12.));
#143166=CARTESIAN_POINT('Ctrl Pts',(-70.7041317254127,-17.0648887432714,
12.));
#143167=CARTESIAN_POINT('Ctrl Pts',(-70.7292324541348,-17.0613650218788,
12.));
#143168=CARTESIAN_POINT('Ctrl Pts',(-70.754368835938,-17.0578119955651,
12.));
#143169=CARTESIAN_POINT('Ctrl Pts',(-70.7795407600127,-17.0542296251462,
12.));
#143170=CARTESIAN_POINT('Ctrl Pts',(-70.8047481159298,-17.0506178716661,
12.));
#143171=CARTESIAN_POINT('Ctrl Pts',(-70.8299907936334,-17.0469766964001,
12.));
#143172=CARTESIAN_POINT('Ctrl Pts',(-70.8552686834423,-17.0433060608474,
12.));
#143173=CARTESIAN_POINT('Ctrl Pts',(-70.8805816760501,-17.0396059267277,
12.));
#143174=CARTESIAN_POINT('Ctrl Pts',(-70.9059296625214,-17.0358762559786,
12.));
#143175=CARTESIAN_POINT('Ctrl Pts',(-70.9313125342876,-17.0321170107564,
12.));
#143176=CARTESIAN_POINT('Ctrl Pts',(-70.956730183136,-17.0283281534392,
12.));
#143177=CARTESIAN_POINT('Ctrl Pts',(-70.9821825012136,-17.0245096466229,
12.));
#143178=CARTESIAN_POINT('Ctrl Pts',(-71.0076693810301,-17.0206614531166,
12.));
#143179=CARTESIAN_POINT('Ctrl Pts',(-71.0331907154574,-17.0167835359419,
12.));
#143180=CARTESIAN_POINT('Ctrl Pts',(-71.0587463977268,-17.0128758583334,
12.));
#143181=CARTESIAN_POINT('Ctrl Pts',(-71.0843363214221,-17.0089383837437,
12.));
#143182=CARTESIAN_POINT('Ctrl Pts',(-71.1099603804786,-17.0049710758393,
12.));
#143183=CARTESIAN_POINT('Ctrl Pts',(-71.1356184691806,-17.0009738984935,
12.));
#143184=CARTESIAN_POINT('Ctrl Pts',(-71.1613104821568,-16.9969468157824,
12.));
#143185=CARTESIAN_POINT('Ctrl Pts',(-71.187036314374,-16.9928897919828,
12.));
#143186=CARTESIAN_POINT('Ctrl Pts',(-71.212795861124,-16.9888027915742,
12.));
#143187=CARTESIAN_POINT('Ctrl Pts',(-71.2385890180221,-16.9846857792383,
12.));
#143188=CARTESIAN_POINT('Ctrl Pts',(-71.2644156810198,-16.9805387198571,
12.));
#143189=CARTESIAN_POINT('Ctrl Pts',(-71.290275746412,-16.9763615785136,
12.));
#143190=CARTESIAN_POINT('Ctrl Pts',(-71.3161691108427,-16.9721543204951,
12.));
#143191=CARTESIAN_POINT('Ctrl Pts',(-71.3420956713082,-16.9679169112994,
12.));
#143192=CARTESIAN_POINT('Ctrl Pts',(-71.3680553251562,-16.9636493166397,
12.));
#143193=CARTESIAN_POINT('Ctrl Pts',(-71.3940479700677,-16.9593515024276,
12.));
#143194=CARTESIAN_POINT('Ctrl Pts',(-71.4200735040384,-16.955023434762,
12.));
#143195=CARTESIAN_POINT('Ctrl Pts',(-71.4461318253563,-16.9506650799189,
12.));
#143196=CARTESIAN_POINT('Ctrl Pts',(-71.4722228325794,-16.9462764043443,
12.));
#143197=CARTESIAN_POINT('Ctrl Pts',(-71.4983464245055,-16.9418573746488,
12.));
#143198=CARTESIAN_POINT('Ctrl Pts',(-71.5245025002139,-16.9374079576201,
12.));
#143199=CARTESIAN_POINT('Ctrl Pts',(-71.5506909591128,-16.9329281202377,
12.));
#143200=CARTESIAN_POINT('Ctrl Pts',(-71.5769117009842,-16.9284178296933,
12.));
#143201=CARTESIAN_POINT('Ctrl Pts',(-71.6031646260174,-16.9238770534071,
12.));
#143202=CARTESIAN_POINT('Ctrl Pts',(-71.6294496348652,-16.9193057590607,
12.));
#143203=CARTESIAN_POINT('Ctrl Pts',(-71.6557666285917,-16.9147039145717,
12.));
#143204=CARTESIAN_POINT('Ctrl Pts',(-71.6821155085612,-16.9100714880368,
12.));
#143205=CARTESIAN_POINT('Ctrl Pts',(-71.7084961763357,-16.9054084476847,
12.));
#143206=CARTESIAN_POINT('Ctrl Pts',(-71.7349085335796,-16.9007147618344,
12.));
#143207=CARTESIAN_POINT('Ctrl Pts',(-71.7613524819235,-16.8959903988409,
12.));
#143208=CARTESIAN_POINT('Ctrl Pts',(-71.7878279229546,-16.8912353270942,
12.));
#143209=CARTESIAN_POINT('Ctrl Pts',(-71.8143347584962,-16.8864495151344,
12.));
#143210=CARTESIAN_POINT('Ctrl Pts',(-71.8408728908258,-16.881632931747,
12.));
#143211=CARTESIAN_POINT('Ctrl Pts',(-71.8674422229149,-16.87678554607,12.));
#143212=CARTESIAN_POINT('Ctrl Pts',(-71.8940426586534,-16.871907327697,
12.));
#143213=CARTESIAN_POINT('Ctrl Pts',(-71.9206741030887,-16.866998246792,
12.));
#143214=CARTESIAN_POINT('Ctrl Pts',(-71.9473364618922,-16.8620582738437,
12.));
#143215=CARTESIAN_POINT('Ctrl Pts',(-71.9740296408347,-16.8570873794269,
12.));
#143216=CARTESIAN_POINT('Ctrl Pts',(-72.0007535452081,-16.8520855339446,
12.));
#143217=CARTESIAN_POINT('Ctrl Pts',(-72.0275080793727,-16.8470527074275,
12.));
#143218=CARTESIAN_POINT('Ctrl Pts',(-72.0542931459825,-16.8419888691976,
12.));
#143219=CARTESIAN_POINT('Ctrl Pts',(-72.0811086466121,-16.8368939881446,
12.));
#143220=CARTESIAN_POINT('Ctrl Pts',(-72.1079544831513,-16.8317680333404,
12.));
#143221=CARTESIAN_POINT('Ctrl Pts',(-72.13483055902,-16.8266109745795,12.));
#143222=CARTESIAN_POINT('Ctrl Pts',(-72.1617367803235,-16.8214227828942,
12.));
#143223=CARTESIAN_POINT('Ctrl Pts',(-72.1886730573452,-16.8162034312269,
12.));
#143224=CARTESIAN_POINT('Ctrl Pts',(-72.2156393048975,-16.8109528945896,
12.));
#143225=CARTESIAN_POINT('Ctrl Pts',(-72.2387802230855,-16.8064254147775,
12.));
#143226=CARTESIAN_POINT('Ctrl Pts',(-72.2565380035259,-16.8029374213794,
12.));
#143227=CARTESIAN_POINT('Ctrl Pts',(-72.2688994295262,-16.8005027425863,
12.));
#143228=CARTESIAN_POINT('Ctrl Pts',(-72.2758557891326,-16.799130531775,
12.));
#143229=CARTESIAN_POINT('Ctrl Pts',(-72.2774028393911,-16.7988252568749,
12.));
#143230=CARTESIAN_POINT('',(-67.8307641965655,-17.2912529479484,0.));
#143231=CARTESIAN_POINT('',(-67.8307641965655,-17.2912529479484,0.));
#143232=CARTESIAN_POINT('Ctrl Pts',(-72.277402839391,-16.7988252568749,
0.));
#143233=CARTESIAN_POINT('Ctrl Pts',(-72.2758557891325,-16.799130531775,
0.));
#143234=CARTESIAN_POINT('Ctrl Pts',(-72.2688994295261,-16.8005027425863,
0.));
#143235=CARTESIAN_POINT('Ctrl Pts',(-72.2565380035259,-16.8029374213794,
0.));
#143236=CARTESIAN_POINT('Ctrl Pts',(-72.2387802230855,-16.8064254147775,
0.));
#143237=CARTESIAN_POINT('Ctrl Pts',(-72.2156393048975,-16.8109528945896,
0.));
#143238=CARTESIAN_POINT('Ctrl Pts',(-72.1886730573452,-16.8162034312269,
0.));
#143239=CARTESIAN_POINT('Ctrl Pts',(-72.1617367803235,-16.8214227828942,
0.));
#143240=CARTESIAN_POINT('Ctrl Pts',(-72.13483055902,-16.8266109745795,0.));
#143241=CARTESIAN_POINT('Ctrl Pts',(-72.1079544831513,-16.8317680333404,
0.));
#143242=CARTESIAN_POINT('Ctrl Pts',(-72.0811086466121,-16.8368939881446,
0.));
#143243=CARTESIAN_POINT('Ctrl Pts',(-72.0542931459825,-16.8419888691976,
0.));
#143244=CARTESIAN_POINT('Ctrl Pts',(-72.0275080793727,-16.8470527074275,
0.));
#143245=CARTESIAN_POINT('Ctrl Pts',(-72.0007535452081,-16.8520855339446,
0.));
#143246=CARTESIAN_POINT('Ctrl Pts',(-71.9740296408347,-16.8570873794269,
0.));
#143247=CARTESIAN_POINT('Ctrl Pts',(-71.9473364618922,-16.8620582738437,
0.));
#143248=CARTESIAN_POINT('Ctrl Pts',(-71.9206741030887,-16.866998246792,
0.));
#143249=CARTESIAN_POINT('Ctrl Pts',(-71.8940426586534,-16.871907327697,
0.));
#143250=CARTESIAN_POINT('Ctrl Pts',(-71.8674422229149,-16.87678554607,0.));
#143251=CARTESIAN_POINT('Ctrl Pts',(-71.8408728908258,-16.881632931747,
0.));
#143252=CARTESIAN_POINT('Ctrl Pts',(-71.8143347584962,-16.8864495151344,
0.));
#143253=CARTESIAN_POINT('Ctrl Pts',(-71.7878279229546,-16.8912353270942,
0.));
#143254=CARTESIAN_POINT('Ctrl Pts',(-71.7613524819235,-16.8959903988409,
0.));
#143255=CARTESIAN_POINT('Ctrl Pts',(-71.7349085335796,-16.9007147618344,
0.));
#143256=CARTESIAN_POINT('Ctrl Pts',(-71.7084961763357,-16.9054084476847,
0.));
#143257=CARTESIAN_POINT('Ctrl Pts',(-71.6821155085612,-16.9100714880368,
0.));
#143258=CARTESIAN_POINT('Ctrl Pts',(-71.6557666285917,-16.9147039145717,
0.));
#143259=CARTESIAN_POINT('Ctrl Pts',(-71.6294496348652,-16.9193057590607,
0.));
#143260=CARTESIAN_POINT('Ctrl Pts',(-71.6031646260174,-16.9238770534071,
0.));
#143261=CARTESIAN_POINT('Ctrl Pts',(-71.5769117009842,-16.9284178296933,
0.));
#143262=CARTESIAN_POINT('Ctrl Pts',(-71.5506909591128,-16.9329281202377,
0.));
#143263=CARTESIAN_POINT('Ctrl Pts',(-71.5245025002139,-16.9374079576201,
0.));
#143264=CARTESIAN_POINT('Ctrl Pts',(-71.4983464245055,-16.9418573746488,
0.));
#143265=CARTESIAN_POINT('Ctrl Pts',(-71.4722228325794,-16.9462764043443,
0.));
#143266=CARTESIAN_POINT('Ctrl Pts',(-71.4461318253563,-16.9506650799189,
0.));
#143267=CARTESIAN_POINT('Ctrl Pts',(-71.4200735040384,-16.955023434762,
0.));
#143268=CARTESIAN_POINT('Ctrl Pts',(-71.3940479700677,-16.9593515024276,
0.));
#143269=CARTESIAN_POINT('Ctrl Pts',(-71.3680553251562,-16.9636493166397,
0.));
#143270=CARTESIAN_POINT('Ctrl Pts',(-71.3420956713082,-16.9679169112994,
0.));
#143271=CARTESIAN_POINT('Ctrl Pts',(-71.3161691108427,-16.9721543204951,
0.));
#143272=CARTESIAN_POINT('Ctrl Pts',(-71.290275746412,-16.9763615785136,
0.));
#143273=CARTESIAN_POINT('Ctrl Pts',(-71.2644156810198,-16.9805387198571,
0.));
#143274=CARTESIAN_POINT('Ctrl Pts',(-71.2385890180221,-16.9846857792383,
0.));
#143275=CARTESIAN_POINT('Ctrl Pts',(-71.212795861124,-16.9888027915742,
0.));
#143276=CARTESIAN_POINT('Ctrl Pts',(-71.187036314374,-16.9928897919828,
0.));
#143277=CARTESIAN_POINT('Ctrl Pts',(-71.1613104821568,-16.9969468157824,
0.));
#143278=CARTESIAN_POINT('Ctrl Pts',(-71.1356184691806,-17.0009738984935,
0.));
#143279=CARTESIAN_POINT('Ctrl Pts',(-71.1099603804786,-17.0049710758393,
0.));
#143280=CARTESIAN_POINT('Ctrl Pts',(-71.0843363214221,-17.0089383837437,
0.));
#143281=CARTESIAN_POINT('Ctrl Pts',(-71.0587463977268,-17.0128758583334,
0.));
#143282=CARTESIAN_POINT('Ctrl Pts',(-71.0331907154574,-17.0167835359419,
0.));
#143283=CARTESIAN_POINT('Ctrl Pts',(-71.0076693810301,-17.0206614531166,
0.));
#143284=CARTESIAN_POINT('Ctrl Pts',(-70.9821825012136,-17.0245096466229,
0.));
#143285=CARTESIAN_POINT('Ctrl Pts',(-70.956730183136,-17.0283281534392,
0.));
#143286=CARTESIAN_POINT('Ctrl Pts',(-70.9313125342876,-17.0321170107564,
0.));
#143287=CARTESIAN_POINT('Ctrl Pts',(-70.9059296625214,-17.0358762559786,
0.));
#143288=CARTESIAN_POINT('Ctrl Pts',(-70.8805816760501,-17.0396059267277,
0.));
#143289=CARTESIAN_POINT('Ctrl Pts',(-70.8552686834423,-17.0433060608474,
0.));
#143290=CARTESIAN_POINT('Ctrl Pts',(-70.8299907936334,-17.0469766964001,
0.));
#143291=CARTESIAN_POINT('Ctrl Pts',(-70.8047481159298,-17.0506178716661,
0.));
#143292=CARTESIAN_POINT('Ctrl Pts',(-70.7795407600127,-17.0542296251462,
0.));
#143293=CARTESIAN_POINT('Ctrl Pts',(-70.754368835938,-17.0578119955651,
0.));
#143294=CARTESIAN_POINT('Ctrl Pts',(-70.7292324541348,-17.0613650218788,
0.));
#143295=CARTESIAN_POINT('Ctrl Pts',(-70.7041317254127,-17.0648887432714,
0.));
#143296=CARTESIAN_POINT('Ctrl Pts',(-70.6790667609678,-17.0683831991532,
0.));
#143297=CARTESIAN_POINT('Ctrl Pts',(-70.6540376723839,-17.0718484291623,
0.));
#143298=CARTESIAN_POINT('Ctrl Pts',(-70.6290445716341,-17.0752844731679,
0.));
#143299=CARTESIAN_POINT('Ctrl Pts',(-70.6040875710762,-17.0786913712766,
0.));
#143300=CARTESIAN_POINT('Ctrl Pts',(-70.5791667834599,-17.0820691638314,
0.));
#143301=CARTESIAN_POINT('Ctrl Pts',(-70.5542823219346,-17.085417891409,
0.));
#143302=CARTESIAN_POINT('Ctrl Pts',(-70.5294343000516,-17.0887375948221,
0.));
#143303=CARTESIAN_POINT('Ctrl Pts',(-70.5046228317669,-17.0920283151217,
0.));
#143304=CARTESIAN_POINT('Ctrl Pts',(-70.4798480314364,-17.0952900936044,
0.));
#143305=CARTESIAN_POINT('Ctrl Pts',(-70.4551100138221,-17.098522971812,
0.));
#143306=CARTESIAN_POINT('Ctrl Pts',(-70.4304088940998,-17.1017269915289,
0.));
#143307=CARTESIAN_POINT('Ctrl Pts',(-70.4057447878621,-17.1049021947833,
0.));
#143308=CARTESIAN_POINT('Ctrl Pts',(-70.3811178111206,-17.1080486238499,
0.));
#143309=CARTESIAN_POINT('Ctrl Pts',(-70.356528080303,-17.111166321257,0.));
#143310=CARTESIAN_POINT('Ctrl Pts',(-70.3319757122576,-17.1142553297869,
0.));
#143311=CARTESIAN_POINT('Ctrl Pts',(-70.3074608242613,-17.1173156924733,
0.));
#143312=CARTESIAN_POINT('Ctrl Pts',(-70.2829835340239,-17.1203474526031,
0.));
#143313=CARTESIAN_POINT('Ctrl Pts',(-70.2585439596899,-17.1233506537176,
0.));
#143314=CARTESIAN_POINT('Ctrl Pts',(-70.2341422198362,-17.1263253396202,
0.));
#143315=CARTESIAN_POINT('Ctrl Pts',(-70.2097784334749,-17.1292715543779,
0.));
#143316=CARTESIAN_POINT('Ctrl Pts',(-70.1854527200636,-17.1321893423183,
0.));
#143317=CARTESIAN_POINT('Ctrl Pts',(-70.1611651995085,-17.1350787480313,
0.));
#143318=CARTESIAN_POINT('Ctrl Pts',(-70.1369159921686,-17.1379398163708,
0.));
#143319=CARTESIAN_POINT('Ctrl Pts',(-70.1127052188515,-17.1407725924615,
0.));
#143320=CARTESIAN_POINT('Ctrl Pts',(-70.0885330008169,-17.1435771217015,
0.));
#143321=CARTESIAN_POINT('Ctrl Pts',(-70.0643994597865,-17.1463534497592,
0.));
#143322=CARTESIAN_POINT('Ctrl Pts',(-70.040304717948,-17.1491016225748,
0.));
#143323=CARTESIAN_POINT('Ctrl Pts',(-70.0162488979586,-17.1518216863624,
0.));
#143324=CARTESIAN_POINT('Ctrl Pts',(-69.9922321229428,-17.1545136876161,
0.));
#143325=CARTESIAN_POINT('Ctrl Pts',(-69.9682545164942,-17.157177673114,
0.));
#143326=CARTESIAN_POINT('Ctrl Pts',(-69.9443162026865,-17.1598136899144,
0.));
#143327=CARTESIAN_POINT('Ctrl Pts',(-69.9204173060779,-17.1624217853577,
0.));
#143328=CARTESIAN_POINT('Ctrl Pts',(-69.8965579517147,-17.1650020070686,
0.));
#143329=CARTESIAN_POINT('Ctrl Pts',(-69.8727382651292,-17.1675544029621,
0.));
#143330=CARTESIAN_POINT('Ctrl Pts',(-69.8489583723417,-17.1700790212476,
0.));
#143331=CARTESIAN_POINT('Ctrl Pts',(-69.8252183998713,-17.1725759104254,
0.));
#143332=CARTESIAN_POINT('Ctrl Pts',(-69.8015184747404,-17.1750451192887,
0.));
#143333=CARTESIAN_POINT('Ctrl Pts',(-69.7778587244788,-17.1774866969256,
0.));
#143334=CARTESIAN_POINT('Ctrl Pts',(-69.7542392771216,-17.1799006927255,
0.));
#143335=CARTESIAN_POINT('Ctrl Pts',(-69.7306602612125,-17.1822871563834,
0.));
#143336=CARTESIAN_POINT('Ctrl Pts',(-69.7071218058149,-17.1846461378966,
0.));
#143337=CARTESIAN_POINT('Ctrl Pts',(-69.6836240405151,-17.1869776875663,
0.));
#143338=CARTESIAN_POINT('Ctrl Pts',(-69.6601670954277,-17.1892818560004,
0.));
#143339=CARTESIAN_POINT('Ctrl Pts',(-69.6367511011927,-17.1915586941198,
0.));
#143340=CARTESIAN_POINT('Ctrl Pts',(-69.6133761889787,-17.1938082531619,
0.));
#143341=CARTESIAN_POINT('Ctrl Pts',(-69.5900424904954,-17.1960305846787,
0.));
#143342=CARTESIAN_POINT('Ctrl Pts',(-69.5667501379984,-17.198225740538,
0.));
#143343=CARTESIAN_POINT('Ctrl Pts',(-69.5434992642932,-17.2003937729266,
0.));
#143344=CARTESIAN_POINT('Ctrl Pts',(-69.5202900027329,-17.2025347343568,
0.));
#143345=CARTESIAN_POINT('Ctrl Pts',(-69.497122487222,-17.2046486776697,
0.));
#143346=CARTESIAN_POINT('Ctrl Pts',(-69.4739968522271,-17.2067356560326,
0.));
#143347=CARTESIAN_POINT('Ctrl Pts',(-69.4509132327836,-17.208795722942,
0.));
#143348=CARTESIAN_POINT('Ctrl Pts',(-69.4278717644989,-17.2108289322258,
0.));
#143349=CARTESIAN_POINT('Ctrl Pts',(-69.4048725835516,-17.2128353380511,
0.));
#143350=CARTESIAN_POINT('Ctrl Pts',(-69.3819158266955,-17.2148149949261,
0.));
#143351=CARTESIAN_POINT('Ctrl Pts',(-69.359001631272,-17.2167679576991,
0.));
#143352=CARTESIAN_POINT('Ctrl Pts',(-69.3361301352149,-17.2186942815603,
0.));
#143353=CARTESIAN_POINT('Ctrl Pts',(-69.3133014770542,-17.2205940220455,
0.));
#143354=CARTESIAN_POINT('Ctrl Pts',(-69.2905157959141,-17.2224672350432,
0.));
#143355=CARTESIAN_POINT('Ctrl Pts',(-69.2677732315199,-17.2243139767963,
0.));
#143356=CARTESIAN_POINT('Ctrl Pts',(-69.2450739242092,-17.2261343039015,
0.));
#143357=CARTESIAN_POINT('Ctrl Pts',(-69.2224180149377,-17.2279282733119,
0.));
#143358=CARTESIAN_POINT('Ctrl Pts',(-69.1998056452837,-17.229695942341,
0.));
#143359=CARTESIAN_POINT('Ctrl Pts',(-69.1772369574462,-17.2314373686705,
0.));
#143360=CARTESIAN_POINT('Ctrl Pts',(-69.1547120942542,-17.2331526103511,
0.));
#143361=CARTESIAN_POINT('Ctrl Pts',(-69.1322311991759,-17.2348417258017,
0.));
#143362=CARTESIAN_POINT('Ctrl Pts',(-69.1097944163244,-17.2365047738125,
0.));
#143363=CARTESIAN_POINT('Ctrl Pts',(-69.0874018904598,-17.238141813549,
0.));
#143364=CARTESIAN_POINT('Ctrl Pts',(-69.0650537669859,-17.2397529045587,
0.));
#143365=CARTESIAN_POINT('Ctrl Pts',(-69.0427501919636,-17.2413381067722,
0.));
#143366=CARTESIAN_POINT('Ctrl Pts',(-69.0204913121226,-17.2428974805043,
0.));
#143367=CARTESIAN_POINT('Ctrl Pts',(-68.9982772748694,-17.2444310864585,
0.));
#143368=CARTESIAN_POINT('Ctrl Pts',(-68.9761082282922,-17.2459389857327,
0.));
#143369=CARTESIAN_POINT('Ctrl Pts',(-68.9539843211618,-17.2474212398275,
0.));
#143370=CARTESIAN_POINT('Ctrl Pts',(-68.9319057029407,-17.248877910643,
0.));
#143371=CARTESIAN_POINT('Ctrl Pts',(-68.9098725237868,-17.2503090604792,
0.));
#143372=CARTESIAN_POINT('Ctrl Pts',(-68.8878849345557,-17.2517147520376,
0.));
#143373=CARTESIAN_POINT('Ctrl Pts',(-68.8659430867977,-17.2530950484259,
0.));
#143374=CARTESIAN_POINT('Ctrl Pts',(-68.8440471327563,-17.2544500131627,
0.));
#143375=CARTESIAN_POINT('Ctrl Pts',(-68.8221972253954,-17.2557797101815,
0.));
#143376=CARTESIAN_POINT('Ctrl Pts',(-68.8003935184193,-17.2570842038385,
0.));
#143377=CARTESIAN_POINT('Ctrl Pts',(-68.7786361662876,-17.2583635589196,
0.));
#143378=CARTESIAN_POINT('Ctrl Pts',(-68.7569253242312,-17.2596178406545,
0.));
#143379=CARTESIAN_POINT('Ctrl Pts',(-68.7352611482519,-17.2608471147178,
0.));
#143380=CARTESIAN_POINT('Ctrl Pts',(-68.7136437951074,-17.2620514472176,
0.));
#143381=CARTESIAN_POINT('Ctrl Pts',(-68.6920734222932,-17.263230904689,
0.));
#143382=CARTESIAN_POINT('Ctrl Pts',(-68.6705501880263,-17.2643855540895,
0.));
#143383=CARTESIAN_POINT('Ctrl Pts',(-68.6490742512085,-17.2655154627935,
0.));
#143384=CARTESIAN_POINT('Ctrl Pts',(-68.6276457714757,-17.266620698609,
0.));
#143385=CARTESIAN_POINT('Ctrl Pts',(-68.606264909278,-17.2677013298061,
0.));
#143386=CARTESIAN_POINT('Ctrl Pts',(-68.5849318259449,-17.2687574251428,
0.));
#143387=CARTESIAN_POINT('Ctrl Pts',(-68.5636466837502,-17.2697890538956,
0.));
#143388=CARTESIAN_POINT('Ctrl Pts',(-68.5424096459746,-17.2707962858912,
0.));
#143389=CARTESIAN_POINT('Ctrl Pts',(-68.5212208767835,-17.2717791914538,
0.));
#143390=CARTESIAN_POINT('Ctrl Pts',(-68.5000805410896,-17.2727378413485,
0.));
#143391=CARTESIAN_POINT('Ctrl Pts',(-68.4789888044357,-17.2736723067366,
0.));
#143392=CARTESIAN_POINT('Ctrl Pts',(-68.4579458328208,-17.2745826591125,
0.));
#143393=CARTESIAN_POINT('Ctrl Pts',(-68.4369517926803,-17.2754689703001,
0.));
#143394=CARTESIAN_POINT('Ctrl Pts',(-68.4160068512781,-17.2763313126025,
0.));
#143395=CARTESIAN_POINT('Ctrl Pts',(-68.3951111770498,-17.2771697589387,
0.));
#143396=CARTESIAN_POINT('Ctrl Pts',(-68.374264939895,-17.2779843829605,
0.));
#143397=CARTESIAN_POINT('Ctrl Pts',(-68.353468311648,-17.2787752592475,
0.));
#143398=CARTESIAN_POINT('Ctrl Pts',(-68.3327214657533,-17.2795424631789,
0.));
#143399=CARTESIAN_POINT('Ctrl Pts',(-68.3120245763884,-17.2802860705807,
0.));
#143400=CARTESIAN_POINT('Ctrl Pts',(-68.2913778177258,-17.2810061574352,
0.));
#143401=CARTESIAN_POINT('Ctrl Pts',(-68.2707813631761,-17.2817027995838,
0.));
#143402=CARTESIAN_POINT('Ctrl Pts',(-68.250235384512,-17.2823760723886,
0.));
#143403=CARTESIAN_POINT('Ctrl Pts',(-68.2297400535339,-17.2830260513878,
0.));
#143404=CARTESIAN_POINT('Ctrl Pts',(-68.2092955440591,-17.2836528130825,
0.));
#143405=CARTESIAN_POINT('Ctrl Pts',(-68.1889020335418,-17.2842564355796,
0.));
#143406=CARTESIAN_POINT('Ctrl Pts',(-68.1685597054193,-17.2848369995283,
0.));
#143407=CARTESIAN_POINT('Ctrl Pts',(-68.1482687493176,-17.2853945882059,
0.));
#143408=CARTESIAN_POINT('Ctrl Pts',(-68.1280293561473,-17.2859292855694,
0.));
#143409=CARTESIAN_POINT('Ctrl Pts',(-68.1078417137865,-17.2864411745455,
0.));
#143410=CARTESIAN_POINT('Ctrl Pts',(-68.0877060033229,-17.2869303355438,
0.));
#143411=CARTESIAN_POINT('Ctrl Pts',(-68.0676223930469,-17.2873968440855,
0.));
#143412=CARTESIAN_POINT('Ctrl Pts',(-68.0475910442494,-17.2878407730981,
0.));
#143413=CARTESIAN_POINT('Ctrl Pts',(-68.027612122741,-17.2882621974737,
0.));
#143414=CARTESIAN_POINT('Ctrl Pts',(-68.007685808115,-17.28866119774,0.));
#143415=CARTESIAN_POINT('Ctrl Pts',(-67.9878123049132,-17.2890378644843,
0.));
#143416=CARTESIAN_POINT('Ctrl Pts',(-67.9679918502441,-17.2893923013852,
0.));
#143417=CARTESIAN_POINT('Ctrl Pts',(-67.9482246901517,-17.2897246158895,
0.));
#143418=CARTESIAN_POINT('Ctrl Pts',(-67.9285110571662,-17.2900349103956,
0.));
#143419=CARTESIAN_POINT('Ctrl Pts',(-67.908851149676,-17.2903232740717,
0.));
#143420=CARTESIAN_POINT('Ctrl Pts',(-67.8892451049871,-17.2905897724029,
0.));
#143421=CARTESIAN_POINT('Ctrl Pts',(-67.8696929979178,-17.2908344459816,
0.));
#143422=CARTESIAN_POINT('Ctrl Pts',(-67.8540944890057,-17.2910127431203,
0.));
#143423=CARTESIAN_POINT('Ctrl Pts',(-67.8424198971214,-17.2911366591419,
0.));
#143424=CARTESIAN_POINT('Ctrl Pts',(-67.8346476309106,-17.2912149114145,
0.));
#143425=CARTESIAN_POINT('Ctrl Pts',(-67.8307641965655,-17.2912529479484,
0.));
#143426=CARTESIAN_POINT('Ctrl Pts',(-73.778495580227,-10.343287191141,0.));
#143427=CARTESIAN_POINT('Ctrl Pts',(-73.778495580227,-10.343287191141,12.));
#143428=CARTESIAN_POINT('Ctrl Pts',(-73.7731377048058,-10.3449014384453,
0.));
#143429=CARTESIAN_POINT('Ctrl Pts',(-73.7731377048058,-10.3449014384453,
12.));
#143430=CARTESIAN_POINT('Ctrl Pts',(-73.7624245587789,-10.3481265449342,
0.));
#143431=CARTESIAN_POINT('Ctrl Pts',(-73.7624245587789,-10.3481265449342,
12.));
#143432=CARTESIAN_POINT('Ctrl Pts',(-73.7463626541854,-10.3529540403092,
0.));
#143433=CARTESIAN_POINT('Ctrl Pts',(-73.7463626541854,-10.3529540403092,
12.));
#143434=CARTESIAN_POINT('Ctrl Pts',(-73.7249624109173,-10.359370371262,
0.));
#143435=CARTESIAN_POINT('Ctrl Pts',(-73.7249624109173,-10.359370371262,
12.));
#143436=CARTESIAN_POINT('Ctrl Pts',(-73.6982381645206,-10.3673568984582,
0.));
#143437=CARTESIAN_POINT('Ctrl Pts',(-73.6982381645206,-10.3673568984582,
12.));
#143438=CARTESIAN_POINT('Ctrl Pts',(-73.6715399947839,-10.3753095356342,
0.));
#143439=CARTESIAN_POINT('Ctrl Pts',(-73.6715399947839,-10.3753095356342,
12.));
#143440=CARTESIAN_POINT('Ctrl Pts',(-73.6448679350696,-10.3832282820371,
0.));
#143441=CARTESIAN_POINT('Ctrl Pts',(-73.6448679350696,-10.3832282820371,
12.));
#143442=CARTESIAN_POINT('Ctrl Pts',(-73.6182220363156,-10.3911131417463,
0.));
#143443=CARTESIAN_POINT('Ctrl Pts',(-73.6182220363156,-10.3911131417463,
12.));
#143444=CARTESIAN_POINT('Ctrl Pts',(-73.5916023719713,-10.3989641265285,
0.));
#143445=CARTESIAN_POINT('Ctrl Pts',(-73.5916023719713,-10.3989641265285,
12.));
#143446=CARTESIAN_POINT('Ctrl Pts',(-73.5650090359839,-10.406781255551,
0.));
#143447=CARTESIAN_POINT('Ctrl Pts',(-73.5650090359839,-10.406781255551,
12.));
#143448=CARTESIAN_POINT('Ctrl Pts',(-73.5384421354543,-10.414564552681,
0.));
#143449=CARTESIAN_POINT('Ctrl Pts',(-73.5384421354543,-10.414564552681,
12.));
#143450=CARTESIAN_POINT('Ctrl Pts',(-73.5119017847575,-10.4223140444605,
0.));
#143451=CARTESIAN_POINT('Ctrl Pts',(-73.5119017847575,-10.4223140444605,
12.));
#143452=CARTESIAN_POINT('Ctrl Pts',(-73.485388099225,-10.430029757865,0.));
#143453=CARTESIAN_POINT('Ctrl Pts',(-73.485388099225,-10.430029757865,12.));
#143454=CARTESIAN_POINT('Ctrl Pts',(-73.4589011886197,-10.4377117180222,
0.));
#143455=CARTESIAN_POINT('Ctrl Pts',(-73.4589011886197,-10.4377117180222,
12.));
#143456=CARTESIAN_POINT('Ctrl Pts',(-73.4324411518554,-10.4453599463547,
0.));
#143457=CARTESIAN_POINT('Ctrl Pts',(-73.4324411518554,-10.4453599463547,
12.));
#143458=CARTESIAN_POINT('Ctrl Pts',(-73.4060080806686,-10.452974461845,
0.));
#143459=CARTESIAN_POINT('Ctrl Pts',(-73.4060080806686,-10.452974461845,
12.));
#143460=CARTESIAN_POINT('Ctrl Pts',(-73.37960206225,-10.4605552819397,0.));
#143461=CARTESIAN_POINT('Ctrl Pts',(-73.37960206225,-10.4605552819397,12.));
#143462=CARTESIAN_POINT('Ctrl Pts',(-73.3532231823659,-10.4681024236289,
0.));
#143463=CARTESIAN_POINT('Ctrl Pts',(-73.3532231823659,-10.4681024236289,
12.));
#143464=CARTESIAN_POINT('Ctrl Pts',(-73.3268715280575,-10.4756159043806,
0.));
#143465=CARTESIAN_POINT('Ctrl Pts',(-73.3268715280575,-10.4756159043806,
12.));
#143466=CARTESIAN_POINT('Ctrl Pts',(-73.3005471910583,-10.4830957433305,
0.));
#143467=CARTESIAN_POINT('Ctrl Pts',(-73.3005471910583,-10.4830957433305,
12.));
#143468=CARTESIAN_POINT('Ctrl Pts',(-73.2742502674304,-10.4905419611523,
0.));
#143469=CARTESIAN_POINT('Ctrl Pts',(-73.2742502674304,-10.4905419611523,
12.));
#143470=CARTESIAN_POINT('Ctrl Pts',(-73.2479808560189,-10.4979545795192,
0.));
#143471=CARTESIAN_POINT('Ctrl Pts',(-73.2479808560189,-10.4979545795192,
12.));
#143472=CARTESIAN_POINT('Ctrl Pts',(-73.2217390572562,-10.5053336206908,
0.));
#143473=CARTESIAN_POINT('Ctrl Pts',(-73.2217390572562,-10.5053336206908,
12.));
#143474=CARTESIAN_POINT('Ctrl Pts',(-73.1955249719048,-10.5126791070805,
0.));
#143475=CARTESIAN_POINT('Ctrl Pts',(-73.1955249719048,-10.5126791070805,
12.));
#143476=CARTESIAN_POINT('Ctrl Pts',(-73.1693386996138,-10.5199910607654,
0.));
#143477=CARTESIAN_POINT('Ctrl Pts',(-73.1693386996138,-10.5199910607654,
12.));
#143478=CARTESIAN_POINT('Ctrl Pts',(-73.1431803382711,-10.5272695032653,
0.));
#143479=CARTESIAN_POINT('Ctrl Pts',(-73.1431803382711,-10.5272695032653,
12.));
#143480=CARTESIAN_POINT('Ctrl Pts',(-73.1170499848039,-10.53451445581,0.));
#143481=CARTESIAN_POINT('Ctrl Pts',(-73.1170499848039,-10.53451445581,12.));
#143482=CARTESIAN_POINT('Ctrl Pts',(-73.0909477356474,-10.5417259395003,
0.));
#143483=CARTESIAN_POINT('Ctrl Pts',(-73.0909477356474,-10.5417259395003,
12.));
#143484=CARTESIAN_POINT('Ctrl Pts',(-73.0648736873434,-10.5489039755138,
0.));
#143485=CARTESIAN_POINT('Ctrl Pts',(-73.0648736873434,-10.5489039755138,
12.));
#143486=CARTESIAN_POINT('Ctrl Pts',(-73.0388279370834,-10.5560485852974,
0.));
#143487=CARTESIAN_POINT('Ctrl Pts',(-73.0388279370834,-10.5560485852974,
12.));
#143488=CARTESIAN_POINT('Ctrl Pts',(-73.0128105832621,-10.5631597907651,
0.));
#143489=CARTESIAN_POINT('Ctrl Pts',(-73.0128105832621,-10.5631597907651,
12.));
#143490=CARTESIAN_POINT('Ctrl Pts',(-72.9868217252283,-10.570237614205,
0.));
#143491=CARTESIAN_POINT('Ctrl Pts',(-72.9868217252283,-10.570237614205,
12.));
#143492=CARTESIAN_POINT('Ctrl Pts',(-72.9608614630534,-10.5772820781958,
0.));
#143493=CARTESIAN_POINT('Ctrl Pts',(-72.9608614630534,-10.5772820781958,
12.));
#143494=CARTESIAN_POINT('Ctrl Pts',(-72.9349298972822,-10.5842932055209,
0.));
#143495=CARTESIAN_POINT('Ctrl Pts',(-72.9349298972822,-10.5842932055209,
12.));
#143496=CARTESIAN_POINT('Ctrl Pts',(-72.9090271287083,-10.5912710190928,
0.));
#143497=CARTESIAN_POINT('Ctrl Pts',(-72.9090271287083,-10.5912710190928,
12.));
#143498=CARTESIAN_POINT('Ctrl Pts',(-72.8831532580845,-10.5982155418626,
0.));
#143499=CARTESIAN_POINT('Ctrl Pts',(-72.8831532580845,-10.5982155418626,
12.));
#143500=CARTESIAN_POINT('Ctrl Pts',(-72.8573083861337,-10.6051267968203,
0.));
#143501=CARTESIAN_POINT('Ctrl Pts',(-72.8573083861337,-10.6051267968203,
12.));
#143502=CARTESIAN_POINT('Ctrl Pts',(-72.8314926136881,-10.6120048070367,
0.));
#143503=CARTESIAN_POINT('Ctrl Pts',(-72.8314926136881,-10.6120048070367,
12.));
#143504=CARTESIAN_POINT('Ctrl Pts',(-72.8057060417887,-10.6188495956973,
0.));
#143505=CARTESIAN_POINT('Ctrl Pts',(-72.8057060417887,-10.6188495956973,
12.));
#143506=CARTESIAN_POINT('Ctrl Pts',(-72.7799487717911,-10.6256611861394,
0.));
#143507=CARTESIAN_POINT('Ctrl Pts',(-72.7799487717911,-10.6256611861394,
12.));
#143508=CARTESIAN_POINT('Ctrl Pts',(-72.7542209054812,-10.6324396018998,
0.));
#143509=CARTESIAN_POINT('Ctrl Pts',(-72.7542209054812,-10.6324396018998,
12.));
#143510=CARTESIAN_POINT('Ctrl Pts',(-72.7285225451293,-10.6391848667352,
0.));
#143511=CARTESIAN_POINT('Ctrl Pts',(-72.7285225451293,-10.6391848667352,
12.));
#143512=CARTESIAN_POINT('Ctrl Pts',(-72.7028537934317,-10.6458970045946,
0.));
#143513=CARTESIAN_POINT('Ctrl Pts',(-72.7028537934317,-10.6458970045946,
12.));
#143514=CARTESIAN_POINT('Ctrl Pts',(-72.6772147534752,-10.6525760396054,
0.));
#143515=CARTESIAN_POINT('Ctrl Pts',(-72.6772147534752,-10.6525760396054,
12.));
#143516=CARTESIAN_POINT('Ctrl Pts',(-72.651605528691,-10.659221996058,0.));
#143517=CARTESIAN_POINT('Ctrl Pts',(-72.651605528691,-10.659221996058,12.));
#143518=CARTESIAN_POINT('Ctrl Pts',(-72.6260262228065,-10.6658348983944,
0.));
#143519=CARTESIAN_POINT('Ctrl Pts',(-72.6260262228065,-10.6658348983944,
12.));
#143520=CARTESIAN_POINT('Ctrl Pts',(-72.6004769398019,-10.6724147711995,
0.));
#143521=CARTESIAN_POINT('Ctrl Pts',(-72.6004769398019,-10.6724147711995,
12.));
#143522=CARTESIAN_POINT('Ctrl Pts',(-72.5749577839415,-10.6789616392042,
0.));
#143523=CARTESIAN_POINT('Ctrl Pts',(-72.5749577839415,-10.6789616392042,
12.));
#143524=CARTESIAN_POINT('Ctrl Pts',(-72.5494688597961,-10.6854755272904,
0.));
#143525=CARTESIAN_POINT('Ctrl Pts',(-72.5494688597961,-10.6854755272904,
12.));
#143526=CARTESIAN_POINT('Ctrl Pts',(-72.5240102722664,-10.691956460499,
0.));
#143527=CARTESIAN_POINT('Ctrl Pts',(-72.5240102722664,-10.691956460499,
12.));
#143528=CARTESIAN_POINT('Ctrl Pts',(-72.4985821266023,-10.6984044640398,
0.));
#143529=CARTESIAN_POINT('Ctrl Pts',(-72.4985821266023,-10.6984044640398,
12.));
#143530=CARTESIAN_POINT('Ctrl Pts',(-72.4731845284227,-10.7048195633061,
0.));
#143531=CARTESIAN_POINT('Ctrl Pts',(-72.4731845284227,-10.7048195633061,
12.));
#143532=CARTESIAN_POINT('Ctrl Pts',(-72.4478175837156,-10.7112017838706,
0.));
#143533=CARTESIAN_POINT('Ctrl Pts',(-72.4478175837156,-10.7112017838706,
12.));
#143534=CARTESIAN_POINT('Ctrl Pts',(-72.4224813988347,-10.7175511514788,
0.));
#143535=CARTESIAN_POINT('Ctrl Pts',(-72.4224813988347,-10.7175511514788,
12.));
#143536=CARTESIAN_POINT('Ctrl Pts',(-72.3971760804933,-10.7238676920469,
0.));
#143537=CARTESIAN_POINT('Ctrl Pts',(-72.3971760804933,-10.7238676920469,
12.));
#143538=CARTESIAN_POINT('Ctrl Pts',(-72.3719017357571,-10.7301514316607,
0.));
#143539=CARTESIAN_POINT('Ctrl Pts',(-72.3719017357571,-10.7301514316607,
12.));
#143540=CARTESIAN_POINT('Ctrl Pts',(-72.3466584720318,-10.73640239658,0.));
#143541=CARTESIAN_POINT('Ctrl Pts',(-72.3466584720318,-10.73640239658,12.));
#143542=CARTESIAN_POINT('Ctrl Pts',(-72.3214463970641,-10.7426206132375,
0.));
#143543=CARTESIAN_POINT('Ctrl Pts',(-72.3214463970641,-10.7426206132375,
12.));
#143544=CARTESIAN_POINT('Ctrl Pts',(-72.2962656189556,-10.7488061082367,
0.));
#143545=CARTESIAN_POINT('Ctrl Pts',(-72.2962656189556,-10.7488061082367,
12.));
#143546=CARTESIAN_POINT('Ctrl Pts',(-72.2711162461681,-10.7549589083535,
0.));
#143547=CARTESIAN_POINT('Ctrl Pts',(-72.2711162461681,-10.7549589083535,
12.));
#143548=CARTESIAN_POINT('Ctrl Pts',(-72.2459983875296,-10.7610790405385,
0.));
#143549=CARTESIAN_POINT('Ctrl Pts',(-72.2459983875296,-10.7610790405385,
12.));
#143550=CARTESIAN_POINT('Ctrl Pts',(-72.2209121522366,-10.7671665319255,
0.));
#143551=CARTESIAN_POINT('Ctrl Pts',(-72.2209121522366,-10.7671665319255,
12.));
#143552=CARTESIAN_POINT('Ctrl Pts',(-72.1958576498558,-10.7732214098344,
0.));
#143553=CARTESIAN_POINT('Ctrl Pts',(-72.1958576498558,-10.7732214098344,
12.));
#143554=CARTESIAN_POINT('Ctrl Pts',(-72.1708349903305,-10.7792437017662,
0.));
#143555=CARTESIAN_POINT('Ctrl Pts',(-72.1708349903305,-10.7792437017662,
12.));
#143556=CARTESIAN_POINT('Ctrl Pts',(-72.1458442839834,-10.7852334354016,
0.));
#143557=CARTESIAN_POINT('Ctrl Pts',(-72.1458442839834,-10.7852334354016,
12.));
#143558=CARTESIAN_POINT('Ctrl Pts',(-72.1208856415171,-10.7911906386027,
0.));
#143559=CARTESIAN_POINT('Ctrl Pts',(-72.1208856415171,-10.7911906386027,
12.));
#143560=CARTESIAN_POINT('Ctrl Pts',(-72.0959591740114,-10.7971153394166,
0.));
#143561=CARTESIAN_POINT('Ctrl Pts',(-72.0959591740114,-10.7971153394166,
12.));
#143562=CARTESIAN_POINT('Ctrl Pts',(-72.0710649929202,-10.8030075660808,
0.));
#143563=CARTESIAN_POINT('Ctrl Pts',(-72.0710649929202,-10.8030075660808,
12.));
#143564=CARTESIAN_POINT('Ctrl Pts',(-72.0462032100815,-10.8088673470184,
0.));
#143565=CARTESIAN_POINT('Ctrl Pts',(-72.0462032100815,-10.8088673470184,
12.));
#143566=CARTESIAN_POINT('Ctrl Pts',(-72.0213739377223,-10.8146947108375,
0.));
#143567=CARTESIAN_POINT('Ctrl Pts',(-72.0213739377223,-10.8146947108375,
12.));
#143568=CARTESIAN_POINT('Ctrl Pts',(-71.9965772884619,-10.8204896863328,
0.));
#143569=CARTESIAN_POINT('Ctrl Pts',(-71.9965772884619,-10.8204896863328,
12.));
#143570=CARTESIAN_POINT('Ctrl Pts',(-71.9718133753127,-10.8262523024898,
0.));
#143571=CARTESIAN_POINT('Ctrl Pts',(-71.9718133753127,-10.8262523024898,
12.));
#143572=CARTESIAN_POINT('Ctrl Pts',(-71.9470823116785,-10.8319825884918,
0.));
#143573=CARTESIAN_POINT('Ctrl Pts',(-71.9470823116785,-10.8319825884918,
12.));
#143574=CARTESIAN_POINT('Ctrl Pts',(-71.9223842113625,-10.8376805737159,
0.));
#143575=CARTESIAN_POINT('Ctrl Pts',(-71.9223842113625,-10.8376805737159,
12.));
#143576=CARTESIAN_POINT('Ctrl Pts',(-71.8977191885725,-10.8433462877311,
0.));
#143577=CARTESIAN_POINT('Ctrl Pts',(-71.8977191885725,-10.8433462877311,
12.));
#143578=CARTESIAN_POINT('Ctrl Pts',(-71.8730873579224,-10.8489797602997,
0.));
#143579=CARTESIAN_POINT('Ctrl Pts',(-71.8730873579224,-10.8489797602997,
12.));
#143580=CARTESIAN_POINT('Ctrl Pts',(-71.8484888344339,-10.8545810213799,
0.));
#143581=CARTESIAN_POINT('Ctrl Pts',(-71.8484888344339,-10.8545810213799,
12.));
#143582=CARTESIAN_POINT('Ctrl Pts',(-71.8239237335331,-10.8601501011332,
0.));
#143583=CARTESIAN_POINT('Ctrl Pts',(-71.8239237335331,-10.8601501011332,
12.));
#143584=CARTESIAN_POINT('Ctrl Pts',(-71.7993921710564,-10.865687029922,
0.));
#143585=CARTESIAN_POINT('Ctrl Pts',(-71.7993921710564,-10.865687029922,
12.));
#143586=CARTESIAN_POINT('Ctrl Pts',(-71.7748942632593,-10.8711918383073,
0.));
#143587=CARTESIAN_POINT('Ctrl Pts',(-71.7748942632593,-10.8711918383073,
12.));
#143588=CARTESIAN_POINT('Ctrl Pts',(-71.7504301268181,-10.8766645570497,
0.));
#143589=CARTESIAN_POINT('Ctrl Pts',(-71.7504301268181,-10.8766645570497,
12.));
#143590=CARTESIAN_POINT('Ctrl Pts',(-71.7259998788328,-10.882105217112,
0.));
#143591=CARTESIAN_POINT('Ctrl Pts',(-71.7259998788328,-10.882105217112,
12.));
#143592=CARTESIAN_POINT('Ctrl Pts',(-71.7016036368236,-10.8875138496671,
0.));
#143593=CARTESIAN_POINT('Ctrl Pts',(-71.7016036368236,-10.8875138496671,
12.));
#143594=CARTESIAN_POINT('Ctrl Pts',(-71.6772415187364,-10.8928904860964,
0.));
#143595=CARTESIAN_POINT('Ctrl Pts',(-71.6772415187364,-10.8928904860964,
12.));
#143596=CARTESIAN_POINT('Ctrl Pts',(-71.6529136429504,-10.8982351579871,
0.));
#143597=CARTESIAN_POINT('Ctrl Pts',(-71.6529136429504,-10.8982351579871,
12.));
#143598=CARTESIAN_POINT('Ctrl Pts',(-71.6286201282812,-10.9035478971328,
0.));
#143599=CARTESIAN_POINT('Ctrl Pts',(-71.6286201282812,-10.9035478971328,
12.));
#143600=CARTESIAN_POINT('Ctrl Pts',(-71.6043610939835,-10.9088287355365,
0.));
#143601=CARTESIAN_POINT('Ctrl Pts',(-71.6043610939835,-10.9088287355365,
12.));
#143602=CARTESIAN_POINT('Ctrl Pts',(-71.5801366597488,-10.914077705417,
0.));
#143603=CARTESIAN_POINT('Ctrl Pts',(-71.5801366597488,-10.914077705417,
12.));
#143604=CARTESIAN_POINT('Ctrl Pts',(-71.5559469457091,-10.91929483921,0.));
#143605=CARTESIAN_POINT('Ctrl Pts',(-71.5559469457091,-10.91929483921,12.));
#143606=CARTESIAN_POINT('Ctrl Pts',(-71.5317920724459,-10.9244801695642,
0.));
#143607=CARTESIAN_POINT('Ctrl Pts',(-71.5317920724459,-10.9244801695642,
12.));
#143608=CARTESIAN_POINT('Ctrl Pts',(-71.5076721609937,-10.9296337293424,
0.));
#143609=CARTESIAN_POINT('Ctrl Pts',(-71.5076721609937,-10.9296337293424,
12.));
#143610=CARTESIAN_POINT('Ctrl Pts',(-71.4835873328423,-10.9347555516235,
0.));
#143611=CARTESIAN_POINT('Ctrl Pts',(-71.4835873328423,-10.9347555516235,
12.));
#143612=CARTESIAN_POINT('Ctrl Pts',(-71.4595377099351,-10.9398456697095,
0.));
#143613=CARTESIAN_POINT('Ctrl Pts',(-71.4595377099351,-10.9398456697095,
12.));
#143614=CARTESIAN_POINT('Ctrl Pts',(-71.435523414672,-10.944904117127,0.));
#143615=CARTESIAN_POINT('Ctrl Pts',(-71.435523414672,-10.944904117127,12.));
#143616=CARTESIAN_POINT('Ctrl Pts',(-71.4115445699194,-10.9499309276236,
0.));
#143617=CARTESIAN_POINT('Ctrl Pts',(-71.4115445699194,-10.9499309276236,
12.));
#143618=CARTESIAN_POINT('Ctrl Pts',(-71.3876012990138,-10.954926135169,
0.));
#143619=CARTESIAN_POINT('Ctrl Pts',(-71.3876012990138,-10.954926135169,
12.));
#143620=CARTESIAN_POINT('Ctrl Pts',(-71.3636937257649,-10.9598897739564,
0.));
#143621=CARTESIAN_POINT('Ctrl Pts',(-71.3636937257649,-10.9598897739564,
12.));
#143622=CARTESIAN_POINT('Ctrl Pts',(-71.339821974454,-10.9648218784098,
0.));
#143623=CARTESIAN_POINT('Ctrl Pts',(-71.339821974454,-10.9648218784098,
12.));
#143624=CARTESIAN_POINT('Ctrl Pts',(-71.3159861698358,-10.969722483186,
0.));
#143625=CARTESIAN_POINT('Ctrl Pts',(-71.3159861698358,-10.969722483186,
12.));
#143626=CARTESIAN_POINT('Ctrl Pts',(-71.2921864371491,-10.9745916231709,
0.));
#143627=CARTESIAN_POINT('Ctrl Pts',(-71.2921864371491,-10.9745916231709,
12.));
#143628=CARTESIAN_POINT('Ctrl Pts',(-71.2684229021207,-10.9794293334805,
0.));
#143629=CARTESIAN_POINT('Ctrl Pts',(-71.2684229021207,-10.9794293334805,
12.));
#143630=CARTESIAN_POINT('Ctrl Pts',(-71.2446956909687,-10.9842356494627,
0.));
#143631=CARTESIAN_POINT('Ctrl Pts',(-71.2446956909687,-10.9842356494627,
12.));
#143632=CARTESIAN_POINT('Ctrl Pts',(-71.2210049304014,-10.9890106067039,
0.));
#143633=CARTESIAN_POINT('Ctrl Pts',(-71.2210049304014,-10.9890106067039,
12.));
#143634=CARTESIAN_POINT('Ctrl Pts',(-71.1973507476191,-10.993754241032,
0.));
#143635=CARTESIAN_POINT('Ctrl Pts',(-71.1973507476191,-10.993754241032,
12.));
#143636=CARTESIAN_POINT('Ctrl Pts',(-71.1737332703248,-10.9984665885127,
0.));
#143637=CARTESIAN_POINT('Ctrl Pts',(-71.1737332703248,-10.9984665885127,
12.));
#143638=CARTESIAN_POINT('Ctrl Pts',(-71.1501526267286,-11.0031476854502,
0.));
#143639=CARTESIAN_POINT('Ctrl Pts',(-71.1501526267286,-11.0031476854502,
12.));
#143640=CARTESIAN_POINT('Ctrl Pts',(-71.1266089455517,-11.0077975683895,
0.));
#143641=CARTESIAN_POINT('Ctrl Pts',(-71.1266089455517,-11.0077975683895,
12.));
#143642=CARTESIAN_POINT('Ctrl Pts',(-71.1031023560249,-11.0124162741224,
0.));
#143643=CARTESIAN_POINT('Ctrl Pts',(-71.1031023560249,-11.0124162741224,
12.));
#143644=CARTESIAN_POINT('Ctrl Pts',(-71.0796329878907,-11.0170038396915,
0.));
#143645=CARTESIAN_POINT('Ctrl Pts',(-71.0796329878907,-11.0170038396915,
12.));
#143646=CARTESIAN_POINT('Ctrl Pts',(-71.0562009714136,-11.0215603023856,
0.));
#143647=CARTESIAN_POINT('Ctrl Pts',(-71.0562009714136,-11.0215603023856,
12.));
#143648=CARTESIAN_POINT('Ctrl Pts',(-71.0328064373856,-11.0260856997415,
0.));
#143649=CARTESIAN_POINT('Ctrl Pts',(-71.0328064373856,-11.0260856997415,
12.));
#143650=CARTESIAN_POINT('Ctrl Pts',(-71.0094495171292,-11.0305800695456,
0.));
#143651=CARTESIAN_POINT('Ctrl Pts',(-71.0094495171292,-11.0305800695456,
12.));
#143652=CARTESIAN_POINT('Ctrl Pts',(-70.986130342497,-11.0350434498405,
0.));
#143653=CARTESIAN_POINT('Ctrl Pts',(-70.986130342497,-11.0350434498405,
12.));
#143654=CARTESIAN_POINT('Ctrl Pts',(-70.9628490458748,-11.0394758789285,
0.));
#143655=CARTESIAN_POINT('Ctrl Pts',(-70.9628490458748,-11.0394758789285,
12.));
#143656=CARTESIAN_POINT('Ctrl Pts',(-70.9396057601924,-11.0438773953681,
0.));
#143657=CARTESIAN_POINT('Ctrl Pts',(-70.9396057601924,-11.0438773953681,
12.));
#143658=CARTESIAN_POINT('Ctrl Pts',(-70.916400618927,-11.048248037975,0.));
#143659=CARTESIAN_POINT('Ctrl Pts',(-70.916400618927,-11.048248037975,12.));
#143660=CARTESIAN_POINT('Ctrl Pts',(-70.8932337561087,-11.0525878458243,
0.));
#143661=CARTESIAN_POINT('Ctrl Pts',(-70.8932337561087,-11.0525878458243,
12.));
#143662=CARTESIAN_POINT('Ctrl Pts',(-70.8701053063186,-11.0568968582569,
0.));
#143663=CARTESIAN_POINT('Ctrl Pts',(-70.8701053063186,-11.0568968582569,
12.));
#143664=CARTESIAN_POINT('Ctrl Pts',(-70.8470154046919,-11.0611751148835,
0.));
#143665=CARTESIAN_POINT('Ctrl Pts',(-70.8470154046919,-11.0611751148835,
12.));
#143666=CARTESIAN_POINT('Ctrl Pts',(-70.8239641869299,-11.0654226555802,
0.));
#143667=CARTESIAN_POINT('Ctrl Pts',(-70.8239641869299,-11.0654226555802,
12.));
#143668=CARTESIAN_POINT('Ctrl Pts',(-70.8009517893057,-11.0696395204909,
0.));
#143669=CARTESIAN_POINT('Ctrl Pts',(-70.8009517893057,-11.0696395204909,
12.));
#143670=CARTESIAN_POINT('Ctrl Pts',(-70.7779783486677,-11.073825750029,
0.));
#143671=CARTESIAN_POINT('Ctrl Pts',(-70.7779783486677,-11.073825750029,
12.));
#143672=CARTESIAN_POINT('Ctrl Pts',(-70.7550440024384,-11.0779813848846,
0.));
#143673=CARTESIAN_POINT('Ctrl Pts',(-70.7550440024384,-11.0779813848846,
12.));
#143674=CARTESIAN_POINT('Ctrl Pts',(-70.732148888618,-11.0821064660269,
0.));
#143675=CARTESIAN_POINT('Ctrl Pts',(-70.732148888618,-11.0821064660269,
12.));
#143676=CARTESIAN_POINT('Ctrl Pts',(-70.7092931457954,-11.0862010347016,
0.));
#143677=CARTESIAN_POINT('Ctrl Pts',(-70.7092931457954,-11.0862010347016,
12.));
#143678=CARTESIAN_POINT('Ctrl Pts',(-70.6864769131546,-11.0902651324323,
0.));
#143679=CARTESIAN_POINT('Ctrl Pts',(-70.6864769131546,-11.0902651324323,
12.));
#143680=CARTESIAN_POINT('Ctrl Pts',(-70.6637003304785,-11.0942988010233,
0.));
#143681=CARTESIAN_POINT('Ctrl Pts',(-70.6637003304785,-11.0942988010233,
12.));
#143682=CARTESIAN_POINT('Ctrl Pts',(-70.6409635381482,-11.0983020825667,
0.));
#143683=CARTESIAN_POINT('Ctrl Pts',(-70.6409635381482,-11.0983020825667,
12.));
#143684=CARTESIAN_POINT('Ctrl Pts',(-70.6182666771481,-11.1022750194445,
0.));
#143685=CARTESIAN_POINT('Ctrl Pts',(-70.6182666771481,-11.1022750194445,
12.));
#143686=CARTESIAN_POINT('Ctrl Pts',(-70.5956098890773,-11.1062176543262,
0.));
#143687=CARTESIAN_POINT('Ctrl Pts',(-70.5956098890773,-11.1062176543262,
12.));
#143688=CARTESIAN_POINT('Ctrl Pts',(-70.5729933161546,-11.1101300301701,
0.));
#143689=CARTESIAN_POINT('Ctrl Pts',(-70.5729933161546,-11.1101300301701,
12.));
#143690=CARTESIAN_POINT('Ctrl Pts',(-70.5504171012234,-11.1140121902271,
0.));
#143691=CARTESIAN_POINT('Ctrl Pts',(-70.5504171012234,-11.1140121902271,
12.));
#143692=CARTESIAN_POINT('Ctrl Pts',(-70.5278813877494,-11.1178641780476,
0.));
#143693=CARTESIAN_POINT('Ctrl Pts',(-70.5278813877494,-11.1178641780476,
12.));
#143694=CARTESIAN_POINT('Ctrl Pts',(-70.505386319828,-11.1216860374826,
0.));
#143695=CARTESIAN_POINT('Ctrl Pts',(-70.505386319828,-11.1216860374826,
12.));
#143696=CARTESIAN_POINT('Ctrl Pts',(-70.4829320421957,-11.1254778126821,
0.));
#143697=CARTESIAN_POINT('Ctrl Pts',(-70.4829320421957,-11.1254778126821,
12.));
#143698=CARTESIAN_POINT('Ctrl Pts',(-70.4605187002354,-11.1292395480974,
0.));
#143699=CARTESIAN_POINT('Ctrl Pts',(-70.4605187002354,-11.1292395480974,
12.));
#143700=CARTESIAN_POINT('Ctrl Pts',(-70.4381464399819,-11.1329712884846,
0.));
#143701=CARTESIAN_POINT('Ctrl Pts',(-70.4381464399819,-11.1329712884846,
12.));
#143702=CARTESIAN_POINT('Ctrl Pts',(-70.4158154081205,-11.1366730789125,
0.));
#143703=CARTESIAN_POINT('Ctrl Pts',(-70.4158154081205,-11.1366730789125,
12.));
#143704=CARTESIAN_POINT('Ctrl Pts',(-70.393525751996,-11.1403449647625,
0.));
#143705=CARTESIAN_POINT('Ctrl Pts',(-70.393525751996,-11.1403449647625,
12.));
#143706=CARTESIAN_POINT('Ctrl Pts',(-70.3712776196223,-11.143986991727,
0.));
#143707=CARTESIAN_POINT('Ctrl Pts',(-70.3712776196223,-11.143986991727,
12.));
#143708=CARTESIAN_POINT('Ctrl Pts',(-70.349071159688,-11.1475992058124,
0.));
#143709=CARTESIAN_POINT('Ctrl Pts',(-70.349071159688,-11.1475992058124,
12.));
#143710=CARTESIAN_POINT('Ctrl Pts',(-70.326906521559,-11.1511816533421,
0.));
#143711=CARTESIAN_POINT('Ctrl Pts',(-70.326906521559,-11.1511816533421,
12.));
#143712=CARTESIAN_POINT('Ctrl Pts',(-70.3047838552756,-11.1547343809646,
0.));
#143713=CARTESIAN_POINT('Ctrl Pts',(-70.3047838552756,-11.1547343809646,
12.));
#143714=CARTESIAN_POINT('Ctrl Pts',(-70.2827033115662,-11.158257435652,
0.));
#143715=CARTESIAN_POINT('Ctrl Pts',(-70.2827033115662,-11.158257435652,
12.));
#143716=CARTESIAN_POINT('Ctrl Pts',(-70.260665041859,-11.1617508647016,
0.));
#143717=CARTESIAN_POINT('Ctrl Pts',(-70.260665041859,-11.1617508647016,
12.));
#143718=CARTESIAN_POINT('Ctrl Pts',(-70.2386691982902,-11.1652147157383,
0.));
#143719=CARTESIAN_POINT('Ctrl Pts',(-70.2386691982902,-11.1652147157383,
12.));
#143720=CARTESIAN_POINT('Ctrl Pts',(-70.2167159337094,-11.168649036721,
0.));
#143721=CARTESIAN_POINT('Ctrl Pts',(-70.2167159337094,-11.168649036721,
12.));
#143722=CARTESIAN_POINT('Ctrl Pts',(-70.1948054016816,-11.1720538759499,
0.));
#143723=CARTESIAN_POINT('Ctrl Pts',(-70.1948054016816,-11.1720538759499,
12.));
#143724=CARTESIAN_POINT('Ctrl Pts',(-70.1729377564954,-11.1754292820631,
0.));
#143725=CARTESIAN_POINT('Ctrl Pts',(-70.1729377564954,-11.1754292820631,
12.));
#143726=CARTESIAN_POINT('Ctrl Pts',(-70.1511131531672,-11.1787753040363,
0.));
#143727=CARTESIAN_POINT('Ctrl Pts',(-70.1511131531672,-11.1787753040363,
12.));
#143728=CARTESIAN_POINT('Ctrl Pts',(-70.1293317474432,-11.1820919911846,
0.));
#143729=CARTESIAN_POINT('Ctrl Pts',(-70.1293317474432,-11.1820919911846,
12.));
#143730=CARTESIAN_POINT('Ctrl Pts',(-70.1075936957973,-11.185379393167,
0.));
#143731=CARTESIAN_POINT('Ctrl Pts',(-70.1075936957973,-11.185379393167,
12.));
#143732=CARTESIAN_POINT('Ctrl Pts',(-70.0858991554295,-11.1886375599916,
0.));
#143733=CARTESIAN_POINT('Ctrl Pts',(-70.0858991554295,-11.1886375599916,
12.));
#143734=CARTESIAN_POINT('Ctrl Pts',(-70.0642482842942,-11.1918665420168,
0.));
#143735=CARTESIAN_POINT('Ctrl Pts',(-70.0642482842942,-11.1918665420168,
12.));
#143736=CARTESIAN_POINT('Ctrl Pts',(-70.0426412411194,-11.1950663899578,
0.));
#143737=CARTESIAN_POINT('Ctrl Pts',(-70.0426412411194,-11.1950663899578,
12.));
#143738=CARTESIAN_POINT('Ctrl Pts',(-70.0210781854236,-11.1982371548918,
0.));
#143739=CARTESIAN_POINT('Ctrl Pts',(-70.0210781854236,-11.1982371548918,
12.));
#143740=CARTESIAN_POINT('Ctrl Pts',(-69.9995592775322,-11.2013788882711,
0.));
#143741=CARTESIAN_POINT('Ctrl Pts',(-69.9995592775322,-11.2013788882711,
12.));
#143742=CARTESIAN_POINT('Ctrl Pts',(-69.9780846785771,-11.2044916419239,
0.));
#143743=CARTESIAN_POINT('Ctrl Pts',(-69.9780846785771,-11.2044916419239,
12.));
#143744=CARTESIAN_POINT('Ctrl Pts',(-69.9566545504813,-11.2075754680445,
0.));
#143745=CARTESIAN_POINT('Ctrl Pts',(-69.9566545504813,-11.2075754680445,
12.));
#143746=CARTESIAN_POINT('Ctrl Pts',(-69.9352690559399,-11.2106304191881,
0.));
#143747=CARTESIAN_POINT('Ctrl Pts',(-69.9352690559399,-11.2106304191881,
12.));
#143748=CARTESIAN_POINT('Ctrl Pts',(-69.9139283584036,-11.2136565482679,
0.));
#143749=CARTESIAN_POINT('Ctrl Pts',(-69.9139283584036,-11.2136565482679,
12.));
#143750=CARTESIAN_POINT('Ctrl Pts',(-69.8926326220414,-11.2166539085527,
0.));
#143751=CARTESIAN_POINT('Ctrl Pts',(-69.8926326220414,-11.2166539085527,
12.));
#143752=CARTESIAN_POINT('Ctrl Pts',(-69.8713820117918,-11.2196225536794,
0.));
#143753=CARTESIAN_POINT('Ctrl Pts',(-69.8713820117918,-11.2196225536794,
12.));
#143754=CARTESIAN_POINT('Ctrl Pts',(-69.8501766934445,-11.2225625376739,
0.));
#143755=CARTESIAN_POINT('Ctrl Pts',(-69.8501766934445,-11.2225625376739,
12.));
#143756=CARTESIAN_POINT('Ctrl Pts',(-69.8290168337076,-11.225473914972,
0.));
#143757=CARTESIAN_POINT('Ctrl Pts',(-69.8290168337076,-11.225473914972,
12.));
#143758=CARTESIAN_POINT('Ctrl Pts',(-69.8079026002753,-11.2283567404434,
0.));
#143759=CARTESIAN_POINT('Ctrl Pts',(-69.8079026002753,-11.2283567404434,
12.));
#143760=CARTESIAN_POINT('Ctrl Pts',(-69.7868341618927,-11.2312110694183,
0.));
#143761=CARTESIAN_POINT('Ctrl Pts',(-69.7868341618927,-11.2312110694183,
12.));
#143762=CARTESIAN_POINT('Ctrl Pts',(-69.7658116882298,-11.2340369576452,
0.));
#143763=CARTESIAN_POINT('Ctrl Pts',(-69.7658116882298,-11.2340369576452,
12.));
#143764=CARTESIAN_POINT('Ctrl Pts',(-69.7448353497394,-11.236834461247,
0.));
#143765=CARTESIAN_POINT('Ctrl Pts',(-69.7448353497394,-11.236834461247,
12.));
#143766=CARTESIAN_POINT('Ctrl Pts',(-69.7239053175362,-11.2396036366861,
0.));
#143767=CARTESIAN_POINT('Ctrl Pts',(-69.7239053175362,-11.2396036366861,
12.));
#143768=CARTESIAN_POINT('Ctrl Pts',(-69.7030217632187,-11.242344540717,
0.));
#143769=CARTESIAN_POINT('Ctrl Pts',(-69.7030217632187,-11.242344540717,
12.));
#143770=CARTESIAN_POINT('Ctrl Pts',(-69.6821848588492,-11.2450572303847,
0.));
#143771=CARTESIAN_POINT('Ctrl Pts',(-69.6821848588492,-11.2450572303847,
12.));
#143772=CARTESIAN_POINT('Ctrl Pts',(-69.6613947773563,-11.247741763139,
0.));
#143773=CARTESIAN_POINT('Ctrl Pts',(-69.6613947773563,-11.247741763139,
12.));
#143774=CARTESIAN_POINT('Ctrl Pts',(-69.6406516928902,-11.2503981969413,
0.));
#143775=CARTESIAN_POINT('Ctrl Pts',(-69.6406516928902,-11.2503981969413,
12.));
#143776=CARTESIAN_POINT('Ctrl Pts',(-69.6199557811231,-11.2530265903555,
0.));
#143777=CARTESIAN_POINT('Ctrl Pts',(-69.6199557811231,-11.2530265903555,
12.));
#143778=CARTESIAN_POINT('Ctrl Pts',(-69.5993072197355,-11.255627002701,
0.));
#143779=CARTESIAN_POINT('Ctrl Pts',(-69.5993072197355,-11.255627002701,
12.));
#143780=CARTESIAN_POINT('Ctrl Pts',(-69.5787061880815,-11.2581994939534,
0.));
#143781=CARTESIAN_POINT('Ctrl Pts',(-69.5787061880815,-11.2581994939534,
12.));
#143782=CARTESIAN_POINT('Ctrl Pts',(-69.5581528662846,-11.2607441244698,
0.));
#143783=CARTESIAN_POINT('Ctrl Pts',(-69.5581528662846,-11.2607441244698,
12.));
#143784=CARTESIAN_POINT('Ctrl Pts',(-69.5376474344768,-11.2632609547629,
0.));
#143785=CARTESIAN_POINT('Ctrl Pts',(-69.5376474344768,-11.2632609547629,
12.));
#143786=CARTESIAN_POINT('Ctrl Pts',(-69.5171900720188,-11.265750045272,
0.));
#143787=CARTESIAN_POINT('Ctrl Pts',(-69.5171900720188,-11.265750045272,
12.));
#143788=CARTESIAN_POINT('Ctrl Pts',(-69.4967809565978,-11.2682114561015,
0.));
#143789=CARTESIAN_POINT('Ctrl Pts',(-69.4967809565978,-11.2682114561015,
12.));
#143790=CARTESIAN_POINT('Ctrl Pts',(-69.4764202659443,-11.2706452475287,
0.));
#143791=CARTESIAN_POINT('Ctrl Pts',(-69.4764202659443,-11.2706452475287,
12.));
#143792=CARTESIAN_POINT('Ctrl Pts',(-69.4561081798815,-11.2730514806143,
0.));
#143793=CARTESIAN_POINT('Ctrl Pts',(-69.4561081798815,-11.2730514806143,
12.));
#143794=CARTESIAN_POINT('Ctrl Pts',(-69.4358448819957,-11.2754302177019,
0.));
#143795=CARTESIAN_POINT('Ctrl Pts',(-69.4358448819957,-11.2754302177019,
12.));
#143796=CARTESIAN_POINT('Ctrl Pts',(-69.4156305620554,-11.2777815231462,
0.));
#143797=CARTESIAN_POINT('Ctrl Pts',(-69.4156305620554,-11.2777815231462,
12.));
#143798=CARTESIAN_POINT('Ctrl Pts',(-69.395465416223,-11.2801054633807,
0.));
#143799=CARTESIAN_POINT('Ctrl Pts',(-69.395465416223,-11.2801054633807,
12.));
#143800=CARTESIAN_POINT('Ctrl Pts',(-69.375349642,-11.2824021054038,0.));
#143801=CARTESIAN_POINT('Ctrl Pts',(-69.375349642,-11.2824021054038,12.));
#143802=CARTESIAN_POINT('Ctrl Pts',(-69.3552834337771,-11.2846715154521,
0.));
#143803=CARTESIAN_POINT('Ctrl Pts',(-69.3552834337771,-11.2846715154521,
12.));
#143804=CARTESIAN_POINT('Ctrl Pts',(-69.3352669789611,-11.2869137578463,
0.));
#143805=CARTESIAN_POINT('Ctrl Pts',(-69.3352669789611,-11.2869137578463,
12.));
#143806=CARTESIAN_POINT('Ctrl Pts',(-69.315300451784,-11.2891288931528,
0.));
#143807=CARTESIAN_POINT('Ctrl Pts',(-69.315300451784,-11.2891288931528,
12.));
#143808=CARTESIAN_POINT('Ctrl Pts',(-69.2953840192792,-11.2913169799642,
0.));
#143809=CARTESIAN_POINT('Ctrl Pts',(-69.2953840192792,-11.2913169799642,
12.));
#143810=CARTESIAN_POINT('Ctrl Pts',(-69.2755178531534,-11.2934780784361,
0.));
#143811=CARTESIAN_POINT('Ctrl Pts',(-69.2755178531534,-11.2934780784361,
12.));
#143812=CARTESIAN_POINT('Ctrl Pts',(-69.255702139335,-11.2956122531375,
0.));
#143813=CARTESIAN_POINT('Ctrl Pts',(-69.255702139335,-11.2956122531375,
12.));
#143814=CARTESIAN_POINT('Ctrl Pts',(-69.2359370894828,-11.2977195764836,
0.));
#143815=CARTESIAN_POINT('Ctrl Pts',(-69.2359370894828,-11.2977195764836,
12.));
#143816=CARTESIAN_POINT('Ctrl Pts',(-69.216222948839,-11.2998001310934,
0.));
#143817=CARTESIAN_POINT('Ctrl Pts',(-69.216222948839,-11.2998001310934,
12.));
#143818=CARTESIAN_POINT('Ctrl Pts',(-69.1965599718761,-11.3018540025605,
0.));
#143819=CARTESIAN_POINT('Ctrl Pts',(-69.1965599718761,-11.3018540025605,
12.));
#143820=CARTESIAN_POINT('Ctrl Pts',(-69.1769483991639,-11.3038812726275,
0.));
#143821=CARTESIAN_POINT('Ctrl Pts',(-69.1769483991639,-11.3038812726275,
12.));
#143822=CARTESIAN_POINT('Ctrl Pts',(-69.1573884361076,-11.3058820128323,
0.));
#143823=CARTESIAN_POINT('Ctrl Pts',(-69.1573884361076,-11.3058820128323,
12.));
#143824=CARTESIAN_POINT('Ctrl Pts',(-69.137880225198,-11.3078562764442,
0.));
#143825=CARTESIAN_POINT('Ctrl Pts',(-69.137880225198,-11.3078562764442,
12.));
#143826=CARTESIAN_POINT('Ctrl Pts',(-69.1184238445065,-11.3098040973799,
0.));
#143827=CARTESIAN_POINT('Ctrl Pts',(-69.1184238445065,-11.3098040973799,
12.));
#143828=CARTESIAN_POINT('Ctrl Pts',(-69.1029002322497,-11.3113412156742,
0.));
#143829=CARTESIAN_POINT('Ctrl Pts',(-69.1029002322497,-11.3113412156742,
12.));
#143830=CARTESIAN_POINT('Ctrl Pts',(-69.0912808657051,-11.3124821678849,
0.));
#143831=CARTESIAN_POINT('Ctrl Pts',(-69.0912808657051,-11.3124821678849,
12.));
#143832=CARTESIAN_POINT('Ctrl Pts',(-69.0835449954486,-11.3132375200184,
0.));
#143833=CARTESIAN_POINT('Ctrl Pts',(-69.0835449954486,-11.3132375200184,
12.));
#143834=CARTESIAN_POINT('Ctrl Pts',(-69.079679653846,-11.3136138754165,
0.));
#143835=CARTESIAN_POINT('Ctrl Pts',(-69.079679653846,-11.3136138754165,
12.));
#143836=CARTESIAN_POINT('',(-69.079679653846,-11.3136138754165,12.));
#143837=CARTESIAN_POINT('Ctrl Pts',(-69.079679653846,-11.3136138754165,
12.));
#143838=CARTESIAN_POINT('Ctrl Pts',(-69.0835449954486,-11.3132375200184,
12.));
#143839=CARTESIAN_POINT('Ctrl Pts',(-69.0912808657051,-11.3124821678849,
12.));
#143840=CARTESIAN_POINT('Ctrl Pts',(-69.1029002322497,-11.3113412156742,
12.));
#143841=CARTESIAN_POINT('Ctrl Pts',(-69.1184238445065,-11.3098040973799,
12.));
#143842=CARTESIAN_POINT('Ctrl Pts',(-69.137880225198,-11.3078562764442,
12.));
#143843=CARTESIAN_POINT('Ctrl Pts',(-69.1573884361076,-11.3058820128323,
12.));
#143844=CARTESIAN_POINT('Ctrl Pts',(-69.1769483991639,-11.3038812726275,
12.));
#143845=CARTESIAN_POINT('Ctrl Pts',(-69.1965599718761,-11.3018540025605,
12.));
#143846=CARTESIAN_POINT('Ctrl Pts',(-69.216222948839,-11.2998001310934,
12.));
#143847=CARTESIAN_POINT('Ctrl Pts',(-69.2359370894828,-11.2977195764836,
12.));
#143848=CARTESIAN_POINT('Ctrl Pts',(-69.255702139335,-11.2956122531375,
12.));
#143849=CARTESIAN_POINT('Ctrl Pts',(-69.2755178531534,-11.2934780784361,
12.));
#143850=CARTESIAN_POINT('Ctrl Pts',(-69.2953840192792,-11.2913169799642,
12.));
#143851=CARTESIAN_POINT('Ctrl Pts',(-69.315300451784,-11.2891288931528,
12.));
#143852=CARTESIAN_POINT('Ctrl Pts',(-69.3352669789611,-11.2869137578463,
12.));
#143853=CARTESIAN_POINT('Ctrl Pts',(-69.3552834337771,-11.2846715154521,
12.));
#143854=CARTESIAN_POINT('Ctrl Pts',(-69.375349642,-11.2824021054038,12.));
#143855=CARTESIAN_POINT('Ctrl Pts',(-69.395465416223,-11.2801054633807,
12.));
#143856=CARTESIAN_POINT('Ctrl Pts',(-69.4156305620554,-11.2777815231462,
12.));
#143857=CARTESIAN_POINT('Ctrl Pts',(-69.4358448819957,-11.2754302177019,
12.));
#143858=CARTESIAN_POINT('Ctrl Pts',(-69.4561081798815,-11.2730514806143,
12.));
#143859=CARTESIAN_POINT('Ctrl Pts',(-69.4764202659443,-11.2706452475287,
12.));
#143860=CARTESIAN_POINT('Ctrl Pts',(-69.4967809565978,-11.2682114561015,
12.));
#143861=CARTESIAN_POINT('Ctrl Pts',(-69.5171900720188,-11.265750045272,
12.));
#143862=CARTESIAN_POINT('Ctrl Pts',(-69.5376474344768,-11.2632609547629,
12.));
#143863=CARTESIAN_POINT('Ctrl Pts',(-69.5581528662846,-11.2607441244698,
12.));
#143864=CARTESIAN_POINT('Ctrl Pts',(-69.5787061880815,-11.2581994939534,
12.));
#143865=CARTESIAN_POINT('Ctrl Pts',(-69.5993072197355,-11.255627002701,
12.));
#143866=CARTESIAN_POINT('Ctrl Pts',(-69.6199557811231,-11.2530265903555,
12.));
#143867=CARTESIAN_POINT('Ctrl Pts',(-69.6406516928902,-11.2503981969413,
12.));
#143868=CARTESIAN_POINT('Ctrl Pts',(-69.6613947773563,-11.247741763139,
12.));
#143869=CARTESIAN_POINT('Ctrl Pts',(-69.6821848588492,-11.2450572303847,
12.));
#143870=CARTESIAN_POINT('Ctrl Pts',(-69.7030217632187,-11.242344540717,
12.));
#143871=CARTESIAN_POINT('Ctrl Pts',(-69.7239053175362,-11.2396036366861,
12.));
#143872=CARTESIAN_POINT('Ctrl Pts',(-69.7448353497394,-11.236834461247,
12.));
#143873=CARTESIAN_POINT('Ctrl Pts',(-69.7658116882298,-11.2340369576452,
12.));
#143874=CARTESIAN_POINT('Ctrl Pts',(-69.7868341618927,-11.2312110694183,
12.));
#143875=CARTESIAN_POINT('Ctrl Pts',(-69.8079026002753,-11.2283567404434,
12.));
#143876=CARTESIAN_POINT('Ctrl Pts',(-69.8290168337076,-11.225473914972,
12.));
#143877=CARTESIAN_POINT('Ctrl Pts',(-69.8501766934445,-11.2225625376739,
12.));
#143878=CARTESIAN_POINT('Ctrl Pts',(-69.8713820117918,-11.2196225536794,
12.));
#143879=CARTESIAN_POINT('Ctrl Pts',(-69.8926326220414,-11.2166539085527,
12.));
#143880=CARTESIAN_POINT('Ctrl Pts',(-69.9139283584036,-11.2136565482679,
12.));
#143881=CARTESIAN_POINT('Ctrl Pts',(-69.9352690559399,-11.2106304191881,
12.));
#143882=CARTESIAN_POINT('Ctrl Pts',(-69.9566545504813,-11.2075754680445,
12.));
#143883=CARTESIAN_POINT('Ctrl Pts',(-69.9780846785771,-11.2044916419239,
12.));
#143884=CARTESIAN_POINT('Ctrl Pts',(-69.9995592775322,-11.2013788882711,
12.));
#143885=CARTESIAN_POINT('Ctrl Pts',(-70.0210781854236,-11.1982371548918,
12.));
#143886=CARTESIAN_POINT('Ctrl Pts',(-70.0426412411194,-11.1950663899578,
12.));
#143887=CARTESIAN_POINT('Ctrl Pts',(-70.0642482842942,-11.1918665420168,
12.));
#143888=CARTESIAN_POINT('Ctrl Pts',(-70.0858991554295,-11.1886375599916,
12.));
#143889=CARTESIAN_POINT('Ctrl Pts',(-70.1075936957973,-11.185379393167,
12.));
#143890=CARTESIAN_POINT('Ctrl Pts',(-70.1293317474432,-11.1820919911846,
12.));
#143891=CARTESIAN_POINT('Ctrl Pts',(-70.1511131531672,-11.1787753040363,
12.));
#143892=CARTESIAN_POINT('Ctrl Pts',(-70.1729377564954,-11.1754292820631,
12.));
#143893=CARTESIAN_POINT('Ctrl Pts',(-70.1948054016816,-11.1720538759499,
12.));
#143894=CARTESIAN_POINT('Ctrl Pts',(-70.2167159337094,-11.168649036721,
12.));
#143895=CARTESIAN_POINT('Ctrl Pts',(-70.2386691982902,-11.1652147157383,
12.));
#143896=CARTESIAN_POINT('Ctrl Pts',(-70.260665041859,-11.1617508647016,
12.));
#143897=CARTESIAN_POINT('Ctrl Pts',(-70.2827033115662,-11.158257435652,
12.));
#143898=CARTESIAN_POINT('Ctrl Pts',(-70.3047838552756,-11.1547343809646,
12.));
#143899=CARTESIAN_POINT('Ctrl Pts',(-70.326906521559,-11.1511816533421,
12.));
#143900=CARTESIAN_POINT('Ctrl Pts',(-70.349071159688,-11.1475992058124,
12.));
#143901=CARTESIAN_POINT('Ctrl Pts',(-70.3712776196223,-11.143986991727,
12.));
#143902=CARTESIAN_POINT('Ctrl Pts',(-70.393525751996,-11.1403449647625,
12.));
#143903=CARTESIAN_POINT('Ctrl Pts',(-70.4158154081205,-11.1366730789125,
12.));
#143904=CARTESIAN_POINT('Ctrl Pts',(-70.4381464399819,-11.1329712884846,
12.));
#143905=CARTESIAN_POINT('Ctrl Pts',(-70.4605187002354,-11.1292395480974,
12.));
#143906=CARTESIAN_POINT('Ctrl Pts',(-70.4829320421957,-11.1254778126821,
12.));
#143907=CARTESIAN_POINT('Ctrl Pts',(-70.505386319828,-11.1216860374826,
12.));
#143908=CARTESIAN_POINT('Ctrl Pts',(-70.5278813877494,-11.1178641780476,
12.));
#143909=CARTESIAN_POINT('Ctrl Pts',(-70.5504171012234,-11.1140121902271,
12.));
#143910=CARTESIAN_POINT('Ctrl Pts',(-70.5729933161546,-11.1101300301701,
12.));
#143911=CARTESIAN_POINT('Ctrl Pts',(-70.5956098890773,-11.1062176543262,
12.));
#143912=CARTESIAN_POINT('Ctrl Pts',(-70.6182666771481,-11.1022750194445,
12.));
#143913=CARTESIAN_POINT('Ctrl Pts',(-70.6409635381482,-11.0983020825667,
12.));
#143914=CARTESIAN_POINT('Ctrl Pts',(-70.6637003304785,-11.0942988010233,
12.));
#143915=CARTESIAN_POINT('Ctrl Pts',(-70.6864769131546,-11.0902651324323,
12.));
#143916=CARTESIAN_POINT('Ctrl Pts',(-70.7092931457954,-11.0862010347016,
12.));
#143917=CARTESIAN_POINT('Ctrl Pts',(-70.732148888618,-11.0821064660269,
12.));
#143918=CARTESIAN_POINT('Ctrl Pts',(-70.7550440024384,-11.0779813848846,
12.));
#143919=CARTESIAN_POINT('Ctrl Pts',(-70.7779783486677,-11.073825750029,
12.));
#143920=CARTESIAN_POINT('Ctrl Pts',(-70.8009517893057,-11.0696395204909,
12.));
#143921=CARTESIAN_POINT('Ctrl Pts',(-70.8239641869299,-11.0654226555802,
12.));
#143922=CARTESIAN_POINT('Ctrl Pts',(-70.8470154046919,-11.0611751148835,
12.));
#143923=CARTESIAN_POINT('Ctrl Pts',(-70.8701053063186,-11.0568968582569,
12.));
#143924=CARTESIAN_POINT('Ctrl Pts',(-70.8932337561087,-11.0525878458243,
12.));
#143925=CARTESIAN_POINT('Ctrl Pts',(-70.916400618927,-11.048248037975,12.));
#143926=CARTESIAN_POINT('Ctrl Pts',(-70.9396057601924,-11.0438773953681,
12.));
#143927=CARTESIAN_POINT('Ctrl Pts',(-70.9628490458748,-11.0394758789285,
12.));
#143928=CARTESIAN_POINT('Ctrl Pts',(-70.986130342497,-11.0350434498405,
12.));
#143929=CARTESIAN_POINT('Ctrl Pts',(-71.0094495171292,-11.0305800695456,
12.));
#143930=CARTESIAN_POINT('Ctrl Pts',(-71.0328064373856,-11.0260856997415,
12.));
#143931=CARTESIAN_POINT('Ctrl Pts',(-71.0562009714136,-11.0215603023856,
12.));
#143932=CARTESIAN_POINT('Ctrl Pts',(-71.0796329878907,-11.0170038396915,
12.));
#143933=CARTESIAN_POINT('Ctrl Pts',(-71.1031023560249,-11.0124162741224,
12.));
#143934=CARTESIAN_POINT('Ctrl Pts',(-71.1266089455517,-11.0077975683895,
12.));
#143935=CARTESIAN_POINT('Ctrl Pts',(-71.1501526267286,-11.0031476854502,
12.));
#143936=CARTESIAN_POINT('Ctrl Pts',(-71.1737332703248,-10.9984665885127,
12.));
#143937=CARTESIAN_POINT('Ctrl Pts',(-71.1973507476191,-10.993754241032,
12.));
#143938=CARTESIAN_POINT('Ctrl Pts',(-71.2210049304014,-10.9890106067039,
12.));
#143939=CARTESIAN_POINT('Ctrl Pts',(-71.2446956909687,-10.9842356494627,
12.));
#143940=CARTESIAN_POINT('Ctrl Pts',(-71.2684229021207,-10.9794293334805,
12.));
#143941=CARTESIAN_POINT('Ctrl Pts',(-71.2921864371491,-10.9745916231709,
12.));
#143942=CARTESIAN_POINT('Ctrl Pts',(-71.3159861698358,-10.969722483186,
12.));
#143943=CARTESIAN_POINT('Ctrl Pts',(-71.339821974454,-10.9648218784098,
12.));
#143944=CARTESIAN_POINT('Ctrl Pts',(-71.3636937257649,-10.9598897739564,
12.));
#143945=CARTESIAN_POINT('Ctrl Pts',(-71.3876012990138,-10.954926135169,
12.));
#143946=CARTESIAN_POINT('Ctrl Pts',(-71.4115445699194,-10.9499309276236,
12.));
#143947=CARTESIAN_POINT('Ctrl Pts',(-71.435523414672,-10.944904117127,12.));
#143948=CARTESIAN_POINT('Ctrl Pts',(-71.4595377099351,-10.9398456697095,
12.));
#143949=CARTESIAN_POINT('Ctrl Pts',(-71.4835873328423,-10.9347555516235,
12.));
#143950=CARTESIAN_POINT('Ctrl Pts',(-71.5076721609937,-10.9296337293424,
12.));
#143951=CARTESIAN_POINT('Ctrl Pts',(-71.5317920724459,-10.9244801695642,
12.));
#143952=CARTESIAN_POINT('Ctrl Pts',(-71.5559469457091,-10.91929483921,12.));
#143953=CARTESIAN_POINT('Ctrl Pts',(-71.5801366597488,-10.914077705417,
12.));
#143954=CARTESIAN_POINT('Ctrl Pts',(-71.6043610939835,-10.9088287355365,
12.));
#143955=CARTESIAN_POINT('Ctrl Pts',(-71.6286201282812,-10.9035478971328,
12.));
#143956=CARTESIAN_POINT('Ctrl Pts',(-71.6529136429504,-10.8982351579871,
12.));
#143957=CARTESIAN_POINT('Ctrl Pts',(-71.6772415187364,-10.8928904860964,
12.));
#143958=CARTESIAN_POINT('Ctrl Pts',(-71.7016036368236,-10.8875138496671,
12.));
#143959=CARTESIAN_POINT('Ctrl Pts',(-71.7259998788328,-10.882105217112,
12.));
#143960=CARTESIAN_POINT('Ctrl Pts',(-71.7504301268181,-10.8766645570497,
12.));
#143961=CARTESIAN_POINT('Ctrl Pts',(-71.7748942632593,-10.8711918383073,
12.));
#143962=CARTESIAN_POINT('Ctrl Pts',(-71.7993921710564,-10.865687029922,
12.));
#143963=CARTESIAN_POINT('Ctrl Pts',(-71.8239237335331,-10.8601501011332,
12.));
#143964=CARTESIAN_POINT('Ctrl Pts',(-71.8484888344339,-10.8545810213799,
12.));
#143965=CARTESIAN_POINT('Ctrl Pts',(-71.8730873579224,-10.8489797602997,
12.));
#143966=CARTESIAN_POINT('Ctrl Pts',(-71.8977191885725,-10.8433462877311,
12.));
#143967=CARTESIAN_POINT('Ctrl Pts',(-71.9223842113625,-10.8376805737159,
12.));
#143968=CARTESIAN_POINT('Ctrl Pts',(-71.9470823116785,-10.8319825884918,
12.));
#143969=CARTESIAN_POINT('Ctrl Pts',(-71.9718133753127,-10.8262523024898,
12.));
#143970=CARTESIAN_POINT('Ctrl Pts',(-71.9965772884619,-10.8204896863328,
12.));
#143971=CARTESIAN_POINT('Ctrl Pts',(-72.0213739377223,-10.8146947108375,
12.));
#143972=CARTESIAN_POINT('Ctrl Pts',(-72.0462032100815,-10.8088673470184,
12.));
#143973=CARTESIAN_POINT('Ctrl Pts',(-72.0710649929202,-10.8030075660808,
12.));
#143974=CARTESIAN_POINT('Ctrl Pts',(-72.0959591740114,-10.7971153394166,
12.));
#143975=CARTESIAN_POINT('Ctrl Pts',(-72.1208856415171,-10.7911906386027,
12.));
#143976=CARTESIAN_POINT('Ctrl Pts',(-72.1458442839834,-10.7852334354016,
12.));
#143977=CARTESIAN_POINT('Ctrl Pts',(-72.1708349903305,-10.7792437017662,
12.));
#143978=CARTESIAN_POINT('Ctrl Pts',(-72.1958576498558,-10.7732214098344,
12.));
#143979=CARTESIAN_POINT('Ctrl Pts',(-72.2209121522366,-10.7671665319255,
12.));
#143980=CARTESIAN_POINT('Ctrl Pts',(-72.2459983875296,-10.7610790405385,
12.));
#143981=CARTESIAN_POINT('Ctrl Pts',(-72.2711162461681,-10.7549589083535,
12.));
#143982=CARTESIAN_POINT('Ctrl Pts',(-72.2962656189556,-10.7488061082367,
12.));
#143983=CARTESIAN_POINT('Ctrl Pts',(-72.3214463970641,-10.7426206132375,
12.));
#143984=CARTESIAN_POINT('Ctrl Pts',(-72.3466584720318,-10.73640239658,12.));
#143985=CARTESIAN_POINT('Ctrl Pts',(-72.3719017357571,-10.7301514316607,
12.));
#143986=CARTESIAN_POINT('Ctrl Pts',(-72.3971760804933,-10.7238676920469,
12.));
#143987=CARTESIAN_POINT('Ctrl Pts',(-72.4224813988347,-10.7175511514788,
12.));
#143988=CARTESIAN_POINT('Ctrl Pts',(-72.4478175837156,-10.7112017838706,
12.));
#143989=CARTESIAN_POINT('Ctrl Pts',(-72.4731845284227,-10.7048195633061,
12.));
#143990=CARTESIAN_POINT('Ctrl Pts',(-72.4985821266023,-10.6984044640398,
12.));
#143991=CARTESIAN_POINT('Ctrl Pts',(-72.5240102722664,-10.691956460499,
12.));
#143992=CARTESIAN_POINT('Ctrl Pts',(-72.5494688597961,-10.6854755272904,
12.));
#143993=CARTESIAN_POINT('Ctrl Pts',(-72.5749577839415,-10.6789616392042,
12.));
#143994=CARTESIAN_POINT('Ctrl Pts',(-72.6004769398019,-10.6724147711995,
12.));
#143995=CARTESIAN_POINT('Ctrl Pts',(-72.6260262228065,-10.6658348983944,
12.));
#143996=CARTESIAN_POINT('Ctrl Pts',(-72.651605528691,-10.659221996058,12.));
#143997=CARTESIAN_POINT('Ctrl Pts',(-72.6772147534752,-10.6525760396054,
12.));
#143998=CARTESIAN_POINT('Ctrl Pts',(-72.7028537934317,-10.6458970045946,
12.));
#143999=CARTESIAN_POINT('Ctrl Pts',(-72.7285225451293,-10.6391848667352,
12.));
#144000=CARTESIAN_POINT('Ctrl Pts',(-72.7542209054812,-10.6324396018998,
12.));
#144001=CARTESIAN_POINT('Ctrl Pts',(-72.7799487717911,-10.6256611861394,
12.));
#144002=CARTESIAN_POINT('Ctrl Pts',(-72.8057060417887,-10.6188495956973,
12.));
#144003=CARTESIAN_POINT('Ctrl Pts',(-72.8314926136881,-10.6120048070367,
12.));
#144004=CARTESIAN_POINT('Ctrl Pts',(-72.8573083861337,-10.6051267968203,
12.));
#144005=CARTESIAN_POINT('Ctrl Pts',(-72.8831532580845,-10.5982155418626,
12.));
#144006=CARTESIAN_POINT('Ctrl Pts',(-72.9090271287083,-10.5912710190928,
12.));
#144007=CARTESIAN_POINT('Ctrl Pts',(-72.9349298972822,-10.5842932055209,
12.));
#144008=CARTESIAN_POINT('Ctrl Pts',(-72.9608614630534,-10.5772820781958,
12.));
#144009=CARTESIAN_POINT('Ctrl Pts',(-72.9868217252283,-10.570237614205,
12.));
#144010=CARTESIAN_POINT('Ctrl Pts',(-73.0128105832621,-10.5631597907651,
12.));
#144011=CARTESIAN_POINT('Ctrl Pts',(-73.0388279370834,-10.5560485852974,
12.));
#144012=CARTESIAN_POINT('Ctrl Pts',(-73.0648736873434,-10.5489039755138,
12.));
#144013=CARTESIAN_POINT('Ctrl Pts',(-73.0909477356474,-10.5417259395003,
12.));
#144014=CARTESIAN_POINT('Ctrl Pts',(-73.1170499848039,-10.53451445581,12.));
#144015=CARTESIAN_POINT('Ctrl Pts',(-73.1431803382711,-10.5272695032653,
12.));
#144016=CARTESIAN_POINT('Ctrl Pts',(-73.1693386996138,-10.5199910607654,
12.));
#144017=CARTESIAN_POINT('Ctrl Pts',(-73.1955249719048,-10.5126791070805,
12.));
#144018=CARTESIAN_POINT('Ctrl Pts',(-73.2217390572562,-10.5053336206908,
12.));
#144019=CARTESIAN_POINT('Ctrl Pts',(-73.2479808560189,-10.4979545795192,
12.));
#144020=CARTESIAN_POINT('Ctrl Pts',(-73.2742502674304,-10.4905419611523,
12.));
#144021=CARTESIAN_POINT('Ctrl Pts',(-73.3005471910583,-10.4830957433305,
12.));
#144022=CARTESIAN_POINT('Ctrl Pts',(-73.3268715280575,-10.4756159043806,
12.));
#144023=CARTESIAN_POINT('Ctrl Pts',(-73.3532231823659,-10.4681024236289,
12.));
#144024=CARTESIAN_POINT('Ctrl Pts',(-73.37960206225,-10.4605552819397,12.));
#144025=CARTESIAN_POINT('Ctrl Pts',(-73.4060080806686,-10.452974461845,
12.));
#144026=CARTESIAN_POINT('Ctrl Pts',(-73.4286663448108,-10.4464473465479,
12.));
#144027=CARTESIAN_POINT('Ctrl Pts',(-73.4460525528801,-10.4414249334738,
12.));
#144028=CARTESIAN_POINT('Ctrl Pts',(-73.458154743684,-10.437922150104,12.));
#144029=CARTESIAN_POINT('Ctrl Pts',(-73.4649650361896,-10.4359488742808,
12.));
#144030=CARTESIAN_POINT('Ctrl Pts',(-73.4664795929942,-10.4355099267295,
12.));
#144031=CARTESIAN_POINT('',(-69.079679653846,-11.3136138754165,0.));
#144032=CARTESIAN_POINT('',(-69.079679653846,-11.3136138754165,0.));
#144033=CARTESIAN_POINT('Ctrl Pts',(-73.4664795929942,-10.4355099267295,
0.));
#144034=CARTESIAN_POINT('Ctrl Pts',(-73.4649650361896,-10.4359488742808,
0.));
#144035=CARTESIAN_POINT('Ctrl Pts',(-73.458154743684,-10.437922150104,0.));
#144036=CARTESIAN_POINT('Ctrl Pts',(-73.4460525528801,-10.4414249334738,
0.));
#144037=CARTESIAN_POINT('Ctrl Pts',(-73.4286663448108,-10.4464473465479,
0.));
#144038=CARTESIAN_POINT('Ctrl Pts',(-73.4060080806686,-10.452974461845,
0.));
#144039=CARTESIAN_POINT('Ctrl Pts',(-73.37960206225,-10.4605552819397,0.));
#144040=CARTESIAN_POINT('Ctrl Pts',(-73.3532231823659,-10.4681024236289,
0.));
#144041=CARTESIAN_POINT('Ctrl Pts',(-73.3268715280575,-10.4756159043806,
0.));
#144042=CARTESIAN_POINT('Ctrl Pts',(-73.3005471910583,-10.4830957433305,
0.));
#144043=CARTESIAN_POINT('Ctrl Pts',(-73.2742502674304,-10.4905419611523,
0.));
#144044=CARTESIAN_POINT('Ctrl Pts',(-73.2479808560189,-10.4979545795192,
0.));
#144045=CARTESIAN_POINT('Ctrl Pts',(-73.2217390572562,-10.5053336206908,
0.));
#144046=CARTESIAN_POINT('Ctrl Pts',(-73.1955249719048,-10.5126791070805,
0.));
#144047=CARTESIAN_POINT('Ctrl Pts',(-73.1693386996138,-10.5199910607654,
0.));
#144048=CARTESIAN_POINT('Ctrl Pts',(-73.1431803382711,-10.5272695032653,
0.));
#144049=CARTESIAN_POINT('Ctrl Pts',(-73.1170499848039,-10.53451445581,0.));
#144050=CARTESIAN_POINT('Ctrl Pts',(-73.0909477356474,-10.5417259395003,
0.));
#144051=CARTESIAN_POINT('Ctrl Pts',(-73.0648736873434,-10.5489039755138,
0.));
#144052=CARTESIAN_POINT('Ctrl Pts',(-73.0388279370834,-10.5560485852974,
0.));
#144053=CARTESIAN_POINT('Ctrl Pts',(-73.0128105832621,-10.5631597907651,
0.));
#144054=CARTESIAN_POINT('Ctrl Pts',(-72.9868217252283,-10.570237614205,
0.));
#144055=CARTESIAN_POINT('Ctrl Pts',(-72.9608614630534,-10.5772820781958,
0.));
#144056=CARTESIAN_POINT('Ctrl Pts',(-72.9349298972822,-10.5842932055209,
0.));
#144057=CARTESIAN_POINT('Ctrl Pts',(-72.9090271287083,-10.5912710190928,
0.));
#144058=CARTESIAN_POINT('Ctrl Pts',(-72.8831532580845,-10.5982155418626,
0.));
#144059=CARTESIAN_POINT('Ctrl Pts',(-72.8573083861337,-10.6051267968203,
0.));
#144060=CARTESIAN_POINT('Ctrl Pts',(-72.8314926136881,-10.6120048070367,
0.));
#144061=CARTESIAN_POINT('Ctrl Pts',(-72.8057060417887,-10.6188495956973,
0.));
#144062=CARTESIAN_POINT('Ctrl Pts',(-72.7799487717911,-10.6256611861394,
0.));
#144063=CARTESIAN_POINT('Ctrl Pts',(-72.7542209054812,-10.6324396018998,
0.));
#144064=CARTESIAN_POINT('Ctrl Pts',(-72.7285225451293,-10.6391848667352,
0.));
#144065=CARTESIAN_POINT('Ctrl Pts',(-72.7028537934317,-10.6458970045946,
0.));
#144066=CARTESIAN_POINT('Ctrl Pts',(-72.6772147534752,-10.6525760396054,
0.));
#144067=CARTESIAN_POINT('Ctrl Pts',(-72.651605528691,-10.659221996058,0.));
#144068=CARTESIAN_POINT('Ctrl Pts',(-72.6260262228065,-10.6658348983944,
0.));
#144069=CARTESIAN_POINT('Ctrl Pts',(-72.6004769398019,-10.6724147711995,
0.));
#144070=CARTESIAN_POINT('Ctrl Pts',(-72.5749577839415,-10.6789616392042,
0.));
#144071=CARTESIAN_POINT('Ctrl Pts',(-72.5494688597961,-10.6854755272904,
0.));
#144072=CARTESIAN_POINT('Ctrl Pts',(-72.5240102722664,-10.691956460499,
0.));
#144073=CARTESIAN_POINT('Ctrl Pts',(-72.4985821266023,-10.6984044640398,
0.));
#144074=CARTESIAN_POINT('Ctrl Pts',(-72.4731845284227,-10.7048195633061,
0.));
#144075=CARTESIAN_POINT('Ctrl Pts',(-72.4478175837156,-10.7112017838706,
0.));
#144076=CARTESIAN_POINT('Ctrl Pts',(-72.4224813988347,-10.7175511514788,
0.));
#144077=CARTESIAN_POINT('Ctrl Pts',(-72.3971760804933,-10.7238676920469,
0.));
#144078=CARTESIAN_POINT('Ctrl Pts',(-72.3719017357571,-10.7301514316607,
0.));
#144079=CARTESIAN_POINT('Ctrl Pts',(-72.3466584720318,-10.73640239658,0.));
#144080=CARTESIAN_POINT('Ctrl Pts',(-72.3214463970641,-10.7426206132375,
0.));
#144081=CARTESIAN_POINT('Ctrl Pts',(-72.2962656189556,-10.7488061082367,
0.));
#144082=CARTESIAN_POINT('Ctrl Pts',(-72.2711162461681,-10.7549589083535,
0.));
#144083=CARTESIAN_POINT('Ctrl Pts',(-72.2459983875296,-10.7610790405385,
0.));
#144084=CARTESIAN_POINT('Ctrl Pts',(-72.2209121522366,-10.7671665319255,
0.));
#144085=CARTESIAN_POINT('Ctrl Pts',(-72.1958576498558,-10.7732214098344,
0.));
#144086=CARTESIAN_POINT('Ctrl Pts',(-72.1708349903305,-10.7792437017662,
0.));
#144087=CARTESIAN_POINT('Ctrl Pts',(-72.1458442839834,-10.7852334354016,
0.));
#144088=CARTESIAN_POINT('Ctrl Pts',(-72.1208856415171,-10.7911906386027,
0.));
#144089=CARTESIAN_POINT('Ctrl Pts',(-72.0959591740114,-10.7971153394166,
0.));
#144090=CARTESIAN_POINT('Ctrl Pts',(-72.0710649929202,-10.8030075660808,
0.));
#144091=CARTESIAN_POINT('Ctrl Pts',(-72.0462032100815,-10.8088673470184,
0.));
#144092=CARTESIAN_POINT('Ctrl Pts',(-72.0213739377223,-10.8146947108375,
0.));
#144093=CARTESIAN_POINT('Ctrl Pts',(-71.9965772884619,-10.8204896863328,
0.));
#144094=CARTESIAN_POINT('Ctrl Pts',(-71.9718133753127,-10.8262523024898,
0.));
#144095=CARTESIAN_POINT('Ctrl Pts',(-71.9470823116785,-10.8319825884918,
0.));
#144096=CARTESIAN_POINT('Ctrl Pts',(-71.9223842113625,-10.8376805737159,
0.));
#144097=CARTESIAN_POINT('Ctrl Pts',(-71.8977191885725,-10.8433462877311,
0.));
#144098=CARTESIAN_POINT('Ctrl Pts',(-71.8730873579224,-10.8489797602997,
0.));
#144099=CARTESIAN_POINT('Ctrl Pts',(-71.8484888344339,-10.8545810213799,
0.));
#144100=CARTESIAN_POINT('Ctrl Pts',(-71.8239237335331,-10.8601501011332,
0.));
#144101=CARTESIAN_POINT('Ctrl Pts',(-71.7993921710564,-10.865687029922,
0.));
#144102=CARTESIAN_POINT('Ctrl Pts',(-71.7748942632593,-10.8711918383073,
0.));
#144103=CARTESIAN_POINT('Ctrl Pts',(-71.7504301268181,-10.8766645570497,
0.));
#144104=CARTESIAN_POINT('Ctrl Pts',(-71.7259998788328,-10.882105217112,
0.));
#144105=CARTESIAN_POINT('Ctrl Pts',(-71.7016036368236,-10.8875138496671,
0.));
#144106=CARTESIAN_POINT('Ctrl Pts',(-71.6772415187364,-10.8928904860964,
0.));
#144107=CARTESIAN_POINT('Ctrl Pts',(-71.6529136429504,-10.8982351579871,
0.));
#144108=CARTESIAN_POINT('Ctrl Pts',(-71.6286201282812,-10.9035478971328,
0.));
#144109=CARTESIAN_POINT('Ctrl Pts',(-71.6043610939835,-10.9088287355365,
0.));
#144110=CARTESIAN_POINT('Ctrl Pts',(-71.5801366597488,-10.914077705417,
0.));
#144111=CARTESIAN_POINT('Ctrl Pts',(-71.5559469457091,-10.91929483921,0.));
#144112=CARTESIAN_POINT('Ctrl Pts',(-71.5317920724459,-10.9244801695642,
0.));
#144113=CARTESIAN_POINT('Ctrl Pts',(-71.5076721609937,-10.9296337293424,
0.));
#144114=CARTESIAN_POINT('Ctrl Pts',(-71.4835873328423,-10.9347555516235,
0.));
#144115=CARTESIAN_POINT('Ctrl Pts',(-71.4595377099351,-10.9398456697095,
0.));
#144116=CARTESIAN_POINT('Ctrl Pts',(-71.435523414672,-10.944904117127,0.));
#144117=CARTESIAN_POINT('Ctrl Pts',(-71.4115445699194,-10.9499309276236,
0.));
#144118=CARTESIAN_POINT('Ctrl Pts',(-71.3876012990138,-10.954926135169,
0.));
#144119=CARTESIAN_POINT('Ctrl Pts',(-71.3636937257649,-10.9598897739564,
0.));
#144120=CARTESIAN_POINT('Ctrl Pts',(-71.339821974454,-10.9648218784098,
0.));
#144121=CARTESIAN_POINT('Ctrl Pts',(-71.3159861698358,-10.969722483186,
0.));
#144122=CARTESIAN_POINT('Ctrl Pts',(-71.2921864371491,-10.9745916231709,
0.));
#144123=CARTESIAN_POINT('Ctrl Pts',(-71.2684229021207,-10.9794293334805,
0.));
#144124=CARTESIAN_POINT('Ctrl Pts',(-71.2446956909687,-10.9842356494627,
0.));
#144125=CARTESIAN_POINT('Ctrl Pts',(-71.2210049304014,-10.9890106067039,
0.));
#144126=CARTESIAN_POINT('Ctrl Pts',(-71.1973507476191,-10.993754241032,
0.));
#144127=CARTESIAN_POINT('Ctrl Pts',(-71.1737332703248,-10.9984665885127,
0.));
#144128=CARTESIAN_POINT('Ctrl Pts',(-71.1501526267286,-11.0031476854502,
0.));
#144129=CARTESIAN_POINT('Ctrl Pts',(-71.1266089455517,-11.0077975683895,
0.));
#144130=CARTESIAN_POINT('Ctrl Pts',(-71.1031023560249,-11.0124162741224,
0.));
#144131=CARTESIAN_POINT('Ctrl Pts',(-71.0796329878907,-11.0170038396915,
0.));
#144132=CARTESIAN_POINT('Ctrl Pts',(-71.0562009714136,-11.0215603023856,
0.));
#144133=CARTESIAN_POINT('Ctrl Pts',(-71.0328064373856,-11.0260856997415,
0.));
#144134=CARTESIAN_POINT('Ctrl Pts',(-71.0094495171292,-11.0305800695456,
0.));
#144135=CARTESIAN_POINT('Ctrl Pts',(-70.986130342497,-11.0350434498405,
0.));
#144136=CARTESIAN_POINT('Ctrl Pts',(-70.9628490458748,-11.0394758789285,
0.));
#144137=CARTESIAN_POINT('Ctrl Pts',(-70.9396057601924,-11.0438773953681,
0.));
#144138=CARTESIAN_POINT('Ctrl Pts',(-70.916400618927,-11.048248037975,0.));
#144139=CARTESIAN_POINT('Ctrl Pts',(-70.8932337561087,-11.0525878458243,
0.));
#144140=CARTESIAN_POINT('Ctrl Pts',(-70.8701053063186,-11.0568968582569,
0.));
#144141=CARTESIAN_POINT('Ctrl Pts',(-70.8470154046919,-11.0611751148835,
0.));
#144142=CARTESIAN_POINT('Ctrl Pts',(-70.8239641869299,-11.0654226555802,
0.));
#144143=CARTESIAN_POINT('Ctrl Pts',(-70.8009517893057,-11.0696395204909,
0.));
#144144=CARTESIAN_POINT('Ctrl Pts',(-70.7779783486677,-11.073825750029,
0.));
#144145=CARTESIAN_POINT('Ctrl Pts',(-70.7550440024384,-11.0779813848846,
0.));
#144146=CARTESIAN_POINT('Ctrl Pts',(-70.732148888618,-11.0821064660269,
0.));
#144147=CARTESIAN_POINT('Ctrl Pts',(-70.7092931457954,-11.0862010347016,
0.));
#144148=CARTESIAN_POINT('Ctrl Pts',(-70.6864769131546,-11.0902651324323,
0.));
#144149=CARTESIAN_POINT('Ctrl Pts',(-70.6637003304785,-11.0942988010233,
0.));
#144150=CARTESIAN_POINT('Ctrl Pts',(-70.6409635381482,-11.0983020825667,
0.));
#144151=CARTESIAN_POINT('Ctrl Pts',(-70.6182666771481,-11.1022750194445,
0.));
#144152=CARTESIAN_POINT('Ctrl Pts',(-70.5956098890773,-11.1062176543262,
0.));
#144153=CARTESIAN_POINT('Ctrl Pts',(-70.5729933161546,-11.1101300301701,
0.));
#144154=CARTESIAN_POINT('Ctrl Pts',(-70.5504171012234,-11.1140121902271,
0.));
#144155=CARTESIAN_POINT('Ctrl Pts',(-70.5278813877494,-11.1178641780476,
0.));
#144156=CARTESIAN_POINT('Ctrl Pts',(-70.505386319828,-11.1216860374826,
0.));
#144157=CARTESIAN_POINT('Ctrl Pts',(-70.4829320421957,-11.1254778126821,
0.));
#144158=CARTESIAN_POINT('Ctrl Pts',(-70.4605187002354,-11.1292395480974,
0.));
#144159=CARTESIAN_POINT('Ctrl Pts',(-70.4381464399819,-11.1329712884846,
0.));
#144160=CARTESIAN_POINT('Ctrl Pts',(-70.4158154081205,-11.1366730789125,
0.));
#144161=CARTESIAN_POINT('Ctrl Pts',(-70.393525751996,-11.1403449647625,
0.));
#144162=CARTESIAN_POINT('Ctrl Pts',(-70.3712776196223,-11.143986991727,
0.));
#144163=CARTESIAN_POINT('Ctrl Pts',(-70.349071159688,-11.1475992058124,
0.));
#144164=CARTESIAN_POINT('Ctrl Pts',(-70.326906521559,-11.1511816533421,
0.));
#144165=CARTESIAN_POINT('Ctrl Pts',(-70.3047838552756,-11.1547343809646,
0.));
#144166=CARTESIAN_POINT('Ctrl Pts',(-70.2827033115662,-11.158257435652,
0.));
#144167=CARTESIAN_POINT('Ctrl Pts',(-70.260665041859,-11.1617508647016,
0.));
#144168=CARTESIAN_POINT('Ctrl Pts',(-70.2386691982902,-11.1652147157383,
0.));
#144169=CARTESIAN_POINT('Ctrl Pts',(-70.2167159337094,-11.168649036721,
0.));
#144170=CARTESIAN_POINT('Ctrl Pts',(-70.1948054016816,-11.1720538759499,
0.));
#144171=CARTESIAN_POINT('Ctrl Pts',(-70.1729377564954,-11.1754292820631,
0.));
#144172=CARTESIAN_POINT('Ctrl Pts',(-70.1511131531672,-11.1787753040363,
0.));
#144173=CARTESIAN_POINT('Ctrl Pts',(-70.1293317474432,-11.1820919911846,
0.));
#144174=CARTESIAN_POINT('Ctrl Pts',(-70.1075936957973,-11.185379393167,
0.));
#144175=CARTESIAN_POINT('Ctrl Pts',(-70.0858991554295,-11.1886375599916,
0.));
#144176=CARTESIAN_POINT('Ctrl Pts',(-70.0642482842942,-11.1918665420168,
0.));
#144177=CARTESIAN_POINT('Ctrl Pts',(-70.0426412411194,-11.1950663899578,
0.));
#144178=CARTESIAN_POINT('Ctrl Pts',(-70.0210781854236,-11.1982371548918,
0.));
#144179=CARTESIAN_POINT('Ctrl Pts',(-69.9995592775322,-11.2013788882711,
0.));
#144180=CARTESIAN_POINT('Ctrl Pts',(-69.9780846785771,-11.2044916419239,
0.));
#144181=CARTESIAN_POINT('Ctrl Pts',(-69.9566545504813,-11.2075754680445,
0.));
#144182=CARTESIAN_POINT('Ctrl Pts',(-69.9352690559399,-11.2106304191881,
0.));
#144183=CARTESIAN_POINT('Ctrl Pts',(-69.9139283584036,-11.2136565482679,
0.));
#144184=CARTESIAN_POINT('Ctrl Pts',(-69.8926326220414,-11.2166539085527,
0.));
#144185=CARTESIAN_POINT('Ctrl Pts',(-69.8713820117918,-11.2196225536794,
0.));
#144186=CARTESIAN_POINT('Ctrl Pts',(-69.8501766934445,-11.2225625376739,
0.));
#144187=CARTESIAN_POINT('Ctrl Pts',(-69.8290168337076,-11.225473914972,
0.));
#144188=CARTESIAN_POINT('Ctrl Pts',(-69.8079026002753,-11.2283567404434,
0.));
#144189=CARTESIAN_POINT('Ctrl Pts',(-69.7868341618927,-11.2312110694183,
0.));
#144190=CARTESIAN_POINT('Ctrl Pts',(-69.7658116882298,-11.2340369576452,
0.));
#144191=CARTESIAN_POINT('Ctrl Pts',(-69.7448353497394,-11.236834461247,
0.));
#144192=CARTESIAN_POINT('Ctrl Pts',(-69.7239053175362,-11.2396036366861,
0.));
#144193=CARTESIAN_POINT('Ctrl Pts',(-69.7030217632187,-11.242344540717,
0.));
#144194=CARTESIAN_POINT('Ctrl Pts',(-69.6821848588492,-11.2450572303847,
0.));
#144195=CARTESIAN_POINT('Ctrl Pts',(-69.6613947773563,-11.247741763139,
0.));
#144196=CARTESIAN_POINT('Ctrl Pts',(-69.6406516928902,-11.2503981969413,
0.));
#144197=CARTESIAN_POINT('Ctrl Pts',(-69.6199557811231,-11.2530265903555,
0.));
#144198=CARTESIAN_POINT('Ctrl Pts',(-69.5993072197355,-11.255627002701,
0.));
#144199=CARTESIAN_POINT('Ctrl Pts',(-69.5787061880815,-11.2581994939534,
0.));
#144200=CARTESIAN_POINT('Ctrl Pts',(-69.5581528662846,-11.2607441244698,
0.));
#144201=CARTESIAN_POINT('Ctrl Pts',(-69.5376474344768,-11.2632609547629,
0.));
#144202=CARTESIAN_POINT('Ctrl Pts',(-69.5171900720188,-11.265750045272,
0.));
#144203=CARTESIAN_POINT('Ctrl Pts',(-69.4967809565978,-11.2682114561015,
0.));
#144204=CARTESIAN_POINT('Ctrl Pts',(-69.4764202659443,-11.2706452475287,
0.));
#144205=CARTESIAN_POINT('Ctrl Pts',(-69.4561081798815,-11.2730514806143,
0.));
#144206=CARTESIAN_POINT('Ctrl Pts',(-69.4358448819957,-11.2754302177019,
0.));
#144207=CARTESIAN_POINT('Ctrl Pts',(-69.4156305620554,-11.2777815231462,
0.));
#144208=CARTESIAN_POINT('Ctrl Pts',(-69.395465416223,-11.2801054633807,
0.));
#144209=CARTESIAN_POINT('Ctrl Pts',(-69.375349642,-11.2824021054038,0.));
#144210=CARTESIAN_POINT('Ctrl Pts',(-69.3552834337771,-11.2846715154521,
0.));
#144211=CARTESIAN_POINT('Ctrl Pts',(-69.3352669789611,-11.2869137578463,
0.));
#144212=CARTESIAN_POINT('Ctrl Pts',(-69.315300451784,-11.2891288931528,
0.));
#144213=CARTESIAN_POINT('Ctrl Pts',(-69.2953840192792,-11.2913169799642,
0.));
#144214=CARTESIAN_POINT('Ctrl Pts',(-69.2755178531534,-11.2934780784361,
0.));
#144215=CARTESIAN_POINT('Ctrl Pts',(-69.255702139335,-11.2956122531375,
0.));
#144216=CARTESIAN_POINT('Ctrl Pts',(-69.2359370894828,-11.2977195764836,
0.));
#144217=CARTESIAN_POINT('Ctrl Pts',(-69.216222948839,-11.2998001310934,
0.));
#144218=CARTESIAN_POINT('Ctrl Pts',(-69.1965599718761,-11.3018540025605,
0.));
#144219=CARTESIAN_POINT('Ctrl Pts',(-69.1769483991639,-11.3038812726275,
0.));
#144220=CARTESIAN_POINT('Ctrl Pts',(-69.1573884361076,-11.3058820128323,
0.));
#144221=CARTESIAN_POINT('Ctrl Pts',(-69.137880225198,-11.3078562764442,
0.));
#144222=CARTESIAN_POINT('Ctrl Pts',(-69.1184238445065,-11.3098040973799,
0.));
#144223=CARTESIAN_POINT('Ctrl Pts',(-69.1029002322497,-11.3113412156742,
0.));
#144224=CARTESIAN_POINT('Ctrl Pts',(-69.0912808657051,-11.3124821678849,
0.));
#144225=CARTESIAN_POINT('Ctrl Pts',(-69.0835449954486,-11.3132375200184,
0.));
#144226=CARTESIAN_POINT('Ctrl Pts',(-69.079679653846,-11.3136138754165,
0.));
#144227=CARTESIAN_POINT('Ctrl Pts',(-74.3992230078037,-3.87370827955543,
0.));
#144228=CARTESIAN_POINT('Ctrl Pts',(-74.3992230078037,-3.87370827955543,
12.));
#144229=CARTESIAN_POINT('Ctrl Pts',(-74.3940262116388,-3.87578335377325,
0.));
#144230=CARTESIAN_POINT('Ctrl Pts',(-74.3940262116388,-3.87578335377325,
12.));
#144231=CARTESIAN_POINT('Ctrl Pts',(-74.3836349189184,-3.87992989995747,
0.));
#144232=CARTESIAN_POINT('Ctrl Pts',(-74.3836349189184,-3.87992989995747,
12.));
#144233=CARTESIAN_POINT('Ctrl Pts',(-74.3680548786661,-3.88613891247983,
0.));
#144234=CARTESIAN_POINT('Ctrl Pts',(-74.3680548786661,-3.88613891247983,
12.));
#144235=CARTESIAN_POINT('Ctrl Pts',(-74.3472952898745,-3.89439598145328,
0.));
#144236=CARTESIAN_POINT('Ctrl Pts',(-74.3472952898745,-3.89439598145328,
12.));
#144237=CARTESIAN_POINT('Ctrl Pts',(-74.3213688090134,-3.90468128904634,
0.));
#144238=CARTESIAN_POINT('Ctrl Pts',(-74.3213688090134,-3.90468128904634,
12.));
#144239=CARTESIAN_POINT('Ctrl Pts',(-74.2954653518728,-3.9149305628503,
0.));
#144240=CARTESIAN_POINT('Ctrl Pts',(-74.2954653518728,-3.9149305628503,
12.));
#144241=CARTESIAN_POINT('Ctrl Pts',(-74.2695849516226,-3.92514379920743,
0.));
#144242=CARTESIAN_POINT('Ctrl Pts',(-74.2695849516226,-3.92514379920743,
12.));
#144243=CARTESIAN_POINT('Ctrl Pts',(-74.2437276593623,-3.93532099774203,
0.));
#144244=CARTESIAN_POINT('Ctrl Pts',(-74.2437276593623,-3.93532099774203,
12.));
#144245=CARTESIAN_POINT('Ctrl Pts',(-74.2178935492876,-3.94546216377451,
0.));
#144246=CARTESIAN_POINT('Ctrl Pts',(-74.2178935492876,-3.94546216377451,
12.));
#144247=CARTESIAN_POINT('Ctrl Pts',(-74.1920827166585,-3.9555673082111,
0.));
#144248=CARTESIAN_POINT('Ctrl Pts',(-74.1920827166585,-3.9555673082111,
12.));
#144249=CARTESIAN_POINT('Ctrl Pts',(-74.1662952702485,-3.96563644549385,
0.));
#144250=CARTESIAN_POINT('Ctrl Pts',(-74.1662952702485,-3.96563644549385,
12.));
#144251=CARTESIAN_POINT('Ctrl Pts',(-74.1405313263109,-3.97566959209528,
0.));
#144252=CARTESIAN_POINT('Ctrl Pts',(-74.1405313263109,-3.97566959209528,
12.));
#144253=CARTESIAN_POINT('Ctrl Pts',(-74.1147910020891,-3.98566676483641,
0.));
#144254=CARTESIAN_POINT('Ctrl Pts',(-74.1147910020891,-3.98566676483641,
12.));
#144255=CARTESIAN_POINT('Ctrl Pts',(-74.0890744091186,-3.99562797918287,
0.));
#144256=CARTESIAN_POINT('Ctrl Pts',(-74.0890744091186,-3.99562797918287,
12.));
#144257=CARTESIAN_POINT('Ctrl Pts',(-74.0633816478037,-4.0055532478548,
0.));
#144258=CARTESIAN_POINT('Ctrl Pts',(-74.0633816478037,-4.0055532478548,
12.));
#144259=CARTESIAN_POINT('Ctrl Pts',(-74.0377128111863,-4.0154425817671,
0.));
#144260=CARTESIAN_POINT('Ctrl Pts',(-74.0377128111863,-4.0154425817671,
12.));
#144261=CARTESIAN_POINT('Ctrl Pts',(-74.012067987646,-4.02529599070094,
0.));
#144262=CARTESIAN_POINT('Ctrl Pts',(-74.012067987646,-4.02529599070094,
12.));
#144263=CARTESIAN_POINT('Ctrl Pts',(-73.9864472641033,-4.03511348410659,
0.));
#144264=CARTESIAN_POINT('Ctrl Pts',(-73.9864472641033,-4.03511348410659,
12.));
#144265=CARTESIAN_POINT('Ctrl Pts',(-73.9608507287909,-4.04489507179957,
0.));
#144266=CARTESIAN_POINT('Ctrl Pts',(-73.9608507287909,-4.04489507179957,
12.));
#144267=CARTESIAN_POINT('Ctrl Pts',(-73.9352784747608,-4.05464076484752,
0.));
#144268=CARTESIAN_POINT('Ctrl Pts',(-73.9352784747608,-4.05464076484752,
12.));
#144269=CARTESIAN_POINT('Ctrl Pts',(-73.9097305995115,-4.06435057547324,
0.));
#144270=CARTESIAN_POINT('Ctrl Pts',(-73.9097305995115,-4.06435057547324,
12.));
#144271=CARTESIAN_POINT('Ctrl Pts',(-73.8842072034008,-4.07402451665244,
0.));
#144272=CARTESIAN_POINT('Ctrl Pts',(-73.8842072034008,-4.07402451665244,
12.));
#144273=CARTESIAN_POINT('Ctrl Pts',(-73.8587083884191,-4.08366260180674,
0.));
#144274=CARTESIAN_POINT('Ctrl Pts',(-73.8587083884191,-4.08366260180674,
12.));
#144275=CARTESIAN_POINT('Ctrl Pts',(-73.8332342568989,-4.09326484448232,
0.));
#144276=CARTESIAN_POINT('Ctrl Pts',(-73.8332342568989,-4.09326484448232,
12.));
#144277=CARTESIAN_POINT('Ctrl Pts',(-73.8077849100342,-4.10283125798729,
0.));
#144278=CARTESIAN_POINT('Ctrl Pts',(-73.8077849100342,-4.10283125798729,
12.));
#144279=CARTESIAN_POINT('Ctrl Pts',(-73.7823604472159,-4.11236185522787,
0.));
#144280=CARTESIAN_POINT('Ctrl Pts',(-73.7823604472159,-4.11236185522787,
12.));
#144281=CARTESIAN_POINT('Ctrl Pts',(-73.7569609668528,-4.12185664890556,
0.));
#144282=CARTESIAN_POINT('Ctrl Pts',(-73.7569609668528,-4.12185664890556,
12.));
#144283=CARTESIAN_POINT('Ctrl Pts',(-73.7315865668522,-4.13131565163578,
0.));
#144284=CARTESIAN_POINT('Ctrl Pts',(-73.7315865668522,-4.13131565163578,
12.));
#144285=CARTESIAN_POINT('Ctrl Pts',(-73.7062373452342,-4.14073887610153,
0.));
#144286=CARTESIAN_POINT('Ctrl Pts',(-73.7062373452342,-4.14073887610153,
12.));
#144287=CARTESIAN_POINT('Ctrl Pts',(-73.6809134006897,-4.15012633519723,
0.));
#144288=CARTESIAN_POINT('Ctrl Pts',(-73.6809134006897,-4.15012633519723,
12.));
#144289=CARTESIAN_POINT('Ctrl Pts',(-73.6556148331489,-4.15947804217783,
0.));
#144290=CARTESIAN_POINT('Ctrl Pts',(-73.6556148331489,-4.15947804217783,
12.));
#144291=CARTESIAN_POINT('Ctrl Pts',(-73.6303417435251,-4.1687940105878,
0.));
#144292=CARTESIAN_POINT('Ctrl Pts',(-73.6303417435251,-4.1687940105878,
12.));
#144293=CARTESIAN_POINT('Ctrl Pts',(-73.6050942334768,-4.17807425419812,
0.));
#144294=CARTESIAN_POINT('Ctrl Pts',(-73.6050942334768,-4.17807425419812,
12.));
#144295=CARTESIAN_POINT('Ctrl Pts',(-73.5798724051519,-4.18731878694236,
0.));
#144296=CARTESIAN_POINT('Ctrl Pts',(-73.5798724051519,-4.18731878694236,
12.));
#144297=CARTESIAN_POINT('Ctrl Pts',(-73.5546763609572,-4.19652762286126,
0.));
#144298=CARTESIAN_POINT('Ctrl Pts',(-73.5546763609572,-4.19652762286126,
12.));
#144299=CARTESIAN_POINT('Ctrl Pts',(-73.5295062032628,-4.2057007760373,
0.));
#144300=CARTESIAN_POINT('Ctrl Pts',(-73.5295062032628,-4.2057007760373,
12.));
#144301=CARTESIAN_POINT('Ctrl Pts',(-73.5043620344116,-4.21483826059441,
0.));
#144302=CARTESIAN_POINT('Ctrl Pts',(-73.5043620344116,-4.21483826059441,
12.));
#144303=CARTESIAN_POINT('Ctrl Pts',(-73.4792439568633,-4.22394009072756,
0.));
#144304=CARTESIAN_POINT('Ctrl Pts',(-73.4792439568633,-4.22394009072756,
12.));
#144305=CARTESIAN_POINT('Ctrl Pts',(-73.4541520732948,-4.23300628072758,
0.));
#144306=CARTESIAN_POINT('Ctrl Pts',(-73.4541520732948,-4.23300628072758,
12.));
#144307=CARTESIAN_POINT('Ctrl Pts',(-73.4290864867101,-4.24203684500938,
0.));
#144308=CARTESIAN_POINT('Ctrl Pts',(-73.4290864867101,-4.24203684500938,
12.));
#144309=CARTESIAN_POINT('Ctrl Pts',(-73.4040473005592,-4.25103179814886,
0.));
#144310=CARTESIAN_POINT('Ctrl Pts',(-73.4040473005592,-4.25103179814886,
12.));
#144311=CARTESIAN_POINT('Ctrl Pts',(-73.3790346187938,-4.25999115489899,
0.));
#144312=CARTESIAN_POINT('Ctrl Pts',(-73.3790346187938,-4.25999115489899,
12.));
#144313=CARTESIAN_POINT('Ctrl Pts',(-73.3540485458065,-4.26891493016699,
0.));
#144314=CARTESIAN_POINT('Ctrl Pts',(-73.3540485458065,-4.26891493016699,
12.));
#144315=CARTESIAN_POINT('Ctrl Pts',(-73.3290891863949,-4.27780313900389,
0.));
#144316=CARTESIAN_POINT('Ctrl Pts',(-73.3290891863949,-4.27780313900389,
12.));
#144317=CARTESIAN_POINT('Ctrl Pts',(-73.3041566457135,-4.28665579659301,
0.));
#144318=CARTESIAN_POINT('Ctrl Pts',(-73.3041566457135,-4.28665579659301,
12.));
#144319=CARTESIAN_POINT('Ctrl Pts',(-73.2792510292254,-4.29547291824287,
0.));
#144320=CARTESIAN_POINT('Ctrl Pts',(-73.2792510292254,-4.29547291824287,
12.));
#144321=CARTESIAN_POINT('Ctrl Pts',(-73.2543724426577,-4.3042545193823,
0.));
#144322=CARTESIAN_POINT('Ctrl Pts',(-73.2543724426577,-4.3042545193823,
12.));
#144323=CARTESIAN_POINT('Ctrl Pts',(-73.2295209920334,-4.31300061556098,
0.));
#144324=CARTESIAN_POINT('Ctrl Pts',(-73.2295209920334,-4.31300061556098,
12.));
#144325=CARTESIAN_POINT('Ctrl Pts',(-73.204696783694,-4.32171122245214,
0.));
#144326=CARTESIAN_POINT('Ctrl Pts',(-73.204696783694,-4.32171122245214,
12.));
#144327=CARTESIAN_POINT('Ctrl Pts',(-73.1798999243235,-4.33038635585876,
0.));
#144328=CARTESIAN_POINT('Ctrl Pts',(-73.1798999243235,-4.33038635585876,
12.));
#144329=CARTESIAN_POINT('Ctrl Pts',(-73.1551305209685,-4.3390260317214,
0.));
#144330=CARTESIAN_POINT('Ctrl Pts',(-73.1551305209685,-4.3390260317214,
12.));
#144331=CARTESIAN_POINT('Ctrl Pts',(-73.130388681059,-4.34763026613157,
0.));
#144332=CARTESIAN_POINT('Ctrl Pts',(-73.130388681059,-4.34763026613157,
12.));
#144333=CARTESIAN_POINT('Ctrl Pts',(-73.1056745124087,-4.35619907532719,
0.));
#144334=CARTESIAN_POINT('Ctrl Pts',(-73.1056745124087,-4.35619907532719,
12.));
#144335=CARTESIAN_POINT('Ctrl Pts',(-73.0809881232103,-4.36473247568641,
0.));
#144336=CARTESIAN_POINT('Ctrl Pts',(-73.0809881232103,-4.36473247568641,
12.));
#144337=CARTESIAN_POINT('Ctrl Pts',(-73.0563296220299,-4.37323048372607,
0.));
#144338=CARTESIAN_POINT('Ctrl Pts',(-73.0563296220299,-4.37323048372607,
12.));
#144339=CARTESIAN_POINT('Ctrl Pts',(-73.0316991177993,-4.3816931161015,
0.));
#144340=CARTESIAN_POINT('Ctrl Pts',(-73.0316991177993,-4.3816931161015,
12.));
#144341=CARTESIAN_POINT('Ctrl Pts',(-73.007096719804,-4.39012038961139,
0.));
#144342=CARTESIAN_POINT('Ctrl Pts',(-73.007096719804,-4.39012038961139,
12.));
#144343=CARTESIAN_POINT('Ctrl Pts',(-72.9825225376846,-4.39851232119722,
0.));
#144344=CARTESIAN_POINT('Ctrl Pts',(-72.9825225376846,-4.39851232119722,
12.));
#144345=CARTESIAN_POINT('Ctrl Pts',(-72.95797668145,-4.40686892793957,0.));
#144346=CARTESIAN_POINT('Ctrl Pts',(-72.95797668145,-4.40686892793957,12.));
#144347=CARTESIAN_POINT('Ctrl Pts',(-72.9334592614829,-4.41519022705921,
0.));
#144348=CARTESIAN_POINT('Ctrl Pts',(-72.9334592614829,-4.41519022705921,
12.));
#144349=CARTESIAN_POINT('Ctrl Pts',(-72.9089703885462,-4.42347623591941,
0.));
#144350=CARTESIAN_POINT('Ctrl Pts',(-72.9089703885462,-4.42347623591941,
12.));
#144351=CARTESIAN_POINT('Ctrl Pts',(-72.8845101737855,-4.43172697203349,
0.));
#144352=CARTESIAN_POINT('Ctrl Pts',(-72.8845101737855,-4.43172697203349,
12.));
#144353=CARTESIAN_POINT('Ctrl Pts',(-72.8600787287318,-4.43994245306818,
0.));
#144354=CARTESIAN_POINT('Ctrl Pts',(-72.8600787287318,-4.43994245306818,
12.));
#144355=CARTESIAN_POINT('Ctrl Pts',(-72.8356761653069,-4.44812269683737,
0.));
#144356=CARTESIAN_POINT('Ctrl Pts',(-72.8356761653069,-4.44812269683737,
12.));
#144357=CARTESIAN_POINT('Ctrl Pts',(-72.8113025958262,-4.45626772130146,
0.));
#144358=CARTESIAN_POINT('Ctrl Pts',(-72.8113025958262,-4.45626772130146,
12.));
#144359=CARTESIAN_POINT('Ctrl Pts',(-72.7869581329994,-4.46437754456792,
0.));
#144360=CARTESIAN_POINT('Ctrl Pts',(-72.7869581329994,-4.46437754456792,
12.));
#144361=CARTESIAN_POINT('Ctrl Pts',(-72.7626428899281,-4.47245218489609,
0.));
#144362=CARTESIAN_POINT('Ctrl Pts',(-72.7626428899281,-4.47245218489609,
12.));
#144363=CARTESIAN_POINT('Ctrl Pts',(-72.738356980103,-4.48049166070205,
0.));
#144364=CARTESIAN_POINT('Ctrl Pts',(-72.738356980103,-4.48049166070205,
12.));
#144365=CARTESIAN_POINT('Ctrl Pts',(-72.714100517414,-4.48849599055337,
0.));
#144366=CARTESIAN_POINT('Ctrl Pts',(-72.714100517414,-4.48849599055337,
12.));
#144367=CARTESIAN_POINT('Ctrl Pts',(-72.6898736161542,-4.49646519316812,
0.));
#144368=CARTESIAN_POINT('Ctrl Pts',(-72.6898736161542,-4.49646519316812,
12.));
#144369=CARTESIAN_POINT('Ctrl Pts',(-72.6656763910241,-4.50439928741604,
0.));
#144370=CARTESIAN_POINT('Ctrl Pts',(-72.6656763910241,-4.50439928741604,
12.));
#144371=CARTESIAN_POINT('Ctrl Pts',(-72.6415089571321,-4.51229829232264,
0.));
#144372=CARTESIAN_POINT('Ctrl Pts',(-72.6415089571321,-4.51229829232264,
12.));
#144373=CARTESIAN_POINT('Ctrl Pts',(-72.6173714299942,-4.52016222707637,
0.));
#144374=CARTESIAN_POINT('Ctrl Pts',(-72.6173714299942,-4.52016222707637,
12.));
#144375=CARTESIAN_POINT('Ctrl Pts',(-72.5932639255409,-4.52799111102391,
0.));
#144376=CARTESIAN_POINT('Ctrl Pts',(-72.5932639255409,-4.52799111102391,
12.));
#144377=CARTESIAN_POINT('Ctrl Pts',(-72.5691865601223,-4.53578496366799,
0.));
#144378=CARTESIAN_POINT('Ctrl Pts',(-72.5691865601223,-4.53578496366799,
12.));
#144379=CARTESIAN_POINT('Ctrl Pts',(-72.5451394505104,-4.54354380466822,
0.));
#144380=CARTESIAN_POINT('Ctrl Pts',(-72.5451394505104,-4.54354380466822,
12.));
#144381=CARTESIAN_POINT('Ctrl Pts',(-72.5211227139001,-4.55126765384404,
0.));
#144382=CARTESIAN_POINT('Ctrl Pts',(-72.5211227139001,-4.55126765384404,
12.));
#144383=CARTESIAN_POINT('Ctrl Pts',(-72.4971364679068,-4.5589565311822,
0.));
#144384=CARTESIAN_POINT('Ctrl Pts',(-72.4971364679068,-4.5589565311822,
12.));
#144385=CARTESIAN_POINT('Ctrl Pts',(-72.4731808305728,-4.56661045683376,
0.));
#144386=CARTESIAN_POINT('Ctrl Pts',(-72.4731808305728,-4.56661045683376,
12.));
#144387=CARTESIAN_POINT('Ctrl Pts',(-72.4492559203745,-4.57422945111102,
0.));
#144388=CARTESIAN_POINT('Ctrl Pts',(-72.4492559203745,-4.57422945111102,
12.));
#144389=CARTESIAN_POINT('Ctrl Pts',(-72.4253618562252,-4.58181353448851,
0.));
#144390=CARTESIAN_POINT('Ctrl Pts',(-72.4253618562252,-4.58181353448851,
12.));
#144391=CARTESIAN_POINT('Ctrl Pts',(-72.401498757478,-4.58936272760544,
0.));
#144392=CARTESIAN_POINT('Ctrl Pts',(-72.401498757478,-4.58936272760544,
12.));
#144393=CARTESIAN_POINT('Ctrl Pts',(-72.3776667439227,-4.5968770512733,
0.));
#144394=CARTESIAN_POINT('Ctrl Pts',(-72.3776667439227,-4.5968770512733,
12.));
#144395=CARTESIAN_POINT('Ctrl Pts',(-72.3538659357913,-4.60435652647453,
0.));
#144396=CARTESIAN_POINT('Ctrl Pts',(-72.3538659357913,-4.60435652647453,
12.));
#144397=CARTESIAN_POINT('Ctrl Pts',(-72.3300964537658,-4.61180117435862,
0.));
#144398=CARTESIAN_POINT('Ctrl Pts',(-72.3300964537658,-4.61180117435862,
12.));
#144399=CARTESIAN_POINT('Ctrl Pts',(-72.3063584189807,-4.61921101624292,
0.));
#144400=CARTESIAN_POINT('Ctrl Pts',(-72.3063584189807,-4.61921101624292,
12.));
#144401=CARTESIAN_POINT('Ctrl Pts',(-72.2826519530259,-4.62658607361466,
0.));
#144402=CARTESIAN_POINT('Ctrl Pts',(-72.2826519530259,-4.62658607361466,
12.));
#144403=CARTESIAN_POINT('Ctrl Pts',(-72.2589771779456,-4.63392636813843,
0.));
#144404=CARTESIAN_POINT('Ctrl Pts',(-72.2589771779456,-4.63392636813843,
12.));
#144405=CARTESIAN_POINT('Ctrl Pts',(-72.2353342162417,-4.64123192165627,
0.));
#144406=CARTESIAN_POINT('Ctrl Pts',(-72.2353342162417,-4.64123192165627,
12.));
#144407=CARTESIAN_POINT('Ctrl Pts',(-72.2117231908822,-4.64850275618323,
0.));
#144408=CARTESIAN_POINT('Ctrl Pts',(-72.2117231908822,-4.64850275618323,
12.));
#144409=CARTESIAN_POINT('Ctrl Pts',(-72.1881442253053,-4.65573889390822,
0.));
#144410=CARTESIAN_POINT('Ctrl Pts',(-72.1881442253053,-4.65573889390822,
12.));
#144411=CARTESIAN_POINT('Ctrl Pts',(-72.1645974434216,-4.66294035719569,
0.));
#144412=CARTESIAN_POINT('Ctrl Pts',(-72.1645974434216,-4.66294035719569,
12.));
#144413=CARTESIAN_POINT('Ctrl Pts',(-72.1410829696128,-4.67010716859285,
0.));
#144414=CARTESIAN_POINT('Ctrl Pts',(-72.1410829696128,-4.67010716859285,
12.));
#144415=CARTESIAN_POINT('Ctrl Pts',(-72.1176009287351,-4.67723935083094,
0.));
#144416=CARTESIAN_POINT('Ctrl Pts',(-72.1176009287351,-4.67723935083094,
12.));
#144417=CARTESIAN_POINT('Ctrl Pts',(-72.0941514461287,-4.68433692682068,
0.));
#144418=CARTESIAN_POINT('Ctrl Pts',(-72.0941514461287,-4.68433692682068,
12.));
#144419=CARTESIAN_POINT('Ctrl Pts',(-72.0707346476213,-4.69139991965283,
0.));
#144420=CARTESIAN_POINT('Ctrl Pts',(-72.0707346476213,-4.69139991965283,
12.));
#144421=CARTESIAN_POINT('Ctrl Pts',(-72.0473506595318,-4.69842835259992,
0.));
#144422=CARTESIAN_POINT('Ctrl Pts',(-72.0473506595318,-4.69842835259992,
12.));
#144423=CARTESIAN_POINT('Ctrl Pts',(-72.0239996086686,-4.705422249123,0.));
#144424=CARTESIAN_POINT('Ctrl Pts',(-72.0239996086686,-4.705422249123,12.));
#144425=CARTESIAN_POINT('Ctrl Pts',(-72.0006816223325,-4.71238163287396,
0.));
#144426=CARTESIAN_POINT('Ctrl Pts',(-72.0006816223325,-4.71238163287396,
12.));
#144427=CARTESIAN_POINT('Ctrl Pts',(-71.9773968283259,-4.7193065276907,
0.));
#144428=CARTESIAN_POINT('Ctrl Pts',(-71.9773968283259,-4.7193065276907,
12.));
#144429=CARTESIAN_POINT('Ctrl Pts',(-71.9541453549579,-4.72619695759774,
0.));
#144430=CARTESIAN_POINT('Ctrl Pts',(-71.9541453549579,-4.72619695759774,
12.));
#144431=CARTESIAN_POINT('Ctrl Pts',(-71.9309273310471,-4.73305294680785,
0.));
#144432=CARTESIAN_POINT('Ctrl Pts',(-71.9309273310471,-4.73305294680785,
12.));
#144433=CARTESIAN_POINT('Ctrl Pts',(-71.9077428859212,-4.73987451972863,
0.));
#144434=CARTESIAN_POINT('Ctrl Pts',(-71.9077428859212,-4.73987451972863,
12.));
#144435=CARTESIAN_POINT('Ctrl Pts',(-71.8845921494189,-4.74666170096547,
0.));
#144436=CARTESIAN_POINT('Ctrl Pts',(-71.8845921494189,-4.74666170096547,
12.));
#144437=CARTESIAN_POINT('Ctrl Pts',(-71.8614752519008,-4.75341451531669,
0.));
#144438=CARTESIAN_POINT('Ctrl Pts',(-71.8614752519008,-4.75341451531669,
12.));
#144439=CARTESIAN_POINT('Ctrl Pts',(-71.8383923242531,-4.76013298777419,
0.));
#144440=CARTESIAN_POINT('Ctrl Pts',(-71.8383923242531,-4.76013298777419,
12.));
#144441=CARTESIAN_POINT('Ctrl Pts',(-71.8153434978923,-4.76681714352502,
0.));
#144442=CARTESIAN_POINT('Ctrl Pts',(-71.8153434978923,-4.76681714352502,
12.));
#144443=CARTESIAN_POINT('Ctrl Pts',(-71.7923289047643,-4.77346700795792,
0.));
#144444=CARTESIAN_POINT('Ctrl Pts',(-71.7923289047643,-4.77346700795792,
12.));
#144445=CARTESIAN_POINT('Ctrl Pts',(-71.769348677346,-4.7800826066665,0.));
#144446=CARTESIAN_POINT('Ctrl Pts',(-71.769348677346,-4.7800826066665,12.));
#144447=CARTESIAN_POINT('Ctrl Pts',(-71.7464029486563,-4.78666396544458,
0.));
#144448=CARTESIAN_POINT('Ctrl Pts',(-71.7464029486563,-4.78666396544458,
12.));
#144449=CARTESIAN_POINT('Ctrl Pts',(-71.723491852261,-4.79321111028676,
0.));
#144450=CARTESIAN_POINT('Ctrl Pts',(-71.723491852261,-4.79321111028676,
12.));
#144451=CARTESIAN_POINT('Ctrl Pts',(-71.7006155222764,-4.7997240673901,
0.));
#144452=CARTESIAN_POINT('Ctrl Pts',(-71.7006155222764,-4.7997240673901,
12.));
#144453=CARTESIAN_POINT('Ctrl Pts',(-71.6777740933687,-4.80620286316075,
0.));
#144454=CARTESIAN_POINT('Ctrl Pts',(-71.6777740933687,-4.80620286316075,
12.));
#144455=CARTESIAN_POINT('Ctrl Pts',(-71.6549677007582,-4.81264752421713,
0.));
#144456=CARTESIAN_POINT('Ctrl Pts',(-71.6549677007582,-4.81264752421713,
12.));
#144457=CARTESIAN_POINT('Ctrl Pts',(-71.6321964802297,-4.81905807738541,
0.));
#144458=CARTESIAN_POINT('Ctrl Pts',(-71.6321964802297,-4.81905807738541,
12.));
#144459=CARTESIAN_POINT('Ctrl Pts',(-71.6094605681353,-4.8254345497002,
0.));
#144460=CARTESIAN_POINT('Ctrl Pts',(-71.6094605681353,-4.8254345497002,
12.));
#144461=CARTESIAN_POINT('Ctrl Pts',(-71.5867601014008,-4.8317769684064,
0.));
#144462=CARTESIAN_POINT('Ctrl Pts',(-71.5867601014008,-4.8317769684064,
12.));
#144463=CARTESIAN_POINT('Ctrl Pts',(-71.5640952175239,-4.83808536096589,
0.));
#144464=CARTESIAN_POINT('Ctrl Pts',(-71.5640952175239,-4.83808536096589,
12.));
#144465=CARTESIAN_POINT('Ctrl Pts',(-71.5414660545778,-4.84435975506056,
0.));
#144466=CARTESIAN_POINT('Ctrl Pts',(-71.5414660545778,-4.84435975506056,
12.));
#144467=CARTESIAN_POINT('Ctrl Pts',(-71.5188727512231,-4.85060017858786,
0.));
#144468=CARTESIAN_POINT('Ctrl Pts',(-71.5188727512231,-4.85060017858786,
12.));
#144469=CARTESIAN_POINT('Ctrl Pts',(-71.4963154467128,-4.85680665966184,
0.));
#144470=CARTESIAN_POINT('Ctrl Pts',(-71.4963154467128,-4.85680665966184,
12.));
#144471=CARTESIAN_POINT('Ctrl Pts',(-71.4737942808971,-4.86297922661498,
0.));
#144472=CARTESIAN_POINT('Ctrl Pts',(-71.4737942808971,-4.86297922661498,
12.));
#144473=CARTESIAN_POINT('Ctrl Pts',(-71.4513093942216,-4.86911790800533,
0.));
#144474=CARTESIAN_POINT('Ctrl Pts',(-71.4513093942216,-4.86911790800533,
12.));
#144475=CARTESIAN_POINT('Ctrl Pts',(-71.4288609277324,-4.8752227326188,
0.));
#144476=CARTESIAN_POINT('Ctrl Pts',(-71.4288609277324,-4.8752227326188,
12.));
#144477=CARTESIAN_POINT('Ctrl Pts',(-71.4064490230857,-4.88129372946524,
0.));
#144478=CARTESIAN_POINT('Ctrl Pts',(-71.4064490230857,-4.88129372946524,
12.));
#144479=CARTESIAN_POINT('Ctrl Pts',(-71.3840738225548,-4.88733092777964,
0.));
#144480=CARTESIAN_POINT('Ctrl Pts',(-71.3840738225548,-4.88733092777964,
12.));
#144481=CARTESIAN_POINT('Ctrl Pts',(-71.3617354690342,-4.89333435702423,
0.));
#144482=CARTESIAN_POINT('Ctrl Pts',(-71.3617354690342,-4.89333435702423,
12.));
#144483=CARTESIAN_POINT('Ctrl Pts',(-71.3394341060396,-4.89930404689599,
0.));
#144484=CARTESIAN_POINT('Ctrl Pts',(-71.3394341060396,-4.89930404689599,
12.));
#144485=CARTESIAN_POINT('Ctrl Pts',(-71.3171698777124,-4.90524002732806,
0.));
#144486=CARTESIAN_POINT('Ctrl Pts',(-71.3171698777124,-4.90524002732806,
12.));
#144487=CARTESIAN_POINT('Ctrl Pts',(-71.2949429288319,-4.91114232848623,
0.));
#144488=CARTESIAN_POINT('Ctrl Pts',(-71.2949429288319,-4.91114232848623,
12.));
#144489=CARTESIAN_POINT('Ctrl Pts',(-71.27275340482,-4.91701098077041,0.));
#144490=CARTESIAN_POINT('Ctrl Pts',(-71.27275340482,-4.91701098077041,12.));
#144491=CARTESIAN_POINT('Ctrl Pts',(-71.2506014517457,-4.9228460148171,
0.));
#144492=CARTESIAN_POINT('Ctrl Pts',(-71.2506014517457,-4.9228460148171,
12.));
#144493=CARTESIAN_POINT('Ctrl Pts',(-71.2284872163248,-4.92864746150711,
0.));
#144494=CARTESIAN_POINT('Ctrl Pts',(-71.2284872163248,-4.92864746150711,
12.));
#144495=CARTESIAN_POINT('Ctrl Pts',(-71.206410845926,-4.93441535196593,
0.));
#144496=CARTESIAN_POINT('Ctrl Pts',(-71.206410845926,-4.93441535196593,
12.));
#144497=CARTESIAN_POINT('Ctrl Pts',(-71.184372488583,-4.94014971756097,
0.));
#144498=CARTESIAN_POINT('Ctrl Pts',(-71.184372488583,-4.94014971756097,
12.));
#144499=CARTESIAN_POINT('Ctrl Pts',(-71.1623722929998,-4.94585058990336,
0.));
#144500=CARTESIAN_POINT('Ctrl Pts',(-71.1623722929998,-4.94585058990336,
12.));
#144501=CARTESIAN_POINT('Ctrl Pts',(-71.1404104085561,-4.9515180008511,
0.));
#144502=CARTESIAN_POINT('Ctrl Pts',(-71.1404104085561,-4.9515180008511,
12.));
#144503=CARTESIAN_POINT('Ctrl Pts',(-71.1184869853071,-4.95715198251703,
0.));
#144504=CARTESIAN_POINT('Ctrl Pts',(-71.1184869853071,-4.95715198251703,
12.));
#144505=CARTESIAN_POINT('Ctrl Pts',(-71.0966021739922,-4.96275256726786,
0.));
#144506=CARTESIAN_POINT('Ctrl Pts',(-71.0966021739922,-4.96275256726786,
12.));
#144507=CARTESIAN_POINT('Ctrl Pts',(-71.0747561260443,-4.96831978772201,
0.));
#144508=CARTESIAN_POINT('Ctrl Pts',(-71.0747561260443,-4.96831978772201,
12.));
#144509=CARTESIAN_POINT('Ctrl Pts',(-71.0529489935959,-4.97385367675157,
0.));
#144510=CARTESIAN_POINT('Ctrl Pts',(-71.0529489935959,-4.97385367675157,
12.));
#144511=CARTESIAN_POINT('Ctrl Pts',(-71.031180929482,-4.97935426748577,
0.));
#144512=CARTESIAN_POINT('Ctrl Pts',(-71.031180929482,-4.97935426748577,
12.));
#144513=CARTESIAN_POINT('Ctrl Pts',(-71.0094520872375,-4.98482159331851,
0.));
#144514=CARTESIAN_POINT('Ctrl Pts',(-71.0094520872375,-4.98482159331851,
12.));
#144515=CARTESIAN_POINT('Ctrl Pts',(-70.9877626211112,-4.99025568790652,
0.));
#144516=CARTESIAN_POINT('Ctrl Pts',(-70.9877626211112,-4.99025568790652,
12.));
#144517=CARTESIAN_POINT('Ctrl Pts',(-70.9661126860773,-4.99565658516905,
0.));
#144518=CARTESIAN_POINT('Ctrl Pts',(-70.9661126860773,-4.99565658516905,
12.));
#144519=CARTESIAN_POINT('Ctrl Pts',(-70.9445024378439,-5.00102431929039,
0.));
#144520=CARTESIAN_POINT('Ctrl Pts',(-70.9445024378439,-5.00102431929039,
12.));
#144521=CARTESIAN_POINT('Ctrl Pts',(-70.9229320328588,-5.00635892472517,
0.));
#144522=CARTESIAN_POINT('Ctrl Pts',(-70.9229320328588,-5.00635892472517,
12.));
#144523=CARTESIAN_POINT('Ctrl Pts',(-70.9014016283123,-5.01166043620573,
0.));
#144524=CARTESIAN_POINT('Ctrl Pts',(-70.9014016283123,-5.01166043620573,
12.));
#144525=CARTESIAN_POINT('Ctrl Pts',(-70.8799113821449,-5.01692888873793,
0.));
#144526=CARTESIAN_POINT('Ctrl Pts',(-70.8799113821449,-5.01692888873793,
12.));
#144527=CARTESIAN_POINT('Ctrl Pts',(-70.8584614530517,-5.0221643176006,
0.));
#144528=CARTESIAN_POINT('Ctrl Pts',(-70.8584614530517,-5.0221643176006,
12.));
#144529=CARTESIAN_POINT('Ctrl Pts',(-70.8370520004844,-5.02736675834691,
0.));
#144530=CARTESIAN_POINT('Ctrl Pts',(-70.8370520004844,-5.02736675834691,
12.));
#144531=CARTESIAN_POINT('Ctrl Pts',(-70.8156831846494,-5.0325362468094,
0.));
#144532=CARTESIAN_POINT('Ctrl Pts',(-70.8156831846494,-5.0325362468094,
12.));
#144533=CARTESIAN_POINT('Ctrl Pts',(-70.7943551665071,-5.03767281910483,
0.));
#144534=CARTESIAN_POINT('Ctrl Pts',(-70.7943551665071,-5.03767281910483,
12.));
#144535=CARTESIAN_POINT('Ctrl Pts',(-70.7730681077997,-5.04277651163356,
0.));
#144536=CARTESIAN_POINT('Ctrl Pts',(-70.7730681077997,-5.04277651163356,
12.));
#144537=CARTESIAN_POINT('Ctrl Pts',(-70.7518221710715,-5.04784736108351,
0.));
#144538=CARTESIAN_POINT('Ctrl Pts',(-70.7518221710715,-5.04784736108351,
12.));
#144539=CARTESIAN_POINT('Ctrl Pts',(-70.7306175196856,-5.05288540443477,
0.));
#144540=CARTESIAN_POINT('Ctrl Pts',(-70.7306175196856,-5.05288540443477,
12.));
#144541=CARTESIAN_POINT('Ctrl Pts',(-70.7094543178416,-5.05789067897041,
0.));
#144542=CARTESIAN_POINT('Ctrl Pts',(-70.7094543178416,-5.05789067897041,
12.));
#144543=CARTESIAN_POINT('Ctrl Pts',(-70.6883327305755,-5.06286322227796,
0.));
#144544=CARTESIAN_POINT('Ctrl Pts',(-70.6883327305755,-5.06286322227796,
12.));
#144545=CARTESIAN_POINT('Ctrl Pts',(-70.6672529237431,-5.06780307224052,
0.));
#144546=CARTESIAN_POINT('Ctrl Pts',(-70.6672529237431,-5.06780307224052,
12.));
#144547=CARTESIAN_POINT('Ctrl Pts',(-70.6462150640009,-5.0727102670335,
0.));
#144548=CARTESIAN_POINT('Ctrl Pts',(-70.6462150640009,-5.0727102670335,
12.));
#144549=CARTESIAN_POINT('Ctrl Pts',(-70.6252193187892,-5.0775848451231,
0.));
#144550=CARTESIAN_POINT('Ctrl Pts',(-70.6252193187892,-5.0775848451231,
12.));
#144551=CARTESIAN_POINT('Ctrl Pts',(-70.6042658562951,-5.08242684526704,
0.));
#144552=CARTESIAN_POINT('Ctrl Pts',(-70.6042658562951,-5.08242684526704,
12.));
#144553=CARTESIAN_POINT('Ctrl Pts',(-70.5833548455043,-5.0872363065229,
0.));
#144554=CARTESIAN_POINT('Ctrl Pts',(-70.5833548455043,-5.0872363065229,
12.));
#144555=CARTESIAN_POINT('Ctrl Pts',(-70.5624864562841,-5.09201326826146,
0.));
#144556=CARTESIAN_POINT('Ctrl Pts',(-70.5624864562841,-5.09201326826146,
12.));
#144557=CARTESIAN_POINT('Ctrl Pts',(-70.5416608594526,-5.09675777018182,
0.));
#144558=CARTESIAN_POINT('Ctrl Pts',(-70.5416608594526,-5.09675777018182,
12.));
#144559=CARTESIAN_POINT('Ctrl Pts',(-70.5208782268482,-5.10146985232928,
0.));
#144560=CARTESIAN_POINT('Ctrl Pts',(-70.5208782268482,-5.10146985232928,
12.));
#144561=CARTESIAN_POINT('Ctrl Pts',(-70.5001387313963,-5.10614955511643,
0.));
#144562=CARTESIAN_POINT('Ctrl Pts',(-70.5001387313963,-5.10614955511643,
12.));
#144563=CARTESIAN_POINT('Ctrl Pts',(-70.4794425469799,-5.11079691929192,
0.));
#144564=CARTESIAN_POINT('Ctrl Pts',(-70.4794425469799,-5.11079691929192,
12.));
#144565=CARTESIAN_POINT('Ctrl Pts',(-70.4587898482946,-5.1154119859092,
0.));
#144566=CARTESIAN_POINT('Ctrl Pts',(-70.4587898482946,-5.1154119859092,
12.));
#144567=CARTESIAN_POINT('Ctrl Pts',(-70.438180810725,-5.11999479630214,
0.));
#144568=CARTESIAN_POINT('Ctrl Pts',(-70.438180810725,-5.11999479630214,
12.));
#144569=CARTESIAN_POINT('Ctrl Pts',(-70.4176156101633,-5.12454539205346,
0.));
#144570=CARTESIAN_POINT('Ctrl Pts',(-70.4176156101633,-5.12454539205346,
12.));
#144571=CARTESIAN_POINT('Ctrl Pts',(-70.3970944229885,-5.12906381499486,
0.));
#144572=CARTESIAN_POINT('Ctrl Pts',(-70.3970944229885,-5.12906381499486,
12.));
#144573=CARTESIAN_POINT('Ctrl Pts',(-70.3766174264786,-5.1335501072859,
0.));
#144574=CARTESIAN_POINT('Ctrl Pts',(-70.3766174264786,-5.1335501072859,
12.));
#144575=CARTESIAN_POINT('Ctrl Pts',(-70.3561847991725,-5.13800431148911,
0.));
#144576=CARTESIAN_POINT('Ctrl Pts',(-70.3561847991725,-5.13800431148911,
12.));
#144577=CARTESIAN_POINT('Ctrl Pts',(-70.3357967211782,-5.14242647063467,
0.));
#144578=CARTESIAN_POINT('Ctrl Pts',(-70.3357967211782,-5.14242647063467,
12.));
#144579=CARTESIAN_POINT('Ctrl Pts',(-70.31545337467,-5.14681662833053,0.));
#144580=CARTESIAN_POINT('Ctrl Pts',(-70.31545337467,-5.14681662833053,12.));
#144581=CARTESIAN_POINT('Ctrl Pts',(-70.2951549435469,-5.15117482869224,
0.));
#144582=CARTESIAN_POINT('Ctrl Pts',(-70.2951549435469,-5.15117482869224,
12.));
#144583=CARTESIAN_POINT('Ctrl Pts',(-70.2749016125073,-5.15550111614837,
0.));
#144584=CARTESIAN_POINT('Ctrl Pts',(-70.2749016125073,-5.15550111614837,
12.));
#144585=CARTESIAN_POINT('Ctrl Pts',(-70.2546935662719,-5.159795535282,0.));
#144586=CARTESIAN_POINT('Ctrl Pts',(-70.2546935662719,-5.159795535282,12.));
#144587=CARTESIAN_POINT('Ctrl Pts',(-70.2345309887864,-5.16405813066994,
0.));
#144588=CARTESIAN_POINT('Ctrl Pts',(-70.2345309887864,-5.16405813066994,
12.));
#144589=CARTESIAN_POINT('Ctrl Pts',(-70.2144140623004,-5.16828894670139,
0.));
#144590=CARTESIAN_POINT('Ctrl Pts',(-70.2144140623004,-5.16828894670139,
12.));
#144591=CARTESIAN_POINT('Ctrl Pts',(-70.1943429691214,-5.17248802793419,
0.));
#144592=CARTESIAN_POINT('Ctrl Pts',(-70.1943429691214,-5.17248802793419,
12.));
#144593=CARTESIAN_POINT('Ctrl Pts',(-70.1743178937102,-5.17665541952399,
0.));
#144594=CARTESIAN_POINT('Ctrl Pts',(-70.1743178937102,-5.17665541952399,
12.));
#144595=CARTESIAN_POINT('Ctrl Pts',(-70.1543390243882,-5.18079116757658,
0.));
#144596=CARTESIAN_POINT('Ctrl Pts',(-70.1543390243882,-5.18079116757658,
12.));
#144597=CARTESIAN_POINT('Ctrl Pts',(-70.1344065558106,-5.18489531966234,
0.));
#144598=CARTESIAN_POINT('Ctrl Pts',(-70.1344065558106,-5.18489531966234,
12.));
#144599=CARTESIAN_POINT('Ctrl Pts',(-70.1145206891833,-5.18896792486522,
0.));
#144600=CARTESIAN_POINT('Ctrl Pts',(-70.1145206891833,-5.18896792486522,
12.));
#144601=CARTESIAN_POINT('Ctrl Pts',(-70.0946816270957,-5.19300903271544,
0.));
#144602=CARTESIAN_POINT('Ctrl Pts',(-70.0946816270957,-5.19300903271544,
12.));
#144603=CARTESIAN_POINT('Ctrl Pts',(-70.0748895689716,-5.19701869225514,
0.));
#144604=CARTESIAN_POINT('Ctrl Pts',(-70.0748895689716,-5.19701869225514,
12.));
#144605=CARTESIAN_POINT('Ctrl Pts',(-70.0551447071106,-5.20099695122677,
0.));
#144606=CARTESIAN_POINT('Ctrl Pts',(-70.0551447071106,-5.20099695122677,
12.));
#144607=CARTESIAN_POINT('Ctrl Pts',(-70.0354472203604,-5.20494385478083,
0.));
#144608=CARTESIAN_POINT('Ctrl Pts',(-70.0354472203604,-5.20494385478083,
12.));
#144609=CARTESIAN_POINT('Ctrl Pts',(-70.0157972802255,-5.20885944672914,
0.));
#144610=CARTESIAN_POINT('Ctrl Pts',(-70.0157972802255,-5.20885944672914,
12.));
#144611=CARTESIAN_POINT('Ctrl Pts',(-69.996195063002,-5.21274377203321,
0.));
#144612=CARTESIAN_POINT('Ctrl Pts',(-69.996195063002,-5.21274377203321,
12.));
#144613=CARTESIAN_POINT('Ctrl Pts',(-69.9766407595385,-5.21659687881139,
0.));
#144614=CARTESIAN_POINT('Ctrl Pts',(-69.9766407595385,-5.21659687881139,
12.));
#144615=CARTESIAN_POINT('Ctrl Pts',(-69.9571345869996,-5.22041882075626,
0.));
#144616=CARTESIAN_POINT('Ctrl Pts',(-69.9571345869996,-5.22041882075626,
12.));
#144617=CARTESIAN_POINT('Ctrl Pts',(-69.9376767968951,-5.22420965879807,
0.));
#144618=CARTESIAN_POINT('Ctrl Pts',(-69.9376767968951,-5.22420965879807,
12.));
#144619=CARTESIAN_POINT('Ctrl Pts',(-69.9182676501892,-5.22796945602602,
0.));
#144620=CARTESIAN_POINT('Ctrl Pts',(-69.9182676501892,-5.22796945602602,
12.));
#144621=CARTESIAN_POINT('Ctrl Pts',(-69.8989073936606,-5.23169827290451,
0.));
#144622=CARTESIAN_POINT('Ctrl Pts',(-69.8989073936606,-5.23169827290451,
12.));
#144623=CARTESIAN_POINT('Ctrl Pts',(-69.8795962381676,-5.23539616279714,
0.));
#144624=CARTESIAN_POINT('Ctrl Pts',(-69.8795962381676,-5.23539616279714,
12.));
#144625=CARTESIAN_POINT('Ctrl Pts',(-69.8603343303016,-5.2390631663514,
0.));
#144626=CARTESIAN_POINT('Ctrl Pts',(-69.8603343303016,-5.2390631663514,
12.));
#144627=CARTESIAN_POINT('Ctrl Pts',(-69.8411217507931,-5.24269931055075,
0.));
#144628=CARTESIAN_POINT('Ctrl Pts',(-69.8411217507931,-5.24269931055075,
12.));
#144629=CARTESIAN_POINT('Ctrl Pts',(-69.8257911792542,-5.2455835516022,
0.));
#144630=CARTESIAN_POINT('Ctrl Pts',(-69.8257911792542,-5.2455835516022,
12.));
#144631=CARTESIAN_POINT('Ctrl Pts',(-69.8143154684447,-5.24773285666673,
0.));
#144632=CARTESIAN_POINT('Ctrl Pts',(-69.8143154684447,-5.24773285666673,
12.));
#144633=CARTESIAN_POINT('Ctrl Pts',(-69.8066748687863,-5.24915955997536,
0.));
#144634=CARTESIAN_POINT('Ctrl Pts',(-69.8066748687863,-5.24915955997536,
12.));
#144635=CARTESIAN_POINT('Ctrl Pts',(-69.8028570375098,-5.24987136994591,
0.));
#144636=CARTESIAN_POINT('Ctrl Pts',(-69.8028570375098,-5.24987136994591,
12.));
#144637=CARTESIAN_POINT('',(-69.8028570375098,-5.24987136994591,12.));
#144638=CARTESIAN_POINT('Ctrl Pts',(-69.8028570375098,-5.24987136994591,
12.));
#144639=CARTESIAN_POINT('Ctrl Pts',(-69.8066748687863,-5.24915955997536,
12.));
#144640=CARTESIAN_POINT('Ctrl Pts',(-69.8143154684447,-5.24773285666673,
12.));
#144641=CARTESIAN_POINT('Ctrl Pts',(-69.8257911792542,-5.2455835516022,
12.));
#144642=CARTESIAN_POINT('Ctrl Pts',(-69.8411217507931,-5.24269931055075,
12.));
#144643=CARTESIAN_POINT('Ctrl Pts',(-69.8603343303016,-5.2390631663514,
12.));
#144644=CARTESIAN_POINT('Ctrl Pts',(-69.8795962381676,-5.23539616279714,
12.));
#144645=CARTESIAN_POINT('Ctrl Pts',(-69.8989073936606,-5.23169827290451,
12.));
#144646=CARTESIAN_POINT('Ctrl Pts',(-69.9182676501892,-5.22796945602602,
12.));
#144647=CARTESIAN_POINT('Ctrl Pts',(-69.9376767968951,-5.22420965879807,
12.));
#144648=CARTESIAN_POINT('Ctrl Pts',(-69.9571345869996,-5.22041882075626,
12.));
#144649=CARTESIAN_POINT('Ctrl Pts',(-69.9766407595385,-5.21659687881139,
12.));
#144650=CARTESIAN_POINT('Ctrl Pts',(-69.996195063002,-5.21274377203321,
12.));
#144651=CARTESIAN_POINT('Ctrl Pts',(-70.0157972802255,-5.20885944672914,
12.));
#144652=CARTESIAN_POINT('Ctrl Pts',(-70.0354472203604,-5.20494385478083,
12.));
#144653=CARTESIAN_POINT('Ctrl Pts',(-70.0551447071106,-5.20099695122677,
12.));
#144654=CARTESIAN_POINT('Ctrl Pts',(-70.0748895689716,-5.19701869225514,
12.));
#144655=CARTESIAN_POINT('Ctrl Pts',(-70.0946816270957,-5.19300903271544,
12.));
#144656=CARTESIAN_POINT('Ctrl Pts',(-70.1145206891833,-5.18896792486522,
12.));
#144657=CARTESIAN_POINT('Ctrl Pts',(-70.1344065558106,-5.18489531966234,
12.));
#144658=CARTESIAN_POINT('Ctrl Pts',(-70.1543390243882,-5.18079116757658,
12.));
#144659=CARTESIAN_POINT('Ctrl Pts',(-70.1743178937102,-5.17665541952399,
12.));
#144660=CARTESIAN_POINT('Ctrl Pts',(-70.1943429691214,-5.17248802793419,
12.));
#144661=CARTESIAN_POINT('Ctrl Pts',(-70.2144140623004,-5.16828894670139,
12.));
#144662=CARTESIAN_POINT('Ctrl Pts',(-70.2345309887864,-5.16405813066994,
12.));
#144663=CARTESIAN_POINT('Ctrl Pts',(-70.2546935662719,-5.159795535282,12.));
#144664=CARTESIAN_POINT('Ctrl Pts',(-70.2749016125073,-5.15550111614837,
12.));
#144665=CARTESIAN_POINT('Ctrl Pts',(-70.2951549435469,-5.15117482869224,
12.));
#144666=CARTESIAN_POINT('Ctrl Pts',(-70.31545337467,-5.14681662833053,12.));
#144667=CARTESIAN_POINT('Ctrl Pts',(-70.3357967211782,-5.14242647063467,
12.));
#144668=CARTESIAN_POINT('Ctrl Pts',(-70.3561847991725,-5.13800431148911,
12.));
#144669=CARTESIAN_POINT('Ctrl Pts',(-70.3766174264786,-5.1335501072859,
12.));
#144670=CARTESIAN_POINT('Ctrl Pts',(-70.3970944229885,-5.12906381499486,
12.));
#144671=CARTESIAN_POINT('Ctrl Pts',(-70.4176156101633,-5.12454539205346,
12.));
#144672=CARTESIAN_POINT('Ctrl Pts',(-70.438180810725,-5.11999479630214,
12.));
#144673=CARTESIAN_POINT('Ctrl Pts',(-70.4587898482946,-5.1154119859092,
12.));
#144674=CARTESIAN_POINT('Ctrl Pts',(-70.4794425469799,-5.11079691929192,
12.));
#144675=CARTESIAN_POINT('Ctrl Pts',(-70.5001387313963,-5.10614955511643,
12.));
#144676=CARTESIAN_POINT('Ctrl Pts',(-70.5208782268482,-5.10146985232928,
12.));
#144677=CARTESIAN_POINT('Ctrl Pts',(-70.5416608594526,-5.09675777018182,
12.));
#144678=CARTESIAN_POINT('Ctrl Pts',(-70.5624864562841,-5.09201326826146,
12.));
#144679=CARTESIAN_POINT('Ctrl Pts',(-70.5833548455043,-5.0872363065229,
12.));
#144680=CARTESIAN_POINT('Ctrl Pts',(-70.6042658562951,-5.08242684526704,
12.));
#144681=CARTESIAN_POINT('Ctrl Pts',(-70.6252193187892,-5.0775848451231,
12.));
#144682=CARTESIAN_POINT('Ctrl Pts',(-70.6462150640009,-5.0727102670335,
12.));
#144683=CARTESIAN_POINT('Ctrl Pts',(-70.6672529237431,-5.06780307224052,
12.));
#144684=CARTESIAN_POINT('Ctrl Pts',(-70.6883327305755,-5.06286322227796,
12.));
#144685=CARTESIAN_POINT('Ctrl Pts',(-70.7094543178416,-5.05789067897041,
12.));
#144686=CARTESIAN_POINT('Ctrl Pts',(-70.7306175196856,-5.05288540443477,
12.));
#144687=CARTESIAN_POINT('Ctrl Pts',(-70.7518221710715,-5.04784736108351,
12.));
#144688=CARTESIAN_POINT('Ctrl Pts',(-70.7730681077997,-5.04277651163356,
12.));
#144689=CARTESIAN_POINT('Ctrl Pts',(-70.7943551665071,-5.03767281910483,
12.));
#144690=CARTESIAN_POINT('Ctrl Pts',(-70.8156831846494,-5.0325362468094,
12.));
#144691=CARTESIAN_POINT('Ctrl Pts',(-70.8370520004844,-5.02736675834691,
12.));
#144692=CARTESIAN_POINT('Ctrl Pts',(-70.8584614530517,-5.0221643176006,
12.));
#144693=CARTESIAN_POINT('Ctrl Pts',(-70.8799113821449,-5.01692888873793,
12.));
#144694=CARTESIAN_POINT('Ctrl Pts',(-70.9014016283123,-5.01166043620573,
12.));
#144695=CARTESIAN_POINT('Ctrl Pts',(-70.9229320328588,-5.00635892472517,
12.));
#144696=CARTESIAN_POINT('Ctrl Pts',(-70.9445024378439,-5.00102431929039,
12.));
#144697=CARTESIAN_POINT('Ctrl Pts',(-70.9661126860773,-4.99565658516905,
12.));
#144698=CARTESIAN_POINT('Ctrl Pts',(-70.9877626211112,-4.99025568790652,
12.));
#144699=CARTESIAN_POINT('Ctrl Pts',(-71.0094520872375,-4.98482159331851,
12.));
#144700=CARTESIAN_POINT('Ctrl Pts',(-71.031180929482,-4.97935426748577,
12.));
#144701=CARTESIAN_POINT('Ctrl Pts',(-71.0529489935959,-4.97385367675157,
12.));
#144702=CARTESIAN_POINT('Ctrl Pts',(-71.0747561260443,-4.96831978772201,
12.));
#144703=CARTESIAN_POINT('Ctrl Pts',(-71.0966021739922,-4.96275256726786,
12.));
#144704=CARTESIAN_POINT('Ctrl Pts',(-71.1184869853071,-4.95715198251703,
12.));
#144705=CARTESIAN_POINT('Ctrl Pts',(-71.1404104085561,-4.9515180008511,
12.));
#144706=CARTESIAN_POINT('Ctrl Pts',(-71.1623722929998,-4.94585058990336,
12.));
#144707=CARTESIAN_POINT('Ctrl Pts',(-71.184372488583,-4.94014971756097,
12.));
#144708=CARTESIAN_POINT('Ctrl Pts',(-71.206410845926,-4.93441535196593,
12.));
#144709=CARTESIAN_POINT('Ctrl Pts',(-71.2284872163248,-4.92864746150711,
12.));
#144710=CARTESIAN_POINT('Ctrl Pts',(-71.2506014517457,-4.9228460148171,
12.));
#144711=CARTESIAN_POINT('Ctrl Pts',(-71.27275340482,-4.91701098077041,12.));
#144712=CARTESIAN_POINT('Ctrl Pts',(-71.2949429288319,-4.91114232848623,
12.));
#144713=CARTESIAN_POINT('Ctrl Pts',(-71.3171698777124,-4.90524002732806,
12.));
#144714=CARTESIAN_POINT('Ctrl Pts',(-71.3394341060396,-4.89930404689599,
12.));
#144715=CARTESIAN_POINT('Ctrl Pts',(-71.3617354690342,-4.89333435702423,
12.));
#144716=CARTESIAN_POINT('Ctrl Pts',(-71.3840738225548,-4.88733092777964,
12.));
#144717=CARTESIAN_POINT('Ctrl Pts',(-71.4064490230857,-4.88129372946524,
12.));
#144718=CARTESIAN_POINT('Ctrl Pts',(-71.4288609277324,-4.8752227326188,
12.));
#144719=CARTESIAN_POINT('Ctrl Pts',(-71.4513093942216,-4.86911790800533,
12.));
#144720=CARTESIAN_POINT('Ctrl Pts',(-71.4737942808971,-4.86297922661498,
12.));
#144721=CARTESIAN_POINT('Ctrl Pts',(-71.4963154467128,-4.85680665966184,
12.));
#144722=CARTESIAN_POINT('Ctrl Pts',(-71.5188727512231,-4.85060017858786,
12.));
#144723=CARTESIAN_POINT('Ctrl Pts',(-71.5414660545778,-4.84435975506056,
12.));
#144724=CARTESIAN_POINT('Ctrl Pts',(-71.5640952175239,-4.83808536096589,
12.));
#144725=CARTESIAN_POINT('Ctrl Pts',(-71.5867601014008,-4.8317769684064,
12.));
#144726=CARTESIAN_POINT('Ctrl Pts',(-71.6094605681353,-4.8254345497002,
12.));
#144727=CARTESIAN_POINT('Ctrl Pts',(-71.6321964802297,-4.81905807738541,
12.));
#144728=CARTESIAN_POINT('Ctrl Pts',(-71.6549677007582,-4.81264752421713,
12.));
#144729=CARTESIAN_POINT('Ctrl Pts',(-71.6777740933687,-4.80620286316075,
12.));
#144730=CARTESIAN_POINT('Ctrl Pts',(-71.7006155222764,-4.7997240673901,
12.));
#144731=CARTESIAN_POINT('Ctrl Pts',(-71.723491852261,-4.79321111028676,
12.));
#144732=CARTESIAN_POINT('Ctrl Pts',(-71.7464029486563,-4.78666396544458,
12.));
#144733=CARTESIAN_POINT('Ctrl Pts',(-71.769348677346,-4.7800826066665,12.));
#144734=CARTESIAN_POINT('Ctrl Pts',(-71.7923289047643,-4.77346700795792,
12.));
#144735=CARTESIAN_POINT('Ctrl Pts',(-71.8153434978923,-4.76681714352502,
12.));
#144736=CARTESIAN_POINT('Ctrl Pts',(-71.8383923242531,-4.76013298777419,
12.));
#144737=CARTESIAN_POINT('Ctrl Pts',(-71.8614752519008,-4.75341451531669,
12.));
#144738=CARTESIAN_POINT('Ctrl Pts',(-71.8845921494189,-4.74666170096547,
12.));
#144739=CARTESIAN_POINT('Ctrl Pts',(-71.9077428859212,-4.73987451972863,
12.));
#144740=CARTESIAN_POINT('Ctrl Pts',(-71.9309273310471,-4.73305294680785,
12.));
#144741=CARTESIAN_POINT('Ctrl Pts',(-71.9541453549579,-4.72619695759774,
12.));
#144742=CARTESIAN_POINT('Ctrl Pts',(-71.9773968283259,-4.7193065276907,
12.));
#144743=CARTESIAN_POINT('Ctrl Pts',(-72.0006816223325,-4.71238163287396,
12.));
#144744=CARTESIAN_POINT('Ctrl Pts',(-72.0239996086686,-4.705422249123,12.));
#144745=CARTESIAN_POINT('Ctrl Pts',(-72.0473506595318,-4.69842835259992,
12.));
#144746=CARTESIAN_POINT('Ctrl Pts',(-72.0707346476213,-4.69139991965283,
12.));
#144747=CARTESIAN_POINT('Ctrl Pts',(-72.0941514461287,-4.68433692682068,
12.));
#144748=CARTESIAN_POINT('Ctrl Pts',(-72.1176009287351,-4.67723935083094,
12.));
#144749=CARTESIAN_POINT('Ctrl Pts',(-72.1410829696128,-4.67010716859285,
12.));
#144750=CARTESIAN_POINT('Ctrl Pts',(-72.1645974434216,-4.66294035719569,
12.));
#144751=CARTESIAN_POINT('Ctrl Pts',(-72.1881442253053,-4.65573889390822,
12.));
#144752=CARTESIAN_POINT('Ctrl Pts',(-72.2117231908822,-4.64850275618323,
12.));
#144753=CARTESIAN_POINT('Ctrl Pts',(-72.2353342162417,-4.64123192165627,
12.));
#144754=CARTESIAN_POINT('Ctrl Pts',(-72.2589771779456,-4.63392636813843,
12.));
#144755=CARTESIAN_POINT('Ctrl Pts',(-72.2826519530259,-4.62658607361466,
12.));
#144756=CARTESIAN_POINT('Ctrl Pts',(-72.3063584189807,-4.61921101624292,
12.));
#144757=CARTESIAN_POINT('Ctrl Pts',(-72.3300964537658,-4.61180117435862,
12.));
#144758=CARTESIAN_POINT('Ctrl Pts',(-72.3538659357913,-4.60435652647453,
12.));
#144759=CARTESIAN_POINT('Ctrl Pts',(-72.3776667439227,-4.5968770512733,
12.));
#144760=CARTESIAN_POINT('Ctrl Pts',(-72.401498757478,-4.58936272760544,
12.));
#144761=CARTESIAN_POINT('Ctrl Pts',(-72.4253618562252,-4.58181353448851,
12.));
#144762=CARTESIAN_POINT('Ctrl Pts',(-72.4492559203745,-4.57422945111102,
12.));
#144763=CARTESIAN_POINT('Ctrl Pts',(-72.4731808305728,-4.56661045683376,
12.));
#144764=CARTESIAN_POINT('Ctrl Pts',(-72.4971364679068,-4.5589565311822,
12.));
#144765=CARTESIAN_POINT('Ctrl Pts',(-72.5211227139001,-4.55126765384404,
12.));
#144766=CARTESIAN_POINT('Ctrl Pts',(-72.5451394505104,-4.54354380466822,
12.));
#144767=CARTESIAN_POINT('Ctrl Pts',(-72.5691865601223,-4.53578496366799,
12.));
#144768=CARTESIAN_POINT('Ctrl Pts',(-72.5932639255409,-4.52799111102391,
12.));
#144769=CARTESIAN_POINT('Ctrl Pts',(-72.6173714299942,-4.52016222707637,
12.));
#144770=CARTESIAN_POINT('Ctrl Pts',(-72.6415089571321,-4.51229829232264,
12.));
#144771=CARTESIAN_POINT('Ctrl Pts',(-72.6656763910241,-4.50439928741604,
12.));
#144772=CARTESIAN_POINT('Ctrl Pts',(-72.6898736161542,-4.49646519316812,
12.));
#144773=CARTESIAN_POINT('Ctrl Pts',(-72.714100517414,-4.48849599055337,
12.));
#144774=CARTESIAN_POINT('Ctrl Pts',(-72.738356980103,-4.48049166070205,
12.));
#144775=CARTESIAN_POINT('Ctrl Pts',(-72.7626428899281,-4.47245218489609,
12.));
#144776=CARTESIAN_POINT('Ctrl Pts',(-72.7869581329994,-4.46437754456792,
12.));
#144777=CARTESIAN_POINT('Ctrl Pts',(-72.8113025958262,-4.45626772130146,
12.));
#144778=CARTESIAN_POINT('Ctrl Pts',(-72.8356761653069,-4.44812269683737,
12.));
#144779=CARTESIAN_POINT('Ctrl Pts',(-72.8600787287318,-4.43994245306818,
12.));
#144780=CARTESIAN_POINT('Ctrl Pts',(-72.8845101737855,-4.43172697203349,
12.));
#144781=CARTESIAN_POINT('Ctrl Pts',(-72.9089703885462,-4.42347623591941,
12.));
#144782=CARTESIAN_POINT('Ctrl Pts',(-72.9334592614829,-4.41519022705921,
12.));
#144783=CARTESIAN_POINT('Ctrl Pts',(-72.95797668145,-4.40686892793957,12.));
#144784=CARTESIAN_POINT('Ctrl Pts',(-72.9825225376846,-4.39851232119722,
12.));
#144785=CARTESIAN_POINT('Ctrl Pts',(-73.007096719804,-4.39012038961139,
12.));
#144786=CARTESIAN_POINT('Ctrl Pts',(-73.0316991177993,-4.3816931161015,
12.));
#144787=CARTESIAN_POINT('Ctrl Pts',(-73.0563296220299,-4.37323048372607,
12.));
#144788=CARTESIAN_POINT('Ctrl Pts',(-73.0809881232103,-4.36473247568641,
12.));
#144789=CARTESIAN_POINT('Ctrl Pts',(-73.1056745124087,-4.35619907532719,
12.));
#144790=CARTESIAN_POINT('Ctrl Pts',(-73.130388681059,-4.34763026613157,
12.));
#144791=CARTESIAN_POINT('Ctrl Pts',(-73.1551305209685,-4.3390260317214,
12.));
#144792=CARTESIAN_POINT('Ctrl Pts',(-73.1798999243235,-4.33038635585876,
12.));
#144793=CARTESIAN_POINT('Ctrl Pts',(-73.204696783694,-4.32171122245214,
12.));
#144794=CARTESIAN_POINT('Ctrl Pts',(-73.2295209920334,-4.31300061556098,
12.));
#144795=CARTESIAN_POINT('Ctrl Pts',(-73.2543724426577,-4.3042545193823,
12.));
#144796=CARTESIAN_POINT('Ctrl Pts',(-73.2792510292254,-4.29547291824287,
12.));
#144797=CARTESIAN_POINT('Ctrl Pts',(-73.3041566457135,-4.28665579659301,
12.));
#144798=CARTESIAN_POINT('Ctrl Pts',(-73.3290891863949,-4.27780313900389,
12.));
#144799=CARTESIAN_POINT('Ctrl Pts',(-73.3540485458065,-4.26891493016699,
12.));
#144800=CARTESIAN_POINT('Ctrl Pts',(-73.3790346187938,-4.25999115489899,
12.));
#144801=CARTESIAN_POINT('Ctrl Pts',(-73.4040473005592,-4.25103179814886,
12.));
#144802=CARTESIAN_POINT('Ctrl Pts',(-73.4290864867101,-4.24203684500938,
12.));
#144803=CARTESIAN_POINT('Ctrl Pts',(-73.4541520732948,-4.23300628072758,
12.));
#144804=CARTESIAN_POINT('Ctrl Pts',(-73.4792439568633,-4.22394009072756,
12.));
#144805=CARTESIAN_POINT('Ctrl Pts',(-73.5043620344116,-4.21483826059441,
12.));
#144806=CARTESIAN_POINT('Ctrl Pts',(-73.5295062032628,-4.2057007760373,
12.));
#144807=CARTESIAN_POINT('Ctrl Pts',(-73.5546763609572,-4.19652762286126,
12.));
#144808=CARTESIAN_POINT('Ctrl Pts',(-73.5798724051519,-4.18731878694236,
12.));
#144809=CARTESIAN_POINT('Ctrl Pts',(-73.6050942334768,-4.17807425419812,
12.));
#144810=CARTESIAN_POINT('Ctrl Pts',(-73.6303417435251,-4.1687940105878,
12.));
#144811=CARTESIAN_POINT('Ctrl Pts',(-73.6556148331489,-4.15947804217783,
12.));
#144812=CARTESIAN_POINT('Ctrl Pts',(-73.6809134006897,-4.15012633519723,
12.));
#144813=CARTESIAN_POINT('Ctrl Pts',(-73.7062373452342,-4.14073887610153,
12.));
#144814=CARTESIAN_POINT('Ctrl Pts',(-73.7315865668522,-4.13131565163578,
12.));
#144815=CARTESIAN_POINT('Ctrl Pts',(-73.7569609668528,-4.12185664890556,
12.));
#144816=CARTESIAN_POINT('Ctrl Pts',(-73.7823604472159,-4.11236185522787,
12.));
#144817=CARTESIAN_POINT('Ctrl Pts',(-73.8077849100342,-4.10283125798729,
12.));
#144818=CARTESIAN_POINT('Ctrl Pts',(-73.8332342568989,-4.09326484448232,
12.));
#144819=CARTESIAN_POINT('Ctrl Pts',(-73.8587083884191,-4.08366260180674,
12.));
#144820=CARTESIAN_POINT('Ctrl Pts',(-73.8842072034008,-4.07402451665244,
12.));
#144821=CARTESIAN_POINT('Ctrl Pts',(-73.9097305995115,-4.06435057547324,
12.));
#144822=CARTESIAN_POINT('Ctrl Pts',(-73.9352784747608,-4.05464076484752,
12.));
#144823=CARTESIAN_POINT('Ctrl Pts',(-73.9608507287909,-4.04489507179957,
12.));
#144824=CARTESIAN_POINT('Ctrl Pts',(-73.9864472641033,-4.03511348410659,
12.));
#144825=CARTESIAN_POINT('Ctrl Pts',(-74.012067987646,-4.02529599070094,
12.));
#144826=CARTESIAN_POINT('Ctrl Pts',(-74.0377128111863,-4.0154425817671,
12.));
#144827=CARTESIAN_POINT('Ctrl Pts',(-74.059715978211,-4.00696550627363,
12.));
#144828=CARTESIAN_POINT('Ctrl Pts',(-74.0765982943677,-4.0004468971198,
12.));
#144829=CARTESIAN_POINT('Ctrl Pts',(-74.0883491449956,-3.99590266746987,
12.));
#144830=CARTESIAN_POINT('Ctrl Pts',(-74.0949615399621,-3.99334334445522,
12.));
#144831=CARTESIAN_POINT('Ctrl Pts',(-74.0964320766209,-3.99277406490865,
12.));
#144832=CARTESIAN_POINT('',(-69.8028570375098,-5.24987136994591,0.));
#144833=CARTESIAN_POINT('',(-69.8028570375097,-5.24987136994591,0.));
#144834=CARTESIAN_POINT('Ctrl Pts',(-74.0964320766209,-3.99277406490865,
0.));
#144835=CARTESIAN_POINT('Ctrl Pts',(-74.094961539962,-3.99334334445523,
0.));
#144836=CARTESIAN_POINT('Ctrl Pts',(-74.0883491449955,-3.99590266746987,
0.));
#144837=CARTESIAN_POINT('Ctrl Pts',(-74.0765982943677,-4.0004468971198,
0.));
#144838=CARTESIAN_POINT('Ctrl Pts',(-74.059715978211,-4.00696550627363,
0.));
#144839=CARTESIAN_POINT('Ctrl Pts',(-74.0377128111863,-4.0154425817671,
0.));
#144840=CARTESIAN_POINT('Ctrl Pts',(-74.012067987646,-4.02529599070094,
0.));
#144841=CARTESIAN_POINT('Ctrl Pts',(-73.9864472641033,-4.03511348410659,
0.));
#144842=CARTESIAN_POINT('Ctrl Pts',(-73.9608507287909,-4.04489507179957,
0.));
#144843=CARTESIAN_POINT('Ctrl Pts',(-73.9352784747608,-4.05464076484752,
0.));
#144844=CARTESIAN_POINT('Ctrl Pts',(-73.9097305995115,-4.06435057547324,
0.));
#144845=CARTESIAN_POINT('Ctrl Pts',(-73.8842072034008,-4.07402451665244,
0.));
#144846=CARTESIAN_POINT('Ctrl Pts',(-73.8587083884191,-4.08366260180674,
0.));
#144847=CARTESIAN_POINT('Ctrl Pts',(-73.8332342568989,-4.09326484448232,
0.));
#144848=CARTESIAN_POINT('Ctrl Pts',(-73.8077849100342,-4.10283125798729,
0.));
#144849=CARTESIAN_POINT('Ctrl Pts',(-73.7823604472159,-4.11236185522787,
0.));
#144850=CARTESIAN_POINT('Ctrl Pts',(-73.7569609668528,-4.12185664890556,
0.));
#144851=CARTESIAN_POINT('Ctrl Pts',(-73.7315865668522,-4.13131565163578,
0.));
#144852=CARTESIAN_POINT('Ctrl Pts',(-73.7062373452342,-4.14073887610153,
0.));
#144853=CARTESIAN_POINT('Ctrl Pts',(-73.6809134006897,-4.15012633519723,
0.));
#144854=CARTESIAN_POINT('Ctrl Pts',(-73.6556148331489,-4.15947804217783,
0.));
#144855=CARTESIAN_POINT('Ctrl Pts',(-73.6303417435251,-4.1687940105878,
0.));
#144856=CARTESIAN_POINT('Ctrl Pts',(-73.6050942334768,-4.17807425419812,
0.));
#144857=CARTESIAN_POINT('Ctrl Pts',(-73.5798724051519,-4.18731878694236,
0.));
#144858=CARTESIAN_POINT('Ctrl Pts',(-73.5546763609572,-4.19652762286126,
0.));
#144859=CARTESIAN_POINT('Ctrl Pts',(-73.5295062032628,-4.2057007760373,
0.));
#144860=CARTESIAN_POINT('Ctrl Pts',(-73.5043620344116,-4.21483826059441,
0.));
#144861=CARTESIAN_POINT('Ctrl Pts',(-73.4792439568633,-4.22394009072756,
0.));
#144862=CARTESIAN_POINT('Ctrl Pts',(-73.4541520732948,-4.23300628072758,
0.));
#144863=CARTESIAN_POINT('Ctrl Pts',(-73.4290864867101,-4.24203684500938,
0.));
#144864=CARTESIAN_POINT('Ctrl Pts',(-73.4040473005592,-4.25103179814886,
0.));
#144865=CARTESIAN_POINT('Ctrl Pts',(-73.3790346187938,-4.25999115489899,
0.));
#144866=CARTESIAN_POINT('Ctrl Pts',(-73.3540485458065,-4.26891493016699,
0.));
#144867=CARTESIAN_POINT('Ctrl Pts',(-73.3290891863949,-4.27780313900389,
0.));
#144868=CARTESIAN_POINT('Ctrl Pts',(-73.3041566457135,-4.28665579659301,
0.));
#144869=CARTESIAN_POINT('Ctrl Pts',(-73.2792510292254,-4.29547291824287,
0.));
#144870=CARTESIAN_POINT('Ctrl Pts',(-73.2543724426577,-4.3042545193823,
0.));
#144871=CARTESIAN_POINT('Ctrl Pts',(-73.2295209920334,-4.31300061556098,
0.));
#144872=CARTESIAN_POINT('Ctrl Pts',(-73.204696783694,-4.32171122245214,
0.));
#144873=CARTESIAN_POINT('Ctrl Pts',(-73.1798999243235,-4.33038635585876,
0.));
#144874=CARTESIAN_POINT('Ctrl Pts',(-73.1551305209685,-4.3390260317214,
0.));
#144875=CARTESIAN_POINT('Ctrl Pts',(-73.130388681059,-4.34763026613157,
0.));
#144876=CARTESIAN_POINT('Ctrl Pts',(-73.1056745124087,-4.35619907532719,
0.));
#144877=CARTESIAN_POINT('Ctrl Pts',(-73.0809881232103,-4.36473247568641,
0.));
#144878=CARTESIAN_POINT('Ctrl Pts',(-73.0563296220299,-4.37323048372607,
0.));
#144879=CARTESIAN_POINT('Ctrl Pts',(-73.0316991177993,-4.3816931161015,
0.));
#144880=CARTESIAN_POINT('Ctrl Pts',(-73.007096719804,-4.39012038961139,
0.));
#144881=CARTESIAN_POINT('Ctrl Pts',(-72.9825225376846,-4.39851232119722,
0.));
#144882=CARTESIAN_POINT('Ctrl Pts',(-72.95797668145,-4.40686892793957,0.));
#144883=CARTESIAN_POINT('Ctrl Pts',(-72.9334592614829,-4.41519022705921,
0.));
#144884=CARTESIAN_POINT('Ctrl Pts',(-72.9089703885462,-4.42347623591941,
0.));
#144885=CARTESIAN_POINT('Ctrl Pts',(-72.8845101737855,-4.43172697203349,
0.));
#144886=CARTESIAN_POINT('Ctrl Pts',(-72.8600787287318,-4.43994245306818,
0.));
#144887=CARTESIAN_POINT('Ctrl Pts',(-72.8356761653069,-4.44812269683737,
0.));
#144888=CARTESIAN_POINT('Ctrl Pts',(-72.8113025958262,-4.45626772130146,
0.));
#144889=CARTESIAN_POINT('Ctrl Pts',(-72.7869581329994,-4.46437754456792,
0.));
#144890=CARTESIAN_POINT('Ctrl Pts',(-72.7626428899281,-4.47245218489609,
0.));
#144891=CARTESIAN_POINT('Ctrl Pts',(-72.738356980103,-4.48049166070205,
0.));
#144892=CARTESIAN_POINT('Ctrl Pts',(-72.714100517414,-4.48849599055337,
0.));
#144893=CARTESIAN_POINT('Ctrl Pts',(-72.6898736161542,-4.49646519316812,
0.));
#144894=CARTESIAN_POINT('Ctrl Pts',(-72.6656763910241,-4.50439928741604,
0.));
#144895=CARTESIAN_POINT('Ctrl Pts',(-72.6415089571321,-4.51229829232264,
0.));
#144896=CARTESIAN_POINT('Ctrl Pts',(-72.6173714299942,-4.52016222707637,
0.));
#144897=CARTESIAN_POINT('Ctrl Pts',(-72.5932639255409,-4.52799111102391,
0.));
#144898=CARTESIAN_POINT('Ctrl Pts',(-72.5691865601223,-4.53578496366799,
0.));
#144899=CARTESIAN_POINT('Ctrl Pts',(-72.5451394505104,-4.54354380466822,
0.));
#144900=CARTESIAN_POINT('Ctrl Pts',(-72.5211227139001,-4.55126765384404,
0.));
#144901=CARTESIAN_POINT('Ctrl Pts',(-72.4971364679068,-4.5589565311822,
0.));
#144902=CARTESIAN_POINT('Ctrl Pts',(-72.4731808305728,-4.56661045683376,
0.));
#144903=CARTESIAN_POINT('Ctrl Pts',(-72.4492559203745,-4.57422945111102,
0.));
#144904=CARTESIAN_POINT('Ctrl Pts',(-72.4253618562252,-4.58181353448851,
0.));
#144905=CARTESIAN_POINT('Ctrl Pts',(-72.401498757478,-4.58936272760544,
0.));
#144906=CARTESIAN_POINT('Ctrl Pts',(-72.3776667439227,-4.5968770512733,
0.));
#144907=CARTESIAN_POINT('Ctrl Pts',(-72.3538659357913,-4.60435652647453,
0.));
#144908=CARTESIAN_POINT('Ctrl Pts',(-72.3300964537658,-4.61180117435862,
0.));
#144909=CARTESIAN_POINT('Ctrl Pts',(-72.3063584189807,-4.61921101624292,
0.));
#144910=CARTESIAN_POINT('Ctrl Pts',(-72.2826519530259,-4.62658607361466,
0.));
#144911=CARTESIAN_POINT('Ctrl Pts',(-72.2589771779456,-4.63392636813843,
0.));
#144912=CARTESIAN_POINT('Ctrl Pts',(-72.2353342162417,-4.64123192165627,
0.));
#144913=CARTESIAN_POINT('Ctrl Pts',(-72.2117231908822,-4.64850275618323,
0.));
#144914=CARTESIAN_POINT('Ctrl Pts',(-72.1881442253053,-4.65573889390822,
0.));
#144915=CARTESIAN_POINT('Ctrl Pts',(-72.1645974434216,-4.66294035719569,
0.));
#144916=CARTESIAN_POINT('Ctrl Pts',(-72.1410829696128,-4.67010716859285,
0.));
#144917=CARTESIAN_POINT('Ctrl Pts',(-72.1176009287351,-4.67723935083094,
0.));
#144918=CARTESIAN_POINT('Ctrl Pts',(-72.0941514461287,-4.68433692682068,
0.));
#144919=CARTESIAN_POINT('Ctrl Pts',(-72.0707346476213,-4.69139991965283,
0.));
#144920=CARTESIAN_POINT('Ctrl Pts',(-72.0473506595318,-4.69842835259992,
0.));
#144921=CARTESIAN_POINT('Ctrl Pts',(-72.0239996086686,-4.705422249123,0.));
#144922=CARTESIAN_POINT('Ctrl Pts',(-72.0006816223325,-4.71238163287396,
0.));
#144923=CARTESIAN_POINT('Ctrl Pts',(-71.9773968283259,-4.7193065276907,
0.));
#144924=CARTESIAN_POINT('Ctrl Pts',(-71.9541453549579,-4.72619695759774,
0.));
#144925=CARTESIAN_POINT('Ctrl Pts',(-71.9309273310471,-4.73305294680785,
0.));
#144926=CARTESIAN_POINT('Ctrl Pts',(-71.9077428859212,-4.73987451972863,
0.));
#144927=CARTESIAN_POINT('Ctrl Pts',(-71.8845921494189,-4.74666170096547,
0.));
#144928=CARTESIAN_POINT('Ctrl Pts',(-71.8614752519008,-4.75341451531669,
0.));
#144929=CARTESIAN_POINT('Ctrl Pts',(-71.8383923242531,-4.76013298777419,
0.));
#144930=CARTESIAN_POINT('Ctrl Pts',(-71.8153434978923,-4.76681714352502,
0.));
#144931=CARTESIAN_POINT('Ctrl Pts',(-71.7923289047643,-4.77346700795792,
0.));
#144932=CARTESIAN_POINT('Ctrl Pts',(-71.769348677346,-4.7800826066665,0.));
#144933=CARTESIAN_POINT('Ctrl Pts',(-71.7464029486563,-4.78666396544458,
0.));
#144934=CARTESIAN_POINT('Ctrl Pts',(-71.723491852261,-4.79321111028676,
0.));
#144935=CARTESIAN_POINT('Ctrl Pts',(-71.7006155222764,-4.7997240673901,
0.));
#144936=CARTESIAN_POINT('Ctrl Pts',(-71.6777740933687,-4.80620286316075,
0.));
#144937=CARTESIAN_POINT('Ctrl Pts',(-71.6549677007582,-4.81264752421713,
0.));
#144938=CARTESIAN_POINT('Ctrl Pts',(-71.6321964802297,-4.81905807738541,
0.));
#144939=CARTESIAN_POINT('Ctrl Pts',(-71.6094605681353,-4.8254345497002,
0.));
#144940=CARTESIAN_POINT('Ctrl Pts',(-71.5867601014008,-4.8317769684064,
0.));
#144941=CARTESIAN_POINT('Ctrl Pts',(-71.5640952175239,-4.83808536096589,
0.));
#144942=CARTESIAN_POINT('Ctrl Pts',(-71.5414660545778,-4.84435975506056,
0.));
#144943=CARTESIAN_POINT('Ctrl Pts',(-71.5188727512231,-4.85060017858786,
0.));
#144944=CARTESIAN_POINT('Ctrl Pts',(-71.4963154467128,-4.85680665966184,
0.));
#144945=CARTESIAN_POINT('Ctrl Pts',(-71.4737942808971,-4.86297922661498,
0.));
#144946=CARTESIAN_POINT('Ctrl Pts',(-71.4513093942216,-4.86911790800533,
0.));
#144947=CARTESIAN_POINT('Ctrl Pts',(-71.4288609277324,-4.8752227326188,
0.));
#144948=CARTESIAN_POINT('Ctrl Pts',(-71.4064490230857,-4.88129372946524,
0.));
#144949=CARTESIAN_POINT('Ctrl Pts',(-71.3840738225548,-4.88733092777964,
0.));
#144950=CARTESIAN_POINT('Ctrl Pts',(-71.3617354690342,-4.89333435702423,
0.));
#144951=CARTESIAN_POINT('Ctrl Pts',(-71.3394341060396,-4.89930404689599,
0.));
#144952=CARTESIAN_POINT('Ctrl Pts',(-71.3171698777124,-4.90524002732806,
0.));
#144953=CARTESIAN_POINT('Ctrl Pts',(-71.2949429288319,-4.91114232848623,
0.));
#144954=CARTESIAN_POINT('Ctrl Pts',(-71.27275340482,-4.91701098077041,0.));
#144955=CARTESIAN_POINT('Ctrl Pts',(-71.2506014517457,-4.9228460148171,
0.));
#144956=CARTESIAN_POINT('Ctrl Pts',(-71.2284872163248,-4.92864746150711,
0.));
#144957=CARTESIAN_POINT('Ctrl Pts',(-71.206410845926,-4.93441535196593,
0.));
#144958=CARTESIAN_POINT('Ctrl Pts',(-71.184372488583,-4.94014971756097,
0.));
#144959=CARTESIAN_POINT('Ctrl Pts',(-71.1623722929998,-4.94585058990336,
0.));
#144960=CARTESIAN_POINT('Ctrl Pts',(-71.1404104085561,-4.9515180008511,
0.));
#144961=CARTESIAN_POINT('Ctrl Pts',(-71.1184869853071,-4.95715198251703,
0.));
#144962=CARTESIAN_POINT('Ctrl Pts',(-71.0966021739922,-4.96275256726786,
0.));
#144963=CARTESIAN_POINT('Ctrl Pts',(-71.0747561260443,-4.96831978772201,
0.));
#144964=CARTESIAN_POINT('Ctrl Pts',(-71.0529489935959,-4.97385367675157,
0.));
#144965=CARTESIAN_POINT('Ctrl Pts',(-71.031180929482,-4.97935426748577,
0.));
#144966=CARTESIAN_POINT('Ctrl Pts',(-71.0094520872375,-4.98482159331851,
0.));
#144967=CARTESIAN_POINT('Ctrl Pts',(-70.9877626211112,-4.99025568790652,
0.));
#144968=CARTESIAN_POINT('Ctrl Pts',(-70.9661126860773,-4.99565658516905,
0.));
#144969=CARTESIAN_POINT('Ctrl Pts',(-70.9445024378439,-5.00102431929039,
0.));
#144970=CARTESIAN_POINT('Ctrl Pts',(-70.9229320328588,-5.00635892472517,
0.));
#144971=CARTESIAN_POINT('Ctrl Pts',(-70.9014016283123,-5.01166043620573,
0.));
#144972=CARTESIAN_POINT('Ctrl Pts',(-70.8799113821449,-5.01692888873793,
0.));
#144973=CARTESIAN_POINT('Ctrl Pts',(-70.8584614530517,-5.0221643176006,
0.));
#144974=CARTESIAN_POINT('Ctrl Pts',(-70.8370520004844,-5.02736675834691,
0.));
#144975=CARTESIAN_POINT('Ctrl Pts',(-70.8156831846494,-5.0325362468094,
0.));
#144976=CARTESIAN_POINT('Ctrl Pts',(-70.7943551665071,-5.03767281910483,
0.));
#144977=CARTESIAN_POINT('Ctrl Pts',(-70.7730681077997,-5.04277651163356,
0.));
#144978=CARTESIAN_POINT('Ctrl Pts',(-70.7518221710715,-5.04784736108351,
0.));
#144979=CARTESIAN_POINT('Ctrl Pts',(-70.7306175196856,-5.05288540443477,
0.));
#144980=CARTESIAN_POINT('Ctrl Pts',(-70.7094543178416,-5.05789067897041,
0.));
#144981=CARTESIAN_POINT('Ctrl Pts',(-70.6883327305755,-5.06286322227796,
0.));
#144982=CARTESIAN_POINT('Ctrl Pts',(-70.6672529237431,-5.06780307224052,
0.));
#144983=CARTESIAN_POINT('Ctrl Pts',(-70.6462150640009,-5.0727102670335,
0.));
#144984=CARTESIAN_POINT('Ctrl Pts',(-70.6252193187892,-5.0775848451231,
0.));
#144985=CARTESIAN_POINT('Ctrl Pts',(-70.6042658562951,-5.08242684526704,
0.));
#144986=CARTESIAN_POINT('Ctrl Pts',(-70.5833548455043,-5.0872363065229,
0.));
#144987=CARTESIAN_POINT('Ctrl Pts',(-70.5624864562841,-5.09201326826146,
0.));
#144988=CARTESIAN_POINT('Ctrl Pts',(-70.5416608594526,-5.09675777018182,
0.));
#144989=CARTESIAN_POINT('Ctrl Pts',(-70.5208782268482,-5.10146985232928,
0.));
#144990=CARTESIAN_POINT('Ctrl Pts',(-70.5001387313963,-5.10614955511643,
0.));
#144991=CARTESIAN_POINT('Ctrl Pts',(-70.4794425469799,-5.11079691929192,
0.));
#144992=CARTESIAN_POINT('Ctrl Pts',(-70.4587898482946,-5.1154119859092,
0.));
#144993=CARTESIAN_POINT('Ctrl Pts',(-70.438180810725,-5.11999479630214,
0.));
#144994=CARTESIAN_POINT('Ctrl Pts',(-70.4176156101633,-5.12454539205346,
0.));
#144995=CARTESIAN_POINT('Ctrl Pts',(-70.3970944229885,-5.12906381499486,
0.));
#144996=CARTESIAN_POINT('Ctrl Pts',(-70.3766174264786,-5.1335501072859,
0.));
#144997=CARTESIAN_POINT('Ctrl Pts',(-70.3561847991725,-5.13800431148911,
0.));
#144998=CARTESIAN_POINT('Ctrl Pts',(-70.3357967211782,-5.14242647063467,
0.));
#144999=CARTESIAN_POINT('Ctrl Pts',(-70.31545337467,-5.14681662833053,0.));
#145000=CARTESIAN_POINT('Ctrl Pts',(-70.2951549435469,-5.15117482869224,
0.));
#145001=CARTESIAN_POINT('Ctrl Pts',(-70.2749016125073,-5.15550111614837,
0.));
#145002=CARTESIAN_POINT('Ctrl Pts',(-70.2546935662719,-5.159795535282,0.));
#145003=CARTESIAN_POINT('Ctrl Pts',(-70.2345309887864,-5.16405813066994,
0.));
#145004=CARTESIAN_POINT('Ctrl Pts',(-70.2144140623004,-5.16828894670139,
0.));
#145005=CARTESIAN_POINT('Ctrl Pts',(-70.1943429691214,-5.17248802793419,
0.));
#145006=CARTESIAN_POINT('Ctrl Pts',(-70.1743178937102,-5.17665541952399,
0.));
#145007=CARTESIAN_POINT('Ctrl Pts',(-70.1543390243882,-5.18079116757658,
0.));
#145008=CARTESIAN_POINT('Ctrl Pts',(-70.1344065558106,-5.18489531966234,
0.));
#145009=CARTESIAN_POINT('Ctrl Pts',(-70.1145206891833,-5.18896792486522,
0.));
#145010=CARTESIAN_POINT('Ctrl Pts',(-70.0946816270957,-5.19300903271544,
0.));
#145011=CARTESIAN_POINT('Ctrl Pts',(-70.0748895689716,-5.19701869225514,
0.));
#145012=CARTESIAN_POINT('Ctrl Pts',(-70.0551447071106,-5.20099695122677,
0.));
#145013=CARTESIAN_POINT('Ctrl Pts',(-70.0354472203604,-5.20494385478083,
0.));
#145014=CARTESIAN_POINT('Ctrl Pts',(-70.0157972802255,-5.20885944672914,
0.));
#145015=CARTESIAN_POINT('Ctrl Pts',(-69.996195063002,-5.21274377203321,
0.));
#145016=CARTESIAN_POINT('Ctrl Pts',(-69.9766407595385,-5.21659687881139,
0.));
#145017=CARTESIAN_POINT('Ctrl Pts',(-69.9571345869996,-5.22041882075626,
0.));
#145018=CARTESIAN_POINT('Ctrl Pts',(-69.9376767968951,-5.22420965879807,
0.));
#145019=CARTESIAN_POINT('Ctrl Pts',(-69.9182676501892,-5.22796945602602,
0.));
#145020=CARTESIAN_POINT('Ctrl Pts',(-69.8989073936606,-5.23169827290451,
0.));
#145021=CARTESIAN_POINT('Ctrl Pts',(-69.8795962381676,-5.23539616279714,
0.));
#145022=CARTESIAN_POINT('Ctrl Pts',(-69.8603343303016,-5.2390631663514,
0.));
#145023=CARTESIAN_POINT('Ctrl Pts',(-69.8411217507931,-5.24269931055075,
0.));
#145024=CARTESIAN_POINT('Ctrl Pts',(-69.8257911792542,-5.2455835516022,
0.));
#145025=CARTESIAN_POINT('Ctrl Pts',(-69.8143154684447,-5.24773285666673,
0.));
#145026=CARTESIAN_POINT('Ctrl Pts',(-69.8066748687863,-5.24915955997536,
0.));
#145027=CARTESIAN_POINT('Ctrl Pts',(-69.8028570375098,-5.24987136994591,
0.));
#145028=CARTESIAN_POINT('Ctrl Pts',(-74.4537274248118,2.62535189104656,
0.));
#145029=CARTESIAN_POINT('Ctrl Pts',(-74.4537274248118,2.62535189104656,
12.));
#145030=CARTESIAN_POINT('Ctrl Pts',(-74.4487312586601,2.62283178248297,
0.));
#145031=CARTESIAN_POINT('Ctrl Pts',(-74.4487312586601,2.62283178248297,
12.));
#145032=CARTESIAN_POINT('Ctrl Pts',(-74.4387409032582,2.6177953543237,0.));
#145033=CARTESIAN_POINT('Ctrl Pts',(-74.4387409032582,2.6177953543237,12.));
#145034=CARTESIAN_POINT('Ctrl Pts',(-74.4237613008609,2.61025207898831,
0.));
#145035=CARTESIAN_POINT('Ctrl Pts',(-74.4237613008609,2.61025207898831,
12.));
#145036=CARTESIAN_POINT('Ctrl Pts',(-74.4038003595514,2.60021711327491,
0.));
#145037=CARTESIAN_POINT('Ctrl Pts',(-74.4038003595514,2.60021711327491,
12.));
#145038=CARTESIAN_POINT('Ctrl Pts',(-74.3788689604,2.58771130268618,0.));
#145039=CARTESIAN_POINT('Ctrl Pts',(-74.3788689604,2.58771130268618,12.));
#145040=CARTESIAN_POINT('Ctrl Pts',(-74.3539573568054,2.57524339541657,
0.));
#145041=CARTESIAN_POINT('Ctrl Pts',(-74.3539573568054,2.57524339541657,
12.));
#145042=CARTESIAN_POINT('Ctrl Pts',(-74.3290655814922,2.56281339800082,
0.));
#145043=CARTESIAN_POINT('Ctrl Pts',(-74.3290655814922,2.56281339800082,
12.));
#145044=CARTESIAN_POINT('Ctrl Pts',(-74.3041936853329,2.55042131526684,
0.));
#145045=CARTESIAN_POINT('Ctrl Pts',(-74.3041936853329,2.55042131526684,
12.));
#145046=CARTESIAN_POINT('Ctrl Pts',(-74.2793417427044,2.53806714838103,
0.));
#145047=CARTESIAN_POINT('Ctrl Pts',(-74.2793417427044,2.53806714838103,
12.));
#145048=CARTESIAN_POINT('Ctrl Pts',(-74.2545098494549,2.52575089478112,
0.));
#145049=CARTESIAN_POINT('Ctrl Pts',(-74.2545098494549,2.52575089478112,
12.));
#145050=CARTESIAN_POINT('Ctrl Pts',(-74.2296981152027,2.51347254956026,
0.));
#145051=CARTESIAN_POINT('Ctrl Pts',(-74.2296981152027,2.51347254956026,
12.));
#145052=CARTESIAN_POINT('Ctrl Pts',(-74.2049066571942,2.50123210644074,
0.));
#145053=CARTESIAN_POINT('Ctrl Pts',(-74.2049066571942,2.50123210644074,
12.));
#145054=CARTESIAN_POINT('Ctrl Pts',(-74.180135593693,2.48902955888401,0.));
#145055=CARTESIAN_POINT('Ctrl Pts',(-74.180135593693,2.48902955888401,12.));
#145056=CARTESIAN_POINT('Ctrl Pts',(-74.1553850371577,2.47686490120423,
0.));
#145057=CARTESIAN_POINT('Ctrl Pts',(-74.1553850371577,2.47686490120423,
12.));
#145058=CARTESIAN_POINT('Ctrl Pts',(-74.1306550887196,2.46473812948048,
0.));
#145059=CARTESIAN_POINT('Ctrl Pts',(-74.1306550887196,2.46473812948048,
12.));
#145060=CARTESIAN_POINT('Ctrl Pts',(-74.1059458420175,2.45264924094852,
0.));
#145061=CARTESIAN_POINT('Ctrl Pts',(-74.1059458420175,2.45264924094852,
12.));
#145062=CARTESIAN_POINT('Ctrl Pts',(-74.0812573859474,2.44059823356721,
0.));
#145063=CARTESIAN_POINT('Ctrl Pts',(-74.0812573859474,2.44059823356721,
12.));
#145064=CARTESIAN_POINT('Ctrl Pts',(-74.0565898079227,2.42858510549786,
0.));
#145065=CARTESIAN_POINT('Ctrl Pts',(-74.0565898079227,2.42858510549786,
12.));
#145066=CARTESIAN_POINT('Ctrl Pts',(-74.0319431966956,2.41660985465228,
0.));
#145067=CARTESIAN_POINT('Ctrl Pts',(-74.0319431966956,2.41660985465228,
12.));
#145068=CARTESIAN_POINT('Ctrl Pts',(-74.0073176459287,2.40467247811496,
0.));
#145069=CARTESIAN_POINT('Ctrl Pts',(-74.0073176459287,2.40467247811496,
12.));
#145070=CARTESIAN_POINT('Ctrl Pts',(-73.9827132538149,2.39277297220716,
0.));
#145071=CARTESIAN_POINT('Ctrl Pts',(-73.9827132538149,2.39277297220716,
12.));
#145072=CARTESIAN_POINT('Ctrl Pts',(-73.9581301214609,2.38091133274932,
0.));
#145073=CARTESIAN_POINT('Ctrl Pts',(-73.9581301214609,2.38091133274932,
12.));
#145074=CARTESIAN_POINT('Ctrl Pts',(-73.9335683516388,2.36908755525994,
0.));
#145075=CARTESIAN_POINT('Ctrl Pts',(-73.9335683516388,2.36908755525994,
12.));
#145076=CARTESIAN_POINT('Ctrl Pts',(-73.9090280474723,2.35730163516323,
0.));
#145077=CARTESIAN_POINT('Ctrl Pts',(-73.9090280474723,2.35730163516323,
12.));
#145078=CARTESIAN_POINT('Ctrl Pts',(-73.8845093109302,2.34555356802139,
0.));
#145079=CARTESIAN_POINT('Ctrl Pts',(-73.8845093109302,2.34555356802139,
12.));
#145080=CARTESIAN_POINT('Ctrl Pts',(-73.8600122421502,2.3338433496398,0.));
#145081=CARTESIAN_POINT('Ctrl Pts',(-73.8600122421502,2.3338433496398,12.));
#145082=CARTESIAN_POINT('Ctrl Pts',(-73.8355369402733,2.32217097594215,
0.));
#145083=CARTESIAN_POINT('Ctrl Pts',(-73.8355369402733,2.32217097594215,
12.));
#145084=CARTESIAN_POINT('Ctrl Pts',(-73.8110835039341,2.31053644289425,
0.));
#145085=CARTESIAN_POINT('Ctrl Pts',(-73.8110835039341,2.31053644289425,
12.));
#145086=CARTESIAN_POINT('Ctrl Pts',(-73.7866520318849,2.29893974640434,
0.));
#145087=CARTESIAN_POINT('Ctrl Pts',(-73.7866520318849,2.29893974640434,
12.));
#145088=CARTESIAN_POINT('Ctrl Pts',(-73.7622426235648,2.28738088222858,
0.));
#145089=CARTESIAN_POINT('Ctrl Pts',(-73.7622426235648,2.28738088222858,
12.));
#145090=CARTESIAN_POINT('Ctrl Pts',(-73.7378553796792,2.27585984587192,
0.));
#145091=CARTESIAN_POINT('Ctrl Pts',(-73.7378553796792,2.27585984587192,
12.));
#145092=CARTESIAN_POINT('Ctrl Pts',(-73.7134904019378,2.26437663263663,
0.));
#145093=CARTESIAN_POINT('Ctrl Pts',(-73.7134904019378,2.26437663263663,
12.));
#145094=CARTESIAN_POINT('Ctrl Pts',(-73.6891477928124,2.25293123766424,
0.));
#145095=CARTESIAN_POINT('Ctrl Pts',(-73.6891477928124,2.25293123766424,
12.));
#145096=CARTESIAN_POINT('Ctrl Pts',(-73.6648276552766,2.24152365597698,
0.));
#145097=CARTESIAN_POINT('Ctrl Pts',(-73.6648276552766,2.24152365597698,
12.));
#145098=CARTESIAN_POINT('Ctrl Pts',(-73.6405300925714,2.23015388251288,
0.));
#145099=CARTESIAN_POINT('Ctrl Pts',(-73.6405300925714,2.23015388251288,
12.));
#145100=CARTESIAN_POINT('Ctrl Pts',(-73.6162552079044,2.2188219121652,0.));
#145101=CARTESIAN_POINT('Ctrl Pts',(-73.6162552079044,2.2188219121652,12.));
#145102=CARTESIAN_POINT('Ctrl Pts',(-73.5920031044604,2.20752773978352,
0.));
#145103=CARTESIAN_POINT('Ctrl Pts',(-73.5920031044604,2.20752773978352,
12.));
#145104=CARTESIAN_POINT('Ctrl Pts',(-73.5677738855461,2.19627136015682,
0.));
#145105=CARTESIAN_POINT('Ctrl Pts',(-73.5677738855461,2.19627136015682,
12.));
#145106=CARTESIAN_POINT('Ctrl Pts',(-73.5435676546934,2.18505276799756,
0.));
#145107=CARTESIAN_POINT('Ctrl Pts',(-73.5435676546934,2.18505276799756,
12.));
#145108=CARTESIAN_POINT('Ctrl Pts',(-73.5193845157705,2.17387195792305,
0.));
#145109=CARTESIAN_POINT('Ctrl Pts',(-73.5193845157705,2.17387195792305,
12.));
#145110=CARTESIAN_POINT('Ctrl Pts',(-73.4952245731044,2.16272892442915,
0.));
#145111=CARTESIAN_POINT('Ctrl Pts',(-73.4952245731044,2.16272892442915,
12.));
#145112=CARTESIAN_POINT('Ctrl Pts',(-73.4710879315367,2.15162366187898,
0.));
#145113=CARTESIAN_POINT('Ctrl Pts',(-73.4710879315367,2.15162366187898,
12.));
#145114=CARTESIAN_POINT('Ctrl Pts',(-73.4469746963622,2.14055616452048,
0.));
#145115=CARTESIAN_POINT('Ctrl Pts',(-73.4469746963622,2.14055616452048,
12.));
#145116=CARTESIAN_POINT('Ctrl Pts',(-73.4228849732914,2.1295264264936,0.));
#145117=CARTESIAN_POINT('Ctrl Pts',(-73.4228849732914,2.1295264264936,12.));
#145118=CARTESIAN_POINT('Ctrl Pts',(-73.3988188684022,2.11853444183763,
0.));
#145119=CARTESIAN_POINT('Ctrl Pts',(-73.3988188684022,2.11853444183763,
12.));
#145120=CARTESIAN_POINT('Ctrl Pts',(-73.3747764880903,2.107580204494,0.));
#145121=CARTESIAN_POINT('Ctrl Pts',(-73.3747764880903,2.107580204494,12.));
#145122=CARTESIAN_POINT('Ctrl Pts',(-73.3507579390254,2.09666370830733,
0.));
#145123=CARTESIAN_POINT('Ctrl Pts',(-73.3507579390254,2.09666370830733,
12.));
#145124=CARTESIAN_POINT('Ctrl Pts',(-73.3267633281822,2.08578494702761,
0.));
#145125=CARTESIAN_POINT('Ctrl Pts',(-73.3267633281822,2.08578494702761,
12.));
#145126=CARTESIAN_POINT('Ctrl Pts',(-73.3027927628636,2.07494391430953,
0.));
#145127=CARTESIAN_POINT('Ctrl Pts',(-73.3027927628636,2.07494391430953,
12.));
#145128=CARTESIAN_POINT('Ctrl Pts',(-73.2788463507248,2.06414060370837,
0.));
#145129=CARTESIAN_POINT('Ctrl Pts',(-73.2788463507248,2.06414060370837,
12.));
#145130=CARTESIAN_POINT('Ctrl Pts',(-73.2549241997946,2.05337500867395,
0.));
#145131=CARTESIAN_POINT('Ctrl Pts',(-73.2549241997946,2.05337500867395,
12.));
#145132=CARTESIAN_POINT('Ctrl Pts',(-73.2310264184965,2.04264712253915,
0.));
#145133=CARTESIAN_POINT('Ctrl Pts',(-73.2310264184965,2.04264712253915,
12.));
#145134=CARTESIAN_POINT('Ctrl Pts',(-73.2071531156492,2.0319569385244,0.));
#145135=CARTESIAN_POINT('Ctrl Pts',(-73.2071531156492,2.0319569385244,12.));
#145136=CARTESIAN_POINT('Ctrl Pts',(-73.1833044004612,2.02130444974351,
0.));
#145137=CARTESIAN_POINT('Ctrl Pts',(-73.1833044004612,2.02130444974351,
12.));
#145138=CARTESIAN_POINT('Ctrl Pts',(-73.159480382525,2.01068964920464,0.));
#145139=CARTESIAN_POINT('Ctrl Pts',(-73.159480382525,2.01068964920464,12.));
#145140=CARTESIAN_POINT('Ctrl Pts',(-73.1356811718094,2.00011252980987,
0.));
#145141=CARTESIAN_POINT('Ctrl Pts',(-73.1356811718094,2.00011252980987,
12.));
#145142=CARTESIAN_POINT('Ctrl Pts',(-73.1119068786482,1.9895730843493,0.));
#145143=CARTESIAN_POINT('Ctrl Pts',(-73.1119068786482,1.9895730843493,12.));
#145144=CARTESIAN_POINT('Ctrl Pts',(-73.0881576137414,1.97907130550172,
0.));
#145145=CARTESIAN_POINT('Ctrl Pts',(-73.0881576137414,1.97907130550172,
12.));
#145146=CARTESIAN_POINT('Ctrl Pts',(-73.0644334881679,1.96860718583944,
0.));
#145147=CARTESIAN_POINT('Ctrl Pts',(-73.0644334881679,1.96860718583944,
12.));
#145148=CARTESIAN_POINT('Ctrl Pts',(-73.0407346133912,1.95818071782773,
0.));
#145149=CARTESIAN_POINT('Ctrl Pts',(-73.0407346133912,1.95818071782773,
12.));
#145150=CARTESIAN_POINT('Ctrl Pts',(-73.0170611012659,1.947791893823,0.));
#145151=CARTESIAN_POINT('Ctrl Pts',(-73.0170611012659,1.947791893823,12.));
#145152=CARTESIAN_POINT('Ctrl Pts',(-72.9934130640414,1.93744070606557,
0.));
#145153=CARTESIAN_POINT('Ctrl Pts',(-72.9934130640414,1.93744070606557,
12.));
#145154=CARTESIAN_POINT('Ctrl Pts',(-72.9697906143638,1.92712714667648,
0.));
#145155=CARTESIAN_POINT('Ctrl Pts',(-72.9697906143638,1.92712714667648,
12.));
#145156=CARTESIAN_POINT('Ctrl Pts',(-72.9461938652816,1.91685120766427,
0.));
#145157=CARTESIAN_POINT('Ctrl Pts',(-72.9461938652816,1.91685120766427,
12.));
#145158=CARTESIAN_POINT('Ctrl Pts',(-72.9226229302483,1.90661288092582,
0.));
#145159=CARTESIAN_POINT('Ctrl Pts',(-72.9226229302483,1.90661288092582,
12.));
#145160=CARTESIAN_POINT('Ctrl Pts',(-72.8990779231226,1.89641215824584,
0.));
#145161=CARTESIAN_POINT('Ctrl Pts',(-72.8990779231226,1.89641215824584,
12.));
#145162=CARTESIAN_POINT('Ctrl Pts',(-72.8755589581674,1.88624903129195,
0.));
#145163=CARTESIAN_POINT('Ctrl Pts',(-72.8755589581674,1.88624903129195,
12.));
#145164=CARTESIAN_POINT('Ctrl Pts',(-72.8520661500465,1.87612349160952,
0.));
#145165=CARTESIAN_POINT('Ctrl Pts',(-72.8520661500465,1.87612349160952,
12.));
#145166=CARTESIAN_POINT('Ctrl Pts',(-72.8285996138346,1.86603553062776,
0.));
#145167=CARTESIAN_POINT('Ctrl Pts',(-72.8285996138346,1.86603553062776,
12.));
#145168=CARTESIAN_POINT('Ctrl Pts',(-72.8051594650214,1.85598513966115,
0.));
#145169=CARTESIAN_POINT('Ctrl Pts',(-72.8051594650214,1.85598513966115,
12.));
#145170=CARTESIAN_POINT('Ctrl Pts',(-72.7817458195155,1.84597230990858,
0.));
#145171=CARTESIAN_POINT('Ctrl Pts',(-72.7817458195155,1.84597230990858,
12.));
#145172=CARTESIAN_POINT('Ctrl Pts',(-72.7583587936454,1.83599703244926,
0.));
#145173=CARTESIAN_POINT('Ctrl Pts',(-72.7583587936454,1.83599703244926,
12.));
#145174=CARTESIAN_POINT('Ctrl Pts',(-72.73499850416,1.82605929823565,0.));
#145175=CARTESIAN_POINT('Ctrl Pts',(-72.73499850416,1.82605929823565,12.));
#145176=CARTESIAN_POINT('Ctrl Pts',(-72.7116650682347,1.81615909809871,
0.));
#145177=CARTESIAN_POINT('Ctrl Pts',(-72.7116650682347,1.81615909809871,
12.));
#145178=CARTESIAN_POINT('Ctrl Pts',(-72.6883586034768,1.80629642275051,
0.));
#145179=CARTESIAN_POINT('Ctrl Pts',(-72.6883586034768,1.80629642275051,
12.));
#145180=CARTESIAN_POINT('Ctrl Pts',(-72.6650792279271,1.79647126278359,
0.));
#145181=CARTESIAN_POINT('Ctrl Pts',(-72.6650792279271,1.79647126278359,
12.));
#145182=CARTESIAN_POINT('Ctrl Pts',(-72.6418270600623,1.78668360866813,
0.));
#145183=CARTESIAN_POINT('Ctrl Pts',(-72.6418270600623,1.78668360866813,
12.));
#145184=CARTESIAN_POINT('Ctrl Pts',(-72.618602218792,1.7769334507443,0.));
#145185=CARTESIAN_POINT('Ctrl Pts',(-72.618602218792,1.7769334507443,12.));
#145186=CARTESIAN_POINT('Ctrl Pts',(-72.5954048234655,1.76722077922579,
0.));
#145187=CARTESIAN_POINT('Ctrl Pts',(-72.5954048234655,1.76722077922579,
12.));
#145188=CARTESIAN_POINT('Ctrl Pts',(-72.5722349938789,1.75754558420349,
0.));
#145189=CARTESIAN_POINT('Ctrl Pts',(-72.5722349938789,1.75754558420349,
12.));
#145190=CARTESIAN_POINT('Ctrl Pts',(-72.5490928502773,1.74790785564476,
0.));
#145191=CARTESIAN_POINT('Ctrl Pts',(-72.5490928502773,1.74790785564476,
12.));
#145192=CARTESIAN_POINT('Ctrl Pts',(-72.5259785133586,1.73830758339123,
0.));
#145193=CARTESIAN_POINT('Ctrl Pts',(-72.5259785133586,1.73830758339123,
12.));
#145194=CARTESIAN_POINT('Ctrl Pts',(-72.5028921042704,1.72874475715098,
0.));
#145195=CARTESIAN_POINT('Ctrl Pts',(-72.5028921042704,1.72874475715098,
12.));
#145196=CARTESIAN_POINT('Ctrl Pts',(-72.4798337446162,1.71921936650032,
0.));
#145197=CARTESIAN_POINT('Ctrl Pts',(-72.4798337446162,1.71921936650032,
12.));
#145198=CARTESIAN_POINT('Ctrl Pts',(-72.4568035564618,1.70973140088837,
0.));
#145199=CARTESIAN_POINT('Ctrl Pts',(-72.4568035564618,1.70973140088837,
12.));
#145200=CARTESIAN_POINT('Ctrl Pts',(-72.4338016623388,1.70028084963646,
0.));
#145201=CARTESIAN_POINT('Ctrl Pts',(-72.4338016623388,1.70028084963646,
12.));
#145202=CARTESIAN_POINT('Ctrl Pts',(-72.4108281852473,1.6908677019364,0.));
#145203=CARTESIAN_POINT('Ctrl Pts',(-72.4108281852473,1.6908677019364,12.));
#145204=CARTESIAN_POINT('Ctrl Pts',(-72.3878832486549,1.68149194684288,
0.));
#145205=CARTESIAN_POINT('Ctrl Pts',(-72.3878832486549,1.68149194684288,
12.));
#145206=CARTESIAN_POINT('Ctrl Pts',(-72.3649669765013,1.67215357327372,
0.));
#145207=CARTESIAN_POINT('Ctrl Pts',(-72.3649669765013,1.67215357327372,
12.));
#145208=CARTESIAN_POINT('Ctrl Pts',(-72.3420794932052,1.66285257001502,
0.));
#145209=CARTESIAN_POINT('Ctrl Pts',(-72.3420794932052,1.66285257001502,
12.));
#145210=CARTESIAN_POINT('Ctrl Pts',(-72.3192209236691,1.65358892572065,
0.));
#145211=CARTESIAN_POINT('Ctrl Pts',(-72.3192209236691,1.65358892572065,
12.));
#145212=CARTESIAN_POINT('Ctrl Pts',(-72.2963913932811,1.64436262891078,
0.));
#145213=CARTESIAN_POINT('Ctrl Pts',(-72.2963913932811,1.64436262891078,
12.));
#145214=CARTESIAN_POINT('Ctrl Pts',(-72.2735910279149,1.63517366796458,
0.));
#145215=CARTESIAN_POINT('Ctrl Pts',(-72.2735910279149,1.63517366796458,
12.));
#145216=CARTESIAN_POINT('Ctrl Pts',(-72.2508199539325,1.62602203111924,
0.));
#145217=CARTESIAN_POINT('Ctrl Pts',(-72.2508199539325,1.62602203111924,
12.));
#145218=CARTESIAN_POINT('Ctrl Pts',(-72.2280782981941,1.61690770647535,
0.));
#145219=CARTESIAN_POINT('Ctrl Pts',(-72.2280782981941,1.61690770647535,
12.));
#145220=CARTESIAN_POINT('Ctrl Pts',(-72.2053661880611,1.60783068199661,
0.));
#145221=CARTESIAN_POINT('Ctrl Pts',(-72.2053661880611,1.60783068199661,
12.));
#145222=CARTESIAN_POINT('Ctrl Pts',(-72.1826837514,1.59879094550849,0.));
#145223=CARTESIAN_POINT('Ctrl Pts',(-72.1826837514,1.59879094550849,12.));
#145224=CARTESIAN_POINT('Ctrl Pts',(-72.1600311165813,1.58978848469128,
0.));
#145225=CARTESIAN_POINT('Ctrl Pts',(-72.1600311165813,1.58978848469128,
12.));
#145226=CARTESIAN_POINT('Ctrl Pts',(-72.1374084124829,1.58082328707808,
0.));
#145227=CARTESIAN_POINT('Ctrl Pts',(-72.1374084124829,1.58082328707808,
12.));
#145228=CARTESIAN_POINT('Ctrl Pts',(-72.1148157684987,1.57189534006043,
0.));
#145229=CARTESIAN_POINT('Ctrl Pts',(-72.1148157684987,1.57189534006043,
12.));
#145230=CARTESIAN_POINT('Ctrl Pts',(-72.092253314543,1.56300463088811,0.));
#145231=CARTESIAN_POINT('Ctrl Pts',(-72.092253314543,1.56300463088811,12.));
#145232=CARTESIAN_POINT('Ctrl Pts',(-72.0697211810548,1.55415114666774,
0.));
#145233=CARTESIAN_POINT('Ctrl Pts',(-72.0697211810548,1.55415114666774,
12.));
#145234=CARTESIAN_POINT('Ctrl Pts',(-72.0472194989968,1.54533487435626,
0.));
#145235=CARTESIAN_POINT('Ctrl Pts',(-72.0472194989968,1.54533487435626,
12.));
#145236=CARTESIAN_POINT('Ctrl Pts',(-72.0247483998582,1.53655580075813,
0.));
#145237=CARTESIAN_POINT('Ctrl Pts',(-72.0247483998582,1.53655580075813,
12.));
#145238=CARTESIAN_POINT('Ctrl Pts',(-72.0023080156647,1.52781391253103,
0.));
#145239=CARTESIAN_POINT('Ctrl Pts',(-72.0023080156647,1.52781391253103,
12.));
#145240=CARTESIAN_POINT('Ctrl Pts',(-71.9798984789828,1.51910919618566,
0.));
#145241=CARTESIAN_POINT('Ctrl Pts',(-71.9798984789828,1.51910919618566,
12.));
#145242=CARTESIAN_POINT('Ctrl Pts',(-71.9575199229241,1.51044163808454,
0.));
#145243=CARTESIAN_POINT('Ctrl Pts',(-71.9575199229241,1.51044163808454,
12.));
#145244=CARTESIAN_POINT('Ctrl Pts',(-71.935172481145,1.50181122443535,0.));
#145245=CARTESIAN_POINT('Ctrl Pts',(-71.935172481145,1.50181122443535,12.));
#145246=CARTESIAN_POINT('Ctrl Pts',(-71.9128562878491,1.493217941288,0.));
#145247=CARTESIAN_POINT('Ctrl Pts',(-71.9128562878491,1.493217941288,12.));
#145248=CARTESIAN_POINT('Ctrl Pts',(-71.8905714777972,1.48466177454021,
0.));
#145249=CARTESIAN_POINT('Ctrl Pts',(-71.8905714777972,1.48466177454021,
12.));
#145250=CARTESIAN_POINT('Ctrl Pts',(-71.8683181863123,1.4761427099373,0.));
#145251=CARTESIAN_POINT('Ctrl Pts',(-71.8683181863123,1.4761427099373,12.));
#145252=CARTESIAN_POINT('Ctrl Pts',(-71.8460965492836,1.46766073307089,
0.));
#145253=CARTESIAN_POINT('Ctrl Pts',(-71.8460965492836,1.46766073307089,
12.));
#145254=CARTESIAN_POINT('Ctrl Pts',(-71.8239067031664,1.45921582937229,
0.));
#145255=CARTESIAN_POINT('Ctrl Pts',(-71.8239067031664,1.45921582937229,
12.));
#145256=CARTESIAN_POINT('Ctrl Pts',(-71.8017487849865,1.45080798410957,
0.));
#145257=CARTESIAN_POINT('Ctrl Pts',(-71.8017487849865,1.45080798410957,
12.));
#145258=CARTESIAN_POINT('Ctrl Pts',(-71.7796229323496,1.44243718239304,
0.));
#145259=CARTESIAN_POINT('Ctrl Pts',(-71.7796229323496,1.44243718239304,
12.));
#145260=CARTESIAN_POINT('Ctrl Pts',(-71.7575292834456,1.43410340917489,
0.));
#145261=CARTESIAN_POINT('Ctrl Pts',(-71.7575292834456,1.43410340917489,
12.));
#145262=CARTESIAN_POINT('Ctrl Pts',(-71.7354679770537,1.42580664924774,
0.));
#145263=CARTESIAN_POINT('Ctrl Pts',(-71.7354679770537,1.42580664924774,
12.));
#145264=CARTESIAN_POINT('Ctrl Pts',(-71.7134391525417,1.41754688723791,
0.));
#145265=CARTESIAN_POINT('Ctrl Pts',(-71.7134391525417,1.41754688723791,
12.));
#145266=CARTESIAN_POINT('Ctrl Pts',(-71.6914429498702,1.40932410760274,
0.));
#145267=CARTESIAN_POINT('Ctrl Pts',(-71.6914429498702,1.40932410760274,
12.));
#145268=CARTESIAN_POINT('Ctrl Pts',(-71.6694795096034,1.40113829463599,
0.));
#145269=CARTESIAN_POINT('Ctrl Pts',(-71.6694795096034,1.40113829463599,
12.));
#145270=CARTESIAN_POINT('Ctrl Pts',(-71.6475489729149,1.39298943246731,
0.));
#145271=CARTESIAN_POINT('Ctrl Pts',(-71.6475489729149,1.39298943246731,
12.));
#145272=CARTESIAN_POINT('Ctrl Pts',(-71.6256514815918,1.38487750506076,
0.));
#145273=CARTESIAN_POINT('Ctrl Pts',(-71.6256514815918,1.38487750506076,
12.));
#145274=CARTESIAN_POINT('Ctrl Pts',(-71.6037871780347,1.37680249620763,
0.));
#145275=CARTESIAN_POINT('Ctrl Pts',(-71.6037871780347,1.37680249620763,
12.));
#145276=CARTESIAN_POINT('Ctrl Pts',(-71.5819562052613,1.36876438952448,
0.));
#145277=CARTESIAN_POINT('Ctrl Pts',(-71.5819562052613,1.36876438952448,
12.));
#145278=CARTESIAN_POINT('Ctrl Pts',(-71.5601587069175,1.36076316845806,
0.));
#145279=CARTESIAN_POINT('Ctrl Pts',(-71.5601587069175,1.36076316845806,
12.));
#145280=CARTESIAN_POINT('Ctrl Pts',(-71.538394827283,1.35279881628453,0.));
#145281=CARTESIAN_POINT('Ctrl Pts',(-71.538394827283,1.35279881628453,12.));
#145282=CARTESIAN_POINT('Ctrl Pts',(-71.5166647112766,1.34487131610785,
0.));
#145283=CARTESIAN_POINT('Ctrl Pts',(-71.5166647112766,1.34487131610785,
12.));
#145284=CARTESIAN_POINT('Ctrl Pts',(-71.4949685044559,1.33698065085227,
0.));
#145285=CARTESIAN_POINT('Ctrl Pts',(-71.4949685044559,1.33698065085227,
12.));
#145286=CARTESIAN_POINT('Ctrl Pts',(-71.4733063530227,1.32912680326131,
0.));
#145287=CARTESIAN_POINT('Ctrl Pts',(-71.4733063530227,1.32912680326131,
12.));
#145288=CARTESIAN_POINT('Ctrl Pts',(-71.4516784038346,1.32130975590231,
0.));
#145289=CARTESIAN_POINT('Ctrl Pts',(-71.4516784038346,1.32130975590231,
12.));
#145290=CARTESIAN_POINT('Ctrl Pts',(-71.4300848044095,1.31352949116538,
0.));
#145291=CARTESIAN_POINT('Ctrl Pts',(-71.4300848044095,1.31352949116538,
12.));
#145292=CARTESIAN_POINT('Ctrl Pts',(-71.4085257029308,1.30578599126139,
0.));
#145293=CARTESIAN_POINT('Ctrl Pts',(-71.4085257029308,1.30578599126139,
12.));
#145294=CARTESIAN_POINT('Ctrl Pts',(-71.3870012482474,1.29807923821413,
0.));
#145295=CARTESIAN_POINT('Ctrl Pts',(-71.3870012482474,1.29807923821413,
12.));
#145296=CARTESIAN_POINT('Ctrl Pts',(-71.3655115898801,1.2904092138606,0.));
#145297=CARTESIAN_POINT('Ctrl Pts',(-71.3655115898801,1.2904092138606,12.));
#145298=CARTESIAN_POINT('Ctrl Pts',(-71.344056878033,1.28277589985474,0.));
#145299=CARTESIAN_POINT('Ctrl Pts',(-71.344056878033,1.28277589985474,12.));
#145300=CARTESIAN_POINT('Ctrl Pts',(-71.3226372635993,1.2751792776661,0.));
#145301=CARTESIAN_POINT('Ctrl Pts',(-71.3226372635993,1.2751792776661,12.));
#145302=CARTESIAN_POINT('Ctrl Pts',(-71.301252898167,1.26761932857723,0.));
#145303=CARTESIAN_POINT('Ctrl Pts',(-71.301252898167,1.26761932857723,12.));
#145304=CARTESIAN_POINT('Ctrl Pts',(-71.2799039340191,1.26009603367564,
0.));
#145305=CARTESIAN_POINT('Ctrl Pts',(-71.2799039340191,1.26009603367564,
12.));
#145306=CARTESIAN_POINT('Ctrl Pts',(-71.2585905241422,1.2526093738556,0.));
#145307=CARTESIAN_POINT('Ctrl Pts',(-71.2585905241422,1.2526093738556,12.));
#145308=CARTESIAN_POINT('Ctrl Pts',(-71.2373128222359,1.24515932982107,
0.));
#145309=CARTESIAN_POINT('Ctrl Pts',(-71.2373128222359,1.24515932982107,
12.));
#145310=CARTESIAN_POINT('Ctrl Pts',(-71.2160709827189,1.23774588208427,
0.));
#145311=CARTESIAN_POINT('Ctrl Pts',(-71.2160709827189,1.23774588208427,
12.));
#145312=CARTESIAN_POINT('Ctrl Pts',(-71.1948651607319,1.23036901096246,
0.));
#145313=CARTESIAN_POINT('Ctrl Pts',(-71.1948651607319,1.23036901096246,
12.));
#145314=CARTESIAN_POINT('Ctrl Pts',(-71.1736955121361,1.22302869657028,
0.));
#145315=CARTESIAN_POINT('Ctrl Pts',(-71.1736955121361,1.22302869657028,
12.));
#145316=CARTESIAN_POINT('Ctrl Pts',(-71.1525621935266,1.21572491882273,
0.));
#145317=CARTESIAN_POINT('Ctrl Pts',(-71.1525621935266,1.21572491882273,
12.));
#145318=CARTESIAN_POINT('Ctrl Pts',(-71.1314653622442,1.20845765743654,
0.));
#145319=CARTESIAN_POINT('Ctrl Pts',(-71.1314653622442,1.20845765743654,
12.));
#145320=CARTESIAN_POINT('Ctrl Pts',(-71.1104051763839,1.20122689192836,
0.));
#145321=CARTESIAN_POINT('Ctrl Pts',(-71.1104051763839,1.20122689192836,
12.));
#145322=CARTESIAN_POINT('Ctrl Pts',(-71.089381794801,1.19403260160997,0.));
#145323=CARTESIAN_POINT('Ctrl Pts',(-71.089381794801,1.19403260160997,12.));
#145324=CARTESIAN_POINT('Ctrl Pts',(-71.0683953771147,1.18687476558126,
0.));
#145325=CARTESIAN_POINT('Ctrl Pts',(-71.0683953771147,1.18687476558126,
12.));
#145326=CARTESIAN_POINT('Ctrl Pts',(-71.0474460837157,1.17975336273499,
0.));
#145327=CARTESIAN_POINT('Ctrl Pts',(-71.0474460837157,1.17975336273499,
12.));
#145328=CARTESIAN_POINT('Ctrl Pts',(-71.0265340757697,1.17266837175775,
0.));
#145329=CARTESIAN_POINT('Ctrl Pts',(-71.0265340757697,1.17266837175775,
12.));
#145330=CARTESIAN_POINT('Ctrl Pts',(-71.0056595152204,1.16561977112882,
0.));
#145331=CARTESIAN_POINT('Ctrl Pts',(-71.0056595152204,1.16561977112882,
12.));
#145332=CARTESIAN_POINT('Ctrl Pts',(-70.9848225647876,1.15860753911489,
0.));
#145333=CARTESIAN_POINT('Ctrl Pts',(-70.9848225647876,1.15860753911489,
12.));
#145334=CARTESIAN_POINT('Ctrl Pts',(-70.9640233879671,1.1516316537653,0.));
#145335=CARTESIAN_POINT('Ctrl Pts',(-70.9640233879671,1.1516316537653,12.));
#145336=CARTESIAN_POINT('Ctrl Pts',(-70.9432621490579,1.14469209291494,
0.));
#145337=CARTESIAN_POINT('Ctrl Pts',(-70.9432621490579,1.14469209291494,
12.));
#145338=CARTESIAN_POINT('Ctrl Pts',(-70.9225390131835,1.13778883418216,
0.));
#145339=CARTESIAN_POINT('Ctrl Pts',(-70.9225390131835,1.13778883418216,
12.));
#145340=CARTESIAN_POINT('Ctrl Pts',(-70.9018541463083,1.13092185496563,
0.));
#145341=CARTESIAN_POINT('Ctrl Pts',(-70.9018541463083,1.13092185496563,
12.));
#145342=CARTESIAN_POINT('Ctrl Pts',(-70.8812077152564,1.12409113243511,
0.));
#145343=CARTESIAN_POINT('Ctrl Pts',(-70.8812077152564,1.12409113243511,
12.));
#145344=CARTESIAN_POINT('Ctrl Pts',(-70.860599887712,1.1172966435299,0.));
#145345=CARTESIAN_POINT('Ctrl Pts',(-70.860599887712,1.1172966435299,12.));
#145346=CARTESIAN_POINT('Ctrl Pts',(-70.8400308322013,1.11053836496637,
0.));
#145347=CARTESIAN_POINT('Ctrl Pts',(-70.8400308322013,1.11053836496637,
12.));
#145348=CARTESIAN_POINT('Ctrl Pts',(-70.8195007180739,1.10381627323945,
0.));
#145349=CARTESIAN_POINT('Ctrl Pts',(-70.8195007180739,1.10381627323945,
12.));
#145350=CARTESIAN_POINT('Ctrl Pts',(-70.7990097154855,1.09713034462269,
0.));
#145351=CARTESIAN_POINT('Ctrl Pts',(-70.7990097154855,1.09713034462269,
12.));
#145352=CARTESIAN_POINT('Ctrl Pts',(-70.7785579953611,1.09048055516434,
0.));
#145353=CARTESIAN_POINT('Ctrl Pts',(-70.7785579953611,1.09048055516434,
12.));
#145354=CARTESIAN_POINT('Ctrl Pts',(-70.7581457294475,1.08386688068348,
0.));
#145355=CARTESIAN_POINT('Ctrl Pts',(-70.7581457294475,1.08386688068348,
12.));
#145356=CARTESIAN_POINT('Ctrl Pts',(-70.737773090397,1.07728929676412,0.));
#145357=CARTESIAN_POINT('Ctrl Pts',(-70.737773090397,1.07728929676412,12.));
#145358=CARTESIAN_POINT('Ctrl Pts',(-70.7174402518378,1.07074777874596,
0.));
#145359=CARTESIAN_POINT('Ctrl Pts',(-70.7174402518378,1.07074777874596,
12.));
#145360=CARTESIAN_POINT('Ctrl Pts',(-70.6971473884443,1.0642423017128,0.));
#145361=CARTESIAN_POINT('Ctrl Pts',(-70.6971473884443,1.0642423017128,12.));
#145362=CARTESIAN_POINT('Ctrl Pts',(-70.6768946760063,1.05777284047727,
0.));
#145363=CARTESIAN_POINT('Ctrl Pts',(-70.6768946760063,1.05777284047727,
12.));
#145364=CARTESIAN_POINT('Ctrl Pts',(-70.6566822912965,1.05133936960068,
0.));
#145365=CARTESIAN_POINT('Ctrl Pts',(-70.6566822912965,1.05133936960068,
12.));
#145366=CARTESIAN_POINT('Ctrl Pts',(-70.6365104119238,1.04494186341155,
0.));
#145367=CARTESIAN_POINT('Ctrl Pts',(-70.6365104119238,1.04494186341155,
12.));
#145368=CARTESIAN_POINT('Ctrl Pts',(-70.6163792162079,1.03858029601905,
0.));
#145369=CARTESIAN_POINT('Ctrl Pts',(-70.6163792162079,1.03858029601905,
12.));
#145370=CARTESIAN_POINT('Ctrl Pts',(-70.5962888829958,1.03225464132872,
0.));
#145371=CARTESIAN_POINT('Ctrl Pts',(-70.5962888829958,1.03225464132872,
12.));
#145372=CARTESIAN_POINT('Ctrl Pts',(-70.5762395916412,1.02596487304049,
0.));
#145373=CARTESIAN_POINT('Ctrl Pts',(-70.5762395916412,1.02596487304049,
12.));
#145374=CARTESIAN_POINT('Ctrl Pts',(-70.5562315224219,1.01971096460599,
0.));
#145375=CARTESIAN_POINT('Ctrl Pts',(-70.5562315224219,1.01971096460599,
12.));
#145376=CARTESIAN_POINT('Ctrl Pts',(-70.5362648569072,1.01349288918539,
0.));
#145377=CARTESIAN_POINT('Ctrl Pts',(-70.5362648569072,1.01349288918539,
12.));
#145378=CARTESIAN_POINT('Ctrl Pts',(-70.5163397782698,1.00731061960967,
0.));
#145379=CARTESIAN_POINT('Ctrl Pts',(-70.5163397782698,1.00731061960967,
12.));
#145380=CARTESIAN_POINT('Ctrl Pts',(-70.4964564717917,1.00116412831437,
0.));
#145381=CARTESIAN_POINT('Ctrl Pts',(-70.4964564717917,1.00116412831437,
12.));
#145382=CARTESIAN_POINT('Ctrl Pts',(-70.4766151245169,0.995053387379677,
0.));
#145383=CARTESIAN_POINT('Ctrl Pts',(-70.4766151245169,0.995053387379677,
12.));
#145384=CARTESIAN_POINT('Ctrl Pts',(-70.4568159243131,0.988978368643586,
0.));
#145385=CARTESIAN_POINT('Ctrl Pts',(-70.4568159243131,0.988978368643586,
12.));
#145386=CARTESIAN_POINT('Ctrl Pts',(-70.4370590590839,0.982939043792156,
0.));
#145387=CARTESIAN_POINT('Ctrl Pts',(-70.4370590590839,0.982939043792156,
12.));
#145388=CARTESIAN_POINT('Ctrl Pts',(-70.41734471596,0.976935384450124,0.));
#145389=CARTESIAN_POINT('Ctrl Pts',(-70.41734471596,0.976935384450124,12.));
#145390=CARTESIAN_POINT('Ctrl Pts',(-70.3976730803664,0.970967362281299,
0.));
#145391=CARTESIAN_POINT('Ctrl Pts',(-70.3976730803664,0.970967362281299,
12.));
#145392=CARTESIAN_POINT('Ctrl Pts',(-70.3780443378003,0.965034948786555,
0.));
#145393=CARTESIAN_POINT('Ctrl Pts',(-70.3780443378003,0.965034948786555,
12.));
#145394=CARTESIAN_POINT('Ctrl Pts',(-70.3584586759561,0.959138115058882,
0.));
#145395=CARTESIAN_POINT('Ctrl Pts',(-70.3584586759561,0.959138115058882,
12.));
#145396=CARTESIAN_POINT('Ctrl Pts',(-70.338916286457,0.953276831581228,
0.));
#145397=CARTESIAN_POINT('Ctrl Pts',(-70.338916286457,0.953276831581228,
12.));
#145398=CARTESIAN_POINT('Ctrl Pts',(-70.3194173673635,0.94745106792956,
0.));
#145399=CARTESIAN_POINT('Ctrl Pts',(-70.3194173673635,0.94745106792956,
12.));
#145400=CARTESIAN_POINT('Ctrl Pts',(-70.2999621233938,0.941660792742949,
0.));
#145401=CARTESIAN_POINT('Ctrl Pts',(-70.2999621233938,0.941660792742949,
12.));
#145402=CARTESIAN_POINT('Ctrl Pts',(-70.2805507606832,0.935905974336487,
0.));
#145403=CARTESIAN_POINT('Ctrl Pts',(-70.2805507606832,0.935905974336487,
12.));
#145404=CARTESIAN_POINT('Ctrl Pts',(-70.2611834821711,0.930186581235571,
0.));
#145405=CARTESIAN_POINT('Ctrl Pts',(-70.2611834821711,0.930186581235571,
12.));
#145406=CARTESIAN_POINT('Ctrl Pts',(-70.241860483586,0.924502582639448,
0.));
#145407=CARTESIAN_POINT('Ctrl Pts',(-70.241860483586,0.924502582639448,
12.));
#145408=CARTESIAN_POINT('Ctrl Pts',(-70.2225819470306,0.91885394915704,
0.));
#145409=CARTESIAN_POINT('Ctrl Pts',(-70.2225819470306,0.91885394915704,
12.));
#145410=CARTESIAN_POINT('Ctrl Pts',(-70.2033480471749,0.913240652090834,
0.));
#145411=CARTESIAN_POINT('Ctrl Pts',(-70.2033480471749,0.913240652090834,
12.));
#145412=CARTESIAN_POINT('Ctrl Pts',(-70.184158963563,0.907662662015646,
0.));
#145413=CARTESIAN_POINT('Ctrl Pts',(-70.184158963563,0.907662662015646,
12.));
#145414=CARTESIAN_POINT('Ctrl Pts',(-70.1650148905109,0.902119947629768,
0.));
#145415=CARTESIAN_POINT('Ctrl Pts',(-70.1650148905109,0.902119947629768,
12.));
#145416=CARTESIAN_POINT('Ctrl Pts',(-70.1459160490366,0.89661247437208,
0.));
#145417=CARTESIAN_POINT('Ctrl Pts',(-70.1459160490366,0.89661247437208,
12.));
#145418=CARTESIAN_POINT('Ctrl Pts',(-70.1268626950031,0.89114020346472,
0.));
#145419=CARTESIAN_POINT('Ctrl Pts',(-70.1268626950031,0.89114020346472,
12.));
#145420=CARTESIAN_POINT('Ctrl Pts',(-70.1078550938801,0.885703094803082,
0.));
#145421=CARTESIAN_POINT('Ctrl Pts',(-70.1078550938801,0.885703094803082,
12.));
#145422=CARTESIAN_POINT('Ctrl Pts',(-70.0888934967772,0.880301109661035,
0.));
#145423=CARTESIAN_POINT('Ctrl Pts',(-70.0888934967772,0.880301109661035,
12.));
#145424=CARTESIAN_POINT('Ctrl Pts',(-70.0699781184013,0.874934213255568,
0.));
#145425=CARTESIAN_POINT('Ctrl Pts',(-70.0699781184013,0.874934213255568,
12.));
#145426=CARTESIAN_POINT('Ctrl Pts',(-70.0511091083285,0.869602377870135,
0.));
#145427=CARTESIAN_POINT('Ctrl Pts',(-70.0511091083285,0.869602377870135,
12.));
#145428=CARTESIAN_POINT('Ctrl Pts',(-70.0322865493339,0.864305583660085,
0.));
#145429=CARTESIAN_POINT('Ctrl Pts',(-70.0322865493339,0.864305583660085,
12.));
#145430=CARTESIAN_POINT('Ctrl Pts',(-70.0172656934192,0.860096170667396,
0.));
#145431=CARTESIAN_POINT('Ctrl Pts',(-70.0172656934192,0.860096170667396,
12.));
#145432=CARTESIAN_POINT('Ctrl Pts',(-70.0060209754332,0.856954870258366,
0.));
#145433=CARTESIAN_POINT('Ctrl Pts',(-70.0060209754332,0.856954870258366,
12.));
#145434=CARTESIAN_POINT('Ctrl Pts',(-69.9985337959499,0.854867673848289,
0.));
#145435=CARTESIAN_POINT('Ctrl Pts',(-69.9985337959499,0.854867673848289,
12.));
#145436=CARTESIAN_POINT('Ctrl Pts',(-69.9947925310006,0.853825826608988,
0.));
#145437=CARTESIAN_POINT('Ctrl Pts',(-69.9947925310006,0.853825826608988,
12.));
#145438=CARTESIAN_POINT('',(-69.9947925310006,0.853825826608988,12.));
#145439=CARTESIAN_POINT('Ctrl Pts',(-69.9947925310006,0.853825826608988,
12.));
#145440=CARTESIAN_POINT('Ctrl Pts',(-69.9985337959499,0.854867673848289,
12.));
#145441=CARTESIAN_POINT('Ctrl Pts',(-70.0060209754332,0.856954870258366,
12.));
#145442=CARTESIAN_POINT('Ctrl Pts',(-70.0172656934192,0.860096170667396,
12.));
#145443=CARTESIAN_POINT('Ctrl Pts',(-70.0322865493339,0.864305583660085,
12.));
#145444=CARTESIAN_POINT('Ctrl Pts',(-70.0511091083285,0.869602377870135,
12.));
#145445=CARTESIAN_POINT('Ctrl Pts',(-70.0699781184013,0.874934213255568,
12.));
#145446=CARTESIAN_POINT('Ctrl Pts',(-70.0888934967772,0.880301109661035,
12.));
#145447=CARTESIAN_POINT('Ctrl Pts',(-70.1078550938801,0.885703094803082,
12.));
#145448=CARTESIAN_POINT('Ctrl Pts',(-70.1268626950031,0.89114020346472,
12.));
#145449=CARTESIAN_POINT('Ctrl Pts',(-70.1459160490366,0.89661247437208,
12.));
#145450=CARTESIAN_POINT('Ctrl Pts',(-70.1650148905109,0.902119947629768,
12.));
#145451=CARTESIAN_POINT('Ctrl Pts',(-70.184158963563,0.907662662015646,
12.));
#145452=CARTESIAN_POINT('Ctrl Pts',(-70.2033480471749,0.913240652090834,
12.));
#145453=CARTESIAN_POINT('Ctrl Pts',(-70.2225819470306,0.91885394915704,
12.));
#145454=CARTESIAN_POINT('Ctrl Pts',(-70.241860483586,0.924502582639448,
12.));
#145455=CARTESIAN_POINT('Ctrl Pts',(-70.2611834821711,0.930186581235571,
12.));
#145456=CARTESIAN_POINT('Ctrl Pts',(-70.2805507606832,0.935905974336487,
12.));
#145457=CARTESIAN_POINT('Ctrl Pts',(-70.2999621233938,0.941660792742949,
12.));
#145458=CARTESIAN_POINT('Ctrl Pts',(-70.3194173673635,0.94745106792956,
12.));
#145459=CARTESIAN_POINT('Ctrl Pts',(-70.338916286457,0.953276831581228,
12.));
#145460=CARTESIAN_POINT('Ctrl Pts',(-70.3584586759561,0.959138115058882,
12.));
#145461=CARTESIAN_POINT('Ctrl Pts',(-70.3780443378003,0.965034948786555,
12.));
#145462=CARTESIAN_POINT('Ctrl Pts',(-70.3976730803664,0.970967362281299,
12.));
#145463=CARTESIAN_POINT('Ctrl Pts',(-70.41734471596,0.976935384450124,12.));
#145464=CARTESIAN_POINT('Ctrl Pts',(-70.4370590590839,0.982939043792156,
12.));
#145465=CARTESIAN_POINT('Ctrl Pts',(-70.4568159243131,0.988978368643586,
12.));
#145466=CARTESIAN_POINT('Ctrl Pts',(-70.4766151245169,0.995053387379677,
12.));
#145467=CARTESIAN_POINT('Ctrl Pts',(-70.4964564717917,1.00116412831437,
12.));
#145468=CARTESIAN_POINT('Ctrl Pts',(-70.5163397782698,1.00731061960967,
12.));
#145469=CARTESIAN_POINT('Ctrl Pts',(-70.5362648569072,1.01349288918539,
12.));
#145470=CARTESIAN_POINT('Ctrl Pts',(-70.5562315224219,1.01971096460599,
12.));
#145471=CARTESIAN_POINT('Ctrl Pts',(-70.5762395916412,1.02596487304049,
12.));
#145472=CARTESIAN_POINT('Ctrl Pts',(-70.5962888829958,1.03225464132872,
12.));
#145473=CARTESIAN_POINT('Ctrl Pts',(-70.6163792162079,1.03858029601905,
12.));
#145474=CARTESIAN_POINT('Ctrl Pts',(-70.6365104119238,1.04494186341155,
12.));
#145475=CARTESIAN_POINT('Ctrl Pts',(-70.6566822912965,1.05133936960068,
12.));
#145476=CARTESIAN_POINT('Ctrl Pts',(-70.6768946760063,1.05777284047727,
12.));
#145477=CARTESIAN_POINT('Ctrl Pts',(-70.6971473884443,1.0642423017128,12.));
#145478=CARTESIAN_POINT('Ctrl Pts',(-70.7174402518378,1.07074777874596,
12.));
#145479=CARTESIAN_POINT('Ctrl Pts',(-70.737773090397,1.07728929676412,12.));
#145480=CARTESIAN_POINT('Ctrl Pts',(-70.7581457294475,1.08386688068348,
12.));
#145481=CARTESIAN_POINT('Ctrl Pts',(-70.7785579953611,1.09048055516434,
12.));
#145482=CARTESIAN_POINT('Ctrl Pts',(-70.7990097154855,1.09713034462269,
12.));
#145483=CARTESIAN_POINT('Ctrl Pts',(-70.8195007180739,1.10381627323945,
12.));
#145484=CARTESIAN_POINT('Ctrl Pts',(-70.8400308322013,1.11053836496637,
12.));
#145485=CARTESIAN_POINT('Ctrl Pts',(-70.860599887712,1.1172966435299,12.));
#145486=CARTESIAN_POINT('Ctrl Pts',(-70.8812077152564,1.12409113243511,
12.));
#145487=CARTESIAN_POINT('Ctrl Pts',(-70.9018541463083,1.13092185496563,
12.));
#145488=CARTESIAN_POINT('Ctrl Pts',(-70.9225390131835,1.13778883418216,
12.));
#145489=CARTESIAN_POINT('Ctrl Pts',(-70.9432621490579,1.14469209291494,
12.));
#145490=CARTESIAN_POINT('Ctrl Pts',(-70.9640233879671,1.1516316537653,12.));
#145491=CARTESIAN_POINT('Ctrl Pts',(-70.9848225647876,1.15860753911489,
12.));
#145492=CARTESIAN_POINT('Ctrl Pts',(-71.0056595152204,1.16561977112882,
12.));
#145493=CARTESIAN_POINT('Ctrl Pts',(-71.0265340757697,1.17266837175775,
12.));
#145494=CARTESIAN_POINT('Ctrl Pts',(-71.0474460837157,1.17975336273499,
12.));
#145495=CARTESIAN_POINT('Ctrl Pts',(-71.0683953771147,1.18687476558126,
12.));
#145496=CARTESIAN_POINT('Ctrl Pts',(-71.089381794801,1.19403260160997,12.));
#145497=CARTESIAN_POINT('Ctrl Pts',(-71.1104051763839,1.20122689192836,
12.));
#145498=CARTESIAN_POINT('Ctrl Pts',(-71.1314653622442,1.20845765743654,
12.));
#145499=CARTESIAN_POINT('Ctrl Pts',(-71.1525621935266,1.21572491882273,
12.));
#145500=CARTESIAN_POINT('Ctrl Pts',(-71.1736955121361,1.22302869657028,
12.));
#145501=CARTESIAN_POINT('Ctrl Pts',(-71.1948651607319,1.23036901096246,
12.));
#145502=CARTESIAN_POINT('Ctrl Pts',(-71.2160709827189,1.23774588208427,
12.));
#145503=CARTESIAN_POINT('Ctrl Pts',(-71.2373128222359,1.24515932982107,
12.));
#145504=CARTESIAN_POINT('Ctrl Pts',(-71.2585905241422,1.2526093738556,12.));
#145505=CARTESIAN_POINT('Ctrl Pts',(-71.2799039340191,1.26009603367564,
12.));
#145506=CARTESIAN_POINT('Ctrl Pts',(-71.301252898167,1.26761932857723,12.));
#145507=CARTESIAN_POINT('Ctrl Pts',(-71.3226372635993,1.2751792776661,12.));
#145508=CARTESIAN_POINT('Ctrl Pts',(-71.344056878033,1.28277589985474,12.));
#145509=CARTESIAN_POINT('Ctrl Pts',(-71.3655115898801,1.2904092138606,12.));
#145510=CARTESIAN_POINT('Ctrl Pts',(-71.3870012482474,1.29807923821413,
12.));
#145511=CARTESIAN_POINT('Ctrl Pts',(-71.4085257029308,1.30578599126139,
12.));
#145512=CARTESIAN_POINT('Ctrl Pts',(-71.4300848044095,1.31352949116538,
12.));
#145513=CARTESIAN_POINT('Ctrl Pts',(-71.4516784038346,1.32130975590231,
12.));
#145514=CARTESIAN_POINT('Ctrl Pts',(-71.4733063530227,1.32912680326131,
12.));
#145515=CARTESIAN_POINT('Ctrl Pts',(-71.4949685044559,1.33698065085227,
12.));
#145516=CARTESIAN_POINT('Ctrl Pts',(-71.5166647112766,1.34487131610785,
12.));
#145517=CARTESIAN_POINT('Ctrl Pts',(-71.538394827283,1.35279881628453,12.));
#145518=CARTESIAN_POINT('Ctrl Pts',(-71.5601587069175,1.36076316845806,
12.));
#145519=CARTESIAN_POINT('Ctrl Pts',(-71.5819562052613,1.36876438952448,
12.));
#145520=CARTESIAN_POINT('Ctrl Pts',(-71.6037871780347,1.37680249620763,
12.));
#145521=CARTESIAN_POINT('Ctrl Pts',(-71.6256514815918,1.38487750506076,
12.));
#145522=CARTESIAN_POINT('Ctrl Pts',(-71.6475489729149,1.39298943246731,
12.));
#145523=CARTESIAN_POINT('Ctrl Pts',(-71.6694795096034,1.40113829463599,
12.));
#145524=CARTESIAN_POINT('Ctrl Pts',(-71.6914429498702,1.40932410760274,
12.));
#145525=CARTESIAN_POINT('Ctrl Pts',(-71.7134391525417,1.41754688723791,
12.));
#145526=CARTESIAN_POINT('Ctrl Pts',(-71.7354679770537,1.42580664924774,
12.));
#145527=CARTESIAN_POINT('Ctrl Pts',(-71.7575292834456,1.43410340917489,
12.));
#145528=CARTESIAN_POINT('Ctrl Pts',(-71.7796229323496,1.44243718239304,
12.));
#145529=CARTESIAN_POINT('Ctrl Pts',(-71.8017487849865,1.45080798410957,
12.));
#145530=CARTESIAN_POINT('Ctrl Pts',(-71.8239067031664,1.45921582937229,
12.));
#145531=CARTESIAN_POINT('Ctrl Pts',(-71.8460965492836,1.46766073307089,
12.));
#145532=CARTESIAN_POINT('Ctrl Pts',(-71.8683181863123,1.4761427099373,12.));
#145533=CARTESIAN_POINT('Ctrl Pts',(-71.8905714777972,1.48466177454021,
12.));
#145534=CARTESIAN_POINT('Ctrl Pts',(-71.9128562878491,1.493217941288,12.));
#145535=CARTESIAN_POINT('Ctrl Pts',(-71.935172481145,1.50181122443535,12.));
#145536=CARTESIAN_POINT('Ctrl Pts',(-71.9575199229241,1.51044163808454,
12.));
#145537=CARTESIAN_POINT('Ctrl Pts',(-71.9798984789828,1.51910919618566,
12.));
#145538=CARTESIAN_POINT('Ctrl Pts',(-72.0023080156647,1.52781391253103,
12.));
#145539=CARTESIAN_POINT('Ctrl Pts',(-72.0247483998582,1.53655580075813,
12.));
#145540=CARTESIAN_POINT('Ctrl Pts',(-72.0472194989968,1.54533487435626,
12.));
#145541=CARTESIAN_POINT('Ctrl Pts',(-72.0697211810548,1.55415114666774,
12.));
#145542=CARTESIAN_POINT('Ctrl Pts',(-72.092253314543,1.56300463088811,12.));
#145543=CARTESIAN_POINT('Ctrl Pts',(-72.1148157684987,1.57189534006043,
12.));
#145544=CARTESIAN_POINT('Ctrl Pts',(-72.1374084124829,1.58082328707808,
12.));
#145545=CARTESIAN_POINT('Ctrl Pts',(-72.1600311165813,1.58978848469128,
12.));
#145546=CARTESIAN_POINT('Ctrl Pts',(-72.1826837514,1.59879094550849,12.));
#145547=CARTESIAN_POINT('Ctrl Pts',(-72.2053661880611,1.60783068199661,
12.));
#145548=CARTESIAN_POINT('Ctrl Pts',(-72.2280782981941,1.61690770647535,
12.));
#145549=CARTESIAN_POINT('Ctrl Pts',(-72.2508199539325,1.62602203111924,
12.));
#145550=CARTESIAN_POINT('Ctrl Pts',(-72.2735910279149,1.63517366796458,
12.));
#145551=CARTESIAN_POINT('Ctrl Pts',(-72.2963913932811,1.64436262891078,
12.));
#145552=CARTESIAN_POINT('Ctrl Pts',(-72.3192209236691,1.65358892572065,
12.));
#145553=CARTESIAN_POINT('Ctrl Pts',(-72.3420794932052,1.66285257001502,
12.));
#145554=CARTESIAN_POINT('Ctrl Pts',(-72.3649669765013,1.67215357327372,
12.));
#145555=CARTESIAN_POINT('Ctrl Pts',(-72.3878832486549,1.68149194684288,
12.));
#145556=CARTESIAN_POINT('Ctrl Pts',(-72.4108281852473,1.6908677019364,12.));
#145557=CARTESIAN_POINT('Ctrl Pts',(-72.4338016623388,1.70028084963646,
12.));
#145558=CARTESIAN_POINT('Ctrl Pts',(-72.4568035564618,1.70973140088837,
12.));
#145559=CARTESIAN_POINT('Ctrl Pts',(-72.4798337446162,1.71921936650032,
12.));
#145560=CARTESIAN_POINT('Ctrl Pts',(-72.5028921042704,1.72874475715098,
12.));
#145561=CARTESIAN_POINT('Ctrl Pts',(-72.5259785133586,1.73830758339123,
12.));
#145562=CARTESIAN_POINT('Ctrl Pts',(-72.5490928502773,1.74790785564476,
12.));
#145563=CARTESIAN_POINT('Ctrl Pts',(-72.5722349938789,1.75754558420349,
12.));
#145564=CARTESIAN_POINT('Ctrl Pts',(-72.5954048234655,1.76722077922579,
12.));
#145565=CARTESIAN_POINT('Ctrl Pts',(-72.618602218792,1.7769334507443,12.));
#145566=CARTESIAN_POINT('Ctrl Pts',(-72.6418270600623,1.78668360866813,
12.));
#145567=CARTESIAN_POINT('Ctrl Pts',(-72.6650792279271,1.79647126278359,
12.));
#145568=CARTESIAN_POINT('Ctrl Pts',(-72.6883586034768,1.80629642275051,
12.));
#145569=CARTESIAN_POINT('Ctrl Pts',(-72.7116650682347,1.81615909809871,
12.));
#145570=CARTESIAN_POINT('Ctrl Pts',(-72.73499850416,1.82605929823565,12.));
#145571=CARTESIAN_POINT('Ctrl Pts',(-72.7583587936454,1.83599703244926,
12.));
#145572=CARTESIAN_POINT('Ctrl Pts',(-72.7817458195155,1.84597230990858,
12.));
#145573=CARTESIAN_POINT('Ctrl Pts',(-72.8051594650214,1.85598513966115,
12.));
#145574=CARTESIAN_POINT('Ctrl Pts',(-72.8285996138346,1.86603553062776,
12.));
#145575=CARTESIAN_POINT('Ctrl Pts',(-72.8520661500465,1.87612349160952,
12.));
#145576=CARTESIAN_POINT('Ctrl Pts',(-72.8755589581674,1.88624903129195,
12.));
#145577=CARTESIAN_POINT('Ctrl Pts',(-72.8990779231226,1.89641215824584,
12.));
#145578=CARTESIAN_POINT('Ctrl Pts',(-72.9226229302483,1.90661288092582,
12.));
#145579=CARTESIAN_POINT('Ctrl Pts',(-72.9461938652816,1.91685120766427,
12.));
#145580=CARTESIAN_POINT('Ctrl Pts',(-72.9697906143638,1.92712714667648,
12.));
#145581=CARTESIAN_POINT('Ctrl Pts',(-72.9934130640414,1.93744070606557,
12.));
#145582=CARTESIAN_POINT('Ctrl Pts',(-73.0170611012659,1.947791893823,12.));
#145583=CARTESIAN_POINT('Ctrl Pts',(-73.0407346133912,1.95818071782773,
12.));
#145584=CARTESIAN_POINT('Ctrl Pts',(-73.0644334881679,1.96860718583944,
12.));
#145585=CARTESIAN_POINT('Ctrl Pts',(-73.0881576137414,1.97907130550172,
12.));
#145586=CARTESIAN_POINT('Ctrl Pts',(-73.1119068786482,1.9895730843493,12.));
#145587=CARTESIAN_POINT('Ctrl Pts',(-73.1356811718094,2.00011252980987,
12.));
#145588=CARTESIAN_POINT('Ctrl Pts',(-73.159480382525,2.01068964920464,12.));
#145589=CARTESIAN_POINT('Ctrl Pts',(-73.1833044004612,2.02130444974351,
12.));
#145590=CARTESIAN_POINT('Ctrl Pts',(-73.2071531156492,2.0319569385244,12.));
#145591=CARTESIAN_POINT('Ctrl Pts',(-73.2310264184965,2.04264712253915,
12.));
#145592=CARTESIAN_POINT('Ctrl Pts',(-73.2549241997946,2.05337500867395,
12.));
#145593=CARTESIAN_POINT('Ctrl Pts',(-73.2788463507248,2.06414060370837,
12.));
#145594=CARTESIAN_POINT('Ctrl Pts',(-73.3027927628636,2.07494391430953,
12.));
#145595=CARTESIAN_POINT('Ctrl Pts',(-73.3267633281822,2.08578494702761,
12.));
#145596=CARTESIAN_POINT('Ctrl Pts',(-73.3507579390254,2.09666370830733,
12.));
#145597=CARTESIAN_POINT('Ctrl Pts',(-73.3747764880903,2.107580204494,12.));
#145598=CARTESIAN_POINT('Ctrl Pts',(-73.3988188684022,2.11853444183763,
12.));
#145599=CARTESIAN_POINT('Ctrl Pts',(-73.4228849732914,2.1295264264936,12.));
#145600=CARTESIAN_POINT('Ctrl Pts',(-73.4469746963622,2.14055616452048,
12.));
#145601=CARTESIAN_POINT('Ctrl Pts',(-73.4710879315367,2.15162366187898,
12.));
#145602=CARTESIAN_POINT('Ctrl Pts',(-73.4952245731044,2.16272892442915,
12.));
#145603=CARTESIAN_POINT('Ctrl Pts',(-73.5193845157705,2.17387195792305,
12.));
#145604=CARTESIAN_POINT('Ctrl Pts',(-73.5435676546934,2.18505276799756,
12.));
#145605=CARTESIAN_POINT('Ctrl Pts',(-73.5677738855461,2.19627136015682,
12.));
#145606=CARTESIAN_POINT('Ctrl Pts',(-73.5920031044604,2.20752773978352,
12.));
#145607=CARTESIAN_POINT('Ctrl Pts',(-73.6162552079044,2.2188219121652,12.));
#145608=CARTESIAN_POINT('Ctrl Pts',(-73.6405300925714,2.23015388251288,
12.));
#145609=CARTESIAN_POINT('Ctrl Pts',(-73.6648276552766,2.24152365597698,
12.));
#145610=CARTESIAN_POINT('Ctrl Pts',(-73.6891477928124,2.25293123766424,
12.));
#145611=CARTESIAN_POINT('Ctrl Pts',(-73.7134904019378,2.26437663263663,
12.));
#145612=CARTESIAN_POINT('Ctrl Pts',(-73.7378553796792,2.27585984587192,
12.));
#145613=CARTESIAN_POINT('Ctrl Pts',(-73.7622426235648,2.28738088222858,
12.));
#145614=CARTESIAN_POINT('Ctrl Pts',(-73.7866520318849,2.29893974640434,
12.));
#145615=CARTESIAN_POINT('Ctrl Pts',(-73.8110835039341,2.31053644289425,
12.));
#145616=CARTESIAN_POINT('Ctrl Pts',(-73.8355369402733,2.32217097594215,
12.));
#145617=CARTESIAN_POINT('Ctrl Pts',(-73.8600122421502,2.3338433496398,12.));
#145618=CARTESIAN_POINT('Ctrl Pts',(-73.8845093109302,2.34555356802139,
12.));
#145619=CARTESIAN_POINT('Ctrl Pts',(-73.9090280474723,2.35730163516323,
12.));
#145620=CARTESIAN_POINT('Ctrl Pts',(-73.9335683516388,2.36908755525994,
12.));
#145621=CARTESIAN_POINT('Ctrl Pts',(-73.9581301214609,2.38091133274932,
12.));
#145622=CARTESIAN_POINT('Ctrl Pts',(-73.9827132538149,2.39277297220716,
12.));
#145623=CARTESIAN_POINT('Ctrl Pts',(-74.0073176459287,2.40467247811496,
12.));
#145624=CARTESIAN_POINT('Ctrl Pts',(-74.0319431966956,2.41660985465228,
12.));
#145625=CARTESIAN_POINT('Ctrl Pts',(-74.0565898079227,2.42858510549786,
12.));
#145626=CARTESIAN_POINT('Ctrl Pts',(-74.0812573859474,2.44059823356721,
12.));
#145627=CARTESIAN_POINT('Ctrl Pts',(-74.1059458420175,2.45264924094852,
12.));
#145628=CARTESIAN_POINT('Ctrl Pts',(-74.1271264545378,2.46301176097528,
12.));
#145629=CARTESIAN_POINT('Ctrl Pts',(-74.1433763941622,2.47097695565719,
12.));
#145630=CARTESIAN_POINT('Ctrl Pts',(-74.1546864735454,2.47652804725575,
12.));
#145631=CARTESIAN_POINT('Ctrl Pts',(-74.1610506466544,2.47965393946828,
12.));
#145632=CARTESIAN_POINT('Ctrl Pts',(-74.1624659714955,2.48034921844905,
12.));
#145633=CARTESIAN_POINT('',(-69.9947925310006,0.853825826608988,0.));
#145634=CARTESIAN_POINT('',(-69.9947925310006,0.853825826608988,0.));
#145635=CARTESIAN_POINT('Ctrl Pts',(-74.1624659714955,2.48034921844905,
0.));
#145636=CARTESIAN_POINT('Ctrl Pts',(-74.1610506466544,2.47965393946828,
0.));
#145637=CARTESIAN_POINT('Ctrl Pts',(-74.1546864735454,2.47652804725575,
0.));
#145638=CARTESIAN_POINT('Ctrl Pts',(-74.1433763941622,2.47097695565719,
0.));
#145639=CARTESIAN_POINT('Ctrl Pts',(-74.1271264545378,2.46301176097528,
0.));
#145640=CARTESIAN_POINT('Ctrl Pts',(-74.1059458420175,2.45264924094852,
0.));
#145641=CARTESIAN_POINT('Ctrl Pts',(-74.0812573859474,2.44059823356721,
0.));
#145642=CARTESIAN_POINT('Ctrl Pts',(-74.0565898079227,2.42858510549786,
0.));
#145643=CARTESIAN_POINT('Ctrl Pts',(-74.0319431966956,2.41660985465228,
0.));
#145644=CARTESIAN_POINT('Ctrl Pts',(-74.0073176459287,2.40467247811496,
0.));
#145645=CARTESIAN_POINT('Ctrl Pts',(-73.9827132538149,2.39277297220716,
0.));
#145646=CARTESIAN_POINT('Ctrl Pts',(-73.9581301214609,2.38091133274932,
0.));
#145647=CARTESIAN_POINT('Ctrl Pts',(-73.9335683516388,2.36908755525994,
0.));
#145648=CARTESIAN_POINT('Ctrl Pts',(-73.9090280474723,2.35730163516323,
0.));
#145649=CARTESIAN_POINT('Ctrl Pts',(-73.8845093109302,2.34555356802139,
0.));
#145650=CARTESIAN_POINT('Ctrl Pts',(-73.8600122421502,2.3338433496398,0.));
#145651=CARTESIAN_POINT('Ctrl Pts',(-73.8355369402733,2.32217097594215,
0.));
#145652=CARTESIAN_POINT('Ctrl Pts',(-73.8110835039341,2.31053644289425,
0.));
#145653=CARTESIAN_POINT('Ctrl Pts',(-73.7866520318849,2.29893974640434,
0.));
#145654=CARTESIAN_POINT('Ctrl Pts',(-73.7622426235648,2.28738088222858,
0.));
#145655=CARTESIAN_POINT('Ctrl Pts',(-73.7378553796792,2.27585984587192,
0.));
#145656=CARTESIAN_POINT('Ctrl Pts',(-73.7134904019378,2.26437663263663,
0.));
#145657=CARTESIAN_POINT('Ctrl Pts',(-73.6891477928124,2.25293123766424,
0.));
#145658=CARTESIAN_POINT('Ctrl Pts',(-73.6648276552766,2.24152365597698,
0.));
#145659=CARTESIAN_POINT('Ctrl Pts',(-73.6405300925714,2.23015388251288,
0.));
#145660=CARTESIAN_POINT('Ctrl Pts',(-73.6162552079044,2.2188219121652,0.));
#145661=CARTESIAN_POINT('Ctrl Pts',(-73.5920031044604,2.20752773978352,
0.));
#145662=CARTESIAN_POINT('Ctrl Pts',(-73.5677738855461,2.19627136015682,
0.));
#145663=CARTESIAN_POINT('Ctrl Pts',(-73.5435676546934,2.18505276799756,
0.));
#145664=CARTESIAN_POINT('Ctrl Pts',(-73.5193845157705,2.17387195792305,
0.));
#145665=CARTESIAN_POINT('Ctrl Pts',(-73.4952245731044,2.16272892442915,
0.));
#145666=CARTESIAN_POINT('Ctrl Pts',(-73.4710879315367,2.15162366187898,
0.));
#145667=CARTESIAN_POINT('Ctrl Pts',(-73.4469746963622,2.14055616452048,
0.));
#145668=CARTESIAN_POINT('Ctrl Pts',(-73.4228849732914,2.1295264264936,0.));
#145669=CARTESIAN_POINT('Ctrl Pts',(-73.3988188684022,2.11853444183763,
0.));
#145670=CARTESIAN_POINT('Ctrl Pts',(-73.3747764880903,2.107580204494,0.));
#145671=CARTESIAN_POINT('Ctrl Pts',(-73.3507579390254,2.09666370830733,
0.));
#145672=CARTESIAN_POINT('Ctrl Pts',(-73.3267633281822,2.08578494702761,
0.));
#145673=CARTESIAN_POINT('Ctrl Pts',(-73.3027927628636,2.07494391430953,
0.));
#145674=CARTESIAN_POINT('Ctrl Pts',(-73.2788463507248,2.06414060370837,
0.));
#145675=CARTESIAN_POINT('Ctrl Pts',(-73.2549241997946,2.05337500867395,
0.));
#145676=CARTESIAN_POINT('Ctrl Pts',(-73.2310264184965,2.04264712253915,
0.));
#145677=CARTESIAN_POINT('Ctrl Pts',(-73.2071531156492,2.0319569385244,0.));
#145678=CARTESIAN_POINT('Ctrl Pts',(-73.1833044004612,2.02130444974351,
0.));
#145679=CARTESIAN_POINT('Ctrl Pts',(-73.159480382525,2.01068964920464,0.));
#145680=CARTESIAN_POINT('Ctrl Pts',(-73.1356811718094,2.00011252980987,
0.));
#145681=CARTESIAN_POINT('Ctrl Pts',(-73.1119068786482,1.9895730843493,0.));
#145682=CARTESIAN_POINT('Ctrl Pts',(-73.0881576137414,1.97907130550172,
0.));
#145683=CARTESIAN_POINT('Ctrl Pts',(-73.0644334881679,1.96860718583944,
0.));
#145684=CARTESIAN_POINT('Ctrl Pts',(-73.0407346133912,1.95818071782773,
0.));
#145685=CARTESIAN_POINT('Ctrl Pts',(-73.0170611012659,1.947791893823,0.));
#145686=CARTESIAN_POINT('Ctrl Pts',(-72.9934130640414,1.93744070606557,
0.));
#145687=CARTESIAN_POINT('Ctrl Pts',(-72.9697906143638,1.92712714667648,
0.));
#145688=CARTESIAN_POINT('Ctrl Pts',(-72.9461938652816,1.91685120766427,
0.));
#145689=CARTESIAN_POINT('Ctrl Pts',(-72.9226229302483,1.90661288092582,
0.));
#145690=CARTESIAN_POINT('Ctrl Pts',(-72.8990779231226,1.89641215824584,
0.));
#145691=CARTESIAN_POINT('Ctrl Pts',(-72.8755589581674,1.88624903129195,
0.));
#145692=CARTESIAN_POINT('Ctrl Pts',(-72.8520661500465,1.87612349160952,
0.));
#145693=CARTESIAN_POINT('Ctrl Pts',(-72.8285996138346,1.86603553062776,
0.));
#145694=CARTESIAN_POINT('Ctrl Pts',(-72.8051594650214,1.85598513966115,
0.));
#145695=CARTESIAN_POINT('Ctrl Pts',(-72.7817458195155,1.84597230990858,
0.));
#145696=CARTESIAN_POINT('Ctrl Pts',(-72.7583587936454,1.83599703244926,
0.));
#145697=CARTESIAN_POINT('Ctrl Pts',(-72.73499850416,1.82605929823565,0.));
#145698=CARTESIAN_POINT('Ctrl Pts',(-72.7116650682347,1.81615909809871,
0.));
#145699=CARTESIAN_POINT('Ctrl Pts',(-72.6883586034768,1.80629642275051,
0.));
#145700=CARTESIAN_POINT('Ctrl Pts',(-72.6650792279271,1.79647126278359,
0.));
#145701=CARTESIAN_POINT('Ctrl Pts',(-72.6418270600623,1.78668360866813,
0.));
#145702=CARTESIAN_POINT('Ctrl Pts',(-72.618602218792,1.7769334507443,0.));
#145703=CARTESIAN_POINT('Ctrl Pts',(-72.5954048234655,1.76722077922579,
0.));
#145704=CARTESIAN_POINT('Ctrl Pts',(-72.5722349938789,1.75754558420349,
0.));
#145705=CARTESIAN_POINT('Ctrl Pts',(-72.5490928502773,1.74790785564476,
0.));
#145706=CARTESIAN_POINT('Ctrl Pts',(-72.5259785133586,1.73830758339123,
0.));
#145707=CARTESIAN_POINT('Ctrl Pts',(-72.5028921042704,1.72874475715098,
0.));
#145708=CARTESIAN_POINT('Ctrl Pts',(-72.4798337446162,1.71921936650032,
0.));
#145709=CARTESIAN_POINT('Ctrl Pts',(-72.4568035564618,1.70973140088837,
0.));
#145710=CARTESIAN_POINT('Ctrl Pts',(-72.4338016623388,1.70028084963646,
0.));
#145711=CARTESIAN_POINT('Ctrl Pts',(-72.4108281852473,1.6908677019364,0.));
#145712=CARTESIAN_POINT('Ctrl Pts',(-72.3878832486549,1.68149194684288,
0.));
#145713=CARTESIAN_POINT('Ctrl Pts',(-72.3649669765013,1.67215357327372,
0.));
#145714=CARTESIAN_POINT('Ctrl Pts',(-72.3420794932052,1.66285257001502,
0.));
#145715=CARTESIAN_POINT('Ctrl Pts',(-72.3192209236691,1.65358892572065,
0.));
#145716=CARTESIAN_POINT('Ctrl Pts',(-72.2963913932811,1.64436262891078,
0.));
#145717=CARTESIAN_POINT('Ctrl Pts',(-72.2735910279149,1.63517366796458,
0.));
#145718=CARTESIAN_POINT('Ctrl Pts',(-72.2508199539325,1.62602203111924,
0.));
#145719=CARTESIAN_POINT('Ctrl Pts',(-72.2280782981941,1.61690770647535,
0.));
#145720=CARTESIAN_POINT('Ctrl Pts',(-72.2053661880611,1.60783068199661,
0.));
#145721=CARTESIAN_POINT('Ctrl Pts',(-72.1826837514,1.59879094550849,0.));
#145722=CARTESIAN_POINT('Ctrl Pts',(-72.1600311165813,1.58978848469128,
0.));
#145723=CARTESIAN_POINT('Ctrl Pts',(-72.1374084124829,1.58082328707808,
0.));
#145724=CARTESIAN_POINT('Ctrl Pts',(-72.1148157684987,1.57189534006043,
0.));
#145725=CARTESIAN_POINT('Ctrl Pts',(-72.092253314543,1.56300463088811,0.));
#145726=CARTESIAN_POINT('Ctrl Pts',(-72.0697211810548,1.55415114666774,
0.));
#145727=CARTESIAN_POINT('Ctrl Pts',(-72.0472194989968,1.54533487435626,
0.));
#145728=CARTESIAN_POINT('Ctrl Pts',(-72.0247483998582,1.53655580075813,
0.));
#145729=CARTESIAN_POINT('Ctrl Pts',(-72.0023080156647,1.52781391253103,
0.));
#145730=CARTESIAN_POINT('Ctrl Pts',(-71.9798984789828,1.51910919618566,
0.));
#145731=CARTESIAN_POINT('Ctrl Pts',(-71.9575199229241,1.51044163808454,
0.));
#145732=CARTESIAN_POINT('Ctrl Pts',(-71.935172481145,1.50181122443535,0.));
#145733=CARTESIAN_POINT('Ctrl Pts',(-71.9128562878491,1.493217941288,0.));
#145734=CARTESIAN_POINT('Ctrl Pts',(-71.8905714777972,1.48466177454021,
0.));
#145735=CARTESIAN_POINT('Ctrl Pts',(-71.8683181863123,1.4761427099373,0.));
#145736=CARTESIAN_POINT('Ctrl Pts',(-71.8460965492836,1.46766073307089,
0.));
#145737=CARTESIAN_POINT('Ctrl Pts',(-71.8239067031664,1.45921582937229,
0.));
#145738=CARTESIAN_POINT('Ctrl Pts',(-71.8017487849865,1.45080798410957,
0.));
#145739=CARTESIAN_POINT('Ctrl Pts',(-71.7796229323496,1.44243718239304,
0.));
#145740=CARTESIAN_POINT('Ctrl Pts',(-71.7575292834456,1.43410340917489,
0.));
#145741=CARTESIAN_POINT('Ctrl Pts',(-71.7354679770537,1.42580664924774,
0.));
#145742=CARTESIAN_POINT('Ctrl Pts',(-71.7134391525417,1.41754688723791,
0.));
#145743=CARTESIAN_POINT('Ctrl Pts',(-71.6914429498702,1.40932410760274,
0.));
#145744=CARTESIAN_POINT('Ctrl Pts',(-71.6694795096034,1.40113829463599,
0.));
#145745=CARTESIAN_POINT('Ctrl Pts',(-71.6475489729149,1.39298943246731,
0.));
#145746=CARTESIAN_POINT('Ctrl Pts',(-71.6256514815918,1.38487750506076,
0.));
#145747=CARTESIAN_POINT('Ctrl Pts',(-71.6037871780347,1.37680249620763,
0.));
#145748=CARTESIAN_POINT('Ctrl Pts',(-71.5819562052613,1.36876438952448,
0.));
#145749=CARTESIAN_POINT('Ctrl Pts',(-71.5601587069175,1.36076316845806,
0.));
#145750=CARTESIAN_POINT('Ctrl Pts',(-71.538394827283,1.35279881628453,0.));
#145751=CARTESIAN_POINT('Ctrl Pts',(-71.5166647112766,1.34487131610785,
0.));
#145752=CARTESIAN_POINT('Ctrl Pts',(-71.4949685044559,1.33698065085227,
0.));
#145753=CARTESIAN_POINT('Ctrl Pts',(-71.4733063530227,1.32912680326131,
0.));
#145754=CARTESIAN_POINT('Ctrl Pts',(-71.4516784038346,1.32130975590231,
0.));
#145755=CARTESIAN_POINT('Ctrl Pts',(-71.4300848044095,1.31352949116538,
0.));
#145756=CARTESIAN_POINT('Ctrl Pts',(-71.4085257029308,1.30578599126139,
0.));
#145757=CARTESIAN_POINT('Ctrl Pts',(-71.3870012482474,1.29807923821413,
0.));
#145758=CARTESIAN_POINT('Ctrl Pts',(-71.3655115898801,1.2904092138606,0.));
#145759=CARTESIAN_POINT('Ctrl Pts',(-71.344056878033,1.28277589985474,0.));
#145760=CARTESIAN_POINT('Ctrl Pts',(-71.3226372635993,1.2751792776661,0.));
#145761=CARTESIAN_POINT('Ctrl Pts',(-71.301252898167,1.26761932857723,0.));
#145762=CARTESIAN_POINT('Ctrl Pts',(-71.2799039340191,1.26009603367564,
0.));
#145763=CARTESIAN_POINT('Ctrl Pts',(-71.2585905241422,1.2526093738556,0.));
#145764=CARTESIAN_POINT('Ctrl Pts',(-71.2373128222359,1.24515932982107,
0.));
#145765=CARTESIAN_POINT('Ctrl Pts',(-71.2160709827189,1.23774588208427,
0.));
#145766=CARTESIAN_POINT('Ctrl Pts',(-71.1948651607319,1.23036901096246,
0.));
#145767=CARTESIAN_POINT('Ctrl Pts',(-71.1736955121361,1.22302869657028,
0.));
#145768=CARTESIAN_POINT('Ctrl Pts',(-71.1525621935266,1.21572491882273,
0.));
#145769=CARTESIAN_POINT('Ctrl Pts',(-71.1314653622442,1.20845765743654,
0.));
#145770=CARTESIAN_POINT('Ctrl Pts',(-71.1104051763839,1.20122689192836,
0.));
#145771=CARTESIAN_POINT('Ctrl Pts',(-71.089381794801,1.19403260160997,0.));
#145772=CARTESIAN_POINT('Ctrl Pts',(-71.0683953771147,1.18687476558126,
0.));
#145773=CARTESIAN_POINT('Ctrl Pts',(-71.0474460837157,1.17975336273499,
0.));
#145774=CARTESIAN_POINT('Ctrl Pts',(-71.0265340757697,1.17266837175775,
0.));
#145775=CARTESIAN_POINT('Ctrl Pts',(-71.0056595152204,1.16561977112882,
0.));
#145776=CARTESIAN_POINT('Ctrl Pts',(-70.9848225647876,1.15860753911489,
0.));
#145777=CARTESIAN_POINT('Ctrl Pts',(-70.9640233879671,1.1516316537653,0.));
#145778=CARTESIAN_POINT('Ctrl Pts',(-70.9432621490579,1.14469209291494,
0.));
#145779=CARTESIAN_POINT('Ctrl Pts',(-70.9225390131835,1.13778883418216,
0.));
#145780=CARTESIAN_POINT('Ctrl Pts',(-70.9018541463083,1.13092185496563,
0.));
#145781=CARTESIAN_POINT('Ctrl Pts',(-70.8812077152564,1.12409113243511,
0.));
#145782=CARTESIAN_POINT('Ctrl Pts',(-70.860599887712,1.1172966435299,0.));
#145783=CARTESIAN_POINT('Ctrl Pts',(-70.8400308322013,1.11053836496637,
0.));
#145784=CARTESIAN_POINT('Ctrl Pts',(-70.8195007180739,1.10381627323945,
0.));
#145785=CARTESIAN_POINT('Ctrl Pts',(-70.7990097154855,1.09713034462269,
0.));
#145786=CARTESIAN_POINT('Ctrl Pts',(-70.7785579953611,1.09048055516434,
0.));
#145787=CARTESIAN_POINT('Ctrl Pts',(-70.7581457294475,1.08386688068348,
0.));
#145788=CARTESIAN_POINT('Ctrl Pts',(-70.737773090397,1.07728929676412,0.));
#145789=CARTESIAN_POINT('Ctrl Pts',(-70.7174402518378,1.07074777874596,
0.));
#145790=CARTESIAN_POINT('Ctrl Pts',(-70.6971473884443,1.0642423017128,0.));
#145791=CARTESIAN_POINT('Ctrl Pts',(-70.6768946760063,1.05777284047727,
0.));
#145792=CARTESIAN_POINT('Ctrl Pts',(-70.6566822912965,1.05133936960068,
0.));
#145793=CARTESIAN_POINT('Ctrl Pts',(-70.6365104119238,1.04494186341155,
0.));
#145794=CARTESIAN_POINT('Ctrl Pts',(-70.6163792162079,1.03858029601905,
0.));
#145795=CARTESIAN_POINT('Ctrl Pts',(-70.5962888829958,1.03225464132872,
0.));
#145796=CARTESIAN_POINT('Ctrl Pts',(-70.5762395916412,1.02596487304049,
0.));
#145797=CARTESIAN_POINT('Ctrl Pts',(-70.5562315224219,1.01971096460599,
0.));
#145798=CARTESIAN_POINT('Ctrl Pts',(-70.5362648569072,1.01349288918539,
0.));
#145799=CARTESIAN_POINT('Ctrl Pts',(-70.5163397782698,1.00731061960967,
0.));
#145800=CARTESIAN_POINT('Ctrl Pts',(-70.4964564717917,1.00116412831437,
0.));
#145801=CARTESIAN_POINT('Ctrl Pts',(-70.4766151245169,0.995053387379677,
0.));
#145802=CARTESIAN_POINT('Ctrl Pts',(-70.4568159243131,0.988978368643586,
0.));
#145803=CARTESIAN_POINT('Ctrl Pts',(-70.4370590590839,0.982939043792156,
0.));
#145804=CARTESIAN_POINT('Ctrl Pts',(-70.41734471596,0.976935384450124,0.));
#145805=CARTESIAN_POINT('Ctrl Pts',(-70.3976730803664,0.970967362281299,
0.));
#145806=CARTESIAN_POINT('Ctrl Pts',(-70.3780443378003,0.965034948786555,
0.));
#145807=CARTESIAN_POINT('Ctrl Pts',(-70.3584586759561,0.959138115058882,
0.));
#145808=CARTESIAN_POINT('Ctrl Pts',(-70.338916286457,0.953276831581228,
0.));
#145809=CARTESIAN_POINT('Ctrl Pts',(-70.3194173673635,0.94745106792956,
0.));
#145810=CARTESIAN_POINT('Ctrl Pts',(-70.2999621233938,0.941660792742949,
0.));
#145811=CARTESIAN_POINT('Ctrl Pts',(-70.2805507606832,0.935905974336487,
0.));
#145812=CARTESIAN_POINT('Ctrl Pts',(-70.2611834821711,0.930186581235571,
0.));
#145813=CARTESIAN_POINT('Ctrl Pts',(-70.241860483586,0.924502582639448,
0.));
#145814=CARTESIAN_POINT('Ctrl Pts',(-70.2225819470306,0.91885394915704,
0.));
#145815=CARTESIAN_POINT('Ctrl Pts',(-70.2033480471749,0.913240652090834,
0.));
#145816=CARTESIAN_POINT('Ctrl Pts',(-70.184158963563,0.907662662015646,
0.));
#145817=CARTESIAN_POINT('Ctrl Pts',(-70.1650148905109,0.902119947629768,
0.));
#145818=CARTESIAN_POINT('Ctrl Pts',(-70.1459160490366,0.89661247437208,
0.));
#145819=CARTESIAN_POINT('Ctrl Pts',(-70.1268626950031,0.89114020346472,
0.));
#145820=CARTESIAN_POINT('Ctrl Pts',(-70.1078550938801,0.885703094803082,
0.));
#145821=CARTESIAN_POINT('Ctrl Pts',(-70.0888934967772,0.880301109661035,
0.));
#145822=CARTESIAN_POINT('Ctrl Pts',(-70.0699781184013,0.874934213255568,
0.));
#145823=CARTESIAN_POINT('Ctrl Pts',(-70.0511091083285,0.869602377870135,
0.));
#145824=CARTESIAN_POINT('Ctrl Pts',(-70.0322865493339,0.864305583660085,
0.));
#145825=CARTESIAN_POINT('Ctrl Pts',(-70.0172656934192,0.860096170667396,
0.));
#145826=CARTESIAN_POINT('Ctrl Pts',(-70.0060209754332,0.856954870258366,
0.));
#145827=CARTESIAN_POINT('Ctrl Pts',(-69.9985337959499,0.854867673848289,
0.));
#145828=CARTESIAN_POINT('Ctrl Pts',(-69.9947925310006,0.853825826608988,
0.));
#145829=CARTESIAN_POINT('Ctrl Pts',(-73.9415940197274,9.10443154852691,
0.));
#145830=CARTESIAN_POINT('Ctrl Pts',(-73.9415940197274,9.10443154852691,
12.));
#145831=CARTESIAN_POINT('Ctrl Pts',(-73.9368365074299,9.1014855851654,0.));
#145832=CARTESIAN_POINT('Ctrl Pts',(-73.9368365074299,9.1014855851654,12.));
#145833=CARTESIAN_POINT('Ctrl Pts',(-73.9273231219835,9.09559760529044,
0.));
#145834=CARTESIAN_POINT('Ctrl Pts',(-73.9273231219835,9.09559760529044,
12.));
#145835=CARTESIAN_POINT('Ctrl Pts',(-73.9130579612604,9.08677747602208,
0.));
#145836=CARTESIAN_POINT('Ctrl Pts',(-73.9130579612604,9.08677747602208,
12.));
#145837=CARTESIAN_POINT('Ctrl Pts',(-73.8940475822492,9.0750409857171,0.));
#145838=CARTESIAN_POINT('Ctrl Pts',(-73.8940475822492,9.0750409857171,12.));
#145839=CARTESIAN_POINT('Ctrl Pts',(-73.8703010078091,9.06040984890249,
0.));
#145840=CARTESIAN_POINT('Ctrl Pts',(-73.8703010078091,9.06040984890249,
12.));
#145841=CARTESIAN_POINT('Ctrl Pts',(-73.8465708501057,9.04581819646987,
0.));
#145842=CARTESIAN_POINT('Ctrl Pts',(-73.8465708501057,9.04581819646987,
12.));
#145843=CARTESIAN_POINT('Ctrl Pts',(-73.8228571411697,9.03126603778128,
0.));
#145844=CARTESIAN_POINT('Ctrl Pts',(-73.8228571411697,9.03126603778128,
12.));
#145845=CARTESIAN_POINT('Ctrl Pts',(-73.7991599312592,9.01675338208007,
0.));
#145846=CARTESIAN_POINT('Ctrl Pts',(-73.7991599312592,9.01675338208007,
12.));
#145847=CARTESIAN_POINT('Ctrl Pts',(-73.7754792943665,9.00228023701058,
0.));
#145848=CARTESIAN_POINT('Ctrl Pts',(-73.7754792943665,9.00228023701058,
12.));
#145849=CARTESIAN_POINT('Ctrl Pts',(-73.7518153261981,8.987846608374,0.));
#145850=CARTESIAN_POINT('Ctrl Pts',(-73.7518153261981,8.987846608374,12.));
#145851=CARTESIAN_POINT('Ctrl Pts',(-73.728168136383,8.97345250083603,0.));
#145852=CARTESIAN_POINT('Ctrl Pts',(-73.728168136383,8.97345250083603,12.));
#145853=CARTESIAN_POINT('Ctrl Pts',(-73.7045378422686,8.95909791836155,
0.));
#145854=CARTESIAN_POINT('Ctrl Pts',(-73.7045378422686,8.95909791836155,
12.));
#145855=CARTESIAN_POINT('Ctrl Pts',(-73.6809245622383,8.94478286474422,
0.));
#145856=CARTESIAN_POINT('Ctrl Pts',(-73.6809245622383,8.94478286474422,
12.));
#145857=CARTESIAN_POINT('Ctrl Pts',(-73.6573284088184,8.93050734412127,
0.));
#145858=CARTESIAN_POINT('Ctrl Pts',(-73.6573284088184,8.93050734412127,
12.));
#145859=CARTESIAN_POINT('Ctrl Pts',(-73.633749483097,8.91627136140087,0.));
#145860=CARTESIAN_POINT('Ctrl Pts',(-73.633749483097,8.91627136140087,12.));
#145861=CARTESIAN_POINT('Ctrl Pts',(-73.6101878785976,8.90207492199045,
0.));
#145862=CARTESIAN_POINT('Ctrl Pts',(-73.6101878785976,8.90207492199045,
12.));
#145863=CARTESIAN_POINT('Ctrl Pts',(-73.5866436840556,8.88791803160445,
0.));
#145864=CARTESIAN_POINT('Ctrl Pts',(-73.5866436840556,8.88791803160445,
12.));
#145865=CARTESIAN_POINT('Ctrl Pts',(-73.5631169867122,8.87380069602973,
0.));
#145866=CARTESIAN_POINT('Ctrl Pts',(-73.5631169867122,8.87380069602973,
12.));
#145867=CARTESIAN_POINT('Ctrl Pts',(-73.5396078751639,8.85972292092133,
0.));
#145868=CARTESIAN_POINT('Ctrl Pts',(-73.5396078751639,8.85972292092133,
12.));
#145869=CARTESIAN_POINT('Ctrl Pts',(-73.5161164429709,8.84568471153808,
0.));
#145870=CARTESIAN_POINT('Ctrl Pts',(-73.5161164429709,8.84568471153808,
12.));
#145871=CARTESIAN_POINT('Ctrl Pts',(-73.492642788273,8.83168607277327,0.));
#145872=CARTESIAN_POINT('Ctrl Pts',(-73.492642788273,8.83168607277327,12.));
#145873=CARTESIAN_POINT('Ctrl Pts',(-73.4691870121567,8.81772700927533,
0.));
#145874=CARTESIAN_POINT('Ctrl Pts',(-73.4691870121567,8.81772700927533,
12.));
#145875=CARTESIAN_POINT('Ctrl Pts',(-73.4457492173933,8.80380752553694,
0.));
#145876=CARTESIAN_POINT('Ctrl Pts',(-73.4457492173933,8.80380752553694,
12.));
#145877=CARTESIAN_POINT('Ctrl Pts',(-73.422329507113,8.78992762598759,0.));
#145878=CARTESIAN_POINT('Ctrl Pts',(-73.422329507113,8.78992762598759,12.));
#145879=CARTESIAN_POINT('Ctrl Pts',(-73.3989279832835,8.7760873150935,0.));
#145880=CARTESIAN_POINT('Ctrl Pts',(-73.3989279832835,8.7760873150935,12.));
#145881=CARTESIAN_POINT('Ctrl Pts',(-73.3755447460268,8.7622865974036,0.));
#145882=CARTESIAN_POINT('Ctrl Pts',(-73.3755447460268,8.7622865974036,12.));
#145883=CARTESIAN_POINT('Ctrl Pts',(-73.3521798944622,8.74852547749781,
0.));
#145884=CARTESIAN_POINT('Ctrl Pts',(-73.3521798944622,8.74852547749781,
12.));
#145885=CARTESIAN_POINT('Ctrl Pts',(-73.3288335272002,8.73480395995383,
0.));
#145886=CARTESIAN_POINT('Ctrl Pts',(-73.3288335272002,8.73480395995383,
12.));
#145887=CARTESIAN_POINT('Ctrl Pts',(-73.3055057429742,8.72112204930234,
0.));
#145888=CARTESIAN_POINT('Ctrl Pts',(-73.3055057429742,8.72112204930234,
12.));
#145889=CARTESIAN_POINT('Ctrl Pts',(-73.2821966412148,8.70747974998232,
0.));
#145890=CARTESIAN_POINT('Ctrl Pts',(-73.2821966412148,8.70747974998232,
12.));
#145891=CARTESIAN_POINT('Ctrl Pts',(-73.2589063226358,8.69387706629287,
0.));
#145892=CARTESIAN_POINT('Ctrl Pts',(-73.2589063226358,8.69387706629287,
12.));
#145893=CARTESIAN_POINT('Ctrl Pts',(-73.2356348889693,8.68031400241874,
0.));
#145894=CARTESIAN_POINT('Ctrl Pts',(-73.2356348889693,8.68031400241874,
12.));
#145895=CARTESIAN_POINT('Ctrl Pts',(-73.2123824427208,8.66679056245095,
0.));
#145896=CARTESIAN_POINT('Ctrl Pts',(-73.2123824427208,8.66679056245095,
12.));
#145897=CARTESIAN_POINT('Ctrl Pts',(-73.1891490869056,8.65330675040539,
0.));
#145898=CARTESIAN_POINT('Ctrl Pts',(-73.1891490869056,8.65330675040539,
12.));
#145899=CARTESIAN_POINT('Ctrl Pts',(-73.1659349248132,8.63986257023741,
0.));
#145900=CARTESIAN_POINT('Ctrl Pts',(-73.1659349248132,8.63986257023741,
12.));
#145901=CARTESIAN_POINT('Ctrl Pts',(-73.1427400597037,8.62645802585486,
0.));
#145902=CARTESIAN_POINT('Ctrl Pts',(-73.1427400597037,8.62645802585486,
12.));
#145903=CARTESIAN_POINT('Ctrl Pts',(-73.1195645948178,8.61309312112004,
0.));
#145904=CARTESIAN_POINT('Ctrl Pts',(-73.1195645948178,8.61309312112004,
12.));
#145905=CARTESIAN_POINT('Ctrl Pts',(-73.0964086335235,8.59976785984554,
0.));
#145906=CARTESIAN_POINT('Ctrl Pts',(-73.0964086335235,8.59976785984554,
12.));
#145907=CARTESIAN_POINT('Ctrl Pts',(-73.0732722794195,8.58648224578734,
0.));
#145908=CARTESIAN_POINT('Ctrl Pts',(-73.0732722794195,8.58648224578734,
12.));
#145909=CARTESIAN_POINT('Ctrl Pts',(-73.0501556364479,8.57323628263595,
0.));
#145910=CARTESIAN_POINT('Ctrl Pts',(-73.0501556364479,8.57323628263595,
12.));
#145911=CARTESIAN_POINT('Ctrl Pts',(-73.0270588090183,8.56002997400086,
0.));
#145912=CARTESIAN_POINT('Ctrl Pts',(-73.0270588090183,8.56002997400086,
12.));
#145913=CARTESIAN_POINT('Ctrl Pts',(-73.0039819020648,8.5468633234042,0.));
#145914=CARTESIAN_POINT('Ctrl Pts',(-73.0039819020648,8.5468633234042,12.));
#145915=CARTESIAN_POINT('Ctrl Pts',(-72.9809250209828,8.53373633429283,
0.));
#145916=CARTESIAN_POINT('Ctrl Pts',(-72.9809250209828,8.53373633429283,
12.));
#145917=CARTESIAN_POINT('Ctrl Pts',(-72.9578882715912,8.5206490100423,0.));
#145918=CARTESIAN_POINT('Ctrl Pts',(-72.9578882715912,8.5206490100423,12.));
#145919=CARTESIAN_POINT('Ctrl Pts',(-72.9348717600838,8.50760135395986,
0.));
#145920=CARTESIAN_POINT('Ctrl Pts',(-72.9348717600838,8.50760135395986,
12.));
#145921=CARTESIAN_POINT('Ctrl Pts',(-72.9118755929795,8.49459336928298,
0.));
#145922=CARTESIAN_POINT('Ctrl Pts',(-72.9118755929795,8.49459336928298,
12.));
#145923=CARTESIAN_POINT('Ctrl Pts',(-72.8888998770785,8.4816250591766,0.));
#145924=CARTESIAN_POINT('Ctrl Pts',(-72.8888998770785,8.4816250591766,12.));
#145925=CARTESIAN_POINT('Ctrl Pts',(-72.8659447194933,8.46869642673797,
0.));
#145926=CARTESIAN_POINT('Ctrl Pts',(-72.8659447194933,8.46869642673797,
12.));
#145927=CARTESIAN_POINT('Ctrl Pts',(-72.8430102276713,8.45580747499796,
0.));
#145928=CARTESIAN_POINT('Ctrl Pts',(-72.8430102276713,8.45580747499796,
12.));
#145929=CARTESIAN_POINT('Ctrl Pts',(-72.8200965094199,8.44295820691914,
0.));
#145930=CARTESIAN_POINT('Ctrl Pts',(-72.8200965094199,8.44295820691914,
12.));
#145931=CARTESIAN_POINT('Ctrl Pts',(-72.7972036729276,8.4301486253916,0.));
#145932=CARTESIAN_POINT('Ctrl Pts',(-72.7972036729276,8.4301486253916,12.));
#145933=CARTESIAN_POINT('Ctrl Pts',(-72.7743318267865,8.41737873322332,
0.));
#145934=CARTESIAN_POINT('Ctrl Pts',(-72.7743318267865,8.41737873322332,
12.));
#145935=CARTESIAN_POINT('Ctrl Pts',(-72.751481079992,8.40464853314471,0.));
#145936=CARTESIAN_POINT('Ctrl Pts',(-72.751481079992,8.40464853314471,12.));
#145937=CARTESIAN_POINT('Ctrl Pts',(-72.7286515419372,8.39195802781393,
0.));
#145938=CARTESIAN_POINT('Ctrl Pts',(-72.7286515419372,8.39195802781393,
12.));
#145939=CARTESIAN_POINT('Ctrl Pts',(-72.705843322407,8.37930721981733,0.));
#145940=CARTESIAN_POINT('Ctrl Pts',(-72.705843322407,8.37930721981733,12.));
#145941=CARTESIAN_POINT('Ctrl Pts',(-72.6830565315703,8.36669611166845,
0.));
#145942=CARTESIAN_POINT('Ctrl Pts',(-72.6830565315703,8.36669611166845,
12.));
#145943=CARTESIAN_POINT('Ctrl Pts',(-72.6602912799696,8.35412470580104,
0.));
#145944=CARTESIAN_POINT('Ctrl Pts',(-72.6602912799696,8.35412470580104,
12.));
#145945=CARTESIAN_POINT('Ctrl Pts',(-72.6375476785215,8.34159300456989,
0.));
#145946=CARTESIAN_POINT('Ctrl Pts',(-72.6375476785215,8.34159300456989,
12.));
#145947=CARTESIAN_POINT('Ctrl Pts',(-72.6148258385296,8.32910101025673,
0.));
#145948=CARTESIAN_POINT('Ctrl Pts',(-72.6148258385296,8.32910101025673,
12.));
#145949=CARTESIAN_POINT('Ctrl Pts',(-72.5921258716901,8.31664872507019,
0.));
#145950=CARTESIAN_POINT('Ctrl Pts',(-72.5921258716901,8.31664872507019,
12.));
#145951=CARTESIAN_POINT('Ctrl Pts',(-72.5694478900981,8.30423615114455,
0.));
#145952=CARTESIAN_POINT('Ctrl Pts',(-72.5694478900981,8.30423615114455,
12.));
#145953=CARTESIAN_POINT('Ctrl Pts',(-72.5467920062521,8.29186329053282,
0.));
#145954=CARTESIAN_POINT('Ctrl Pts',(-72.5467920062521,8.29186329053282,
12.));
#145955=CARTESIAN_POINT('Ctrl Pts',(-72.5241583330562,8.27953014520378,
0.));
#145956=CARTESIAN_POINT('Ctrl Pts',(-72.5241583330562,8.27953014520378,
12.));
#145957=CARTESIAN_POINT('Ctrl Pts',(-72.5015469838254,8.26723671704922,
0.));
#145958=CARTESIAN_POINT('Ctrl Pts',(-72.5015469838254,8.26723671704922,
12.));
#145959=CARTESIAN_POINT('Ctrl Pts',(-72.4789580722875,8.25498300788496,
0.));
#145960=CARTESIAN_POINT('Ctrl Pts',(-72.4789580722875,8.25498300788496,
12.));
#145961=CARTESIAN_POINT('Ctrl Pts',(-72.4563917125842,8.24276901945042,
0.));
#145962=CARTESIAN_POINT('Ctrl Pts',(-72.4563917125842,8.24276901945042,
12.));
#145963=CARTESIAN_POINT('Ctrl Pts',(-72.4338480192694,8.23059475340359,
0.));
#145964=CARTESIAN_POINT('Ctrl Pts',(-72.4338480192694,8.23059475340359,
12.));
#145965=CARTESIAN_POINT('Ctrl Pts',(-72.4113271073079,8.21846021131563,
0.));
#145966=CARTESIAN_POINT('Ctrl Pts',(-72.4113271073079,8.21846021131563,
12.));
#145967=CARTESIAN_POINT('Ctrl Pts',(-72.3888290920832,8.20636539467778,
0.));
#145968=CARTESIAN_POINT('Ctrl Pts',(-72.3888290920832,8.20636539467778,
12.));
#145969=CARTESIAN_POINT('Ctrl Pts',(-72.3663540894026,8.19431030490317,
0.));
#145970=CARTESIAN_POINT('Ctrl Pts',(-72.3663540894026,8.19431030490317,
12.));
#145971=CARTESIAN_POINT('Ctrl Pts',(-72.3439022155007,8.18229494332626,
0.));
#145972=CARTESIAN_POINT('Ctrl Pts',(-72.3439022155007,8.18229494332626,
12.));
#145973=CARTESIAN_POINT('Ctrl Pts',(-72.3214735870409,8.17031931119893,
0.));
#145974=CARTESIAN_POINT('Ctrl Pts',(-72.3214735870409,8.17031931119893,
12.));
#145975=CARTESIAN_POINT('Ctrl Pts',(-72.2990683211162,8.15838340968338,
0.));
#145976=CARTESIAN_POINT('Ctrl Pts',(-72.2990683211162,8.15838340968338,
12.));
#145977=CARTESIAN_POINT('Ctrl Pts',(-72.2766865352555,8.146487239858,0.));
#145978=CARTESIAN_POINT('Ctrl Pts',(-72.2766865352555,8.146487239858,12.));
#145979=CARTESIAN_POINT('Ctrl Pts',(-72.2543283474278,8.13463080272031,
0.));
#145980=CARTESIAN_POINT('Ctrl Pts',(-72.2543283474278,8.13463080272031,
12.));
#145981=CARTESIAN_POINT('Ctrl Pts',(-72.2319938760449,8.12281409918663,
0.));
#145982=CARTESIAN_POINT('Ctrl Pts',(-72.2319938760449,8.12281409918663,
12.));
#145983=CARTESIAN_POINT('Ctrl Pts',(-72.209683239963,8.11103713008931,0.));
#145984=CARTESIAN_POINT('Ctrl Pts',(-72.209683239963,8.11103713008931,12.));
#145985=CARTESIAN_POINT('Ctrl Pts',(-72.1873965584813,8.09929989616892,
0.));
#145986=CARTESIAN_POINT('Ctrl Pts',(-72.1873965584813,8.09929989616892,
12.));
#145987=CARTESIAN_POINT('Ctrl Pts',(-72.1651339513477,8.08760239807839,
0.));
#145988=CARTESIAN_POINT('Ctrl Pts',(-72.1651339513477,8.08760239807839,
12.));
#145989=CARTESIAN_POINT('Ctrl Pts',(-72.1428955387663,8.07594463638721,
0.));
#145990=CARTESIAN_POINT('Ctrl Pts',(-72.1428955387663,8.07594463638721,
12.));
#145991=CARTESIAN_POINT('Ctrl Pts',(-72.1206814413988,8.06432661158098,
0.));
#145992=CARTESIAN_POINT('Ctrl Pts',(-72.1206814413988,8.06432661158098,
12.));
#145993=CARTESIAN_POINT('Ctrl Pts',(-72.0984917803693,8.05274832405951,
0.));
#145994=CARTESIAN_POINT('Ctrl Pts',(-72.0984917803693,8.05274832405951,
12.));
#145995=CARTESIAN_POINT('Ctrl Pts',(-72.0763266772615,8.04120977412874,
0.));
#145996=CARTESIAN_POINT('Ctrl Pts',(-72.0763266772615,8.04120977412874,
12.));
#145997=CARTESIAN_POINT('Ctrl Pts',(-72.0541862541243,8.0297109620031,0.));
#145998=CARTESIAN_POINT('Ctrl Pts',(-72.0541862541243,8.0297109620031,12.));
#145999=CARTESIAN_POINT('Ctrl Pts',(-72.032070633479,8.01825188781059,0.));
#146000=CARTESIAN_POINT('Ctrl Pts',(-72.032070633479,8.01825188781059,12.));
#146001=CARTESIAN_POINT('Ctrl Pts',(-72.0099799383213,8.0068325515925,0.));
#146002=CARTESIAN_POINT('Ctrl Pts',(-72.0099799383213,8.0068325515925,12.));
#146003=CARTESIAN_POINT('Ctrl Pts',(-71.9879142921254,7.99545295330193,
0.));
#146004=CARTESIAN_POINT('Ctrl Pts',(-71.9879142921254,7.99545295330193,
12.));
#146005=CARTESIAN_POINT('Ctrl Pts',(-71.965873818843,7.98411309279615,0.));
#146006=CARTESIAN_POINT('Ctrl Pts',(-71.965873818843,7.98411309279615,12.));
#146007=CARTESIAN_POINT('Ctrl Pts',(-71.943858642908,7.9728129698372,0.));
#146008=CARTESIAN_POINT('Ctrl Pts',(-71.943858642908,7.9728129698372,12.));
#146009=CARTESIAN_POINT('Ctrl Pts',(-71.9218688892431,7.96155258409766,
0.));
#146010=CARTESIAN_POINT('Ctrl Pts',(-71.9218688892431,7.96155258409766,
12.));
#146011=CARTESIAN_POINT('Ctrl Pts',(-71.8999046832643,7.95033193516053,
0.));
#146012=CARTESIAN_POINT('Ctrl Pts',(-71.8999046832643,7.95033193516053,
12.));
#146013=CARTESIAN_POINT('Ctrl Pts',(-71.8779661508832,7.93915102251797,
0.));
#146014=CARTESIAN_POINT('Ctrl Pts',(-71.8779661508832,7.93915102251797,
12.));
#146015=CARTESIAN_POINT('Ctrl Pts',(-71.8560534185071,7.92800984556398,
0.));
#146016=CARTESIAN_POINT('Ctrl Pts',(-71.8560534185071,7.92800984556398,
12.));
#146017=CARTESIAN_POINT('Ctrl Pts',(-71.8341666130426,7.91690840359369,
0.));
#146018=CARTESIAN_POINT('Ctrl Pts',(-71.8341666130426,7.91690840359369,
12.));
#146019=CARTESIAN_POINT('Ctrl Pts',(-71.8123058619042,7.90584669580958,
0.));
#146020=CARTESIAN_POINT('Ctrl Pts',(-71.8123058619042,7.90584669580958,
12.));
#146021=CARTESIAN_POINT('Ctrl Pts',(-71.7904712930175,7.8948247213214,0.));
#146022=CARTESIAN_POINT('Ctrl Pts',(-71.7904712930175,7.8948247213214,12.));
#146023=CARTESIAN_POINT('Ctrl Pts',(-71.7686630348238,7.88384247914526,
0.));
#146024=CARTESIAN_POINT('Ctrl Pts',(-71.7686630348238,7.88384247914526,
12.));
#146025=CARTESIAN_POINT('Ctrl Pts',(-71.7468812162788,7.87289996819656,
0.));
#146026=CARTESIAN_POINT('Ctrl Pts',(-71.7468812162788,7.87289996819656,
12.));
#146027=CARTESIAN_POINT('Ctrl Pts',(-71.7251259668563,7.86199718728829,
0.));
#146028=CARTESIAN_POINT('Ctrl Pts',(-71.7251259668563,7.86199718728829,
12.));
#146029=CARTESIAN_POINT('Ctrl Pts',(-71.7033974165568,7.85113413513738,
0.));
#146030=CARTESIAN_POINT('Ctrl Pts',(-71.7033974165568,7.85113413513738,
12.));
#146031=CARTESIAN_POINT('Ctrl Pts',(-71.6816956959117,7.84031081036492,
0.));
#146032=CARTESIAN_POINT('Ctrl Pts',(-71.6816956959117,7.84031081036492,
12.));
#146033=CARTESIAN_POINT('Ctrl Pts',(-71.6600209359872,7.8295272114951,0.));
#146034=CARTESIAN_POINT('Ctrl Pts',(-71.6600209359872,7.8295272114951,12.));
#146035=CARTESIAN_POINT('Ctrl Pts',(-71.6383732683844,7.81878333694863,
0.));
#146036=CARTESIAN_POINT('Ctrl Pts',(-71.6383732683844,7.81878333694863,
12.));
#146037=CARTESIAN_POINT('Ctrl Pts',(-71.6167528252423,7.80807918504024,
0.));
#146038=CARTESIAN_POINT('Ctrl Pts',(-71.6167528252423,7.80807918504024,
12.));
#146039=CARTESIAN_POINT('Ctrl Pts',(-71.5951597392471,7.79741475398516,
0.));
#146040=CARTESIAN_POINT('Ctrl Pts',(-71.5951597392471,7.79741475398516,
12.));
#146041=CARTESIAN_POINT('Ctrl Pts',(-71.5735941436364,7.78679004189937,
0.));
#146042=CARTESIAN_POINT('Ctrl Pts',(-71.5735941436364,7.78679004189937,
12.));
#146043=CARTESIAN_POINT('Ctrl Pts',(-71.5520561722039,7.77620504679872,
0.));
#146044=CARTESIAN_POINT('Ctrl Pts',(-71.5520561722039,7.77620504679872,
12.));
#146045=CARTESIAN_POINT('Ctrl Pts',(-71.5305459592994,7.76565976659228,
0.));
#146046=CARTESIAN_POINT('Ctrl Pts',(-71.5305459592994,7.76565976659228,
12.));
#146047=CARTESIAN_POINT('Ctrl Pts',(-71.5090636398318,7.75515419907969,
0.));
#146048=CARTESIAN_POINT('Ctrl Pts',(-71.5090636398318,7.75515419907969,
12.));
#146049=CARTESIAN_POINT('Ctrl Pts',(-71.4876093492781,7.74468834195749,
0.));
#146050=CARTESIAN_POINT('Ctrl Pts',(-71.4876093492781,7.74468834195749,
12.));
#146051=CARTESIAN_POINT('Ctrl Pts',(-71.4661832236888,7.73426219281942,
0.));
#146052=CARTESIAN_POINT('Ctrl Pts',(-71.4661832236888,7.73426219281942,
12.));
#146053=CARTESIAN_POINT('Ctrl Pts',(-71.4447853996916,7.72387574915546,
0.));
#146054=CARTESIAN_POINT('Ctrl Pts',(-71.4447853996916,7.72387574915546,
12.));
#146055=CARTESIAN_POINT('Ctrl Pts',(-71.4234160144925,7.71352900834522,
0.));
#146056=CARTESIAN_POINT('Ctrl Pts',(-71.4234160144925,7.71352900834522,
12.));
#146057=CARTESIAN_POINT('Ctrl Pts',(-71.4020752058796,7.70322196765541,
0.));
#146058=CARTESIAN_POINT('Ctrl Pts',(-71.4020752058796,7.70322196765541,
12.));
#146059=CARTESIAN_POINT('Ctrl Pts',(-71.380763112233,7.69295462424614,0.));
#146060=CARTESIAN_POINT('Ctrl Pts',(-71.380763112233,7.69295462424614,12.));
#146061=CARTESIAN_POINT('Ctrl Pts',(-71.3594798725281,7.68272697517089,
0.));
#146062=CARTESIAN_POINT('Ctrl Pts',(-71.3594798725281,7.68272697517089,
12.));
#146063=CARTESIAN_POINT('Ctrl Pts',(-71.3382256263414,7.67253901737555,
0.));
#146064=CARTESIAN_POINT('Ctrl Pts',(-71.3382256263414,7.67253901737555,
12.));
#146065=CARTESIAN_POINT('Ctrl Pts',(-71.3170005138502,7.66239074769165,
0.));
#146066=CARTESIAN_POINT('Ctrl Pts',(-71.3170005138502,7.66239074769165,
12.));
#146067=CARTESIAN_POINT('Ctrl Pts',(-71.2958046758372,7.65228216283406,
0.));
#146068=CARTESIAN_POINT('Ctrl Pts',(-71.2958046758372,7.65228216283406,
12.));
#146069=CARTESIAN_POINT('Ctrl Pts',(-71.2746382537007,7.64221325940727,
0.));
#146070=CARTESIAN_POINT('Ctrl Pts',(-71.2746382537007,7.64221325940727,
12.));
#146071=CARTESIAN_POINT('Ctrl Pts',(-71.2535013894602,7.6321840339054,0.));
#146072=CARTESIAN_POINT('Ctrl Pts',(-71.2535013894602,7.6321840339054,12.));
#146073=CARTESIAN_POINT('Ctrl Pts',(-71.2323942257609,7.62219448271111,
0.));
#146074=CARTESIAN_POINT('Ctrl Pts',(-71.2323942257609,7.62219448271111,
12.));
#146075=CARTESIAN_POINT('Ctrl Pts',(-71.211316905874,7.6122446020884,0.));
#146076=CARTESIAN_POINT('Ctrl Pts',(-71.211316905874,7.6122446020884,12.));
#146077=CARTESIAN_POINT('Ctrl Pts',(-71.1902695737013,7.60233438818099,
0.));
#146078=CARTESIAN_POINT('Ctrl Pts',(-71.1902695737013,7.60233438818099,
12.));
#146079=CARTESIAN_POINT('Ctrl Pts',(-71.1692523737844,7.59246383701816,
0.));
#146080=CARTESIAN_POINT('Ctrl Pts',(-71.1692523737844,7.59246383701816,
12.));
#146081=CARTESIAN_POINT('Ctrl Pts',(-71.1482654513119,7.58263294451454,
0.));
#146082=CARTESIAN_POINT('Ctrl Pts',(-71.1482654513119,7.58263294451454,
12.));
#146083=CARTESIAN_POINT('Ctrl Pts',(-71.1273089521234,7.57284170646889,
0.));
#146084=CARTESIAN_POINT('Ctrl Pts',(-71.1273089521234,7.57284170646889,
12.));
#146085=CARTESIAN_POINT('Ctrl Pts',(-71.106383022711,7.5630901185566,0.));
#146086=CARTESIAN_POINT('Ctrl Pts',(-71.106383022711,7.5630901185566,12.));
#146087=CARTESIAN_POINT('Ctrl Pts',(-71.0854878102243,7.55337817632919,
0.));
#146088=CARTESIAN_POINT('Ctrl Pts',(-71.0854878102243,7.55337817632919,
12.));
#146089=CARTESIAN_POINT('Ctrl Pts',(-71.0646234624811,7.54370587521982,
0.));
#146090=CARTESIAN_POINT('Ctrl Pts',(-71.0646234624811,7.54370587521982,
12.));
#146091=CARTESIAN_POINT('Ctrl Pts',(-71.043790127973,7.53407321054265,0.));
#146092=CARTESIAN_POINT('Ctrl Pts',(-71.043790127973,7.53407321054265,12.));
#146093=CARTESIAN_POINT('Ctrl Pts',(-71.0229879558699,7.52448017749127,
0.));
#146094=CARTESIAN_POINT('Ctrl Pts',(-71.0229879558699,7.52448017749127,
12.));
#146095=CARTESIAN_POINT('Ctrl Pts',(-71.0022170960211,7.51492677113092,
0.));
#146096=CARTESIAN_POINT('Ctrl Pts',(-71.0022170960211,7.51492677113092,
12.));
#146097=CARTESIAN_POINT('Ctrl Pts',(-70.9814776989612,7.50541298639931,
0.));
#146098=CARTESIAN_POINT('Ctrl Pts',(-70.9814776989612,7.50541298639931,
12.));
#146099=CARTESIAN_POINT('Ctrl Pts',(-70.9607699159218,7.49593881811132,
0.));
#146100=CARTESIAN_POINT('Ctrl Pts',(-70.9607699159218,7.49593881811132,
12.));
#146101=CARTESIAN_POINT('Ctrl Pts',(-70.940093898837,7.48650426095826,0.));
#146102=CARTESIAN_POINT('Ctrl Pts',(-70.940093898837,7.48650426095826,12.));
#146103=CARTESIAN_POINT('Ctrl Pts',(-70.9194498003493,7.47710930950564,
0.));
#146104=CARTESIAN_POINT('Ctrl Pts',(-70.9194498003493,7.47710930950564,
12.));
#146105=CARTESIAN_POINT('Ctrl Pts',(-70.8988377738104,7.46775395818529,
0.));
#146106=CARTESIAN_POINT('Ctrl Pts',(-70.8988377738104,7.46775395818529,
12.));
#146107=CARTESIAN_POINT('Ctrl Pts',(-70.87825797329,7.45843820129784,0.));
#146108=CARTESIAN_POINT('Ctrl Pts',(-70.87825797329,7.45843820129784,12.));
#146109=CARTESIAN_POINT('Ctrl Pts',(-70.8577105535848,7.4491620330165,0.));
#146110=CARTESIAN_POINT('Ctrl Pts',(-70.8577105535848,7.4491620330165,12.));
#146111=CARTESIAN_POINT('Ctrl Pts',(-70.8371956702241,7.43992544738608,
0.));
#146112=CARTESIAN_POINT('Ctrl Pts',(-70.8371956702241,7.43992544738608,
12.));
#146113=CARTESIAN_POINT('Ctrl Pts',(-70.8167134794737,7.43072843832017,
0.));
#146114=CARTESIAN_POINT('Ctrl Pts',(-70.8167134794737,7.43072843832017,
12.));
#146115=CARTESIAN_POINT('Ctrl Pts',(-70.7962641383349,7.42157099959328,
0.));
#146116=CARTESIAN_POINT('Ctrl Pts',(-70.7962641383349,7.42157099959328,
12.));
#146117=CARTESIAN_POINT('Ctrl Pts',(-70.7758478045576,7.412453124845,0.));
#146118=CARTESIAN_POINT('Ctrl Pts',(-70.7758478045576,7.412453124845,12.));
#146119=CARTESIAN_POINT('Ctrl Pts',(-70.7554646366514,7.4033748075824,0.));
#146120=CARTESIAN_POINT('Ctrl Pts',(-70.7554646366514,7.4033748075824,12.));
#146121=CARTESIAN_POINT('Ctrl Pts',(-70.735114793895,7.39433604117894,0.));
#146122=CARTESIAN_POINT('Ctrl Pts',(-70.735114793895,7.39433604117894,12.));
#146123=CARTESIAN_POINT('Ctrl Pts',(-70.7147984363423,7.3853368188703,0.));
#146124=CARTESIAN_POINT('Ctrl Pts',(-70.7147984363423,7.3853368188703,12.));
#146125=CARTESIAN_POINT('Ctrl Pts',(-70.6945157248269,7.37637713374763,
0.));
#146126=CARTESIAN_POINT('Ctrl Pts',(-70.6945157248269,7.37637713374763,
12.));
#146127=CARTESIAN_POINT('Ctrl Pts',(-70.6742668209685,7.36745697876297,
0.));
#146128=CARTESIAN_POINT('Ctrl Pts',(-70.6742668209685,7.36745697876297,
12.));
#146129=CARTESIAN_POINT('Ctrl Pts',(-70.6540518871772,7.35857634673054,
0.));
#146130=CARTESIAN_POINT('Ctrl Pts',(-70.6540518871772,7.35857634673054,
12.));
#146131=CARTESIAN_POINT('Ctrl Pts',(-70.6338710866562,7.34973523032583,
0.));
#146132=CARTESIAN_POINT('Ctrl Pts',(-70.6338710866562,7.34973523032583,
12.));
#146133=CARTESIAN_POINT('Ctrl Pts',(-70.6137245834002,7.3409336220802,0.));
#146134=CARTESIAN_POINT('Ctrl Pts',(-70.6137245834002,7.3409336220802,12.));
#146135=CARTESIAN_POINT('Ctrl Pts',(-70.5936125421958,7.3321715143761,0.));
#146136=CARTESIAN_POINT('Ctrl Pts',(-70.5936125421958,7.3321715143761,12.));
#146137=CARTESIAN_POINT('Ctrl Pts',(-70.573535128649,7.3234488994524,0.));
#146138=CARTESIAN_POINT('Ctrl Pts',(-70.573535128649,7.3234488994524,12.));
#146139=CARTESIAN_POINT('Ctrl Pts',(-70.5534925092052,7.31476576940406,
0.));
#146140=CARTESIAN_POINT('Ctrl Pts',(-70.5534925092052,7.31476576940406,
12.));
#146141=CARTESIAN_POINT('Ctrl Pts',(-70.5334848511675,7.30612211618049,
0.));
#146142=CARTESIAN_POINT('Ctrl Pts',(-70.5334848511675,7.30612211618049,
12.));
#146143=CARTESIAN_POINT('Ctrl Pts',(-70.5135123227147,7.29751793157804,
0.));
#146144=CARTESIAN_POINT('Ctrl Pts',(-70.5135123227147,7.29751793157804,
12.));
#146145=CARTESIAN_POINT('Ctrl Pts',(-70.4935750929029,7.28895320723838,
0.));
#146146=CARTESIAN_POINT('Ctrl Pts',(-70.4935750929029,7.28895320723838,
12.));
#146147=CARTESIAN_POINT('Ctrl Pts',(-70.4736733316463,7.28042793465452,
0.));
#146148=CARTESIAN_POINT('Ctrl Pts',(-70.4736733316463,7.28042793465452,
12.));
#146149=CARTESIAN_POINT('Ctrl Pts',(-70.4538072096986,7.2719421051706,0.));
#146150=CARTESIAN_POINT('Ctrl Pts',(-70.4538072096986,7.2719421051706,12.));
#146151=CARTESIAN_POINT('Ctrl Pts',(-70.433976898636,7.26349570998052,0.));
#146152=CARTESIAN_POINT('Ctrl Pts',(-70.433976898636,7.26349570998052,12.));
#146153=CARTESIAN_POINT('Ctrl Pts',(-70.4141825708207,7.25508874012078,
0.));
#146154=CARTESIAN_POINT('Ctrl Pts',(-70.4141825708207,7.25508874012078,
12.));
#146155=CARTESIAN_POINT('Ctrl Pts',(-70.3944243994532,7.24672118647119,
0.));
#146156=CARTESIAN_POINT('Ctrl Pts',(-70.3944243994532,7.24672118647119,
12.));
#146157=CARTESIAN_POINT('Ctrl Pts',(-70.3747025586569,7.23839303975629,
0.));
#146158=CARTESIAN_POINT('Ctrl Pts',(-70.3747025586569,7.23839303975629,
12.));
#146159=CARTESIAN_POINT('Ctrl Pts',(-70.3550172235486,7.23010429054233,
0.));
#146160=CARTESIAN_POINT('Ctrl Pts',(-70.3550172235486,7.23010429054233,
12.));
#146161=CARTESIAN_POINT('Ctrl Pts',(-70.3353685703097,7.2218549292318,0.));
#146162=CARTESIAN_POINT('Ctrl Pts',(-70.3353685703097,7.2218549292318,12.));
#146163=CARTESIAN_POINT('Ctrl Pts',(-70.3157567762561,7.21364494605427,
0.));
#146164=CARTESIAN_POINT('Ctrl Pts',(-70.3157567762561,7.21364494605427,
12.));
#146165=CARTESIAN_POINT('Ctrl Pts',(-70.2961820197051,7.2054743310746,0.));
#146166=CARTESIAN_POINT('Ctrl Pts',(-70.2961820197051,7.2054743310746,12.));
#146167=CARTESIAN_POINT('Ctrl Pts',(-70.276644479827,7.19734307419863,0.));
#146168=CARTESIAN_POINT('Ctrl Pts',(-70.276644479827,7.19734307419863,12.));
#146169=CARTESIAN_POINT('Ctrl Pts',(-70.2571443365198,7.18925116517565,
0.));
#146170=CARTESIAN_POINT('Ctrl Pts',(-70.2571443365198,7.18925116517565,
12.));
#146171=CARTESIAN_POINT('Ctrl Pts',(-70.2376817702239,7.18119859359803,
0.));
#146172=CARTESIAN_POINT('Ctrl Pts',(-70.2376817702239,7.18119859359803,
12.));
#146173=CARTESIAN_POINT('Ctrl Pts',(-70.2182569619028,7.1731853488975,0.));
#146174=CARTESIAN_POINT('Ctrl Pts',(-70.2182569619028,7.1731853488975,12.));
#146175=CARTESIAN_POINT('Ctrl Pts',(-70.1988700934622,7.16521142033895,
0.));
#146176=CARTESIAN_POINT('Ctrl Pts',(-70.1988700934622,7.16521142033895,
12.));
#146177=CARTESIAN_POINT('Ctrl Pts',(-70.1795213481196,7.15727679700949,
0.));
#146178=CARTESIAN_POINT('Ctrl Pts',(-70.1795213481196,7.15727679700949,
12.));
#146179=CARTESIAN_POINT('Ctrl Pts',(-70.1602109107188,7.14938146780804,
0.));
#146180=CARTESIAN_POINT('Ctrl Pts',(-70.1602109107188,7.14938146780804,
12.));
#146181=CARTESIAN_POINT('Ctrl Pts',(-70.1409389682389,7.14152542142342,
0.));
#146182=CARTESIAN_POINT('Ctrl Pts',(-70.1409389682389,7.14152542142342,
12.));
#146183=CARTESIAN_POINT('Ctrl Pts',(-70.1217057094456,7.13370864634401,
0.));
#146184=CARTESIAN_POINT('Ctrl Pts',(-70.1217057094456,7.13370864634401,
12.));
#146185=CARTESIAN_POINT('Ctrl Pts',(-70.1025113239463,7.12593113088873,
0.));
#146186=CARTESIAN_POINT('Ctrl Pts',(-70.1025113239463,7.12593113088873,
12.));
#146187=CARTESIAN_POINT('Ctrl Pts',(-70.0833560013971,7.11819286322826,
0.));
#146188=CARTESIAN_POINT('Ctrl Pts',(-70.0833560013971,7.11819286322826,
12.));
#146189=CARTESIAN_POINT('Ctrl Pts',(-70.06423993069,7.11049383140484,0.));
#146190=CARTESIAN_POINT('Ctrl Pts',(-70.06423993069,7.11049383140484,12.));
#146191=CARTESIAN_POINT('Ctrl Pts',(-70.0451632990136,7.10283402335094,
0.));
#146192=CARTESIAN_POINT('Ctrl Pts',(-70.0451632990136,7.10283402335094,
12.));
#146193=CARTESIAN_POINT('Ctrl Pts',(-70.0261262936435,7.09521342684304,
0.));
#146194=CARTESIAN_POINT('Ctrl Pts',(-70.0261262936435,7.09521342684304,
12.));
#146195=CARTESIAN_POINT('Ctrl Pts',(-70.0071291040791,7.08763202944276,
0.));
#146196=CARTESIAN_POINT('Ctrl Pts',(-70.0071291040791,7.08763202944276,
12.));
#146197=CARTESIAN_POINT('Ctrl Pts',(-69.988171923787,7.08008981844645,0.));
#146198=CARTESIAN_POINT('Ctrl Pts',(-69.988171923787,7.08008981844645,12.));
#146199=CARTESIAN_POINT('Ctrl Pts',(-69.9692549527256,7.07258678080795,
0.));
#146200=CARTESIAN_POINT('Ctrl Pts',(-69.9692549527256,7.07258678080795,
12.));
#146201=CARTESIAN_POINT('Ctrl Pts',(-69.9503783975676,7.06512290312805,
0.));
#146202=CARTESIAN_POINT('Ctrl Pts',(-69.9503783975676,7.06512290312805,
12.));
#146203=CARTESIAN_POINT('Ctrl Pts',(-69.9315424664252,7.05769817180827,
0.));
#146204=CARTESIAN_POINT('Ctrl Pts',(-69.9315424664252,7.05769817180827,
12.));
#146205=CARTESIAN_POINT('Ctrl Pts',(-69.9127473642086,7.0503125731811,0.));
#146206=CARTESIAN_POINT('Ctrl Pts',(-69.9127473642086,7.0503125731811,12.));
#146207=CARTESIAN_POINT('Ctrl Pts',(-69.8939932885864,7.04296609362189,
0.));
#146208=CARTESIAN_POINT('Ctrl Pts',(-69.8939932885864,7.04296609362189,
12.));
#146209=CARTESIAN_POINT('Ctrl Pts',(-69.8752804235296,7.03565871972267,
0.));
#146210=CARTESIAN_POINT('Ctrl Pts',(-69.8752804235296,7.03565871972267,
12.));
#146211=CARTESIAN_POINT('Ctrl Pts',(-69.8566089455448,7.02839043811865,
0.));
#146212=CARTESIAN_POINT('Ctrl Pts',(-69.8566089455448,7.02839043811865,
12.));
#146213=CARTESIAN_POINT('Ctrl Pts',(-69.8379790360574,7.02116123514489,
0.));
#146214=CARTESIAN_POINT('Ctrl Pts',(-69.8379790360574,7.02116123514489,
12.));
#146215=CARTESIAN_POINT('Ctrl Pts',(-69.8193908913722,7.01397109655458,
0.));
#146216=CARTESIAN_POINT('Ctrl Pts',(-69.8193908913722,7.01397109655458,
12.));
#146217=CARTESIAN_POINT('Ctrl Pts',(-69.8008447346782,7.00682000718107,
0.));
#146218=CARTESIAN_POINT('Ctrl Pts',(-69.8008447346782,7.00682000718107,
12.));
#146219=CARTESIAN_POINT('Ctrl Pts',(-69.7823408242446,6.99970795069402,
0.));
#146220=CARTESIAN_POINT('Ctrl Pts',(-69.7823408242446,6.99970795069402,
12.));
#146221=CARTESIAN_POINT('Ctrl Pts',(-69.7638794280263,6.99263491027862,
0.));
#146222=CARTESIAN_POINT('Ctrl Pts',(-69.7638794280263,6.99263491027862,
12.));
#146223=CARTESIAN_POINT('Ctrl Pts',(-69.7454607995524,6.98560086924175,
0.));
#146224=CARTESIAN_POINT('Ctrl Pts',(-69.7454607995524,6.98560086924175,
12.));
#146225=CARTESIAN_POINT('Ctrl Pts',(-69.7270851557443,6.97860581164571,
0.));
#146226=CARTESIAN_POINT('Ctrl Pts',(-69.7270851557443,6.97860581164571,
12.));
#146227=CARTESIAN_POINT('Ctrl Pts',(-69.7087526480248,6.97164972291584,
0.));
#146228=CARTESIAN_POINT('Ctrl Pts',(-69.7087526480248,6.97164972291584,
12.));
#146229=CARTESIAN_POINT('Ctrl Pts',(-69.6904633605834,6.96473259049732,
0.));
#146230=CARTESIAN_POINT('Ctrl Pts',(-69.6904633605834,6.96473259049732,
12.));
#146231=CARTESIAN_POINT('Ctrl Pts',(-69.6758665380764,6.95923004173798,
0.));
#146232=CARTESIAN_POINT('Ctrl Pts',(-69.6758665380764,6.95923004173798,
12.));
#146233=CARTESIAN_POINT('Ctrl Pts',(-69.6649383920075,6.95512065317733,
0.));
#146234=CARTESIAN_POINT('Ctrl Pts',(-69.6649383920075,6.95512065317733,
12.));
#146235=CARTESIAN_POINT('Ctrl Pts',(-69.6576616146559,6.95238884849078,
0.));
#146236=CARTESIAN_POINT('Ctrl Pts',(-69.6576616146559,6.95238884849078,
12.));
#146237=CARTESIAN_POINT('Ctrl Pts',(-69.6540253893193,6.9510248930693,0.));
#146238=CARTESIAN_POINT('Ctrl Pts',(-69.6540253893193,6.9510248930693,12.));
#146239=CARTESIAN_POINT('',(-69.6540253893193,6.9510248930693,12.));
#146240=CARTESIAN_POINT('Ctrl Pts',(-69.6540253893193,6.9510248930693,12.));
#146241=CARTESIAN_POINT('Ctrl Pts',(-69.6576616146559,6.95238884849078,
12.));
#146242=CARTESIAN_POINT('Ctrl Pts',(-69.6649383920075,6.95512065317733,
12.));
#146243=CARTESIAN_POINT('Ctrl Pts',(-69.6758665380764,6.95923004173798,
12.));
#146244=CARTESIAN_POINT('Ctrl Pts',(-69.6904633605834,6.96473259049732,
12.));
#146245=CARTESIAN_POINT('Ctrl Pts',(-69.7087526480248,6.97164972291584,
12.));
#146246=CARTESIAN_POINT('Ctrl Pts',(-69.7270851557443,6.97860581164571,
12.));
#146247=CARTESIAN_POINT('Ctrl Pts',(-69.7454607995524,6.98560086924175,
12.));
#146248=CARTESIAN_POINT('Ctrl Pts',(-69.7638794280263,6.99263491027862,
12.));
#146249=CARTESIAN_POINT('Ctrl Pts',(-69.7823408242446,6.99970795069402,
12.));
#146250=CARTESIAN_POINT('Ctrl Pts',(-69.8008447346782,7.00682000718107,
12.));
#146251=CARTESIAN_POINT('Ctrl Pts',(-69.8193908913722,7.01397109655458,
12.));
#146252=CARTESIAN_POINT('Ctrl Pts',(-69.8379790360574,7.02116123514489,
12.));
#146253=CARTESIAN_POINT('Ctrl Pts',(-69.8566089455448,7.02839043811865,
12.));
#146254=CARTESIAN_POINT('Ctrl Pts',(-69.8752804235296,7.03565871972267,
12.));
#146255=CARTESIAN_POINT('Ctrl Pts',(-69.8939932885864,7.04296609362189,
12.));
#146256=CARTESIAN_POINT('Ctrl Pts',(-69.9127473642086,7.0503125731811,12.));
#146257=CARTESIAN_POINT('Ctrl Pts',(-69.9315424664252,7.05769817180827,
12.));
#146258=CARTESIAN_POINT('Ctrl Pts',(-69.9503783975676,7.06512290312805,
12.));
#146259=CARTESIAN_POINT('Ctrl Pts',(-69.9692549527256,7.07258678080795,
12.));
#146260=CARTESIAN_POINT('Ctrl Pts',(-69.988171923787,7.08008981844645,12.));
#146261=CARTESIAN_POINT('Ctrl Pts',(-70.0071291040791,7.08763202944276,
12.));
#146262=CARTESIAN_POINT('Ctrl Pts',(-70.0261262936435,7.09521342684304,
12.));
#146263=CARTESIAN_POINT('Ctrl Pts',(-70.0451632990136,7.10283402335094,
12.));
#146264=CARTESIAN_POINT('Ctrl Pts',(-70.06423993069,7.11049383140484,12.));
#146265=CARTESIAN_POINT('Ctrl Pts',(-70.0833560013971,7.11819286322826,
12.));
#146266=CARTESIAN_POINT('Ctrl Pts',(-70.1025113239463,7.12593113088873,
12.));
#146267=CARTESIAN_POINT('Ctrl Pts',(-70.1217057094456,7.13370864634401,
12.));
#146268=CARTESIAN_POINT('Ctrl Pts',(-70.1409389682389,7.14152542142342,
12.));
#146269=CARTESIAN_POINT('Ctrl Pts',(-70.1602109107188,7.14938146780804,
12.));
#146270=CARTESIAN_POINT('Ctrl Pts',(-70.1795213481196,7.15727679700949,
12.));
#146271=CARTESIAN_POINT('Ctrl Pts',(-70.1988700934622,7.16521142033895,
12.));
#146272=CARTESIAN_POINT('Ctrl Pts',(-70.2182569619028,7.1731853488975,12.));
#146273=CARTESIAN_POINT('Ctrl Pts',(-70.2376817702239,7.18119859359803,
12.));
#146274=CARTESIAN_POINT('Ctrl Pts',(-70.2571443365198,7.18925116517565,
12.));
#146275=CARTESIAN_POINT('Ctrl Pts',(-70.276644479827,7.19734307419863,12.));
#146276=CARTESIAN_POINT('Ctrl Pts',(-70.2961820197051,7.2054743310746,12.));
#146277=CARTESIAN_POINT('Ctrl Pts',(-70.3157567762561,7.21364494605427,
12.));
#146278=CARTESIAN_POINT('Ctrl Pts',(-70.3353685703097,7.2218549292318,12.));
#146279=CARTESIAN_POINT('Ctrl Pts',(-70.3550172235486,7.23010429054233,
12.));
#146280=CARTESIAN_POINT('Ctrl Pts',(-70.3747025586569,7.23839303975629,
12.));
#146281=CARTESIAN_POINT('Ctrl Pts',(-70.3944243994532,7.24672118647119,
12.));
#146282=CARTESIAN_POINT('Ctrl Pts',(-70.4141825708207,7.25508874012078,
12.));
#146283=CARTESIAN_POINT('Ctrl Pts',(-70.433976898636,7.26349570998052,12.));
#146284=CARTESIAN_POINT('Ctrl Pts',(-70.4538072096986,7.2719421051706,12.));
#146285=CARTESIAN_POINT('Ctrl Pts',(-70.4736733316463,7.28042793465452,
12.));
#146286=CARTESIAN_POINT('Ctrl Pts',(-70.4935750929029,7.28895320723838,
12.));
#146287=CARTESIAN_POINT('Ctrl Pts',(-70.5135123227147,7.29751793157804,
12.));
#146288=CARTESIAN_POINT('Ctrl Pts',(-70.5334848511675,7.30612211618049,
12.));
#146289=CARTESIAN_POINT('Ctrl Pts',(-70.5534925092052,7.31476576940406,
12.));
#146290=CARTESIAN_POINT('Ctrl Pts',(-70.573535128649,7.3234488994524,12.));
#146291=CARTESIAN_POINT('Ctrl Pts',(-70.5936125421958,7.3321715143761,12.));
#146292=CARTESIAN_POINT('Ctrl Pts',(-70.6137245834002,7.3409336220802,12.));
#146293=CARTESIAN_POINT('Ctrl Pts',(-70.6338710866562,7.34973523032583,
12.));
#146294=CARTESIAN_POINT('Ctrl Pts',(-70.6540518871772,7.35857634673054,
12.));
#146295=CARTESIAN_POINT('Ctrl Pts',(-70.6742668209685,7.36745697876297,
12.));
#146296=CARTESIAN_POINT('Ctrl Pts',(-70.6945157248269,7.37637713374763,
12.));
#146297=CARTESIAN_POINT('Ctrl Pts',(-70.7147984363423,7.3853368188703,12.));
#146298=CARTESIAN_POINT('Ctrl Pts',(-70.735114793895,7.39433604117894,12.));
#146299=CARTESIAN_POINT('Ctrl Pts',(-70.7554646366514,7.4033748075824,12.));
#146300=CARTESIAN_POINT('Ctrl Pts',(-70.7758478045576,7.412453124845,12.));
#146301=CARTESIAN_POINT('Ctrl Pts',(-70.7962641383349,7.42157099959328,
12.));
#146302=CARTESIAN_POINT('Ctrl Pts',(-70.8167134794737,7.43072843832017,
12.));
#146303=CARTESIAN_POINT('Ctrl Pts',(-70.8371956702241,7.43992544738608,
12.));
#146304=CARTESIAN_POINT('Ctrl Pts',(-70.8577105535848,7.4491620330165,12.));
#146305=CARTESIAN_POINT('Ctrl Pts',(-70.87825797329,7.45843820129784,12.));
#146306=CARTESIAN_POINT('Ctrl Pts',(-70.8988377738104,7.46775395818529,
12.));
#146307=CARTESIAN_POINT('Ctrl Pts',(-70.9194498003493,7.47710930950564,
12.));
#146308=CARTESIAN_POINT('Ctrl Pts',(-70.940093898837,7.48650426095826,12.));
#146309=CARTESIAN_POINT('Ctrl Pts',(-70.9607699159218,7.49593881811132,
12.));
#146310=CARTESIAN_POINT('Ctrl Pts',(-70.9814776989612,7.50541298639931,
12.));
#146311=CARTESIAN_POINT('Ctrl Pts',(-71.0022170960211,7.51492677113092,
12.));
#146312=CARTESIAN_POINT('Ctrl Pts',(-71.0229879558699,7.52448017749127,
12.));
#146313=CARTESIAN_POINT('Ctrl Pts',(-71.043790127973,7.53407321054265,12.));
#146314=CARTESIAN_POINT('Ctrl Pts',(-71.0646234624811,7.54370587521982,
12.));
#146315=CARTESIAN_POINT('Ctrl Pts',(-71.0854878102243,7.55337817632919,
12.));
#146316=CARTESIAN_POINT('Ctrl Pts',(-71.106383022711,7.5630901185566,12.));
#146317=CARTESIAN_POINT('Ctrl Pts',(-71.1273089521234,7.57284170646889,
12.));
#146318=CARTESIAN_POINT('Ctrl Pts',(-71.1482654513119,7.58263294451454,
12.));
#146319=CARTESIAN_POINT('Ctrl Pts',(-71.1692523737844,7.59246383701816,
12.));
#146320=CARTESIAN_POINT('Ctrl Pts',(-71.1902695737013,7.60233438818099,
12.));
#146321=CARTESIAN_POINT('Ctrl Pts',(-71.211316905874,7.6122446020884,12.));
#146322=CARTESIAN_POINT('Ctrl Pts',(-71.2323942257609,7.62219448271111,
12.));
#146323=CARTESIAN_POINT('Ctrl Pts',(-71.2535013894602,7.6321840339054,12.));
#146324=CARTESIAN_POINT('Ctrl Pts',(-71.2746382537007,7.64221325940727,
12.));
#146325=CARTESIAN_POINT('Ctrl Pts',(-71.2958046758372,7.65228216283406,
12.));
#146326=CARTESIAN_POINT('Ctrl Pts',(-71.3170005138502,7.66239074769165,
12.));
#146327=CARTESIAN_POINT('Ctrl Pts',(-71.3382256263414,7.67253901737555,
12.));
#146328=CARTESIAN_POINT('Ctrl Pts',(-71.3594798725281,7.68272697517089,
12.));
#146329=CARTESIAN_POINT('Ctrl Pts',(-71.380763112233,7.69295462424614,12.));
#146330=CARTESIAN_POINT('Ctrl Pts',(-71.4020752058796,7.70322196765541,
12.));
#146331=CARTESIAN_POINT('Ctrl Pts',(-71.4234160144925,7.71352900834522,
12.));
#146332=CARTESIAN_POINT('Ctrl Pts',(-71.4447853996916,7.72387574915546,
12.));
#146333=CARTESIAN_POINT('Ctrl Pts',(-71.4661832236888,7.73426219281942,
12.));
#146334=CARTESIAN_POINT('Ctrl Pts',(-71.4876093492781,7.74468834195749,
12.));
#146335=CARTESIAN_POINT('Ctrl Pts',(-71.5090636398318,7.75515419907969,
12.));
#146336=CARTESIAN_POINT('Ctrl Pts',(-71.5305459592994,7.76565976659228,
12.));
#146337=CARTESIAN_POINT('Ctrl Pts',(-71.5520561722039,7.77620504679872,
12.));
#146338=CARTESIAN_POINT('Ctrl Pts',(-71.5735941436364,7.78679004189937,
12.));
#146339=CARTESIAN_POINT('Ctrl Pts',(-71.5951597392471,7.79741475398516,
12.));
#146340=CARTESIAN_POINT('Ctrl Pts',(-71.6167528252423,7.80807918504024,
12.));
#146341=CARTESIAN_POINT('Ctrl Pts',(-71.6383732683844,7.81878333694863,
12.));
#146342=CARTESIAN_POINT('Ctrl Pts',(-71.6600209359872,7.8295272114951,12.));
#146343=CARTESIAN_POINT('Ctrl Pts',(-71.6816956959117,7.84031081036492,
12.));
#146344=CARTESIAN_POINT('Ctrl Pts',(-71.7033974165568,7.85113413513738,
12.));
#146345=CARTESIAN_POINT('Ctrl Pts',(-71.7251259668563,7.86199718728829,
12.));
#146346=CARTESIAN_POINT('Ctrl Pts',(-71.7468812162788,7.87289996819656,
12.));
#146347=CARTESIAN_POINT('Ctrl Pts',(-71.7686630348238,7.88384247914526,
12.));
#146348=CARTESIAN_POINT('Ctrl Pts',(-71.7904712930175,7.8948247213214,12.));
#146349=CARTESIAN_POINT('Ctrl Pts',(-71.8123058619042,7.90584669580958,
12.));
#146350=CARTESIAN_POINT('Ctrl Pts',(-71.8341666130426,7.91690840359369,
12.));
#146351=CARTESIAN_POINT('Ctrl Pts',(-71.8560534185071,7.92800984556398,
12.));
#146352=CARTESIAN_POINT('Ctrl Pts',(-71.8779661508832,7.93915102251797,
12.));
#146353=CARTESIAN_POINT('Ctrl Pts',(-71.8999046832643,7.95033193516053,
12.));
#146354=CARTESIAN_POINT('Ctrl Pts',(-71.9218688892431,7.96155258409766,
12.));
#146355=CARTESIAN_POINT('Ctrl Pts',(-71.943858642908,7.9728129698372,12.));
#146356=CARTESIAN_POINT('Ctrl Pts',(-71.965873818843,7.98411309279615,12.));
#146357=CARTESIAN_POINT('Ctrl Pts',(-71.9879142921254,7.99545295330193,
12.));
#146358=CARTESIAN_POINT('Ctrl Pts',(-72.0099799383213,8.0068325515925,12.));
#146359=CARTESIAN_POINT('Ctrl Pts',(-72.032070633479,8.01825188781059,12.));
#146360=CARTESIAN_POINT('Ctrl Pts',(-72.0541862541243,8.0297109620031,12.));
#146361=CARTESIAN_POINT('Ctrl Pts',(-72.0763266772615,8.04120977412874,
12.));
#146362=CARTESIAN_POINT('Ctrl Pts',(-72.0984917803693,8.05274832405951,
12.));
#146363=CARTESIAN_POINT('Ctrl Pts',(-72.1206814413988,8.06432661158098,
12.));
#146364=CARTESIAN_POINT('Ctrl Pts',(-72.1428955387663,8.07594463638721,
12.));
#146365=CARTESIAN_POINT('Ctrl Pts',(-72.1651339513477,8.08760239807839,
12.));
#146366=CARTESIAN_POINT('Ctrl Pts',(-72.1873965584813,8.09929989616892,
12.));
#146367=CARTESIAN_POINT('Ctrl Pts',(-72.209683239963,8.11103713008931,12.));
#146368=CARTESIAN_POINT('Ctrl Pts',(-72.2319938760449,8.12281409918663,
12.));
#146369=CARTESIAN_POINT('Ctrl Pts',(-72.2543283474278,8.13463080272031,
12.));
#146370=CARTESIAN_POINT('Ctrl Pts',(-72.2766865352555,8.146487239858,12.));
#146371=CARTESIAN_POINT('Ctrl Pts',(-72.2990683211162,8.15838340968338,
12.));
#146372=CARTESIAN_POINT('Ctrl Pts',(-72.3214735870409,8.17031931119893,
12.));
#146373=CARTESIAN_POINT('Ctrl Pts',(-72.3439022155007,8.18229494332626,
12.));
#146374=CARTESIAN_POINT('Ctrl Pts',(-72.3663540894026,8.19431030490317,
12.));
#146375=CARTESIAN_POINT('Ctrl Pts',(-72.3888290920832,8.20636539467778,
12.));
#146376=CARTESIAN_POINT('Ctrl Pts',(-72.4113271073079,8.21846021131563,
12.));
#146377=CARTESIAN_POINT('Ctrl Pts',(-72.4338480192694,8.23059475340359,
12.));
#146378=CARTESIAN_POINT('Ctrl Pts',(-72.4563917125842,8.24276901945042,
12.));
#146379=CARTESIAN_POINT('Ctrl Pts',(-72.4789580722875,8.25498300788496,
12.));
#146380=CARTESIAN_POINT('Ctrl Pts',(-72.5015469838254,8.26723671704922,
12.));
#146381=CARTESIAN_POINT('Ctrl Pts',(-72.5241583330562,8.27953014520378,
12.));
#146382=CARTESIAN_POINT('Ctrl Pts',(-72.5467920062521,8.29186329053282,
12.));
#146383=CARTESIAN_POINT('Ctrl Pts',(-72.5694478900981,8.30423615114455,
12.));
#146384=CARTESIAN_POINT('Ctrl Pts',(-72.5921258716901,8.31664872507019,
12.));
#146385=CARTESIAN_POINT('Ctrl Pts',(-72.6148258385296,8.32910101025673,
12.));
#146386=CARTESIAN_POINT('Ctrl Pts',(-72.6375476785215,8.34159300456989,
12.));
#146387=CARTESIAN_POINT('Ctrl Pts',(-72.6602912799696,8.35412470580104,
12.));
#146388=CARTESIAN_POINT('Ctrl Pts',(-72.6830565315703,8.36669611166845,
12.));
#146389=CARTESIAN_POINT('Ctrl Pts',(-72.705843322407,8.37930721981733,12.));
#146390=CARTESIAN_POINT('Ctrl Pts',(-72.7286515419372,8.39195802781393,
12.));
#146391=CARTESIAN_POINT('Ctrl Pts',(-72.751481079992,8.40464853314471,12.));
#146392=CARTESIAN_POINT('Ctrl Pts',(-72.7743318267865,8.41737873322332,
12.));
#146393=CARTESIAN_POINT('Ctrl Pts',(-72.7972036729276,8.4301486253916,12.));
#146394=CARTESIAN_POINT('Ctrl Pts',(-72.8200965094199,8.44295820691914,
12.));
#146395=CARTESIAN_POINT('Ctrl Pts',(-72.8430102276713,8.45580747499796,
12.));
#146396=CARTESIAN_POINT('Ctrl Pts',(-72.8659447194933,8.46869642673797,
12.));
#146397=CARTESIAN_POINT('Ctrl Pts',(-72.8888998770785,8.4816250591766,12.));
#146398=CARTESIAN_POINT('Ctrl Pts',(-72.9118755929795,8.49459336928298,
12.));
#146399=CARTESIAN_POINT('Ctrl Pts',(-72.9348717600838,8.50760135395986,
12.));
#146400=CARTESIAN_POINT('Ctrl Pts',(-72.9578882715912,8.5206490100423,12.));
#146401=CARTESIAN_POINT('Ctrl Pts',(-72.9809250209828,8.53373633429283,
12.));
#146402=CARTESIAN_POINT('Ctrl Pts',(-73.0039819020648,8.5468633234042,12.));
#146403=CARTESIAN_POINT('Ctrl Pts',(-73.0270588090183,8.56002997400086,
12.));
#146404=CARTESIAN_POINT('Ctrl Pts',(-73.0501556364479,8.57323628263595,
12.));
#146405=CARTESIAN_POINT('Ctrl Pts',(-73.0732722794195,8.58648224578734,
12.));
#146406=CARTESIAN_POINT('Ctrl Pts',(-73.0964086335235,8.59976785984554,
12.));
#146407=CARTESIAN_POINT('Ctrl Pts',(-73.1195645948178,8.61309312112004,
12.));
#146408=CARTESIAN_POINT('Ctrl Pts',(-73.1427400597037,8.62645802585486,
12.));
#146409=CARTESIAN_POINT('Ctrl Pts',(-73.1659349248132,8.63986257023741,
12.));
#146410=CARTESIAN_POINT('Ctrl Pts',(-73.1891490869056,8.65330675040539,
12.));
#146411=CARTESIAN_POINT('Ctrl Pts',(-73.2123824427208,8.66679056245095,
12.));
#146412=CARTESIAN_POINT('Ctrl Pts',(-73.2356348889693,8.68031400241874,
12.));
#146413=CARTESIAN_POINT('Ctrl Pts',(-73.2589063226358,8.69387706629287,
12.));
#146414=CARTESIAN_POINT('Ctrl Pts',(-73.2821966412148,8.70747974998232,
12.));
#146415=CARTESIAN_POINT('Ctrl Pts',(-73.3055057429742,8.72112204930234,
12.));
#146416=CARTESIAN_POINT('Ctrl Pts',(-73.3288335272002,8.73480395995383,
12.));
#146417=CARTESIAN_POINT('Ctrl Pts',(-73.3521798944622,8.74852547749781,
12.));
#146418=CARTESIAN_POINT('Ctrl Pts',(-73.3755447460268,8.7622865974036,12.));
#146419=CARTESIAN_POINT('Ctrl Pts',(-73.3989279832835,8.7760873150935,12.));
#146420=CARTESIAN_POINT('Ctrl Pts',(-73.422329507113,8.78992762598759,12.));
#146421=CARTESIAN_POINT('Ctrl Pts',(-73.4457492173933,8.80380752553694,
12.));
#146422=CARTESIAN_POINT('Ctrl Pts',(-73.4691870121567,8.81772700927533,
12.));
#146423=CARTESIAN_POINT('Ctrl Pts',(-73.492642788273,8.83168607277327,12.));
#146424=CARTESIAN_POINT('Ctrl Pts',(-73.5161164429709,8.84568471153808,
12.));
#146425=CARTESIAN_POINT('Ctrl Pts',(-73.5396078751639,8.85972292092133,
12.));
#146426=CARTESIAN_POINT('Ctrl Pts',(-73.5631169867122,8.87380069602973,
12.));
#146427=CARTESIAN_POINT('Ctrl Pts',(-73.5866436840556,8.88791803160445,
12.));
#146428=CARTESIAN_POINT('Ctrl Pts',(-73.6101878785976,8.90207492199045,
12.));
#146429=CARTESIAN_POINT('Ctrl Pts',(-73.6303847393629,8.914244021516,12.));
#146430=CARTESIAN_POINT('Ctrl Pts',(-73.6458786306023,8.92359518178491,
12.));
#146431=CARTESIAN_POINT('Ctrl Pts',(-73.6566618622073,8.93011088817314,
12.));
#146432=CARTESIAN_POINT('Ctrl Pts',(-73.6627293782587,8.93377955965632,
12.));
#146433=CARTESIAN_POINT('Ctrl Pts',(-73.6640787198055,8.93459554657838,
12.));
#146434=CARTESIAN_POINT('',(-69.6540253893193,6.9510248930693,0.));
#146435=CARTESIAN_POINT('',(-69.6540253893193,6.9510248930693,0.));
#146436=CARTESIAN_POINT('Ctrl Pts',(-73.6640787198055,8.93459554657839,
0.));
#146437=CARTESIAN_POINT('Ctrl Pts',(-73.6627293782587,8.93377955965634,
0.));
#146438=CARTESIAN_POINT('Ctrl Pts',(-73.6566618622074,8.93011088817316,
0.));
#146439=CARTESIAN_POINT('Ctrl Pts',(-73.6458786306023,8.92359518178491,
0.));
#146440=CARTESIAN_POINT('Ctrl Pts',(-73.6303847393629,8.914244021516,0.));
#146441=CARTESIAN_POINT('Ctrl Pts',(-73.6101878785976,8.90207492199045,
0.));
#146442=CARTESIAN_POINT('Ctrl Pts',(-73.5866436840556,8.88791803160445,
0.));
#146443=CARTESIAN_POINT('Ctrl Pts',(-73.5631169867122,8.87380069602973,
0.));
#146444=CARTESIAN_POINT('Ctrl Pts',(-73.5396078751639,8.85972292092133,
0.));
#146445=CARTESIAN_POINT('Ctrl Pts',(-73.5161164429709,8.84568471153808,
0.));
#146446=CARTESIAN_POINT('Ctrl Pts',(-73.492642788273,8.83168607277327,0.));
#146447=CARTESIAN_POINT('Ctrl Pts',(-73.4691870121567,8.81772700927533,
0.));
#146448=CARTESIAN_POINT('Ctrl Pts',(-73.4457492173933,8.80380752553694,
0.));
#146449=CARTESIAN_POINT('Ctrl Pts',(-73.422329507113,8.78992762598759,0.));
#146450=CARTESIAN_POINT('Ctrl Pts',(-73.3989279832835,8.7760873150935,0.));
#146451=CARTESIAN_POINT('Ctrl Pts',(-73.3755447460268,8.7622865974036,0.));
#146452=CARTESIAN_POINT('Ctrl Pts',(-73.3521798944622,8.74852547749781,
0.));
#146453=CARTESIAN_POINT('Ctrl Pts',(-73.3288335272002,8.73480395995383,
0.));
#146454=CARTESIAN_POINT('Ctrl Pts',(-73.3055057429742,8.72112204930234,
0.));
#146455=CARTESIAN_POINT('Ctrl Pts',(-73.2821966412148,8.70747974998232,
0.));
#146456=CARTESIAN_POINT('Ctrl Pts',(-73.2589063226358,8.69387706629287,
0.));
#146457=CARTESIAN_POINT('Ctrl Pts',(-73.2356348889693,8.68031400241874,
0.));
#146458=CARTESIAN_POINT('Ctrl Pts',(-73.2123824427208,8.66679056245095,
0.));
#146459=CARTESIAN_POINT('Ctrl Pts',(-73.1891490869056,8.65330675040539,
0.));
#146460=CARTESIAN_POINT('Ctrl Pts',(-73.1659349248132,8.63986257023741,
0.));
#146461=CARTESIAN_POINT('Ctrl Pts',(-73.1427400597037,8.62645802585486,
0.));
#146462=CARTESIAN_POINT('Ctrl Pts',(-73.1195645948178,8.61309312112004,
0.));
#146463=CARTESIAN_POINT('Ctrl Pts',(-73.0964086335235,8.59976785984554,
0.));
#146464=CARTESIAN_POINT('Ctrl Pts',(-73.0732722794195,8.58648224578734,
0.));
#146465=CARTESIAN_POINT('Ctrl Pts',(-73.0501556364479,8.57323628263595,
0.));
#146466=CARTESIAN_POINT('Ctrl Pts',(-73.0270588090183,8.56002997400086,
0.));
#146467=CARTESIAN_POINT('Ctrl Pts',(-73.0039819020648,8.5468633234042,0.));
#146468=CARTESIAN_POINT('Ctrl Pts',(-72.9809250209828,8.53373633429283,
0.));
#146469=CARTESIAN_POINT('Ctrl Pts',(-72.9578882715912,8.5206490100423,0.));
#146470=CARTESIAN_POINT('Ctrl Pts',(-72.9348717600838,8.50760135395986,
0.));
#146471=CARTESIAN_POINT('Ctrl Pts',(-72.9118755929795,8.49459336928298,
0.));
#146472=CARTESIAN_POINT('Ctrl Pts',(-72.8888998770785,8.4816250591766,0.));
#146473=CARTESIAN_POINT('Ctrl Pts',(-72.8659447194933,8.46869642673797,
0.));
#146474=CARTESIAN_POINT('Ctrl Pts',(-72.8430102276713,8.45580747499796,
0.));
#146475=CARTESIAN_POINT('Ctrl Pts',(-72.8200965094199,8.44295820691914,
0.));
#146476=CARTESIAN_POINT('Ctrl Pts',(-72.7972036729276,8.4301486253916,0.));
#146477=CARTESIAN_POINT('Ctrl Pts',(-72.7743318267865,8.41737873322332,
0.));
#146478=CARTESIAN_POINT('Ctrl Pts',(-72.751481079992,8.40464853314471,0.));
#146479=CARTESIAN_POINT('Ctrl Pts',(-72.7286515419372,8.39195802781393,
0.));
#146480=CARTESIAN_POINT('Ctrl Pts',(-72.705843322407,8.37930721981733,0.));
#146481=CARTESIAN_POINT('Ctrl Pts',(-72.6830565315703,8.36669611166845,
0.));
#146482=CARTESIAN_POINT('Ctrl Pts',(-72.6602912799696,8.35412470580104,
0.));
#146483=CARTESIAN_POINT('Ctrl Pts',(-72.6375476785215,8.34159300456989,
0.));
#146484=CARTESIAN_POINT('Ctrl Pts',(-72.6148258385296,8.32910101025673,
0.));
#146485=CARTESIAN_POINT('Ctrl Pts',(-72.5921258716901,8.31664872507019,
0.));
#146486=CARTESIAN_POINT('Ctrl Pts',(-72.5694478900981,8.30423615114455,
0.));
#146487=CARTESIAN_POINT('Ctrl Pts',(-72.5467920062521,8.29186329053282,
0.));
#146488=CARTESIAN_POINT('Ctrl Pts',(-72.5241583330562,8.27953014520378,
0.));
#146489=CARTESIAN_POINT('Ctrl Pts',(-72.5015469838254,8.26723671704922,
0.));
#146490=CARTESIAN_POINT('Ctrl Pts',(-72.4789580722875,8.25498300788496,
0.));
#146491=CARTESIAN_POINT('Ctrl Pts',(-72.4563917125842,8.24276901945042,
0.));
#146492=CARTESIAN_POINT('Ctrl Pts',(-72.4338480192694,8.23059475340359,
0.));
#146493=CARTESIAN_POINT('Ctrl Pts',(-72.4113271073079,8.21846021131563,
0.));
#146494=CARTESIAN_POINT('Ctrl Pts',(-72.3888290920832,8.20636539467778,
0.));
#146495=CARTESIAN_POINT('Ctrl Pts',(-72.3663540894026,8.19431030490317,
0.));
#146496=CARTESIAN_POINT('Ctrl Pts',(-72.3439022155007,8.18229494332626,
0.));
#146497=CARTESIAN_POINT('Ctrl Pts',(-72.3214735870409,8.17031931119893,
0.));
#146498=CARTESIAN_POINT('Ctrl Pts',(-72.2990683211162,8.15838340968338,
0.));
#146499=CARTESIAN_POINT('Ctrl Pts',(-72.2766865352555,8.146487239858,0.));
#146500=CARTESIAN_POINT('Ctrl Pts',(-72.2543283474278,8.13463080272031,
0.));
#146501=CARTESIAN_POINT('Ctrl Pts',(-72.2319938760449,8.12281409918663,
0.));
#146502=CARTESIAN_POINT('Ctrl Pts',(-72.209683239963,8.11103713008931,0.));
#146503=CARTESIAN_POINT('Ctrl Pts',(-72.1873965584813,8.09929989616892,
0.));
#146504=CARTESIAN_POINT('Ctrl Pts',(-72.1651339513477,8.08760239807839,
0.));
#146505=CARTESIAN_POINT('Ctrl Pts',(-72.1428955387663,8.07594463638721,
0.));
#146506=CARTESIAN_POINT('Ctrl Pts',(-72.1206814413988,8.06432661158098,
0.));
#146507=CARTESIAN_POINT('Ctrl Pts',(-72.0984917803693,8.05274832405951,
0.));
#146508=CARTESIAN_POINT('Ctrl Pts',(-72.0763266772615,8.04120977412874,
0.));
#146509=CARTESIAN_POINT('Ctrl Pts',(-72.0541862541243,8.0297109620031,0.));
#146510=CARTESIAN_POINT('Ctrl Pts',(-72.032070633479,8.01825188781059,0.));
#146511=CARTESIAN_POINT('Ctrl Pts',(-72.0099799383213,8.0068325515925,0.));
#146512=CARTESIAN_POINT('Ctrl Pts',(-71.9879142921254,7.99545295330193,
0.));
#146513=CARTESIAN_POINT('Ctrl Pts',(-71.965873818843,7.98411309279615,0.));
#146514=CARTESIAN_POINT('Ctrl Pts',(-71.943858642908,7.9728129698372,0.));
#146515=CARTESIAN_POINT('Ctrl Pts',(-71.9218688892431,7.96155258409766,
0.));
#146516=CARTESIAN_POINT('Ctrl Pts',(-71.8999046832643,7.95033193516053,
0.));
#146517=CARTESIAN_POINT('Ctrl Pts',(-71.8779661508832,7.93915102251797,
0.));
#146518=CARTESIAN_POINT('Ctrl Pts',(-71.8560534185071,7.92800984556398,
0.));
#146519=CARTESIAN_POINT('Ctrl Pts',(-71.8341666130426,7.91690840359369,
0.));
#146520=CARTESIAN_POINT('Ctrl Pts',(-71.8123058619042,7.90584669580958,
0.));
#146521=CARTESIAN_POINT('Ctrl Pts',(-71.7904712930175,7.8948247213214,0.));
#146522=CARTESIAN_POINT('Ctrl Pts',(-71.7686630348238,7.88384247914526,
0.));
#146523=CARTESIAN_POINT('Ctrl Pts',(-71.7468812162788,7.87289996819656,
0.));
#146524=CARTESIAN_POINT('Ctrl Pts',(-71.7251259668563,7.86199718728829,
0.));
#146525=CARTESIAN_POINT('Ctrl Pts',(-71.7033974165568,7.85113413513738,
0.));
#146526=CARTESIAN_POINT('Ctrl Pts',(-71.6816956959117,7.84031081036492,
0.));
#146527=CARTESIAN_POINT('Ctrl Pts',(-71.6600209359872,7.8295272114951,0.));
#146528=CARTESIAN_POINT('Ctrl Pts',(-71.6383732683844,7.81878333694863,
0.));
#146529=CARTESIAN_POINT('Ctrl Pts',(-71.6167528252423,7.80807918504024,
0.));
#146530=CARTESIAN_POINT('Ctrl Pts',(-71.5951597392471,7.79741475398516,
0.));
#146531=CARTESIAN_POINT('Ctrl Pts',(-71.5735941436364,7.78679004189937,
0.));
#146532=CARTESIAN_POINT('Ctrl Pts',(-71.5520561722039,7.77620504679872,
0.));
#146533=CARTESIAN_POINT('Ctrl Pts',(-71.5305459592994,7.76565976659228,
0.));
#146534=CARTESIAN_POINT('Ctrl Pts',(-71.5090636398318,7.75515419907969,
0.));
#146535=CARTESIAN_POINT('Ctrl Pts',(-71.4876093492781,7.74468834195749,
0.));
#146536=CARTESIAN_POINT('Ctrl Pts',(-71.4661832236888,7.73426219281942,
0.));
#146537=CARTESIAN_POINT('Ctrl Pts',(-71.4447853996916,7.72387574915546,
0.));
#146538=CARTESIAN_POINT('Ctrl Pts',(-71.4234160144925,7.71352900834522,
0.));
#146539=CARTESIAN_POINT('Ctrl Pts',(-71.4020752058796,7.70322196765541,
0.));
#146540=CARTESIAN_POINT('Ctrl Pts',(-71.380763112233,7.69295462424614,0.));
#146541=CARTESIAN_POINT('Ctrl Pts',(-71.3594798725281,7.68272697517089,
0.));
#146542=CARTESIAN_POINT('Ctrl Pts',(-71.3382256263414,7.67253901737555,
0.));
#146543=CARTESIAN_POINT('Ctrl Pts',(-71.3170005138502,7.66239074769165,
0.));
#146544=CARTESIAN_POINT('Ctrl Pts',(-71.2958046758372,7.65228216283406,
0.));
#146545=CARTESIAN_POINT('Ctrl Pts',(-71.2746382537007,7.64221325940727,
0.));
#146546=CARTESIAN_POINT('Ctrl Pts',(-71.2535013894602,7.6321840339054,0.));
#146547=CARTESIAN_POINT('Ctrl Pts',(-71.2323942257609,7.62219448271111,
0.));
#146548=CARTESIAN_POINT('Ctrl Pts',(-71.211316905874,7.6122446020884,0.));
#146549=CARTESIAN_POINT('Ctrl Pts',(-71.1902695737013,7.60233438818099,
0.));
#146550=CARTESIAN_POINT('Ctrl Pts',(-71.1692523737844,7.59246383701816,
0.));
#146551=CARTESIAN_POINT('Ctrl Pts',(-71.1482654513119,7.58263294451454,
0.));
#146552=CARTESIAN_POINT('Ctrl Pts',(-71.1273089521234,7.57284170646889,
0.));
#146553=CARTESIAN_POINT('Ctrl Pts',(-71.106383022711,7.5630901185566,0.));
#146554=CARTESIAN_POINT('Ctrl Pts',(-71.0854878102243,7.55337817632919,
0.));
#146555=CARTESIAN_POINT('Ctrl Pts',(-71.0646234624811,7.54370587521982,
0.));
#146556=CARTESIAN_POINT('Ctrl Pts',(-71.043790127973,7.53407321054265,0.));
#146557=CARTESIAN_POINT('Ctrl Pts',(-71.0229879558699,7.52448017749127,
0.));
#146558=CARTESIAN_POINT('Ctrl Pts',(-71.0022170960211,7.51492677113092,
0.));
#146559=CARTESIAN_POINT('Ctrl Pts',(-70.9814776989612,7.50541298639931,
0.));
#146560=CARTESIAN_POINT('Ctrl Pts',(-70.9607699159218,7.49593881811132,
0.));
#146561=CARTESIAN_POINT('Ctrl Pts',(-70.940093898837,7.48650426095826,0.));
#146562=CARTESIAN_POINT('Ctrl Pts',(-70.9194498003493,7.47710930950564,
0.));
#146563=CARTESIAN_POINT('Ctrl Pts',(-70.8988377738104,7.46775395818529,
0.));
#146564=CARTESIAN_POINT('Ctrl Pts',(-70.87825797329,7.45843820129784,0.));
#146565=CARTESIAN_POINT('Ctrl Pts',(-70.8577105535848,7.4491620330165,0.));
#146566=CARTESIAN_POINT('Ctrl Pts',(-70.8371956702241,7.43992544738608,
0.));
#146567=CARTESIAN_POINT('Ctrl Pts',(-70.8167134794737,7.43072843832017,
0.));
#146568=CARTESIAN_POINT('Ctrl Pts',(-70.7962641383349,7.42157099959328,
0.));
#146569=CARTESIAN_POINT('Ctrl Pts',(-70.7758478045576,7.412453124845,0.));
#146570=CARTESIAN_POINT('Ctrl Pts',(-70.7554646366514,7.4033748075824,0.));
#146571=CARTESIAN_POINT('Ctrl Pts',(-70.735114793895,7.39433604117894,0.));
#146572=CARTESIAN_POINT('Ctrl Pts',(-70.7147984363423,7.3853368188703,0.));
#146573=CARTESIAN_POINT('Ctrl Pts',(-70.6945157248269,7.37637713374763,
0.));
#146574=CARTESIAN_POINT('Ctrl Pts',(-70.6742668209685,7.36745697876297,
0.));
#146575=CARTESIAN_POINT('Ctrl Pts',(-70.6540518871772,7.35857634673054,
0.));
#146576=CARTESIAN_POINT('Ctrl Pts',(-70.6338710866562,7.34973523032583,
0.));
#146577=CARTESIAN_POINT('Ctrl Pts',(-70.6137245834002,7.3409336220802,0.));
#146578=CARTESIAN_POINT('Ctrl Pts',(-70.5936125421958,7.3321715143761,0.));
#146579=CARTESIAN_POINT('Ctrl Pts',(-70.573535128649,7.3234488994524,0.));
#146580=CARTESIAN_POINT('Ctrl Pts',(-70.5534925092052,7.31476576940406,
0.));
#146581=CARTESIAN_POINT('Ctrl Pts',(-70.5334848511675,7.30612211618049,
0.));
#146582=CARTESIAN_POINT('Ctrl Pts',(-70.5135123227147,7.29751793157804,
0.));
#146583=CARTESIAN_POINT('Ctrl Pts',(-70.4935750929029,7.28895320723838,
0.));
#146584=CARTESIAN_POINT('Ctrl Pts',(-70.4736733316463,7.28042793465452,
0.));
#146585=CARTESIAN_POINT('Ctrl Pts',(-70.4538072096986,7.2719421051706,0.));
#146586=CARTESIAN_POINT('Ctrl Pts',(-70.433976898636,7.26349570998052,0.));
#146587=CARTESIAN_POINT('Ctrl Pts',(-70.4141825708207,7.25508874012078,
0.));
#146588=CARTESIAN_POINT('Ctrl Pts',(-70.3944243994532,7.24672118647119,
0.));
#146589=CARTESIAN_POINT('Ctrl Pts',(-70.3747025586569,7.23839303975629,
0.));
#146590=CARTESIAN_POINT('Ctrl Pts',(-70.3550172235486,7.23010429054233,
0.));
#146591=CARTESIAN_POINT('Ctrl Pts',(-70.3353685703097,7.2218549292318,0.));
#146592=CARTESIAN_POINT('Ctrl Pts',(-70.3157567762561,7.21364494605427,
0.));
#146593=CARTESIAN_POINT('Ctrl Pts',(-70.2961820197051,7.2054743310746,0.));
#146594=CARTESIAN_POINT('Ctrl Pts',(-70.276644479827,7.19734307419863,0.));
#146595=CARTESIAN_POINT('Ctrl Pts',(-70.2571443365198,7.18925116517565,
0.));
#146596=CARTESIAN_POINT('Ctrl Pts',(-70.2376817702239,7.18119859359803,
0.));
#146597=CARTESIAN_POINT('Ctrl Pts',(-70.2182569619028,7.1731853488975,0.));
#146598=CARTESIAN_POINT('Ctrl Pts',(-70.1988700934622,7.16521142033895,
0.));
#146599=CARTESIAN_POINT('Ctrl Pts',(-70.1795213481196,7.15727679700949,
0.));
#146600=CARTESIAN_POINT('Ctrl Pts',(-70.1602109107188,7.14938146780804,
0.));
#146601=CARTESIAN_POINT('Ctrl Pts',(-70.1409389682389,7.14152542142342,
0.));
#146602=CARTESIAN_POINT('Ctrl Pts',(-70.1217057094456,7.13370864634401,
0.));
#146603=CARTESIAN_POINT('Ctrl Pts',(-70.1025113239463,7.12593113088873,
0.));
#146604=CARTESIAN_POINT('Ctrl Pts',(-70.0833560013971,7.11819286322826,
0.));
#146605=CARTESIAN_POINT('Ctrl Pts',(-70.06423993069,7.11049383140484,0.));
#146606=CARTESIAN_POINT('Ctrl Pts',(-70.0451632990136,7.10283402335094,
0.));
#146607=CARTESIAN_POINT('Ctrl Pts',(-70.0261262936435,7.09521342684304,
0.));
#146608=CARTESIAN_POINT('Ctrl Pts',(-70.0071291040791,7.08763202944276,
0.));
#146609=CARTESIAN_POINT('Ctrl Pts',(-69.988171923787,7.08008981844645,0.));
#146610=CARTESIAN_POINT('Ctrl Pts',(-69.9692549527256,7.07258678080795,
0.));
#146611=CARTESIAN_POINT('Ctrl Pts',(-69.9503783975676,7.06512290312805,
0.));
#146612=CARTESIAN_POINT('Ctrl Pts',(-69.9315424664252,7.05769817180827,
0.));
#146613=CARTESIAN_POINT('Ctrl Pts',(-69.9127473642086,7.0503125731811,0.));
#146614=CARTESIAN_POINT('Ctrl Pts',(-69.8939932885864,7.04296609362189,
0.));
#146615=CARTESIAN_POINT('Ctrl Pts',(-69.8752804235296,7.03565871972267,
0.));
#146616=CARTESIAN_POINT('Ctrl Pts',(-69.8566089455448,7.02839043811865,
0.));
#146617=CARTESIAN_POINT('Ctrl Pts',(-69.8379790360574,7.02116123514489,
0.));
#146618=CARTESIAN_POINT('Ctrl Pts',(-69.8193908913722,7.01397109655458,
0.));
#146619=CARTESIAN_POINT('Ctrl Pts',(-69.8008447346782,7.00682000718107,
0.));
#146620=CARTESIAN_POINT('Ctrl Pts',(-69.7823408242446,6.99970795069402,
0.));
#146621=CARTESIAN_POINT('Ctrl Pts',(-69.7638794280263,6.99263491027862,
0.));
#146622=CARTESIAN_POINT('Ctrl Pts',(-69.7454607995524,6.98560086924175,
0.));
#146623=CARTESIAN_POINT('Ctrl Pts',(-69.7270851557443,6.97860581164571,
0.));
#146624=CARTESIAN_POINT('Ctrl Pts',(-69.7087526480248,6.97164972291584,
0.));
#146625=CARTESIAN_POINT('Ctrl Pts',(-69.6904633605834,6.96473259049732,
0.));
#146626=CARTESIAN_POINT('Ctrl Pts',(-69.6758665380764,6.95923004173798,
0.));
#146627=CARTESIAN_POINT('Ctrl Pts',(-69.6649383920075,6.95512065317733,
0.));
#146628=CARTESIAN_POINT('Ctrl Pts',(-69.6576616146559,6.95238884849078,
0.));
#146629=CARTESIAN_POINT('Ctrl Pts',(-69.6540253893193,6.9510248930693,0.));
#146630=CARTESIAN_POINT('Ctrl Pts',(-72.8667204369977,15.5142209845169,
0.));
#146631=CARTESIAN_POINT('Ctrl Pts',(-72.8667204369977,15.5142209845169,
12.));
#146632=CARTESIAN_POINT('Ctrl Pts',(-72.8622377860957,15.5108715869174,
0.));
#146633=CARTESIAN_POINT('Ctrl Pts',(-72.8622377860957,15.5108715869174,
12.));
#146634=CARTESIAN_POINT('Ctrl Pts',(-72.8532737732123,15.5041768664089,
0.));
#146635=CARTESIAN_POINT('Ctrl Pts',(-72.8532737732123,15.5041768664089,
12.));
#146636=CARTESIAN_POINT('Ctrl Pts',(-72.8398316206501,15.494147009717,0.));
#146637=CARTESIAN_POINT('Ctrl Pts',(-72.8398316206501,15.494147009717,12.));
#146638=CARTESIAN_POINT('Ctrl Pts',(-72.8219164844002,15.4807983165984,
0.));
#146639=CARTESIAN_POINT('Ctrl Pts',(-72.8219164844002,15.4807983165984,
12.));
#146640=CARTESIAN_POINT('Ctrl Pts',(-72.7995354604414,15.4641532053436,
0.));
#146641=CARTESIAN_POINT('Ctrl Pts',(-72.7995354604414,15.4641532053436,
12.));
#146642=CARTESIAN_POINT('Ctrl Pts',(-72.7771673494582,15.4475488590336,
0.));
#146643=CARTESIAN_POINT('Ctrl Pts',(-72.7771673494582,15.4475488590336,
12.));
#146644=CARTESIAN_POINT('Ctrl Pts',(-72.7548121825431,15.4309852897867,
0.));
#146645=CARTESIAN_POINT('Ctrl Pts',(-72.7548121825431,15.4309852897867,
12.));
#146646=CARTESIAN_POINT('Ctrl Pts',(-72.7324700089576,15.4144625111911,
0.));
#146647=CARTESIAN_POINT('Ctrl Pts',(-72.7324700089576,15.4144625111911,
12.));
#146648=CARTESIAN_POINT('Ctrl Pts',(-72.710140901746,15.397980537311,0.));
#146649=CARTESIAN_POINT('Ctrl Pts',(-72.710140901746,15.397980537311,12.));
#146650=CARTESIAN_POINT('Ctrl Pts',(-72.6878249557452,15.381539382267,0.));
#146651=CARTESIAN_POINT('Ctrl Pts',(-72.6878249557452,15.381539382267,12.));
#146652=CARTESIAN_POINT('Ctrl Pts',(-72.6655222797603,15.3651390602616,
0.));
#146653=CARTESIAN_POINT('Ctrl Pts',(-72.6655222797603,15.3651390602616,
12.));
#146654=CARTESIAN_POINT('Ctrl Pts',(-72.6432329903466,15.3487795854724,
0.));
#146655=CARTESIAN_POINT('Ctrl Pts',(-72.6432329903466,15.3487795854724,
12.));
#146656=CARTESIAN_POINT('Ctrl Pts',(-72.6209572051064,15.3324609719961,
0.));
#146657=CARTESIAN_POINT('Ctrl Pts',(-72.6209572051064,15.3324609719961,
12.));
#146658=CARTESIAN_POINT('Ctrl Pts',(-72.5986950357771,15.3161832337618,
0.));
#146659=CARTESIAN_POINT('Ctrl Pts',(-72.5986950357771,15.3161832337618,
12.));
#146660=CARTESIAN_POINT('Ctrl Pts',(-72.5764465826345,15.2999463844691,
0.));
#146661=CARTESIAN_POINT('Ctrl Pts',(-72.5764465826345,15.2999463844691,
12.));
#146662=CARTESIAN_POINT('Ctrl Pts',(-72.5542119383748,15.2837504376562,
0.));
#146663=CARTESIAN_POINT('Ctrl Pts',(-72.5542119383748,15.2837504376562,
12.));
#146664=CARTESIAN_POINT('Ctrl Pts',(-72.5319911908978,15.2675954067495,
0.));
#146665=CARTESIAN_POINT('Ctrl Pts',(-72.5319911908978,15.2675954067495,
12.));
#146666=CARTESIAN_POINT('Ctrl Pts',(-72.5097844266083,15.2514813051174,
0.));
#146667=CARTESIAN_POINT('Ctrl Pts',(-72.5097844266083,15.2514813051174,
12.));
#146668=CARTESIAN_POINT('Ctrl Pts',(-72.4875917332729,15.2354081461152,
0.));
#146669=CARTESIAN_POINT('Ctrl Pts',(-72.4875917332729,15.2354081461152,
12.));
#146670=CARTESIAN_POINT('Ctrl Pts',(-72.4654132036373,15.2193759431359,
0.));
#146671=CARTESIAN_POINT('Ctrl Pts',(-72.4654132036373,15.2193759431359,
12.));
#146672=CARTESIAN_POINT('Ctrl Pts',(-72.4432489350415,15.2033847096077,
0.));
#146673=CARTESIAN_POINT('Ctrl Pts',(-72.4432489350415,15.2033847096077,
12.));
#146674=CARTESIAN_POINT('Ctrl Pts',(-72.4210990277819,15.1874344589716,
0.));
#146675=CARTESIAN_POINT('Ctrl Pts',(-72.4210990277819,15.1874344589716,
12.));
#146676=CARTESIAN_POINT('Ctrl Pts',(-72.3989635838476,15.1715252046603,
0.));
#146677=CARTESIAN_POINT('Ctrl Pts',(-72.3989635838476,15.1715252046603,
12.));
#146678=CARTESIAN_POINT('Ctrl Pts',(-72.37684270559,15.1556569600747,0.));
#146679=CARTESIAN_POINT('Ctrl Pts',(-72.37684270559,15.1556569600747,12.));
#146680=CARTESIAN_POINT('Ctrl Pts',(-72.3547364941996,15.1398297385513,
0.));
#146681=CARTESIAN_POINT('Ctrl Pts',(-72.3547364941996,15.1398297385513,
12.));
#146682=CARTESIAN_POINT('Ctrl Pts',(-72.332645049021,15.1240435533478,0.));
#146683=CARTESIAN_POINT('Ctrl Pts',(-72.332645049021,15.1240435533478,12.));
#146684=CARTESIAN_POINT('Ctrl Pts',(-72.3105684683971,15.1082984176656,
0.));
#146685=CARTESIAN_POINT('Ctrl Pts',(-72.3105684683971,15.1082984176656,
12.));
#146686=CARTESIAN_POINT('Ctrl Pts',(-72.2885068501641,15.0925943446593,
0.));
#146687=CARTESIAN_POINT('Ctrl Pts',(-72.2885068501641,15.0925943446593,
12.));
#146688=CARTESIAN_POINT('Ctrl Pts',(-72.266460292285,15.0769313474476,0.));
#146689=CARTESIAN_POINT('Ctrl Pts',(-72.266460292285,15.0769313474476,12.));
#146690=CARTESIAN_POINT('Ctrl Pts',(-72.244428893425,15.0613094391186,0.));
#146691=CARTESIAN_POINT('Ctrl Pts',(-72.244428893425,15.0613094391186,12.));
#146692=CARTESIAN_POINT('Ctrl Pts',(-72.2224127535401,15.0457286327328,
0.));
#146693=CARTESIAN_POINT('Ctrl Pts',(-72.2224127535401,15.0457286327328,
12.));
#146694=CARTESIAN_POINT('Ctrl Pts',(-72.2004119736104,15.0301889413255,
0.));
#146695=CARTESIAN_POINT('Ctrl Pts',(-72.2004119736104,15.0301889413255,
12.));
#146696=CARTESIAN_POINT('Ctrl Pts',(-72.1784266553948,15.0146903779061,
0.));
#146697=CARTESIAN_POINT('Ctrl Pts',(-72.1784266553948,15.0146903779061,
12.));
#146698=CARTESIAN_POINT('Ctrl Pts',(-72.1564569011668,14.9992329554537,
0.));
#146699=CARTESIAN_POINT('Ctrl Pts',(-72.1564569011668,14.9992329554537,
12.));
#146700=CARTESIAN_POINT('Ctrl Pts',(-72.1345028134779,14.9838166869107,
0.));
#146701=CARTESIAN_POINT('Ctrl Pts',(-72.1345028134779,14.9838166869107,
12.));
#146702=CARTESIAN_POINT('Ctrl Pts',(-72.1125644948547,14.96844158517,0.));
#146703=CARTESIAN_POINT('Ctrl Pts',(-72.1125644948547,14.96844158517,12.));
#146704=CARTESIAN_POINT('Ctrl Pts',(-72.0906420478085,14.953107663077,0.));
#146705=CARTESIAN_POINT('Ctrl Pts',(-72.0906420478085,14.953107663077,12.));
#146706=CARTESIAN_POINT('Ctrl Pts',(-72.0687355749815,14.937814933439,0.));
#146707=CARTESIAN_POINT('Ctrl Pts',(-72.0687355749815,14.937814933439,12.));
#146708=CARTESIAN_POINT('Ctrl Pts',(-72.046845179251,14.9225634090269,0.));
#146709=CARTESIAN_POINT('Ctrl Pts',(-72.046845179251,14.9225634090269,12.));
#146710=CARTESIAN_POINT('Ctrl Pts',(-72.0249709638419,14.9073531025764,
0.));
#146711=CARTESIAN_POINT('Ctrl Pts',(-72.0249709638419,14.9073531025764,
12.));
#146712=CARTESIAN_POINT('Ctrl Pts',(-72.0031130324519,14.892184026783,0.));
#146713=CARTESIAN_POINT('Ctrl Pts',(-72.0031130324519,14.892184026783,12.));
#146714=CARTESIAN_POINT('Ctrl Pts',(-71.9812714893087,14.8770561943011,
0.));
#146715=CARTESIAN_POINT('Ctrl Pts',(-71.9812714893087,14.8770561943011,
12.));
#146716=CARTESIAN_POINT('Ctrl Pts',(-71.9594464391063,14.8619696177503,
0.));
#146717=CARTESIAN_POINT('Ctrl Pts',(-71.9594464391063,14.8619696177503,
12.));
#146718=CARTESIAN_POINT('Ctrl Pts',(-71.9376379869668,14.846924309716,0.));
#146719=CARTESIAN_POINT('Ctrl Pts',(-71.9376379869668,14.846924309716,12.));
#146720=CARTESIAN_POINT('Ctrl Pts',(-71.9158462383915,14.8319202827483,
0.));
#146721=CARTESIAN_POINT('Ctrl Pts',(-71.9158462383915,14.8319202827483,
12.));
#146722=CARTESIAN_POINT('Ctrl Pts',(-71.8940712992119,14.816957549356,0.));
#146723=CARTESIAN_POINT('Ctrl Pts',(-71.8940712992119,14.816957549356,12.));
#146724=CARTESIAN_POINT('Ctrl Pts',(-71.872313275546,14.8020361220003,0.));
#146725=CARTESIAN_POINT('Ctrl Pts',(-71.872313275546,14.8020361220003,12.));
#146726=CARTESIAN_POINT('Ctrl Pts',(-71.8505722738286,14.7871560131021,
0.));
#146727=CARTESIAN_POINT('Ctrl Pts',(-71.8505722738286,14.7871560131021,
12.));
#146728=CARTESIAN_POINT('Ctrl Pts',(-71.8288484008343,14.7723172350455,
0.));
#146729=CARTESIAN_POINT('Ctrl Pts',(-71.8288484008343,14.7723172350455,
12.));
#146730=CARTESIAN_POINT('Ctrl Pts',(-71.8071417637018,14.7575198001777,
0.));
#146731=CARTESIAN_POINT('Ctrl Pts',(-71.8071417637018,14.7575198001777,
12.));
#146732=CARTESIAN_POINT('Ctrl Pts',(-71.7854524699562,14.7427637208071,
0.));
#146733=CARTESIAN_POINT('Ctrl Pts',(-71.7854524699562,14.7427637208071,
12.));
#146734=CARTESIAN_POINT('Ctrl Pts',(-71.7637806275316,14.7280490091954,
0.));
#146735=CARTESIAN_POINT('Ctrl Pts',(-71.7637806275316,14.7280490091954,
12.));
#146736=CARTESIAN_POINT('Ctrl Pts',(-71.7421263447707,14.7133756775622,
0.));
#146737=CARTESIAN_POINT('Ctrl Pts',(-71.7421263447707,14.7133756775622,
12.));
#146738=CARTESIAN_POINT('Ctrl Pts',(-71.7204897304186,14.6987437380898,
0.));
#146739=CARTESIAN_POINT('Ctrl Pts',(-71.7204897304186,14.6987437380898,
12.));
#146740=CARTESIAN_POINT('Ctrl Pts',(-71.698870893617,14.6841532029232,0.));
#146741=CARTESIAN_POINT('Ctrl Pts',(-71.698870893617,14.6841532029232,12.));
#146742=CARTESIAN_POINT('Ctrl Pts',(-71.6772699438966,14.669604084168,0.));
#146743=CARTESIAN_POINT('Ctrl Pts',(-71.6772699438966,14.669604084168,12.));
#146744=CARTESIAN_POINT('Ctrl Pts',(-71.6556869911669,14.6550963938832,
0.));
#146745=CARTESIAN_POINT('Ctrl Pts',(-71.6556869911669,14.6550963938832,
12.));
#146746=CARTESIAN_POINT('Ctrl Pts',(-71.6341221457175,14.6406301440817,
0.));
#146747=CARTESIAN_POINT('Ctrl Pts',(-71.6341221457175,14.6406301440817,
12.));
#146748=CARTESIAN_POINT('Ctrl Pts',(-71.6125755182295,14.6262053467372,
0.));
#146749=CARTESIAN_POINT('Ctrl Pts',(-71.6125755182295,14.6262053467372,
12.));
#146750=CARTESIAN_POINT('Ctrl Pts',(-71.5910472197814,14.611822013785,0.));
#146751=CARTESIAN_POINT('Ctrl Pts',(-71.5910472197814,14.611822013785,12.));
#146752=CARTESIAN_POINT('Ctrl Pts',(-71.569537361856,14.597480157121,0.));
#146753=CARTESIAN_POINT('Ctrl Pts',(-71.569537361856,14.597480157121,12.));
#146754=CARTESIAN_POINT('Ctrl Pts',(-71.5480460563445,14.5831797885951,
0.));
#146755=CARTESIAN_POINT('Ctrl Pts',(-71.5480460563445,14.5831797885951,
12.));
#146756=CARTESIAN_POINT('Ctrl Pts',(-71.52657341555,14.5689209200091,0.));
#146757=CARTESIAN_POINT('Ctrl Pts',(-71.52657341555,14.5689209200091,12.));
#146758=CARTESIAN_POINT('Ctrl Pts',(-71.5051195521914,14.5547035631234,
0.));
#146759=CARTESIAN_POINT('Ctrl Pts',(-71.5051195521914,14.5547035631234,
12.));
#146760=CARTESIAN_POINT('Ctrl Pts',(-71.4836845794052,14.540527729659,0.));
#146761=CARTESIAN_POINT('Ctrl Pts',(-71.4836845794052,14.540527729659,12.));
#146762=CARTESIAN_POINT('Ctrl Pts',(-71.4622686107475,14.5263934312969,
0.));
#146763=CARTESIAN_POINT('Ctrl Pts',(-71.4622686107475,14.5263934312969,
12.));
#146764=CARTESIAN_POINT('Ctrl Pts',(-71.4408717601917,14.5123006796728,
0.));
#146765=CARTESIAN_POINT('Ctrl Pts',(-71.4408717601917,14.5123006796728,
12.));
#146766=CARTESIAN_POINT('Ctrl Pts',(-71.4194941421279,14.4982494863716,
0.));
#146767=CARTESIAN_POINT('Ctrl Pts',(-71.4194941421279,14.4982494863716,
12.));
#146768=CARTESIAN_POINT('Ctrl Pts',(-71.398135871371,14.4842398629354,0.));
#146769=CARTESIAN_POINT('Ctrl Pts',(-71.398135871371,14.4842398629354,12.));
#146770=CARTESIAN_POINT('Ctrl Pts',(-71.3767970631642,14.470271820865,0.));
#146771=CARTESIAN_POINT('Ctrl Pts',(-71.3767970631642,14.470271820865,12.));
#146772=CARTESIAN_POINT('Ctrl Pts',(-71.3554778331835,14.4563453716204,
0.));
#146773=CARTESIAN_POINT('Ctrl Pts',(-71.3554778331835,14.4563453716204,
12.));
#146774=CARTESIAN_POINT('Ctrl Pts',(-71.3341782975393,14.4424605266167,
0.));
#146775=CARTESIAN_POINT('Ctrl Pts',(-71.3341782975393,14.4424605266167,
12.));
#146776=CARTESIAN_POINT('Ctrl Pts',(-71.3128985727777,14.4286172972168,
0.));
#146777=CARTESIAN_POINT('Ctrl Pts',(-71.3128985727777,14.4286172972168,
12.));
#146778=CARTESIAN_POINT('Ctrl Pts',(-71.2916387758864,14.4148156947384,
0.));
#146779=CARTESIAN_POINT('Ctrl Pts',(-71.2916387758864,14.4148156947384,
12.));
#146780=CARTESIAN_POINT('Ctrl Pts',(-71.2703990242986,14.401055730457,0.));
#146781=CARTESIAN_POINT('Ctrl Pts',(-71.2703990242986,14.401055730457,12.));
#146782=CARTESIAN_POINT('Ctrl Pts',(-71.2491794358956,14.3873374156056,
0.));
#146783=CARTESIAN_POINT('Ctrl Pts',(-71.2491794358956,14.3873374156056,
12.));
#146784=CARTESIAN_POINT('Ctrl Pts',(-71.2279801290088,14.3736607613723,
0.));
#146785=CARTESIAN_POINT('Ctrl Pts',(-71.2279801290088,14.3736607613723,
12.));
#146786=CARTESIAN_POINT('Ctrl Pts',(-71.2068012224187,14.3600257788927,
0.));
#146787=CARTESIAN_POINT('Ctrl Pts',(-71.2068012224187,14.3600257788927,
12.));
#146788=CARTESIAN_POINT('Ctrl Pts',(-71.185642835361,14.3464324792537,0.));
#146789=CARTESIAN_POINT('Ctrl Pts',(-71.185642835361,14.3464324792537,12.));
#146790=CARTESIAN_POINT('Ctrl Pts',(-71.1645050875323,14.3328808734993,
0.));
#146791=CARTESIAN_POINT('Ctrl Pts',(-71.1645050875323,14.3328808734993,
12.));
#146792=CARTESIAN_POINT('Ctrl Pts',(-71.1433880990932,14.3193709726295,
0.));
#146793=CARTESIAN_POINT('Ctrl Pts',(-71.1433880990932,14.3193709726295,
12.));
#146794=CARTESIAN_POINT('Ctrl Pts',(-71.1222919906718,14.3059027875993,
0.));
#146795=CARTESIAN_POINT('Ctrl Pts',(-71.1222919906718,14.3059027875993,
12.));
#146796=CARTESIAN_POINT('Ctrl Pts',(-71.1012168833626,14.2924763293101,
0.));
#146797=CARTESIAN_POINT('Ctrl Pts',(-71.1012168833626,14.2924763293101,
12.));
#146798=CARTESIAN_POINT('Ctrl Pts',(-71.0801628987314,14.279091608613,0.));
#146799=CARTESIAN_POINT('Ctrl Pts',(-71.0801628987314,14.279091608613,12.));
#146800=CARTESIAN_POINT('Ctrl Pts',(-71.059130158822,14.2657486363137,0.));
#146801=CARTESIAN_POINT('Ctrl Pts',(-71.059130158822,14.2657486363137,12.));
#146802=CARTESIAN_POINT('Ctrl Pts',(-71.0381187861585,14.2524474231732,
0.));
#146803=CARTESIAN_POINT('Ctrl Pts',(-71.0381187861585,14.2524474231732,
12.));
#146804=CARTESIAN_POINT('Ctrl Pts',(-71.0171289037493,14.2391879799063,
0.));
#146805=CARTESIAN_POINT('Ctrl Pts',(-71.0171289037493,14.2391879799063,
12.));
#146806=CARTESIAN_POINT('Ctrl Pts',(-70.996160635087,14.2259703171739,0.));
#146807=CARTESIAN_POINT('Ctrl Pts',(-70.996160635087,14.2259703171739,12.));
#146808=CARTESIAN_POINT('Ctrl Pts',(-70.9752141041527,14.2127944455841,
0.));
#146809=CARTESIAN_POINT('Ctrl Pts',(-70.9752141041527,14.2127944455841,
12.));
#146810=CARTESIAN_POINT('Ctrl Pts',(-70.9542894354221,14.1996603756984,
0.));
#146811=CARTESIAN_POINT('Ctrl Pts',(-70.9542894354221,14.1996603756984,
12.));
#146812=CARTESIAN_POINT('Ctrl Pts',(-70.9333867538704,14.1865681180321,
0.));
#146813=CARTESIAN_POINT('Ctrl Pts',(-70.9333867538704,14.1865681180321,
12.));
#146814=CARTESIAN_POINT('Ctrl Pts',(-70.9125061849744,14.1735176830533,
0.));
#146815=CARTESIAN_POINT('Ctrl Pts',(-70.9125061849744,14.1735176830533,
12.));
#146816=CARTESIAN_POINT('Ctrl Pts',(-70.8916478547131,14.1605090811754,
0.));
#146817=CARTESIAN_POINT('Ctrl Pts',(-70.8916478547131,14.1605090811754,
12.));
#146818=CARTESIAN_POINT('Ctrl Pts',(-70.8708118895717,14.1475423227568,
0.));
#146819=CARTESIAN_POINT('Ctrl Pts',(-70.8708118895717,14.1475423227568,
12.));
#146820=CARTESIAN_POINT('Ctrl Pts',(-70.8499984165493,14.1346174181079,
0.));
#146821=CARTESIAN_POINT('Ctrl Pts',(-70.8499984165493,14.1346174181079,
12.));
#146822=CARTESIAN_POINT('Ctrl Pts',(-70.8292075631624,14.1217343774914,
0.));
#146823=CARTESIAN_POINT('Ctrl Pts',(-70.8292075631624,14.1217343774914,
12.));
#146824=CARTESIAN_POINT('Ctrl Pts',(-70.8084394574491,14.1088932111215,
0.));
#146825=CARTESIAN_POINT('Ctrl Pts',(-70.8084394574491,14.1088932111215,
12.));
#146826=CARTESIAN_POINT('Ctrl Pts',(-70.787694227969,14.0960939291569,0.));
#146827=CARTESIAN_POINT('Ctrl Pts',(-70.787694227969,14.0960939291569,12.));
#146828=CARTESIAN_POINT('Ctrl Pts',(-70.7669720038067,14.0833365416995,
0.));
#146829=CARTESIAN_POINT('Ctrl Pts',(-70.7669720038067,14.0833365416995,
12.));
#146830=CARTESIAN_POINT('Ctrl Pts',(-70.7462729145799,14.0706210588015,
0.));
#146831=CARTESIAN_POINT('Ctrl Pts',(-70.7462729145799,14.0706210588015,
12.));
#146832=CARTESIAN_POINT('Ctrl Pts',(-70.7255970904433,14.0579474904657,
0.));
#146833=CARTESIAN_POINT('Ctrl Pts',(-70.7255970904433,14.0579474904657,
12.));
#146834=CARTESIAN_POINT('Ctrl Pts',(-70.7049446620931,14.0453158466451,
0.));
#146835=CARTESIAN_POINT('Ctrl Pts',(-70.7049446620931,14.0453158466451,
12.));
#146836=CARTESIAN_POINT('Ctrl Pts',(-70.6843157607672,14.0327261372363,
0.));
#146837=CARTESIAN_POINT('Ctrl Pts',(-70.6843157607672,14.0327261372363,
12.));
#146838=CARTESIAN_POINT('Ctrl Pts',(-70.6637105182487,14.020178372077,0.));
#146839=CARTESIAN_POINT('Ctrl Pts',(-70.6637105182487,14.020178372077,12.));
#146840=CARTESIAN_POINT('Ctrl Pts',(-70.6431290668744,14.0076725609537,
0.));
#146841=CARTESIAN_POINT('Ctrl Pts',(-70.6431290668744,14.0076725609537,
12.));
#146842=CARTESIAN_POINT('Ctrl Pts',(-70.6225715395392,13.9952087136018,
0.));
#146843=CARTESIAN_POINT('Ctrl Pts',(-70.6225715395392,13.9952087136018,
12.));
#146844=CARTESIAN_POINT('Ctrl Pts',(-70.6020380697004,13.9827868397057,
0.));
#146845=CARTESIAN_POINT('Ctrl Pts',(-70.6020380697004,13.9827868397057,
12.));
#146846=CARTESIAN_POINT('Ctrl Pts',(-70.5815287913791,13.9704069488918,
0.));
#146847=CARTESIAN_POINT('Ctrl Pts',(-70.5815287913791,13.9704069488918,
12.));
#146848=CARTESIAN_POINT('Ctrl Pts',(-70.5610438391622,13.9580690507262,
0.));
#146849=CARTESIAN_POINT('Ctrl Pts',(-70.5610438391622,13.9580690507262,
12.));
#146850=CARTESIAN_POINT('Ctrl Pts',(-70.5405833482123,13.9457731547218,
0.));
#146851=CARTESIAN_POINT('Ctrl Pts',(-70.5405833482123,13.9457731547218,
12.));
#146852=CARTESIAN_POINT('Ctrl Pts',(-70.5201474542717,13.933519270339,0.));
#146853=CARTESIAN_POINT('Ctrl Pts',(-70.5201474542717,13.933519270339,12.));
#146854=CARTESIAN_POINT('Ctrl Pts',(-70.4997362936671,13.9213074069852,
0.));
#146855=CARTESIAN_POINT('Ctrl Pts',(-70.4997362936671,13.9213074069852,
12.));
#146856=CARTESIAN_POINT('Ctrl Pts',(-70.4793500033106,13.9091375740085,
0.));
#146857=CARTESIAN_POINT('Ctrl Pts',(-70.4793500033106,13.9091375740085,
12.));
#146858=CARTESIAN_POINT('Ctrl Pts',(-70.4589887207043,13.8970097806948,
0.));
#146859=CARTESIAN_POINT('Ctrl Pts',(-70.4589887207043,13.8970097806948,
12.));
#146860=CARTESIAN_POINT('Ctrl Pts',(-70.4386525839492,13.8849240362757,
0.));
#146861=CARTESIAN_POINT('Ctrl Pts',(-70.4386525839492,13.8849240362757,
12.));
#146862=CARTESIAN_POINT('Ctrl Pts',(-70.4183417317486,13.8728803499284,
0.));
#146863=CARTESIAN_POINT('Ctrl Pts',(-70.4183417317486,13.8728803499284,
12.));
#146864=CARTESIAN_POINT('Ctrl Pts',(-70.3980563034142,13.8608787307754,
0.));
#146865=CARTESIAN_POINT('Ctrl Pts',(-70.3980563034142,13.8608787307754,
12.));
#146866=CARTESIAN_POINT('Ctrl Pts',(-70.377796438866,13.8489191878774,0.));
#146867=CARTESIAN_POINT('Ctrl Pts',(-70.377796438866,13.8489191878774,12.));
#146868=CARTESIAN_POINT('Ctrl Pts',(-70.3575622786373,13.8370017302319,
0.));
#146869=CARTESIAN_POINT('Ctrl Pts',(-70.3575622786373,13.8370017302319,
12.));
#146870=CARTESIAN_POINT('Ctrl Pts',(-70.3373539638841,13.8251263667799,
0.));
#146871=CARTESIAN_POINT('Ctrl Pts',(-70.3373539638841,13.8251263667799,
12.));
#146872=CARTESIAN_POINT('Ctrl Pts',(-70.3171716363912,13.8132931064067,
0.));
#146873=CARTESIAN_POINT('Ctrl Pts',(-70.3171716363912,13.8132931064067,
12.));
#146874=CARTESIAN_POINT('Ctrl Pts',(-70.2970154385763,13.8015019579411,
0.));
#146875=CARTESIAN_POINT('Ctrl Pts',(-70.2970154385763,13.8015019579411,
12.));
#146876=CARTESIAN_POINT('Ctrl Pts',(-70.2768855134909,13.7897529301483,
0.));
#146877=CARTESIAN_POINT('Ctrl Pts',(-70.2768855134909,13.7897529301483,
12.));
#146878=CARTESIAN_POINT('Ctrl Pts',(-70.2567820048253,13.7780460317284,
0.));
#146879=CARTESIAN_POINT('Ctrl Pts',(-70.2567820048253,13.7780460317284,
12.));
#146880=CARTESIAN_POINT('Ctrl Pts',(-70.2367050569174,13.7663812713235,
0.));
#146881=CARTESIAN_POINT('Ctrl Pts',(-70.2367050569174,13.7663812713235,
12.));
#146882=CARTESIAN_POINT('Ctrl Pts',(-70.216654814759,13.7547586575178,0.));
#146883=CARTESIAN_POINT('Ctrl Pts',(-70.216654814759,13.7547586575178,12.));
#146884=CARTESIAN_POINT('Ctrl Pts',(-70.1966314240012,13.7431781988368,
0.));
#146885=CARTESIAN_POINT('Ctrl Pts',(-70.1966314240012,13.7431781988368,
12.));
#146886=CARTESIAN_POINT('Ctrl Pts',(-70.1766350309554,13.73163990374,0.));
#146887=CARTESIAN_POINT('Ctrl Pts',(-70.1766350309554,13.73163990374,12.));
#146888=CARTESIAN_POINT('Ctrl Pts',(-70.1566657825989,13.7201437806207,
0.));
#146889=CARTESIAN_POINT('Ctrl Pts',(-70.1566657825989,13.7201437806207,
12.));
#146890=CARTESIAN_POINT('Ctrl Pts',(-70.1367238265853,13.7086898378127,
0.));
#146891=CARTESIAN_POINT('Ctrl Pts',(-70.1367238265853,13.7086898378127,
12.));
#146892=CARTESIAN_POINT('Ctrl Pts',(-70.1168093112493,13.6972780835899,
0.));
#146893=CARTESIAN_POINT('Ctrl Pts',(-70.1168093112493,13.6972780835899,
12.));
#146894=CARTESIAN_POINT('Ctrl Pts',(-70.0969223856123,13.6859085261651,
0.));
#146895=CARTESIAN_POINT('Ctrl Pts',(-70.0969223856123,13.6859085261651,
12.));
#146896=CARTESIAN_POINT('Ctrl Pts',(-70.0770631993831,13.6745811736825,
0.));
#146897=CARTESIAN_POINT('Ctrl Pts',(-70.0770631993831,13.6745811736825,
12.));
#146898=CARTESIAN_POINT('Ctrl Pts',(-70.057231902965,13.6632960342192,0.));
#146899=CARTESIAN_POINT('Ctrl Pts',(-70.057231902965,13.6632960342192,12.));
#146900=CARTESIAN_POINT('Ctrl Pts',(-70.037428647466,13.6520531157904,0.));
#146901=CARTESIAN_POINT('Ctrl Pts',(-70.037428647466,13.6520531157904,12.));
#146902=CARTESIAN_POINT('Ctrl Pts',(-70.0176535847047,13.6408524263496,
0.));
#146903=CARTESIAN_POINT('Ctrl Pts',(-70.0176535847047,13.6408524263496,
12.));
#146904=CARTESIAN_POINT('Ctrl Pts',(-69.9979068672163,13.6296939737866,
0.));
#146905=CARTESIAN_POINT('Ctrl Pts',(-69.9979068672163,13.6296939737866,
12.));
#146906=CARTESIAN_POINT('Ctrl Pts',(-69.9781886482543,13.61857776592,0.));
#146907=CARTESIAN_POINT('Ctrl Pts',(-69.9781886482543,13.61857776592,12.));
#146908=CARTESIAN_POINT('Ctrl Pts',(-69.9584990817989,13.6075038105001,
0.));
#146909=CARTESIAN_POINT('Ctrl Pts',(-69.9584990817989,13.6075038105001,
12.));
#146910=CARTESIAN_POINT('Ctrl Pts',(-69.9388383225655,13.5964721152136,
0.));
#146911=CARTESIAN_POINT('Ctrl Pts',(-69.9388383225655,13.5964721152136,
12.));
#146912=CARTESIAN_POINT('Ctrl Pts',(-69.9192065260107,13.5854826876834,
0.));
#146913=CARTESIAN_POINT('Ctrl Pts',(-69.9192065260107,13.5854826876834,
12.));
#146914=CARTESIAN_POINT('Ctrl Pts',(-69.899603848336,13.5745355354657,0.));
#146915=CARTESIAN_POINT('Ctrl Pts',(-69.899603848336,13.5745355354657,12.));
#146916=CARTESIAN_POINT('Ctrl Pts',(-69.880030446488,13.5636306660423,0.));
#146917=CARTESIAN_POINT('Ctrl Pts',(-69.880030446488,13.5636306660423,12.));
#146918=CARTESIAN_POINT('Ctrl Pts',(-69.8604864781705,13.5527680868256,
0.));
#146919=CARTESIAN_POINT('Ctrl Pts',(-69.8604864781705,13.5527680868256,
12.));
#146920=CARTESIAN_POINT('Ctrl Pts',(-69.840972101856,13.5419478051626,0.));
#146921=CARTESIAN_POINT('Ctrl Pts',(-69.840972101856,13.5419478051626,12.));
#146922=CARTESIAN_POINT('Ctrl Pts',(-69.8214874767944,13.5311698283339,
0.));
#146923=CARTESIAN_POINT('Ctrl Pts',(-69.8214874767944,13.5311698283339,
12.));
#146924=CARTESIAN_POINT('Ctrl Pts',(-69.8020327630204,13.5204341635507,
0.));
#146925=CARTESIAN_POINT('Ctrl Pts',(-69.8020327630204,13.5204341635507,
12.));
#146926=CARTESIAN_POINT('Ctrl Pts',(-69.7826081213575,13.5097408179479,
0.));
#146927=CARTESIAN_POINT('Ctrl Pts',(-69.7826081213575,13.5097408179479,
12.));
#146928=CARTESIAN_POINT('Ctrl Pts',(-69.7632137134247,13.4990897985904,
0.));
#146929=CARTESIAN_POINT('Ctrl Pts',(-69.7632137134247,13.4990897985904,
12.));
#146930=CARTESIAN_POINT('Ctrl Pts',(-69.7438497016404,13.4884811124748,
0.));
#146931=CARTESIAN_POINT('Ctrl Pts',(-69.7438497016404,13.4884811124748,
12.));
#146932=CARTESIAN_POINT('Ctrl Pts',(-69.7245162492251,13.4779147665286,
0.));
#146933=CARTESIAN_POINT('Ctrl Pts',(-69.7245162492251,13.4779147665286,
12.));
#146934=CARTESIAN_POINT('Ctrl Pts',(-69.7052135202003,13.4673907676045,
0.));
#146935=CARTESIAN_POINT('Ctrl Pts',(-69.7052135202003,13.4673907676045,
12.));
#146936=CARTESIAN_POINT('Ctrl Pts',(-69.6859416793898,13.4569091224763,
0.));
#146937=CARTESIAN_POINT('Ctrl Pts',(-69.6859416793898,13.4569091224763,
12.));
#146938=CARTESIAN_POINT('Ctrl Pts',(-69.6667008924454,13.4464698378456,
0.));
#146939=CARTESIAN_POINT('Ctrl Pts',(-69.6667008924454,13.4464698378456,
12.));
#146940=CARTESIAN_POINT('Ctrl Pts',(-69.6474913258684,13.4360729203444,
0.));
#146941=CARTESIAN_POINT('Ctrl Pts',(-69.6474913258684,13.4360729203444,
12.));
#146942=CARTESIAN_POINT('Ctrl Pts',(-69.6283131470267,13.425718376534,0.));
#146943=CARTESIAN_POINT('Ctrl Pts',(-69.6283131470267,13.425718376534,12.));
#146944=CARTESIAN_POINT('Ctrl Pts',(-69.6091665241743,13.4154062128998,
0.));
#146945=CARTESIAN_POINT('Ctrl Pts',(-69.6091665241743,13.4154062128998,
12.));
#146946=CARTESIAN_POINT('Ctrl Pts',(-69.5900516264524,13.4051364358495,
0.));
#146947=CARTESIAN_POINT('Ctrl Pts',(-69.5900516264524,13.4051364358495,
12.));
#146948=CARTESIAN_POINT('Ctrl Pts',(-69.5709686238701,13.3949090517173,
0.));
#146949=CARTESIAN_POINT('Ctrl Pts',(-69.5709686238701,13.3949090517173,
12.));
#146950=CARTESIAN_POINT('Ctrl Pts',(-69.5519176872857,13.3847240667627,
0.));
#146951=CARTESIAN_POINT('Ctrl Pts',(-69.5519176872857,13.3847240667627,
12.));
#146952=CARTESIAN_POINT('Ctrl Pts',(-69.5328989883899,13.3745814871668,
0.));
#146953=CARTESIAN_POINT('Ctrl Pts',(-69.5328989883899,13.3745814871668,
12.));
#146954=CARTESIAN_POINT('Ctrl Pts',(-69.5139126996703,13.3644813190225,
0.));
#146955=CARTESIAN_POINT('Ctrl Pts',(-69.5139126996703,13.3644813190225,
12.));
#146956=CARTESIAN_POINT('Ctrl Pts',(-69.4949589944633,13.3544235683399,
0.));
#146957=CARTESIAN_POINT('Ctrl Pts',(-69.4949589944633,13.3544235683399,
12.));
#146958=CARTESIAN_POINT('Ctrl Pts',(-69.4760380470382,13.3444082410547,
0.));
#146959=CARTESIAN_POINT('Ctrl Pts',(-69.4760380470382,13.3444082410547,
12.));
#146960=CARTESIAN_POINT('Ctrl Pts',(-69.4571500326673,13.3344353430313,
0.));
#146961=CARTESIAN_POINT('Ctrl Pts',(-69.4571500326673,13.3344353430313,
12.));
#146962=CARTESIAN_POINT('Ctrl Pts',(-69.4382951276983,13.3245048800641,
0.));
#146963=CARTESIAN_POINT('Ctrl Pts',(-69.4382951276983,13.3245048800641,
12.));
#146964=CARTESIAN_POINT('Ctrl Pts',(-69.4194735096238,13.3146168578739,
0.));
#146965=CARTESIAN_POINT('Ctrl Pts',(-69.4194735096238,13.3146168578739,
12.));
#146966=CARTESIAN_POINT('Ctrl Pts',(-69.4006853569485,13.3047712821046,
0.));
#146967=CARTESIAN_POINT('Ctrl Pts',(-69.4006853569485,13.3047712821046,
12.));
#146968=CARTESIAN_POINT('Ctrl Pts',(-69.3819308490407,13.2949681583165,
0.));
#146969=CARTESIAN_POINT('Ctrl Pts',(-69.3819308490407,13.2949681583165,
12.));
#146970=CARTESIAN_POINT('Ctrl Pts',(-69.3632101660071,13.2852074919767,
0.));
#146971=CARTESIAN_POINT('Ctrl Pts',(-69.3632101660071,13.2852074919767,
12.));
#146972=CARTESIAN_POINT('Ctrl Pts',(-69.3445234885088,13.2754892884438,
0.));
#146973=CARTESIAN_POINT('Ctrl Pts',(-69.3445234885088,13.2754892884438,
12.));
#146974=CARTESIAN_POINT('Ctrl Pts',(-69.3258709977416,13.2658135529616,
0.));
#146975=CARTESIAN_POINT('Ctrl Pts',(-69.3258709977416,13.2658135529616,
12.));
#146976=CARTESIAN_POINT('Ctrl Pts',(-69.3072528758546,13.2561802906901,
0.));
#146977=CARTESIAN_POINT('Ctrl Pts',(-69.3072528758546,13.2561802906901,
12.));
#146978=CARTESIAN_POINT('Ctrl Pts',(-69.2886693063193,13.2465895067264,
0.));
#146979=CARTESIAN_POINT('Ctrl Pts',(-69.2886693063193,13.2465895067264,
12.));
#146980=CARTESIAN_POINT('Ctrl Pts',(-69.2701204742435,13.2370412061218,
0.));
#146981=CARTESIAN_POINT('Ctrl Pts',(-69.2701204742435,13.2370412061218,
12.));
#146982=CARTESIAN_POINT('Ctrl Pts',(-69.2516065668809,13.2275353939044,
0.));
#146983=CARTESIAN_POINT('Ctrl Pts',(-69.2516065668809,13.2275353939044,
12.));
#146984=CARTESIAN_POINT('Ctrl Pts',(-69.2331277732819,13.2180720750586,
0.));
#146985=CARTESIAN_POINT('Ctrl Pts',(-69.2331277732819,13.2180720750586,
12.));
#146986=CARTESIAN_POINT('Ctrl Pts',(-69.2146842833506,13.2086512544729,
0.));
#146987=CARTESIAN_POINT('Ctrl Pts',(-69.2146842833506,13.2086512544729,
12.));
#146988=CARTESIAN_POINT('Ctrl Pts',(-69.1962762870524,13.1992729368928,
0.));
#146989=CARTESIAN_POINT('Ctrl Pts',(-69.1962762870524,13.1992729368928,
12.));
#146990=CARTESIAN_POINT('Ctrl Pts',(-69.1779039736026,13.189937126869,0.));
#146991=CARTESIAN_POINT('Ctrl Pts',(-69.1779039736026,13.189937126869,12.));
#146992=CARTESIAN_POINT('Ctrl Pts',(-69.1595675305294,13.1806438286944,
0.));
#146993=CARTESIAN_POINT('Ctrl Pts',(-69.1595675305294,13.1806438286944,
12.));
#146994=CARTESIAN_POINT('Ctrl Pts',(-69.141267145461,13.1713930465142,0.));
#146995=CARTESIAN_POINT('Ctrl Pts',(-69.141267145461,13.1713930465142,12.));
#146996=CARTESIAN_POINT('Ctrl Pts',(-69.1230030082598,13.1621847844533,
0.));
#146997=CARTESIAN_POINT('Ctrl Pts',(-69.1230030082598,13.1621847844533,
12.));
#146998=CARTESIAN_POINT('Ctrl Pts',(-69.1047753127633,13.1530190467181,
0.));
#146999=CARTESIAN_POINT('Ctrl Pts',(-69.1047753127633,13.1530190467181,
12.));
#147000=CARTESIAN_POINT('Ctrl Pts',(-69.0865842593063,13.1438958377397,
0.));
#147001=CARTESIAN_POINT('Ctrl Pts',(-69.0865842593063,13.1438958377397,
12.));
#147002=CARTESIAN_POINT('Ctrl Pts',(-69.0684300549426,13.1348151621825,
0.));
#147003=CARTESIAN_POINT('Ctrl Pts',(-69.0684300549426,13.1348151621825,
12.));
#147004=CARTESIAN_POINT('Ctrl Pts',(-69.0503129081778,13.1257770246379,
0.));
#147005=CARTESIAN_POINT('Ctrl Pts',(-69.0503129081778,13.1257770246379,
12.));
#147006=CARTESIAN_POINT('Ctrl Pts',(-69.0322330243336,13.1167814293496,
0.));
#147007=CARTESIAN_POINT('Ctrl Pts',(-69.0322330243336,13.1167814293496,
12.));
#147008=CARTESIAN_POINT('Ctrl Pts',(-69.0141906015137,13.1078283799726,
0.));
#147009=CARTESIAN_POINT('Ctrl Pts',(-69.0141906015137,13.1078283799726,
12.));
#147010=CARTESIAN_POINT('Ctrl Pts',(-68.9961858241577,13.0989178791843,
0.));
#147011=CARTESIAN_POINT('Ctrl Pts',(-68.9961858241577,13.0989178791843,
12.));
#147012=CARTESIAN_POINT('Ctrl Pts',(-68.9782188692654,13.0900499290542,
0.));
#147013=CARTESIAN_POINT('Ctrl Pts',(-68.9782188692654,13.0900499290542,
12.));
#147014=CARTESIAN_POINT('Ctrl Pts',(-68.9602899187628,13.0812245317816,
0.));
#147015=CARTESIAN_POINT('Ctrl Pts',(-68.9602899187628,13.0812245317816,
12.));
#147016=CARTESIAN_POINT('Ctrl Pts',(-68.9423991694492,13.072441690283,0.));
#147017=CARTESIAN_POINT('Ctrl Pts',(-68.9423991694492,13.072441690283,12.));
#147018=CARTESIAN_POINT('Ctrl Pts',(-68.9245468449865,13.0637014089018,
0.));
#147019=CARTESIAN_POINT('Ctrl Pts',(-68.9245468449865,13.0637014089018,
12.));
#147020=CARTESIAN_POINT('Ctrl Pts',(-68.9067332040842,13.0550036938793,
0.));
#147021=CARTESIAN_POINT('Ctrl Pts',(-68.9067332040842,13.0550036938793,
12.));
#147022=CARTESIAN_POINT('Ctrl Pts',(-68.8889585151431,13.0463485518185,
0.));
#147023=CARTESIAN_POINT('Ctrl Pts',(-68.8889585151431,13.0463485518185,
12.));
#147024=CARTESIAN_POINT('Ctrl Pts',(-68.8712230321823,13.0377359881864,
0.));
#147025=CARTESIAN_POINT('Ctrl Pts',(-68.8712230321823,13.0377359881864,
12.));
#147026=CARTESIAN_POINT('Ctrl Pts',(-68.853526972687,13.0291660060118,0.));
#147027=CARTESIAN_POINT('Ctrl Pts',(-68.853526972687,13.0291660060118,12.));
#147028=CARTESIAN_POINT('Ctrl Pts',(-68.835870488774,13.0206386039729,0.));
#147029=CARTESIAN_POINT('Ctrl Pts',(-68.835870488774,13.0206386039729,12.));
#147030=CARTESIAN_POINT('Ctrl Pts',(-68.8182536654066,13.0121537769003,
0.));
#147031=CARTESIAN_POINT('Ctrl Pts',(-68.8182536654066,13.0121537769003,
12.));
#147032=CARTESIAN_POINT('Ctrl Pts',(-68.8041919669403,13.0053999700929,
0.));
#147033=CARTESIAN_POINT('Ctrl Pts',(-68.8041919669403,13.0053999700929,
12.));
#147034=CARTESIAN_POINT('Ctrl Pts',(-68.7936635625787,13.0003537683089,
0.));
#147035=CARTESIAN_POINT('Ctrl Pts',(-68.7936635625787,13.0003537683089,
12.));
#147036=CARTESIAN_POINT('Ctrl Pts',(-68.7866525680284,12.996998146029,0.));
#147037=CARTESIAN_POINT('Ctrl Pts',(-68.7866525680284,12.996998146029,12.));
#147038=CARTESIAN_POINT('Ctrl Pts',(-68.7831490561748,12.9953224629497,
0.));
#147039=CARTESIAN_POINT('Ctrl Pts',(-68.7831490561748,12.9953224629497,
12.));
#147040=CARTESIAN_POINT('',(-68.7831490561748,12.9953224629497,12.));
#147041=CARTESIAN_POINT('Ctrl Pts',(-68.7831490561748,12.9953224629497,
12.));
#147042=CARTESIAN_POINT('Ctrl Pts',(-68.7866525680284,12.996998146029,12.));
#147043=CARTESIAN_POINT('Ctrl Pts',(-68.7936635625787,13.0003537683089,
12.));
#147044=CARTESIAN_POINT('Ctrl Pts',(-68.8041919669403,13.0053999700929,
12.));
#147045=CARTESIAN_POINT('Ctrl Pts',(-68.8182536654066,13.0121537769003,
12.));
#147046=CARTESIAN_POINT('Ctrl Pts',(-68.835870488774,13.0206386039729,12.));
#147047=CARTESIAN_POINT('Ctrl Pts',(-68.853526972687,13.0291660060118,12.));
#147048=CARTESIAN_POINT('Ctrl Pts',(-68.8712230321823,13.0377359881864,
12.));
#147049=CARTESIAN_POINT('Ctrl Pts',(-68.8889585151431,13.0463485518185,
12.));
#147050=CARTESIAN_POINT('Ctrl Pts',(-68.9067332040842,13.0550036938793,
12.));
#147051=CARTESIAN_POINT('Ctrl Pts',(-68.9245468449865,13.0637014089018,
12.));
#147052=CARTESIAN_POINT('Ctrl Pts',(-68.9423991694492,13.072441690283,12.));
#147053=CARTESIAN_POINT('Ctrl Pts',(-68.9602899187628,13.0812245317816,
12.));
#147054=CARTESIAN_POINT('Ctrl Pts',(-68.9782188692654,13.0900499290542,
12.));
#147055=CARTESIAN_POINT('Ctrl Pts',(-68.9961858241577,13.0989178791843,
12.));
#147056=CARTESIAN_POINT('Ctrl Pts',(-69.0141906015137,13.1078283799726,
12.));
#147057=CARTESIAN_POINT('Ctrl Pts',(-69.0322330243336,13.1167814293496,
12.));
#147058=CARTESIAN_POINT('Ctrl Pts',(-69.0503129081778,13.1257770246379,
12.));
#147059=CARTESIAN_POINT('Ctrl Pts',(-69.0684300549426,13.1348151621825,
12.));
#147060=CARTESIAN_POINT('Ctrl Pts',(-69.0865842593063,13.1438958377397,
12.));
#147061=CARTESIAN_POINT('Ctrl Pts',(-69.1047753127633,13.1530190467181,
12.));
#147062=CARTESIAN_POINT('Ctrl Pts',(-69.1230030082598,13.1621847844533,
12.));
#147063=CARTESIAN_POINT('Ctrl Pts',(-69.141267145461,13.1713930465142,12.));
#147064=CARTESIAN_POINT('Ctrl Pts',(-69.1595675305294,13.1806438286944,
12.));
#147065=CARTESIAN_POINT('Ctrl Pts',(-69.1779039736026,13.189937126869,12.));
#147066=CARTESIAN_POINT('Ctrl Pts',(-69.1962762870524,13.1992729368928,
12.));
#147067=CARTESIAN_POINT('Ctrl Pts',(-69.2146842833506,13.2086512544729,
12.));
#147068=CARTESIAN_POINT('Ctrl Pts',(-69.2331277732819,13.2180720750586,
12.));
#147069=CARTESIAN_POINT('Ctrl Pts',(-69.2516065668809,13.2275353939044,
12.));
#147070=CARTESIAN_POINT('Ctrl Pts',(-69.2701204742435,13.2370412061218,
12.));
#147071=CARTESIAN_POINT('Ctrl Pts',(-69.2886693063193,13.2465895067264,
12.));
#147072=CARTESIAN_POINT('Ctrl Pts',(-69.3072528758546,13.2561802906901,
12.));
#147073=CARTESIAN_POINT('Ctrl Pts',(-69.3258709977416,13.2658135529616,
12.));
#147074=CARTESIAN_POINT('Ctrl Pts',(-69.3445234885088,13.2754892884438,
12.));
#147075=CARTESIAN_POINT('Ctrl Pts',(-69.3632101660071,13.2852074919767,
12.));
#147076=CARTESIAN_POINT('Ctrl Pts',(-69.3819308490407,13.2949681583165,
12.));
#147077=CARTESIAN_POINT('Ctrl Pts',(-69.4006853569485,13.3047712821046,
12.));
#147078=CARTESIAN_POINT('Ctrl Pts',(-69.4194735096238,13.3146168578739,
12.));
#147079=CARTESIAN_POINT('Ctrl Pts',(-69.4382951276983,13.3245048800641,
12.));
#147080=CARTESIAN_POINT('Ctrl Pts',(-69.4571500326673,13.3344353430313,
12.));
#147081=CARTESIAN_POINT('Ctrl Pts',(-69.4760380470382,13.3444082410547,
12.));
#147082=CARTESIAN_POINT('Ctrl Pts',(-69.4949589944633,13.3544235683399,
12.));
#147083=CARTESIAN_POINT('Ctrl Pts',(-69.5139126996703,13.3644813190225,
12.));
#147084=CARTESIAN_POINT('Ctrl Pts',(-69.5328989883899,13.3745814871668,
12.));
#147085=CARTESIAN_POINT('Ctrl Pts',(-69.5519176872857,13.3847240667627,
12.));
#147086=CARTESIAN_POINT('Ctrl Pts',(-69.5709686238701,13.3949090517173,
12.));
#147087=CARTESIAN_POINT('Ctrl Pts',(-69.5900516264524,13.4051364358495,
12.));
#147088=CARTESIAN_POINT('Ctrl Pts',(-69.6091665241743,13.4154062128998,
12.));
#147089=CARTESIAN_POINT('Ctrl Pts',(-69.6283131470267,13.425718376534,12.));
#147090=CARTESIAN_POINT('Ctrl Pts',(-69.6474913258684,13.4360729203444,
12.));
#147091=CARTESIAN_POINT('Ctrl Pts',(-69.6667008924454,13.4464698378456,
12.));
#147092=CARTESIAN_POINT('Ctrl Pts',(-69.6859416793898,13.4569091224763,
12.));
#147093=CARTESIAN_POINT('Ctrl Pts',(-69.7052135202003,13.4673907676045,
12.));
#147094=CARTESIAN_POINT('Ctrl Pts',(-69.7245162492251,13.4779147665286,
12.));
#147095=CARTESIAN_POINT('Ctrl Pts',(-69.7438497016404,13.4884811124748,
12.));
#147096=CARTESIAN_POINT('Ctrl Pts',(-69.7632137134247,13.4990897985904,
12.));
#147097=CARTESIAN_POINT('Ctrl Pts',(-69.7826081213575,13.5097408179479,
12.));
#147098=CARTESIAN_POINT('Ctrl Pts',(-69.8020327630204,13.5204341635507,
12.));
#147099=CARTESIAN_POINT('Ctrl Pts',(-69.8214874767944,13.5311698283339,
12.));
#147100=CARTESIAN_POINT('Ctrl Pts',(-69.840972101856,13.5419478051626,12.));
#147101=CARTESIAN_POINT('Ctrl Pts',(-69.8604864781705,13.5527680868256,
12.));
#147102=CARTESIAN_POINT('Ctrl Pts',(-69.880030446488,13.5636306660423,12.));
#147103=CARTESIAN_POINT('Ctrl Pts',(-69.899603848336,13.5745355354657,12.));
#147104=CARTESIAN_POINT('Ctrl Pts',(-69.9192065260107,13.5854826876834,
12.));
#147105=CARTESIAN_POINT('Ctrl Pts',(-69.9388383225655,13.5964721152136,
12.));
#147106=CARTESIAN_POINT('Ctrl Pts',(-69.9584990817989,13.6075038105001,
12.));
#147107=CARTESIAN_POINT('Ctrl Pts',(-69.9781886482543,13.61857776592,12.));
#147108=CARTESIAN_POINT('Ctrl Pts',(-69.9979068672163,13.6296939737866,
12.));
#147109=CARTESIAN_POINT('Ctrl Pts',(-70.0176535847047,13.6408524263496,
12.));
#147110=CARTESIAN_POINT('Ctrl Pts',(-70.037428647466,13.6520531157904,12.));
#147111=CARTESIAN_POINT('Ctrl Pts',(-70.057231902965,13.6632960342192,12.));
#147112=CARTESIAN_POINT('Ctrl Pts',(-70.0770631993831,13.6745811736825,
12.));
#147113=CARTESIAN_POINT('Ctrl Pts',(-70.0969223856123,13.6859085261651,
12.));
#147114=CARTESIAN_POINT('Ctrl Pts',(-70.1168093112493,13.6972780835899,
12.));
#147115=CARTESIAN_POINT('Ctrl Pts',(-70.1367238265853,13.7086898378127,
12.));
#147116=CARTESIAN_POINT('Ctrl Pts',(-70.1566657825989,13.7201437806207,
12.));
#147117=CARTESIAN_POINT('Ctrl Pts',(-70.1766350309554,13.73163990374,12.));
#147118=CARTESIAN_POINT('Ctrl Pts',(-70.1966314240012,13.7431781988368,
12.));
#147119=CARTESIAN_POINT('Ctrl Pts',(-70.216654814759,13.7547586575178,12.));
#147120=CARTESIAN_POINT('Ctrl Pts',(-70.2367050569174,13.7663812713235,
12.));
#147121=CARTESIAN_POINT('Ctrl Pts',(-70.2567820048253,13.7780460317284,
12.));
#147122=CARTESIAN_POINT('Ctrl Pts',(-70.2768855134909,13.7897529301483,
12.));
#147123=CARTESIAN_POINT('Ctrl Pts',(-70.2970154385763,13.8015019579411,
12.));
#147124=CARTESIAN_POINT('Ctrl Pts',(-70.3171716363912,13.8132931064067,
12.));
#147125=CARTESIAN_POINT('Ctrl Pts',(-70.3373539638841,13.8251263667799,
12.));
#147126=CARTESIAN_POINT('Ctrl Pts',(-70.3575622786373,13.8370017302319,
12.));
#147127=CARTESIAN_POINT('Ctrl Pts',(-70.377796438866,13.8489191878774,12.));
#147128=CARTESIAN_POINT('Ctrl Pts',(-70.3980563034142,13.8608787307754,
12.));
#147129=CARTESIAN_POINT('Ctrl Pts',(-70.4183417317486,13.8728803499284,
12.));
#147130=CARTESIAN_POINT('Ctrl Pts',(-70.4386525839492,13.8849240362757,
12.));
#147131=CARTESIAN_POINT('Ctrl Pts',(-70.4589887207043,13.8970097806948,
12.));
#147132=CARTESIAN_POINT('Ctrl Pts',(-70.4793500033106,13.9091375740085,
12.));
#147133=CARTESIAN_POINT('Ctrl Pts',(-70.4997362936671,13.9213074069852,
12.));
#147134=CARTESIAN_POINT('Ctrl Pts',(-70.5201474542717,13.933519270339,12.));
#147135=CARTESIAN_POINT('Ctrl Pts',(-70.5405833482123,13.9457731547218,
12.));
#147136=CARTESIAN_POINT('Ctrl Pts',(-70.5610438391622,13.9580690507262,
12.));
#147137=CARTESIAN_POINT('Ctrl Pts',(-70.5815287913791,13.9704069488918,
12.));
#147138=CARTESIAN_POINT('Ctrl Pts',(-70.6020380697004,13.9827868397057,
12.));
#147139=CARTESIAN_POINT('Ctrl Pts',(-70.6225715395392,13.9952087136018,
12.));
#147140=CARTESIAN_POINT('Ctrl Pts',(-70.6431290668744,14.0076725609537,
12.));
#147141=CARTESIAN_POINT('Ctrl Pts',(-70.6637105182487,14.020178372077,12.));
#147142=CARTESIAN_POINT('Ctrl Pts',(-70.6843157607672,14.0327261372363,
12.));
#147143=CARTESIAN_POINT('Ctrl Pts',(-70.7049446620931,14.0453158466451,
12.));
#147144=CARTESIAN_POINT('Ctrl Pts',(-70.7255970904433,14.0579474904657,
12.));
#147145=CARTESIAN_POINT('Ctrl Pts',(-70.7462729145799,14.0706210588015,
12.));
#147146=CARTESIAN_POINT('Ctrl Pts',(-70.7669720038067,14.0833365416995,
12.));
#147147=CARTESIAN_POINT('Ctrl Pts',(-70.787694227969,14.0960939291569,12.));
#147148=CARTESIAN_POINT('Ctrl Pts',(-70.8084394574491,14.1088932111215,
12.));
#147149=CARTESIAN_POINT('Ctrl Pts',(-70.8292075631624,14.1217343774914,
12.));
#147150=CARTESIAN_POINT('Ctrl Pts',(-70.8499984165493,14.1346174181079,
12.));
#147151=CARTESIAN_POINT('Ctrl Pts',(-70.8708118895717,14.1475423227568,
12.));
#147152=CARTESIAN_POINT('Ctrl Pts',(-70.8916478547131,14.1605090811754,
12.));
#147153=CARTESIAN_POINT('Ctrl Pts',(-70.9125061849744,14.1735176830533,
12.));
#147154=CARTESIAN_POINT('Ctrl Pts',(-70.9333867538704,14.1865681180321,
12.));
#147155=CARTESIAN_POINT('Ctrl Pts',(-70.9542894354221,14.1996603756984,
12.));
#147156=CARTESIAN_POINT('Ctrl Pts',(-70.9752141041527,14.2127944455841,
12.));
#147157=CARTESIAN_POINT('Ctrl Pts',(-70.996160635087,14.2259703171739,12.));
#147158=CARTESIAN_POINT('Ctrl Pts',(-71.0171289037493,14.2391879799063,
12.));
#147159=CARTESIAN_POINT('Ctrl Pts',(-71.0381187861585,14.2524474231732,
12.));
#147160=CARTESIAN_POINT('Ctrl Pts',(-71.059130158822,14.2657486363137,12.));
#147161=CARTESIAN_POINT('Ctrl Pts',(-71.0801628987314,14.279091608613,12.));
#147162=CARTESIAN_POINT('Ctrl Pts',(-71.1012168833626,14.2924763293101,
12.));
#147163=CARTESIAN_POINT('Ctrl Pts',(-71.1222919906718,14.3059027875993,
12.));
#147164=CARTESIAN_POINT('Ctrl Pts',(-71.1433880990932,14.3193709726295,
12.));
#147165=CARTESIAN_POINT('Ctrl Pts',(-71.1645050875323,14.3328808734993,
12.));
#147166=CARTESIAN_POINT('Ctrl Pts',(-71.185642835361,14.3464324792537,12.));
#147167=CARTESIAN_POINT('Ctrl Pts',(-71.2068012224187,14.3600257788927,
12.));
#147168=CARTESIAN_POINT('Ctrl Pts',(-71.2279801290088,14.3736607613723,
12.));
#147169=CARTESIAN_POINT('Ctrl Pts',(-71.2491794358956,14.3873374156056,
12.));
#147170=CARTESIAN_POINT('Ctrl Pts',(-71.2703990242986,14.401055730457,12.));
#147171=CARTESIAN_POINT('Ctrl Pts',(-71.2916387758864,14.4148156947384,
12.));
#147172=CARTESIAN_POINT('Ctrl Pts',(-71.3128985727777,14.4286172972168,
12.));
#147173=CARTESIAN_POINT('Ctrl Pts',(-71.3341782975393,14.4424605266167,
12.));
#147174=CARTESIAN_POINT('Ctrl Pts',(-71.3554778331835,14.4563453716204,
12.));
#147175=CARTESIAN_POINT('Ctrl Pts',(-71.3767970631642,14.470271820865,12.));
#147176=CARTESIAN_POINT('Ctrl Pts',(-71.398135871371,14.4842398629354,12.));
#147177=CARTESIAN_POINT('Ctrl Pts',(-71.4194941421279,14.4982494863716,
12.));
#147178=CARTESIAN_POINT('Ctrl Pts',(-71.4408717601917,14.5123006796728,
12.));
#147179=CARTESIAN_POINT('Ctrl Pts',(-71.4622686107475,14.5263934312969,
12.));
#147180=CARTESIAN_POINT('Ctrl Pts',(-71.4836845794052,14.540527729659,12.));
#147181=CARTESIAN_POINT('Ctrl Pts',(-71.5051195521914,14.5547035631234,
12.));
#147182=CARTESIAN_POINT('Ctrl Pts',(-71.52657341555,14.5689209200091,12.));
#147183=CARTESIAN_POINT('Ctrl Pts',(-71.5480460563445,14.5831797885951,
12.));
#147184=CARTESIAN_POINT('Ctrl Pts',(-71.569537361856,14.597480157121,12.));
#147185=CARTESIAN_POINT('Ctrl Pts',(-71.5910472197814,14.611822013785,12.));
#147186=CARTESIAN_POINT('Ctrl Pts',(-71.6125755182295,14.6262053467372,
12.));
#147187=CARTESIAN_POINT('Ctrl Pts',(-71.6341221457175,14.6406301440817,
12.));
#147188=CARTESIAN_POINT('Ctrl Pts',(-71.6556869911669,14.6550963938832,
12.));
#147189=CARTESIAN_POINT('Ctrl Pts',(-71.6772699438966,14.669604084168,12.));
#147190=CARTESIAN_POINT('Ctrl Pts',(-71.698870893617,14.6841532029232,12.));
#147191=CARTESIAN_POINT('Ctrl Pts',(-71.7204897304186,14.6987437380898,
12.));
#147192=CARTESIAN_POINT('Ctrl Pts',(-71.7421263447707,14.7133756775622,
12.));
#147193=CARTESIAN_POINT('Ctrl Pts',(-71.7637806275316,14.7280490091954,
12.));
#147194=CARTESIAN_POINT('Ctrl Pts',(-71.7854524699562,14.7427637208071,
12.));
#147195=CARTESIAN_POINT('Ctrl Pts',(-71.8071417637018,14.7575198001777,
12.));
#147196=CARTESIAN_POINT('Ctrl Pts',(-71.8288484008343,14.7723172350455,
12.));
#147197=CARTESIAN_POINT('Ctrl Pts',(-71.8505722738286,14.7871560131021,
12.));
#147198=CARTESIAN_POINT('Ctrl Pts',(-71.872313275546,14.8020361220003,12.));
#147199=CARTESIAN_POINT('Ctrl Pts',(-71.8940712992119,14.816957549356,12.));
#147200=CARTESIAN_POINT('Ctrl Pts',(-71.9158462383915,14.8319202827483,
12.));
#147201=CARTESIAN_POINT('Ctrl Pts',(-71.9376379869668,14.846924309716,12.));
#147202=CARTESIAN_POINT('Ctrl Pts',(-71.9594464391063,14.8619696177503,
12.));
#147203=CARTESIAN_POINT('Ctrl Pts',(-71.9812714893087,14.8770561943011,
12.));
#147204=CARTESIAN_POINT('Ctrl Pts',(-72.0031130324519,14.892184026783,12.));
#147205=CARTESIAN_POINT('Ctrl Pts',(-72.0249709638419,14.9073531025764,
12.));
#147206=CARTESIAN_POINT('Ctrl Pts',(-72.046845179251,14.9225634090269,12.));
#147207=CARTESIAN_POINT('Ctrl Pts',(-72.0687355749815,14.937814933439,12.));
#147208=CARTESIAN_POINT('Ctrl Pts',(-72.0906420478085,14.953107663077,12.));
#147209=CARTESIAN_POINT('Ctrl Pts',(-72.1125644948547,14.96844158517,12.));
#147210=CARTESIAN_POINT('Ctrl Pts',(-72.1345028134779,14.9838166869107,
12.));
#147211=CARTESIAN_POINT('Ctrl Pts',(-72.1564569011668,14.9992329554537,
12.));
#147212=CARTESIAN_POINT('Ctrl Pts',(-72.1784266553948,15.0146903779061,
12.));
#147213=CARTESIAN_POINT('Ctrl Pts',(-72.2004119736104,15.0301889413255,
12.));
#147214=CARTESIAN_POINT('Ctrl Pts',(-72.2224127535401,15.0457286327328,
12.));
#147215=CARTESIAN_POINT('Ctrl Pts',(-72.244428893425,15.0613094391186,12.));
#147216=CARTESIAN_POINT('Ctrl Pts',(-72.266460292285,15.0769313474476,12.));
#147217=CARTESIAN_POINT('Ctrl Pts',(-72.2885068501641,15.0925943446593,
12.));
#147218=CARTESIAN_POINT('Ctrl Pts',(-72.3105684683971,15.1082984176656,
12.));
#147219=CARTESIAN_POINT('Ctrl Pts',(-72.332645049021,15.1240435533478,12.));
#147220=CARTESIAN_POINT('Ctrl Pts',(-72.3547364941996,15.1398297385513,
12.));
#147221=CARTESIAN_POINT('Ctrl Pts',(-72.37684270559,15.1556569600747,12.));
#147222=CARTESIAN_POINT('Ctrl Pts',(-72.3989635838476,15.1715252046603,
12.));
#147223=CARTESIAN_POINT('Ctrl Pts',(-72.4210990277819,15.1874344589716,
12.));
#147224=CARTESIAN_POINT('Ctrl Pts',(-72.4432489350415,15.2033847096077,
12.));
#147225=CARTESIAN_POINT('Ctrl Pts',(-72.4654132036373,15.2193759431359,
12.));
#147226=CARTESIAN_POINT('Ctrl Pts',(-72.4875917332729,15.2354081461152,
12.));
#147227=CARTESIAN_POINT('Ctrl Pts',(-72.5097844266083,15.2514813051174,
12.));
#147228=CARTESIAN_POINT('Ctrl Pts',(-72.5319911908978,15.2675954067495,
12.));
#147229=CARTESIAN_POINT('Ctrl Pts',(-72.5542119383748,15.2837504376562,
12.));
#147230=CARTESIAN_POINT('Ctrl Pts',(-72.5732713370795,15.2976335024853,
12.));
#147231=CARTESIAN_POINT('Ctrl Pts',(-72.5878912620662,15.3082994603651,
12.));
#147232=CARTESIAN_POINT('Ctrl Pts',(-72.5980655789897,15.3157301930832,
12.));
#147233=CARTESIAN_POINT('Ctrl Pts',(-72.6037902605225,15.3199137230318,
12.));
#147234=CARTESIAN_POINT('Ctrl Pts',(-72.6050633494711,15.320844207742,12.));
#147235=CARTESIAN_POINT('',(-68.7831490561748,12.9953224629497,0.));
#147236=CARTESIAN_POINT('',(-68.7831490561748,12.9953224629497,0.));
#147237=CARTESIAN_POINT('Ctrl Pts',(-72.6050633494711,15.320844207742,0.));
#147238=CARTESIAN_POINT('Ctrl Pts',(-72.6037902605226,15.3199137230318,
0.));
#147239=CARTESIAN_POINT('Ctrl Pts',(-72.5980655789897,15.3157301930832,
0.));
#147240=CARTESIAN_POINT('Ctrl Pts',(-72.5878912620662,15.3082994603651,
0.));
#147241=CARTESIAN_POINT('Ctrl Pts',(-72.5732713370795,15.2976335024853,
0.));
#147242=CARTESIAN_POINT('Ctrl Pts',(-72.5542119383748,15.2837504376562,
0.));
#147243=CARTESIAN_POINT('Ctrl Pts',(-72.5319911908978,15.2675954067495,
0.));
#147244=CARTESIAN_POINT('Ctrl Pts',(-72.5097844266083,15.2514813051174,
0.));
#147245=CARTESIAN_POINT('Ctrl Pts',(-72.4875917332729,15.2354081461152,
0.));
#147246=CARTESIAN_POINT('Ctrl Pts',(-72.4654132036373,15.2193759431359,
0.));
#147247=CARTESIAN_POINT('Ctrl Pts',(-72.4432489350415,15.2033847096077,
0.));
#147248=CARTESIAN_POINT('Ctrl Pts',(-72.4210990277819,15.1874344589716,
0.));
#147249=CARTESIAN_POINT('Ctrl Pts',(-72.3989635838476,15.1715252046603,
0.));
#147250=CARTESIAN_POINT('Ctrl Pts',(-72.37684270559,15.1556569600747,0.));
#147251=CARTESIAN_POINT('Ctrl Pts',(-72.3547364941996,15.1398297385513,
0.));
#147252=CARTESIAN_POINT('Ctrl Pts',(-72.332645049021,15.1240435533478,0.));
#147253=CARTESIAN_POINT('Ctrl Pts',(-72.3105684683971,15.1082984176656,
0.));
#147254=CARTESIAN_POINT('Ctrl Pts',(-72.2885068501641,15.0925943446593,
0.));
#147255=CARTESIAN_POINT('Ctrl Pts',(-72.266460292285,15.0769313474476,0.));
#147256=CARTESIAN_POINT('Ctrl Pts',(-72.244428893425,15.0613094391186,0.));
#147257=CARTESIAN_POINT('Ctrl Pts',(-72.2224127535401,15.0457286327328,
0.));
#147258=CARTESIAN_POINT('Ctrl Pts',(-72.2004119736104,15.0301889413255,
0.));
#147259=CARTESIAN_POINT('Ctrl Pts',(-72.1784266553948,15.0146903779061,
0.));
#147260=CARTESIAN_POINT('Ctrl Pts',(-72.1564569011668,14.9992329554537,
0.));
#147261=CARTESIAN_POINT('Ctrl Pts',(-72.1345028134779,14.9838166869107,
0.));
#147262=CARTESIAN_POINT('Ctrl Pts',(-72.1125644948547,14.96844158517,0.));
#147263=CARTESIAN_POINT('Ctrl Pts',(-72.0906420478085,14.953107663077,0.));
#147264=CARTESIAN_POINT('Ctrl Pts',(-72.0687355749815,14.937814933439,0.));
#147265=CARTESIAN_POINT('Ctrl Pts',(-72.046845179251,14.9225634090269,0.));
#147266=CARTESIAN_POINT('Ctrl Pts',(-72.0249709638419,14.9073531025764,
0.));
#147267=CARTESIAN_POINT('Ctrl Pts',(-72.0031130324519,14.892184026783,0.));
#147268=CARTESIAN_POINT('Ctrl Pts',(-71.9812714893087,14.8770561943011,
0.));
#147269=CARTESIAN_POINT('Ctrl Pts',(-71.9594464391063,14.8619696177503,
0.));
#147270=CARTESIAN_POINT('Ctrl Pts',(-71.9376379869668,14.846924309716,0.));
#147271=CARTESIAN_POINT('Ctrl Pts',(-71.9158462383915,14.8319202827483,
0.));
#147272=CARTESIAN_POINT('Ctrl Pts',(-71.8940712992119,14.816957549356,0.));
#147273=CARTESIAN_POINT('Ctrl Pts',(-71.872313275546,14.8020361220003,0.));
#147274=CARTESIAN_POINT('Ctrl Pts',(-71.8505722738286,14.7871560131021,
0.));
#147275=CARTESIAN_POINT('Ctrl Pts',(-71.8288484008343,14.7723172350455,
0.));
#147276=CARTESIAN_POINT('Ctrl Pts',(-71.8071417637018,14.7575198001777,
0.));
#147277=CARTESIAN_POINT('Ctrl Pts',(-71.7854524699562,14.7427637208071,
0.));
#147278=CARTESIAN_POINT('Ctrl Pts',(-71.7637806275316,14.7280490091954,
0.));
#147279=CARTESIAN_POINT('Ctrl Pts',(-71.7421263447707,14.7133756775622,
0.));
#147280=CARTESIAN_POINT('Ctrl Pts',(-71.7204897304186,14.6987437380898,
0.));
#147281=CARTESIAN_POINT('Ctrl Pts',(-71.698870893617,14.6841532029232,0.));
#147282=CARTESIAN_POINT('Ctrl Pts',(-71.6772699438966,14.669604084168,0.));
#147283=CARTESIAN_POINT('Ctrl Pts',(-71.6556869911669,14.6550963938832,
0.));
#147284=CARTESIAN_POINT('Ctrl Pts',(-71.6341221457175,14.6406301440817,
0.));
#147285=CARTESIAN_POINT('Ctrl Pts',(-71.6125755182295,14.6262053467372,
0.));
#147286=CARTESIAN_POINT('Ctrl Pts',(-71.5910472197814,14.611822013785,0.));
#147287=CARTESIAN_POINT('Ctrl Pts',(-71.569537361856,14.597480157121,0.));
#147288=CARTESIAN_POINT('Ctrl Pts',(-71.5480460563445,14.5831797885951,
0.));
#147289=CARTESIAN_POINT('Ctrl Pts',(-71.52657341555,14.5689209200091,0.));
#147290=CARTESIAN_POINT('Ctrl Pts',(-71.5051195521914,14.5547035631234,
0.));
#147291=CARTESIAN_POINT('Ctrl Pts',(-71.4836845794052,14.540527729659,0.));
#147292=CARTESIAN_POINT('Ctrl Pts',(-71.4622686107475,14.5263934312969,
0.));
#147293=CARTESIAN_POINT('Ctrl Pts',(-71.4408717601917,14.5123006796728,
0.));
#147294=CARTESIAN_POINT('Ctrl Pts',(-71.4194941421279,14.4982494863716,
0.));
#147295=CARTESIAN_POINT('Ctrl Pts',(-71.398135871371,14.4842398629354,0.));
#147296=CARTESIAN_POINT('Ctrl Pts',(-71.3767970631642,14.470271820865,0.));
#147297=CARTESIAN_POINT('Ctrl Pts',(-71.3554778331835,14.4563453716204,
0.));
#147298=CARTESIAN_POINT('Ctrl Pts',(-71.3341782975393,14.4424605266167,
0.));
#147299=CARTESIAN_POINT('Ctrl Pts',(-71.3128985727777,14.4286172972168,
0.));
#147300=CARTESIAN_POINT('Ctrl Pts',(-71.2916387758864,14.4148156947384,
0.));
#147301=CARTESIAN_POINT('Ctrl Pts',(-71.2703990242986,14.401055730457,0.));
#147302=CARTESIAN_POINT('Ctrl Pts',(-71.2491794358956,14.3873374156056,
0.));
#147303=CARTESIAN_POINT('Ctrl Pts',(-71.2279801290088,14.3736607613723,
0.));
#147304=CARTESIAN_POINT('Ctrl Pts',(-71.2068012224187,14.3600257788927,
0.));
#147305=CARTESIAN_POINT('Ctrl Pts',(-71.185642835361,14.3464324792537,0.));
#147306=CARTESIAN_POINT('Ctrl Pts',(-71.1645050875323,14.3328808734993,
0.));
#147307=CARTESIAN_POINT('Ctrl Pts',(-71.1433880990932,14.3193709726295,
0.));
#147308=CARTESIAN_POINT('Ctrl Pts',(-71.1222919906718,14.3059027875993,
0.));
#147309=CARTESIAN_POINT('Ctrl Pts',(-71.1012168833626,14.2924763293101,
0.));
#147310=CARTESIAN_POINT('Ctrl Pts',(-71.0801628987314,14.279091608613,0.));
#147311=CARTESIAN_POINT('Ctrl Pts',(-71.059130158822,14.2657486363137,0.));
#147312=CARTESIAN_POINT('Ctrl Pts',(-71.0381187861585,14.2524474231732,
0.));
#147313=CARTESIAN_POINT('Ctrl Pts',(-71.0171289037493,14.2391879799063,
0.));
#147314=CARTESIAN_POINT('Ctrl Pts',(-70.996160635087,14.2259703171739,0.));
#147315=CARTESIAN_POINT('Ctrl Pts',(-70.9752141041527,14.2127944455841,
0.));
#147316=CARTESIAN_POINT('Ctrl Pts',(-70.9542894354221,14.1996603756984,
0.));
#147317=CARTESIAN_POINT('Ctrl Pts',(-70.9333867538704,14.1865681180321,
0.));
#147318=CARTESIAN_POINT('Ctrl Pts',(-70.9125061849744,14.1735176830533,
0.));
#147319=CARTESIAN_POINT('Ctrl Pts',(-70.8916478547131,14.1605090811754,
0.));
#147320=CARTESIAN_POINT('Ctrl Pts',(-70.8708118895717,14.1475423227568,
0.));
#147321=CARTESIAN_POINT('Ctrl Pts',(-70.8499984165493,14.1346174181079,
0.));
#147322=CARTESIAN_POINT('Ctrl Pts',(-70.8292075631624,14.1217343774914,
0.));
#147323=CARTESIAN_POINT('Ctrl Pts',(-70.8084394574491,14.1088932111215,
0.));
#147324=CARTESIAN_POINT('Ctrl Pts',(-70.787694227969,14.0960939291569,0.));
#147325=CARTESIAN_POINT('Ctrl Pts',(-70.7669720038067,14.0833365416995,
0.));
#147326=CARTESIAN_POINT('Ctrl Pts',(-70.7462729145799,14.0706210588015,
0.));
#147327=CARTESIAN_POINT('Ctrl Pts',(-70.7255970904433,14.0579474904657,
0.));
#147328=CARTESIAN_POINT('Ctrl Pts',(-70.7049446620931,14.0453158466451,
0.));
#147329=CARTESIAN_POINT('Ctrl Pts',(-70.6843157607672,14.0327261372363,
0.));
#147330=CARTESIAN_POINT('Ctrl Pts',(-70.6637105182487,14.020178372077,0.));
#147331=CARTESIAN_POINT('Ctrl Pts',(-70.6431290668744,14.0076725609537,
0.));
#147332=CARTESIAN_POINT('Ctrl Pts',(-70.6225715395392,13.9952087136018,
0.));
#147333=CARTESIAN_POINT('Ctrl Pts',(-70.6020380697004,13.9827868397057,
0.));
#147334=CARTESIAN_POINT('Ctrl Pts',(-70.5815287913791,13.9704069488918,
0.));
#147335=CARTESIAN_POINT('Ctrl Pts',(-70.5610438391622,13.9580690507262,
0.));
#147336=CARTESIAN_POINT('Ctrl Pts',(-70.5405833482123,13.9457731547218,
0.));
#147337=CARTESIAN_POINT('Ctrl Pts',(-70.5201474542717,13.933519270339,0.));
#147338=CARTESIAN_POINT('Ctrl Pts',(-70.4997362936671,13.9213074069852,
0.));
#147339=CARTESIAN_POINT('Ctrl Pts',(-70.4793500033106,13.9091375740085,
0.));
#147340=CARTESIAN_POINT('Ctrl Pts',(-70.4589887207043,13.8970097806948,
0.));
#147341=CARTESIAN_POINT('Ctrl Pts',(-70.4386525839492,13.8849240362757,
0.));
#147342=CARTESIAN_POINT('Ctrl Pts',(-70.4183417317486,13.8728803499284,
0.));
#147343=CARTESIAN_POINT('Ctrl Pts',(-70.3980563034142,13.8608787307754,
0.));
#147344=CARTESIAN_POINT('Ctrl Pts',(-70.377796438866,13.8489191878774,0.));
#147345=CARTESIAN_POINT('Ctrl Pts',(-70.3575622786373,13.8370017302319,
0.));
#147346=CARTESIAN_POINT('Ctrl Pts',(-70.3373539638841,13.8251263667799,
0.));
#147347=CARTESIAN_POINT('Ctrl Pts',(-70.3171716363912,13.8132931064067,
0.));
#147348=CARTESIAN_POINT('Ctrl Pts',(-70.2970154385763,13.8015019579411,
0.));
#147349=CARTESIAN_POINT('Ctrl Pts',(-70.2768855134909,13.7897529301483,
0.));
#147350=CARTESIAN_POINT('Ctrl Pts',(-70.2567820048253,13.7780460317284,
0.));
#147351=CARTESIAN_POINT('Ctrl Pts',(-70.2367050569174,13.7663812713235,
0.));
#147352=CARTESIAN_POINT('Ctrl Pts',(-70.216654814759,13.7547586575178,0.));
#147353=CARTESIAN_POINT('Ctrl Pts',(-70.1966314240012,13.7431781988368,
0.));
#147354=CARTESIAN_POINT('Ctrl Pts',(-70.1766350309554,13.73163990374,0.));
#147355=CARTESIAN_POINT('Ctrl Pts',(-70.1566657825989,13.7201437806207,
0.));
#147356=CARTESIAN_POINT('Ctrl Pts',(-70.1367238265853,13.7086898378127,
0.));
#147357=CARTESIAN_POINT('Ctrl Pts',(-70.1168093112493,13.6972780835899,
0.));
#147358=CARTESIAN_POINT('Ctrl Pts',(-70.0969223856123,13.6859085261651,
0.));
#147359=CARTESIAN_POINT('Ctrl Pts',(-70.0770631993831,13.6745811736825,
0.));
#147360=CARTESIAN_POINT('Ctrl Pts',(-70.057231902965,13.6632960342192,0.));
#147361=CARTESIAN_POINT('Ctrl Pts',(-70.037428647466,13.6520531157904,0.));
#147362=CARTESIAN_POINT('Ctrl Pts',(-70.0176535847047,13.6408524263496,
0.));
#147363=CARTESIAN_POINT('Ctrl Pts',(-69.9979068672163,13.6296939737866,
0.));
#147364=CARTESIAN_POINT('Ctrl Pts',(-69.9781886482543,13.61857776592,0.));
#147365=CARTESIAN_POINT('Ctrl Pts',(-69.9584990817989,13.6075038105001,
0.));
#147366=CARTESIAN_POINT('Ctrl Pts',(-69.9388383225655,13.5964721152136,
0.));
#147367=CARTESIAN_POINT('Ctrl Pts',(-69.9192065260107,13.5854826876834,
0.));
#147368=CARTESIAN_POINT('Ctrl Pts',(-69.899603848336,13.5745355354657,0.));
#147369=CARTESIAN_POINT('Ctrl Pts',(-69.880030446488,13.5636306660423,0.));
#147370=CARTESIAN_POINT('Ctrl Pts',(-69.8604864781705,13.5527680868256,
0.));
#147371=CARTESIAN_POINT('Ctrl Pts',(-69.840972101856,13.5419478051626,0.));
#147372=CARTESIAN_POINT('Ctrl Pts',(-69.8214874767944,13.5311698283339,
0.));
#147373=CARTESIAN_POINT('Ctrl Pts',(-69.8020327630204,13.5204341635507,
0.));
#147374=CARTESIAN_POINT('Ctrl Pts',(-69.7826081213575,13.5097408179479,
0.));
#147375=CARTESIAN_POINT('Ctrl Pts',(-69.7632137134247,13.4990897985904,
0.));
#147376=CARTESIAN_POINT('Ctrl Pts',(-69.7438497016404,13.4884811124748,
0.));
#147377=CARTESIAN_POINT('Ctrl Pts',(-69.7245162492251,13.4779147665286,
0.));
#147378=CARTESIAN_POINT('Ctrl Pts',(-69.7052135202003,13.4673907676045,
0.));
#147379=CARTESIAN_POINT('Ctrl Pts',(-69.6859416793898,13.4569091224763,
0.));
#147380=CARTESIAN_POINT('Ctrl Pts',(-69.6667008924454,13.4464698378456,
0.));
#147381=CARTESIAN_POINT('Ctrl Pts',(-69.6474913258684,13.4360729203444,
0.));
#147382=CARTESIAN_POINT('Ctrl Pts',(-69.6283131470267,13.425718376534,0.));
#147383=CARTESIAN_POINT('Ctrl Pts',(-69.6091665241743,13.4154062128998,
0.));
#147384=CARTESIAN_POINT('Ctrl Pts',(-69.5900516264524,13.4051364358495,
0.));
#147385=CARTESIAN_POINT('Ctrl Pts',(-69.5709686238701,13.3949090517173,
0.));
#147386=CARTESIAN_POINT('Ctrl Pts',(-69.5519176872857,13.3847240667627,
0.));
#147387=CARTESIAN_POINT('Ctrl Pts',(-69.5328989883899,13.3745814871668,
0.));
#147388=CARTESIAN_POINT('Ctrl Pts',(-69.5139126996703,13.3644813190225,
0.));
#147389=CARTESIAN_POINT('Ctrl Pts',(-69.4949589944633,13.3544235683399,
0.));
#147390=CARTESIAN_POINT('Ctrl Pts',(-69.4760380470382,13.3444082410547,
0.));
#147391=CARTESIAN_POINT('Ctrl Pts',(-69.4571500326673,13.3344353430313,
0.));
#147392=CARTESIAN_POINT('Ctrl Pts',(-69.4382951276983,13.3245048800641,
0.));
#147393=CARTESIAN_POINT('Ctrl Pts',(-69.4194735096238,13.3146168578739,
0.));
#147394=CARTESIAN_POINT('Ctrl Pts',(-69.4006853569485,13.3047712821046,
0.));
#147395=CARTESIAN_POINT('Ctrl Pts',(-69.3819308490407,13.2949681583165,
0.));
#147396=CARTESIAN_POINT('Ctrl Pts',(-69.3632101660071,13.2852074919767,
0.));
#147397=CARTESIAN_POINT('Ctrl Pts',(-69.3445234885088,13.2754892884438,
0.));
#147398=CARTESIAN_POINT('Ctrl Pts',(-69.3258709977416,13.2658135529616,
0.));
#147399=CARTESIAN_POINT('Ctrl Pts',(-69.3072528758546,13.2561802906901,
0.));
#147400=CARTESIAN_POINT('Ctrl Pts',(-69.2886693063193,13.2465895067264,
0.));
#147401=CARTESIAN_POINT('Ctrl Pts',(-69.2701204742435,13.2370412061218,
0.));
#147402=CARTESIAN_POINT('Ctrl Pts',(-69.2516065668809,13.2275353939044,
0.));
#147403=CARTESIAN_POINT('Ctrl Pts',(-69.2331277732819,13.2180720750586,
0.));
#147404=CARTESIAN_POINT('Ctrl Pts',(-69.2146842833506,13.2086512544729,
0.));
#147405=CARTESIAN_POINT('Ctrl Pts',(-69.1962762870524,13.1992729368928,
0.));
#147406=CARTESIAN_POINT('Ctrl Pts',(-69.1779039736026,13.189937126869,0.));
#147407=CARTESIAN_POINT('Ctrl Pts',(-69.1595675305294,13.1806438286944,
0.));
#147408=CARTESIAN_POINT('Ctrl Pts',(-69.141267145461,13.1713930465142,0.));
#147409=CARTESIAN_POINT('Ctrl Pts',(-69.1230030082598,13.1621847844533,
0.));
#147410=CARTESIAN_POINT('Ctrl Pts',(-69.1047753127633,13.1530190467181,
0.));
#147411=CARTESIAN_POINT('Ctrl Pts',(-69.0865842593063,13.1438958377397,
0.));
#147412=CARTESIAN_POINT('Ctrl Pts',(-69.0684300549426,13.1348151621825,
0.));
#147413=CARTESIAN_POINT('Ctrl Pts',(-69.0503129081778,13.1257770246379,
0.));
#147414=CARTESIAN_POINT('Ctrl Pts',(-69.0322330243336,13.1167814293496,
0.));
#147415=CARTESIAN_POINT('Ctrl Pts',(-69.0141906015137,13.1078283799726,
0.));
#147416=CARTESIAN_POINT('Ctrl Pts',(-68.9961858241577,13.0989178791843,
0.));
#147417=CARTESIAN_POINT('Ctrl Pts',(-68.9782188692654,13.0900499290542,
0.));
#147418=CARTESIAN_POINT('Ctrl Pts',(-68.9602899187628,13.0812245317816,
0.));
#147419=CARTESIAN_POINT('Ctrl Pts',(-68.9423991694492,13.072441690283,0.));
#147420=CARTESIAN_POINT('Ctrl Pts',(-68.9245468449865,13.0637014089018,
0.));
#147421=CARTESIAN_POINT('Ctrl Pts',(-68.9067332040842,13.0550036938793,
0.));
#147422=CARTESIAN_POINT('Ctrl Pts',(-68.8889585151431,13.0463485518185,
0.));
#147423=CARTESIAN_POINT('Ctrl Pts',(-68.8712230321823,13.0377359881864,
0.));
#147424=CARTESIAN_POINT('Ctrl Pts',(-68.853526972687,13.0291660060118,0.));
#147425=CARTESIAN_POINT('Ctrl Pts',(-68.835870488774,13.0206386039729,0.));
#147426=CARTESIAN_POINT('Ctrl Pts',(-68.8182536654066,13.0121537769003,
0.));
#147427=CARTESIAN_POINT('Ctrl Pts',(-68.8041919669403,13.0053999700929,
0.));
#147428=CARTESIAN_POINT('Ctrl Pts',(-68.7936635625787,13.0003537683089,
0.));
#147429=CARTESIAN_POINT('Ctrl Pts',(-68.7866525680284,12.996998146029,0.));
#147430=CARTESIAN_POINT('Ctrl Pts',(-68.7831490561748,12.9953224629497,
0.));
#147431=CARTESIAN_POINT('Ctrl Pts',(-71.2372871136137,21.8059378310719,
0.));
#147432=CARTESIAN_POINT('Ctrl Pts',(-71.2372871136137,21.8059378310719,
12.));
#147433=CARTESIAN_POINT('Ctrl Pts',(-71.2331134397872,21.8022104901727,
0.));
#147434=CARTESIAN_POINT('Ctrl Pts',(-71.2331134397872,21.8022104901727,
12.));
#147435=CARTESIAN_POINT('Ctrl Pts',(-71.2247670210176,21.794759979896,0.));
#147436=CARTESIAN_POINT('Ctrl Pts',(-71.2247670210176,21.794759979896,12.));
#147437=CARTESIAN_POINT('Ctrl Pts',(-71.2122501795138,21.7835967290463,
0.));
#147438=CARTESIAN_POINT('Ctrl Pts',(-71.2122501795138,21.7835967290463,
12.));
#147439=CARTESIAN_POINT('Ctrl Pts',(-71.1955666310295,21.7687374247287,
0.));
#147440=CARTESIAN_POINT('Ctrl Pts',(-71.1955666310295,21.7687374247287,
12.));
#147441=CARTESIAN_POINT('Ctrl Pts',(-71.1747214906585,21.750205018381,0.));
#147442=CARTESIAN_POINT('Ctrl Pts',(-71.1747214906585,21.750205018381,12.));
#147443=CARTESIAN_POINT('Ctrl Pts',(-71.1538856612261,21.7317143472951,
0.));
#147444=CARTESIAN_POINT('Ctrl Pts',(-71.1538856612261,21.7317143472951,
12.));
#147445=CARTESIAN_POINT('Ctrl Pts',(-71.1330591726507,21.7132654262531,
0.));
#147446=CARTESIAN_POINT('Ctrl Pts',(-71.1330591726507,21.7132654262531,
12.));
#147447=CARTESIAN_POINT('Ctrl Pts',(-71.1122420728217,21.694858273085,0.));
#147448=CARTESIAN_POINT('Ctrl Pts',(-71.1122420728217,21.694858273085,12.));
#147449=CARTESIAN_POINT('Ctrl Pts',(-71.0914344332798,21.6764929081677,
0.));
#147450=CARTESIAN_POINT('Ctrl Pts',(-71.0914344332798,21.6764929081677,
12.));
#147451=CARTESIAN_POINT('Ctrl Pts',(-71.0706363472704,21.6581693538335,
0.));
#147452=CARTESIAN_POINT('Ctrl Pts',(-71.0706363472704,21.6581693538335,
12.));
#147453=CARTESIAN_POINT('Ctrl Pts',(-71.0498479219467,21.639887633714,0.));
#147454=CARTESIAN_POINT('Ctrl Pts',(-71.0498479219467,21.639887633714,12.));
#147455=CARTESIAN_POINT('Ctrl Pts',(-71.0290692721848,21.6216477720912,
0.));
#147456=CARTESIAN_POINT('Ctrl Pts',(-71.0290692721848,21.6216477720912,
12.));
#147457=CARTESIAN_POINT('Ctrl Pts',(-71.0083005139107,21.6034497932581,
0.));
#147458=CARTESIAN_POINT('Ctrl Pts',(-71.0083005139107,21.6034497932581,
12.));
#147459=CARTESIAN_POINT('Ctrl Pts',(-70.987541757223,21.585293720829,0.));
#147460=CARTESIAN_POINT('Ctrl Pts',(-70.987541757223,21.585293720829,12.));
#147461=CARTESIAN_POINT('Ctrl Pts',(-70.9667931008215,21.5671795771913,
0.));
#147462=CARTESIAN_POINT('Ctrl Pts',(-70.9667931008215,21.5671795771913,
12.));
#147463=CARTESIAN_POINT('Ctrl Pts',(-70.94605463587,21.5491073839106,0.));
#147464=CARTESIAN_POINT('Ctrl Pts',(-70.94605463587,21.5491073839106,12.));
#147465=CARTESIAN_POINT('Ctrl Pts',(-70.9253264487637,21.531077162023,0.));
#147466=CARTESIAN_POINT('Ctrl Pts',(-70.9253264487637,21.531077162023,12.));
#147467=CARTESIAN_POINT('Ctrl Pts',(-70.9046086244131,21.513088932377,0.));
#147468=CARTESIAN_POINT('Ctrl Pts',(-70.9046086244131,21.513088932377,12.));
#147469=CARTESIAN_POINT('Ctrl Pts',(-70.8839012490871,21.4951427159261,
0.));
#147470=CARTESIAN_POINT('Ctrl Pts',(-70.8839012490871,21.4951427159261,
12.));
#147471=CARTESIAN_POINT('Ctrl Pts',(-70.8632044140112,21.477238534096,0.));
#147472=CARTESIAN_POINT('Ctrl Pts',(-70.8632044140112,21.477238534096,12.));
#147473=CARTESIAN_POINT('Ctrl Pts',(-70.8425182149846,21.4593764087473,
0.));
#147474=CARTESIAN_POINT('Ctrl Pts',(-70.8425182149846,21.4593764087473,
12.));
#147475=CARTESIAN_POINT('Ctrl Pts',(-70.8218427507506,21.4415563620114,
0.));
#147476=CARTESIAN_POINT('Ctrl Pts',(-70.8218427507506,21.4415563620114,
12.));
#147477=CARTESIAN_POINT('Ctrl Pts',(-70.8011781217394,21.4237784161587,
0.));
#147478=CARTESIAN_POINT('Ctrl Pts',(-70.8011781217394,21.4237784161587,
12.));
#147479=CARTESIAN_POINT('Ctrl Pts',(-70.780524428745,21.4060425934598,0.));
#147480=CARTESIAN_POINT('Ctrl Pts',(-70.780524428745,21.4060425934598,12.));
#147481=CARTESIAN_POINT('Ctrl Pts',(-70.7598817714105,21.3883489160196,
0.));
#147482=CARTESIAN_POINT('Ctrl Pts',(-70.7598817714105,21.3883489160196,
12.));
#147483=CARTESIAN_POINT('Ctrl Pts',(-70.7392502475469,21.3706974057039,
0.));
#147484=CARTESIAN_POINT('Ctrl Pts',(-70.7392502475469,21.3706974057039,
12.));
#147485=CARTESIAN_POINT('Ctrl Pts',(-70.7186299539724,21.3530880842349,
0.));
#147486=CARTESIAN_POINT('Ctrl Pts',(-70.7186299539724,21.3530880842349,
12.));
#147487=CARTESIAN_POINT('Ctrl Pts',(-70.6980209870045,21.3355209732443,
0.));
#147488=CARTESIAN_POINT('Ctrl Pts',(-70.6980209870045,21.3355209732443,
12.));
#147489=CARTESIAN_POINT('Ctrl Pts',(-70.6774234430897,21.3179960943388,
0.));
#147490=CARTESIAN_POINT('Ctrl Pts',(-70.6774234430897,21.3179960943388,
12.));
#147491=CARTESIAN_POINT('Ctrl Pts',(-70.6568374193774,21.300513469156,0.));
#147492=CARTESIAN_POINT('Ctrl Pts',(-70.6568374193774,21.300513469156,12.));
#147493=CARTESIAN_POINT('Ctrl Pts',(-70.6362630143047,21.2830731194183,
0.));
#147494=CARTESIAN_POINT('Ctrl Pts',(-70.6362630143047,21.2830731194183,
12.));
#147495=CARTESIAN_POINT('Ctrl Pts',(-70.6157003273316,21.2656750669126,
0.));
#147496=CARTESIAN_POINT('Ctrl Pts',(-70.6157003273316,21.2656750669126,
12.));
#147497=CARTESIAN_POINT('Ctrl Pts',(-70.5951494586957,21.2483193334675,
0.));
#147498=CARTESIAN_POINT('Ctrl Pts',(-70.5951494586957,21.2483193334675,
12.));
#147499=CARTESIAN_POINT('Ctrl Pts',(-70.5746105091502,21.2310059409265,
0.));
#147500=CARTESIAN_POINT('Ctrl Pts',(-70.5746105091502,21.2310059409265,
12.));
#147501=CARTESIAN_POINT('Ctrl Pts',(-70.5540835797283,21.2137349111208,
0.));
#147502=CARTESIAN_POINT('Ctrl Pts',(-70.5540835797283,21.2137349111208,
12.));
#147503=CARTESIAN_POINT('Ctrl Pts',(-70.5335687714429,21.1965062658298,
0.));
#147504=CARTESIAN_POINT('Ctrl Pts',(-70.5335687714429,21.1965062658298,
12.));
#147505=CARTESIAN_POINT('Ctrl Pts',(-70.5130661852955,21.1793200267846,
0.));
#147506=CARTESIAN_POINT('Ctrl Pts',(-70.5130661852955,21.1793200267846,
12.));
#147507=CARTESIAN_POINT('Ctrl Pts',(-70.4925759224216,21.1621762156897,
0.));
#147508=CARTESIAN_POINT('Ctrl Pts',(-70.4925759224216,21.1621762156897,
12.));
#147509=CARTESIAN_POINT('Ctrl Pts',(-70.4720980841939,21.1450748542336,
0.));
#147510=CARTESIAN_POINT('Ctrl Pts',(-70.4720980841939,21.1450748542336,
12.));
#147511=CARTESIAN_POINT('Ctrl Pts',(-70.4516327723346,21.1280159641002,
0.));
#147512=CARTESIAN_POINT('Ctrl Pts',(-70.4516327723346,21.1280159641002,
12.));
#147513=CARTESIAN_POINT('Ctrl Pts',(-70.4311800890402,21.1109995669747,
0.));
#147514=CARTESIAN_POINT('Ctrl Pts',(-70.4311800890402,21.1109995669747,
12.));
#147515=CARTESIAN_POINT('Ctrl Pts',(-70.4107401370389,21.0940256845472,
0.));
#147516=CARTESIAN_POINT('Ctrl Pts',(-70.4107401370389,21.0940256845472,
12.));
#147517=CARTESIAN_POINT('Ctrl Pts',(-70.3903130195265,21.0770943385141,
0.));
#147518=CARTESIAN_POINT('Ctrl Pts',(-70.3903130195265,21.0770943385141,
12.));
#147519=CARTESIAN_POINT('Ctrl Pts',(-70.3698988401281,21.0602055505748,
0.));
#147520=CARTESIAN_POINT('Ctrl Pts',(-70.3698988401281,21.0602055505748,
12.));
#147521=CARTESIAN_POINT('Ctrl Pts',(-70.3494977028498,21.0433593424266,
0.));
#147522=CARTESIAN_POINT('Ctrl Pts',(-70.3494977028498,21.0433593424266,
12.));
#147523=CARTESIAN_POINT('Ctrl Pts',(-70.3291097120302,21.0265557357548,
0.));
#147524=CARTESIAN_POINT('Ctrl Pts',(-70.3291097120302,21.0265557357548,
12.));
#147525=CARTESIAN_POINT('Ctrl Pts',(-70.3087349722973,21.0097947522218,
0.));
#147526=CARTESIAN_POINT('Ctrl Pts',(-70.3087349722973,21.0097947522218,
12.));
#147527=CARTESIAN_POINT('Ctrl Pts',(-70.2883735885984,20.9930764134776,
0.));
#147528=CARTESIAN_POINT('Ctrl Pts',(-70.2883735885984,20.9930764134776,
12.));
#147529=CARTESIAN_POINT('Ctrl Pts',(-70.2680256662224,20.9764007411652,
0.));
#147530=CARTESIAN_POINT('Ctrl Pts',(-70.2680256662224,20.9764007411652,
12.));
#147531=CARTESIAN_POINT('Ctrl Pts',(-70.2476913108244,20.9597677569228,
0.));
#147532=CARTESIAN_POINT('Ctrl Pts',(-70.2476913108244,20.9597677569228,
12.));
#147533=CARTESIAN_POINT('Ctrl Pts',(-70.2273706284472,20.9431774823831,
0.));
#147534=CARTESIAN_POINT('Ctrl Pts',(-70.2273706284472,20.9431774823831,
12.));
#147535=CARTESIAN_POINT('Ctrl Pts',(-70.2070637255458,20.9266299391684,
0.));
#147536=CARTESIAN_POINT('Ctrl Pts',(-70.2070637255458,20.9266299391684,
12.));
#147537=CARTESIAN_POINT('Ctrl Pts',(-70.1867707089854,20.9101251488943,
0.));
#147538=CARTESIAN_POINT('Ctrl Pts',(-70.1867707089854,20.9101251488943,
12.));
#147539=CARTESIAN_POINT('Ctrl Pts',(-70.1664916860358,20.8936631331748,
0.));
#147540=CARTESIAN_POINT('Ctrl Pts',(-70.1664916860358,20.8936631331748,
12.));
#147541=CARTESIAN_POINT('Ctrl Pts',(-70.1462267643647,20.8772439136206,
0.));
#147542=CARTESIAN_POINT('Ctrl Pts',(-70.1462267643647,20.8772439136206,
12.));
#147543=CARTESIAN_POINT('Ctrl Pts',(-70.1259760520309,20.8608675118378,
0.));
#147544=CARTESIAN_POINT('Ctrl Pts',(-70.1259760520309,20.8608675118378,
12.));
#147545=CARTESIAN_POINT('Ctrl Pts',(-70.1057396574747,20.8445339494187,
0.));
#147546=CARTESIAN_POINT('Ctrl Pts',(-70.1057396574747,20.8445339494187,
12.));
#147547=CARTESIAN_POINT('Ctrl Pts',(-70.0855176895191,20.8282432479428,
0.));
#147548=CARTESIAN_POINT('Ctrl Pts',(-70.0855176895191,20.8282432479428,
12.));
#147549=CARTESIAN_POINT('Ctrl Pts',(-70.0653102573803,20.8119954289848,
0.));
#147550=CARTESIAN_POINT('Ctrl Pts',(-70.0653102573803,20.8119954289848,
12.));
#147551=CARTESIAN_POINT('Ctrl Pts',(-70.0451174706741,20.7957905141156,
0.));
#147552=CARTESIAN_POINT('Ctrl Pts',(-70.0451174706741,20.7957905141156,
12.));
#147553=CARTESIAN_POINT('Ctrl Pts',(-70.024939439422,20.7796285249022,0.));
#147554=CARTESIAN_POINT('Ctrl Pts',(-70.024939439422,20.7796285249022,12.));
#147555=CARTESIAN_POINT('Ctrl Pts',(-70.0047762740568,20.7635094829015,
0.));
#147556=CARTESIAN_POINT('Ctrl Pts',(-70.0047762740568,20.7635094829015,
12.));
#147557=CARTESIAN_POINT('Ctrl Pts',(-69.9846280854257,20.7474334096581,
0.));
#147558=CARTESIAN_POINT('Ctrl Pts',(-69.9846280854257,20.7474334096581,
12.));
#147559=CARTESIAN_POINT('Ctrl Pts',(-69.9644949847934,20.7314003267119,
0.));
#147560=CARTESIAN_POINT('Ctrl Pts',(-69.9644949847934,20.7314003267119,
12.));
#147561=CARTESIAN_POINT('Ctrl Pts',(-69.9443770838448,20.7154102555997,
0.));
#147562=CARTESIAN_POINT('Ctrl Pts',(-69.9443770838448,20.7154102555997,
12.));
#147563=CARTESIAN_POINT('Ctrl Pts',(-69.9242744946854,20.6994632178551,
0.));
#147564=CARTESIAN_POINT('Ctrl Pts',(-69.9242744946854,20.6994632178551,
12.));
#147565=CARTESIAN_POINT('Ctrl Pts',(-69.904187329841,20.683559235003,0.));
#147566=CARTESIAN_POINT('Ctrl Pts',(-69.904187329841,20.683559235003,12.));
#147567=CARTESIAN_POINT('Ctrl Pts',(-69.8841157022568,20.667698328554,0.));
#147568=CARTESIAN_POINT('Ctrl Pts',(-69.8841157022568,20.667698328554,12.));
#147569=CARTESIAN_POINT('Ctrl Pts',(-69.8640597253045,20.6518805200129,
0.));
#147570=CARTESIAN_POINT('Ctrl Pts',(-69.8640597253045,20.6518805200129,
12.));
#147571=CARTESIAN_POINT('Ctrl Pts',(-69.8440195127866,20.636105830881,0.));
#147572=CARTESIAN_POINT('Ctrl Pts',(-69.8440195127866,20.636105830881,12.));
#147573=CARTESIAN_POINT('Ctrl Pts',(-69.8239951789402,20.6203742826566,
0.));
#147574=CARTESIAN_POINT('Ctrl Pts',(-69.8239951789402,20.6203742826566,
12.));
#147575=CARTESIAN_POINT('Ctrl Pts',(-69.8039868384389,20.6046858968307,
0.));
#147576=CARTESIAN_POINT('Ctrl Pts',(-69.8039868384389,20.6046858968307,
12.));
#147577=CARTESIAN_POINT('Ctrl Pts',(-69.7839946063949,20.5890406948811,
0.));
#147578=CARTESIAN_POINT('Ctrl Pts',(-69.7839946063949,20.5890406948811,
12.));
#147579=CARTESIAN_POINT('Ctrl Pts',(-69.7640185983644,20.5734386982782,
0.));
#147580=CARTESIAN_POINT('Ctrl Pts',(-69.7640185983644,20.5734386982782,
12.));
#147581=CARTESIAN_POINT('Ctrl Pts',(-69.744058930351,20.5578799284897,0.));
#147582=CARTESIAN_POINT('Ctrl Pts',(-69.744058930351,20.5578799284897,12.));
#147583=CARTESIAN_POINT('Ctrl Pts',(-69.7241157188083,20.5423644069799,
0.));
#147584=CARTESIAN_POINT('Ctrl Pts',(-69.7241157188083,20.5423644069799,
12.));
#147585=CARTESIAN_POINT('Ctrl Pts',(-69.7041890806425,20.5268921552077,
0.));
#147586=CARTESIAN_POINT('Ctrl Pts',(-69.7041890806425,20.5268921552077,
12.));
#147587=CARTESIAN_POINT('Ctrl Pts',(-69.6842791332115,20.5114631946184,
0.));
#147588=CARTESIAN_POINT('Ctrl Pts',(-69.6842791332115,20.5114631946184,
12.));
#147589=CARTESIAN_POINT('Ctrl Pts',(-69.6643859943308,20.4960775466492,
0.));
#147590=CARTESIAN_POINT('Ctrl Pts',(-69.6643859943308,20.4960775466492,
12.));
#147591=CARTESIAN_POINT('Ctrl Pts',(-69.6445097822792,20.480735232734,0.));
#147592=CARTESIAN_POINT('Ctrl Pts',(-69.6445097822792,20.480735232734,12.));
#147593=CARTESIAN_POINT('Ctrl Pts',(-69.6246506158013,20.4654362743037,
0.));
#147594=CARTESIAN_POINT('Ctrl Pts',(-69.6246506158013,20.4654362743037,
12.));
#147595=CARTESIAN_POINT('Ctrl Pts',(-69.6048086141113,20.4501806927851,
0.));
#147596=CARTESIAN_POINT('Ctrl Pts',(-69.6048086141113,20.4501806927851,
12.));
#147597=CARTESIAN_POINT('Ctrl Pts',(-69.5849838968928,20.4349685095923,
0.));
#147598=CARTESIAN_POINT('Ctrl Pts',(-69.5849838968928,20.4349685095923,
12.));
#147599=CARTESIAN_POINT('Ctrl Pts',(-69.5651765843033,20.41979974613,0.));
#147600=CARTESIAN_POINT('Ctrl Pts',(-69.5651765843033,20.41979974613,12.));
#147601=CARTESIAN_POINT('Ctrl Pts',(-69.5453867969804,20.4046744237999,
0.));
#147602=CARTESIAN_POINT('Ctrl Pts',(-69.5453867969804,20.4046744237999,
12.));
#147603=CARTESIAN_POINT('Ctrl Pts',(-69.5256146560441,20.3895925640005,
0.));
#147604=CARTESIAN_POINT('Ctrl Pts',(-69.5256146560441,20.3895925640005,
12.));
#147605=CARTESIAN_POINT('Ctrl Pts',(-69.5058602831008,20.3745541881268,
0.));
#147606=CARTESIAN_POINT('Ctrl Pts',(-69.5058602831008,20.3745541881268,
12.));
#147607=CARTESIAN_POINT('Ctrl Pts',(-69.4861238002441,20.3595593175623,
0.));
#147608=CARTESIAN_POINT('Ctrl Pts',(-69.4861238002441,20.3595593175623,
12.));
#147609=CARTESIAN_POINT('Ctrl Pts',(-69.4664053300587,20.3446079736802,
0.));
#147610=CARTESIAN_POINT('Ctrl Pts',(-69.4664053300587,20.3446079736802,
12.));
#147611=CARTESIAN_POINT('Ctrl Pts',(-69.4467049956262,20.3297001778507,
0.));
#147612=CARTESIAN_POINT('Ctrl Pts',(-69.4467049956262,20.3297001778507,
12.));
#147613=CARTESIAN_POINT('Ctrl Pts',(-69.4270229205297,20.3148359514415,
0.));
#147614=CARTESIAN_POINT('Ctrl Pts',(-69.4270229205297,20.3148359514415,
12.));
#147615=CARTESIAN_POINT('Ctrl Pts',(-69.407359228856,20.3000153158166,0.));
#147616=CARTESIAN_POINT('Ctrl Pts',(-69.407359228856,20.3000153158166,12.));
#147617=CARTESIAN_POINT('Ctrl Pts',(-69.3877140451975,20.2852382923299,
0.));
#147618=CARTESIAN_POINT('Ctrl Pts',(-69.3877140451975,20.2852382923299,
12.));
#147619=CARTESIAN_POINT('Ctrl Pts',(-69.368087494655,20.2705049023241,0.));
#147620=CARTESIAN_POINT('Ctrl Pts',(-69.368087494655,20.2705049023241,12.));
#147621=CARTESIAN_POINT('Ctrl Pts',(-69.3484797028458,20.2558151671391,
0.));
#147622=CARTESIAN_POINT('Ctrl Pts',(-69.3484797028458,20.2558151671391,
12.));
#147623=CARTESIAN_POINT('Ctrl Pts',(-69.3288907959067,20.2411691081123,
0.));
#147624=CARTESIAN_POINT('Ctrl Pts',(-69.3288907959067,20.2411691081123,
12.));
#147625=CARTESIAN_POINT('Ctrl Pts',(-69.3093209004984,20.2265667465784,
0.));
#147626=CARTESIAN_POINT('Ctrl Pts',(-69.3093209004984,20.2265667465784,
12.));
#147627=CARTESIAN_POINT('Ctrl Pts',(-69.2897701438059,20.212008103862,0.));
#147628=CARTESIAN_POINT('Ctrl Pts',(-69.2897701438059,20.212008103862,12.));
#147629=CARTESIAN_POINT('Ctrl Pts',(-69.2702386535422,20.1974932012773,
0.));
#147630=CARTESIAN_POINT('Ctrl Pts',(-69.2702386535422,20.1974932012773,
12.));
#147631=CARTESIAN_POINT('Ctrl Pts',(-69.2507265579554,20.1830220601348,
0.));
#147632=CARTESIAN_POINT('Ctrl Pts',(-69.2507265579554,20.1830220601348,
12.));
#147633=CARTESIAN_POINT('Ctrl Pts',(-69.2312339858335,20.1685947017433,
0.));
#147634=CARTESIAN_POINT('Ctrl Pts',(-69.2312339858335,20.1685947017433,
12.));
#147635=CARTESIAN_POINT('Ctrl Pts',(-69.2117610665076,20.1542111474087,
0.));
#147636=CARTESIAN_POINT('Ctrl Pts',(-69.2117610665076,20.1542111474087,
12.));
#147637=CARTESIAN_POINT('Ctrl Pts',(-69.1923079298538,20.1398714184279,
0.));
#147638=CARTESIAN_POINT('Ctrl Pts',(-69.1923079298538,20.1398714184279,
12.));
#147639=CARTESIAN_POINT('Ctrl Pts',(-69.1728747062963,20.1255755360872,
0.));
#147640=CARTESIAN_POINT('Ctrl Pts',(-69.1728747062963,20.1255755360872,
12.));
#147641=CARTESIAN_POINT('Ctrl Pts',(-69.1534615268153,20.1113235216694,
0.));
#147642=CARTESIAN_POINT('Ctrl Pts',(-69.1534615268153,20.1113235216694,
12.));
#147643=CARTESIAN_POINT('Ctrl Pts',(-69.1340685229515,20.0971153964557,
0.));
#147644=CARTESIAN_POINT('Ctrl Pts',(-69.1340685229515,20.0971153964557,
12.));
#147645=CARTESIAN_POINT('Ctrl Pts',(-69.1146958268104,20.0829511817251,
0.));
#147646=CARTESIAN_POINT('Ctrl Pts',(-69.1146958268104,20.0829511817251,
12.));
#147647=CARTESIAN_POINT('Ctrl Pts',(-69.095343571064,20.068830898748,0.));
#147648=CARTESIAN_POINT('Ctrl Pts',(-69.095343571064,20.068830898748,12.));
#147649=CARTESIAN_POINT('Ctrl Pts',(-69.0760118889535,20.0547545687842,
0.));
#147650=CARTESIAN_POINT('Ctrl Pts',(-69.0760118889535,20.0547545687842,
12.));
#147651=CARTESIAN_POINT('Ctrl Pts',(-69.0567009142978,20.0407222130905,
0.));
#147652=CARTESIAN_POINT('Ctrl Pts',(-69.0567009142978,20.0407222130905,
12.));
#147653=CARTESIAN_POINT('Ctrl Pts',(-69.0374107814984,20.0267338529223,
0.));
#147654=CARTESIAN_POINT('Ctrl Pts',(-69.0374107814984,20.0267338529223,
12.));
#147655=CARTESIAN_POINT('Ctrl Pts',(-69.0181416255431,20.0127895095326,
0.));
#147656=CARTESIAN_POINT('Ctrl Pts',(-69.0181416255431,20.0127895095326,
12.));
#147657=CARTESIAN_POINT('Ctrl Pts',(-68.9988935820084,19.9988892041666,
0.));
#147658=CARTESIAN_POINT('Ctrl Pts',(-68.9988935820084,19.9988892041666,
12.));
#147659=CARTESIAN_POINT('Ctrl Pts',(-68.9796667870638,19.9850329580591,
0.));
#147660=CARTESIAN_POINT('Ctrl Pts',(-68.9796667870638,19.9850329580591,
12.));
#147661=CARTESIAN_POINT('Ctrl Pts',(-68.9604613774802,19.9712207924428,
0.));
#147662=CARTESIAN_POINT('Ctrl Pts',(-68.9604613774802,19.9712207924428,
12.));
#147663=CARTESIAN_POINT('Ctrl Pts',(-68.9412774906333,19.9574527285488,
0.));
#147664=CARTESIAN_POINT('Ctrl Pts',(-68.9412774906333,19.9574527285488,
12.));
#147665=CARTESIAN_POINT('Ctrl Pts',(-68.9221152645095,19.9437287876066,
0.));
#147666=CARTESIAN_POINT('Ctrl Pts',(-68.9221152645095,19.9437287876066,
12.));
#147667=CARTESIAN_POINT('Ctrl Pts',(-68.9029748377067,19.9300489908374,
0.));
#147668=CARTESIAN_POINT('Ctrl Pts',(-68.9029748377067,19.9300489908374,
12.));
#147669=CARTESIAN_POINT('Ctrl Pts',(-68.8838563494393,19.9164133594525,
0.));
#147670=CARTESIAN_POINT('Ctrl Pts',(-68.8838563494393,19.9164133594525,
12.));
#147671=CARTESIAN_POINT('Ctrl Pts',(-68.8647599395469,19.9028219146618,
0.));
#147672=CARTESIAN_POINT('Ctrl Pts',(-68.8647599395469,19.9028219146618,
12.));
#147673=CARTESIAN_POINT('Ctrl Pts',(-68.8456857485002,19.8892746776739,
0.));
#147674=CARTESIAN_POINT('Ctrl Pts',(-68.8456857485002,19.8892746776739,
12.));
#147675=CARTESIAN_POINT('Ctrl Pts',(-68.8266339174056,19.8757716696965,
0.));
#147676=CARTESIAN_POINT('Ctrl Pts',(-68.8266339174056,19.8757716696965,
12.));
#147677=CARTESIAN_POINT('Ctrl Pts',(-68.8076045880065,19.8623129119293,
0.));
#147678=CARTESIAN_POINT('Ctrl Pts',(-68.8076045880065,19.8623129119293,
12.));
#147679=CARTESIAN_POINT('Ctrl Pts',(-68.7885979026879,19.8488984255627,
0.));
#147680=CARTESIAN_POINT('Ctrl Pts',(-68.7885979026879,19.8488984255627,
12.));
#147681=CARTESIAN_POINT('Ctrl Pts',(-68.7696140044851,19.8355282317858,
0.));
#147682=CARTESIAN_POINT('Ctrl Pts',(-68.7696140044851,19.8355282317858,
12.));
#147683=CARTESIAN_POINT('Ctrl Pts',(-68.7506530370904,19.822202351787,0.));
#147684=CARTESIAN_POINT('Ctrl Pts',(-68.7506530370904,19.822202351787,12.));
#147685=CARTESIAN_POINT('Ctrl Pts',(-68.7317151448573,19.8089208067537,
0.));
#147686=CARTESIAN_POINT('Ctrl Pts',(-68.7317151448573,19.8089208067537,
12.));
#147687=CARTESIAN_POINT('Ctrl Pts',(-68.7128004728034,19.7956836178651,
0.));
#147688=CARTESIAN_POINT('Ctrl Pts',(-68.7128004728034,19.7956836178651,
12.));
#147689=CARTESIAN_POINT('Ctrl Pts',(-68.693909166615,19.7824908062924,0.));
#147690=CARTESIAN_POINT('Ctrl Pts',(-68.693909166615,19.7824908062924,12.));
#147691=CARTESIAN_POINT('Ctrl Pts',(-68.6750413726575,19.7693423932066,
0.));
#147692=CARTESIAN_POINT('Ctrl Pts',(-68.6750413726575,19.7693423932066,
12.));
#147693=CARTESIAN_POINT('Ctrl Pts',(-68.65619723798,19.7562383997783,0.));
#147694=CARTESIAN_POINT('Ctrl Pts',(-68.65619723798,19.7562383997783,12.));
#147695=CARTESIAN_POINT('Ctrl Pts',(-68.6373769103211,19.7431788471772,
0.));
#147696=CARTESIAN_POINT('Ctrl Pts',(-68.6373769103211,19.7431788471772,
12.));
#147697=CARTESIAN_POINT('Ctrl Pts',(-68.6185805381102,19.7301637565645,
0.));
#147698=CARTESIAN_POINT('Ctrl Pts',(-68.6185805381102,19.7301637565645,
12.));
#147699=CARTESIAN_POINT('Ctrl Pts',(-68.5998082704741,19.717193149095,0.));
#147700=CARTESIAN_POINT('Ctrl Pts',(-68.5998082704741,19.717193149095,12.));
#147701=CARTESIAN_POINT('Ctrl Pts',(-68.5810602572474,19.7042670459233,
0.));
#147702=CARTESIAN_POINT('Ctrl Pts',(-68.5810602572474,19.7042670459233,
12.));
#147703=CARTESIAN_POINT('Ctrl Pts',(-68.5623366489776,19.6913854682046,
0.));
#147704=CARTESIAN_POINT('Ctrl Pts',(-68.5623366489776,19.6913854682046,
12.));
#147705=CARTESIAN_POINT('Ctrl Pts',(-68.543637596932,19.6785484370929,0.));
#147706=CARTESIAN_POINT('Ctrl Pts',(-68.543637596932,19.6785484370929,12.));
#147707=CARTESIAN_POINT('Ctrl Pts',(-68.5249632530994,19.665755973734,0.));
#147708=CARTESIAN_POINT('Ctrl Pts',(-68.5249632530994,19.665755973734,12.));
#147709=CARTESIAN_POINT('Ctrl Pts',(-68.5063137701986,19.6530080992689,
0.));
#147710=CARTESIAN_POINT('Ctrl Pts',(-68.5063137701986,19.6530080992689,
12.));
#147711=CARTESIAN_POINT('Ctrl Pts',(-68.4876893016863,19.6403048348396,
0.));
#147712=CARTESIAN_POINT('Ctrl Pts',(-68.4876893016863,19.6403048348396,
12.));
#147713=CARTESIAN_POINT('Ctrl Pts',(-68.4690900017631,19.6276462015888,
0.));
#147714=CARTESIAN_POINT('Ctrl Pts',(-68.4690900017631,19.6276462015888,
12.));
#147715=CARTESIAN_POINT('Ctrl Pts',(-68.4505160253777,19.6150322206577,
0.));
#147716=CARTESIAN_POINT('Ctrl Pts',(-68.4505160253777,19.6150322206577,
12.));
#147717=CARTESIAN_POINT('Ctrl Pts',(-68.4319675282273,19.6024629131785,
0.));
#147718=CARTESIAN_POINT('Ctrl Pts',(-68.4319675282273,19.6024629131785,
12.));
#147719=CARTESIAN_POINT('Ctrl Pts',(-68.4134446667695,19.5899383002803,
0.));
#147720=CARTESIAN_POINT('Ctrl Pts',(-68.4134446667695,19.5899383002803,
12.));
#147721=CARTESIAN_POINT('Ctrl Pts',(-68.3949475982334,19.5774584030938,
0.));
#147722=CARTESIAN_POINT('Ctrl Pts',(-68.3949475982334,19.5774584030938,
12.));
#147723=CARTESIAN_POINT('Ctrl Pts',(-68.3764764806287,19.5650232427516,
0.));
#147724=CARTESIAN_POINT('Ctrl Pts',(-68.3764764806287,19.5650232427516,
12.));
#147725=CARTESIAN_POINT('Ctrl Pts',(-68.3580314727522,19.5526328403851,
0.));
#147726=CARTESIAN_POINT('Ctrl Pts',(-68.3580314727522,19.5526328403851,
12.));
#147727=CARTESIAN_POINT('Ctrl Pts',(-68.3396127341937,19.540287217119,0.));
#147728=CARTESIAN_POINT('Ctrl Pts',(-68.3396127341937,19.540287217119,12.));
#147729=CARTESIAN_POINT('Ctrl Pts',(-68.3212204253416,19.5279863940772,
0.));
#147730=CARTESIAN_POINT('Ctrl Pts',(-68.3212204253416,19.5279863940772,
12.));
#147731=CARTESIAN_POINT('Ctrl Pts',(-68.3028547073862,19.5157303923855,
0.));
#147732=CARTESIAN_POINT('Ctrl Pts',(-68.3028547073862,19.5157303923855,
12.));
#147733=CARTESIAN_POINT('Ctrl Pts',(-68.2845157423234,19.5035192331706,
0.));
#147734=CARTESIAN_POINT('Ctrl Pts',(-68.2845157423234,19.5035192331706,
12.));
#147735=CARTESIAN_POINT('Ctrl Pts',(-68.2662036929531,19.4913529375545,
0.));
#147736=CARTESIAN_POINT('Ctrl Pts',(-68.2662036929531,19.4913529375545,
12.));
#147737=CARTESIAN_POINT('Ctrl Pts',(-68.2479187228815,19.4792315266505,
0.));
#147738=CARTESIAN_POINT('Ctrl Pts',(-68.2479187228815,19.4792315266505,
12.));
#147739=CARTESIAN_POINT('Ctrl Pts',(-68.2296609965461,19.4671550215724,
0.));
#147740=CARTESIAN_POINT('Ctrl Pts',(-68.2296609965461,19.4671550215724,
12.));
#147741=CARTESIAN_POINT('Ctrl Pts',(-68.2114306792366,19.4551234434383,
0.));
#147742=CARTESIAN_POINT('Ctrl Pts',(-68.2114306792366,19.4551234434383,
12.));
#147743=CARTESIAN_POINT('Ctrl Pts',(-68.1932279371121,19.4431368133718,
0.));
#147744=CARTESIAN_POINT('Ctrl Pts',(-68.1932279371121,19.4431368133718,
12.));
#147745=CARTESIAN_POINT('Ctrl Pts',(-68.1750529372211,19.4311951524977,
0.));
#147746=CARTESIAN_POINT('Ctrl Pts',(-68.1750529372211,19.4311951524977,
12.));
#147747=CARTESIAN_POINT('Ctrl Pts',(-68.1569058475026,19.419298481941,0.));
#147748=CARTESIAN_POINT('Ctrl Pts',(-68.1569058475026,19.419298481941,12.));
#147749=CARTESIAN_POINT('Ctrl Pts',(-68.1387868367668,19.4074468228293,
0.));
#147750=CARTESIAN_POINT('Ctrl Pts',(-68.1387868367668,19.4074468228293,
12.));
#147751=CARTESIAN_POINT('Ctrl Pts',(-68.1206960746763,19.3956401962893,
0.));
#147752=CARTESIAN_POINT('Ctrl Pts',(-68.1206960746763,19.3956401962893,
12.));
#147753=CARTESIAN_POINT('Ctrl Pts',(-68.1026337317298,19.3838786234425,
0.));
#147754=CARTESIAN_POINT('Ctrl Pts',(-68.1026337317298,19.3838786234425,
12.));
#147755=CARTESIAN_POINT('Ctrl Pts',(-68.0845999792274,19.372162125392,0.));
#147756=CARTESIAN_POINT('Ctrl Pts',(-68.0845999792274,19.372162125392,12.));
#147757=CARTESIAN_POINT('Ctrl Pts',(-68.0665949893222,19.3604907232322,
0.));
#147758=CARTESIAN_POINT('Ctrl Pts',(-68.0665949893222,19.3604907232322,
12.));
#147759=CARTESIAN_POINT('Ctrl Pts',(-68.0486189351027,19.3488644380646,
0.));
#147760=CARTESIAN_POINT('Ctrl Pts',(-68.0486189351027,19.3488644380646,
12.));
#147761=CARTESIAN_POINT('Ctrl Pts',(-68.0306719906636,19.3372832910076,
0.));
#147762=CARTESIAN_POINT('Ctrl Pts',(-68.0306719906636,19.3372832910076,
12.));
#147763=CARTESIAN_POINT('Ctrl Pts',(-68.0127543311761,19.3257473032031,
0.));
#147764=CARTESIAN_POINT('Ctrl Pts',(-68.0127543311761,19.3257473032031,
12.));
#147765=CARTESIAN_POINT('Ctrl Pts',(-67.9948661329592,19.3142564958195,
0.));
#147766=CARTESIAN_POINT('Ctrl Pts',(-67.9948661329592,19.3142564958195,
12.));
#147767=CARTESIAN_POINT('Ctrl Pts',(-67.977007573346,19.3028108900373,0.));
#147768=CARTESIAN_POINT('Ctrl Pts',(-67.977007573346,19.3028108900373,12.));
#147769=CARTESIAN_POINT('Ctrl Pts',(-67.959178830538,19.2914105070282,0.));
#147770=CARTESIAN_POINT('Ctrl Pts',(-67.959178830538,19.2914105070282,12.));
#147771=CARTESIAN_POINT('Ctrl Pts',(-67.9413800834798,19.2800553679362,
0.));
#147772=CARTESIAN_POINT('Ctrl Pts',(-67.9413800834798,19.2800553679362,
12.));
#147773=CARTESIAN_POINT('Ctrl Pts',(-67.9236115116781,19.2687454938448,
0.));
#147774=CARTESIAN_POINT('Ctrl Pts',(-67.9236115116781,19.2687454938448,
12.));
#147775=CARTESIAN_POINT('Ctrl Pts',(-67.9058732951822,19.2574809057705,
0.));
#147776=CARTESIAN_POINT('Ctrl Pts',(-67.9058732951822,19.2574809057705,
12.));
#147777=CARTESIAN_POINT('Ctrl Pts',(-67.8881656149983,19.2462616247287,
0.));
#147778=CARTESIAN_POINT('Ctrl Pts',(-67.8881656149983,19.2462616247287,
12.));
#147779=CARTESIAN_POINT('Ctrl Pts',(-67.8704886534555,19.2350876717877,
0.));
#147780=CARTESIAN_POINT('Ctrl Pts',(-67.8704886534555,19.2350876717877,
12.));
#147781=CARTESIAN_POINT('Ctrl Pts',(-67.852842594517,19.2239590681129,0.));
#147782=CARTESIAN_POINT('Ctrl Pts',(-67.852842594517,19.2239590681129,12.));
#147783=CARTESIAN_POINT('Ctrl Pts',(-67.8352276242856,19.2128758350336,
0.));
#147784=CARTESIAN_POINT('Ctrl Pts',(-67.8352276242856,19.2128758350336,
12.));
#147785=CARTESIAN_POINT('Ctrl Pts',(-67.817643930658,19.2018379939918,0.));
#147786=CARTESIAN_POINT('Ctrl Pts',(-67.817643930658,19.2018379939918,12.));
#147787=CARTESIAN_POINT('Ctrl Pts',(-67.8000917023896,19.1908455664089,
0.));
#147788=CARTESIAN_POINT('Ctrl Pts',(-67.8000917023896,19.1908455664089,
12.));
#147789=CARTESIAN_POINT('Ctrl Pts',(-67.7825711283092,19.1798985735687,
0.));
#147790=CARTESIAN_POINT('Ctrl Pts',(-67.7825711283092,19.1798985735687,
12.));
#147791=CARTESIAN_POINT('Ctrl Pts',(-67.7650823965156,19.1689970364958,
0.));
#147792=CARTESIAN_POINT('Ctrl Pts',(-67.7650823965156,19.1689970364958,
12.));
#147793=CARTESIAN_POINT('Ctrl Pts',(-67.7476256934493,19.1581409758112,
0.));
#147794=CARTESIAN_POINT('Ctrl Pts',(-67.7476256934493,19.1581409758112,
12.));
#147795=CARTESIAN_POINT('Ctrl Pts',(-67.730201205663,19.1473304119968,0.));
#147796=CARTESIAN_POINT('Ctrl Pts',(-67.730201205663,19.1473304119968,12.));
#147797=CARTESIAN_POINT('Ctrl Pts',(-67.7128091219372,19.1365653657097,
0.));
#147798=CARTESIAN_POINT('Ctrl Pts',(-67.7128091219372,19.1365653657097,
12.));
#147799=CARTESIAN_POINT('Ctrl Pts',(-67.6954496350053,19.1258458580343,
0.));
#147800=CARTESIAN_POINT('Ctrl Pts',(-67.6954496350053,19.1258458580343,
12.));
#147801=CARTESIAN_POINT('Ctrl Pts',(-67.6781229440535,19.115171910845,0.));
#147802=CARTESIAN_POINT('Ctrl Pts',(-67.6781229440535,19.115171910845,12.));
#147803=CARTESIAN_POINT('Ctrl Pts',(-67.6608292549412,19.1045435468344,
0.));
#147804=CARTESIAN_POINT('Ctrl Pts',(-67.6608292549412,19.1045435468344,
12.));
#147805=CARTESIAN_POINT('Ctrl Pts',(-67.6435687749803,19.0939607887491,
0.));
#147806=CARTESIAN_POINT('Ctrl Pts',(-67.6435687749803,19.0939607887491,
12.));
#147807=CARTESIAN_POINT('Ctrl Pts',(-67.6263417083414,19.0834236587115,
0.));
#147808=CARTESIAN_POINT('Ctrl Pts',(-67.6263417083414,19.0834236587115,
12.));
#147809=CARTESIAN_POINT('Ctrl Pts',(-67.6091482520558,19.0729321776286,
0.));
#147810=CARTESIAN_POINT('Ctrl Pts',(-67.6091482520558,19.0729321776286,
12.));
#147811=CARTESIAN_POINT('Ctrl Pts',(-67.5919885896278,19.0624863642425,
0.));
#147812=CARTESIAN_POINT('Ctrl Pts',(-67.5919885896278,19.0624863642425,
12.));
#147813=CARTESIAN_POINT('Ctrl Pts',(-67.5748628972035,19.0520862360413,
0.));
#147814=CARTESIAN_POINT('Ctrl Pts',(-67.5748628972035,19.0520862360413,
12.));
#147815=CARTESIAN_POINT('Ctrl Pts',(-67.5577713558248,19.0417318110721,
0.));
#147816=CARTESIAN_POINT('Ctrl Pts',(-67.5577713558248,19.0417318110721,
12.));
#147817=CARTESIAN_POINT('Ctrl Pts',(-67.5407141612881,19.0314231093923,
0.));
#147818=CARTESIAN_POINT('Ctrl Pts',(-67.5407141612881,19.0314231093923,
12.));
#147819=CARTESIAN_POINT('Ctrl Pts',(-67.5236915360253,19.0211601548222,
0.));
#147820=CARTESIAN_POINT('Ctrl Pts',(-67.5236915360253,19.0211601548222,
12.));
#147821=CARTESIAN_POINT('Ctrl Pts',(-67.5067037372177,19.0109429761274,
0.));
#147822=CARTESIAN_POINT('Ctrl Pts',(-67.5067037372177,19.0109429761274,
12.));
#147823=CARTESIAN_POINT('Ctrl Pts',(-67.4897510316692,19.0007716032784,
0.));
#147824=CARTESIAN_POINT('Ctrl Pts',(-67.4897510316692,19.0007716032784,
12.));
#147825=CARTESIAN_POINT('Ctrl Pts',(-67.4728336719559,18.9906460638607,
0.));
#147826=CARTESIAN_POINT('Ctrl Pts',(-67.4728336719559,18.9906460638607,
12.));
#147827=CARTESIAN_POINT('Ctrl Pts',(-67.4559518744714,18.9805663798466,
0.));
#147828=CARTESIAN_POINT('Ctrl Pts',(-67.4559518744714,18.9805663798466,
12.));
#147829=CARTESIAN_POINT('Ctrl Pts',(-67.4391057908687,18.9705325631772,
0.));
#147830=CARTESIAN_POINT('Ctrl Pts',(-67.4391057908687,18.9705325631772,
12.));
#147831=CARTESIAN_POINT('Ctrl Pts',(-67.4222955062385,18.9605446161078,
0.));
#147832=CARTESIAN_POINT('Ctrl Pts',(-67.4222955062385,18.9605446161078,
12.));
#147833=CARTESIAN_POINT('Ctrl Pts',(-67.4088759498287,18.9525909518002,
0.));
#147834=CARTESIAN_POINT('Ctrl Pts',(-67.4088759498287,18.9525909518002,
12.));
#147835=CARTESIAN_POINT('Ctrl Pts',(-67.398827414689,18.9466463414354,0.));
#147836=CARTESIAN_POINT('Ctrl Pts',(-67.398827414689,18.9466463414354,12.));
#147837=CARTESIAN_POINT('Ctrl Pts',(-67.3921355608417,18.942692439874,0.));
#147838=CARTESIAN_POINT('Ctrl Pts',(-67.3921355608417,18.942692439874,12.));
#147839=CARTESIAN_POINT('Ctrl Pts',(-67.3887914263119,18.9407177820969,
0.));
#147840=CARTESIAN_POINT('Ctrl Pts',(-67.3887914263119,18.9407177820969,
12.));
#147841=CARTESIAN_POINT('',(-67.3887914263119,18.9407177820969,12.));
#147842=CARTESIAN_POINT('Ctrl Pts',(-67.3887914263119,18.9407177820969,
12.));
#147843=CARTESIAN_POINT('Ctrl Pts',(-67.3921355608417,18.942692439874,12.));
#147844=CARTESIAN_POINT('Ctrl Pts',(-67.398827414689,18.9466463414354,12.));
#147845=CARTESIAN_POINT('Ctrl Pts',(-67.4088759498287,18.9525909518002,
12.));
#147846=CARTESIAN_POINT('Ctrl Pts',(-67.4222955062385,18.9605446161078,
12.));
#147847=CARTESIAN_POINT('Ctrl Pts',(-67.4391057908687,18.9705325631772,
12.));
#147848=CARTESIAN_POINT('Ctrl Pts',(-67.4559518744714,18.9805663798466,
12.));
#147849=CARTESIAN_POINT('Ctrl Pts',(-67.4728336719559,18.9906460638607,
12.));
#147850=CARTESIAN_POINT('Ctrl Pts',(-67.4897510316692,19.0007716032784,
12.));
#147851=CARTESIAN_POINT('Ctrl Pts',(-67.5067037372177,19.0109429761274,
12.));
#147852=CARTESIAN_POINT('Ctrl Pts',(-67.5236915360253,19.0211601548222,
12.));
#147853=CARTESIAN_POINT('Ctrl Pts',(-67.5407141612881,19.0314231093923,
12.));
#147854=CARTESIAN_POINT('Ctrl Pts',(-67.5577713558248,19.0417318110721,
12.));
#147855=CARTESIAN_POINT('Ctrl Pts',(-67.5748628972035,19.0520862360413,
12.));
#147856=CARTESIAN_POINT('Ctrl Pts',(-67.5919885896278,19.0624863642425,
12.));
#147857=CARTESIAN_POINT('Ctrl Pts',(-67.6091482520558,19.0729321776286,
12.));
#147858=CARTESIAN_POINT('Ctrl Pts',(-67.6263417083414,19.0834236587115,
12.));
#147859=CARTESIAN_POINT('Ctrl Pts',(-67.6435687749803,19.0939607887491,
12.));
#147860=CARTESIAN_POINT('Ctrl Pts',(-67.6608292549412,19.1045435468344,
12.));
#147861=CARTESIAN_POINT('Ctrl Pts',(-67.6781229440535,19.115171910845,12.));
#147862=CARTESIAN_POINT('Ctrl Pts',(-67.6954496350053,19.1258458580343,
12.));
#147863=CARTESIAN_POINT('Ctrl Pts',(-67.7128091219372,19.1365653657097,
12.));
#147864=CARTESIAN_POINT('Ctrl Pts',(-67.730201205663,19.1473304119968,12.));
#147865=CARTESIAN_POINT('Ctrl Pts',(-67.7476256934493,19.1581409758112,
12.));
#147866=CARTESIAN_POINT('Ctrl Pts',(-67.7650823965156,19.1689970364958,
12.));
#147867=CARTESIAN_POINT('Ctrl Pts',(-67.7825711283092,19.1798985735687,
12.));
#147868=CARTESIAN_POINT('Ctrl Pts',(-67.8000917023896,19.1908455664089,
12.));
#147869=CARTESIAN_POINT('Ctrl Pts',(-67.817643930658,19.2018379939918,12.));
#147870=CARTESIAN_POINT('Ctrl Pts',(-67.8352276242856,19.2128758350336,
12.));
#147871=CARTESIAN_POINT('Ctrl Pts',(-67.852842594517,19.2239590681129,12.));
#147872=CARTESIAN_POINT('Ctrl Pts',(-67.8704886534555,19.2350876717877,
12.));
#147873=CARTESIAN_POINT('Ctrl Pts',(-67.8881656149983,19.2462616247287,
12.));
#147874=CARTESIAN_POINT('Ctrl Pts',(-67.9058732951822,19.2574809057705,
12.));
#147875=CARTESIAN_POINT('Ctrl Pts',(-67.9236115116781,19.2687454938448,
12.));
#147876=CARTESIAN_POINT('Ctrl Pts',(-67.9413800834798,19.2800553679362,
12.));
#147877=CARTESIAN_POINT('Ctrl Pts',(-67.959178830538,19.2914105070282,12.));
#147878=CARTESIAN_POINT('Ctrl Pts',(-67.977007573346,19.3028108900373,12.));
#147879=CARTESIAN_POINT('Ctrl Pts',(-67.9948661329592,19.3142564958195,
12.));
#147880=CARTESIAN_POINT('Ctrl Pts',(-68.0127543311761,19.3257473032031,
12.));
#147881=CARTESIAN_POINT('Ctrl Pts',(-68.0306719906636,19.3372832910076,
12.));
#147882=CARTESIAN_POINT('Ctrl Pts',(-68.0486189351027,19.3488644380646,
12.));
#147883=CARTESIAN_POINT('Ctrl Pts',(-68.0665949893222,19.3604907232322,
12.));
#147884=CARTESIAN_POINT('Ctrl Pts',(-68.0845999792274,19.372162125392,12.));
#147885=CARTESIAN_POINT('Ctrl Pts',(-68.1026337317298,19.3838786234425,
12.));
#147886=CARTESIAN_POINT('Ctrl Pts',(-68.1206960746763,19.3956401962893,
12.));
#147887=CARTESIAN_POINT('Ctrl Pts',(-68.1387868367668,19.4074468228293,
12.));
#147888=CARTESIAN_POINT('Ctrl Pts',(-68.1569058475026,19.419298481941,12.));
#147889=CARTESIAN_POINT('Ctrl Pts',(-68.1750529372211,19.4311951524977,
12.));
#147890=CARTESIAN_POINT('Ctrl Pts',(-68.1932279371121,19.4431368133718,
12.));
#147891=CARTESIAN_POINT('Ctrl Pts',(-68.2114306792366,19.4551234434383,
12.));
#147892=CARTESIAN_POINT('Ctrl Pts',(-68.2296609965461,19.4671550215724,
12.));
#147893=CARTESIAN_POINT('Ctrl Pts',(-68.2479187228815,19.4792315266505,
12.));
#147894=CARTESIAN_POINT('Ctrl Pts',(-68.2662036929531,19.4913529375545,
12.));
#147895=CARTESIAN_POINT('Ctrl Pts',(-68.2845157423234,19.5035192331706,
12.));
#147896=CARTESIAN_POINT('Ctrl Pts',(-68.3028547073862,19.5157303923855,
12.));
#147897=CARTESIAN_POINT('Ctrl Pts',(-68.3212204253416,19.5279863940772,
12.));
#147898=CARTESIAN_POINT('Ctrl Pts',(-68.3396127341937,19.540287217119,12.));
#147899=CARTESIAN_POINT('Ctrl Pts',(-68.3580314727522,19.5526328403851,
12.));
#147900=CARTESIAN_POINT('Ctrl Pts',(-68.3764764806287,19.5650232427516,
12.));
#147901=CARTESIAN_POINT('Ctrl Pts',(-68.3949475982334,19.5774584030938,
12.));
#147902=CARTESIAN_POINT('Ctrl Pts',(-68.4134446667695,19.5899383002803,
12.));
#147903=CARTESIAN_POINT('Ctrl Pts',(-68.4319675282273,19.6024629131785,
12.));
#147904=CARTESIAN_POINT('Ctrl Pts',(-68.4505160253777,19.6150322206577,
12.));
#147905=CARTESIAN_POINT('Ctrl Pts',(-68.4690900017631,19.6276462015888,
12.));
#147906=CARTESIAN_POINT('Ctrl Pts',(-68.4876893016863,19.6403048348396,
12.));
#147907=CARTESIAN_POINT('Ctrl Pts',(-68.5063137701986,19.6530080992689,
12.));
#147908=CARTESIAN_POINT('Ctrl Pts',(-68.5249632530994,19.665755973734,12.));
#147909=CARTESIAN_POINT('Ctrl Pts',(-68.543637596932,19.6785484370929,12.));
#147910=CARTESIAN_POINT('Ctrl Pts',(-68.5623366489776,19.6913854682046,
12.));
#147911=CARTESIAN_POINT('Ctrl Pts',(-68.5810602572474,19.7042670459233,
12.));
#147912=CARTESIAN_POINT('Ctrl Pts',(-68.5998082704741,19.717193149095,12.));
#147913=CARTESIAN_POINT('Ctrl Pts',(-68.6185805381102,19.7301637565645,
12.));
#147914=CARTESIAN_POINT('Ctrl Pts',(-68.6373769103211,19.7431788471772,
12.));
#147915=CARTESIAN_POINT('Ctrl Pts',(-68.65619723798,19.7562383997783,12.));
#147916=CARTESIAN_POINT('Ctrl Pts',(-68.6750413726575,19.7693423932066,
12.));
#147917=CARTESIAN_POINT('Ctrl Pts',(-68.693909166615,19.7824908062924,12.));
#147918=CARTESIAN_POINT('Ctrl Pts',(-68.7128004728034,19.7956836178651,
12.));
#147919=CARTESIAN_POINT('Ctrl Pts',(-68.7317151448573,19.8089208067537,
12.));
#147920=CARTESIAN_POINT('Ctrl Pts',(-68.7506530370904,19.822202351787,12.));
#147921=CARTESIAN_POINT('Ctrl Pts',(-68.7696140044851,19.8355282317858,
12.));
#147922=CARTESIAN_POINT('Ctrl Pts',(-68.7885979026879,19.8488984255627,
12.));
#147923=CARTESIAN_POINT('Ctrl Pts',(-68.8076045880065,19.8623129119293,
12.));
#147924=CARTESIAN_POINT('Ctrl Pts',(-68.8266339174056,19.8757716696965,
12.));
#147925=CARTESIAN_POINT('Ctrl Pts',(-68.8456857485002,19.8892746776739,
12.));
#147926=CARTESIAN_POINT('Ctrl Pts',(-68.8647599395469,19.9028219146618,
12.));
#147927=CARTESIAN_POINT('Ctrl Pts',(-68.8838563494393,19.9164133594525,
12.));
#147928=CARTESIAN_POINT('Ctrl Pts',(-68.9029748377067,19.9300489908374,
12.));
#147929=CARTESIAN_POINT('Ctrl Pts',(-68.9221152645095,19.9437287876066,
12.));
#147930=CARTESIAN_POINT('Ctrl Pts',(-68.9412774906333,19.9574527285488,
12.));
#147931=CARTESIAN_POINT('Ctrl Pts',(-68.9604613774802,19.9712207924428,
12.));
#147932=CARTESIAN_POINT('Ctrl Pts',(-68.9796667870638,19.9850329580591,
12.));
#147933=CARTESIAN_POINT('Ctrl Pts',(-68.9988935820084,19.9988892041666,
12.));
#147934=CARTESIAN_POINT('Ctrl Pts',(-69.0181416255431,20.0127895095326,
12.));
#147935=CARTESIAN_POINT('Ctrl Pts',(-69.0374107814984,20.0267338529223,
12.));
#147936=CARTESIAN_POINT('Ctrl Pts',(-69.0567009142978,20.0407222130905,
12.));
#147937=CARTESIAN_POINT('Ctrl Pts',(-69.0760118889535,20.0547545687842,
12.));
#147938=CARTESIAN_POINT('Ctrl Pts',(-69.095343571064,20.068830898748,12.));
#147939=CARTESIAN_POINT('Ctrl Pts',(-69.1146958268104,20.0829511817251,
12.));
#147940=CARTESIAN_POINT('Ctrl Pts',(-69.1340685229515,20.0971153964557,
12.));
#147941=CARTESIAN_POINT('Ctrl Pts',(-69.1534615268153,20.1113235216694,
12.));
#147942=CARTESIAN_POINT('Ctrl Pts',(-69.1728747062963,20.1255755360872,
12.));
#147943=CARTESIAN_POINT('Ctrl Pts',(-69.1923079298538,20.1398714184279,
12.));
#147944=CARTESIAN_POINT('Ctrl Pts',(-69.2117610665076,20.1542111474087,
12.));
#147945=CARTESIAN_POINT('Ctrl Pts',(-69.2312339858335,20.1685947017433,
12.));
#147946=CARTESIAN_POINT('Ctrl Pts',(-69.2507265579554,20.1830220601348,
12.));
#147947=CARTESIAN_POINT('Ctrl Pts',(-69.2702386535422,20.1974932012773,
12.));
#147948=CARTESIAN_POINT('Ctrl Pts',(-69.2897701438059,20.212008103862,12.));
#147949=CARTESIAN_POINT('Ctrl Pts',(-69.3093209004984,20.2265667465784,
12.));
#147950=CARTESIAN_POINT('Ctrl Pts',(-69.3288907959067,20.2411691081123,
12.));
#147951=CARTESIAN_POINT('Ctrl Pts',(-69.3484797028458,20.2558151671391,
12.));
#147952=CARTESIAN_POINT('Ctrl Pts',(-69.368087494655,20.2705049023241,12.));
#147953=CARTESIAN_POINT('Ctrl Pts',(-69.3877140451975,20.2852382923299,
12.));
#147954=CARTESIAN_POINT('Ctrl Pts',(-69.407359228856,20.3000153158166,12.));
#147955=CARTESIAN_POINT('Ctrl Pts',(-69.4270229205297,20.3148359514415,
12.));
#147956=CARTESIAN_POINT('Ctrl Pts',(-69.4467049956262,20.3297001778507,
12.));
#147957=CARTESIAN_POINT('Ctrl Pts',(-69.4664053300587,20.3446079736802,
12.));
#147958=CARTESIAN_POINT('Ctrl Pts',(-69.4861238002441,20.3595593175623,
12.));
#147959=CARTESIAN_POINT('Ctrl Pts',(-69.5058602831008,20.3745541881268,
12.));
#147960=CARTESIAN_POINT('Ctrl Pts',(-69.5256146560441,20.3895925640005,
12.));
#147961=CARTESIAN_POINT('Ctrl Pts',(-69.5453867969804,20.4046744237999,
12.));
#147962=CARTESIAN_POINT('Ctrl Pts',(-69.5651765843033,20.41979974613,12.));
#147963=CARTESIAN_POINT('Ctrl Pts',(-69.5849838968928,20.4349685095923,
12.));
#147964=CARTESIAN_POINT('Ctrl Pts',(-69.6048086141113,20.4501806927851,
12.));
#147965=CARTESIAN_POINT('Ctrl Pts',(-69.6246506158013,20.4654362743037,
12.));
#147966=CARTESIAN_POINT('Ctrl Pts',(-69.6445097822792,20.480735232734,12.));
#147967=CARTESIAN_POINT('Ctrl Pts',(-69.6643859943308,20.4960775466492,
12.));
#147968=CARTESIAN_POINT('Ctrl Pts',(-69.6842791332115,20.5114631946184,
12.));
#147969=CARTESIAN_POINT('Ctrl Pts',(-69.7041890806425,20.5268921552077,
12.));
#147970=CARTESIAN_POINT('Ctrl Pts',(-69.7241157188083,20.5423644069799,
12.));
#147971=CARTESIAN_POINT('Ctrl Pts',(-69.744058930351,20.5578799284897,12.));
#147972=CARTESIAN_POINT('Ctrl Pts',(-69.7640185983644,20.5734386982782,
12.));
#147973=CARTESIAN_POINT('Ctrl Pts',(-69.7839946063949,20.5890406948811,
12.));
#147974=CARTESIAN_POINT('Ctrl Pts',(-69.8039868384389,20.6046858968307,
12.));
#147975=CARTESIAN_POINT('Ctrl Pts',(-69.8239951789402,20.6203742826566,
12.));
#147976=CARTESIAN_POINT('Ctrl Pts',(-69.8440195127866,20.636105830881,12.));
#147977=CARTESIAN_POINT('Ctrl Pts',(-69.8640597253045,20.6518805200129,
12.));
#147978=CARTESIAN_POINT('Ctrl Pts',(-69.8841157022568,20.667698328554,12.));
#147979=CARTESIAN_POINT('Ctrl Pts',(-69.904187329841,20.683559235003,12.));
#147980=CARTESIAN_POINT('Ctrl Pts',(-69.9242744946854,20.6994632178551,
12.));
#147981=CARTESIAN_POINT('Ctrl Pts',(-69.9443770838448,20.7154102555997,
12.));
#147982=CARTESIAN_POINT('Ctrl Pts',(-69.9644949847934,20.7314003267119,
12.));
#147983=CARTESIAN_POINT('Ctrl Pts',(-69.9846280854257,20.7474334096581,
12.));
#147984=CARTESIAN_POINT('Ctrl Pts',(-70.0047762740568,20.7635094829015,
12.));
#147985=CARTESIAN_POINT('Ctrl Pts',(-70.024939439422,20.7796285249022,12.));
#147986=CARTESIAN_POINT('Ctrl Pts',(-70.0451174706741,20.7957905141156,
12.));
#147987=CARTESIAN_POINT('Ctrl Pts',(-70.0653102573803,20.8119954289848,
12.));
#147988=CARTESIAN_POINT('Ctrl Pts',(-70.0855176895191,20.8282432479428,
12.));
#147989=CARTESIAN_POINT('Ctrl Pts',(-70.1057396574747,20.8445339494187,
12.));
#147990=CARTESIAN_POINT('Ctrl Pts',(-70.1259760520309,20.8608675118378,
12.));
#147991=CARTESIAN_POINT('Ctrl Pts',(-70.1462267643647,20.8772439136206,
12.));
#147992=CARTESIAN_POINT('Ctrl Pts',(-70.1664916860358,20.8936631331748,
12.));
#147993=CARTESIAN_POINT('Ctrl Pts',(-70.1867707089854,20.9101251488943,
12.));
#147994=CARTESIAN_POINT('Ctrl Pts',(-70.2070637255458,20.9266299391684,
12.));
#147995=CARTESIAN_POINT('Ctrl Pts',(-70.2273706284472,20.9431774823831,
12.));
#147996=CARTESIAN_POINT('Ctrl Pts',(-70.2476913108244,20.9597677569228,
12.));
#147997=CARTESIAN_POINT('Ctrl Pts',(-70.2680256662224,20.9764007411652,
12.));
#147998=CARTESIAN_POINT('Ctrl Pts',(-70.2883735885984,20.9930764134776,
12.));
#147999=CARTESIAN_POINT('Ctrl Pts',(-70.3087349722973,21.0097947522218,
12.));
#148000=CARTESIAN_POINT('Ctrl Pts',(-70.3291097120302,21.0265557357548,
12.));
#148001=CARTESIAN_POINT('Ctrl Pts',(-70.3494977028498,21.0433593424266,
12.));
#148002=CARTESIAN_POINT('Ctrl Pts',(-70.3698988401281,21.0602055505748,
12.));
#148003=CARTESIAN_POINT('Ctrl Pts',(-70.3903130195265,21.0770943385141,
12.));
#148004=CARTESIAN_POINT('Ctrl Pts',(-70.4107401370389,21.0940256845472,
12.));
#148005=CARTESIAN_POINT('Ctrl Pts',(-70.4311800890402,21.1109995669747,
12.));
#148006=CARTESIAN_POINT('Ctrl Pts',(-70.4516327723346,21.1280159641002,
12.));
#148007=CARTESIAN_POINT('Ctrl Pts',(-70.4720980841939,21.1450748542336,
12.));
#148008=CARTESIAN_POINT('Ctrl Pts',(-70.4925759224216,21.1621762156897,
12.));
#148009=CARTESIAN_POINT('Ctrl Pts',(-70.5130661852955,21.1793200267846,
12.));
#148010=CARTESIAN_POINT('Ctrl Pts',(-70.5335687714429,21.1965062658298,
12.));
#148011=CARTESIAN_POINT('Ctrl Pts',(-70.5540835797283,21.2137349111208,
12.));
#148012=CARTESIAN_POINT('Ctrl Pts',(-70.5746105091502,21.2310059409265,
12.));
#148013=CARTESIAN_POINT('Ctrl Pts',(-70.5951494586957,21.2483193334675,
12.));
#148014=CARTESIAN_POINT('Ctrl Pts',(-70.6157003273316,21.2656750669126,
12.));
#148015=CARTESIAN_POINT('Ctrl Pts',(-70.6362630143047,21.2830731194183,
12.));
#148016=CARTESIAN_POINT('Ctrl Pts',(-70.6568374193774,21.300513469156,12.));
#148017=CARTESIAN_POINT('Ctrl Pts',(-70.6774234430897,21.3179960943388,
12.));
#148018=CARTESIAN_POINT('Ctrl Pts',(-70.6980209870045,21.3355209732443,
12.));
#148019=CARTESIAN_POINT('Ctrl Pts',(-70.7186299539724,21.3530880842349,
12.));
#148020=CARTESIAN_POINT('Ctrl Pts',(-70.7392502475469,21.3706974057039,
12.));
#148021=CARTESIAN_POINT('Ctrl Pts',(-70.7598817714105,21.3883489160196,
12.));
#148022=CARTESIAN_POINT('Ctrl Pts',(-70.780524428745,21.4060425934598,12.));
#148023=CARTESIAN_POINT('Ctrl Pts',(-70.8011781217394,21.4237784161587,
12.));
#148024=CARTESIAN_POINT('Ctrl Pts',(-70.8218427507506,21.4415563620114,
12.));
#148025=CARTESIAN_POINT('Ctrl Pts',(-70.8425182149846,21.4593764087473,
12.));
#148026=CARTESIAN_POINT('Ctrl Pts',(-70.8632044140112,21.477238534096,12.));
#148027=CARTESIAN_POINT('Ctrl Pts',(-70.8839012490871,21.4951427159261,
12.));
#148028=CARTESIAN_POINT('Ctrl Pts',(-70.9046086244131,21.513088932377,12.));
#148029=CARTESIAN_POINT('Ctrl Pts',(-70.9253264487637,21.531077162023,12.));
#148030=CARTESIAN_POINT('Ctrl Pts',(-70.94605463587,21.5491073839106,12.));
#148031=CARTESIAN_POINT('Ctrl Pts',(-70.9638315189817,21.5645987555369,
12.));
#148032=CARTESIAN_POINT('Ctrl Pts',(-70.9774662112587,21.576498336648,12.));
#148033=CARTESIAN_POINT('Ctrl Pts',(-70.9869541808053,21.584787543333,12.));
#148034=CARTESIAN_POINT('Ctrl Pts',(-70.9922924595366,21.5894540925581,
12.));
#148035=CARTESIAN_POINT('Ctrl Pts',(-70.9934796069113,21.5904919935059,
12.));
#148036=CARTESIAN_POINT('',(-67.3887914263119,18.9407177820969,0.));
#148037=CARTESIAN_POINT('',(-67.3887914263118,18.9407177820969,0.));
#148038=CARTESIAN_POINT('Ctrl Pts',(-70.9934796069113,21.5904919935059,
0.));
#148039=CARTESIAN_POINT('Ctrl Pts',(-70.9922924595366,21.5894540925581,
0.));
#148040=CARTESIAN_POINT('Ctrl Pts',(-70.9869541808053,21.584787543333,0.));
#148041=CARTESIAN_POINT('Ctrl Pts',(-70.9774662112587,21.576498336648,0.));
#148042=CARTESIAN_POINT('Ctrl Pts',(-70.9638315189817,21.5645987555369,
0.));
#148043=CARTESIAN_POINT('Ctrl Pts',(-70.94605463587,21.5491073839106,0.));
#148044=CARTESIAN_POINT('Ctrl Pts',(-70.9253264487637,21.531077162023,0.));
#148045=CARTESIAN_POINT('Ctrl Pts',(-70.9046086244131,21.513088932377,0.));
#148046=CARTESIAN_POINT('Ctrl Pts',(-70.8839012490871,21.4951427159261,
0.));
#148047=CARTESIAN_POINT('Ctrl Pts',(-70.8632044140112,21.477238534096,0.));
#148048=CARTESIAN_POINT('Ctrl Pts',(-70.8425182149846,21.4593764087473,
0.));
#148049=CARTESIAN_POINT('Ctrl Pts',(-70.8218427507506,21.4415563620114,
0.));
#148050=CARTESIAN_POINT('Ctrl Pts',(-70.8011781217394,21.4237784161587,
0.));
#148051=CARTESIAN_POINT('Ctrl Pts',(-70.780524428745,21.4060425934598,0.));
#148052=CARTESIAN_POINT('Ctrl Pts',(-70.7598817714105,21.3883489160196,
0.));
#148053=CARTESIAN_POINT('Ctrl Pts',(-70.7392502475469,21.3706974057039,
0.));
#148054=CARTESIAN_POINT('Ctrl Pts',(-70.7186299539724,21.3530880842349,
0.));
#148055=CARTESIAN_POINT('Ctrl Pts',(-70.6980209870045,21.3355209732443,
0.));
#148056=CARTESIAN_POINT('Ctrl Pts',(-70.6774234430897,21.3179960943388,
0.));
#148057=CARTESIAN_POINT('Ctrl Pts',(-70.6568374193774,21.300513469156,0.));
#148058=CARTESIAN_POINT('Ctrl Pts',(-70.6362630143047,21.2830731194183,
0.));
#148059=CARTESIAN_POINT('Ctrl Pts',(-70.6157003273316,21.2656750669126,
0.));
#148060=CARTESIAN_POINT('Ctrl Pts',(-70.5951494586957,21.2483193334675,
0.));
#148061=CARTESIAN_POINT('Ctrl Pts',(-70.5746105091502,21.2310059409265,
0.));
#148062=CARTESIAN_POINT('Ctrl Pts',(-70.5540835797283,21.2137349111208,
0.));
#148063=CARTESIAN_POINT('Ctrl Pts',(-70.5335687714429,21.1965062658298,
0.));
#148064=CARTESIAN_POINT('Ctrl Pts',(-70.5130661852955,21.1793200267846,
0.));
#148065=CARTESIAN_POINT('Ctrl Pts',(-70.4925759224216,21.1621762156897,
0.));
#148066=CARTESIAN_POINT('Ctrl Pts',(-70.4720980841939,21.1450748542336,
0.));
#148067=CARTESIAN_POINT('Ctrl Pts',(-70.4516327723346,21.1280159641002,
0.));
#148068=CARTESIAN_POINT('Ctrl Pts',(-70.4311800890402,21.1109995669747,
0.));
#148069=CARTESIAN_POINT('Ctrl Pts',(-70.4107401370389,21.0940256845472,
0.));
#148070=CARTESIAN_POINT('Ctrl Pts',(-70.3903130195265,21.0770943385141,
0.));
#148071=CARTESIAN_POINT('Ctrl Pts',(-70.3698988401281,21.0602055505748,
0.));
#148072=CARTESIAN_POINT('Ctrl Pts',(-70.3494977028498,21.0433593424266,
0.));
#148073=CARTESIAN_POINT('Ctrl Pts',(-70.3291097120302,21.0265557357548,
0.));
#148074=CARTESIAN_POINT('Ctrl Pts',(-70.3087349722973,21.0097947522218,
0.));
#148075=CARTESIAN_POINT('Ctrl Pts',(-70.2883735885984,20.9930764134776,
0.));
#148076=CARTESIAN_POINT('Ctrl Pts',(-70.2680256662224,20.9764007411652,
0.));
#148077=CARTESIAN_POINT('Ctrl Pts',(-70.2476913108244,20.9597677569228,
0.));
#148078=CARTESIAN_POINT('Ctrl Pts',(-70.2273706284472,20.9431774823831,
0.));
#148079=CARTESIAN_POINT('Ctrl Pts',(-70.2070637255458,20.9266299391684,
0.));
#148080=CARTESIAN_POINT('Ctrl Pts',(-70.1867707089854,20.9101251488943,
0.));
#148081=CARTESIAN_POINT('Ctrl Pts',(-70.1664916860358,20.8936631331748,
0.));
#148082=CARTESIAN_POINT('Ctrl Pts',(-70.1462267643647,20.8772439136206,
0.));
#148083=CARTESIAN_POINT('Ctrl Pts',(-70.1259760520309,20.8608675118378,
0.));
#148084=CARTESIAN_POINT('Ctrl Pts',(-70.1057396574747,20.8445339494187,
0.));
#148085=CARTESIAN_POINT('Ctrl Pts',(-70.0855176895191,20.8282432479428,
0.));
#148086=CARTESIAN_POINT('Ctrl Pts',(-70.0653102573803,20.8119954289848,
0.));
#148087=CARTESIAN_POINT('Ctrl Pts',(-70.0451174706741,20.7957905141156,
0.));
#148088=CARTESIAN_POINT('Ctrl Pts',(-70.024939439422,20.7796285249022,0.));
#148089=CARTESIAN_POINT('Ctrl Pts',(-70.0047762740568,20.7635094829015,
0.));
#148090=CARTESIAN_POINT('Ctrl Pts',(-69.9846280854257,20.7474334096581,
0.));
#148091=CARTESIAN_POINT('Ctrl Pts',(-69.9644949847934,20.7314003267119,
0.));
#148092=CARTESIAN_POINT('Ctrl Pts',(-69.9443770838448,20.7154102555997,
0.));
#148093=CARTESIAN_POINT('Ctrl Pts',(-69.9242744946854,20.6994632178551,
0.));
#148094=CARTESIAN_POINT('Ctrl Pts',(-69.904187329841,20.683559235003,0.));
#148095=CARTESIAN_POINT('Ctrl Pts',(-69.8841157022568,20.667698328554,0.));
#148096=CARTESIAN_POINT('Ctrl Pts',(-69.8640597253045,20.6518805200129,
0.));
#148097=CARTESIAN_POINT('Ctrl Pts',(-69.8440195127866,20.636105830881,0.));
#148098=CARTESIAN_POINT('Ctrl Pts',(-69.8239951789402,20.6203742826566,
0.));
#148099=CARTESIAN_POINT('Ctrl Pts',(-69.8039868384389,20.6046858968307,
0.));
#148100=CARTESIAN_POINT('Ctrl Pts',(-69.7839946063949,20.5890406948811,
0.));
#148101=CARTESIAN_POINT('Ctrl Pts',(-69.7640185983644,20.5734386982782,
0.));
#148102=CARTESIAN_POINT('Ctrl Pts',(-69.744058930351,20.5578799284897,0.));
#148103=CARTESIAN_POINT('Ctrl Pts',(-69.7241157188083,20.5423644069799,
0.));
#148104=CARTESIAN_POINT('Ctrl Pts',(-69.7041890806425,20.5268921552077,
0.));
#148105=CARTESIAN_POINT('Ctrl Pts',(-69.6842791332115,20.5114631946184,
0.));
#148106=CARTESIAN_POINT('Ctrl Pts',(-69.6643859943308,20.4960775466492,
0.));
#148107=CARTESIAN_POINT('Ctrl Pts',(-69.6445097822792,20.480735232734,0.));
#148108=CARTESIAN_POINT('Ctrl Pts',(-69.6246506158013,20.4654362743037,
0.));
#148109=CARTESIAN_POINT('Ctrl Pts',(-69.6048086141113,20.4501806927851,
0.));
#148110=CARTESIAN_POINT('Ctrl Pts',(-69.5849838968928,20.4349685095923,
0.));
#148111=CARTESIAN_POINT('Ctrl Pts',(-69.5651765843033,20.41979974613,0.));
#148112=CARTESIAN_POINT('Ctrl Pts',(-69.5453867969804,20.4046744237999,
0.));
#148113=CARTESIAN_POINT('Ctrl Pts',(-69.5256146560441,20.3895925640005,
0.));
#148114=CARTESIAN_POINT('Ctrl Pts',(-69.5058602831008,20.3745541881268,
0.));
#148115=CARTESIAN_POINT('Ctrl Pts',(-69.4861238002441,20.3595593175623,
0.));
#148116=CARTESIAN_POINT('Ctrl Pts',(-69.4664053300587,20.3446079736802,
0.));
#148117=CARTESIAN_POINT('Ctrl Pts',(-69.4467049956262,20.3297001778507,
0.));
#148118=CARTESIAN_POINT('Ctrl Pts',(-69.4270229205297,20.3148359514415,
0.));
#148119=CARTESIAN_POINT('Ctrl Pts',(-69.407359228856,20.3000153158166,0.));
#148120=CARTESIAN_POINT('Ctrl Pts',(-69.3877140451975,20.2852382923299,
0.));
#148121=CARTESIAN_POINT('Ctrl Pts',(-69.368087494655,20.2705049023241,0.));
#148122=CARTESIAN_POINT('Ctrl Pts',(-69.3484797028458,20.2558151671391,
0.));
#148123=CARTESIAN_POINT('Ctrl Pts',(-69.3288907959067,20.2411691081123,
0.));
#148124=CARTESIAN_POINT('Ctrl Pts',(-69.3093209004984,20.2265667465784,
0.));
#148125=CARTESIAN_POINT('Ctrl Pts',(-69.2897701438059,20.212008103862,0.));
#148126=CARTESIAN_POINT('Ctrl Pts',(-69.2702386535422,20.1974932012773,
0.));
#148127=CARTESIAN_POINT('Ctrl Pts',(-69.2507265579554,20.1830220601348,
0.));
#148128=CARTESIAN_POINT('Ctrl Pts',(-69.2312339858335,20.1685947017433,
0.));
#148129=CARTESIAN_POINT('Ctrl Pts',(-69.2117610665076,20.1542111474087,
0.));
#148130=CARTESIAN_POINT('Ctrl Pts',(-69.1923079298538,20.1398714184279,
0.));
#148131=CARTESIAN_POINT('Ctrl Pts',(-69.1728747062963,20.1255755360872,
0.));
#148132=CARTESIAN_POINT('Ctrl Pts',(-69.1534615268153,20.1113235216694,
0.));
#148133=CARTESIAN_POINT('Ctrl Pts',(-69.1340685229515,20.0971153964557,
0.));
#148134=CARTESIAN_POINT('Ctrl Pts',(-69.1146958268104,20.0829511817251,
0.));
#148135=CARTESIAN_POINT('Ctrl Pts',(-69.095343571064,20.068830898748,0.));
#148136=CARTESIAN_POINT('Ctrl Pts',(-69.0760118889535,20.0547545687842,
0.));
#148137=CARTESIAN_POINT('Ctrl Pts',(-69.0567009142978,20.0407222130905,
0.));
#148138=CARTESIAN_POINT('Ctrl Pts',(-69.0374107814984,20.0267338529223,
0.));
#148139=CARTESIAN_POINT('Ctrl Pts',(-69.0181416255431,20.0127895095326,
0.));
#148140=CARTESIAN_POINT('Ctrl Pts',(-68.9988935820084,19.9988892041666,
0.));
#148141=CARTESIAN_POINT('Ctrl Pts',(-68.9796667870638,19.9850329580591,
0.));
#148142=CARTESIAN_POINT('Ctrl Pts',(-68.9604613774802,19.9712207924428,
0.));
#148143=CARTESIAN_POINT('Ctrl Pts',(-68.9412774906333,19.9574527285488,
0.));
#148144=CARTESIAN_POINT('Ctrl Pts',(-68.9221152645095,19.9437287876066,
0.));
#148145=CARTESIAN_POINT('Ctrl Pts',(-68.9029748377067,19.9300489908374,
0.));
#148146=CARTESIAN_POINT('Ctrl Pts',(-68.8838563494393,19.9164133594525,
0.));
#148147=CARTESIAN_POINT('Ctrl Pts',(-68.8647599395469,19.9028219146618,
0.));
#148148=CARTESIAN_POINT('Ctrl Pts',(-68.8456857485002,19.8892746776739,
0.));
#148149=CARTESIAN_POINT('Ctrl Pts',(-68.8266339174056,19.8757716696965,
0.));
#148150=CARTESIAN_POINT('Ctrl Pts',(-68.8076045880065,19.8623129119293,
0.));
#148151=CARTESIAN_POINT('Ctrl Pts',(-68.7885979026879,19.8488984255627,
0.));
#148152=CARTESIAN_POINT('Ctrl Pts',(-68.7696140044851,19.8355282317858,
0.));
#148153=CARTESIAN_POINT('Ctrl Pts',(-68.7506530370904,19.822202351787,0.));
#148154=CARTESIAN_POINT('Ctrl Pts',(-68.7317151448573,19.8089208067537,
0.));
#148155=CARTESIAN_POINT('Ctrl Pts',(-68.7128004728034,19.7956836178651,
0.));
#148156=CARTESIAN_POINT('Ctrl Pts',(-68.693909166615,19.7824908062924,0.));
#148157=CARTESIAN_POINT('Ctrl Pts',(-68.6750413726575,19.7693423932066,
0.));
#148158=CARTESIAN_POINT('Ctrl Pts',(-68.65619723798,19.7562383997783,0.));
#148159=CARTESIAN_POINT('Ctrl Pts',(-68.6373769103211,19.7431788471772,
0.));
#148160=CARTESIAN_POINT('Ctrl Pts',(-68.6185805381102,19.7301637565645,
0.));
#148161=CARTESIAN_POINT('Ctrl Pts',(-68.5998082704741,19.717193149095,0.));
#148162=CARTESIAN_POINT('Ctrl Pts',(-68.5810602572474,19.7042670459233,
0.));
#148163=CARTESIAN_POINT('Ctrl Pts',(-68.5623366489776,19.6913854682046,
0.));
#148164=CARTESIAN_POINT('Ctrl Pts',(-68.543637596932,19.6785484370929,0.));
#148165=CARTESIAN_POINT('Ctrl Pts',(-68.5249632530994,19.665755973734,0.));
#148166=CARTESIAN_POINT('Ctrl Pts',(-68.5063137701986,19.6530080992689,
0.));
#148167=CARTESIAN_POINT('Ctrl Pts',(-68.4876893016863,19.6403048348396,
0.));
#148168=CARTESIAN_POINT('Ctrl Pts',(-68.4690900017631,19.6276462015888,
0.));
#148169=CARTESIAN_POINT('Ctrl Pts',(-68.4505160253777,19.6150322206577,
0.));
#148170=CARTESIAN_POINT('Ctrl Pts',(-68.4319675282273,19.6024629131785,
0.));
#148171=CARTESIAN_POINT('Ctrl Pts',(-68.4134446667695,19.5899383002803,
0.));
#148172=CARTESIAN_POINT('Ctrl Pts',(-68.3949475982334,19.5774584030938,
0.));
#148173=CARTESIAN_POINT('Ctrl Pts',(-68.3764764806287,19.5650232427516,
0.));
#148174=CARTESIAN_POINT('Ctrl Pts',(-68.3580314727522,19.5526328403851,
0.));
#148175=CARTESIAN_POINT('Ctrl Pts',(-68.3396127341937,19.540287217119,0.));
#148176=CARTESIAN_POINT('Ctrl Pts',(-68.3212204253416,19.5279863940772,
0.));
#148177=CARTESIAN_POINT('Ctrl Pts',(-68.3028547073862,19.5157303923855,
0.));
#148178=CARTESIAN_POINT('Ctrl Pts',(-68.2845157423234,19.5035192331706,
0.));
#148179=CARTESIAN_POINT('Ctrl Pts',(-68.2662036929531,19.4913529375545,
0.));
#148180=CARTESIAN_POINT('Ctrl Pts',(-68.2479187228815,19.4792315266505,
0.));
#148181=CARTESIAN_POINT('Ctrl Pts',(-68.2296609965461,19.4671550215724,
0.));
#148182=CARTESIAN_POINT('Ctrl Pts',(-68.2114306792366,19.4551234434383,
0.));
#148183=CARTESIAN_POINT('Ctrl Pts',(-68.1932279371121,19.4431368133718,
0.));
#148184=CARTESIAN_POINT('Ctrl Pts',(-68.1750529372211,19.4311951524977,
0.));
#148185=CARTESIAN_POINT('Ctrl Pts',(-68.1569058475026,19.419298481941,0.));
#148186=CARTESIAN_POINT('Ctrl Pts',(-68.1387868367668,19.4074468228293,
0.));
#148187=CARTESIAN_POINT('Ctrl Pts',(-68.1206960746763,19.3956401962893,
0.));
#148188=CARTESIAN_POINT('Ctrl Pts',(-68.1026337317298,19.3838786234425,
0.));
#148189=CARTESIAN_POINT('Ctrl Pts',(-68.0845999792274,19.372162125392,0.));
#148190=CARTESIAN_POINT('Ctrl Pts',(-68.0665949893222,19.3604907232322,
0.));
#148191=CARTESIAN_POINT('Ctrl Pts',(-68.0486189351027,19.3488644380646,
0.));
#148192=CARTESIAN_POINT('Ctrl Pts',(-68.0306719906636,19.3372832910076,
0.));
#148193=CARTESIAN_POINT('Ctrl Pts',(-68.0127543311761,19.3257473032031,
0.));
#148194=CARTESIAN_POINT('Ctrl Pts',(-67.9948661329592,19.3142564958195,
0.));
#148195=CARTESIAN_POINT('Ctrl Pts',(-67.977007573346,19.3028108900373,0.));
#148196=CARTESIAN_POINT('Ctrl Pts',(-67.959178830538,19.2914105070282,0.));
#148197=CARTESIAN_POINT('Ctrl Pts',(-67.9413800834798,19.2800553679362,
0.));
#148198=CARTESIAN_POINT('Ctrl Pts',(-67.9236115116781,19.2687454938448,
0.));
#148199=CARTESIAN_POINT('Ctrl Pts',(-67.9058732951822,19.2574809057705,
0.));
#148200=CARTESIAN_POINT('Ctrl Pts',(-67.8881656149983,19.2462616247287,
0.));
#148201=CARTESIAN_POINT('Ctrl Pts',(-67.8704886534555,19.2350876717877,
0.));
#148202=CARTESIAN_POINT('Ctrl Pts',(-67.852842594517,19.2239590681129,0.));
#148203=CARTESIAN_POINT('Ctrl Pts',(-67.8352276242856,19.2128758350336,
0.));
#148204=CARTESIAN_POINT('Ctrl Pts',(-67.817643930658,19.2018379939918,0.));
#148205=CARTESIAN_POINT('Ctrl Pts',(-67.8000917023896,19.1908455664089,
0.));
#148206=CARTESIAN_POINT('Ctrl Pts',(-67.7825711283092,19.1798985735687,
0.));
#148207=CARTESIAN_POINT('Ctrl Pts',(-67.7650823965156,19.1689970364958,
0.));
#148208=CARTESIAN_POINT('Ctrl Pts',(-67.7476256934493,19.1581409758112,
0.));
#148209=CARTESIAN_POINT('Ctrl Pts',(-67.730201205663,19.1473304119968,0.));
#148210=CARTESIAN_POINT('Ctrl Pts',(-67.7128091219372,19.1365653657097,
0.));
#148211=CARTESIAN_POINT('Ctrl Pts',(-67.6954496350053,19.1258458580343,
0.));
#148212=CARTESIAN_POINT('Ctrl Pts',(-67.6781229440535,19.115171910845,0.));
#148213=CARTESIAN_POINT('Ctrl Pts',(-67.6608292549412,19.1045435468344,
0.));
#148214=CARTESIAN_POINT('Ctrl Pts',(-67.6435687749803,19.0939607887491,
0.));
#148215=CARTESIAN_POINT('Ctrl Pts',(-67.6263417083414,19.0834236587115,
0.));
#148216=CARTESIAN_POINT('Ctrl Pts',(-67.6091482520558,19.0729321776286,
0.));
#148217=CARTESIAN_POINT('Ctrl Pts',(-67.5919885896278,19.0624863642425,
0.));
#148218=CARTESIAN_POINT('Ctrl Pts',(-67.5748628972035,19.0520862360413,
0.));
#148219=CARTESIAN_POINT('Ctrl Pts',(-67.5577713558248,19.0417318110721,
0.));
#148220=CARTESIAN_POINT('Ctrl Pts',(-67.5407141612881,19.0314231093923,
0.));
#148221=CARTESIAN_POINT('Ctrl Pts',(-67.5236915360253,19.0211601548222,
0.));
#148222=CARTESIAN_POINT('Ctrl Pts',(-67.5067037372177,19.0109429761274,
0.));
#148223=CARTESIAN_POINT('Ctrl Pts',(-67.4897510316692,19.0007716032784,
0.));
#148224=CARTESIAN_POINT('Ctrl Pts',(-67.4728336719559,18.9906460638607,
0.));
#148225=CARTESIAN_POINT('Ctrl Pts',(-67.4559518744714,18.9805663798466,
0.));
#148226=CARTESIAN_POINT('Ctrl Pts',(-67.4391057908687,18.9705325631772,
0.));
#148227=CARTESIAN_POINT('Ctrl Pts',(-67.4222955062385,18.9605446161078,
0.));
#148228=CARTESIAN_POINT('Ctrl Pts',(-67.4088759498287,18.9525909518002,
0.));
#148229=CARTESIAN_POINT('Ctrl Pts',(-67.398827414689,18.9466463414354,0.));
#148230=CARTESIAN_POINT('Ctrl Pts',(-67.3921355608417,18.942692439874,0.));
#148231=CARTESIAN_POINT('Ctrl Pts',(-67.3887914263119,18.9407177820969,
0.));
#148232=CARTESIAN_POINT('Ctrl Pts',(-69.065695021045,27.9316983239472,0.));
#148233=CARTESIAN_POINT('Ctrl Pts',(-69.065695021045,27.9316983239472,12.));
#148234=CARTESIAN_POINT('Ctrl Pts',(-69.0618620884721,27.9276214070631,
0.));
#148235=CARTESIAN_POINT('Ctrl Pts',(-69.0618620884721,27.9276214070631,
12.));
#148236=CARTESIAN_POINT('Ctrl Pts',(-69.0541967851028,27.9194718099003,
0.));
#148237=CARTESIAN_POINT('Ctrl Pts',(-69.0541967851028,27.9194718099003,
12.));
#148238=CARTESIAN_POINT('Ctrl Pts',(-69.0427005153791,27.9072601239722,
0.));
#148239=CARTESIAN_POINT('Ctrl Pts',(-69.0427005153791,27.9072601239722,
12.));
#148240=CARTESIAN_POINT('Ctrl Pts',(-69.0273755265383,27.8910032967339,
0.));
#148241=CARTESIAN_POINT('Ctrl Pts',(-69.0273755265383,27.8910032967339,
12.));
#148242=CARTESIAN_POINT('Ctrl Pts',(-69.0082249138598,27.8707246380957,
0.));
#148243=CARTESIAN_POINT('Ctrl Pts',(-69.0082249138598,27.8707246380957,
12.));
#148244=CARTESIAN_POINT('Ctrl Pts',(-68.9890799392213,27.8504883674058,
0.));
#148245=CARTESIAN_POINT('Ctrl Pts',(-68.9890799392213,27.8504883674058,
12.));
#148246=CARTESIAN_POINT('Ctrl Pts',(-68.9699406311389,27.8302945019976,
0.));
#148247=CARTESIAN_POINT('Ctrl Pts',(-68.9699406311389,27.8302945019976,
12.));
#148248=CARTESIAN_POINT('Ctrl Pts',(-68.9508070357658,27.8101430638071,
0.));
#148249=CARTESIAN_POINT('Ctrl Pts',(-68.9508070357658,27.8101430638071,
12.));
#148250=CARTESIAN_POINT('Ctrl Pts',(-68.9316792225946,27.7900340793689,
0.));
#148251=CARTESIAN_POINT('Ctrl Pts',(-68.9316792225946,27.7900340793689,
12.));
#148252=CARTESIAN_POINT('Ctrl Pts',(-68.9125572825694,27.7699675790571,
0.));
#148253=CARTESIAN_POINT('Ctrl Pts',(-68.9125572825694,27.7699675790571,
12.));
#148254=CARTESIAN_POINT('Ctrl Pts',(-68.8934413203759,27.7499435957525,
0.));
#148255=CARTESIAN_POINT('Ctrl Pts',(-68.8934413203759,27.7499435957525,
12.));
#148256=CARTESIAN_POINT('Ctrl Pts',(-68.8743314483369,27.7299621636566,
0.));
#148257=CARTESIAN_POINT('Ctrl Pts',(-68.8743314483369,27.7299621636566,
12.));
#148258=CARTESIAN_POINT('Ctrl Pts',(-68.85522777982,27.7100233170737,0.));
#148259=CARTESIAN_POINT('Ctrl Pts',(-68.85522777982,27.7100233170737,12.));
#148260=CARTESIAN_POINT('Ctrl Pts',(-68.8361304224467,27.6901270891241,
0.));
#148261=CARTESIAN_POINT('Ctrl Pts',(-68.8361304224467,27.6901270891241,
12.));
#148262=CARTESIAN_POINT('Ctrl Pts',(-68.81703947259,27.6702735107121,0.));
#148263=CARTESIAN_POINT('Ctrl Pts',(-68.81703947259,27.6702735107121,12.));
#148264=CARTESIAN_POINT('Ctrl Pts',(-68.7979550191872,27.6504626112666,
0.));
#148265=CARTESIAN_POINT('Ctrl Pts',(-68.7979550191872,27.6504626112666,
12.));
#148266=CARTESIAN_POINT('Ctrl Pts',(-68.7788771464713,27.6306944192737,
0.));
#148267=CARTESIAN_POINT('Ctrl Pts',(-68.7788771464713,27.6306944192737,
12.));
#148268=CARTESIAN_POINT('Ctrl Pts',(-68.7598059372129,27.6109689629029,
0.));
#148269=CARTESIAN_POINT('Ctrl Pts',(-68.7598059372129,27.6109689629029,
12.));
#148270=CARTESIAN_POINT('Ctrl Pts',(-68.740741475526,27.5912862705468,0.));
#148271=CARTESIAN_POINT('Ctrl Pts',(-68.740741475526,27.5912862705468,12.));
#148272=CARTESIAN_POINT('Ctrl Pts',(-68.7216838504218,27.5716463715004,
0.));
#148273=CARTESIAN_POINT('Ctrl Pts',(-68.7216838504218,27.5716463715004,
12.));
#148274=CARTESIAN_POINT('Ctrl Pts',(-68.7026331554296,27.5520492958907,
0.));
#148275=CARTESIAN_POINT('Ctrl Pts',(-68.7026331554296,27.5520492958907,
12.));
#148276=CARTESIAN_POINT('Ctrl Pts',(-68.6835894869882,27.5324950743706,
0.));
#148277=CARTESIAN_POINT('Ctrl Pts',(-68.6835894869882,27.5324950743706,
12.));
#148278=CARTESIAN_POINT('Ctrl Pts',(-68.6645529432045,27.5129837378791,
0.));
#148279=CARTESIAN_POINT('Ctrl Pts',(-68.6645529432045,27.5129837378791,
12.));
#148280=CARTESIAN_POINT('Ctrl Pts',(-68.645523622548,27.4935153173868,0.));
#148281=CARTESIAN_POINT('Ctrl Pts',(-68.645523622548,27.4935153173868,12.));
#148282=CARTESIAN_POINT('Ctrl Pts',(-68.6265016223561,27.4740898435988,
0.));
#148283=CARTESIAN_POINT('Ctrl Pts',(-68.6265016223561,27.4740898435988,
12.));
#148284=CARTESIAN_POINT('Ctrl Pts',(-68.6074870381619,27.4547073468226,
0.));
#148285=CARTESIAN_POINT('Ctrl Pts',(-68.6074870381619,27.4547073468226,
12.));
#148286=CARTESIAN_POINT('Ctrl Pts',(-68.5884799645218,27.4353678571361,
0.));
#148287=CARTESIAN_POINT('Ctrl Pts',(-68.5884799645218,27.4353678571361,
12.));
#148288=CARTESIAN_POINT('Ctrl Pts',(-68.5694804955014,27.4160714044831,
0.));
#148289=CARTESIAN_POINT('Ctrl Pts',(-68.5694804955014,27.4160714044831,
12.));
#148290=CARTESIAN_POINT('Ctrl Pts',(-68.5504887252975,27.3968180187941,
0.));
#148291=CARTESIAN_POINT('Ctrl Pts',(-68.5504887252975,27.3968180187941,
12.));
#148292=CARTESIAN_POINT('Ctrl Pts',(-68.5315047488035,27.3776077300914,
0.));
#148293=CARTESIAN_POINT('Ctrl Pts',(-68.5315047488035,27.3776077300914,
12.));
#148294=CARTESIAN_POINT('Ctrl Pts',(-68.5125286621888,27.3584405685941,
0.));
#148295=CARTESIAN_POINT('Ctrl Pts',(-68.5125286621888,27.3584405685941,
12.));
#148296=CARTESIAN_POINT('Ctrl Pts',(-68.4935605626362,27.3393165646748,
0.));
#148297=CARTESIAN_POINT('Ctrl Pts',(-68.4935605626362,27.3393165646748,
12.));
#148298=CARTESIAN_POINT('Ctrl Pts',(-68.4746005480993,27.3202357488153,
0.));
#148299=CARTESIAN_POINT('Ctrl Pts',(-68.4746005480993,27.3202357488153,
12.));
#148300=CARTESIAN_POINT('Ctrl Pts',(-68.455648717044,27.301198151557,0.));
#148301=CARTESIAN_POINT('Ctrl Pts',(-68.455648717044,27.301198151557,12.));
#148302=CARTESIAN_POINT('Ctrl Pts',(-68.4367051682166,27.2822038034539,
0.));
#148303=CARTESIAN_POINT('Ctrl Pts',(-68.4367051682166,27.2822038034539,
12.));
#148304=CARTESIAN_POINT('Ctrl Pts',(-68.4177700003471,27.2632527350062,
0.));
#148305=CARTESIAN_POINT('Ctrl Pts',(-68.4177700003471,27.2632527350062,
12.));
#148306=CARTESIAN_POINT('Ctrl Pts',(-68.398843312159,27.2443449766654,0.));
#148307=CARTESIAN_POINT('Ctrl Pts',(-68.398843312159,27.2443449766654,12.));
#148308=CARTESIAN_POINT('Ctrl Pts',(-68.379925202511,27.2254805588677,0.));
#148309=CARTESIAN_POINT('Ctrl Pts',(-68.379925202511,27.2254805588677,12.));
#148310=CARTESIAN_POINT('Ctrl Pts',(-68.3610157704999,27.2066595120544,
0.));
#148311=CARTESIAN_POINT('Ctrl Pts',(-68.3610157704999,27.2066595120544,
12.));
#148312=CARTESIAN_POINT('Ctrl Pts',(-68.3421151155708,27.1878818666925,
0.));
#148313=CARTESIAN_POINT('Ctrl Pts',(-68.3421151155708,27.1878818666925,
12.));
#148314=CARTESIAN_POINT('Ctrl Pts',(-68.3232233376415,27.1691476532917,
0.));
#148315=CARTESIAN_POINT('Ctrl Pts',(-68.3232233376415,27.1691476532917,
12.));
#148316=CARTESIAN_POINT('Ctrl Pts',(-68.3043405371589,27.150456902413,0.));
#148317=CARTESIAN_POINT('Ctrl Pts',(-68.3043405371589,27.150456902413,12.));
#148318=CARTESIAN_POINT('Ctrl Pts',(-68.285466815035,27.1318096446643,0.));
#148319=CARTESIAN_POINT('Ctrl Pts',(-68.285466815035,27.1318096446643,12.));
#148320=CARTESIAN_POINT('Ctrl Pts',(-68.2666022726094,27.1132059106939,
0.));
#148321=CARTESIAN_POINT('Ctrl Pts',(-68.2666022726094,27.1132059106939,
12.));
#148322=CARTESIAN_POINT('Ctrl Pts',(-68.2477470116014,27.0946457311813,
0.));
#148323=CARTESIAN_POINT('Ctrl Pts',(-68.2477470116014,27.0946457311813,
12.));
#148324=CARTESIAN_POINT('Ctrl Pts',(-68.2289011340624,27.076129136823,0.));
#148325=CARTESIAN_POINT('Ctrl Pts',(-68.2289011340624,27.076129136823,12.));
#148326=CARTESIAN_POINT('Ctrl Pts',(-68.2100647423345,27.0576561583179,
0.));
#148327=CARTESIAN_POINT('Ctrl Pts',(-68.2100647423345,27.0576561583179,
12.));
#148328=CARTESIAN_POINT('Ctrl Pts',(-68.1912379390787,27.0392268263804,
0.));
#148329=CARTESIAN_POINT('Ctrl Pts',(-68.1912379390787,27.0392268263804,
12.));
#148330=CARTESIAN_POINT('Ctrl Pts',(-68.1724208272967,27.0208411717477,
0.));
#148331=CARTESIAN_POINT('Ctrl Pts',(-68.1724208272967,27.0208411717477,
12.));
#148332=CARTESIAN_POINT('Ctrl Pts',(-68.1536135103558,27.0024992251839,
0.));
#148333=CARTESIAN_POINT('Ctrl Pts',(-68.1536135103558,27.0024992251839,
12.));
#148334=CARTESIAN_POINT('Ctrl Pts',(-68.13481609201,26.9842010174819,0.));
#148335=CARTESIAN_POINT('Ctrl Pts',(-68.13481609201,26.9842010174819,12.));
#148336=CARTESIAN_POINT('Ctrl Pts',(-68.1160286764244,26.9659465794596,
0.));
#148337=CARTESIAN_POINT('Ctrl Pts',(-68.1160286764244,26.9659465794596,
12.));
#148338=CARTESIAN_POINT('Ctrl Pts',(-68.0972513681739,26.9477359419646,
0.));
#148339=CARTESIAN_POINT('Ctrl Pts',(-68.0972513681739,26.9477359419646,
12.));
#148340=CARTESIAN_POINT('Ctrl Pts',(-68.0784842722362,26.9295691358775,
0.));
#148341=CARTESIAN_POINT('Ctrl Pts',(-68.0784842722362,26.9295691358775,
12.));
#148342=CARTESIAN_POINT('Ctrl Pts',(-68.0597274939857,26.9114461921109,
0.));
#148343=CARTESIAN_POINT('Ctrl Pts',(-68.0597274939857,26.9114461921109,
12.));
#148344=CARTESIAN_POINT('Ctrl Pts',(-68.0409811391872,26.8933671416064,
0.));
#148345=CARTESIAN_POINT('Ctrl Pts',(-68.0409811391872,26.8933671416064,
12.));
#148346=CARTESIAN_POINT('Ctrl Pts',(-68.0222453139862,26.8753320153255,
0.));
#148347=CARTESIAN_POINT('Ctrl Pts',(-68.0222453139862,26.8753320153255,
12.));
#148348=CARTESIAN_POINT('Ctrl Pts',(-68.0035201249108,26.85734084425,0.));
#148349=CARTESIAN_POINT('Ctrl Pts',(-68.0035201249108,26.85734084425,12.));
#148350=CARTESIAN_POINT('Ctrl Pts',(-67.9848056788814,26.8393936593914,
0.));
#148351=CARTESIAN_POINT('Ctrl Pts',(-67.9848056788814,26.8393936593914,
12.));
#148352=CARTESIAN_POINT('Ctrl Pts',(-67.9661020832165,26.8214904917922,
0.));
#148353=CARTESIAN_POINT('Ctrl Pts',(-67.9661020832165,26.8214904917922,
12.));
#148354=CARTESIAN_POINT('Ctrl Pts',(-67.9474094456395,26.8036313725262,
0.));
#148355=CARTESIAN_POINT('Ctrl Pts',(-67.9474094456395,26.8036313725262,
12.));
#148356=CARTESIAN_POINT('Ctrl Pts',(-67.9287278742839,26.7858163326932,
0.));
#148357=CARTESIAN_POINT('Ctrl Pts',(-67.9287278742839,26.7858163326932,
12.));
#148358=CARTESIAN_POINT('Ctrl Pts',(-67.9100574776974,26.7680454034168,
0.));
#148359=CARTESIAN_POINT('Ctrl Pts',(-67.9100574776974,26.7680454034168,
12.));
#148360=CARTESIAN_POINT('Ctrl Pts',(-67.8913983648441,26.7503186158523,
0.));
#148361=CARTESIAN_POINT('Ctrl Pts',(-67.8913983648441,26.7503186158523,
12.));
#148362=CARTESIAN_POINT('Ctrl Pts',(-67.8727506451068,26.7326360011886,
0.));
#148363=CARTESIAN_POINT('Ctrl Pts',(-67.8727506451068,26.7326360011886,
12.));
#148364=CARTESIAN_POINT('Ctrl Pts',(-67.8541144282875,26.7149975906478,
0.));
#148365=CARTESIAN_POINT('Ctrl Pts',(-67.8541144282875,26.7149975906478,
12.));
#148366=CARTESIAN_POINT('Ctrl Pts',(-67.8354898246079,26.6974034154803,
0.));
#148367=CARTESIAN_POINT('Ctrl Pts',(-67.8354898246079,26.6974034154803,
12.));
#148368=CARTESIAN_POINT('Ctrl Pts',(-67.8168769447086,26.6798535069586,
0.));
#148369=CARTESIAN_POINT('Ctrl Pts',(-67.8168769447086,26.6798535069586,
12.));
#148370=CARTESIAN_POINT('Ctrl Pts',(-67.7982758996557,26.6623478963867,
0.));
#148371=CARTESIAN_POINT('Ctrl Pts',(-67.7982758996557,26.6623478963867,
12.));
#148372=CARTESIAN_POINT('Ctrl Pts',(-67.7796868009447,26.6448866151027,
0.));
#148373=CARTESIAN_POINT('Ctrl Pts',(-67.7796868009447,26.6448866151027,
12.));
#148374=CARTESIAN_POINT('Ctrl Pts',(-67.7611097605042,26.6274696944793,
0.));
#148375=CARTESIAN_POINT('Ctrl Pts',(-67.7611097605042,26.6274696944793,
12.));
#148376=CARTESIAN_POINT('Ctrl Pts',(-67.7425448906983,26.6100971659204,
0.));
#148377=CARTESIAN_POINT('Ctrl Pts',(-67.7425448906983,26.6100971659204,
12.));
#148378=CARTESIAN_POINT('Ctrl Pts',(-67.7239923043295,26.5927690608546,
0.));
#148379=CARTESIAN_POINT('Ctrl Pts',(-67.7239923043295,26.5927690608546,
12.));
#148380=CARTESIAN_POINT('Ctrl Pts',(-67.7054521146427,26.5754854107422,
0.));
#148381=CARTESIAN_POINT('Ctrl Pts',(-67.7054521146427,26.5754854107422,
12.));
#148382=CARTESIAN_POINT('Ctrl Pts',(-67.6869244353292,26.5582462470794,
0.));
#148383=CARTESIAN_POINT('Ctrl Pts',(-67.6869244353292,26.5582462470794,
12.));
#148384=CARTESIAN_POINT('Ctrl Pts',(-67.6684093805288,26.5410516013984,
0.));
#148385=CARTESIAN_POINT('Ctrl Pts',(-67.6684093805288,26.5410516013984,
12.));
#148386=CARTESIAN_POINT('Ctrl Pts',(-67.6499070648323,26.5239015052655,
0.));
#148387=CARTESIAN_POINT('Ctrl Pts',(-67.6499070648323,26.5239015052655,
12.));
#148388=CARTESIAN_POINT('Ctrl Pts',(-67.6314176032823,26.506795990273,0.));
#148389=CARTESIAN_POINT('Ctrl Pts',(-67.6314176032823,26.506795990273,12.));
#148390=CARTESIAN_POINT('Ctrl Pts',(-67.6129411113774,26.4897350880446,
0.));
#148391=CARTESIAN_POINT('Ctrl Pts',(-67.6129411113774,26.4897350880446,
12.));
#148392=CARTESIAN_POINT('Ctrl Pts',(-67.5944777050782,26.4727188302415,
0.));
#148393=CARTESIAN_POINT('Ctrl Pts',(-67.5944777050782,26.4727188302415,
12.));
#148394=CARTESIAN_POINT('Ctrl Pts',(-67.5760275008096,26.4557472485622,
0.));
#148395=CARTESIAN_POINT('Ctrl Pts',(-67.5760275008096,26.4557472485622,
12.));
#148396=CARTESIAN_POINT('Ctrl Pts',(-67.5575906154648,26.4388203747422,
0.));
#148397=CARTESIAN_POINT('Ctrl Pts',(-67.5575906154648,26.4388203747422,
12.));
#148398=CARTESIAN_POINT('Ctrl Pts',(-67.5391671664055,26.4219382405452,
0.));
#148399=CARTESIAN_POINT('Ctrl Pts',(-67.5391671664055,26.4219382405452,
12.));
#148400=CARTESIAN_POINT('Ctrl Pts',(-67.5207572714666,26.4051008777669,
0.));
#148401=CARTESIAN_POINT('Ctrl Pts',(-67.5207572714666,26.4051008777669,
12.));
#148402=CARTESIAN_POINT('Ctrl Pts',(-67.5023610489611,26.3883083182417,
0.));
#148403=CARTESIAN_POINT('Ctrl Pts',(-67.5023610489611,26.3883083182417,
12.));
#148404=CARTESIAN_POINT('Ctrl Pts',(-67.4839786176833,26.3715605938432,
0.));
#148405=CARTESIAN_POINT('Ctrl Pts',(-67.4839786176833,26.3715605938432,
12.));
#148406=CARTESIAN_POINT('Ctrl Pts',(-67.4656100969121,26.3548577364835,
0.));
#148407=CARTESIAN_POINT('Ctrl Pts',(-67.4656100969121,26.3548577364835,
12.));
#148408=CARTESIAN_POINT('Ctrl Pts',(-67.4472556064127,26.3381997781059,
0.));
#148409=CARTESIAN_POINT('Ctrl Pts',(-67.4472556064127,26.3381997781059,
12.));
#148410=CARTESIAN_POINT('Ctrl Pts',(-67.4289152664406,26.3215867506864,
0.));
#148411=CARTESIAN_POINT('Ctrl Pts',(-67.4289152664406,26.3215867506864,
12.));
#148412=CARTESIAN_POINT('Ctrl Pts',(-67.4105891977465,26.305018686241,0.));
#148413=CARTESIAN_POINT('Ctrl Pts',(-67.4105891977465,26.305018686241,12.));
#148414=CARTESIAN_POINT('Ctrl Pts',(-67.392277521581,26.288495616827,0.));
#148415=CARTESIAN_POINT('Ctrl Pts',(-67.392277521581,26.288495616827,12.));
#148416=CARTESIAN_POINT('Ctrl Pts',(-67.3739803596967,26.2720175745422,
0.));
#148417=CARTESIAN_POINT('Ctrl Pts',(-67.3739803596967,26.2720175745422,
12.));
#148418=CARTESIAN_POINT('Ctrl Pts',(-67.3556978343506,26.255584591518,0.));
#148419=CARTESIAN_POINT('Ctrl Pts',(-67.3556978343506,26.255584591518,12.));
#148420=CARTESIAN_POINT('Ctrl Pts',(-67.3374300683076,26.2391966999192,
0.));
#148421=CARTESIAN_POINT('Ctrl Pts',(-67.3374300683076,26.2391966999192,
12.));
#148422=CARTESIAN_POINT('Ctrl Pts',(-67.3191771848468,26.2228539319527,
0.));
#148423=CARTESIAN_POINT('Ctrl Pts',(-67.3191771848468,26.2228539319527,
12.));
#148424=CARTESIAN_POINT('Ctrl Pts',(-67.3009393077654,26.2065563198684,
0.));
#148425=CARTESIAN_POINT('Ctrl Pts',(-67.3009393077654,26.2065563198684,
12.));
#148426=CARTESIAN_POINT('Ctrl Pts',(-67.2827165613828,26.1903038959589,
0.));
#148427=CARTESIAN_POINT('Ctrl Pts',(-67.2827165613828,26.1903038959589,
12.));
#148428=CARTESIAN_POINT('Ctrl Pts',(-67.2645090705414,26.1740966925527,
0.));
#148429=CARTESIAN_POINT('Ctrl Pts',(-67.2645090705414,26.1740966925527,
12.));
#148430=CARTESIAN_POINT('Ctrl Pts',(-67.2463169606105,26.1579347420135,
0.));
#148431=CARTESIAN_POINT('Ctrl Pts',(-67.2463169606105,26.1579347420135,
12.));
#148432=CARTESIAN_POINT('Ctrl Pts',(-67.228140357493,26.1418180767487,0.));
#148433=CARTESIAN_POINT('Ctrl Pts',(-67.228140357493,26.1418180767487,12.));
#148434=CARTESIAN_POINT('Ctrl Pts',(-67.2099793876295,26.1257467292102,
0.));
#148435=CARTESIAN_POINT('Ctrl Pts',(-67.2099793876295,26.1257467292102,
12.));
#148436=CARTESIAN_POINT('Ctrl Pts',(-67.191834178002,26.109720731895,0.));
#148437=CARTESIAN_POINT('Ctrl Pts',(-67.191834178002,26.109720731895,12.));
#148438=CARTESIAN_POINT('Ctrl Pts',(-67.1737048561364,26.0937401173385,
0.));
#148439=CARTESIAN_POINT('Ctrl Pts',(-67.1737048561364,26.0937401173385,
12.));
#148440=CARTESIAN_POINT('Ctrl Pts',(-67.1555915501052,26.0778049181129,
0.));
#148441=CARTESIAN_POINT('Ctrl Pts',(-67.1555915501052,26.0778049181129,
12.));
#148442=CARTESIAN_POINT('Ctrl Pts',(-67.1374943885353,26.061915166836,0.));
#148443=CARTESIAN_POINT('Ctrl Pts',(-67.1374943885353,26.061915166836,12.));
#148444=CARTESIAN_POINT('Ctrl Pts',(-67.1194135006122,26.0460708961725,
0.));
#148445=CARTESIAN_POINT('Ctrl Pts',(-67.1194135006122,26.0460708961725,
12.));
#148446=CARTESIAN_POINT('Ctrl Pts',(-67.101349016084,26.030272138834,0.));
#148447=CARTESIAN_POINT('Ctrl Pts',(-67.101349016084,26.030272138834,12.));
#148448=CARTESIAN_POINT('Ctrl Pts',(-67.083301065264,26.0145189275733,0.));
#148449=CARTESIAN_POINT('Ctrl Pts',(-67.083301065264,26.0145189275733,12.));
#148450=CARTESIAN_POINT('Ctrl Pts',(-67.0652697790335,25.9988112951818,
0.));
#148451=CARTESIAN_POINT('Ctrl Pts',(-67.0652697790335,25.9988112951818,
12.));
#148452=CARTESIAN_POINT('Ctrl Pts',(-67.0472552888495,25.9831492744988,
0.));
#148453=CARTESIAN_POINT('Ctrl Pts',(-67.0472552888495,25.9831492744988,
12.));
#148454=CARTESIAN_POINT('Ctrl Pts',(-67.0292577267495,25.9675328984123,
0.));
#148455=CARTESIAN_POINT('Ctrl Pts',(-67.0292577267495,25.9675328984123,
12.));
#148456=CARTESIAN_POINT('Ctrl Pts',(-67.0112772253553,25.9519621998598,
0.));
#148457=CARTESIAN_POINT('Ctrl Pts',(-67.0112772253553,25.9519621998598,
12.));
#148458=CARTESIAN_POINT('Ctrl Pts',(-66.993313917876,25.9364372118216,0.));
#148459=CARTESIAN_POINT('Ctrl Pts',(-66.993313917876,25.9364372118216,12.));
#148460=CARTESIAN_POINT('Ctrl Pts',(-66.9753679381122,25.9209579673198,
0.));
#148461=CARTESIAN_POINT('Ctrl Pts',(-66.9753679381122,25.9209579673198,
12.));
#148462=CARTESIAN_POINT('Ctrl Pts',(-66.9574394204635,25.9055244994266,
0.));
#148463=CARTESIAN_POINT('Ctrl Pts',(-66.9574394204635,25.9055244994266,
12.));
#148464=CARTESIAN_POINT('Ctrl Pts',(-66.9395284999327,25.8901368412655,
0.));
#148465=CARTESIAN_POINT('Ctrl Pts',(-66.9395284999327,25.8901368412655,
12.));
#148466=CARTESIAN_POINT('Ctrl Pts',(-66.9216353121308,25.8747950260114,
0.));
#148467=CARTESIAN_POINT('Ctrl Pts',(-66.9216353121308,25.8747950260114,
12.));
#148468=CARTESIAN_POINT('Ctrl Pts',(-66.9037599932787,25.8594990868845,
0.));
#148469=CARTESIAN_POINT('Ctrl Pts',(-66.9037599932787,25.8594990868845,
12.));
#148470=CARTESIAN_POINT('Ctrl Pts',(-66.8859026802123,25.8442490571486,
0.));
#148471=CARTESIAN_POINT('Ctrl Pts',(-66.8859026802123,25.8442490571486,
12.));
#148472=CARTESIAN_POINT('Ctrl Pts',(-66.8680635103907,25.8290449701206,
0.));
#148473=CARTESIAN_POINT('Ctrl Pts',(-66.8680635103907,25.8290449701206,
12.));
#148474=CARTESIAN_POINT('Ctrl Pts',(-66.8502426219015,25.8138868591715,
0.));
#148475=CARTESIAN_POINT('Ctrl Pts',(-66.8502426219015,25.8138868591715,
12.));
#148476=CARTESIAN_POINT('Ctrl Pts',(-66.8324401534658,25.7987747577264,
0.));
#148477=CARTESIAN_POINT('Ctrl Pts',(-66.8324401534658,25.7987747577264,
12.));
#148478=CARTESIAN_POINT('Ctrl Pts',(-66.8146562444397,25.783708699258,0.));
#148479=CARTESIAN_POINT('Ctrl Pts',(-66.8146562444397,25.783708699258,12.));
#148480=CARTESIAN_POINT('Ctrl Pts',(-66.7968910348199,25.7686887172859,
0.));
#148481=CARTESIAN_POINT('Ctrl Pts',(-66.7968910348199,25.7686887172859,
12.));
#148482=CARTESIAN_POINT('Ctrl Pts',(-66.7791446652505,25.7537148453848,
0.));
#148483=CARTESIAN_POINT('Ctrl Pts',(-66.7791446652505,25.7537148453848,
12.));
#148484=CARTESIAN_POINT('Ctrl Pts',(-66.7614172770302,25.7387871171861,
0.));
#148485=CARTESIAN_POINT('Ctrl Pts',(-66.7614172770302,25.7387871171861,
12.));
#148486=CARTESIAN_POINT('Ctrl Pts',(-66.7437090121168,25.7239055663778,
0.));
#148487=CARTESIAN_POINT('Ctrl Pts',(-66.7437090121168,25.7239055663778,
12.));
#148488=CARTESIAN_POINT('Ctrl Pts',(-66.72602001313,25.7090702266976,0.));
#148489=CARTESIAN_POINT('Ctrl Pts',(-66.72602001313,25.7090702266976,12.));
#148490=CARTESIAN_POINT('Ctrl Pts',(-66.7083504233566,25.6942811319337,
0.));
#148491=CARTESIAN_POINT('Ctrl Pts',(-66.7083504233566,25.6942811319337,
12.));
#148492=CARTESIAN_POINT('Ctrl Pts',(-66.6907003867599,25.6795383159329,
0.));
#148493=CARTESIAN_POINT('Ctrl Pts',(-66.6907003867599,25.6795383159329,
12.));
#148494=CARTESIAN_POINT('Ctrl Pts',(-66.6730700479844,25.6648418126016,
0.));
#148495=CARTESIAN_POINT('Ctrl Pts',(-66.6730700479844,25.6648418126016,
12.));
#148496=CARTESIAN_POINT('Ctrl Pts',(-66.6554595523611,25.650191655905,0.));
#148497=CARTESIAN_POINT('Ctrl Pts',(-66.6554595523611,25.650191655905,12.));
#148498=CARTESIAN_POINT('Ctrl Pts',(-66.6378690459105,25.6355878798605,
0.));
#148499=CARTESIAN_POINT('Ctrl Pts',(-66.6378690459105,25.6355878798605,
12.));
#148500=CARTESIAN_POINT('Ctrl Pts',(-66.6202986753482,25.6210305185394,
0.));
#148501=CARTESIAN_POINT('Ctrl Pts',(-66.6202986753482,25.6210305185394,
12.));
#148502=CARTESIAN_POINT('Ctrl Pts',(-66.6027485880947,25.606519606075,0.));
#148503=CARTESIAN_POINT('Ctrl Pts',(-66.6027485880947,25.606519606075,12.));
#148504=CARTESIAN_POINT('Ctrl Pts',(-66.5852189322811,25.5920551766629,
0.));
#148505=CARTESIAN_POINT('Ctrl Pts',(-66.5852189322811,25.5920551766629,
12.));
#148506=CARTESIAN_POINT('Ctrl Pts',(-66.5677098567551,25.5776372645605,
0.));
#148507=CARTESIAN_POINT('Ctrl Pts',(-66.5677098567551,25.5776372645605,
12.));
#148508=CARTESIAN_POINT('Ctrl Pts',(-66.5502215110843,25.5632659040797,
0.));
#148509=CARTESIAN_POINT('Ctrl Pts',(-66.5502215110843,25.5632659040797,
12.));
#148510=CARTESIAN_POINT('Ctrl Pts',(-66.5327540455639,25.5489411295916,
0.));
#148511=CARTESIAN_POINT('Ctrl Pts',(-66.5327540455639,25.5489411295916,
12.));
#148512=CARTESIAN_POINT('Ctrl Pts',(-66.5153076112237,25.5346629755322,
0.));
#148513=CARTESIAN_POINT('Ctrl Pts',(-66.5153076112237,25.5346629755322,
12.));
#148514=CARTESIAN_POINT('Ctrl Pts',(-66.4978823598352,25.5204314764033,
0.));
#148515=CARTESIAN_POINT('Ctrl Pts',(-66.4978823598352,25.5204314764033,
12.));
#148516=CARTESIAN_POINT('Ctrl Pts',(-66.4804784439146,25.5062466667703,
0.));
#148517=CARTESIAN_POINT('Ctrl Pts',(-66.4804784439146,25.5062466667703,
12.));
#148518=CARTESIAN_POINT('Ctrl Pts',(-66.463096016725,25.4921085812548,0.));
#148519=CARTESIAN_POINT('Ctrl Pts',(-66.463096016725,25.4921085812548,12.));
#148520=CARTESIAN_POINT('Ctrl Pts',(-66.445735232287,25.4780172545418,0.));
#148521=CARTESIAN_POINT('Ctrl Pts',(-66.445735232287,25.4780172545418,12.));
#148522=CARTESIAN_POINT('Ctrl Pts',(-66.4283962453899,25.463972721385,0.));
#148523=CARTESIAN_POINT('Ctrl Pts',(-66.4283962453899,25.463972721385,12.));
#148524=CARTESIAN_POINT('Ctrl Pts',(-66.4110792116,25.4499750166079,0.));
#148525=CARTESIAN_POINT('Ctrl Pts',(-66.4110792116,25.4499750166079,12.));
#148526=CARTESIAN_POINT('Ctrl Pts',(-66.3937842872684,25.4360241751017,
0.));
#148527=CARTESIAN_POINT('Ctrl Pts',(-66.3937842872684,25.4360241751017,
12.));
#148528=CARTESIAN_POINT('Ctrl Pts',(-66.3765116295364,25.4221202318198,
0.));
#148529=CARTESIAN_POINT('Ctrl Pts',(-66.3765116295364,25.4221202318198,
12.));
#148530=CARTESIAN_POINT('Ctrl Pts',(-66.3592613963407,25.4082632217846,
0.));
#148531=CARTESIAN_POINT('Ctrl Pts',(-66.3592613963407,25.4082632217846,
12.));
#148532=CARTESIAN_POINT('Ctrl Pts',(-66.3420337464176,25.39445318009,0.));
#148533=CARTESIAN_POINT('Ctrl Pts',(-66.3420337464176,25.39445318009,12.));
#148534=CARTESIAN_POINT('Ctrl Pts',(-66.3248288393046,25.3806901419012,
0.));
#148535=CARTESIAN_POINT('Ctrl Pts',(-66.3248288393046,25.3806901419012,
12.));
#148536=CARTESIAN_POINT('Ctrl Pts',(-66.3076468353417,25.366974142449,0.));
#148537=CARTESIAN_POINT('Ctrl Pts',(-66.3076468353417,25.366974142449,12.));
#148538=CARTESIAN_POINT('Ctrl Pts',(-66.2904878956721,25.3533052170253,
0.));
#148539=CARTESIAN_POINT('Ctrl Pts',(-66.2904878956721,25.3533052170253,
12.));
#148540=CARTESIAN_POINT('Ctrl Pts',(-66.2733521822675,25.3396834009954,
0.));
#148541=CARTESIAN_POINT('Ctrl Pts',(-66.2733521822675,25.3396834009954,
12.));
#148542=CARTESIAN_POINT('Ctrl Pts',(-66.2562398579479,25.3261087298029,
0.));
#148543=CARTESIAN_POINT('Ctrl Pts',(-66.2562398579479,25.3261087298029,
12.));
#148544=CARTESIAN_POINT('Ctrl Pts',(-66.2391510863992,25.3125812389727,
0.));
#148545=CARTESIAN_POINT('Ctrl Pts',(-66.2391510863992,25.3125812389727,
12.));
#148546=CARTESIAN_POINT('Ctrl Pts',(-66.2220860321931,25.2991009641086,
0.));
#148547=CARTESIAN_POINT('Ctrl Pts',(-66.2220860321931,25.2991009641086,
12.));
#148548=CARTESIAN_POINT('Ctrl Pts',(-66.2050448607883,25.285667940892,0.));
#148549=CARTESIAN_POINT('Ctrl Pts',(-66.2050448607883,25.285667940892,12.));
#148550=CARTESIAN_POINT('Ctrl Pts',(-66.1880277385114,25.2722822050828,
0.));
#148551=CARTESIAN_POINT('Ctrl Pts',(-66.1880277385114,25.2722822050828,
12.));
#148552=CARTESIAN_POINT('Ctrl Pts',(-66.1710348325378,25.2589437925145,
0.));
#148553=CARTESIAN_POINT('Ctrl Pts',(-66.1710348325378,25.2589437925145,
12.));
#148554=CARTESIAN_POINT('Ctrl Pts',(-66.1540663108767,25.245652739088,0.));
#148555=CARTESIAN_POINT('Ctrl Pts',(-66.1540663108767,25.245652739088,12.));
#148556=CARTESIAN_POINT('Ctrl Pts',(-66.1371223423372,25.232409080756,0.));
#148557=CARTESIAN_POINT('Ctrl Pts',(-66.1371223423372,25.232409080756,12.));
#148558=CARTESIAN_POINT('Ctrl Pts',(-66.1202030965785,25.2192128535367,
0.));
#148559=CARTESIAN_POINT('Ctrl Pts',(-66.1202030965785,25.2192128535367,
12.));
#148560=CARTESIAN_POINT('Ctrl Pts',(-66.1033087441916,25.2060640935371,
0.));
#148561=CARTESIAN_POINT('Ctrl Pts',(-66.1033087441916,25.2060640935371,
12.));
#148562=CARTESIAN_POINT('Ctrl Pts',(-66.086439456768,25.1929628369685,0.));
#148563=CARTESIAN_POINT('Ctrl Pts',(-66.086439456768,25.1929628369685,12.));
#148564=CARTESIAN_POINT('Ctrl Pts',(-66.0695954069699,25.1799091201594,
0.));
#148565=CARTESIAN_POINT('Ctrl Pts',(-66.0695954069699,25.1799091201594,
12.));
#148566=CARTESIAN_POINT('Ctrl Pts',(-66.0527767686,25.1669029795651,0.));
#148567=CARTESIAN_POINT('Ctrl Pts',(-66.0527767686,25.1669029795651,12.));
#148568=CARTESIAN_POINT('Ctrl Pts',(-66.0359837164709,25.1539444517409,
0.));
#148569=CARTESIAN_POINT('Ctrl Pts',(-66.0359837164709,25.1539444517409,
12.));
#148570=CARTESIAN_POINT('Ctrl Pts',(-66.0192164262607,25.1410335733094,
0.));
#148571=CARTESIAN_POINT('Ctrl Pts',(-66.0192164262607,25.1410335733094,
12.));
#148572=CARTESIAN_POINT('Ctrl Pts',(-66.0024750743902,25.1281703809299,
0.));
#148573=CARTESIAN_POINT('Ctrl Pts',(-66.0024750743902,25.1281703809299,
12.));
#148574=CARTESIAN_POINT('Ctrl Pts',(-65.9857598378455,25.1153549112511,
0.));
#148575=CARTESIAN_POINT('Ctrl Pts',(-65.9857598378455,25.1153549112511,
12.));
#148576=CARTESIAN_POINT('Ctrl Pts',(-65.9690708941591,25.1025872009016,
0.));
#148577=CARTESIAN_POINT('Ctrl Pts',(-65.9690708941591,25.1025872009016,
12.));
#148578=CARTESIAN_POINT('Ctrl Pts',(-65.9524084218167,25.0898672865926,
0.));
#148579=CARTESIAN_POINT('Ctrl Pts',(-65.9524084218167,25.0898672865926,
12.));
#148580=CARTESIAN_POINT('Ctrl Pts',(-65.9357726006174,25.0771952052032,
0.));
#148581=CARTESIAN_POINT('Ctrl Pts',(-65.9357726006174,25.0771952052032,
12.));
#148582=CARTESIAN_POINT('Ctrl Pts',(-65.9191636119796,25.0645709938519,
0.));
#148583=CARTESIAN_POINT('Ctrl Pts',(-65.9191636119796,25.0645709938519,
12.));
#148584=CARTESIAN_POINT('Ctrl Pts',(-65.9025816394391,25.0519946900066,
0.));
#148585=CARTESIAN_POINT('Ctrl Pts',(-65.9025816394391,25.0519946900066,
12.));
#148586=CARTESIAN_POINT('Ctrl Pts',(-65.8860268683088,25.039466331404,0.));
#148587=CARTESIAN_POINT('Ctrl Pts',(-65.8860268683088,25.039466331404,12.));
#148588=CARTESIAN_POINT('Ctrl Pts',(-65.8694994847587,25.0269859558351,
0.));
#148589=CARTESIAN_POINT('Ctrl Pts',(-65.8694994847587,25.0269859558351,
12.));
#148590=CARTESIAN_POINT('Ctrl Pts',(-65.8529996750441,25.0145536009603,
0.));
#148591=CARTESIAN_POINT('Ctrl Pts',(-65.8529996750441,25.0145536009603,
12.));
#148592=CARTESIAN_POINT('Ctrl Pts',(-65.8365276247157,25.0021693041181,
0.));
#148593=CARTESIAN_POINT('Ctrl Pts',(-65.8365276247157,25.0021693041181,
12.));
#148594=CARTESIAN_POINT('Ctrl Pts',(-65.8200835177071,24.9898331021002,
0.));
#148595=CARTESIAN_POINT('Ctrl Pts',(-65.8200835177071,24.9898331021002,
12.));
#148596=CARTESIAN_POINT('Ctrl Pts',(-65.8036675380761,24.97754503157,0.));
#148597=CARTESIAN_POINT('Ctrl Pts',(-65.8036675380761,24.97754503157,12.));
#148598=CARTESIAN_POINT('Ctrl Pts',(-65.7872798720847,24.965305129559,0.));
#148599=CARTESIAN_POINT('Ctrl Pts',(-65.7872798720847,24.965305129559,12.));
#148600=CARTESIAN_POINT('Ctrl Pts',(-65.7709207098949,24.9531134338693,
0.));
#148601=CARTESIAN_POINT('Ctrl Pts',(-65.7709207098949,24.9531134338693,
12.));
#148602=CARTESIAN_POINT('Ctrl Pts',(-65.7545902480286,24.9409699836523,
0.));
#148603=CARTESIAN_POINT('Ctrl Pts',(-65.7545902480286,24.9409699836523,
12.));
#148604=CARTESIAN_POINT('Ctrl Pts',(-65.7382886895839,24.9288748194562,
0.));
#148605=CARTESIAN_POINT('Ctrl Pts',(-65.7382886895839,24.9288748194562,
12.));
#148606=CARTESIAN_POINT('Ctrl Pts',(-65.7220162391016,24.9168279820093,
0.));
#148607=CARTESIAN_POINT('Ctrl Pts',(-65.7220162391016,24.9168279820093,
12.));
#148608=CARTESIAN_POINT('Ctrl Pts',(-65.7057730980471,24.9048295111444,
0.));
#148609=CARTESIAN_POINT('Ctrl Pts',(-65.7057730980471,24.9048295111444,
12.));
#148610=CARTESIAN_POINT('Ctrl Pts',(-65.6895594608798,24.8928794448615,
0.));
#148611=CARTESIAN_POINT('Ctrl Pts',(-65.6895594608798,24.8928794448615,
12.));
#148612=CARTESIAN_POINT('Ctrl Pts',(-65.6733755087724,24.8809778178248,
0.));
#148613=CARTESIAN_POINT('Ctrl Pts',(-65.6733755087724,24.8809778178248,
12.));
#148614=CARTESIAN_POINT('Ctrl Pts',(-65.6572214156761,24.869124662808,0.));
#148615=CARTESIAN_POINT('Ctrl Pts',(-65.6572214156761,24.869124662808,12.));
#148616=CARTESIAN_POINT('Ctrl Pts',(-65.6410973603713,24.8573200135683,
0.));
#148617=CARTESIAN_POINT('Ctrl Pts',(-65.6410973603713,24.8573200135683,
12.));
#148618=CARTESIAN_POINT('Ctrl Pts',(-65.6250035361612,24.8455639071517,
0.));
#148619=CARTESIAN_POINT('Ctrl Pts',(-65.6250035361612,24.8455639071517,
12.));
#148620=CARTESIAN_POINT('Ctrl Pts',(-65.6089401625552,24.8338563866739,
0.));
#148621=CARTESIAN_POINT('Ctrl Pts',(-65.6089401625552,24.8338563866739,
12.));
#148622=CARTESIAN_POINT('Ctrl Pts',(-65.5929074932487,24.8221975032059,
0.));
#148623=CARTESIAN_POINT('Ctrl Pts',(-65.5929074932487,24.8221975032059,
12.));
#148624=CARTESIAN_POINT('Ctrl Pts',(-65.5769057914184,24.8105873098578,
0.));
#148625=CARTESIAN_POINT('Ctrl Pts',(-65.5769057914184,24.8105873098578,
12.));
#148626=CARTESIAN_POINT('Ctrl Pts',(-65.560935306275,24.7990258561234,0.));
#148627=CARTESIAN_POINT('Ctrl Pts',(-65.560935306275,24.7990258561234,12.));
#148628=CARTESIAN_POINT('Ctrl Pts',(-65.5449962514735,24.7875131827515,
0.));
#148629=CARTESIAN_POINT('Ctrl Pts',(-65.5449962514735,24.7875131827515,
12.));
#148630=CARTESIAN_POINT('Ctrl Pts',(-65.5290887770494,24.776049314855,0.));
#148631=CARTESIAN_POINT('Ctrl Pts',(-65.5290887770494,24.776049314855,12.));
#148632=CARTESIAN_POINT('Ctrl Pts',(-65.5132129675727,24.7646342620969,
0.));
#148633=CARTESIAN_POINT('Ctrl Pts',(-65.5132129675727,24.7646342620969,
12.));
#148634=CARTESIAN_POINT('Ctrl Pts',(-65.5005376841469,24.755541272477,0.));
#148635=CARTESIAN_POINT('Ctrl Pts',(-65.5005376841469,24.755541272477,12.));
#148636=CARTESIAN_POINT('Ctrl Pts',(-65.4910454936487,24.7487434956058,
0.));
#148637=CARTESIAN_POINT('Ctrl Pts',(-65.4910454936487,24.7487434956058,
12.));
#148638=CARTESIAN_POINT('Ctrl Pts',(-65.484723709553,24.7442214063411,0.));
#148639=CARTESIAN_POINT('Ctrl Pts',(-65.484723709553,24.7442214063411,12.));
#148640=CARTESIAN_POINT('Ctrl Pts',(-65.4815644032299,24.7419628022042,
0.));
#148641=CARTESIAN_POINT('Ctrl Pts',(-65.4815644032299,24.7419628022042,
12.));
#148642=CARTESIAN_POINT('',(-65.4815644032299,24.7419628022042,12.));
#148643=CARTESIAN_POINT('Ctrl Pts',(-65.4815644032299,24.7419628022042,
12.));
#148644=CARTESIAN_POINT('Ctrl Pts',(-65.484723709553,24.7442214063411,12.));
#148645=CARTESIAN_POINT('Ctrl Pts',(-65.4910454936487,24.7487434956058,
12.));
#148646=CARTESIAN_POINT('Ctrl Pts',(-65.5005376841469,24.755541272477,12.));
#148647=CARTESIAN_POINT('Ctrl Pts',(-65.5132129675727,24.7646342620969,
12.));
#148648=CARTESIAN_POINT('Ctrl Pts',(-65.5290887770494,24.776049314855,12.));
#148649=CARTESIAN_POINT('Ctrl Pts',(-65.5449962514735,24.7875131827515,
12.));
#148650=CARTESIAN_POINT('Ctrl Pts',(-65.560935306275,24.7990258561234,12.));
#148651=CARTESIAN_POINT('Ctrl Pts',(-65.5769057914184,24.8105873098578,
12.));
#148652=CARTESIAN_POINT('Ctrl Pts',(-65.5929074932487,24.8221975032059,
12.));
#148653=CARTESIAN_POINT('Ctrl Pts',(-65.6089401625552,24.8338563866739,
12.));
#148654=CARTESIAN_POINT('Ctrl Pts',(-65.6250035361612,24.8455639071517,
12.));
#148655=CARTESIAN_POINT('Ctrl Pts',(-65.6410973603713,24.8573200135683,
12.));
#148656=CARTESIAN_POINT('Ctrl Pts',(-65.6572214156761,24.869124662808,12.));
#148657=CARTESIAN_POINT('Ctrl Pts',(-65.6733755087724,24.8809778178248,
12.));
#148658=CARTESIAN_POINT('Ctrl Pts',(-65.6895594608798,24.8928794448615,
12.));
#148659=CARTESIAN_POINT('Ctrl Pts',(-65.7057730980471,24.9048295111444,
12.));
#148660=CARTESIAN_POINT('Ctrl Pts',(-65.7220162391016,24.9168279820093,
12.));
#148661=CARTESIAN_POINT('Ctrl Pts',(-65.7382886895839,24.9288748194562,
12.));
#148662=CARTESIAN_POINT('Ctrl Pts',(-65.7545902480286,24.9409699836523,
12.));
#148663=CARTESIAN_POINT('Ctrl Pts',(-65.7709207098949,24.9531134338693,
12.));
#148664=CARTESIAN_POINT('Ctrl Pts',(-65.7872798720847,24.965305129559,12.));
#148665=CARTESIAN_POINT('Ctrl Pts',(-65.8036675380761,24.97754503157,12.));
#148666=CARTESIAN_POINT('Ctrl Pts',(-65.8200835177071,24.9898331021002,
12.));
#148667=CARTESIAN_POINT('Ctrl Pts',(-65.8365276247157,25.0021693041181,
12.));
#148668=CARTESIAN_POINT('Ctrl Pts',(-65.8529996750441,25.0145536009603,
12.));
#148669=CARTESIAN_POINT('Ctrl Pts',(-65.8694994847587,25.0269859558351,
12.));
#148670=CARTESIAN_POINT('Ctrl Pts',(-65.8860268683088,25.039466331404,12.));
#148671=CARTESIAN_POINT('Ctrl Pts',(-65.9025816394391,25.0519946900066,
12.));
#148672=CARTESIAN_POINT('Ctrl Pts',(-65.9191636119796,25.0645709938519,
12.));
#148673=CARTESIAN_POINT('Ctrl Pts',(-65.9357726006174,25.0771952052032,
12.));
#148674=CARTESIAN_POINT('Ctrl Pts',(-65.9524084218167,25.0898672865926,
12.));
#148675=CARTESIAN_POINT('Ctrl Pts',(-65.9690708941591,25.1025872009016,
12.));
#148676=CARTESIAN_POINT('Ctrl Pts',(-65.9857598378455,25.1153549112511,
12.));
#148677=CARTESIAN_POINT('Ctrl Pts',(-66.0024750743902,25.1281703809299,
12.));
#148678=CARTESIAN_POINT('Ctrl Pts',(-66.0192164262607,25.1410335733094,
12.));
#148679=CARTESIAN_POINT('Ctrl Pts',(-66.0359837164709,25.1539444517409,
12.));
#148680=CARTESIAN_POINT('Ctrl Pts',(-66.0527767686,25.1669029795651,12.));
#148681=CARTESIAN_POINT('Ctrl Pts',(-66.0695954069699,25.1799091201594,
12.));
#148682=CARTESIAN_POINT('Ctrl Pts',(-66.086439456768,25.1929628369685,12.));
#148683=CARTESIAN_POINT('Ctrl Pts',(-66.1033087441916,25.2060640935371,
12.));
#148684=CARTESIAN_POINT('Ctrl Pts',(-66.1202030965785,25.2192128535367,
12.));
#148685=CARTESIAN_POINT('Ctrl Pts',(-66.1371223423372,25.232409080756,12.));
#148686=CARTESIAN_POINT('Ctrl Pts',(-66.1540663108767,25.245652739088,12.));
#148687=CARTESIAN_POINT('Ctrl Pts',(-66.1710348325378,25.2589437925145,
12.));
#148688=CARTESIAN_POINT('Ctrl Pts',(-66.1880277385114,25.2722822050828,
12.));
#148689=CARTESIAN_POINT('Ctrl Pts',(-66.2050448607883,25.285667940892,12.));
#148690=CARTESIAN_POINT('Ctrl Pts',(-66.2220860321931,25.2991009641086,
12.));
#148691=CARTESIAN_POINT('Ctrl Pts',(-66.2391510863992,25.3125812389727,
12.));
#148692=CARTESIAN_POINT('Ctrl Pts',(-66.2562398579479,25.3261087298029,
12.));
#148693=CARTESIAN_POINT('Ctrl Pts',(-66.2733521822675,25.3396834009954,
12.));
#148694=CARTESIAN_POINT('Ctrl Pts',(-66.2904878956721,25.3533052170253,
12.));
#148695=CARTESIAN_POINT('Ctrl Pts',(-66.3076468353417,25.366974142449,12.));
#148696=CARTESIAN_POINT('Ctrl Pts',(-66.3248288393046,25.3806901419012,
12.));
#148697=CARTESIAN_POINT('Ctrl Pts',(-66.3420337464176,25.39445318009,12.));
#148698=CARTESIAN_POINT('Ctrl Pts',(-66.3592613963407,25.4082632217846,
12.));
#148699=CARTESIAN_POINT('Ctrl Pts',(-66.3765116295364,25.4221202318198,
12.));
#148700=CARTESIAN_POINT('Ctrl Pts',(-66.3937842872684,25.4360241751017,
12.));
#148701=CARTESIAN_POINT('Ctrl Pts',(-66.4110792116,25.4499750166079,12.));
#148702=CARTESIAN_POINT('Ctrl Pts',(-66.4283962453899,25.463972721385,12.));
#148703=CARTESIAN_POINT('Ctrl Pts',(-66.445735232287,25.4780172545418,12.));
#148704=CARTESIAN_POINT('Ctrl Pts',(-66.463096016725,25.4921085812548,12.));
#148705=CARTESIAN_POINT('Ctrl Pts',(-66.4804784439146,25.5062466667703,
12.));
#148706=CARTESIAN_POINT('Ctrl Pts',(-66.4978823598352,25.5204314764033,
12.));
#148707=CARTESIAN_POINT('Ctrl Pts',(-66.5153076112237,25.5346629755322,
12.));
#148708=CARTESIAN_POINT('Ctrl Pts',(-66.5327540455639,25.5489411295916,
12.));
#148709=CARTESIAN_POINT('Ctrl Pts',(-66.5502215110843,25.5632659040797,
12.));
#148710=CARTESIAN_POINT('Ctrl Pts',(-66.5677098567551,25.5776372645605,
12.));
#148711=CARTESIAN_POINT('Ctrl Pts',(-66.5852189322811,25.5920551766629,
12.));
#148712=CARTESIAN_POINT('Ctrl Pts',(-66.6027485880947,25.606519606075,12.));
#148713=CARTESIAN_POINT('Ctrl Pts',(-66.6202986753482,25.6210305185394,
12.));
#148714=CARTESIAN_POINT('Ctrl Pts',(-66.6378690459105,25.6355878798605,
12.));
#148715=CARTESIAN_POINT('Ctrl Pts',(-66.6554595523611,25.650191655905,12.));
#148716=CARTESIAN_POINT('Ctrl Pts',(-66.6730700479844,25.6648418126016,
12.));
#148717=CARTESIAN_POINT('Ctrl Pts',(-66.6907003867599,25.6795383159329,
12.));
#148718=CARTESIAN_POINT('Ctrl Pts',(-66.7083504233566,25.6942811319337,
12.));
#148719=CARTESIAN_POINT('Ctrl Pts',(-66.72602001313,25.7090702266976,12.));
#148720=CARTESIAN_POINT('Ctrl Pts',(-66.7437090121168,25.7239055663778,
12.));
#148721=CARTESIAN_POINT('Ctrl Pts',(-66.7614172770302,25.7387871171861,
12.));
#148722=CARTESIAN_POINT('Ctrl Pts',(-66.7791446652505,25.7537148453848,
12.));
#148723=CARTESIAN_POINT('Ctrl Pts',(-66.7968910348199,25.7686887172859,
12.));
#148724=CARTESIAN_POINT('Ctrl Pts',(-66.8146562444397,25.783708699258,12.));
#148725=CARTESIAN_POINT('Ctrl Pts',(-66.8324401534658,25.7987747577264,
12.));
#148726=CARTESIAN_POINT('Ctrl Pts',(-66.8502426219015,25.8138868591715,
12.));
#148727=CARTESIAN_POINT('Ctrl Pts',(-66.8680635103907,25.8290449701206,
12.));
#148728=CARTESIAN_POINT('Ctrl Pts',(-66.8859026802123,25.8442490571486,
12.));
#148729=CARTESIAN_POINT('Ctrl Pts',(-66.9037599932787,25.8594990868845,
12.));
#148730=CARTESIAN_POINT('Ctrl Pts',(-66.9216353121308,25.8747950260114,
12.));
#148731=CARTESIAN_POINT('Ctrl Pts',(-66.9395284999327,25.8901368412655,
12.));
#148732=CARTESIAN_POINT('Ctrl Pts',(-66.9574394204635,25.9055244994266,
12.));
#148733=CARTESIAN_POINT('Ctrl Pts',(-66.9753679381122,25.9209579673198,
12.));
#148734=CARTESIAN_POINT('Ctrl Pts',(-66.993313917876,25.9364372118216,12.));
#148735=CARTESIAN_POINT('Ctrl Pts',(-67.0112772253553,25.9519621998598,
12.));
#148736=CARTESIAN_POINT('Ctrl Pts',(-67.0292577267495,25.9675328984123,
12.));
#148737=CARTESIAN_POINT('Ctrl Pts',(-67.0472552888495,25.9831492744988,
12.));
#148738=CARTESIAN_POINT('Ctrl Pts',(-67.0652697790335,25.9988112951818,
12.));
#148739=CARTESIAN_POINT('Ctrl Pts',(-67.083301065264,26.0145189275733,12.));
#148740=CARTESIAN_POINT('Ctrl Pts',(-67.101349016084,26.030272138834,12.));
#148741=CARTESIAN_POINT('Ctrl Pts',(-67.1194135006122,26.0460708961725,
12.));
#148742=CARTESIAN_POINT('Ctrl Pts',(-67.1374943885353,26.061915166836,12.));
#148743=CARTESIAN_POINT('Ctrl Pts',(-67.1555915501052,26.0778049181129,
12.));
#148744=CARTESIAN_POINT('Ctrl Pts',(-67.1737048561364,26.0937401173385,
12.));
#148745=CARTESIAN_POINT('Ctrl Pts',(-67.191834178002,26.109720731895,12.));
#148746=CARTESIAN_POINT('Ctrl Pts',(-67.2099793876295,26.1257467292102,
12.));
#148747=CARTESIAN_POINT('Ctrl Pts',(-67.228140357493,26.1418180767487,12.));
#148748=CARTESIAN_POINT('Ctrl Pts',(-67.2463169606105,26.1579347420135,
12.));
#148749=CARTESIAN_POINT('Ctrl Pts',(-67.2645090705414,26.1740966925527,
12.));
#148750=CARTESIAN_POINT('Ctrl Pts',(-67.2827165613828,26.1903038959589,
12.));
#148751=CARTESIAN_POINT('Ctrl Pts',(-67.3009393077654,26.2065563198684,
12.));
#148752=CARTESIAN_POINT('Ctrl Pts',(-67.3191771848468,26.2228539319527,
12.));
#148753=CARTESIAN_POINT('Ctrl Pts',(-67.3374300683076,26.2391966999192,
12.));
#148754=CARTESIAN_POINT('Ctrl Pts',(-67.3556978343506,26.255584591518,12.));
#148755=CARTESIAN_POINT('Ctrl Pts',(-67.3739803596967,26.2720175745422,
12.));
#148756=CARTESIAN_POINT('Ctrl Pts',(-67.392277521581,26.288495616827,12.));
#148757=CARTESIAN_POINT('Ctrl Pts',(-67.4105891977465,26.305018686241,12.));
#148758=CARTESIAN_POINT('Ctrl Pts',(-67.4289152664406,26.3215867506864,
12.));
#148759=CARTESIAN_POINT('Ctrl Pts',(-67.4472556064127,26.3381997781059,
12.));
#148760=CARTESIAN_POINT('Ctrl Pts',(-67.4656100969121,26.3548577364835,
12.));
#148761=CARTESIAN_POINT('Ctrl Pts',(-67.4839786176833,26.3715605938432,
12.));
#148762=CARTESIAN_POINT('Ctrl Pts',(-67.5023610489611,26.3883083182417,
12.));
#148763=CARTESIAN_POINT('Ctrl Pts',(-67.5207572714666,26.4051008777669,
12.));
#148764=CARTESIAN_POINT('Ctrl Pts',(-67.5391671664055,26.4219382405452,
12.));
#148765=CARTESIAN_POINT('Ctrl Pts',(-67.5575906154648,26.4388203747422,
12.));
#148766=CARTESIAN_POINT('Ctrl Pts',(-67.5760275008096,26.4557472485622,
12.));
#148767=CARTESIAN_POINT('Ctrl Pts',(-67.5944777050782,26.4727188302415,
12.));
#148768=CARTESIAN_POINT('Ctrl Pts',(-67.6129411113774,26.4897350880446,
12.));
#148769=CARTESIAN_POINT('Ctrl Pts',(-67.6314176032823,26.506795990273,12.));
#148770=CARTESIAN_POINT('Ctrl Pts',(-67.6499070648323,26.5239015052655,
12.));
#148771=CARTESIAN_POINT('Ctrl Pts',(-67.6684093805288,26.5410516013984,
12.));
#148772=CARTESIAN_POINT('Ctrl Pts',(-67.6869244353292,26.5582462470794,
12.));
#148773=CARTESIAN_POINT('Ctrl Pts',(-67.7054521146427,26.5754854107422,
12.));
#148774=CARTESIAN_POINT('Ctrl Pts',(-67.7239923043295,26.5927690608546,
12.));
#148775=CARTESIAN_POINT('Ctrl Pts',(-67.7425448906983,26.6100971659204,
12.));
#148776=CARTESIAN_POINT('Ctrl Pts',(-67.7611097605042,26.6274696944793,
12.));
#148777=CARTESIAN_POINT('Ctrl Pts',(-67.7796868009447,26.6448866151027,
12.));
#148778=CARTESIAN_POINT('Ctrl Pts',(-67.7982758996557,26.6623478963867,
12.));
#148779=CARTESIAN_POINT('Ctrl Pts',(-67.8168769447086,26.6798535069586,
12.));
#148780=CARTESIAN_POINT('Ctrl Pts',(-67.8354898246079,26.6974034154803,
12.));
#148781=CARTESIAN_POINT('Ctrl Pts',(-67.8541144282875,26.7149975906478,
12.));
#148782=CARTESIAN_POINT('Ctrl Pts',(-67.8727506451068,26.7326360011886,
12.));
#148783=CARTESIAN_POINT('Ctrl Pts',(-67.8913983648441,26.7503186158523,
12.));
#148784=CARTESIAN_POINT('Ctrl Pts',(-67.9100574776974,26.7680454034168,
12.));
#148785=CARTESIAN_POINT('Ctrl Pts',(-67.9287278742839,26.7858163326932,
12.));
#148786=CARTESIAN_POINT('Ctrl Pts',(-67.9474094456395,26.8036313725262,
12.));
#148787=CARTESIAN_POINT('Ctrl Pts',(-67.9661020832165,26.8214904917922,
12.));
#148788=CARTESIAN_POINT('Ctrl Pts',(-67.9848056788814,26.8393936593914,
12.));
#148789=CARTESIAN_POINT('Ctrl Pts',(-68.0035201249108,26.85734084425,12.));
#148790=CARTESIAN_POINT('Ctrl Pts',(-68.0222453139862,26.8753320153255,
12.));
#148791=CARTESIAN_POINT('Ctrl Pts',(-68.0409811391872,26.8933671416064,
12.));
#148792=CARTESIAN_POINT('Ctrl Pts',(-68.0597274939857,26.9114461921109,
12.));
#148793=CARTESIAN_POINT('Ctrl Pts',(-68.0784842722362,26.9295691358775,
12.));
#148794=CARTESIAN_POINT('Ctrl Pts',(-68.0972513681739,26.9477359419646,
12.));
#148795=CARTESIAN_POINT('Ctrl Pts',(-68.1160286764244,26.9659465794596,
12.));
#148796=CARTESIAN_POINT('Ctrl Pts',(-68.13481609201,26.9842010174819,12.));
#148797=CARTESIAN_POINT('Ctrl Pts',(-68.1536135103558,27.0024992251839,
12.));
#148798=CARTESIAN_POINT('Ctrl Pts',(-68.1724208272967,27.0208411717477,
12.));
#148799=CARTESIAN_POINT('Ctrl Pts',(-68.1912379390787,27.0392268263804,
12.));
#148800=CARTESIAN_POINT('Ctrl Pts',(-68.2100647423345,27.0576561583179,
12.));
#148801=CARTESIAN_POINT('Ctrl Pts',(-68.2289011340624,27.076129136823,12.));
#148802=CARTESIAN_POINT('Ctrl Pts',(-68.2477470116014,27.0946457311813,
12.));
#148803=CARTESIAN_POINT('Ctrl Pts',(-68.2666022726094,27.1132059106939,
12.));
#148804=CARTESIAN_POINT('Ctrl Pts',(-68.285466815035,27.1318096446643,12.));
#148805=CARTESIAN_POINT('Ctrl Pts',(-68.3043405371589,27.150456902413,12.));
#148806=CARTESIAN_POINT('Ctrl Pts',(-68.3232233376415,27.1691476532917,
12.));
#148807=CARTESIAN_POINT('Ctrl Pts',(-68.3421151155708,27.1878818666925,
12.));
#148808=CARTESIAN_POINT('Ctrl Pts',(-68.3610157704999,27.2066595120544,
12.));
#148809=CARTESIAN_POINT('Ctrl Pts',(-68.379925202511,27.2254805588677,12.));
#148810=CARTESIAN_POINT('Ctrl Pts',(-68.398843312159,27.2443449766654,12.));
#148811=CARTESIAN_POINT('Ctrl Pts',(-68.4177700003471,27.2632527350062,
12.));
#148812=CARTESIAN_POINT('Ctrl Pts',(-68.4367051682166,27.2822038034539,
12.));
#148813=CARTESIAN_POINT('Ctrl Pts',(-68.455648717044,27.301198151557,12.));
#148814=CARTESIAN_POINT('Ctrl Pts',(-68.4746005480993,27.3202357488153,
12.));
#148815=CARTESIAN_POINT('Ctrl Pts',(-68.4935605626362,27.3393165646748,
12.));
#148816=CARTESIAN_POINT('Ctrl Pts',(-68.5125286621888,27.3584405685941,
12.));
#148817=CARTESIAN_POINT('Ctrl Pts',(-68.5315047488035,27.3776077300914,
12.));
#148818=CARTESIAN_POINT('Ctrl Pts',(-68.5504887252975,27.3968180187941,
12.));
#148819=CARTESIAN_POINT('Ctrl Pts',(-68.5694804955014,27.4160714044831,
12.));
#148820=CARTESIAN_POINT('Ctrl Pts',(-68.5884799645218,27.4353678571361,
12.));
#148821=CARTESIAN_POINT('Ctrl Pts',(-68.6074870381619,27.4547073468226,
12.));
#148822=CARTESIAN_POINT('Ctrl Pts',(-68.6265016223561,27.4740898435988,
12.));
#148823=CARTESIAN_POINT('Ctrl Pts',(-68.645523622548,27.4935153173868,12.));
#148824=CARTESIAN_POINT('Ctrl Pts',(-68.6645529432045,27.5129837378791,
12.));
#148825=CARTESIAN_POINT('Ctrl Pts',(-68.6835894869882,27.5324950743706,
12.));
#148826=CARTESIAN_POINT('Ctrl Pts',(-68.7026331554296,27.5520492958907,
12.));
#148827=CARTESIAN_POINT('Ctrl Pts',(-68.7216838504218,27.5716463715004,
12.));
#148828=CARTESIAN_POINT('Ctrl Pts',(-68.740741475526,27.5912862705468,12.));
#148829=CARTESIAN_POINT('Ctrl Pts',(-68.7598059372129,27.6109689629029,
12.));
#148830=CARTESIAN_POINT('Ctrl Pts',(-68.7788771464713,27.6306944192737,
12.));
#148831=CARTESIAN_POINT('Ctrl Pts',(-68.7979550191872,27.6504626112666,
12.));
#148832=CARTESIAN_POINT('Ctrl Pts',(-68.8143140938915,27.6674443909983,
12.));
#148833=CARTESIAN_POINT('Ctrl Pts',(-68.8268597852179,27.6804870323434,
12.));
#148834=CARTESIAN_POINT('Ctrl Pts',(-68.8355891982106,27.6895716271274,
12.));
#148835=CARTESIAN_POINT('Ctrl Pts',(-68.8405004466159,27.6946856803718,
12.));
#148836=CARTESIAN_POINT('Ctrl Pts',(-68.8415926175085,27.6958230985044,
12.));
#148837=CARTESIAN_POINT('',(-65.4815644032299,24.7419628022042,0.));
#148838=CARTESIAN_POINT('',(-65.4815644032299,24.7419628022042,0.));
#148839=CARTESIAN_POINT('Ctrl Pts',(-68.8415926175085,27.6958230985044,
0.));
#148840=CARTESIAN_POINT('Ctrl Pts',(-68.8405004466159,27.6946856803718,
0.));
#148841=CARTESIAN_POINT('Ctrl Pts',(-68.8355891982106,27.6895716271274,
0.));
#148842=CARTESIAN_POINT('Ctrl Pts',(-68.8268597852179,27.6804870323434,
0.));
#148843=CARTESIAN_POINT('Ctrl Pts',(-68.8143140938915,27.6674443909983,
0.));
#148844=CARTESIAN_POINT('Ctrl Pts',(-68.7979550191872,27.6504626112666,
0.));
#148845=CARTESIAN_POINT('Ctrl Pts',(-68.7788771464713,27.6306944192737,
0.));
#148846=CARTESIAN_POINT('Ctrl Pts',(-68.7598059372129,27.6109689629029,
0.));
#148847=CARTESIAN_POINT('Ctrl Pts',(-68.740741475526,27.5912862705468,0.));
#148848=CARTESIAN_POINT('Ctrl Pts',(-68.7216838504218,27.5716463715004,
0.));
#148849=CARTESIAN_POINT('Ctrl Pts',(-68.7026331554296,27.5520492958907,
0.));
#148850=CARTESIAN_POINT('Ctrl Pts',(-68.6835894869882,27.5324950743706,
0.));
#148851=CARTESIAN_POINT('Ctrl Pts',(-68.6645529432045,27.5129837378791,
0.));
#148852=CARTESIAN_POINT('Ctrl Pts',(-68.645523622548,27.4935153173868,0.));
#148853=CARTESIAN_POINT('Ctrl Pts',(-68.6265016223561,27.4740898435988,
0.));
#148854=CARTESIAN_POINT('Ctrl Pts',(-68.6074870381619,27.4547073468226,
0.));
#148855=CARTESIAN_POINT('Ctrl Pts',(-68.5884799645218,27.4353678571361,
0.));
#148856=CARTESIAN_POINT('Ctrl Pts',(-68.5694804955014,27.4160714044831,
0.));
#148857=CARTESIAN_POINT('Ctrl Pts',(-68.5504887252975,27.3968180187941,
0.));
#148858=CARTESIAN_POINT('Ctrl Pts',(-68.5315047488035,27.3776077300914,
0.));
#148859=CARTESIAN_POINT('Ctrl Pts',(-68.5125286621888,27.3584405685941,
0.));
#148860=CARTESIAN_POINT('Ctrl Pts',(-68.4935605626362,27.3393165646748,
0.));
#148861=CARTESIAN_POINT('Ctrl Pts',(-68.4746005480993,27.3202357488153,
0.));
#148862=CARTESIAN_POINT('Ctrl Pts',(-68.455648717044,27.301198151557,0.));
#148863=CARTESIAN_POINT('Ctrl Pts',(-68.4367051682166,27.2822038034539,
0.));
#148864=CARTESIAN_POINT('Ctrl Pts',(-68.4177700003471,27.2632527350062,
0.));
#148865=CARTESIAN_POINT('Ctrl Pts',(-68.398843312159,27.2443449766654,0.));
#148866=CARTESIAN_POINT('Ctrl Pts',(-68.379925202511,27.2254805588677,0.));
#148867=CARTESIAN_POINT('Ctrl Pts',(-68.3610157704999,27.2066595120544,
0.));
#148868=CARTESIAN_POINT('Ctrl Pts',(-68.3421151155708,27.1878818666925,
0.));
#148869=CARTESIAN_POINT('Ctrl Pts',(-68.3232233376415,27.1691476532917,
0.));
#148870=CARTESIAN_POINT('Ctrl Pts',(-68.3043405371589,27.150456902413,0.));
#148871=CARTESIAN_POINT('Ctrl Pts',(-68.285466815035,27.1318096446643,0.));
#148872=CARTESIAN_POINT('Ctrl Pts',(-68.2666022726094,27.1132059106939,
0.));
#148873=CARTESIAN_POINT('Ctrl Pts',(-68.2477470116014,27.0946457311813,
0.));
#148874=CARTESIAN_POINT('Ctrl Pts',(-68.2289011340624,27.076129136823,0.));
#148875=CARTESIAN_POINT('Ctrl Pts',(-68.2100647423345,27.0576561583179,
0.));
#148876=CARTESIAN_POINT('Ctrl Pts',(-68.1912379390787,27.0392268263804,
0.));
#148877=CARTESIAN_POINT('Ctrl Pts',(-68.1724208272967,27.0208411717477,
0.));
#148878=CARTESIAN_POINT('Ctrl Pts',(-68.1536135103558,27.0024992251839,
0.));
#148879=CARTESIAN_POINT('Ctrl Pts',(-68.13481609201,26.9842010174819,0.));
#148880=CARTESIAN_POINT('Ctrl Pts',(-68.1160286764244,26.9659465794596,
0.));
#148881=CARTESIAN_POINT('Ctrl Pts',(-68.0972513681739,26.9477359419646,
0.));
#148882=CARTESIAN_POINT('Ctrl Pts',(-68.0784842722362,26.9295691358775,
0.));
#148883=CARTESIAN_POINT('Ctrl Pts',(-68.0597274939857,26.9114461921109,
0.));
#148884=CARTESIAN_POINT('Ctrl Pts',(-68.0409811391872,26.8933671416064,
0.));
#148885=CARTESIAN_POINT('Ctrl Pts',(-68.0222453139862,26.8753320153255,
0.));
#148886=CARTESIAN_POINT('Ctrl Pts',(-68.0035201249108,26.85734084425,0.));
#148887=CARTESIAN_POINT('Ctrl Pts',(-67.9848056788814,26.8393936593914,
0.));
#148888=CARTESIAN_POINT('Ctrl Pts',(-67.9661020832165,26.8214904917922,
0.));
#148889=CARTESIAN_POINT('Ctrl Pts',(-67.9474094456395,26.8036313725262,
0.));
#148890=CARTESIAN_POINT('Ctrl Pts',(-67.9287278742839,26.7858163326932,
0.));
#148891=CARTESIAN_POINT('Ctrl Pts',(-67.9100574776974,26.7680454034168,
0.));
#148892=CARTESIAN_POINT('Ctrl Pts',(-67.8913983648441,26.7503186158523,
0.));
#148893=CARTESIAN_POINT('Ctrl Pts',(-67.8727506451068,26.7326360011886,
0.));
#148894=CARTESIAN_POINT('Ctrl Pts',(-67.8541144282875,26.7149975906478,
0.));
#148895=CARTESIAN_POINT('Ctrl Pts',(-67.8354898246079,26.6974034154803,
0.));
#148896=CARTESIAN_POINT('Ctrl Pts',(-67.8168769447086,26.6798535069586,
0.));
#148897=CARTESIAN_POINT('Ctrl Pts',(-67.7982758996557,26.6623478963867,
0.));
#148898=CARTESIAN_POINT('Ctrl Pts',(-67.7796868009447,26.6448866151027,
0.));
#148899=CARTESIAN_POINT('Ctrl Pts',(-67.7611097605042,26.6274696944793,
0.));
#148900=CARTESIAN_POINT('Ctrl Pts',(-67.7425448906983,26.6100971659204,
0.));
#148901=CARTESIAN_POINT('Ctrl Pts',(-67.7239923043295,26.5927690608546,
0.));
#148902=CARTESIAN_POINT('Ctrl Pts',(-67.7054521146427,26.5754854107422,
0.));
#148903=CARTESIAN_POINT('Ctrl Pts',(-67.6869244353292,26.5582462470794,
0.));
#148904=CARTESIAN_POINT('Ctrl Pts',(-67.6684093805288,26.5410516013984,
0.));
#148905=CARTESIAN_POINT('Ctrl Pts',(-67.6499070648323,26.5239015052655,
0.));
#148906=CARTESIAN_POINT('Ctrl Pts',(-67.6314176032823,26.506795990273,0.));
#148907=CARTESIAN_POINT('Ctrl Pts',(-67.6129411113774,26.4897350880446,
0.));
#148908=CARTESIAN_POINT('Ctrl Pts',(-67.5944777050782,26.4727188302415,
0.));
#148909=CARTESIAN_POINT('Ctrl Pts',(-67.5760275008096,26.4557472485622,
0.));
#148910=CARTESIAN_POINT('Ctrl Pts',(-67.5575906154648,26.4388203747422,
0.));
#148911=CARTESIAN_POINT('Ctrl Pts',(-67.5391671664055,26.4219382405452,
0.));
#148912=CARTESIAN_POINT('Ctrl Pts',(-67.5207572714666,26.4051008777669,
0.));
#148913=CARTESIAN_POINT('Ctrl Pts',(-67.5023610489611,26.3883083182417,
0.));
#148914=CARTESIAN_POINT('Ctrl Pts',(-67.4839786176833,26.3715605938432,
0.));
#148915=CARTESIAN_POINT('Ctrl Pts',(-67.4656100969121,26.3548577364835,
0.));
#148916=CARTESIAN_POINT('Ctrl Pts',(-67.4472556064127,26.3381997781059,
0.));
#148917=CARTESIAN_POINT('Ctrl Pts',(-67.4289152664406,26.3215867506864,
0.));
#148918=CARTESIAN_POINT('Ctrl Pts',(-67.4105891977465,26.305018686241,0.));
#148919=CARTESIAN_POINT('Ctrl Pts',(-67.392277521581,26.288495616827,0.));
#148920=CARTESIAN_POINT('Ctrl Pts',(-67.3739803596967,26.2720175745422,
0.));
#148921=CARTESIAN_POINT('Ctrl Pts',(-67.3556978343506,26.255584591518,0.));
#148922=CARTESIAN_POINT('Ctrl Pts',(-67.3374300683076,26.2391966999192,
0.));
#148923=CARTESIAN_POINT('Ctrl Pts',(-67.3191771848468,26.2228539319527,
0.));
#148924=CARTESIAN_POINT('Ctrl Pts',(-67.3009393077654,26.2065563198684,
0.));
#148925=CARTESIAN_POINT('Ctrl Pts',(-67.2827165613828,26.1903038959589,
0.));
#148926=CARTESIAN_POINT('Ctrl Pts',(-67.2645090705414,26.1740966925527,
0.));
#148927=CARTESIAN_POINT('Ctrl Pts',(-67.2463169606105,26.1579347420135,
0.));
#148928=CARTESIAN_POINT('Ctrl Pts',(-67.228140357493,26.1418180767487,0.));
#148929=CARTESIAN_POINT('Ctrl Pts',(-67.2099793876295,26.1257467292102,
0.));
#148930=CARTESIAN_POINT('Ctrl Pts',(-67.191834178002,26.109720731895,0.));
#148931=CARTESIAN_POINT('Ctrl Pts',(-67.1737048561364,26.0937401173385,
0.));
#148932=CARTESIAN_POINT('Ctrl Pts',(-67.1555915501052,26.0778049181129,
0.));
#148933=CARTESIAN_POINT('Ctrl Pts',(-67.1374943885353,26.061915166836,0.));
#148934=CARTESIAN_POINT('Ctrl Pts',(-67.1194135006122,26.0460708961725,
0.));
#148935=CARTESIAN_POINT('Ctrl Pts',(-67.101349016084,26.030272138834,0.));
#148936=CARTESIAN_POINT('Ctrl Pts',(-67.083301065264,26.0145189275733,0.));
#148937=CARTESIAN_POINT('Ctrl Pts',(-67.0652697790335,25.9988112951818,
0.));
#148938=CARTESIAN_POINT('Ctrl Pts',(-67.0472552888495,25.9831492744988,
0.));
#148939=CARTESIAN_POINT('Ctrl Pts',(-67.0292577267495,25.9675328984123,
0.));
#148940=CARTESIAN_POINT('Ctrl Pts',(-67.0112772253553,25.9519621998598,
0.));
#148941=CARTESIAN_POINT('Ctrl Pts',(-66.993313917876,25.9364372118216,0.));
#148942=CARTESIAN_POINT('Ctrl Pts',(-66.9753679381122,25.9209579673198,
0.));
#148943=CARTESIAN_POINT('Ctrl Pts',(-66.9574394204635,25.9055244994266,
0.));
#148944=CARTESIAN_POINT('Ctrl Pts',(-66.9395284999327,25.8901368412655,
0.));
#148945=CARTESIAN_POINT('Ctrl Pts',(-66.9216353121308,25.8747950260114,
0.));
#148946=CARTESIAN_POINT('Ctrl Pts',(-66.9037599932787,25.8594990868845,
0.));
#148947=CARTESIAN_POINT('Ctrl Pts',(-66.8859026802123,25.8442490571486,
0.));
#148948=CARTESIAN_POINT('Ctrl Pts',(-66.8680635103907,25.8290449701206,
0.));
#148949=CARTESIAN_POINT('Ctrl Pts',(-66.8502426219015,25.8138868591715,
0.));
#148950=CARTESIAN_POINT('Ctrl Pts',(-66.8324401534658,25.7987747577264,
0.));
#148951=CARTESIAN_POINT('Ctrl Pts',(-66.8146562444397,25.783708699258,0.));
#148952=CARTESIAN_POINT('Ctrl Pts',(-66.7968910348199,25.7686887172859,
0.));
#148953=CARTESIAN_POINT('Ctrl Pts',(-66.7791446652505,25.7537148453848,
0.));
#148954=CARTESIAN_POINT('Ctrl Pts',(-66.7614172770302,25.7387871171861,
0.));
#148955=CARTESIAN_POINT('Ctrl Pts',(-66.7437090121168,25.7239055663778,
0.));
#148956=CARTESIAN_POINT('Ctrl Pts',(-66.72602001313,25.7090702266976,0.));
#148957=CARTESIAN_POINT('Ctrl Pts',(-66.7083504233566,25.6942811319337,
0.));
#148958=CARTESIAN_POINT('Ctrl Pts',(-66.6907003867599,25.6795383159329,
0.));
#148959=CARTESIAN_POINT('Ctrl Pts',(-66.6730700479844,25.6648418126016,
0.));
#148960=CARTESIAN_POINT('Ctrl Pts',(-66.6554595523611,25.650191655905,0.));
#148961=CARTESIAN_POINT('Ctrl Pts',(-66.6378690459105,25.6355878798605,
0.));
#148962=CARTESIAN_POINT('Ctrl Pts',(-66.6202986753482,25.6210305185394,
0.));
#148963=CARTESIAN_POINT('Ctrl Pts',(-66.6027485880947,25.606519606075,0.));
#148964=CARTESIAN_POINT('Ctrl Pts',(-66.5852189322811,25.5920551766629,
0.));
#148965=CARTESIAN_POINT('Ctrl Pts',(-66.5677098567551,25.5776372645605,
0.));
#148966=CARTESIAN_POINT('Ctrl Pts',(-66.5502215110843,25.5632659040797,
0.));
#148967=CARTESIAN_POINT('Ctrl Pts',(-66.5327540455639,25.5489411295916,
0.));
#148968=CARTESIAN_POINT('Ctrl Pts',(-66.5153076112237,25.5346629755322,
0.));
#148969=CARTESIAN_POINT('Ctrl Pts',(-66.4978823598352,25.5204314764033,
0.));
#148970=CARTESIAN_POINT('Ctrl Pts',(-66.4804784439146,25.5062466667703,
0.));
#148971=CARTESIAN_POINT('Ctrl Pts',(-66.463096016725,25.4921085812548,0.));
#148972=CARTESIAN_POINT('Ctrl Pts',(-66.445735232287,25.4780172545418,0.));
#148973=CARTESIAN_POINT('Ctrl Pts',(-66.4283962453899,25.463972721385,0.));
#148974=CARTESIAN_POINT('Ctrl Pts',(-66.4110792116,25.4499750166079,0.));
#148975=CARTESIAN_POINT('Ctrl Pts',(-66.3937842872684,25.4360241751017,
0.));
#148976=CARTESIAN_POINT('Ctrl Pts',(-66.3765116295364,25.4221202318198,
0.));
#148977=CARTESIAN_POINT('Ctrl Pts',(-66.3592613963407,25.4082632217846,
0.));
#148978=CARTESIAN_POINT('Ctrl Pts',(-66.3420337464176,25.39445318009,0.));
#148979=CARTESIAN_POINT('Ctrl Pts',(-66.3248288393046,25.3806901419012,
0.));
#148980=CARTESIAN_POINT('Ctrl Pts',(-66.3076468353417,25.366974142449,0.));
#148981=CARTESIAN_POINT('Ctrl Pts',(-66.2904878956721,25.3533052170253,
0.));
#148982=CARTESIAN_POINT('Ctrl Pts',(-66.2733521822675,25.3396834009954,
0.));
#148983=CARTESIAN_POINT('Ctrl Pts',(-66.2562398579479,25.3261087298029,
0.));
#148984=CARTESIAN_POINT('Ctrl Pts',(-66.2391510863992,25.3125812389727,
0.));
#148985=CARTESIAN_POINT('Ctrl Pts',(-66.2220860321931,25.2991009641086,
0.));
#148986=CARTESIAN_POINT('Ctrl Pts',(-66.2050448607883,25.285667940892,0.));
#148987=CARTESIAN_POINT('Ctrl Pts',(-66.1880277385114,25.2722822050828,
0.));
#148988=CARTESIAN_POINT('Ctrl Pts',(-66.1710348325378,25.2589437925145,
0.));
#148989=CARTESIAN_POINT('Ctrl Pts',(-66.1540663108767,25.245652739088,0.));
#148990=CARTESIAN_POINT('Ctrl Pts',(-66.1371223423372,25.232409080756,0.));
#148991=CARTESIAN_POINT('Ctrl Pts',(-66.1202030965785,25.2192128535367,
0.));
#148992=CARTESIAN_POINT('Ctrl Pts',(-66.1033087441916,25.2060640935371,
0.));
#148993=CARTESIAN_POINT('Ctrl Pts',(-66.086439456768,25.1929628369685,0.));
#148994=CARTESIAN_POINT('Ctrl Pts',(-66.0695954069699,25.1799091201594,
0.));
#148995=CARTESIAN_POINT('Ctrl Pts',(-66.0527767686,25.1669029795651,0.));
#148996=CARTESIAN_POINT('Ctrl Pts',(-66.0359837164709,25.1539444517409,
0.));
#148997=CARTESIAN_POINT('Ctrl Pts',(-66.0192164262607,25.1410335733094,
0.));
#148998=CARTESIAN_POINT('Ctrl Pts',(-66.0024750743902,25.1281703809299,
0.));
#148999=CARTESIAN_POINT('Ctrl Pts',(-65.9857598378455,25.1153549112511,
0.));
#149000=CARTESIAN_POINT('Ctrl Pts',(-65.9690708941591,25.1025872009016,
0.));
#149001=CARTESIAN_POINT('Ctrl Pts',(-65.9524084218167,25.0898672865926,
0.));
#149002=CARTESIAN_POINT('Ctrl Pts',(-65.9357726006174,25.0771952052032,
0.));
#149003=CARTESIAN_POINT('Ctrl Pts',(-65.9191636119796,25.0645709938519,
0.));
#149004=CARTESIAN_POINT('Ctrl Pts',(-65.9025816394391,25.0519946900066,
0.));
#149005=CARTESIAN_POINT('Ctrl Pts',(-65.8860268683088,25.039466331404,0.));
#149006=CARTESIAN_POINT('Ctrl Pts',(-65.8694994847587,25.0269859558351,
0.));
#149007=CARTESIAN_POINT('Ctrl Pts',(-65.8529996750441,25.0145536009603,
0.));
#149008=CARTESIAN_POINT('Ctrl Pts',(-65.8365276247157,25.0021693041181,
0.));
#149009=CARTESIAN_POINT('Ctrl Pts',(-65.8200835177071,24.9898331021002,
0.));
#149010=CARTESIAN_POINT('Ctrl Pts',(-65.8036675380761,24.97754503157,0.));
#149011=CARTESIAN_POINT('Ctrl Pts',(-65.7872798720847,24.965305129559,0.));
#149012=CARTESIAN_POINT('Ctrl Pts',(-65.7709207098949,24.9531134338693,
0.));
#149013=CARTESIAN_POINT('Ctrl Pts',(-65.7545902480286,24.9409699836523,
0.));
#149014=CARTESIAN_POINT('Ctrl Pts',(-65.7382886895839,24.9288748194562,
0.));
#149015=CARTESIAN_POINT('Ctrl Pts',(-65.7220162391016,24.9168279820093,
0.));
#149016=CARTESIAN_POINT('Ctrl Pts',(-65.7057730980471,24.9048295111444,
0.));
#149017=CARTESIAN_POINT('Ctrl Pts',(-65.6895594608798,24.8928794448615,
0.));
#149018=CARTESIAN_POINT('Ctrl Pts',(-65.6733755087724,24.8809778178248,
0.));
#149019=CARTESIAN_POINT('Ctrl Pts',(-65.6572214156761,24.869124662808,0.));
#149020=CARTESIAN_POINT('Ctrl Pts',(-65.6410973603713,24.8573200135683,
0.));
#149021=CARTESIAN_POINT('Ctrl Pts',(-65.6250035361612,24.8455639071517,
0.));
#149022=CARTESIAN_POINT('Ctrl Pts',(-65.6089401625552,24.8338563866739,
0.));
#149023=CARTESIAN_POINT('Ctrl Pts',(-65.5929074932487,24.8221975032059,
0.));
#149024=CARTESIAN_POINT('Ctrl Pts',(-65.5769057914184,24.8105873098578,
0.));
#149025=CARTESIAN_POINT('Ctrl Pts',(-65.560935306275,24.7990258561234,0.));
#149026=CARTESIAN_POINT('Ctrl Pts',(-65.5449962514735,24.7875131827515,
0.));
#149027=CARTESIAN_POINT('Ctrl Pts',(-65.5290887770494,24.776049314855,0.));
#149028=CARTESIAN_POINT('Ctrl Pts',(-65.5132129675727,24.7646342620969,
0.));
#149029=CARTESIAN_POINT('Ctrl Pts',(-65.5005376841469,24.755541272477,0.));
#149030=CARTESIAN_POINT('Ctrl Pts',(-65.4910454936487,24.7487434956058,
0.));
#149031=CARTESIAN_POINT('Ctrl Pts',(-65.484723709553,24.7442214063411,0.));
#149032=CARTESIAN_POINT('Ctrl Pts',(-65.4815644032299,24.7419628022042,
0.));
#149033=CARTESIAN_POINT('Ctrl Pts',(-66.3684712863594,33.8448817269567,
0.));
#149034=CARTESIAN_POINT('Ctrl Pts',(-66.3684712863594,33.8448817269567,
12.));
#149035=CARTESIAN_POINT('Ctrl Pts',(-66.3650082659713,33.8404862618869,
0.));
#149036=CARTESIAN_POINT('Ctrl Pts',(-66.3650082659713,33.8404862618869,
12.));
#149037=CARTESIAN_POINT('Ctrl Pts',(-66.3580824155893,33.8316996011932,
0.));
#149038=CARTESIAN_POINT('Ctrl Pts',(-66.3580824155893,33.8316996011932,
12.));
#149039=CARTESIAN_POINT('Ctrl Pts',(-66.3476942112,33.8185324184903,0.));
#149040=CARTESIAN_POINT('Ctrl Pts',(-66.3476942112,33.8185324184903,12.));
#149041=CARTESIAN_POINT('Ctrl Pts',(-66.3338444144211,33.8010017926027,
0.));
#149042=CARTESIAN_POINT('Ctrl Pts',(-66.3338444144211,33.8010017926027,
12.));
#149043=CARTESIAN_POINT('Ctrl Pts',(-66.3165340771611,33.7791312145108,
0.));
#149044=CARTESIAN_POINT('Ctrl Pts',(-66.3165340771611,33.7791312145108,
12.));
#149045=CARTESIAN_POINT('Ctrl Pts',(-66.2992256621336,33.7573033544559,
0.));
#149046=CARTESIAN_POINT('Ctrl Pts',(-66.2992256621336,33.7573033544559,
12.));
#149047=CARTESIAN_POINT('Ctrl Pts',(-66.2819191962353,33.7355182321907,
0.));
#149048=CARTESIAN_POINT('Ctrl Pts',(-66.2819191962353,33.7355182321907,
12.));
#149049=CARTESIAN_POINT('Ctrl Pts',(-66.2646147235322,33.7137758735902,
0.));
#149050=CARTESIAN_POINT('Ctrl Pts',(-66.2646147235322,33.7137758735902,
12.));
#149051=CARTESIAN_POINT('Ctrl Pts',(-66.2473123109395,33.6920763111448,
0.));
#149052=CARTESIAN_POINT('Ctrl Pts',(-66.2473123109395,33.6920763111448,
12.));
#149053=CARTESIAN_POINT('Ctrl Pts',(-66.2300120464082,33.6704195830392,
0.));
#149054=CARTESIAN_POINT('Ctrl Pts',(-66.2300120464082,33.6704195830392,
12.));
#149055=CARTESIAN_POINT('Ctrl Pts',(-66.2127140313598,33.6488057311532,
0.));
#149056=CARTESIAN_POINT('Ctrl Pts',(-66.2127140313598,33.6488057311532,
12.));
#149057=CARTESIAN_POINT('Ctrl Pts',(-66.1954183747089,33.6272347993476,
0.));
#149058=CARTESIAN_POINT('Ctrl Pts',(-66.1954183747089,33.6272347993476,
12.));
#149059=CARTESIAN_POINT('Ctrl Pts',(-66.1781251864017,33.6057068316769,
0.));
#149060=CARTESIAN_POINT('Ctrl Pts',(-66.1781251864017,33.6057068316769,
12.));
#149061=CARTESIAN_POINT('Ctrl Pts',(-66.1608345707637,33.584221870515,0.));
#149062=CARTESIAN_POINT('Ctrl Pts',(-66.1608345707637,33.584221870515,12.));
#149063=CARTESIAN_POINT('Ctrl Pts',(-66.1435466211076,33.5627799550483,
0.));
#149064=CARTESIAN_POINT('Ctrl Pts',(-66.1435466211076,33.5627799550483,
12.));
#149065=CARTESIAN_POINT('Ctrl Pts',(-66.1262614234675,33.541381122345,0.));
#149066=CARTESIAN_POINT('Ctrl Pts',(-66.1262614234675,33.541381122345,12.));
#149067=CARTESIAN_POINT('Ctrl Pts',(-66.1089790592729,33.5200254081243,
0.));
#149068=CARTESIAN_POINT('Ctrl Pts',(-66.1089790592729,33.5200254081243,
12.));
#149069=CARTESIAN_POINT('Ctrl Pts',(-66.0916996085245,33.4987128476622,
0.));
#149070=CARTESIAN_POINT('Ctrl Pts',(-66.0916996085245,33.4987128476622,
12.));
#149071=CARTESIAN_POINT('Ctrl Pts',(-66.0744231525415,33.4774434765745,
0.));
#149072=CARTESIAN_POINT('Ctrl Pts',(-66.0744231525415,33.4774434765745,
12.));
#149073=CARTESIAN_POINT('Ctrl Pts',(-66.0571497774434,33.4562173318025,
0.));
#149074=CARTESIAN_POINT('Ctrl Pts',(-66.0571497774434,33.4562173318025,
12.));
#149075=CARTESIAN_POINT('Ctrl Pts',(-66.0398795737777,33.43503445151,0.));
#149076=CARTESIAN_POINT('Ctrl Pts',(-66.0398795737777,33.43503445151,12.));
#149077=CARTESIAN_POINT('Ctrl Pts',(-66.0226126349446,33.4138948746388,
0.));
#149078=CARTESIAN_POINT('Ctrl Pts',(-66.0226126349446,33.4138948746388,
12.));
#149079=CARTESIAN_POINT('Ctrl Pts',(-66.0053490559812,33.3927986405605,
0.));
#149080=CARTESIAN_POINT('Ctrl Pts',(-66.0053490559812,33.3927986405605,
12.));
#149081=CARTESIAN_POINT('Ctrl Pts',(-65.9880889322831,33.37174578871,0.));
#149082=CARTESIAN_POINT('Ctrl Pts',(-65.9880889322831,33.37174578871,12.));
#149083=CARTESIAN_POINT('Ctrl Pts',(-65.970832358141,33.3507363581592,0.));
#149084=CARTESIAN_POINT('Ctrl Pts',(-65.970832358141,33.3507363581592,12.));
#149085=CARTESIAN_POINT('Ctrl Pts',(-65.9535794260831,33.3297703874265,
0.));
#149086=CARTESIAN_POINT('Ctrl Pts',(-65.9535794260831,33.3297703874265,
12.));
#149087=CARTESIAN_POINT('Ctrl Pts',(-65.9363302276846,33.3088479147164,
0.));
#149088=CARTESIAN_POINT('Ctrl Pts',(-65.9363302276846,33.3088479147164,
12.));
#149089=CARTESIAN_POINT('Ctrl Pts',(-65.9190848540433,33.2879689780572,
0.));
#149090=CARTESIAN_POINT('Ctrl Pts',(-65.9190848540433,33.2879689780572,
12.));
#149091=CARTESIAN_POINT('Ctrl Pts',(-65.9018433963889,33.2671336154753,
0.));
#149092=CARTESIAN_POINT('Ctrl Pts',(-65.9018433963889,33.2671336154753,
12.));
#149093=CARTESIAN_POINT('Ctrl Pts',(-65.8846059466372,33.2463418651492,
0.));
#149094=CARTESIAN_POINT('Ctrl Pts',(-65.8846059466372,33.2463418651492,
12.));
#149095=CARTESIAN_POINT('Ctrl Pts',(-65.8673725979578,33.2255937655649,
0.));
#149096=CARTESIAN_POINT('Ctrl Pts',(-65.8673725979578,33.2255937655649,
12.));
#149097=CARTESIAN_POINT('Ctrl Pts',(-65.8501434445164,33.2048893554491,
0.));
#149098=CARTESIAN_POINT('Ctrl Pts',(-65.8501434445164,33.2048893554491,
12.));
#149099=CARTESIAN_POINT('Ctrl Pts',(-65.8329185812375,33.1842286737051,
0.));
#149100=CARTESIAN_POINT('Ctrl Pts',(-65.8329185812375,33.1842286737051,
12.));
#149101=CARTESIAN_POINT('Ctrl Pts',(-65.8156981035503,33.16361175934,0.));
#149102=CARTESIAN_POINT('Ctrl Pts',(-65.8156981035503,33.16361175934,12.));
#149103=CARTESIAN_POINT('Ctrl Pts',(-65.7984821071623,33.1430386513976,
0.));
#149104=CARTESIAN_POINT('Ctrl Pts',(-65.7984821071623,33.1430386513976,
12.));
#149105=CARTESIAN_POINT('Ctrl Pts',(-65.7812706877697,33.1225093888671,
0.));
#149106=CARTESIAN_POINT('Ctrl Pts',(-65.7812706877697,33.1225093888671,
12.));
#149107=CARTESIAN_POINT('Ctrl Pts',(-65.7640639410661,33.1020240106884,
0.));
#149108=CARTESIAN_POINT('Ctrl Pts',(-65.7640639410661,33.1020240106884,
12.));
#149109=CARTESIAN_POINT('Ctrl Pts',(-65.7468619628816,33.081582555798,0.));
#149110=CARTESIAN_POINT('Ctrl Pts',(-65.7468619628816,33.081582555798,12.));
#149111=CARTESIAN_POINT('Ctrl Pts',(-65.7296648492825,33.0611850631582,
0.));
#149112=CARTESIAN_POINT('Ctrl Pts',(-65.7296648492825,33.0611850631582,
12.));
#149113=CARTESIAN_POINT('Ctrl Pts',(-65.7124726966802,33.0408315717873,
0.));
#149114=CARTESIAN_POINT('Ctrl Pts',(-65.7124726966802,33.0408315717873,
12.));
#149115=CARTESIAN_POINT('Ctrl Pts',(-65.6952856019533,33.0205221207872,
0.));
#149116=CARTESIAN_POINT('Ctrl Pts',(-65.6952856019533,33.0205221207872,
12.));
#149117=CARTESIAN_POINT('Ctrl Pts',(-65.6781036625027,33.0002567493573,
0.));
#149118=CARTESIAN_POINT('Ctrl Pts',(-65.6781036625027,33.0002567493573,
12.));
#149119=CARTESIAN_POINT('Ctrl Pts',(-65.6609269761889,32.9800354967839,
0.));
#149120=CARTESIAN_POINT('Ctrl Pts',(-65.6609269761889,32.9800354967839,
12.));
#149121=CARTESIAN_POINT('Ctrl Pts',(-65.6437556412947,32.9598584024312,
0.));
#149122=CARTESIAN_POINT('Ctrl Pts',(-65.6437556412947,32.9598584024312,
12.));
#149123=CARTESIAN_POINT('Ctrl Pts',(-65.6265897564783,32.9397255057274,
0.));
#149124=CARTESIAN_POINT('Ctrl Pts',(-65.6265897564783,32.9397255057274,
12.));
#149125=CARTESIAN_POINT('Ctrl Pts',(-65.6094294207276,32.9196368461463,
0.));
#149126=CARTESIAN_POINT('Ctrl Pts',(-65.6094294207276,32.9196368461463,
12.));
#149127=CARTESIAN_POINT('Ctrl Pts',(-65.5922747333194,32.8995924631898,
0.));
#149128=CARTESIAN_POINT('Ctrl Pts',(-65.5922747333194,32.8995924631898,
12.));
#149129=CARTESIAN_POINT('Ctrl Pts',(-65.5751257938473,32.879592396403,0.));
#149130=CARTESIAN_POINT('Ctrl Pts',(-65.5751257938473,32.879592396403,12.));
#149131=CARTESIAN_POINT('Ctrl Pts',(-65.5579827022421,32.8596366853832,
0.));
#149132=CARTESIAN_POINT('Ctrl Pts',(-65.5579827022421,32.8596366853832,
12.));
#149133=CARTESIAN_POINT('Ctrl Pts',(-65.5408455587965,32.8397253697865,
0.));
#149134=CARTESIAN_POINT('Ctrl Pts',(-65.5408455587965,32.8397253697865,
12.));
#149135=CARTESIAN_POINT('Ctrl Pts',(-65.5237144641858,32.8198584893315,
0.));
#149136=CARTESIAN_POINT('Ctrl Pts',(-65.5237144641858,32.8198584893315,
12.));
#149137=CARTESIAN_POINT('Ctrl Pts',(-65.5065895194929,32.8000360837974,
0.));
#149138=CARTESIAN_POINT('Ctrl Pts',(-65.5065895194929,32.8000360837974,
12.));
#149139=CARTESIAN_POINT('Ctrl Pts',(-65.4894708262061,32.7802581930287,
0.));
#149140=CARTESIAN_POINT('Ctrl Pts',(-65.4894708262061,32.7802581930287,
12.));
#149141=CARTESIAN_POINT('Ctrl Pts',(-65.4723584862122,32.7605248569378,
0.));
#149142=CARTESIAN_POINT('Ctrl Pts',(-65.4723584862122,32.7605248569378,
12.));
#149143=CARTESIAN_POINT('Ctrl Pts',(-65.4552526017905,32.7408361155037,
0.));
#149144=CARTESIAN_POINT('Ctrl Pts',(-65.4552526017905,32.7408361155037,
12.));
#149145=CARTESIAN_POINT('Ctrl Pts',(-65.4381532756065,32.7211920087683,
0.));
#149146=CARTESIAN_POINT('Ctrl Pts',(-65.4381532756065,32.7211920087683,
12.));
#149147=CARTESIAN_POINT('Ctrl Pts',(-65.4210606107035,32.7015925768265,
0.));
#149148=CARTESIAN_POINT('Ctrl Pts',(-65.4210606107035,32.7015925768265,
12.));
#149149=CARTESIAN_POINT('Ctrl Pts',(-65.4039747105039,32.6820378598267,
0.));
#149150=CARTESIAN_POINT('Ctrl Pts',(-65.4039747105039,32.6820378598267,
12.));
#149151=CARTESIAN_POINT('Ctrl Pts',(-65.3868956788182,32.662527897981,0.));
#149152=CARTESIAN_POINT('Ctrl Pts',(-65.3868956788182,32.662527897981,12.));
#149153=CARTESIAN_POINT('Ctrl Pts',(-65.3698236198513,32.6430627315674,
0.));
#149154=CARTESIAN_POINT('Ctrl Pts',(-65.3698236198513,32.6430627315674,
12.));
#149155=CARTESIAN_POINT('Ctrl Pts',(-65.3527586382081,32.6236424009301,
0.));
#149156=CARTESIAN_POINT('Ctrl Pts',(-65.3527586382081,32.6236424009301,
12.));
#149157=CARTESIAN_POINT('Ctrl Pts',(-65.3357008389004,32.604266946475,0.));
#149158=CARTESIAN_POINT('Ctrl Pts',(-65.3357008389004,32.604266946475,12.));
#149159=CARTESIAN_POINT('Ctrl Pts',(-65.31865032735,32.5849364086678,0.));
#149160=CARTESIAN_POINT('Ctrl Pts',(-65.31865032735,32.5849364086678,12.));
#149161=CARTESIAN_POINT('Ctrl Pts',(-65.3016072093912,32.5656508280421,
0.));
#149162=CARTESIAN_POINT('Ctrl Pts',(-65.3016072093912,32.5656508280421,
12.));
#149163=CARTESIAN_POINT('Ctrl Pts',(-65.2845715912721,32.5464102452014,
0.));
#149164=CARTESIAN_POINT('Ctrl Pts',(-65.2845715912721,32.5464102452014,
12.));
#149165=CARTESIAN_POINT('Ctrl Pts',(-65.2675435796558,32.5272147008191,
0.));
#149166=CARTESIAN_POINT('Ctrl Pts',(-65.2675435796558,32.5272147008191,
12.));
#149167=CARTESIAN_POINT('Ctrl Pts',(-65.2505232816209,32.5080642356328,
0.));
#149168=CARTESIAN_POINT('Ctrl Pts',(-65.2505232816209,32.5080642356328,
12.));
#149169=CARTESIAN_POINT('Ctrl Pts',(-65.2335108046614,32.4889588904392,
0.));
#149170=CARTESIAN_POINT('Ctrl Pts',(-65.2335108046614,32.4889588904392,
12.));
#149171=CARTESIAN_POINT('Ctrl Pts',(-65.2165062566924,32.4698987061032,
0.));
#149172=CARTESIAN_POINT('Ctrl Pts',(-65.2165062566924,32.4698987061032,
12.));
#149173=CARTESIAN_POINT('Ctrl Pts',(-65.1995097460538,32.450883723561,0.));
#149174=CARTESIAN_POINT('Ctrl Pts',(-65.1995097460538,32.450883723561,12.));
#149175=CARTESIAN_POINT('Ctrl Pts',(-65.182521381514,32.4319139838212,0.));
#149176=CARTESIAN_POINT('Ctrl Pts',(-65.182521381514,32.4319139838212,12.));
#149177=CARTESIAN_POINT('Ctrl Pts',(-65.1655412722726,32.4129895279615,
0.));
#149178=CARTESIAN_POINT('Ctrl Pts',(-65.1655412722726,32.4129895279615,
12.));
#149179=CARTESIAN_POINT('Ctrl Pts',(-65.1485695279635,32.3941103971221,
0.));
#149180=CARTESIAN_POINT('Ctrl Pts',(-65.1485695279635,32.3941103971221,
12.));
#149181=CARTESIAN_POINT('Ctrl Pts',(-65.1316062586588,32.3752766325136,
0.));
#149182=CARTESIAN_POINT('Ctrl Pts',(-65.1316062586588,32.3752766325136,
12.));
#149183=CARTESIAN_POINT('Ctrl Pts',(-65.1146515748722,32.3564882754212,
0.));
#149184=CARTESIAN_POINT('Ctrl Pts',(-65.1146515748722,32.3564882754212,
12.));
#149185=CARTESIAN_POINT('Ctrl Pts',(-65.0977055875608,32.3377453672051,
0.));
#149186=CARTESIAN_POINT('Ctrl Pts',(-65.0977055875608,32.3377453672051,
12.));
#149187=CARTESIAN_POINT('Ctrl Pts',(-65.0807684081282,32.3190479492987,
0.));
#149188=CARTESIAN_POINT('Ctrl Pts',(-65.0807684081282,32.3190479492987,
12.));
#149189=CARTESIAN_POINT('Ctrl Pts',(-65.0638401484257,32.3003960632006,
0.));
#149190=CARTESIAN_POINT('Ctrl Pts',(-65.0638401484257,32.3003960632006,
12.));
#149191=CARTESIAN_POINT('Ctrl Pts',(-65.0469209207563,32.2817897504807,
0.));
#149192=CARTESIAN_POINT('Ctrl Pts',(-65.0469209207563,32.2817897504807,
12.));
#149193=CARTESIAN_POINT('Ctrl Pts',(-65.03001083788,32.2632290527862,0.));
#149194=CARTESIAN_POINT('Ctrl Pts',(-65.03001083788,32.2632290527862,12.));
#149195=CARTESIAN_POINT('Ctrl Pts',(-65.0131100130158,32.2447140118422,
0.));
#149196=CARTESIAN_POINT('Ctrl Pts',(-65.0131100130158,32.2447140118422,
12.));
#149197=CARTESIAN_POINT('Ctrl Pts',(-64.9962185598462,32.2262446694512,
0.));
#149198=CARTESIAN_POINT('Ctrl Pts',(-64.9962185598462,32.2262446694512,
12.));
#149199=CARTESIAN_POINT('Ctrl Pts',(-64.9793365925178,32.207821067485,0.));
#149200=CARTESIAN_POINT('Ctrl Pts',(-64.9793365925178,32.207821067485,12.));
#149201=CARTESIAN_POINT('Ctrl Pts',(-64.9624642256461,32.189443247888,0.));
#149202=CARTESIAN_POINT('Ctrl Pts',(-64.9624642256461,32.189443247888,12.));
#149203=CARTESIAN_POINT('Ctrl Pts',(-64.9456015743193,32.1711112526854,
0.));
#149204=CARTESIAN_POINT('Ctrl Pts',(-64.9456015743193,32.1711112526854,
12.));
#149205=CARTESIAN_POINT('Ctrl Pts',(-64.9287487541015,32.152825123983,0.));
#149206=CARTESIAN_POINT('Ctrl Pts',(-64.9287487541015,32.152825123983,12.));
#149207=CARTESIAN_POINT('Ctrl Pts',(-64.9119058810367,32.1345849039674,
0.));
#149208=CARTESIAN_POINT('Ctrl Pts',(-64.9119058810367,32.1345849039674,
12.));
#149209=CARTESIAN_POINT('Ctrl Pts',(-64.8950730716501,32.1163906348983,
0.));
#149210=CARTESIAN_POINT('Ctrl Pts',(-64.8950730716501,32.1163906348983,
12.));
#149211=CARTESIAN_POINT('Ctrl Pts',(-64.8782504429527,32.0982423591112,
0.));
#149212=CARTESIAN_POINT('Ctrl Pts',(-64.8782504429527,32.0982423591112,
12.));
#149213=CARTESIAN_POINT('Ctrl Pts',(-64.8614381124455,32.0801401190244,
0.));
#149214=CARTESIAN_POINT('Ctrl Pts',(-64.8614381124455,32.0801401190244,
12.));
#149215=CARTESIAN_POINT('Ctrl Pts',(-64.8446361981234,32.0620839571409,
0.));
#149216=CARTESIAN_POINT('Ctrl Pts',(-64.8446361981234,32.0620839571409,
12.));
#149217=CARTESIAN_POINT('Ctrl Pts',(-64.8278448184785,32.0440739160476,
0.));
#149218=CARTESIAN_POINT('Ctrl Pts',(-64.8278448184785,32.0440739160476,
12.));
#149219=CARTESIAN_POINT('Ctrl Pts',(-64.8110640925021,32.0261100384092,
0.));
#149220=CARTESIAN_POINT('Ctrl Pts',(-64.8110640925021,32.0261100384092,
12.));
#149221=CARTESIAN_POINT('Ctrl Pts',(-64.7942941396883,32.0081923669677,
0.));
#149222=CARTESIAN_POINT('Ctrl Pts',(-64.7942941396883,32.0081923669677,
12.));
#149223=CARTESIAN_POINT('Ctrl Pts',(-64.7775350800405,31.9903209445521,
0.));
#149224=CARTESIAN_POINT('Ctrl Pts',(-64.7775350800405,31.9903209445521,
12.));
#149225=CARTESIAN_POINT('Ctrl Pts',(-64.7607870340738,31.972495814079,0.));
#149226=CARTESIAN_POINT('Ctrl Pts',(-64.7607870340738,31.972495814079,12.));
#149227=CARTESIAN_POINT('Ctrl Pts',(-64.7440501228201,31.9547170185533,
0.));
#149228=CARTESIAN_POINT('Ctrl Pts',(-64.7440501228201,31.9547170185533,
12.));
#149229=CARTESIAN_POINT('Ctrl Pts',(-64.727324467829,31.9369846010613,0.));
#149230=CARTESIAN_POINT('Ctrl Pts',(-64.727324467829,31.9369846010613,12.));
#149231=CARTESIAN_POINT('Ctrl Pts',(-64.7106101911723,31.9192986047702,
0.));
#149232=CARTESIAN_POINT('Ctrl Pts',(-64.7106101911723,31.9192986047702,
12.));
#149233=CARTESIAN_POINT('Ctrl Pts',(-64.6939074154491,31.9016590729371,
0.));
#149234=CARTESIAN_POINT('Ctrl Pts',(-64.6939074154491,31.9016590729371,
12.));
#149235=CARTESIAN_POINT('Ctrl Pts',(-64.6772162637905,31.8840660489106,
0.));
#149236=CARTESIAN_POINT('Ctrl Pts',(-64.6772162637905,31.8840660489106,
12.));
#149237=CARTESIAN_POINT('Ctrl Pts',(-64.6605368598631,31.8665195761311,
0.));
#149238=CARTESIAN_POINT('Ctrl Pts',(-64.6605368598631,31.8665195761311,
12.));
#149239=CARTESIAN_POINT('Ctrl Pts',(-64.6438693278718,31.849019698125,0.));
#149240=CARTESIAN_POINT('Ctrl Pts',(-64.6438693278718,31.849019698125,12.));
#149241=CARTESIAN_POINT('Ctrl Pts',(-64.627213792563,31.8315664585027,0.));
#149242=CARTESIAN_POINT('Ctrl Pts',(-64.627213792563,31.8315664585027,12.));
#149243=CARTESIAN_POINT('Ctrl Pts',(-64.6105703792312,31.8141599009684,
0.));
#149244=CARTESIAN_POINT('Ctrl Pts',(-64.6105703792312,31.8141599009684,
12.));
#149245=CARTESIAN_POINT('Ctrl Pts',(-64.5939392137233,31.7968000693218,
0.));
#149246=CARTESIAN_POINT('Ctrl Pts',(-64.5939392137233,31.7968000693218,
12.));
#149247=CARTESIAN_POINT('Ctrl Pts',(-64.5773204224429,31.7794870074583,
0.));
#149248=CARTESIAN_POINT('Ctrl Pts',(-64.5773204224429,31.7794870074583,
12.));
#149249=CARTESIAN_POINT('Ctrl Pts',(-64.5607141323527,31.7622207593637,
0.));
#149250=CARTESIAN_POINT('Ctrl Pts',(-64.5607141323527,31.7622207593637,
12.));
#149251=CARTESIAN_POINT('Ctrl Pts',(-64.544120470978,31.7450013691116,0.));
#149252=CARTESIAN_POINT('Ctrl Pts',(-64.544120470978,31.7450013691116,12.));
#149253=CARTESIAN_POINT('Ctrl Pts',(-64.5275395664134,31.7278288808736,
0.));
#149254=CARTESIAN_POINT('Ctrl Pts',(-64.5275395664134,31.7278288808736,
12.));
#149255=CARTESIAN_POINT('Ctrl Pts',(-64.5109715473277,31.7107033389204,
0.));
#149256=CARTESIAN_POINT('Ctrl Pts',(-64.5109715473277,31.7107033389204,
12.));
#149257=CARTESIAN_POINT('Ctrl Pts',(-64.4944165429672,31.6936247876228,
0.));
#149258=CARTESIAN_POINT('Ctrl Pts',(-64.4944165429672,31.6936247876228,
12.));
#149259=CARTESIAN_POINT('Ctrl Pts',(-64.4778746831598,31.6765932714456,
0.));
#149260=CARTESIAN_POINT('Ctrl Pts',(-64.4778746831598,31.6765932714456,
12.));
#149261=CARTESIAN_POINT('Ctrl Pts',(-64.4613460983186,31.6596088349468,
0.));
#149262=CARTESIAN_POINT('Ctrl Pts',(-64.4613460983186,31.6596088349468,
12.));
#149263=CARTESIAN_POINT('Ctrl Pts',(-64.4448309194499,31.6426715227865,
0.));
#149264=CARTESIAN_POINT('Ctrl Pts',(-64.4448309194499,31.6426715227865,
12.));
#149265=CARTESIAN_POINT('Ctrl Pts',(-64.4283292781553,31.6257813797281,
0.));
#149266=CARTESIAN_POINT('Ctrl Pts',(-64.4283292781553,31.6257813797281,
12.));
#149267=CARTESIAN_POINT('Ctrl Pts',(-64.4118413066386,31.6089384506399,
0.));
#149268=CARTESIAN_POINT('Ctrl Pts',(-64.4118413066386,31.6089384506399,
12.));
#149269=CARTESIAN_POINT('Ctrl Pts',(-64.3953671377071,31.5921427804879,
0.));
#149270=CARTESIAN_POINT('Ctrl Pts',(-64.3953671377071,31.5921427804879,
12.));
#149271=CARTESIAN_POINT('Ctrl Pts',(-64.3789069047768,31.5753944143355,
0.));
#149272=CARTESIAN_POINT('Ctrl Pts',(-64.3789069047768,31.5753944143355,
12.));
#149273=CARTESIAN_POINT('Ctrl Pts',(-64.3624607418798,31.5586933973531,
0.));
#149274=CARTESIAN_POINT('Ctrl Pts',(-64.3624607418798,31.5586933973531,
12.));
#149275=CARTESIAN_POINT('Ctrl Pts',(-64.34602878367,31.5420397748198,0.));
#149276=CARTESIAN_POINT('Ctrl Pts',(-64.34602878367,31.5420397748198,12.));
#149277=CARTESIAN_POINT('Ctrl Pts',(-64.3296111654273,31.5254335921239,
0.));
#149278=CARTESIAN_POINT('Ctrl Pts',(-64.3296111654273,31.5254335921239,
12.));
#149279=CARTESIAN_POINT('Ctrl Pts',(-64.3132080230603,31.5088748947564,
0.));
#149280=CARTESIAN_POINT('Ctrl Pts',(-64.3132080230603,31.5088748947564,
12.));
#149281=CARTESIAN_POINT('Ctrl Pts',(-64.2968194931113,31.4923637283109,
0.));
#149282=CARTESIAN_POINT('Ctrl Pts',(-64.2968194931113,31.4923637283109,
12.));
#149283=CARTESIAN_POINT('Ctrl Pts',(-64.2804457127633,31.4759001384922,
0.));
#149284=CARTESIAN_POINT('Ctrl Pts',(-64.2804457127633,31.4759001384922,
12.));
#149285=CARTESIAN_POINT('Ctrl Pts',(-64.264086819846,31.4594841711188,0.));
#149286=CARTESIAN_POINT('Ctrl Pts',(-64.264086819846,31.4594841711188,12.));
#149287=CARTESIAN_POINT('Ctrl Pts',(-64.2477429528408,31.4431158721229,
0.));
#149288=CARTESIAN_POINT('Ctrl Pts',(-64.2477429528408,31.4431158721229,
12.));
#149289=CARTESIAN_POINT('Ctrl Pts',(-64.2314142508843,31.4267952875439,
0.));
#149290=CARTESIAN_POINT('Ctrl Pts',(-64.2314142508843,31.4267952875439,
12.));
#149291=CARTESIAN_POINT('Ctrl Pts',(-64.2151008537733,31.4105224635298,
0.));
#149292=CARTESIAN_POINT('Ctrl Pts',(-64.2151008537733,31.4105224635298,
12.));
#149293=CARTESIAN_POINT('Ctrl Pts',(-64.1988029019733,31.3942974463458,
0.));
#149294=CARTESIAN_POINT('Ctrl Pts',(-64.1988029019733,31.3942974463458,
12.));
#149295=CARTESIAN_POINT('Ctrl Pts',(-64.1825205366231,31.3781202823758,
0.));
#149296=CARTESIAN_POINT('Ctrl Pts',(-64.1825205366231,31.3781202823758,
12.));
#149297=CARTESIAN_POINT('Ctrl Pts',(-64.1662538995407,31.3619910181222,
0.));
#149298=CARTESIAN_POINT('Ctrl Pts',(-64.1662538995407,31.3619910181222,
12.));
#149299=CARTESIAN_POINT('Ctrl Pts',(-64.150003133226,31.3459097001995,0.));
#149300=CARTESIAN_POINT('Ctrl Pts',(-64.150003133226,31.3459097001995,12.));
#149301=CARTESIAN_POINT('Ctrl Pts',(-64.1337683808667,31.3298763753366,
0.));
#149302=CARTESIAN_POINT('Ctrl Pts',(-64.1337683808667,31.3298763753366,
12.));
#149303=CARTESIAN_POINT('Ctrl Pts',(-64.1175497863475,31.3138910903852,
0.));
#149304=CARTESIAN_POINT('Ctrl Pts',(-64.1175497863475,31.3138910903852,
12.));
#149305=CARTESIAN_POINT('Ctrl Pts',(-64.1013474942554,31.2979538923213,
0.));
#149306=CARTESIAN_POINT('Ctrl Pts',(-64.1013474942554,31.2979538923213,
12.));
#149307=CARTESIAN_POINT('Ctrl Pts',(-64.0851616498861,31.2820648282451,
0.));
#149308=CARTESIAN_POINT('Ctrl Pts',(-64.0851616498861,31.2820648282451,
12.));
#149309=CARTESIAN_POINT('Ctrl Pts',(-64.0689923992475,31.2662239453734,
0.));
#149310=CARTESIAN_POINT('Ctrl Pts',(-64.0689923992475,31.2662239453734,
12.));
#149311=CARTESIAN_POINT('Ctrl Pts',(-64.0528398890671,31.2504312910457,
0.));
#149312=CARTESIAN_POINT('Ctrl Pts',(-64.0528398890671,31.2504312910457,
12.));
#149313=CARTESIAN_POINT('Ctrl Pts',(-64.036704266799,31.23468691273,0.));
#149314=CARTESIAN_POINT('Ctrl Pts',(-64.036704266799,31.23468691273,12.));
#149315=CARTESIAN_POINT('Ctrl Pts',(-64.0205856806298,31.2189908580245,
0.));
#149316=CARTESIAN_POINT('Ctrl Pts',(-64.0205856806298,31.2189908580245,
12.));
#149317=CARTESIAN_POINT('Ctrl Pts',(-64.004484279483,31.2033431746558,0.));
#149318=CARTESIAN_POINT('Ctrl Pts',(-64.004484279483,31.2033431746558,12.));
#149319=CARTESIAN_POINT('Ctrl Pts',(-63.9884002130209,31.1877439104717,
0.));
#149320=CARTESIAN_POINT('Ctrl Pts',(-63.9884002130209,31.1877439104717,
12.));
#149321=CARTESIAN_POINT('Ctrl Pts',(-63.972333631655,31.1721931134488,0.));
#149322=CARTESIAN_POINT('Ctrl Pts',(-63.972333631655,31.1721931134488,12.));
#149323=CARTESIAN_POINT('Ctrl Pts',(-63.9562846865566,31.1566908316992,
0.));
#149324=CARTESIAN_POINT('Ctrl Pts',(-63.9562846865566,31.1566908316992,
12.));
#149325=CARTESIAN_POINT('Ctrl Pts',(-63.9402535296651,31.1412371134727,
0.));
#149326=CARTESIAN_POINT('Ctrl Pts',(-63.9402535296651,31.1412371134727,
12.));
#149327=CARTESIAN_POINT('Ctrl Pts',(-63.9242403136955,31.1258320071545,
0.));
#149328=CARTESIAN_POINT('Ctrl Pts',(-63.9242403136955,31.1258320071545,
12.));
#149329=CARTESIAN_POINT('Ctrl Pts',(-63.9082451921447,31.1104755612606,
0.));
#149330=CARTESIAN_POINT('Ctrl Pts',(-63.9082451921447,31.1104755612606,
12.));
#149331=CARTESIAN_POINT('Ctrl Pts',(-63.8922683192963,31.0951678244454,
0.));
#149332=CARTESIAN_POINT('Ctrl Pts',(-63.8922683192963,31.0951678244454,
12.));
#149333=CARTESIAN_POINT('Ctrl Pts',(-63.8763098502235,31.079908845504,0.));
#149334=CARTESIAN_POINT('Ctrl Pts',(-63.8763098502235,31.079908845504,12.));
#149335=CARTESIAN_POINT('Ctrl Pts',(-63.8603699407922,31.0646986733723,
0.));
#149336=CARTESIAN_POINT('Ctrl Pts',(-63.8603699407922,31.0646986733723,
12.));
#149337=CARTESIAN_POINT('Ctrl Pts',(-63.8444487476615,31.0495373571217,
0.));
#149338=CARTESIAN_POINT('Ctrl Pts',(-63.8444487476615,31.0495373571217,
12.));
#149339=CARTESIAN_POINT('Ctrl Pts',(-63.8285464282857,31.0344249459544,
0.));
#149340=CARTESIAN_POINT('Ctrl Pts',(-63.8285464282857,31.0344249459544,
12.));
#149341=CARTESIAN_POINT('Ctrl Pts',(-63.8126631409376,31.0193614892177,
0.));
#149342=CARTESIAN_POINT('Ctrl Pts',(-63.8126631409376,31.0193614892177,
12.));
#149343=CARTESIAN_POINT('Ctrl Pts',(-63.7967990447288,31.0043470364112,
0.));
#149344=CARTESIAN_POINT('Ctrl Pts',(-63.7967990447288,31.0043470364112,
12.));
#149345=CARTESIAN_POINT('Ctrl Pts',(-63.7809542996258,30.9893816371907,
0.));
#149346=CARTESIAN_POINT('Ctrl Pts',(-63.7809542996258,30.9893816371907,
12.));
#149347=CARTESIAN_POINT('Ctrl Pts',(-63.7651290664713,30.9744653413679,
0.));
#149348=CARTESIAN_POINT('Ctrl Pts',(-63.7651290664713,30.9744653413679,
12.));
#149349=CARTESIAN_POINT('Ctrl Pts',(-63.7493235069844,30.9595981989091,
0.));
#149350=CARTESIAN_POINT('Ctrl Pts',(-63.7493235069844,30.9595981989091,
12.));
#149351=CARTESIAN_POINT('Ctrl Pts',(-63.733537783742,30.9447802599345,0.));
#149352=CARTESIAN_POINT('Ctrl Pts',(-63.733537783742,30.9447802599345,12.));
#149353=CARTESIAN_POINT('Ctrl Pts',(-63.7177720601604,30.9300115747113,
0.));
#149354=CARTESIAN_POINT('Ctrl Pts',(-63.7177720601604,30.9300115747113,
12.));
#149355=CARTESIAN_POINT('Ctrl Pts',(-63.7020265004805,30.9152921936471,
0.));
#149356=CARTESIAN_POINT('Ctrl Pts',(-63.7020265004805,30.9152921936471,
12.));
#149357=CARTESIAN_POINT('Ctrl Pts',(-63.6863012697354,30.9006221672703,
0.));
#149358=CARTESIAN_POINT('Ctrl Pts',(-63.6863012697354,30.9006221672703,
12.));
#149359=CARTESIAN_POINT('Ctrl Pts',(-63.6705965337996,30.8860015462488,
0.));
#149360=CARTESIAN_POINT('Ctrl Pts',(-63.6705965337996,30.8860015462488,
12.));
#149361=CARTESIAN_POINT('Ctrl Pts',(-63.6549124594681,30.8714303814202,
0.));
#149362=CARTESIAN_POINT('Ctrl Pts',(-63.6549124594681,30.8714303814202,
12.));
#149363=CARTESIAN_POINT('Ctrl Pts',(-63.6392492145233,30.8569087238131,
0.));
#149364=CARTESIAN_POINT('Ctrl Pts',(-63.6392492145233,30.8569087238131,
12.));
#149365=CARTESIAN_POINT('Ctrl Pts',(-63.6236069678041,30.8424366246665,
0.));
#149366=CARTESIAN_POINT('Ctrl Pts',(-63.6236069678041,30.8424366246665,
12.));
#149367=CARTESIAN_POINT('Ctrl Pts',(-63.6079858892747,30.8280141354447,
0.));
#149368=CARTESIAN_POINT('Ctrl Pts',(-63.6079858892747,30.8280141354447,
12.));
#149369=CARTESIAN_POINT('Ctrl Pts',(-63.5923861498964,30.8136413077999,
0.));
#149370=CARTESIAN_POINT('Ctrl Pts',(-63.5923861498964,30.8136413077999,
12.));
#149371=CARTESIAN_POINT('Ctrl Pts',(-63.5768079214868,30.7993181935265,
0.));
#149372=CARTESIAN_POINT('Ctrl Pts',(-63.5768079214868,30.7993181935265,
12.));
#149373=CARTESIAN_POINT('Ctrl Pts',(-63.5612513766005,30.7850448445207,
0.));
#149374=CARTESIAN_POINT('Ctrl Pts',(-63.5612513766005,30.7850448445207,
12.));
#149375=CARTESIAN_POINT('Ctrl Pts',(-63.5457166883558,30.7708213127169,
0.));
#149376=CARTESIAN_POINT('Ctrl Pts',(-63.5457166883558,30.7708213127169,
12.));
#149377=CARTESIAN_POINT('Ctrl Pts',(-63.5302040304174,30.7566476500772,
0.));
#149378=CARTESIAN_POINT('Ctrl Pts',(-63.5302040304174,30.7566476500772,
12.));
#149379=CARTESIAN_POINT('Ctrl Pts',(-63.514713577392,30.7425239087294,0.));
#149380=CARTESIAN_POINT('Ctrl Pts',(-63.514713577392,30.7425239087294,12.));
#149381=CARTESIAN_POINT('Ctrl Pts',(-63.4992455051805,30.7284501410827,
0.));
#149382=CARTESIAN_POINT('Ctrl Pts',(-63.4992455051805,30.7284501410827,
12.));
#149383=CARTESIAN_POINT('Ctrl Pts',(-63.4837999912759,30.7144263999259,
0.));
#149384=CARTESIAN_POINT('Ctrl Pts',(-63.4837999912759,30.7144263999259,
12.));
#149385=CARTESIAN_POINT('Ctrl Pts',(-63.4683772152497,30.7004527385806,
0.));
#149386=CARTESIAN_POINT('Ctrl Pts',(-63.4683772152497,30.7004527385806,
12.));
#149387=CARTESIAN_POINT('Ctrl Pts',(-63.4529773584211,30.686529210791,0.));
#149388=CARTESIAN_POINT('Ctrl Pts',(-63.4529773584211,30.686529210791,12.));
#149389=CARTESIAN_POINT('Ctrl Pts',(-63.4376006029575,30.6726558704301,
0.));
#149390=CARTESIAN_POINT('Ctrl Pts',(-63.4376006029575,30.6726558704301,
12.));
#149391=CARTESIAN_POINT('Ctrl Pts',(-63.4222471311236,30.6588327712482,
0.));
#149392=CARTESIAN_POINT('Ctrl Pts',(-63.4222471311236,30.6588327712482,
12.));
#149393=CARTESIAN_POINT('Ctrl Pts',(-63.4069171245094,30.6450599666134,
0.));
#149394=CARTESIAN_POINT('Ctrl Pts',(-63.4069171245094,30.6450599666134,
12.));
#149395=CARTESIAN_POINT('Ctrl Pts',(-63.3916107631421,30.6313375092084,
0.));
#149396=CARTESIAN_POINT('Ctrl Pts',(-63.3916107631421,30.6313375092084,
12.));
#149397=CARTESIAN_POINT('Ctrl Pts',(-63.3763282271838,30.6176654515988,
0.));
#149398=CARTESIAN_POINT('Ctrl Pts',(-63.3763282271838,30.6176654515988,
12.));
#149399=CARTESIAN_POINT('Ctrl Pts',(-63.3610696989599,30.6040438469089,
0.));
#149400=CARTESIAN_POINT('Ctrl Pts',(-63.3610696989599,30.6040438469089,
12.));
#149401=CARTESIAN_POINT('Ctrl Pts',(-63.3458353646145,30.5904727493707,
0.));
#149402=CARTESIAN_POINT('Ctrl Pts',(-63.3458353646145,30.5904727493707,
12.));
#149403=CARTESIAN_POINT('Ctrl Pts',(-63.330625416509,30.5769522151147,0.));
#149404=CARTESIAN_POINT('Ctrl Pts',(-63.330625416509,30.5769522151147,12.));
#149405=CARTESIAN_POINT('Ctrl Pts',(-63.315440053435,30.5634823022357,0.));
#149406=CARTESIAN_POINT('Ctrl Pts',(-63.315440053435,30.5634823022357,12.));
#149407=CARTESIAN_POINT('Ctrl Pts',(-63.300279475605,30.5500630691342,0.));
#149408=CARTESIAN_POINT('Ctrl Pts',(-63.300279475605,30.5500630691342,12.));
#149409=CARTESIAN_POINT('Ctrl Pts',(-63.2851438802462,30.5366945730503,
0.));
#149410=CARTESIAN_POINT('Ctrl Pts',(-63.2851438802462,30.5366945730503,
12.));
#149411=CARTESIAN_POINT('Ctrl Pts',(-63.2700334577661,30.5233768687875,
0.));
#149412=CARTESIAN_POINT('Ctrl Pts',(-63.2700334577661,30.5233768687875,
12.));
#149413=CARTESIAN_POINT('Ctrl Pts',(-63.2549483856268,30.5101100066683,
0.));
#149414=CARTESIAN_POINT('Ctrl Pts',(-63.2549483856268,30.5101100066683,
12.));
#149415=CARTESIAN_POINT('Ctrl Pts',(-63.2398888342612,30.4968940345027,
0.));
#149416=CARTESIAN_POINT('Ctrl Pts',(-63.2398888342612,30.4968940345027,
12.));
#149417=CARTESIAN_POINT('Ctrl Pts',(-63.2248549788272,30.4837290015011,
0.));
#149418=CARTESIAN_POINT('Ctrl Pts',(-63.2248549788272,30.4837290015011,
12.));
#149419=CARTESIAN_POINT('Ctrl Pts',(-63.2098470086636,30.470614961416,0.));
#149420=CARTESIAN_POINT('Ctrl Pts',(-63.2098470086636,30.470614961416,12.));
#149421=CARTESIAN_POINT('Ctrl Pts',(-63.1948651386868,30.4575519763305,
0.));
#149422=CARTESIAN_POINT('Ctrl Pts',(-63.1948651386868,30.4575519763305,
12.));
#149423=CARTESIAN_POINT('Ctrl Pts',(-63.1799096171757,30.4445401192324,
0.));
#149424=CARTESIAN_POINT('Ctrl Pts',(-63.1799096171757,30.4445401192324,
12.));
#149425=CARTESIAN_POINT('Ctrl Pts',(-63.1649807016766,30.431579465967,0.));
#149426=CARTESIAN_POINT('Ctrl Pts',(-63.1649807016766,30.431579465967,12.));
#149427=CARTESIAN_POINT('Ctrl Pts',(-63.1500786361382,30.4186700875598,
0.));
#149428=CARTESIAN_POINT('Ctrl Pts',(-63.1500786361382,30.4186700875598,
12.));
#149429=CARTESIAN_POINT('Ctrl Pts',(-63.1352036298512,30.4058120432259,
0.));
#149430=CARTESIAN_POINT('Ctrl Pts',(-63.1352036298512,30.4058120432259,
12.));
#149431=CARTESIAN_POINT('Ctrl Pts',(-63.1203558300911,30.3930053710592,
0.));
#149432=CARTESIAN_POINT('Ctrl Pts',(-63.1203558300911,30.3930053710592,
12.));
#149433=CARTESIAN_POINT('Ctrl Pts',(-63.1055353202641,30.3802500880564,
0.));
#149434=CARTESIAN_POINT('Ctrl Pts',(-63.1055353202641,30.3802500880564,
12.));
#149435=CARTESIAN_POINT('Ctrl Pts',(-63.0937007763826,30.3700869762658,
0.));
#149436=CARTESIAN_POINT('Ctrl Pts',(-63.0937007763826,30.3700869762658,
12.));
#149437=CARTESIAN_POINT('Ctrl Pts',(-63.0848371718274,30.3624877680747,
0.));
#149438=CARTESIAN_POINT('Ctrl Pts',(-63.0848371718274,30.3624877680747,
12.));
#149439=CARTESIAN_POINT('Ctrl Pts',(-63.0789335700774,30.3574319069365,
0.));
#149440=CARTESIAN_POINT('Ctrl Pts',(-63.0789335700774,30.3574319069365,
12.));
#149441=CARTESIAN_POINT('Ctrl Pts',(-63.0759831361898,30.3549065457811,
0.));
#149442=CARTESIAN_POINT('Ctrl Pts',(-63.0759831361898,30.3549065457811,
12.));
#149443=CARTESIAN_POINT('',(-63.0759831361898,30.3549065457811,12.));
#149444=CARTESIAN_POINT('Ctrl Pts',(-63.0759831361898,30.3549065457811,
12.));
#149445=CARTESIAN_POINT('Ctrl Pts',(-63.0789335700774,30.3574319069365,
12.));
#149446=CARTESIAN_POINT('Ctrl Pts',(-63.0848371718274,30.3624877680747,
12.));
#149447=CARTESIAN_POINT('Ctrl Pts',(-63.0937007763826,30.3700869762658,
12.));
#149448=CARTESIAN_POINT('Ctrl Pts',(-63.1055353202641,30.3802500880564,
12.));
#149449=CARTESIAN_POINT('Ctrl Pts',(-63.1203558300911,30.3930053710592,
12.));
#149450=CARTESIAN_POINT('Ctrl Pts',(-63.1352036298512,30.4058120432259,
12.));
#149451=CARTESIAN_POINT('Ctrl Pts',(-63.1500786361382,30.4186700875598,
12.));
#149452=CARTESIAN_POINT('Ctrl Pts',(-63.1649807016766,30.431579465967,12.));
#149453=CARTESIAN_POINT('Ctrl Pts',(-63.1799096171757,30.4445401192324,
12.));
#149454=CARTESIAN_POINT('Ctrl Pts',(-63.1948651386868,30.4575519763305,
12.));
#149455=CARTESIAN_POINT('Ctrl Pts',(-63.2098470086636,30.470614961416,12.));
#149456=CARTESIAN_POINT('Ctrl Pts',(-63.2248549788272,30.4837290015011,
12.));
#149457=CARTESIAN_POINT('Ctrl Pts',(-63.2398888342612,30.4968940345027,
12.));
#149458=CARTESIAN_POINT('Ctrl Pts',(-63.2549483856268,30.5101100066683,
12.));
#149459=CARTESIAN_POINT('Ctrl Pts',(-63.2700334577661,30.5233768687875,
12.));
#149460=CARTESIAN_POINT('Ctrl Pts',(-63.2851438802462,30.5366945730503,
12.));
#149461=CARTESIAN_POINT('Ctrl Pts',(-63.300279475605,30.5500630691342,12.));
#149462=CARTESIAN_POINT('Ctrl Pts',(-63.315440053435,30.5634823022357,12.));
#149463=CARTESIAN_POINT('Ctrl Pts',(-63.330625416509,30.5769522151147,12.));
#149464=CARTESIAN_POINT('Ctrl Pts',(-63.3458353646145,30.5904727493707,
12.));
#149465=CARTESIAN_POINT('Ctrl Pts',(-63.3610696989599,30.6040438469089,
12.));
#149466=CARTESIAN_POINT('Ctrl Pts',(-63.3763282271838,30.6176654515988,
12.));
#149467=CARTESIAN_POINT('Ctrl Pts',(-63.3916107631421,30.6313375092084,
12.));
#149468=CARTESIAN_POINT('Ctrl Pts',(-63.4069171245094,30.6450599666134,
12.));
#149469=CARTESIAN_POINT('Ctrl Pts',(-63.4222471311236,30.6588327712482,
12.));
#149470=CARTESIAN_POINT('Ctrl Pts',(-63.4376006029575,30.6726558704301,
12.));
#149471=CARTESIAN_POINT('Ctrl Pts',(-63.4529773584211,30.686529210791,12.));
#149472=CARTESIAN_POINT('Ctrl Pts',(-63.4683772152497,30.7004527385806,
12.));
#149473=CARTESIAN_POINT('Ctrl Pts',(-63.4837999912759,30.7144263999259,
12.));
#149474=CARTESIAN_POINT('Ctrl Pts',(-63.4992455051805,30.7284501410827,
12.));
#149475=CARTESIAN_POINT('Ctrl Pts',(-63.514713577392,30.7425239087294,12.));
#149476=CARTESIAN_POINT('Ctrl Pts',(-63.5302040304174,30.7566476500772,
12.));
#149477=CARTESIAN_POINT('Ctrl Pts',(-63.5457166883558,30.7708213127169,
12.));
#149478=CARTESIAN_POINT('Ctrl Pts',(-63.5612513766005,30.7850448445207,
12.));
#149479=CARTESIAN_POINT('Ctrl Pts',(-63.5768079214868,30.7993181935265,
12.));
#149480=CARTESIAN_POINT('Ctrl Pts',(-63.5923861498964,30.8136413077999,
12.));
#149481=CARTESIAN_POINT('Ctrl Pts',(-63.6079858892747,30.8280141354447,
12.));
#149482=CARTESIAN_POINT('Ctrl Pts',(-63.6236069678041,30.8424366246665,
12.));
#149483=CARTESIAN_POINT('Ctrl Pts',(-63.6392492145233,30.8569087238131,
12.));
#149484=CARTESIAN_POINT('Ctrl Pts',(-63.6549124594681,30.8714303814202,
12.));
#149485=CARTESIAN_POINT('Ctrl Pts',(-63.6705965337996,30.8860015462488,
12.));
#149486=CARTESIAN_POINT('Ctrl Pts',(-63.6863012697354,30.9006221672703,
12.));
#149487=CARTESIAN_POINT('Ctrl Pts',(-63.7020265004805,30.9152921936471,
12.));
#149488=CARTESIAN_POINT('Ctrl Pts',(-63.7177720601604,30.9300115747113,
12.));
#149489=CARTESIAN_POINT('Ctrl Pts',(-63.733537783742,30.9447802599345,12.));
#149490=CARTESIAN_POINT('Ctrl Pts',(-63.7493235069844,30.9595981989091,
12.));
#149491=CARTESIAN_POINT('Ctrl Pts',(-63.7651290664713,30.9744653413679,
12.));
#149492=CARTESIAN_POINT('Ctrl Pts',(-63.7809542996258,30.9893816371907,
12.));
#149493=CARTESIAN_POINT('Ctrl Pts',(-63.7967990447288,31.0043470364112,
12.));
#149494=CARTESIAN_POINT('Ctrl Pts',(-63.8126631409376,31.0193614892177,
12.));
#149495=CARTESIAN_POINT('Ctrl Pts',(-63.8285464282857,31.0344249459544,
12.));
#149496=CARTESIAN_POINT('Ctrl Pts',(-63.8444487476615,31.0495373571217,
12.));
#149497=CARTESIAN_POINT('Ctrl Pts',(-63.8603699407922,31.0646986733723,
12.));
#149498=CARTESIAN_POINT('Ctrl Pts',(-63.8763098502235,31.079908845504,12.));
#149499=CARTESIAN_POINT('Ctrl Pts',(-63.8922683192963,31.0951678244454,
12.));
#149500=CARTESIAN_POINT('Ctrl Pts',(-63.9082451921447,31.1104755612606,
12.));
#149501=CARTESIAN_POINT('Ctrl Pts',(-63.9242403136955,31.1258320071545,
12.));
#149502=CARTESIAN_POINT('Ctrl Pts',(-63.9402535296651,31.1412371134727,
12.));
#149503=CARTESIAN_POINT('Ctrl Pts',(-63.9562846865566,31.1566908316992,
12.));
#149504=CARTESIAN_POINT('Ctrl Pts',(-63.972333631655,31.1721931134488,12.));
#149505=CARTESIAN_POINT('Ctrl Pts',(-63.9884002130209,31.1877439104717,
12.));
#149506=CARTESIAN_POINT('Ctrl Pts',(-64.004484279483,31.2033431746558,12.));
#149507=CARTESIAN_POINT('Ctrl Pts',(-64.0205856806298,31.2189908580245,
12.));
#149508=CARTESIAN_POINT('Ctrl Pts',(-64.036704266799,31.23468691273,12.));
#149509=CARTESIAN_POINT('Ctrl Pts',(-64.0528398890671,31.2504312910457,
12.));
#149510=CARTESIAN_POINT('Ctrl Pts',(-64.0689923992475,31.2662239453734,
12.));
#149511=CARTESIAN_POINT('Ctrl Pts',(-64.0851616498861,31.2820648282451,
12.));
#149512=CARTESIAN_POINT('Ctrl Pts',(-64.1013474942554,31.2979538923213,
12.));
#149513=CARTESIAN_POINT('Ctrl Pts',(-64.1175497863475,31.3138910903852,
12.));
#149514=CARTESIAN_POINT('Ctrl Pts',(-64.1337683808667,31.3298763753366,
12.));
#149515=CARTESIAN_POINT('Ctrl Pts',(-64.150003133226,31.3459097001995,12.));
#149516=CARTESIAN_POINT('Ctrl Pts',(-64.1662538995407,31.3619910181222,
12.));
#149517=CARTESIAN_POINT('Ctrl Pts',(-64.1825205366231,31.3781202823758,
12.));
#149518=CARTESIAN_POINT('Ctrl Pts',(-64.1988029019733,31.3942974463458,
12.));
#149519=CARTESIAN_POINT('Ctrl Pts',(-64.2151008537733,31.4105224635298,
12.));
#149520=CARTESIAN_POINT('Ctrl Pts',(-64.2314142508843,31.4267952875439,
12.));
#149521=CARTESIAN_POINT('Ctrl Pts',(-64.2477429528408,31.4431158721229,
12.));
#149522=CARTESIAN_POINT('Ctrl Pts',(-64.264086819846,31.4594841711188,12.));
#149523=CARTESIAN_POINT('Ctrl Pts',(-64.2804457127633,31.4759001384922,
12.));
#149524=CARTESIAN_POINT('Ctrl Pts',(-64.2968194931113,31.4923637283109,
12.));
#149525=CARTESIAN_POINT('Ctrl Pts',(-64.3132080230603,31.5088748947564,
12.));
#149526=CARTESIAN_POINT('Ctrl Pts',(-64.3296111654273,31.5254335921239,
12.));
#149527=CARTESIAN_POINT('Ctrl Pts',(-64.34602878367,31.5420397748198,12.));
#149528=CARTESIAN_POINT('Ctrl Pts',(-64.3624607418798,31.5586933973531,
12.));
#149529=CARTESIAN_POINT('Ctrl Pts',(-64.3789069047768,31.5753944143355,
12.));
#149530=CARTESIAN_POINT('Ctrl Pts',(-64.3953671377071,31.5921427804879,
12.));
#149531=CARTESIAN_POINT('Ctrl Pts',(-64.4118413066386,31.6089384506399,
12.));
#149532=CARTESIAN_POINT('Ctrl Pts',(-64.4283292781553,31.6257813797281,
12.));
#149533=CARTESIAN_POINT('Ctrl Pts',(-64.4448309194499,31.6426715227865,
12.));
#149534=CARTESIAN_POINT('Ctrl Pts',(-64.4613460983186,31.6596088349468,
12.));
#149535=CARTESIAN_POINT('Ctrl Pts',(-64.4778746831598,31.6765932714456,
12.));
#149536=CARTESIAN_POINT('Ctrl Pts',(-64.4944165429672,31.6936247876228,
12.));
#149537=CARTESIAN_POINT('Ctrl Pts',(-64.5109715473277,31.7107033389204,
12.));
#149538=CARTESIAN_POINT('Ctrl Pts',(-64.5275395664134,31.7278288808736,
12.));
#149539=CARTESIAN_POINT('Ctrl Pts',(-64.544120470978,31.7450013691116,12.));
#149540=CARTESIAN_POINT('Ctrl Pts',(-64.5607141323527,31.7622207593637,
12.));
#149541=CARTESIAN_POINT('Ctrl Pts',(-64.5773204224429,31.7794870074583,
12.));
#149542=CARTESIAN_POINT('Ctrl Pts',(-64.5939392137233,31.7968000693218,
12.));
#149543=CARTESIAN_POINT('Ctrl Pts',(-64.6105703792312,31.8141599009684,
12.));
#149544=CARTESIAN_POINT('Ctrl Pts',(-64.627213792563,31.8315664585027,12.));
#149545=CARTESIAN_POINT('Ctrl Pts',(-64.6438693278718,31.849019698125,12.));
#149546=CARTESIAN_POINT('Ctrl Pts',(-64.6605368598631,31.8665195761311,
12.));
#149547=CARTESIAN_POINT('Ctrl Pts',(-64.6772162637905,31.8840660489106,
12.));
#149548=CARTESIAN_POINT('Ctrl Pts',(-64.6939074154491,31.9016590729371,
12.));
#149549=CARTESIAN_POINT('Ctrl Pts',(-64.7106101911723,31.9192986047702,
12.));
#149550=CARTESIAN_POINT('Ctrl Pts',(-64.727324467829,31.9369846010613,12.));
#149551=CARTESIAN_POINT('Ctrl Pts',(-64.7440501228201,31.9547170185533,
12.));
#149552=CARTESIAN_POINT('Ctrl Pts',(-64.7607870340738,31.972495814079,12.));
#149553=CARTESIAN_POINT('Ctrl Pts',(-64.7775350800405,31.9903209445521,
12.));
#149554=CARTESIAN_POINT('Ctrl Pts',(-64.7942941396883,32.0081923669677,
12.));
#149555=CARTESIAN_POINT('Ctrl Pts',(-64.8110640925021,32.0261100384092,
12.));
#149556=CARTESIAN_POINT('Ctrl Pts',(-64.8278448184785,32.0440739160476,
12.));
#149557=CARTESIAN_POINT('Ctrl Pts',(-64.8446361981234,32.0620839571409,
12.));
#149558=CARTESIAN_POINT('Ctrl Pts',(-64.8614381124455,32.0801401190244,
12.));
#149559=CARTESIAN_POINT('Ctrl Pts',(-64.8782504429527,32.0982423591112,
12.));
#149560=CARTESIAN_POINT('Ctrl Pts',(-64.8950730716501,32.1163906348983,
12.));
#149561=CARTESIAN_POINT('Ctrl Pts',(-64.9119058810367,32.1345849039674,
12.));
#149562=CARTESIAN_POINT('Ctrl Pts',(-64.9287487541015,32.152825123983,12.));
#149563=CARTESIAN_POINT('Ctrl Pts',(-64.9456015743193,32.1711112526854,
12.));
#149564=CARTESIAN_POINT('Ctrl Pts',(-64.9624642256461,32.189443247888,12.));
#149565=CARTESIAN_POINT('Ctrl Pts',(-64.9793365925178,32.207821067485,12.));
#149566=CARTESIAN_POINT('Ctrl Pts',(-64.9962185598462,32.2262446694512,
12.));
#149567=CARTESIAN_POINT('Ctrl Pts',(-65.0131100130158,32.2447140118422,
12.));
#149568=CARTESIAN_POINT('Ctrl Pts',(-65.03001083788,32.2632290527862,12.));
#149569=CARTESIAN_POINT('Ctrl Pts',(-65.0469209207563,32.2817897504807,
12.));
#149570=CARTESIAN_POINT('Ctrl Pts',(-65.0638401484257,32.3003960632006,
12.));
#149571=CARTESIAN_POINT('Ctrl Pts',(-65.0807684081282,32.3190479492987,
12.));
#149572=CARTESIAN_POINT('Ctrl Pts',(-65.0977055875608,32.3377453672051,
12.));
#149573=CARTESIAN_POINT('Ctrl Pts',(-65.1146515748722,32.3564882754212,
12.));
#149574=CARTESIAN_POINT('Ctrl Pts',(-65.1316062586588,32.3752766325136,
12.));
#149575=CARTESIAN_POINT('Ctrl Pts',(-65.1485695279635,32.3941103971221,
12.));
#149576=CARTESIAN_POINT('Ctrl Pts',(-65.1655412722726,32.4129895279615,
12.));
#149577=CARTESIAN_POINT('Ctrl Pts',(-65.182521381514,32.4319139838212,12.));
#149578=CARTESIAN_POINT('Ctrl Pts',(-65.1995097460538,32.450883723561,12.));
#149579=CARTESIAN_POINT('Ctrl Pts',(-65.2165062566924,32.4698987061032,
12.));
#149580=CARTESIAN_POINT('Ctrl Pts',(-65.2335108046614,32.4889588904392,
12.));
#149581=CARTESIAN_POINT('Ctrl Pts',(-65.2505232816209,32.5080642356328,
12.));
#149582=CARTESIAN_POINT('Ctrl Pts',(-65.2675435796558,32.5272147008191,
12.));
#149583=CARTESIAN_POINT('Ctrl Pts',(-65.2845715912721,32.5464102452014,
12.));
#149584=CARTESIAN_POINT('Ctrl Pts',(-65.3016072093912,32.5656508280421,
12.));
#149585=CARTESIAN_POINT('Ctrl Pts',(-65.31865032735,32.5849364086678,12.));
#149586=CARTESIAN_POINT('Ctrl Pts',(-65.3357008389004,32.604266946475,12.));
#149587=CARTESIAN_POINT('Ctrl Pts',(-65.3527586382081,32.6236424009301,
12.));
#149588=CARTESIAN_POINT('Ctrl Pts',(-65.3698236198513,32.6430627315674,
12.));
#149589=CARTESIAN_POINT('Ctrl Pts',(-65.3868956788182,32.662527897981,12.));
#149590=CARTESIAN_POINT('Ctrl Pts',(-65.4039747105039,32.6820378598267,
12.));
#149591=CARTESIAN_POINT('Ctrl Pts',(-65.4210606107035,32.7015925768265,
12.));
#149592=CARTESIAN_POINT('Ctrl Pts',(-65.4381532756065,32.7211920087683,
12.));
#149593=CARTESIAN_POINT('Ctrl Pts',(-65.4552526017905,32.7408361155037,
12.));
#149594=CARTESIAN_POINT('Ctrl Pts',(-65.4723584862122,32.7605248569378,
12.));
#149595=CARTESIAN_POINT('Ctrl Pts',(-65.4894708262061,32.7802581930287,
12.));
#149596=CARTESIAN_POINT('Ctrl Pts',(-65.5065895194929,32.8000360837974,
12.));
#149597=CARTESIAN_POINT('Ctrl Pts',(-65.5237144641858,32.8198584893315,
12.));
#149598=CARTESIAN_POINT('Ctrl Pts',(-65.5408455587965,32.8397253697865,
12.));
#149599=CARTESIAN_POINT('Ctrl Pts',(-65.5579827022421,32.8596366853832,
12.));
#149600=CARTESIAN_POINT('Ctrl Pts',(-65.5751257938473,32.879592396403,12.));
#149601=CARTESIAN_POINT('Ctrl Pts',(-65.5922747333194,32.8995924631898,
12.));
#149602=CARTESIAN_POINT('Ctrl Pts',(-65.6094294207276,32.9196368461463,
12.));
#149603=CARTESIAN_POINT('Ctrl Pts',(-65.6265897564783,32.9397255057274,
12.));
#149604=CARTESIAN_POINT('Ctrl Pts',(-65.6437556412947,32.9598584024312,
12.));
#149605=CARTESIAN_POINT('Ctrl Pts',(-65.6609269761889,32.9800354967839,
12.));
#149606=CARTESIAN_POINT('Ctrl Pts',(-65.6781036625027,33.0002567493573,
12.));
#149607=CARTESIAN_POINT('Ctrl Pts',(-65.6952856019533,33.0205221207872,
12.));
#149608=CARTESIAN_POINT('Ctrl Pts',(-65.7124726966802,33.0408315717873,
12.));
#149609=CARTESIAN_POINT('Ctrl Pts',(-65.7296648492825,33.0611850631582,
12.));
#149610=CARTESIAN_POINT('Ctrl Pts',(-65.7468619628816,33.081582555798,12.));
#149611=CARTESIAN_POINT('Ctrl Pts',(-65.7640639410661,33.1020240106884,
12.));
#149612=CARTESIAN_POINT('Ctrl Pts',(-65.7812706877697,33.1225093888671,
12.));
#149613=CARTESIAN_POINT('Ctrl Pts',(-65.7984821071623,33.1430386513976,
12.));
#149614=CARTESIAN_POINT('Ctrl Pts',(-65.8156981035503,33.16361175934,12.));
#149615=CARTESIAN_POINT('Ctrl Pts',(-65.8329185812375,33.1842286737051,
12.));
#149616=CARTESIAN_POINT('Ctrl Pts',(-65.8501434445164,33.2048893554491,
12.));
#149617=CARTESIAN_POINT('Ctrl Pts',(-65.8673725979578,33.2255937655649,
12.));
#149618=CARTESIAN_POINT('Ctrl Pts',(-65.8846059466372,33.2463418651492,
12.));
#149619=CARTESIAN_POINT('Ctrl Pts',(-65.9018433963889,33.2671336154753,
12.));
#149620=CARTESIAN_POINT('Ctrl Pts',(-65.9190848540433,33.2879689780572,
12.));
#149621=CARTESIAN_POINT('Ctrl Pts',(-65.9363302276846,33.3088479147164,
12.));
#149622=CARTESIAN_POINT('Ctrl Pts',(-65.9535794260831,33.3297703874265,
12.));
#149623=CARTESIAN_POINT('Ctrl Pts',(-65.970832358141,33.3507363581592,12.));
#149624=CARTESIAN_POINT('Ctrl Pts',(-65.9880889322831,33.37174578871,12.));
#149625=CARTESIAN_POINT('Ctrl Pts',(-66.0053490559812,33.3927986405605,
12.));
#149626=CARTESIAN_POINT('Ctrl Pts',(-66.0226126349446,33.4138948746388,
12.));
#149627=CARTESIAN_POINT('Ctrl Pts',(-66.0398795737777,33.43503445151,12.));
#149628=CARTESIAN_POINT('Ctrl Pts',(-66.0571497774434,33.4562173318025,
12.));
#149629=CARTESIAN_POINT('Ctrl Pts',(-66.0744231525415,33.4774434765745,
12.));
#149630=CARTESIAN_POINT('Ctrl Pts',(-66.0916996085245,33.4987128476622,
12.));
#149631=CARTESIAN_POINT('Ctrl Pts',(-66.1089790592729,33.5200254081243,
12.));
#149632=CARTESIAN_POINT('Ctrl Pts',(-66.1262614234675,33.541381122345,12.));
#149633=CARTESIAN_POINT('Ctrl Pts',(-66.1410781873279,33.5597240685847,
12.));
#149634=CARTESIAN_POINT('Ctrl Pts',(-66.1524393974176,33.5738105077877,
12.));
#149635=CARTESIAN_POINT('Ctrl Pts',(-66.1603438177524,33.5836213514192,
12.));
#149636=CARTESIAN_POINT('Ctrl Pts',(-66.1647906582661,33.5891439876497,
12.));
#149637=CARTESIAN_POINT('Ctrl Pts',(-66.1657795405966,33.5903722665284,
12.));
#149638=CARTESIAN_POINT('',(-63.0759831361898,30.3549065457811,0.));
#149639=CARTESIAN_POINT('',(-63.0759831361898,30.3549065457811,0.));
#149640=CARTESIAN_POINT('Ctrl Pts',(-66.1657795405966,33.5903722665284,
0.));
#149641=CARTESIAN_POINT('Ctrl Pts',(-66.1647906582661,33.5891439876497,
0.));
#149642=CARTESIAN_POINT('Ctrl Pts',(-66.1603438177524,33.5836213514192,
0.));
#149643=CARTESIAN_POINT('Ctrl Pts',(-66.1524393974176,33.5738105077877,
0.));
#149644=CARTESIAN_POINT('Ctrl Pts',(-66.1410781873279,33.5597240685847,
0.));
#149645=CARTESIAN_POINT('Ctrl Pts',(-66.1262614234675,33.541381122345,0.));
#149646=CARTESIAN_POINT('Ctrl Pts',(-66.1089790592729,33.5200254081243,
0.));
#149647=CARTESIAN_POINT('Ctrl Pts',(-66.0916996085245,33.4987128476622,
0.));
#149648=CARTESIAN_POINT('Ctrl Pts',(-66.0744231525415,33.4774434765745,
0.));
#149649=CARTESIAN_POINT('Ctrl Pts',(-66.0571497774434,33.4562173318025,
0.));
#149650=CARTESIAN_POINT('Ctrl Pts',(-66.0398795737777,33.43503445151,0.));
#149651=CARTESIAN_POINT('Ctrl Pts',(-66.0226126349446,33.4138948746388,
0.));
#149652=CARTESIAN_POINT('Ctrl Pts',(-66.0053490559812,33.3927986405605,
0.));
#149653=CARTESIAN_POINT('Ctrl Pts',(-65.9880889322831,33.37174578871,0.));
#149654=CARTESIAN_POINT('Ctrl Pts',(-65.970832358141,33.3507363581592,0.));
#149655=CARTESIAN_POINT('Ctrl Pts',(-65.9535794260831,33.3297703874265,
0.));
#149656=CARTESIAN_POINT('Ctrl Pts',(-65.9363302276846,33.3088479147164,
0.));
#149657=CARTESIAN_POINT('Ctrl Pts',(-65.9190848540433,33.2879689780572,
0.));
#149658=CARTESIAN_POINT('Ctrl Pts',(-65.9018433963889,33.2671336154753,
0.));
#149659=CARTESIAN_POINT('Ctrl Pts',(-65.8846059466372,33.2463418651492,
0.));
#149660=CARTESIAN_POINT('Ctrl Pts',(-65.8673725979578,33.2255937655649,
0.));
#149661=CARTESIAN_POINT('Ctrl Pts',(-65.8501434445164,33.2048893554491,
0.));
#149662=CARTESIAN_POINT('Ctrl Pts',(-65.8329185812375,33.1842286737051,
0.));
#149663=CARTESIAN_POINT('Ctrl Pts',(-65.8156981035503,33.16361175934,0.));
#149664=CARTESIAN_POINT('Ctrl Pts',(-65.7984821071623,33.1430386513976,
0.));
#149665=CARTESIAN_POINT('Ctrl Pts',(-65.7812706877697,33.1225093888671,
0.));
#149666=CARTESIAN_POINT('Ctrl Pts',(-65.7640639410661,33.1020240106884,
0.));
#149667=CARTESIAN_POINT('Ctrl Pts',(-65.7468619628816,33.081582555798,0.));
#149668=CARTESIAN_POINT('Ctrl Pts',(-65.7296648492825,33.0611850631582,
0.));
#149669=CARTESIAN_POINT('Ctrl Pts',(-65.7124726966802,33.0408315717873,
0.));
#149670=CARTESIAN_POINT('Ctrl Pts',(-65.6952856019533,33.0205221207872,
0.));
#149671=CARTESIAN_POINT('Ctrl Pts',(-65.6781036625027,33.0002567493573,
0.));
#149672=CARTESIAN_POINT('Ctrl Pts',(-65.6609269761889,32.9800354967839,
0.));
#149673=CARTESIAN_POINT('Ctrl Pts',(-65.6437556412947,32.9598584024312,
0.));
#149674=CARTESIAN_POINT('Ctrl Pts',(-65.6265897564783,32.9397255057274,
0.));
#149675=CARTESIAN_POINT('Ctrl Pts',(-65.6094294207276,32.9196368461463,
0.));
#149676=CARTESIAN_POINT('Ctrl Pts',(-65.5922747333194,32.8995924631898,
0.));
#149677=CARTESIAN_POINT('Ctrl Pts',(-65.5751257938473,32.879592396403,0.));
#149678=CARTESIAN_POINT('Ctrl Pts',(-65.5579827022421,32.8596366853832,
0.));
#149679=CARTESIAN_POINT('Ctrl Pts',(-65.5408455587965,32.8397253697865,
0.));
#149680=CARTESIAN_POINT('Ctrl Pts',(-65.5237144641858,32.8198584893315,
0.));
#149681=CARTESIAN_POINT('Ctrl Pts',(-65.5065895194929,32.8000360837974,
0.));
#149682=CARTESIAN_POINT('Ctrl Pts',(-65.4894708262061,32.7802581930287,
0.));
#149683=CARTESIAN_POINT('Ctrl Pts',(-65.4723584862122,32.7605248569378,
0.));
#149684=CARTESIAN_POINT('Ctrl Pts',(-65.4552526017905,32.7408361155037,
0.));
#149685=CARTESIAN_POINT('Ctrl Pts',(-65.4381532756065,32.7211920087683,
0.));
#149686=CARTESIAN_POINT('Ctrl Pts',(-65.4210606107035,32.7015925768265,
0.));
#149687=CARTESIAN_POINT('Ctrl Pts',(-65.4039747105039,32.6820378598267,
0.));
#149688=CARTESIAN_POINT('Ctrl Pts',(-65.3868956788182,32.662527897981,0.));
#149689=CARTESIAN_POINT('Ctrl Pts',(-65.3698236198513,32.6430627315674,
0.));
#149690=CARTESIAN_POINT('Ctrl Pts',(-65.3527586382081,32.6236424009301,
0.));
#149691=CARTESIAN_POINT('Ctrl Pts',(-65.3357008389004,32.604266946475,0.));
#149692=CARTESIAN_POINT('Ctrl Pts',(-65.31865032735,32.5849364086678,0.));
#149693=CARTESIAN_POINT('Ctrl Pts',(-65.3016072093912,32.5656508280421,
0.));
#149694=CARTESIAN_POINT('Ctrl Pts',(-65.2845715912721,32.5464102452014,
0.));
#149695=CARTESIAN_POINT('Ctrl Pts',(-65.2675435796558,32.5272147008191,
0.));
#149696=CARTESIAN_POINT('Ctrl Pts',(-65.2505232816209,32.5080642356328,
0.));
#149697=CARTESIAN_POINT('Ctrl Pts',(-65.2335108046614,32.4889588904392,
0.));
#149698=CARTESIAN_POINT('Ctrl Pts',(-65.2165062566924,32.4698987061032,
0.));
#149699=CARTESIAN_POINT('Ctrl Pts',(-65.1995097460538,32.450883723561,0.));
#149700=CARTESIAN_POINT('Ctrl Pts',(-65.182521381514,32.4319139838212,0.));
#149701=CARTESIAN_POINT('Ctrl Pts',(-65.1655412722726,32.4129895279615,
0.));
#149702=CARTESIAN_POINT('Ctrl Pts',(-65.1485695279635,32.3941103971221,
0.));
#149703=CARTESIAN_POINT('Ctrl Pts',(-65.1316062586588,32.3752766325136,
0.));
#149704=CARTESIAN_POINT('Ctrl Pts',(-65.1146515748722,32.3564882754212,
0.));
#149705=CARTESIAN_POINT('Ctrl Pts',(-65.0977055875608,32.3377453672051,
0.));
#149706=CARTESIAN_POINT('Ctrl Pts',(-65.0807684081282,32.3190479492987,
0.));
#149707=CARTESIAN_POINT('Ctrl Pts',(-65.0638401484257,32.3003960632006,
0.));
#149708=CARTESIAN_POINT('Ctrl Pts',(-65.0469209207563,32.2817897504807,
0.));
#149709=CARTESIAN_POINT('Ctrl Pts',(-65.03001083788,32.2632290527862,0.));
#149710=CARTESIAN_POINT('Ctrl Pts',(-65.0131100130158,32.2447140118422,
0.));
#149711=CARTESIAN_POINT('Ctrl Pts',(-64.9962185598462,32.2262446694512,
0.));
#149712=CARTESIAN_POINT('Ctrl Pts',(-64.9793365925178,32.207821067485,0.));
#149713=CARTESIAN_POINT('Ctrl Pts',(-64.9624642256461,32.189443247888,0.));
#149714=CARTESIAN_POINT('Ctrl Pts',(-64.9456015743193,32.1711112526854,
0.));
#149715=CARTESIAN_POINT('Ctrl Pts',(-64.9287487541015,32.152825123983,0.));
#149716=CARTESIAN_POINT('Ctrl Pts',(-64.9119058810367,32.1345849039674,
0.));
#149717=CARTESIAN_POINT('Ctrl Pts',(-64.8950730716501,32.1163906348983,
0.));
#149718=CARTESIAN_POINT('Ctrl Pts',(-64.8782504429527,32.0982423591112,
0.));
#149719=CARTESIAN_POINT('Ctrl Pts',(-64.8614381124455,32.0801401190244,
0.));
#149720=CARTESIAN_POINT('Ctrl Pts',(-64.8446361981234,32.0620839571409,
0.));
#149721=CARTESIAN_POINT('Ctrl Pts',(-64.8278448184785,32.0440739160476,
0.));
#149722=CARTESIAN_POINT('Ctrl Pts',(-64.8110640925021,32.0261100384092,
0.));
#149723=CARTESIAN_POINT('Ctrl Pts',(-64.7942941396883,32.0081923669677,
0.));
#149724=CARTESIAN_POINT('Ctrl Pts',(-64.7775350800405,31.9903209445521,
0.));
#149725=CARTESIAN_POINT('Ctrl Pts',(-64.7607870340738,31.972495814079,0.));
#149726=CARTESIAN_POINT('Ctrl Pts',(-64.7440501228201,31.9547170185533,
0.));
#149727=CARTESIAN_POINT('Ctrl Pts',(-64.727324467829,31.9369846010613,0.));
#149728=CARTESIAN_POINT('Ctrl Pts',(-64.7106101911723,31.9192986047702,
0.));
#149729=CARTESIAN_POINT('Ctrl Pts',(-64.6939074154491,31.9016590729371,
0.));
#149730=CARTESIAN_POINT('Ctrl Pts',(-64.6772162637905,31.8840660489106,
0.));
#149731=CARTESIAN_POINT('Ctrl Pts',(-64.6605368598631,31.8665195761311,
0.));
#149732=CARTESIAN_POINT('Ctrl Pts',(-64.6438693278718,31.849019698125,0.));
#149733=CARTESIAN_POINT('Ctrl Pts',(-64.627213792563,31.8315664585027,0.));
#149734=CARTESIAN_POINT('Ctrl Pts',(-64.6105703792312,31.8141599009684,
0.));
#149735=CARTESIAN_POINT('Ctrl Pts',(-64.5939392137233,31.7968000693218,
0.));
#149736=CARTESIAN_POINT('Ctrl Pts',(-64.5773204224429,31.7794870074583,
0.));
#149737=CARTESIAN_POINT('Ctrl Pts',(-64.5607141323527,31.7622207593637,
0.));
#149738=CARTESIAN_POINT('Ctrl Pts',(-64.544120470978,31.7450013691116,0.));
#149739=CARTESIAN_POINT('Ctrl Pts',(-64.5275395664134,31.7278288808736,
0.));
#149740=CARTESIAN_POINT('Ctrl Pts',(-64.5109715473277,31.7107033389204,
0.));
#149741=CARTESIAN_POINT('Ctrl Pts',(-64.4944165429672,31.6936247876228,
0.));
#149742=CARTESIAN_POINT('Ctrl Pts',(-64.4778746831598,31.6765932714456,
0.));
#149743=CARTESIAN_POINT('Ctrl Pts',(-64.4613460983186,31.6596088349468,
0.));
#149744=CARTESIAN_POINT('Ctrl Pts',(-64.4448309194499,31.6426715227865,
0.));
#149745=CARTESIAN_POINT('Ctrl Pts',(-64.4283292781553,31.6257813797281,
0.));
#149746=CARTESIAN_POINT('Ctrl Pts',(-64.4118413066386,31.6089384506399,
0.));
#149747=CARTESIAN_POINT('Ctrl Pts',(-64.3953671377071,31.5921427804879,
0.));
#149748=CARTESIAN_POINT('Ctrl Pts',(-64.3789069047768,31.5753944143355,
0.));
#149749=CARTESIAN_POINT('Ctrl Pts',(-64.3624607418798,31.5586933973531,
0.));
#149750=CARTESIAN_POINT('Ctrl Pts',(-64.34602878367,31.5420397748198,0.));
#149751=CARTESIAN_POINT('Ctrl Pts',(-64.3296111654273,31.5254335921239,
0.));
#149752=CARTESIAN_POINT('Ctrl Pts',(-64.3132080230603,31.5088748947564,
0.));
#149753=CARTESIAN_POINT('Ctrl Pts',(-64.2968194931113,31.4923637283109,
0.));
#149754=CARTESIAN_POINT('Ctrl Pts',(-64.2804457127633,31.4759001384922,
0.));
#149755=CARTESIAN_POINT('Ctrl Pts',(-64.264086819846,31.4594841711188,0.));
#149756=CARTESIAN_POINT('Ctrl Pts',(-64.2477429528408,31.4431158721229,
0.));
#149757=CARTESIAN_POINT('Ctrl Pts',(-64.2314142508843,31.4267952875439,
0.));
#149758=CARTESIAN_POINT('Ctrl Pts',(-64.2151008537733,31.4105224635298,
0.));
#149759=CARTESIAN_POINT('Ctrl Pts',(-64.1988029019733,31.3942974463458,
0.));
#149760=CARTESIAN_POINT('Ctrl Pts',(-64.1825205366231,31.3781202823758,
0.));
#149761=CARTESIAN_POINT('Ctrl Pts',(-64.1662538995407,31.3619910181222,
0.));
#149762=CARTESIAN_POINT('Ctrl Pts',(-64.150003133226,31.3459097001995,0.));
#149763=CARTESIAN_POINT('Ctrl Pts',(-64.1337683808667,31.3298763753366,
0.));
#149764=CARTESIAN_POINT('Ctrl Pts',(-64.1175497863475,31.3138910903852,
0.));
#149765=CARTESIAN_POINT('Ctrl Pts',(-64.1013474942554,31.2979538923213,
0.));
#149766=CARTESIAN_POINT('Ctrl Pts',(-64.0851616498861,31.2820648282451,
0.));
#149767=CARTESIAN_POINT('Ctrl Pts',(-64.0689923992475,31.2662239453734,
0.));
#149768=CARTESIAN_POINT('Ctrl Pts',(-64.0528398890671,31.2504312910457,
0.));
#149769=CARTESIAN_POINT('Ctrl Pts',(-64.036704266799,31.23468691273,0.));
#149770=CARTESIAN_POINT('Ctrl Pts',(-64.0205856806298,31.2189908580245,
0.));
#149771=CARTESIAN_POINT('Ctrl Pts',(-64.004484279483,31.2033431746558,0.));
#149772=CARTESIAN_POINT('Ctrl Pts',(-63.9884002130209,31.1877439104717,
0.));
#149773=CARTESIAN_POINT('Ctrl Pts',(-63.972333631655,31.1721931134488,0.));
#149774=CARTESIAN_POINT('Ctrl Pts',(-63.9562846865566,31.1566908316992,
0.));
#149775=CARTESIAN_POINT('Ctrl Pts',(-63.9402535296651,31.1412371134727,
0.));
#149776=CARTESIAN_POINT('Ctrl Pts',(-63.9242403136955,31.1258320071545,
0.));
#149777=CARTESIAN_POINT('Ctrl Pts',(-63.9082451921447,31.1104755612606,
0.));
#149778=CARTESIAN_POINT('Ctrl Pts',(-63.8922683192963,31.0951678244454,
0.));
#149779=CARTESIAN_POINT('Ctrl Pts',(-63.8763098502235,31.079908845504,0.));
#149780=CARTESIAN_POINT('Ctrl Pts',(-63.8603699407922,31.0646986733723,
0.));
#149781=CARTESIAN_POINT('Ctrl Pts',(-63.8444487476615,31.0495373571217,
0.));
#149782=CARTESIAN_POINT('Ctrl Pts',(-63.8285464282857,31.0344249459544,
0.));
#149783=CARTESIAN_POINT('Ctrl Pts',(-63.8126631409376,31.0193614892177,
0.));
#149784=CARTESIAN_POINT('Ctrl Pts',(-63.7967990447288,31.0043470364112,
0.));
#149785=CARTESIAN_POINT('Ctrl Pts',(-63.7809542996258,30.9893816371907,
0.));
#149786=CARTESIAN_POINT('Ctrl Pts',(-63.7651290664713,30.9744653413679,
0.));
#149787=CARTESIAN_POINT('Ctrl Pts',(-63.7493235069844,30.9595981989091,
0.));
#149788=CARTESIAN_POINT('Ctrl Pts',(-63.733537783742,30.9447802599345,0.));
#149789=CARTESIAN_POINT('Ctrl Pts',(-63.7177720601604,30.9300115747113,
0.));
#149790=CARTESIAN_POINT('Ctrl Pts',(-63.7020265004805,30.9152921936471,
0.));
#149791=CARTESIAN_POINT('Ctrl Pts',(-63.6863012697354,30.9006221672703,
0.));
#149792=CARTESIAN_POINT('Ctrl Pts',(-63.6705965337996,30.8860015462488,
0.));
#149793=CARTESIAN_POINT('Ctrl Pts',(-63.6549124594681,30.8714303814202,
0.));
#149794=CARTESIAN_POINT('Ctrl Pts',(-63.6392492145233,30.8569087238131,
0.));
#149795=CARTESIAN_POINT('Ctrl Pts',(-63.6236069678041,30.8424366246665,
0.));
#149796=CARTESIAN_POINT('Ctrl Pts',(-63.6079858892747,30.8280141354447,
0.));
#149797=CARTESIAN_POINT('Ctrl Pts',(-63.5923861498964,30.8136413077999,
0.));
#149798=CARTESIAN_POINT('Ctrl Pts',(-63.5768079214868,30.7993181935265,
0.));
#149799=CARTESIAN_POINT('Ctrl Pts',(-63.5612513766005,30.7850448445207,
0.));
#149800=CARTESIAN_POINT('Ctrl Pts',(-63.5457166883558,30.7708213127169,
0.));
#149801=CARTESIAN_POINT('Ctrl Pts',(-63.5302040304174,30.7566476500772,
0.));
#149802=CARTESIAN_POINT('Ctrl Pts',(-63.514713577392,30.7425239087294,0.));
#149803=CARTESIAN_POINT('Ctrl Pts',(-63.4992455051805,30.7284501410827,
0.));
#149804=CARTESIAN_POINT('Ctrl Pts',(-63.4837999912759,30.7144263999259,
0.));
#149805=CARTESIAN_POINT('Ctrl Pts',(-63.4683772152497,30.7004527385806,
0.));
#149806=CARTESIAN_POINT('Ctrl Pts',(-63.4529773584211,30.686529210791,0.));
#149807=CARTESIAN_POINT('Ctrl Pts',(-63.4376006029575,30.6726558704301,
0.));
#149808=CARTESIAN_POINT('Ctrl Pts',(-63.4222471311236,30.6588327712482,
0.));
#149809=CARTESIAN_POINT('Ctrl Pts',(-63.4069171245094,30.6450599666134,
0.));
#149810=CARTESIAN_POINT('Ctrl Pts',(-63.3916107631421,30.6313375092084,
0.));
#149811=CARTESIAN_POINT('Ctrl Pts',(-63.3763282271838,30.6176654515988,
0.));
#149812=CARTESIAN_POINT('Ctrl Pts',(-63.3610696989599,30.6040438469089,
0.));
#149813=CARTESIAN_POINT('Ctrl Pts',(-63.3458353646145,30.5904727493707,
0.));
#149814=CARTESIAN_POINT('Ctrl Pts',(-63.330625416509,30.5769522151147,0.));
#149815=CARTESIAN_POINT('Ctrl Pts',(-63.315440053435,30.5634823022357,0.));
#149816=CARTESIAN_POINT('Ctrl Pts',(-63.300279475605,30.5500630691342,0.));
#149817=CARTESIAN_POINT('Ctrl Pts',(-63.2851438802462,30.5366945730503,
0.));
#149818=CARTESIAN_POINT('Ctrl Pts',(-63.2700334577661,30.5233768687875,
0.));
#149819=CARTESIAN_POINT('Ctrl Pts',(-63.2549483856268,30.5101100066683,
0.));
#149820=CARTESIAN_POINT('Ctrl Pts',(-63.2398888342612,30.4968940345027,
0.));
#149821=CARTESIAN_POINT('Ctrl Pts',(-63.2248549788272,30.4837290015011,
0.));
#149822=CARTESIAN_POINT('Ctrl Pts',(-63.2098470086636,30.470614961416,0.));
#149823=CARTESIAN_POINT('Ctrl Pts',(-63.1948651386868,30.4575519763305,
0.));
#149824=CARTESIAN_POINT('Ctrl Pts',(-63.1799096171757,30.4445401192324,
0.));
#149825=CARTESIAN_POINT('Ctrl Pts',(-63.1649807016766,30.431579465967,0.));
#149826=CARTESIAN_POINT('Ctrl Pts',(-63.1500786361382,30.4186700875598,
0.));
#149827=CARTESIAN_POINT('Ctrl Pts',(-63.1352036298512,30.4058120432259,
0.));
#149828=CARTESIAN_POINT('Ctrl Pts',(-63.1203558300911,30.3930053710592,
0.));
#149829=CARTESIAN_POINT('Ctrl Pts',(-63.1055353202641,30.3802500880564,
0.));
#149830=CARTESIAN_POINT('Ctrl Pts',(-63.0937007763826,30.3700869762658,
0.));
#149831=CARTESIAN_POINT('Ctrl Pts',(-63.0848371718274,30.3624877680747,
0.));
#149832=CARTESIAN_POINT('Ctrl Pts',(-63.0789335700774,30.3574319069365,
0.));
#149833=CARTESIAN_POINT('Ctrl Pts',(-63.0759831361898,30.3549065457811,
0.));
#149834=CARTESIAN_POINT('Ctrl Pts',(-63.1661434108059,39.5004851439258,
0.));
#149835=CARTESIAN_POINT('Ctrl Pts',(-63.1661434108059,39.5004851439258,
12.));
#149836=CARTESIAN_POINT('Ctrl Pts',(-63.1630766582788,39.4958045828135,
0.));
#149837=CARTESIAN_POINT('Ctrl Pts',(-63.1630766582788,39.4958045828135,
12.));
#149838=CARTESIAN_POINT('Ctrl Pts',(-63.1569429707875,39.4864477303823,
0.));
#149839=CARTESIAN_POINT('Ctrl Pts',(-63.1569429707875,39.4864477303823,
12.));
#149840=CARTESIAN_POINT('Ctrl Pts',(-63.1477418922406,39.4724252611155,
0.));
#149841=CARTESIAN_POINT('Ctrl Pts',(-63.1477418922406,39.4724252611155,
12.));
#149842=CARTESIAN_POINT('Ctrl Pts',(-63.1354726928398,39.4537542552268,
0.));
#149843=CARTESIAN_POINT('Ctrl Pts',(-63.1354726928398,39.4537542552268,
12.));
#149844=CARTESIAN_POINT('Ctrl Pts',(-63.1201343731172,39.4304582059864,
0.));
#149845=CARTESIAN_POINT('Ctrl Pts',(-63.1201343731172,39.4304582059864,
12.));
#149846=CARTESIAN_POINT('Ctrl Pts',(-63.10479424519,39.4072048797616,0.));
#149847=CARTESIAN_POINT('Ctrl Pts',(-63.10479424519,39.4072048797616,12.));
#149848=CARTESIAN_POINT('Ctrl Pts',(-63.0894523341314,39.383994298574,0.));
#149849=CARTESIAN_POINT('Ctrl Pts',(-63.0894523341314,39.383994298574,12.));
#149850=CARTESIAN_POINT('Ctrl Pts',(-63.0741086815841,39.3608264920409,
0.));
#149851=CARTESIAN_POINT('Ctrl Pts',(-63.0741086815841,39.3608264920409,
12.));
#149852=CARTESIAN_POINT('Ctrl Pts',(-63.0587633513774,39.3377014983609,
0.));
#149853=CARTESIAN_POINT('Ctrl Pts',(-63.0587633513774,39.3377014983609,
12.));
#149854=CARTESIAN_POINT('Ctrl Pts',(-63.0434164277992,39.3146193632392,
0.));
#149855=CARTESIAN_POINT('Ctrl Pts',(-63.0434164277992,39.3146193632392,
12.));
#149856=CARTESIAN_POINT('Ctrl Pts',(-63.0280680082353,39.2915801372354,
0.));
#149857=CARTESIAN_POINT('Ctrl Pts',(-63.0280680082353,39.2915801372354,
12.));
#149858=CARTESIAN_POINT('Ctrl Pts',(-63.0127181973628,39.2685838735361,
0.));
#149859=CARTESIAN_POINT('Ctrl Pts',(-63.0127181973628,39.2685838735361,
12.));
#149860=CARTESIAN_POINT('Ctrl Pts',(-62.9973671008703,39.2456306256104,
0.));
#149861=CARTESIAN_POINT('Ctrl Pts',(-62.9973671008703,39.2456306256104,
12.));
#149862=CARTESIAN_POINT('Ctrl Pts',(-62.9820148189929,39.2227204447638,
0.));
#149863=CARTESIAN_POINT('Ctrl Pts',(-62.9820148189929,39.2227204447638,
12.));
#149864=CARTESIAN_POINT('Ctrl Pts',(-62.9666614412731,39.1998533781661,
0.));
#149865=CARTESIAN_POINT('Ctrl Pts',(-62.9666614412731,39.1998533781661,
12.));
#149866=CARTESIAN_POINT('Ctrl Pts',(-62.9513070501867,39.1770294702428,
0.));
#149867=CARTESIAN_POINT('Ctrl Pts',(-62.9513070501867,39.1770294702428,
12.));
#149868=CARTESIAN_POINT('Ctrl Pts',(-62.9359517237404,39.1542487636744,
0.));
#149869=CARTESIAN_POINT('Ctrl Pts',(-62.9359517237404,39.1542487636744,
12.));
#149870=CARTESIAN_POINT('Ctrl Pts',(-62.9205955385558,39.131511300575,0.));
#149871=CARTESIAN_POINT('Ctrl Pts',(-62.9205955385558,39.131511300575,12.));
#149872=CARTESIAN_POINT('Ctrl Pts',(-62.9052385725387,39.1088171235125,
0.));
#149873=CARTESIAN_POINT('Ctrl Pts',(-62.9052385725387,39.1088171235125,
12.));
#149874=CARTESIAN_POINT('Ctrl Pts',(-62.8898809082612,39.0861662767932,
0.));
#149875=CARTESIAN_POINT('Ctrl Pts',(-62.8898809082612,39.0861662767932,
12.));
#149876=CARTESIAN_POINT('Ctrl Pts',(-62.8745226325998,39.0635588063276,
0.));
#149877=CARTESIAN_POINT('Ctrl Pts',(-62.8745226325998,39.0635588063276,
12.));
#149878=CARTESIAN_POINT('Ctrl Pts',(-62.8591638352056,39.0409947590497,
0.));
#149879=CARTESIAN_POINT('Ctrl Pts',(-62.8591638352056,39.0409947590497,
12.));
#149880=CARTESIAN_POINT('Ctrl Pts',(-62.8438046073224,39.0184741824641,
0.));
#149881=CARTESIAN_POINT('Ctrl Pts',(-62.8438046073224,39.0184741824641,
12.));
#149882=CARTESIAN_POINT('Ctrl Pts',(-62.8284450405459,38.9959971241701,
0.));
#149883=CARTESIAN_POINT('Ctrl Pts',(-62.8284450405459,38.9959971241701,
12.));
#149884=CARTESIAN_POINT('Ctrl Pts',(-62.8130852254027,38.9735636313089,
0.));
#149885=CARTESIAN_POINT('Ctrl Pts',(-62.8130852254027,38.9735636313089,
12.));
#149886=CARTESIAN_POINT('Ctrl Pts',(-62.7977252507118,38.9511737503165,
0.));
#149887=CARTESIAN_POINT('Ctrl Pts',(-62.7977252507118,38.9511737503165,
12.));
#149888=CARTESIAN_POINT('Ctrl Pts',(-62.78236520437,38.9288275272335,0.));
#149889=CARTESIAN_POINT('Ctrl Pts',(-62.78236520437,38.9288275272335,12.));
#149890=CARTESIAN_POINT('Ctrl Pts',(-62.7670051738143,38.9065250078832,
0.));
#149891=CARTESIAN_POINT('Ctrl Pts',(-62.7670051738143,38.9065250078832,
12.));
#149892=CARTESIAN_POINT('Ctrl Pts',(-62.7516452466128,38.8842662380984,
0.));
#149893=CARTESIAN_POINT('Ctrl Pts',(-62.7516452466128,38.8842662380984,
12.));
#149894=CARTESIAN_POINT('Ctrl Pts',(-62.7362855110042,38.8620512639232,
0.));
#149895=CARTESIAN_POINT('Ctrl Pts',(-62.7362855110042,38.8620512639232,
12.));
#149896=CARTESIAN_POINT('Ctrl Pts',(-62.7209260564493,38.8398801318177,
0.));
#149897=CARTESIAN_POINT('Ctrl Pts',(-62.7209260564493,38.8398801318177,
12.));
#149898=CARTESIAN_POINT('Ctrl Pts',(-62.7055669733802,38.8177528885681,
0.));
#149899=CARTESIAN_POINT('Ctrl Pts',(-62.7055669733802,38.8177528885681,
12.));
#149900=CARTESIAN_POINT('Ctrl Pts',(-62.6902083529694,38.795669581203,0.));
#149901=CARTESIAN_POINT('Ctrl Pts',(-62.6902083529694,38.795669581203,12.));
#149902=CARTESIAN_POINT('Ctrl Pts',(-62.6748502868835,38.7736302568982,
0.));
#149903=CARTESIAN_POINT('Ctrl Pts',(-62.6748502868835,38.7736302568982,
12.));
#149904=CARTESIAN_POINT('Ctrl Pts',(-62.6594928670628,38.7516349628904,
0.));
#149905=CARTESIAN_POINT('Ctrl Pts',(-62.6594928670628,38.7516349628904,
12.));
#149906=CARTESIAN_POINT('Ctrl Pts',(-62.6441361854411,38.7296837463609,
0.));
#149907=CARTESIAN_POINT('Ctrl Pts',(-62.6441361854411,38.7296837463609,
12.));
#149908=CARTESIAN_POINT('Ctrl Pts',(-62.6287803339542,38.7077766544416,
0.));
#149909=CARTESIAN_POINT('Ctrl Pts',(-62.6287803339542,38.7077766544416,
12.));
#149910=CARTESIAN_POINT('Ctrl Pts',(-62.6134254046739,38.6859137342731,
0.));
#149911=CARTESIAN_POINT('Ctrl Pts',(-62.6134254046739,38.6859137342731,
12.));
#149912=CARTESIAN_POINT('Ctrl Pts',(-62.5980714899052,38.6640950330421,
0.));
#149913=CARTESIAN_POINT('Ctrl Pts',(-62.5980714899052,38.6640950330421,
12.));
#149914=CARTESIAN_POINT('Ctrl Pts',(-62.5827186822921,38.6423205980213,
0.));
#149915=CARTESIAN_POINT('Ctrl Pts',(-62.5827186822921,38.6423205980213,
12.));
#149916=CARTESIAN_POINT('Ctrl Pts',(-62.5673670749361,38.6205904766073,
0.));
#149917=CARTESIAN_POINT('Ctrl Pts',(-62.5673670749361,38.6205904766073,
12.));
#149918=CARTESIAN_POINT('Ctrl Pts',(-62.5520167614516,38.5989047163393,
0.));
#149919=CARTESIAN_POINT('Ctrl Pts',(-62.5520167614516,38.5989047163393,
12.));
#149920=CARTESIAN_POINT('Ctrl Pts',(-62.5366678359023,38.5772633648832,
0.));
#149921=CARTESIAN_POINT('Ctrl Pts',(-62.5366678359023,38.5772633648832,
12.));
#149922=CARTESIAN_POINT('Ctrl Pts',(-62.5213203927663,38.5556664700195,
0.));
#149923=CARTESIAN_POINT('Ctrl Pts',(-62.5213203927663,38.5556664700195,
12.));
#149924=CARTESIAN_POINT('Ctrl Pts',(-62.5059745268901,38.5341140796248,
0.));
#149925=CARTESIAN_POINT('Ctrl Pts',(-62.5059745268901,38.5341140796248,
12.));
#149926=CARTESIAN_POINT('Ctrl Pts',(-62.4906303334443,38.5126062416502,
0.));
#149927=CARTESIAN_POINT('Ctrl Pts',(-62.4906303334443,38.5126062416502,
12.));
#149928=CARTESIAN_POINT('Ctrl Pts',(-62.4752879078854,38.4911430040997,
0.));
#149929=CARTESIAN_POINT('Ctrl Pts',(-62.4752879078854,38.4911430040997,
12.));
#149930=CARTESIAN_POINT('Ctrl Pts',(-62.4599473459811,38.4697244150482,
0.));
#149931=CARTESIAN_POINT('Ctrl Pts',(-62.4599473459811,38.4697244150482,
12.));
#149932=CARTESIAN_POINT('Ctrl Pts',(-62.4446087438312,38.4483505226518,
0.));
#149933=CARTESIAN_POINT('Ctrl Pts',(-62.4446087438312,38.4483505226518,
12.));
#149934=CARTESIAN_POINT('Ctrl Pts',(-62.4292721978901,38.4270213751568,
0.));
#149935=CARTESIAN_POINT('Ctrl Pts',(-62.4292721978901,38.4270213751568,
12.));
#149936=CARTESIAN_POINT('Ctrl Pts',(-62.4139378049885,38.405737020905,0.));
#149937=CARTESIAN_POINT('Ctrl Pts',(-62.4139378049885,38.405737020905,12.));
#149938=CARTESIAN_POINT('Ctrl Pts',(-62.3986056623577,38.3844975083343,
0.));
#149939=CARTESIAN_POINT('Ctrl Pts',(-62.3986056623577,38.3844975083343,
12.));
#149940=CARTESIAN_POINT('Ctrl Pts',(-62.3832758676271,38.3633028859828,
0.));
#149941=CARTESIAN_POINT('Ctrl Pts',(-62.3832758676271,38.3633028859828,
12.));
#149942=CARTESIAN_POINT('Ctrl Pts',(-62.3679485188172,38.342153202491,0.));
#149943=CARTESIAN_POINT('Ctrl Pts',(-62.3679485188172,38.342153202491,12.));
#149944=CARTESIAN_POINT('Ctrl Pts',(-62.3526237143336,38.3210485066001,
0.));
#149945=CARTESIAN_POINT('Ctrl Pts',(-62.3526237143336,38.3210485066001,
12.));
#149946=CARTESIAN_POINT('Ctrl Pts',(-62.3373015529613,38.2999888471476,
0.));
#149947=CARTESIAN_POINT('Ctrl Pts',(-62.3373015529613,38.2999888471476,
12.));
#149948=CARTESIAN_POINT('Ctrl Pts',(-62.3219821338569,38.2789742730564,
0.));
#149949=CARTESIAN_POINT('Ctrl Pts',(-62.3219821338569,38.2789742730564,
12.));
#149950=CARTESIAN_POINT('Ctrl Pts',(-62.3066655565503,38.2580048333361,
0.));
#149951=CARTESIAN_POINT('Ctrl Pts',(-62.3066655565503,38.2580048333361,
12.));
#149952=CARTESIAN_POINT('Ctrl Pts',(-62.2913519209521,38.2370805770935,
0.));
#149953=CARTESIAN_POINT('Ctrl Pts',(-62.2913519209521,38.2370805770935,
12.));
#149954=CARTESIAN_POINT('Ctrl Pts',(-62.2760413273602,38.2162015535353,
0.));
#149955=CARTESIAN_POINT('Ctrl Pts',(-62.2760413273602,38.2162015535353,
12.));
#149956=CARTESIAN_POINT('Ctrl Pts',(-62.2607338764654,38.1953678119691,
0.));
#149957=CARTESIAN_POINT('Ctrl Pts',(-62.2607338764654,38.1953678119691,
12.));
#149958=CARTESIAN_POINT('Ctrl Pts',(-62.245429669358,38.1745794017996,0.));
#149959=CARTESIAN_POINT('Ctrl Pts',(-62.245429669358,38.1745794017996,12.));
#149960=CARTESIAN_POINT('Ctrl Pts',(-62.2301288075321,38.1538363725264,
0.));
#149961=CARTESIAN_POINT('Ctrl Pts',(-62.2301288075321,38.1538363725264,
12.));
#149962=CARTESIAN_POINT('Ctrl Pts',(-62.2148313928863,38.133138773753,0.));
#149963=CARTESIAN_POINT('Ctrl Pts',(-62.2148313928863,38.133138773753,12.));
#149964=CARTESIAN_POINT('Ctrl Pts',(-62.1995375277257,38.1124866551886,
0.));
#149965=CARTESIAN_POINT('Ctrl Pts',(-62.1995375277257,38.1124866551886,
12.));
#149966=CARTESIAN_POINT('Ctrl Pts',(-62.1842473147626,38.0918800666479,
0.));
#149967=CARTESIAN_POINT('Ctrl Pts',(-62.1842473147626,38.0918800666479,
12.));
#149968=CARTESIAN_POINT('Ctrl Pts',(-62.1689608571176,38.0713190580463,
0.));
#149969=CARTESIAN_POINT('Ctrl Pts',(-62.1689608571176,38.0713190580463,
12.));
#149970=CARTESIAN_POINT('Ctrl Pts',(-62.1536782583199,38.0508036793939,
0.));
#149971=CARTESIAN_POINT('Ctrl Pts',(-62.1536782583199,38.0508036793939,
12.));
#149972=CARTESIAN_POINT('Ctrl Pts',(-62.1383996223125,38.0303339808053,
0.));
#149973=CARTESIAN_POINT('Ctrl Pts',(-62.1383996223125,38.0303339808053,
12.));
#149974=CARTESIAN_POINT('Ctrl Pts',(-62.123125053455,38.0099100125037,0.));
#149975=CARTESIAN_POINT('Ctrl Pts',(-62.123125053455,38.0099100125037,12.));
#149976=CARTESIAN_POINT('Ctrl Pts',(-62.107854656528,37.9895318248212,0.));
#149977=CARTESIAN_POINT('Ctrl Pts',(-62.107854656528,37.9895318248212,12.));
#149978=CARTESIAN_POINT('Ctrl Pts',(-62.0925885367352,37.9691994681966,
0.));
#149979=CARTESIAN_POINT('Ctrl Pts',(-62.0925885367352,37.9691994681966,
12.));
#149980=CARTESIAN_POINT('Ctrl Pts',(-62.0773267997079,37.9489129931689,
0.));
#149981=CARTESIAN_POINT('Ctrl Pts',(-62.0773267997079,37.9489129931689,
12.));
#149982=CARTESIAN_POINT('Ctrl Pts',(-62.0620695515074,37.9286724503851,
0.));
#149983=CARTESIAN_POINT('Ctrl Pts',(-62.0620695515074,37.9286724503851,
12.));
#149984=CARTESIAN_POINT('Ctrl Pts',(-62.0468168986288,37.9084778906053,
0.));
#149985=CARTESIAN_POINT('Ctrl Pts',(-62.0468168986288,37.9084778906053,
12.));
#149986=CARTESIAN_POINT('Ctrl Pts',(-62.031568948002,37.8883293647029,0.));
#149987=CARTESIAN_POINT('Ctrl Pts',(-62.031568948002,37.8883293647029,12.));
#149988=CARTESIAN_POINT('Ctrl Pts',(-62.0163258069957,37.868226923663,0.));
#149989=CARTESIAN_POINT('Ctrl Pts',(-62.0163258069957,37.868226923663,12.));
#149990=CARTESIAN_POINT('Ctrl Pts',(-62.0010875834187,37.8481706185749,
0.));
#149991=CARTESIAN_POINT('Ctrl Pts',(-62.0010875834187,37.8481706185749,
12.));
#149992=CARTESIAN_POINT('Ctrl Pts',(-61.9858543855236,37.828160500638,0.));
#149993=CARTESIAN_POINT('Ctrl Pts',(-61.9858543855236,37.828160500638,12.));
#149994=CARTESIAN_POINT('Ctrl Pts',(-61.9706263220114,37.8081966211689,
0.));
#149995=CARTESIAN_POINT('Ctrl Pts',(-61.9706263220114,37.8081966211689,
12.));
#149996=CARTESIAN_POINT('Ctrl Pts',(-61.9554035020338,37.7882790316014,
0.));
#149997=CARTESIAN_POINT('Ctrl Pts',(-61.9554035020338,37.7882790316014,
12.));
#149998=CARTESIAN_POINT('Ctrl Pts',(-61.9401860351972,37.7684077834872,
0.));
#149999=CARTESIAN_POINT('Ctrl Pts',(-61.9401860351972,37.7684077834872,
12.));
#150000=CARTESIAN_POINT('Ctrl Pts',(-61.9249740315649,37.7485829284871,
0.));
#150001=CARTESIAN_POINT('Ctrl Pts',(-61.9249740315649,37.7485829284871,
12.));
#150002=CARTESIAN_POINT('Ctrl Pts',(-61.9097676016601,37.7288045183756,
0.));
#150003=CARTESIAN_POINT('Ctrl Pts',(-61.9097676016601,37.7288045183756,
12.));
#150004=CARTESIAN_POINT('Ctrl Pts',(-61.8945668564704,37.7090726050482,
0.));
#150005=CARTESIAN_POINT('Ctrl Pts',(-61.8945668564704,37.7090726050482,
12.));
#150006=CARTESIAN_POINT('Ctrl Pts',(-61.8793719074507,37.6893872405228,
0.));
#150007=CARTESIAN_POINT('Ctrl Pts',(-61.8793719074507,37.6893872405228,
12.));
#150008=CARTESIAN_POINT('Ctrl Pts',(-61.8641828665261,37.6697484769392,
0.));
#150009=CARTESIAN_POINT('Ctrl Pts',(-61.8641828665261,37.6697484769392,
12.));
#150010=CARTESIAN_POINT('Ctrl Pts',(-61.8489998460957,37.6501563665523,
0.));
#150011=CARTESIAN_POINT('Ctrl Pts',(-61.8489998460957,37.6501563665523,
12.));
#150012=CARTESIAN_POINT('Ctrl Pts',(-61.8338229590353,37.6306109617346,
0.));
#150013=CARTESIAN_POINT('Ctrl Pts',(-61.8338229590353,37.6306109617346,
12.));
#150014=CARTESIAN_POINT('Ctrl Pts',(-61.8186523187015,37.6111123149839,
0.));
#150015=CARTESIAN_POINT('Ctrl Pts',(-61.8186523187015,37.6111123149839,
12.));
#150016=CARTESIAN_POINT('Ctrl Pts',(-61.8034880389362,37.5916604789253,
0.));
#150017=CARTESIAN_POINT('Ctrl Pts',(-61.8034880389362,37.5916604789253,
12.));
#150018=CARTESIAN_POINT('Ctrl Pts',(-61.7883302340687,37.5722555063111,
0.));
#150019=CARTESIAN_POINT('Ctrl Pts',(-61.7883302340687,37.5722555063111,
12.));
#150020=CARTESIAN_POINT('Ctrl Pts',(-61.7731790189191,37.5528974500142,
0.));
#150021=CARTESIAN_POINT('Ctrl Pts',(-61.7731790189191,37.5528974500142,
12.));
#150022=CARTESIAN_POINT('Ctrl Pts',(-61.7580345088016,37.5335863630287,
0.));
#150023=CARTESIAN_POINT('Ctrl Pts',(-61.7580345088016,37.5335863630287,
12.));
#150024=CARTESIAN_POINT('Ctrl Pts',(-61.7428968195299,37.5143222984796,
0.));
#150025=CARTESIAN_POINT('Ctrl Pts',(-61.7428968195299,37.5143222984796,
12.));
#150026=CARTESIAN_POINT('Ctrl Pts',(-61.7277660674205,37.4951053096237,
0.));
#150027=CARTESIAN_POINT('Ctrl Pts',(-61.7277660674205,37.4951053096237,
12.));
#150028=CARTESIAN_POINT('Ctrl Pts',(-61.7126423692963,37.4759354498509,
0.));
#150029=CARTESIAN_POINT('Ctrl Pts',(-61.7126423692963,37.4759354498509,
12.));
#150030=CARTESIAN_POINT('Ctrl Pts',(-61.6975258424894,37.4568127726773,
0.));
#150031=CARTESIAN_POINT('Ctrl Pts',(-61.6975258424894,37.4568127726773,
12.));
#150032=CARTESIAN_POINT('Ctrl Pts',(-61.6824166048444,37.4377373317451,
0.));
#150033=CARTESIAN_POINT('Ctrl Pts',(-61.6824166048444,37.4377373317451,
12.));
#150034=CARTESIAN_POINT('Ctrl Pts',(-61.6673147747242,37.4187091808321,
0.));
#150035=CARTESIAN_POINT('Ctrl Pts',(-61.6673147747242,37.4187091808321,
12.));
#150036=CARTESIAN_POINT('Ctrl Pts',(-61.6522204710131,37.3997283738533,
0.));
#150037=CARTESIAN_POINT('Ctrl Pts',(-61.6522204710131,37.3997283738533,
12.));
#150038=CARTESIAN_POINT('Ctrl Pts',(-61.637133813121,37.3807949648624,0.));
#150039=CARTESIAN_POINT('Ctrl Pts',(-61.637133813121,37.3807949648624,12.));
#150040=CARTESIAN_POINT('Ctrl Pts',(-61.6220549209866,37.361909008045,0.));
#150041=CARTESIAN_POINT('Ctrl Pts',(-61.6220549209866,37.361909008045,12.));
#150042=CARTESIAN_POINT('Ctrl Pts',(-61.6069839150807,37.343070557718,0.));
#150043=CARTESIAN_POINT('Ctrl Pts',(-61.6069839150807,37.343070557718,12.));
#150044=CARTESIAN_POINT('Ctrl Pts',(-61.591920916412,37.3242796683395,0.));
#150045=CARTESIAN_POINT('Ctrl Pts',(-61.591920916412,37.3242796683395,12.));
#150046=CARTESIAN_POINT('Ctrl Pts',(-61.5768660465311,37.3055363945107,
0.));
#150047=CARTESIAN_POINT('Ctrl Pts',(-61.5768660465311,37.3055363945107,
12.));
#150048=CARTESIAN_POINT('Ctrl Pts',(-61.5618194275348,37.286840790977,0.));
#150049=CARTESIAN_POINT('Ctrl Pts',(-61.5618194275348,37.286840790977,12.));
#150050=CARTESIAN_POINT('Ctrl Pts',(-61.5467811820691,37.2681929126221,
0.));
#150051=CARTESIAN_POINT('Ctrl Pts',(-61.5467811820691,37.2681929126221,
12.));
#150052=CARTESIAN_POINT('Ctrl Pts',(-61.5317514333328,37.2495928144667,
0.));
#150053=CARTESIAN_POINT('Ctrl Pts',(-61.5317514333328,37.2495928144667,
12.));
#150054=CARTESIAN_POINT('Ctrl Pts',(-61.5167303050832,37.2310405516781,
0.));
#150055=CARTESIAN_POINT('Ctrl Pts',(-61.5167303050832,37.2310405516781,
12.));
#150056=CARTESIAN_POINT('Ctrl Pts',(-61.501717921641,37.2125361795731,0.));
#150057=CARTESIAN_POINT('Ctrl Pts',(-61.501717921641,37.2125361795731,12.));
#150058=CARTESIAN_POINT('Ctrl Pts',(-61.4867144078936,37.1940797536181,
0.));
#150059=CARTESIAN_POINT('Ctrl Pts',(-61.4867144078936,37.1940797536181,
12.));
#150060=CARTESIAN_POINT('Ctrl Pts',(-61.4717198892994,37.175671329424,0.));
#150061=CARTESIAN_POINT('Ctrl Pts',(-61.4717198892994,37.175671329424,12.));
#150062=CARTESIAN_POINT('Ctrl Pts',(-61.4567344918919,37.1573109627454,
0.));
#150063=CARTESIAN_POINT('Ctrl Pts',(-61.4567344918919,37.1573109627454,
12.));
#150064=CARTESIAN_POINT('Ctrl Pts',(-61.4417583422863,37.1389987094905,
0.));
#150065=CARTESIAN_POINT('Ctrl Pts',(-61.4417583422863,37.1389987094905,
12.));
#150066=CARTESIAN_POINT('Ctrl Pts',(-61.4267915676822,37.1207346257222,
0.));
#150067=CARTESIAN_POINT('Ctrl Pts',(-61.4267915676822,37.1207346257222,
12.));
#150068=CARTESIAN_POINT('Ctrl Pts',(-61.4118342958697,37.1025187676602,
0.));
#150069=CARTESIAN_POINT('Ctrl Pts',(-61.4118342958697,37.1025187676602,
12.));
#150070=CARTESIAN_POINT('Ctrl Pts',(-61.3968866552317,37.0843511916745,
0.));
#150071=CARTESIAN_POINT('Ctrl Pts',(-61.3968866552317,37.0843511916745,
12.));
#150072=CARTESIAN_POINT('Ctrl Pts',(-61.381948774749,37.0662319542849,0.));
#150073=CARTESIAN_POINT('Ctrl Pts',(-61.381948774749,37.0662319542849,12.));
#150074=CARTESIAN_POINT('Ctrl Pts',(-61.3670207840069,37.0481611121717,
0.));
#150075=CARTESIAN_POINT('Ctrl Pts',(-61.3670207840069,37.0481611121717,
12.));
#150076=CARTESIAN_POINT('Ctrl Pts',(-61.3521028132003,37.0301387221774,
0.));
#150077=CARTESIAN_POINT('Ctrl Pts',(-61.3521028132003,37.0301387221774,
12.));
#150078=CARTESIAN_POINT('Ctrl Pts',(-61.3371949931387,37.0121648413082,
0.));
#150079=CARTESIAN_POINT('Ctrl Pts',(-61.3371949931387,37.0121648413082,
12.));
#150080=CARTESIAN_POINT('Ctrl Pts',(-61.3222974552487,36.994239526727,0.));
#150081=CARTESIAN_POINT('Ctrl Pts',(-61.3222974552487,36.994239526727,12.));
#150082=CARTESIAN_POINT('Ctrl Pts',(-61.3074103315792,36.9763628357544,
0.));
#150083=CARTESIAN_POINT('Ctrl Pts',(-61.3074103315792,36.9763628357544,
12.));
#150084=CARTESIAN_POINT('Ctrl Pts',(-61.2925337548077,36.9585348258776,
0.));
#150085=CARTESIAN_POINT('Ctrl Pts',(-61.2925337548077,36.9585348258776,
12.));
#150086=CARTESIAN_POINT('Ctrl Pts',(-61.2776678582461,36.9407555547535,
0.));
#150087=CARTESIAN_POINT('Ctrl Pts',(-61.2776678582461,36.9407555547535,
12.));
#150088=CARTESIAN_POINT('Ctrl Pts',(-61.2628127758457,36.9230250802087,
0.));
#150089=CARTESIAN_POINT('Ctrl Pts',(-61.2628127758457,36.9230250802087,
12.));
#150090=CARTESIAN_POINT('Ctrl Pts',(-61.247968642201,36.9053434602343,0.));
#150091=CARTESIAN_POINT('Ctrl Pts',(-61.247968642201,36.9053434602343,12.));
#150092=CARTESIAN_POINT('Ctrl Pts',(-61.2331355925547,36.8877107529865,
0.));
#150093=CARTESIAN_POINT('Ctrl Pts',(-61.2331355925547,36.8877107529865,
12.));
#150094=CARTESIAN_POINT('Ctrl Pts',(-61.2183137628056,36.8701270167969,
0.));
#150095=CARTESIAN_POINT('Ctrl Pts',(-61.2183137628056,36.8701270167969,
12.));
#150096=CARTESIAN_POINT('Ctrl Pts',(-61.2035032895127,36.852592310174,0.));
#150097=CARTESIAN_POINT('Ctrl Pts',(-61.2035032895127,36.852592310174,12.));
#150098=CARTESIAN_POINT('Ctrl Pts',(-61.1887043099014,36.8351066918036,
0.));
#150099=CARTESIAN_POINT('Ctrl Pts',(-61.1887043099014,36.8351066918036,
12.));
#150100=CARTESIAN_POINT('Ctrl Pts',(-61.1739169618666,36.8176702205423,
0.));
#150101=CARTESIAN_POINT('Ctrl Pts',(-61.1739169618666,36.8176702205423,
12.));
#150102=CARTESIAN_POINT('Ctrl Pts',(-61.1591413839787,36.8002829554209,
0.));
#150103=CARTESIAN_POINT('Ctrl Pts',(-61.1591413839787,36.8002829554209,
12.));
#150104=CARTESIAN_POINT('Ctrl Pts',(-61.1443777154911,36.7829449556532,
0.));
#150105=CARTESIAN_POINT('Ctrl Pts',(-61.1443777154911,36.7829449556532,
12.));
#150106=CARTESIAN_POINT('Ctrl Pts',(-61.1296260963466,36.765656280638,0.));
#150107=CARTESIAN_POINT('Ctrl Pts',(-61.1296260963466,36.765656280638,12.));
#150108=CARTESIAN_POINT('Ctrl Pts',(-61.1148866671829,36.7484169899596,
0.));
#150109=CARTESIAN_POINT('Ctrl Pts',(-61.1148866671829,36.7484169899596,
12.));
#150110=CARTESIAN_POINT('Ctrl Pts',(-61.100159569337,36.7312271433807,0.));
#150111=CARTESIAN_POINT('Ctrl Pts',(-61.100159569337,36.7312271433807,12.));
#150112=CARTESIAN_POINT('Ctrl Pts',(-61.0854449448524,36.7140868008486,
0.));
#150113=CARTESIAN_POINT('Ctrl Pts',(-61.0854449448524,36.7140868008486,
12.));
#150114=CARTESIAN_POINT('Ctrl Pts',(-61.0707429364847,36.6969960225022,
0.));
#150115=CARTESIAN_POINT('Ctrl Pts',(-61.0707429364847,36.6969960225022,
12.));
#150116=CARTESIAN_POINT('Ctrl Pts',(-61.0560536877083,36.679954868674,0.));
#150117=CARTESIAN_POINT('Ctrl Pts',(-61.0560536877083,36.679954868674,12.));
#150118=CARTESIAN_POINT('Ctrl Pts',(-61.0413773427203,36.6629633998886,
0.));
#150119=CARTESIAN_POINT('Ctrl Pts',(-61.0413773427203,36.6629633998886,
12.));
#150120=CARTESIAN_POINT('Ctrl Pts',(-61.0267140464432,36.6460216768553,
0.));
#150121=CARTESIAN_POINT('Ctrl Pts',(-61.0267140464432,36.6460216768553,
12.));
#150122=CARTESIAN_POINT('Ctrl Pts',(-61.0120639445349,36.6291297604776,
0.));
#150123=CARTESIAN_POINT('Ctrl Pts',(-61.0120639445349,36.6291297604776,
12.));
#150124=CARTESIAN_POINT('Ctrl Pts',(-60.9974271833981,36.61228771186,0.));
#150125=CARTESIAN_POINT('Ctrl Pts',(-60.9974271833981,36.61228771186,12.));
#150126=CARTESIAN_POINT('Ctrl Pts',(-60.9828039101887,36.5954955923109,
0.));
#150127=CARTESIAN_POINT('Ctrl Pts',(-60.9828039101887,36.5954955923109,
12.));
#150128=CARTESIAN_POINT('Ctrl Pts',(-60.9681942728236,36.5787534633416,
0.));
#150129=CARTESIAN_POINT('Ctrl Pts',(-60.9681942728236,36.5787534633416,
12.));
#150130=CARTESIAN_POINT('Ctrl Pts',(-60.9535984199873,36.5620613866615,
0.));
#150131=CARTESIAN_POINT('Ctrl Pts',(-60.9535984199873,36.5620613866615,
12.));
#150132=CARTESIAN_POINT('Ctrl Pts',(-60.9390165011355,36.5454194241865,
0.));
#150133=CARTESIAN_POINT('Ctrl Pts',(-60.9390165011355,36.5454194241865,
12.));
#150134=CARTESIAN_POINT('Ctrl Pts',(-60.9244486664988,36.5288276380416,
0.));
#150135=CARTESIAN_POINT('Ctrl Pts',(-60.9244486664988,36.5288276380416,
12.));
#150136=CARTESIAN_POINT('Ctrl Pts',(-60.9098950670847,36.5122860905612,
0.));
#150137=CARTESIAN_POINT('Ctrl Pts',(-60.9098950670847,36.5122860905612,
12.));
#150138=CARTESIAN_POINT('Ctrl Pts',(-60.8953558546795,36.4957948442835,
0.));
#150139=CARTESIAN_POINT('Ctrl Pts',(-60.8953558546795,36.4957948442835,
12.));
#150140=CARTESIAN_POINT('Ctrl Pts',(-60.8808311818499,36.4793539619466,
0.));
#150141=CARTESIAN_POINT('Ctrl Pts',(-60.8808311818499,36.4793539619466,
12.));
#150142=CARTESIAN_POINT('Ctrl Pts',(-60.8663212019657,36.4629635065045,
0.));
#150143=CARTESIAN_POINT('Ctrl Pts',(-60.8663212019657,36.4629635065045,
12.));
#150144=CARTESIAN_POINT('Ctrl Pts',(-60.8518260692188,36.4466235411358,
0.));
#150145=CARTESIAN_POINT('Ctrl Pts',(-60.8518260692188,36.4466235411358,
12.));
#150146=CARTESIAN_POINT('Ctrl Pts',(-60.8373459386392,36.4303341292494,
0.));
#150147=CARTESIAN_POINT('Ctrl Pts',(-60.8373459386392,36.4303341292494,
12.));
#150148=CARTESIAN_POINT('Ctrl Pts',(-60.822880966116,36.4140953344858,0.));
#150149=CARTESIAN_POINT('Ctrl Pts',(-60.822880966116,36.4140953344858,12.));
#150150=CARTESIAN_POINT('Ctrl Pts',(-60.8084313083984,36.397907220716,0.));
#150151=CARTESIAN_POINT('Ctrl Pts',(-60.8084313083984,36.397907220716,12.));
#150152=CARTESIAN_POINT('Ctrl Pts',(-60.793997123076,36.3817698520388,0.));
#150153=CARTESIAN_POINT('Ctrl Pts',(-60.793997123076,36.3817698520388,12.));
#150154=CARTESIAN_POINT('Ctrl Pts',(-60.7795785685625,36.365683292773,0.));
#150155=CARTESIAN_POINT('Ctrl Pts',(-60.7795785685625,36.365683292773,12.));
#150156=CARTESIAN_POINT('Ctrl Pts',(-60.7651758040803,36.3496476074488,
0.));
#150157=CARTESIAN_POINT('Ctrl Pts',(-60.7651758040803,36.3496476074488,
12.));
#150158=CARTESIAN_POINT('Ctrl Pts',(-60.7507889896308,36.3336628607859,
0.));
#150159=CARTESIAN_POINT('Ctrl Pts',(-60.7507889896308,36.3336628607859,
12.));
#150160=CARTESIAN_POINT('Ctrl Pts',(-60.7364182860412,36.3177291177163,
0.));
#150161=CARTESIAN_POINT('Ctrl Pts',(-60.7364182860412,36.3177291177163,
12.));
#150162=CARTESIAN_POINT('Ctrl Pts',(-60.722063855041,36.3018464434213,0.));
#150163=CARTESIAN_POINT('Ctrl Pts',(-60.722063855041,36.3018464434213,12.));
#150164=CARTESIAN_POINT('Ctrl Pts',(-60.7077258593268,36.2860149033587,
0.));
#150165=CARTESIAN_POINT('Ctrl Pts',(-60.7077258593268,36.2860149033587,
12.));
#150166=CARTESIAN_POINT('Ctrl Pts',(-60.6934044626291,36.2702345632875,
0.));
#150167=CARTESIAN_POINT('Ctrl Pts',(-60.6934044626291,36.2702345632875,
12.));
#150168=CARTESIAN_POINT('Ctrl Pts',(-60.67909982978,36.2545054892897,0.));
#150169=CARTESIAN_POINT('Ctrl Pts',(-60.67909982978,36.2545054892897,12.));
#150170=CARTESIAN_POINT('Ctrl Pts',(-60.6648121265885,36.2388277477212,
0.));
#150171=CARTESIAN_POINT('Ctrl Pts',(-60.6648121265885,36.2388277477212,
12.));
#150172=CARTESIAN_POINT('Ctrl Pts',(-60.6505415197042,36.2232014051541,
0.));
#150173=CARTESIAN_POINT('Ctrl Pts',(-60.6505415197042,36.2232014051541,
12.));
#150174=CARTESIAN_POINT('Ctrl Pts',(-60.6362881765019,36.2076265283264,
0.));
#150175=CARTESIAN_POINT('Ctrl Pts',(-60.6362881765019,36.2076265283264,
12.));
#150176=CARTESIAN_POINT('Ctrl Pts',(-60.6220522649149,36.192103184063,0.));
#150177=CARTESIAN_POINT('Ctrl Pts',(-60.6220522649149,36.192103184063,12.));
#150178=CARTESIAN_POINT('Ctrl Pts',(-60.6078339534181,36.1766314392641,
0.));
#150179=CARTESIAN_POINT('Ctrl Pts',(-60.6078339534181,36.1766314392641,
12.));
#150180=CARTESIAN_POINT('Ctrl Pts',(-60.5936334114108,36.1612113610773,
0.));
#150181=CARTESIAN_POINT('Ctrl Pts',(-60.5936334114108,36.1612113610773,
12.));
#150182=CARTESIAN_POINT('Ctrl Pts',(-60.5794508095565,36.1458430170431,
0.));
#150183=CARTESIAN_POINT('Ctrl Pts',(-60.5794508095565,36.1458430170431,
12.));
#150184=CARTESIAN_POINT('Ctrl Pts',(-60.565286320072,36.1305264752188,0.));
#150185=CARTESIAN_POINT('Ctrl Pts',(-60.565286320072,36.1305264752188,12.));
#150186=CARTESIAN_POINT('Ctrl Pts',(-60.5511401171984,36.1152618043739,
0.));
#150187=CARTESIAN_POINT('Ctrl Pts',(-60.5511401171984,36.1152618043739,
12.));
#150188=CARTESIAN_POINT('Ctrl Pts',(-60.5370123768804,36.100049073851,0.));
#150189=CARTESIAN_POINT('Ctrl Pts',(-60.5370123768804,36.100049073851,12.));
#150190=CARTESIAN_POINT('Ctrl Pts',(-60.5229032758974,36.0848883531952,
0.));
#150191=CARTESIAN_POINT('Ctrl Pts',(-60.5229032758974,36.0848883531952,
12.));
#150192=CARTESIAN_POINT('Ctrl Pts',(-60.5088129911354,36.0697797118376,
0.));
#150193=CARTESIAN_POINT('Ctrl Pts',(-60.5088129911354,36.0697797118376,
12.));
#150194=CARTESIAN_POINT('Ctrl Pts',(-60.4947416988422,36.0547232187698,
0.));
#150195=CARTESIAN_POINT('Ctrl Pts',(-60.4947416988422,36.0547232187698,
12.));
#150196=CARTESIAN_POINT('Ctrl Pts',(-60.4806895737686,36.0397189421644,
0.));
#150197=CARTESIAN_POINT('Ctrl Pts',(-60.4806895737686,36.0397189421644,
12.));
#150198=CARTESIAN_POINT('Ctrl Pts',(-60.4666567908093,36.0247669500891,
0.));
#150199=CARTESIAN_POINT('Ctrl Pts',(-60.4666567908093,36.0247669500891,
12.));
#150200=CARTESIAN_POINT('Ctrl Pts',(-60.4526435269662,36.009867311357,0.));
#150201=CARTESIAN_POINT('Ctrl Pts',(-60.4526435269662,36.009867311357,12.));
#150202=CARTESIAN_POINT('Ctrl Pts',(-60.4386499629481,35.995020096217,0.));
#150203=CARTESIAN_POINT('Ctrl Pts',(-60.4386499629481,35.995020096217,12.));
#150204=CARTESIAN_POINT('Ctrl Pts',(-60.4246762854926,35.9802253773515,
0.));
#150205=CARTESIAN_POINT('Ctrl Pts',(-60.4246762854926,35.9802253773515,
12.));
#150206=CARTESIAN_POINT('Ctrl Pts',(-60.4107226875714,35.9654832299601,
0.));
#150207=CARTESIAN_POINT('Ctrl Pts',(-60.4107226875714,35.9654832299601,
12.));
#150208=CARTESIAN_POINT('Ctrl Pts',(-60.3967893635452,35.9507937296707,
0.));
#150209=CARTESIAN_POINT('Ctrl Pts',(-60.3967893635452,35.9507937296707,
12.));
#150210=CARTESIAN_POINT('Ctrl Pts',(-60.3828765049019,35.936156950695,0.));
#150211=CARTESIAN_POINT('Ctrl Pts',(-60.3828765049019,35.936156950695,12.));
#150212=CARTESIAN_POINT('Ctrl Pts',(-60.3689842965481,35.9215729642231,
0.));
#150213=CARTESIAN_POINT('Ctrl Pts',(-60.3689842965481,35.9215729642231,
12.));
#150214=CARTESIAN_POINT('Ctrl Pts',(-60.3551129108845,35.907041835853,0.));
#150215=CARTESIAN_POINT('Ctrl Pts',(-60.3551129108845,35.907041835853,12.));
#150216=CARTESIAN_POINT('Ctrl Pts',(-60.3412625135287,35.8925636280668,
0.));
#150217=CARTESIAN_POINT('Ctrl Pts',(-60.3412625135287,35.8925636280668,
12.));
#150218=CARTESIAN_POINT('Ctrl Pts',(-60.327433274683,35.8781384051537,0.));
#150219=CARTESIAN_POINT('Ctrl Pts',(-60.327433274683,35.8781384051537,12.));
#150220=CARTESIAN_POINT('Ctrl Pts',(-60.313625378281,35.8637662371635,0.));
#150221=CARTESIAN_POINT('Ctrl Pts',(-60.313625378281,35.8637662371635,12.));
#150222=CARTESIAN_POINT('Ctrl Pts',(-60.2998390330102,35.8494472046745,
0.));
#150223=CARTESIAN_POINT('Ctrl Pts',(-60.2998390330102,35.8494472046745,
12.));
#150224=CARTESIAN_POINT('Ctrl Pts',(-60.2860744798436,35.8351814020357,
0.));
#150225=CARTESIAN_POINT('Ctrl Pts',(-60.2860744798436,35.8351814020357,
12.));
#150226=CARTESIAN_POINT('Ctrl Pts',(-60.2723319687369,35.8209689272501,
0.));
#150227=CARTESIAN_POINT('Ctrl Pts',(-60.2723319687369,35.8209689272501,
12.));
#150228=CARTESIAN_POINT('Ctrl Pts',(-60.2586117365205,35.8068098723347,
0.));
#150229=CARTESIAN_POINT('Ctrl Pts',(-60.2586117365205,35.8068098723347,
12.));
#150230=CARTESIAN_POINT('Ctrl Pts',(-60.2449139865275,35.7927043145201,
0.));
#150231=CARTESIAN_POINT('Ctrl Pts',(-60.2449139865275,35.7927043145201,
12.));
#150232=CARTESIAN_POINT('Ctrl Pts',(-60.2312388621529,35.7786523045912,
0.));
#150233=CARTESIAN_POINT('Ctrl Pts',(-60.2312388621529,35.7786523045912,
12.));
#150234=CARTESIAN_POINT('Ctrl Pts',(-60.2175864450043,35.7646538667493,
0.));
#150235=CARTESIAN_POINT('Ctrl Pts',(-60.2175864450043,35.7646538667493,
12.));
#150236=CARTESIAN_POINT('Ctrl Pts',(-60.206682708692,35.7534979802053,0.));
#150237=CARTESIAN_POINT('Ctrl Pts',(-60.206682708692,35.7534979802053,12.));
#150238=CARTESIAN_POINT('Ctrl Pts',(-60.1985151474623,35.7451551752572,
0.));
#150239=CARTESIAN_POINT('Ctrl Pts',(-60.1985151474623,35.7451551752572,
12.));
#150240=CARTESIAN_POINT('Ctrl Pts',(-60.193074658032,35.7396040204017,0.));
#150241=CARTESIAN_POINT('Ctrl Pts',(-60.193074658032,35.7396040204017,12.));
#150242=CARTESIAN_POINT('Ctrl Pts',(-60.1903555511633,35.736831121751,0.));
#150243=CARTESIAN_POINT('Ctrl Pts',(-60.1903555511633,35.736831121751,12.));
#150244=CARTESIAN_POINT('',(-60.1903555511633,35.736831121751,12.));
#150245=CARTESIAN_POINT('Ctrl Pts',(-60.1903555511633,35.736831121751,12.));
#150246=CARTESIAN_POINT('Ctrl Pts',(-60.193074658032,35.7396040204017,12.));
#150247=CARTESIAN_POINT('Ctrl Pts',(-60.1985151474623,35.7451551752572,
12.));
#150248=CARTESIAN_POINT('Ctrl Pts',(-60.206682708692,35.7534979802053,12.));
#150249=CARTESIAN_POINT('Ctrl Pts',(-60.2175864450043,35.7646538667493,
12.));
#150250=CARTESIAN_POINT('Ctrl Pts',(-60.2312388621529,35.7786523045912,
12.));
#150251=CARTESIAN_POINT('Ctrl Pts',(-60.2449139865275,35.7927043145201,
12.));
#150252=CARTESIAN_POINT('Ctrl Pts',(-60.2586117365205,35.8068098723347,
12.));
#150253=CARTESIAN_POINT('Ctrl Pts',(-60.2723319687369,35.8209689272501,
12.));
#150254=CARTESIAN_POINT('Ctrl Pts',(-60.2860744798436,35.8351814020357,
12.));
#150255=CARTESIAN_POINT('Ctrl Pts',(-60.2998390330102,35.8494472046745,
12.));
#150256=CARTESIAN_POINT('Ctrl Pts',(-60.313625378281,35.8637662371635,12.));
#150257=CARTESIAN_POINT('Ctrl Pts',(-60.327433274683,35.8781384051537,12.));
#150258=CARTESIAN_POINT('Ctrl Pts',(-60.3412625135287,35.8925636280668,
12.));
#150259=CARTESIAN_POINT('Ctrl Pts',(-60.3551129108845,35.907041835853,12.));
#150260=CARTESIAN_POINT('Ctrl Pts',(-60.3689842965481,35.9215729642231,
12.));
#150261=CARTESIAN_POINT('Ctrl Pts',(-60.3828765049019,35.936156950695,12.));
#150262=CARTESIAN_POINT('Ctrl Pts',(-60.3967893635452,35.9507937296707,
12.));
#150263=CARTESIAN_POINT('Ctrl Pts',(-60.4107226875714,35.9654832299601,
12.));
#150264=CARTESIAN_POINT('Ctrl Pts',(-60.4246762854926,35.9802253773515,
12.));
#150265=CARTESIAN_POINT('Ctrl Pts',(-60.4386499629481,35.995020096217,12.));
#150266=CARTESIAN_POINT('Ctrl Pts',(-60.4526435269662,36.009867311357,12.));
#150267=CARTESIAN_POINT('Ctrl Pts',(-60.4666567908093,36.0247669500891,
12.));
#150268=CARTESIAN_POINT('Ctrl Pts',(-60.4806895737686,36.0397189421644,
12.));
#150269=CARTESIAN_POINT('Ctrl Pts',(-60.4947416988422,36.0547232187698,
12.));
#150270=CARTESIAN_POINT('Ctrl Pts',(-60.5088129911354,36.0697797118376,
12.));
#150271=CARTESIAN_POINT('Ctrl Pts',(-60.5229032758974,36.0848883531952,
12.));
#150272=CARTESIAN_POINT('Ctrl Pts',(-60.5370123768804,36.100049073851,12.));
#150273=CARTESIAN_POINT('Ctrl Pts',(-60.5511401171984,36.1152618043739,
12.));
#150274=CARTESIAN_POINT('Ctrl Pts',(-60.565286320072,36.1305264752188,12.));
#150275=CARTESIAN_POINT('Ctrl Pts',(-60.5794508095565,36.1458430170431,
12.));
#150276=CARTESIAN_POINT('Ctrl Pts',(-60.5936334114108,36.1612113610773,
12.));
#150277=CARTESIAN_POINT('Ctrl Pts',(-60.6078339534181,36.1766314392641,
12.));
#150278=CARTESIAN_POINT('Ctrl Pts',(-60.6220522649149,36.192103184063,12.));
#150279=CARTESIAN_POINT('Ctrl Pts',(-60.6362881765019,36.2076265283264,
12.));
#150280=CARTESIAN_POINT('Ctrl Pts',(-60.6505415197042,36.2232014051541,
12.));
#150281=CARTESIAN_POINT('Ctrl Pts',(-60.6648121265885,36.2388277477212,
12.));
#150282=CARTESIAN_POINT('Ctrl Pts',(-60.67909982978,36.2545054892897,12.));
#150283=CARTESIAN_POINT('Ctrl Pts',(-60.6934044626291,36.2702345632875,
12.));
#150284=CARTESIAN_POINT('Ctrl Pts',(-60.7077258593268,36.2860149033587,
12.));
#150285=CARTESIAN_POINT('Ctrl Pts',(-60.722063855041,36.3018464434213,12.));
#150286=CARTESIAN_POINT('Ctrl Pts',(-60.7364182860412,36.3177291177163,
12.));
#150287=CARTESIAN_POINT('Ctrl Pts',(-60.7507889896308,36.3336628607859,
12.));
#150288=CARTESIAN_POINT('Ctrl Pts',(-60.7651758040803,36.3496476074488,
12.));
#150289=CARTESIAN_POINT('Ctrl Pts',(-60.7795785685625,36.365683292773,12.));
#150290=CARTESIAN_POINT('Ctrl Pts',(-60.793997123076,36.3817698520388,12.));
#150291=CARTESIAN_POINT('Ctrl Pts',(-60.8084313083984,36.397907220716,12.));
#150292=CARTESIAN_POINT('Ctrl Pts',(-60.822880966116,36.4140953344858,12.));
#150293=CARTESIAN_POINT('Ctrl Pts',(-60.8373459386392,36.4303341292494,
12.));
#150294=CARTESIAN_POINT('Ctrl Pts',(-60.8518260692188,36.4466235411358,
12.));
#150295=CARTESIAN_POINT('Ctrl Pts',(-60.8663212019657,36.4629635065045,
12.));
#150296=CARTESIAN_POINT('Ctrl Pts',(-60.8808311818499,36.4793539619466,
12.));
#150297=CARTESIAN_POINT('Ctrl Pts',(-60.8953558546795,36.4957948442835,
12.));
#150298=CARTESIAN_POINT('Ctrl Pts',(-60.9098950670847,36.5122860905612,
12.));
#150299=CARTESIAN_POINT('Ctrl Pts',(-60.9244486664988,36.5288276380416,
12.));
#150300=CARTESIAN_POINT('Ctrl Pts',(-60.9390165011355,36.5454194241865,
12.));
#150301=CARTESIAN_POINT('Ctrl Pts',(-60.9535984199873,36.5620613866615,
12.));
#150302=CARTESIAN_POINT('Ctrl Pts',(-60.9681942728236,36.5787534633416,
12.));
#150303=CARTESIAN_POINT('Ctrl Pts',(-60.9828039101887,36.5954955923109,
12.));
#150304=CARTESIAN_POINT('Ctrl Pts',(-60.9974271833981,36.61228771186,12.));
#150305=CARTESIAN_POINT('Ctrl Pts',(-61.0120639445349,36.6291297604776,
12.));
#150306=CARTESIAN_POINT('Ctrl Pts',(-61.0267140464432,36.6460216768553,
12.));
#150307=CARTESIAN_POINT('Ctrl Pts',(-61.0413773427203,36.6629633998886,
12.));
#150308=CARTESIAN_POINT('Ctrl Pts',(-61.0560536877083,36.679954868674,12.));
#150309=CARTESIAN_POINT('Ctrl Pts',(-61.0707429364847,36.6969960225022,
12.));
#150310=CARTESIAN_POINT('Ctrl Pts',(-61.0854449448524,36.7140868008486,
12.));
#150311=CARTESIAN_POINT('Ctrl Pts',(-61.100159569337,36.7312271433807,12.));
#150312=CARTESIAN_POINT('Ctrl Pts',(-61.1148866671829,36.7484169899596,
12.));
#150313=CARTESIAN_POINT('Ctrl Pts',(-61.1296260963466,36.765656280638,12.));
#150314=CARTESIAN_POINT('Ctrl Pts',(-61.1443777154911,36.7829449556532,
12.));
#150315=CARTESIAN_POINT('Ctrl Pts',(-61.1591413839787,36.8002829554209,
12.));
#150316=CARTESIAN_POINT('Ctrl Pts',(-61.1739169618666,36.8176702205423,
12.));
#150317=CARTESIAN_POINT('Ctrl Pts',(-61.1887043099014,36.8351066918036,
12.));
#150318=CARTESIAN_POINT('Ctrl Pts',(-61.2035032895127,36.852592310174,12.));
#150319=CARTESIAN_POINT('Ctrl Pts',(-61.2183137628056,36.8701270167969,
12.));
#150320=CARTESIAN_POINT('Ctrl Pts',(-61.2331355925547,36.8877107529865,
12.));
#150321=CARTESIAN_POINT('Ctrl Pts',(-61.247968642201,36.9053434602343,12.));
#150322=CARTESIAN_POINT('Ctrl Pts',(-61.2628127758457,36.9230250802087,
12.));
#150323=CARTESIAN_POINT('Ctrl Pts',(-61.2776678582461,36.9407555547535,
12.));
#150324=CARTESIAN_POINT('Ctrl Pts',(-61.2925337548077,36.9585348258776,
12.));
#150325=CARTESIAN_POINT('Ctrl Pts',(-61.3074103315792,36.9763628357544,
12.));
#150326=CARTESIAN_POINT('Ctrl Pts',(-61.3222974552487,36.994239526727,12.));
#150327=CARTESIAN_POINT('Ctrl Pts',(-61.3371949931387,37.0121648413082,
12.));
#150328=CARTESIAN_POINT('Ctrl Pts',(-61.3521028132003,37.0301387221774,
12.));
#150329=CARTESIAN_POINT('Ctrl Pts',(-61.3670207840069,37.0481611121717,
12.));
#150330=CARTESIAN_POINT('Ctrl Pts',(-61.381948774749,37.0662319542849,12.));
#150331=CARTESIAN_POINT('Ctrl Pts',(-61.3968866552317,37.0843511916745,
12.));
#150332=CARTESIAN_POINT('Ctrl Pts',(-61.4118342958697,37.1025187676602,
12.));
#150333=CARTESIAN_POINT('Ctrl Pts',(-61.4267915676822,37.1207346257222,
12.));
#150334=CARTESIAN_POINT('Ctrl Pts',(-61.4417583422863,37.1389987094905,
12.));
#150335=CARTESIAN_POINT('Ctrl Pts',(-61.4567344918919,37.1573109627454,
12.));
#150336=CARTESIAN_POINT('Ctrl Pts',(-61.4717198892994,37.175671329424,12.));
#150337=CARTESIAN_POINT('Ctrl Pts',(-61.4867144078936,37.1940797536181,
12.));
#150338=CARTESIAN_POINT('Ctrl Pts',(-61.501717921641,37.2125361795731,12.));
#150339=CARTESIAN_POINT('Ctrl Pts',(-61.5167303050832,37.2310405516781,
12.));
#150340=CARTESIAN_POINT('Ctrl Pts',(-61.5317514333328,37.2495928144667,
12.));
#150341=CARTESIAN_POINT('Ctrl Pts',(-61.5467811820691,37.2681929126221,
12.));
#150342=CARTESIAN_POINT('Ctrl Pts',(-61.5618194275348,37.286840790977,12.));
#150343=CARTESIAN_POINT('Ctrl Pts',(-61.5768660465311,37.3055363945107,
12.));
#150344=CARTESIAN_POINT('Ctrl Pts',(-61.591920916412,37.3242796683395,12.));
#150345=CARTESIAN_POINT('Ctrl Pts',(-61.6069839150807,37.343070557718,12.));
#150346=CARTESIAN_POINT('Ctrl Pts',(-61.6220549209866,37.361909008045,12.));
#150347=CARTESIAN_POINT('Ctrl Pts',(-61.637133813121,37.3807949648624,12.));
#150348=CARTESIAN_POINT('Ctrl Pts',(-61.6522204710131,37.3997283738533,
12.));
#150349=CARTESIAN_POINT('Ctrl Pts',(-61.6673147747242,37.4187091808321,
12.));
#150350=CARTESIAN_POINT('Ctrl Pts',(-61.6824166048444,37.4377373317451,
12.));
#150351=CARTESIAN_POINT('Ctrl Pts',(-61.6975258424894,37.4568127726773,
12.));
#150352=CARTESIAN_POINT('Ctrl Pts',(-61.7126423692963,37.4759354498509,
12.));
#150353=CARTESIAN_POINT('Ctrl Pts',(-61.7277660674205,37.4951053096237,
12.));
#150354=CARTESIAN_POINT('Ctrl Pts',(-61.7428968195299,37.5143222984796,
12.));
#150355=CARTESIAN_POINT('Ctrl Pts',(-61.7580345088016,37.5335863630287,
12.));
#150356=CARTESIAN_POINT('Ctrl Pts',(-61.7731790189191,37.5528974500142,
12.));
#150357=CARTESIAN_POINT('Ctrl Pts',(-61.7883302340687,37.5722555063111,
12.));
#150358=CARTESIAN_POINT('Ctrl Pts',(-61.8034880389362,37.5916604789253,
12.));
#150359=CARTESIAN_POINT('Ctrl Pts',(-61.8186523187015,37.6111123149839,
12.));
#150360=CARTESIAN_POINT('Ctrl Pts',(-61.8338229590353,37.6306109617346,
12.));
#150361=CARTESIAN_POINT('Ctrl Pts',(-61.8489998460957,37.6501563665523,
12.));
#150362=CARTESIAN_POINT('Ctrl Pts',(-61.8641828665261,37.6697484769392,
12.));
#150363=CARTESIAN_POINT('Ctrl Pts',(-61.8793719074507,37.6893872405228,
12.));
#150364=CARTESIAN_POINT('Ctrl Pts',(-61.8945668564704,37.7090726050482,
12.));
#150365=CARTESIAN_POINT('Ctrl Pts',(-61.9097676016601,37.7288045183756,
12.));
#150366=CARTESIAN_POINT('Ctrl Pts',(-61.9249740315649,37.7485829284871,
12.));
#150367=CARTESIAN_POINT('Ctrl Pts',(-61.9401860351972,37.7684077834872,
12.));
#150368=CARTESIAN_POINT('Ctrl Pts',(-61.9554035020338,37.7882790316014,
12.));
#150369=CARTESIAN_POINT('Ctrl Pts',(-61.9706263220114,37.8081966211689,
12.));
#150370=CARTESIAN_POINT('Ctrl Pts',(-61.9858543855236,37.828160500638,12.));
#150371=CARTESIAN_POINT('Ctrl Pts',(-62.0010875834187,37.8481706185749,
12.));
#150372=CARTESIAN_POINT('Ctrl Pts',(-62.0163258069957,37.868226923663,12.));
#150373=CARTESIAN_POINT('Ctrl Pts',(-62.031568948002,37.8883293647029,12.));
#150374=CARTESIAN_POINT('Ctrl Pts',(-62.0468168986288,37.9084778906053,
12.));
#150375=CARTESIAN_POINT('Ctrl Pts',(-62.0620695515074,37.9286724503851,
12.));
#150376=CARTESIAN_POINT('Ctrl Pts',(-62.0773267997079,37.9489129931689,
12.));
#150377=CARTESIAN_POINT('Ctrl Pts',(-62.0925885367352,37.9691994681966,
12.));
#150378=CARTESIAN_POINT('Ctrl Pts',(-62.107854656528,37.9895318248212,12.));
#150379=CARTESIAN_POINT('Ctrl Pts',(-62.123125053455,38.0099100125037,12.));
#150380=CARTESIAN_POINT('Ctrl Pts',(-62.1383996223125,38.0303339808053,
12.));
#150381=CARTESIAN_POINT('Ctrl Pts',(-62.1536782583199,38.0508036793939,
12.));
#150382=CARTESIAN_POINT('Ctrl Pts',(-62.1689608571176,38.0713190580463,
12.));
#150383=CARTESIAN_POINT('Ctrl Pts',(-62.1842473147626,38.0918800666479,
12.));
#150384=CARTESIAN_POINT('Ctrl Pts',(-62.1995375277257,38.1124866551886,
12.));
#150385=CARTESIAN_POINT('Ctrl Pts',(-62.2148313928863,38.133138773753,12.));
#150386=CARTESIAN_POINT('Ctrl Pts',(-62.2301288075321,38.1538363725264,
12.));
#150387=CARTESIAN_POINT('Ctrl Pts',(-62.245429669358,38.1745794017996,12.));
#150388=CARTESIAN_POINT('Ctrl Pts',(-62.2607338764654,38.1953678119691,
12.));
#150389=CARTESIAN_POINT('Ctrl Pts',(-62.2760413273602,38.2162015535353,
12.));
#150390=CARTESIAN_POINT('Ctrl Pts',(-62.2913519209521,38.2370805770935,
12.));
#150391=CARTESIAN_POINT('Ctrl Pts',(-62.3066655565503,38.2580048333361,
12.));
#150392=CARTESIAN_POINT('Ctrl Pts',(-62.3219821338569,38.2789742730564,
12.));
#150393=CARTESIAN_POINT('Ctrl Pts',(-62.3373015529613,38.2999888471476,
12.));
#150394=CARTESIAN_POINT('Ctrl Pts',(-62.3526237143336,38.3210485066001,
12.));
#150395=CARTESIAN_POINT('Ctrl Pts',(-62.3679485188172,38.342153202491,12.));
#150396=CARTESIAN_POINT('Ctrl Pts',(-62.3832758676271,38.3633028859828,
12.));
#150397=CARTESIAN_POINT('Ctrl Pts',(-62.3986056623577,38.3844975083343,
12.));
#150398=CARTESIAN_POINT('Ctrl Pts',(-62.4139378049885,38.405737020905,12.));
#150399=CARTESIAN_POINT('Ctrl Pts',(-62.4292721978901,38.4270213751568,
12.));
#150400=CARTESIAN_POINT('Ctrl Pts',(-62.4446087438312,38.4483505226518,
12.));
#150401=CARTESIAN_POINT('Ctrl Pts',(-62.4599473459811,38.4697244150482,
12.));
#150402=CARTESIAN_POINT('Ctrl Pts',(-62.4752879078854,38.4911430040997,
12.));
#150403=CARTESIAN_POINT('Ctrl Pts',(-62.4906303334443,38.5126062416502,
12.));
#150404=CARTESIAN_POINT('Ctrl Pts',(-62.5059745268901,38.5341140796248,
12.));
#150405=CARTESIAN_POINT('Ctrl Pts',(-62.5213203927663,38.5556664700195,
12.));
#150406=CARTESIAN_POINT('Ctrl Pts',(-62.5366678359023,38.5772633648832,
12.));
#150407=CARTESIAN_POINT('Ctrl Pts',(-62.5520167614516,38.5989047163393,
12.));
#150408=CARTESIAN_POINT('Ctrl Pts',(-62.5673670749361,38.6205904766073,
12.));
#150409=CARTESIAN_POINT('Ctrl Pts',(-62.5827186822921,38.6423205980213,
12.));
#150410=CARTESIAN_POINT('Ctrl Pts',(-62.5980714899052,38.6640950330421,
12.));
#150411=CARTESIAN_POINT('Ctrl Pts',(-62.6134254046739,38.6859137342731,
12.));
#150412=CARTESIAN_POINT('Ctrl Pts',(-62.6287803339542,38.7077766544416,
12.));
#150413=CARTESIAN_POINT('Ctrl Pts',(-62.6441361854411,38.7296837463609,
12.));
#150414=CARTESIAN_POINT('Ctrl Pts',(-62.6594928670628,38.7516349628904,
12.));
#150415=CARTESIAN_POINT('Ctrl Pts',(-62.6748502868835,38.7736302568982,
12.));
#150416=CARTESIAN_POINT('Ctrl Pts',(-62.6902083529694,38.795669581203,12.));
#150417=CARTESIAN_POINT('Ctrl Pts',(-62.7055669733802,38.8177528885681,
12.));
#150418=CARTESIAN_POINT('Ctrl Pts',(-62.7209260564493,38.8398801318177,
12.));
#150419=CARTESIAN_POINT('Ctrl Pts',(-62.7362855110042,38.8620512639232,
12.));
#150420=CARTESIAN_POINT('Ctrl Pts',(-62.7516452466128,38.8842662380984,
12.));
#150421=CARTESIAN_POINT('Ctrl Pts',(-62.7670051738143,38.9065250078832,
12.));
#150422=CARTESIAN_POINT('Ctrl Pts',(-62.78236520437,38.9288275272335,12.));
#150423=CARTESIAN_POINT('Ctrl Pts',(-62.7977252507118,38.9511737503165,
12.));
#150424=CARTESIAN_POINT('Ctrl Pts',(-62.8130852254027,38.9735636313089,
12.));
#150425=CARTESIAN_POINT('Ctrl Pts',(-62.8284450405459,38.9959971241701,
12.));
#150426=CARTESIAN_POINT('Ctrl Pts',(-62.8438046073224,39.0184741824641,
12.));
#150427=CARTESIAN_POINT('Ctrl Pts',(-62.8591638352056,39.0409947590497,
12.));
#150428=CARTESIAN_POINT('Ctrl Pts',(-62.8745226325998,39.0635588063276,
12.));
#150429=CARTESIAN_POINT('Ctrl Pts',(-62.8898809082612,39.0861662767932,
12.));
#150430=CARTESIAN_POINT('Ctrl Pts',(-62.9052385725387,39.1088171235125,
12.));
#150431=CARTESIAN_POINT('Ctrl Pts',(-62.9205955385558,39.131511300575,12.));
#150432=CARTESIAN_POINT('Ctrl Pts',(-62.9359517237404,39.1542487636744,
12.));
#150433=CARTESIAN_POINT('Ctrl Pts',(-62.9513070501867,39.1770294702428,
12.));
#150434=CARTESIAN_POINT('Ctrl Pts',(-62.9644687386836,39.1965939820933,
12.));
#150435=CARTESIAN_POINT('Ctrl Pts',(-62.9745590018672,39.2116170128461,
12.));
#150436=CARTESIAN_POINT('Ctrl Pts',(-62.9815782721325,39.2220794388806,
12.));
#150437=CARTESIAN_POINT('Ctrl Pts',(-62.9855268616127,39.2279686275006,
12.));
#150438=CARTESIAN_POINT('Ctrl Pts',(-62.9864049293894,39.2292784191812,
12.));
#150439=CARTESIAN_POINT('',(-60.1903555511633,35.736831121751,0.));
#150440=CARTESIAN_POINT('',(-60.1903555511633,35.7368311217509,0.));
#150441=CARTESIAN_POINT('Ctrl Pts',(-62.9864049293893,39.2292784191812,
0.));
#150442=CARTESIAN_POINT('Ctrl Pts',(-62.9855268616127,39.2279686275006,
0.));
#150443=CARTESIAN_POINT('Ctrl Pts',(-62.9815782721325,39.2220794388806,
0.));
#150444=CARTESIAN_POINT('Ctrl Pts',(-62.9745590018672,39.211617012846,0.));
#150445=CARTESIAN_POINT('Ctrl Pts',(-62.9644687386836,39.1965939820933,
0.));
#150446=CARTESIAN_POINT('Ctrl Pts',(-62.9513070501867,39.1770294702428,
0.));
#150447=CARTESIAN_POINT('Ctrl Pts',(-62.9359517237404,39.1542487636744,
0.));
#150448=CARTESIAN_POINT('Ctrl Pts',(-62.9205955385558,39.131511300575,0.));
#150449=CARTESIAN_POINT('Ctrl Pts',(-62.9052385725387,39.1088171235125,
0.));
#150450=CARTESIAN_POINT('Ctrl Pts',(-62.8898809082612,39.0861662767932,
0.));
#150451=CARTESIAN_POINT('Ctrl Pts',(-62.8745226325998,39.0635588063276,
0.));
#150452=CARTESIAN_POINT('Ctrl Pts',(-62.8591638352056,39.0409947590497,
0.));
#150453=CARTESIAN_POINT('Ctrl Pts',(-62.8438046073224,39.0184741824641,
0.));
#150454=CARTESIAN_POINT('Ctrl Pts',(-62.8284450405459,38.9959971241701,
0.));
#150455=CARTESIAN_POINT('Ctrl Pts',(-62.8130852254027,38.9735636313089,
0.));
#150456=CARTESIAN_POINT('Ctrl Pts',(-62.7977252507118,38.9511737503165,
0.));
#150457=CARTESIAN_POINT('Ctrl Pts',(-62.78236520437,38.9288275272335,0.));
#150458=CARTESIAN_POINT('Ctrl Pts',(-62.7670051738143,38.9065250078832,
0.));
#150459=CARTESIAN_POINT('Ctrl Pts',(-62.7516452466128,38.8842662380984,
0.));
#150460=CARTESIAN_POINT('Ctrl Pts',(-62.7362855110042,38.8620512639232,
0.));
#150461=CARTESIAN_POINT('Ctrl Pts',(-62.7209260564493,38.8398801318177,
0.));
#150462=CARTESIAN_POINT('Ctrl Pts',(-62.7055669733802,38.8177528885681,
0.));
#150463=CARTESIAN_POINT('Ctrl Pts',(-62.6902083529694,38.795669581203,0.));
#150464=CARTESIAN_POINT('Ctrl Pts',(-62.6748502868835,38.7736302568982,
0.));
#150465=CARTESIAN_POINT('Ctrl Pts',(-62.6594928670628,38.7516349628904,
0.));
#150466=CARTESIAN_POINT('Ctrl Pts',(-62.6441361854411,38.7296837463609,
0.));
#150467=CARTESIAN_POINT('Ctrl Pts',(-62.6287803339542,38.7077766544416,
0.));
#150468=CARTESIAN_POINT('Ctrl Pts',(-62.6134254046739,38.6859137342731,
0.));
#150469=CARTESIAN_POINT('Ctrl Pts',(-62.5980714899052,38.6640950330421,
0.));
#150470=CARTESIAN_POINT('Ctrl Pts',(-62.5827186822921,38.6423205980213,
0.));
#150471=CARTESIAN_POINT('Ctrl Pts',(-62.5673670749361,38.6205904766073,
0.));
#150472=CARTESIAN_POINT('Ctrl Pts',(-62.5520167614516,38.5989047163393,
0.));
#150473=CARTESIAN_POINT('Ctrl Pts',(-62.5366678359023,38.5772633648832,
0.));
#150474=CARTESIAN_POINT('Ctrl Pts',(-62.5213203927663,38.5556664700195,
0.));
#150475=CARTESIAN_POINT('Ctrl Pts',(-62.5059745268901,38.5341140796248,
0.));
#150476=CARTESIAN_POINT('Ctrl Pts',(-62.4906303334443,38.5126062416502,
0.));
#150477=CARTESIAN_POINT('Ctrl Pts',(-62.4752879078854,38.4911430040997,
0.));
#150478=CARTESIAN_POINT('Ctrl Pts',(-62.4599473459811,38.4697244150482,
0.));
#150479=CARTESIAN_POINT('Ctrl Pts',(-62.4446087438312,38.4483505226518,
0.));
#150480=CARTESIAN_POINT('Ctrl Pts',(-62.4292721978901,38.4270213751568,
0.));
#150481=CARTESIAN_POINT('Ctrl Pts',(-62.4139378049885,38.405737020905,0.));
#150482=CARTESIAN_POINT('Ctrl Pts',(-62.3986056623577,38.3844975083343,
0.));
#150483=CARTESIAN_POINT('Ctrl Pts',(-62.3832758676271,38.3633028859828,
0.));
#150484=CARTESIAN_POINT('Ctrl Pts',(-62.3679485188172,38.342153202491,0.));
#150485=CARTESIAN_POINT('Ctrl Pts',(-62.3526237143336,38.3210485066001,
0.));
#150486=CARTESIAN_POINT('Ctrl Pts',(-62.3373015529613,38.2999888471476,
0.));
#150487=CARTESIAN_POINT('Ctrl Pts',(-62.3219821338569,38.2789742730564,
0.));
#150488=CARTESIAN_POINT('Ctrl Pts',(-62.3066655565503,38.2580048333361,
0.));
#150489=CARTESIAN_POINT('Ctrl Pts',(-62.2913519209521,38.2370805770935,
0.));
#150490=CARTESIAN_POINT('Ctrl Pts',(-62.2760413273602,38.2162015535353,
0.));
#150491=CARTESIAN_POINT('Ctrl Pts',(-62.2607338764654,38.1953678119691,
0.));
#150492=CARTESIAN_POINT('Ctrl Pts',(-62.245429669358,38.1745794017996,0.));
#150493=CARTESIAN_POINT('Ctrl Pts',(-62.2301288075321,38.1538363725264,
0.));
#150494=CARTESIAN_POINT('Ctrl Pts',(-62.2148313928863,38.133138773753,0.));
#150495=CARTESIAN_POINT('Ctrl Pts',(-62.1995375277257,38.1124866551886,
0.));
#150496=CARTESIAN_POINT('Ctrl Pts',(-62.1842473147626,38.0918800666479,
0.));
#150497=CARTESIAN_POINT('Ctrl Pts',(-62.1689608571176,38.0713190580463,
0.));
#150498=CARTESIAN_POINT('Ctrl Pts',(-62.1536782583199,38.0508036793939,
0.));
#150499=CARTESIAN_POINT('Ctrl Pts',(-62.1383996223125,38.0303339808053,
0.));
#150500=CARTESIAN_POINT('Ctrl Pts',(-62.123125053455,38.0099100125037,0.));
#150501=CARTESIAN_POINT('Ctrl Pts',(-62.107854656528,37.9895318248212,0.));
#150502=CARTESIAN_POINT('Ctrl Pts',(-62.0925885367352,37.9691994681966,
0.));
#150503=CARTESIAN_POINT('Ctrl Pts',(-62.0773267997079,37.9489129931689,
0.));
#150504=CARTESIAN_POINT('Ctrl Pts',(-62.0620695515074,37.9286724503851,
0.));
#150505=CARTESIAN_POINT('Ctrl Pts',(-62.0468168986288,37.9084778906053,
0.));
#150506=CARTESIAN_POINT('Ctrl Pts',(-62.031568948002,37.8883293647029,0.));
#150507=CARTESIAN_POINT('Ctrl Pts',(-62.0163258069957,37.868226923663,0.));
#150508=CARTESIAN_POINT('Ctrl Pts',(-62.0010875834187,37.8481706185749,
0.));
#150509=CARTESIAN_POINT('Ctrl Pts',(-61.9858543855236,37.828160500638,0.));
#150510=CARTESIAN_POINT('Ctrl Pts',(-61.9706263220114,37.8081966211689,
0.));
#150511=CARTESIAN_POINT('Ctrl Pts',(-61.9554035020338,37.7882790316014,
0.));
#150512=CARTESIAN_POINT('Ctrl Pts',(-61.9401860351972,37.7684077834872,
0.));
#150513=CARTESIAN_POINT('Ctrl Pts',(-61.9249740315649,37.7485829284871,
0.));
#150514=CARTESIAN_POINT('Ctrl Pts',(-61.9097676016601,37.7288045183756,
0.));
#150515=CARTESIAN_POINT('Ctrl Pts',(-61.8945668564704,37.7090726050482,
0.));
#150516=CARTESIAN_POINT('Ctrl Pts',(-61.8793719074507,37.6893872405228,
0.));
#150517=CARTESIAN_POINT('Ctrl Pts',(-61.8641828665261,37.6697484769392,
0.));
#150518=CARTESIAN_POINT('Ctrl Pts',(-61.8489998460957,37.6501563665523,
0.));
#150519=CARTESIAN_POINT('Ctrl Pts',(-61.8338229590353,37.6306109617346,
0.));
#150520=CARTESIAN_POINT('Ctrl Pts',(-61.8186523187015,37.6111123149839,
0.));
#150521=CARTESIAN_POINT('Ctrl Pts',(-61.8034880389362,37.5916604789253,
0.));
#150522=CARTESIAN_POINT('Ctrl Pts',(-61.7883302340687,37.5722555063111,
0.));
#150523=CARTESIAN_POINT('Ctrl Pts',(-61.7731790189191,37.5528974500142,
0.));
#150524=CARTESIAN_POINT('Ctrl Pts',(-61.7580345088016,37.5335863630287,
0.));
#150525=CARTESIAN_POINT('Ctrl Pts',(-61.7428968195299,37.5143222984796,
0.));
#150526=CARTESIAN_POINT('Ctrl Pts',(-61.7277660674205,37.4951053096237,
0.));
#150527=CARTESIAN_POINT('Ctrl Pts',(-61.7126423692963,37.4759354498509,
0.));
#150528=CARTESIAN_POINT('Ctrl Pts',(-61.6975258424894,37.4568127726773,
0.));
#150529=CARTESIAN_POINT('Ctrl Pts',(-61.6824166048444,37.4377373317451,
0.));
#150530=CARTESIAN_POINT('Ctrl Pts',(-61.6673147747242,37.4187091808321,
0.));
#150531=CARTESIAN_POINT('Ctrl Pts',(-61.6522204710131,37.3997283738533,
0.));
#150532=CARTESIAN_POINT('Ctrl Pts',(-61.637133813121,37.3807949648624,0.));
#150533=CARTESIAN_POINT('Ctrl Pts',(-61.6220549209866,37.361909008045,0.));
#150534=CARTESIAN_POINT('Ctrl Pts',(-61.6069839150807,37.343070557718,0.));
#150535=CARTESIAN_POINT('Ctrl Pts',(-61.591920916412,37.3242796683395,0.));
#150536=CARTESIAN_POINT('Ctrl Pts',(-61.5768660465311,37.3055363945107,
0.));
#150537=CARTESIAN_POINT('Ctrl Pts',(-61.5618194275348,37.286840790977,0.));
#150538=CARTESIAN_POINT('Ctrl Pts',(-61.5467811820691,37.2681929126221,
0.));
#150539=CARTESIAN_POINT('Ctrl Pts',(-61.5317514333328,37.2495928144667,
0.));
#150540=CARTESIAN_POINT('Ctrl Pts',(-61.5167303050832,37.2310405516781,
0.));
#150541=CARTESIAN_POINT('Ctrl Pts',(-61.501717921641,37.2125361795731,0.));
#150542=CARTESIAN_POINT('Ctrl Pts',(-61.4867144078936,37.1940797536181,
0.));
#150543=CARTESIAN_POINT('Ctrl Pts',(-61.4717198892994,37.175671329424,0.));
#150544=CARTESIAN_POINT('Ctrl Pts',(-61.4567344918919,37.1573109627454,
0.));
#150545=CARTESIAN_POINT('Ctrl Pts',(-61.4417583422863,37.1389987094905,
0.));
#150546=CARTESIAN_POINT('Ctrl Pts',(-61.4267915676822,37.1207346257222,
0.));
#150547=CARTESIAN_POINT('Ctrl Pts',(-61.4118342958697,37.1025187676602,
0.));
#150548=CARTESIAN_POINT('Ctrl Pts',(-61.3968866552317,37.0843511916745,
0.));
#150549=CARTESIAN_POINT('Ctrl Pts',(-61.381948774749,37.0662319542849,0.));
#150550=CARTESIAN_POINT('Ctrl Pts',(-61.3670207840069,37.0481611121717,
0.));
#150551=CARTESIAN_POINT('Ctrl Pts',(-61.3521028132003,37.0301387221774,
0.));
#150552=CARTESIAN_POINT('Ctrl Pts',(-61.3371949931387,37.0121648413082,
0.));
#150553=CARTESIAN_POINT('Ctrl Pts',(-61.3222974552487,36.994239526727,0.));
#150554=CARTESIAN_POINT('Ctrl Pts',(-61.3074103315792,36.9763628357544,
0.));
#150555=CARTESIAN_POINT('Ctrl Pts',(-61.2925337548077,36.9585348258776,
0.));
#150556=CARTESIAN_POINT('Ctrl Pts',(-61.2776678582461,36.9407555547535,
0.));
#150557=CARTESIAN_POINT('Ctrl Pts',(-61.2628127758457,36.9230250802087,
0.));
#150558=CARTESIAN_POINT('Ctrl Pts',(-61.247968642201,36.9053434602343,0.));
#150559=CARTESIAN_POINT('Ctrl Pts',(-61.2331355925547,36.8877107529865,
0.));
#150560=CARTESIAN_POINT('Ctrl Pts',(-61.2183137628056,36.8701270167969,
0.));
#150561=CARTESIAN_POINT('Ctrl Pts',(-61.2035032895127,36.852592310174,0.));
#150562=CARTESIAN_POINT('Ctrl Pts',(-61.1887043099014,36.8351066918036,
0.));
#150563=CARTESIAN_POINT('Ctrl Pts',(-61.1739169618666,36.8176702205423,
0.));
#150564=CARTESIAN_POINT('Ctrl Pts',(-61.1591413839787,36.8002829554209,
0.));
#150565=CARTESIAN_POINT('Ctrl Pts',(-61.1443777154911,36.7829449556532,
0.));
#150566=CARTESIAN_POINT('Ctrl Pts',(-61.1296260963466,36.765656280638,0.));
#150567=CARTESIAN_POINT('Ctrl Pts',(-61.1148866671829,36.7484169899596,
0.));
#150568=CARTESIAN_POINT('Ctrl Pts',(-61.100159569337,36.7312271433807,0.));
#150569=CARTESIAN_POINT('Ctrl Pts',(-61.0854449448524,36.7140868008486,
0.));
#150570=CARTESIAN_POINT('Ctrl Pts',(-61.0707429364847,36.6969960225022,
0.));
#150571=CARTESIAN_POINT('Ctrl Pts',(-61.0560536877083,36.679954868674,0.));
#150572=CARTESIAN_POINT('Ctrl Pts',(-61.0413773427203,36.6629633998886,
0.));
#150573=CARTESIAN_POINT('Ctrl Pts',(-61.0267140464432,36.6460216768553,
0.));
#150574=CARTESIAN_POINT('Ctrl Pts',(-61.0120639445349,36.6291297604776,
0.));
#150575=CARTESIAN_POINT('Ctrl Pts',(-60.9974271833981,36.61228771186,0.));
#150576=CARTESIAN_POINT('Ctrl Pts',(-60.9828039101887,36.5954955923109,
0.));
#150577=CARTESIAN_POINT('Ctrl Pts',(-60.9681942728236,36.5787534633416,
0.));
#150578=CARTESIAN_POINT('Ctrl Pts',(-60.9535984199873,36.5620613866615,
0.));
#150579=CARTESIAN_POINT('Ctrl Pts',(-60.9390165011355,36.5454194241865,
0.));
#150580=CARTESIAN_POINT('Ctrl Pts',(-60.9244486664988,36.5288276380416,
0.));
#150581=CARTESIAN_POINT('Ctrl Pts',(-60.9098950670847,36.5122860905612,
0.));
#150582=CARTESIAN_POINT('Ctrl Pts',(-60.8953558546795,36.4957948442835,
0.));
#150583=CARTESIAN_POINT('Ctrl Pts',(-60.8808311818499,36.4793539619466,
0.));
#150584=CARTESIAN_POINT('Ctrl Pts',(-60.8663212019657,36.4629635065045,
0.));
#150585=CARTESIAN_POINT('Ctrl Pts',(-60.8518260692188,36.4466235411358,
0.));
#150586=CARTESIAN_POINT('Ctrl Pts',(-60.8373459386392,36.4303341292494,
0.));
#150587=CARTESIAN_POINT('Ctrl Pts',(-60.822880966116,36.4140953344858,0.));
#150588=CARTESIAN_POINT('Ctrl Pts',(-60.8084313083984,36.397907220716,0.));
#150589=CARTESIAN_POINT('Ctrl Pts',(-60.793997123076,36.3817698520388,0.));
#150590=CARTESIAN_POINT('Ctrl Pts',(-60.7795785685625,36.365683292773,0.));
#150591=CARTESIAN_POINT('Ctrl Pts',(-60.7651758040803,36.3496476074488,
0.));
#150592=CARTESIAN_POINT('Ctrl Pts',(-60.7507889896308,36.3336628607859,
0.));
#150593=CARTESIAN_POINT('Ctrl Pts',(-60.7364182860412,36.3177291177163,
0.));
#150594=CARTESIAN_POINT('Ctrl Pts',(-60.722063855041,36.3018464434213,0.));
#150595=CARTESIAN_POINT('Ctrl Pts',(-60.7077258593268,36.2860149033587,
0.));
#150596=CARTESIAN_POINT('Ctrl Pts',(-60.6934044626291,36.2702345632875,
0.));
#150597=CARTESIAN_POINT('Ctrl Pts',(-60.67909982978,36.2545054892897,0.));
#150598=CARTESIAN_POINT('Ctrl Pts',(-60.6648121265885,36.2388277477212,
0.));
#150599=CARTESIAN_POINT('Ctrl Pts',(-60.6505415197042,36.2232014051541,
0.));
#150600=CARTESIAN_POINT('Ctrl Pts',(-60.6362881765019,36.2076265283264,
0.));
#150601=CARTESIAN_POINT('Ctrl Pts',(-60.6220522649149,36.192103184063,0.));
#150602=CARTESIAN_POINT('Ctrl Pts',(-60.6078339534181,36.1766314392641,
0.));
#150603=CARTESIAN_POINT('Ctrl Pts',(-60.5936334114108,36.1612113610773,
0.));
#150604=CARTESIAN_POINT('Ctrl Pts',(-60.5794508095565,36.1458430170431,
0.));
#150605=CARTESIAN_POINT('Ctrl Pts',(-60.565286320072,36.1305264752188,0.));
#150606=CARTESIAN_POINT('Ctrl Pts',(-60.5511401171984,36.1152618043739,
0.));
#150607=CARTESIAN_POINT('Ctrl Pts',(-60.5370123768804,36.100049073851,0.));
#150608=CARTESIAN_POINT('Ctrl Pts',(-60.5229032758974,36.0848883531952,
0.));
#150609=CARTESIAN_POINT('Ctrl Pts',(-60.5088129911354,36.0697797118376,
0.));
#150610=CARTESIAN_POINT('Ctrl Pts',(-60.4947416988422,36.0547232187698,
0.));
#150611=CARTESIAN_POINT('Ctrl Pts',(-60.4806895737686,36.0397189421644,
0.));
#150612=CARTESIAN_POINT('Ctrl Pts',(-60.4666567908093,36.0247669500891,
0.));
#150613=CARTESIAN_POINT('Ctrl Pts',(-60.4526435269662,36.009867311357,0.));
#150614=CARTESIAN_POINT('Ctrl Pts',(-60.4386499629481,35.995020096217,0.));
#150615=CARTESIAN_POINT('Ctrl Pts',(-60.4246762854926,35.9802253773515,
0.));
#150616=CARTESIAN_POINT('Ctrl Pts',(-60.4107226875714,35.9654832299601,
0.));
#150617=CARTESIAN_POINT('Ctrl Pts',(-60.3967893635452,35.9507937296707,
0.));
#150618=CARTESIAN_POINT('Ctrl Pts',(-60.3828765049019,35.936156950695,0.));
#150619=CARTESIAN_POINT('Ctrl Pts',(-60.3689842965481,35.9215729642231,
0.));
#150620=CARTESIAN_POINT('Ctrl Pts',(-60.3551129108845,35.907041835853,0.));
#150621=CARTESIAN_POINT('Ctrl Pts',(-60.3412625135287,35.8925636280668,
0.));
#150622=CARTESIAN_POINT('Ctrl Pts',(-60.327433274683,35.8781384051537,0.));
#150623=CARTESIAN_POINT('Ctrl Pts',(-60.313625378281,35.8637662371635,0.));
#150624=CARTESIAN_POINT('Ctrl Pts',(-60.2998390330102,35.8494472046745,
0.));
#150625=CARTESIAN_POINT('Ctrl Pts',(-60.2860744798436,35.8351814020357,
0.));
#150626=CARTESIAN_POINT('Ctrl Pts',(-60.2723319687369,35.8209689272501,
0.));
#150627=CARTESIAN_POINT('Ctrl Pts',(-60.2586117365205,35.8068098723347,
0.));
#150628=CARTESIAN_POINT('Ctrl Pts',(-60.2449139865275,35.7927043145201,
0.));
#150629=CARTESIAN_POINT('Ctrl Pts',(-60.2312388621529,35.7786523045912,
0.));
#150630=CARTESIAN_POINT('Ctrl Pts',(-60.2175864450043,35.7646538667493,
0.));
#150631=CARTESIAN_POINT('Ctrl Pts',(-60.206682708692,35.7534979802053,0.));
#150632=CARTESIAN_POINT('Ctrl Pts',(-60.1985151474623,35.7451551752572,
0.));
#150633=CARTESIAN_POINT('Ctrl Pts',(-60.193074658032,35.7396040204017,0.));
#150634=CARTESIAN_POINT('Ctrl Pts',(-60.1903555511633,35.736831121751,0.));
#150635=CARTESIAN_POINT('Ctrl Pts',(-59.483083043136,44.8554660179045,0.));
#150636=CARTESIAN_POINT('Ctrl Pts',(-59.483083043136,44.8554660179045,12.));
#150637=CARTESIAN_POINT('Ctrl Pts',(-59.4804358983083,44.8505359826461,
0.));
#150638=CARTESIAN_POINT('Ctrl Pts',(-59.4804358983083,44.8505359826461,
12.));
#150639=CARTESIAN_POINT('Ctrl Pts',(-59.4751410547732,44.8406801497742,
0.));
#150640=CARTESIAN_POINT('Ctrl Pts',(-59.4751410547732,44.8406801497742,
12.));
#150641=CARTESIAN_POINT('Ctrl Pts',(-59.4671971278321,44.8259091134016,
0.));
#150642=CARTESIAN_POINT('Ctrl Pts',(-59.4671971278321,44.8259091134016,
12.));
#150643=CARTESIAN_POINT('Ctrl Pts',(-59.4566019018254,44.8062398251406,
0.));
#150644=CARTESIAN_POINT('Ctrl Pts',(-59.4566019018254,44.8062398251406,
12.));
#150645=CARTESIAN_POINT('Ctrl Pts',(-59.4433523335147,44.7816956017528,
0.));
#150646=CARTESIAN_POINT('Ctrl Pts',(-59.4433523335147,44.7816956017528,
12.));
#150647=CARTESIAN_POINT('Ctrl Pts',(-59.430097240324,44.7571937812113,0.));
#150648=CARTESIAN_POINT('Ctrl Pts',(-59.430097240324,44.7571937812113,12.));
#150649=CARTESIAN_POINT('Ctrl Pts',(-59.4168366453118,44.7327343876391,
0.));
#150650=CARTESIAN_POINT('Ctrl Pts',(-59.4168366453118,44.7327343876391,
12.));
#150651=CARTESIAN_POINT('Ctrl Pts',(-59.4035705873811,44.7083174541702,
0.));
#150652=CARTESIAN_POINT('Ctrl Pts',(-59.4035705873811,44.7083174541702,
12.));
#150653=CARTESIAN_POINT('Ctrl Pts',(-59.3902991267889,44.683943024421,0.));
#150654=CARTESIAN_POINT('Ctrl Pts',(-59.3902991267889,44.683943024421,12.));
#150655=CARTESIAN_POINT('Ctrl Pts',(-59.377022343519,44.6596111512687,0.));
#150656=CARTESIAN_POINT('Ctrl Pts',(-59.377022343519,44.6596111512687,12.));
#150657=CARTESIAN_POINT('Ctrl Pts',(-59.3637403301801,44.6353218935685,
0.));
#150658=CARTESIAN_POINT('Ctrl Pts',(-59.3637403301801,44.6353218935685,
12.));
#150659=CARTESIAN_POINT('Ctrl Pts',(-59.3504531864154,44.6110753134277,
0.));
#150660=CARTESIAN_POINT('Ctrl Pts',(-59.3504531864154,44.6110753134277,
12.));
#150661=CARTESIAN_POINT('Ctrl Pts',(-59.3371610128511,44.5868714733234,
0.));
#150662=CARTESIAN_POINT('Ctrl Pts',(-59.3371610128511,44.5868714733234,
12.));
#150663=CARTESIAN_POINT('Ctrl Pts',(-59.3238639048694,44.5627104331017,
0.));
#150664=CARTESIAN_POINT('Ctrl Pts',(-59.3238639048694,44.5627104331017,
12.));
#150665=CARTESIAN_POINT('Ctrl Pts',(-59.3105619475609,44.5385922475573,
0.));
#150666=CARTESIAN_POINT('Ctrl Pts',(-59.3105619475609,44.5385922475573,
12.));
#150667=CARTESIAN_POINT('Ctrl Pts',(-59.2972552192156,44.5145169681349,
0.));
#150668=CARTESIAN_POINT('Ctrl Pts',(-59.2972552192156,44.5145169681349,
12.));
#150669=CARTESIAN_POINT('Ctrl Pts',(-59.2839437938237,44.490484644151,0.));
#150670=CARTESIAN_POINT('Ctrl Pts',(-59.2839437938237,44.490484644151,12.));
#150671=CARTESIAN_POINT('Ctrl Pts',(-59.2706277440445,44.4664953242379,
0.));
#150672=CARTESIAN_POINT('Ctrl Pts',(-59.2706277440445,44.4664953242379,
12.));
#150673=CARTESIAN_POINT('Ctrl Pts',(-59.2573071437774,44.4425490575911,
0.));
#150674=CARTESIAN_POINT('Ctrl Pts',(-59.2573071437774,44.4425490575911,
12.));
#150675=CARTESIAN_POINT('Ctrl Pts',(-59.2439820714187,44.4186458955451,
0.));
#150676=CARTESIAN_POINT('Ctrl Pts',(-59.2439820714187,44.4186458955451,
12.));
#150677=CARTESIAN_POINT('Ctrl Pts',(-59.2306526095131,44.3947858914074,
0.));
#150678=CARTESIAN_POINT('Ctrl Pts',(-59.2306526095131,44.3947858914074,
12.));
#150679=CARTESIAN_POINT('Ctrl Pts',(-59.2173188432798,44.3709690997469,
0.));
#150680=CARTESIAN_POINT('Ctrl Pts',(-59.2173188432798,44.3709690997469,
12.));
#150681=CARTESIAN_POINT('Ctrl Pts',(-59.2039808594752,44.3471955758403,
0.));
#150682=CARTESIAN_POINT('Ctrl Pts',(-59.2039808594752,44.3471955758403,
12.));
#150683=CARTESIAN_POINT('Ctrl Pts',(-59.1906387451979,44.3234653750884,
0.));
#150684=CARTESIAN_POINT('Ctrl Pts',(-59.1906387451979,44.3234653750884,
12.));
#150685=CARTESIAN_POINT('Ctrl Pts',(-59.1772925865213,44.2997785523431,
0.));
#150686=CARTESIAN_POINT('Ctrl Pts',(-59.1772925865213,44.2997785523431,
12.));
#150687=CARTESIAN_POINT('Ctrl Pts',(-59.1639424678793,44.2761351616048,
0.));
#150688=CARTESIAN_POINT('Ctrl Pts',(-59.1639424678793,44.2761351616048,
12.));
#150689=CARTESIAN_POINT('Ctrl Pts',(-59.1505884728215,44.2525352563996,
0.));
#150690=CARTESIAN_POINT('Ctrl Pts',(-59.1505884728215,44.2525352563996,
12.));
#150691=CARTESIAN_POINT('Ctrl Pts',(-59.1372306844586,44.228978889997,0.));
#150692=CARTESIAN_POINT('Ctrl Pts',(-59.1372306844586,44.228978889997,12.));
#150693=CARTESIAN_POINT('Ctrl Pts',(-59.1238691860306,44.2054661156875,
0.));
#150694=CARTESIAN_POINT('Ctrl Pts',(-59.1238691860306,44.2054661156875,
12.));
#150695=CARTESIAN_POINT('Ctrl Pts',(-59.1105040614276,44.1819969870307,
0.));
#150696=CARTESIAN_POINT('Ctrl Pts',(-59.1105040614276,44.1819969870307,
12.));
#150697=CARTESIAN_POINT('Ctrl Pts',(-59.0971353957206,44.1585715581064,
0.));
#150698=CARTESIAN_POINT('Ctrl Pts',(-59.0971353957206,44.1585715581064,
12.));
#150699=CARTESIAN_POINT('Ctrl Pts',(-59.08376327492,44.1351898834051,0.));
#150700=CARTESIAN_POINT('Ctrl Pts',(-59.08376327492,44.1351898834051,12.));
#150701=CARTESIAN_POINT('Ctrl Pts',(-59.0703877857526,44.1118520177221,
0.));
#150702=CARTESIAN_POINT('Ctrl Pts',(-59.0703877857526,44.1118520177221,
12.));
#150703=CARTESIAN_POINT('Ctrl Pts',(-59.0570090154243,44.0885580160432,
0.));
#150704=CARTESIAN_POINT('Ctrl Pts',(-59.0570090154243,44.0885580160432,
12.));
#150705=CARTESIAN_POINT('Ctrl Pts',(-59.0436270514087,44.0653079334385,
0.));
#150706=CARTESIAN_POINT('Ctrl Pts',(-59.0436270514087,44.0653079334385,
12.));
#150707=CARTESIAN_POINT('Ctrl Pts',(-59.0302419811777,44.0421018249223,
0.));
#150708=CARTESIAN_POINT('Ctrl Pts',(-59.0302419811777,44.0421018249223,
12.));
#150709=CARTESIAN_POINT('Ctrl Pts',(-59.0168538922095,44.0189397454599,
0.));
#150710=CARTESIAN_POINT('Ctrl Pts',(-59.0168538922095,44.0189397454599,
12.));
#150711=CARTESIAN_POINT('Ctrl Pts',(-59.0034628721168,43.9958217500369,
0.));
#150712=CARTESIAN_POINT('Ctrl Pts',(-59.0034628721168,43.9958217500369,
12.));
#150713=CARTESIAN_POINT('Ctrl Pts',(-58.9900690087408,43.9727478937056,
0.));
#150714=CARTESIAN_POINT('Ctrl Pts',(-58.9900690087408,43.9727478937056,
12.));
#150715=CARTESIAN_POINT('Ctrl Pts',(-58.9766723902529,43.9497182316331,
0.));
#150716=CARTESIAN_POINT('Ctrl Pts',(-58.9766723902529,43.9497182316331,
12.));
#150717=CARTESIAN_POINT('Ctrl Pts',(-58.9632731052696,43.9267328191501,
0.));
#150718=CARTESIAN_POINT('Ctrl Pts',(-58.9632731052696,43.9267328191501,
12.));
#150719=CARTESIAN_POINT('Ctrl Pts',(-58.9498712429054,43.9037917117739,
0.));
#150720=CARTESIAN_POINT('Ctrl Pts',(-58.9498712429054,43.9037917117739,
12.));
#150721=CARTESIAN_POINT('Ctrl Pts',(-58.936466892712,43.8808949651873,0.));
#150722=CARTESIAN_POINT('Ctrl Pts',(-58.936466892712,43.8808949651873,12.));
#150723=CARTESIAN_POINT('Ctrl Pts',(-58.9230601446436,43.858042635223,0.));
#150724=CARTESIAN_POINT('Ctrl Pts',(-58.9230601446436,43.858042635223,12.));
#150725=CARTESIAN_POINT('Ctrl Pts',(-58.9096510890129,43.835234777842,0.));
#150726=CARTESIAN_POINT('Ctrl Pts',(-58.9096510890129,43.835234777842,12.));
#150727=CARTESIAN_POINT('Ctrl Pts',(-58.8962398164493,43.8124714491076,
0.));
#150728=CARTESIAN_POINT('Ctrl Pts',(-58.8962398164493,43.8124714491076,
12.));
#150729=CARTESIAN_POINT('Ctrl Pts',(-58.8828264178621,43.7897527051609,
0.));
#150730=CARTESIAN_POINT('Ctrl Pts',(-58.8828264178621,43.7897527051609,
12.));
#150731=CARTESIAN_POINT('Ctrl Pts',(-58.8694109844648,43.7670786022402,
0.));
#150732=CARTESIAN_POINT('Ctrl Pts',(-58.8694109844648,43.7670786022402,
12.));
#150733=CARTESIAN_POINT('Ctrl Pts',(-58.855993607794,43.7444491966942,0.));
#150734=CARTESIAN_POINT('Ctrl Pts',(-58.855993607794,43.7444491966942,12.));
#150735=CARTESIAN_POINT('Ctrl Pts',(-58.8425743797326,43.7218645449922,
0.));
#150736=CARTESIAN_POINT('Ctrl Pts',(-58.8425743797326,43.7218645449922,
12.));
#150737=CARTESIAN_POINT('Ctrl Pts',(-58.8291533925293,43.6993247037314,
0.));
#150738=CARTESIAN_POINT('Ctrl Pts',(-58.8291533925293,43.6993247037314,
12.));
#150739=CARTESIAN_POINT('Ctrl Pts',(-58.8157307388238,43.6768297296395,
0.));
#150740=CARTESIAN_POINT('Ctrl Pts',(-58.8157307388238,43.6768297296395,
12.));
#150741=CARTESIAN_POINT('Ctrl Pts',(-58.8023065116436,43.6543796795789,
0.));
#150742=CARTESIAN_POINT('Ctrl Pts',(-58.8023065116436,43.6543796795789,
12.));
#150743=CARTESIAN_POINT('Ctrl Pts',(-58.788880804397,43.6319746105482,0.));
#150744=CARTESIAN_POINT('Ctrl Pts',(-58.788880804397,43.6319746105482,12.));
#150745=CARTESIAN_POINT('Ctrl Pts',(-58.775453710867,43.6096145796797,0.));
#150746=CARTESIAN_POINT('Ctrl Pts',(-58.775453710867,43.6096145796797,12.));
#150747=CARTESIAN_POINT('Ctrl Pts',(-58.7620253252062,43.5872996442345,
0.));
#150748=CARTESIAN_POINT('Ctrl Pts',(-58.7620253252062,43.5872996442345,
12.));
#150749=CARTESIAN_POINT('Ctrl Pts',(-58.74859574193,43.5650298615917,0.));
#150750=CARTESIAN_POINT('Ctrl Pts',(-58.74859574193,43.5650298615917,12.));
#150751=CARTESIAN_POINT('Ctrl Pts',(-58.735165055918,43.5428052892488,0.));
#150752=CARTESIAN_POINT('Ctrl Pts',(-58.735165055918,43.5428052892488,12.));
#150753=CARTESIAN_POINT('Ctrl Pts',(-58.7217333624209,43.5206259848337,
0.));
#150754=CARTESIAN_POINT('Ctrl Pts',(-58.7217333624209,43.5206259848337,
12.));
#150755=CARTESIAN_POINT('Ctrl Pts',(-58.7083007570661,43.4984920061073,
0.));
#150756=CARTESIAN_POINT('Ctrl Pts',(-58.7083007570661,43.4984920061073,
12.));
#150757=CARTESIAN_POINT('Ctrl Pts',(-58.6948673358638,43.4764034109654,
0.));
#150758=CARTESIAN_POINT('Ctrl Pts',(-58.6948673358638,43.4764034109654,
12.));
#150759=CARTESIAN_POINT('Ctrl Pts',(-58.6814331952138,43.4543602574351,
0.));
#150760=CARTESIAN_POINT('Ctrl Pts',(-58.6814331952138,43.4543602574351,
12.));
#150761=CARTESIAN_POINT('Ctrl Pts',(-58.6679984319097,43.4323626036737,
0.));
#150762=CARTESIAN_POINT('Ctrl Pts',(-58.6679984319097,43.4323626036737,
12.));
#150763=CARTESIAN_POINT('Ctrl Pts',(-58.6545631431393,43.4104105079768,
0.));
#150764=CARTESIAN_POINT('Ctrl Pts',(-58.6545631431393,43.4104105079768,
12.));
#150765=CARTESIAN_POINT('Ctrl Pts',(-58.6411274264857,43.388504028781,0.));
#150766=CARTESIAN_POINT('Ctrl Pts',(-58.6411274264857,43.388504028781,12.));
#150767=CARTESIAN_POINT('Ctrl Pts',(-58.627691379929,43.3666432246635,0.));
#150768=CARTESIAN_POINT('Ctrl Pts',(-58.627691379929,43.3666432246635,12.));
#150769=CARTESIAN_POINT('Ctrl Pts',(-58.6142551018467,43.3448281543371,
0.));
#150770=CARTESIAN_POINT('Ctrl Pts',(-58.6142551018467,43.3448281543371,
12.));
#150771=CARTESIAN_POINT('Ctrl Pts',(-58.6008186910156,43.3230588766449,
0.));
#150772=CARTESIAN_POINT('Ctrl Pts',(-58.6008186910156,43.3230588766449,
12.));
#150773=CARTESIAN_POINT('Ctrl Pts',(-58.5873822466152,43.3013354505701,
0.));
#150774=CARTESIAN_POINT('Ctrl Pts',(-58.5873822466152,43.3013354505701,
12.));
#150775=CARTESIAN_POINT('Ctrl Pts',(-58.573945868231,43.27965793524,0.));
#150776=CARTESIAN_POINT('Ctrl Pts',(-58.573945868231,43.27965793524,12.));
#150777=CARTESIAN_POINT('Ctrl Pts',(-58.5605096558578,43.2580263899278,
0.));
#150778=CARTESIAN_POINT('Ctrl Pts',(-58.5605096558578,43.2580263899278,
12.));
#150779=CARTESIAN_POINT('Ctrl Pts',(-58.5470737099032,43.2364408740493,
0.));
#150780=CARTESIAN_POINT('Ctrl Pts',(-58.5470737099032,43.2364408740493,
12.));
#150781=CARTESIAN_POINT('Ctrl Pts',(-58.5336381311917,43.2149014471574,
0.));
#150782=CARTESIAN_POINT('Ctrl Pts',(-58.5336381311917,43.2149014471574,
12.));
#150783=CARTESIAN_POINT('Ctrl Pts',(-58.5202030209669,43.1934081689505,
0.));
#150784=CARTESIAN_POINT('Ctrl Pts',(-58.5202030209669,43.1934081689505,
12.));
#150785=CARTESIAN_POINT('Ctrl Pts',(-58.5067684808944,43.1719610992771,
0.));
#150786=CARTESIAN_POINT('Ctrl Pts',(-58.5067684808944,43.1719610992771,
12.));
#150787=CARTESIAN_POINT('Ctrl Pts',(-58.4933346130636,43.1505602981365,
0.));
#150788=CARTESIAN_POINT('Ctrl Pts',(-58.4933346130636,43.1505602981365,
12.));
#150789=CARTESIAN_POINT('Ctrl Pts',(-58.4799015199907,43.1292058256777,
0.));
#150790=CARTESIAN_POINT('Ctrl Pts',(-58.4799015199907,43.1292058256777,
12.));
#150791=CARTESIAN_POINT('Ctrl Pts',(-58.4664693046217,43.1078977421916,
0.));
#150792=CARTESIAN_POINT('Ctrl Pts',(-58.4664693046217,43.1078977421916,
12.));
#150793=CARTESIAN_POINT('Ctrl Pts',(-58.4530380703348,43.0866361081177,
0.));
#150794=CARTESIAN_POINT('Ctrl Pts',(-58.4530380703348,43.0866361081177,
12.));
#150795=CARTESIAN_POINT('Ctrl Pts',(-58.439607920945,43.0654209840511,0.));
#150796=CARTESIAN_POINT('Ctrl Pts',(-58.439607920945,43.0654209840511,12.));
#150797=CARTESIAN_POINT('Ctrl Pts',(-58.4261789607058,43.0442524307434,
0.));
#150798=CARTESIAN_POINT('Ctrl Pts',(-58.4261789607058,43.0442524307434,
12.));
#150799=CARTESIAN_POINT('Ctrl Pts',(-58.4127512943136,43.0231305091027,
0.));
#150800=CARTESIAN_POINT('Ctrl Pts',(-58.4127512943136,43.0231305091027,
12.));
#150801=CARTESIAN_POINT('Ctrl Pts',(-58.3993250269101,43.0020552801859,
0.));
#150802=CARTESIAN_POINT('Ctrl Pts',(-58.3993250269101,43.0020552801859,
12.));
#150803=CARTESIAN_POINT('Ctrl Pts',(-58.3859002640856,42.9810268052032,
0.));
#150804=CARTESIAN_POINT('Ctrl Pts',(-58.3859002640856,42.9810268052032,
12.));
#150805=CARTESIAN_POINT('Ctrl Pts',(-58.3724771118826,42.960045145526,0.));
#150806=CARTESIAN_POINT('Ctrl Pts',(-58.3724771118826,42.960045145526,12.));
#150807=CARTESIAN_POINT('Ctrl Pts',(-58.3590556767978,42.9391103626879,
0.));
#150808=CARTESIAN_POINT('Ctrl Pts',(-58.3590556767978,42.9391103626879,
12.));
#150809=CARTESIAN_POINT('Ctrl Pts',(-58.3456360657865,42.9182225183855,
0.));
#150810=CARTESIAN_POINT('Ctrl Pts',(-58.3456360657865,42.9182225183855,
12.));
#150811=CARTESIAN_POINT('Ctrl Pts',(-58.3322183862654,42.8973816744709,
0.));
#150812=CARTESIAN_POINT('Ctrl Pts',(-58.3322183862654,42.8973816744709,
12.));
#150813=CARTESIAN_POINT('Ctrl Pts',(-58.3188027461164,42.8765878929551,
0.));
#150814=CARTESIAN_POINT('Ctrl Pts',(-58.3188027461164,42.8765878929551,
12.));
#150815=CARTESIAN_POINT('Ctrl Pts',(-58.3053892536894,42.8558412360158,
0.));
#150816=CARTESIAN_POINT('Ctrl Pts',(-58.3053892536894,42.8558412360158,
12.));
#150817=CARTESIAN_POINT('Ctrl Pts',(-58.2919780178064,42.8351417659999,
0.));
#150818=CARTESIAN_POINT('Ctrl Pts',(-58.2919780178064,42.8351417659999,
12.));
#150819=CARTESIAN_POINT('Ctrl Pts',(-58.2785691477638,42.8144895454233,
0.));
#150820=CARTESIAN_POINT('Ctrl Pts',(-58.2785691477638,42.8144895454233,
12.));
#150821=CARTESIAN_POINT('Ctrl Pts',(-58.2651627533368,42.7938846369651,
0.));
#150822=CARTESIAN_POINT('Ctrl Pts',(-58.2651627533368,42.7938846369651,
12.));
#150823=CARTESIAN_POINT('Ctrl Pts',(-58.251758944782,42.7733271034679,0.));
#150824=CARTESIAN_POINT('Ctrl Pts',(-58.251758944782,42.7733271034679,12.));
#150825=CARTESIAN_POINT('Ctrl Pts',(-58.2383578328424,42.7528170079484,
0.));
#150826=CARTESIAN_POINT('Ctrl Pts',(-58.2383578328424,42.7528170079484,
12.));
#150827=CARTESIAN_POINT('Ctrl Pts',(-58.22495952875,42.7323544135985,0.));
#150828=CARTESIAN_POINT('Ctrl Pts',(-58.22495952875,42.7323544135985,12.));
#150829=CARTESIAN_POINT('Ctrl Pts',(-58.21156414423,42.7119393837866,0.));
#150830=CARTESIAN_POINT('Ctrl Pts',(-58.21156414423,42.7119393837866,12.));
#150831=CARTESIAN_POINT('Ctrl Pts',(-58.1981717915037,42.6915719820513,
0.));
#150832=CARTESIAN_POINT('Ctrl Pts',(-58.1981717915037,42.6915719820513,
12.));
#150833=CARTESIAN_POINT('Ctrl Pts',(-58.1847825832923,42.6712522721016,
0.));
#150834=CARTESIAN_POINT('Ctrl Pts',(-58.1847825832923,42.6712522721016,
12.));
#150835=CARTESIAN_POINT('Ctrl Pts',(-58.171396632821,42.6509803178265,0.));
#150836=CARTESIAN_POINT('Ctrl Pts',(-58.171396632821,42.6509803178265,12.));
#150837=CARTESIAN_POINT('Ctrl Pts',(-58.1580140538228,42.6307561832976,
0.));
#150838=CARTESIAN_POINT('Ctrl Pts',(-58.1580140538228,42.6307561832976,
12.));
#150839=CARTESIAN_POINT('Ctrl Pts',(-58.1446349605421,42.6105799327699,
0.));
#150840=CARTESIAN_POINT('Ctrl Pts',(-58.1446349605421,42.6105799327699,
12.));
#150841=CARTESIAN_POINT('Ctrl Pts',(-58.1312594677386,42.5904516306762,
0.));
#150842=CARTESIAN_POINT('Ctrl Pts',(-58.1312594677386,42.5904516306762,
12.));
#150843=CARTESIAN_POINT('Ctrl Pts',(-58.1178876906907,42.5703713416265,
0.));
#150844=CARTESIAN_POINT('Ctrl Pts',(-58.1178876906907,42.5703713416265,
12.));
#150845=CARTESIAN_POINT('Ctrl Pts',(-58.1045197452002,42.5503391304183,
0.));
#150846=CARTESIAN_POINT('Ctrl Pts',(-58.1045197452002,42.5503391304183,
12.));
#150847=CARTESIAN_POINT('Ctrl Pts',(-58.0911557475965,42.5303550620387,
0.));
#150848=CARTESIAN_POINT('Ctrl Pts',(-58.0911557475965,42.5303550620387,
12.));
#150849=CARTESIAN_POINT('Ctrl Pts',(-58.0777958147403,42.5104192016664,
0.));
#150850=CARTESIAN_POINT('Ctrl Pts',(-58.0777958147403,42.5104192016664,
12.));
#150851=CARTESIAN_POINT('Ctrl Pts',(-58.0644400640275,42.4905316146653,
0.));
#150852=CARTESIAN_POINT('Ctrl Pts',(-58.0644400640275,42.4905316146653,
12.));
#150853=CARTESIAN_POINT('Ctrl Pts',(-58.0510886133926,42.4706923665845,
0.));
#150854=CARTESIAN_POINT('Ctrl Pts',(-58.0510886133926,42.4706923665845,
12.));
#150855=CARTESIAN_POINT('Ctrl Pts',(-58.037741581314,42.4509015231674,0.));
#150856=CARTESIAN_POINT('Ctrl Pts',(-58.037741581314,42.4509015231674,12.));
#150857=CARTESIAN_POINT('Ctrl Pts',(-58.0243990868181,42.4311591503555,
0.));
#150858=CARTESIAN_POINT('Ctrl Pts',(-58.0243990868181,42.4311591503555,
12.));
#150859=CARTESIAN_POINT('Ctrl Pts',(-58.0110612494828,42.411465314289,0.));
#150860=CARTESIAN_POINT('Ctrl Pts',(-58.0110612494828,42.411465314289,12.));
#150861=CARTESIAN_POINT('Ctrl Pts',(-57.9977281894422,42.3918200813014,
0.));
#150862=CARTESIAN_POINT('Ctrl Pts',(-57.9977281894422,42.3918200813014,
12.));
#150863=CARTESIAN_POINT('Ctrl Pts',(-57.9844000273911,42.3722235179197,
0.));
#150864=CARTESIAN_POINT('Ctrl Pts',(-57.9844000273911,42.3722235179197,
12.));
#150865=CARTESIAN_POINT('Ctrl Pts',(-57.9710768845899,42.3526756908746,
0.));
#150866=CARTESIAN_POINT('Ctrl Pts',(-57.9710768845899,42.3526756908746,
12.));
#150867=CARTESIAN_POINT('Ctrl Pts',(-57.9577588828682,42.333176667102,0.));
#150868=CARTESIAN_POINT('Ctrl Pts',(-57.9577588828682,42.333176667102,12.));
#150869=CARTESIAN_POINT('Ctrl Pts',(-57.9444461446299,42.3137265137452,
0.));
#150870=CARTESIAN_POINT('Ctrl Pts',(-57.9444461446299,42.3137265137452,
12.));
#150871=CARTESIAN_POINT('Ctrl Pts',(-57.9311387928563,42.2943252981489,
0.));
#150872=CARTESIAN_POINT('Ctrl Pts',(-57.9311387928563,42.2943252981489,
12.));
#150873=CARTESIAN_POINT('Ctrl Pts',(-57.9178369511114,42.2749730878594,
0.));
#150874=CARTESIAN_POINT('Ctrl Pts',(-57.9178369511114,42.2749730878594,
12.));
#150875=CARTESIAN_POINT('Ctrl Pts',(-57.9045407435474,42.2556699506353,
0.));
#150876=CARTESIAN_POINT('Ctrl Pts',(-57.9045407435474,42.2556699506353,
12.));
#150877=CARTESIAN_POINT('Ctrl Pts',(-57.8912502949096,42.2364159544501,
0.));
#150878=CARTESIAN_POINT('Ctrl Pts',(-57.8912502949096,42.2364159544501,
12.));
#150879=CARTESIAN_POINT('Ctrl Pts',(-57.8779657305413,42.2172111674938,
0.));
#150880=CARTESIAN_POINT('Ctrl Pts',(-57.8779657305413,42.2172111674938,
12.));
#150881=CARTESIAN_POINT('Ctrl Pts',(-57.864687176387,42.1980556581665,0.));
#150882=CARTESIAN_POINT('Ctrl Pts',(-57.864687176387,42.1980556581665,12.));
#150883=CARTESIAN_POINT('Ctrl Pts',(-57.8514147589972,42.1789494950794,
0.));
#150884=CARTESIAN_POINT('Ctrl Pts',(-57.8514147589972,42.1789494950794,
12.));
#150885=CARTESIAN_POINT('Ctrl Pts',(-57.8381486055342,42.1598927470646,
0.));
#150886=CARTESIAN_POINT('Ctrl Pts',(-57.8381486055342,42.1598927470646,
12.));
#150887=CARTESIAN_POINT('Ctrl Pts',(-57.8248888437775,42.1408854831783,
0.));
#150888=CARTESIAN_POINT('Ctrl Pts',(-57.8248888437775,42.1408854831783,
12.));
#150889=CARTESIAN_POINT('Ctrl Pts',(-57.8116356021288,42.1219277727021,
0.));
#150890=CARTESIAN_POINT('Ctrl Pts',(-57.8116356021288,42.1219277727021,
12.));
#150891=CARTESIAN_POINT('Ctrl Pts',(-57.798389009616,42.1030196851366,0.));
#150892=CARTESIAN_POINT('Ctrl Pts',(-57.798389009616,42.1030196851366,12.));
#150893=CARTESIAN_POINT('Ctrl Pts',(-57.7851491958987,42.0841612902042,
0.));
#150894=CARTESIAN_POINT('Ctrl Pts',(-57.7851491958987,42.0841612902042,
12.));
#150895=CARTESIAN_POINT('Ctrl Pts',(-57.7719162912744,42.0653526578588,
0.));
#150896=CARTESIAN_POINT('Ctrl Pts',(-57.7719162912744,42.0653526578588,
12.));
#150897=CARTESIAN_POINT('Ctrl Pts',(-57.7586904266834,42.0465938582882,
0.));
#150898=CARTESIAN_POINT('Ctrl Pts',(-57.7586904266834,42.0465938582882,
12.));
#150899=CARTESIAN_POINT('Ctrl Pts',(-57.745471733714,42.0278849619148,0.));
#150900=CARTESIAN_POINT('Ctrl Pts',(-57.745471733714,42.0278849619148,12.));
#150901=CARTESIAN_POINT('Ctrl Pts',(-57.7322603446066,42.0092260393897,
0.));
#150902=CARTESIAN_POINT('Ctrl Pts',(-57.7322603446066,42.0092260393897,
12.));
#150903=CARTESIAN_POINT('Ctrl Pts',(-57.7190563922593,41.990617161596,0.));
#150904=CARTESIAN_POINT('Ctrl Pts',(-57.7190563922593,41.990617161596,12.));
#150905=CARTESIAN_POINT('Ctrl Pts',(-57.7058600102351,41.9720583996592,
0.));
#150906=CARTESIAN_POINT('Ctrl Pts',(-57.7058600102351,41.9720583996592,
12.));
#150907=CARTESIAN_POINT('Ctrl Pts',(-57.6926713327672,41.9535498249488,
0.));
#150908=CARTESIAN_POINT('Ctrl Pts',(-57.6926713327672,41.9535498249488,
12.));
#150909=CARTESIAN_POINT('Ctrl Pts',(-57.6794904947649,41.9350915090796,
0.));
#150910=CARTESIAN_POINT('Ctrl Pts',(-57.6794904947649,41.9350915090796,
12.));
#150911=CARTESIAN_POINT('Ctrl Pts',(-57.6663176318189,41.9166835239054,
0.));
#150912=CARTESIAN_POINT('Ctrl Pts',(-57.6663176318189,41.9166835239054,
12.));
#150913=CARTESIAN_POINT('Ctrl Pts',(-57.6531528802072,41.8983259415253,
0.));
#150914=CARTESIAN_POINT('Ctrl Pts',(-57.6531528802072,41.8983259415253,
12.));
#150915=CARTESIAN_POINT('Ctrl Pts',(-57.6399963769009,41.8800188342912,
0.));
#150916=CARTESIAN_POINT('Ctrl Pts',(-57.6399963769009,41.8800188342912,
12.));
#150917=CARTESIAN_POINT('Ctrl Pts',(-57.6268482595701,41.8617622748107,
0.));
#150918=CARTESIAN_POINT('Ctrl Pts',(-57.6268482595701,41.8617622748107,
12.));
#150919=CARTESIAN_POINT('Ctrl Pts',(-57.613708666588,41.8435563359456,0.));
#150920=CARTESIAN_POINT('Ctrl Pts',(-57.613708666588,41.8435563359456,12.));
#150921=CARTESIAN_POINT('Ctrl Pts',(-57.6005777370347,41.8254010908051,
0.));
#150922=CARTESIAN_POINT('Ctrl Pts',(-57.6005777370347,41.8254010908051,
12.));
#150923=CARTESIAN_POINT('Ctrl Pts',(-57.5874556107054,41.8072966127559,
0.));
#150924=CARTESIAN_POINT('Ctrl Pts',(-57.5874556107054,41.8072966127559,
12.));
#150925=CARTESIAN_POINT('Ctrl Pts',(-57.5743424281204,41.7892429754298,
0.));
#150926=CARTESIAN_POINT('Ctrl Pts',(-57.5743424281204,41.7892429754298,
12.));
#150927=CARTESIAN_POINT('Ctrl Pts',(-57.561238330532,41.7712402527273,0.));
#150928=CARTESIAN_POINT('Ctrl Pts',(-57.561238330532,41.7712402527273,12.));
#150929=CARTESIAN_POINT('Ctrl Pts',(-57.5481434599334,41.7532885188174,
0.));
#150930=CARTESIAN_POINT('Ctrl Pts',(-57.5481434599334,41.7532885188174,
12.));
#150931=CARTESIAN_POINT('Ctrl Pts',(-57.5350579590648,41.7353878481336,
0.));
#150932=CARTESIAN_POINT('Ctrl Pts',(-57.5350579590648,41.7353878481336,
12.));
#150933=CARTESIAN_POINT('Ctrl Pts',(-57.5219819714169,41.7175383153819,
0.));
#150934=CARTESIAN_POINT('Ctrl Pts',(-57.5219819714169,41.7175383153819,
12.));
#150935=CARTESIAN_POINT('Ctrl Pts',(-57.5089156412341,41.6997399955445,
0.));
#150936=CARTESIAN_POINT('Ctrl Pts',(-57.5089156412341,41.6997399955445,
12.));
#150937=CARTESIAN_POINT('Ctrl Pts',(-57.4958591135165,41.6819929638797,
0.));
#150938=CARTESIAN_POINT('Ctrl Pts',(-57.4958591135165,41.6819929638797,
12.));
#150939=CARTESIAN_POINT('Ctrl Pts',(-57.4828125340222,41.6642972959168,
0.));
#150940=CARTESIAN_POINT('Ctrl Pts',(-57.4828125340222,41.6642972959168,
12.));
#150941=CARTESIAN_POINT('Ctrl Pts',(-57.4697760492693,41.6466530674522,
0.));
#150942=CARTESIAN_POINT('Ctrl Pts',(-57.4697760492693,41.6466530674522,
12.));
#150943=CARTESIAN_POINT('Ctrl Pts',(-57.4567498065573,41.6290603545674,
0.));
#150944=CARTESIAN_POINT('Ctrl Pts',(-57.4567498065573,41.6290603545674,
12.));
#150945=CARTESIAN_POINT('Ctrl Pts',(-57.4437339539848,41.6115192336393,
0.));
#150946=CARTESIAN_POINT('Ctrl Pts',(-57.4437339539848,41.6115192336393,
12.));
#150947=CARTESIAN_POINT('Ctrl Pts',(-57.4307286404656,41.5940297813474,
0.));
#150948=CARTESIAN_POINT('Ctrl Pts',(-57.4307286404656,41.5940297813474,
12.));
#150949=CARTESIAN_POINT('Ctrl Pts',(-57.417734015749,41.5765920746764,0.));
#150950=CARTESIAN_POINT('Ctrl Pts',(-57.417734015749,41.5765920746764,12.));
#150951=CARTESIAN_POINT('Ctrl Pts',(-57.4047502304207,41.5592061909159,
0.));
#150952=CARTESIAN_POINT('Ctrl Pts',(-57.4047502304207,41.5592061909159,
12.));
#150953=CARTESIAN_POINT('Ctrl Pts',(-57.3917774358844,41.5418722076558,
0.));
#150954=CARTESIAN_POINT('Ctrl Pts',(-57.3917774358844,41.5418722076558,
12.));
#150955=CARTESIAN_POINT('Ctrl Pts',(-57.378815784345,41.5245902027767,0.));
#150956=CARTESIAN_POINT('Ctrl Pts',(-57.378815784345,41.5245902027767,12.));
#150957=CARTESIAN_POINT('Ctrl Pts',(-57.3658654287948,41.5073602544404,
0.));
#150958=CARTESIAN_POINT('Ctrl Pts',(-57.3658654287948,41.5073602544404,
12.));
#150959=CARTESIAN_POINT('Ctrl Pts',(-57.3529265229858,41.4901824410654,
0.));
#150960=CARTESIAN_POINT('Ctrl Pts',(-57.3529265229858,41.4901824410654,
12.));
#150961=CARTESIAN_POINT('Ctrl Pts',(-57.339999221474,41.4730568413535,0.));
#150962=CARTESIAN_POINT('Ctrl Pts',(-57.339999221474,41.4730568413535,12.));
#150963=CARTESIAN_POINT('Ctrl Pts',(-57.3270836796925,41.4559835343338,
0.));
#150964=CARTESIAN_POINT('Ctrl Pts',(-57.3270836796925,41.4559835343338,
12.));
#150965=CARTESIAN_POINT('Ctrl Pts',(-57.3141800540137,41.4389625993948,
0.));
#150966=CARTESIAN_POINT('Ctrl Pts',(-57.3141800540137,41.4389625993948,
12.));
#150967=CARTESIAN_POINT('Ctrl Pts',(-57.3012885018139,41.4219941163154,
0.));
#150968=CARTESIAN_POINT('Ctrl Pts',(-57.3012885018139,41.4219941163154,
12.));
#150969=CARTESIAN_POINT('Ctrl Pts',(-57.2884091815385,41.4050781652923,
0.));
#150970=CARTESIAN_POINT('Ctrl Pts',(-57.2884091815385,41.4050781652923,
12.));
#150971=CARTESIAN_POINT('Ctrl Pts',(-57.2755422525822,41.3882148268798,
0.));
#150972=CARTESIAN_POINT('Ctrl Pts',(-57.2755422525822,41.3882148268798,
12.));
#150973=CARTESIAN_POINT('Ctrl Pts',(-57.2626878751584,41.3714041819215,
0.));
#150974=CARTESIAN_POINT('Ctrl Pts',(-57.2626878751584,41.3714041819215,
12.));
#150975=CARTESIAN_POINT('Ctrl Pts',(-57.2498462101883,41.3546463114889,
0.));
#150976=CARTESIAN_POINT('Ctrl Pts',(-57.2498462101883,41.3546463114889,
12.));
#150977=CARTESIAN_POINT('Ctrl Pts',(-57.237017419142,41.3379412967889,0.));
#150978=CARTESIAN_POINT('Ctrl Pts',(-57.237017419142,41.3379412967889,12.));
#150979=CARTESIAN_POINT('Ctrl Pts',(-57.2242016640226,41.321289219151,0.));
#150980=CARTESIAN_POINT('Ctrl Pts',(-57.2242016640226,41.321289219151,12.));
#150981=CARTESIAN_POINT('Ctrl Pts',(-57.2113991077325,41.304690160231,0.));
#150982=CARTESIAN_POINT('Ctrl Pts',(-57.2113991077325,41.304690160231,12.));
#150983=CARTESIAN_POINT('Ctrl Pts',(-57.1986099143992,41.2881442021869,
0.));
#150984=CARTESIAN_POINT('Ctrl Pts',(-57.1986099143992,41.2881442021869,
12.));
#150985=CARTESIAN_POINT('Ctrl Pts',(-57.1858342496526,41.2716514278268,
0.));
#150986=CARTESIAN_POINT('Ctrl Pts',(-57.1858342496526,41.2716514278268,
12.));
#150987=CARTESIAN_POINT('Ctrl Pts',(-57.1730722810771,41.2552119208445,
0.));
#150988=CARTESIAN_POINT('Ctrl Pts',(-57.1730722810771,41.2552119208445,
12.));
#150989=CARTESIAN_POINT('Ctrl Pts',(-57.1603241779042,41.2388257656534,
0.));
#150990=CARTESIAN_POINT('Ctrl Pts',(-57.1603241779042,41.2388257656534,
12.));
#150991=CARTESIAN_POINT('Ctrl Pts',(-57.1475901101795,41.2224930469412,
0.));
#150992=CARTESIAN_POINT('Ctrl Pts',(-57.1475901101795,41.2224930469412,
12.));
#150993=CARTESIAN_POINT('Ctrl Pts',(-57.1348702480644,41.2062138492913,
0.));
#150994=CARTESIAN_POINT('Ctrl Pts',(-57.1348702480644,41.2062138492913,
12.));
#150995=CARTESIAN_POINT('Ctrl Pts',(-57.1221647611231,41.1899882567941,
0.));
#150996=CARTESIAN_POINT('Ctrl Pts',(-57.1221647611231,41.1899882567941,
12.));
#150997=CARTESIAN_POINT('Ctrl Pts',(-57.1094738174998,41.1738163525931,
0.));
#150998=CARTESIAN_POINT('Ctrl Pts',(-57.1094738174998,41.1738163525931,
12.));
#150999=CARTESIAN_POINT('Ctrl Pts',(-57.0967975854912,41.1576982197402,
0.));
#151000=CARTESIAN_POINT('Ctrl Pts',(-57.0967975854912,41.1576982197402,
12.));
#151001=CARTESIAN_POINT('Ctrl Pts',(-57.0841362354281,41.1416339422132,
0.));
#151002=CARTESIAN_POINT('Ctrl Pts',(-57.0841362354281,41.1416339422132,
12.));
#151003=CARTESIAN_POINT('Ctrl Pts',(-57.0714899412091,41.1256236057436,
0.));
#151004=CARTESIAN_POINT('Ctrl Pts',(-57.0714899412091,41.1256236057436,
12.));
#151005=CARTESIAN_POINT('Ctrl Pts',(-57.0588588825266,41.1096672990125,
0.));
#151006=CARTESIAN_POINT('Ctrl Pts',(-57.0588588825266,41.1096672990125,
12.));
#151007=CARTESIAN_POINT('Ctrl Pts',(-57.0462432450637,41.0937651137519,
0.));
#151008=CARTESIAN_POINT('Ctrl Pts',(-57.0462432450637,41.0937651137519,
12.));
#151009=CARTESIAN_POINT('Ctrl Pts',(-57.0336432158503,41.0779171422415,
0.));
#151010=CARTESIAN_POINT('Ctrl Pts',(-57.0336432158503,41.0779171422415,
12.));
#151011=CARTESIAN_POINT('Ctrl Pts',(-57.0210589791777,41.0621234751,0.));
#151012=CARTESIAN_POINT('Ctrl Pts',(-57.0210589791777,41.0621234751,12.));
#151013=CARTESIAN_POINT('Ctrl Pts',(-57.008490713044,41.0463841993622,0.));
#151014=CARTESIAN_POINT('Ctrl Pts',(-57.008490713044,41.0463841993622,12.));
#151015=CARTESIAN_POINT('Ctrl Pts',(-56.9959385834768,41.0306993954021,
0.));
#151016=CARTESIAN_POINT('Ctrl Pts',(-56.9959385834768,41.0306993954021,
12.));
#151017=CARTESIAN_POINT('Ctrl Pts',(-56.9834027500178,41.0150691398988,
0.));
#151018=CARTESIAN_POINT('Ctrl Pts',(-56.9834027500178,41.0150691398988,
12.));
#151019=CARTESIAN_POINT('Ctrl Pts',(-56.9708833766183,40.9994935117307,
0.));
#151020=CARTESIAN_POINT('Ctrl Pts',(-56.9708833766183,40.9994935117307,
12.));
#151021=CARTESIAN_POINT('Ctrl Pts',(-56.9583806404069,40.9839725967121,
0.));
#151022=CARTESIAN_POINT('Ctrl Pts',(-56.9583806404069,40.9839725967121,
12.));
#151023=CARTESIAN_POINT('Ctrl Pts',(-56.9458947422541,40.968506493303,0.));
#151024=CARTESIAN_POINT('Ctrl Pts',(-56.9458947422541,40.968506493303,12.));
#151025=CARTESIAN_POINT('Ctrl Pts',(-56.9334259139928,40.9530953164952,
0.));
#151026=CARTESIAN_POINT('Ctrl Pts',(-56.9334259139928,40.9530953164952,
12.));
#151027=CARTESIAN_POINT('Ctrl Pts',(-56.9209743960861,40.9377391857044,
0.));
#151028=CARTESIAN_POINT('Ctrl Pts',(-56.9209743960861,40.9377391857044,
12.));
#151029=CARTESIAN_POINT('Ctrl Pts',(-56.9085404164432,40.9224382132382,
0.));
#151030=CARTESIAN_POINT('Ctrl Pts',(-56.9085404164432,40.9224382132382,
12.));
#151031=CARTESIAN_POINT('Ctrl Pts',(-56.8961241708926,40.9071924937551,
0.));
#151032=CARTESIAN_POINT('Ctrl Pts',(-56.8961241708926,40.9071924937551,
12.));
#151033=CARTESIAN_POINT('Ctrl Pts',(-56.8837257978574,40.8920020903443,
0.));
#151034=CARTESIAN_POINT('Ctrl Pts',(-56.8837257978574,40.8920020903443,
12.));
#151035=CARTESIAN_POINT('Ctrl Pts',(-56.8713453765252,40.8768670342278,
0.));
#151036=CARTESIAN_POINT('Ctrl Pts',(-56.8713453765252,40.8768670342278,
12.));
#151037=CARTESIAN_POINT('Ctrl Pts',(-56.8614554317993,40.8648032759631,
0.));
#151038=CARTESIAN_POINT('Ctrl Pts',(-56.8614554317993,40.8648032759631,
12.));
#151039=CARTESIAN_POINT('Ctrl Pts',(-56.8540460739677,40.8557803680411,
0.));
#151040=CARTESIAN_POINT('Ctrl Pts',(-56.8540460739677,40.8557803680411,
12.));
#151041=CARTESIAN_POINT('Ctrl Pts',(-56.8491101022668,40.8497761671086,
0.));
#151042=CARTESIAN_POINT('Ctrl Pts',(-56.8491101022668,40.8497761671086,
12.));
#151043=CARTESIAN_POINT('Ctrl Pts',(-56.8466430164621,40.8467768343956,
0.));
#151044=CARTESIAN_POINT('Ctrl Pts',(-56.8466430164621,40.8467768343956,
12.));
#151045=CARTESIAN_POINT('',(-56.8466430164621,40.8467768343956,12.));
#151046=CARTESIAN_POINT('Ctrl Pts',(-56.8466430164621,40.8467768343956,
12.));
#151047=CARTESIAN_POINT('Ctrl Pts',(-56.8491101022668,40.8497761671086,
12.));
#151048=CARTESIAN_POINT('Ctrl Pts',(-56.8540460739677,40.8557803680411,
12.));
#151049=CARTESIAN_POINT('Ctrl Pts',(-56.8614554317993,40.8648032759631,
12.));
#151050=CARTESIAN_POINT('Ctrl Pts',(-56.8713453765252,40.8768670342278,
12.));
#151051=CARTESIAN_POINT('Ctrl Pts',(-56.8837257978574,40.8920020903443,
12.));
#151052=CARTESIAN_POINT('Ctrl Pts',(-56.8961241708926,40.9071924937551,
12.));
#151053=CARTESIAN_POINT('Ctrl Pts',(-56.9085404164432,40.9224382132382,
12.));
#151054=CARTESIAN_POINT('Ctrl Pts',(-56.9209743960861,40.9377391857044,
12.));
#151055=CARTESIAN_POINT('Ctrl Pts',(-56.9334259139928,40.9530953164952,
12.));
#151056=CARTESIAN_POINT('Ctrl Pts',(-56.9458947422541,40.968506493303,12.));
#151057=CARTESIAN_POINT('Ctrl Pts',(-56.9583806404069,40.9839725967121,
12.));
#151058=CARTESIAN_POINT('Ctrl Pts',(-56.9708833766183,40.9994935117307,
12.));
#151059=CARTESIAN_POINT('Ctrl Pts',(-56.9834027500178,41.0150691398988,
12.));
#151060=CARTESIAN_POINT('Ctrl Pts',(-56.9959385834768,41.0306993954021,
12.));
#151061=CARTESIAN_POINT('Ctrl Pts',(-57.008490713044,41.0463841993622,12.));
#151062=CARTESIAN_POINT('Ctrl Pts',(-57.0210589791777,41.0621234751,12.));
#151063=CARTESIAN_POINT('Ctrl Pts',(-57.0336432158503,41.0779171422415,
12.));
#151064=CARTESIAN_POINT('Ctrl Pts',(-57.0462432450637,41.0937651137519,
12.));
#151065=CARTESIAN_POINT('Ctrl Pts',(-57.0588588825266,41.1096672990125,
12.));
#151066=CARTESIAN_POINT('Ctrl Pts',(-57.0714899412091,41.1256236057436,
12.));
#151067=CARTESIAN_POINT('Ctrl Pts',(-57.0841362354281,41.1416339422132,
12.));
#151068=CARTESIAN_POINT('Ctrl Pts',(-57.0967975854912,41.1576982197402,
12.));
#151069=CARTESIAN_POINT('Ctrl Pts',(-57.1094738174998,41.1738163525931,
12.));
#151070=CARTESIAN_POINT('Ctrl Pts',(-57.1221647611231,41.1899882567941,
12.));
#151071=CARTESIAN_POINT('Ctrl Pts',(-57.1348702480644,41.2062138492913,
12.));
#151072=CARTESIAN_POINT('Ctrl Pts',(-57.1475901101795,41.2224930469412,
12.));
#151073=CARTESIAN_POINT('Ctrl Pts',(-57.1603241779042,41.2388257656534,
12.));
#151074=CARTESIAN_POINT('Ctrl Pts',(-57.1730722810771,41.2552119208445,
12.));
#151075=CARTESIAN_POINT('Ctrl Pts',(-57.1858342496526,41.2716514278268,
12.));
#151076=CARTESIAN_POINT('Ctrl Pts',(-57.1986099143992,41.2881442021869,
12.));
#151077=CARTESIAN_POINT('Ctrl Pts',(-57.2113991077325,41.304690160231,12.));
#151078=CARTESIAN_POINT('Ctrl Pts',(-57.2242016640226,41.321289219151,12.));
#151079=CARTESIAN_POINT('Ctrl Pts',(-57.237017419142,41.3379412967889,12.));
#151080=CARTESIAN_POINT('Ctrl Pts',(-57.2498462101883,41.3546463114889,
12.));
#151081=CARTESIAN_POINT('Ctrl Pts',(-57.2626878751584,41.3714041819215,
12.));
#151082=CARTESIAN_POINT('Ctrl Pts',(-57.2755422525822,41.3882148268798,
12.));
#151083=CARTESIAN_POINT('Ctrl Pts',(-57.2884091815385,41.4050781652923,
12.));
#151084=CARTESIAN_POINT('Ctrl Pts',(-57.3012885018139,41.4219941163154,
12.));
#151085=CARTESIAN_POINT('Ctrl Pts',(-57.3141800540137,41.4389625993948,
12.));
#151086=CARTESIAN_POINT('Ctrl Pts',(-57.3270836796925,41.4559835343338,
12.));
#151087=CARTESIAN_POINT('Ctrl Pts',(-57.339999221474,41.4730568413535,12.));
#151088=CARTESIAN_POINT('Ctrl Pts',(-57.3529265229858,41.4901824410654,
12.));
#151089=CARTESIAN_POINT('Ctrl Pts',(-57.3658654287948,41.5073602544404,
12.));
#151090=CARTESIAN_POINT('Ctrl Pts',(-57.378815784345,41.5245902027767,12.));
#151091=CARTESIAN_POINT('Ctrl Pts',(-57.3917774358844,41.5418722076558,
12.));
#151092=CARTESIAN_POINT('Ctrl Pts',(-57.4047502304207,41.5592061909159,
12.));
#151093=CARTESIAN_POINT('Ctrl Pts',(-57.417734015749,41.5765920746764,12.));
#151094=CARTESIAN_POINT('Ctrl Pts',(-57.4307286404656,41.5940297813474,
12.));
#151095=CARTESIAN_POINT('Ctrl Pts',(-57.4437339539848,41.6115192336393,
12.));
#151096=CARTESIAN_POINT('Ctrl Pts',(-57.4567498065573,41.6290603545674,
12.));
#151097=CARTESIAN_POINT('Ctrl Pts',(-57.4697760492693,41.6466530674522,
12.));
#151098=CARTESIAN_POINT('Ctrl Pts',(-57.4828125340222,41.6642972959168,
12.));
#151099=CARTESIAN_POINT('Ctrl Pts',(-57.4958591135165,41.6819929638797,
12.));
#151100=CARTESIAN_POINT('Ctrl Pts',(-57.5089156412341,41.6997399955445,
12.));
#151101=CARTESIAN_POINT('Ctrl Pts',(-57.5219819714169,41.7175383153819,
12.));
#151102=CARTESIAN_POINT('Ctrl Pts',(-57.5350579590648,41.7353878481336,
12.));
#151103=CARTESIAN_POINT('Ctrl Pts',(-57.5481434599334,41.7532885188174,
12.));
#151104=CARTESIAN_POINT('Ctrl Pts',(-57.561238330532,41.7712402527273,12.));
#151105=CARTESIAN_POINT('Ctrl Pts',(-57.5743424281204,41.7892429754298,
12.));
#151106=CARTESIAN_POINT('Ctrl Pts',(-57.5874556107054,41.8072966127559,
12.));
#151107=CARTESIAN_POINT('Ctrl Pts',(-57.6005777370347,41.8254010908051,
12.));
#151108=CARTESIAN_POINT('Ctrl Pts',(-57.613708666588,41.8435563359456,12.));
#151109=CARTESIAN_POINT('Ctrl Pts',(-57.6268482595701,41.8617622748107,
12.));
#151110=CARTESIAN_POINT('Ctrl Pts',(-57.6399963769009,41.8800188342912,
12.));
#151111=CARTESIAN_POINT('Ctrl Pts',(-57.6531528802072,41.8983259415253,
12.));
#151112=CARTESIAN_POINT('Ctrl Pts',(-57.6663176318189,41.9166835239054,
12.));
#151113=CARTESIAN_POINT('Ctrl Pts',(-57.6794904947649,41.9350915090796,
12.));
#151114=CARTESIAN_POINT('Ctrl Pts',(-57.6926713327672,41.9535498249488,
12.));
#151115=CARTESIAN_POINT('Ctrl Pts',(-57.7058600102351,41.9720583996592,
12.));
#151116=CARTESIAN_POINT('Ctrl Pts',(-57.7190563922593,41.990617161596,12.));
#151117=CARTESIAN_POINT('Ctrl Pts',(-57.7322603446066,42.0092260393897,
12.));
#151118=CARTESIAN_POINT('Ctrl Pts',(-57.745471733714,42.0278849619148,12.));
#151119=CARTESIAN_POINT('Ctrl Pts',(-57.7586904266834,42.0465938582882,
12.));
#151120=CARTESIAN_POINT('Ctrl Pts',(-57.7719162912744,42.0653526578588,
12.));
#151121=CARTESIAN_POINT('Ctrl Pts',(-57.7851491958987,42.0841612902042,
12.));
#151122=CARTESIAN_POINT('Ctrl Pts',(-57.798389009616,42.1030196851366,12.));
#151123=CARTESIAN_POINT('Ctrl Pts',(-57.8116356021288,42.1219277727021,
12.));
#151124=CARTESIAN_POINT('Ctrl Pts',(-57.8248888437775,42.1408854831783,
12.));
#151125=CARTESIAN_POINT('Ctrl Pts',(-57.8381486055342,42.1598927470646,
12.));
#151126=CARTESIAN_POINT('Ctrl Pts',(-57.8514147589972,42.1789494950794,
12.));
#151127=CARTESIAN_POINT('Ctrl Pts',(-57.864687176387,42.1980556581665,12.));
#151128=CARTESIAN_POINT('Ctrl Pts',(-57.8779657305413,42.2172111674938,
12.));
#151129=CARTESIAN_POINT('Ctrl Pts',(-57.8912502949096,42.2364159544501,
12.));
#151130=CARTESIAN_POINT('Ctrl Pts',(-57.9045407435474,42.2556699506353,
12.));
#151131=CARTESIAN_POINT('Ctrl Pts',(-57.9178369511114,42.2749730878594,
12.));
#151132=CARTESIAN_POINT('Ctrl Pts',(-57.9311387928563,42.2943252981489,
12.));
#151133=CARTESIAN_POINT('Ctrl Pts',(-57.9444461446299,42.3137265137452,
12.));
#151134=CARTESIAN_POINT('Ctrl Pts',(-57.9577588828682,42.333176667102,12.));
#151135=CARTESIAN_POINT('Ctrl Pts',(-57.9710768845899,42.3526756908746,
12.));
#151136=CARTESIAN_POINT('Ctrl Pts',(-57.9844000273911,42.3722235179197,
12.));
#151137=CARTESIAN_POINT('Ctrl Pts',(-57.9977281894422,42.3918200813014,
12.));
#151138=CARTESIAN_POINT('Ctrl Pts',(-58.0110612494828,42.411465314289,12.));
#151139=CARTESIAN_POINT('Ctrl Pts',(-58.0243990868181,42.4311591503555,
12.));
#151140=CARTESIAN_POINT('Ctrl Pts',(-58.037741581314,42.4509015231674,12.));
#151141=CARTESIAN_POINT('Ctrl Pts',(-58.0510886133926,42.4706923665845,
12.));
#151142=CARTESIAN_POINT('Ctrl Pts',(-58.0644400640275,42.4905316146653,
12.));
#151143=CARTESIAN_POINT('Ctrl Pts',(-58.0777958147403,42.5104192016664,
12.));
#151144=CARTESIAN_POINT('Ctrl Pts',(-58.0911557475965,42.5303550620387,
12.));
#151145=CARTESIAN_POINT('Ctrl Pts',(-58.1045197452002,42.5503391304183,
12.));
#151146=CARTESIAN_POINT('Ctrl Pts',(-58.1178876906907,42.5703713416265,
12.));
#151147=CARTESIAN_POINT('Ctrl Pts',(-58.1312594677386,42.5904516306762,
12.));
#151148=CARTESIAN_POINT('Ctrl Pts',(-58.1446349605421,42.6105799327699,
12.));
#151149=CARTESIAN_POINT('Ctrl Pts',(-58.1580140538228,42.6307561832976,
12.));
#151150=CARTESIAN_POINT('Ctrl Pts',(-58.171396632821,42.6509803178265,12.));
#151151=CARTESIAN_POINT('Ctrl Pts',(-58.1847825832923,42.6712522721016,
12.));
#151152=CARTESIAN_POINT('Ctrl Pts',(-58.1981717915037,42.6915719820513,
12.));
#151153=CARTESIAN_POINT('Ctrl Pts',(-58.21156414423,42.7119393837866,12.));
#151154=CARTESIAN_POINT('Ctrl Pts',(-58.22495952875,42.7323544135985,12.));
#151155=CARTESIAN_POINT('Ctrl Pts',(-58.2383578328424,42.7528170079484,
12.));
#151156=CARTESIAN_POINT('Ctrl Pts',(-58.251758944782,42.7733271034679,12.));
#151157=CARTESIAN_POINT('Ctrl Pts',(-58.2651627533368,42.7938846369651,
12.));
#151158=CARTESIAN_POINT('Ctrl Pts',(-58.2785691477638,42.8144895454233,
12.));
#151159=CARTESIAN_POINT('Ctrl Pts',(-58.2919780178064,42.8351417659999,
12.));
#151160=CARTESIAN_POINT('Ctrl Pts',(-58.3053892536894,42.8558412360158,
12.));
#151161=CARTESIAN_POINT('Ctrl Pts',(-58.3188027461164,42.8765878929551,
12.));
#151162=CARTESIAN_POINT('Ctrl Pts',(-58.3322183862654,42.8973816744709,
12.));
#151163=CARTESIAN_POINT('Ctrl Pts',(-58.3456360657865,42.9182225183855,
12.));
#151164=CARTESIAN_POINT('Ctrl Pts',(-58.3590556767978,42.9391103626879,
12.));
#151165=CARTESIAN_POINT('Ctrl Pts',(-58.3724771118826,42.960045145526,12.));
#151166=CARTESIAN_POINT('Ctrl Pts',(-58.3859002640856,42.9810268052032,
12.));
#151167=CARTESIAN_POINT('Ctrl Pts',(-58.3993250269101,43.0020552801859,
12.));
#151168=CARTESIAN_POINT('Ctrl Pts',(-58.4127512943136,43.0231305091027,
12.));
#151169=CARTESIAN_POINT('Ctrl Pts',(-58.4261789607058,43.0442524307434,
12.));
#151170=CARTESIAN_POINT('Ctrl Pts',(-58.439607920945,43.0654209840511,12.));
#151171=CARTESIAN_POINT('Ctrl Pts',(-58.4530380703348,43.0866361081177,
12.));
#151172=CARTESIAN_POINT('Ctrl Pts',(-58.4664693046217,43.1078977421916,
12.));
#151173=CARTESIAN_POINT('Ctrl Pts',(-58.4799015199907,43.1292058256777,
12.));
#151174=CARTESIAN_POINT('Ctrl Pts',(-58.4933346130636,43.1505602981365,
12.));
#151175=CARTESIAN_POINT('Ctrl Pts',(-58.5067684808944,43.1719610992771,
12.));
#151176=CARTESIAN_POINT('Ctrl Pts',(-58.5202030209669,43.1934081689505,
12.));
#151177=CARTESIAN_POINT('Ctrl Pts',(-58.5336381311917,43.2149014471574,
12.));
#151178=CARTESIAN_POINT('Ctrl Pts',(-58.5470737099032,43.2364408740493,
12.));
#151179=CARTESIAN_POINT('Ctrl Pts',(-58.5605096558578,43.2580263899278,
12.));
#151180=CARTESIAN_POINT('Ctrl Pts',(-58.573945868231,43.27965793524,12.));
#151181=CARTESIAN_POINT('Ctrl Pts',(-58.5873822466152,43.3013354505701,
12.));
#151182=CARTESIAN_POINT('Ctrl Pts',(-58.6008186910156,43.3230588766449,
12.));
#151183=CARTESIAN_POINT('Ctrl Pts',(-58.6142551018467,43.3448281543371,
12.));
#151184=CARTESIAN_POINT('Ctrl Pts',(-58.627691379929,43.3666432246635,12.));
#151185=CARTESIAN_POINT('Ctrl Pts',(-58.6411274264857,43.388504028781,12.));
#151186=CARTESIAN_POINT('Ctrl Pts',(-58.6545631431393,43.4104105079768,
12.));
#151187=CARTESIAN_POINT('Ctrl Pts',(-58.6679984319097,43.4323626036737,
12.));
#151188=CARTESIAN_POINT('Ctrl Pts',(-58.6814331952138,43.4543602574351,
12.));
#151189=CARTESIAN_POINT('Ctrl Pts',(-58.6948673358638,43.4764034109654,
12.));
#151190=CARTESIAN_POINT('Ctrl Pts',(-58.7083007570661,43.4984920061073,
12.));
#151191=CARTESIAN_POINT('Ctrl Pts',(-58.7217333624209,43.5206259848337,
12.));
#151192=CARTESIAN_POINT('Ctrl Pts',(-58.735165055918,43.5428052892488,12.));
#151193=CARTESIAN_POINT('Ctrl Pts',(-58.74859574193,43.5650298615917,12.));
#151194=CARTESIAN_POINT('Ctrl Pts',(-58.7620253252062,43.5872996442345,
12.));
#151195=CARTESIAN_POINT('Ctrl Pts',(-58.775453710867,43.6096145796797,12.));
#151196=CARTESIAN_POINT('Ctrl Pts',(-58.788880804397,43.6319746105482,12.));
#151197=CARTESIAN_POINT('Ctrl Pts',(-58.8023065116436,43.6543796795789,
12.));
#151198=CARTESIAN_POINT('Ctrl Pts',(-58.8157307388238,43.6768297296395,
12.));
#151199=CARTESIAN_POINT('Ctrl Pts',(-58.8291533925293,43.6993247037314,
12.));
#151200=CARTESIAN_POINT('Ctrl Pts',(-58.8425743797326,43.7218645449922,
12.));
#151201=CARTESIAN_POINT('Ctrl Pts',(-58.855993607794,43.7444491966942,12.));
#151202=CARTESIAN_POINT('Ctrl Pts',(-58.8694109844648,43.7670786022402,
12.));
#151203=CARTESIAN_POINT('Ctrl Pts',(-58.8828264178621,43.7897527051609,
12.));
#151204=CARTESIAN_POINT('Ctrl Pts',(-58.8962398164493,43.8124714491076,
12.));
#151205=CARTESIAN_POINT('Ctrl Pts',(-58.9096510890129,43.835234777842,12.));
#151206=CARTESIAN_POINT('Ctrl Pts',(-58.9230601446436,43.858042635223,12.));
#151207=CARTESIAN_POINT('Ctrl Pts',(-58.936466892712,43.8808949651873,12.));
#151208=CARTESIAN_POINT('Ctrl Pts',(-58.9498712429054,43.9037917117739,
12.));
#151209=CARTESIAN_POINT('Ctrl Pts',(-58.9632731052696,43.9267328191501,
12.));
#151210=CARTESIAN_POINT('Ctrl Pts',(-58.9766723902529,43.9497182316331,
12.));
#151211=CARTESIAN_POINT('Ctrl Pts',(-58.9900690087408,43.9727478937056,
12.));
#151212=CARTESIAN_POINT('Ctrl Pts',(-59.0034628721168,43.9958217500369,
12.));
#151213=CARTESIAN_POINT('Ctrl Pts',(-59.0168538922095,44.0189397454599,
12.));
#151214=CARTESIAN_POINT('Ctrl Pts',(-59.0302419811777,44.0421018249223,
12.));
#151215=CARTESIAN_POINT('Ctrl Pts',(-59.0436270514087,44.0653079334385,
12.));
#151216=CARTESIAN_POINT('Ctrl Pts',(-59.0570090154243,44.0885580160432,
12.));
#151217=CARTESIAN_POINT('Ctrl Pts',(-59.0703877857526,44.1118520177221,
12.));
#151218=CARTESIAN_POINT('Ctrl Pts',(-59.08376327492,44.1351898834051,12.));
#151219=CARTESIAN_POINT('Ctrl Pts',(-59.0971353957206,44.1585715581064,
12.));
#151220=CARTESIAN_POINT('Ctrl Pts',(-59.1105040614276,44.1819969870307,
12.));
#151221=CARTESIAN_POINT('Ctrl Pts',(-59.1238691860306,44.2054661156875,
12.));
#151222=CARTESIAN_POINT('Ctrl Pts',(-59.1372306844586,44.228978889997,12.));
#151223=CARTESIAN_POINT('Ctrl Pts',(-59.1505884728215,44.2525352563996,
12.));
#151224=CARTESIAN_POINT('Ctrl Pts',(-59.1639424678793,44.2761351616048,
12.));
#151225=CARTESIAN_POINT('Ctrl Pts',(-59.1772925865213,44.2997785523431,
12.));
#151226=CARTESIAN_POINT('Ctrl Pts',(-59.1906387451979,44.3234653750884,
12.));
#151227=CARTESIAN_POINT('Ctrl Pts',(-59.2039808594752,44.3471955758403,
12.));
#151228=CARTESIAN_POINT('Ctrl Pts',(-59.2173188432798,44.3709690997469,
12.));
#151229=CARTESIAN_POINT('Ctrl Pts',(-59.2306526095131,44.3947858914074,
12.));
#151230=CARTESIAN_POINT('Ctrl Pts',(-59.2439820714187,44.4186458955451,
12.));
#151231=CARTESIAN_POINT('Ctrl Pts',(-59.2573071437774,44.4425490575911,
12.));
#151232=CARTESIAN_POINT('Ctrl Pts',(-59.2706277440445,44.4664953242379,
12.));
#151233=CARTESIAN_POINT('Ctrl Pts',(-59.2839437938237,44.490484644151,12.));
#151234=CARTESIAN_POINT('Ctrl Pts',(-59.2972552192156,44.5145169681349,
12.));
#151235=CARTESIAN_POINT('Ctrl Pts',(-59.3086616639523,44.5351541478479,
12.));
#151236=CARTESIAN_POINT('Ctrl Pts',(-59.3174041872347,44.5509994358154,
12.));
#151237=CARTESIAN_POINT('Ctrl Pts',(-59.3234848865455,44.5620338188738,
12.));
#151238=CARTESIAN_POINT('Ctrl Pts',(-59.3269051738423,44.5682447396021,
12.));
#151239=CARTESIAN_POINT('Ctrl Pts',(-59.3276657444392,44.5696260757792,
12.));
#151240=CARTESIAN_POINT('',(-56.8466430164621,40.8467768343956,0.));
#151241=CARTESIAN_POINT('',(-56.8466430164621,40.8467768343956,0.));
#151242=CARTESIAN_POINT('Ctrl Pts',(-59.3276657444392,44.5696260757791,
0.));
#151243=CARTESIAN_POINT('Ctrl Pts',(-59.3269051738423,44.5682447396021,
0.));
#151244=CARTESIAN_POINT('Ctrl Pts',(-59.3234848865455,44.5620338188738,
0.));
#151245=CARTESIAN_POINT('Ctrl Pts',(-59.3174041872347,44.5509994358154,
0.));
#151246=CARTESIAN_POINT('Ctrl Pts',(-59.3086616639523,44.5351541478479,
0.));
#151247=CARTESIAN_POINT('Ctrl Pts',(-59.2972552192156,44.5145169681349,
0.));
#151248=CARTESIAN_POINT('Ctrl Pts',(-59.2839437938237,44.490484644151,0.));
#151249=CARTESIAN_POINT('Ctrl Pts',(-59.2706277440445,44.4664953242379,
0.));
#151250=CARTESIAN_POINT('Ctrl Pts',(-59.2573071437774,44.4425490575911,
0.));
#151251=CARTESIAN_POINT('Ctrl Pts',(-59.2439820714187,44.4186458955451,
0.));
#151252=CARTESIAN_POINT('Ctrl Pts',(-59.2306526095131,44.3947858914074,
0.));
#151253=CARTESIAN_POINT('Ctrl Pts',(-59.2173188432798,44.3709690997469,
0.));
#151254=CARTESIAN_POINT('Ctrl Pts',(-59.2039808594752,44.3471955758403,
0.));
#151255=CARTESIAN_POINT('Ctrl Pts',(-59.1906387451979,44.3234653750884,
0.));
#151256=CARTESIAN_POINT('Ctrl Pts',(-59.1772925865213,44.2997785523431,
0.));
#151257=CARTESIAN_POINT('Ctrl Pts',(-59.1639424678793,44.2761351616048,
0.));
#151258=CARTESIAN_POINT('Ctrl Pts',(-59.1505884728215,44.2525352563996,
0.));
#151259=CARTESIAN_POINT('Ctrl Pts',(-59.1372306844586,44.228978889997,0.));
#151260=CARTESIAN_POINT('Ctrl Pts',(-59.1238691860306,44.2054661156875,
0.));
#151261=CARTESIAN_POINT('Ctrl Pts',(-59.1105040614276,44.1819969870307,
0.));
#151262=CARTESIAN_POINT('Ctrl Pts',(-59.0971353957206,44.1585715581064,
0.));
#151263=CARTESIAN_POINT('Ctrl Pts',(-59.08376327492,44.1351898834051,0.));
#151264=CARTESIAN_POINT('Ctrl Pts',(-59.0703877857526,44.1118520177221,
0.));
#151265=CARTESIAN_POINT('Ctrl Pts',(-59.0570090154243,44.0885580160432,
0.));
#151266=CARTESIAN_POINT('Ctrl Pts',(-59.0436270514087,44.0653079334385,
0.));
#151267=CARTESIAN_POINT('Ctrl Pts',(-59.0302419811777,44.0421018249223,
0.));
#151268=CARTESIAN_POINT('Ctrl Pts',(-59.0168538922095,44.0189397454599,
0.));
#151269=CARTESIAN_POINT('Ctrl Pts',(-59.0034628721168,43.9958217500369,
0.));
#151270=CARTESIAN_POINT('Ctrl Pts',(-58.9900690087408,43.9727478937056,
0.));
#151271=CARTESIAN_POINT('Ctrl Pts',(-58.9766723902529,43.9497182316331,
0.));
#151272=CARTESIAN_POINT('Ctrl Pts',(-58.9632731052696,43.9267328191501,
0.));
#151273=CARTESIAN_POINT('Ctrl Pts',(-58.9498712429054,43.9037917117739,
0.));
#151274=CARTESIAN_POINT('Ctrl Pts',(-58.936466892712,43.8808949651873,0.));
#151275=CARTESIAN_POINT('Ctrl Pts',(-58.9230601446436,43.858042635223,0.));
#151276=CARTESIAN_POINT('Ctrl Pts',(-58.9096510890129,43.835234777842,0.));
#151277=CARTESIAN_POINT('Ctrl Pts',(-58.8962398164493,43.8124714491076,
0.));
#151278=CARTESIAN_POINT('Ctrl Pts',(-58.8828264178621,43.7897527051609,
0.));
#151279=CARTESIAN_POINT('Ctrl Pts',(-58.8694109844648,43.7670786022402,
0.));
#151280=CARTESIAN_POINT('Ctrl Pts',(-58.855993607794,43.7444491966942,0.));
#151281=CARTESIAN_POINT('Ctrl Pts',(-58.8425743797326,43.7218645449922,
0.));
#151282=CARTESIAN_POINT('Ctrl Pts',(-58.8291533925293,43.6993247037314,
0.));
#151283=CARTESIAN_POINT('Ctrl Pts',(-58.8157307388238,43.6768297296395,
0.));
#151284=CARTESIAN_POINT('Ctrl Pts',(-58.8023065116436,43.6543796795789,
0.));
#151285=CARTESIAN_POINT('Ctrl Pts',(-58.788880804397,43.6319746105482,0.));
#151286=CARTESIAN_POINT('Ctrl Pts',(-58.775453710867,43.6096145796797,0.));
#151287=CARTESIAN_POINT('Ctrl Pts',(-58.7620253252062,43.5872996442345,
0.));
#151288=CARTESIAN_POINT('Ctrl Pts',(-58.74859574193,43.5650298615917,0.));
#151289=CARTESIAN_POINT('Ctrl Pts',(-58.735165055918,43.5428052892488,0.));
#151290=CARTESIAN_POINT('Ctrl Pts',(-58.7217333624209,43.5206259848337,
0.));
#151291=CARTESIAN_POINT('Ctrl Pts',(-58.7083007570661,43.4984920061073,
0.));
#151292=CARTESIAN_POINT('Ctrl Pts',(-58.6948673358638,43.4764034109654,
0.));
#151293=CARTESIAN_POINT('Ctrl Pts',(-58.6814331952138,43.4543602574351,
0.));
#151294=CARTESIAN_POINT('Ctrl Pts',(-58.6679984319097,43.4323626036737,
0.));
#151295=CARTESIAN_POINT('Ctrl Pts',(-58.6545631431393,43.4104105079768,
0.));
#151296=CARTESIAN_POINT('Ctrl Pts',(-58.6411274264857,43.388504028781,0.));
#151297=CARTESIAN_POINT('Ctrl Pts',(-58.627691379929,43.3666432246635,0.));
#151298=CARTESIAN_POINT('Ctrl Pts',(-58.6142551018467,43.3448281543371,
0.));
#151299=CARTESIAN_POINT('Ctrl Pts',(-58.6008186910156,43.3230588766449,
0.));
#151300=CARTESIAN_POINT('Ctrl Pts',(-58.5873822466152,43.3013354505701,
0.));
#151301=CARTESIAN_POINT('Ctrl Pts',(-58.573945868231,43.27965793524,0.));
#151302=CARTESIAN_POINT('Ctrl Pts',(-58.5605096558578,43.2580263899278,
0.));
#151303=CARTESIAN_POINT('Ctrl Pts',(-58.5470737099032,43.2364408740493,
0.));
#151304=CARTESIAN_POINT('Ctrl Pts',(-58.5336381311917,43.2149014471574,
0.));
#151305=CARTESIAN_POINT('Ctrl Pts',(-58.5202030209669,43.1934081689505,
0.));
#151306=CARTESIAN_POINT('Ctrl Pts',(-58.5067684808944,43.1719610992771,
0.));
#151307=CARTESIAN_POINT('Ctrl Pts',(-58.4933346130636,43.1505602981365,
0.));
#151308=CARTESIAN_POINT('Ctrl Pts',(-58.4799015199907,43.1292058256777,
0.));
#151309=CARTESIAN_POINT('Ctrl Pts',(-58.4664693046217,43.1078977421916,
0.));
#151310=CARTESIAN_POINT('Ctrl Pts',(-58.4530380703348,43.0866361081177,
0.));
#151311=CARTESIAN_POINT('Ctrl Pts',(-58.439607920945,43.0654209840511,0.));
#151312=CARTESIAN_POINT('Ctrl Pts',(-58.4261789607058,43.0442524307434,
0.));
#151313=CARTESIAN_POINT('Ctrl Pts',(-58.4127512943136,43.0231305091027,
0.));
#151314=CARTESIAN_POINT('Ctrl Pts',(-58.3993250269101,43.0020552801859,
0.));
#151315=CARTESIAN_POINT('Ctrl Pts',(-58.3859002640856,42.9810268052032,
0.));
#151316=CARTESIAN_POINT('Ctrl Pts',(-58.3724771118826,42.960045145526,0.));
#151317=CARTESIAN_POINT('Ctrl Pts',(-58.3590556767978,42.9391103626879,
0.));
#151318=CARTESIAN_POINT('Ctrl Pts',(-58.3456360657865,42.9182225183855,
0.));
#151319=CARTESIAN_POINT('Ctrl Pts',(-58.3322183862654,42.8973816744709,
0.));
#151320=CARTESIAN_POINT('Ctrl Pts',(-58.3188027461164,42.8765878929551,
0.));
#151321=CARTESIAN_POINT('Ctrl Pts',(-58.3053892536894,42.8558412360158,
0.));
#151322=CARTESIAN_POINT('Ctrl Pts',(-58.2919780178064,42.8351417659999,
0.));
#151323=CARTESIAN_POINT('Ctrl Pts',(-58.2785691477638,42.8144895454233,
0.));
#151324=CARTESIAN_POINT('Ctrl Pts',(-58.2651627533368,42.7938846369651,
0.));
#151325=CARTESIAN_POINT('Ctrl Pts',(-58.251758944782,42.7733271034679,0.));
#151326=CARTESIAN_POINT('Ctrl Pts',(-58.2383578328424,42.7528170079484,
0.));
#151327=CARTESIAN_POINT('Ctrl Pts',(-58.22495952875,42.7323544135985,0.));
#151328=CARTESIAN_POINT('Ctrl Pts',(-58.21156414423,42.7119393837866,0.));
#151329=CARTESIAN_POINT('Ctrl Pts',(-58.1981717915037,42.6915719820513,
0.));
#151330=CARTESIAN_POINT('Ctrl Pts',(-58.1847825832923,42.6712522721016,
0.));
#151331=CARTESIAN_POINT('Ctrl Pts',(-58.171396632821,42.6509803178265,0.));
#151332=CARTESIAN_POINT('Ctrl Pts',(-58.1580140538228,42.6307561832976,
0.));
#151333=CARTESIAN_POINT('Ctrl Pts',(-58.1446349605421,42.6105799327699,
0.));
#151334=CARTESIAN_POINT('Ctrl Pts',(-58.1312594677386,42.5904516306762,
0.));
#151335=CARTESIAN_POINT('Ctrl Pts',(-58.1178876906907,42.5703713416265,
0.));
#151336=CARTESIAN_POINT('Ctrl Pts',(-58.1045197452002,42.5503391304183,
0.));
#151337=CARTESIAN_POINT('Ctrl Pts',(-58.0911557475965,42.5303550620387,
0.));
#151338=CARTESIAN_POINT('Ctrl Pts',(-58.0777958147403,42.5104192016664,
0.));
#151339=CARTESIAN_POINT('Ctrl Pts',(-58.0644400640275,42.4905316146653,
0.));
#151340=CARTESIAN_POINT('Ctrl Pts',(-58.0510886133926,42.4706923665845,
0.));
#151341=CARTESIAN_POINT('Ctrl Pts',(-58.037741581314,42.4509015231674,0.));
#151342=CARTESIAN_POINT('Ctrl Pts',(-58.0243990868181,42.4311591503555,
0.));
#151343=CARTESIAN_POINT('Ctrl Pts',(-58.0110612494828,42.411465314289,0.));
#151344=CARTESIAN_POINT('Ctrl Pts',(-57.9977281894422,42.3918200813014,
0.));
#151345=CARTESIAN_POINT('Ctrl Pts',(-57.9844000273911,42.3722235179197,
0.));
#151346=CARTESIAN_POINT('Ctrl Pts',(-57.9710768845899,42.3526756908746,
0.));
#151347=CARTESIAN_POINT('Ctrl Pts',(-57.9577588828682,42.333176667102,0.));
#151348=CARTESIAN_POINT('Ctrl Pts',(-57.9444461446299,42.3137265137452,
0.));
#151349=CARTESIAN_POINT('Ctrl Pts',(-57.9311387928563,42.2943252981489,
0.));
#151350=CARTESIAN_POINT('Ctrl Pts',(-57.9178369511114,42.2749730878594,
0.));
#151351=CARTESIAN_POINT('Ctrl Pts',(-57.9045407435474,42.2556699506353,
0.));
#151352=CARTESIAN_POINT('Ctrl Pts',(-57.8912502949096,42.2364159544501,
0.));
#151353=CARTESIAN_POINT('Ctrl Pts',(-57.8779657305413,42.2172111674938,
0.));
#151354=CARTESIAN_POINT('Ctrl Pts',(-57.864687176387,42.1980556581665,0.));
#151355=CARTESIAN_POINT('Ctrl Pts',(-57.8514147589972,42.1789494950794,
0.));
#151356=CARTESIAN_POINT('Ctrl Pts',(-57.8381486055342,42.1598927470646,
0.));
#151357=CARTESIAN_POINT('Ctrl Pts',(-57.8248888437775,42.1408854831783,
0.));
#151358=CARTESIAN_POINT('Ctrl Pts',(-57.8116356021288,42.1219277727021,
0.));
#151359=CARTESIAN_POINT('Ctrl Pts',(-57.798389009616,42.1030196851366,0.));
#151360=CARTESIAN_POINT('Ctrl Pts',(-57.7851491958987,42.0841612902042,
0.));
#151361=CARTESIAN_POINT('Ctrl Pts',(-57.7719162912744,42.0653526578588,
0.));
#151362=CARTESIAN_POINT('Ctrl Pts',(-57.7586904266834,42.0465938582882,
0.));
#151363=CARTESIAN_POINT('Ctrl Pts',(-57.745471733714,42.0278849619148,0.));
#151364=CARTESIAN_POINT('Ctrl Pts',(-57.7322603446066,42.0092260393897,
0.));
#151365=CARTESIAN_POINT('Ctrl Pts',(-57.7190563922593,41.990617161596,0.));
#151366=CARTESIAN_POINT('Ctrl Pts',(-57.7058600102351,41.9720583996592,
0.));
#151367=CARTESIAN_POINT('Ctrl Pts',(-57.6926713327672,41.9535498249488,
0.));
#151368=CARTESIAN_POINT('Ctrl Pts',(-57.6794904947649,41.9350915090796,
0.));
#151369=CARTESIAN_POINT('Ctrl Pts',(-57.6663176318189,41.9166835239054,
0.));
#151370=CARTESIAN_POINT('Ctrl Pts',(-57.6531528802072,41.8983259415253,
0.));
#151371=CARTESIAN_POINT('Ctrl Pts',(-57.6399963769009,41.8800188342912,
0.));
#151372=CARTESIAN_POINT('Ctrl Pts',(-57.6268482595701,41.8617622748107,
0.));
#151373=CARTESIAN_POINT('Ctrl Pts',(-57.613708666588,41.8435563359456,0.));
#151374=CARTESIAN_POINT('Ctrl Pts',(-57.6005777370347,41.8254010908051,
0.));
#151375=CARTESIAN_POINT('Ctrl Pts',(-57.5874556107054,41.8072966127559,
0.));
#151376=CARTESIAN_POINT('Ctrl Pts',(-57.5743424281204,41.7892429754298,
0.));
#151377=CARTESIAN_POINT('Ctrl Pts',(-57.561238330532,41.7712402527273,0.));
#151378=CARTESIAN_POINT('Ctrl Pts',(-57.5481434599334,41.7532885188174,
0.));
#151379=CARTESIAN_POINT('Ctrl Pts',(-57.5350579590648,41.7353878481336,
0.));
#151380=CARTESIAN_POINT('Ctrl Pts',(-57.5219819714169,41.7175383153819,
0.));
#151381=CARTESIAN_POINT('Ctrl Pts',(-57.5089156412341,41.6997399955445,
0.));
#151382=CARTESIAN_POINT('Ctrl Pts',(-57.4958591135165,41.6819929638797,
0.));
#151383=CARTESIAN_POINT('Ctrl Pts',(-57.4828125340222,41.6642972959168,
0.));
#151384=CARTESIAN_POINT('Ctrl Pts',(-57.4697760492693,41.6466530674522,
0.));
#151385=CARTESIAN_POINT('Ctrl Pts',(-57.4567498065573,41.6290603545674,
0.));
#151386=CARTESIAN_POINT('Ctrl Pts',(-57.4437339539848,41.6115192336393,
0.));
#151387=CARTESIAN_POINT('Ctrl Pts',(-57.4307286404656,41.5940297813474,
0.));
#151388=CARTESIAN_POINT('Ctrl Pts',(-57.417734015749,41.5765920746764,0.));
#151389=CARTESIAN_POINT('Ctrl Pts',(-57.4047502304207,41.5592061909159,
0.));
#151390=CARTESIAN_POINT('Ctrl Pts',(-57.3917774358844,41.5418722076558,
0.));
#151391=CARTESIAN_POINT('Ctrl Pts',(-57.378815784345,41.5245902027767,0.));
#151392=CARTESIAN_POINT('Ctrl Pts',(-57.3658654287948,41.5073602544404,
0.));
#151393=CARTESIAN_POINT('Ctrl Pts',(-57.3529265229858,41.4901824410654,
0.));
#151394=CARTESIAN_POINT('Ctrl Pts',(-57.339999221474,41.4730568413535,0.));
#151395=CARTESIAN_POINT('Ctrl Pts',(-57.3270836796925,41.4559835343338,
0.));
#151396=CARTESIAN_POINT('Ctrl Pts',(-57.3141800540137,41.4389625993948,
0.));
#151397=CARTESIAN_POINT('Ctrl Pts',(-57.3012885018139,41.4219941163154,
0.));
#151398=CARTESIAN_POINT('Ctrl Pts',(-57.2884091815385,41.4050781652923,
0.));
#151399=CARTESIAN_POINT('Ctrl Pts',(-57.2755422525822,41.3882148268798,
0.));
#151400=CARTESIAN_POINT('Ctrl Pts',(-57.2626878751584,41.3714041819215,
0.));
#151401=CARTESIAN_POINT('Ctrl Pts',(-57.2498462101883,41.3546463114889,
0.));
#151402=CARTESIAN_POINT('Ctrl Pts',(-57.237017419142,41.3379412967889,0.));
#151403=CARTESIAN_POINT('Ctrl Pts',(-57.2242016640226,41.321289219151,0.));
#151404=CARTESIAN_POINT('Ctrl Pts',(-57.2113991077325,41.304690160231,0.));
#151405=CARTESIAN_POINT('Ctrl Pts',(-57.1986099143992,41.2881442021869,
0.));
#151406=CARTESIAN_POINT('Ctrl Pts',(-57.1858342496526,41.2716514278268,
0.));
#151407=CARTESIAN_POINT('Ctrl Pts',(-57.1730722810771,41.2552119208445,
0.));
#151408=CARTESIAN_POINT('Ctrl Pts',(-57.1603241779042,41.2388257656534,
0.));
#151409=CARTESIAN_POINT('Ctrl Pts',(-57.1475901101795,41.2224930469412,
0.));
#151410=CARTESIAN_POINT('Ctrl Pts',(-57.1348702480644,41.2062138492913,
0.));
#151411=CARTESIAN_POINT('Ctrl Pts',(-57.1221647611231,41.1899882567941,
0.));
#151412=CARTESIAN_POINT('Ctrl Pts',(-57.1094738174998,41.1738163525931,
0.));
#151413=CARTESIAN_POINT('Ctrl Pts',(-57.0967975854912,41.1576982197402,
0.));
#151414=CARTESIAN_POINT('Ctrl Pts',(-57.0841362354281,41.1416339422132,
0.));
#151415=CARTESIAN_POINT('Ctrl Pts',(-57.0714899412091,41.1256236057436,
0.));
#151416=CARTESIAN_POINT('Ctrl Pts',(-57.0588588825266,41.1096672990125,
0.));
#151417=CARTESIAN_POINT('Ctrl Pts',(-57.0462432450637,41.0937651137519,
0.));
#151418=CARTESIAN_POINT('Ctrl Pts',(-57.0336432158503,41.0779171422415,
0.));
#151419=CARTESIAN_POINT('Ctrl Pts',(-57.0210589791777,41.0621234751,0.));
#151420=CARTESIAN_POINT('Ctrl Pts',(-57.008490713044,41.0463841993622,0.));
#151421=CARTESIAN_POINT('Ctrl Pts',(-56.9959385834768,41.0306993954021,
0.));
#151422=CARTESIAN_POINT('Ctrl Pts',(-56.9834027500178,41.0150691398988,
0.));
#151423=CARTESIAN_POINT('Ctrl Pts',(-56.9708833766183,40.9994935117307,
0.));
#151424=CARTESIAN_POINT('Ctrl Pts',(-56.9583806404069,40.9839725967121,
0.));
#151425=CARTESIAN_POINT('Ctrl Pts',(-56.9458947422541,40.968506493303,0.));
#151426=CARTESIAN_POINT('Ctrl Pts',(-56.9334259139928,40.9530953164952,
0.));
#151427=CARTESIAN_POINT('Ctrl Pts',(-56.9209743960861,40.9377391857044,
0.));
#151428=CARTESIAN_POINT('Ctrl Pts',(-56.9085404164432,40.9224382132382,
0.));
#151429=CARTESIAN_POINT('Ctrl Pts',(-56.8961241708926,40.9071924937551,
0.));
#151430=CARTESIAN_POINT('Ctrl Pts',(-56.8837257978574,40.8920020903443,
0.));
#151431=CARTESIAN_POINT('Ctrl Pts',(-56.8713453765252,40.8768670342278,
0.));
#151432=CARTESIAN_POINT('Ctrl Pts',(-56.8614554317993,40.8648032759631,
0.));
#151433=CARTESIAN_POINT('Ctrl Pts',(-56.8540460739677,40.8557803680411,
0.));
#151434=CARTESIAN_POINT('Ctrl Pts',(-56.8491101022668,40.8497761671086,
0.));
#151435=CARTESIAN_POINT('Ctrl Pts',(-56.8466430164621,40.8467768343956,
0.));
#151436=CARTESIAN_POINT('Ctrl Pts',(-55.3473204966403,49.8690697110161,
0.));
#151437=CARTESIAN_POINT('Ctrl Pts',(-55.3473204966403,49.8690697110161,
12.));
#151438=CARTESIAN_POINT('Ctrl Pts',(-55.3451131058826,49.8639277221566,
0.));
#151439=CARTESIAN_POINT('Ctrl Pts',(-55.3451131058826,49.8639277221566,
12.));
#151440=CARTESIAN_POINT('Ctrl Pts',(-55.34069740326,49.8536479176833,0.));
#151441=CARTESIAN_POINT('Ctrl Pts',(-55.34069740326,49.8536479176833,12.));
#151442=CARTESIAN_POINT('Ctrl Pts',(-55.3340710860055,49.8382407307107,
0.));
#151443=CARTESIAN_POINT('Ctrl Pts',(-55.3340710860055,49.8382407307107,
12.));
#151444=CARTESIAN_POINT('Ctrl Pts',(-55.3252304694602,49.8177228552376,
0.));
#151445=CARTESIAN_POINT('Ctrl Pts',(-55.3252304694602,49.8177228552376,
12.));
#151446=CARTESIAN_POINT('Ctrl Pts',(-55.3141704897766,49.7921172540628,
0.));
#151447=CARTESIAN_POINT('Ctrl Pts',(-55.3141704897766,49.7921172540628,
12.));
#151448=CARTESIAN_POINT('Ctrl Pts',(-55.3031013105853,49.7665534128535,
0.));
#151449=CARTESIAN_POINT('Ctrl Pts',(-55.3031013105853,49.7665534128535,
12.));
#151450=CARTESIAN_POINT('Ctrl Pts',(-55.2920229527546,49.7410313576508,
0.));
#151451=CARTESIAN_POINT('Ctrl Pts',(-55.2920229527546,49.7410313576508,
12.));
#151452=CARTESIAN_POINT('Ctrl Pts',(-55.2809354521515,49.7155511248531,
0.));
#151453=CARTESIAN_POINT('Ctrl Pts',(-55.2809354521515,49.7155511248531,
12.));
#151454=CARTESIAN_POINT('Ctrl Pts',(-55.2698388650025,49.6901127631627,
0.));
#151455=CARTESIAN_POINT('Ctrl Pts',(-55.2698388650025,49.6901127631627,
12.));
#151456=CARTESIAN_POINT('Ctrl Pts',(-55.2587332663783,49.6647163322266,
0.));
#151457=CARTESIAN_POINT('Ctrl Pts',(-55.2587332663783,49.6647163322266,
12.));
#151458=CARTESIAN_POINT('Ctrl Pts',(-55.2476187434057,49.6393618987473,
0.));
#151459=CARTESIAN_POINT('Ctrl Pts',(-55.2476187434057,49.6393618987473,
12.));
#151460=CARTESIAN_POINT('Ctrl Pts',(-55.2364953899358,49.6140495332803,
0.));
#151461=CARTESIAN_POINT('Ctrl Pts',(-55.2364953899358,49.6140495332803,
12.));
#151462=CARTESIAN_POINT('Ctrl Pts',(-55.2253633007666,49.5887793068352,
0.));
#151463=CARTESIAN_POINT('Ctrl Pts',(-55.2253633007666,49.5887793068352,
12.));
#151464=CARTESIAN_POINT('Ctrl Pts',(-55.2142225657013,49.5635512873435,
0.));
#151465=CARTESIAN_POINT('Ctrl Pts',(-55.2142225657013,49.5635512873435,
12.));
#151466=CARTESIAN_POINT('Ctrl Pts',(-55.2030732647312,49.5383655368073,
0.));
#151467=CARTESIAN_POINT('Ctrl Pts',(-55.2030732647312,49.5383655368073,
12.));
#151468=CARTESIAN_POINT('Ctrl Pts',(-55.1919154713647,49.5132221132992,
0.));
#151469=CARTESIAN_POINT('Ctrl Pts',(-55.1919154713647,49.5132221132992,
12.));
#151470=CARTESIAN_POINT('Ctrl Pts',(-55.1807492550119,49.4881210723966,
0.));
#151471=CARTESIAN_POINT('Ctrl Pts',(-55.1807492550119,49.4881210723966,
12.));
#151472=CARTESIAN_POINT('Ctrl Pts',(-55.1695746838174,49.4630624688793,
0.));
#151473=CARTESIAN_POINT('Ctrl Pts',(-55.1695746838174,49.4630624688793,
12.));
#151474=CARTESIAN_POINT('Ctrl Pts',(-55.1583918271116,49.4380463581965,
0.));
#151475=CARTESIAN_POINT('Ctrl Pts',(-55.1583918271116,49.4380463581965,
12.));
#151476=CARTESIAN_POINT('Ctrl Pts',(-55.1472007585183,49.4130727983201,
0.));
#151477=CARTESIAN_POINT('Ctrl Pts',(-55.1472007585183,49.4130727983201,
12.));
#151478=CARTESIAN_POINT('Ctrl Pts',(-55.1360015556221,49.3881418495489,
0.));
#151479=CARTESIAN_POINT('Ctrl Pts',(-55.1360015556221,49.3881418495489,
12.));
#151480=CARTESIAN_POINT('Ctrl Pts',(-55.1247942985619,49.3632535736715,
0.));
#151481=CARTESIAN_POINT('Ctrl Pts',(-55.1247942985619,49.3632535736715,
12.));
#151482=CARTESIAN_POINT('Ctrl Pts',(-55.1135790689464,49.3384080333155,
0.));
#151483=CARTESIAN_POINT('Ctrl Pts',(-55.1135790689464,49.3384080333155,
12.));
#151484=CARTESIAN_POINT('Ctrl Pts',(-55.102355948714,49.3136052912621,0.));
#151485=CARTESIAN_POINT('Ctrl Pts',(-55.102355948714,49.3136052912621,12.));
#151486=CARTESIAN_POINT('Ctrl Pts',(-55.0911250188302,49.2888454096563,
0.));
#151487=CARTESIAN_POINT('Ctrl Pts',(-55.0911250188302,49.2888454096563,
12.));
#151488=CARTESIAN_POINT('Ctrl Pts',(-55.079886358701,49.264128449652,0.));
#151489=CARTESIAN_POINT('Ctrl Pts',(-55.079886358701,49.264128449652,12.));
#151490=CARTESIAN_POINT('Ctrl Pts',(-55.0686400468931,49.2394544718531,
0.));
#151491=CARTESIAN_POINT('Ctrl Pts',(-55.0686400468931,49.2394544718531,
12.));
#151492=CARTESIAN_POINT('Ctrl Pts',(-55.0573861615579,49.2148235365703,
0.));
#151493=CARTESIAN_POINT('Ctrl Pts',(-55.0573861615579,49.2148235365703,
12.));
#151494=CARTESIAN_POINT('Ctrl Pts',(-55.0461247809744,49.1902357041461,
0.));
#151495=CARTESIAN_POINT('Ctrl Pts',(-55.0461247809744,49.1902357041461,
12.));
#151496=CARTESIAN_POINT('Ctrl Pts',(-55.0348559840453,49.1656910352476,
0.));
#151497=CARTESIAN_POINT('Ctrl Pts',(-55.0348559840453,49.1656910352476,
12.));
#151498=CARTESIAN_POINT('Ctrl Pts',(-55.0235798508045,49.1411895911635,
0.));
#151499=CARTESIAN_POINT('Ctrl Pts',(-55.0235798508045,49.1411895911635,
12.));
#151500=CARTESIAN_POINT('Ctrl Pts',(-55.012296462186,49.116731433673,0.));
#151501=CARTESIAN_POINT('Ctrl Pts',(-55.012296462186,49.116731433673,12.));
#151502=CARTESIAN_POINT('Ctrl Pts',(-55.0010058998107,49.0923166249219,
0.));
#151503=CARTESIAN_POINT('Ctrl Pts',(-55.0010058998107,49.0923166249219,
12.));
#151504=CARTESIAN_POINT('Ctrl Pts',(-54.9897082457606,49.067945227287,0.));
#151505=CARTESIAN_POINT('Ctrl Pts',(-54.9897082457606,49.067945227287,12.));
#151506=CARTESIAN_POINT('Ctrl Pts',(-54.9784035823766,49.0436173032528,
0.));
#151507=CARTESIAN_POINT('Ctrl Pts',(-54.9784035823766,49.0436173032528,
12.));
#151508=CARTESIAN_POINT('Ctrl Pts',(-54.9670919920029,49.0193329152479,
0.));
#151509=CARTESIAN_POINT('Ctrl Pts',(-54.9670919920029,49.0193329152479,
12.));
#151510=CARTESIAN_POINT('Ctrl Pts',(-54.9557735569943,48.9950921256526,
0.));
#151511=CARTESIAN_POINT('Ctrl Pts',(-54.9557735569943,48.9950921256526,
12.));
#151512=CARTESIAN_POINT('Ctrl Pts',(-54.9444483598378,48.9708949968795,
0.));
#151513=CARTESIAN_POINT('Ctrl Pts',(-54.9444483598378,48.9708949968795,
12.));
#151514=CARTESIAN_POINT('Ctrl Pts',(-54.9331164832424,48.9467415914269,
0.));
#151515=CARTESIAN_POINT('Ctrl Pts',(-54.9331164832424,48.9467415914269,
12.));
#151516=CARTESIAN_POINT('Ctrl Pts',(-54.9217780102355,48.9226319719368,
0.));
#151517=CARTESIAN_POINT('Ctrl Pts',(-54.9217780102355,48.9226319719368,
12.));
#151518=CARTESIAN_POINT('Ctrl Pts',(-54.9104330242742,48.8985662012528,
0.));
#151519=CARTESIAN_POINT('Ctrl Pts',(-54.9104330242742,48.8985662012528,
12.));
#151520=CARTESIAN_POINT('Ctrl Pts',(-54.8990816092953,48.8745443424477,
0.));
#151521=CARTESIAN_POINT('Ctrl Pts',(-54.8990816092953,48.8745443424477,
12.));
#151522=CARTESIAN_POINT('Ctrl Pts',(-54.8877238496566,48.8505664587974,
0.));
#151523=CARTESIAN_POINT('Ctrl Pts',(-54.8877238496566,48.8505664587974,
12.));
#151524=CARTESIAN_POINT('Ctrl Pts',(-54.8763598301037,48.8266326137622,
0.));
#151525=CARTESIAN_POINT('Ctrl Pts',(-54.8763598301037,48.8266326137622,
12.));
#151526=CARTESIAN_POINT('Ctrl Pts',(-54.8649896357285,48.8027428709614,
0.));
#151527=CARTESIAN_POINT('Ctrl Pts',(-54.8649896357285,48.8027428709614,
12.));
#151528=CARTESIAN_POINT('Ctrl Pts',(-54.8536133519292,48.7788972941438,
0.));
#151529=CARTESIAN_POINT('Ctrl Pts',(-54.8536133519292,48.7788972941438,
12.));
#151530=CARTESIAN_POINT('Ctrl Pts',(-54.8422310643763,48.7550959471601,
0.));
#151531=CARTESIAN_POINT('Ctrl Pts',(-54.8422310643763,48.7550959471601,
12.));
#151532=CARTESIAN_POINT('Ctrl Pts',(-54.8308428590344,48.7313388939845,
0.));
#151533=CARTESIAN_POINT('Ctrl Pts',(-54.8308428590344,48.7313388939845,
12.));
#151534=CARTESIAN_POINT('Ctrl Pts',(-54.819448822181,48.7076261987292,0.));
#151535=CARTESIAN_POINT('Ctrl Pts',(-54.819448822181,48.7076261987292,12.));
#151536=CARTESIAN_POINT('Ctrl Pts',(-54.8080490404275,48.6839579256566,
0.));
#151537=CARTESIAN_POINT('Ctrl Pts',(-54.8080490404275,48.6839579256566,
12.));
#151538=CARTESIAN_POINT('Ctrl Pts',(-54.796643600739,48.6603341391886,0.));
#151539=CARTESIAN_POINT('Ctrl Pts',(-54.796643600739,48.6603341391886,12.));
#151540=CARTESIAN_POINT('Ctrl Pts',(-54.7852325904583,48.6367549039112,
0.));
#151541=CARTESIAN_POINT('Ctrl Pts',(-54.7852325904583,48.6367549039112,
12.));
#151542=CARTESIAN_POINT('Ctrl Pts',(-54.7738160973031,48.6132202845783,
0.));
#151543=CARTESIAN_POINT('Ctrl Pts',(-54.7738160973031,48.6132202845783,
12.));
#151544=CARTESIAN_POINT('Ctrl Pts',(-54.7623942093586,48.5897303461125,
0.));
#151545=CARTESIAN_POINT('Ctrl Pts',(-54.7623942093586,48.5897303461125,
12.));
#151546=CARTESIAN_POINT('Ctrl Pts',(-54.7509670150714,48.5662851536026,
0.));
#151547=CARTESIAN_POINT('Ctrl Pts',(-54.7509670150714,48.5662851536026,
12.));
#151548=CARTESIAN_POINT('Ctrl Pts',(-54.7395346032453,48.5428847722977,
0.));
#151549=CARTESIAN_POINT('Ctrl Pts',(-54.7395346032453,48.5428847722977,
12.));
#151550=CARTESIAN_POINT('Ctrl Pts',(-54.7280970630351,48.519529267596,0.));
#151551=CARTESIAN_POINT('Ctrl Pts',(-54.7280970630351,48.519529267596,12.));
#151552=CARTESIAN_POINT('Ctrl Pts',(-54.716654483948,48.4962187050457,0.));
#151553=CARTESIAN_POINT('Ctrl Pts',(-54.716654483948,48.4962187050457,12.));
#151554=CARTESIAN_POINT('Ctrl Pts',(-54.7052069558497,48.472953150357,0.));
#151555=CARTESIAN_POINT('Ctrl Pts',(-54.7052069558497,48.472953150357,12.));
#151556=CARTESIAN_POINT('Ctrl Pts',(-54.6937545689695,48.4497326694052,
0.));
#151557=CARTESIAN_POINT('Ctrl Pts',(-54.6937545689695,48.4497326694052,
12.));
#151558=CARTESIAN_POINT('Ctrl Pts',(-54.6822974139064,48.426557328234,0.));
#151559=CARTESIAN_POINT('Ctrl Pts',(-54.6822974139064,48.426557328234,12.));
#151560=CARTESIAN_POINT('Ctrl Pts',(-54.6708355816358,48.4034271930514,
0.));
#151561=CARTESIAN_POINT('Ctrl Pts',(-54.6708355816358,48.4034271930514,
12.));
#151562=CARTESIAN_POINT('Ctrl Pts',(-54.6593691635145,48.3803423302294,
0.));
#151563=CARTESIAN_POINT('Ctrl Pts',(-54.6593691635145,48.3803423302294,
12.));
#151564=CARTESIAN_POINT('Ctrl Pts',(-54.6478982512794,48.3573028063124,
0.));
#151565=CARTESIAN_POINT('Ctrl Pts',(-54.6478982512794,48.3573028063124,
12.));
#151566=CARTESIAN_POINT('Ctrl Pts',(-54.6364229370494,48.3343086880194,
0.));
#151567=CARTESIAN_POINT('Ctrl Pts',(-54.6364229370494,48.3343086880194,
12.));
#151568=CARTESIAN_POINT('Ctrl Pts',(-54.6249433133261,48.3113600422443,
0.));
#151569=CARTESIAN_POINT('Ctrl Pts',(-54.6249433133261,48.3113600422443,
12.));
#151570=CARTESIAN_POINT('Ctrl Pts',(-54.6134594729959,48.2884569360506,
0.));
#151571=CARTESIAN_POINT('Ctrl Pts',(-54.6134594729959,48.2884569360506,
12.));
#151572=CARTESIAN_POINT('Ctrl Pts',(-54.6019715093309,48.2655994366665,
0.));
#151573=CARTESIAN_POINT('Ctrl Pts',(-54.6019715093309,48.2655994366665,
12.));
#151574=CARTESIAN_POINT('Ctrl Pts',(-54.5904795159926,48.2427876114947,
0.));
#151575=CARTESIAN_POINT('Ctrl Pts',(-54.5904795159926,48.2427876114947,
12.));
#151576=CARTESIAN_POINT('Ctrl Pts',(-54.5789835870342,48.2200215281173,
0.));
#151577=CARTESIAN_POINT('Ctrl Pts',(-54.5789835870342,48.2200215281173,
12.));
#151578=CARTESIAN_POINT('Ctrl Pts',(-54.5674838169041,48.1973012542966,
0.));
#151579=CARTESIAN_POINT('Ctrl Pts',(-54.5674838169041,48.1973012542966,
12.));
#151580=CARTESIAN_POINT('Ctrl Pts',(-54.5559803004492,48.1746268579736,
0.));
#151581=CARTESIAN_POINT('Ctrl Pts',(-54.5559803004492,48.1746268579736,
12.));
#151582=CARTESIAN_POINT('Ctrl Pts',(-54.5444731329201,48.1519984072622,
0.));
#151583=CARTESIAN_POINT('Ctrl Pts',(-54.5444731329201,48.1519984072622,
12.));
#151584=CARTESIAN_POINT('Ctrl Pts',(-54.5329624099721,48.1294159704573,
0.));
#151585=CARTESIAN_POINT('Ctrl Pts',(-54.5329624099721,48.1294159704573,
12.));
#151586=CARTESIAN_POINT('Ctrl Pts',(-54.5214482276678,48.1068796160405,
0.));
#151587=CARTESIAN_POINT('Ctrl Pts',(-54.5214482276678,48.1068796160405,
12.));
#151588=CARTESIAN_POINT('Ctrl Pts',(-54.5099306824786,48.0843894126806,
0.));
#151589=CARTESIAN_POINT('Ctrl Pts',(-54.5099306824786,48.0843894126806,
12.));
#151590=CARTESIAN_POINT('Ctrl Pts',(-54.4984098712886,48.0619454292324,
0.));
#151591=CARTESIAN_POINT('Ctrl Pts',(-54.4984098712886,48.0619454292324,
12.));
#151592=CARTESIAN_POINT('Ctrl Pts',(-54.4868858913971,48.0395477347298,
0.));
#151593=CARTESIAN_POINT('Ctrl Pts',(-54.4868858913971,48.0395477347298,
12.));
#151594=CARTESIAN_POINT('Ctrl Pts',(-54.4753588405215,48.0171963983924,
0.));
#151595=CARTESIAN_POINT('Ctrl Pts',(-54.4753588405215,48.0171963983924,
12.));
#151596=CARTESIAN_POINT('Ctrl Pts',(-54.4638288168003,47.9948914896326,
0.));
#151597=CARTESIAN_POINT('Ctrl Pts',(-54.4638288168003,47.9948914896326,
12.));
#151598=CARTESIAN_POINT('Ctrl Pts',(-54.4522959187955,47.9726330780572,
0.));
#151599=CARTESIAN_POINT('Ctrl Pts',(-54.4522959187955,47.9726330780572,
12.));
#151600=CARTESIAN_POINT('Ctrl Pts',(-54.4407602454967,47.9504212334675,
0.));
#151601=CARTESIAN_POINT('Ctrl Pts',(-54.4407602454967,47.9504212334675,
12.));
#151602=CARTESIAN_POINT('Ctrl Pts',(-54.429221896324,47.9282560258516,0.));
#151603=CARTESIAN_POINT('Ctrl Pts',(-54.429221896324,47.9282560258516,12.));
#151604=CARTESIAN_POINT('Ctrl Pts',(-54.4176809711311,47.9061375253897,
0.));
#151605=CARTESIAN_POINT('Ctrl Pts',(-54.4176809711311,47.9061375253897,
12.));
#151606=CARTESIAN_POINT('Ctrl Pts',(-54.4061375702079,47.8840658024618,
0.));
#151607=CARTESIAN_POINT('Ctrl Pts',(-54.4061375702079,47.8840658024618,
12.));
#151608=CARTESIAN_POINT('Ctrl Pts',(-54.3945917942832,47.8620409276493,
0.));
#151609=CARTESIAN_POINT('Ctrl Pts',(-54.3945917942832,47.8620409276493,
12.));
#151610=CARTESIAN_POINT('Ctrl Pts',(-54.3830437445279,47.8400629717355,
0.));
#151611=CARTESIAN_POINT('Ctrl Pts',(-54.3830437445279,47.8400629717355,
12.));
#151612=CARTESIAN_POINT('Ctrl Pts',(-54.3714935225591,47.8181320056995,
0.));
#151613=CARTESIAN_POINT('Ctrl Pts',(-54.3714935225591,47.8181320056995,
12.));
#151614=CARTESIAN_POINT('Ctrl Pts',(-54.3599412304437,47.7962481007185,
0.));
#151615=CARTESIAN_POINT('Ctrl Pts',(-54.3599412304437,47.7962481007185,
12.));
#151616=CARTESIAN_POINT('Ctrl Pts',(-54.3483869707002,47.7744113281771,
0.));
#151617=CARTESIAN_POINT('Ctrl Pts',(-54.3483869707002,47.7744113281771,
12.));
#151618=CARTESIAN_POINT('Ctrl Pts',(-54.3368308463023,47.7526217596694,
0.));
#151619=CARTESIAN_POINT('Ctrl Pts',(-54.3368308463023,47.7526217596694,
12.));
#151620=CARTESIAN_POINT('Ctrl Pts',(-54.3252729606823,47.7308794669993,
0.));
#151621=CARTESIAN_POINT('Ctrl Pts',(-54.3252729606823,47.7308794669993,
12.));
#151622=CARTESIAN_POINT('Ctrl Pts',(-54.3137134177345,47.7091845221747,
0.));
#151623=CARTESIAN_POINT('Ctrl Pts',(-54.3137134177345,47.7091845221747,
12.));
#151624=CARTESIAN_POINT('Ctrl Pts',(-54.302152321819,47.6875369974087,0.));
#151625=CARTESIAN_POINT('Ctrl Pts',(-54.302152321819,47.6875369974087,12.));
#151626=CARTESIAN_POINT('Ctrl Pts',(-54.290589777765,47.6659369651301,0.));
#151627=CARTESIAN_POINT('Ctrl Pts',(-54.290589777765,47.6659369651301,12.));
#151628=CARTESIAN_POINT('Ctrl Pts',(-54.2790258908738,47.6443844979847,
0.));
#151629=CARTESIAN_POINT('Ctrl Pts',(-54.2790258908738,47.6443844979847,
12.));
#151630=CARTESIAN_POINT('Ctrl Pts',(-54.2674607669226,47.6228796688375,
0.));
#151631=CARTESIAN_POINT('Ctrl Pts',(-54.2674607669226,47.6228796688375,
12.));
#151632=CARTESIAN_POINT('Ctrl Pts',(-54.2558945121678,47.6014225507659,
0.));
#151633=CARTESIAN_POINT('Ctrl Pts',(-54.2558945121678,47.6014225507659,
12.));
#151634=CARTESIAN_POINT('Ctrl Pts',(-54.244327233349,47.5800132170608,0.));
#151635=CARTESIAN_POINT('Ctrl Pts',(-54.244327233349,47.5800132170608,12.));
#151636=CARTESIAN_POINT('Ctrl Pts',(-54.2327590376924,47.5586517412363,
0.));
#151637=CARTESIAN_POINT('Ctrl Pts',(-54.2327590376924,47.5586517412363,
12.));
#151638=CARTESIAN_POINT('Ctrl Pts',(-54.2211900329138,47.5373381970326,
0.));
#151639=CARTESIAN_POINT('Ctrl Pts',(-54.2211900329138,47.5373381970326,
12.));
#151640=CARTESIAN_POINT('Ctrl Pts',(-54.209620327223,47.5160726584174,0.));
#151641=CARTESIAN_POINT('Ctrl Pts',(-54.209620327223,47.5160726584174,12.));
#151642=CARTESIAN_POINT('Ctrl Pts',(-54.198050029327,47.4948551995801,0.));
#151643=CARTESIAN_POINT('Ctrl Pts',(-54.198050029327,47.4948551995801,12.));
#151644=CARTESIAN_POINT('Ctrl Pts',(-54.1864792484345,47.4736858949322,
0.));
#151645=CARTESIAN_POINT('Ctrl Pts',(-54.1864792484345,47.4736858949322,
12.));
#151646=CARTESIAN_POINT('Ctrl Pts',(-54.1749080942593,47.4525648191173,
0.));
#151647=CARTESIAN_POINT('Ctrl Pts',(-54.1749080942593,47.4525648191173,
12.));
#151648=CARTESIAN_POINT('Ctrl Pts',(-54.1633366770239,47.4314920470141,
0.));
#151649=CARTESIAN_POINT('Ctrl Pts',(-54.1633366770239,47.4314920470141,
12.));
#151650=CARTESIAN_POINT('Ctrl Pts',(-54.1517651074637,47.4104676537381,
0.));
#151651=CARTESIAN_POINT('Ctrl Pts',(-54.1517651074637,47.4104676537381,
12.));
#151652=CARTESIAN_POINT('Ctrl Pts',(-54.1401934968311,47.3894917146365,
0.));
#151653=CARTESIAN_POINT('Ctrl Pts',(-54.1401934968311,47.3894917146365,
12.));
#151654=CARTESIAN_POINT('Ctrl Pts',(-54.1286219568989,47.3685643052874,
0.));
#151655=CARTESIAN_POINT('Ctrl Pts',(-54.1286219568989,47.3685643052874,
12.));
#151656=CARTESIAN_POINT('Ctrl Pts',(-54.1170505999645,47.3476855015102,
0.));
#151657=CARTESIAN_POINT('Ctrl Pts',(-54.1170505999645,47.3476855015102,
12.));
#151658=CARTESIAN_POINT('Ctrl Pts',(-54.1054795388543,47.3268553793694,
0.));
#151659=CARTESIAN_POINT('Ctrl Pts',(-54.1054795388543,47.3268553793694,
12.));
#151660=CARTESIAN_POINT('Ctrl Pts',(-54.0939088869269,47.3060740151752,
0.));
#151661=CARTESIAN_POINT('Ctrl Pts',(-54.0939088869269,47.3060740151752,
12.));
#151662=CARTESIAN_POINT('Ctrl Pts',(-54.0823387580776,47.2853414854793,
0.));
#151663=CARTESIAN_POINT('Ctrl Pts',(-54.0823387580776,47.2853414854793,
12.));
#151664=CARTESIAN_POINT('Ctrl Pts',(-54.0707692667438,47.2646578670746,
0.));
#151665=CARTESIAN_POINT('Ctrl Pts',(-54.0707692667438,47.2646578670746,
12.));
#151666=CARTESIAN_POINT('Ctrl Pts',(-54.0592005279086,47.2440232370065,
0.));
#151667=CARTESIAN_POINT('Ctrl Pts',(-54.0592005279086,47.2440232370065,
12.));
#151668=CARTESIAN_POINT('Ctrl Pts',(-54.047632657104,47.2234376725743,0.));
#151669=CARTESIAN_POINT('Ctrl Pts',(-54.047632657104,47.2234376725743,12.));
#151670=CARTESIAN_POINT('Ctrl Pts',(-54.0360657704163,47.202901251334,0.));
#151671=CARTESIAN_POINT('Ctrl Pts',(-54.0360657704163,47.202901251334,12.));
#151672=CARTESIAN_POINT('Ctrl Pts',(-54.0244999844893,47.1824140510926,
0.));
#151673=CARTESIAN_POINT('Ctrl Pts',(-54.0244999844893,47.1824140510926,
12.));
#151674=CARTESIAN_POINT('Ctrl Pts',(-54.0129354165297,47.1619761499087,
0.));
#151675=CARTESIAN_POINT('Ctrl Pts',(-54.0129354165297,47.1619761499087,
12.));
#151676=CARTESIAN_POINT('Ctrl Pts',(-54.0013721843118,47.1415876261035,
0.));
#151677=CARTESIAN_POINT('Ctrl Pts',(-54.0013721843118,47.1415876261035,
12.));
#151678=CARTESIAN_POINT('Ctrl Pts',(-53.989810406182,47.1212485582643,0.));
#151679=CARTESIAN_POINT('Ctrl Pts',(-53.989810406182,47.1212485582643,12.));
#151680=CARTESIAN_POINT('Ctrl Pts',(-53.9782502010634,47.1009590252458,
0.));
#151681=CARTESIAN_POINT('Ctrl Pts',(-53.9782502010634,47.1009590252458,
12.));
#151682=CARTESIAN_POINT('Ctrl Pts',(-53.9666916884596,47.0807191061648,
0.));
#151683=CARTESIAN_POINT('Ctrl Pts',(-53.9666916884596,47.0807191061648,
12.));
#151684=CARTESIAN_POINT('Ctrl Pts',(-53.95513498846,47.0605288804008,0.));
#151685=CARTESIAN_POINT('Ctrl Pts',(-53.95513498846,47.0605288804008,12.));
#151686=CARTESIAN_POINT('Ctrl Pts',(-53.9435802217436,47.0403884276071,
0.));
#151687=CARTESIAN_POINT('Ctrl Pts',(-53.9435802217436,47.0403884276071,
12.));
#151688=CARTESIAN_POINT('Ctrl Pts',(-53.9320275095853,47.0202978277138,
0.));
#151689=CARTESIAN_POINT('Ctrl Pts',(-53.9320275095853,47.0202978277138,
12.));
#151690=CARTESIAN_POINT('Ctrl Pts',(-53.9204769738596,47.0002571609297,
0.));
#151691=CARTESIAN_POINT('Ctrl Pts',(-53.9204769738596,47.0002571609297,
12.));
#151692=CARTESIAN_POINT('Ctrl Pts',(-53.9089287370463,46.9802665077366,
0.));
#151693=CARTESIAN_POINT('Ctrl Pts',(-53.9089287370463,46.9802665077366,
12.));
#151694=CARTESIAN_POINT('Ctrl Pts',(-53.8973829222348,46.960325948892,0.));
#151695=CARTESIAN_POINT('Ctrl Pts',(-53.8973829222348,46.960325948892,12.));
#151696=CARTESIAN_POINT('Ctrl Pts',(-53.8858396531298,46.94043556544,0.));
#151697=CARTESIAN_POINT('Ctrl Pts',(-53.8858396531298,46.94043556544,12.));
#151698=CARTESIAN_POINT('Ctrl Pts',(-53.8742990540563,46.9205954387133,
0.));
#151699=CARTESIAN_POINT('Ctrl Pts',(-53.8742990540563,46.9205954387133,
12.));
#151700=CARTESIAN_POINT('Ctrl Pts',(-53.8627612499638,46.9008056503351,
0.));
#151701=CARTESIAN_POINT('Ctrl Pts',(-53.8627612499638,46.9008056503351,
12.));
#151702=CARTESIAN_POINT('Ctrl Pts',(-53.8512263664321,46.881066282213,0.));
#151703=CARTESIAN_POINT('Ctrl Pts',(-53.8512263664321,46.881066282213,12.));
#151704=CARTESIAN_POINT('Ctrl Pts',(-53.8396945296757,46.8613774165435,
0.));
#151705=CARTESIAN_POINT('Ctrl Pts',(-53.8396945296757,46.8613774165435,
12.));
#151706=CARTESIAN_POINT('Ctrl Pts',(-53.8281658665503,46.841739135822,0.));
#151707=CARTESIAN_POINT('Ctrl Pts',(-53.8281658665503,46.841739135822,12.));
#151708=CARTESIAN_POINT('Ctrl Pts',(-53.816640504558,46.8221515228457,0.));
#151709=CARTESIAN_POINT('Ctrl Pts',(-53.816640504558,46.8221515228457,12.));
#151710=CARTESIAN_POINT('Ctrl Pts',(-53.8051185718532,46.802614660715,0.));
#151711=CARTESIAN_POINT('Ctrl Pts',(-53.8051185718532,46.802614660715,12.));
#151712=CARTESIAN_POINT('Ctrl Pts',(-53.793600197248,46.7831286328278,0.));
#151713=CARTESIAN_POINT('Ctrl Pts',(-53.793600197248,46.7831286328278,12.));
#151714=CARTESIAN_POINT('Ctrl Pts',(-53.7820855102182,46.763693522886,0.));
#151715=CARTESIAN_POINT('Ctrl Pts',(-53.7820855102182,46.763693522886,12.));
#151716=CARTESIAN_POINT('Ctrl Pts',(-53.7705746409076,46.7443094149045,
0.));
#151717=CARTESIAN_POINT('Ctrl Pts',(-53.7705746409076,46.7443094149045,
12.));
#151718=CARTESIAN_POINT('Ctrl Pts',(-53.7590677201342,46.7249763932129,
0.));
#151719=CARTESIAN_POINT('Ctrl Pts',(-53.7590677201342,46.7249763932129,
12.));
#151720=CARTESIAN_POINT('Ctrl Pts',(-53.7475648793946,46.7056945424559,
0.));
#151721=CARTESIAN_POINT('Ctrl Pts',(-53.7475648793946,46.7056945424559,
12.));
#151722=CARTESIAN_POINT('Ctrl Pts',(-53.7360662508675,46.6864639475862,
0.));
#151723=CARTESIAN_POINT('Ctrl Pts',(-53.7360662508675,46.6864639475862,
12.));
#151724=CARTESIAN_POINT('Ctrl Pts',(-53.7245719674221,46.6672846938752,
0.));
#151725=CARTESIAN_POINT('Ctrl Pts',(-53.7245719674221,46.6672846938752,
12.));
#151726=CARTESIAN_POINT('Ctrl Pts',(-53.7130821626262,46.6481568669217,
0.));
#151727=CARTESIAN_POINT('Ctrl Pts',(-53.7130821626262,46.6481568669217,
12.));
#151728=CARTESIAN_POINT('Ctrl Pts',(-53.7015969707541,46.6290805526559,
0.));
#151729=CARTESIAN_POINT('Ctrl Pts',(-53.7015969707541,46.6290805526559,
12.));
#151730=CARTESIAN_POINT('Ctrl Pts',(-53.690116526794,46.6100558373401,0.));
#151731=CARTESIAN_POINT('Ctrl Pts',(-53.690116526794,46.6100558373401,12.));
#151732=CARTESIAN_POINT('Ctrl Pts',(-53.678640966456,46.5910828075652,0.));
#151733=CARTESIAN_POINT('Ctrl Pts',(-53.678640966456,46.5910828075652,12.));
#151734=CARTESIAN_POINT('Ctrl Pts',(-53.6671704261735,46.5721615502589,
0.));
#151735=CARTESIAN_POINT('Ctrl Pts',(-53.6671704261735,46.5721615502589,
12.));
#151736=CARTESIAN_POINT('Ctrl Pts',(-53.6557050431069,46.5532921526899,
0.));
#151737=CARTESIAN_POINT('Ctrl Pts',(-53.6557050431069,46.5532921526899,
12.));
#151738=CARTESIAN_POINT('Ctrl Pts',(-53.6442449551455,46.5344747024677,
0.));
#151739=CARTESIAN_POINT('Ctrl Pts',(-53.6442449551455,46.5344747024677,
12.));
#151740=CARTESIAN_POINT('Ctrl Pts',(-53.6327903009098,46.5157092875377,
0.));
#151741=CARTESIAN_POINT('Ctrl Pts',(-53.6327903009098,46.5157092875377,
12.));
#151742=CARTESIAN_POINT('Ctrl Pts',(-53.6213412197542,46.4969959961779,
0.));
#151743=CARTESIAN_POINT('Ctrl Pts',(-53.6213412197542,46.4969959961779,
12.));
#151744=CARTESIAN_POINT('Ctrl Pts',(-53.6098978517869,46.4783349170182,
0.));
#151745=CARTESIAN_POINT('Ctrl Pts',(-53.6098978517869,46.4783349170182,
12.));
#151746=CARTESIAN_POINT('Ctrl Pts',(-53.5984603378862,46.4597261390526,
0.));
#151747=CARTESIAN_POINT('Ctrl Pts',(-53.5984603378862,46.4597261390526,
12.));
#151748=CARTESIAN_POINT('Ctrl Pts',(-53.5870288197161,46.4411697516474,
0.));
#151749=CARTESIAN_POINT('Ctrl Pts',(-53.5870288197161,46.4411697516474,
12.));
#151750=CARTESIAN_POINT('Ctrl Pts',(-53.5756034397464,46.422665844546,0.));
#151751=CARTESIAN_POINT('Ctrl Pts',(-53.5756034397464,46.422665844546,12.));
#151752=CARTESIAN_POINT('Ctrl Pts',(-53.5641843412537,46.4042145078682,
0.));
#151753=CARTESIAN_POINT('Ctrl Pts',(-53.5641843412537,46.4042145078682,
12.));
#151754=CARTESIAN_POINT('Ctrl Pts',(-53.552771668303,46.3858158321044,0.));
#151755=CARTESIAN_POINT('Ctrl Pts',(-53.552771668303,46.3858158321044,12.));
#151756=CARTESIAN_POINT('Ctrl Pts',(-53.5413655657323,46.3674699081043,
0.));
#151757=CARTESIAN_POINT('Ctrl Pts',(-53.5413655657323,46.3674699081043,
12.));
#151758=CARTESIAN_POINT('Ctrl Pts',(-53.5299661791396,46.3491768270664,
0.));
#151759=CARTESIAN_POINT('Ctrl Pts',(-53.5299661791396,46.3491768270664,
12.));
#151760=CARTESIAN_POINT('Ctrl Pts',(-53.518573654857,46.3309366805112,0.));
#151761=CARTESIAN_POINT('Ctrl Pts',(-53.518573654857,46.3309366805112,12.));
#151762=CARTESIAN_POINT('Ctrl Pts',(-53.5071881399932,46.3127495603117,
0.));
#151763=CARTESIAN_POINT('Ctrl Pts',(-53.5071881399932,46.3127495603117,
12.));
#151764=CARTESIAN_POINT('Ctrl Pts',(-53.4958097825019,46.2946155587428,
0.));
#151765=CARTESIAN_POINT('Ctrl Pts',(-53.4958097825019,46.2946155587428,
12.));
#151766=CARTESIAN_POINT('Ctrl Pts',(-53.4844387312414,46.2765347685198,
0.));
#151767=CARTESIAN_POINT('Ctrl Pts',(-53.4844387312414,46.2765347685198,
12.));
#151768=CARTESIAN_POINT('Ctrl Pts',(-53.4730751360359,46.2585072828343,
0.));
#151769=CARTESIAN_POINT('Ctrl Pts',(-53.4730751360359,46.2585072828343,
12.));
#151770=CARTESIAN_POINT('Ctrl Pts',(-53.4617191477382,46.2405331953872,
0.));
#151771=CARTESIAN_POINT('Ctrl Pts',(-53.4617191477382,46.2405331953872,
12.));
#151772=CARTESIAN_POINT('Ctrl Pts',(-53.4503709181158,46.2226126003185,
0.));
#151773=CARTESIAN_POINT('Ctrl Pts',(-53.4503709181158,46.2226126003185,
12.));
#151774=CARTESIAN_POINT('Ctrl Pts',(-53.4390305997263,46.2047455921276,
0.));
#151775=CARTESIAN_POINT('Ctrl Pts',(-53.4390305997263,46.2047455921276,
12.));
#151776=CARTESIAN_POINT('Ctrl Pts',(-53.4276983458129,46.1869322656027,
0.));
#151777=CARTESIAN_POINT('Ctrl Pts',(-53.4276983458129,46.1869322656027,
12.));
#151778=CARTESIAN_POINT('Ctrl Pts',(-53.4163743101535,46.1691727157149,
0.));
#151779=CARTESIAN_POINT('Ctrl Pts',(-53.4163743101535,46.1691727157149,
12.));
#151780=CARTESIAN_POINT('Ctrl Pts',(-53.4050586470463,46.1514670376035,
0.));
#151781=CARTESIAN_POINT('Ctrl Pts',(-53.4050586470463,46.1514670376035,
12.));
#151782=CARTESIAN_POINT('Ctrl Pts',(-53.3937515116572,46.1338153268116,
0.));
#151783=CARTESIAN_POINT('Ctrl Pts',(-53.3937515116572,46.1338153268116,
12.));
#151784=CARTESIAN_POINT('Ctrl Pts',(-53.3824530603284,46.1162176794891,
0.));
#151785=CARTESIAN_POINT('Ctrl Pts',(-53.3824530603284,46.1162176794891,
12.));
#151786=CARTESIAN_POINT('Ctrl Pts',(-53.3711634508426,46.0986741925646,
0.));
#151787=CARTESIAN_POINT('Ctrl Pts',(-53.3711634508426,46.0986741925646,
12.));
#151788=CARTESIAN_POINT('Ctrl Pts',(-53.3598828428519,46.0811849640195,
0.));
#151789=CARTESIAN_POINT('Ctrl Pts',(-53.3598828428519,46.0811849640195,
12.));
#151790=CARTESIAN_POINT('Ctrl Pts',(-53.3486113975868,46.0637500926954,
0.));
#151791=CARTESIAN_POINT('Ctrl Pts',(-53.3486113975868,46.0637500926954,
12.));
#151792=CARTESIAN_POINT('Ctrl Pts',(-53.3373492770647,46.046369677778,0.));
#151793=CARTESIAN_POINT('Ctrl Pts',(-53.3373492770647,46.046369677778,12.));
#151794=CARTESIAN_POINT('Ctrl Pts',(-53.3260966434277,46.0290438183598,
0.));
#151795=CARTESIAN_POINT('Ctrl Pts',(-53.3260966434277,46.0290438183598,
12.));
#151796=CARTESIAN_POINT('Ctrl Pts',(-53.3148536582658,46.0117726129893,
0.));
#151797=CARTESIAN_POINT('Ctrl Pts',(-53.3148536582658,46.0117726129893,
12.));
#151798=CARTESIAN_POINT('Ctrl Pts',(-53.3036204818367,45.9945561591486,
0.));
#151799=CARTESIAN_POINT('Ctrl Pts',(-53.3036204818367,45.9945561591486,
12.));
#151800=CARTESIAN_POINT('Ctrl Pts',(-53.2923972745585,45.9773945542415,
0.));
#151801=CARTESIAN_POINT('Ctrl Pts',(-53.2923972745585,45.9773945542415,
12.));
#151802=CARTESIAN_POINT('Ctrl Pts',(-53.2811841987945,45.9602878967714,
0.));
#151803=CARTESIAN_POINT('Ctrl Pts',(-53.2811841987945,45.9602878967714,
12.));
#151804=CARTESIAN_POINT('Ctrl Pts',(-53.2699814203097,45.9432362873001,
0.));
#151805=CARTESIAN_POINT('Ctrl Pts',(-53.2699814203097,45.9432362873001,
12.));
#151806=CARTESIAN_POINT('Ctrl Pts',(-53.2587891103835,45.9262398298323,
0.));
#151807=CARTESIAN_POINT('Ctrl Pts',(-53.2587891103835,45.9262398298323,
12.));
#151808=CARTESIAN_POINT('Ctrl Pts',(-53.2476074459977,45.9092986319343,
0.));
#151809=CARTESIAN_POINT('Ctrl Pts',(-53.2476074459977,45.9092986319343,
12.));
#151810=CARTESIAN_POINT('Ctrl Pts',(-53.2364366054276,45.8924128018354,
0.));
#151811=CARTESIAN_POINT('Ctrl Pts',(-53.2364366054276,45.8924128018354,
12.));
#151812=CARTESIAN_POINT('Ctrl Pts',(-53.2252767643652,45.8755824458715,
0.));
#151813=CARTESIAN_POINT('Ctrl Pts',(-53.2252767643652,45.8755824458715,
12.));
#151814=CARTESIAN_POINT('Ctrl Pts',(-53.2141280925458,45.8588076662598,
0.));
#151815=CARTESIAN_POINT('Ctrl Pts',(-53.2141280925458,45.8588076662598,
12.));
#151816=CARTESIAN_POINT('Ctrl Pts',(-53.2029907483602,45.8420885575386,
0.));
#151817=CARTESIAN_POINT('Ctrl Pts',(-53.2029907483602,45.8420885575386,
12.));
#151818=CARTESIAN_POINT('Ctrl Pts',(-53.1918648840598,45.8254252100003,
0.));
#151819=CARTESIAN_POINT('Ctrl Pts',(-53.1918648840598,45.8254252100003,
12.));
#151820=CARTESIAN_POINT('Ctrl Pts',(-53.1807506560977,45.8088177165124,
0.));
#151821=CARTESIAN_POINT('Ctrl Pts',(-53.1807506560977,45.8088177165124,
12.));
#151822=CARTESIAN_POINT('Ctrl Pts',(-53.1696482334487,45.7922661780005,
0.));
#151823=CARTESIAN_POINT('Ctrl Pts',(-53.1696482334487,45.7922661780005,
12.));
#151824=CARTESIAN_POINT('Ctrl Pts',(-53.158557807638,45.7757707100568,0.));
#151825=CARTESIAN_POINT('Ctrl Pts',(-53.158557807638,45.7757707100568,12.));
#151826=CARTESIAN_POINT('Ctrl Pts',(-53.147479599594,45.7593314474412,0.));
#151827=CARTESIAN_POINT('Ctrl Pts',(-53.147479599594,45.7593314474412,12.));
#151828=CARTESIAN_POINT('Ctrl Pts',(-53.136413838457,45.7429485300727,0.));
#151829=CARTESIAN_POINT('Ctrl Pts',(-53.136413838457,45.7429485300727,12.));
#151830=CARTESIAN_POINT('Ctrl Pts',(-53.1253607414806,45.7266220896951,
0.));
#151831=CARTESIAN_POINT('Ctrl Pts',(-53.1253607414806,45.7266220896951,
12.));
#151832=CARTESIAN_POINT('Ctrl Pts',(-53.1143204954981,45.7103522376744,
0.));
#151833=CARTESIAN_POINT('Ctrl Pts',(-53.1143204954981,45.7103522376744,
12.));
#151834=CARTESIAN_POINT('Ctrl Pts',(-53.1032932329074,45.6941390489239,
0.));
#151835=CARTESIAN_POINT('Ctrl Pts',(-53.1032932329074,45.6941390489239,
12.));
#151836=CARTESIAN_POINT('Ctrl Pts',(-53.0922790298736,45.6779825614486,
0.));
#151837=CARTESIAN_POINT('Ctrl Pts',(-53.0922790298736,45.6779825614486,
12.));
#151838=CARTESIAN_POINT('Ctrl Pts',(-53.083478145185,45.6651027439479,0.));
#151839=CARTESIAN_POINT('Ctrl Pts',(-53.083478145185,45.6651027439479,12.));
#151840=CARTESIAN_POINT('Ctrl Pts',(-53.0768833804386,45.6554684028296,
0.));
#151841=CARTESIAN_POINT('Ctrl Pts',(-53.0768833804386,45.6554684028296,
12.));
#151842=CARTESIAN_POINT('Ctrl Pts',(-53.0724894921921,45.6490568514146,
0.));
#151843=CARTESIAN_POINT('Ctrl Pts',(-53.0724894921921,45.6490568514146,
12.));
#151844=CARTESIAN_POINT('Ctrl Pts',(-53.0702932034641,45.6458539113724,
0.));
#151845=CARTESIAN_POINT('Ctrl Pts',(-53.0702932034641,45.6458539113724,
12.));
#151846=CARTESIAN_POINT('',(-53.0702932034641,45.6458539113724,12.));
#151847=CARTESIAN_POINT('Ctrl Pts',(-53.0702932034641,45.6458539113724,
12.));
#151848=CARTESIAN_POINT('Ctrl Pts',(-53.0724894921921,45.6490568514146,
12.));
#151849=CARTESIAN_POINT('Ctrl Pts',(-53.0768833804386,45.6554684028296,
12.));
#151850=CARTESIAN_POINT('Ctrl Pts',(-53.083478145185,45.6651027439479,12.));
#151851=CARTESIAN_POINT('Ctrl Pts',(-53.0922790298736,45.6779825614486,
12.));
#151852=CARTESIAN_POINT('Ctrl Pts',(-53.1032932329074,45.6941390489239,
12.));
#151853=CARTESIAN_POINT('Ctrl Pts',(-53.1143204954981,45.7103522376744,
12.));
#151854=CARTESIAN_POINT('Ctrl Pts',(-53.1253607414806,45.7266220896951,
12.));
#151855=CARTESIAN_POINT('Ctrl Pts',(-53.136413838457,45.7429485300727,12.));
#151856=CARTESIAN_POINT('Ctrl Pts',(-53.147479599594,45.7593314474412,12.));
#151857=CARTESIAN_POINT('Ctrl Pts',(-53.158557807638,45.7757707100568,12.));
#151858=CARTESIAN_POINT('Ctrl Pts',(-53.1696482334487,45.7922661780005,
12.));
#151859=CARTESIAN_POINT('Ctrl Pts',(-53.1807506560977,45.8088177165124,
12.));
#151860=CARTESIAN_POINT('Ctrl Pts',(-53.1918648840598,45.8254252100003,
12.));
#151861=CARTESIAN_POINT('Ctrl Pts',(-53.2029907483602,45.8420885575386,
12.));
#151862=CARTESIAN_POINT('Ctrl Pts',(-53.2141280925458,45.8588076662598,
12.));
#151863=CARTESIAN_POINT('Ctrl Pts',(-53.2252767643652,45.8755824458715,
12.));
#151864=CARTESIAN_POINT('Ctrl Pts',(-53.2364366054276,45.8924128018354,
12.));
#151865=CARTESIAN_POINT('Ctrl Pts',(-53.2476074459977,45.9092986319343,
12.));
#151866=CARTESIAN_POINT('Ctrl Pts',(-53.2587891103835,45.9262398298323,
12.));
#151867=CARTESIAN_POINT('Ctrl Pts',(-53.2699814203097,45.9432362873001,
12.));
#151868=CARTESIAN_POINT('Ctrl Pts',(-53.2811841987945,45.9602878967714,
12.));
#151869=CARTESIAN_POINT('Ctrl Pts',(-53.2923972745585,45.9773945542415,
12.));
#151870=CARTESIAN_POINT('Ctrl Pts',(-53.3036204818367,45.9945561591486,
12.));
#151871=CARTESIAN_POINT('Ctrl Pts',(-53.3148536582658,46.0117726129893,
12.));
#151872=CARTESIAN_POINT('Ctrl Pts',(-53.3260966434277,46.0290438183598,
12.));
#151873=CARTESIAN_POINT('Ctrl Pts',(-53.3373492770647,46.046369677778,12.));
#151874=CARTESIAN_POINT('Ctrl Pts',(-53.3486113975868,46.0637500926954,
12.));
#151875=CARTESIAN_POINT('Ctrl Pts',(-53.3598828428519,46.0811849640195,
12.));
#151876=CARTESIAN_POINT('Ctrl Pts',(-53.3711634508426,46.0986741925646,
12.));
#151877=CARTESIAN_POINT('Ctrl Pts',(-53.3824530603284,46.1162176794891,
12.));
#151878=CARTESIAN_POINT('Ctrl Pts',(-53.3937515116572,46.1338153268116,
12.));
#151879=CARTESIAN_POINT('Ctrl Pts',(-53.4050586470463,46.1514670376035,
12.));
#151880=CARTESIAN_POINT('Ctrl Pts',(-53.4163743101535,46.1691727157149,
12.));
#151881=CARTESIAN_POINT('Ctrl Pts',(-53.4276983458129,46.1869322656027,
12.));
#151882=CARTESIAN_POINT('Ctrl Pts',(-53.4390305997263,46.2047455921276,
12.));
#151883=CARTESIAN_POINT('Ctrl Pts',(-53.4503709181158,46.2226126003185,
12.));
#151884=CARTESIAN_POINT('Ctrl Pts',(-53.4617191477382,46.2405331953872,
12.));
#151885=CARTESIAN_POINT('Ctrl Pts',(-53.4730751360359,46.2585072828343,
12.));
#151886=CARTESIAN_POINT('Ctrl Pts',(-53.4844387312414,46.2765347685198,
12.));
#151887=CARTESIAN_POINT('Ctrl Pts',(-53.4958097825019,46.2946155587428,
12.));
#151888=CARTESIAN_POINT('Ctrl Pts',(-53.5071881399932,46.3127495603117,
12.));
#151889=CARTESIAN_POINT('Ctrl Pts',(-53.518573654857,46.3309366805112,12.));
#151890=CARTESIAN_POINT('Ctrl Pts',(-53.5299661791396,46.3491768270664,
12.));
#151891=CARTESIAN_POINT('Ctrl Pts',(-53.5413655657323,46.3674699081043,
12.));
#151892=CARTESIAN_POINT('Ctrl Pts',(-53.552771668303,46.3858158321044,12.));
#151893=CARTESIAN_POINT('Ctrl Pts',(-53.5641843412537,46.4042145078682,
12.));
#151894=CARTESIAN_POINT('Ctrl Pts',(-53.5756034397464,46.422665844546,12.));
#151895=CARTESIAN_POINT('Ctrl Pts',(-53.5870288197161,46.4411697516474,
12.));
#151896=CARTESIAN_POINT('Ctrl Pts',(-53.5984603378862,46.4597261390526,
12.));
#151897=CARTESIAN_POINT('Ctrl Pts',(-53.6098978517869,46.4783349170182,
12.));
#151898=CARTESIAN_POINT('Ctrl Pts',(-53.6213412197542,46.4969959961779,
12.));
#151899=CARTESIAN_POINT('Ctrl Pts',(-53.6327903009098,46.5157092875377,
12.));
#151900=CARTESIAN_POINT('Ctrl Pts',(-53.6442449551455,46.5344747024677,
12.));
#151901=CARTESIAN_POINT('Ctrl Pts',(-53.6557050431069,46.5532921526899,
12.));
#151902=CARTESIAN_POINT('Ctrl Pts',(-53.6671704261735,46.5721615502589,
12.));
#151903=CARTESIAN_POINT('Ctrl Pts',(-53.678640966456,46.5910828075652,12.));
#151904=CARTESIAN_POINT('Ctrl Pts',(-53.690116526794,46.6100558373401,12.));
#151905=CARTESIAN_POINT('Ctrl Pts',(-53.7015969707541,46.6290805526559,
12.));
#151906=CARTESIAN_POINT('Ctrl Pts',(-53.7130821626262,46.6481568669217,
12.));
#151907=CARTESIAN_POINT('Ctrl Pts',(-53.7245719674221,46.6672846938752,
12.));
#151908=CARTESIAN_POINT('Ctrl Pts',(-53.7360662508675,46.6864639475862,
12.));
#151909=CARTESIAN_POINT('Ctrl Pts',(-53.7475648793946,46.7056945424559,
12.));
#151910=CARTESIAN_POINT('Ctrl Pts',(-53.7590677201342,46.7249763932129,
12.));
#151911=CARTESIAN_POINT('Ctrl Pts',(-53.7705746409076,46.7443094149045,
12.));
#151912=CARTESIAN_POINT('Ctrl Pts',(-53.7820855102182,46.763693522886,12.));
#151913=CARTESIAN_POINT('Ctrl Pts',(-53.793600197248,46.7831286328278,12.));
#151914=CARTESIAN_POINT('Ctrl Pts',(-53.8051185718532,46.802614660715,12.));
#151915=CARTESIAN_POINT('Ctrl Pts',(-53.816640504558,46.8221515228457,12.));
#151916=CARTESIAN_POINT('Ctrl Pts',(-53.8281658665503,46.841739135822,12.));
#151917=CARTESIAN_POINT('Ctrl Pts',(-53.8396945296757,46.8613774165435,
12.));
#151918=CARTESIAN_POINT('Ctrl Pts',(-53.8512263664321,46.881066282213,12.));
#151919=CARTESIAN_POINT('Ctrl Pts',(-53.8627612499638,46.9008056503351,
12.));
#151920=CARTESIAN_POINT('Ctrl Pts',(-53.8742990540563,46.9205954387133,
12.));
#151921=CARTESIAN_POINT('Ctrl Pts',(-53.8858396531298,46.94043556544,12.));
#151922=CARTESIAN_POINT('Ctrl Pts',(-53.8973829222348,46.960325948892,12.));
#151923=CARTESIAN_POINT('Ctrl Pts',(-53.9089287370463,46.9802665077366,
12.));
#151924=CARTESIAN_POINT('Ctrl Pts',(-53.9204769738596,47.0002571609297,
12.));
#151925=CARTESIAN_POINT('Ctrl Pts',(-53.9320275095853,47.0202978277138,
12.));
#151926=CARTESIAN_POINT('Ctrl Pts',(-53.9435802217436,47.0403884276071,
12.));
#151927=CARTESIAN_POINT('Ctrl Pts',(-53.95513498846,47.0605288804008,12.));
#151928=CARTESIAN_POINT('Ctrl Pts',(-53.9666916884596,47.0807191061648,
12.));
#151929=CARTESIAN_POINT('Ctrl Pts',(-53.9782502010634,47.1009590252458,
12.));
#151930=CARTESIAN_POINT('Ctrl Pts',(-53.989810406182,47.1212485582643,12.));
#151931=CARTESIAN_POINT('Ctrl Pts',(-54.0013721843118,47.1415876261035,
12.));
#151932=CARTESIAN_POINT('Ctrl Pts',(-54.0129354165297,47.1619761499087,
12.));
#151933=CARTESIAN_POINT('Ctrl Pts',(-54.0244999844893,47.1824140510926,
12.));
#151934=CARTESIAN_POINT('Ctrl Pts',(-54.0360657704163,47.202901251334,12.));
#151935=CARTESIAN_POINT('Ctrl Pts',(-54.047632657104,47.2234376725743,12.));
#151936=CARTESIAN_POINT('Ctrl Pts',(-54.0592005279086,47.2440232370065,
12.));
#151937=CARTESIAN_POINT('Ctrl Pts',(-54.0707692667438,47.2646578670746,
12.));
#151938=CARTESIAN_POINT('Ctrl Pts',(-54.0823387580776,47.2853414854793,
12.));
#151939=CARTESIAN_POINT('Ctrl Pts',(-54.0939088869269,47.3060740151752,
12.));
#151940=CARTESIAN_POINT('Ctrl Pts',(-54.1054795388543,47.3268553793694,
12.));
#151941=CARTESIAN_POINT('Ctrl Pts',(-54.1170505999645,47.3476855015102,
12.));
#151942=CARTESIAN_POINT('Ctrl Pts',(-54.1286219568989,47.3685643052874,
12.));
#151943=CARTESIAN_POINT('Ctrl Pts',(-54.1401934968311,47.3894917146365,
12.));
#151944=CARTESIAN_POINT('Ctrl Pts',(-54.1517651074637,47.4104676537381,
12.));
#151945=CARTESIAN_POINT('Ctrl Pts',(-54.1633366770239,47.4314920470141,
12.));
#151946=CARTESIAN_POINT('Ctrl Pts',(-54.1749080942593,47.4525648191173,
12.));
#151947=CARTESIAN_POINT('Ctrl Pts',(-54.1864792484345,47.4736858949322,
12.));
#151948=CARTESIAN_POINT('Ctrl Pts',(-54.198050029327,47.4948551995801,12.));
#151949=CARTESIAN_POINT('Ctrl Pts',(-54.209620327223,47.5160726584174,12.));
#151950=CARTESIAN_POINT('Ctrl Pts',(-54.2211900329138,47.5373381970326,
12.));
#151951=CARTESIAN_POINT('Ctrl Pts',(-54.2327590376924,47.5586517412363,
12.));
#151952=CARTESIAN_POINT('Ctrl Pts',(-54.244327233349,47.5800132170608,12.));
#151953=CARTESIAN_POINT('Ctrl Pts',(-54.2558945121678,47.6014225507659,
12.));
#151954=CARTESIAN_POINT('Ctrl Pts',(-54.2674607669226,47.6228796688375,
12.));
#151955=CARTESIAN_POINT('Ctrl Pts',(-54.2790258908738,47.6443844979847,
12.));
#151956=CARTESIAN_POINT('Ctrl Pts',(-54.290589777765,47.6659369651301,12.));
#151957=CARTESIAN_POINT('Ctrl Pts',(-54.302152321819,47.6875369974087,12.));
#151958=CARTESIAN_POINT('Ctrl Pts',(-54.3137134177345,47.7091845221747,
12.));
#151959=CARTESIAN_POINT('Ctrl Pts',(-54.3252729606823,47.7308794669993,
12.));
#151960=CARTESIAN_POINT('Ctrl Pts',(-54.3368308463023,47.7526217596694,
12.));
#151961=CARTESIAN_POINT('Ctrl Pts',(-54.3483869707002,47.7744113281771,
12.));
#151962=CARTESIAN_POINT('Ctrl Pts',(-54.3599412304437,47.7962481007185,
12.));
#151963=CARTESIAN_POINT('Ctrl Pts',(-54.3714935225591,47.8181320056995,
12.));
#151964=CARTESIAN_POINT('Ctrl Pts',(-54.3830437445279,47.8400629717355,
12.));
#151965=CARTESIAN_POINT('Ctrl Pts',(-54.3945917942832,47.8620409276493,
12.));
#151966=CARTESIAN_POINT('Ctrl Pts',(-54.4061375702079,47.8840658024618,
12.));
#151967=CARTESIAN_POINT('Ctrl Pts',(-54.4176809711311,47.9061375253897,
12.));
#151968=CARTESIAN_POINT('Ctrl Pts',(-54.429221896324,47.9282560258516,12.));
#151969=CARTESIAN_POINT('Ctrl Pts',(-54.4407602454967,47.9504212334675,
12.));
#151970=CARTESIAN_POINT('Ctrl Pts',(-54.4522959187955,47.9726330780572,
12.));
#151971=CARTESIAN_POINT('Ctrl Pts',(-54.4638288168003,47.9948914896326,
12.));
#151972=CARTESIAN_POINT('Ctrl Pts',(-54.4753588405215,48.0171963983924,
12.));
#151973=CARTESIAN_POINT('Ctrl Pts',(-54.4868858913971,48.0395477347298,
12.));
#151974=CARTESIAN_POINT('Ctrl Pts',(-54.4984098712886,48.0619454292324,
12.));
#151975=CARTESIAN_POINT('Ctrl Pts',(-54.5099306824786,48.0843894126806,
12.));
#151976=CARTESIAN_POINT('Ctrl Pts',(-54.5214482276678,48.1068796160405,
12.));
#151977=CARTESIAN_POINT('Ctrl Pts',(-54.5329624099721,48.1294159704573,
12.));
#151978=CARTESIAN_POINT('Ctrl Pts',(-54.5444731329201,48.1519984072622,
12.));
#151979=CARTESIAN_POINT('Ctrl Pts',(-54.5559803004492,48.1746268579736,
12.));
#151980=CARTESIAN_POINT('Ctrl Pts',(-54.5674838169041,48.1973012542966,
12.));
#151981=CARTESIAN_POINT('Ctrl Pts',(-54.5789835870342,48.2200215281173,
12.));
#151982=CARTESIAN_POINT('Ctrl Pts',(-54.5904795159926,48.2427876114947,
12.));
#151983=CARTESIAN_POINT('Ctrl Pts',(-54.6019715093309,48.2655994366665,
12.));
#151984=CARTESIAN_POINT('Ctrl Pts',(-54.6134594729959,48.2884569360506,
12.));
#151985=CARTESIAN_POINT('Ctrl Pts',(-54.6249433133261,48.3113600422443,
12.));
#151986=CARTESIAN_POINT('Ctrl Pts',(-54.6364229370494,48.3343086880194,
12.));
#151987=CARTESIAN_POINT('Ctrl Pts',(-54.6478982512794,48.3573028063124,
12.));
#151988=CARTESIAN_POINT('Ctrl Pts',(-54.6593691635145,48.3803423302294,
12.));
#151989=CARTESIAN_POINT('Ctrl Pts',(-54.6708355816358,48.4034271930514,
12.));
#151990=CARTESIAN_POINT('Ctrl Pts',(-54.6822974139064,48.426557328234,12.));
#151991=CARTESIAN_POINT('Ctrl Pts',(-54.6937545689695,48.4497326694052,
12.));
#151992=CARTESIAN_POINT('Ctrl Pts',(-54.7052069558497,48.472953150357,12.));
#151993=CARTESIAN_POINT('Ctrl Pts',(-54.716654483948,48.4962187050457,12.));
#151994=CARTESIAN_POINT('Ctrl Pts',(-54.7280970630351,48.519529267596,12.));
#151995=CARTESIAN_POINT('Ctrl Pts',(-54.7395346032453,48.5428847722977,
12.));
#151996=CARTESIAN_POINT('Ctrl Pts',(-54.7509670150714,48.5662851536026,
12.));
#151997=CARTESIAN_POINT('Ctrl Pts',(-54.7623942093586,48.5897303461125,
12.));
#151998=CARTESIAN_POINT('Ctrl Pts',(-54.7738160973031,48.6132202845783,
12.));
#151999=CARTESIAN_POINT('Ctrl Pts',(-54.7852325904583,48.6367549039112,
12.));
#152000=CARTESIAN_POINT('Ctrl Pts',(-54.796643600739,48.6603341391886,12.));
#152001=CARTESIAN_POINT('Ctrl Pts',(-54.8080490404275,48.6839579256566,
12.));
#152002=CARTESIAN_POINT('Ctrl Pts',(-54.819448822181,48.7076261987292,12.));
#152003=CARTESIAN_POINT('Ctrl Pts',(-54.8308428590344,48.7313388939845,
12.));
#152004=CARTESIAN_POINT('Ctrl Pts',(-54.8422310643763,48.7550959471601,
12.));
#152005=CARTESIAN_POINT('Ctrl Pts',(-54.8536133519292,48.7788972941438,
12.));
#152006=CARTESIAN_POINT('Ctrl Pts',(-54.8649896357285,48.8027428709614,
12.));
#152007=CARTESIAN_POINT('Ctrl Pts',(-54.8763598301037,48.8266326137622,
12.));
#152008=CARTESIAN_POINT('Ctrl Pts',(-54.8877238496566,48.8505664587974,
12.));
#152009=CARTESIAN_POINT('Ctrl Pts',(-54.8990816092953,48.8745443424477,
12.));
#152010=CARTESIAN_POINT('Ctrl Pts',(-54.9104330242742,48.8985662012528,
12.));
#152011=CARTESIAN_POINT('Ctrl Pts',(-54.9217780102355,48.9226319719368,
12.));
#152012=CARTESIAN_POINT('Ctrl Pts',(-54.9331164832424,48.9467415914269,
12.));
#152013=CARTESIAN_POINT('Ctrl Pts',(-54.9444483598378,48.9708949968795,
12.));
#152014=CARTESIAN_POINT('Ctrl Pts',(-54.9557735569943,48.9950921256526,
12.));
#152015=CARTESIAN_POINT('Ctrl Pts',(-54.9670919920029,49.0193329152479,
12.));
#152016=CARTESIAN_POINT('Ctrl Pts',(-54.9784035823766,49.0436173032528,
12.));
#152017=CARTESIAN_POINT('Ctrl Pts',(-54.9897082457606,49.067945227287,12.));
#152018=CARTESIAN_POINT('Ctrl Pts',(-55.0010058998107,49.0923166249219,
12.));
#152019=CARTESIAN_POINT('Ctrl Pts',(-55.012296462186,49.116731433673,12.));
#152020=CARTESIAN_POINT('Ctrl Pts',(-55.0235798508045,49.1411895911635,
12.));
#152021=CARTESIAN_POINT('Ctrl Pts',(-55.0348559840453,49.1656910352476,
12.));
#152022=CARTESIAN_POINT('Ctrl Pts',(-55.0461247809744,49.1902357041461,
12.));
#152023=CARTESIAN_POINT('Ctrl Pts',(-55.0573861615579,49.2148235365703,
12.));
#152024=CARTESIAN_POINT('Ctrl Pts',(-55.0686400468931,49.2394544718531,
12.));
#152025=CARTESIAN_POINT('Ctrl Pts',(-55.079886358701,49.264128449652,12.));
#152026=CARTESIAN_POINT('Ctrl Pts',(-55.0911250188302,49.2888454096563,
12.));
#152027=CARTESIAN_POINT('Ctrl Pts',(-55.102355948714,49.3136052912621,12.));
#152028=CARTESIAN_POINT('Ctrl Pts',(-55.1135790689464,49.3384080333155,
12.));
#152029=CARTESIAN_POINT('Ctrl Pts',(-55.1247942985619,49.3632535736715,
12.));
#152030=CARTESIAN_POINT('Ctrl Pts',(-55.1360015556221,49.3881418495489,
12.));
#152031=CARTESIAN_POINT('Ctrl Pts',(-55.1472007585183,49.4130727983201,
12.));
#152032=CARTESIAN_POINT('Ctrl Pts',(-55.1583918271116,49.4380463581965,
12.));
#152033=CARTESIAN_POINT('Ctrl Pts',(-55.1695746838174,49.4630624688793,
12.));
#152034=CARTESIAN_POINT('Ctrl Pts',(-55.1807492550119,49.4881210723966,
12.));
#152035=CARTESIAN_POINT('Ctrl Pts',(-55.1919154713647,49.5132221132992,
12.));
#152036=CARTESIAN_POINT('Ctrl Pts',(-55.2014798624093,49.5347748994759,
12.));
#152037=CARTESIAN_POINT('Ctrl Pts',(-55.2088081099093,49.551321852449,12.));
#152038=CARTESIAN_POINT('Ctrl Pts',(-55.2139039604722,49.5628442142133,
12.));
#152039=CARTESIAN_POINT('Ctrl Pts',(-55.2167699151339,49.5693295981928,
12.));
#152040=CARTESIAN_POINT('Ctrl Pts',(-55.2174072001495,49.5707719660639,
12.));
#152041=CARTESIAN_POINT('',(-53.0702932034641,45.6458539113724,0.));
#152042=CARTESIAN_POINT('',(-53.0702932034641,45.6458539113724,0.));
#152043=CARTESIAN_POINT('Ctrl Pts',(-55.2174072001495,49.5707719660639,
0.));
#152044=CARTESIAN_POINT('Ctrl Pts',(-55.2167699151339,49.5693295981928,
0.));
#152045=CARTESIAN_POINT('Ctrl Pts',(-55.2139039604722,49.5628442142133,
0.));
#152046=CARTESIAN_POINT('Ctrl Pts',(-55.2088081099093,49.551321852449,0.));
#152047=CARTESIAN_POINT('Ctrl Pts',(-55.2014798624093,49.5347748994759,
0.));
#152048=CARTESIAN_POINT('Ctrl Pts',(-55.1919154713647,49.5132221132992,
0.));
#152049=CARTESIAN_POINT('Ctrl Pts',(-55.1807492550119,49.4881210723966,
0.));
#152050=CARTESIAN_POINT('Ctrl Pts',(-55.1695746838174,49.4630624688793,
0.));
#152051=CARTESIAN_POINT('Ctrl Pts',(-55.1583918271116,49.4380463581965,
0.));
#152052=CARTESIAN_POINT('Ctrl Pts',(-55.1472007585183,49.4130727983201,
0.));
#152053=CARTESIAN_POINT('Ctrl Pts',(-55.1360015556221,49.3881418495489,
0.));
#152054=CARTESIAN_POINT('Ctrl Pts',(-55.1247942985619,49.3632535736715,
0.));
#152055=CARTESIAN_POINT('Ctrl Pts',(-55.1135790689464,49.3384080333155,
0.));
#152056=CARTESIAN_POINT('Ctrl Pts',(-55.102355948714,49.3136052912621,0.));
#152057=CARTESIAN_POINT('Ctrl Pts',(-55.0911250188302,49.2888454096563,
0.));
#152058=CARTESIAN_POINT('Ctrl Pts',(-55.079886358701,49.264128449652,0.));
#152059=CARTESIAN_POINT('Ctrl Pts',(-55.0686400468931,49.2394544718531,
0.));
#152060=CARTESIAN_POINT('Ctrl Pts',(-55.0573861615579,49.2148235365703,
0.));
#152061=CARTESIAN_POINT('Ctrl Pts',(-55.0461247809744,49.1902357041461,
0.));
#152062=CARTESIAN_POINT('Ctrl Pts',(-55.0348559840453,49.1656910352476,
0.));
#152063=CARTESIAN_POINT('Ctrl Pts',(-55.0235798508045,49.1411895911635,
0.));
#152064=CARTESIAN_POINT('Ctrl Pts',(-55.012296462186,49.116731433673,0.));
#152065=CARTESIAN_POINT('Ctrl Pts',(-55.0010058998107,49.0923166249219,
0.));
#152066=CARTESIAN_POINT('Ctrl Pts',(-54.9897082457606,49.067945227287,0.));
#152067=CARTESIAN_POINT('Ctrl Pts',(-54.9784035823766,49.0436173032528,
0.));
#152068=CARTESIAN_POINT('Ctrl Pts',(-54.9670919920029,49.0193329152479,
0.));
#152069=CARTESIAN_POINT('Ctrl Pts',(-54.9557735569943,48.9950921256526,
0.));
#152070=CARTESIAN_POINT('Ctrl Pts',(-54.9444483598378,48.9708949968795,
0.));
#152071=CARTESIAN_POINT('Ctrl Pts',(-54.9331164832424,48.9467415914269,
0.));
#152072=CARTESIAN_POINT('Ctrl Pts',(-54.9217780102355,48.9226319719368,
0.));
#152073=CARTESIAN_POINT('Ctrl Pts',(-54.9104330242742,48.8985662012528,
0.));
#152074=CARTESIAN_POINT('Ctrl Pts',(-54.8990816092953,48.8745443424477,
0.));
#152075=CARTESIAN_POINT('Ctrl Pts',(-54.8877238496566,48.8505664587974,
0.));
#152076=CARTESIAN_POINT('Ctrl Pts',(-54.8763598301037,48.8266326137622,
0.));
#152077=CARTESIAN_POINT('Ctrl Pts',(-54.8649896357285,48.8027428709614,
0.));
#152078=CARTESIAN_POINT('Ctrl Pts',(-54.8536133519292,48.7788972941438,
0.));
#152079=CARTESIAN_POINT('Ctrl Pts',(-54.8422310643763,48.7550959471601,
0.));
#152080=CARTESIAN_POINT('Ctrl Pts',(-54.8308428590344,48.7313388939845,
0.));
#152081=CARTESIAN_POINT('Ctrl Pts',(-54.819448822181,48.7076261987292,0.));
#152082=CARTESIAN_POINT('Ctrl Pts',(-54.8080490404275,48.6839579256566,
0.));
#152083=CARTESIAN_POINT('Ctrl Pts',(-54.796643600739,48.6603341391886,0.));
#152084=CARTESIAN_POINT('Ctrl Pts',(-54.7852325904583,48.6367549039112,
0.));
#152085=CARTESIAN_POINT('Ctrl Pts',(-54.7738160973031,48.6132202845783,
0.));
#152086=CARTESIAN_POINT('Ctrl Pts',(-54.7623942093586,48.5897303461125,
0.));
#152087=CARTESIAN_POINT('Ctrl Pts',(-54.7509670150714,48.5662851536026,
0.));
#152088=CARTESIAN_POINT('Ctrl Pts',(-54.7395346032453,48.5428847722977,
0.));
#152089=CARTESIAN_POINT('Ctrl Pts',(-54.7280970630351,48.519529267596,0.));
#152090=CARTESIAN_POINT('Ctrl Pts',(-54.716654483948,48.4962187050457,0.));
#152091=CARTESIAN_POINT('Ctrl Pts',(-54.7052069558497,48.472953150357,0.));
#152092=CARTESIAN_POINT('Ctrl Pts',(-54.6937545689695,48.4497326694052,
0.));
#152093=CARTESIAN_POINT('Ctrl Pts',(-54.6822974139064,48.426557328234,0.));
#152094=CARTESIAN_POINT('Ctrl Pts',(-54.6708355816358,48.4034271930514,
0.));
#152095=CARTESIAN_POINT('Ctrl Pts',(-54.6593691635145,48.3803423302294,
0.));
#152096=CARTESIAN_POINT('Ctrl Pts',(-54.6478982512794,48.3573028063124,
0.));
#152097=CARTESIAN_POINT('Ctrl Pts',(-54.6364229370494,48.3343086880194,
0.));
#152098=CARTESIAN_POINT('Ctrl Pts',(-54.6249433133261,48.3113600422443,
0.));
#152099=CARTESIAN_POINT('Ctrl Pts',(-54.6134594729959,48.2884569360506,
0.));
#152100=CARTESIAN_POINT('Ctrl Pts',(-54.6019715093309,48.2655994366665,
0.));
#152101=CARTESIAN_POINT('Ctrl Pts',(-54.5904795159926,48.2427876114947,
0.));
#152102=CARTESIAN_POINT('Ctrl Pts',(-54.5789835870342,48.2200215281173,
0.));
#152103=CARTESIAN_POINT('Ctrl Pts',(-54.5674838169041,48.1973012542966,
0.));
#152104=CARTESIAN_POINT('Ctrl Pts',(-54.5559803004492,48.1746268579736,
0.));
#152105=CARTESIAN_POINT('Ctrl Pts',(-54.5444731329201,48.1519984072622,
0.));
#152106=CARTESIAN_POINT('Ctrl Pts',(-54.5329624099721,48.1294159704573,
0.));
#152107=CARTESIAN_POINT('Ctrl Pts',(-54.5214482276678,48.1068796160405,
0.));
#152108=CARTESIAN_POINT('Ctrl Pts',(-54.5099306824786,48.0843894126806,
0.));
#152109=CARTESIAN_POINT('Ctrl Pts',(-54.4984098712886,48.0619454292324,
0.));
#152110=CARTESIAN_POINT('Ctrl Pts',(-54.4868858913971,48.0395477347298,
0.));
#152111=CARTESIAN_POINT('Ctrl Pts',(-54.4753588405215,48.0171963983924,
0.));
#152112=CARTESIAN_POINT('Ctrl Pts',(-54.4638288168003,47.9948914896326,
0.));
#152113=CARTESIAN_POINT('Ctrl Pts',(-54.4522959187955,47.9726330780572,
0.));
#152114=CARTESIAN_POINT('Ctrl Pts',(-54.4407602454967,47.9504212334675,
0.));
#152115=CARTESIAN_POINT('Ctrl Pts',(-54.429221896324,47.9282560258516,0.));
#152116=CARTESIAN_POINT('Ctrl Pts',(-54.4176809711311,47.9061375253897,
0.));
#152117=CARTESIAN_POINT('Ctrl Pts',(-54.4061375702079,47.8840658024618,
0.));
#152118=CARTESIAN_POINT('Ctrl Pts',(-54.3945917942832,47.8620409276493,
0.));
#152119=CARTESIAN_POINT('Ctrl Pts',(-54.3830437445279,47.8400629717355,
0.));
#152120=CARTESIAN_POINT('Ctrl Pts',(-54.3714935225591,47.8181320056995,
0.));
#152121=CARTESIAN_POINT('Ctrl Pts',(-54.3599412304437,47.7962481007185,
0.));
#152122=CARTESIAN_POINT('Ctrl Pts',(-54.3483869707002,47.7744113281771,
0.));
#152123=CARTESIAN_POINT('Ctrl Pts',(-54.3368308463023,47.7526217596694,
0.));
#152124=CARTESIAN_POINT('Ctrl Pts',(-54.3252729606823,47.7308794669993,
0.));
#152125=CARTESIAN_POINT('Ctrl Pts',(-54.3137134177345,47.7091845221747,
0.));
#152126=CARTESIAN_POINT('Ctrl Pts',(-54.302152321819,47.6875369974087,0.));
#152127=CARTESIAN_POINT('Ctrl Pts',(-54.290589777765,47.6659369651301,0.));
#152128=CARTESIAN_POINT('Ctrl Pts',(-54.2790258908738,47.6443844979847,
0.));
#152129=CARTESIAN_POINT('Ctrl Pts',(-54.2674607669226,47.6228796688375,
0.));
#152130=CARTESIAN_POINT('Ctrl Pts',(-54.2558945121678,47.6014225507659,
0.));
#152131=CARTESIAN_POINT('Ctrl Pts',(-54.244327233349,47.5800132170608,0.));
#152132=CARTESIAN_POINT('Ctrl Pts',(-54.2327590376924,47.5586517412363,
0.));
#152133=CARTESIAN_POINT('Ctrl Pts',(-54.2211900329138,47.5373381970326,
0.));
#152134=CARTESIAN_POINT('Ctrl Pts',(-54.209620327223,47.5160726584174,0.));
#152135=CARTESIAN_POINT('Ctrl Pts',(-54.198050029327,47.4948551995801,0.));
#152136=CARTESIAN_POINT('Ctrl Pts',(-54.1864792484345,47.4736858949322,
0.));
#152137=CARTESIAN_POINT('Ctrl Pts',(-54.1749080942593,47.4525648191173,
0.));
#152138=CARTESIAN_POINT('Ctrl Pts',(-54.1633366770239,47.4314920470141,
0.));
#152139=CARTESIAN_POINT('Ctrl Pts',(-54.1517651074637,47.4104676537381,
0.));
#152140=CARTESIAN_POINT('Ctrl Pts',(-54.1401934968311,47.3894917146365,
0.));
#152141=CARTESIAN_POINT('Ctrl Pts',(-54.1286219568989,47.3685643052874,
0.));
#152142=CARTESIAN_POINT('Ctrl Pts',(-54.1170505999645,47.3476855015102,
0.));
#152143=CARTESIAN_POINT('Ctrl Pts',(-54.1054795388543,47.3268553793694,
0.));
#152144=CARTESIAN_POINT('Ctrl Pts',(-54.0939088869269,47.3060740151752,
0.));
#152145=CARTESIAN_POINT('Ctrl Pts',(-54.0823387580776,47.2853414854793,
0.));
#152146=CARTESIAN_POINT('Ctrl Pts',(-54.0707692667438,47.2646578670746,
0.));
#152147=CARTESIAN_POINT('Ctrl Pts',(-54.0592005279086,47.2440232370065,
0.));
#152148=CARTESIAN_POINT('Ctrl Pts',(-54.047632657104,47.2234376725743,0.));
#152149=CARTESIAN_POINT('Ctrl Pts',(-54.0360657704163,47.202901251334,0.));
#152150=CARTESIAN_POINT('Ctrl Pts',(-54.0244999844893,47.1824140510926,
0.));
#152151=CARTESIAN_POINT('Ctrl Pts',(-54.0129354165297,47.1619761499087,
0.));
#152152=CARTESIAN_POINT('Ctrl Pts',(-54.0013721843118,47.1415876261035,
0.));
#152153=CARTESIAN_POINT('Ctrl Pts',(-53.989810406182,47.1212485582643,0.));
#152154=CARTESIAN_POINT('Ctrl Pts',(-53.9782502010634,47.1009590252458,
0.));
#152155=CARTESIAN_POINT('Ctrl Pts',(-53.9666916884596,47.0807191061648,
0.));
#152156=CARTESIAN_POINT('Ctrl Pts',(-53.95513498846,47.0605288804008,0.));
#152157=CARTESIAN_POINT('Ctrl Pts',(-53.9435802217436,47.0403884276071,
0.));
#152158=CARTESIAN_POINT('Ctrl Pts',(-53.9320275095853,47.0202978277138,
0.));
#152159=CARTESIAN_POINT('Ctrl Pts',(-53.9204769738596,47.0002571609297,
0.));
#152160=CARTESIAN_POINT('Ctrl Pts',(-53.9089287370463,46.9802665077366,
0.));
#152161=CARTESIAN_POINT('Ctrl Pts',(-53.8973829222348,46.960325948892,0.));
#152162=CARTESIAN_POINT('Ctrl Pts',(-53.8858396531298,46.94043556544,0.));
#152163=CARTESIAN_POINT('Ctrl Pts',(-53.8742990540563,46.9205954387133,
0.));
#152164=CARTESIAN_POINT('Ctrl Pts',(-53.8627612499638,46.9008056503351,
0.));
#152165=CARTESIAN_POINT('Ctrl Pts',(-53.8512263664321,46.881066282213,0.));
#152166=CARTESIAN_POINT('Ctrl Pts',(-53.8396945296757,46.8613774165435,
0.));
#152167=CARTESIAN_POINT('Ctrl Pts',(-53.8281658665503,46.841739135822,0.));
#152168=CARTESIAN_POINT('Ctrl Pts',(-53.816640504558,46.8221515228457,0.));
#152169=CARTESIAN_POINT('Ctrl Pts',(-53.8051185718532,46.802614660715,0.));
#152170=CARTESIAN_POINT('Ctrl Pts',(-53.793600197248,46.7831286328278,0.));
#152171=CARTESIAN_POINT('Ctrl Pts',(-53.7820855102182,46.763693522886,0.));
#152172=CARTESIAN_POINT('Ctrl Pts',(-53.7705746409076,46.7443094149045,
0.));
#152173=CARTESIAN_POINT('Ctrl Pts',(-53.7590677201342,46.7249763932129,
0.));
#152174=CARTESIAN_POINT('Ctrl Pts',(-53.7475648793946,46.7056945424559,
0.));
#152175=CARTESIAN_POINT('Ctrl Pts',(-53.7360662508675,46.6864639475862,
0.));
#152176=CARTESIAN_POINT('Ctrl Pts',(-53.7245719674221,46.6672846938752,
0.));
#152177=CARTESIAN_POINT('Ctrl Pts',(-53.7130821626262,46.6481568669217,
0.));
#152178=CARTESIAN_POINT('Ctrl Pts',(-53.7015969707541,46.6290805526559,
0.));
#152179=CARTESIAN_POINT('Ctrl Pts',(-53.690116526794,46.6100558373401,0.));
#152180=CARTESIAN_POINT('Ctrl Pts',(-53.678640966456,46.5910828075652,0.));
#152181=CARTESIAN_POINT('Ctrl Pts',(-53.6671704261735,46.5721615502589,
0.));
#152182=CARTESIAN_POINT('Ctrl Pts',(-53.6557050431069,46.5532921526899,
0.));
#152183=CARTESIAN_POINT('Ctrl Pts',(-53.6442449551455,46.5344747024677,
0.));
#152184=CARTESIAN_POINT('Ctrl Pts',(-53.6327903009098,46.5157092875377,
0.));
#152185=CARTESIAN_POINT('Ctrl Pts',(-53.6213412197542,46.4969959961779,
0.));
#152186=CARTESIAN_POINT('Ctrl Pts',(-53.6098978517869,46.4783349170182,
0.));
#152187=CARTESIAN_POINT('Ctrl Pts',(-53.5984603378862,46.4597261390526,
0.));
#152188=CARTESIAN_POINT('Ctrl Pts',(-53.5870288197161,46.4411697516474,
0.));
#152189=CARTESIAN_POINT('Ctrl Pts',(-53.5756034397464,46.422665844546,0.));
#152190=CARTESIAN_POINT('Ctrl Pts',(-53.5641843412537,46.4042145078682,
0.));
#152191=CARTESIAN_POINT('Ctrl Pts',(-53.552771668303,46.3858158321044,0.));
#152192=CARTESIAN_POINT('Ctrl Pts',(-53.5413655657323,46.3674699081043,
0.));
#152193=CARTESIAN_POINT('Ctrl Pts',(-53.5299661791396,46.3491768270664,
0.));
#152194=CARTESIAN_POINT('Ctrl Pts',(-53.518573654857,46.3309366805112,0.));
#152195=CARTESIAN_POINT('Ctrl Pts',(-53.5071881399932,46.3127495603117,
0.));
#152196=CARTESIAN_POINT('Ctrl Pts',(-53.4958097825019,46.2946155587428,
0.));
#152197=CARTESIAN_POINT('Ctrl Pts',(-53.4844387312414,46.2765347685198,
0.));
#152198=CARTESIAN_POINT('Ctrl Pts',(-53.4730751360359,46.2585072828343,
0.));
#152199=CARTESIAN_POINT('Ctrl Pts',(-53.4617191477382,46.2405331953872,
0.));
#152200=CARTESIAN_POINT('Ctrl Pts',(-53.4503709181158,46.2226126003185,
0.));
#152201=CARTESIAN_POINT('Ctrl Pts',(-53.4390305997263,46.2047455921276,
0.));
#152202=CARTESIAN_POINT('Ctrl Pts',(-53.4276983458129,46.1869322656027,
0.));
#152203=CARTESIAN_POINT('Ctrl Pts',(-53.4163743101535,46.1691727157149,
0.));
#152204=CARTESIAN_POINT('Ctrl Pts',(-53.4050586470463,46.1514670376035,
0.));
#152205=CARTESIAN_POINT('Ctrl Pts',(-53.3937515116572,46.1338153268116,
0.));
#152206=CARTESIAN_POINT('Ctrl Pts',(-53.3824530603284,46.1162176794891,
0.));
#152207=CARTESIAN_POINT('Ctrl Pts',(-53.3711634508426,46.0986741925646,
0.));
#152208=CARTESIAN_POINT('Ctrl Pts',(-53.3598828428519,46.0811849640195,
0.));
#152209=CARTESIAN_POINT('Ctrl Pts',(-53.3486113975868,46.0637500926954,
0.));
#152210=CARTESIAN_POINT('Ctrl Pts',(-53.3373492770647,46.046369677778,0.));
#152211=CARTESIAN_POINT('Ctrl Pts',(-53.3260966434277,46.0290438183598,
0.));
#152212=CARTESIAN_POINT('Ctrl Pts',(-53.3148536582658,46.0117726129893,
0.));
#152213=CARTESIAN_POINT('Ctrl Pts',(-53.3036204818367,45.9945561591486,
0.));
#152214=CARTESIAN_POINT('Ctrl Pts',(-53.2923972745585,45.9773945542415,
0.));
#152215=CARTESIAN_POINT('Ctrl Pts',(-53.2811841987945,45.9602878967714,
0.));
#152216=CARTESIAN_POINT('Ctrl Pts',(-53.2699814203097,45.9432362873001,
0.));
#152217=CARTESIAN_POINT('Ctrl Pts',(-53.2587891103835,45.9262398298323,
0.));
#152218=CARTESIAN_POINT('Ctrl Pts',(-53.2476074459977,45.9092986319343,
0.));
#152219=CARTESIAN_POINT('Ctrl Pts',(-53.2364366054276,45.8924128018354,
0.));
#152220=CARTESIAN_POINT('Ctrl Pts',(-53.2252767643652,45.8755824458715,
0.));
#152221=CARTESIAN_POINT('Ctrl Pts',(-53.2141280925458,45.8588076662598,
0.));
#152222=CARTESIAN_POINT('Ctrl Pts',(-53.2029907483602,45.8420885575386,
0.));
#152223=CARTESIAN_POINT('Ctrl Pts',(-53.1918648840598,45.8254252100003,
0.));
#152224=CARTESIAN_POINT('Ctrl Pts',(-53.1807506560977,45.8088177165124,
0.));
#152225=CARTESIAN_POINT('Ctrl Pts',(-53.1696482334487,45.7922661780005,
0.));
#152226=CARTESIAN_POINT('Ctrl Pts',(-53.158557807638,45.7757707100568,0.));
#152227=CARTESIAN_POINT('Ctrl Pts',(-53.147479599594,45.7593314474412,0.));
#152228=CARTESIAN_POINT('Ctrl Pts',(-53.136413838457,45.7429485300727,0.));
#152229=CARTESIAN_POINT('Ctrl Pts',(-53.1253607414806,45.7266220896951,
0.));
#152230=CARTESIAN_POINT('Ctrl Pts',(-53.1143204954981,45.7103522376744,
0.));
#152231=CARTESIAN_POINT('Ctrl Pts',(-53.1032932329074,45.6941390489239,
0.));
#152232=CARTESIAN_POINT('Ctrl Pts',(-53.0922790298736,45.6779825614486,
0.));
#152233=CARTESIAN_POINT('Ctrl Pts',(-53.083478145185,45.6651027439479,0.));
#152234=CARTESIAN_POINT('Ctrl Pts',(-53.0768833804386,45.6554684028296,
0.));
#152235=CARTESIAN_POINT('Ctrl Pts',(-53.0724894921921,45.6490568514146,
0.));
#152236=CARTESIAN_POINT('Ctrl Pts',(-53.0702932034641,45.6458539113724,
0.));
#152237=CARTESIAN_POINT('Ctrl Pts',(-50.7903314215393,54.5031396718592,
0.));
#152238=CARTESIAN_POINT('Ctrl Pts',(-50.7903314215393,54.5031396718592,
12.));
#152239=CARTESIAN_POINT('Ctrl Pts',(-50.7885805844281,54.4978248630387,
0.));
#152240=CARTESIAN_POINT('Ctrl Pts',(-50.7885805844281,54.4978248630387,
12.));
#152241=CARTESIAN_POINT('Ctrl Pts',(-50.7850776288814,54.4871993224832,
0.));
#152242=CARTESIAN_POINT('Ctrl Pts',(-50.7850776288814,54.4871993224832,
12.));
#152243=CARTESIAN_POINT('Ctrl Pts',(-50.7798193515888,54.4712732429066,
0.));
#152244=CARTESIAN_POINT('Ctrl Pts',(-50.7798193515888,54.4712732429066,
12.));
#152245=CARTESIAN_POINT('Ctrl Pts',(-50.7728006269349,54.4500629336429,
0.));
#152246=CARTESIAN_POINT('Ctrl Pts',(-50.7728006269349,54.4500629336429,
12.));
#152247=CARTESIAN_POINT('Ctrl Pts',(-50.764014409002,54.423590828767,0.));
#152248=CARTESIAN_POINT('Ctrl Pts',(-50.764014409002,54.423590828767,12.));
#152249=CARTESIAN_POINT('Ctrl Pts',(-50.7552153869475,54.3971595231574,
0.));
#152250=CARTESIAN_POINT('Ctrl Pts',(-50.7552153869475,54.3971595231574,
12.));
#152251=CARTESIAN_POINT('Ctrl Pts',(-50.7464035792906,54.3707690445748,
0.));
#152252=CARTESIAN_POINT('Ctrl Pts',(-50.7464035792906,54.3707690445748,
12.));
#152253=CARTESIAN_POINT('Ctrl Pts',(-50.7375790185896,54.3444194324054,
0.));
#152254=CARTESIAN_POINT('Ctrl Pts',(-50.7375790185896,54.3444194324054,
12.));
#152255=CARTESIAN_POINT('Ctrl Pts',(-50.7287417566123,54.3181107400663,
0.));
#152256=CARTESIAN_POINT('Ctrl Pts',(-50.7287417566123,54.3181107400663,
12.));
#152257=CARTESIAN_POINT('Ctrl Pts',(-50.7198918629451,54.2918430335206,
0.));
#152258=CARTESIAN_POINT('Ctrl Pts',(-50.7198918629451,54.2918430335206,
12.));
#152259=CARTESIAN_POINT('Ctrl Pts',(-50.7110294185698,54.2656163868104,
0.));
#152260=CARTESIAN_POINT('Ctrl Pts',(-50.7110294185698,54.2656163868104,
12.));
#152261=CARTESIAN_POINT('Ctrl Pts',(-50.7021545108311,54.2394308784026,
0.));
#152262=CARTESIAN_POINT('Ctrl Pts',(-50.7021545108311,54.2394308784026,
12.));
#152263=CARTESIAN_POINT('Ctrl Pts',(-50.6932672279772,54.2132865872985,
0.));
#152264=CARTESIAN_POINT('Ctrl Pts',(-50.6932672279772,54.2132865872985,
12.));
#152265=CARTESIAN_POINT('Ctrl Pts',(-50.6843676535492,54.1871835889981,
0.));
#152266=CARTESIAN_POINT('Ctrl Pts',(-50.6843676535492,54.1871835889981,
12.));
#152267=CARTESIAN_POINT('Ctrl Pts',(-50.67545586183,54.1611219522394,0.));
#152268=CARTESIAN_POINT('Ctrl Pts',(-50.67545586183,54.1611219522394,12.));
#152269=CARTESIAN_POINT('Ctrl Pts',(-50.6665319209869,54.1351017412804,
0.));
#152270=CARTESIAN_POINT('Ctrl Pts',(-50.6665319209869,54.1351017412804,
12.));
#152271=CARTESIAN_POINT('Ctrl Pts',(-50.6575958953221,54.1091230175367,
0.));
#152272=CARTESIAN_POINT('Ctrl Pts',(-50.6575958953221,54.1091230175367,
12.));
#152273=CARTESIAN_POINT('Ctrl Pts',(-50.6486478479465,54.0831858415189,
0.));
#152274=CARTESIAN_POINT('Ctrl Pts',(-50.6486478479465,54.0831858415189,
12.));
#152275=CARTESIAN_POINT('Ctrl Pts',(-50.6396878430939,54.0572902745076,
0.));
#152276=CARTESIAN_POINT('Ctrl Pts',(-50.6396878430939,54.0572902745076,
12.));
#152277=CARTESIAN_POINT('Ctrl Pts',(-50.6307159490553,54.0314363806708,
0.));
#152278=CARTESIAN_POINT('Ctrl Pts',(-50.6307159490553,54.0314363806708,
12.));
#152279=CARTESIAN_POINT('Ctrl Pts',(-50.6217322378648,54.0056242268399,
0.));
#152280=CARTESIAN_POINT('Ctrl Pts',(-50.6217322378648,54.0056242268399,
12.));
#152281=CARTESIAN_POINT('Ctrl Pts',(-50.6127367839711,53.979853881553,0.));
#152282=CARTESIAN_POINT('Ctrl Pts',(-50.6127367839711,53.979853881553,12.));
#152283=CARTESIAN_POINT('Ctrl Pts',(-50.603729663214,53.9541254143119,0.));
#152284=CARTESIAN_POINT('Ctrl Pts',(-50.603729663214,53.9541254143119,12.));
#152285=CARTESIAN_POINT('Ctrl Pts',(-50.5947109517483,53.9284388948004,
0.));
#152286=CARTESIAN_POINT('Ctrl Pts',(-50.5947109517483,53.9284388948004,
12.));
#152287=CARTESIAN_POINT('Ctrl Pts',(-50.5856807248151,53.9027943919836,
0.));
#152288=CARTESIAN_POINT('Ctrl Pts',(-50.5856807248151,53.9027943919836,
12.));
#152289=CARTESIAN_POINT('Ctrl Pts',(-50.5766390561884,53.8771919737032,
0.));
#152290=CARTESIAN_POINT('Ctrl Pts',(-50.5766390561884,53.8771919737032,
12.));
#152291=CARTESIAN_POINT('Ctrl Pts',(-50.5675860188538,53.8516317071804,
0.));
#152292=CARTESIAN_POINT('Ctrl Pts',(-50.5675860188538,53.8516317071804,
12.));
#152293=CARTESIAN_POINT('Ctrl Pts',(-50.5585216854091,53.8261136593075,
0.));
#152294=CARTESIAN_POINT('Ctrl Pts',(-50.5585216854091,53.8261136593075,
12.));
#152295=CARTESIAN_POINT('Ctrl Pts',(-50.5494461285761,53.8006378970197,
0.));
#152296=CARTESIAN_POINT('Ctrl Pts',(-50.5494461285761,53.8006378970197,
12.));
#152297=CARTESIAN_POINT('Ctrl Pts',(-50.5403594216698,53.7752044876304,
0.));
#152298=CARTESIAN_POINT('Ctrl Pts',(-50.5403594216698,53.7752044876304,
12.));
#152299=CARTESIAN_POINT('Ctrl Pts',(-50.5312616390779,53.7498134991703,
0.));
#152300=CARTESIAN_POINT('Ctrl Pts',(-50.5312616390779,53.7498134991703,
12.));
#152301=CARTESIAN_POINT('Ctrl Pts',(-50.522152856042,53.7244650002374,0.));
#152302=CARTESIAN_POINT('Ctrl Pts',(-50.522152856042,53.7244650002374,12.));
#152303=CARTESIAN_POINT('Ctrl Pts',(-50.513033148456,53.6991590598548,0.));
#152304=CARTESIAN_POINT('Ctrl Pts',(-50.513033148456,53.6991590598548,12.));
#152305=CARTESIAN_POINT('Ctrl Pts',(-50.503902592653,53.6738957473158,0.));
#152306=CARTESIAN_POINT('Ctrl Pts',(-50.503902592653,53.6738957473158,12.));
#152307=CARTESIAN_POINT('Ctrl Pts',(-50.4947612652148,53.6486751320436,
0.));
#152308=CARTESIAN_POINT('Ctrl Pts',(-50.4947612652148,53.6486751320436,
12.));
#152309=CARTESIAN_POINT('Ctrl Pts',(-50.4856092427314,53.623497283406,0.));
#152310=CARTESIAN_POINT('Ctrl Pts',(-50.4856092427314,53.623497283406,12.));
#152311=CARTESIAN_POINT('Ctrl Pts',(-50.4764466018071,53.5983622707238,
0.));
#152312=CARTESIAN_POINT('Ctrl Pts',(-50.4764466018071,53.5983622707238,
12.));
#152313=CARTESIAN_POINT('Ctrl Pts',(-50.4672734191756,53.5732701633609,
0.));
#152314=CARTESIAN_POINT('Ctrl Pts',(-50.4672734191756,53.5732701633609,
12.));
#152315=CARTESIAN_POINT('Ctrl Pts',(-50.4580897717838,53.5482210307868,
0.));
#152316=CARTESIAN_POINT('Ctrl Pts',(-50.4580897717838,53.5482210307868,
12.));
#152317=CARTESIAN_POINT('Ctrl Pts',(-50.4488957368839,53.5232149426413,
0.));
#152318=CARTESIAN_POINT('Ctrl Pts',(-50.4488957368839,53.5232149426413,
12.));
#152319=CARTESIAN_POINT('Ctrl Pts',(-50.4396913921382,53.4982519688024,
0.));
#152320=CARTESIAN_POINT('Ctrl Pts',(-50.4396913921382,53.4982519688024,
12.));
#152321=CARTESIAN_POINT('Ctrl Pts',(-50.4304768156667,53.4733321794188,
0.));
#152322=CARTESIAN_POINT('Ctrl Pts',(-50.4304768156667,53.4733321794188,
12.));
#152323=CARTESIAN_POINT('Ctrl Pts',(-50.4212520859914,53.4484556448776,
0.));
#152324=CARTESIAN_POINT('Ctrl Pts',(-50.4212520859914,53.4484556448776,
12.));
#152325=CARTESIAN_POINT('Ctrl Pts',(-50.4120172820047,53.4236224357838,
0.));
#152326=CARTESIAN_POINT('Ctrl Pts',(-50.4120172820047,53.4236224357838,
12.));
#152327=CARTESIAN_POINT('Ctrl Pts',(-50.4027724829297,53.398832622931,0.));
#152328=CARTESIAN_POINT('Ctrl Pts',(-50.4027724829297,53.398832622931,12.));
#152329=CARTESIAN_POINT('Ctrl Pts',(-50.3935177682837,53.3740862772681,
0.));
#152330=CARTESIAN_POINT('Ctrl Pts',(-50.3935177682837,53.3740862772681,
12.));
#152331=CARTESIAN_POINT('Ctrl Pts',(-50.384253217846,53.3493834698697,0.));
#152332=CARTESIAN_POINT('Ctrl Pts',(-50.384253217846,53.3493834698697,12.));
#152333=CARTESIAN_POINT('Ctrl Pts',(-50.3749789116786,53.3247242719587,
0.));
#152334=CARTESIAN_POINT('Ctrl Pts',(-50.3749789116786,53.3247242719587,
12.));
#152335=CARTESIAN_POINT('Ctrl Pts',(-50.365694930143,53.300108754923,0.));
#152336=CARTESIAN_POINT('Ctrl Pts',(-50.365694930143,53.300108754923,12.));
#152337=CARTESIAN_POINT('Ctrl Pts',(-50.3564013539199,53.2755369903293,
0.));
#152338=CARTESIAN_POINT('Ctrl Pts',(-50.3564013539199,53.2755369903293,
12.));
#152339=CARTESIAN_POINT('Ctrl Pts',(-50.3470982640289,53.2510090499336,
0.));
#152340=CARTESIAN_POINT('Ctrl Pts',(-50.3470982640289,53.2510090499336,
12.));
#152341=CARTESIAN_POINT('Ctrl Pts',(-50.3377857418514,53.2265250056887,
0.));
#152342=CARTESIAN_POINT('Ctrl Pts',(-50.3377857418514,53.2265250056887,
12.));
#152343=CARTESIAN_POINT('Ctrl Pts',(-50.3284638691278,53.2020849297471,
0.));
#152344=CARTESIAN_POINT('Ctrl Pts',(-50.3284638691278,53.2020849297471,
12.));
#152345=CARTESIAN_POINT('Ctrl Pts',(-50.3191327279493,53.1776888944616,
0.));
#152346=CARTESIAN_POINT('Ctrl Pts',(-50.3191327279493,53.1776888944616,
12.));
#152347=CARTESIAN_POINT('Ctrl Pts',(-50.3097924007534,53.1533369723818,
0.));
#152348=CARTESIAN_POINT('Ctrl Pts',(-50.3097924007534,53.1533369723818,
12.));
#152349=CARTESIAN_POINT('Ctrl Pts',(-50.300442970319,53.1290292362485,0.));
#152350=CARTESIAN_POINT('Ctrl Pts',(-50.300442970319,53.1290292362485,12.));
#152351=CARTESIAN_POINT('Ctrl Pts',(-50.2910845197619,53.1047657589812,
0.));
#152352=CARTESIAN_POINT('Ctrl Pts',(-50.2910845197619,53.1047657589812,
12.));
#152353=CARTESIAN_POINT('Ctrl Pts',(-50.2817171325358,53.0805466136797,
0.));
#152354=CARTESIAN_POINT('Ctrl Pts',(-50.2817171325358,53.0805466136797,
12.));
#152355=CARTESIAN_POINT('Ctrl Pts',(-50.2723408924373,53.0563718736366,
0.));
#152356=CARTESIAN_POINT('Ctrl Pts',(-50.2723408924373,53.0563718736366,
12.));
#152357=CARTESIAN_POINT('Ctrl Pts',(-50.2629558836111,53.0322416123406,
0.));
#152358=CARTESIAN_POINT('Ctrl Pts',(-50.2629558836111,53.0322416123406,
12.));
#152359=CARTESIAN_POINT('Ctrl Pts',(-50.2535621905552,53.0081559034801,
0.));
#152360=CARTESIAN_POINT('Ctrl Pts',(-50.2535621905552,53.0081559034801,
12.));
#152361=CARTESIAN_POINT('Ctrl Pts',(-50.2441598981286,52.9841148209402,
0.));
#152362=CARTESIAN_POINT('Ctrl Pts',(-50.2441598981286,52.9841148209402,
12.));
#152363=CARTESIAN_POINT('Ctrl Pts',(-50.2347490915555,52.9601184388027,
0.));
#152364=CARTESIAN_POINT('Ctrl Pts',(-50.2347490915555,52.9601184388027,
12.));
#152365=CARTESIAN_POINT('Ctrl Pts',(-50.2253298564241,52.9361668313542,
0.));
#152366=CARTESIAN_POINT('Ctrl Pts',(-50.2253298564241,52.9361668313542,
12.));
#152367=CARTESIAN_POINT('Ctrl Pts',(-50.2159022786879,52.9122600730884,
0.));
#152368=CARTESIAN_POINT('Ctrl Pts',(-50.2159022786879,52.9122600730884,
12.));
#152369=CARTESIAN_POINT('Ctrl Pts',(-50.2064664446663,52.8883982387068,
0.));
#152370=CARTESIAN_POINT('Ctrl Pts',(-50.2064664446663,52.8883982387068,
12.));
#152371=CARTESIAN_POINT('Ctrl Pts',(-50.1970224410471,52.8645814031133,
0.));
#152372=CARTESIAN_POINT('Ctrl Pts',(-50.1970224410471,52.8645814031133,
12.));
#152373=CARTESIAN_POINT('Ctrl Pts',(-50.1875703548884,52.8408096414093,
0.));
#152374=CARTESIAN_POINT('Ctrl Pts',(-50.1875703548884,52.8408096414093,
12.));
#152375=CARTESIAN_POINT('Ctrl Pts',(-50.1781102736205,52.8170830289044,
0.));
#152376=CARTESIAN_POINT('Ctrl Pts',(-50.1781102736205,52.8170830289044,
12.));
#152377=CARTESIAN_POINT('Ctrl Pts',(-50.1686422850488,52.7934016411205,
0.));
#152378=CARTESIAN_POINT('Ctrl Pts',(-50.1686422850488,52.7934016411205,
12.));
#152379=CARTESIAN_POINT('Ctrl Pts',(-50.1591664773561,52.769765553794,0.));
#152380=CARTESIAN_POINT('Ctrl Pts',(-50.1591664773561,52.769765553794,12.));
#152381=CARTESIAN_POINT('Ctrl Pts',(-50.1496829391073,52.7461748428738,
0.));
#152382=CARTESIAN_POINT('Ctrl Pts',(-50.1496829391073,52.7461748428738,
12.));
#152383=CARTESIAN_POINT('Ctrl Pts',(-50.1401917592537,52.7226295845161,
0.));
#152384=CARTESIAN_POINT('Ctrl Pts',(-50.1401917592537,52.7226295845161,
12.));
#152385=CARTESIAN_POINT('Ctrl Pts',(-50.1306930271345,52.699129855093,0.));
#152386=CARTESIAN_POINT('Ctrl Pts',(-50.1306930271345,52.699129855093,12.));
#152387=CARTESIAN_POINT('Ctrl Pts',(-50.1211868324781,52.6756757311978,
0.));
#152388=CARTESIAN_POINT('Ctrl Pts',(-50.1211868324781,52.6756757311978,
12.));
#152389=CARTESIAN_POINT('Ctrl Pts',(-50.111673265404,52.652267289646,0.));
#152390=CARTESIAN_POINT('Ctrl Pts',(-50.111673265404,52.652267289646,12.));
#152391=CARTESIAN_POINT('Ctrl Pts',(-50.1021524164264,52.6289046074746,
0.));
#152392=CARTESIAN_POINT('Ctrl Pts',(-50.1021524164264,52.6289046074746,
12.));
#152393=CARTESIAN_POINT('Ctrl Pts',(-50.0926243764578,52.6055877619348,
0.));
#152394=CARTESIAN_POINT('Ctrl Pts',(-50.0926243764578,52.6055877619348,
12.));
#152395=CARTESIAN_POINT('Ctrl Pts',(-50.0830892368107,52.5823168304994,
0.));
#152396=CARTESIAN_POINT('Ctrl Pts',(-50.0830892368107,52.5823168304994,
12.));
#152397=CARTESIAN_POINT('Ctrl Pts',(-50.0735470892007,52.5590918908702,
0.));
#152398=CARTESIAN_POINT('Ctrl Pts',(-50.0735470892007,52.5590918908702,
12.));
#152399=CARTESIAN_POINT('Ctrl Pts',(-50.0639980257479,52.5359130209792,
0.));
#152400=CARTESIAN_POINT('Ctrl Pts',(-50.0639980257479,52.5359130209792,
12.));
#152401=CARTESIAN_POINT('Ctrl Pts',(-50.0544421389818,52.5127802989896,
0.));
#152402=CARTESIAN_POINT('Ctrl Pts',(-50.0544421389818,52.5127802989896,
12.));
#152403=CARTESIAN_POINT('Ctrl Pts',(-50.0448795218441,52.4896938032884,
0.));
#152404=CARTESIAN_POINT('Ctrl Pts',(-50.0448795218441,52.4896938032884,
12.));
#152405=CARTESIAN_POINT('Ctrl Pts',(-50.0353102676921,52.4666536124913,
0.));
#152406=CARTESIAN_POINT('Ctrl Pts',(-50.0353102676921,52.4666536124913,
12.));
#152407=CARTESIAN_POINT('Ctrl Pts',(-50.0257344703,52.4436598054515,0.));
#152408=CARTESIAN_POINT('Ctrl Pts',(-50.0257344703,52.4436598054515,12.));
#152409=CARTESIAN_POINT('Ctrl Pts',(-50.0161522238616,52.4207124612608,
0.));
#152410=CARTESIAN_POINT('Ctrl Pts',(-50.0161522238616,52.4207124612608,
12.));
#152411=CARTESIAN_POINT('Ctrl Pts',(-50.0065636229938,52.3978116592509,
0.));
#152412=CARTESIAN_POINT('Ctrl Pts',(-50.0065636229938,52.3978116592509,
12.));
#152413=CARTESIAN_POINT('Ctrl Pts',(-49.9969687627408,52.3749574789871,
0.));
#152414=CARTESIAN_POINT('Ctrl Pts',(-49.9969687627408,52.3749574789871,
12.));
#152415=CARTESIAN_POINT('Ctrl Pts',(-49.9873677385775,52.3521500002718,
0.));
#152416=CARTESIAN_POINT('Ctrl Pts',(-49.9873677385775,52.3521500002718,
12.));
#152417=CARTESIAN_POINT('Ctrl Pts',(-49.9777606464106,52.3293893031528,
0.));
#152418=CARTESIAN_POINT('Ctrl Pts',(-49.9777606464106,52.3293893031528,
12.));
#152419=CARTESIAN_POINT('Ctrl Pts',(-49.9681475825824,52.3066754679265,
0.));
#152420=CARTESIAN_POINT('Ctrl Pts',(-49.9681475825824,52.3066754679265,
12.));
#152421=CARTESIAN_POINT('Ctrl Pts',(-49.9585286438733,52.2840085751384,
0.));
#152422=CARTESIAN_POINT('Ctrl Pts',(-49.9585286438733,52.2840085751384,
12.));
#152423=CARTESIAN_POINT('Ctrl Pts',(-49.9489039275064,52.2613887055773,
0.));
#152424=CARTESIAN_POINT('Ctrl Pts',(-49.9489039275064,52.2613887055773,
12.));
#152425=CARTESIAN_POINT('Ctrl Pts',(-49.9392735311509,52.2388159402771,
0.));
#152426=CARTESIAN_POINT('Ctrl Pts',(-49.9392735311509,52.2388159402771,
12.));
#152427=CARTESIAN_POINT('Ctrl Pts',(-49.9296375529245,52.2162903605275,
0.));
#152428=CARTESIAN_POINT('Ctrl Pts',(-49.9296375529245,52.2162903605275,
12.));
#152429=CARTESIAN_POINT('Ctrl Pts',(-49.9199960913962,52.1938120478754,
0.));
#152430=CARTESIAN_POINT('Ctrl Pts',(-49.9199960913962,52.1938120478754,
12.));
#152431=CARTESIAN_POINT('Ctrl Pts',(-49.9103492455902,52.1713810841276,
0.));
#152432=CARTESIAN_POINT('Ctrl Pts',(-49.9103492455902,52.1713810841276,
12.));
#152433=CARTESIAN_POINT('Ctrl Pts',(-49.9006971149895,52.1489975513444,
0.));
#152434=CARTESIAN_POINT('Ctrl Pts',(-49.9006971149895,52.1489975513444,
12.));
#152435=CARTESIAN_POINT('Ctrl Pts',(-49.8910397995397,52.1266615318407,
0.));
#152436=CARTESIAN_POINT('Ctrl Pts',(-49.8910397995397,52.1266615318407,
12.));
#152437=CARTESIAN_POINT('Ctrl Pts',(-49.8813773996517,52.1043731081962,
0.));
#152438=CARTESIAN_POINT('Ctrl Pts',(-49.8813773996517,52.1043731081962,
12.));
#152439=CARTESIAN_POINT('Ctrl Pts',(-49.8717100162048,52.0821323632587,
0.));
#152440=CARTESIAN_POINT('Ctrl Pts',(-49.8717100162048,52.0821323632587,
12.));
#152441=CARTESIAN_POINT('Ctrl Pts',(-49.86203775055,52.0599393801452,0.));
#152442=CARTESIAN_POINT('Ctrl Pts',(-49.86203775055,52.0599393801452,12.));
#152443=CARTESIAN_POINT('Ctrl Pts',(-49.8523607045149,52.0377942422376,
0.));
#152444=CARTESIAN_POINT('Ctrl Pts',(-49.8523607045149,52.0377942422376,
12.));
#152445=CARTESIAN_POINT('Ctrl Pts',(-49.8426789804071,52.0156970331822,
0.));
#152446=CARTESIAN_POINT('Ctrl Pts',(-49.8426789804071,52.0156970331822,
12.));
#152447=CARTESIAN_POINT('Ctrl Pts',(-49.8329926810172,51.9936478369008,
0.));
#152448=CARTESIAN_POINT('Ctrl Pts',(-49.8329926810172,51.9936478369008,
12.));
#152449=CARTESIAN_POINT('Ctrl Pts',(-49.8233019096222,51.9716467375937,
0.));
#152450=CARTESIAN_POINT('Ctrl Pts',(-49.8233019096222,51.9716467375937,
12.));
#152451=CARTESIAN_POINT('Ctrl Pts',(-49.8136067699896,51.9496938197418,
0.));
#152452=CARTESIAN_POINT('Ctrl Pts',(-49.8136067699896,51.9496938197418,
12.));
#152453=CARTESIAN_POINT('Ctrl Pts',(-49.8039073663812,51.9277891681018,
0.));
#152454=CARTESIAN_POINT('Ctrl Pts',(-49.8039073663812,51.9277891681018,
12.));
#152455=CARTESIAN_POINT('Ctrl Pts',(-49.7942038035576,51.9059328677059,
0.));
#152456=CARTESIAN_POINT('Ctrl Pts',(-49.7942038035576,51.9059328677059,
12.));
#152457=CARTESIAN_POINT('Ctrl Pts',(-49.7844961867807,51.8841250038724,
0.));
#152458=CARTESIAN_POINT('Ctrl Pts',(-49.7844961867807,51.8841250038724,
12.));
#152459=CARTESIAN_POINT('Ctrl Pts',(-49.7747846218182,51.8623656622097,
0.));
#152460=CARTESIAN_POINT('Ctrl Pts',(-49.7747846218182,51.8623656622097,
12.));
#152461=CARTESIAN_POINT('Ctrl Pts',(-49.7650692149462,51.8406549286175,
0.));
#152462=CARTESIAN_POINT('Ctrl Pts',(-49.7650692149462,51.8406549286175,
12.));
#152463=CARTESIAN_POINT('Ctrl Pts',(-49.755350072955,51.8189928892828,0.));
#152464=CARTESIAN_POINT('Ctrl Pts',(-49.755350072955,51.8189928892828,12.));
#152465=CARTESIAN_POINT('Ctrl Pts',(-49.7456273031534,51.7973796306803,
0.));
#152466=CARTESIAN_POINT('Ctrl Pts',(-49.7456273031534,51.7973796306803,
12.));
#152467=CARTESIAN_POINT('Ctrl Pts',(-49.7359010133721,51.7758152395836,
0.));
#152468=CARTESIAN_POINT('Ctrl Pts',(-49.7359010133721,51.7758152395836,
12.));
#152469=CARTESIAN_POINT('Ctrl Pts',(-49.7261713119663,51.754299803067,0.));
#152470=CARTESIAN_POINT('Ctrl Pts',(-49.7261713119663,51.754299803067,12.));
#152471=CARTESIAN_POINT('Ctrl Pts',(-49.7164383078212,51.7328334085091,
0.));
#152472=CARTESIAN_POINT('Ctrl Pts',(-49.7164383078212,51.7328334085091,
12.));
#152473=CARTESIAN_POINT('Ctrl Pts',(-49.7067021103553,51.7114161435869,
0.));
#152474=CARTESIAN_POINT('Ctrl Pts',(-49.7067021103553,51.7114161435869,
12.));
#152475=CARTESIAN_POINT('Ctrl Pts',(-49.6969628295262,51.6900480962773,
0.));
#152476=CARTESIAN_POINT('Ctrl Pts',(-49.6969628295262,51.6900480962773,
12.));
#152477=CARTESIAN_POINT('Ctrl Pts',(-49.6872205758336,51.6687293548682,
0.));
#152478=CARTESIAN_POINT('Ctrl Pts',(-49.6872205758336,51.6687293548682,
12.));
#152479=CARTESIAN_POINT('Ctrl Pts',(-49.6774754603245,51.6474600079622,
0.));
#152480=CARTESIAN_POINT('Ctrl Pts',(-49.6774754603245,51.6474600079622,
12.));
#152481=CARTESIAN_POINT('Ctrl Pts',(-49.6677275945967,51.626240144479,0.));
#152482=CARTESIAN_POINT('Ctrl Pts',(-49.6677275945967,51.626240144479,12.));
#152483=CARTESIAN_POINT('Ctrl Pts',(-49.6579770908037,51.6050698536496,
0.));
#152484=CARTESIAN_POINT('Ctrl Pts',(-49.6579770908037,51.6050698536496,
12.));
#152485=CARTESIAN_POINT('Ctrl Pts',(-49.6482240616593,51.5839492250181,
0.));
#152486=CARTESIAN_POINT('Ctrl Pts',(-49.6482240616593,51.5839492250181,
12.));
#152487=CARTESIAN_POINT('Ctrl Pts',(-49.6384686204413,51.5628783484525,
0.));
#152488=CARTESIAN_POINT('Ctrl Pts',(-49.6384686204413,51.5628783484525,
12.));
#152489=CARTESIAN_POINT('Ctrl Pts',(-49.6287108809966,51.5418573141484,
0.));
#152490=CARTESIAN_POINT('Ctrl Pts',(-49.6287108809966,51.5418573141484,
12.));
#152491=CARTESIAN_POINT('Ctrl Pts',(-49.6189509577452,51.5208862126315,
0.));
#152492=CARTESIAN_POINT('Ctrl Pts',(-49.6189509577452,51.5208862126315,
12.));
#152493=CARTESIAN_POINT('Ctrl Pts',(-49.6091889656866,51.4999651347522,
0.));
#152494=CARTESIAN_POINT('Ctrl Pts',(-49.6091889656866,51.4999651347522,
12.));
#152495=CARTESIAN_POINT('Ctrl Pts',(-49.5994250204031,51.4790941716888,
0.));
#152496=CARTESIAN_POINT('Ctrl Pts',(-49.5994250204031,51.4790941716888,
12.));
#152497=CARTESIAN_POINT('Ctrl Pts',(-49.5896592380654,51.4582734149583,
0.));
#152498=CARTESIAN_POINT('Ctrl Pts',(-49.5896592380654,51.4582734149583,
12.));
#152499=CARTESIAN_POINT('Ctrl Pts',(-49.5798917354366,51.4375029564197,
0.));
#152500=CARTESIAN_POINT('Ctrl Pts',(-49.5798917354366,51.4375029564197,
12.));
#152501=CARTESIAN_POINT('Ctrl Pts',(-49.5701226298769,51.4167828882756,
0.));
#152502=CARTESIAN_POINT('Ctrl Pts',(-49.5701226298769,51.4167828882756,
12.));
#152503=CARTESIAN_POINT('Ctrl Pts',(-49.5603520393496,51.396113303067,0.));
#152504=CARTESIAN_POINT('Ctrl Pts',(-49.5603520393496,51.396113303067,12.));
#152505=CARTESIAN_POINT('Ctrl Pts',(-49.550580082425,51.3754942936778,0.));
#152506=CARTESIAN_POINT('Ctrl Pts',(-49.550580082425,51.3754942936778,12.));
#152507=CARTESIAN_POINT('Ctrl Pts',(-49.5408068782859,51.3549259533458,
0.));
#152508=CARTESIAN_POINT('Ctrl Pts',(-49.5408068782859,51.3549259533458,
12.));
#152509=CARTESIAN_POINT('Ctrl Pts',(-49.5310325467332,51.3344083756657,
0.));
#152510=CARTESIAN_POINT('Ctrl Pts',(-49.5310325467332,51.3344083756657,
12.));
#152511=CARTESIAN_POINT('Ctrl Pts',(-49.5212572081908,51.313941654591,0.));
#152512=CARTESIAN_POINT('Ctrl Pts',(-49.5212572081908,51.313941654591,12.));
#152513=CARTESIAN_POINT('Ctrl Pts',(-49.5114809837122,51.2935258844289,
0.));
#152514=CARTESIAN_POINT('Ctrl Pts',(-49.5114809837122,51.2935258844289,
12.));
#152515=CARTESIAN_POINT('Ctrl Pts',(-49.5017039949852,51.2731611598475,
0.));
#152516=CARTESIAN_POINT('Ctrl Pts',(-49.5017039949852,51.2731611598475,
12.));
#152517=CARTESIAN_POINT('Ctrl Pts',(-49.4919263643362,51.2528475758846,
0.));
#152518=CARTESIAN_POINT('Ctrl Pts',(-49.4919263643362,51.2528475758846,
12.));
#152519=CARTESIAN_POINT('Ctrl Pts',(-49.4821482147356,51.2325852279506,
0.));
#152520=CARTESIAN_POINT('Ctrl Pts',(-49.4821482147356,51.2325852279506,
12.));
#152521=CARTESIAN_POINT('Ctrl Pts',(-49.4723696698021,51.2123742118287,
0.));
#152522=CARTESIAN_POINT('Ctrl Pts',(-49.4723696698021,51.2123742118287,
12.));
#152523=CARTESIAN_POINT('Ctrl Pts',(-49.4625908538074,51.1922146236686,
0.));
#152524=CARTESIAN_POINT('Ctrl Pts',(-49.4625908538074,51.1922146236686,
12.));
#152525=CARTESIAN_POINT('Ctrl Pts',(-49.4528118916832,51.1721065599972,
0.));
#152526=CARTESIAN_POINT('Ctrl Pts',(-49.4528118916832,51.1721065599972,
12.));
#152527=CARTESIAN_POINT('Ctrl Pts',(-49.4430329090287,51.1520501177291,
0.));
#152528=CARTESIAN_POINT('Ctrl Pts',(-49.4430329090287,51.1520501177291,
12.));
#152529=CARTESIAN_POINT('Ctrl Pts',(-49.4332540321178,51.1320453941702,
0.));
#152530=CARTESIAN_POINT('Ctrl Pts',(-49.4332540321178,51.1320453941702,
12.));
#152531=CARTESIAN_POINT('Ctrl Pts',(-49.423475387907,51.1120924870195,0.));
#152532=CARTESIAN_POINT('Ctrl Pts',(-49.423475387907,51.1120924870195,12.));
#152533=CARTESIAN_POINT('Ctrl Pts',(-49.4136971040428,51.0921914943662,
0.));
#152534=CARTESIAN_POINT('Ctrl Pts',(-49.4136971040428,51.0921914943662,
12.));
#152535=CARTESIAN_POINT('Ctrl Pts',(-49.4039193088634,51.0723425146985,
0.));
#152536=CARTESIAN_POINT('Ctrl Pts',(-49.4039193088634,51.0723425146985,
12.));
#152537=CARTESIAN_POINT('Ctrl Pts',(-49.3941421314013,51.052545646907,0.));
#152538=CARTESIAN_POINT('Ctrl Pts',(-49.3941421314013,51.052545646907,12.));
#152539=CARTESIAN_POINT('Ctrl Pts',(-49.3843657013852,51.0328009902858,
0.));
#152540=CARTESIAN_POINT('Ctrl Pts',(-49.3843657013852,51.0328009902858,
12.));
#152541=CARTESIAN_POINT('Ctrl Pts',(-49.3745901492432,51.0131086445272,
0.));
#152542=CARTESIAN_POINT('Ctrl Pts',(-49.3745901492432,51.0131086445272,
12.));
#152543=CARTESIAN_POINT('Ctrl Pts',(-49.3648156061058,50.9934687097188,
0.));
#152544=CARTESIAN_POINT('Ctrl Pts',(-49.3648156061058,50.9934687097188,
12.));
#152545=CARTESIAN_POINT('Ctrl Pts',(-49.355042203823,50.9738812863646,0.));
#152546=CARTESIAN_POINT('Ctrl Pts',(-49.355042203823,50.9738812863646,12.));
#152547=CARTESIAN_POINT('Ctrl Pts',(-49.345270074981,50.9543464753981,0.));
#152548=CARTESIAN_POINT('Ctrl Pts',(-49.345270074981,50.9543464753981,12.));
#152549=CARTESIAN_POINT('Ctrl Pts',(-49.3354993529158,50.9348643781924,
0.));
#152550=CARTESIAN_POINT('Ctrl Pts',(-49.3354993529158,50.9348643781924,
12.));
#152551=CARTESIAN_POINT('Ctrl Pts',(-49.3257301717335,50.9154350965666,
0.));
#152552=CARTESIAN_POINT('Ctrl Pts',(-49.3257301717335,50.9154350965666,
12.));
#152553=CARTESIAN_POINT('Ctrl Pts',(-49.3159626663109,50.8960587327848,
0.));
#152554=CARTESIAN_POINT('Ctrl Pts',(-49.3159626663109,50.8960587327848,
12.));
#152555=CARTESIAN_POINT('Ctrl Pts',(-49.3061969722781,50.8767353895492,
0.));
#152556=CARTESIAN_POINT('Ctrl Pts',(-49.3061969722781,50.8767353895492,
12.));
#152557=CARTESIAN_POINT('Ctrl Pts',(-49.2964332260039,50.8574651699873,
0.));
#152558=CARTESIAN_POINT('Ctrl Pts',(-49.2964332260039,50.8574651699873,
12.));
#152559=CARTESIAN_POINT('Ctrl Pts',(-49.2866715645838,50.8382481776403,
0.));
#152560=CARTESIAN_POINT('Ctrl Pts',(-49.2866715645838,50.8382481776403,
12.));
#152561=CARTESIAN_POINT('Ctrl Pts',(-49.2769121258164,50.819084516434,0.));
#152562=CARTESIAN_POINT('Ctrl Pts',(-49.2769121258164,50.819084516434,12.));
#152563=CARTESIAN_POINT('Ctrl Pts',(-49.2671550482435,50.7999742907131,
0.));
#152564=CARTESIAN_POINT('Ctrl Pts',(-49.2671550482435,50.7999742907131,
12.));
#152565=CARTESIAN_POINT('Ctrl Pts',(-49.2574004712134,50.7809176052966,
0.));
#152566=CARTESIAN_POINT('Ctrl Pts',(-49.2574004712134,50.7809176052966,
12.));
#152567=CARTESIAN_POINT('Ctrl Pts',(-49.2476485349373,50.7619145655207,
0.));
#152568=CARTESIAN_POINT('Ctrl Pts',(-49.2476485349373,50.7619145655207,
12.));
#152569=CARTESIAN_POINT('Ctrl Pts',(-49.2378993805471,50.7429652772805,
0.));
#152570=CARTESIAN_POINT('Ctrl Pts',(-49.2378993805471,50.7429652772805,
12.));
#152571=CARTESIAN_POINT('Ctrl Pts',(-49.228153150155,50.7240698470679,0.));
#152572=CARTESIAN_POINT('Ctrl Pts',(-49.228153150155,50.7240698470679,12.));
#152573=CARTESIAN_POINT('Ctrl Pts',(-49.2184099867461,50.7052283818922,
0.));
#152574=CARTESIAN_POINT('Ctrl Pts',(-49.2184099867461,50.7052283818922,
12.));
#152575=CARTESIAN_POINT('Ctrl Pts',(-49.2086700340614,50.6864409891895,
0.));
#152576=CARTESIAN_POINT('Ctrl Pts',(-49.2086700340614,50.6864409891895,
12.));
#152577=CARTESIAN_POINT('Ctrl Pts',(-49.1989334364996,50.6677077767432,
0.));
#152578=CARTESIAN_POINT('Ctrl Pts',(-49.1989334364996,50.6677077767432,
12.));
#152579=CARTESIAN_POINT('Ctrl Pts',(-49.189200338976,50.6490288525656,0.));
#152580=CARTESIAN_POINT('Ctrl Pts',(-49.189200338976,50.6490288525656,12.));
#152581=CARTESIAN_POINT('Ctrl Pts',(-49.1794708869099,50.6304043248821,
0.));
#152582=CARTESIAN_POINT('Ctrl Pts',(-49.1794708869099,50.6304043248821,
12.));
#152583=CARTESIAN_POINT('Ctrl Pts',(-49.1697452265494,50.6118343023957,
0.));
#152584=CARTESIAN_POINT('Ctrl Pts',(-49.1697452265494,50.6118343023957,
12.));
#152585=CARTESIAN_POINT('Ctrl Pts',(-49.1600235052621,50.5933188945168,
0.));
#152586=CARTESIAN_POINT('Ctrl Pts',(-49.1600235052621,50.5933188945168,
12.));
#152587=CARTESIAN_POINT('Ctrl Pts',(-49.1503058717821,50.5748582115565,
0.));
#152588=CARTESIAN_POINT('Ctrl Pts',(-49.1503058717821,50.5748582115565,
12.));
#152589=CARTESIAN_POINT('Ctrl Pts',(-49.1405924766144,50.556452365038,0.));
#152590=CARTESIAN_POINT('Ctrl Pts',(-49.1405924766144,50.556452365038,12.));
#152591=CARTESIAN_POINT('Ctrl Pts',(-49.1308834717615,50.5381014674791,
0.));
#152592=CARTESIAN_POINT('Ctrl Pts',(-49.1308834717615,50.5381014674791,
12.));
#152593=CARTESIAN_POINT('Ctrl Pts',(-49.1211790099795,50.5198056318088,
0.));
#152594=CARTESIAN_POINT('Ctrl Pts',(-49.1211790099795,50.5198056318088,
12.));
#152595=CARTESIAN_POINT('Ctrl Pts',(-49.1114792441571,50.501564970874,0.));
#152596=CARTESIAN_POINT('Ctrl Pts',(-49.1114792441571,50.501564970874,12.));
#152597=CARTESIAN_POINT('Ctrl Pts',(-49.1017843266803,50.4833795969318,
0.));
#152598=CARTESIAN_POINT('Ctrl Pts',(-49.1017843266803,50.4833795969318,
12.));
#152599=CARTESIAN_POINT('Ctrl Pts',(-49.0920944087008,50.4652496210607,
0.));
#152600=CARTESIAN_POINT('Ctrl Pts',(-49.0920944087008,50.4652496210607,
12.));
#152601=CARTESIAN_POINT('Ctrl Pts',(-49.0824096415371,50.4471751542751,
0.));
#152602=CARTESIAN_POINT('Ctrl Pts',(-49.0824096415371,50.4471751542751,
12.));
#152603=CARTESIAN_POINT('Ctrl Pts',(-49.0727301783494,50.4291563088547,
0.));
#152604=CARTESIAN_POINT('Ctrl Pts',(-49.0727301783494,50.4291563088547,
12.));
#152605=CARTESIAN_POINT('Ctrl Pts',(-49.0630561755075,50.4111931994257,
0.));
#152606=CARTESIAN_POINT('Ctrl Pts',(-49.0630561755075,50.4111931994257,
12.));
#152607=CARTESIAN_POINT('Ctrl Pts',(-49.0533877945744,50.3932859445252,
0.));
#152608=CARTESIAN_POINT('Ctrl Pts',(-49.0533877945744,50.3932859445252,
12.));
#152609=CARTESIAN_POINT('Ctrl Pts',(-49.0437252024832,50.3754346667353,
0.));
#152610=CARTESIAN_POINT('Ctrl Pts',(-49.0437252024832,50.3754346667353,
12.));
#152611=CARTESIAN_POINT('Ctrl Pts',(-49.0340685673982,50.3576394894108,
0.));
#152612=CARTESIAN_POINT('Ctrl Pts',(-49.0340685673982,50.3576394894108,
12.));
#152613=CARTESIAN_POINT('Ctrl Pts',(-49.024418055075,50.3399005337958,0.));
#152614=CARTESIAN_POINT('Ctrl Pts',(-49.024418055075,50.3399005337958,12.));
#152615=CARTESIAN_POINT('Ctrl Pts',(-49.0147738256942,50.3222179165119,
0.));
#152616=CARTESIAN_POINT('Ctrl Pts',(-49.0147738256942,50.3222179165119,
12.));
#152617=CARTESIAN_POINT('Ctrl Pts',(-49.0051360288044,50.3045917455424,
0.));
#152618=CARTESIAN_POINT('Ctrl Pts',(-49.0051360288044,50.3045917455424,
12.));
#152619=CARTESIAN_POINT('Ctrl Pts',(-48.9955048082081,50.2870221241054,
0.));
#152620=CARTESIAN_POINT('Ctrl Pts',(-48.9955048082081,50.2870221241054,
12.));
#152621=CARTESIAN_POINT('Ctrl Pts',(-48.9858803116689,50.2695091583511,
0.));
#152622=CARTESIAN_POINT('Ctrl Pts',(-48.9858803116689,50.2695091583511,
12.));
#152623=CARTESIAN_POINT('Ctrl Pts',(-48.9762626987227,50.252052963548,0.));
#152624=CARTESIAN_POINT('Ctrl Pts',(-48.9762626987227,50.252052963548,12.));
#152625=CARTESIAN_POINT('Ctrl Pts',(-48.9666521500911,50.234653671541,0.));
#152626=CARTESIAN_POINT('Ctrl Pts',(-48.9666521500911,50.234653671541,12.));
#152627=CARTESIAN_POINT('Ctrl Pts',(-48.9570488741167,50.2173114358325,
0.));
#152628=CARTESIAN_POINT('Ctrl Pts',(-48.9570488741167,50.2173114358325,
12.));
#152629=CARTESIAN_POINT('Ctrl Pts',(-48.9474530868733,50.2000264157797,
0.));
#152630=CARTESIAN_POINT('Ctrl Pts',(-48.9474530868733,50.2000264157797,
12.));
#152631=CARTESIAN_POINT('Ctrl Pts',(-48.9378649933055,50.1827987615602,
0.));
#152632=CARTESIAN_POINT('Ctrl Pts',(-48.9378649933055,50.1827987615602,
12.));
#152633=CARTESIAN_POINT('Ctrl Pts',(-48.9282847698294,50.1656286003997,
0.));
#152634=CARTESIAN_POINT('Ctrl Pts',(-48.9282847698294,50.1656286003997,
12.));
#152635=CARTESIAN_POINT('Ctrl Pts',(-48.9187125418099,50.1485160184657,
0.));
#152636=CARTESIAN_POINT('Ctrl Pts',(-48.9187125418099,50.1485160184657,
12.));
#152637=CARTESIAN_POINT('Ctrl Pts',(-48.90914838181,50.1314610602569,0.));
#152638=CARTESIAN_POINT('Ctrl Pts',(-48.90914838181,50.1314610602569,12.));
#152639=CARTESIAN_POINT('Ctrl Pts',(-48.9015035372055,50.1178632067084,
0.));
#152640=CARTESIAN_POINT('Ctrl Pts',(-48.9015035372055,50.1178632067084,
12.));
#152641=CARTESIAN_POINT('Ctrl Pts',(-48.895773555686,50.1076907555471,0.));
#152642=CARTESIAN_POINT('Ctrl Pts',(-48.895773555686,50.1076907555471,12.));
#152643=CARTESIAN_POINT('Ctrl Pts',(-48.8919551910366,50.1009206494272,
0.));
#152644=CARTESIAN_POINT('Ctrl Pts',(-48.8919551910366,50.1009206494272,
12.));
#152645=CARTESIAN_POINT('Ctrl Pts',(-48.8900464144686,50.0975384783635,
0.));
#152646=CARTESIAN_POINT('Ctrl Pts',(-48.8900464144686,50.0975384783635,
12.));
#152647=CARTESIAN_POINT('',(-48.8900464144686,50.0975384783635,12.));
#152648=CARTESIAN_POINT('Ctrl Pts',(-48.8900464144686,50.0975384783635,
12.));
#152649=CARTESIAN_POINT('Ctrl Pts',(-48.8919551910366,50.1009206494272,
12.));
#152650=CARTESIAN_POINT('Ctrl Pts',(-48.895773555686,50.1076907555471,12.));
#152651=CARTESIAN_POINT('Ctrl Pts',(-48.9015035372055,50.1178632067084,
12.));
#152652=CARTESIAN_POINT('Ctrl Pts',(-48.90914838181,50.1314610602569,12.));
#152653=CARTESIAN_POINT('Ctrl Pts',(-48.9187125418099,50.1485160184657,
12.));
#152654=CARTESIAN_POINT('Ctrl Pts',(-48.9282847698294,50.1656286003997,
12.));
#152655=CARTESIAN_POINT('Ctrl Pts',(-48.9378649933055,50.1827987615602,
12.));
#152656=CARTESIAN_POINT('Ctrl Pts',(-48.9474530868733,50.2000264157797,
12.));
#152657=CARTESIAN_POINT('Ctrl Pts',(-48.9570488741167,50.2173114358325,
12.));
#152658=CARTESIAN_POINT('Ctrl Pts',(-48.9666521500911,50.234653671541,12.));
#152659=CARTESIAN_POINT('Ctrl Pts',(-48.9762626987227,50.252052963548,12.));
#152660=CARTESIAN_POINT('Ctrl Pts',(-48.9858803116689,50.2695091583511,
12.));
#152661=CARTESIAN_POINT('Ctrl Pts',(-48.9955048082081,50.2870221241054,
12.));
#152662=CARTESIAN_POINT('Ctrl Pts',(-49.0051360288044,50.3045917455424,
12.));
#152663=CARTESIAN_POINT('Ctrl Pts',(-49.0147738256942,50.3222179165119,
12.));
#152664=CARTESIAN_POINT('Ctrl Pts',(-49.024418055075,50.3399005337958,12.));
#152665=CARTESIAN_POINT('Ctrl Pts',(-49.0340685673982,50.3576394894108,
12.));
#152666=CARTESIAN_POINT('Ctrl Pts',(-49.0437252024832,50.3754346667353,
12.));
#152667=CARTESIAN_POINT('Ctrl Pts',(-49.0533877945744,50.3932859445252,
12.));
#152668=CARTESIAN_POINT('Ctrl Pts',(-49.0630561755075,50.4111931994257,
12.));
#152669=CARTESIAN_POINT('Ctrl Pts',(-49.0727301783494,50.4291563088547,
12.));
#152670=CARTESIAN_POINT('Ctrl Pts',(-49.0824096415371,50.4471751542751,
12.));
#152671=CARTESIAN_POINT('Ctrl Pts',(-49.0920944087008,50.4652496210607,
12.));
#152672=CARTESIAN_POINT('Ctrl Pts',(-49.1017843266803,50.4833795969318,
12.));
#152673=CARTESIAN_POINT('Ctrl Pts',(-49.1114792441571,50.501564970874,12.));
#152674=CARTESIAN_POINT('Ctrl Pts',(-49.1211790099795,50.5198056318088,
12.));
#152675=CARTESIAN_POINT('Ctrl Pts',(-49.1308834717615,50.5381014674791,
12.));
#152676=CARTESIAN_POINT('Ctrl Pts',(-49.1405924766144,50.556452365038,12.));
#152677=CARTESIAN_POINT('Ctrl Pts',(-49.1503058717821,50.5748582115565,
12.));
#152678=CARTESIAN_POINT('Ctrl Pts',(-49.1600235052621,50.5933188945168,
12.));
#152679=CARTESIAN_POINT('Ctrl Pts',(-49.1697452265494,50.6118343023957,
12.));
#152680=CARTESIAN_POINT('Ctrl Pts',(-49.1794708869099,50.6304043248821,
12.));
#152681=CARTESIAN_POINT('Ctrl Pts',(-49.189200338976,50.6490288525656,12.));
#152682=CARTESIAN_POINT('Ctrl Pts',(-49.1989334364996,50.6677077767432,
12.));
#152683=CARTESIAN_POINT('Ctrl Pts',(-49.2086700340614,50.6864409891895,
12.));
#152684=CARTESIAN_POINT('Ctrl Pts',(-49.2184099867461,50.7052283818922,
12.));
#152685=CARTESIAN_POINT('Ctrl Pts',(-49.228153150155,50.7240698470679,12.));
#152686=CARTESIAN_POINT('Ctrl Pts',(-49.2378993805471,50.7429652772805,
12.));
#152687=CARTESIAN_POINT('Ctrl Pts',(-49.2476485349373,50.7619145655207,
12.));
#152688=CARTESIAN_POINT('Ctrl Pts',(-49.2574004712134,50.7809176052966,
12.));
#152689=CARTESIAN_POINT('Ctrl Pts',(-49.2671550482435,50.7999742907131,
12.));
#152690=CARTESIAN_POINT('Ctrl Pts',(-49.2769121258164,50.819084516434,12.));
#152691=CARTESIAN_POINT('Ctrl Pts',(-49.2866715645838,50.8382481776403,
12.));
#152692=CARTESIAN_POINT('Ctrl Pts',(-49.2964332260039,50.8574651699873,
12.));
#152693=CARTESIAN_POINT('Ctrl Pts',(-49.3061969722781,50.8767353895492,
12.));
#152694=CARTESIAN_POINT('Ctrl Pts',(-49.3159626663109,50.8960587327848,
12.));
#152695=CARTESIAN_POINT('Ctrl Pts',(-49.3257301717335,50.9154350965666,
12.));
#152696=CARTESIAN_POINT('Ctrl Pts',(-49.3354993529158,50.9348643781924,
12.));
#152697=CARTESIAN_POINT('Ctrl Pts',(-49.345270074981,50.9543464753981,12.));
#152698=CARTESIAN_POINT('Ctrl Pts',(-49.355042203823,50.9738812863646,12.));
#152699=CARTESIAN_POINT('Ctrl Pts',(-49.3648156061058,50.9934687097188,
12.));
#152700=CARTESIAN_POINT('Ctrl Pts',(-49.3745901492432,51.0131086445272,
12.));
#152701=CARTESIAN_POINT('Ctrl Pts',(-49.3843657013852,51.0328009902858,
12.));
#152702=CARTESIAN_POINT('Ctrl Pts',(-49.3941421314013,51.052545646907,12.));
#152703=CARTESIAN_POINT('Ctrl Pts',(-49.4039193088634,51.0723425146985,
12.));
#152704=CARTESIAN_POINT('Ctrl Pts',(-49.4136971040428,51.0921914943662,
12.));
#152705=CARTESIAN_POINT('Ctrl Pts',(-49.423475387907,51.1120924870195,12.));
#152706=CARTESIAN_POINT('Ctrl Pts',(-49.4332540321178,51.1320453941702,
12.));
#152707=CARTESIAN_POINT('Ctrl Pts',(-49.4430329090287,51.1520501177291,
12.));
#152708=CARTESIAN_POINT('Ctrl Pts',(-49.4528118916832,51.1721065599972,
12.));
#152709=CARTESIAN_POINT('Ctrl Pts',(-49.4625908538074,51.1922146236686,
12.));
#152710=CARTESIAN_POINT('Ctrl Pts',(-49.4723696698021,51.2123742118287,
12.));
#152711=CARTESIAN_POINT('Ctrl Pts',(-49.4821482147356,51.2325852279506,
12.));
#152712=CARTESIAN_POINT('Ctrl Pts',(-49.4919263643362,51.2528475758846,
12.));
#152713=CARTESIAN_POINT('Ctrl Pts',(-49.5017039949852,51.2731611598475,
12.));
#152714=CARTESIAN_POINT('Ctrl Pts',(-49.5114809837122,51.2935258844289,
12.));
#152715=CARTESIAN_POINT('Ctrl Pts',(-49.5212572081908,51.313941654591,12.));
#152716=CARTESIAN_POINT('Ctrl Pts',(-49.5310325467332,51.3344083756657,
12.));
#152717=CARTESIAN_POINT('Ctrl Pts',(-49.5408068782859,51.3549259533458,
12.));
#152718=CARTESIAN_POINT('Ctrl Pts',(-49.550580082425,51.3754942936778,12.));
#152719=CARTESIAN_POINT('Ctrl Pts',(-49.5603520393496,51.396113303067,12.));
#152720=CARTESIAN_POINT('Ctrl Pts',(-49.5701226298769,51.4167828882756,
12.));
#152721=CARTESIAN_POINT('Ctrl Pts',(-49.5798917354366,51.4375029564197,
12.));
#152722=CARTESIAN_POINT('Ctrl Pts',(-49.5896592380654,51.4582734149583,
12.));
#152723=CARTESIAN_POINT('Ctrl Pts',(-49.5994250204031,51.4790941716888,
12.));
#152724=CARTESIAN_POINT('Ctrl Pts',(-49.6091889656866,51.4999651347522,
12.));
#152725=CARTESIAN_POINT('Ctrl Pts',(-49.6189509577452,51.5208862126315,
12.));
#152726=CARTESIAN_POINT('Ctrl Pts',(-49.6287108809966,51.5418573141484,
12.));
#152727=CARTESIAN_POINT('Ctrl Pts',(-49.6384686204413,51.5628783484525,
12.));
#152728=CARTESIAN_POINT('Ctrl Pts',(-49.6482240616593,51.5839492250181,
12.));
#152729=CARTESIAN_POINT('Ctrl Pts',(-49.6579770908037,51.6050698536496,
12.));
#152730=CARTESIAN_POINT('Ctrl Pts',(-49.6677275945967,51.626240144479,12.));
#152731=CARTESIAN_POINT('Ctrl Pts',(-49.6774754603245,51.6474600079622,
12.));
#152732=CARTESIAN_POINT('Ctrl Pts',(-49.6872205758336,51.6687293548682,
12.));
#152733=CARTESIAN_POINT('Ctrl Pts',(-49.6969628295262,51.6900480962773,
12.));
#152734=CARTESIAN_POINT('Ctrl Pts',(-49.7067021103553,51.7114161435869,
12.));
#152735=CARTESIAN_POINT('Ctrl Pts',(-49.7164383078212,51.7328334085091,
12.));
#152736=CARTESIAN_POINT('Ctrl Pts',(-49.7261713119663,51.754299803067,12.));
#152737=CARTESIAN_POINT('Ctrl Pts',(-49.7359010133721,51.7758152395836,
12.));
#152738=CARTESIAN_POINT('Ctrl Pts',(-49.7456273031534,51.7973796306803,
12.));
#152739=CARTESIAN_POINT('Ctrl Pts',(-49.755350072955,51.8189928892828,12.));
#152740=CARTESIAN_POINT('Ctrl Pts',(-49.7650692149462,51.8406549286175,
12.));
#152741=CARTESIAN_POINT('Ctrl Pts',(-49.7747846218182,51.8623656622097,
12.));
#152742=CARTESIAN_POINT('Ctrl Pts',(-49.7844961867807,51.8841250038724,
12.));
#152743=CARTESIAN_POINT('Ctrl Pts',(-49.7942038035576,51.9059328677059,
12.));
#152744=CARTESIAN_POINT('Ctrl Pts',(-49.8039073663812,51.9277891681018,
12.));
#152745=CARTESIAN_POINT('Ctrl Pts',(-49.8136067699896,51.9496938197418,
12.));
#152746=CARTESIAN_POINT('Ctrl Pts',(-49.8233019096222,51.9716467375937,
12.));
#152747=CARTESIAN_POINT('Ctrl Pts',(-49.8329926810172,51.9936478369008,
12.));
#152748=CARTESIAN_POINT('Ctrl Pts',(-49.8426789804071,52.0156970331822,
12.));
#152749=CARTESIAN_POINT('Ctrl Pts',(-49.8523607045149,52.0377942422376,
12.));
#152750=CARTESIAN_POINT('Ctrl Pts',(-49.86203775055,52.0599393801452,12.));
#152751=CARTESIAN_POINT('Ctrl Pts',(-49.8717100162048,52.0821323632587,
12.));
#152752=CARTESIAN_POINT('Ctrl Pts',(-49.8813773996517,52.1043731081962,
12.));
#152753=CARTESIAN_POINT('Ctrl Pts',(-49.8910397995397,52.1266615318407,
12.));
#152754=CARTESIAN_POINT('Ctrl Pts',(-49.9006971149895,52.1489975513444,
12.));
#152755=CARTESIAN_POINT('Ctrl Pts',(-49.9103492455902,52.1713810841276,
12.));
#152756=CARTESIAN_POINT('Ctrl Pts',(-49.9199960913962,52.1938120478754,
12.));
#152757=CARTESIAN_POINT('Ctrl Pts',(-49.9296375529245,52.2162903605275,
12.));
#152758=CARTESIAN_POINT('Ctrl Pts',(-49.9392735311509,52.2388159402771,
12.));
#152759=CARTESIAN_POINT('Ctrl Pts',(-49.9489039275064,52.2613887055773,
12.));
#152760=CARTESIAN_POINT('Ctrl Pts',(-49.9585286438733,52.2840085751384,
12.));
#152761=CARTESIAN_POINT('Ctrl Pts',(-49.9681475825824,52.3066754679265,
12.));
#152762=CARTESIAN_POINT('Ctrl Pts',(-49.9777606464106,52.3293893031528,
12.));
#152763=CARTESIAN_POINT('Ctrl Pts',(-49.9873677385775,52.3521500002718,
12.));
#152764=CARTESIAN_POINT('Ctrl Pts',(-49.9969687627408,52.3749574789871,
12.));
#152765=CARTESIAN_POINT('Ctrl Pts',(-50.0065636229938,52.3978116592509,
12.));
#152766=CARTESIAN_POINT('Ctrl Pts',(-50.0161522238616,52.4207124612608,
12.));
#152767=CARTESIAN_POINT('Ctrl Pts',(-50.0257344703,52.4436598054515,12.));
#152768=CARTESIAN_POINT('Ctrl Pts',(-50.0353102676921,52.4666536124913,
12.));
#152769=CARTESIAN_POINT('Ctrl Pts',(-50.0448795218441,52.4896938032884,
12.));
#152770=CARTESIAN_POINT('Ctrl Pts',(-50.0544421389818,52.5127802989896,
12.));
#152771=CARTESIAN_POINT('Ctrl Pts',(-50.0639980257479,52.5359130209792,
12.));
#152772=CARTESIAN_POINT('Ctrl Pts',(-50.0735470892007,52.5590918908702,
12.));
#152773=CARTESIAN_POINT('Ctrl Pts',(-50.0830892368107,52.5823168304994,
12.));
#152774=CARTESIAN_POINT('Ctrl Pts',(-50.0926243764578,52.6055877619348,
12.));
#152775=CARTESIAN_POINT('Ctrl Pts',(-50.1021524164264,52.6289046074746,
12.));
#152776=CARTESIAN_POINT('Ctrl Pts',(-50.111673265404,52.652267289646,12.));
#152777=CARTESIAN_POINT('Ctrl Pts',(-50.1211868324781,52.6756757311978,
12.));
#152778=CARTESIAN_POINT('Ctrl Pts',(-50.1306930271345,52.699129855093,12.));
#152779=CARTESIAN_POINT('Ctrl Pts',(-50.1401917592537,52.7226295845161,
12.));
#152780=CARTESIAN_POINT('Ctrl Pts',(-50.1496829391073,52.7461748428738,
12.));
#152781=CARTESIAN_POINT('Ctrl Pts',(-50.1591664773561,52.769765553794,12.));
#152782=CARTESIAN_POINT('Ctrl Pts',(-50.1686422850488,52.7934016411205,
12.));
#152783=CARTESIAN_POINT('Ctrl Pts',(-50.1781102736205,52.8170830289044,
12.));
#152784=CARTESIAN_POINT('Ctrl Pts',(-50.1875703548884,52.8408096414093,
12.));
#152785=CARTESIAN_POINT('Ctrl Pts',(-50.1970224410471,52.8645814031133,
12.));
#152786=CARTESIAN_POINT('Ctrl Pts',(-50.2064664446663,52.8883982387068,
12.));
#152787=CARTESIAN_POINT('Ctrl Pts',(-50.2159022786879,52.9122600730884,
12.));
#152788=CARTESIAN_POINT('Ctrl Pts',(-50.2253298564241,52.9361668313542,
12.));
#152789=CARTESIAN_POINT('Ctrl Pts',(-50.2347490915555,52.9601184388027,
12.));
#152790=CARTESIAN_POINT('Ctrl Pts',(-50.2441598981286,52.9841148209402,
12.));
#152791=CARTESIAN_POINT('Ctrl Pts',(-50.2535621905552,53.0081559034801,
12.));
#152792=CARTESIAN_POINT('Ctrl Pts',(-50.2629558836111,53.0322416123406,
12.));
#152793=CARTESIAN_POINT('Ctrl Pts',(-50.2723408924373,53.0563718736366,
12.));
#152794=CARTESIAN_POINT('Ctrl Pts',(-50.2817171325358,53.0805466136797,
12.));
#152795=CARTESIAN_POINT('Ctrl Pts',(-50.2910845197619,53.1047657589812,
12.));
#152796=CARTESIAN_POINT('Ctrl Pts',(-50.300442970319,53.1290292362485,12.));
#152797=CARTESIAN_POINT('Ctrl Pts',(-50.3097924007534,53.1533369723818,
12.));
#152798=CARTESIAN_POINT('Ctrl Pts',(-50.3191327279493,53.1776888944616,
12.));
#152799=CARTESIAN_POINT('Ctrl Pts',(-50.3284638691278,53.2020849297471,
12.));
#152800=CARTESIAN_POINT('Ctrl Pts',(-50.3377857418514,53.2265250056887,
12.));
#152801=CARTESIAN_POINT('Ctrl Pts',(-50.3470982640289,53.2510090499336,
12.));
#152802=CARTESIAN_POINT('Ctrl Pts',(-50.3564013539199,53.2755369903293,
12.));
#152803=CARTESIAN_POINT('Ctrl Pts',(-50.365694930143,53.300108754923,12.));
#152804=CARTESIAN_POINT('Ctrl Pts',(-50.3749789116786,53.3247242719587,
12.));
#152805=CARTESIAN_POINT('Ctrl Pts',(-50.384253217846,53.3493834698697,12.));
#152806=CARTESIAN_POINT('Ctrl Pts',(-50.3935177682837,53.3740862772681,
12.));
#152807=CARTESIAN_POINT('Ctrl Pts',(-50.4027724829297,53.398832622931,12.));
#152808=CARTESIAN_POINT('Ctrl Pts',(-50.4120172820047,53.4236224357838,
12.));
#152809=CARTESIAN_POINT('Ctrl Pts',(-50.4212520859914,53.4484556448776,
12.));
#152810=CARTESIAN_POINT('Ctrl Pts',(-50.4304768156667,53.4733321794188,
12.));
#152811=CARTESIAN_POINT('Ctrl Pts',(-50.4396913921382,53.4982519688024,
12.));
#152812=CARTESIAN_POINT('Ctrl Pts',(-50.4488957368839,53.5232149426413,
12.));
#152813=CARTESIAN_POINT('Ctrl Pts',(-50.4580897717838,53.5482210307868,
12.));
#152814=CARTESIAN_POINT('Ctrl Pts',(-50.4672734191756,53.5732701633609,
12.));
#152815=CARTESIAN_POINT('Ctrl Pts',(-50.4764466018071,53.5983622707238,
12.));
#152816=CARTESIAN_POINT('Ctrl Pts',(-50.4856092427314,53.623497283406,12.));
#152817=CARTESIAN_POINT('Ctrl Pts',(-50.4947612652148,53.6486751320436,
12.));
#152818=CARTESIAN_POINT('Ctrl Pts',(-50.503902592653,53.6738957473158,12.));
#152819=CARTESIAN_POINT('Ctrl Pts',(-50.513033148456,53.6991590598548,12.));
#152820=CARTESIAN_POINT('Ctrl Pts',(-50.522152856042,53.7244650002374,12.));
#152821=CARTESIAN_POINT('Ctrl Pts',(-50.5312616390779,53.7498134991703,
12.));
#152822=CARTESIAN_POINT('Ctrl Pts',(-50.5403594216698,53.7752044876304,
12.));
#152823=CARTESIAN_POINT('Ctrl Pts',(-50.5494461285761,53.8006378970197,
12.));
#152824=CARTESIAN_POINT('Ctrl Pts',(-50.5585216854091,53.8261136593075,
12.));
#152825=CARTESIAN_POINT('Ctrl Pts',(-50.5675860188538,53.8516317071804,
12.));
#152826=CARTESIAN_POINT('Ctrl Pts',(-50.5766390561884,53.8771919737032,
12.));
#152827=CARTESIAN_POINT('Ctrl Pts',(-50.5856807248151,53.9027943919836,
12.));
#152828=CARTESIAN_POINT('Ctrl Pts',(-50.5947109517483,53.9284388948004,
12.));
#152829=CARTESIAN_POINT('Ctrl Pts',(-50.603729663214,53.9541254143119,12.));
#152830=CARTESIAN_POINT('Ctrl Pts',(-50.6127367839711,53.979853881553,12.));
#152831=CARTESIAN_POINT('Ctrl Pts',(-50.6217322378648,54.0056242268399,
12.));
#152832=CARTESIAN_POINT('Ctrl Pts',(-50.6307159490553,54.0314363806708,
12.));
#152833=CARTESIAN_POINT('Ctrl Pts',(-50.6396878430939,54.0572902745076,
12.));
#152834=CARTESIAN_POINT('Ctrl Pts',(-50.6486478479465,54.0831858415189,
12.));
#152835=CARTESIAN_POINT('Ctrl Pts',(-50.6575958953221,54.1091230175367,
12.));
#152836=CARTESIAN_POINT('Ctrl Pts',(-50.6665319209869,54.1351017412804,
12.));
#152837=CARTESIAN_POINT('Ctrl Pts',(-50.6741814675486,54.1574061042042,
12.));
#152838=CARTESIAN_POINT('Ctrl Pts',(-50.6800396668778,54.1745287898795,
12.));
#152839=CARTESIAN_POINT('Ctrl Pts',(-50.684111886193,54.1864514382194,12.));
#152840=CARTESIAN_POINT('Ctrl Pts',(-50.6864016965743,54.1931619277621,
12.));
#152841=CARTESIAN_POINT('Ctrl Pts',(-50.6869108458849,54.194654350037,12.));
#152842=CARTESIAN_POINT('',(-48.8900464144686,50.0975384783635,0.));
#152843=CARTESIAN_POINT('',(-48.8900464144686,50.0975384783634,0.));
#152844=CARTESIAN_POINT('Ctrl Pts',(-50.6869108458849,54.1946543500369,
0.));
#152845=CARTESIAN_POINT('Ctrl Pts',(-50.6864016965743,54.1931619277621,
0.));
#152846=CARTESIAN_POINT('Ctrl Pts',(-50.684111886193,54.1864514382194,0.));
#152847=CARTESIAN_POINT('Ctrl Pts',(-50.6800396668778,54.1745287898795,
0.));
#152848=CARTESIAN_POINT('Ctrl Pts',(-50.6741814675486,54.1574061042042,
0.));
#152849=CARTESIAN_POINT('Ctrl Pts',(-50.6665319209869,54.1351017412804,
0.));
#152850=CARTESIAN_POINT('Ctrl Pts',(-50.6575958953221,54.1091230175367,
0.));
#152851=CARTESIAN_POINT('Ctrl Pts',(-50.6486478479465,54.0831858415189,
0.));
#152852=CARTESIAN_POINT('Ctrl Pts',(-50.6396878430939,54.0572902745076,
0.));
#152853=CARTESIAN_POINT('Ctrl Pts',(-50.6307159490553,54.0314363806708,
0.));
#152854=CARTESIAN_POINT('Ctrl Pts',(-50.6217322378648,54.0056242268399,
0.));
#152855=CARTESIAN_POINT('Ctrl Pts',(-50.6127367839711,53.979853881553,0.));
#152856=CARTESIAN_POINT('Ctrl Pts',(-50.603729663214,53.9541254143119,0.));
#152857=CARTESIAN_POINT('Ctrl Pts',(-50.5947109517483,53.9284388948004,
0.));
#152858=CARTESIAN_POINT('Ctrl Pts',(-50.5856807248151,53.9027943919836,
0.));
#152859=CARTESIAN_POINT('Ctrl Pts',(-50.5766390561884,53.8771919737032,
0.));
#152860=CARTESIAN_POINT('Ctrl Pts',(-50.5675860188538,53.8516317071804,
0.));
#152861=CARTESIAN_POINT('Ctrl Pts',(-50.5585216854091,53.8261136593075,
0.));
#152862=CARTESIAN_POINT('Ctrl Pts',(-50.5494461285761,53.8006378970197,
0.));
#152863=CARTESIAN_POINT('Ctrl Pts',(-50.5403594216698,53.7752044876304,
0.));
#152864=CARTESIAN_POINT('Ctrl Pts',(-50.5312616390779,53.7498134991703,
0.));
#152865=CARTESIAN_POINT('Ctrl Pts',(-50.522152856042,53.7244650002374,0.));
#152866=CARTESIAN_POINT('Ctrl Pts',(-50.513033148456,53.6991590598548,0.));
#152867=CARTESIAN_POINT('Ctrl Pts',(-50.503902592653,53.6738957473158,0.));
#152868=CARTESIAN_POINT('Ctrl Pts',(-50.4947612652148,53.6486751320436,
0.));
#152869=CARTESIAN_POINT('Ctrl Pts',(-50.4856092427314,53.623497283406,0.));
#152870=CARTESIAN_POINT('Ctrl Pts',(-50.4764466018071,53.5983622707238,
0.));
#152871=CARTESIAN_POINT('Ctrl Pts',(-50.4672734191756,53.5732701633609,
0.));
#152872=CARTESIAN_POINT('Ctrl Pts',(-50.4580897717838,53.5482210307868,
0.));
#152873=CARTESIAN_POINT('Ctrl Pts',(-50.4488957368839,53.5232149426413,
0.));
#152874=CARTESIAN_POINT('Ctrl Pts',(-50.4396913921382,53.4982519688024,
0.));
#152875=CARTESIAN_POINT('Ctrl Pts',(-50.4304768156667,53.4733321794188,
0.));
#152876=CARTESIAN_POINT('Ctrl Pts',(-50.4212520859914,53.4484556448776,
0.));
#152877=CARTESIAN_POINT('Ctrl Pts',(-50.4120172820047,53.4236224357838,
0.));
#152878=CARTESIAN_POINT('Ctrl Pts',(-50.4027724829297,53.398832622931,0.));
#152879=CARTESIAN_POINT('Ctrl Pts',(-50.3935177682837,53.3740862772681,
0.));
#152880=CARTESIAN_POINT('Ctrl Pts',(-50.384253217846,53.3493834698697,0.));
#152881=CARTESIAN_POINT('Ctrl Pts',(-50.3749789116786,53.3247242719587,
0.));
#152882=CARTESIAN_POINT('Ctrl Pts',(-50.365694930143,53.300108754923,0.));
#152883=CARTESIAN_POINT('Ctrl Pts',(-50.3564013539199,53.2755369903293,
0.));
#152884=CARTESIAN_POINT('Ctrl Pts',(-50.3470982640289,53.2510090499336,
0.));
#152885=CARTESIAN_POINT('Ctrl Pts',(-50.3377857418514,53.2265250056887,
0.));
#152886=CARTESIAN_POINT('Ctrl Pts',(-50.3284638691278,53.2020849297471,
0.));
#152887=CARTESIAN_POINT('Ctrl Pts',(-50.3191327279493,53.1776888944616,
0.));
#152888=CARTESIAN_POINT('Ctrl Pts',(-50.3097924007534,53.1533369723818,
0.));
#152889=CARTESIAN_POINT('Ctrl Pts',(-50.300442970319,53.1290292362485,0.));
#152890=CARTESIAN_POINT('Ctrl Pts',(-50.2910845197619,53.1047657589812,
0.));
#152891=CARTESIAN_POINT('Ctrl Pts',(-50.2817171325358,53.0805466136797,
0.));
#152892=CARTESIAN_POINT('Ctrl Pts',(-50.2723408924373,53.0563718736366,
0.));
#152893=CARTESIAN_POINT('Ctrl Pts',(-50.2629558836111,53.0322416123406,
0.));
#152894=CARTESIAN_POINT('Ctrl Pts',(-50.2535621905552,53.0081559034801,
0.));
#152895=CARTESIAN_POINT('Ctrl Pts',(-50.2441598981286,52.9841148209402,
0.));
#152896=CARTESIAN_POINT('Ctrl Pts',(-50.2347490915555,52.9601184388027,
0.));
#152897=CARTESIAN_POINT('Ctrl Pts',(-50.2253298564241,52.9361668313542,
0.));
#152898=CARTESIAN_POINT('Ctrl Pts',(-50.2159022786879,52.9122600730884,
0.));
#152899=CARTESIAN_POINT('Ctrl Pts',(-50.2064664446663,52.8883982387068,
0.));
#152900=CARTESIAN_POINT('Ctrl Pts',(-50.1970224410471,52.8645814031133,
0.));
#152901=CARTESIAN_POINT('Ctrl Pts',(-50.1875703548884,52.8408096414093,
0.));
#152902=CARTESIAN_POINT('Ctrl Pts',(-50.1781102736205,52.8170830289044,
0.));
#152903=CARTESIAN_POINT('Ctrl Pts',(-50.1686422850488,52.7934016411205,
0.));
#152904=CARTESIAN_POINT('Ctrl Pts',(-50.1591664773561,52.769765553794,0.));
#152905=CARTESIAN_POINT('Ctrl Pts',(-50.1496829391073,52.7461748428738,
0.));
#152906=CARTESIAN_POINT('Ctrl Pts',(-50.1401917592537,52.7226295845161,
0.));
#152907=CARTESIAN_POINT('Ctrl Pts',(-50.1306930271345,52.699129855093,0.));
#152908=CARTESIAN_POINT('Ctrl Pts',(-50.1211868324781,52.6756757311978,
0.));
#152909=CARTESIAN_POINT('Ctrl Pts',(-50.111673265404,52.652267289646,0.));
#152910=CARTESIAN_POINT('Ctrl Pts',(-50.1021524164264,52.6289046074746,
0.));
#152911=CARTESIAN_POINT('Ctrl Pts',(-50.0926243764578,52.6055877619348,
0.));
#152912=CARTESIAN_POINT('Ctrl Pts',(-50.0830892368107,52.5823168304994,
0.));
#152913=CARTESIAN_POINT('Ctrl Pts',(-50.0735470892007,52.5590918908702,
0.));
#152914=CARTESIAN_POINT('Ctrl Pts',(-50.0639980257479,52.5359130209792,
0.));
#152915=CARTESIAN_POINT('Ctrl Pts',(-50.0544421389818,52.5127802989896,
0.));
#152916=CARTESIAN_POINT('Ctrl Pts',(-50.0448795218441,52.4896938032884,
0.));
#152917=CARTESIAN_POINT('Ctrl Pts',(-50.0353102676921,52.4666536124913,
0.));
#152918=CARTESIAN_POINT('Ctrl Pts',(-50.0257344703,52.4436598054515,0.));
#152919=CARTESIAN_POINT('Ctrl Pts',(-50.0161522238616,52.4207124612608,
0.));
#152920=CARTESIAN_POINT('Ctrl Pts',(-50.0065636229938,52.3978116592509,
0.));
#152921=CARTESIAN_POINT('Ctrl Pts',(-49.9969687627408,52.3749574789871,
0.));
#152922=CARTESIAN_POINT('Ctrl Pts',(-49.9873677385775,52.3521500002718,
0.));
#152923=CARTESIAN_POINT('Ctrl Pts',(-49.9777606464106,52.3293893031528,
0.));
#152924=CARTESIAN_POINT('Ctrl Pts',(-49.9681475825824,52.3066754679265,
0.));
#152925=CARTESIAN_POINT('Ctrl Pts',(-49.9585286438733,52.2840085751384,
0.));
#152926=CARTESIAN_POINT('Ctrl Pts',(-49.9489039275064,52.2613887055773,
0.));
#152927=CARTESIAN_POINT('Ctrl Pts',(-49.9392735311509,52.2388159402771,
0.));
#152928=CARTESIAN_POINT('Ctrl Pts',(-49.9296375529245,52.2162903605275,
0.));
#152929=CARTESIAN_POINT('Ctrl Pts',(-49.9199960913962,52.1938120478754,
0.));
#152930=CARTESIAN_POINT('Ctrl Pts',(-49.9103492455902,52.1713810841276,
0.));
#152931=CARTESIAN_POINT('Ctrl Pts',(-49.9006971149895,52.1489975513444,
0.));
#152932=CARTESIAN_POINT('Ctrl Pts',(-49.8910397995397,52.1266615318407,
0.));
#152933=CARTESIAN_POINT('Ctrl Pts',(-49.8813773996517,52.1043731081962,
0.));
#152934=CARTESIAN_POINT('Ctrl Pts',(-49.8717100162048,52.0821323632587,
0.));
#152935=CARTESIAN_POINT('Ctrl Pts',(-49.86203775055,52.0599393801452,0.));
#152936=CARTESIAN_POINT('Ctrl Pts',(-49.8523607045149,52.0377942422376,
0.));
#152937=CARTESIAN_POINT('Ctrl Pts',(-49.8426789804071,52.0156970331822,
0.));
#152938=CARTESIAN_POINT('Ctrl Pts',(-49.8329926810172,51.9936478369008,
0.));
#152939=CARTESIAN_POINT('Ctrl Pts',(-49.8233019096222,51.9716467375937,
0.));
#152940=CARTESIAN_POINT('Ctrl Pts',(-49.8136067699896,51.9496938197418,
0.));
#152941=CARTESIAN_POINT('Ctrl Pts',(-49.8039073663812,51.9277891681018,
0.));
#152942=CARTESIAN_POINT('Ctrl Pts',(-49.7942038035576,51.9059328677059,
0.));
#152943=CARTESIAN_POINT('Ctrl Pts',(-49.7844961867807,51.8841250038724,
0.));
#152944=CARTESIAN_POINT('Ctrl Pts',(-49.7747846218182,51.8623656622097,
0.));
#152945=CARTESIAN_POINT('Ctrl Pts',(-49.7650692149462,51.8406549286175,
0.));
#152946=CARTESIAN_POINT('Ctrl Pts',(-49.755350072955,51.8189928892828,0.));
#152947=CARTESIAN_POINT('Ctrl Pts',(-49.7456273031534,51.7973796306803,
0.));
#152948=CARTESIAN_POINT('Ctrl Pts',(-49.7359010133721,51.7758152395836,
0.));
#152949=CARTESIAN_POINT('Ctrl Pts',(-49.7261713119663,51.754299803067,0.));
#152950=CARTESIAN_POINT('Ctrl Pts',(-49.7164383078212,51.7328334085091,
0.));
#152951=CARTESIAN_POINT('Ctrl Pts',(-49.7067021103553,51.7114161435869,
0.));
#152952=CARTESIAN_POINT('Ctrl Pts',(-49.6969628295262,51.6900480962773,
0.));
#152953=CARTESIAN_POINT('Ctrl Pts',(-49.6872205758336,51.6687293548682,
0.));
#152954=CARTESIAN_POINT('Ctrl Pts',(-49.6774754603245,51.6474600079622,
0.));
#152955=CARTESIAN_POINT('Ctrl Pts',(-49.6677275945967,51.626240144479,0.));
#152956=CARTESIAN_POINT('Ctrl Pts',(-49.6579770908037,51.6050698536496,
0.));
#152957=CARTESIAN_POINT('Ctrl Pts',(-49.6482240616593,51.5839492250181,
0.));
#152958=CARTESIAN_POINT('Ctrl Pts',(-49.6384686204413,51.5628783484525,
0.));
#152959=CARTESIAN_POINT('Ctrl Pts',(-49.6287108809966,51.5418573141484,
0.));
#152960=CARTESIAN_POINT('Ctrl Pts',(-49.6189509577452,51.5208862126315,
0.));
#152961=CARTESIAN_POINT('Ctrl Pts',(-49.6091889656866,51.4999651347522,
0.));
#152962=CARTESIAN_POINT('Ctrl Pts',(-49.5994250204031,51.4790941716888,
0.));
#152963=CARTESIAN_POINT('Ctrl Pts',(-49.5896592380654,51.4582734149583,
0.));
#152964=CARTESIAN_POINT('Ctrl Pts',(-49.5798917354366,51.4375029564197,
0.));
#152965=CARTESIAN_POINT('Ctrl Pts',(-49.5701226298769,51.4167828882756,
0.));
#152966=CARTESIAN_POINT('Ctrl Pts',(-49.5603520393496,51.396113303067,0.));
#152967=CARTESIAN_POINT('Ctrl Pts',(-49.550580082425,51.3754942936778,0.));
#152968=CARTESIAN_POINT('Ctrl Pts',(-49.5408068782859,51.3549259533458,
0.));
#152969=CARTESIAN_POINT('Ctrl Pts',(-49.5310325467332,51.3344083756657,
0.));
#152970=CARTESIAN_POINT('Ctrl Pts',(-49.5212572081908,51.313941654591,0.));
#152971=CARTESIAN_POINT('Ctrl Pts',(-49.5114809837122,51.2935258844289,
0.));
#152972=CARTESIAN_POINT('Ctrl Pts',(-49.5017039949852,51.2731611598475,
0.));
#152973=CARTESIAN_POINT('Ctrl Pts',(-49.4919263643362,51.2528475758846,
0.));
#152974=CARTESIAN_POINT('Ctrl Pts',(-49.4821482147356,51.2325852279506,
0.));
#152975=CARTESIAN_POINT('Ctrl Pts',(-49.4723696698021,51.2123742118287,
0.));
#152976=CARTESIAN_POINT('Ctrl Pts',(-49.4625908538074,51.1922146236686,
0.));
#152977=CARTESIAN_POINT('Ctrl Pts',(-49.4528118916832,51.1721065599972,
0.));
#152978=CARTESIAN_POINT('Ctrl Pts',(-49.4430329090287,51.1520501177291,
0.));
#152979=CARTESIAN_POINT('Ctrl Pts',(-49.4332540321178,51.1320453941702,
0.));
#152980=CARTESIAN_POINT('Ctrl Pts',(-49.423475387907,51.1120924870195,0.));
#152981=CARTESIAN_POINT('Ctrl Pts',(-49.4136971040428,51.0921914943662,
0.));
#152982=CARTESIAN_POINT('Ctrl Pts',(-49.4039193088634,51.0723425146985,
0.));
#152983=CARTESIAN_POINT('Ctrl Pts',(-49.3941421314013,51.052545646907,0.));
#152984=CARTESIAN_POINT('Ctrl Pts',(-49.3843657013852,51.0328009902858,
0.));
#152985=CARTESIAN_POINT('Ctrl Pts',(-49.3745901492432,51.0131086445272,
0.));
#152986=CARTESIAN_POINT('Ctrl Pts',(-49.3648156061058,50.9934687097188,
0.));
#152987=CARTESIAN_POINT('Ctrl Pts',(-49.355042203823,50.9738812863646,0.));
#152988=CARTESIAN_POINT('Ctrl Pts',(-49.345270074981,50.9543464753981,0.));
#152989=CARTESIAN_POINT('Ctrl Pts',(-49.3354993529158,50.9348643781924,
0.));
#152990=CARTESIAN_POINT('Ctrl Pts',(-49.3257301717335,50.9154350965666,
0.));
#152991=CARTESIAN_POINT('Ctrl Pts',(-49.3159626663109,50.8960587327848,
0.));
#152992=CARTESIAN_POINT('Ctrl Pts',(-49.3061969722781,50.8767353895492,
0.));
#152993=CARTESIAN_POINT('Ctrl Pts',(-49.2964332260039,50.8574651699873,
0.));
#152994=CARTESIAN_POINT('Ctrl Pts',(-49.2866715645838,50.8382481776403,
0.));
#152995=CARTESIAN_POINT('Ctrl Pts',(-49.2769121258164,50.819084516434,0.));
#152996=CARTESIAN_POINT('Ctrl Pts',(-49.2671550482435,50.7999742907131,
0.));
#152997=CARTESIAN_POINT('Ctrl Pts',(-49.2574004712134,50.7809176052966,
0.));
#152998=CARTESIAN_POINT('Ctrl Pts',(-49.2476485349373,50.7619145655207,
0.));
#152999=CARTESIAN_POINT('Ctrl Pts',(-49.2378993805471,50.7429652772805,
0.));
#153000=CARTESIAN_POINT('Ctrl Pts',(-49.228153150155,50.7240698470679,0.));
#153001=CARTESIAN_POINT('Ctrl Pts',(-49.2184099867461,50.7052283818922,
0.));
#153002=CARTESIAN_POINT('Ctrl Pts',(-49.2086700340614,50.6864409891895,
0.));
#153003=CARTESIAN_POINT('Ctrl Pts',(-49.1989334364996,50.6677077767432,
0.));
#153004=CARTESIAN_POINT('Ctrl Pts',(-49.189200338976,50.6490288525656,0.));
#153005=CARTESIAN_POINT('Ctrl Pts',(-49.1794708869099,50.6304043248821,
0.));
#153006=CARTESIAN_POINT('Ctrl Pts',(-49.1697452265494,50.6118343023957,
0.));
#153007=CARTESIAN_POINT('Ctrl Pts',(-49.1600235052621,50.5933188945168,
0.));
#153008=CARTESIAN_POINT('Ctrl Pts',(-49.1503058717821,50.5748582115565,
0.));
#153009=CARTESIAN_POINT('Ctrl Pts',(-49.1405924766144,50.556452365038,0.));
#153010=CARTESIAN_POINT('Ctrl Pts',(-49.1308834717615,50.5381014674791,
0.));
#153011=CARTESIAN_POINT('Ctrl Pts',(-49.1211790099795,50.5198056318088,
0.));
#153012=CARTESIAN_POINT('Ctrl Pts',(-49.1114792441571,50.501564970874,0.));
#153013=CARTESIAN_POINT('Ctrl Pts',(-49.1017843266803,50.4833795969318,
0.));
#153014=CARTESIAN_POINT('Ctrl Pts',(-49.0920944087008,50.4652496210607,
0.));
#153015=CARTESIAN_POINT('Ctrl Pts',(-49.0824096415371,50.4471751542751,
0.));
#153016=CARTESIAN_POINT('Ctrl Pts',(-49.0727301783494,50.4291563088547,
0.));
#153017=CARTESIAN_POINT('Ctrl Pts',(-49.0630561755075,50.4111931994257,
0.));
#153018=CARTESIAN_POINT('Ctrl Pts',(-49.0533877945744,50.3932859445252,
0.));
#153019=CARTESIAN_POINT('Ctrl Pts',(-49.0437252024832,50.3754346667353,
0.));
#153020=CARTESIAN_POINT('Ctrl Pts',(-49.0340685673982,50.3576394894108,
0.));
#153021=CARTESIAN_POINT('Ctrl Pts',(-49.024418055075,50.3399005337958,0.));
#153022=CARTESIAN_POINT('Ctrl Pts',(-49.0147738256942,50.3222179165119,
0.));
#153023=CARTESIAN_POINT('Ctrl Pts',(-49.0051360288044,50.3045917455424,
0.));
#153024=CARTESIAN_POINT('Ctrl Pts',(-48.9955048082081,50.2870221241054,
0.));
#153025=CARTESIAN_POINT('Ctrl Pts',(-48.9858803116689,50.2695091583511,
0.));
#153026=CARTESIAN_POINT('Ctrl Pts',(-48.9762626987227,50.252052963548,0.));
#153027=CARTESIAN_POINT('Ctrl Pts',(-48.9666521500911,50.234653671541,0.));
#153028=CARTESIAN_POINT('Ctrl Pts',(-48.9570488741167,50.2173114358325,
0.));
#153029=CARTESIAN_POINT('Ctrl Pts',(-48.9474530868733,50.2000264157797,
0.));
#153030=CARTESIAN_POINT('Ctrl Pts',(-48.9378649933055,50.1827987615602,
0.));
#153031=CARTESIAN_POINT('Ctrl Pts',(-48.9282847698294,50.1656286003997,
0.));
#153032=CARTESIAN_POINT('Ctrl Pts',(-48.9187125418099,50.1485160184657,
0.));
#153033=CARTESIAN_POINT('Ctrl Pts',(-48.90914838181,50.1314610602569,0.));
#153034=CARTESIAN_POINT('Ctrl Pts',(-48.9015035372055,50.1178632067084,
0.));
#153035=CARTESIAN_POINT('Ctrl Pts',(-48.895773555686,50.1076907555471,0.));
#153036=CARTESIAN_POINT('Ctrl Pts',(-48.8919551910366,50.1009206494272,
0.));
#153037=CARTESIAN_POINT('Ctrl Pts',(-48.8900464144686,50.0975384783635,
0.));
#153038=CARTESIAN_POINT('Ctrl Pts',(-45.8467972562798,58.722407829904,0.));
#153039=CARTESIAN_POINT('Ctrl Pts',(-45.8467972562798,58.722407829904,12.));
#153040=CARTESIAN_POINT('Ctrl Pts',(-45.8455162977427,58.7169606500268,
0.));
#153041=CARTESIAN_POINT('Ctrl Pts',(-45.8455162977427,58.7169606500268,
12.));
#153042=CARTESIAN_POINT('Ctrl Pts',(-45.8429527488786,58.7060702401686,
0.));
#153043=CARTESIAN_POINT('Ctrl Pts',(-45.8429527488786,58.7060702401686,
12.));
#153044=CARTESIAN_POINT('Ctrl Pts',(-45.8391025302132,58.68974647507,0.));
#153045=CARTESIAN_POINT('Ctrl Pts',(-45.8391025302132,58.68974647507,12.));
#153046=CARTESIAN_POINT('Ctrl Pts',(-45.8339591141834,58.6680051552762,
0.));
#153047=CARTESIAN_POINT('Ctrl Pts',(-45.8339591141834,58.6680051552762,
12.));
#153048=CARTESIAN_POINT('Ctrl Pts',(-45.8275135264249,58.6408680154016,
0.));
#153049=CARTESIAN_POINT('Ctrl Pts',(-45.8275135264249,58.6408680154016,
12.));
#153050=CARTESIAN_POINT('Ctrl Pts',(-45.8210516273781,58.6137704035871,
0.));
#153051=CARTESIAN_POINT('Ctrl Pts',(-45.8210516273781,58.6137704035871,
12.));
#153052=CARTESIAN_POINT('Ctrl Pts',(-45.814573433072,58.5867123491018,0.));
#153053=CARTESIAN_POINT('Ctrl Pts',(-45.814573433072,58.5867123491018,12.));
#153054=CARTESIAN_POINT('Ctrl Pts',(-45.8080789725084,58.5596938940195,
0.));
#153055=CARTESIAN_POINT('Ctrl Pts',(-45.8080789725084,58.5596938940195,
12.));
#153056=CARTESIAN_POINT('Ctrl Pts',(-45.8015682926024,58.5327150960661,
0.));
#153057=CARTESIAN_POINT('Ctrl Pts',(-45.8015682926024,58.5327150960661,
12.));
#153058=CARTESIAN_POINT('Ctrl Pts',(-45.7950414569268,58.5057760270184,
0.));
#153059=CARTESIAN_POINT('Ctrl Pts',(-45.7950414569268,58.5057760270184,
12.));
#153060=CARTESIAN_POINT('Ctrl Pts',(-45.7884985397018,58.4788767676949,
0.));
#153061=CARTESIAN_POINT('Ctrl Pts',(-45.7884985397018,58.4788767676949,
12.));
#153062=CARTESIAN_POINT('Ctrl Pts',(-45.7819396211009,58.4520174038764,
0.));
#153063=CARTESIAN_POINT('Ctrl Pts',(-45.7819396211009,58.4520174038764,
12.));
#153064=CARTESIAN_POINT('Ctrl Pts',(-45.7753647821513,58.425198021955,0.));
#153065=CARTESIAN_POINT('Ctrl Pts',(-45.7753647821513,58.425198021955,12.));
#153066=CARTESIAN_POINT('Ctrl Pts',(-45.7687740994956,58.3984187044245,
0.));
#153067=CARTESIAN_POINT('Ctrl Pts',(-45.7687740994956,58.3984187044245,
12.));
#153068=CARTESIAN_POINT('Ctrl Pts',(-45.7621676411434,58.3716795262353,
0.));
#153069=CARTESIAN_POINT('Ctrl Pts',(-45.7621676411434,58.3716795262353,
12.));
#153070=CARTESIAN_POINT('Ctrl Pts',(-45.755545469402,58.3449805573423,0.));
#153071=CARTESIAN_POINT('Ctrl Pts',(-45.755545469402,58.3449805573423,12.));
#153072=CARTESIAN_POINT('Ctrl Pts',(-45.7489076429763,58.3183218645317,
0.));
#153073=CARTESIAN_POINT('Ctrl Pts',(-45.7489076429763,58.3183218645317,
12.));
#153074=CARTESIAN_POINT('Ctrl Pts',(-45.742254219463,58.291703513584,0.));
#153075=CARTESIAN_POINT('Ctrl Pts',(-45.742254219463,58.291703513584,12.));
#153076=CARTESIAN_POINT('Ctrl Pts',(-45.7355852575106,58.2651255711453,
0.));
#153077=CARTESIAN_POINT('Ctrl Pts',(-45.7355852575106,58.2651255711453,
12.));
#153078=CARTESIAN_POINT('Ctrl Pts',(-45.7289008195578,58.2385881070913,
0.));
#153079=CARTESIAN_POINT('Ctrl Pts',(-45.7289008195578,58.2385881070913,
12.));
#153080=CARTESIAN_POINT('Ctrl Pts',(-45.7222009715397,58.2120911942772,
0.));
#153081=CARTESIAN_POINT('Ctrl Pts',(-45.7222009715397,58.2120911942772,
12.));
#153082=CARTESIAN_POINT('Ctrl Pts',(-45.7154857816483,58.185634907469,0.));
#153083=CARTESIAN_POINT('Ctrl Pts',(-45.7154857816483,58.185634907469,12.));
#153084=CARTESIAN_POINT('Ctrl Pts',(-45.7087553193771,58.1592193225137,
0.));
#153085=CARTESIAN_POINT('Ctrl Pts',(-45.7087553193771,58.1592193225137,
12.));
#153086=CARTESIAN_POINT('Ctrl Pts',(-45.702009654518,58.1328445154676,0.));
#153087=CARTESIAN_POINT('Ctrl Pts',(-45.702009654518,58.1328445154676,12.));
#153088=CARTESIAN_POINT('Ctrl Pts',(-45.695248856015,58.1065105615907,0.));
#153089=CARTESIAN_POINT('Ctrl Pts',(-45.695248856015,58.1065105615907,12.));
#153090=CARTESIAN_POINT('Ctrl Pts',(-45.6884729914485,58.0802175348966,
0.));
#153091=CARTESIAN_POINT('Ctrl Pts',(-45.6884729914485,58.0802175348966,
12.));
#153092=CARTESIAN_POINT('Ctrl Pts',(-45.6816821276678,58.0539655087117,
0.));
#153093=CARTESIAN_POINT('Ctrl Pts',(-45.6816821276678,58.0539655087117,
12.));
#153094=CARTESIAN_POINT('Ctrl Pts',(-45.6748763311643,58.0277545560012,
0.));
#153095=CARTESIAN_POINT('Ctrl Pts',(-45.6748763311643,58.0277545560012,
12.));
#153096=CARTESIAN_POINT('Ctrl Pts',(-45.6680556685493,58.0015847497837,
0.));
#153097=CARTESIAN_POINT('Ctrl Pts',(-45.6680556685493,58.0015847497837,
12.));
#153098=CARTESIAN_POINT('Ctrl Pts',(-45.661220206992,57.9754561635061,0.));
#153099=CARTESIAN_POINT('Ctrl Pts',(-45.661220206992,57.9754561635061,12.));
#153100=CARTESIAN_POINT('Ctrl Pts',(-45.6543700146679,57.9493688714237,
0.));
#153101=CARTESIAN_POINT('Ctrl Pts',(-45.6543700146679,57.9493688714237,
12.));
#153102=CARTESIAN_POINT('Ctrl Pts',(-45.6475051605535,57.9233229484311,
0.));
#153103=CARTESIAN_POINT('Ctrl Pts',(-45.6475051605535,57.9233229484311,
12.));
#153104=CARTESIAN_POINT('Ctrl Pts',(-45.6406257142381,57.8973184699034,
0.));
#153105=CARTESIAN_POINT('Ctrl Pts',(-45.6406257142381,57.8973184699034,
12.));
#153106=CARTESIAN_POINT('Ctrl Pts',(-45.6337317457252,57.8713555115232,
0.));
#153107=CARTESIAN_POINT('Ctrl Pts',(-45.6337317457252,57.8713555115232,
12.));
#153108=CARTESIAN_POINT('Ctrl Pts',(-45.6268233252544,57.8454341491238,
0.));
#153109=CARTESIAN_POINT('Ctrl Pts',(-45.6268233252544,57.8454341491238,
12.));
#153110=CARTESIAN_POINT('Ctrl Pts',(-45.6199005230783,57.8195544584845,
0.));
#153111=CARTESIAN_POINT('Ctrl Pts',(-45.6199005230783,57.8195544584845,
12.));
#153112=CARTESIAN_POINT('Ctrl Pts',(-45.6129634094683,57.7937165153387,
0.));
#153113=CARTESIAN_POINT('Ctrl Pts',(-45.6129634094683,57.7937165153387,
12.));
#153114=CARTESIAN_POINT('Ctrl Pts',(-45.6060120548205,57.7679203954742,
0.));
#153115=CARTESIAN_POINT('Ctrl Pts',(-45.6060120548205,57.7679203954742,
12.));
#153116=CARTESIAN_POINT('Ctrl Pts',(-45.5990465297343,57.7421661748026,
0.));
#153117=CARTESIAN_POINT('Ctrl Pts',(-45.5990465297343,57.7421661748026,
12.));
#153118=CARTESIAN_POINT('Ctrl Pts',(-45.5920669050986,57.7164539294314,
0.));
#153119=CARTESIAN_POINT('Ctrl Pts',(-45.5920669050986,57.7164539294314,
12.));
#153120=CARTESIAN_POINT('Ctrl Pts',(-45.5850732521895,57.6907837357418,
0.));
#153121=CARTESIAN_POINT('Ctrl Pts',(-45.5850732521895,57.6907837357418,
12.));
#153122=CARTESIAN_POINT('Ctrl Pts',(-45.5780656427163,57.6651556704237,
0.));
#153123=CARTESIAN_POINT('Ctrl Pts',(-45.5780656427163,57.6651556704237,
12.));
#153124=CARTESIAN_POINT('Ctrl Pts',(-45.5710441487674,57.6395698104404,
0.));
#153125=CARTESIAN_POINT('Ctrl Pts',(-45.5710441487674,57.6395698104404,
12.));
#153126=CARTESIAN_POINT('Ctrl Pts',(-45.5640088427813,57.614026233004,0.));
#153127=CARTESIAN_POINT('Ctrl Pts',(-45.5640088427813,57.614026233004,12.));
#153128=CARTESIAN_POINT('Ctrl Pts',(-45.5569597975096,57.5885250155433,
0.));
#153129=CARTESIAN_POINT('Ctrl Pts',(-45.5569597975096,57.5885250155433,
12.));
#153130=CARTESIAN_POINT('Ctrl Pts',(-45.5498970859834,57.563066235668,0.));
#153131=CARTESIAN_POINT('Ctrl Pts',(-45.5498970859834,57.563066235668,12.));
#153132=CARTESIAN_POINT('Ctrl Pts',(-45.542820781484,57.537649971135,0.));
#153133=CARTESIAN_POINT('Ctrl Pts',(-45.542820781484,57.537649971135,12.));
#153134=CARTESIAN_POINT('Ctrl Pts',(-45.5357309575611,57.5122762998745,
0.));
#153135=CARTESIAN_POINT('Ctrl Pts',(-45.5357309575611,57.5122762998745,
12.));
#153136=CARTESIAN_POINT('Ctrl Pts',(-45.5286276880484,57.4869453000063,
0.));
#153137=CARTESIAN_POINT('Ctrl Pts',(-45.5286276880484,57.4869453000063,
12.));
#153138=CARTESIAN_POINT('Ctrl Pts',(-45.5215110470825,57.4616570498568,
0.));
#153139=CARTESIAN_POINT('Ctrl Pts',(-45.5215110470825,57.4616570498568,
12.));
#153140=CARTESIAN_POINT('Ctrl Pts',(-45.5143811091205,57.4364116279702,
0.));
#153141=CARTESIAN_POINT('Ctrl Pts',(-45.5143811091205,57.4364116279702,
12.));
#153142=CARTESIAN_POINT('Ctrl Pts',(-45.5072379489631,57.4112091131183,
0.));
#153143=CARTESIAN_POINT('Ctrl Pts',(-45.5072379489631,57.4112091131183,
12.));
#153144=CARTESIAN_POINT('Ctrl Pts',(-45.5000816417509,57.3860495843033,
0.));
#153145=CARTESIAN_POINT('Ctrl Pts',(-45.5000816417509,57.3860495843033,
12.));
#153146=CARTESIAN_POINT('Ctrl Pts',(-45.4929122629572,57.3609331207574,
0.));
#153147=CARTESIAN_POINT('Ctrl Pts',(-45.4929122629572,57.3609331207574,
12.));
#153148=CARTESIAN_POINT('Ctrl Pts',(-45.4857298883824,57.3358598019389,
0.));
#153149=CARTESIAN_POINT('Ctrl Pts',(-45.4857298883824,57.3358598019389,
12.));
#153150=CARTESIAN_POINT('Ctrl Pts',(-45.4785345941507,57.3108297075265,
0.));
#153151=CARTESIAN_POINT('Ctrl Pts',(-45.4785345941507,57.3108297075265,
12.));
#153152=CARTESIAN_POINT('Ctrl Pts',(-45.4713264567063,57.2858429174062,
0.));
#153153=CARTESIAN_POINT('Ctrl Pts',(-45.4713264567063,57.2858429174062,
12.));
#153154=CARTESIAN_POINT('Ctrl Pts',(-45.4641055528141,57.2608995116733,
0.));
#153155=CARTESIAN_POINT('Ctrl Pts',(-45.4641055528141,57.2608995116733,
12.));
#153156=CARTESIAN_POINT('Ctrl Pts',(-45.4568719595641,57.2359995706447,
0.));
#153157=CARTESIAN_POINT('Ctrl Pts',(-45.4568719595641,57.2359995706447,
12.));
#153158=CARTESIAN_POINT('Ctrl Pts',(-45.4496257543759,57.2111431748631,
0.));
#153159=CARTESIAN_POINT('Ctrl Pts',(-45.4496257543759,57.2111431748631,
12.));
#153160=CARTESIAN_POINT('Ctrl Pts',(-45.4423670150034,57.186330405101,0.));
#153161=CARTESIAN_POINT('Ctrl Pts',(-45.4423670150034,57.186330405101,12.));
#153162=CARTESIAN_POINT('Ctrl Pts',(-45.4350958195433,57.1615613423584,
0.));
#153163=CARTESIAN_POINT('Ctrl Pts',(-45.4350958195433,57.1615613423584,
12.));
#153164=CARTESIAN_POINT('Ctrl Pts',(-45.4278122464389,57.136836067863,0.));
#153165=CARTESIAN_POINT('Ctrl Pts',(-45.4278122464389,57.136836067863,12.));
#153166=CARTESIAN_POINT('Ctrl Pts',(-45.4205163744781,57.112154663078,0.));
#153167=CARTESIAN_POINT('Ctrl Pts',(-45.4205163744781,57.112154663078,12.));
#153168=CARTESIAN_POINT('Ctrl Pts',(-45.4132082827948,57.0875172097051,
0.));
#153169=CARTESIAN_POINT('Ctrl Pts',(-45.4132082827948,57.0875172097051,
12.));
#153170=CARTESIAN_POINT('Ctrl Pts',(-45.4058880508693,57.0629237896848,
0.));
#153171=CARTESIAN_POINT('Ctrl Pts',(-45.4058880508693,57.0629237896848,
12.));
#153172=CARTESIAN_POINT('Ctrl Pts',(-45.3985557585311,57.0383744851913,
0.));
#153173=CARTESIAN_POINT('Ctrl Pts',(-45.3985557585311,57.0383744851913,
12.));
#153174=CARTESIAN_POINT('Ctrl Pts',(-45.3912114859616,57.0138693786278,
0.));
#153175=CARTESIAN_POINT('Ctrl Pts',(-45.3912114859616,57.0138693786278,
12.));
#153176=CARTESIAN_POINT('Ctrl Pts',(-45.3838553136948,56.9894085526373,
0.));
#153177=CARTESIAN_POINT('Ctrl Pts',(-45.3838553136948,56.9894085526373,
12.));
#153178=CARTESIAN_POINT('Ctrl Pts',(-45.3764873226196,56.9649920901073,
0.));
#153179=CARTESIAN_POINT('Ctrl Pts',(-45.3764873226196,56.9649920901073,
12.));
#153180=CARTESIAN_POINT('Ctrl Pts',(-45.3691075939826,56.9406200741714,
0.));
#153181=CARTESIAN_POINT('Ctrl Pts',(-45.3691075939826,56.9406200741714,
12.));
#153182=CARTESIAN_POINT('Ctrl Pts',(-45.3617162093922,56.9162925882085,
0.));
#153183=CARTESIAN_POINT('Ctrl Pts',(-45.3617162093922,56.9162925882085,
12.));
#153184=CARTESIAN_POINT('Ctrl Pts',(-45.3543132508238,56.8920097158377,
0.));
#153185=CARTESIAN_POINT('Ctrl Pts',(-45.3543132508238,56.8920097158377,
12.));
#153186=CARTESIAN_POINT('Ctrl Pts',(-45.3468988006203,56.8677715409268,
0.));
#153187=CARTESIAN_POINT('Ctrl Pts',(-45.3468988006203,56.8677715409268,
12.));
#153188=CARTESIAN_POINT('Ctrl Pts',(-45.3394729414931,56.8435781475981,
0.));
#153189=CARTESIAN_POINT('Ctrl Pts',(-45.3394729414931,56.8435781475981,
12.));
#153190=CARTESIAN_POINT('Ctrl Pts',(-45.332035756524,56.8194296202291,0.));
#153191=CARTESIAN_POINT('Ctrl Pts',(-45.332035756524,56.8194296202291,12.));
#153192=CARTESIAN_POINT('Ctrl Pts',(-45.3245873291684,56.7953260434524,
0.));
#153193=CARTESIAN_POINT('Ctrl Pts',(-45.3245873291684,56.7953260434524,
12.));
#153194=CARTESIAN_POINT('Ctrl Pts',(-45.31712774326,56.7712675021491,0.));
#153195=CARTESIAN_POINT('Ctrl Pts',(-45.31712774326,56.7712675021491,12.));
#153196=CARTESIAN_POINT('Ctrl Pts',(-45.3096570830117,56.7472540814554,
0.));
#153197=CARTESIAN_POINT('Ctrl Pts',(-45.3096570830117,56.7472540814554,
12.));
#153198=CARTESIAN_POINT('Ctrl Pts',(-45.3021754330178,56.7232858667709,
0.));
#153199=CARTESIAN_POINT('Ctrl Pts',(-45.3021754330178,56.7232858667709,
12.));
#153200=CARTESIAN_POINT('Ctrl Pts',(-45.2946828782559,56.69936294376,0.));
#153201=CARTESIAN_POINT('Ctrl Pts',(-45.2946828782559,56.69936294376,12.));
#153202=CARTESIAN_POINT('Ctrl Pts',(-45.2871795040906,56.6754853983528,
0.));
#153203=CARTESIAN_POINT('Ctrl Pts',(-45.2871795040906,56.6754853983528,
12.));
#153204=CARTESIAN_POINT('Ctrl Pts',(-45.2796653962785,56.6516533167384,
0.));
#153205=CARTESIAN_POINT('Ctrl Pts',(-45.2796653962785,56.6516533167384,
12.));
#153206=CARTESIAN_POINT('Ctrl Pts',(-45.2721406409695,56.6278667853702,
0.));
#153207=CARTESIAN_POINT('Ctrl Pts',(-45.2721406409695,56.6278667853702,
12.));
#153208=CARTESIAN_POINT('Ctrl Pts',(-45.2646053247087,56.6041258909741,
0.));
#153209=CARTESIAN_POINT('Ctrl Pts',(-45.2646053247087,56.6041258909741,
12.));
#153210=CARTESIAN_POINT('Ctrl Pts',(-45.257059534438,56.5804307205505,0.));
#153211=CARTESIAN_POINT('Ctrl Pts',(-45.257059534438,56.5804307205505,12.));
#153212=CARTESIAN_POINT('Ctrl Pts',(-45.2495033575,56.5567813613756,0.));
#153213=CARTESIAN_POINT('Ctrl Pts',(-45.2495033575,56.5567813613756,12.));
#153214=CARTESIAN_POINT('Ctrl Pts',(-45.2419368816428,56.5331779009958,
0.));
#153215=CARTESIAN_POINT('Ctrl Pts',(-45.2419368816428,56.5331779009958,
12.));
#153216=CARTESIAN_POINT('Ctrl Pts',(-45.2343601950227,56.5096204272306,
0.));
#153217=CARTESIAN_POINT('Ctrl Pts',(-45.2343601950227,56.5096204272306,
12.));
#153218=CARTESIAN_POINT('Ctrl Pts',(-45.2267733862049,56.4861090281823,
0.));
#153219=CARTESIAN_POINT('Ctrl Pts',(-45.2267733862049,56.4861090281823,
12.));
#153220=CARTESIAN_POINT('Ctrl Pts',(-45.2191765441666,56.4626437922386,
0.));
#153221=CARTESIAN_POINT('Ctrl Pts',(-45.2191765441666,56.4626437922386,
12.));
#153222=CARTESIAN_POINT('Ctrl Pts',(-45.2115697583,56.4392248080732,0.));
#153223=CARTESIAN_POINT('Ctrl Pts',(-45.2115697583,56.4392248080732,12.));
#153224=CARTESIAN_POINT('Ctrl Pts',(-45.2039531184171,56.4158521646411,
0.));
#153225=CARTESIAN_POINT('Ctrl Pts',(-45.2039531184171,56.4158521646411,
12.));
#153226=CARTESIAN_POINT('Ctrl Pts',(-45.1963267147529,56.3925259511806,
0.));
#153227=CARTESIAN_POINT('Ctrl Pts',(-45.1963267147529,56.3925259511806,
12.));
#153228=CARTESIAN_POINT('Ctrl Pts',(-45.1886906379667,56.3692462572231,
0.));
#153229=CARTESIAN_POINT('Ctrl Pts',(-45.1886906379667,56.3692462572231,
12.));
#153230=CARTESIAN_POINT('Ctrl Pts',(-45.1810449791453,56.3460131725964,
0.));
#153231=CARTESIAN_POINT('Ctrl Pts',(-45.1810449791453,56.3460131725964,
12.));
#153232=CARTESIAN_POINT('Ctrl Pts',(-45.173389829806,56.3228267874264,0.));
#153233=CARTESIAN_POINT('Ctrl Pts',(-45.173389829806,56.3228267874264,12.));
#153234=CARTESIAN_POINT('Ctrl Pts',(-45.1657252819013,56.2996871921316,
0.));
#153235=CARTESIAN_POINT('Ctrl Pts',(-45.1657252819013,56.2996871921316,
12.));
#153236=CARTESIAN_POINT('Ctrl Pts',(-45.1580514278223,56.2765944774245,
0.));
#153237=CARTESIAN_POINT('Ctrl Pts',(-45.1580514278223,56.2765944774245,
12.));
#153238=CARTESIAN_POINT('Ctrl Pts',(-45.1503683604005,56.2535487343221,
0.));
#153239=CARTESIAN_POINT('Ctrl Pts',(-45.1503683604005,56.2535487343221,
12.));
#153240=CARTESIAN_POINT('Ctrl Pts',(-45.1426761729105,56.230550054149,0.));
#153241=CARTESIAN_POINT('Ctrl Pts',(-45.1426761729105,56.230550054149,12.));
#153242=CARTESIAN_POINT('Ctrl Pts',(-45.1349749590737,56.2075985285393,
0.));
#153243=CARTESIAN_POINT('Ctrl Pts',(-45.1349749590737,56.2075985285393,
12.));
#153244=CARTESIAN_POINT('Ctrl Pts',(-45.127264813063,56.1846942494325,0.));
#153245=CARTESIAN_POINT('Ctrl Pts',(-45.127264813063,56.1846942494325,12.));
#153246=CARTESIAN_POINT('Ctrl Pts',(-45.1195458295062,56.1618373090732,
0.));
#153247=CARTESIAN_POINT('Ctrl Pts',(-45.1195458295062,56.1618373090732,
12.));
#153248=CARTESIAN_POINT('Ctrl Pts',(-45.1118181034888,56.1390278000226,
0.));
#153249=CARTESIAN_POINT('Ctrl Pts',(-45.1118181034888,56.1390278000226,
12.));
#153250=CARTESIAN_POINT('Ctrl Pts',(-45.1040817305561,56.116265815162,0.));
#153251=CARTESIAN_POINT('Ctrl Pts',(-45.1040817305561,56.116265815162,12.));
#153252=CARTESIAN_POINT('Ctrl Pts',(-45.0963368067177,56.0935514476945,
0.));
#153253=CARTESIAN_POINT('Ctrl Pts',(-45.0963368067177,56.0935514476945,
12.));
#153254=CARTESIAN_POINT('Ctrl Pts',(-45.0885834284517,56.0708847911416,
0.));
#153255=CARTESIAN_POINT('Ctrl Pts',(-45.0885834284517,56.0708847911416,
12.));
#153256=CARTESIAN_POINT('Ctrl Pts',(-45.0808216927089,56.048265939342,0.));
#153257=CARTESIAN_POINT('Ctrl Pts',(-45.0808216927089,56.048265939342,12.));
#153258=CARTESIAN_POINT('Ctrl Pts',(-45.0730516969148,56.0256949864639,
0.));
#153259=CARTESIAN_POINT('Ctrl Pts',(-45.0730516969148,56.0256949864639,
12.));
#153260=CARTESIAN_POINT('Ctrl Pts',(-45.0652735389733,56.003172027008,0.));
#153261=CARTESIAN_POINT('Ctrl Pts',(-45.0652735389733,56.003172027008,12.));
#153262=CARTESIAN_POINT('Ctrl Pts',(-45.0574873172694,55.9806971558097,
0.));
#153263=CARTESIAN_POINT('Ctrl Pts',(-45.0574873172694,55.9806971558097,
12.));
#153264=CARTESIAN_POINT('Ctrl Pts',(-45.0496931306755,55.9582704680356,
0.));
#153265=CARTESIAN_POINT('Ctrl Pts',(-45.0496931306755,55.9582704680356,
12.));
#153266=CARTESIAN_POINT('Ctrl Pts',(-45.041891078555,55.9358920591837,0.));
#153267=CARTESIAN_POINT('Ctrl Pts',(-45.041891078555,55.9358920591837,12.));
#153268=CARTESIAN_POINT('Ctrl Pts',(-45.0340812607657,55.9135620250954,
0.));
#153269=CARTESIAN_POINT('Ctrl Pts',(-45.0340812607657,55.9135620250954,
12.));
#153270=CARTESIAN_POINT('Ctrl Pts',(-45.0262637776614,55.8912804619577,
0.));
#153271=CARTESIAN_POINT('Ctrl Pts',(-45.0262637776614,55.8912804619577,
12.));
#153272=CARTESIAN_POINT('Ctrl Pts',(-45.0184387300973,55.8690474663065,
0.));
#153273=CARTESIAN_POINT('Ctrl Pts',(-45.0184387300973,55.8690474663065,
12.));
#153274=CARTESIAN_POINT('Ctrl Pts',(-45.0106062194342,55.8468631350218,
0.));
#153275=CARTESIAN_POINT('Ctrl Pts',(-45.0106062194342,55.8468631350218,
12.));
#153276=CARTESIAN_POINT('Ctrl Pts',(-45.0027663475433,55.8247275653289,
0.));
#153277=CARTESIAN_POINT('Ctrl Pts',(-45.0027663475433,55.8247275653289,
12.));
#153278=CARTESIAN_POINT('Ctrl Pts',(-44.9949192168093,55.8026408548105,
0.));
#153279=CARTESIAN_POINT('Ctrl Pts',(-44.9949192168093,55.8026408548105,
12.));
#153280=CARTESIAN_POINT('Ctrl Pts',(-44.9870649301342,55.7806031014106,
0.));
#153281=CARTESIAN_POINT('Ctrl Pts',(-44.9870649301342,55.7806031014106,
12.));
#153282=CARTESIAN_POINT('Ctrl Pts',(-44.9792035909413,55.7586144034367,
0.));
#153283=CARTESIAN_POINT('Ctrl Pts',(-44.9792035909413,55.7586144034367,
12.));
#153284=CARTESIAN_POINT('Ctrl Pts',(-44.9713353031804,55.7366748595552,
0.));
#153285=CARTESIAN_POINT('Ctrl Pts',(-44.9713353031804,55.7366748595552,
12.));
#153286=CARTESIAN_POINT('Ctrl Pts',(-44.9634601713321,55.714784568793,0.));
#153287=CARTESIAN_POINT('Ctrl Pts',(-44.9634601713321,55.714784568793,12.));
#153288=CARTESIAN_POINT('Ctrl Pts',(-44.9555783004106,55.6929436305489,
0.));
#153289=CARTESIAN_POINT('Ctrl Pts',(-44.9555783004106,55.6929436305489,
12.));
#153290=CARTESIAN_POINT('Ctrl Pts',(-44.9476897959684,55.6711521445979,
0.));
#153291=CARTESIAN_POINT('Ctrl Pts',(-44.9476897959684,55.6711521445979,
12.));
#153292=CARTESIAN_POINT('Ctrl Pts',(-44.9397947641006,55.6494102110935,
0.));
#153293=CARTESIAN_POINT('Ctrl Pts',(-44.9397947641006,55.6494102110935,
12.));
#153294=CARTESIAN_POINT('Ctrl Pts',(-44.9318933114506,55.6277179305633,
0.));
#153295=CARTESIAN_POINT('Ctrl Pts',(-44.9318933114506,55.6277179305633,
12.));
#153296=CARTESIAN_POINT('Ctrl Pts',(-44.9239855452144,55.6060754039121,
0.));
#153297=CARTESIAN_POINT('Ctrl Pts',(-44.9239855452144,55.6060754039121,
12.));
#153298=CARTESIAN_POINT('Ctrl Pts',(-44.9160715731443,55.5844827324338,
0.));
#153299=CARTESIAN_POINT('Ctrl Pts',(-44.9160715731443,55.5844827324338,
12.));
#153300=CARTESIAN_POINT('Ctrl Pts',(-44.908151503553,55.5629400178142,0.));
#153301=CARTESIAN_POINT('Ctrl Pts',(-44.908151503553,55.5629400178142,12.));
#153302=CARTESIAN_POINT('Ctrl Pts',(-44.9002254453183,55.541447362134,0.));
#153303=CARTESIAN_POINT('Ctrl Pts',(-44.9002254453183,55.541447362134,12.));
#153304=CARTESIAN_POINT('Ctrl Pts',(-44.8922935078889,55.5200048678629,
0.));
#153305=CARTESIAN_POINT('Ctrl Pts',(-44.8922935078889,55.5200048678629,
12.));
#153306=CARTESIAN_POINT('Ctrl Pts',(-44.8843558012886,55.4986126378656,
0.));
#153307=CARTESIAN_POINT('Ctrl Pts',(-44.8843558012886,55.4986126378656,
12.));
#153308=CARTESIAN_POINT('Ctrl Pts',(-44.8764124361206,55.4772707754126,
0.));
#153309=CARTESIAN_POINT('Ctrl Pts',(-44.8764124361206,55.4772707754126,
12.));
#153310=CARTESIAN_POINT('Ctrl Pts',(-44.8684635235725,55.4559793841836,
0.));
#153311=CARTESIAN_POINT('Ctrl Pts',(-44.8684635235725,55.4559793841836,
12.));
#153312=CARTESIAN_POINT('Ctrl Pts',(-44.8605091754214,55.4347385682704,
0.));
#153313=CARTESIAN_POINT('Ctrl Pts',(-44.8605091754214,55.4347385682704,
12.));
#153314=CARTESIAN_POINT('Ctrl Pts',(-44.8525495040408,55.4135484321718,
0.));
#153315=CARTESIAN_POINT('Ctrl Pts',(-44.8525495040408,55.4135484321718,
12.));
#153316=CARTESIAN_POINT('Ctrl Pts',(-44.8445846224044,55.3924090808014,
0.));
#153317=CARTESIAN_POINT('Ctrl Pts',(-44.8445846224044,55.3924090808014,
12.));
#153318=CARTESIAN_POINT('Ctrl Pts',(-44.8366146440901,55.3713206194967,
0.));
#153319=CARTESIAN_POINT('Ctrl Pts',(-44.8366146440901,55.3713206194967,
12.));
#153320=CARTESIAN_POINT('Ctrl Pts',(-44.8286396832847,55.3502831540228,
0.));
#153321=CARTESIAN_POINT('Ctrl Pts',(-44.8286396832847,55.3502831540228,
12.));
#153322=CARTESIAN_POINT('Ctrl Pts',(-44.8206598547887,55.3292967905725,
0.));
#153323=CARTESIAN_POINT('Ctrl Pts',(-44.8206598547887,55.3292967905725,
12.));
#153324=CARTESIAN_POINT('Ctrl Pts',(-44.8126752740208,55.3083616357605,
0.));
#153325=CARTESIAN_POINT('Ctrl Pts',(-44.8126752740208,55.3083616357605,
12.));
#153326=CARTESIAN_POINT('Ctrl Pts',(-44.8046860570244,55.287477796635,0.));
#153327=CARTESIAN_POINT('Ctrl Pts',(-44.8046860570244,55.287477796635,12.));
#153328=CARTESIAN_POINT('Ctrl Pts',(-44.796692320474,55.2666453806883,0.));
#153329=CARTESIAN_POINT('Ctrl Pts',(-44.796692320474,55.2666453806883,12.));
#153330=CARTESIAN_POINT('Ctrl Pts',(-44.7886941816823,55.2458644958617,
0.));
#153331=CARTESIAN_POINT('Ctrl Pts',(-44.7886941816823,55.2458644958617,
12.));
#153332=CARTESIAN_POINT('Ctrl Pts',(-44.7806917586077,55.2251352505474,
0.));
#153333=CARTESIAN_POINT('Ctrl Pts',(-44.7806917586077,55.2251352505474,
12.));
#153334=CARTESIAN_POINT('Ctrl Pts',(-44.7726851698618,55.2044577535865,
0.));
#153335=CARTESIAN_POINT('Ctrl Pts',(-44.7726851698618,55.2044577535865,
12.));
#153336=CARTESIAN_POINT('Ctrl Pts',(-44.7646745347108,55.1838321142777,
0.));
#153337=CARTESIAN_POINT('Ctrl Pts',(-44.7646745347108,55.1838321142777,
12.));
#153338=CARTESIAN_POINT('Ctrl Pts',(-44.7566599730771,55.1632584423813,
0.));
#153339=CARTESIAN_POINT('Ctrl Pts',(-44.7566599730771,55.1632584423813,
12.));
#153340=CARTESIAN_POINT('Ctrl Pts',(-44.7486416055419,55.1427368481201,
0.));
#153341=CARTESIAN_POINT('Ctrl Pts',(-44.7486416055419,55.1427368481201,
12.));
#153342=CARTESIAN_POINT('Ctrl Pts',(-44.7406195533482,55.1222674421747,
0.));
#153343=CARTESIAN_POINT('Ctrl Pts',(-44.7406195533482,55.1222674421747,
12.));
#153344=CARTESIAN_POINT('Ctrl Pts',(-44.7325939384042,55.1018503356806,
0.));
#153345=CARTESIAN_POINT('Ctrl Pts',(-44.7325939384042,55.1018503356806,
12.));
#153346=CARTESIAN_POINT('Ctrl Pts',(-44.7245648832988,55.0814856402507,
0.));
#153347=CARTESIAN_POINT('Ctrl Pts',(-44.7245648832988,55.0814856402507,
12.));
#153348=CARTESIAN_POINT('Ctrl Pts',(-44.7165325113165,55.0611734679902,
0.));
#153349=CARTESIAN_POINT('Ctrl Pts',(-44.7165325113165,55.0611734679902,
12.));
#153350=CARTESIAN_POINT('Ctrl Pts',(-44.7084969464509,55.0409139315074,
0.));
#153351=CARTESIAN_POINT('Ctrl Pts',(-44.7084969464509,55.0409139315074,
12.));
#153352=CARTESIAN_POINT('Ctrl Pts',(-44.7004583134235,55.020707143922,0.));
#153353=CARTESIAN_POINT('Ctrl Pts',(-44.7004583134235,55.020707143922,12.));
#153354=CARTESIAN_POINT('Ctrl Pts',(-44.6924167376851,55.0005532188644,
0.));
#153355=CARTESIAN_POINT('Ctrl Pts',(-44.6924167376851,55.0005532188644,
12.));
#153356=CARTESIAN_POINT('Ctrl Pts',(-44.6843723453985,54.9804522704668,
0.));
#153357=CARTESIAN_POINT('Ctrl Pts',(-44.6843723453985,54.9804522704668,
12.));
#153358=CARTESIAN_POINT('Ctrl Pts',(-44.6763252634255,54.9604044133497,
0.));
#153359=CARTESIAN_POINT('Ctrl Pts',(-44.6763252634255,54.9604044133497,
12.));
#153360=CARTESIAN_POINT('Ctrl Pts',(-44.6682756193155,54.9404097626088,
0.));
#153361=CARTESIAN_POINT('Ctrl Pts',(-44.6682756193155,54.9404097626088,
12.));
#153362=CARTESIAN_POINT('Ctrl Pts',(-44.6602235412853,54.9204684337845,
0.));
#153363=CARTESIAN_POINT('Ctrl Pts',(-44.6602235412853,54.9204684337845,
12.));
#153364=CARTESIAN_POINT('Ctrl Pts',(-44.6521691582551,54.9005805428991,
0.));
#153365=CARTESIAN_POINT('Ctrl Pts',(-44.6521691582551,54.9005805428991,
12.));
#153366=CARTESIAN_POINT('Ctrl Pts',(-44.6441125999074,54.8807462065177,
0.));
#153367=CARTESIAN_POINT('Ctrl Pts',(-44.6441125999074,54.8807462065177,
12.));
#153368=CARTESIAN_POINT('Ctrl Pts',(-44.6360539967392,54.860965541796,0.));
#153369=CARTESIAN_POINT('Ctrl Pts',(-44.6360539967392,54.860965541796,12.));
#153370=CARTESIAN_POINT('Ctrl Pts',(-44.6279934801159,54.8412386665264,
0.));
#153371=CARTESIAN_POINT('Ctrl Pts',(-44.6279934801159,54.8412386665264,
12.));
#153372=CARTESIAN_POINT('Ctrl Pts',(-44.6199311823276,54.8215656991817,
0.));
#153373=CARTESIAN_POINT('Ctrl Pts',(-44.6199311823276,54.8215656991817,
12.));
#153374=CARTESIAN_POINT('Ctrl Pts',(-44.6118672364889,54.8019467588258,
0.));
#153375=CARTESIAN_POINT('Ctrl Pts',(-44.6118672364889,54.8019467588258,
12.));
#153376=CARTESIAN_POINT('Ctrl Pts',(-44.60380177643,54.7823819650137,0.));
#153377=CARTESIAN_POINT('Ctrl Pts',(-44.60380177643,54.7823819650137,12.));
#153378=CARTESIAN_POINT('Ctrl Pts',(-44.5957349366062,54.7628714377042,
0.));
#153379=CARTESIAN_POINT('Ctrl Pts',(-44.5957349366062,54.7628714377042,
12.));
#153380=CARTESIAN_POINT('Ctrl Pts',(-44.5876668519676,54.7434152971285,
0.));
#153381=CARTESIAN_POINT('Ctrl Pts',(-44.5876668519676,54.7434152971285,
12.));
#153382=CARTESIAN_POINT('Ctrl Pts',(-44.5795976579476,54.7240136637744,
0.));
#153383=CARTESIAN_POINT('Ctrl Pts',(-44.5795976579476,54.7240136637744,
12.));
#153384=CARTESIAN_POINT('Ctrl Pts',(-44.5715274907637,54.7046666586777,
0.));
#153385=CARTESIAN_POINT('Ctrl Pts',(-44.5715274907637,54.7046666586777,
12.));
#153386=CARTESIAN_POINT('Ctrl Pts',(-44.5634564876869,54.685374403676,0.));
#153387=CARTESIAN_POINT('Ctrl Pts',(-44.5634564876869,54.685374403676,12.));
#153388=CARTESIAN_POINT('Ctrl Pts',(-44.5553847872712,54.6661370216242,
0.));
#153389=CARTESIAN_POINT('Ctrl Pts',(-44.5553847872712,54.6661370216242,
12.));
#153390=CARTESIAN_POINT('Ctrl Pts',(-44.5473125297289,54.6469546367381,
0.));
#153391=CARTESIAN_POINT('Ctrl Pts',(-44.5473125297289,54.6469546367381,
12.));
#153392=CARTESIAN_POINT('Ctrl Pts',(-44.5392398566775,54.6278273743554,
0.));
#153393=CARTESIAN_POINT('Ctrl Pts',(-44.5392398566775,54.6278273743554,
12.));
#153394=CARTESIAN_POINT('Ctrl Pts',(-44.5311669104494,54.6087553602889,
0.));
#153395=CARTESIAN_POINT('Ctrl Pts',(-44.5311669104494,54.6087553602889,
12.));
#153396=CARTESIAN_POINT('Ctrl Pts',(-44.5230938335165,54.5897387202812,
0.));
#153397=CARTESIAN_POINT('Ctrl Pts',(-44.5230938335165,54.5897387202812,
12.));
#153398=CARTESIAN_POINT('Ctrl Pts',(-44.5150207679007,54.5707775794436,
0.));
#153399=CARTESIAN_POINT('Ctrl Pts',(-44.5150207679007,54.5707775794436,
12.));
#153400=CARTESIAN_POINT('Ctrl Pts',(-44.5069478544977,54.5518720616056,
0.));
#153401=CARTESIAN_POINT('Ctrl Pts',(-44.5069478544977,54.5518720616056,
12.));
#153402=CARTESIAN_POINT('Ctrl Pts',(-44.4988752343744,54.5330222905475,
0.));
#153403=CARTESIAN_POINT('Ctrl Pts',(-44.4988752343744,54.5330222905475,
12.));
#153404=CARTESIAN_POINT('Ctrl Pts',(-44.4908030503225,54.5142283914704,
0.));
#153405=CARTESIAN_POINT('Ctrl Pts',(-44.4908030503225,54.5142283914704,
12.));
#153406=CARTESIAN_POINT('Ctrl Pts',(-44.4827314481264,54.495490492193,0.));
#153407=CARTESIAN_POINT('Ctrl Pts',(-44.4827314481264,54.495490492193,12.));
#153408=CARTESIAN_POINT('Ctrl Pts',(-44.4746605784031,54.4768087248824,
0.));
#153409=CARTESIAN_POINT('Ctrl Pts',(-44.4746605784031,54.4768087248824,
12.));
#153410=CARTESIAN_POINT('Ctrl Pts',(-44.4665905967668,54.4581832262033,
0.));
#153411=CARTESIAN_POINT('Ctrl Pts',(-44.4665905967668,54.4581832262033,
12.));
#153412=CARTESIAN_POINT('Ctrl Pts',(-44.4585216599907,54.4396141336978,
0.));
#153413=CARTESIAN_POINT('Ctrl Pts',(-44.4585216599907,54.4396141336978,
12.));
#153414=CARTESIAN_POINT('Ctrl Pts',(-44.4504539226327,54.421101582595,0.));
#153415=CARTESIAN_POINT('Ctrl Pts',(-44.4504539226327,54.421101582595,12.));
#153416=CARTESIAN_POINT('Ctrl Pts',(-44.4423875340995,54.4026457030335,
0.));
#153417=CARTESIAN_POINT('Ctrl Pts',(-44.4423875340995,54.4026457030335,
12.));
#153418=CARTESIAN_POINT('Ctrl Pts',(-44.4343226339592,54.3842466156196,
0.));
#153419=CARTESIAN_POINT('Ctrl Pts',(-44.4343226339592,54.3842466156196,
12.));
#153420=CARTESIAN_POINT('Ctrl Pts',(-44.4262593564712,54.3659044357119,
0.));
#153421=CARTESIAN_POINT('Ctrl Pts',(-44.4262593564712,54.3659044357119,
12.));
#153422=CARTESIAN_POINT('Ctrl Pts',(-44.4181978395851,54.3476192819352,
0.));
#153423=CARTESIAN_POINT('Ctrl Pts',(-44.4181978395851,54.3476192819352,
12.));
#153424=CARTESIAN_POINT('Ctrl Pts',(-44.4101382321834,54.3293912830237,
0.));
#153425=CARTESIAN_POINT('Ctrl Pts',(-44.4101382321834,54.3293912830237,
12.));
#153426=CARTESIAN_POINT('Ctrl Pts',(-44.402080702809,54.3112205860716,0.));
#153427=CARTESIAN_POINT('Ctrl Pts',(-44.402080702809,54.3112205860716,12.));
#153428=CARTESIAN_POINT('Ctrl Pts',(-44.3940254456331,54.2931073621553,
0.));
#153429=CARTESIAN_POINT('Ctrl Pts',(-44.3940254456331,54.2931073621553,
12.));
#153430=CARTESIAN_POINT('Ctrl Pts',(-44.3859726620183,54.2750517888579,
0.));
#153431=CARTESIAN_POINT('Ctrl Pts',(-44.3859726620183,54.2750517888579,
12.));
#153432=CARTESIAN_POINT('Ctrl Pts',(-44.3779225430405,54.2570540336475,
0.));
#153433=CARTESIAN_POINT('Ctrl Pts',(-44.3779225430405,54.2570540336475,
12.));
#153434=CARTESIAN_POINT('Ctrl Pts',(-44.3698752533561,54.2391142386412,
0.));
#153435=CARTESIAN_POINT('Ctrl Pts',(-44.3698752533561,54.2391142386412,
12.));
#153436=CARTESIAN_POINT('Ctrl Pts',(-44.361830910343,54.2212325006052,0.));
#153437=CARTESIAN_POINT('Ctrl Pts',(-44.361830910343,54.2212325006052,12.));
#153438=CARTESIAN_POINT('Ctrl Pts',(-44.3537895824096,54.2034088701928,
0.));
#153439=CARTESIAN_POINT('Ctrl Pts',(-44.3537895824096,54.2034088701928,
12.));
#153440=CARTESIAN_POINT('Ctrl Pts',(-44.3473589597726,54.1891964684727,
0.));
#153441=CARTESIAN_POINT('Ctrl Pts',(-44.3473589597726,54.1891964684727,
12.));
#153442=CARTESIAN_POINT('Ctrl Pts',(-44.3425373700993,54.1785633257639,
0.));
#153443=CARTESIAN_POINT('Ctrl Pts',(-44.3425373700993,54.1785633257639,
12.));
#153444=CARTESIAN_POINT('Ctrl Pts',(-44.3393235891075,54.1714861895346,
0.));
#153445=CARTESIAN_POINT('Ctrl Pts',(-44.3393235891075,54.1714861895346,
12.));
#153446=CARTESIAN_POINT('Ctrl Pts',(-44.3377168516418,54.1679505278134,
0.));
#153447=CARTESIAN_POINT('Ctrl Pts',(-44.3377168516418,54.1679505278134,
12.));
#153448=CARTESIAN_POINT('',(-44.3377168516418,54.1679505278134,12.));
#153449=CARTESIAN_POINT('Ctrl Pts',(-44.3377168516418,54.1679505278134,
12.));
#153450=CARTESIAN_POINT('Ctrl Pts',(-44.3393235891075,54.1714861895346,
12.));
#153451=CARTESIAN_POINT('Ctrl Pts',(-44.3425373700993,54.1785633257639,
12.));
#153452=CARTESIAN_POINT('Ctrl Pts',(-44.3473589597726,54.1891964684727,
12.));
#153453=CARTESIAN_POINT('Ctrl Pts',(-44.3537895824096,54.2034088701928,
12.));
#153454=CARTESIAN_POINT('Ctrl Pts',(-44.361830910343,54.2212325006052,12.));
#153455=CARTESIAN_POINT('Ctrl Pts',(-44.3698752533561,54.2391142386412,
12.));
#153456=CARTESIAN_POINT('Ctrl Pts',(-44.3779225430405,54.2570540336475,
12.));
#153457=CARTESIAN_POINT('Ctrl Pts',(-44.3859726620183,54.2750517888579,
12.));
#153458=CARTESIAN_POINT('Ctrl Pts',(-44.3940254456331,54.2931073621553,
12.));
#153459=CARTESIAN_POINT('Ctrl Pts',(-44.402080702809,54.3112205860716,12.));
#153460=CARTESIAN_POINT('Ctrl Pts',(-44.4101382321834,54.3293912830237,
12.));
#153461=CARTESIAN_POINT('Ctrl Pts',(-44.4181978395851,54.3476192819352,
12.));
#153462=CARTESIAN_POINT('Ctrl Pts',(-44.4262593564712,54.3659044357119,
12.));
#153463=CARTESIAN_POINT('Ctrl Pts',(-44.4343226339592,54.3842466156196,
12.));
#153464=CARTESIAN_POINT('Ctrl Pts',(-44.4423875340995,54.4026457030335,
12.));
#153465=CARTESIAN_POINT('Ctrl Pts',(-44.4504539226327,54.421101582595,12.));
#153466=CARTESIAN_POINT('Ctrl Pts',(-44.4585216599907,54.4396141336978,
12.));
#153467=CARTESIAN_POINT('Ctrl Pts',(-44.4665905967668,54.4581832262033,
12.));
#153468=CARTESIAN_POINT('Ctrl Pts',(-44.4746605784031,54.4768087248824,
12.));
#153469=CARTESIAN_POINT('Ctrl Pts',(-44.4827314481264,54.495490492193,12.));
#153470=CARTESIAN_POINT('Ctrl Pts',(-44.4908030503225,54.5142283914704,
12.));
#153471=CARTESIAN_POINT('Ctrl Pts',(-44.4988752343744,54.5330222905475,
12.));
#153472=CARTESIAN_POINT('Ctrl Pts',(-44.5069478544977,54.5518720616056,
12.));
#153473=CARTESIAN_POINT('Ctrl Pts',(-44.5150207679007,54.5707775794436,
12.));
#153474=CARTESIAN_POINT('Ctrl Pts',(-44.5230938335165,54.5897387202812,
12.));
#153475=CARTESIAN_POINT('Ctrl Pts',(-44.5311669104494,54.6087553602889,
12.));
#153476=CARTESIAN_POINT('Ctrl Pts',(-44.5392398566775,54.6278273743554,
12.));
#153477=CARTESIAN_POINT('Ctrl Pts',(-44.5473125297289,54.6469546367381,
12.));
#153478=CARTESIAN_POINT('Ctrl Pts',(-44.5553847872712,54.6661370216242,
12.));
#153479=CARTESIAN_POINT('Ctrl Pts',(-44.5634564876869,54.685374403676,12.));
#153480=CARTESIAN_POINT('Ctrl Pts',(-44.5715274907637,54.7046666586777,
12.));
#153481=CARTESIAN_POINT('Ctrl Pts',(-44.5795976579476,54.7240136637744,
12.));
#153482=CARTESIAN_POINT('Ctrl Pts',(-44.5876668519676,54.7434152971285,
12.));
#153483=CARTESIAN_POINT('Ctrl Pts',(-44.5957349366062,54.7628714377042,
12.));
#153484=CARTESIAN_POINT('Ctrl Pts',(-44.60380177643,54.7823819650137,12.));
#153485=CARTESIAN_POINT('Ctrl Pts',(-44.6118672364889,54.8019467588258,
12.));
#153486=CARTESIAN_POINT('Ctrl Pts',(-44.6199311823276,54.8215656991817,
12.));
#153487=CARTESIAN_POINT('Ctrl Pts',(-44.6279934801159,54.8412386665264,
12.));
#153488=CARTESIAN_POINT('Ctrl Pts',(-44.6360539967392,54.860965541796,12.));
#153489=CARTESIAN_POINT('Ctrl Pts',(-44.6441125999074,54.8807462065177,
12.));
#153490=CARTESIAN_POINT('Ctrl Pts',(-44.6521691582551,54.9005805428991,
12.));
#153491=CARTESIAN_POINT('Ctrl Pts',(-44.6602235412853,54.9204684337845,
12.));
#153492=CARTESIAN_POINT('Ctrl Pts',(-44.6682756193155,54.9404097626088,
12.));
#153493=CARTESIAN_POINT('Ctrl Pts',(-44.6763252634255,54.9604044133497,
12.));
#153494=CARTESIAN_POINT('Ctrl Pts',(-44.6843723453985,54.9804522704668,
12.));
#153495=CARTESIAN_POINT('Ctrl Pts',(-44.6924167376851,55.0005532188644,
12.));
#153496=CARTESIAN_POINT('Ctrl Pts',(-44.7004583134235,55.020707143922,12.));
#153497=CARTESIAN_POINT('Ctrl Pts',(-44.7084969464509,55.0409139315074,
12.));
#153498=CARTESIAN_POINT('Ctrl Pts',(-44.7165325113165,55.0611734679902,
12.));
#153499=CARTESIAN_POINT('Ctrl Pts',(-44.7245648832988,55.0814856402507,
12.));
#153500=CARTESIAN_POINT('Ctrl Pts',(-44.7325939384042,55.1018503356806,
12.));
#153501=CARTESIAN_POINT('Ctrl Pts',(-44.7406195533482,55.1222674421747,
12.));
#153502=CARTESIAN_POINT('Ctrl Pts',(-44.7486416055419,55.1427368481201,
12.));
#153503=CARTESIAN_POINT('Ctrl Pts',(-44.7566599730771,55.1632584423813,
12.));
#153504=CARTESIAN_POINT('Ctrl Pts',(-44.7646745347108,55.1838321142777,
12.));
#153505=CARTESIAN_POINT('Ctrl Pts',(-44.7726851698618,55.2044577535865,
12.));
#153506=CARTESIAN_POINT('Ctrl Pts',(-44.7806917586077,55.2251352505474,
12.));
#153507=CARTESIAN_POINT('Ctrl Pts',(-44.7886941816823,55.2458644958617,
12.));
#153508=CARTESIAN_POINT('Ctrl Pts',(-44.796692320474,55.2666453806883,12.));
#153509=CARTESIAN_POINT('Ctrl Pts',(-44.8046860570244,55.287477796635,12.));
#153510=CARTESIAN_POINT('Ctrl Pts',(-44.8126752740208,55.3083616357605,
12.));
#153511=CARTESIAN_POINT('Ctrl Pts',(-44.8206598547887,55.3292967905725,
12.));
#153512=CARTESIAN_POINT('Ctrl Pts',(-44.8286396832847,55.3502831540228,
12.));
#153513=CARTESIAN_POINT('Ctrl Pts',(-44.8366146440901,55.3713206194967,
12.));
#153514=CARTESIAN_POINT('Ctrl Pts',(-44.8445846224044,55.3924090808014,
12.));
#153515=CARTESIAN_POINT('Ctrl Pts',(-44.8525495040408,55.4135484321718,
12.));
#153516=CARTESIAN_POINT('Ctrl Pts',(-44.8605091754214,55.4347385682704,
12.));
#153517=CARTESIAN_POINT('Ctrl Pts',(-44.8684635235725,55.4559793841836,
12.));
#153518=CARTESIAN_POINT('Ctrl Pts',(-44.8764124361206,55.4772707754126,
12.));
#153519=CARTESIAN_POINT('Ctrl Pts',(-44.8843558012886,55.4986126378656,
12.));
#153520=CARTESIAN_POINT('Ctrl Pts',(-44.8922935078889,55.5200048678629,
12.));
#153521=CARTESIAN_POINT('Ctrl Pts',(-44.9002254453183,55.541447362134,12.));
#153522=CARTESIAN_POINT('Ctrl Pts',(-44.908151503553,55.5629400178142,12.));
#153523=CARTESIAN_POINT('Ctrl Pts',(-44.9160715731443,55.5844827324338,
12.));
#153524=CARTESIAN_POINT('Ctrl Pts',(-44.9239855452144,55.6060754039121,
12.));
#153525=CARTESIAN_POINT('Ctrl Pts',(-44.9318933114506,55.6277179305633,
12.));
#153526=CARTESIAN_POINT('Ctrl Pts',(-44.9397947641006,55.6494102110935,
12.));
#153527=CARTESIAN_POINT('Ctrl Pts',(-44.9476897959684,55.6711521445979,
12.));
#153528=CARTESIAN_POINT('Ctrl Pts',(-44.9555783004106,55.6929436305489,
12.));
#153529=CARTESIAN_POINT('Ctrl Pts',(-44.9634601713321,55.714784568793,12.));
#153530=CARTESIAN_POINT('Ctrl Pts',(-44.9713353031804,55.7366748595552,
12.));
#153531=CARTESIAN_POINT('Ctrl Pts',(-44.9792035909413,55.7586144034367,
12.));
#153532=CARTESIAN_POINT('Ctrl Pts',(-44.9870649301342,55.7806031014106,
12.));
#153533=CARTESIAN_POINT('Ctrl Pts',(-44.9949192168093,55.8026408548105,
12.));
#153534=CARTESIAN_POINT('Ctrl Pts',(-45.0027663475433,55.8247275653289,
12.));
#153535=CARTESIAN_POINT('Ctrl Pts',(-45.0106062194342,55.8468631350218,
12.));
#153536=CARTESIAN_POINT('Ctrl Pts',(-45.0184387300973,55.8690474663065,
12.));
#153537=CARTESIAN_POINT('Ctrl Pts',(-45.0262637776614,55.8912804619577,
12.));
#153538=CARTESIAN_POINT('Ctrl Pts',(-45.0340812607657,55.9135620250954,
12.));
#153539=CARTESIAN_POINT('Ctrl Pts',(-45.041891078555,55.9358920591837,12.));
#153540=CARTESIAN_POINT('Ctrl Pts',(-45.0496931306755,55.9582704680356,
12.));
#153541=CARTESIAN_POINT('Ctrl Pts',(-45.0574873172694,55.9806971558097,
12.));
#153542=CARTESIAN_POINT('Ctrl Pts',(-45.0652735389733,56.003172027008,12.));
#153543=CARTESIAN_POINT('Ctrl Pts',(-45.0730516969148,56.0256949864639,
12.));
#153544=CARTESIAN_POINT('Ctrl Pts',(-45.0808216927089,56.048265939342,12.));
#153545=CARTESIAN_POINT('Ctrl Pts',(-45.0885834284517,56.0708847911416,
12.));
#153546=CARTESIAN_POINT('Ctrl Pts',(-45.0963368067177,56.0935514476945,
12.));
#153547=CARTESIAN_POINT('Ctrl Pts',(-45.1040817305561,56.116265815162,12.));
#153548=CARTESIAN_POINT('Ctrl Pts',(-45.1118181034888,56.1390278000226,
12.));
#153549=CARTESIAN_POINT('Ctrl Pts',(-45.1195458295062,56.1618373090732,
12.));
#153550=CARTESIAN_POINT('Ctrl Pts',(-45.127264813063,56.1846942494325,12.));
#153551=CARTESIAN_POINT('Ctrl Pts',(-45.1349749590737,56.2075985285393,
12.));
#153552=CARTESIAN_POINT('Ctrl Pts',(-45.1426761729105,56.230550054149,12.));
#153553=CARTESIAN_POINT('Ctrl Pts',(-45.1503683604005,56.2535487343221,
12.));
#153554=CARTESIAN_POINT('Ctrl Pts',(-45.1580514278223,56.2765944774245,
12.));
#153555=CARTESIAN_POINT('Ctrl Pts',(-45.1657252819013,56.2996871921316,
12.));
#153556=CARTESIAN_POINT('Ctrl Pts',(-45.173389829806,56.3228267874264,12.));
#153557=CARTESIAN_POINT('Ctrl Pts',(-45.1810449791453,56.3460131725964,
12.));
#153558=CARTESIAN_POINT('Ctrl Pts',(-45.1886906379667,56.3692462572231,
12.));
#153559=CARTESIAN_POINT('Ctrl Pts',(-45.1963267147529,56.3925259511806,
12.));
#153560=CARTESIAN_POINT('Ctrl Pts',(-45.2039531184171,56.4158521646411,
12.));
#153561=CARTESIAN_POINT('Ctrl Pts',(-45.2115697583,56.4392248080732,12.));
#153562=CARTESIAN_POINT('Ctrl Pts',(-45.2191765441666,56.4626437922386,
12.));
#153563=CARTESIAN_POINT('Ctrl Pts',(-45.2267733862049,56.4861090281823,
12.));
#153564=CARTESIAN_POINT('Ctrl Pts',(-45.2343601950227,56.5096204272306,
12.));
#153565=CARTESIAN_POINT('Ctrl Pts',(-45.2419368816428,56.5331779009958,
12.));
#153566=CARTESIAN_POINT('Ctrl Pts',(-45.2495033575,56.5567813613756,12.));
#153567=CARTESIAN_POINT('Ctrl Pts',(-45.257059534438,56.5804307205505,12.));
#153568=CARTESIAN_POINT('Ctrl Pts',(-45.2646053247087,56.6041258909741,
12.));
#153569=CARTESIAN_POINT('Ctrl Pts',(-45.2721406409695,56.6278667853702,
12.));
#153570=CARTESIAN_POINT('Ctrl Pts',(-45.2796653962785,56.6516533167384,
12.));
#153571=CARTESIAN_POINT('Ctrl Pts',(-45.2871795040906,56.6754853983528,
12.));
#153572=CARTESIAN_POINT('Ctrl Pts',(-45.2946828782559,56.69936294376,12.));
#153573=CARTESIAN_POINT('Ctrl Pts',(-45.3021754330178,56.7232858667709,
12.));
#153574=CARTESIAN_POINT('Ctrl Pts',(-45.3096570830117,56.7472540814554,
12.));
#153575=CARTESIAN_POINT('Ctrl Pts',(-45.31712774326,56.7712675021491,12.));
#153576=CARTESIAN_POINT('Ctrl Pts',(-45.3245873291684,56.7953260434524,
12.));
#153577=CARTESIAN_POINT('Ctrl Pts',(-45.332035756524,56.8194296202291,12.));
#153578=CARTESIAN_POINT('Ctrl Pts',(-45.3394729414931,56.8435781475981,
12.));
#153579=CARTESIAN_POINT('Ctrl Pts',(-45.3468988006203,56.8677715409268,
12.));
#153580=CARTESIAN_POINT('Ctrl Pts',(-45.3543132508238,56.8920097158377,
12.));
#153581=CARTESIAN_POINT('Ctrl Pts',(-45.3617162093922,56.9162925882085,
12.));
#153582=CARTESIAN_POINT('Ctrl Pts',(-45.3691075939826,56.9406200741714,
12.));
#153583=CARTESIAN_POINT('Ctrl Pts',(-45.3764873226196,56.9649920901073,
12.));
#153584=CARTESIAN_POINT('Ctrl Pts',(-45.3838553136948,56.9894085526373,
12.));
#153585=CARTESIAN_POINT('Ctrl Pts',(-45.3912114859616,57.0138693786278,
12.));
#153586=CARTESIAN_POINT('Ctrl Pts',(-45.3985557585311,57.0383744851913,
12.));
#153587=CARTESIAN_POINT('Ctrl Pts',(-45.4058880508693,57.0629237896848,
12.));
#153588=CARTESIAN_POINT('Ctrl Pts',(-45.4132082827948,57.0875172097051,
12.));
#153589=CARTESIAN_POINT('Ctrl Pts',(-45.4205163744781,57.112154663078,12.));
#153590=CARTESIAN_POINT('Ctrl Pts',(-45.4278122464389,57.136836067863,12.));
#153591=CARTESIAN_POINT('Ctrl Pts',(-45.4350958195433,57.1615613423584,
12.));
#153592=CARTESIAN_POINT('Ctrl Pts',(-45.4423670150034,57.186330405101,12.));
#153593=CARTESIAN_POINT('Ctrl Pts',(-45.4496257543759,57.2111431748631,
12.));
#153594=CARTESIAN_POINT('Ctrl Pts',(-45.4568719595641,57.2359995706447,
12.));
#153595=CARTESIAN_POINT('Ctrl Pts',(-45.4641055528141,57.2608995116733,
12.));
#153596=CARTESIAN_POINT('Ctrl Pts',(-45.4713264567063,57.2858429174062,
12.));
#153597=CARTESIAN_POINT('Ctrl Pts',(-45.4785345941507,57.3108297075265,
12.));
#153598=CARTESIAN_POINT('Ctrl Pts',(-45.4857298883824,57.3358598019389,
12.));
#153599=CARTESIAN_POINT('Ctrl Pts',(-45.4929122629572,57.3609331207574,
12.));
#153600=CARTESIAN_POINT('Ctrl Pts',(-45.5000816417509,57.3860495843033,
12.));
#153601=CARTESIAN_POINT('Ctrl Pts',(-45.5072379489631,57.4112091131183,
12.));
#153602=CARTESIAN_POINT('Ctrl Pts',(-45.5143811091205,57.4364116279702,
12.));
#153603=CARTESIAN_POINT('Ctrl Pts',(-45.5215110470825,57.4616570498568,
12.));
#153604=CARTESIAN_POINT('Ctrl Pts',(-45.5286276880484,57.4869453000063,
12.));
#153605=CARTESIAN_POINT('Ctrl Pts',(-45.5357309575611,57.5122762998745,
12.));
#153606=CARTESIAN_POINT('Ctrl Pts',(-45.542820781484,57.537649971135,12.));
#153607=CARTESIAN_POINT('Ctrl Pts',(-45.5498970859834,57.563066235668,12.));
#153608=CARTESIAN_POINT('Ctrl Pts',(-45.5569597975096,57.5885250155433,
12.));
#153609=CARTESIAN_POINT('Ctrl Pts',(-45.5640088427813,57.614026233004,12.));
#153610=CARTESIAN_POINT('Ctrl Pts',(-45.5710441487674,57.6395698104404,
12.));
#153611=CARTESIAN_POINT('Ctrl Pts',(-45.5780656427163,57.6651556704237,
12.));
#153612=CARTESIAN_POINT('Ctrl Pts',(-45.5850732521895,57.6907837357418,
12.));
#153613=CARTESIAN_POINT('Ctrl Pts',(-45.5920669050986,57.7164539294314,
12.));
#153614=CARTESIAN_POINT('Ctrl Pts',(-45.5990465297343,57.7421661748026,
12.));
#153615=CARTESIAN_POINT('Ctrl Pts',(-45.6060120548205,57.7679203954742,
12.));
#153616=CARTESIAN_POINT('Ctrl Pts',(-45.6129634094683,57.7937165153387,
12.));
#153617=CARTESIAN_POINT('Ctrl Pts',(-45.6199005230783,57.8195544584845,
12.));
#153618=CARTESIAN_POINT('Ctrl Pts',(-45.6268233252544,57.8454341491238,
12.));
#153619=CARTESIAN_POINT('Ctrl Pts',(-45.6337317457252,57.8713555115232,
12.));
#153620=CARTESIAN_POINT('Ctrl Pts',(-45.6406257142381,57.8973184699034,
12.));
#153621=CARTESIAN_POINT('Ctrl Pts',(-45.6475051605535,57.9233229484311,
12.));
#153622=CARTESIAN_POINT('Ctrl Pts',(-45.6543700146679,57.9493688714237,
12.));
#153623=CARTESIAN_POINT('Ctrl Pts',(-45.661220206992,57.9754561635061,12.));
#153624=CARTESIAN_POINT('Ctrl Pts',(-45.6680556685493,58.0015847497837,
12.));
#153625=CARTESIAN_POINT('Ctrl Pts',(-45.6748763311643,58.0277545560012,
12.));
#153626=CARTESIAN_POINT('Ctrl Pts',(-45.6816821276678,58.0539655087117,
12.));
#153627=CARTESIAN_POINT('Ctrl Pts',(-45.6884729914485,58.0802175348966,
12.));
#153628=CARTESIAN_POINT('Ctrl Pts',(-45.695248856015,58.1065105615907,12.));
#153629=CARTESIAN_POINT('Ctrl Pts',(-45.702009654518,58.1328445154676,12.));
#153630=CARTESIAN_POINT('Ctrl Pts',(-45.7087553193771,58.1592193225137,
12.));
#153631=CARTESIAN_POINT('Ctrl Pts',(-45.7154857816483,58.185634907469,12.));
#153632=CARTESIAN_POINT('Ctrl Pts',(-45.7222009715397,58.2120911942772,
12.));
#153633=CARTESIAN_POINT('Ctrl Pts',(-45.7289008195578,58.2385881070913,
12.));
#153634=CARTESIAN_POINT('Ctrl Pts',(-45.7355852575106,58.2651255711453,
12.));
#153635=CARTESIAN_POINT('Ctrl Pts',(-45.742254219463,58.291703513584,12.));
#153636=CARTESIAN_POINT('Ctrl Pts',(-45.7489076429763,58.3183218645317,
12.));
#153637=CARTESIAN_POINT('Ctrl Pts',(-45.755545469402,58.3449805573423,12.));
#153638=CARTESIAN_POINT('Ctrl Pts',(-45.7612219538124,58.3678667473438,
12.));
#153639=CARTESIAN_POINT('Ctrl Pts',(-45.7655655205367,58.3854348517444,
12.));
#153640=CARTESIAN_POINT('Ctrl Pts',(-45.7685831165565,58.397667048107,12.));
#153641=CARTESIAN_POINT('Ctrl Pts',(-45.7702793558177,58.4045515723357,
12.));
#153642=CARTESIAN_POINT('Ctrl Pts',(-45.7706564944896,58.4060826907797,
12.));
#153643=CARTESIAN_POINT('',(-44.3377168516418,54.1679505278134,0.));
#153644=CARTESIAN_POINT('',(-44.3377168516418,54.1679505278134,0.));
#153645=CARTESIAN_POINT('Ctrl Pts',(-45.7706564944896,58.4060826907797,
0.));
#153646=CARTESIAN_POINT('Ctrl Pts',(-45.7702793558177,58.4045515723357,
0.));
#153647=CARTESIAN_POINT('Ctrl Pts',(-45.7685831165565,58.397667048107,0.));
#153648=CARTESIAN_POINT('Ctrl Pts',(-45.7655655205367,58.3854348517444,
0.));
#153649=CARTESIAN_POINT('Ctrl Pts',(-45.7612219538124,58.3678667473437,
0.));
#153650=CARTESIAN_POINT('Ctrl Pts',(-45.755545469402,58.3449805573423,0.));
#153651=CARTESIAN_POINT('Ctrl Pts',(-45.7489076429763,58.3183218645317,
0.));
#153652=CARTESIAN_POINT('Ctrl Pts',(-45.742254219463,58.291703513584,0.));
#153653=CARTESIAN_POINT('Ctrl Pts',(-45.7355852575106,58.2651255711453,
0.));
#153654=CARTESIAN_POINT('Ctrl Pts',(-45.7289008195578,58.2385881070913,
0.));
#153655=CARTESIAN_POINT('Ctrl Pts',(-45.7222009715397,58.2120911942772,
0.));
#153656=CARTESIAN_POINT('Ctrl Pts',(-45.7154857816483,58.185634907469,0.));
#153657=CARTESIAN_POINT('Ctrl Pts',(-45.7087553193771,58.1592193225137,
0.));
#153658=CARTESIAN_POINT('Ctrl Pts',(-45.702009654518,58.1328445154676,0.));
#153659=CARTESIAN_POINT('Ctrl Pts',(-45.695248856015,58.1065105615907,0.));
#153660=CARTESIAN_POINT('Ctrl Pts',(-45.6884729914485,58.0802175348966,
0.));
#153661=CARTESIAN_POINT('Ctrl Pts',(-45.6816821276678,58.0539655087117,
0.));
#153662=CARTESIAN_POINT('Ctrl Pts',(-45.6748763311643,58.0277545560012,
0.));
#153663=CARTESIAN_POINT('Ctrl Pts',(-45.6680556685493,58.0015847497837,
0.));
#153664=CARTESIAN_POINT('Ctrl Pts',(-45.661220206992,57.9754561635061,0.));
#153665=CARTESIAN_POINT('Ctrl Pts',(-45.6543700146679,57.9493688714237,
0.));
#153666=CARTESIAN_POINT('Ctrl Pts',(-45.6475051605535,57.9233229484311,
0.));
#153667=CARTESIAN_POINT('Ctrl Pts',(-45.6406257142381,57.8973184699034,
0.));
#153668=CARTESIAN_POINT('Ctrl Pts',(-45.6337317457252,57.8713555115232,
0.));
#153669=CARTESIAN_POINT('Ctrl Pts',(-45.6268233252544,57.8454341491238,
0.));
#153670=CARTESIAN_POINT('Ctrl Pts',(-45.6199005230783,57.8195544584845,
0.));
#153671=CARTESIAN_POINT('Ctrl Pts',(-45.6129634094683,57.7937165153387,
0.));
#153672=CARTESIAN_POINT('Ctrl Pts',(-45.6060120548205,57.7679203954742,
0.));
#153673=CARTESIAN_POINT('Ctrl Pts',(-45.5990465297343,57.7421661748026,
0.));
#153674=CARTESIAN_POINT('Ctrl Pts',(-45.5920669050986,57.7164539294314,
0.));
#153675=CARTESIAN_POINT('Ctrl Pts',(-45.5850732521895,57.6907837357418,
0.));
#153676=CARTESIAN_POINT('Ctrl Pts',(-45.5780656427163,57.6651556704237,
0.));
#153677=CARTESIAN_POINT('Ctrl Pts',(-45.5710441487674,57.6395698104404,
0.));
#153678=CARTESIAN_POINT('Ctrl Pts',(-45.5640088427813,57.614026233004,0.));
#153679=CARTESIAN_POINT('Ctrl Pts',(-45.5569597975096,57.5885250155433,
0.));
#153680=CARTESIAN_POINT('Ctrl Pts',(-45.5498970859834,57.563066235668,0.));
#153681=CARTESIAN_POINT('Ctrl Pts',(-45.542820781484,57.537649971135,0.));
#153682=CARTESIAN_POINT('Ctrl Pts',(-45.5357309575611,57.5122762998745,
0.));
#153683=CARTESIAN_POINT('Ctrl Pts',(-45.5286276880484,57.4869453000063,
0.));
#153684=CARTESIAN_POINT('Ctrl Pts',(-45.5215110470825,57.4616570498568,
0.));
#153685=CARTESIAN_POINT('Ctrl Pts',(-45.5143811091205,57.4364116279702,
0.));
#153686=CARTESIAN_POINT('Ctrl Pts',(-45.5072379489631,57.4112091131183,
0.));
#153687=CARTESIAN_POINT('Ctrl Pts',(-45.5000816417509,57.3860495843033,
0.));
#153688=CARTESIAN_POINT('Ctrl Pts',(-45.4929122629572,57.3609331207574,
0.));
#153689=CARTESIAN_POINT('Ctrl Pts',(-45.4857298883824,57.3358598019389,
0.));
#153690=CARTESIAN_POINT('Ctrl Pts',(-45.4785345941507,57.3108297075265,
0.));
#153691=CARTESIAN_POINT('Ctrl Pts',(-45.4713264567063,57.2858429174062,
0.));
#153692=CARTESIAN_POINT('Ctrl Pts',(-45.4641055528141,57.2608995116733,
0.));
#153693=CARTESIAN_POINT('Ctrl Pts',(-45.4568719595641,57.2359995706447,
0.));
#153694=CARTESIAN_POINT('Ctrl Pts',(-45.4496257543759,57.2111431748631,
0.));
#153695=CARTESIAN_POINT('Ctrl Pts',(-45.4423670150034,57.186330405101,0.));
#153696=CARTESIAN_POINT('Ctrl Pts',(-45.4350958195433,57.1615613423584,
0.));
#153697=CARTESIAN_POINT('Ctrl Pts',(-45.4278122464389,57.136836067863,0.));
#153698=CARTESIAN_POINT('Ctrl Pts',(-45.4205163744781,57.112154663078,0.));
#153699=CARTESIAN_POINT('Ctrl Pts',(-45.4132082827948,57.0875172097051,
0.));
#153700=CARTESIAN_POINT('Ctrl Pts',(-45.4058880508693,57.0629237896848,
0.));
#153701=CARTESIAN_POINT('Ctrl Pts',(-45.3985557585311,57.0383744851913,
0.));
#153702=CARTESIAN_POINT('Ctrl Pts',(-45.3912114859616,57.0138693786278,
0.));
#153703=CARTESIAN_POINT('Ctrl Pts',(-45.3838553136948,56.9894085526373,
0.));
#153704=CARTESIAN_POINT('Ctrl Pts',(-45.3764873226196,56.9649920901073,
0.));
#153705=CARTESIAN_POINT('Ctrl Pts',(-45.3691075939826,56.9406200741714,
0.));
#153706=CARTESIAN_POINT('Ctrl Pts',(-45.3617162093922,56.9162925882085,
0.));
#153707=CARTESIAN_POINT('Ctrl Pts',(-45.3543132508238,56.8920097158377,
0.));
#153708=CARTESIAN_POINT('Ctrl Pts',(-45.3468988006203,56.8677715409268,
0.));
#153709=CARTESIAN_POINT('Ctrl Pts',(-45.3394729414931,56.8435781475981,
0.));
#153710=CARTESIAN_POINT('Ctrl Pts',(-45.332035756524,56.8194296202291,0.));
#153711=CARTESIAN_POINT('Ctrl Pts',(-45.3245873291684,56.7953260434524,
0.));
#153712=CARTESIAN_POINT('Ctrl Pts',(-45.31712774326,56.7712675021491,0.));
#153713=CARTESIAN_POINT('Ctrl Pts',(-45.3096570830117,56.7472540814554,
0.));
#153714=CARTESIAN_POINT('Ctrl Pts',(-45.3021754330178,56.7232858667709,
0.));
#153715=CARTESIAN_POINT('Ctrl Pts',(-45.2946828782559,56.69936294376,0.));
#153716=CARTESIAN_POINT('Ctrl Pts',(-45.2871795040906,56.6754853983528,
0.));
#153717=CARTESIAN_POINT('Ctrl Pts',(-45.2796653962785,56.6516533167384,
0.));
#153718=CARTESIAN_POINT('Ctrl Pts',(-45.2721406409695,56.6278667853702,
0.));
#153719=CARTESIAN_POINT('Ctrl Pts',(-45.2646053247087,56.6041258909741,
0.));
#153720=CARTESIAN_POINT('Ctrl Pts',(-45.257059534438,56.5804307205505,0.));
#153721=CARTESIAN_POINT('Ctrl Pts',(-45.2495033575,56.5567813613756,0.));
#153722=CARTESIAN_POINT('Ctrl Pts',(-45.2419368816428,56.5331779009958,
0.));
#153723=CARTESIAN_POINT('Ctrl Pts',(-45.2343601950227,56.5096204272306,
0.));
#153724=CARTESIAN_POINT('Ctrl Pts',(-45.2267733862049,56.4861090281823,
0.));
#153725=CARTESIAN_POINT('Ctrl Pts',(-45.2191765441666,56.4626437922386,
0.));
#153726=CARTESIAN_POINT('Ctrl Pts',(-45.2115697583,56.4392248080732,0.));
#153727=CARTESIAN_POINT('Ctrl Pts',(-45.2039531184171,56.4158521646411,
0.));
#153728=CARTESIAN_POINT('Ctrl Pts',(-45.1963267147529,56.3925259511806,
0.));
#153729=CARTESIAN_POINT('Ctrl Pts',(-45.1886906379667,56.3692462572231,
0.));
#153730=CARTESIAN_POINT('Ctrl Pts',(-45.1810449791453,56.3460131725964,
0.));
#153731=CARTESIAN_POINT('Ctrl Pts',(-45.173389829806,56.3228267874264,0.));
#153732=CARTESIAN_POINT('Ctrl Pts',(-45.1657252819013,56.2996871921316,
0.));
#153733=CARTESIAN_POINT('Ctrl Pts',(-45.1580514278223,56.2765944774245,
0.));
#153734=CARTESIAN_POINT('Ctrl Pts',(-45.1503683604005,56.2535487343221,
0.));
#153735=CARTESIAN_POINT('Ctrl Pts',(-45.1426761729105,56.230550054149,0.));
#153736=CARTESIAN_POINT('Ctrl Pts',(-45.1349749590737,56.2075985285393,
0.));
#153737=CARTESIAN_POINT('Ctrl Pts',(-45.127264813063,56.1846942494325,0.));
#153738=CARTESIAN_POINT('Ctrl Pts',(-45.1195458295062,56.1618373090732,
0.));
#153739=CARTESIAN_POINT('Ctrl Pts',(-45.1118181034888,56.1390278000226,
0.));
#153740=CARTESIAN_POINT('Ctrl Pts',(-45.1040817305561,56.116265815162,0.));
#153741=CARTESIAN_POINT('Ctrl Pts',(-45.0963368067177,56.0935514476945,
0.));
#153742=CARTESIAN_POINT('Ctrl Pts',(-45.0885834284517,56.0708847911416,
0.));
#153743=CARTESIAN_POINT('Ctrl Pts',(-45.0808216927089,56.048265939342,0.));
#153744=CARTESIAN_POINT('Ctrl Pts',(-45.0730516969148,56.0256949864639,
0.));
#153745=CARTESIAN_POINT('Ctrl Pts',(-45.0652735389733,56.003172027008,0.));
#153746=CARTESIAN_POINT('Ctrl Pts',(-45.0574873172694,55.9806971558097,
0.));
#153747=CARTESIAN_POINT('Ctrl Pts',(-45.0496931306755,55.9582704680356,
0.));
#153748=CARTESIAN_POINT('Ctrl Pts',(-45.041891078555,55.9358920591837,0.));
#153749=CARTESIAN_POINT('Ctrl Pts',(-45.0340812607657,55.9135620250954,
0.));
#153750=CARTESIAN_POINT('Ctrl Pts',(-45.0262637776614,55.8912804619577,
0.));
#153751=CARTESIAN_POINT('Ctrl Pts',(-45.0184387300973,55.8690474663065,
0.));
#153752=CARTESIAN_POINT('Ctrl Pts',(-45.0106062194342,55.8468631350218,
0.));
#153753=CARTESIAN_POINT('Ctrl Pts',(-45.0027663475433,55.8247275653289,
0.));
#153754=CARTESIAN_POINT('Ctrl Pts',(-44.9949192168093,55.8026408548105,
0.));
#153755=CARTESIAN_POINT('Ctrl Pts',(-44.9870649301342,55.7806031014106,
0.));
#153756=CARTESIAN_POINT('Ctrl Pts',(-44.9792035909413,55.7586144034367,
0.));
#153757=CARTESIAN_POINT('Ctrl Pts',(-44.9713353031804,55.7366748595552,
0.));
#153758=CARTESIAN_POINT('Ctrl Pts',(-44.9634601713321,55.714784568793,0.));
#153759=CARTESIAN_POINT('Ctrl Pts',(-44.9555783004106,55.6929436305489,
0.));
#153760=CARTESIAN_POINT('Ctrl Pts',(-44.9476897959684,55.6711521445979,
0.));
#153761=CARTESIAN_POINT('Ctrl Pts',(-44.9397947641006,55.6494102110935,
0.));
#153762=CARTESIAN_POINT('Ctrl Pts',(-44.9318933114506,55.6277179305633,
0.));
#153763=CARTESIAN_POINT('Ctrl Pts',(-44.9239855452144,55.6060754039121,
0.));
#153764=CARTESIAN_POINT('Ctrl Pts',(-44.9160715731443,55.5844827324338,
0.));
#153765=CARTESIAN_POINT('Ctrl Pts',(-44.908151503553,55.5629400178142,0.));
#153766=CARTESIAN_POINT('Ctrl Pts',(-44.9002254453183,55.541447362134,0.));
#153767=CARTESIAN_POINT('Ctrl Pts',(-44.8922935078889,55.5200048678629,
0.));
#153768=CARTESIAN_POINT('Ctrl Pts',(-44.8843558012886,55.4986126378656,
0.));
#153769=CARTESIAN_POINT('Ctrl Pts',(-44.8764124361206,55.4772707754126,
0.));
#153770=CARTESIAN_POINT('Ctrl Pts',(-44.8684635235725,55.4559793841836,
0.));
#153771=CARTESIAN_POINT('Ctrl Pts',(-44.8605091754214,55.4347385682704,
0.));
#153772=CARTESIAN_POINT('Ctrl Pts',(-44.8525495040408,55.4135484321718,
0.));
#153773=CARTESIAN_POINT('Ctrl Pts',(-44.8445846224044,55.3924090808014,
0.));
#153774=CARTESIAN_POINT('Ctrl Pts',(-44.8366146440901,55.3713206194967,
0.));
#153775=CARTESIAN_POINT('Ctrl Pts',(-44.8286396832847,55.3502831540228,
0.));
#153776=CARTESIAN_POINT('Ctrl Pts',(-44.8206598547887,55.3292967905725,
0.));
#153777=CARTESIAN_POINT('Ctrl Pts',(-44.8126752740208,55.3083616357605,
0.));
#153778=CARTESIAN_POINT('Ctrl Pts',(-44.8046860570244,55.287477796635,0.));
#153779=CARTESIAN_POINT('Ctrl Pts',(-44.796692320474,55.2666453806883,0.));
#153780=CARTESIAN_POINT('Ctrl Pts',(-44.7886941816823,55.2458644958617,
0.));
#153781=CARTESIAN_POINT('Ctrl Pts',(-44.7806917586077,55.2251352505474,
0.));
#153782=CARTESIAN_POINT('Ctrl Pts',(-44.7726851698618,55.2044577535865,
0.));
#153783=CARTESIAN_POINT('Ctrl Pts',(-44.7646745347108,55.1838321142777,
0.));
#153784=CARTESIAN_POINT('Ctrl Pts',(-44.7566599730771,55.1632584423813,
0.));
#153785=CARTESIAN_POINT('Ctrl Pts',(-44.7486416055419,55.1427368481201,
0.));
#153786=CARTESIAN_POINT('Ctrl Pts',(-44.7406195533482,55.1222674421747,
0.));
#153787=CARTESIAN_POINT('Ctrl Pts',(-44.7325939384042,55.1018503356806,
0.));
#153788=CARTESIAN_POINT('Ctrl Pts',(-44.7245648832988,55.0814856402507,
0.));
#153789=CARTESIAN_POINT('Ctrl Pts',(-44.7165325113165,55.0611734679902,
0.));
#153790=CARTESIAN_POINT('Ctrl Pts',(-44.7084969464509,55.0409139315074,
0.));
#153791=CARTESIAN_POINT('Ctrl Pts',(-44.7004583134235,55.020707143922,0.));
#153792=CARTESIAN_POINT('Ctrl Pts',(-44.6924167376851,55.0005532188644,
0.));
#153793=CARTESIAN_POINT('Ctrl Pts',(-44.6843723453985,54.9804522704668,
0.));
#153794=CARTESIAN_POINT('Ctrl Pts',(-44.6763252634255,54.9604044133497,
0.));
#153795=CARTESIAN_POINT('Ctrl Pts',(-44.6682756193155,54.9404097626088,
0.));
#153796=CARTESIAN_POINT('Ctrl Pts',(-44.6602235412853,54.9204684337845,
0.));
#153797=CARTESIAN_POINT('Ctrl Pts',(-44.6521691582551,54.9005805428991,
0.));
#153798=CARTESIAN_POINT('Ctrl Pts',(-44.6441125999074,54.8807462065177,
0.));
#153799=CARTESIAN_POINT('Ctrl Pts',(-44.6360539967392,54.860965541796,0.));
#153800=CARTESIAN_POINT('Ctrl Pts',(-44.6279934801159,54.8412386665264,
0.));
#153801=CARTESIAN_POINT('Ctrl Pts',(-44.6199311823276,54.8215656991817,
0.));
#153802=CARTESIAN_POINT('Ctrl Pts',(-44.6118672364889,54.8019467588258,
0.));
#153803=CARTESIAN_POINT('Ctrl Pts',(-44.60380177643,54.7823819650137,0.));
#153804=CARTESIAN_POINT('Ctrl Pts',(-44.5957349366062,54.7628714377042,
0.));
#153805=CARTESIAN_POINT('Ctrl Pts',(-44.5876668519676,54.7434152971285,
0.));
#153806=CARTESIAN_POINT('Ctrl Pts',(-44.5795976579476,54.7240136637744,
0.));
#153807=CARTESIAN_POINT('Ctrl Pts',(-44.5715274907637,54.7046666586777,
0.));
#153808=CARTESIAN_POINT('Ctrl Pts',(-44.5634564876869,54.685374403676,0.));
#153809=CARTESIAN_POINT('Ctrl Pts',(-44.5553847872712,54.6661370216242,
0.));
#153810=CARTESIAN_POINT('Ctrl Pts',(-44.5473125297289,54.6469546367381,
0.));
#153811=CARTESIAN_POINT('Ctrl Pts',(-44.5392398566775,54.6278273743554,
0.));
#153812=CARTESIAN_POINT('Ctrl Pts',(-44.5311669104494,54.6087553602889,
0.));
#153813=CARTESIAN_POINT('Ctrl Pts',(-44.5230938335165,54.5897387202812,
0.));
#153814=CARTESIAN_POINT('Ctrl Pts',(-44.5150207679007,54.5707775794436,
0.));
#153815=CARTESIAN_POINT('Ctrl Pts',(-44.5069478544977,54.5518720616056,
0.));
#153816=CARTESIAN_POINT('Ctrl Pts',(-44.4988752343744,54.5330222905475,
0.));
#153817=CARTESIAN_POINT('Ctrl Pts',(-44.4908030503225,54.5142283914704,
0.));
#153818=CARTESIAN_POINT('Ctrl Pts',(-44.4827314481264,54.495490492193,0.));
#153819=CARTESIAN_POINT('Ctrl Pts',(-44.4746605784031,54.4768087248824,
0.));
#153820=CARTESIAN_POINT('Ctrl Pts',(-44.4665905967668,54.4581832262033,
0.));
#153821=CARTESIAN_POINT('Ctrl Pts',(-44.4585216599907,54.4396141336978,
0.));
#153822=CARTESIAN_POINT('Ctrl Pts',(-44.4504539226327,54.421101582595,0.));
#153823=CARTESIAN_POINT('Ctrl Pts',(-44.4423875340995,54.4026457030335,
0.));
#153824=CARTESIAN_POINT('Ctrl Pts',(-44.4343226339592,54.3842466156196,
0.));
#153825=CARTESIAN_POINT('Ctrl Pts',(-44.4262593564712,54.3659044357119,
0.));
#153826=CARTESIAN_POINT('Ctrl Pts',(-44.4181978395851,54.3476192819352,
0.));
#153827=CARTESIAN_POINT('Ctrl Pts',(-44.4101382321834,54.3293912830237,
0.));
#153828=CARTESIAN_POINT('Ctrl Pts',(-44.402080702809,54.3112205860716,0.));
#153829=CARTESIAN_POINT('Ctrl Pts',(-44.3940254456331,54.2931073621553,
0.));
#153830=CARTESIAN_POINT('Ctrl Pts',(-44.3859726620183,54.2750517888579,
0.));
#153831=CARTESIAN_POINT('Ctrl Pts',(-44.3779225430405,54.2570540336475,
0.));
#153832=CARTESIAN_POINT('Ctrl Pts',(-44.3698752533561,54.2391142386412,
0.));
#153833=CARTESIAN_POINT('Ctrl Pts',(-44.361830910343,54.2212325006052,0.));
#153834=CARTESIAN_POINT('Ctrl Pts',(-44.3537895824096,54.2034088701928,
0.));
#153835=CARTESIAN_POINT('Ctrl Pts',(-44.3473589597726,54.1891964684727,
0.));
#153836=CARTESIAN_POINT('Ctrl Pts',(-44.3425373700993,54.1785633257639,
0.));
#153837=CARTESIAN_POINT('Ctrl Pts',(-44.3393235891075,54.1714861895346,
0.));
#153838=CARTESIAN_POINT('Ctrl Pts',(-44.3377168516418,54.1679505278134,
0.));
#153839=CARTESIAN_POINT('Ctrl Pts',(-40.5543412808469,62.494763006804,0.));
#153840=CARTESIAN_POINT('Ctrl Pts',(-40.5543412808469,62.494763006804,12.));
#153841=CARTESIAN_POINT('Ctrl Pts',(-40.5535399497519,62.489224912198,0.));
#153842=CARTESIAN_POINT('Ctrl Pts',(-40.5535399497519,62.489224912198,12.));
#153843=CARTESIAN_POINT('Ctrl Pts',(-40.5519353177252,62.4781525156318,
0.));
#153844=CARTESIAN_POINT('Ctrl Pts',(-40.5519353177252,62.4781525156318,
12.));
#153845=CARTESIAN_POINT('Ctrl Pts',(-40.5495224601758,62.4615552987202,
0.));
#153846=CARTESIAN_POINT('Ctrl Pts',(-40.5495224601758,62.4615552987202,
12.));
#153847=CARTESIAN_POINT('Ctrl Pts',(-40.5462934972718,62.4394484329678,
0.));
#153848=CARTESIAN_POINT('Ctrl Pts',(-40.5462934972718,62.4394484329678,
12.));
#153849=CARTESIAN_POINT('Ctrl Pts',(-40.5422375945026,62.4118527881148,
0.));
#153850=CARTESIAN_POINT('Ctrl Pts',(-40.5422375945026,62.4118527881148,
12.));
#153851=CARTESIAN_POINT('Ctrl Pts',(-40.5381619974169,62.3842950992833,
0.));
#153852=CARTESIAN_POINT('Ctrl Pts',(-40.5381619974169,62.3842950992833,
12.));
#153853=CARTESIAN_POINT('Ctrl Pts',(-40.5340667194319,62.3567753970279,
0.));
#153854=CARTESIAN_POINT('Ctrl Pts',(-40.5340667194319,62.3567753970279,
12.));
#153855=CARTESIAN_POINT('Ctrl Pts',(-40.5299517857721,62.3292937257901,
0.));
#153856=CARTESIAN_POINT('Ctrl Pts',(-40.5299517857721,62.3292937257901,
12.));
#153857=CARTESIAN_POINT('Ctrl Pts',(-40.5258172381428,62.301850147165,0.));
#153858=CARTESIAN_POINT('Ctrl Pts',(-40.5258172381428,62.301850147165,12.));
#153859=CARTESIAN_POINT('Ctrl Pts',(-40.5216631336193,62.2744447381971,
0.));
#153860=CARTESIAN_POINT('Ctrl Pts',(-40.5216631336193,62.2744447381971,
12.));
#153861=CARTESIAN_POINT('Ctrl Pts',(-40.5174895390954,62.247077585866,0.));
#153862=CARTESIAN_POINT('Ctrl Pts',(-40.5174895390954,62.247077585866,12.));
#153863=CARTESIAN_POINT('Ctrl Pts',(-40.5132965269633,62.2197487826136,
0.));
#153864=CARTESIAN_POINT('Ctrl Pts',(-40.5132965269633,62.2197487826136,
12.));
#153865=CARTESIAN_POINT('Ctrl Pts',(-40.5090841704122,62.1924584215653,
0.));
#153866=CARTESIAN_POINT('Ctrl Pts',(-40.5090841704122,62.1924584215653,
12.));
#153867=CARTESIAN_POINT('Ctrl Pts',(-40.5048525386035,62.1652065915808,
0.));
#153868=CARTESIAN_POINT('Ctrl Pts',(-40.5048525386035,62.1652065915808,
12.));
#153869=CARTESIAN_POINT('Ctrl Pts',(-40.5006016927554,62.1379933732528,
0.));
#153870=CARTESIAN_POINT('Ctrl Pts',(-40.5006016927554,62.1379933732528,
12.));
#153871=CARTESIAN_POINT('Ctrl Pts',(-40.4963316888412,62.1108188417003,
0.));
#153872=CARTESIAN_POINT('Ctrl Pts',(-40.4963316888412,62.1108188417003,
12.));
#153873=CARTESIAN_POINT('Ctrl Pts',(-40.4920425795216,62.0836830685719,
0.));
#153874=CARTESIAN_POINT('Ctrl Pts',(-40.4920425795216,62.0836830685719,
12.));
#153875=CARTESIAN_POINT('Ctrl Pts',(-40.4877344164411,62.0565861244179,
0.));
#153876=CARTESIAN_POINT('Ctrl Pts',(-40.4877344164411,62.0565861244179,
12.));
#153877=CARTESIAN_POINT('Ctrl Pts',(-40.4834072522164,62.029528080742,0.));
#153878=CARTESIAN_POINT('Ctrl Pts',(-40.4834072522164,62.029528080742,12.));
#153879=CARTESIAN_POINT('Ctrl Pts',(-40.4790611429583,62.0025090125959,
0.));
#153880=CARTESIAN_POINT('Ctrl Pts',(-40.4790611429583,62.0025090125959,
12.));
#153881=CARTESIAN_POINT('Ctrl Pts',(-40.4746961480015,61.9755289983044,
0.));
#153882=CARTESIAN_POINT('Ctrl Pts',(-40.4746961480015,61.9755289983044,
12.));
#153883=CARTESIAN_POINT('Ctrl Pts',(-40.470312328762,61.9485881182921,0.));
#153884=CARTESIAN_POINT('Ctrl Pts',(-40.470312328762,61.9485881182921,12.));
#153885=CARTESIAN_POINT('Ctrl Pts',(-40.4659097478587,61.9216864541744,
0.));
#153886=CARTESIAN_POINT('Ctrl Pts',(-40.4659097478587,61.9216864541744,
12.));
#153887=CARTESIAN_POINT('Ctrl Pts',(-40.4614884681889,61.8948240878008,
0.));
#153888=CARTESIAN_POINT('Ctrl Pts',(-40.4614884681889,61.8948240878008,
12.));
#153889=CARTESIAN_POINT('Ctrl Pts',(-40.4570485518749,61.8680011001537,
0.));
#153890=CARTESIAN_POINT('Ctrl Pts',(-40.4570485518749,61.8680011001537,
12.));
#153891=CARTESIAN_POINT('Ctrl Pts',(-40.4525900597894,61.8412175708552,
0.));
#153892=CARTESIAN_POINT('Ctrl Pts',(-40.4525900597894,61.8412175708552,
12.));
#153893=CARTESIAN_POINT('Ctrl Pts',(-40.4481130521364,61.814473578779,0.));
#153894=CARTESIAN_POINT('Ctrl Pts',(-40.4481130521364,61.814473578779,12.));
#153895=CARTESIAN_POINT('Ctrl Pts',(-40.4436175887949,61.7877692024076,
0.));
#153896=CARTESIAN_POINT('Ctrl Pts',(-40.4436175887949,61.7877692024076,
12.));
#153897=CARTESIAN_POINT('Ctrl Pts',(-40.4391037297588,61.7611045202874,
0.));
#153898=CARTESIAN_POINT('Ctrl Pts',(-40.4391037297588,61.7611045202874,
12.));
#153899=CARTESIAN_POINT('Ctrl Pts',(-40.4345715355404,61.7344796114399,
0.));
#153900=CARTESIAN_POINT('Ctrl Pts',(-40.4345715355404,61.7344796114399,
12.));
#153901=CARTESIAN_POINT('Ctrl Pts',(-40.430021067584,61.7078945557799,0.));
#153902=CARTESIAN_POINT('Ctrl Pts',(-40.430021067584,61.7078945557799,12.));
#153903=CARTESIAN_POINT('Ctrl Pts',(-40.425452388076,61.6813494339286,0.));
#153904=CARTESIAN_POINT('Ctrl Pts',(-40.425452388076,61.6813494339286,12.));
#153905=CARTESIAN_POINT('Ctrl Pts',(-40.4208655597717,61.6548443270394,
0.));
#153906=CARTESIAN_POINT('Ctrl Pts',(-40.4208655597717,61.6548443270394,
12.));
#153907=CARTESIAN_POINT('Ctrl Pts',(-40.4162606458119,61.628379316608,0.));
#153908=CARTESIAN_POINT('Ctrl Pts',(-40.4162606458119,61.628379316608,12.));
#153909=CARTESIAN_POINT('Ctrl Pts',(-40.4116377095596,61.601954484301,0.));
#153910=CARTESIAN_POINT('Ctrl Pts',(-40.4116377095596,61.601954484301,12.));
#153911=CARTESIAN_POINT('Ctrl Pts',(-40.4069968143956,61.5755699117324,
0.));
#153912=CARTESIAN_POINT('Ctrl Pts',(-40.4069968143956,61.5755699117324,
12.));
#153913=CARTESIAN_POINT('Ctrl Pts',(-40.4023380237232,61.5492256804717,
0.));
#153914=CARTESIAN_POINT('Ctrl Pts',(-40.4023380237232,61.5492256804717,
12.));
#153915=CARTESIAN_POINT('Ctrl Pts',(-40.3976614010652,61.522921872154,0.));
#153916=CARTESIAN_POINT('Ctrl Pts',(-40.3976614010652,61.522921872154,12.));
#153917=CARTESIAN_POINT('Ctrl Pts',(-40.3929670101366,61.4966585685549,
0.));
#153918=CARTESIAN_POINT('Ctrl Pts',(-40.3929670101366,61.4966585685549,
12.));
#153919=CARTESIAN_POINT('Ctrl Pts',(-40.3882549149227,61.4704358516709,
0.));
#153920=CARTESIAN_POINT('Ctrl Pts',(-40.3882549149227,61.4704358516709,
12.));
#153921=CARTESIAN_POINT('Ctrl Pts',(-40.383525179772,61.4442538038044,0.));
#153922=CARTESIAN_POINT('Ctrl Pts',(-40.383525179772,61.4442538038044,12.));
#153923=CARTESIAN_POINT('Ctrl Pts',(-40.3787778694364,61.4181125076037,
0.));
#153924=CARTESIAN_POINT('Ctrl Pts',(-40.3787778694364,61.4181125076037,
12.));
#153925=CARTESIAN_POINT('Ctrl Pts',(-40.3740130490225,61.3920120460219,
0.));
#153926=CARTESIAN_POINT('Ctrl Pts',(-40.3740130490225,61.3920120460219,
12.));
#153927=CARTESIAN_POINT('Ctrl Pts',(-40.3692307839636,61.3659525022908,
0.));
#153928=CARTESIAN_POINT('Ctrl Pts',(-40.3692307839636,61.3659525022908,
12.));
#153929=CARTESIAN_POINT('Ctrl Pts',(-40.3644311399861,61.3399339598853,
0.));
#153930=CARTESIAN_POINT('Ctrl Pts',(-40.3644311399861,61.3399339598853,
12.));
#153931=CARTESIAN_POINT('Ctrl Pts',(-40.3596141830791,61.3139565024847,
0.));
#153932=CARTESIAN_POINT('Ctrl Pts',(-40.3596141830791,61.3139565024847,
12.));
#153933=CARTESIAN_POINT('Ctrl Pts',(-40.3547799794679,61.2880202139371,
0.));
#153934=CARTESIAN_POINT('Ctrl Pts',(-40.3547799794679,61.2880202139371,
12.));
#153935=CARTESIAN_POINT('Ctrl Pts',(-40.3499285956304,61.2621251782863,
0.));
#153936=CARTESIAN_POINT('Ctrl Pts',(-40.3499285956304,61.2621251782863,
12.));
#153937=CARTESIAN_POINT('Ctrl Pts',(-40.3450600983109,61.23627147979,0.));
#153938=CARTESIAN_POINT('Ctrl Pts',(-40.3450600983109,61.23627147979,12.));
#153939=CARTESIAN_POINT('Ctrl Pts',(-40.340174554537,61.2104592029377,0.));
#153940=CARTESIAN_POINT('Ctrl Pts',(-40.340174554537,61.2104592029377,12.));
#153941=CARTESIAN_POINT('Ctrl Pts',(-40.335272031637,61.1846884324644,0.));
#153942=CARTESIAN_POINT('Ctrl Pts',(-40.335272031637,61.1846884324644,12.));
#153943=CARTESIAN_POINT('Ctrl Pts',(-40.3303525972615,61.1589592533613,
0.));
#153944=CARTESIAN_POINT('Ctrl Pts',(-40.3303525972615,61.1589592533613,
12.));
#153945=CARTESIAN_POINT('Ctrl Pts',(-40.32541631938,61.1332717508789,0.));
#153946=CARTESIAN_POINT('Ctrl Pts',(-40.32541631938,61.1332717508789,12.));
#153947=CARTESIAN_POINT('Ctrl Pts',(-40.3204632662725,61.1076260105258,
0.));
#153948=CARTESIAN_POINT('Ctrl Pts',(-40.3204632662725,61.1076260105258,
12.));
#153949=CARTESIAN_POINT('Ctrl Pts',(-40.3154935065262,61.0820221180645,
0.));
#153950=CARTESIAN_POINT('Ctrl Pts',(-40.3154935065262,61.0820221180645,
12.));
#153951=CARTESIAN_POINT('Ctrl Pts',(-40.3105071090309,61.056460159505,0.));
#153952=CARTESIAN_POINT('Ctrl Pts',(-40.3105071090309,61.056460159505,12.));
#153953=CARTESIAN_POINT('Ctrl Pts',(-40.3055041429775,61.0309402210921,
0.));
#153954=CARTESIAN_POINT('Ctrl Pts',(-40.3055041429775,61.0309402210921,
12.));
#153955=CARTESIAN_POINT('Ctrl Pts',(-40.300484677858,61.0054623893066,0.));
#153956=CARTESIAN_POINT('Ctrl Pts',(-40.300484677858,61.0054623893066,12.));
#153957=CARTESIAN_POINT('Ctrl Pts',(-40.295448783469,60.9800267508786,0.));
#153958=CARTESIAN_POINT('Ctrl Pts',(-40.295448783469,60.9800267508786,12.));
#153959=CARTESIAN_POINT('Ctrl Pts',(-40.2903965299155,60.9546333927921,
0.));
#153960=CARTESIAN_POINT('Ctrl Pts',(-40.2903965299155,60.9546333927921,
12.));
#153961=CARTESIAN_POINT('Ctrl Pts',(-40.2853279876161,60.9292824022887,
0.));
#153962=CARTESIAN_POINT('Ctrl Pts',(-40.2853279876161,60.9292824022887,
12.));
#153963=CARTESIAN_POINT('Ctrl Pts',(-40.2802432273104,60.9039738668669,
0.));
#153964=CARTESIAN_POINT('Ctrl Pts',(-40.2802432273104,60.9039738668669,
12.));
#153965=CARTESIAN_POINT('Ctrl Pts',(-40.2751423200639,60.8787078742818,
0.));
#153966=CARTESIAN_POINT('Ctrl Pts',(-40.2751423200639,60.8787078742818,
12.));
#153967=CARTESIAN_POINT('Ctrl Pts',(-40.2700253372647,60.8534845125538,
0.));
#153968=CARTESIAN_POINT('Ctrl Pts',(-40.2700253372647,60.8534845125538,
12.));
#153969=CARTESIAN_POINT('Ctrl Pts',(-40.2648923506248,60.8283038699706,
0.));
#153970=CARTESIAN_POINT('Ctrl Pts',(-40.2648923506248,60.8283038699706,
12.));
#153971=CARTESIAN_POINT('Ctrl Pts',(-40.2597434321803,60.8031660350879,
0.));
#153972=CARTESIAN_POINT('Ctrl Pts',(-40.2597434321803,60.8031660350879,
12.));
#153973=CARTESIAN_POINT('Ctrl Pts',(-40.2545786542953,60.7780710967248,
0.));
#153974=CARTESIAN_POINT('Ctrl Pts',(-40.2545786542953,60.7780710967248,
12.));
#153975=CARTESIAN_POINT('Ctrl Pts',(-40.2493980896638,60.7530191439593,
0.));
#153976=CARTESIAN_POINT('Ctrl Pts',(-40.2493980896638,60.7530191439593,
12.));
#153977=CARTESIAN_POINT('Ctrl Pts',(-40.2442018113108,60.728010266139,0.));
#153978=CARTESIAN_POINT('Ctrl Pts',(-40.2442018113108,60.728010266139,12.));
#153979=CARTESIAN_POINT('Ctrl Pts',(-40.2389898925932,60.7030445528857,
0.));
#153980=CARTESIAN_POINT('Ctrl Pts',(-40.2389898925932,60.7030445528857,
12.));
#153981=CARTESIAN_POINT('Ctrl Pts',(-40.2337624072029,60.678122094098,0.));
#153982=CARTESIAN_POINT('Ctrl Pts',(-40.2337624072029,60.678122094098,12.));
#153983=CARTESIAN_POINT('Ctrl Pts',(-40.2285194291706,60.6532429799499,
0.));
#153984=CARTESIAN_POINT('Ctrl Pts',(-40.2285194291706,60.6532429799499,
12.));
#153985=CARTESIAN_POINT('Ctrl Pts',(-40.2232610328721,60.6284073008871,
0.));
#153986=CARTESIAN_POINT('Ctrl Pts',(-40.2232610328721,60.6284073008871,
12.));
#153987=CARTESIAN_POINT('Ctrl Pts',(-40.2179872930273,60.6036151476349,
0.));
#153988=CARTESIAN_POINT('Ctrl Pts',(-40.2179872930273,60.6036151476349,
12.));
#153989=CARTESIAN_POINT('Ctrl Pts',(-40.2126982847011,60.5788666112042,
0.));
#153990=CARTESIAN_POINT('Ctrl Pts',(-40.2126982847011,60.5788666112042,
12.));
#153991=CARTESIAN_POINT('Ctrl Pts',(-40.2073940833052,60.5541617828925,
0.));
#153992=CARTESIAN_POINT('Ctrl Pts',(-40.2073940833052,60.5541617828925,
12.));
#153993=CARTESIAN_POINT('Ctrl Pts',(-40.2020747646014,60.5295007542841,
0.));
#153994=CARTESIAN_POINT('Ctrl Pts',(-40.2020747646014,60.5295007542841,
12.));
#153995=CARTESIAN_POINT('Ctrl Pts',(-40.1967404047062,60.5048836172435,
0.));
#153996=CARTESIAN_POINT('Ctrl Pts',(-40.1967404047062,60.5048836172435,
12.));
#153997=CARTESIAN_POINT('Ctrl Pts',(-40.1913910800921,60.4803104639226,
0.));
#153998=CARTESIAN_POINT('Ctrl Pts',(-40.1913910800921,60.4803104639226,
12.));
#153999=CARTESIAN_POINT('Ctrl Pts',(-40.1860268675883,60.455781386769,0.));
#154000=CARTESIAN_POINT('Ctrl Pts',(-40.1860268675883,60.455781386769,12.));
#154001=CARTESIAN_POINT('Ctrl Pts',(-40.180647844383,60.4312964785273,0.));
#154002=CARTESIAN_POINT('Ctrl Pts',(-40.180647844383,60.4312964785273,12.));
#154003=CARTESIAN_POINT('Ctrl Pts',(-40.1752540880268,60.4068558322407,
0.));
#154004=CARTESIAN_POINT('Ctrl Pts',(-40.1752540880268,60.4068558322407,
12.));
#154005=CARTESIAN_POINT('Ctrl Pts',(-40.1698456764377,60.3824595412445,
0.));
#154006=CARTESIAN_POINT('Ctrl Pts',(-40.1698456764377,60.3824595412445,
12.));
#154007=CARTESIAN_POINT('Ctrl Pts',(-40.1644226879033,60.3581076991716,
0.));
#154008=CARTESIAN_POINT('Ctrl Pts',(-40.1644226879033,60.3581076991716,
12.));
#154009=CARTESIAN_POINT('Ctrl Pts',(-40.1589852010804,60.3338003999607,
0.));
#154010=CARTESIAN_POINT('Ctrl Pts',(-40.1589852010804,60.3338003999607,
12.));
#154011=CARTESIAN_POINT('Ctrl Pts',(-40.1535332949976,60.3095377378586,
0.));
#154012=CARTESIAN_POINT('Ctrl Pts',(-40.1535332949976,60.3095377378586,
12.));
#154013=CARTESIAN_POINT('Ctrl Pts',(-40.1480670490586,60.285319807422,0.));
#154014=CARTESIAN_POINT('Ctrl Pts',(-40.1480670490586,60.285319807422,12.));
#154015=CARTESIAN_POINT('Ctrl Pts',(-40.1425865430472,60.2611467035117,
0.));
#154016=CARTESIAN_POINT('Ctrl Pts',(-40.1425865430472,60.2611467035117,
12.));
#154017=CARTESIAN_POINT('Ctrl Pts',(-40.1370918571304,60.2370185212964,
0.));
#154018=CARTESIAN_POINT('Ctrl Pts',(-40.1370918571304,60.2370185212964,
12.));
#154019=CARTESIAN_POINT('Ctrl Pts',(-40.1315830718577,60.2129353562622,
0.));
#154020=CARTESIAN_POINT('Ctrl Pts',(-40.1315830718577,60.2129353562622,
12.));
#154021=CARTESIAN_POINT('Ctrl Pts',(-40.1260602681644,60.1888973042152,
0.));
#154022=CARTESIAN_POINT('Ctrl Pts',(-40.1260602681644,60.1888973042152,
12.));
#154023=CARTESIAN_POINT('Ctrl Pts',(-40.1205235273739,60.1649044612828,
0.));
#154024=CARTESIAN_POINT('Ctrl Pts',(-40.1205235273739,60.1649044612828,
12.));
#154025=CARTESIAN_POINT('Ctrl Pts',(-40.1149729312036,60.1409569239092,
0.));
#154026=CARTESIAN_POINT('Ctrl Pts',(-40.1149729312036,60.1409569239092,
12.));
#154027=CARTESIAN_POINT('Ctrl Pts',(-40.1094085617674,60.1170547888574,
0.));
#154028=CARTESIAN_POINT('Ctrl Pts',(-40.1094085617674,60.1170547888574,
12.));
#154029=CARTESIAN_POINT('Ctrl Pts',(-40.1038305015766,60.0931981532198,
0.));
#154030=CARTESIAN_POINT('Ctrl Pts',(-40.1038305015766,60.0931981532198,
12.));
#154031=CARTESIAN_POINT('Ctrl Pts',(-40.0982388335423,60.069387114421,0.));
#154032=CARTESIAN_POINT('Ctrl Pts',(-40.0982388335423,60.069387114421,12.));
#154033=CARTESIAN_POINT('Ctrl Pts',(-40.0926336409785,60.0456217702202,
0.));
#154034=CARTESIAN_POINT('Ctrl Pts',(-40.0926336409785,60.0456217702202,
12.));
#154035=CARTESIAN_POINT('Ctrl Pts',(-40.0870150076074,60.021902218706,0.));
#154036=CARTESIAN_POINT('Ctrl Pts',(-40.0870150076074,60.021902218706,12.));
#154037=CARTESIAN_POINT('Ctrl Pts',(-40.0813830175623,59.9982285582983,
0.));
#154038=CARTESIAN_POINT('Ctrl Pts',(-40.0813830175623,59.9982285582983,
12.));
#154039=CARTESIAN_POINT('Ctrl Pts',(-40.0757377553888,59.9746008877584,
0.));
#154040=CARTESIAN_POINT('Ctrl Pts',(-40.0757377553888,59.9746008877584,
12.));
#154041=CARTESIAN_POINT('Ctrl Pts',(-40.0700793060473,59.9510193061927,
0.));
#154042=CARTESIAN_POINT('Ctrl Pts',(-40.0700793060473,59.9510193061927,
12.));
#154043=CARTESIAN_POINT('Ctrl Pts',(-40.0644077549159,59.9274839130553,
0.));
#154044=CARTESIAN_POINT('Ctrl Pts',(-40.0644077549159,59.9274839130553,
12.));
#154045=CARTESIAN_POINT('Ctrl Pts',(-40.0587231877961,59.9039948081432,
0.));
#154046=CARTESIAN_POINT('Ctrl Pts',(-40.0587231877961,59.9039948081432,
12.));
#154047=CARTESIAN_POINT('Ctrl Pts',(-40.0530256909162,59.8805520915975,
0.));
#154048=CARTESIAN_POINT('Ctrl Pts',(-40.0530256909162,59.8805520915975,
12.));
#154049=CARTESIAN_POINT('Ctrl Pts',(-40.0473153509323,59.8571558639145,
0.));
#154050=CARTESIAN_POINT('Ctrl Pts',(-40.0473153509323,59.8571558639145,
12.));
#154051=CARTESIAN_POINT('Ctrl Pts',(-40.0415922549313,59.8338062259491,
0.));
#154052=CARTESIAN_POINT('Ctrl Pts',(-40.0415922549313,59.8338062259491,
12.));
#154053=CARTESIAN_POINT('Ctrl Pts',(-40.035856490434,59.8105032789179,0.));
#154054=CARTESIAN_POINT('Ctrl Pts',(-40.035856490434,59.8105032789179,12.));
#154055=CARTESIAN_POINT('Ctrl Pts',(-40.0301081454006,59.7872471243948,
0.));
#154056=CARTESIAN_POINT('Ctrl Pts',(-40.0301081454006,59.7872471243948,
12.));
#154057=CARTESIAN_POINT('Ctrl Pts',(-40.0243473082343,59.7640378643115,
0.));
#154058=CARTESIAN_POINT('Ctrl Pts',(-40.0243473082343,59.7640378643115,
12.));
#154059=CARTESIAN_POINT('Ctrl Pts',(-40.0185740677827,59.7408756009688,
0.));
#154060=CARTESIAN_POINT('Ctrl Pts',(-40.0185740677827,59.7408756009688,
12.));
#154061=CARTESIAN_POINT('Ctrl Pts',(-40.0127885133407,59.7177604370409,
0.));
#154062=CARTESIAN_POINT('Ctrl Pts',(-40.0127885133407,59.7177604370409,
12.));
#154063=CARTESIAN_POINT('Ctrl Pts',(-40.0069907346536,59.6946924755771,
0.));
#154064=CARTESIAN_POINT('Ctrl Pts',(-40.0069907346536,59.6946924755771,
12.));
#154065=CARTESIAN_POINT('Ctrl Pts',(-40.001180821923,59.671671819999,0.));
#154066=CARTESIAN_POINT('Ctrl Pts',(-40.001180821923,59.671671819999,12.));
#154067=CARTESIAN_POINT('Ctrl Pts',(-39.9953588658114,59.6486985741015,
0.));
#154068=CARTESIAN_POINT('Ctrl Pts',(-39.9953588658114,59.6486985741015,
12.));
#154069=CARTESIAN_POINT('Ctrl Pts',(-39.9895249574432,59.6257728420644,
0.));
#154070=CARTESIAN_POINT('Ctrl Pts',(-39.9895249574432,59.6257728420644,
12.));
#154071=CARTESIAN_POINT('Ctrl Pts',(-39.9836791884071,59.6028947284551,
0.));
#154072=CARTESIAN_POINT('Ctrl Pts',(-39.9836791884071,59.6028947284551,
12.));
#154073=CARTESIAN_POINT('Ctrl Pts',(-39.9778216507609,59.5800643382322,
0.));
#154074=CARTESIAN_POINT('Ctrl Pts',(-39.9778216507609,59.5800643382322,
12.));
#154075=CARTESIAN_POINT('Ctrl Pts',(-39.971952437036,59.5572817767412,0.));
#154076=CARTESIAN_POINT('Ctrl Pts',(-39.971952437036,59.5572817767412,12.));
#154077=CARTESIAN_POINT('Ctrl Pts',(-39.9660716402423,59.5345471497162,
0.));
#154078=CARTESIAN_POINT('Ctrl Pts',(-39.9660716402423,59.5345471497162,
12.));
#154079=CARTESIAN_POINT('Ctrl Pts',(-39.96017935387,59.511860563292,0.));
#154080=CARTESIAN_POINT('Ctrl Pts',(-39.96017935387,59.511860563292,12.));
#154081=CARTESIAN_POINT('Ctrl Pts',(-39.954275671893,59.4892221240081,0.));
#154082=CARTESIAN_POINT('Ctrl Pts',(-39.954275671893,59.4892221240081,12.));
#154083=CARTESIAN_POINT('Ctrl Pts',(-39.9483606887731,59.4666319388123,
0.));
#154084=CARTESIAN_POINT('Ctrl Pts',(-39.9483606887731,59.4666319388123,
12.));
#154085=CARTESIAN_POINT('Ctrl Pts',(-39.9424344994652,59.444090115055,0.));
#154086=CARTESIAN_POINT('Ctrl Pts',(-39.9424344994652,59.444090115055,12.));
#154087=CARTESIAN_POINT('Ctrl Pts',(-39.9364971994215,59.4215967604925,
0.));
#154088=CARTESIAN_POINT('Ctrl Pts',(-39.9364971994215,59.4215967604925,
12.));
#154089=CARTESIAN_POINT('Ctrl Pts',(-39.9305488845934,59.3991519832981,
0.));
#154090=CARTESIAN_POINT('Ctrl Pts',(-39.9305488845934,59.3991519832981,
12.));
#154091=CARTESIAN_POINT('Ctrl Pts',(-39.9245896514359,59.3767558920663,
0.));
#154092=CARTESIAN_POINT('Ctrl Pts',(-39.9245896514359,59.3767558920663,
12.));
#154093=CARTESIAN_POINT('Ctrl Pts',(-39.9186195969113,59.3544085958165,
0.));
#154094=CARTESIAN_POINT('Ctrl Pts',(-39.9186195969113,59.3544085958165,
12.));
#154095=CARTESIAN_POINT('Ctrl Pts',(-39.9126388184956,59.3321102039883,
0.));
#154096=CARTESIAN_POINT('Ctrl Pts',(-39.9126388184956,59.3321102039883,
12.));
#154097=CARTESIAN_POINT('Ctrl Pts',(-39.9066474141826,59.3098608264452,
0.));
#154098=CARTESIAN_POINT('Ctrl Pts',(-39.9066474141826,59.3098608264452,
12.));
#154099=CARTESIAN_POINT('Ctrl Pts',(-39.9006454824861,59.2876605734871,
0.));
#154100=CARTESIAN_POINT('Ctrl Pts',(-39.9006454824861,59.2876605734871,
12.));
#154101=CARTESIAN_POINT('Ctrl Pts',(-39.8946331224442,59.2655095558527,
0.));
#154102=CARTESIAN_POINT('Ctrl Pts',(-39.8946331224442,59.2655095558527,
12.));
#154103=CARTESIAN_POINT('Ctrl Pts',(-39.8886104336234,59.2434078847236,
0.));
#154104=CARTESIAN_POINT('Ctrl Pts',(-39.8886104336234,59.2434078847236,
12.));
#154105=CARTESIAN_POINT('Ctrl Pts',(-39.8825775161252,59.2213556717189,
0.));
#154106=CARTESIAN_POINT('Ctrl Pts',(-39.8825775161252,59.2213556717189,
12.));
#154107=CARTESIAN_POINT('Ctrl Pts',(-39.8765344705894,59.1993530289008,
0.));
#154108=CARTESIAN_POINT('Ctrl Pts',(-39.8765344705894,59.1993530289008,
12.));
#154109=CARTESIAN_POINT('Ctrl Pts',(-39.8704813981978,59.1774000687865,
0.));
#154110=CARTESIAN_POINT('Ctrl Pts',(-39.8704813981978,59.1774000687865,
12.));
#154111=CARTESIAN_POINT('Ctrl Pts',(-39.8644184006785,59.155496904352,0.));
#154112=CARTESIAN_POINT('Ctrl Pts',(-39.8644184006785,59.155496904352,12.));
#154113=CARTESIAN_POINT('Ctrl Pts',(-39.8583455803111,59.133643649035,0.));
#154114=CARTESIAN_POINT('Ctrl Pts',(-39.8583455803111,59.133643649035,12.));
#154115=CARTESIAN_POINT('Ctrl Pts',(-39.8522630399337,59.1118404167304,
0.));
#154116=CARTESIAN_POINT('Ctrl Pts',(-39.8522630399337,59.1118404167304,
12.));
#154117=CARTESIAN_POINT('Ctrl Pts',(-39.8461708829465,59.0900873217992,
0.));
#154118=CARTESIAN_POINT('Ctrl Pts',(-39.8461708829465,59.0900873217992,
12.));
#154119=CARTESIAN_POINT('Ctrl Pts',(-39.8400692133143,59.068384479077,0.));
#154120=CARTESIAN_POINT('Ctrl Pts',(-39.8400692133143,59.068384479077,12.));
#154121=CARTESIAN_POINT('Ctrl Pts',(-39.8339581355714,59.0467320038782,
0.));
#154122=CARTESIAN_POINT('Ctrl Pts',(-39.8339581355714,59.0467320038782,
12.));
#154123=CARTESIAN_POINT('Ctrl Pts',(-39.8278377548261,59.0251300119973,
0.));
#154124=CARTESIAN_POINT('Ctrl Pts',(-39.8278377548261,59.0251300119973,
12.));
#154125=CARTESIAN_POINT('Ctrl Pts',(-39.8217081767658,59.0035786197024,
0.));
#154126=CARTESIAN_POINT('Ctrl Pts',(-39.8217081767658,59.0035786197024,
12.));
#154127=CARTESIAN_POINT('Ctrl Pts',(-39.8155695076625,58.9820779437485,
0.));
#154128=CARTESIAN_POINT('Ctrl Pts',(-39.8155695076625,58.9820779437485,
12.));
#154129=CARTESIAN_POINT('Ctrl Pts',(-39.8094218543781,58.9606281013876,
0.));
#154130=CARTESIAN_POINT('Ctrl Pts',(-39.8094218543781,58.9606281013876,
12.));
#154131=CARTESIAN_POINT('Ctrl Pts',(-39.8032653243712,58.9392292103747,
0.));
#154132=CARTESIAN_POINT('Ctrl Pts',(-39.8032653243712,58.9392292103747,
12.));
#154133=CARTESIAN_POINT('Ctrl Pts',(-39.7971000257044,58.9178813889703,
0.));
#154134=CARTESIAN_POINT('Ctrl Pts',(-39.7971000257044,58.9178813889703,
12.));
#154135=CARTESIAN_POINT('Ctrl Pts',(-39.7909260670517,58.896584755939,0.));
#154136=CARTESIAN_POINT('Ctrl Pts',(-39.7909260670517,58.896584755939,12.));
#154137=CARTESIAN_POINT('Ctrl Pts',(-39.7847435576995,58.8753394305583,
0.));
#154138=CARTESIAN_POINT('Ctrl Pts',(-39.7847435576995,58.8753394305583,
12.));
#154139=CARTESIAN_POINT('Ctrl Pts',(-39.7785526075477,58.8541455326229,
0.));
#154140=CARTESIAN_POINT('Ctrl Pts',(-39.7785526075477,58.8541455326229,
12.));
#154141=CARTESIAN_POINT('Ctrl Pts',(-39.772353327112,58.8330031824453,0.));
#154142=CARTESIAN_POINT('Ctrl Pts',(-39.772353327112,58.8330031824453,12.));
#154143=CARTESIAN_POINT('Ctrl Pts',(-39.7661458275276,58.8119125008521,
0.));
#154144=CARTESIAN_POINT('Ctrl Pts',(-39.7661458275276,58.8119125008521,
12.));
#154145=CARTESIAN_POINT('Ctrl Pts',(-39.7599302205527,58.7908736091808,
0.));
#154146=CARTESIAN_POINT('Ctrl Pts',(-39.7599302205527,58.7908736091808,
12.));
#154147=CARTESIAN_POINT('Ctrl Pts',(-39.753706618582,58.7698866293041,0.));
#154148=CARTESIAN_POINT('Ctrl Pts',(-39.753706618582,58.7698866293041,12.));
#154149=CARTESIAN_POINT('Ctrl Pts',(-39.7474751346603,58.7489516836453,
0.));
#154150=CARTESIAN_POINT('Ctrl Pts',(-39.7474751346603,58.7489516836453,
12.));
#154151=CARTESIAN_POINT('Ctrl Pts',(-39.7412358824949,58.7280688951911,
0.));
#154152=CARTESIAN_POINT('Ctrl Pts',(-39.7412358824949,58.7280688951911,
12.));
#154153=CARTESIAN_POINT('Ctrl Pts',(-39.7349889764737,58.7072383875009,
0.));
#154154=CARTESIAN_POINT('Ctrl Pts',(-39.7349889764737,58.7072383875009,
12.));
#154155=CARTESIAN_POINT('Ctrl Pts',(-39.7287345316664,58.6864602847064,
0.));
#154156=CARTESIAN_POINT('Ctrl Pts',(-39.7287345316664,58.6864602847064,
12.));
#154157=CARTESIAN_POINT('Ctrl Pts',(-39.7224726638087,58.6657347115014,
0.));
#154158=CARTESIAN_POINT('Ctrl Pts',(-39.7224726638087,58.6657347115014,
12.));
#154159=CARTESIAN_POINT('Ctrl Pts',(-39.7162034892896,58.6450617931269,
0.));
#154160=CARTESIAN_POINT('Ctrl Pts',(-39.7162034892896,58.6450617931269,
12.));
#154161=CARTESIAN_POINT('Ctrl Pts',(-39.7099271251421,58.6244416553574,
0.));
#154162=CARTESIAN_POINT('Ctrl Pts',(-39.7099271251421,58.6244416553574,
12.));
#154163=CARTESIAN_POINT('Ctrl Pts',(-39.7036436890248,58.6038744244683,
0.));
#154164=CARTESIAN_POINT('Ctrl Pts',(-39.7036436890248,58.6038744244683,
12.));
#154165=CARTESIAN_POINT('Ctrl Pts',(-39.6973532992555,58.5833602272767,
0.));
#154166=CARTESIAN_POINT('Ctrl Pts',(-39.6973532992555,58.5833602272767,
12.));
#154167=CARTESIAN_POINT('Ctrl Pts',(-39.6910560748639,58.5628991912067,
0.));
#154168=CARTESIAN_POINT('Ctrl Pts',(-39.6910560748639,58.5628991912067,
12.));
#154169=CARTESIAN_POINT('Ctrl Pts',(-39.6847521356395,58.5424914443415,
0.));
#154170=CARTESIAN_POINT('Ctrl Pts',(-39.6847521356395,58.5424914443415,
12.));
#154171=CARTESIAN_POINT('Ctrl Pts',(-39.6784416021817,58.5221371154748,
0.));
#154172=CARTESIAN_POINT('Ctrl Pts',(-39.6784416021817,58.5221371154748,
12.));
#154173=CARTESIAN_POINT('Ctrl Pts',(-39.6721245959516,58.5018363341582,
0.));
#154174=CARTESIAN_POINT('Ctrl Pts',(-39.6721245959516,58.5018363341582,
12.));
#154175=CARTESIAN_POINT('Ctrl Pts',(-39.66580123918,58.4815892306044,0.));
#154176=CARTESIAN_POINT('Ctrl Pts',(-39.66580123918,58.4815892306044,12.));
#154177=CARTESIAN_POINT('Ctrl Pts',(-39.659471654768,58.4613959355776,0.));
#154178=CARTESIAN_POINT('Ctrl Pts',(-39.659471654768,58.4613959355776,12.));
#154179=CARTESIAN_POINT('Ctrl Pts',(-39.6531359662043,58.4412565802984,
0.));
#154180=CARTESIAN_POINT('Ctrl Pts',(-39.6531359662043,58.4412565802984,
12.));
#154181=CARTESIAN_POINT('Ctrl Pts',(-39.6467942974464,58.4211712963024,
0.));
#154182=CARTESIAN_POINT('Ctrl Pts',(-39.6467942974464,58.4211712963024,
12.));
#154183=CARTESIAN_POINT('Ctrl Pts',(-39.6404467729113,58.4011402154225,
0.));
#154184=CARTESIAN_POINT('Ctrl Pts',(-39.6404467729113,58.4011402154225,
12.));
#154185=CARTESIAN_POINT('Ctrl Pts',(-39.6340935177492,58.3811634701061,
0.));
#154186=CARTESIAN_POINT('Ctrl Pts',(-39.6340935177492,58.3811634701061,
12.));
#154187=CARTESIAN_POINT('Ctrl Pts',(-39.6277346580898,58.3612411936914,
0.));
#154188=CARTESIAN_POINT('Ctrl Pts',(-39.6277346580898,58.3612411936914,
12.));
#154189=CARTESIAN_POINT('Ctrl Pts',(-39.6213703212523,58.3413735206412,
0.));
#154190=CARTESIAN_POINT('Ctrl Pts',(-39.6213703212523,58.3413735206412,
12.));
#154191=CARTESIAN_POINT('Ctrl Pts',(-39.6150006360894,58.3215605869192,
0.));
#154192=CARTESIAN_POINT('Ctrl Pts',(-39.6150006360894,58.3215605869192,
12.));
#154193=CARTESIAN_POINT('Ctrl Pts',(-39.6086257327559,58.3018025297288,
0.));
#154194=CARTESIAN_POINT('Ctrl Pts',(-39.6086257327559,58.3018025297288,
12.));
#154195=CARTESIAN_POINT('Ctrl Pts',(-39.6022457420772,58.2820994868092,
0.));
#154196=CARTESIAN_POINT('Ctrl Pts',(-39.6022457420772,58.2820994868092,
12.));
#154197=CARTESIAN_POINT('Ctrl Pts',(-39.5958607950237,58.2624515958416,
0.));
#154198=CARTESIAN_POINT('Ctrl Pts',(-39.5958607950237,58.2624515958416,
12.));
#154199=CARTESIAN_POINT('Ctrl Pts',(-39.5894710221729,58.2428589938394,
0.));
#154200=CARTESIAN_POINT('Ctrl Pts',(-39.5894710221729,58.2428589938394,
12.));
#154201=CARTESIAN_POINT('Ctrl Pts',(-39.5830765530919,58.2233218164407,
0.));
#154202=CARTESIAN_POINT('Ctrl Pts',(-39.5830765530919,58.2233218164407,
12.));
#154203=CARTESIAN_POINT('Ctrl Pts',(-39.5766775175226,58.2038401992496,
0.));
#154204=CARTESIAN_POINT('Ctrl Pts',(-39.5766775175226,58.2038401992496,
12.));
#154205=CARTESIAN_POINT('Ctrl Pts',(-39.5702740468013,58.1844142794359,
0.));
#154206=CARTESIAN_POINT('Ctrl Pts',(-39.5702740468013,58.1844142794359,
12.));
#154207=CARTESIAN_POINT('Ctrl Pts',(-39.5638662750174,58.1650441970379,
0.));
#154208=CARTESIAN_POINT('Ctrl Pts',(-39.5638662750174,58.1650441970379,
12.));
#154209=CARTESIAN_POINT('Ctrl Pts',(-39.5574543406959,58.1457300968467,
0.));
#154210=CARTESIAN_POINT('Ctrl Pts',(-39.5574543406959,58.1457300968467,
12.));
#154211=CARTESIAN_POINT('Ctrl Pts',(-39.5510383869476,58.1264721285698,
0.));
#154212=CARTESIAN_POINT('Ctrl Pts',(-39.5510383869476,58.1264721285698,
12.));
#154213=CARTESIAN_POINT('Ctrl Pts',(-39.5446185579615,58.1072704428895,
0.));
#154214=CARTESIAN_POINT('Ctrl Pts',(-39.5446185579615,58.1072704428895,
12.));
#154215=CARTESIAN_POINT('Ctrl Pts',(-39.5381949959214,58.088125187991,0.));
#154216=CARTESIAN_POINT('Ctrl Pts',(-39.5381949959214,58.088125187991,12.));
#154217=CARTESIAN_POINT('Ctrl Pts',(-39.5317678383231,58.0690365065393,
0.));
#154218=CARTESIAN_POINT('Ctrl Pts',(-39.5317678383231,58.0690365065393,
12.));
#154219=CARTESIAN_POINT('Ctrl Pts',(-39.5253372136921,58.050004530846,0.));
#154220=CARTESIAN_POINT('Ctrl Pts',(-39.5253372136921,58.050004530846,12.));
#154221=CARTESIAN_POINT('Ctrl Pts',(-39.5189032457227,58.0310293875321,
0.));
#154222=CARTESIAN_POINT('Ctrl Pts',(-39.5189032457227,58.0310293875321,
12.));
#154223=CARTESIAN_POINT('Ctrl Pts',(-39.5124660615009,58.012111206794,0.));
#154224=CARTESIAN_POINT('Ctrl Pts',(-39.5124660615009,58.012111206794,12.));
#154225=CARTESIAN_POINT('Ctrl Pts',(-39.5060257981225,57.9932501298522,
0.));
#154226=CARTESIAN_POINT('Ctrl Pts',(-39.5060257981225,57.9932501298522,
12.));
#154227=CARTESIAN_POINT('Ctrl Pts',(-39.4995826106691,57.9744463179305,
0.));
#154228=CARTESIAN_POINT('Ctrl Pts',(-39.4995826106691,57.9744463179305,
12.));
#154229=CARTESIAN_POINT('Ctrl Pts',(-39.4931366776627,57.9556999583777,
0.));
#154230=CARTESIAN_POINT('Ctrl Pts',(-39.4931366776627,57.9556999583777,
12.));
#154231=CARTESIAN_POINT('Ctrl Pts',(-39.4866881842223,57.9370112456506,
0.));
#154232=CARTESIAN_POINT('Ctrl Pts',(-39.4866881842223,57.9370112456506,
12.));
#154233=CARTESIAN_POINT('Ctrl Pts',(-39.4802373061008,57.9183803632337,
0.));
#154234=CARTESIAN_POINT('Ctrl Pts',(-39.4802373061008,57.9183803632337,
12.));
#154235=CARTESIAN_POINT('Ctrl Pts',(-39.4737841949417,57.8998074670541,
0.));
#154236=CARTESIAN_POINT('Ctrl Pts',(-39.4737841949417,57.8998074670541,
12.));
#154237=CARTESIAN_POINT('Ctrl Pts',(-39.4673289592425,57.8812926637397,
0.));
#154238=CARTESIAN_POINT('Ctrl Pts',(-39.4673289592425,57.8812926637397,
12.));
#154239=CARTESIAN_POINT('Ctrl Pts',(-39.4608716627367,57.8628360097134,
0.));
#154240=CARTESIAN_POINT('Ctrl Pts',(-39.4608716627367,57.8628360097134,
12.));
#154241=CARTESIAN_POINT('Ctrl Pts',(-39.4557042029884,57.8481172247805,
0.));
#154242=CARTESIAN_POINT('Ctrl Pts',(-39.4557042029884,57.8481172247805,
12.));
#154243=CARTESIAN_POINT('Ctrl Pts',(-39.45182770037,57.8371043151607,0.));
#154244=CARTESIAN_POINT('Ctrl Pts',(-39.45182770037,57.8371043151607,12.));
#154245=CARTESIAN_POINT('Ctrl Pts',(-39.4492429618498,57.829774010102,0.));
#154246=CARTESIAN_POINT('Ctrl Pts',(-39.4492429618498,57.829774010102,12.));
#154247=CARTESIAN_POINT('Ctrl Pts',(-39.4479504917286,57.8261117662439,
0.));
#154248=CARTESIAN_POINT('Ctrl Pts',(-39.4479504917286,57.8261117662439,
12.));
#154249=CARTESIAN_POINT('',(-39.4479504917286,57.8261117662439,12.));
#154250=CARTESIAN_POINT('Ctrl Pts',(-39.4479504917286,57.8261117662439,
12.));
#154251=CARTESIAN_POINT('Ctrl Pts',(-39.4492429618498,57.829774010102,12.));
#154252=CARTESIAN_POINT('Ctrl Pts',(-39.45182770037,57.8371043151607,12.));
#154253=CARTESIAN_POINT('Ctrl Pts',(-39.4557042029884,57.8481172247805,
12.));
#154254=CARTESIAN_POINT('Ctrl Pts',(-39.4608716627367,57.8628360097134,
12.));
#154255=CARTESIAN_POINT('Ctrl Pts',(-39.4673289592425,57.8812926637397,
12.));
#154256=CARTESIAN_POINT('Ctrl Pts',(-39.4737841949417,57.8998074670541,
12.));
#154257=CARTESIAN_POINT('Ctrl Pts',(-39.4802373061008,57.9183803632337,
12.));
#154258=CARTESIAN_POINT('Ctrl Pts',(-39.4866881842223,57.9370112456506,
12.));
#154259=CARTESIAN_POINT('Ctrl Pts',(-39.4931366776627,57.9556999583777,
12.));
#154260=CARTESIAN_POINT('Ctrl Pts',(-39.4995826106691,57.9744463179305,
12.));
#154261=CARTESIAN_POINT('Ctrl Pts',(-39.5060257981225,57.9932501298522,
12.));
#154262=CARTESIAN_POINT('Ctrl Pts',(-39.5124660615009,58.012111206794,12.));
#154263=CARTESIAN_POINT('Ctrl Pts',(-39.5189032457227,58.0310293875321,
12.));
#154264=CARTESIAN_POINT('Ctrl Pts',(-39.5253372136921,58.050004530846,12.));
#154265=CARTESIAN_POINT('Ctrl Pts',(-39.5317678383231,58.0690365065393,
12.));
#154266=CARTESIAN_POINT('Ctrl Pts',(-39.5381949959214,58.088125187991,12.));
#154267=CARTESIAN_POINT('Ctrl Pts',(-39.5446185579615,58.1072704428895,
12.));
#154268=CARTESIAN_POINT('Ctrl Pts',(-39.5510383869476,58.1264721285698,
12.));
#154269=CARTESIAN_POINT('Ctrl Pts',(-39.5574543406959,58.1457300968467,
12.));
#154270=CARTESIAN_POINT('Ctrl Pts',(-39.5638662750174,58.1650441970379,
12.));
#154271=CARTESIAN_POINT('Ctrl Pts',(-39.5702740468013,58.1844142794359,
12.));
#154272=CARTESIAN_POINT('Ctrl Pts',(-39.5766775175226,58.2038401992496,
12.));
#154273=CARTESIAN_POINT('Ctrl Pts',(-39.5830765530919,58.2233218164407,
12.));
#154274=CARTESIAN_POINT('Ctrl Pts',(-39.5894710221729,58.2428589938394,
12.));
#154275=CARTESIAN_POINT('Ctrl Pts',(-39.5958607950237,58.2624515958416,
12.));
#154276=CARTESIAN_POINT('Ctrl Pts',(-39.6022457420772,58.2820994868092,
12.));
#154277=CARTESIAN_POINT('Ctrl Pts',(-39.6086257327559,58.3018025297288,
12.));
#154278=CARTESIAN_POINT('Ctrl Pts',(-39.6150006360894,58.3215605869192,
12.));
#154279=CARTESIAN_POINT('Ctrl Pts',(-39.6213703212523,58.3413735206412,
12.));
#154280=CARTESIAN_POINT('Ctrl Pts',(-39.6277346580898,58.3612411936914,
12.));
#154281=CARTESIAN_POINT('Ctrl Pts',(-39.6340935177492,58.3811634701061,
12.));
#154282=CARTESIAN_POINT('Ctrl Pts',(-39.6404467729113,58.4011402154225,
12.));
#154283=CARTESIAN_POINT('Ctrl Pts',(-39.6467942974464,58.4211712963024,
12.));
#154284=CARTESIAN_POINT('Ctrl Pts',(-39.6531359662043,58.4412565802984,
12.));
#154285=CARTESIAN_POINT('Ctrl Pts',(-39.659471654768,58.4613959355776,12.));
#154286=CARTESIAN_POINT('Ctrl Pts',(-39.66580123918,58.4815892306044,12.));
#154287=CARTESIAN_POINT('Ctrl Pts',(-39.6721245959516,58.5018363341582,
12.));
#154288=CARTESIAN_POINT('Ctrl Pts',(-39.6784416021817,58.5221371154748,
12.));
#154289=CARTESIAN_POINT('Ctrl Pts',(-39.6847521356395,58.5424914443415,
12.));
#154290=CARTESIAN_POINT('Ctrl Pts',(-39.6910560748639,58.5628991912067,
12.));
#154291=CARTESIAN_POINT('Ctrl Pts',(-39.6973532992555,58.5833602272767,
12.));
#154292=CARTESIAN_POINT('Ctrl Pts',(-39.7036436890248,58.6038744244683,
12.));
#154293=CARTESIAN_POINT('Ctrl Pts',(-39.7099271251421,58.6244416553574,
12.));
#154294=CARTESIAN_POINT('Ctrl Pts',(-39.7162034892896,58.6450617931269,
12.));
#154295=CARTESIAN_POINT('Ctrl Pts',(-39.7224726638087,58.6657347115014,
12.));
#154296=CARTESIAN_POINT('Ctrl Pts',(-39.7287345316664,58.6864602847064,
12.));
#154297=CARTESIAN_POINT('Ctrl Pts',(-39.7349889764737,58.7072383875009,
12.));
#154298=CARTESIAN_POINT('Ctrl Pts',(-39.7412358824949,58.7280688951911,
12.));
#154299=CARTESIAN_POINT('Ctrl Pts',(-39.7474751346603,58.7489516836453,
12.));
#154300=CARTESIAN_POINT('Ctrl Pts',(-39.753706618582,58.7698866293041,12.));
#154301=CARTESIAN_POINT('Ctrl Pts',(-39.7599302205527,58.7908736091808,
12.));
#154302=CARTESIAN_POINT('Ctrl Pts',(-39.7661458275276,58.8119125008521,
12.));
#154303=CARTESIAN_POINT('Ctrl Pts',(-39.772353327112,58.8330031824453,12.));
#154304=CARTESIAN_POINT('Ctrl Pts',(-39.7785526075477,58.8541455326229,
12.));
#154305=CARTESIAN_POINT('Ctrl Pts',(-39.7847435576995,58.8753394305583,
12.));
#154306=CARTESIAN_POINT('Ctrl Pts',(-39.7909260670517,58.896584755939,12.));
#154307=CARTESIAN_POINT('Ctrl Pts',(-39.7971000257044,58.9178813889703,
12.));
#154308=CARTESIAN_POINT('Ctrl Pts',(-39.8032653243712,58.9392292103747,
12.));
#154309=CARTESIAN_POINT('Ctrl Pts',(-39.8094218543781,58.9606281013876,
12.));
#154310=CARTESIAN_POINT('Ctrl Pts',(-39.8155695076625,58.9820779437485,
12.));
#154311=CARTESIAN_POINT('Ctrl Pts',(-39.8217081767658,59.0035786197024,
12.));
#154312=CARTESIAN_POINT('Ctrl Pts',(-39.8278377548261,59.0251300119973,
12.));
#154313=CARTESIAN_POINT('Ctrl Pts',(-39.8339581355714,59.0467320038782,
12.));
#154314=CARTESIAN_POINT('Ctrl Pts',(-39.8400692133143,59.068384479077,12.));
#154315=CARTESIAN_POINT('Ctrl Pts',(-39.8461708829465,59.0900873217992,
12.));
#154316=CARTESIAN_POINT('Ctrl Pts',(-39.8522630399337,59.1118404167304,
12.));
#154317=CARTESIAN_POINT('Ctrl Pts',(-39.8583455803111,59.133643649035,12.));
#154318=CARTESIAN_POINT('Ctrl Pts',(-39.8644184006785,59.155496904352,12.));
#154319=CARTESIAN_POINT('Ctrl Pts',(-39.8704813981978,59.1774000687865,
12.));
#154320=CARTESIAN_POINT('Ctrl Pts',(-39.8765344705894,59.1993530289008,
12.));
#154321=CARTESIAN_POINT('Ctrl Pts',(-39.8825775161252,59.2213556717189,
12.));
#154322=CARTESIAN_POINT('Ctrl Pts',(-39.8886104336234,59.2434078847236,
12.));
#154323=CARTESIAN_POINT('Ctrl Pts',(-39.8946331224442,59.2655095558527,
12.));
#154324=CARTESIAN_POINT('Ctrl Pts',(-39.9006454824861,59.2876605734871,
12.));
#154325=CARTESIAN_POINT('Ctrl Pts',(-39.9066474141826,59.3098608264452,
12.));
#154326=CARTESIAN_POINT('Ctrl Pts',(-39.9126388184956,59.3321102039883,
12.));
#154327=CARTESIAN_POINT('Ctrl Pts',(-39.9186195969113,59.3544085958165,
12.));
#154328=CARTESIAN_POINT('Ctrl Pts',(-39.9245896514359,59.3767558920663,
12.));
#154329=CARTESIAN_POINT('Ctrl Pts',(-39.9305488845934,59.3991519832981,
12.));
#154330=CARTESIAN_POINT('Ctrl Pts',(-39.9364971994215,59.4215967604925,
12.));
#154331=CARTESIAN_POINT('Ctrl Pts',(-39.9424344994652,59.444090115055,12.));
#154332=CARTESIAN_POINT('Ctrl Pts',(-39.9483606887731,59.4666319388123,
12.));
#154333=CARTESIAN_POINT('Ctrl Pts',(-39.954275671893,59.4892221240081,12.));
#154334=CARTESIAN_POINT('Ctrl Pts',(-39.96017935387,59.511860563292,12.));
#154335=CARTESIAN_POINT('Ctrl Pts',(-39.9660716402423,59.5345471497162,
12.));
#154336=CARTESIAN_POINT('Ctrl Pts',(-39.971952437036,59.5572817767412,12.));
#154337=CARTESIAN_POINT('Ctrl Pts',(-39.9778216507609,59.5800643382322,
12.));
#154338=CARTESIAN_POINT('Ctrl Pts',(-39.9836791884071,59.6028947284551,
12.));
#154339=CARTESIAN_POINT('Ctrl Pts',(-39.9895249574432,59.6257728420644,
12.));
#154340=CARTESIAN_POINT('Ctrl Pts',(-39.9953588658114,59.6486985741015,
12.));
#154341=CARTESIAN_POINT('Ctrl Pts',(-40.001180821923,59.671671819999,12.));
#154342=CARTESIAN_POINT('Ctrl Pts',(-40.0069907346536,59.6946924755771,
12.));
#154343=CARTESIAN_POINT('Ctrl Pts',(-40.0127885133407,59.7177604370409,
12.));
#154344=CARTESIAN_POINT('Ctrl Pts',(-40.0185740677827,59.7408756009688,
12.));
#154345=CARTESIAN_POINT('Ctrl Pts',(-40.0243473082343,59.7640378643115,
12.));
#154346=CARTESIAN_POINT('Ctrl Pts',(-40.0301081454006,59.7872471243948,
12.));
#154347=CARTESIAN_POINT('Ctrl Pts',(-40.035856490434,59.8105032789179,12.));
#154348=CARTESIAN_POINT('Ctrl Pts',(-40.0415922549313,59.8338062259491,
12.));
#154349=CARTESIAN_POINT('Ctrl Pts',(-40.0473153509323,59.8571558639145,
12.));
#154350=CARTESIAN_POINT('Ctrl Pts',(-40.0530256909162,59.8805520915975,
12.));
#154351=CARTESIAN_POINT('Ctrl Pts',(-40.0587231877961,59.9039948081432,
12.));
#154352=CARTESIAN_POINT('Ctrl Pts',(-40.0644077549159,59.9274839130553,
12.));
#154353=CARTESIAN_POINT('Ctrl Pts',(-40.0700793060473,59.9510193061927,
12.));
#154354=CARTESIAN_POINT('Ctrl Pts',(-40.0757377553888,59.9746008877584,
12.));
#154355=CARTESIAN_POINT('Ctrl Pts',(-40.0813830175623,59.9982285582983,
12.));
#154356=CARTESIAN_POINT('Ctrl Pts',(-40.0870150076074,60.021902218706,12.));
#154357=CARTESIAN_POINT('Ctrl Pts',(-40.0926336409785,60.0456217702202,
12.));
#154358=CARTESIAN_POINT('Ctrl Pts',(-40.0982388335423,60.069387114421,12.));
#154359=CARTESIAN_POINT('Ctrl Pts',(-40.1038305015766,60.0931981532198,
12.));
#154360=CARTESIAN_POINT('Ctrl Pts',(-40.1094085617674,60.1170547888574,
12.));
#154361=CARTESIAN_POINT('Ctrl Pts',(-40.1149729312036,60.1409569239092,
12.));
#154362=CARTESIAN_POINT('Ctrl Pts',(-40.1205235273739,60.1649044612828,
12.));
#154363=CARTESIAN_POINT('Ctrl Pts',(-40.1260602681644,60.1888973042152,
12.));
#154364=CARTESIAN_POINT('Ctrl Pts',(-40.1315830718577,60.2129353562622,
12.));
#154365=CARTESIAN_POINT('Ctrl Pts',(-40.1370918571304,60.2370185212964,
12.));
#154366=CARTESIAN_POINT('Ctrl Pts',(-40.1425865430472,60.2611467035117,
12.));
#154367=CARTESIAN_POINT('Ctrl Pts',(-40.1480670490586,60.285319807422,12.));
#154368=CARTESIAN_POINT('Ctrl Pts',(-40.1535332949976,60.3095377378586,
12.));
#154369=CARTESIAN_POINT('Ctrl Pts',(-40.1589852010804,60.3338003999607,
12.));
#154370=CARTESIAN_POINT('Ctrl Pts',(-40.1644226879033,60.3581076991716,
12.));
#154371=CARTESIAN_POINT('Ctrl Pts',(-40.1698456764377,60.3824595412445,
12.));
#154372=CARTESIAN_POINT('Ctrl Pts',(-40.1752540880268,60.4068558322407,
12.));
#154373=CARTESIAN_POINT('Ctrl Pts',(-40.180647844383,60.4312964785273,12.));
#154374=CARTESIAN_POINT('Ctrl Pts',(-40.1860268675883,60.455781386769,12.));
#154375=CARTESIAN_POINT('Ctrl Pts',(-40.1913910800921,60.4803104639226,
12.));
#154376=CARTESIAN_POINT('Ctrl Pts',(-40.1967404047062,60.5048836172435,
12.));
#154377=CARTESIAN_POINT('Ctrl Pts',(-40.2020747646014,60.5295007542841,
12.));
#154378=CARTESIAN_POINT('Ctrl Pts',(-40.2073940833052,60.5541617828925,
12.));
#154379=CARTESIAN_POINT('Ctrl Pts',(-40.2126982847011,60.5788666112042,
12.));
#154380=CARTESIAN_POINT('Ctrl Pts',(-40.2179872930273,60.6036151476349,
12.));
#154381=CARTESIAN_POINT('Ctrl Pts',(-40.2232610328721,60.6284073008871,
12.));
#154382=CARTESIAN_POINT('Ctrl Pts',(-40.2285194291706,60.6532429799499,
12.));
#154383=CARTESIAN_POINT('Ctrl Pts',(-40.2337624072029,60.678122094098,12.));
#154384=CARTESIAN_POINT('Ctrl Pts',(-40.2389898925932,60.7030445528857,
12.));
#154385=CARTESIAN_POINT('Ctrl Pts',(-40.2442018113108,60.728010266139,12.));
#154386=CARTESIAN_POINT('Ctrl Pts',(-40.2493980896638,60.7530191439593,
12.));
#154387=CARTESIAN_POINT('Ctrl Pts',(-40.2545786542953,60.7780710967248,
12.));
#154388=CARTESIAN_POINT('Ctrl Pts',(-40.2597434321803,60.8031660350879,
12.));
#154389=CARTESIAN_POINT('Ctrl Pts',(-40.2648923506248,60.8283038699706,
12.));
#154390=CARTESIAN_POINT('Ctrl Pts',(-40.2700253372647,60.8534845125538,
12.));
#154391=CARTESIAN_POINT('Ctrl Pts',(-40.2751423200639,60.8787078742818,
12.));
#154392=CARTESIAN_POINT('Ctrl Pts',(-40.2802432273104,60.9039738668669,
12.));
#154393=CARTESIAN_POINT('Ctrl Pts',(-40.2853279876161,60.9292824022887,
12.));
#154394=CARTESIAN_POINT('Ctrl Pts',(-40.2903965299155,60.9546333927921,
12.));
#154395=CARTESIAN_POINT('Ctrl Pts',(-40.295448783469,60.9800267508786,12.));
#154396=CARTESIAN_POINT('Ctrl Pts',(-40.300484677858,61.0054623893066,12.));
#154397=CARTESIAN_POINT('Ctrl Pts',(-40.3055041429775,61.0309402210921,
12.));
#154398=CARTESIAN_POINT('Ctrl Pts',(-40.3105071090309,61.056460159505,12.));
#154399=CARTESIAN_POINT('Ctrl Pts',(-40.3154935065262,61.0820221180645,
12.));
#154400=CARTESIAN_POINT('Ctrl Pts',(-40.3204632662725,61.1076260105258,
12.));
#154401=CARTESIAN_POINT('Ctrl Pts',(-40.32541631938,61.1332717508789,12.));
#154402=CARTESIAN_POINT('Ctrl Pts',(-40.3303525972615,61.1589592533613,
12.));
#154403=CARTESIAN_POINT('Ctrl Pts',(-40.335272031637,61.1846884324644,12.));
#154404=CARTESIAN_POINT('Ctrl Pts',(-40.340174554537,61.2104592029377,12.));
#154405=CARTESIAN_POINT('Ctrl Pts',(-40.3450600983109,61.23627147979,12.));
#154406=CARTESIAN_POINT('Ctrl Pts',(-40.3499285956304,61.2621251782863,
12.));
#154407=CARTESIAN_POINT('Ctrl Pts',(-40.3547799794679,61.2880202139371,
12.));
#154408=CARTESIAN_POINT('Ctrl Pts',(-40.3596141830791,61.3139565024847,
12.));
#154409=CARTESIAN_POINT('Ctrl Pts',(-40.3644311399861,61.3399339598853,
12.));
#154410=CARTESIAN_POINT('Ctrl Pts',(-40.3692307839636,61.3659525022908,
12.));
#154411=CARTESIAN_POINT('Ctrl Pts',(-40.3740130490225,61.3920120460219,
12.));
#154412=CARTESIAN_POINT('Ctrl Pts',(-40.3787778694364,61.4181125076037,
12.));
#154413=CARTESIAN_POINT('Ctrl Pts',(-40.383525179772,61.4442538038044,12.));
#154414=CARTESIAN_POINT('Ctrl Pts',(-40.3882549149227,61.4704358516709,
12.));
#154415=CARTESIAN_POINT('Ctrl Pts',(-40.3929670101366,61.4966585685549,
12.));
#154416=CARTESIAN_POINT('Ctrl Pts',(-40.3976614010652,61.522921872154,12.));
#154417=CARTESIAN_POINT('Ctrl Pts',(-40.4023380237232,61.5492256804717,
12.));
#154418=CARTESIAN_POINT('Ctrl Pts',(-40.4069968143956,61.5755699117324,
12.));
#154419=CARTESIAN_POINT('Ctrl Pts',(-40.4116377095596,61.601954484301,12.));
#154420=CARTESIAN_POINT('Ctrl Pts',(-40.4162606458119,61.628379316608,12.));
#154421=CARTESIAN_POINT('Ctrl Pts',(-40.4208655597717,61.6548443270394,
12.));
#154422=CARTESIAN_POINT('Ctrl Pts',(-40.425452388076,61.6813494339286,12.));
#154423=CARTESIAN_POINT('Ctrl Pts',(-40.430021067584,61.7078945557799,12.));
#154424=CARTESIAN_POINT('Ctrl Pts',(-40.4345715355404,61.7344796114399,
12.));
#154425=CARTESIAN_POINT('Ctrl Pts',(-40.4391037297588,61.7611045202874,
12.));
#154426=CARTESIAN_POINT('Ctrl Pts',(-40.4436175887949,61.7877692024076,
12.));
#154427=CARTESIAN_POINT('Ctrl Pts',(-40.4481130521364,61.814473578779,12.));
#154428=CARTESIAN_POINT('Ctrl Pts',(-40.4525900597894,61.8412175708552,
12.));
#154429=CARTESIAN_POINT('Ctrl Pts',(-40.4570485518749,61.8680011001537,
12.));
#154430=CARTESIAN_POINT('Ctrl Pts',(-40.4614884681889,61.8948240878008,
12.));
#154431=CARTESIAN_POINT('Ctrl Pts',(-40.4659097478587,61.9216864541744,
12.));
#154432=CARTESIAN_POINT('Ctrl Pts',(-40.470312328762,61.9485881182921,12.));
#154433=CARTESIAN_POINT('Ctrl Pts',(-40.4746961480015,61.9755289983044,
12.));
#154434=CARTESIAN_POINT('Ctrl Pts',(-40.4790611429583,62.0025090125959,
12.));
#154435=CARTESIAN_POINT('Ctrl Pts',(-40.4834072522164,62.029528080742,12.));
#154436=CARTESIAN_POINT('Ctrl Pts',(-40.4877344164411,62.0565861244179,
12.));
#154437=CARTESIAN_POINT('Ctrl Pts',(-40.4920425795216,62.0836830685719,
12.));
#154438=CARTESIAN_POINT('Ctrl Pts',(-40.4963316888412,62.1108188417003,
12.));
#154439=CARTESIAN_POINT('Ctrl Pts',(-40.4999919096264,62.1341126810541,
12.));
#154440=CARTESIAN_POINT('Ctrl Pts',(-40.5027877865802,62.1519925002973,
12.));
#154441=CARTESIAN_POINT('Ctrl Pts',(-40.5047277935766,62.164441150282,12.));
#154442=CARTESIAN_POINT('Ctrl Pts',(-40.5058175523127,62.17144731381,12.));
#154443=CARTESIAN_POINT('Ctrl Pts',(-40.5060598100929,62.1730054756869,
12.));
#154444=CARTESIAN_POINT('',(-39.4479504917286,57.8261117662439,0.));
#154445=CARTESIAN_POINT('',(-39.4479504917286,57.8261117662439,0.));
#154446=CARTESIAN_POINT('Ctrl Pts',(-40.5060598100929,62.1730054756869,
0.));
#154447=CARTESIAN_POINT('Ctrl Pts',(-40.5058175523127,62.17144731381,0.));
#154448=CARTESIAN_POINT('Ctrl Pts',(-40.5047277935766,62.164441150282,0.));
#154449=CARTESIAN_POINT('Ctrl Pts',(-40.5027877865802,62.1519925002973,
0.));
#154450=CARTESIAN_POINT('Ctrl Pts',(-40.4999919096264,62.1341126810541,
0.));
#154451=CARTESIAN_POINT('Ctrl Pts',(-40.4963316888412,62.1108188417003,
0.));
#154452=CARTESIAN_POINT('Ctrl Pts',(-40.4920425795216,62.0836830685719,
0.));
#154453=CARTESIAN_POINT('Ctrl Pts',(-40.4877344164411,62.0565861244179,
0.));
#154454=CARTESIAN_POINT('Ctrl Pts',(-40.4834072522164,62.029528080742,0.));
#154455=CARTESIAN_POINT('Ctrl Pts',(-40.4790611429583,62.0025090125959,
0.));
#154456=CARTESIAN_POINT('Ctrl Pts',(-40.4746961480015,61.9755289983044,
0.));
#154457=CARTESIAN_POINT('Ctrl Pts',(-40.470312328762,61.9485881182921,0.));
#154458=CARTESIAN_POINT('Ctrl Pts',(-40.4659097478587,61.9216864541744,
0.));
#154459=CARTESIAN_POINT('Ctrl Pts',(-40.4614884681889,61.8948240878008,
0.));
#154460=CARTESIAN_POINT('Ctrl Pts',(-40.4570485518749,61.8680011001537,
0.));
#154461=CARTESIAN_POINT('Ctrl Pts',(-40.4525900597894,61.8412175708552,
0.));
#154462=CARTESIAN_POINT('Ctrl Pts',(-40.4481130521364,61.814473578779,0.));
#154463=CARTESIAN_POINT('Ctrl Pts',(-40.4436175887949,61.7877692024076,
0.));
#154464=CARTESIAN_POINT('Ctrl Pts',(-40.4391037297588,61.7611045202874,
0.));
#154465=CARTESIAN_POINT('Ctrl Pts',(-40.4345715355404,61.7344796114399,
0.));
#154466=CARTESIAN_POINT('Ctrl Pts',(-40.430021067584,61.7078945557799,0.));
#154467=CARTESIAN_POINT('Ctrl Pts',(-40.425452388076,61.6813494339286,0.));
#154468=CARTESIAN_POINT('Ctrl Pts',(-40.4208655597717,61.6548443270394,
0.));
#154469=CARTESIAN_POINT('Ctrl Pts',(-40.4162606458119,61.628379316608,0.));
#154470=CARTESIAN_POINT('Ctrl Pts',(-40.4116377095596,61.601954484301,0.));
#154471=CARTESIAN_POINT('Ctrl Pts',(-40.4069968143956,61.5755699117324,
0.));
#154472=CARTESIAN_POINT('Ctrl Pts',(-40.4023380237232,61.5492256804717,
0.));
#154473=CARTESIAN_POINT('Ctrl Pts',(-40.3976614010652,61.522921872154,0.));
#154474=CARTESIAN_POINT('Ctrl Pts',(-40.3929670101366,61.4966585685549,
0.));
#154475=CARTESIAN_POINT('Ctrl Pts',(-40.3882549149227,61.4704358516709,
0.));
#154476=CARTESIAN_POINT('Ctrl Pts',(-40.383525179772,61.4442538038044,0.));
#154477=CARTESIAN_POINT('Ctrl Pts',(-40.3787778694364,61.4181125076037,
0.));
#154478=CARTESIAN_POINT('Ctrl Pts',(-40.3740130490225,61.3920120460219,
0.));
#154479=CARTESIAN_POINT('Ctrl Pts',(-40.3692307839636,61.3659525022908,
0.));
#154480=CARTESIAN_POINT('Ctrl Pts',(-40.3644311399861,61.3399339598853,
0.));
#154481=CARTESIAN_POINT('Ctrl Pts',(-40.3596141830791,61.3139565024847,
0.));
#154482=CARTESIAN_POINT('Ctrl Pts',(-40.3547799794679,61.2880202139371,
0.));
#154483=CARTESIAN_POINT('Ctrl Pts',(-40.3499285956304,61.2621251782863,
0.));
#154484=CARTESIAN_POINT('Ctrl Pts',(-40.3450600983109,61.23627147979,0.));
#154485=CARTESIAN_POINT('Ctrl Pts',(-40.340174554537,61.2104592029377,0.));
#154486=CARTESIAN_POINT('Ctrl Pts',(-40.335272031637,61.1846884324644,0.));
#154487=CARTESIAN_POINT('Ctrl Pts',(-40.3303525972615,61.1589592533613,
0.));
#154488=CARTESIAN_POINT('Ctrl Pts',(-40.32541631938,61.1332717508789,0.));
#154489=CARTESIAN_POINT('Ctrl Pts',(-40.3204632662725,61.1076260105258,
0.));
#154490=CARTESIAN_POINT('Ctrl Pts',(-40.3154935065262,61.0820221180645,
0.));
#154491=CARTESIAN_POINT('Ctrl Pts',(-40.3105071090309,61.056460159505,0.));
#154492=CARTESIAN_POINT('Ctrl Pts',(-40.3055041429775,61.0309402210921,
0.));
#154493=CARTESIAN_POINT('Ctrl Pts',(-40.300484677858,61.0054623893066,0.));
#154494=CARTESIAN_POINT('Ctrl Pts',(-40.295448783469,60.9800267508786,0.));
#154495=CARTESIAN_POINT('Ctrl Pts',(-40.2903965299155,60.9546333927921,
0.));
#154496=CARTESIAN_POINT('Ctrl Pts',(-40.2853279876161,60.9292824022887,
0.));
#154497=CARTESIAN_POINT('Ctrl Pts',(-40.2802432273104,60.9039738668669,
0.));
#154498=CARTESIAN_POINT('Ctrl Pts',(-40.2751423200639,60.8787078742818,
0.));
#154499=CARTESIAN_POINT('Ctrl Pts',(-40.2700253372647,60.8534845125538,
0.));
#154500=CARTESIAN_POINT('Ctrl Pts',(-40.2648923506248,60.8283038699706,
0.));
#154501=CARTESIAN_POINT('Ctrl Pts',(-40.2597434321803,60.8031660350879,
0.));
#154502=CARTESIAN_POINT('Ctrl Pts',(-40.2545786542953,60.7780710967248,
0.));
#154503=CARTESIAN_POINT('Ctrl Pts',(-40.2493980896638,60.7530191439593,
0.));
#154504=CARTESIAN_POINT('Ctrl Pts',(-40.2442018113108,60.728010266139,0.));
#154505=CARTESIAN_POINT('Ctrl Pts',(-40.2389898925932,60.7030445528857,
0.));
#154506=CARTESIAN_POINT('Ctrl Pts',(-40.2337624072029,60.678122094098,0.));
#154507=CARTESIAN_POINT('Ctrl Pts',(-40.2285194291706,60.6532429799499,
0.));
#154508=CARTESIAN_POINT('Ctrl Pts',(-40.2232610328721,60.6284073008871,
0.));
#154509=CARTESIAN_POINT('Ctrl Pts',(-40.2179872930273,60.6036151476349,
0.));
#154510=CARTESIAN_POINT('Ctrl Pts',(-40.2126982847011,60.5788666112042,
0.));
#154511=CARTESIAN_POINT('Ctrl Pts',(-40.2073940833052,60.5541617828925,
0.));
#154512=CARTESIAN_POINT('Ctrl Pts',(-40.2020747646014,60.5295007542841,
0.));
#154513=CARTESIAN_POINT('Ctrl Pts',(-40.1967404047062,60.5048836172435,
0.));
#154514=CARTESIAN_POINT('Ctrl Pts',(-40.1913910800921,60.4803104639226,
0.));
#154515=CARTESIAN_POINT('Ctrl Pts',(-40.1860268675883,60.455781386769,0.));
#154516=CARTESIAN_POINT('Ctrl Pts',(-40.180647844383,60.4312964785273,0.));
#154517=CARTESIAN_POINT('Ctrl Pts',(-40.1752540880268,60.4068558322407,
0.));
#154518=CARTESIAN_POINT('Ctrl Pts',(-40.1698456764377,60.3824595412445,
0.));
#154519=CARTESIAN_POINT('Ctrl Pts',(-40.1644226879033,60.3581076991716,
0.));
#154520=CARTESIAN_POINT('Ctrl Pts',(-40.1589852010804,60.3338003999607,
0.));
#154521=CARTESIAN_POINT('Ctrl Pts',(-40.1535332949976,60.3095377378586,
0.));
#154522=CARTESIAN_POINT('Ctrl Pts',(-40.1480670490586,60.285319807422,0.));
#154523=CARTESIAN_POINT('Ctrl Pts',(-40.1425865430472,60.2611467035117,
0.));
#154524=CARTESIAN_POINT('Ctrl Pts',(-40.1370918571304,60.2370185212964,
0.));
#154525=CARTESIAN_POINT('Ctrl Pts',(-40.1315830718577,60.2129353562622,
0.));
#154526=CARTESIAN_POINT('Ctrl Pts',(-40.1260602681644,60.1888973042152,
0.));
#154527=CARTESIAN_POINT('Ctrl Pts',(-40.1205235273739,60.1649044612828,
0.));
#154528=CARTESIAN_POINT('Ctrl Pts',(-40.1149729312036,60.1409569239092,
0.));
#154529=CARTESIAN_POINT('Ctrl Pts',(-40.1094085617674,60.1170547888574,
0.));
#154530=CARTESIAN_POINT('Ctrl Pts',(-40.1038305015766,60.0931981532198,
0.));
#154531=CARTESIAN_POINT('Ctrl Pts',(-40.0982388335423,60.069387114421,0.));
#154532=CARTESIAN_POINT('Ctrl Pts',(-40.0926336409785,60.0456217702202,
0.));
#154533=CARTESIAN_POINT('Ctrl Pts',(-40.0870150076074,60.021902218706,0.));
#154534=CARTESIAN_POINT('Ctrl Pts',(-40.0813830175623,59.9982285582983,
0.));
#154535=CARTESIAN_POINT('Ctrl Pts',(-40.0757377553888,59.9746008877584,
0.));
#154536=CARTESIAN_POINT('Ctrl Pts',(-40.0700793060473,59.9510193061927,
0.));
#154537=CARTESIAN_POINT('Ctrl Pts',(-40.0644077549159,59.9274839130553,
0.));
#154538=CARTESIAN_POINT('Ctrl Pts',(-40.0587231877961,59.9039948081432,
0.));
#154539=CARTESIAN_POINT('Ctrl Pts',(-40.0530256909162,59.8805520915975,
0.));
#154540=CARTESIAN_POINT('Ctrl Pts',(-40.0473153509323,59.8571558639145,
0.));
#154541=CARTESIAN_POINT('Ctrl Pts',(-40.0415922549313,59.8338062259491,
0.));
#154542=CARTESIAN_POINT('Ctrl Pts',(-40.035856490434,59.8105032789179,0.));
#154543=CARTESIAN_POINT('Ctrl Pts',(-40.0301081454006,59.7872471243948,
0.));
#154544=CARTESIAN_POINT('Ctrl Pts',(-40.0243473082343,59.7640378643115,
0.));
#154545=CARTESIAN_POINT('Ctrl Pts',(-40.0185740677827,59.7408756009688,
0.));
#154546=CARTESIAN_POINT('Ctrl Pts',(-40.0127885133407,59.7177604370409,
0.));
#154547=CARTESIAN_POINT('Ctrl Pts',(-40.0069907346536,59.6946924755771,
0.));
#154548=CARTESIAN_POINT('Ctrl Pts',(-40.001180821923,59.671671819999,0.));
#154549=CARTESIAN_POINT('Ctrl Pts',(-39.9953588658114,59.6486985741015,
0.));
#154550=CARTESIAN_POINT('Ctrl Pts',(-39.9895249574432,59.6257728420644,
0.));
#154551=CARTESIAN_POINT('Ctrl Pts',(-39.9836791884071,59.6028947284551,
0.));
#154552=CARTESIAN_POINT('Ctrl Pts',(-39.9778216507609,59.5800643382322,
0.));
#154553=CARTESIAN_POINT('Ctrl Pts',(-39.971952437036,59.5572817767412,0.));
#154554=CARTESIAN_POINT('Ctrl Pts',(-39.9660716402423,59.5345471497162,
0.));
#154555=CARTESIAN_POINT('Ctrl Pts',(-39.96017935387,59.511860563292,0.));
#154556=CARTESIAN_POINT('Ctrl Pts',(-39.954275671893,59.4892221240081,0.));
#154557=CARTESIAN_POINT('Ctrl Pts',(-39.9483606887731,59.4666319388123,
0.));
#154558=CARTESIAN_POINT('Ctrl Pts',(-39.9424344994652,59.444090115055,0.));
#154559=CARTESIAN_POINT('Ctrl Pts',(-39.9364971994215,59.4215967604925,
0.));
#154560=CARTESIAN_POINT('Ctrl Pts',(-39.9305488845934,59.3991519832981,
0.));
#154561=CARTESIAN_POINT('Ctrl Pts',(-39.9245896514359,59.3767558920663,
0.));
#154562=CARTESIAN_POINT('Ctrl Pts',(-39.9186195969113,59.3544085958165,
0.));
#154563=CARTESIAN_POINT('Ctrl Pts',(-39.9126388184956,59.3321102039883,
0.));
#154564=CARTESIAN_POINT('Ctrl Pts',(-39.9066474141826,59.3098608264452,
0.));
#154565=CARTESIAN_POINT('Ctrl Pts',(-39.9006454824861,59.2876605734871,
0.));
#154566=CARTESIAN_POINT('Ctrl Pts',(-39.8946331224442,59.2655095558527,
0.));
#154567=CARTESIAN_POINT('Ctrl Pts',(-39.8886104336234,59.2434078847236,
0.));
#154568=CARTESIAN_POINT('Ctrl Pts',(-39.8825775161252,59.2213556717189,
0.));
#154569=CARTESIAN_POINT('Ctrl Pts',(-39.8765344705894,59.1993530289008,
0.));
#154570=CARTESIAN_POINT('Ctrl Pts',(-39.8704813981978,59.1774000687865,
0.));
#154571=CARTESIAN_POINT('Ctrl Pts',(-39.8644184006785,59.155496904352,0.));
#154572=CARTESIAN_POINT('Ctrl Pts',(-39.8583455803111,59.133643649035,0.));
#154573=CARTESIAN_POINT('Ctrl Pts',(-39.8522630399337,59.1118404167304,
0.));
#154574=CARTESIAN_POINT('Ctrl Pts',(-39.8461708829465,59.0900873217992,
0.));
#154575=CARTESIAN_POINT('Ctrl Pts',(-39.8400692133143,59.068384479077,0.));
#154576=CARTESIAN_POINT('Ctrl Pts',(-39.8339581355714,59.0467320038782,
0.));
#154577=CARTESIAN_POINT('Ctrl Pts',(-39.8278377548261,59.0251300119973,
0.));
#154578=CARTESIAN_POINT('Ctrl Pts',(-39.8217081767658,59.0035786197024,
0.));
#154579=CARTESIAN_POINT('Ctrl Pts',(-39.8155695076625,58.9820779437485,
0.));
#154580=CARTESIAN_POINT('Ctrl Pts',(-39.8094218543781,58.9606281013876,
0.));
#154581=CARTESIAN_POINT('Ctrl Pts',(-39.8032653243712,58.9392292103747,
0.));
#154582=CARTESIAN_POINT('Ctrl Pts',(-39.7971000257044,58.9178813889703,
0.));
#154583=CARTESIAN_POINT('Ctrl Pts',(-39.7909260670517,58.896584755939,0.));
#154584=CARTESIAN_POINT('Ctrl Pts',(-39.7847435576995,58.8753394305583,
0.));
#154585=CARTESIAN_POINT('Ctrl Pts',(-39.7785526075477,58.8541455326229,
0.));
#154586=CARTESIAN_POINT('Ctrl Pts',(-39.772353327112,58.8330031824453,0.));
#154587=CARTESIAN_POINT('Ctrl Pts',(-39.7661458275276,58.8119125008521,
0.));
#154588=CARTESIAN_POINT('Ctrl Pts',(-39.7599302205527,58.7908736091808,
0.));
#154589=CARTESIAN_POINT('Ctrl Pts',(-39.753706618582,58.7698866293041,0.));
#154590=CARTESIAN_POINT('Ctrl Pts',(-39.7474751346603,58.7489516836453,
0.));
#154591=CARTESIAN_POINT('Ctrl Pts',(-39.7412358824949,58.7280688951911,
0.));
#154592=CARTESIAN_POINT('Ctrl Pts',(-39.7349889764737,58.7072383875009,
0.));
#154593=CARTESIAN_POINT('Ctrl Pts',(-39.7287345316664,58.6864602847064,
0.));
#154594=CARTESIAN_POINT('Ctrl Pts',(-39.7224726638087,58.6657347115014,
0.));
#154595=CARTESIAN_POINT('Ctrl Pts',(-39.7162034892896,58.6450617931269,
0.));
#154596=CARTESIAN_POINT('Ctrl Pts',(-39.7099271251421,58.6244416553574,
0.));
#154597=CARTESIAN_POINT('Ctrl Pts',(-39.7036436890248,58.6038744244683,
0.));
#154598=CARTESIAN_POINT('Ctrl Pts',(-39.6973532992555,58.5833602272767,
0.));
#154599=CARTESIAN_POINT('Ctrl Pts',(-39.6910560748639,58.5628991912067,
0.));
#154600=CARTESIAN_POINT('Ctrl Pts',(-39.6847521356395,58.5424914443415,
0.));
#154601=CARTESIAN_POINT('Ctrl Pts',(-39.6784416021817,58.5221371154748,
0.));
#154602=CARTESIAN_POINT('Ctrl Pts',(-39.6721245959516,58.5018363341582,
0.));
#154603=CARTESIAN_POINT('Ctrl Pts',(-39.66580123918,58.4815892306044,0.));
#154604=CARTESIAN_POINT('Ctrl Pts',(-39.659471654768,58.4613959355776,0.));
#154605=CARTESIAN_POINT('Ctrl Pts',(-39.6531359662043,58.4412565802984,
0.));
#154606=CARTESIAN_POINT('Ctrl Pts',(-39.6467942974464,58.4211712963024,
0.));
#154607=CARTESIAN_POINT('Ctrl Pts',(-39.6404467729113,58.4011402154225,
0.));
#154608=CARTESIAN_POINT('Ctrl Pts',(-39.6340935177492,58.3811634701061,
0.));
#154609=CARTESIAN_POINT('Ctrl Pts',(-39.6277346580898,58.3612411936914,
0.));
#154610=CARTESIAN_POINT('Ctrl Pts',(-39.6213703212523,58.3413735206412,
0.));
#154611=CARTESIAN_POINT('Ctrl Pts',(-39.6150006360894,58.3215605869192,
0.));
#154612=CARTESIAN_POINT('Ctrl Pts',(-39.6086257327559,58.3018025297288,
0.));
#154613=CARTESIAN_POINT('Ctrl Pts',(-39.6022457420772,58.2820994868092,
0.));
#154614=CARTESIAN_POINT('Ctrl Pts',(-39.5958607950237,58.2624515958416,
0.));
#154615=CARTESIAN_POINT('Ctrl Pts',(-39.5894710221729,58.2428589938394,
0.));
#154616=CARTESIAN_POINT('Ctrl Pts',(-39.5830765530919,58.2233218164407,
0.));
#154617=CARTESIAN_POINT('Ctrl Pts',(-39.5766775175226,58.2038401992496,
0.));
#154618=CARTESIAN_POINT('Ctrl Pts',(-39.5702740468013,58.1844142794359,
0.));
#154619=CARTESIAN_POINT('Ctrl Pts',(-39.5638662750174,58.1650441970379,
0.));
#154620=CARTESIAN_POINT('Ctrl Pts',(-39.5574543406959,58.1457300968467,
0.));
#154621=CARTESIAN_POINT('Ctrl Pts',(-39.5510383869476,58.1264721285698,
0.));
#154622=CARTESIAN_POINT('Ctrl Pts',(-39.5446185579615,58.1072704428895,
0.));
#154623=CARTESIAN_POINT('Ctrl Pts',(-39.5381949959214,58.088125187991,0.));
#154624=CARTESIAN_POINT('Ctrl Pts',(-39.5317678383231,58.0690365065393,
0.));
#154625=CARTESIAN_POINT('Ctrl Pts',(-39.5253372136921,58.050004530846,0.));
#154626=CARTESIAN_POINT('Ctrl Pts',(-39.5189032457227,58.0310293875321,
0.));
#154627=CARTESIAN_POINT('Ctrl Pts',(-39.5124660615009,58.012111206794,0.));
#154628=CARTESIAN_POINT('Ctrl Pts',(-39.5060257981225,57.9932501298522,
0.));
#154629=CARTESIAN_POINT('Ctrl Pts',(-39.4995826106691,57.9744463179305,
0.));
#154630=CARTESIAN_POINT('Ctrl Pts',(-39.4931366776627,57.9556999583777,
0.));
#154631=CARTESIAN_POINT('Ctrl Pts',(-39.4866881842223,57.9370112456506,
0.));
#154632=CARTESIAN_POINT('Ctrl Pts',(-39.4802373061008,57.9183803632337,
0.));
#154633=CARTESIAN_POINT('Ctrl Pts',(-39.4737841949417,57.8998074670541,
0.));
#154634=CARTESIAN_POINT('Ctrl Pts',(-39.4673289592425,57.8812926637397,
0.));
#154635=CARTESIAN_POINT('Ctrl Pts',(-39.4608716627367,57.8628360097134,
0.));
#154636=CARTESIAN_POINT('Ctrl Pts',(-39.4557042029884,57.8481172247805,
0.));
#154637=CARTESIAN_POINT('Ctrl Pts',(-39.45182770037,57.8371043151607,0.));
#154638=CARTESIAN_POINT('Ctrl Pts',(-39.4492429618498,57.829774010102,0.));
#154639=CARTESIAN_POINT('Ctrl Pts',(-39.4479504917286,57.8261117662439,
0.));
#154640=CARTESIAN_POINT('Ctrl Pts',(-34.9532422808861,65.7914953018525,
0.));
#154641=CARTESIAN_POINT('Ctrl Pts',(-34.9532422808861,65.7914953018525,
12.));
#154642=CARTESIAN_POINT('Ctrl Pts',(-34.9529266758466,65.7859084407617,
0.));
#154643=CARTESIAN_POINT('Ctrl Pts',(-34.9529266758466,65.7859084407617,
12.));
#154644=CARTESIAN_POINT('Ctrl Pts',(-34.9522931728759,65.7747383251112,
0.));
#154645=CARTESIAN_POINT('Ctrl Pts',(-34.9522931728759,65.7747383251112,
12.));
#154646=CARTESIAN_POINT('Ctrl Pts',(-34.9513360397454,65.7579939712289,
0.));
#154647=CARTESIAN_POINT('Ctrl Pts',(-34.9513360397454,65.7579939712289,
12.));
#154648=CARTESIAN_POINT('Ctrl Pts',(-34.9500461043246,65.7356898061147,
0.));
#154649=CARTESIAN_POINT('Ctrl Pts',(-34.9500461043246,65.7356898061147,
12.));
#154650=CARTESIAN_POINT('Ctrl Pts',(-34.9484107544137,65.7078456758034,
0.));
#154651=CARTESIAN_POINT('Ctrl Pts',(-34.9484107544137,65.7078456758034,
12.));
#154652=CARTESIAN_POINT('Ctrl Pts',(-34.9467524770439,65.6800376406066,
0.));
#154653=CARTESIAN_POINT('Ctrl Pts',(-34.9467524770439,65.6800376406066,
12.));
#154654=CARTESIAN_POINT('Ctrl Pts',(-34.9450712829183,65.6522657321322,
0.));
#154655=CARTESIAN_POINT('Ctrl Pts',(-34.9450712829183,65.6522657321322,
12.));
#154656=CARTESIAN_POINT('Ctrl Pts',(-34.943367193292,65.624529996851,0.));
#154657=CARTESIAN_POINT('Ctrl Pts',(-34.943367193292,65.624529996851,12.));
#154658=CARTESIAN_POINT('Ctrl Pts',(-34.9416402443435,65.5968304997584,
0.));
#154659=CARTESIAN_POINT('Ctrl Pts',(-34.9416402443435,65.5968304997584,
12.));
#154660=CARTESIAN_POINT('Ctrl Pts',(-34.9398904862157,65.5691673225803,
0.));
#154661=CARTESIAN_POINT('Ctrl Pts',(-34.9398904862157,65.5691673225803,
12.));
#154662=CARTESIAN_POINT('Ctrl Pts',(-34.9381179779673,65.5415405577955,
0.));
#154663=CARTESIAN_POINT('Ctrl Pts',(-34.9381179779673,65.5415405577955,
12.));
#154664=CARTESIAN_POINT('Ctrl Pts',(-34.9363227836582,65.5139503038036,
0.));
#154665=CARTESIAN_POINT('Ctrl Pts',(-34.9363227836582,65.5139503038036,
12.));
#154666=CARTESIAN_POINT('Ctrl Pts',(-34.9345049680825,65.4863966597544,
0.));
#154667=CARTESIAN_POINT('Ctrl Pts',(-34.9345049680825,65.4863966597544,
12.));
#154668=CARTESIAN_POINT('Ctrl Pts',(-34.932664592394,65.4588797201972,0.));
#154669=CARTESIAN_POINT('Ctrl Pts',(-34.932664592394,65.4588797201972,12.));
#154670=CARTESIAN_POINT('Ctrl Pts',(-34.9308017105536,65.4313995707536,
0.));
#154671=CARTESIAN_POINT('Ctrl Pts',(-34.9308017105536,65.4313995707536,
12.));
#154672=CARTESIAN_POINT('Ctrl Pts',(-34.9289163717747,65.4039562911352,
0.));
#154673=CARTESIAN_POINT('Ctrl Pts',(-34.9289163717747,65.4039562911352,
12.));
#154674=CARTESIAN_POINT('Ctrl Pts',(-34.9270086222731,65.3765499573077,
0.));
#154675=CARTESIAN_POINT('Ctrl Pts',(-34.9270086222731,65.3765499573077,
12.));
#154676=CARTESIAN_POINT('Ctrl Pts',(-34.9250785073477,65.3491806440537,
0.));
#154677=CARTESIAN_POINT('Ctrl Pts',(-34.9250785073477,65.3491806440537,
12.));
#154678=CARTESIAN_POINT('Ctrl Pts',(-34.9231260731831,65.321848427191,0.));
#154679=CARTESIAN_POINT('Ctrl Pts',(-34.9231260731831,65.321848427191,12.));
#154680=CARTESIAN_POINT('Ctrl Pts',(-34.9211513691355,65.2945533863761,
0.));
#154681=CARTESIAN_POINT('Ctrl Pts',(-34.9211513691355,65.2945533863761,
12.));
#154682=CARTESIAN_POINT('Ctrl Pts',(-34.9191544474872,65.2672956048069,
0.));
#154683=CARTESIAN_POINT('Ctrl Pts',(-34.9191544474872,65.2672956048069,
12.));
#154684=CARTESIAN_POINT('Ctrl Pts',(-34.9171353624113,65.2400751679549,
0.));
#154685=CARTESIAN_POINT('Ctrl Pts',(-34.9171353624113,65.2400751679549,
12.));
#154686=CARTESIAN_POINT('Ctrl Pts',(-34.9150941691747,65.2128921625823,
0.));
#154687=CARTESIAN_POINT('Ctrl Pts',(-34.9150941691747,65.2128921625823,
12.));
#154688=CARTESIAN_POINT('Ctrl Pts',(-34.9130309233022,65.1857466757092,
0.));
#154689=CARTESIAN_POINT('Ctrl Pts',(-34.9130309233022,65.1857466757092,
12.));
#154690=CARTESIAN_POINT('Ctrl Pts',(-34.9109456796213,65.1586387934241,
0.));
#154691=CARTESIAN_POINT('Ctrl Pts',(-34.9109456796213,65.1586387934241,
12.));
#154692=CARTESIAN_POINT('Ctrl Pts',(-34.9088384918336,65.1315686003516,
0.));
#154693=CARTESIAN_POINT('Ctrl Pts',(-34.9088384918336,65.1315686003516,
12.));
#154694=CARTESIAN_POINT('Ctrl Pts',(-34.9067094130399,65.1045361803121,
0.));
#154695=CARTESIAN_POINT('Ctrl Pts',(-34.9067094130399,65.1045361803121,
12.));
#154696=CARTESIAN_POINT('Ctrl Pts',(-34.9045584960509,65.0775416167085,
0.));
#154697=CARTESIAN_POINT('Ctrl Pts',(-34.9045584960509,65.0775416167085,
12.));
#154698=CARTESIAN_POINT('Ctrl Pts',(-34.9023857937865,65.0505849930171,
0.));
#154699=CARTESIAN_POINT('Ctrl Pts',(-34.9023857937865,65.0505849930171,
12.));
#154700=CARTESIAN_POINT('Ctrl Pts',(-34.9001913596416,65.0236663932328,
0.));
#154701=CARTESIAN_POINT('Ctrl Pts',(-34.9001913596416,65.0236663932328,
12.));
#154702=CARTESIAN_POINT('Ctrl Pts',(-34.8979752478616,64.9967859023212,
0.));
#154703=CARTESIAN_POINT('Ctrl Pts',(-34.8979752478616,64.9967859023212,
12.));
#154704=CARTESIAN_POINT('Ctrl Pts',(-34.8957375133697,64.9699436060169,
0.));
#154705=CARTESIAN_POINT('Ctrl Pts',(-34.8957375133697,64.9699436060169,
12.));
#154706=CARTESIAN_POINT('Ctrl Pts',(-34.8934782116095,64.9431395906337,
0.));
#154707=CARTESIAN_POINT('Ctrl Pts',(-34.8934782116095,64.9431395906337,
12.));
#154708=CARTESIAN_POINT('Ctrl Pts',(-34.8911973983785,64.9163739428605,
0.));
#154709=CARTESIAN_POINT('Ctrl Pts',(-34.8911973983785,64.9163739428605,
12.));
#154710=CARTESIAN_POINT('Ctrl Pts',(-34.888895129681,64.8896467495757,0.));
#154711=CARTESIAN_POINT('Ctrl Pts',(-34.888895129681,64.8896467495757,12.));
#154712=CARTESIAN_POINT('Ctrl Pts',(-34.8865714615436,64.8629580976063,
0.));
#154713=CARTESIAN_POINT('Ctrl Pts',(-34.8865714615436,64.8629580976063,
12.));
#154714=CARTESIAN_POINT('Ctrl Pts',(-34.8842264500188,64.8363080737377,
0.));
#154715=CARTESIAN_POINT('Ctrl Pts',(-34.8842264500188,64.8363080737377,
12.));
#154716=CARTESIAN_POINT('Ctrl Pts',(-34.881860151273,64.8096967648307,0.));
#154717=CARTESIAN_POINT('Ctrl Pts',(-34.881860151273,64.8096967648307,12.));
#154718=CARTESIAN_POINT('Ctrl Pts',(-34.8794726216513,64.7831242579028,
0.));
#154719=CARTESIAN_POINT('Ctrl Pts',(-34.8794726216513,64.7831242579028,
12.));
#154720=CARTESIAN_POINT('Ctrl Pts',(-34.8770639177493,64.7565906402151,
0.));
#154721=CARTESIAN_POINT('Ctrl Pts',(-34.8770639177493,64.7565906402151,
12.));
#154722=CARTESIAN_POINT('Ctrl Pts',(-34.8746340964971,64.7300959993653,
0.));
#154723=CARTESIAN_POINT('Ctrl Pts',(-34.8746340964971,64.7300959993653,
12.));
#154724=CARTESIAN_POINT('Ctrl Pts',(-34.8721832151974,64.7036404233306,
0.));
#154725=CARTESIAN_POINT('Ctrl Pts',(-34.8721832151974,64.7036404233306,
12.));
#154726=CARTESIAN_POINT('Ctrl Pts',(-34.869711331479,64.6772240004228,0.));
#154727=CARTESIAN_POINT('Ctrl Pts',(-34.869711331479,64.6772240004228,12.));
#154728=CARTESIAN_POINT('Ctrl Pts',(-34.867218503272,64.6508468192599,0.));
#154729=CARTESIAN_POINT('Ctrl Pts',(-34.867218503272,64.6508468192599,12.));
#154730=CARTESIAN_POINT('Ctrl Pts',(-34.8647047887774,64.6245089687277,
0.));
#154731=CARTESIAN_POINT('Ctrl Pts',(-34.8647047887774,64.6245089687277,
12.));
#154732=CARTESIAN_POINT('Ctrl Pts',(-34.8621702464401,64.5982105379383,
0.));
#154733=CARTESIAN_POINT('Ctrl Pts',(-34.8621702464401,64.5982105379383,
12.));
#154734=CARTESIAN_POINT('Ctrl Pts',(-34.8596149349257,64.5719516161927,
0.));
#154735=CARTESIAN_POINT('Ctrl Pts',(-34.8596149349257,64.5719516161927,
12.));
#154736=CARTESIAN_POINT('Ctrl Pts',(-34.857038913134,64.5457322930088,0.));
#154737=CARTESIAN_POINT('Ctrl Pts',(-34.857038913134,64.5457322930088,12.));
#154738=CARTESIAN_POINT('Ctrl Pts',(-34.8544422402118,64.5195526581407,
0.));
#154739=CARTESIAN_POINT('Ctrl Pts',(-34.8544422402118,64.5195526581407,
12.));
#154740=CARTESIAN_POINT('Ctrl Pts',(-34.851824975568,64.4934128015985,0.));
#154741=CARTESIAN_POINT('Ctrl Pts',(-34.851824975568,64.4934128015985,12.));
#154742=CARTESIAN_POINT('Ctrl Pts',(-34.8491871788895,64.4673128136625,
0.));
#154743=CARTESIAN_POINT('Ctrl Pts',(-34.8491871788895,64.4673128136625,
12.));
#154744=CARTESIAN_POINT('Ctrl Pts',(-34.8465289101621,64.4412527848969,
0.));
#154745=CARTESIAN_POINT('Ctrl Pts',(-34.8465289101621,64.4412527848969,
12.));
#154746=CARTESIAN_POINT('Ctrl Pts',(-34.8438502296664,64.4152328061515,
0.));
#154747=CARTESIAN_POINT('Ctrl Pts',(-34.8438502296664,64.4152328061515,
12.));
#154748=CARTESIAN_POINT('Ctrl Pts',(-34.8411511979702,64.3892529685607,
0.));
#154749=CARTESIAN_POINT('Ctrl Pts',(-34.8411511979702,64.3892529685607,
12.));
#154750=CARTESIAN_POINT('Ctrl Pts',(-34.8384318759248,64.3633133635382,
0.));
#154751=CARTESIAN_POINT('Ctrl Pts',(-34.8384318759248,64.3633133635382,
12.));
#154752=CARTESIAN_POINT('Ctrl Pts',(-34.8356923246618,64.3374140827711,
0.));
#154753=CARTESIAN_POINT('Ctrl Pts',(-34.8356923246618,64.3374140827711,
12.));
#154754=CARTESIAN_POINT('Ctrl Pts',(-34.8329326055919,64.3115552182062,
0.));
#154755=CARTESIAN_POINT('Ctrl Pts',(-34.8329326055919,64.3115552182062,
12.));
#154756=CARTESIAN_POINT('Ctrl Pts',(-34.8301527804054,64.285736862052,0.));
#154757=CARTESIAN_POINT('Ctrl Pts',(-34.8301527804054,64.285736862052,12.));
#154758=CARTESIAN_POINT('Ctrl Pts',(-34.8273529110744,64.2599591067916,
0.));
#154759=CARTESIAN_POINT('Ctrl Pts',(-34.8273529110744,64.2599591067916,
12.));
#154760=CARTESIAN_POINT('Ctrl Pts',(-34.8245330598559,64.234222045188,0.));
#154761=CARTESIAN_POINT('Ctrl Pts',(-34.8245330598559,64.234222045188,12.));
#154762=CARTESIAN_POINT('Ctrl Pts',(-34.8216932892968,64.2085257702884,
0.));
#154763=CARTESIAN_POINT('Ctrl Pts',(-34.8216932892968,64.2085257702884,
12.));
#154764=CARTESIAN_POINT('Ctrl Pts',(-34.8188336622419,64.1828703754236,
0.));
#154765=CARTESIAN_POINT('Ctrl Pts',(-34.8188336622419,64.1828703754236,
12.));
#154766=CARTESIAN_POINT('Ctrl Pts',(-34.8159542418374,64.1572559542086,
0.));
#154767=CARTESIAN_POINT('Ctrl Pts',(-34.8159542418374,64.1572559542086,
12.));
#154768=CARTESIAN_POINT('Ctrl Pts',(-34.8130550915287,64.1316826005506,
0.));
#154769=CARTESIAN_POINT('Ctrl Pts',(-34.8130550915287,64.1316826005506,
12.));
#154770=CARTESIAN_POINT('Ctrl Pts',(-34.8101362750597,64.1061504086515,
0.));
#154771=CARTESIAN_POINT('Ctrl Pts',(-34.8101362750597,64.1061504086515,
12.));
#154772=CARTESIAN_POINT('Ctrl Pts',(-34.8071978564747,64.0806594730085,
0.));
#154773=CARTESIAN_POINT('Ctrl Pts',(-34.8071978564747,64.0806594730085,
12.));
#154774=CARTESIAN_POINT('Ctrl Pts',(-34.8042399001211,64.0552098884095,
0.));
#154775=CARTESIAN_POINT('Ctrl Pts',(-34.8042399001211,64.0552098884095,
12.));
#154776=CARTESIAN_POINT('Ctrl Pts',(-34.8012624706526,64.0298017499294,
0.));
#154777=CARTESIAN_POINT('Ctrl Pts',(-34.8012624706526,64.0298017499294,
12.));
#154778=CARTESIAN_POINT('Ctrl Pts',(-34.7982656330293,64.0044351529402,
0.));
#154779=CARTESIAN_POINT('Ctrl Pts',(-34.7982656330293,64.0044351529402,
12.));
#154780=CARTESIAN_POINT('Ctrl Pts',(-34.7952494525177,63.9791101931162,
0.));
#154781=CARTESIAN_POINT('Ctrl Pts',(-34.7952494525177,63.9791101931162,
12.));
#154782=CARTESIAN_POINT('Ctrl Pts',(-34.7922139946943,63.9538269664366,
0.));
#154783=CARTESIAN_POINT('Ctrl Pts',(-34.7922139946943,63.9538269664366,
12.));
#154784=CARTESIAN_POINT('Ctrl Pts',(-34.7891593254488,63.9285855691845,
0.));
#154785=CARTESIAN_POINT('Ctrl Pts',(-34.7891593254488,63.9285855691845,
12.));
#154786=CARTESIAN_POINT('Ctrl Pts',(-34.7860855109911,63.9033860979435,
0.));
#154787=CARTESIAN_POINT('Ctrl Pts',(-34.7860855109911,63.9033860979435,
12.));
#154788=CARTESIAN_POINT('Ctrl Pts',(-34.7829926178496,63.8782286496062,
0.));
#154789=CARTESIAN_POINT('Ctrl Pts',(-34.7829926178496,63.8782286496062,
12.));
#154790=CARTESIAN_POINT('Ctrl Pts',(-34.7798807128715,63.8531133213793,
0.));
#154791=CARTESIAN_POINT('Ctrl Pts',(-34.7798807128715,63.8531133213793,
12.));
#154792=CARTESIAN_POINT('Ctrl Pts',(-34.7767498632243,63.8280402107856,
0.));
#154793=CARTESIAN_POINT('Ctrl Pts',(-34.7767498632243,63.8280402107856,
12.));
#154794=CARTESIAN_POINT('Ctrl Pts',(-34.7736001363993,63.8030094156639,
0.));
#154795=CARTESIAN_POINT('Ctrl Pts',(-34.7736001363993,63.8030094156639,
12.));
#154796=CARTESIAN_POINT('Ctrl Pts',(-34.7704316002171,63.778021034163,0.));
#154797=CARTESIAN_POINT('Ctrl Pts',(-34.7704316002171,63.778021034163,12.));
#154798=CARTESIAN_POINT('Ctrl Pts',(-34.7672443228275,63.7530751647494,
0.));
#154799=CARTESIAN_POINT('Ctrl Pts',(-34.7672443228275,63.7530751647494,
12.));
#154800=CARTESIAN_POINT('Ctrl Pts',(-34.7640383727101,63.7281719062149,
0.));
#154801=CARTESIAN_POINT('Ctrl Pts',(-34.7640383727101,63.7281719062149,
12.));
#154802=CARTESIAN_POINT('Ctrl Pts',(-34.7608138186759,63.7033113576785,
0.));
#154803=CARTESIAN_POINT('Ctrl Pts',(-34.7608138186759,63.7033113576785,
12.));
#154804=CARTESIAN_POINT('Ctrl Pts',(-34.7575707298713,63.6784936185885,
0.));
#154805=CARTESIAN_POINT('Ctrl Pts',(-34.7575707298713,63.6784936185885,
12.));
#154806=CARTESIAN_POINT('Ctrl Pts',(-34.7543091757833,63.6537187887159,
0.));
#154807=CARTESIAN_POINT('Ctrl Pts',(-34.7543091757833,63.6537187887159,
12.));
#154808=CARTESIAN_POINT('Ctrl Pts',(-34.7510292262406,63.6289869681604,
0.));
#154809=CARTESIAN_POINT('Ctrl Pts',(-34.7510292262406,63.6289869681604,
12.));
#154810=CARTESIAN_POINT('Ctrl Pts',(-34.7477309514136,63.6042982573588,
0.));
#154811=CARTESIAN_POINT('Ctrl Pts',(-34.7477309514136,63.6042982573588,
12.));
#154812=CARTESIAN_POINT('Ctrl Pts',(-34.744414421816,63.5796527570871,0.));
#154813=CARTESIAN_POINT('Ctrl Pts',(-34.744414421816,63.5796527570871,12.));
#154814=CARTESIAN_POINT('Ctrl Pts',(-34.7410797083081,63.5550505684626,
0.));
#154815=CARTESIAN_POINT('Ctrl Pts',(-34.7410797083081,63.5550505684626,
12.));
#154816=CARTESIAN_POINT('Ctrl Pts',(-34.7377268821025,63.5304917929386,
0.));
#154817=CARTESIAN_POINT('Ctrl Pts',(-34.7377268821025,63.5304917929386,
12.));
#154818=CARTESIAN_POINT('Ctrl Pts',(-34.7343560147667,63.505976532309,0.));
#154819=CARTESIAN_POINT('Ctrl Pts',(-34.7343560147667,63.505976532309,12.));
#154820=CARTESIAN_POINT('Ctrl Pts',(-34.7309671782214,63.4815048887165,
0.));
#154821=CARTESIAN_POINT('Ctrl Pts',(-34.7309671782214,63.4815048887165,
12.));
#154822=CARTESIAN_POINT('Ctrl Pts',(-34.7275604447439,63.4570769646569,
0.));
#154823=CARTESIAN_POINT('Ctrl Pts',(-34.7275604447439,63.4570769646569,
12.));
#154824=CARTESIAN_POINT('Ctrl Pts',(-34.7241358869701,63.4326928629795,
0.));
#154825=CARTESIAN_POINT('Ctrl Pts',(-34.7241358869701,63.4326928629795,
12.));
#154826=CARTESIAN_POINT('Ctrl Pts',(-34.7206935779007,63.4083526868836,
0.));
#154827=CARTESIAN_POINT('Ctrl Pts',(-34.7206935779007,63.4083526868836,
12.));
#154828=CARTESIAN_POINT('Ctrl Pts',(-34.7172335909038,63.3840565399208,
0.));
#154829=CARTESIAN_POINT('Ctrl Pts',(-34.7172335909038,63.3840565399208,
12.));
#154830=CARTESIAN_POINT('Ctrl Pts',(-34.7137559997146,63.3598045260053,
0.));
#154831=CARTESIAN_POINT('Ctrl Pts',(-34.7137559997146,63.3598045260053,
12.));
#154832=CARTESIAN_POINT('Ctrl Pts',(-34.7102608784374,63.3355967494171,
0.));
#154833=CARTESIAN_POINT('Ctrl Pts',(-34.7102608784374,63.3355967494171,
12.));
#154834=CARTESIAN_POINT('Ctrl Pts',(-34.7067483015491,63.3114333148048,
0.));
#154835=CARTESIAN_POINT('Ctrl Pts',(-34.7067483015491,63.3114333148048,
12.));
#154836=CARTESIAN_POINT('Ctrl Pts',(-34.703218343904,63.2873143271807,0.));
#154837=CARTESIAN_POINT('Ctrl Pts',(-34.703218343904,63.2873143271807,12.));
#154838=CARTESIAN_POINT('Ctrl Pts',(-34.6996710807378,63.2632398919225,
0.));
#154839=CARTESIAN_POINT('Ctrl Pts',(-34.6996710807378,63.2632398919225,
12.));
#154840=CARTESIAN_POINT('Ctrl Pts',(-34.6961065876666,63.2392101147847,
0.));
#154841=CARTESIAN_POINT('Ctrl Pts',(-34.6961065876666,63.2392101147847,
12.));
#154842=CARTESIAN_POINT('Ctrl Pts',(-34.6925249406897,63.2152251019012,
0.));
#154843=CARTESIAN_POINT('Ctrl Pts',(-34.6925249406897,63.2152251019012,
12.));
#154844=CARTESIAN_POINT('Ctrl Pts',(-34.6889262161924,63.1912849597887,
0.));
#154845=CARTESIAN_POINT('Ctrl Pts',(-34.6889262161924,63.1912849597887,
12.));
#154846=CARTESIAN_POINT('Ctrl Pts',(-34.6853104909518,63.1673897953429,
0.));
#154847=CARTESIAN_POINT('Ctrl Pts',(-34.6853104909518,63.1673897953429,
12.));
#154848=CARTESIAN_POINT('Ctrl Pts',(-34.6816778421402,63.1435397158388,
0.));
#154849=CARTESIAN_POINT('Ctrl Pts',(-34.6816778421402,63.1435397158388,
12.));
#154850=CARTESIAN_POINT('Ctrl Pts',(-34.6780283473252,63.119734828943,0.));
#154851=CARTESIAN_POINT('Ctrl Pts',(-34.6780283473252,63.119734828943,12.));
#154852=CARTESIAN_POINT('Ctrl Pts',(-34.674362084472,63.0959752427168,0.));
#154853=CARTESIAN_POINT('Ctrl Pts',(-34.674362084472,63.0959752427168,12.));
#154854=CARTESIAN_POINT('Ctrl Pts',(-34.670679131947,63.0722610656194,0.));
#154855=CARTESIAN_POINT('Ctrl Pts',(-34.670679131947,63.0722610656194,12.));
#154856=CARTESIAN_POINT('Ctrl Pts',(-34.6669795685228,63.0485924065045,
0.));
#154857=CARTESIAN_POINT('Ctrl Pts',(-34.6669795685228,63.0485924065045,
12.));
#154858=CARTESIAN_POINT('Ctrl Pts',(-34.6632634733824,63.0249693746208,
0.));
#154859=CARTESIAN_POINT('Ctrl Pts',(-34.6632634733824,63.0249693746208,
12.));
#154860=CARTESIAN_POINT('Ctrl Pts',(-34.6595309261191,63.0013920796235,
0.));
#154861=CARTESIAN_POINT('Ctrl Pts',(-34.6595309261191,63.0013920796235,
12.));
#154862=CARTESIAN_POINT('Ctrl Pts',(-34.6557820067393,62.9778606315783,
0.));
#154863=CARTESIAN_POINT('Ctrl Pts',(-34.6557820067393,62.9778606315783,
12.));
#154864=CARTESIAN_POINT('Ctrl Pts',(-34.6520167956655,62.9543751409645,
0.));
#154865=CARTESIAN_POINT('Ctrl Pts',(-34.6520167956655,62.9543751409645,
12.));
#154866=CARTESIAN_POINT('Ctrl Pts',(-34.6482353737424,62.9309357186717,
0.));
#154867=CARTESIAN_POINT('Ctrl Pts',(-34.6482353737424,62.9309357186717,
12.));
#154868=CARTESIAN_POINT('Ctrl Pts',(-34.6444378222411,62.9075424760015,
0.));
#154869=CARTESIAN_POINT('Ctrl Pts',(-34.6444378222411,62.9075424760015,
12.));
#154870=CARTESIAN_POINT('Ctrl Pts',(-34.6406242228592,62.8841955246794,
0.));
#154871=CARTESIAN_POINT('Ctrl Pts',(-34.6406242228592,62.8841955246794,
12.));
#154872=CARTESIAN_POINT('Ctrl Pts',(-34.6367946577235,62.8608949768571,
0.));
#154873=CARTESIAN_POINT('Ctrl Pts',(-34.6367946577235,62.8608949768571,
12.));
#154874=CARTESIAN_POINT('Ctrl Pts',(-34.6329492093935,62.8376409451175,
0.));
#154875=CARTESIAN_POINT('Ctrl Pts',(-34.6329492093935,62.8376409451175,
12.));
#154876=CARTESIAN_POINT('Ctrl Pts',(-34.6290879608673,62.8144335424697,
0.));
#154877=CARTESIAN_POINT('Ctrl Pts',(-34.6290879608673,62.8144335424697,
12.));
#154878=CARTESIAN_POINT('Ctrl Pts',(-34.6252109955853,62.7912728823518,
0.));
#154879=CARTESIAN_POINT('Ctrl Pts',(-34.6252109955853,62.7912728823518,
12.));
#154880=CARTESIAN_POINT('Ctrl Pts',(-34.6213183974317,62.7681590786429,
0.));
#154881=CARTESIAN_POINT('Ctrl Pts',(-34.6213183974317,62.7681590786429,
12.));
#154882=CARTESIAN_POINT('Ctrl Pts',(-34.6174102507375,62.7450922456676,
0.));
#154883=CARTESIAN_POINT('Ctrl Pts',(-34.6174102507375,62.7450922456676,
12.));
#154884=CARTESIAN_POINT('Ctrl Pts',(-34.6134866402837,62.7220724981994,
0.));
#154885=CARTESIAN_POINT('Ctrl Pts',(-34.6134866402837,62.7220724981994,
12.));
#154886=CARTESIAN_POINT('Ctrl Pts',(-34.6095476513077,62.6990999514563,
0.));
#154887=CARTESIAN_POINT('Ctrl Pts',(-34.6095476513077,62.6990999514563,
12.));
#154888=CARTESIAN_POINT('Ctrl Pts',(-34.6055933695069,62.6761747211037,
0.));
#154889=CARTESIAN_POINT('Ctrl Pts',(-34.6055933695069,62.6761747211037,
12.));
#154890=CARTESIAN_POINT('Ctrl Pts',(-34.6016238810399,62.6532969232657,
0.));
#154891=CARTESIAN_POINT('Ctrl Pts',(-34.6016238810399,62.6532969232657,
12.));
#154892=CARTESIAN_POINT('Ctrl Pts',(-34.5976392725296,62.6304666745306,
0.));
#154893=CARTESIAN_POINT('Ctrl Pts',(-34.5976392725296,62.6304666745306,
12.));
#154894=CARTESIAN_POINT('Ctrl Pts',(-34.5936396310679,62.6076840919536,
0.));
#154895=CARTESIAN_POINT('Ctrl Pts',(-34.5936396310679,62.6076840919536,
12.));
#154896=CARTESIAN_POINT('Ctrl Pts',(-34.5896250442216,62.5849492930533,
0.));
#154897=CARTESIAN_POINT('Ctrl Pts',(-34.5896250442216,62.5849492930533,
12.));
#154898=CARTESIAN_POINT('Ctrl Pts',(-34.5855956000363,62.562262395816,0.));
#154899=CARTESIAN_POINT('Ctrl Pts',(-34.5855956000363,62.562262395816,12.));
#154900=CARTESIAN_POINT('Ctrl Pts',(-34.5815513870377,62.5396235187079,
0.));
#154901=CARTESIAN_POINT('Ctrl Pts',(-34.5815513870377,62.5396235187079,
12.));
#154902=CARTESIAN_POINT('Ctrl Pts',(-34.5774924942355,62.5170327806781,
0.));
#154903=CARTESIAN_POINT('Ctrl Pts',(-34.5774924942355,62.5170327806781,
12.));
#154904=CARTESIAN_POINT('Ctrl Pts',(-34.5734190111272,62.4944903011628,
0.));
#154905=CARTESIAN_POINT('Ctrl Pts',(-34.5734190111272,62.4944903011628,
12.));
#154906=CARTESIAN_POINT('Ctrl Pts',(-34.5693310277051,62.4719962000808,
0.));
#154907=CARTESIAN_POINT('Ctrl Pts',(-34.5693310277051,62.4719962000808,
12.));
#154908=CARTESIAN_POINT('Ctrl Pts',(-34.5652286344593,62.4495505978393,
0.));
#154909=CARTESIAN_POINT('Ctrl Pts',(-34.5652286344593,62.4495505978393,
12.));
#154910=CARTESIAN_POINT('Ctrl Pts',(-34.5611119223798,62.4271536153459,
0.));
#154911=CARTESIAN_POINT('Ctrl Pts',(-34.5611119223798,62.4271536153459,
12.));
#154912=CARTESIAN_POINT('Ctrl Pts',(-34.5569809829613,62.4048053740127,
0.));
#154913=CARTESIAN_POINT('Ctrl Pts',(-34.5569809829613,62.4048053740127,
12.));
#154914=CARTESIAN_POINT('Ctrl Pts',(-34.5528359082075,62.3825059957601,
0.));
#154915=CARTESIAN_POINT('Ctrl Pts',(-34.5528359082075,62.3825059957601,
12.));
#154916=CARTESIAN_POINT('Ctrl Pts',(-34.5486767906384,62.3602556030127,
0.));
#154917=CARTESIAN_POINT('Ctrl Pts',(-34.5486767906384,62.3602556030127,
12.));
#154918=CARTESIAN_POINT('Ctrl Pts',(-34.5445037232936,62.338054318708,0.));
#154919=CARTESIAN_POINT('Ctrl Pts',(-34.5445037232936,62.338054318708,12.));
#154920=CARTESIAN_POINT('Ctrl Pts',(-34.5403167997337,62.3159022663058,
0.));
#154921=CARTESIAN_POINT('Ctrl Pts',(-34.5403167997337,62.3159022663058,
12.));
#154922=CARTESIAN_POINT('Ctrl Pts',(-34.5361161140449,62.2937995697925,
0.));
#154923=CARTESIAN_POINT('Ctrl Pts',(-34.5361161140449,62.2937995697925,
12.));
#154924=CARTESIAN_POINT('Ctrl Pts',(-34.5319017608433,62.2717463536827,
0.));
#154925=CARTESIAN_POINT('Ctrl Pts',(-34.5319017608433,62.2717463536827,
12.));
#154926=CARTESIAN_POINT('Ctrl Pts',(-34.5276738352808,62.2497427430135,
0.));
#154927=CARTESIAN_POINT('Ctrl Pts',(-34.5276738352808,62.2497427430135,
12.));
#154928=CARTESIAN_POINT('Ctrl Pts',(-34.523432433049,62.2277888633576,0.));
#154929=CARTESIAN_POINT('Ctrl Pts',(-34.523432433049,62.2277888633576,12.));
#154930=CARTESIAN_POINT('Ctrl Pts',(-34.5191776503842,62.2058848408347,
0.));
#154931=CARTESIAN_POINT('Ctrl Pts',(-34.5191776503842,62.2058848408347,
12.));
#154932=CARTESIAN_POINT('Ctrl Pts',(-34.514909584073,62.1840308021171,0.));
#154933=CARTESIAN_POINT('Ctrl Pts',(-34.514909584073,62.1840308021171,12.));
#154934=CARTESIAN_POINT('Ctrl Pts',(-34.5106283314594,62.1622268744336,
0.));
#154935=CARTESIAN_POINT('Ctrl Pts',(-34.5106283314594,62.1622268744336,
12.));
#154936=CARTESIAN_POINT('Ctrl Pts',(-34.5063339904533,62.1404731855686,
0.));
#154937=CARTESIAN_POINT('Ctrl Pts',(-34.5063339904533,62.1404731855686,
12.));
#154938=CARTESIAN_POINT('Ctrl Pts',(-34.5020266595292,62.1187698638705,
0.));
#154939=CARTESIAN_POINT('Ctrl Pts',(-34.5020266595292,62.1187698638705,
12.));
#154940=CARTESIAN_POINT('Ctrl Pts',(-34.4977064377281,62.0971170382565,
0.));
#154941=CARTESIAN_POINT('Ctrl Pts',(-34.4977064377281,62.0971170382565,
12.));
#154942=CARTESIAN_POINT('Ctrl Pts',(-34.4933734246592,62.0755148382136,
0.));
#154943=CARTESIAN_POINT('Ctrl Pts',(-34.4933734246592,62.0755148382136,
12.));
#154944=CARTESIAN_POINT('Ctrl Pts',(-34.4890277205042,62.0539633937944,
0.));
#154945=CARTESIAN_POINT('Ctrl Pts',(-34.4890277205042,62.0539633937944,
12.));
#154946=CARTESIAN_POINT('Ctrl Pts',(-34.4846694260205,62.0324628356152,
0.));
#154947=CARTESIAN_POINT('Ctrl Pts',(-34.4846694260205,62.0324628356152,
12.));
#154948=CARTESIAN_POINT('Ctrl Pts',(-34.4802986425535,62.0110132948807,
0.));
#154949=CARTESIAN_POINT('Ctrl Pts',(-34.4802986425535,62.0110132948807,
12.));
#154950=CARTESIAN_POINT('Ctrl Pts',(-34.4759154720477,61.9896149034009,
0.));
#154951=CARTESIAN_POINT('Ctrl Pts',(-34.4759154720477,61.9896149034009,
12.));
#154952=CARTESIAN_POINT('Ctrl Pts',(-34.4715200170589,61.9682677936048,
0.));
#154953=CARTESIAN_POINT('Ctrl Pts',(-34.4715200170589,61.9682677936048,
12.));
#154954=CARTESIAN_POINT('Ctrl Pts',(-34.4671123807706,61.9469720985512,
0.));
#154955=CARTESIAN_POINT('Ctrl Pts',(-34.4671123807706,61.9469720985512,
12.));
#154956=CARTESIAN_POINT('Ctrl Pts',(-34.462692666996,61.9257279519283,0.));
#154957=CARTESIAN_POINT('Ctrl Pts',(-34.462692666996,61.9257279519283,12.));
#154958=CARTESIAN_POINT('Ctrl Pts',(-34.4582609801625,61.9045354880424,
0.));
#154959=CARTESIAN_POINT('Ctrl Pts',(-34.4582609801625,61.9045354880424,
12.));
#154960=CARTESIAN_POINT('Ctrl Pts',(-34.4538174253009,61.883394841802,0.));
#154961=CARTESIAN_POINT('Ctrl Pts',(-34.4538174253009,61.883394841802,12.));
#154962=CARTESIAN_POINT('Ctrl Pts',(-34.4493621080367,61.862306148703,0.));
#154963=CARTESIAN_POINT('Ctrl Pts',(-34.4493621080367,61.862306148703,12.));
#154964=CARTESIAN_POINT('Ctrl Pts',(-34.4448951345753,61.8412695447951,
0.));
#154965=CARTESIAN_POINT('Ctrl Pts',(-34.4448951345753,61.8412695447951,
12.));
#154966=CARTESIAN_POINT('Ctrl Pts',(-34.4404166117313,61.8202851667247,
0.));
#154967=CARTESIAN_POINT('Ctrl Pts',(-34.4404166117313,61.8202851667247,
12.));
#154968=CARTESIAN_POINT('Ctrl Pts',(-34.4359266469757,61.7993531518052,
0.));
#154969=CARTESIAN_POINT('Ctrl Pts',(-34.4359266469757,61.7993531518052,
12.));
#154970=CARTESIAN_POINT('Ctrl Pts',(-34.4314253484791,61.7784736380727,
0.));
#154971=CARTESIAN_POINT('Ctrl Pts',(-34.4314253484791,61.7784736380727,
12.));
#154972=CARTESIAN_POINT('Ctrl Pts',(-34.4269128251569,61.7576467643419,
0.));
#154973=CARTESIAN_POINT('Ctrl Pts',(-34.4269128251569,61.7576467643419,
12.));
#154974=CARTESIAN_POINT('Ctrl Pts',(-34.4223891867166,61.7368726702573,
0.));
#154975=CARTESIAN_POINT('Ctrl Pts',(-34.4223891867166,61.7368726702573,
12.));
#154976=CARTESIAN_POINT('Ctrl Pts',(-34.4178545435753,61.7161514961892,
0.));
#154977=CARTESIAN_POINT('Ctrl Pts',(-34.4178545435753,61.7161514961892,
12.));
#154978=CARTESIAN_POINT('Ctrl Pts',(-34.4133090067696,61.6954833831157,
0.));
#154979=CARTESIAN_POINT('Ctrl Pts',(-34.4133090067696,61.6954833831157,
12.));
#154980=CARTESIAN_POINT('Ctrl Pts',(-34.4087526878815,61.674868472521,0.));
#154981=CARTESIAN_POINT('Ctrl Pts',(-34.4087526878815,61.674868472521,12.));
#154982=CARTESIAN_POINT('Ctrl Pts',(-34.4041856989328,61.6543069062436,
0.));
#154983=CARTESIAN_POINT('Ctrl Pts',(-34.4041856989328,61.6543069062436,
12.));
#154984=CARTESIAN_POINT('Ctrl Pts',(-34.399608152377,61.6337988264586,0.));
#154985=CARTESIAN_POINT('Ctrl Pts',(-34.399608152377,61.6337988264586,12.));
#154986=CARTESIAN_POINT('Ctrl Pts',(-34.3950201613446,61.6133443760168,
0.));
#154987=CARTESIAN_POINT('Ctrl Pts',(-34.3950201613446,61.6133443760168,
12.));
#154988=CARTESIAN_POINT('Ctrl Pts',(-34.3904218398642,61.5929436987419,
0.));
#154989=CARTESIAN_POINT('Ctrl Pts',(-34.3904218398642,61.5929436987419,
12.));
#154990=CARTESIAN_POINT('Ctrl Pts',(-34.3858133030511,61.5725969396817,
0.));
#154991=CARTESIAN_POINT('Ctrl Pts',(-34.3858133030511,61.5725969396817,
12.));
#154992=CARTESIAN_POINT('Ctrl Pts',(-34.3811946674179,61.5523042455127,
0.));
#154993=CARTESIAN_POINT('Ctrl Pts',(-34.3811946674179,61.5523042455127,
12.));
#154994=CARTESIAN_POINT('Ctrl Pts',(-34.3765660506659,61.5320657642601,
0.));
#154995=CARTESIAN_POINT('Ctrl Pts',(-34.3765660506659,61.5320657642601,
12.));
#154996=CARTESIAN_POINT('Ctrl Pts',(-34.3719275711179,61.511881644541,0.));
#154997=CARTESIAN_POINT('Ctrl Pts',(-34.3719275711179,61.511881644541,12.));
#154998=CARTESIAN_POINT('Ctrl Pts',(-34.3672793472464,61.4917520349276,
0.));
#154999=CARTESIAN_POINT('Ctrl Pts',(-34.3672793472464,61.4917520349276,
12.));
#155000=CARTESIAN_POINT('Ctrl Pts',(-34.3626214971903,61.4716770832924,
0.));
#155001=CARTESIAN_POINT('Ctrl Pts',(-34.3626214971903,61.4716770832924,
12.));
#155002=CARTESIAN_POINT('Ctrl Pts',(-34.357954138202,61.4516569360499,0.));
#155003=CARTESIAN_POINT('Ctrl Pts',(-34.357954138202,61.4516569360499,12.));
#155004=CARTESIAN_POINT('Ctrl Pts',(-34.3532773877112,61.4316917395959,
0.));
#155005=CARTESIAN_POINT('Ctrl Pts',(-34.3532773877112,61.4316917395959,
12.));
#155006=CARTESIAN_POINT('Ctrl Pts',(-34.3485913645991,61.4117816420251,
0.));
#155007=CARTESIAN_POINT('Ctrl Pts',(-34.3485913645991,61.4117816420251,
12.));
#155008=CARTESIAN_POINT('Ctrl Pts',(-34.34389619024,61.3919267945293,0.));
#155009=CARTESIAN_POINT('Ctrl Pts',(-34.34389619024,61.3919267945293,12.));
#155010=CARTESIAN_POINT('Ctrl Pts',(-34.339191990012,61.3721273534222,0.));
#155011=CARTESIAN_POINT('Ctrl Pts',(-34.339191990012,61.3721273534222,12.));
#155012=CARTESIAN_POINT('Ctrl Pts',(-34.3344788934337,61.3523834803144,
0.));
#155013=CARTESIAN_POINT('Ctrl Pts',(-34.3344788934337,61.3523834803144,
12.));
#155014=CARTESIAN_POINT('Ctrl Pts',(-34.3297570310126,61.3326953378817,
0.));
#155015=CARTESIAN_POINT('Ctrl Pts',(-34.3297570310126,61.3326953378817,
12.));
#155016=CARTESIAN_POINT('Ctrl Pts',(-34.3250265314761,61.3130630861375,
0.));
#155017=CARTESIAN_POINT('Ctrl Pts',(-34.3250265314761,61.3130630861375,
12.));
#155018=CARTESIAN_POINT('Ctrl Pts',(-34.3202875193629,61.2934868791875,
0.));
#155019=CARTESIAN_POINT('Ctrl Pts',(-34.3202875193629,61.2934868791875,
12.));
#155020=CARTESIAN_POINT('Ctrl Pts',(-34.3155401111776,61.2739668600415,
0.));
#155021=CARTESIAN_POINT('Ctrl Pts',(-34.3155401111776,61.2739668600415,
12.));
#155022=CARTESIAN_POINT('Ctrl Pts',(-34.3107844191081,61.2545031656196,
0.));
#155023=CARTESIAN_POINT('Ctrl Pts',(-34.3107844191081,61.2545031656196,
12.));
#155024=CARTESIAN_POINT('Ctrl Pts',(-34.3060205584093,61.2350959366987,
0.));
#155025=CARTESIAN_POINT('Ctrl Pts',(-34.3060205584093,61.2350959366987,
12.));
#155026=CARTESIAN_POINT('Ctrl Pts',(-34.3012486533474,61.2157453259107,
0.));
#155027=CARTESIAN_POINT('Ctrl Pts',(-34.3012486533474,61.2157453259107,
12.));
#155028=CARTESIAN_POINT('Ctrl Pts',(-34.296468844362,61.1964515073823,0.));
#155029=CARTESIAN_POINT('Ctrl Pts',(-34.296468844362,61.1964515073823,12.));
#155030=CARTESIAN_POINT('Ctrl Pts',(-34.2916812929675,61.1772146833083,
0.));
#155031=CARTESIAN_POINT('Ctrl Pts',(-34.2916812929675,61.1772146833083,
12.));
#155032=CARTESIAN_POINT('Ctrl Pts',(-34.2868861666301,61.15803506354,0.));
#155033=CARTESIAN_POINT('Ctrl Pts',(-34.2868861666301,61.15803506354,12.));
#155034=CARTESIAN_POINT('Ctrl Pts',(-34.2820836244425,61.1389128461815,
0.));
#155035=CARTESIAN_POINT('Ctrl Pts',(-34.2820836244425,61.1389128461815,
12.));
#155036=CARTESIAN_POINT('Ctrl Pts',(-34.2772738038812,61.119848199783,0.));
#155037=CARTESIAN_POINT('Ctrl Pts',(-34.2772738038812,61.119848199783,12.));
#155038=CARTESIAN_POINT('Ctrl Pts',(-34.2724568037374,61.100841240023,0.));
#155039=CARTESIAN_POINT('Ctrl Pts',(-34.2724568037374,61.100841240023,12.));
#155040=CARTESIAN_POINT('Ctrl Pts',(-34.2676326825846,61.0818920286644,
0.));
#155041=CARTESIAN_POINT('Ctrl Pts',(-34.2676326825846,61.0818920286644,
12.));
#155042=CARTESIAN_POINT('Ctrl Pts',(-34.2637677132139,61.0667788793594,
0.));
#155043=CARTESIAN_POINT('Ctrl Pts',(-34.2637677132139,61.0667788793594,
12.));
#155044=CARTESIAN_POINT('Ctrl Pts',(-34.2608658001761,61.0554700177206,
0.));
#155045=CARTESIAN_POINT('Ctrl Pts',(-34.2608658001761,61.0554700177206,
12.));
#155046=CARTESIAN_POINT('Ctrl Pts',(-34.2589297755482,61.0479423318803,
0.));
#155047=CARTESIAN_POINT('Ctrl Pts',(-34.2589297755482,61.0479423318803,
12.));
#155048=CARTESIAN_POINT('Ctrl Pts',(-34.2579614092497,61.0441813777723,
0.));
#155049=CARTESIAN_POINT('Ctrl Pts',(-34.2579614092497,61.0441813777723,
12.));
#155050=CARTESIAN_POINT('',(-34.2579614092497,61.0441813777723,12.));
#155051=CARTESIAN_POINT('Ctrl Pts',(-34.2579614092497,61.0441813777723,
12.));
#155052=CARTESIAN_POINT('Ctrl Pts',(-34.2589297755482,61.0479423318803,
12.));
#155053=CARTESIAN_POINT('Ctrl Pts',(-34.2608658001761,61.0554700177206,
12.));
#155054=CARTESIAN_POINT('Ctrl Pts',(-34.2637677132139,61.0667788793594,
12.));
#155055=CARTESIAN_POINT('Ctrl Pts',(-34.2676326825846,61.0818920286644,
12.));
#155056=CARTESIAN_POINT('Ctrl Pts',(-34.2724568037374,61.100841240023,12.));
#155057=CARTESIAN_POINT('Ctrl Pts',(-34.2772738038812,61.119848199783,12.));
#155058=CARTESIAN_POINT('Ctrl Pts',(-34.2820836244425,61.1389128461815,
12.));
#155059=CARTESIAN_POINT('Ctrl Pts',(-34.2868861666301,61.15803506354,12.));
#155060=CARTESIAN_POINT('Ctrl Pts',(-34.2916812929675,61.1772146833083,
12.));
#155061=CARTESIAN_POINT('Ctrl Pts',(-34.296468844362,61.1964515073823,12.));
#155062=CARTESIAN_POINT('Ctrl Pts',(-34.3012486533474,61.2157453259107,
12.));
#155063=CARTESIAN_POINT('Ctrl Pts',(-34.3060205584093,61.2350959366987,
12.));
#155064=CARTESIAN_POINT('Ctrl Pts',(-34.3107844191081,61.2545031656196,
12.));
#155065=CARTESIAN_POINT('Ctrl Pts',(-34.3155401111776,61.2739668600415,
12.));
#155066=CARTESIAN_POINT('Ctrl Pts',(-34.3202875193629,61.2934868791875,
12.));
#155067=CARTESIAN_POINT('Ctrl Pts',(-34.3250265314761,61.3130630861375,
12.));
#155068=CARTESIAN_POINT('Ctrl Pts',(-34.3297570310126,61.3326953378817,
12.));
#155069=CARTESIAN_POINT('Ctrl Pts',(-34.3344788934337,61.3523834803144,
12.));
#155070=CARTESIAN_POINT('Ctrl Pts',(-34.339191990012,61.3721273534222,12.));
#155071=CARTESIAN_POINT('Ctrl Pts',(-34.34389619024,61.3919267945293,12.));
#155072=CARTESIAN_POINT('Ctrl Pts',(-34.3485913645991,61.4117816420251,
12.));
#155073=CARTESIAN_POINT('Ctrl Pts',(-34.3532773877112,61.4316917395959,
12.));
#155074=CARTESIAN_POINT('Ctrl Pts',(-34.357954138202,61.4516569360499,12.));
#155075=CARTESIAN_POINT('Ctrl Pts',(-34.3626214971903,61.4716770832924,
12.));
#155076=CARTESIAN_POINT('Ctrl Pts',(-34.3672793472464,61.4917520349276,
12.));
#155077=CARTESIAN_POINT('Ctrl Pts',(-34.3719275711179,61.511881644541,12.));
#155078=CARTESIAN_POINT('Ctrl Pts',(-34.3765660506659,61.5320657642601,
12.));
#155079=CARTESIAN_POINT('Ctrl Pts',(-34.3811946674179,61.5523042455127,
12.));
#155080=CARTESIAN_POINT('Ctrl Pts',(-34.3858133030511,61.5725969396817,
12.));
#155081=CARTESIAN_POINT('Ctrl Pts',(-34.3904218398642,61.5929436987419,
12.));
#155082=CARTESIAN_POINT('Ctrl Pts',(-34.3950201613446,61.6133443760168,
12.));
#155083=CARTESIAN_POINT('Ctrl Pts',(-34.399608152377,61.6337988264586,12.));
#155084=CARTESIAN_POINT('Ctrl Pts',(-34.4041856989328,61.6543069062436,
12.));
#155085=CARTESIAN_POINT('Ctrl Pts',(-34.4087526878815,61.674868472521,12.));
#155086=CARTESIAN_POINT('Ctrl Pts',(-34.4133090067696,61.6954833831157,
12.));
#155087=CARTESIAN_POINT('Ctrl Pts',(-34.4178545435753,61.7161514961892,
12.));
#155088=CARTESIAN_POINT('Ctrl Pts',(-34.4223891867166,61.7368726702573,
12.));
#155089=CARTESIAN_POINT('Ctrl Pts',(-34.4269128251569,61.7576467643419,
12.));
#155090=CARTESIAN_POINT('Ctrl Pts',(-34.4314253484791,61.7784736380727,
12.));
#155091=CARTESIAN_POINT('Ctrl Pts',(-34.4359266469757,61.7993531518052,
12.));
#155092=CARTESIAN_POINT('Ctrl Pts',(-34.4404166117313,61.8202851667247,
12.));
#155093=CARTESIAN_POINT('Ctrl Pts',(-34.4448951345753,61.8412695447951,
12.));
#155094=CARTESIAN_POINT('Ctrl Pts',(-34.4493621080367,61.862306148703,12.));
#155095=CARTESIAN_POINT('Ctrl Pts',(-34.4538174253009,61.883394841802,12.));
#155096=CARTESIAN_POINT('Ctrl Pts',(-34.4582609801625,61.9045354880424,
12.));
#155097=CARTESIAN_POINT('Ctrl Pts',(-34.462692666996,61.9257279519283,12.));
#155098=CARTESIAN_POINT('Ctrl Pts',(-34.4671123807706,61.9469720985512,
12.));
#155099=CARTESIAN_POINT('Ctrl Pts',(-34.4715200170589,61.9682677936048,
12.));
#155100=CARTESIAN_POINT('Ctrl Pts',(-34.4759154720477,61.9896149034009,
12.));
#155101=CARTESIAN_POINT('Ctrl Pts',(-34.4802986425535,62.0110132948807,
12.));
#155102=CARTESIAN_POINT('Ctrl Pts',(-34.4846694260205,62.0324628356152,
12.));
#155103=CARTESIAN_POINT('Ctrl Pts',(-34.4890277205042,62.0539633937944,
12.));
#155104=CARTESIAN_POINT('Ctrl Pts',(-34.4933734246592,62.0755148382136,
12.));
#155105=CARTESIAN_POINT('Ctrl Pts',(-34.4977064377281,62.0971170382565,
12.));
#155106=CARTESIAN_POINT('Ctrl Pts',(-34.5020266595292,62.1187698638705,
12.));
#155107=CARTESIAN_POINT('Ctrl Pts',(-34.5063339904533,62.1404731855686,
12.));
#155108=CARTESIAN_POINT('Ctrl Pts',(-34.5106283314594,62.1622268744336,
12.));
#155109=CARTESIAN_POINT('Ctrl Pts',(-34.514909584073,62.1840308021171,12.));
#155110=CARTESIAN_POINT('Ctrl Pts',(-34.5191776503842,62.2058848408347,
12.));
#155111=CARTESIAN_POINT('Ctrl Pts',(-34.523432433049,62.2277888633576,12.));
#155112=CARTESIAN_POINT('Ctrl Pts',(-34.5276738352808,62.2497427430135,
12.));
#155113=CARTESIAN_POINT('Ctrl Pts',(-34.5319017608433,62.2717463536827,
12.));
#155114=CARTESIAN_POINT('Ctrl Pts',(-34.5361161140449,62.2937995697925,
12.));
#155115=CARTESIAN_POINT('Ctrl Pts',(-34.5403167997337,62.3159022663058,
12.));
#155116=CARTESIAN_POINT('Ctrl Pts',(-34.5445037232936,62.338054318708,12.));
#155117=CARTESIAN_POINT('Ctrl Pts',(-34.5486767906384,62.3602556030127,
12.));
#155118=CARTESIAN_POINT('Ctrl Pts',(-34.5528359082075,62.3825059957601,
12.));
#155119=CARTESIAN_POINT('Ctrl Pts',(-34.5569809829613,62.4048053740127,
12.));
#155120=CARTESIAN_POINT('Ctrl Pts',(-34.5611119223798,62.4271536153459,
12.));
#155121=CARTESIAN_POINT('Ctrl Pts',(-34.5652286344593,62.4495505978393,
12.));
#155122=CARTESIAN_POINT('Ctrl Pts',(-34.5693310277051,62.4719962000808,
12.));
#155123=CARTESIAN_POINT('Ctrl Pts',(-34.5734190111272,62.4944903011628,
12.));
#155124=CARTESIAN_POINT('Ctrl Pts',(-34.5774924942355,62.5170327806781,
12.));
#155125=CARTESIAN_POINT('Ctrl Pts',(-34.5815513870377,62.5396235187079,
12.));
#155126=CARTESIAN_POINT('Ctrl Pts',(-34.5855956000363,62.562262395816,12.));
#155127=CARTESIAN_POINT('Ctrl Pts',(-34.5896250442216,62.5849492930533,
12.));
#155128=CARTESIAN_POINT('Ctrl Pts',(-34.5936396310679,62.6076840919536,
12.));
#155129=CARTESIAN_POINT('Ctrl Pts',(-34.5976392725296,62.6304666745306,
12.));
#155130=CARTESIAN_POINT('Ctrl Pts',(-34.6016238810399,62.6532969232657,
12.));
#155131=CARTESIAN_POINT('Ctrl Pts',(-34.6055933695069,62.6761747211037,
12.));
#155132=CARTESIAN_POINT('Ctrl Pts',(-34.6095476513077,62.6990999514563,
12.));
#155133=CARTESIAN_POINT('Ctrl Pts',(-34.6134866402837,62.7220724981994,
12.));
#155134=CARTESIAN_POINT('Ctrl Pts',(-34.6174102507375,62.7450922456676,
12.));
#155135=CARTESIAN_POINT('Ctrl Pts',(-34.6213183974317,62.7681590786429,
12.));
#155136=CARTESIAN_POINT('Ctrl Pts',(-34.6252109955853,62.7912728823518,
12.));
#155137=CARTESIAN_POINT('Ctrl Pts',(-34.6290879608673,62.8144335424697,
12.));
#155138=CARTESIAN_POINT('Ctrl Pts',(-34.6329492093935,62.8376409451175,
12.));
#155139=CARTESIAN_POINT('Ctrl Pts',(-34.6367946577235,62.8608949768571,
12.));
#155140=CARTESIAN_POINT('Ctrl Pts',(-34.6406242228592,62.8841955246794,
12.));
#155141=CARTESIAN_POINT('Ctrl Pts',(-34.6444378222411,62.9075424760015,
12.));
#155142=CARTESIAN_POINT('Ctrl Pts',(-34.6482353737424,62.9309357186717,
12.));
#155143=CARTESIAN_POINT('Ctrl Pts',(-34.6520167956655,62.9543751409645,
12.));
#155144=CARTESIAN_POINT('Ctrl Pts',(-34.6557820067393,62.9778606315783,
12.));
#155145=CARTESIAN_POINT('Ctrl Pts',(-34.6595309261191,63.0013920796235,
12.));
#155146=CARTESIAN_POINT('Ctrl Pts',(-34.6632634733824,63.0249693746208,
12.));
#155147=CARTESIAN_POINT('Ctrl Pts',(-34.6669795685228,63.0485924065045,
12.));
#155148=CARTESIAN_POINT('Ctrl Pts',(-34.670679131947,63.0722610656194,12.));
#155149=CARTESIAN_POINT('Ctrl Pts',(-34.674362084472,63.0959752427168,12.));
#155150=CARTESIAN_POINT('Ctrl Pts',(-34.6780283473252,63.119734828943,12.));
#155151=CARTESIAN_POINT('Ctrl Pts',(-34.6816778421402,63.1435397158388,
12.));
#155152=CARTESIAN_POINT('Ctrl Pts',(-34.6853104909518,63.1673897953429,
12.));
#155153=CARTESIAN_POINT('Ctrl Pts',(-34.6889262161924,63.1912849597887,
12.));
#155154=CARTESIAN_POINT('Ctrl Pts',(-34.6925249406897,63.2152251019012,
12.));
#155155=CARTESIAN_POINT('Ctrl Pts',(-34.6961065876666,63.2392101147847,
12.));
#155156=CARTESIAN_POINT('Ctrl Pts',(-34.6996710807378,63.2632398919225,
12.));
#155157=CARTESIAN_POINT('Ctrl Pts',(-34.703218343904,63.2873143271807,12.));
#155158=CARTESIAN_POINT('Ctrl Pts',(-34.7067483015491,63.3114333148048,
12.));
#155159=CARTESIAN_POINT('Ctrl Pts',(-34.7102608784374,63.3355967494171,
12.));
#155160=CARTESIAN_POINT('Ctrl Pts',(-34.7137559997146,63.3598045260053,
12.));
#155161=CARTESIAN_POINT('Ctrl Pts',(-34.7172335909038,63.3840565399208,
12.));
#155162=CARTESIAN_POINT('Ctrl Pts',(-34.7206935779007,63.4083526868836,
12.));
#155163=CARTESIAN_POINT('Ctrl Pts',(-34.7241358869701,63.4326928629795,
12.));
#155164=CARTESIAN_POINT('Ctrl Pts',(-34.7275604447439,63.4570769646569,
12.));
#155165=CARTESIAN_POINT('Ctrl Pts',(-34.7309671782214,63.4815048887165,
12.));
#155166=CARTESIAN_POINT('Ctrl Pts',(-34.7343560147667,63.505976532309,12.));
#155167=CARTESIAN_POINT('Ctrl Pts',(-34.7377268821025,63.5304917929386,
12.));
#155168=CARTESIAN_POINT('Ctrl Pts',(-34.7410797083081,63.5550505684626,
12.));
#155169=CARTESIAN_POINT('Ctrl Pts',(-34.744414421816,63.5796527570871,12.));
#155170=CARTESIAN_POINT('Ctrl Pts',(-34.7477309514136,63.6042982573588,
12.));
#155171=CARTESIAN_POINT('Ctrl Pts',(-34.7510292262406,63.6289869681604,
12.));
#155172=CARTESIAN_POINT('Ctrl Pts',(-34.7543091757833,63.6537187887159,
12.));
#155173=CARTESIAN_POINT('Ctrl Pts',(-34.7575707298713,63.6784936185885,
12.));
#155174=CARTESIAN_POINT('Ctrl Pts',(-34.7608138186759,63.7033113576785,
12.));
#155175=CARTESIAN_POINT('Ctrl Pts',(-34.7640383727101,63.7281719062149,
12.));
#155176=CARTESIAN_POINT('Ctrl Pts',(-34.7672443228275,63.7530751647494,
12.));
#155177=CARTESIAN_POINT('Ctrl Pts',(-34.7704316002171,63.778021034163,12.));
#155178=CARTESIAN_POINT('Ctrl Pts',(-34.7736001363993,63.8030094156639,
12.));
#155179=CARTESIAN_POINT('Ctrl Pts',(-34.7767498632243,63.8280402107856,
12.));
#155180=CARTESIAN_POINT('Ctrl Pts',(-34.7798807128715,63.8531133213793,
12.));
#155181=CARTESIAN_POINT('Ctrl Pts',(-34.7829926178496,63.8782286496062,
12.));
#155182=CARTESIAN_POINT('Ctrl Pts',(-34.7860855109911,63.9033860979435,
12.));
#155183=CARTESIAN_POINT('Ctrl Pts',(-34.7891593254488,63.9285855691845,
12.));
#155184=CARTESIAN_POINT('Ctrl Pts',(-34.7922139946943,63.9538269664366,
12.));
#155185=CARTESIAN_POINT('Ctrl Pts',(-34.7952494525177,63.9791101931162,
12.));
#155186=CARTESIAN_POINT('Ctrl Pts',(-34.7982656330293,64.0044351529402,
12.));
#155187=CARTESIAN_POINT('Ctrl Pts',(-34.8012624706526,64.0298017499294,
12.));
#155188=CARTESIAN_POINT('Ctrl Pts',(-34.8042399001211,64.0552098884095,
12.));
#155189=CARTESIAN_POINT('Ctrl Pts',(-34.8071978564747,64.0806594730085,
12.));
#155190=CARTESIAN_POINT('Ctrl Pts',(-34.8101362750597,64.1061504086515,
12.));
#155191=CARTESIAN_POINT('Ctrl Pts',(-34.8130550915287,64.1316826005506,
12.));
#155192=CARTESIAN_POINT('Ctrl Pts',(-34.8159542418374,64.1572559542086,
12.));
#155193=CARTESIAN_POINT('Ctrl Pts',(-34.8188336622419,64.1828703754236,
12.));
#155194=CARTESIAN_POINT('Ctrl Pts',(-34.8216932892968,64.2085257702884,
12.));
#155195=CARTESIAN_POINT('Ctrl Pts',(-34.8245330598559,64.234222045188,12.));
#155196=CARTESIAN_POINT('Ctrl Pts',(-34.8273529110744,64.2599591067916,
12.));
#155197=CARTESIAN_POINT('Ctrl Pts',(-34.8301527804054,64.285736862052,12.));
#155198=CARTESIAN_POINT('Ctrl Pts',(-34.8329326055919,64.3115552182062,
12.));
#155199=CARTESIAN_POINT('Ctrl Pts',(-34.8356923246618,64.3374140827711,
12.));
#155200=CARTESIAN_POINT('Ctrl Pts',(-34.8384318759248,64.3633133635382,
12.));
#155201=CARTESIAN_POINT('Ctrl Pts',(-34.8411511979702,64.3892529685607,
12.));
#155202=CARTESIAN_POINT('Ctrl Pts',(-34.8438502296664,64.4152328061515,
12.));
#155203=CARTESIAN_POINT('Ctrl Pts',(-34.8465289101621,64.4412527848969,
12.));
#155204=CARTESIAN_POINT('Ctrl Pts',(-34.8491871788895,64.4673128136625,
12.));
#155205=CARTESIAN_POINT('Ctrl Pts',(-34.851824975568,64.4934128015985,12.));
#155206=CARTESIAN_POINT('Ctrl Pts',(-34.8544422402118,64.5195526581407,
12.));
#155207=CARTESIAN_POINT('Ctrl Pts',(-34.857038913134,64.5457322930088,12.));
#155208=CARTESIAN_POINT('Ctrl Pts',(-34.8596149349257,64.5719516161927,
12.));
#155209=CARTESIAN_POINT('Ctrl Pts',(-34.8621702464401,64.5982105379383,
12.));
#155210=CARTESIAN_POINT('Ctrl Pts',(-34.8647047887774,64.6245089687277,
12.));
#155211=CARTESIAN_POINT('Ctrl Pts',(-34.867218503272,64.6508468192599,12.));
#155212=CARTESIAN_POINT('Ctrl Pts',(-34.869711331479,64.6772240004228,12.));
#155213=CARTESIAN_POINT('Ctrl Pts',(-34.8721832151974,64.7036404233306,
12.));
#155214=CARTESIAN_POINT('Ctrl Pts',(-34.8746340964971,64.7300959993653,
12.));
#155215=CARTESIAN_POINT('Ctrl Pts',(-34.8770639177493,64.7565906402151,
12.));
#155216=CARTESIAN_POINT('Ctrl Pts',(-34.8794726216513,64.7831242579028,
12.));
#155217=CARTESIAN_POINT('Ctrl Pts',(-34.881860151273,64.8096967648307,12.));
#155218=CARTESIAN_POINT('Ctrl Pts',(-34.8842264500188,64.8363080737377,
12.));
#155219=CARTESIAN_POINT('Ctrl Pts',(-34.8865714615436,64.8629580976063,
12.));
#155220=CARTESIAN_POINT('Ctrl Pts',(-34.888895129681,64.8896467495757,12.));
#155221=CARTESIAN_POINT('Ctrl Pts',(-34.8911973983785,64.9163739428605,
12.));
#155222=CARTESIAN_POINT('Ctrl Pts',(-34.8934782116095,64.9431395906337,
12.));
#155223=CARTESIAN_POINT('Ctrl Pts',(-34.8957375133697,64.9699436060169,
12.));
#155224=CARTESIAN_POINT('Ctrl Pts',(-34.8979752478616,64.9967859023212,
12.));
#155225=CARTESIAN_POINT('Ctrl Pts',(-34.9001913596416,65.0236663932328,
12.));
#155226=CARTESIAN_POINT('Ctrl Pts',(-34.9023857937865,65.0505849930171,
12.));
#155227=CARTESIAN_POINT('Ctrl Pts',(-34.9045584960509,65.0775416167085,
12.));
#155228=CARTESIAN_POINT('Ctrl Pts',(-34.9067094130399,65.1045361803121,
12.));
#155229=CARTESIAN_POINT('Ctrl Pts',(-34.9088384918336,65.1315686003516,
12.));
#155230=CARTESIAN_POINT('Ctrl Pts',(-34.9109456796213,65.1586387934241,
12.));
#155231=CARTESIAN_POINT('Ctrl Pts',(-34.9130309233022,65.1857466757092,
12.));
#155232=CARTESIAN_POINT('Ctrl Pts',(-34.9150941691747,65.2128921625823,
12.));
#155233=CARTESIAN_POINT('Ctrl Pts',(-34.9171353624113,65.2400751679549,
12.));
#155234=CARTESIAN_POINT('Ctrl Pts',(-34.9191544474872,65.2672956048069,
12.));
#155235=CARTESIAN_POINT('Ctrl Pts',(-34.9211513691355,65.2945533863761,
12.));
#155236=CARTESIAN_POINT('Ctrl Pts',(-34.9231260731831,65.321848427191,12.));
#155237=CARTESIAN_POINT('Ctrl Pts',(-34.9250785073477,65.3491806440537,
12.));
#155238=CARTESIAN_POINT('Ctrl Pts',(-34.9270086222731,65.3765499573077,
12.));
#155239=CARTESIAN_POINT('Ctrl Pts',(-34.9289163717747,65.4039562911352,
12.));
#155240=CARTESIAN_POINT('Ctrl Pts',(-34.9305324724445,65.4274804996589,
12.));
#155241=CARTESIAN_POINT('Ctrl Pts',(-34.931759381316,65.4455359575244,12.));
#155242=CARTESIAN_POINT('Ctrl Pts',(-34.9326070346645,65.4581063193883,
12.));
#155243=CARTESIAN_POINT('Ctrl Pts',(-34.9330820191535,65.465180801081,12.));
#155244=CARTESIAN_POINT('Ctrl Pts',(-34.933187552314,65.4667541478384,12.));
#155245=CARTESIAN_POINT('',(-34.2579614092497,61.0441813777723,0.));
#155246=CARTESIAN_POINT('',(-34.2579614092497,61.0441813777723,0.));
#155247=CARTESIAN_POINT('Ctrl Pts',(-34.933187552314,65.4667541478384,0.));
#155248=CARTESIAN_POINT('Ctrl Pts',(-34.9330820191535,65.465180801081,0.));
#155249=CARTESIAN_POINT('Ctrl Pts',(-34.9326070346645,65.4581063193883,
0.));
#155250=CARTESIAN_POINT('Ctrl Pts',(-34.931759381316,65.4455359575244,0.));
#155251=CARTESIAN_POINT('Ctrl Pts',(-34.9305324724445,65.4274804996589,
0.));
#155252=CARTESIAN_POINT('Ctrl Pts',(-34.9289163717747,65.4039562911352,
0.));
#155253=CARTESIAN_POINT('Ctrl Pts',(-34.9270086222731,65.3765499573077,
0.));
#155254=CARTESIAN_POINT('Ctrl Pts',(-34.9250785073477,65.3491806440537,
0.));
#155255=CARTESIAN_POINT('Ctrl Pts',(-34.9231260731831,65.321848427191,0.));
#155256=CARTESIAN_POINT('Ctrl Pts',(-34.9211513691355,65.2945533863761,
0.));
#155257=CARTESIAN_POINT('Ctrl Pts',(-34.9191544474872,65.2672956048069,
0.));
#155258=CARTESIAN_POINT('Ctrl Pts',(-34.9171353624113,65.2400751679549,
0.));
#155259=CARTESIAN_POINT('Ctrl Pts',(-34.9150941691747,65.2128921625823,
0.));
#155260=CARTESIAN_POINT('Ctrl Pts',(-34.9130309233022,65.1857466757092,
0.));
#155261=CARTESIAN_POINT('Ctrl Pts',(-34.9109456796213,65.1586387934241,
0.));
#155262=CARTESIAN_POINT('Ctrl Pts',(-34.9088384918336,65.1315686003516,
0.));
#155263=CARTESIAN_POINT('Ctrl Pts',(-34.9067094130399,65.1045361803121,
0.));
#155264=CARTESIAN_POINT('Ctrl Pts',(-34.9045584960509,65.0775416167085,
0.));
#155265=CARTESIAN_POINT('Ctrl Pts',(-34.9023857937865,65.0505849930171,
0.));
#155266=CARTESIAN_POINT('Ctrl Pts',(-34.9001913596416,65.0236663932328,
0.));
#155267=CARTESIAN_POINT('Ctrl Pts',(-34.8979752478616,64.9967859023212,
0.));
#155268=CARTESIAN_POINT('Ctrl Pts',(-34.8957375133697,64.9699436060169,
0.));
#155269=CARTESIAN_POINT('Ctrl Pts',(-34.8934782116095,64.9431395906337,
0.));
#155270=CARTESIAN_POINT('Ctrl Pts',(-34.8911973983785,64.9163739428605,
0.));
#155271=CARTESIAN_POINT('Ctrl Pts',(-34.888895129681,64.8896467495757,0.));
#155272=CARTESIAN_POINT('Ctrl Pts',(-34.8865714615436,64.8629580976063,
0.));
#155273=CARTESIAN_POINT('Ctrl Pts',(-34.8842264500188,64.8363080737377,
0.));
#155274=CARTESIAN_POINT('Ctrl Pts',(-34.881860151273,64.8096967648307,0.));
#155275=CARTESIAN_POINT('Ctrl Pts',(-34.8794726216513,64.7831242579028,
0.));
#155276=CARTESIAN_POINT('Ctrl Pts',(-34.8770639177493,64.7565906402151,
0.));
#155277=CARTESIAN_POINT('Ctrl Pts',(-34.8746340964971,64.7300959993653,
0.));
#155278=CARTESIAN_POINT('Ctrl Pts',(-34.8721832151974,64.7036404233306,
0.));
#155279=CARTESIAN_POINT('Ctrl Pts',(-34.869711331479,64.6772240004228,0.));
#155280=CARTESIAN_POINT('Ctrl Pts',(-34.867218503272,64.6508468192599,0.));
#155281=CARTESIAN_POINT('Ctrl Pts',(-34.8647047887774,64.6245089687277,
0.));
#155282=CARTESIAN_POINT('Ctrl Pts',(-34.8621702464401,64.5982105379383,
0.));
#155283=CARTESIAN_POINT('Ctrl Pts',(-34.8596149349257,64.5719516161927,
0.));
#155284=CARTESIAN_POINT('Ctrl Pts',(-34.857038913134,64.5457322930088,0.));
#155285=CARTESIAN_POINT('Ctrl Pts',(-34.8544422402118,64.5195526581407,
0.));
#155286=CARTESIAN_POINT('Ctrl Pts',(-34.851824975568,64.4934128015985,0.));
#155287=CARTESIAN_POINT('Ctrl Pts',(-34.8491871788895,64.4673128136625,
0.));
#155288=CARTESIAN_POINT('Ctrl Pts',(-34.8465289101621,64.4412527848969,
0.));
#155289=CARTESIAN_POINT('Ctrl Pts',(-34.8438502296664,64.4152328061515,
0.));
#155290=CARTESIAN_POINT('Ctrl Pts',(-34.8411511979702,64.3892529685607,
0.));
#155291=CARTESIAN_POINT('Ctrl Pts',(-34.8384318759248,64.3633133635382,
0.));
#155292=CARTESIAN_POINT('Ctrl Pts',(-34.8356923246618,64.3374140827711,
0.));
#155293=CARTESIAN_POINT('Ctrl Pts',(-34.8329326055919,64.3115552182062,
0.));
#155294=CARTESIAN_POINT('Ctrl Pts',(-34.8301527804054,64.285736862052,0.));
#155295=CARTESIAN_POINT('Ctrl Pts',(-34.8273529110744,64.2599591067916,
0.));
#155296=CARTESIAN_POINT('Ctrl Pts',(-34.8245330598559,64.234222045188,0.));
#155297=CARTESIAN_POINT('Ctrl Pts',(-34.8216932892968,64.2085257702884,
0.));
#155298=CARTESIAN_POINT('Ctrl Pts',(-34.8188336622419,64.1828703754236,
0.));
#155299=CARTESIAN_POINT('Ctrl Pts',(-34.8159542418374,64.1572559542086,
0.));
#155300=CARTESIAN_POINT('Ctrl Pts',(-34.8130550915287,64.1316826005506,
0.));
#155301=CARTESIAN_POINT('Ctrl Pts',(-34.8101362750597,64.1061504086515,
0.));
#155302=CARTESIAN_POINT('Ctrl Pts',(-34.8071978564747,64.0806594730085,
0.));
#155303=CARTESIAN_POINT('Ctrl Pts',(-34.8042399001211,64.0552098884095,
0.));
#155304=CARTESIAN_POINT('Ctrl Pts',(-34.8012624706526,64.0298017499294,
0.));
#155305=CARTESIAN_POINT('Ctrl Pts',(-34.7982656330293,64.0044351529402,
0.));
#155306=CARTESIAN_POINT('Ctrl Pts',(-34.7952494525177,63.9791101931162,
0.));
#155307=CARTESIAN_POINT('Ctrl Pts',(-34.7922139946943,63.9538269664366,
0.));
#155308=CARTESIAN_POINT('Ctrl Pts',(-34.7891593254488,63.9285855691845,
0.));
#155309=CARTESIAN_POINT('Ctrl Pts',(-34.7860855109911,63.9033860979435,
0.));
#155310=CARTESIAN_POINT('Ctrl Pts',(-34.7829926178496,63.8782286496062,
0.));
#155311=CARTESIAN_POINT('Ctrl Pts',(-34.7798807128715,63.8531133213793,
0.));
#155312=CARTESIAN_POINT('Ctrl Pts',(-34.7767498632243,63.8280402107856,
0.));
#155313=CARTESIAN_POINT('Ctrl Pts',(-34.7736001363993,63.8030094156639,
0.));
#155314=CARTESIAN_POINT('Ctrl Pts',(-34.7704316002171,63.778021034163,0.));
#155315=CARTESIAN_POINT('Ctrl Pts',(-34.7672443228275,63.7530751647494,
0.));
#155316=CARTESIAN_POINT('Ctrl Pts',(-34.7640383727101,63.7281719062149,
0.));
#155317=CARTESIAN_POINT('Ctrl Pts',(-34.7608138186759,63.7033113576785,
0.));
#155318=CARTESIAN_POINT('Ctrl Pts',(-34.7575707298713,63.6784936185885,
0.));
#155319=CARTESIAN_POINT('Ctrl Pts',(-34.7543091757833,63.6537187887159,
0.));
#155320=CARTESIAN_POINT('Ctrl Pts',(-34.7510292262406,63.6289869681604,
0.));
#155321=CARTESIAN_POINT('Ctrl Pts',(-34.7477309514136,63.6042982573588,
0.));
#155322=CARTESIAN_POINT('Ctrl Pts',(-34.744414421816,63.5796527570871,0.));
#155323=CARTESIAN_POINT('Ctrl Pts',(-34.7410797083081,63.5550505684626,
0.));
#155324=CARTESIAN_POINT('Ctrl Pts',(-34.7377268821025,63.5304917929386,
0.));
#155325=CARTESIAN_POINT('Ctrl Pts',(-34.7343560147667,63.505976532309,0.));
#155326=CARTESIAN_POINT('Ctrl Pts',(-34.7309671782214,63.4815048887165,
0.));
#155327=CARTESIAN_POINT('Ctrl Pts',(-34.7275604447439,63.4570769646569,
0.));
#155328=CARTESIAN_POINT('Ctrl Pts',(-34.7241358869701,63.4326928629795,
0.));
#155329=CARTESIAN_POINT('Ctrl Pts',(-34.7206935779007,63.4083526868836,
0.));
#155330=CARTESIAN_POINT('Ctrl Pts',(-34.7172335909038,63.3840565399208,
0.));
#155331=CARTESIAN_POINT('Ctrl Pts',(-34.7137559997146,63.3598045260053,
0.));
#155332=CARTESIAN_POINT('Ctrl Pts',(-34.7102608784374,63.3355967494171,
0.));
#155333=CARTESIAN_POINT('Ctrl Pts',(-34.7067483015491,63.3114333148048,
0.));
#155334=CARTESIAN_POINT('Ctrl Pts',(-34.703218343904,63.2873143271807,0.));
#155335=CARTESIAN_POINT('Ctrl Pts',(-34.6996710807378,63.2632398919225,
0.));
#155336=CARTESIAN_POINT('Ctrl Pts',(-34.6961065876666,63.2392101147847,
0.));
#155337=CARTESIAN_POINT('Ctrl Pts',(-34.6925249406897,63.2152251019012,
0.));
#155338=CARTESIAN_POINT('Ctrl Pts',(-34.6889262161924,63.1912849597887,
0.));
#155339=CARTESIAN_POINT('Ctrl Pts',(-34.6853104909518,63.1673897953429,
0.));
#155340=CARTESIAN_POINT('Ctrl Pts',(-34.6816778421402,63.1435397158388,
0.));
#155341=CARTESIAN_POINT('Ctrl Pts',(-34.6780283473252,63.119734828943,0.));
#155342=CARTESIAN_POINT('Ctrl Pts',(-34.674362084472,63.0959752427168,0.));
#155343=CARTESIAN_POINT('Ctrl Pts',(-34.670679131947,63.0722610656194,0.));
#155344=CARTESIAN_POINT('Ctrl Pts',(-34.6669795685228,63.0485924065045,
0.));
#155345=CARTESIAN_POINT('Ctrl Pts',(-34.6632634733824,63.0249693746208,
0.));
#155346=CARTESIAN_POINT('Ctrl Pts',(-34.6595309261191,63.0013920796235,
0.));
#155347=CARTESIAN_POINT('Ctrl Pts',(-34.6557820067393,62.9778606315783,
0.));
#155348=CARTESIAN_POINT('Ctrl Pts',(-34.6520167956655,62.9543751409645,
0.));
#155349=CARTESIAN_POINT('Ctrl Pts',(-34.6482353737424,62.9309357186717,
0.));
#155350=CARTESIAN_POINT('Ctrl Pts',(-34.6444378222411,62.9075424760015,
0.));
#155351=CARTESIAN_POINT('Ctrl Pts',(-34.6406242228592,62.8841955246794,
0.));
#155352=CARTESIAN_POINT('Ctrl Pts',(-34.6367946577235,62.8608949768571,
0.));
#155353=CARTESIAN_POINT('Ctrl Pts',(-34.6329492093935,62.8376409451175,
0.));
#155354=CARTESIAN_POINT('Ctrl Pts',(-34.6290879608673,62.8144335424697,
0.));
#155355=CARTESIAN_POINT('Ctrl Pts',(-34.6252109955853,62.7912728823518,
0.));
#155356=CARTESIAN_POINT('Ctrl Pts',(-34.6213183974317,62.7681590786429,
0.));
#155357=CARTESIAN_POINT('Ctrl Pts',(-34.6174102507375,62.7450922456676,
0.));
#155358=CARTESIAN_POINT('Ctrl Pts',(-34.6134866402837,62.7220724981994,
0.));
#155359=CARTESIAN_POINT('Ctrl Pts',(-34.6095476513077,62.6990999514563,
0.));
#155360=CARTESIAN_POINT('Ctrl Pts',(-34.6055933695069,62.6761747211037,
0.));
#155361=CARTESIAN_POINT('Ctrl Pts',(-34.6016238810399,62.6532969232657,
0.));
#155362=CARTESIAN_POINT('Ctrl Pts',(-34.5976392725296,62.6304666745306,
0.));
#155363=CARTESIAN_POINT('Ctrl Pts',(-34.5936396310679,62.6076840919536,
0.));
#155364=CARTESIAN_POINT('Ctrl Pts',(-34.5896250442216,62.5849492930533,
0.));
#155365=CARTESIAN_POINT('Ctrl Pts',(-34.5855956000363,62.562262395816,0.));
#155366=CARTESIAN_POINT('Ctrl Pts',(-34.5815513870377,62.5396235187079,
0.));
#155367=CARTESIAN_POINT('Ctrl Pts',(-34.5774924942355,62.5170327806781,
0.));
#155368=CARTESIAN_POINT('Ctrl Pts',(-34.5734190111272,62.4944903011628,
0.));
#155369=CARTESIAN_POINT('Ctrl Pts',(-34.5693310277051,62.4719962000808,
0.));
#155370=CARTESIAN_POINT('Ctrl Pts',(-34.5652286344593,62.4495505978393,
0.));
#155371=CARTESIAN_POINT('Ctrl Pts',(-34.5611119223798,62.4271536153459,
0.));
#155372=CARTESIAN_POINT('Ctrl Pts',(-34.5569809829613,62.4048053740127,
0.));
#155373=CARTESIAN_POINT('Ctrl Pts',(-34.5528359082075,62.3825059957601,
0.));
#155374=CARTESIAN_POINT('Ctrl Pts',(-34.5486767906384,62.3602556030127,
0.));
#155375=CARTESIAN_POINT('Ctrl Pts',(-34.5445037232936,62.338054318708,0.));
#155376=CARTESIAN_POINT('Ctrl Pts',(-34.5403167997337,62.3159022663058,
0.));
#155377=CARTESIAN_POINT('Ctrl Pts',(-34.5361161140449,62.2937995697925,
0.));
#155378=CARTESIAN_POINT('Ctrl Pts',(-34.5319017608433,62.2717463536827,
0.));
#155379=CARTESIAN_POINT('Ctrl Pts',(-34.5276738352808,62.2497427430135,
0.));
#155380=CARTESIAN_POINT('Ctrl Pts',(-34.523432433049,62.2277888633576,0.));
#155381=CARTESIAN_POINT('Ctrl Pts',(-34.5191776503842,62.2058848408347,
0.));
#155382=CARTESIAN_POINT('Ctrl Pts',(-34.514909584073,62.1840308021171,0.));
#155383=CARTESIAN_POINT('Ctrl Pts',(-34.5106283314594,62.1622268744336,
0.));
#155384=CARTESIAN_POINT('Ctrl Pts',(-34.5063339904533,62.1404731855686,
0.));
#155385=CARTESIAN_POINT('Ctrl Pts',(-34.5020266595292,62.1187698638705,
0.));
#155386=CARTESIAN_POINT('Ctrl Pts',(-34.4977064377281,62.0971170382565,
0.));
#155387=CARTESIAN_POINT('Ctrl Pts',(-34.4933734246592,62.0755148382136,
0.));
#155388=CARTESIAN_POINT('Ctrl Pts',(-34.4890277205042,62.0539633937944,
0.));
#155389=CARTESIAN_POINT('Ctrl Pts',(-34.4846694260205,62.0324628356152,
0.));
#155390=CARTESIAN_POINT('Ctrl Pts',(-34.4802986425535,62.0110132948807,
0.));
#155391=CARTESIAN_POINT('Ctrl Pts',(-34.4759154720477,61.9896149034009,
0.));
#155392=CARTESIAN_POINT('Ctrl Pts',(-34.4715200170589,61.9682677936048,
0.));
#155393=CARTESIAN_POINT('Ctrl Pts',(-34.4671123807706,61.9469720985512,
0.));
#155394=CARTESIAN_POINT('Ctrl Pts',(-34.462692666996,61.9257279519283,0.));
#155395=CARTESIAN_POINT('Ctrl Pts',(-34.4582609801625,61.9045354880424,
0.));
#155396=CARTESIAN_POINT('Ctrl Pts',(-34.4538174253009,61.883394841802,0.));
#155397=CARTESIAN_POINT('Ctrl Pts',(-34.4493621080367,61.862306148703,0.));
#155398=CARTESIAN_POINT('Ctrl Pts',(-34.4448951345753,61.8412695447951,
0.));
#155399=CARTESIAN_POINT('Ctrl Pts',(-34.4404166117313,61.8202851667247,
0.));
#155400=CARTESIAN_POINT('Ctrl Pts',(-34.4359266469757,61.7993531518052,
0.));
#155401=CARTESIAN_POINT('Ctrl Pts',(-34.4314253484791,61.7784736380727,
0.));
#155402=CARTESIAN_POINT('Ctrl Pts',(-34.4269128251569,61.7576467643419,
0.));
#155403=CARTESIAN_POINT('Ctrl Pts',(-34.4223891867166,61.7368726702573,
0.));
#155404=CARTESIAN_POINT('Ctrl Pts',(-34.4178545435753,61.7161514961892,
0.));
#155405=CARTESIAN_POINT('Ctrl Pts',(-34.4133090067696,61.6954833831157,
0.));
#155406=CARTESIAN_POINT('Ctrl Pts',(-34.4087526878815,61.674868472521,0.));
#155407=CARTESIAN_POINT('Ctrl Pts',(-34.4041856989328,61.6543069062436,
0.));
#155408=CARTESIAN_POINT('Ctrl Pts',(-34.399608152377,61.6337988264586,0.));
#155409=CARTESIAN_POINT('Ctrl Pts',(-34.3950201613446,61.6133443760168,
0.));
#155410=CARTESIAN_POINT('Ctrl Pts',(-34.3904218398642,61.5929436987419,
0.));
#155411=CARTESIAN_POINT('Ctrl Pts',(-34.3858133030511,61.5725969396817,
0.));
#155412=CARTESIAN_POINT('Ctrl Pts',(-34.3811946674179,61.5523042455127,
0.));
#155413=CARTESIAN_POINT('Ctrl Pts',(-34.3765660506659,61.5320657642601,
0.));
#155414=CARTESIAN_POINT('Ctrl Pts',(-34.3719275711179,61.511881644541,0.));
#155415=CARTESIAN_POINT('Ctrl Pts',(-34.3672793472464,61.4917520349276,
0.));
#155416=CARTESIAN_POINT('Ctrl Pts',(-34.3626214971903,61.4716770832924,
0.));
#155417=CARTESIAN_POINT('Ctrl Pts',(-34.357954138202,61.4516569360499,0.));
#155418=CARTESIAN_POINT('Ctrl Pts',(-34.3532773877112,61.4316917395959,
0.));
#155419=CARTESIAN_POINT('Ctrl Pts',(-34.3485913645991,61.4117816420251,
0.));
#155420=CARTESIAN_POINT('Ctrl Pts',(-34.34389619024,61.3919267945293,0.));
#155421=CARTESIAN_POINT('Ctrl Pts',(-34.339191990012,61.3721273534222,0.));
#155422=CARTESIAN_POINT('Ctrl Pts',(-34.3344788934337,61.3523834803144,
0.));
#155423=CARTESIAN_POINT('Ctrl Pts',(-34.3297570310126,61.3326953378817,
0.));
#155424=CARTESIAN_POINT('Ctrl Pts',(-34.3250265314761,61.3130630861375,
0.));
#155425=CARTESIAN_POINT('Ctrl Pts',(-34.3202875193629,61.2934868791875,
0.));
#155426=CARTESIAN_POINT('Ctrl Pts',(-34.3155401111776,61.2739668600415,
0.));
#155427=CARTESIAN_POINT('Ctrl Pts',(-34.3107844191081,61.2545031656196,
0.));
#155428=CARTESIAN_POINT('Ctrl Pts',(-34.3060205584093,61.2350959366987,
0.));
#155429=CARTESIAN_POINT('Ctrl Pts',(-34.3012486533474,61.2157453259107,
0.));
#155430=CARTESIAN_POINT('Ctrl Pts',(-34.296468844362,61.1964515073823,0.));
#155431=CARTESIAN_POINT('Ctrl Pts',(-34.2916812929675,61.1772146833083,
0.));
#155432=CARTESIAN_POINT('Ctrl Pts',(-34.2868861666301,61.15803506354,0.));
#155433=CARTESIAN_POINT('Ctrl Pts',(-34.2820836244425,61.1389128461815,
0.));
#155434=CARTESIAN_POINT('Ctrl Pts',(-34.2772738038812,61.119848199783,0.));
#155435=CARTESIAN_POINT('Ctrl Pts',(-34.2724568037374,61.100841240023,0.));
#155436=CARTESIAN_POINT('Ctrl Pts',(-34.2676326825846,61.0818920286644,
0.));
#155437=CARTESIAN_POINT('Ctrl Pts',(-34.2637677132139,61.0667788793594,
0.));
#155438=CARTESIAN_POINT('Ctrl Pts',(-34.2608658001761,61.0554700177206,
0.));
#155439=CARTESIAN_POINT('Ctrl Pts',(-34.2589297755482,61.0479423318803,
0.));
#155440=CARTESIAN_POINT('Ctrl Pts',(-34.2579614092497,61.0441813777723,
0.));
#155441=CARTESIAN_POINT('Ctrl Pts',(-29.0861280018229,68.5875145916629,
0.));
#155442=CARTESIAN_POINT('Ctrl Pts',(-29.0861280018229,68.5875145916629,
12.));
#155443=CARTESIAN_POINT('Ctrl Pts',(-29.0863005247839,68.5819214834737,
0.));
#155444=CARTESIAN_POINT('Ctrl Pts',(-29.0863005247839,68.5819214834737,
12.));
#155445=CARTESIAN_POINT('Ctrl Pts',(-29.0866429722093,68.5707386600636,
0.));
#155446=CARTESIAN_POINT('Ctrl Pts',(-29.0866429722093,68.5707386600636,
12.));
#155447=CARTESIAN_POINT('Ctrl Pts',(-29.0871488478589,68.5539746038542,
0.));
#155448=CARTESIAN_POINT('Ctrl Pts',(-29.0871488478589,68.5539746038542,
12.));
#155449=CARTESIAN_POINT('Ctrl Pts',(-29.0878077571086,68.5316428875424,
0.));
#155450=CARTESIAN_POINT('Ctrl Pts',(-29.0878077571086,68.5316428875424,
12.));
#155451=CARTESIAN_POINT('Ctrl Pts',(-29.0886054060563,68.5037621824171,
0.));
#155452=CARTESIAN_POINT('Ctrl Pts',(-29.0886054060563,68.5037621824171,
12.));
#155453=CARTESIAN_POINT('Ctrl Pts',(-29.0893770688944,68.4759154367939,
0.));
#155454=CARTESIAN_POINT('Ctrl Pts',(-29.0893770688944,68.4759154367939,
12.));
#155455=CARTESIAN_POINT('Ctrl Pts',(-29.0901227535307,68.4481026830931,
0.));
#155456=CARTESIAN_POINT('Ctrl Pts',(-29.0901227535307,68.4481026830931,
12.));
#155457=CARTESIAN_POINT('Ctrl Pts',(-29.090842477089,68.4203239694612,0.));
#155458=CARTESIAN_POINT('Ctrl Pts',(-29.090842477089,68.4203239694612,12.));
#155459=CARTESIAN_POINT('Ctrl Pts',(-29.0915362699455,68.3925793637995,
0.));
#155460=CARTESIAN_POINT('Ctrl Pts',(-29.0915362699455,68.3925793637995,
12.));
#155461=CARTESIAN_POINT('Ctrl Pts',(-29.0922041749294,68.364868951893,0.));
#155462=CARTESIAN_POINT('Ctrl Pts',(-29.0922041749294,68.364868951893,12.));
#155463=CARTESIAN_POINT('Ctrl Pts',(-29.0928462428145,68.3371928310161,
0.));
#155464=CARTESIAN_POINT('Ctrl Pts',(-29.0928462428145,68.3371928310161,
12.));
#155465=CARTESIAN_POINT('Ctrl Pts',(-29.0934625288409,68.3095511047769,
0.));
#155466=CARTESIAN_POINT('Ctrl Pts',(-29.0934625288409,68.3095511047769,
12.));
#155467=CARTESIAN_POINT('Ctrl Pts',(-29.0940530889149,68.2819438775953,
0.));
#155468=CARTESIAN_POINT('Ctrl Pts',(-29.0940530889149,68.2819438775953,
12.));
#155469=CARTESIAN_POINT('Ctrl Pts',(-29.0946179757167,68.2543712489906,
0.));
#155470=CARTESIAN_POINT('Ctrl Pts',(-29.0946179757167,68.2543712489906,
12.));
#155471=CARTESIAN_POINT('Ctrl Pts',(-29.0951572355397,68.2268333089617,
0.));
#155472=CARTESIAN_POINT('Ctrl Pts',(-29.0951572355397,68.2268333089617,
12.));
#155473=CARTESIAN_POINT('Ctrl Pts',(-29.0956709104627,68.1993301412061,
0.));
#155474=CARTESIAN_POINT('Ctrl Pts',(-29.0956709104627,68.1993301412061,
12.));
#155475=CARTESIAN_POINT('Ctrl Pts',(-29.0961590399046,68.1718618254281,
0.));
#155476=CARTESIAN_POINT('Ctrl Pts',(-29.0961590399046,68.1718618254281,
12.));
#155477=CARTESIAN_POINT('Ctrl Pts',(-29.0966216624743,68.1444284400742,
0.));
#155478=CARTESIAN_POINT('Ctrl Pts',(-29.0966216624743,68.1444284400742,
12.));
#155479=CARTESIAN_POINT('Ctrl Pts',(-29.0970588175728,68.1170300646987,
0.));
#155480=CARTESIAN_POINT('Ctrl Pts',(-29.0970588175728,68.1170300646987,
12.));
#155481=CARTESIAN_POINT('Ctrl Pts',(-29.0974705474259,68.0896667829567,
0.));
#155482=CARTESIAN_POINT('Ctrl Pts',(-29.0974705474259,68.0896667829567,
12.));
#155483=CARTESIAN_POINT('Ctrl Pts',(-29.0978568968657,68.0623386822863,
0.));
#155484=CARTESIAN_POINT('Ctrl Pts',(-29.0978568968657,68.0623386822863,
12.));
#155485=CARTESIAN_POINT('Ctrl Pts',(-29.0982179124097,68.0350458525551,
0.));
#155486=CARTESIAN_POINT('Ctrl Pts',(-29.0982179124097,68.0350458525551,
12.));
#155487=CARTESIAN_POINT('Ctrl Pts',(-29.0985536415531,68.0077883850121,
0.));
#155488=CARTESIAN_POINT('Ctrl Pts',(-29.0985536415531,68.0077883850121,
12.));
#155489=CARTESIAN_POINT('Ctrl Pts',(-29.0988641320247,67.9805663711855,
0.));
#155490=CARTESIAN_POINT('Ctrl Pts',(-29.0988641320247,67.9805663711855,
12.));
#155491=CARTESIAN_POINT('Ctrl Pts',(-29.0991494309404,67.9533799016148,
0.));
#155492=CARTESIAN_POINT('Ctrl Pts',(-29.0991494309404,67.9533799016148,
12.));
#155493=CARTESIAN_POINT('Ctrl Pts',(-29.099409584422,67.9262290652829,0.));
#155494=CARTESIAN_POINT('Ctrl Pts',(-29.099409584422,67.9262290652829,12.));
#155495=CARTESIAN_POINT('Ctrl Pts',(-29.0996446380626,67.8991139503193,
0.));
#155496=CARTESIAN_POINT('Ctrl Pts',(-29.0996446380626,67.8991139503193,
12.));
#155497=CARTESIAN_POINT('Ctrl Pts',(-29.0998546372032,67.8720346444124,
0.));
#155498=CARTESIAN_POINT('Ctrl Pts',(-29.0998546372032,67.8720346444124,
12.));
#155499=CARTESIAN_POINT('Ctrl Pts',(-29.1000396272867,67.8449912353329,
0.));
#155500=CARTESIAN_POINT('Ctrl Pts',(-29.1000396272867,67.8449912353329,
12.));
#155501=CARTESIAN_POINT('Ctrl Pts',(-29.1001996541842,67.8179838114099,
0.));
#155502=CARTESIAN_POINT('Ctrl Pts',(-29.1001996541842,67.8179838114099,
12.));
#155503=CARTESIAN_POINT('Ctrl Pts',(-29.1003347645294,67.7910124620135,
0.));
#155504=CARTESIAN_POINT('Ctrl Pts',(-29.1003347645294,67.7910124620135,
12.));
#155505=CARTESIAN_POINT('Ctrl Pts',(-29.1004450055643,67.7640772773387,
0.));
#155506=CARTESIAN_POINT('Ctrl Pts',(-29.1004450055643,67.7640772773387,
12.));
#155507=CARTESIAN_POINT('Ctrl Pts',(-29.1005304249987,67.7371783482035,
0.));
#155508=CARTESIAN_POINT('Ctrl Pts',(-29.1005304249987,67.7371783482035,
12.));
#155509=CARTESIAN_POINT('Ctrl Pts',(-29.1005910708624,67.7103157658296,
0.));
#155510=CARTESIAN_POINT('Ctrl Pts',(-29.1005910708624,67.7103157658296,
12.));
#155511=CARTESIAN_POINT('Ctrl Pts',(-29.1006269913747,67.6834896216461,
0.));
#155512=CARTESIAN_POINT('Ctrl Pts',(-29.1006269913747,67.6834896216461,
12.));
#155513=CARTESIAN_POINT('Ctrl Pts',(-29.1006382347814,67.6567000070326,
0.));
#155514=CARTESIAN_POINT('Ctrl Pts',(-29.1006382347814,67.6567000070326,
12.));
#155515=CARTESIAN_POINT('Ctrl Pts',(-29.100624849358,67.6299470133295,0.));
#155516=CARTESIAN_POINT('Ctrl Pts',(-29.100624849358,67.6299470133295,12.));
#155517=CARTESIAN_POINT('Ctrl Pts',(-29.1005868834866,67.6032307319623,
0.));
#155518=CARTESIAN_POINT('Ctrl Pts',(-29.1005868834866,67.6032307319623,
12.));
#155519=CARTESIAN_POINT('Ctrl Pts',(-29.1005243857139,67.5765512545281,
0.));
#155520=CARTESIAN_POINT('Ctrl Pts',(-29.1005243857139,67.5765512545281,
12.));
#155521=CARTESIAN_POINT('Ctrl Pts',(-29.1004374048148,67.5499086728888,
0.));
#155522=CARTESIAN_POINT('Ctrl Pts',(-29.1004374048148,67.5499086728888,
12.));
#155523=CARTESIAN_POINT('Ctrl Pts',(-29.1003259898682,67.5233030792704,
0.));
#155524=CARTESIAN_POINT('Ctrl Pts',(-29.1003259898682,67.5233030792704,
12.));
#155525=CARTESIAN_POINT('Ctrl Pts',(-29.1001901902909,67.4967345663096,
0.));
#155526=CARTESIAN_POINT('Ctrl Pts',(-29.1001901902909,67.4967345663096,
12.));
#155527=CARTESIAN_POINT('Ctrl Pts',(-29.1000300557955,67.4702032270048,
0.));
#155528=CARTESIAN_POINT('Ctrl Pts',(-29.1000300557955,67.4702032270048,
12.));
#155529=CARTESIAN_POINT('Ctrl Pts',(-29.0998456363683,67.4437091546859,
0.));
#155530=CARTESIAN_POINT('Ctrl Pts',(-29.0998456363683,67.4437091546859,
12.));
#155531=CARTESIAN_POINT('Ctrl Pts',(-29.0996369822418,67.4172524429727,
0.));
#155532=CARTESIAN_POINT('Ctrl Pts',(-29.0996369822418,67.4172524429727,
12.));
#155533=CARTESIAN_POINT('Ctrl Pts',(-29.0994041438719,67.3908331857323,
0.));
#155534=CARTESIAN_POINT('Ctrl Pts',(-29.0994041438719,67.3908331857323,
12.));
#155535=CARTESIAN_POINT('Ctrl Pts',(-29.0991471719176,67.3644514770387,
0.));
#155536=CARTESIAN_POINT('Ctrl Pts',(-29.0991471719176,67.3644514770387,
12.));
#155537=CARTESIAN_POINT('Ctrl Pts',(-29.0988661172531,67.3381074112027,
0.));
#155538=CARTESIAN_POINT('Ctrl Pts',(-29.0988661172531,67.3381074112027,
12.));
#155539=CARTESIAN_POINT('Ctrl Pts',(-29.0985610309771,67.311801082792,0.));
#155540=CARTESIAN_POINT('Ctrl Pts',(-29.0985610309771,67.311801082792,12.));
#155541=CARTESIAN_POINT('Ctrl Pts',(-29.0982319644277,67.2855325866517,
0.));
#155542=CARTESIAN_POINT('Ctrl Pts',(-29.0982319644277,67.2855325866517,
12.));
#155543=CARTESIAN_POINT('Ctrl Pts',(-29.0978789691962,67.2593020179209,
0.));
#155544=CARTESIAN_POINT('Ctrl Pts',(-29.0978789691962,67.2593020179209,
12.));
#155545=CARTESIAN_POINT('Ctrl Pts',(-29.097502097147,67.2331094720471,0.));
#155546=CARTESIAN_POINT('Ctrl Pts',(-29.097502097147,67.2331094720471,12.));
#155547=CARTESIAN_POINT('Ctrl Pts',(-29.0971014004131,67.2069550447883,
0.));
#155548=CARTESIAN_POINT('Ctrl Pts',(-29.0971014004131,67.2069550447883,
12.));
#155549=CARTESIAN_POINT('Ctrl Pts',(-29.096676931389,67.1808388322109,0.));
#155550=CARTESIAN_POINT('Ctrl Pts',(-29.096676931389,67.1808388322109,12.));
#155551=CARTESIAN_POINT('Ctrl Pts',(-29.0962287427273,67.1547609306843,
0.));
#155552=CARTESIAN_POINT('Ctrl Pts',(-29.0962287427273,67.1547609306843,
12.));
#155553=CARTESIAN_POINT('Ctrl Pts',(-29.0957568873358,67.1287214368746,
0.));
#155554=CARTESIAN_POINT('Ctrl Pts',(-29.0957568873358,67.1287214368746,
12.));
#155555=CARTESIAN_POINT('Ctrl Pts',(-29.0952614183779,67.1027204477311,
0.));
#155556=CARTESIAN_POINT('Ctrl Pts',(-29.0952614183779,67.1027204477311,
12.));
#155557=CARTESIAN_POINT('Ctrl Pts',(-29.0947423892727,67.0767580604879,
0.));
#155558=CARTESIAN_POINT('Ctrl Pts',(-29.0947423892727,67.0767580604879,
12.));
#155559=CARTESIAN_POINT('Ctrl Pts',(-29.0941998536959,67.0508343726776,
0.));
#155560=CARTESIAN_POINT('Ctrl Pts',(-29.0941998536959,67.0508343726776,
12.));
#155561=CARTESIAN_POINT('Ctrl Pts',(-29.0936338655828,67.0249494821363,
0.));
#155562=CARTESIAN_POINT('Ctrl Pts',(-29.0936338655828,67.0249494821363,
12.));
#155563=CARTESIAN_POINT('Ctrl Pts',(-29.0930444791328,66.9991034870083,
0.));
#155564=CARTESIAN_POINT('Ctrl Pts',(-29.0930444791328,66.9991034870083,
12.));
#155565=CARTESIAN_POINT('Ctrl Pts',(-29.092431748817,66.9732964857466,0.));
#155566=CARTESIAN_POINT('Ctrl Pts',(-29.092431748817,66.9732964857466,12.));
#155567=CARTESIAN_POINT('Ctrl Pts',(-29.0917957293826,66.9475285771135,
0.));
#155568=CARTESIAN_POINT('Ctrl Pts',(-29.0917957293826,66.9475285771135,
12.));
#155569=CARTESIAN_POINT('Ctrl Pts',(-29.0911364758487,66.9217998601885,
0.));
#155570=CARTESIAN_POINT('Ctrl Pts',(-29.0911364758487,66.9217998601885,
12.));
#155571=CARTESIAN_POINT('Ctrl Pts',(-29.0904540435065,66.8961104343707,
0.));
#155572=CARTESIAN_POINT('Ctrl Pts',(-29.0904540435065,66.8961104343707,
12.));
#155573=CARTESIAN_POINT('Ctrl Pts',(-29.0897484879207,66.8704603993794,
0.));
#155574=CARTESIAN_POINT('Ctrl Pts',(-29.0897484879207,66.8704603993794,
12.));
#155575=CARTESIAN_POINT('Ctrl Pts',(-29.0890198649323,66.8448498552503,
0.));
#155576=CARTESIAN_POINT('Ctrl Pts',(-29.0890198649323,66.8448498552503,
12.));
#155577=CARTESIAN_POINT('Ctrl Pts',(-29.088268230663,66.8192789023312,0.));
#155578=CARTESIAN_POINT('Ctrl Pts',(-29.088268230663,66.8192789023312,12.));
#155579=CARTESIAN_POINT('Ctrl Pts',(-29.0874936415132,66.793747641293,0.));
#155580=CARTESIAN_POINT('Ctrl Pts',(-29.0874936415132,66.793747641293,12.));
#155581=CARTESIAN_POINT('Ctrl Pts',(-29.0866961541626,66.7682561731341,
0.));
#155582=CARTESIAN_POINT('Ctrl Pts',(-29.0866961541626,66.7682561731341,
12.));
#155583=CARTESIAN_POINT('Ctrl Pts',(-29.0858758255729,66.7428045991841,
0.));
#155584=CARTESIAN_POINT('Ctrl Pts',(-29.0858758255729,66.7428045991841,
12.));
#155585=CARTESIAN_POINT('Ctrl Pts',(-29.0850327129916,66.7173930211022,
0.));
#155586=CARTESIAN_POINT('Ctrl Pts',(-29.0850327129916,66.7173930211022,
12.));
#155587=CARTESIAN_POINT('Ctrl Pts',(-29.0841668739588,66.6920215408751,
0.));
#155588=CARTESIAN_POINT('Ctrl Pts',(-29.0841668739588,66.6920215408751,
12.));
#155589=CARTESIAN_POINT('Ctrl Pts',(-29.083278366305,66.6666902608249,0.));
#155590=CARTESIAN_POINT('Ctrl Pts',(-29.083278366305,66.6666902608249,12.));
#155591=CARTESIAN_POINT('Ctrl Pts',(-29.0823672481507,66.6413992836147,
0.));
#155592=CARTESIAN_POINT('Ctrl Pts',(-29.0823672481507,66.6413992836147,
12.));
#155593=CARTESIAN_POINT('Ctrl Pts',(-29.0814335779084,66.6161487122502,
0.));
#155594=CARTESIAN_POINT('Ctrl Pts',(-29.0814335779084,66.6161487122502,
12.));
#155595=CARTESIAN_POINT('Ctrl Pts',(-29.0804774142854,66.59093865008,0.));
#155596=CARTESIAN_POINT('Ctrl Pts',(-29.0804774142854,66.59093865008,12.));
#155597=CARTESIAN_POINT('Ctrl Pts',(-29.0794988162897,66.5657692007906,
0.));
#155598=CARTESIAN_POINT('Ctrl Pts',(-29.0794988162897,66.5657692007906,
12.));
#155599=CARTESIAN_POINT('Ctrl Pts',(-29.0784978432301,66.5406404684132,
0.));
#155600=CARTESIAN_POINT('Ctrl Pts',(-29.0784978432301,66.5406404684132,
12.));
#155601=CARTESIAN_POINT('Ctrl Pts',(-29.0774745547152,66.5155525573323,
0.));
#155602=CARTESIAN_POINT('Ctrl Pts',(-29.0774745547152,66.5155525573323,
12.));
#155603=CARTESIAN_POINT('Ctrl Pts',(-29.0764290106554,66.4905055722868,
0.));
#155604=CARTESIAN_POINT('Ctrl Pts',(-29.0764290106554,66.4905055722868,
12.));
#155605=CARTESIAN_POINT('Ctrl Pts',(-29.0753612712666,66.4654996183731,
0.));
#155606=CARTESIAN_POINT('Ctrl Pts',(-29.0753612712666,66.4654996183731,
12.));
#155607=CARTESIAN_POINT('Ctrl Pts',(-29.0742713970755,66.4405348010388,
0.));
#155608=CARTESIAN_POINT('Ctrl Pts',(-29.0742713970755,66.4405348010388,
12.));
#155609=CARTESIAN_POINT('Ctrl Pts',(-29.0731594489211,66.4156112260887,
0.));
#155610=CARTESIAN_POINT('Ctrl Pts',(-29.0731594489211,66.4156112260887,
12.));
#155611=CARTESIAN_POINT('Ctrl Pts',(-29.072025487953,66.3907289996932,0.));
#155612=CARTESIAN_POINT('Ctrl Pts',(-29.072025487953,66.3907289996932,12.));
#155613=CARTESIAN_POINT('Ctrl Pts',(-29.0708695756334,66.3658882283903,
0.));
#155614=CARTESIAN_POINT('Ctrl Pts',(-29.0708695756334,66.3658882283903,
12.));
#155615=CARTESIAN_POINT('Ctrl Pts',(-29.0696917737399,66.3410890190884,
0.));
#155616=CARTESIAN_POINT('Ctrl Pts',(-29.0696917737399,66.3410890190884,
12.));
#155617=CARTESIAN_POINT('Ctrl Pts',(-29.0684921443721,66.3163314790615,
0.));
#155618=CARTESIAN_POINT('Ctrl Pts',(-29.0684921443721,66.3163314790615,
12.));
#155619=CARTESIAN_POINT('Ctrl Pts',(-29.067270749953,66.2916157159536,0.));
#155620=CARTESIAN_POINT('Ctrl Pts',(-29.067270749953,66.2916157159536,12.));
#155621=CARTESIAN_POINT('Ctrl Pts',(-29.0660276532274,66.2669418377871,
0.));
#155622=CARTESIAN_POINT('Ctrl Pts',(-29.0660276532274,66.2669418377871,
12.));
#155623=CARTESIAN_POINT('Ctrl Pts',(-29.0647629172645,66.2423099529669,
0.));
#155624=CARTESIAN_POINT('Ctrl Pts',(-29.0647629172645,66.2423099529669,
12.));
#155625=CARTESIAN_POINT('Ctrl Pts',(-29.0634766054598,66.2177201702818,
0.));
#155626=CARTESIAN_POINT('Ctrl Pts',(-29.0634766054598,66.2177201702818,
12.));
#155627=CARTESIAN_POINT('Ctrl Pts',(-29.062168781542,66.1931725989008,0.));
#155628=CARTESIAN_POINT('Ctrl Pts',(-29.062168781542,66.1931725989008,12.));
#155629=CARTESIAN_POINT('Ctrl Pts',(-29.0608395095747,66.1686673483757,
0.));
#155630=CARTESIAN_POINT('Ctrl Pts',(-29.0608395095747,66.1686673483757,
12.));
#155631=CARTESIAN_POINT('Ctrl Pts',(-29.0594888539558,66.144204528652,0.));
#155632=CARTESIAN_POINT('Ctrl Pts',(-29.0594888539558,66.144204528652,12.));
#155633=CARTESIAN_POINT('Ctrl Pts',(-29.0581168794191,66.1197842500714,
0.));
#155634=CARTESIAN_POINT('Ctrl Pts',(-29.0581168794191,66.1197842500714,
12.));
#155635=CARTESIAN_POINT('Ctrl Pts',(-29.0567236510372,66.0954066233752,
0.));
#155636=CARTESIAN_POINT('Ctrl Pts',(-29.0567236510372,66.0954066233752,
12.));
#155637=CARTESIAN_POINT('Ctrl Pts',(-29.0553092342275,66.0710717597003,
0.));
#155638=CARTESIAN_POINT('Ctrl Pts',(-29.0553092342275,66.0710717597003,
12.));
#155639=CARTESIAN_POINT('Ctrl Pts',(-29.0538736947547,66.0467797705806,
0.));
#155640=CARTESIAN_POINT('Ctrl Pts',(-29.0538736947547,66.0467797705806,
12.));
#155641=CARTESIAN_POINT('Ctrl Pts',(-29.0524170987303,66.0225307679584,
0.));
#155642=CARTESIAN_POINT('Ctrl Pts',(-29.0524170987303,66.0225307679584,
12.));
#155643=CARTESIAN_POINT('Ctrl Pts',(-29.0509395126141,65.9983248641877,
0.));
#155644=CARTESIAN_POINT('Ctrl Pts',(-29.0509395126141,65.9983248641877,
12.));
#155645=CARTESIAN_POINT('Ctrl Pts',(-29.0494410032173,65.9741621720372,
0.));
#155646=CARTESIAN_POINT('Ctrl Pts',(-29.0494410032173,65.9741621720372,
12.));
#155647=CARTESIAN_POINT('Ctrl Pts',(-29.0479216377082,65.9500428046873,
0.));
#155648=CARTESIAN_POINT('Ctrl Pts',(-29.0479216377082,65.9500428046873,
12.));
#155649=CARTESIAN_POINT('Ctrl Pts',(-29.0463814836159,65.9259668757309,
0.));
#155650=CARTESIAN_POINT('Ctrl Pts',(-29.0463814836159,65.9259668757309,
12.));
#155651=CARTESIAN_POINT('Ctrl Pts',(-29.0448206088288,65.9019344991854,
0.));
#155652=CARTESIAN_POINT('Ctrl Pts',(-29.0448206088288,65.9019344991854,
12.));
#155653=CARTESIAN_POINT('Ctrl Pts',(-29.0432390815977,65.8779457894959,
0.));
#155654=CARTESIAN_POINT('Ctrl Pts',(-29.0432390815977,65.8779457894959,
12.));
#155655=CARTESIAN_POINT('Ctrl Pts',(-29.0416369705375,65.854000861539,0.));
#155656=CARTESIAN_POINT('Ctrl Pts',(-29.0416369705375,65.854000861539,12.));
#155657=CARTESIAN_POINT('Ctrl Pts',(-29.0400143446341,65.8300998306198,
0.));
#155658=CARTESIAN_POINT('Ctrl Pts',(-29.0400143446341,65.8300998306198,
12.));
#155659=CARTESIAN_POINT('Ctrl Pts',(-29.0383712732473,65.8062428124723,
0.));
#155660=CARTESIAN_POINT('Ctrl Pts',(-29.0383712732473,65.8062428124723,
12.));
#155661=CARTESIAN_POINT('Ctrl Pts',(-29.0367078261107,65.7824299232715,
0.));
#155662=CARTESIAN_POINT('Ctrl Pts',(-29.0367078261107,65.7824299232715,
12.));
#155663=CARTESIAN_POINT('Ctrl Pts',(-29.0350240733333,65.7586612796375,
0.));
#155664=CARTESIAN_POINT('Ctrl Pts',(-29.0350240733333,65.7586612796375,
12.));
#155665=CARTESIAN_POINT('Ctrl Pts',(-29.0333200854026,65.7349369986382,
0.));
#155666=CARTESIAN_POINT('Ctrl Pts',(-29.0333200854026,65.7349369986382,
12.));
#155667=CARTESIAN_POINT('Ctrl Pts',(-29.0315959331911,65.7112571977874,
0.));
#155668=CARTESIAN_POINT('Ctrl Pts',(-29.0315959331911,65.7112571977874,
12.));
#155669=CARTESIAN_POINT('Ctrl Pts',(-29.0298516879599,65.6876219950465,
0.));
#155670=CARTESIAN_POINT('Ctrl Pts',(-29.0298516879599,65.6876219950465,
12.));
#155671=CARTESIAN_POINT('Ctrl Pts',(-29.0280874213584,65.664031508836,0.));
#155672=CARTESIAN_POINT('Ctrl Pts',(-29.0280874213584,65.664031508836,12.));
#155673=CARTESIAN_POINT('Ctrl Pts',(-29.0263032054261,65.6404858580391,
0.));
#155674=CARTESIAN_POINT('Ctrl Pts',(-29.0263032054261,65.6404858580391,
12.));
#155675=CARTESIAN_POINT('Ctrl Pts',(-29.0244991125962,65.6169851620054,
0.));
#155676=CARTESIAN_POINT('Ctrl Pts',(-29.0244991125962,65.6169851620054,
12.));
#155677=CARTESIAN_POINT('Ctrl Pts',(-29.0226752157013,65.593529540548,0.));
#155678=CARTESIAN_POINT('Ctrl Pts',(-29.0226752157013,65.593529540548,12.));
#155679=CARTESIAN_POINT('Ctrl Pts',(-29.0208315879778,65.5701191139455,
0.));
#155680=CARTESIAN_POINT('Ctrl Pts',(-29.0208315879778,65.5701191139455,
12.));
#155681=CARTESIAN_POINT('Ctrl Pts',(-29.0189683030654,65.5467540029546,
0.));
#155682=CARTESIAN_POINT('Ctrl Pts',(-29.0189683030654,65.5467540029546,
12.));
#155683=CARTESIAN_POINT('Ctrl Pts',(-29.01708543501,65.523434328815,0.));
#155684=CARTESIAN_POINT('Ctrl Pts',(-29.01708543501,65.523434328815,12.));
#155685=CARTESIAN_POINT('Ctrl Pts',(-29.015183058267,65.5001602132524,0.));
#155686=CARTESIAN_POINT('Ctrl Pts',(-29.015183058267,65.5001602132524,12.));
#155687=CARTESIAN_POINT('Ctrl Pts',(-29.0132612477075,65.4769317784754,
0.));
#155688=CARTESIAN_POINT('Ctrl Pts',(-29.0132612477075,65.4769317784754,
12.));
#155689=CARTESIAN_POINT('Ctrl Pts',(-29.0113200786219,65.4537491471782,
0.));
#155690=CARTESIAN_POINT('Ctrl Pts',(-29.0113200786219,65.4537491471782,
12.));
#155691=CARTESIAN_POINT('Ctrl Pts',(-29.0093596267198,65.4306124425524,
0.));
#155692=CARTESIAN_POINT('Ctrl Pts',(-29.0093596267198,65.4306124425524,
12.));
#155693=CARTESIAN_POINT('Ctrl Pts',(-29.0073799681336,65.4075217882921,
0.));
#155694=CARTESIAN_POINT('Ctrl Pts',(-29.0073799681336,65.4075217882921,
12.));
#155695=CARTESIAN_POINT('Ctrl Pts',(-29.0053811794214,65.3844773085976,
0.));
#155696=CARTESIAN_POINT('Ctrl Pts',(-29.0053811794214,65.3844773085976,
12.));
#155697=CARTESIAN_POINT('Ctrl Pts',(-29.0033633375745,65.3614791281725,
0.));
#155698=CARTESIAN_POINT('Ctrl Pts',(-29.0033633375745,65.3614791281725,
12.));
#155699=CARTESIAN_POINT('Ctrl Pts',(-29.0013265200201,65.3385273722278,
0.));
#155700=CARTESIAN_POINT('Ctrl Pts',(-29.0013265200201,65.3385273722278,
12.));
#155701=CARTESIAN_POINT('Ctrl Pts',(-28.9992708046223,65.3156221664942,
0.));
#155702=CARTESIAN_POINT('Ctrl Pts',(-28.9992708046223,65.3156221664942,
12.));
#155703=CARTESIAN_POINT('Ctrl Pts',(-28.9971962696848,65.2927636372261,
0.));
#155704=CARTESIAN_POINT('Ctrl Pts',(-28.9971962696848,65.2927636372261,
12.));
#155705=CARTESIAN_POINT('Ctrl Pts',(-28.9951029939551,65.2699519112052,
0.));
#155706=CARTESIAN_POINT('Ctrl Pts',(-28.9951029939551,65.2699519112052,
12.));
#155707=CARTESIAN_POINT('Ctrl Pts',(-28.9929910566314,65.2471871157375,
0.));
#155708=CARTESIAN_POINT('Ctrl Pts',(-28.9929910566314,65.2471871157375,
12.));
#155709=CARTESIAN_POINT('Ctrl Pts',(-28.9908605373652,65.2244693786586,
0.));
#155710=CARTESIAN_POINT('Ctrl Pts',(-28.9908605373652,65.2244693786586,
12.));
#155711=CARTESIAN_POINT('Ctrl Pts',(-28.9887115162626,65.2017988283465,
0.));
#155712=CARTESIAN_POINT('Ctrl Pts',(-28.9887115162626,65.2017988283465,
12.));
#155713=CARTESIAN_POINT('Ctrl Pts',(-28.9865440738882,65.1791755937254,
0.));
#155714=CARTESIAN_POINT('Ctrl Pts',(-28.9865440738882,65.1791755937254,
12.));
#155715=CARTESIAN_POINT('Ctrl Pts',(-28.9843582912697,65.1565998042705,
0.));
#155716=CARTESIAN_POINT('Ctrl Pts',(-28.9843582912697,65.1565998042705,
12.));
#155717=CARTESIAN_POINT('Ctrl Pts',(-28.9821542499049,65.1340715900042,
0.));
#155718=CARTESIAN_POINT('Ctrl Pts',(-28.9821542499049,65.1340715900042,
12.));
#155719=CARTESIAN_POINT('Ctrl Pts',(-28.9799320317648,65.111591081505,0.));
#155720=CARTESIAN_POINT('Ctrl Pts',(-28.9799320317648,65.111591081505,12.));
#155721=CARTESIAN_POINT('Ctrl Pts',(-28.9776917192936,65.0891584099174,
0.));
#155722=CARTESIAN_POINT('Ctrl Pts',(-28.9776917192936,65.0891584099174,
12.));
#155723=CARTESIAN_POINT('Ctrl Pts',(-28.9754333954134,65.0667737069562,
0.));
#155724=CARTESIAN_POINT('Ctrl Pts',(-28.9754333954134,65.0667737069562,
12.));
#155725=CARTESIAN_POINT('Ctrl Pts',(-28.9731571435281,65.0444371049082,
0.));
#155726=CARTESIAN_POINT('Ctrl Pts',(-28.9731571435281,65.0444371049082,
12.));
#155727=CARTESIAN_POINT('Ctrl Pts',(-28.9708630475298,65.0221487366279,
0.));
#155728=CARTESIAN_POINT('Ctrl Pts',(-28.9708630475298,65.0221487366279,
12.));
#155729=CARTESIAN_POINT('Ctrl Pts',(-28.9685511918017,64.9999087355504,
0.));
#155730=CARTESIAN_POINT('Ctrl Pts',(-28.9685511918017,64.9999087355504,
12.));
#155731=CARTESIAN_POINT('Ctrl Pts',(-28.9662216612216,64.9777172357028,
0.));
#155732=CARTESIAN_POINT('Ctrl Pts',(-28.9662216612216,64.9777172357028,
12.));
#155733=CARTESIAN_POINT('Ctrl Pts',(-28.9638745411677,64.955574371711,0.));
#155734=CARTESIAN_POINT('Ctrl Pts',(-28.9638745411677,64.955574371711,12.));
#155735=CARTESIAN_POINT('Ctrl Pts',(-28.961509917525,64.9334802788037,0.));
#155736=CARTESIAN_POINT('Ctrl Pts',(-28.961509917525,64.9334802788037,12.));
#155737=CARTESIAN_POINT('Ctrl Pts',(-28.9591278766934,64.9114350928124,
0.));
#155738=CARTESIAN_POINT('Ctrl Pts',(-28.9591278766934,64.9114350928124,
12.));
#155739=CARTESIAN_POINT('Ctrl Pts',(-28.9567285055866,64.8894389501799,
0.));
#155740=CARTESIAN_POINT('Ctrl Pts',(-28.9567285055866,64.8894389501799,
12.));
#155741=CARTESIAN_POINT('Ctrl Pts',(-28.9543118916327,64.8674919879646,
0.));
#155742=CARTESIAN_POINT('Ctrl Pts',(-28.9543118916327,64.8674919879646,
12.));
#155743=CARTESIAN_POINT('Ctrl Pts',(-28.9518781227765,64.8455943438423,
0.));
#155744=CARTESIAN_POINT('Ctrl Pts',(-28.9518781227765,64.8455943438423,
12.));
#155745=CARTESIAN_POINT('Ctrl Pts',(-28.9494272874833,64.8237461561024,
0.));
#155746=CARTESIAN_POINT('Ctrl Pts',(-28.9494272874833,64.8237461561024,
12.));
#155747=CARTESIAN_POINT('Ctrl Pts',(-28.9469594747436,64.8019475636454,
0.));
#155748=CARTESIAN_POINT('Ctrl Pts',(-28.9469594747436,64.8019475636454,
12.));
#155749=CARTESIAN_POINT('Ctrl Pts',(-28.9444747740815,64.7801987060097,
0.));
#155750=CARTESIAN_POINT('Ctrl Pts',(-28.9444747740815,64.7801987060097,
12.));
#155751=CARTESIAN_POINT('Ctrl Pts',(-28.9419732755659,64.7584997233889,
0.));
#155752=CARTESIAN_POINT('Ctrl Pts',(-28.9419732755659,64.7584997233889,
12.));
#155753=CARTESIAN_POINT('Ctrl Pts',(-28.9394550698201,64.7368507566461,
0.));
#155754=CARTESIAN_POINT('Ctrl Pts',(-28.9394550698201,64.7368507566461,
12.));
#155755=CARTESIAN_POINT('Ctrl Pts',(-28.9369202480383,64.715251947327,0.));
#155756=CARTESIAN_POINT('Ctrl Pts',(-28.9369202480383,64.715251947327,12.));
#155757=CARTESIAN_POINT('Ctrl Pts',(-28.934368901987,64.6937034376591,0.));
#155758=CARTESIAN_POINT('Ctrl Pts',(-28.934368901987,64.6937034376591,12.));
#155759=CARTESIAN_POINT('Ctrl Pts',(-28.9318011239905,64.6722053705389,
0.));
#155760=CARTESIAN_POINT('Ctrl Pts',(-28.9318011239905,64.6722053705389,
12.));
#155761=CARTESIAN_POINT('Ctrl Pts',(-28.9292170069219,64.6507578895155,
0.));
#155762=CARTESIAN_POINT('Ctrl Pts',(-28.9292170069219,64.6507578895155,
12.));
#155763=CARTESIAN_POINT('Ctrl Pts',(-28.9266166441956,64.6293611387753,
0.));
#155764=CARTESIAN_POINT('Ctrl Pts',(-28.9266166441956,64.6293611387753,
12.));
#155765=CARTESIAN_POINT('Ctrl Pts',(-28.9240001297553,64.6080152631065,
0.));
#155766=CARTESIAN_POINT('Ctrl Pts',(-28.9240001297553,64.6080152631065,
12.));
#155767=CARTESIAN_POINT('Ctrl Pts',(-28.9213675580996,64.5867204079452,
0.));
#155768=CARTESIAN_POINT('Ctrl Pts',(-28.9213675580996,64.5867204079452,
12.));
#155769=CARTESIAN_POINT('Ctrl Pts',(-28.9187190243231,64.5654767194487,
0.));
#155770=CARTESIAN_POINT('Ctrl Pts',(-28.9187190243231,64.5654767194487,
12.));
#155771=CARTESIAN_POINT('Ctrl Pts',(-28.9160546241538,64.544284344556,0.));
#155772=CARTESIAN_POINT('Ctrl Pts',(-28.9160546241538,64.544284344556,12.));
#155773=CARTESIAN_POINT('Ctrl Pts',(-28.9133744539943,64.5231434310457,
0.));
#155774=CARTESIAN_POINT('Ctrl Pts',(-28.9133744539943,64.5231434310457,
12.));
#155775=CARTESIAN_POINT('Ctrl Pts',(-28.9106786109639,64.5020541275927,
0.));
#155776=CARTESIAN_POINT('Ctrl Pts',(-28.9106786109639,64.5020541275927,
12.));
#155777=CARTESIAN_POINT('Ctrl Pts',(-28.9079671928253,64.4810165836568,
0.));
#155778=CARTESIAN_POINT('Ctrl Pts',(-28.9079671928253,64.4810165836568,
12.));
#155779=CARTESIAN_POINT('Ctrl Pts',(-28.9052402979055,64.460030949357,0.));
#155780=CARTESIAN_POINT('Ctrl Pts',(-28.9052402979055,64.460030949357,12.));
#155781=CARTESIAN_POINT('Ctrl Pts',(-28.9024980250309,64.439097375364,0.));
#155782=CARTESIAN_POINT('Ctrl Pts',(-28.9024980250309,64.439097375364,12.));
#155783=CARTESIAN_POINT('Ctrl Pts',(-28.899740473435,64.41821601274,0.));
#155784=CARTESIAN_POINT('Ctrl Pts',(-28.899740473435,64.41821601274,12.));
#155785=CARTESIAN_POINT('Ctrl Pts',(-28.8969677427519,64.3973870129201,
0.));
#155786=CARTESIAN_POINT('Ctrl Pts',(-28.8969677427519,64.3973870129201,
12.));
#155787=CARTESIAN_POINT('Ctrl Pts',(-28.8941799332312,64.3766105280715,
0.));
#155788=CARTESIAN_POINT('Ctrl Pts',(-28.8941799332312,64.3766105280715,
12.));
#155789=CARTESIAN_POINT('Ctrl Pts',(-28.8913771459327,64.3558867114087,
0.));
#155790=CARTESIAN_POINT('Ctrl Pts',(-28.8913771459327,64.3558867114087,
12.));
#155791=CARTESIAN_POINT('Ctrl Pts',(-28.888559482892,64.3352157174606,0.));
#155792=CARTESIAN_POINT('Ctrl Pts',(-28.888559482892,64.3352157174606,12.));
#155793=CARTESIAN_POINT('Ctrl Pts',(-28.8857270473944,64.3145977025005,
0.));
#155794=CARTESIAN_POINT('Ctrl Pts',(-28.8857270473944,64.3145977025005,
12.));
#155795=CARTESIAN_POINT('Ctrl Pts',(-28.8828799437922,64.2940328242482,
0.));
#155796=CARTESIAN_POINT('Ctrl Pts',(-28.8828799437922,64.2940328242482,
12.));
#155797=CARTESIAN_POINT('Ctrl Pts',(-28.8800182770052,64.2735212410682,
0.));
#155798=CARTESIAN_POINT('Ctrl Pts',(-28.8800182770052,64.2735212410682,
12.));
#155799=CARTESIAN_POINT('Ctrl Pts',(-28.8771421521058,64.2530631112926,
0.));
#155800=CARTESIAN_POINT('Ctrl Pts',(-28.8771421521058,64.2530631112926,
12.));
#155801=CARTESIAN_POINT('Ctrl Pts',(-28.8742516738959,64.232658592528,0.));
#155802=CARTESIAN_POINT('Ctrl Pts',(-28.8742516738959,64.232658592528,12.));
#155803=CARTESIAN_POINT('Ctrl Pts',(-28.8713469464205,64.2123078408507,
0.));
#155804=CARTESIAN_POINT('Ctrl Pts',(-28.8713469464205,64.2123078408507,
12.));
#155805=CARTESIAN_POINT('Ctrl Pts',(-28.8684280739033,64.1920110123342,
0.));
#155806=CARTESIAN_POINT('Ctrl Pts',(-28.8684280739033,64.1920110123342,
12.));
#155807=CARTESIAN_POINT('Ctrl Pts',(-28.8654951618659,64.1717682648708,
0.));
#155808=CARTESIAN_POINT('Ctrl Pts',(-28.8654951618659,64.1717682648708,
12.));
#155809=CARTESIAN_POINT('Ctrl Pts',(-28.8625483180433,64.1515797596555,
0.));
#155810=CARTESIAN_POINT('Ctrl Pts',(-28.8625483180433,64.1515797596555,
12.));
#155811=CARTESIAN_POINT('Ctrl Pts',(-28.8595876537132,64.1314456633345,
0.));
#155812=CARTESIAN_POINT('Ctrl Pts',(-28.8595876537132,64.1314456633345,
12.));
#155813=CARTESIAN_POINT('Ctrl Pts',(-28.8566132838157,64.1113661481918,
0.));
#155814=CARTESIAN_POINT('Ctrl Pts',(-28.8566132838157,64.1113661481918,
12.));
#155815=CARTESIAN_POINT('Ctrl Pts',(-28.8536253241837,64.0913413876586,
0.));
#155816=CARTESIAN_POINT('Ctrl Pts',(-28.8536253241837,64.0913413876586,
12.));
#155817=CARTESIAN_POINT('Ctrl Pts',(-28.8506238891087,64.0713715523588,
0.));
#155818=CARTESIAN_POINT('Ctrl Pts',(-28.8506238891087,64.0713715523588,
12.));
#155819=CARTESIAN_POINT('Ctrl Pts',(-28.8476090892242,64.0514568066659,
0.));
#155820=CARTESIAN_POINT('Ctrl Pts',(-28.8476090892242,64.0514568066659,
12.));
#155821=CARTESIAN_POINT('Ctrl Pts',(-28.8445810281275,64.0315973031994,
0.));
#155822=CARTESIAN_POINT('Ctrl Pts',(-28.8445810281275,64.0315973031994,
12.));
#155823=CARTESIAN_POINT('Ctrl Pts',(-28.841539805646,64.0117931881364,0.));
#155824=CARTESIAN_POINT('Ctrl Pts',(-28.841539805646,64.0117931881364,12.));
#155825=CARTESIAN_POINT('Ctrl Pts',(-28.8384855243267,63.9920446117632,
0.));
#155826=CARTESIAN_POINT('Ctrl Pts',(-28.8384855243267,63.9920446117632,
12.));
#155827=CARTESIAN_POINT('Ctrl Pts',(-28.8354182946601,63.9723517369614,
0.));
#155828=CARTESIAN_POINT('Ctrl Pts',(-28.8354182946601,63.9723517369614,
12.));
#155829=CARTESIAN_POINT('Ctrl Pts',(-28.8323382413753,63.9527147494351,
0.));
#155830=CARTESIAN_POINT('Ctrl Pts',(-28.8323382413753,63.9527147494351,
12.));
#155831=CARTESIAN_POINT('Ctrl Pts',(-28.8292455077494,63.9331338646868,
0.));
#155832=CARTESIAN_POINT('Ctrl Pts',(-28.8292455077494,63.9331338646868,
12.));
#155833=CARTESIAN_POINT('Ctrl Pts',(-28.826140242322,63.9136093063647,0.));
#155834=CARTESIAN_POINT('Ctrl Pts',(-28.826140242322,63.9136093063647,12.));
#155835=CARTESIAN_POINT('Ctrl Pts',(-28.8230225863142,63.894141285685,0.));
#155836=CARTESIAN_POINT('Ctrl Pts',(-28.8230225863142,63.894141285685,12.));
#155837=CARTESIAN_POINT('Ctrl Pts',(-28.8198926619893,63.8747299825383,
0.));
#155838=CARTESIAN_POINT('Ctrl Pts',(-28.8198926619893,63.8747299825383,
12.));
#155839=CARTESIAN_POINT('Ctrl Pts',(-28.8167505576806,63.8553755207732,
0.));
#155840=CARTESIAN_POINT('Ctrl Pts',(-28.8167505576806,63.8553755207732,
12.));
#155841=CARTESIAN_POINT('Ctrl Pts',(-28.8135963263557,63.8360779670225,
0.));
#155842=CARTESIAN_POINT('Ctrl Pts',(-28.8135963263557,63.8360779670225,
12.));
#155843=CARTESIAN_POINT('Ctrl Pts',(-28.8110632621133,63.8206854735372,
0.));
#155844=CARTESIAN_POINT('Ctrl Pts',(-28.8110632621133,63.8206854735372,
12.));
#155845=CARTESIAN_POINT('Ctrl Pts',(-28.8091580239664,63.809166727145,0.));
#155846=CARTESIAN_POINT('Ctrl Pts',(-28.8091580239664,63.809166727145,12.));
#155847=CARTESIAN_POINT('Ctrl Pts',(-28.8078854475473,63.8014989507575,
0.));
#155848=CARTESIAN_POINT('Ctrl Pts',(-28.8078854475473,63.8014989507575,
12.));
#155849=CARTESIAN_POINT('Ctrl Pts',(-28.8072485549236,63.7976679095314,
0.));
#155850=CARTESIAN_POINT('Ctrl Pts',(-28.8072485549236,63.7976679095314,
12.));
#155851=CARTESIAN_POINT('',(-28.8072485549236,63.7976679095314,12.));
#155852=CARTESIAN_POINT('Ctrl Pts',(-28.8072485549236,63.7976679095314,
12.));
#155853=CARTESIAN_POINT('Ctrl Pts',(-28.8078854475473,63.8014989507575,
12.));
#155854=CARTESIAN_POINT('Ctrl Pts',(-28.8091580239664,63.809166727145,12.));
#155855=CARTESIAN_POINT('Ctrl Pts',(-28.8110632621133,63.8206854735372,
12.));
#155856=CARTESIAN_POINT('Ctrl Pts',(-28.8135963263557,63.8360779670225,
12.));
#155857=CARTESIAN_POINT('Ctrl Pts',(-28.8167505576806,63.8553755207732,
12.));
#155858=CARTESIAN_POINT('Ctrl Pts',(-28.8198926619893,63.8747299825383,
12.));
#155859=CARTESIAN_POINT('Ctrl Pts',(-28.8230225863142,63.894141285685,12.));
#155860=CARTESIAN_POINT('Ctrl Pts',(-28.826140242322,63.9136093063647,12.));
#155861=CARTESIAN_POINT('Ctrl Pts',(-28.8292455077494,63.9331338646868,
12.));
#155862=CARTESIAN_POINT('Ctrl Pts',(-28.8323382413753,63.9527147494351,
12.));
#155863=CARTESIAN_POINT('Ctrl Pts',(-28.8354182946601,63.9723517369614,
12.));
#155864=CARTESIAN_POINT('Ctrl Pts',(-28.8384855243267,63.9920446117632,
12.));
#155865=CARTESIAN_POINT('Ctrl Pts',(-28.841539805646,64.0117931881364,12.));
#155866=CARTESIAN_POINT('Ctrl Pts',(-28.8445810281275,64.0315973031994,
12.));
#155867=CARTESIAN_POINT('Ctrl Pts',(-28.8476090892242,64.0514568066659,
12.));
#155868=CARTESIAN_POINT('Ctrl Pts',(-28.8506238891087,64.0713715523588,
12.));
#155869=CARTESIAN_POINT('Ctrl Pts',(-28.8536253241837,64.0913413876586,
12.));
#155870=CARTESIAN_POINT('Ctrl Pts',(-28.8566132838157,64.1113661481918,
12.));
#155871=CARTESIAN_POINT('Ctrl Pts',(-28.8595876537132,64.1314456633345,
12.));
#155872=CARTESIAN_POINT('Ctrl Pts',(-28.8625483180433,64.1515797596555,
12.));
#155873=CARTESIAN_POINT('Ctrl Pts',(-28.8654951618659,64.1717682648708,
12.));
#155874=CARTESIAN_POINT('Ctrl Pts',(-28.8684280739033,64.1920110123342,
12.));
#155875=CARTESIAN_POINT('Ctrl Pts',(-28.8713469464205,64.2123078408507,
12.));
#155876=CARTESIAN_POINT('Ctrl Pts',(-28.8742516738959,64.232658592528,12.));
#155877=CARTESIAN_POINT('Ctrl Pts',(-28.8771421521058,64.2530631112926,
12.));
#155878=CARTESIAN_POINT('Ctrl Pts',(-28.8800182770052,64.2735212410682,
12.));
#155879=CARTESIAN_POINT('Ctrl Pts',(-28.8828799437922,64.2940328242482,
12.));
#155880=CARTESIAN_POINT('Ctrl Pts',(-28.8857270473944,64.3145977025005,
12.));
#155881=CARTESIAN_POINT('Ctrl Pts',(-28.888559482892,64.3352157174606,12.));
#155882=CARTESIAN_POINT('Ctrl Pts',(-28.8913771459327,64.3558867114087,
12.));
#155883=CARTESIAN_POINT('Ctrl Pts',(-28.8941799332312,64.3766105280715,
12.));
#155884=CARTESIAN_POINT('Ctrl Pts',(-28.8969677427519,64.3973870129201,
12.));
#155885=CARTESIAN_POINT('Ctrl Pts',(-28.899740473435,64.41821601274,12.));
#155886=CARTESIAN_POINT('Ctrl Pts',(-28.9024980250309,64.439097375364,12.));
#155887=CARTESIAN_POINT('Ctrl Pts',(-28.9052402979055,64.460030949357,12.));
#155888=CARTESIAN_POINT('Ctrl Pts',(-28.9079671928253,64.4810165836568,
12.));
#155889=CARTESIAN_POINT('Ctrl Pts',(-28.9106786109639,64.5020541275927,
12.));
#155890=CARTESIAN_POINT('Ctrl Pts',(-28.9133744539943,64.5231434310457,
12.));
#155891=CARTESIAN_POINT('Ctrl Pts',(-28.9160546241538,64.544284344556,12.));
#155892=CARTESIAN_POINT('Ctrl Pts',(-28.9187190243231,64.5654767194487,
12.));
#155893=CARTESIAN_POINT('Ctrl Pts',(-28.9213675580996,64.5867204079452,
12.));
#155894=CARTESIAN_POINT('Ctrl Pts',(-28.9240001297553,64.6080152631065,
12.));
#155895=CARTESIAN_POINT('Ctrl Pts',(-28.9266166441956,64.6293611387753,
12.));
#155896=CARTESIAN_POINT('Ctrl Pts',(-28.9292170069219,64.6507578895155,
12.));
#155897=CARTESIAN_POINT('Ctrl Pts',(-28.9318011239905,64.6722053705389,
12.));
#155898=CARTESIAN_POINT('Ctrl Pts',(-28.934368901987,64.6937034376591,12.));
#155899=CARTESIAN_POINT('Ctrl Pts',(-28.9369202480383,64.715251947327,12.));
#155900=CARTESIAN_POINT('Ctrl Pts',(-28.9394550698201,64.7368507566461,
12.));
#155901=CARTESIAN_POINT('Ctrl Pts',(-28.9419732755659,64.7584997233889,
12.));
#155902=CARTESIAN_POINT('Ctrl Pts',(-28.9444747740815,64.7801987060097,
12.));
#155903=CARTESIAN_POINT('Ctrl Pts',(-28.9469594747436,64.8019475636454,
12.));
#155904=CARTESIAN_POINT('Ctrl Pts',(-28.9494272874833,64.8237461561024,
12.));
#155905=CARTESIAN_POINT('Ctrl Pts',(-28.9518781227765,64.8455943438423,
12.));
#155906=CARTESIAN_POINT('Ctrl Pts',(-28.9543118916327,64.8674919879646,
12.));
#155907=CARTESIAN_POINT('Ctrl Pts',(-28.9567285055866,64.8894389501799,
12.));
#155908=CARTESIAN_POINT('Ctrl Pts',(-28.9591278766934,64.9114350928124,
12.));
#155909=CARTESIAN_POINT('Ctrl Pts',(-28.961509917525,64.9334802788037,12.));
#155910=CARTESIAN_POINT('Ctrl Pts',(-28.9638745411677,64.955574371711,12.));
#155911=CARTESIAN_POINT('Ctrl Pts',(-28.9662216612216,64.9777172357028,
12.));
#155912=CARTESIAN_POINT('Ctrl Pts',(-28.9685511918017,64.9999087355504,
12.));
#155913=CARTESIAN_POINT('Ctrl Pts',(-28.9708630475298,65.0221487366279,
12.));
#155914=CARTESIAN_POINT('Ctrl Pts',(-28.9731571435281,65.0444371049082,
12.));
#155915=CARTESIAN_POINT('Ctrl Pts',(-28.9754333954134,65.0667737069562,
12.));
#155916=CARTESIAN_POINT('Ctrl Pts',(-28.9776917192936,65.0891584099174,
12.));
#155917=CARTESIAN_POINT('Ctrl Pts',(-28.9799320317648,65.111591081505,12.));
#155918=CARTESIAN_POINT('Ctrl Pts',(-28.9821542499049,65.1340715900042,
12.));
#155919=CARTESIAN_POINT('Ctrl Pts',(-28.9843582912697,65.1565998042705,
12.));
#155920=CARTESIAN_POINT('Ctrl Pts',(-28.9865440738882,65.1791755937254,
12.));
#155921=CARTESIAN_POINT('Ctrl Pts',(-28.9887115162626,65.2017988283465,
12.));
#155922=CARTESIAN_POINT('Ctrl Pts',(-28.9908605373652,65.2244693786586,
12.));
#155923=CARTESIAN_POINT('Ctrl Pts',(-28.9929910566314,65.2471871157375,
12.));
#155924=CARTESIAN_POINT('Ctrl Pts',(-28.9951029939551,65.2699519112052,
12.));
#155925=CARTESIAN_POINT('Ctrl Pts',(-28.9971962696848,65.2927636372261,
12.));
#155926=CARTESIAN_POINT('Ctrl Pts',(-28.9992708046223,65.3156221664942,
12.));
#155927=CARTESIAN_POINT('Ctrl Pts',(-29.0013265200201,65.3385273722278,
12.));
#155928=CARTESIAN_POINT('Ctrl Pts',(-29.0033633375745,65.3614791281725,
12.));
#155929=CARTESIAN_POINT('Ctrl Pts',(-29.0053811794214,65.3844773085976,
12.));
#155930=CARTESIAN_POINT('Ctrl Pts',(-29.0073799681336,65.4075217882921,
12.));
#155931=CARTESIAN_POINT('Ctrl Pts',(-29.0093596267198,65.4306124425524,
12.));
#155932=CARTESIAN_POINT('Ctrl Pts',(-29.0113200786219,65.4537491471782,
12.));
#155933=CARTESIAN_POINT('Ctrl Pts',(-29.0132612477075,65.4769317784754,
12.));
#155934=CARTESIAN_POINT('Ctrl Pts',(-29.015183058267,65.5001602132524,12.));
#155935=CARTESIAN_POINT('Ctrl Pts',(-29.01708543501,65.523434328815,12.));
#155936=CARTESIAN_POINT('Ctrl Pts',(-29.0189683030654,65.5467540029546,
12.));
#155937=CARTESIAN_POINT('Ctrl Pts',(-29.0208315879778,65.5701191139455,
12.));
#155938=CARTESIAN_POINT('Ctrl Pts',(-29.0226752157013,65.593529540548,12.));
#155939=CARTESIAN_POINT('Ctrl Pts',(-29.0244991125962,65.6169851620054,
12.));
#155940=CARTESIAN_POINT('Ctrl Pts',(-29.0263032054261,65.6404858580391,
12.));
#155941=CARTESIAN_POINT('Ctrl Pts',(-29.0280874213584,65.664031508836,12.));
#155942=CARTESIAN_POINT('Ctrl Pts',(-29.0298516879599,65.6876219950465,
12.));
#155943=CARTESIAN_POINT('Ctrl Pts',(-29.0315959331911,65.7112571977874,
12.));
#155944=CARTESIAN_POINT('Ctrl Pts',(-29.0333200854026,65.7349369986382,
12.));
#155945=CARTESIAN_POINT('Ctrl Pts',(-29.0350240733333,65.7586612796375,
12.));
#155946=CARTESIAN_POINT('Ctrl Pts',(-29.0367078261107,65.7824299232715,
12.));
#155947=CARTESIAN_POINT('Ctrl Pts',(-29.0383712732473,65.8062428124723,
12.));
#155948=CARTESIAN_POINT('Ctrl Pts',(-29.0400143446341,65.8300998306198,
12.));
#155949=CARTESIAN_POINT('Ctrl Pts',(-29.0416369705375,65.854000861539,12.));
#155950=CARTESIAN_POINT('Ctrl Pts',(-29.0432390815977,65.8779457894959,
12.));
#155951=CARTESIAN_POINT('Ctrl Pts',(-29.0448206088288,65.9019344991854,
12.));
#155952=CARTESIAN_POINT('Ctrl Pts',(-29.0463814836159,65.9259668757309,
12.));
#155953=CARTESIAN_POINT('Ctrl Pts',(-29.0479216377082,65.9500428046873,
12.));
#155954=CARTESIAN_POINT('Ctrl Pts',(-29.0494410032173,65.9741621720372,
12.));
#155955=CARTESIAN_POINT('Ctrl Pts',(-29.0509395126141,65.9983248641877,
12.));
#155956=CARTESIAN_POINT('Ctrl Pts',(-29.0524170987303,66.0225307679584,
12.));
#155957=CARTESIAN_POINT('Ctrl Pts',(-29.0538736947547,66.0467797705806,
12.));
#155958=CARTESIAN_POINT('Ctrl Pts',(-29.0553092342275,66.0710717597003,
12.));
#155959=CARTESIAN_POINT('Ctrl Pts',(-29.0567236510372,66.0954066233752,
12.));
#155960=CARTESIAN_POINT('Ctrl Pts',(-29.0581168794191,66.1197842500714,
12.));
#155961=CARTESIAN_POINT('Ctrl Pts',(-29.0594888539558,66.144204528652,12.));
#155962=CARTESIAN_POINT('Ctrl Pts',(-29.0608395095747,66.1686673483757,
12.));
#155963=CARTESIAN_POINT('Ctrl Pts',(-29.062168781542,66.1931725989008,12.));
#155964=CARTESIAN_POINT('Ctrl Pts',(-29.0634766054598,66.2177201702818,
12.));
#155965=CARTESIAN_POINT('Ctrl Pts',(-29.0647629172645,66.2423099529669,
12.));
#155966=CARTESIAN_POINT('Ctrl Pts',(-29.0660276532274,66.2669418377871,
12.));
#155967=CARTESIAN_POINT('Ctrl Pts',(-29.067270749953,66.2916157159536,12.));
#155968=CARTESIAN_POINT('Ctrl Pts',(-29.0684921443721,66.3163314790615,
12.));
#155969=CARTESIAN_POINT('Ctrl Pts',(-29.0696917737399,66.3410890190884,
12.));
#155970=CARTESIAN_POINT('Ctrl Pts',(-29.0708695756334,66.3658882283903,
12.));
#155971=CARTESIAN_POINT('Ctrl Pts',(-29.072025487953,66.3907289996932,12.));
#155972=CARTESIAN_POINT('Ctrl Pts',(-29.0731594489211,66.4156112260887,
12.));
#155973=CARTESIAN_POINT('Ctrl Pts',(-29.0742713970755,66.4405348010388,
12.));
#155974=CARTESIAN_POINT('Ctrl Pts',(-29.0753612712666,66.4654996183731,
12.));
#155975=CARTESIAN_POINT('Ctrl Pts',(-29.0764290106554,66.4905055722868,
12.));
#155976=CARTESIAN_POINT('Ctrl Pts',(-29.0774745547152,66.5155525573323,
12.));
#155977=CARTESIAN_POINT('Ctrl Pts',(-29.0784978432301,66.5406404684132,
12.));
#155978=CARTESIAN_POINT('Ctrl Pts',(-29.0794988162897,66.5657692007906,
12.));
#155979=CARTESIAN_POINT('Ctrl Pts',(-29.0804774142854,66.59093865008,12.));
#155980=CARTESIAN_POINT('Ctrl Pts',(-29.0814335779084,66.6161487122502,
12.));
#155981=CARTESIAN_POINT('Ctrl Pts',(-29.0823672481507,66.6413992836147,
12.));
#155982=CARTESIAN_POINT('Ctrl Pts',(-29.083278366305,66.6666902608249,12.));
#155983=CARTESIAN_POINT('Ctrl Pts',(-29.0841668739588,66.6920215408751,
12.));
#155984=CARTESIAN_POINT('Ctrl Pts',(-29.0850327129916,66.7173930211022,
12.));
#155985=CARTESIAN_POINT('Ctrl Pts',(-29.0858758255729,66.7428045991841,
12.));
#155986=CARTESIAN_POINT('Ctrl Pts',(-29.0866961541626,66.7682561731341,
12.));
#155987=CARTESIAN_POINT('Ctrl Pts',(-29.0874936415132,66.793747641293,12.));
#155988=CARTESIAN_POINT('Ctrl Pts',(-29.088268230663,66.8192789023312,12.));
#155989=CARTESIAN_POINT('Ctrl Pts',(-29.0890198649323,66.8448498552503,
12.));
#155990=CARTESIAN_POINT('Ctrl Pts',(-29.0897484879207,66.8704603993794,
12.));
#155991=CARTESIAN_POINT('Ctrl Pts',(-29.0904540435065,66.8961104343707,
12.));
#155992=CARTESIAN_POINT('Ctrl Pts',(-29.0911364758487,66.9217998601885,
12.));
#155993=CARTESIAN_POINT('Ctrl Pts',(-29.0917957293826,66.9475285771135,
12.));
#155994=CARTESIAN_POINT('Ctrl Pts',(-29.092431748817,66.9732964857466,12.));
#155995=CARTESIAN_POINT('Ctrl Pts',(-29.0930444791328,66.9991034870083,
12.));
#155996=CARTESIAN_POINT('Ctrl Pts',(-29.0936338655828,67.0249494821363,
12.));
#155997=CARTESIAN_POINT('Ctrl Pts',(-29.0941998536959,67.0508343726776,
12.));
#155998=CARTESIAN_POINT('Ctrl Pts',(-29.0947423892727,67.0767580604879,
12.));
#155999=CARTESIAN_POINT('Ctrl Pts',(-29.0952614183779,67.1027204477311,
12.));
#156000=CARTESIAN_POINT('Ctrl Pts',(-29.0957568873358,67.1287214368746,
12.));
#156001=CARTESIAN_POINT('Ctrl Pts',(-29.0962287427273,67.1547609306843,
12.));
#156002=CARTESIAN_POINT('Ctrl Pts',(-29.096676931389,67.1808388322109,12.));
#156003=CARTESIAN_POINT('Ctrl Pts',(-29.0971014004131,67.2069550447883,
12.));
#156004=CARTESIAN_POINT('Ctrl Pts',(-29.097502097147,67.2331094720471,12.));
#156005=CARTESIAN_POINT('Ctrl Pts',(-29.0978789691962,67.2593020179209,
12.));
#156006=CARTESIAN_POINT('Ctrl Pts',(-29.0982319644277,67.2855325866517,
12.));
#156007=CARTESIAN_POINT('Ctrl Pts',(-29.0985610309771,67.311801082792,12.));
#156008=CARTESIAN_POINT('Ctrl Pts',(-29.0988661172531,67.3381074112027,
12.));
#156009=CARTESIAN_POINT('Ctrl Pts',(-29.0991471719176,67.3644514770387,
12.));
#156010=CARTESIAN_POINT('Ctrl Pts',(-29.0994041438719,67.3908331857323,
12.));
#156011=CARTESIAN_POINT('Ctrl Pts',(-29.0996369822418,67.4172524429727,
12.));
#156012=CARTESIAN_POINT('Ctrl Pts',(-29.0998456363683,67.4437091546859,
12.));
#156013=CARTESIAN_POINT('Ctrl Pts',(-29.1000300557955,67.4702032270048,
12.));
#156014=CARTESIAN_POINT('Ctrl Pts',(-29.1001901902909,67.4967345663096,
12.));
#156015=CARTESIAN_POINT('Ctrl Pts',(-29.1003259898682,67.5233030792704,
12.));
#156016=CARTESIAN_POINT('Ctrl Pts',(-29.1004374048148,67.5499086728888,
12.));
#156017=CARTESIAN_POINT('Ctrl Pts',(-29.1005243857139,67.5765512545281,
12.));
#156018=CARTESIAN_POINT('Ctrl Pts',(-29.1005868834866,67.6032307319623,
12.));
#156019=CARTESIAN_POINT('Ctrl Pts',(-29.100624849358,67.6299470133295,12.));
#156020=CARTESIAN_POINT('Ctrl Pts',(-29.1006382347814,67.6567000070326,
12.));
#156021=CARTESIAN_POINT('Ctrl Pts',(-29.1006269913747,67.6834896216461,
12.));
#156022=CARTESIAN_POINT('Ctrl Pts',(-29.1005910708624,67.7103157658296,
12.));
#156023=CARTESIAN_POINT('Ctrl Pts',(-29.1005304249987,67.7371783482035,
12.));
#156024=CARTESIAN_POINT('Ctrl Pts',(-29.1004450055643,67.7640772773387,
12.));
#156025=CARTESIAN_POINT('Ctrl Pts',(-29.1003347645294,67.7910124620135,
12.));
#156026=CARTESIAN_POINT('Ctrl Pts',(-29.1001996541842,67.8179838114099,
12.));
#156027=CARTESIAN_POINT('Ctrl Pts',(-29.1000396272867,67.8449912353329,
12.));
#156028=CARTESIAN_POINT('Ctrl Pts',(-29.0998546372032,67.8720346444124,
12.));
#156029=CARTESIAN_POINT('Ctrl Pts',(-29.0996446380626,67.8991139503193,
12.));
#156030=CARTESIAN_POINT('Ctrl Pts',(-29.099409584422,67.9262290652829,12.));
#156031=CARTESIAN_POINT('Ctrl Pts',(-29.0991494309404,67.9533799016148,
12.));
#156032=CARTESIAN_POINT('Ctrl Pts',(-29.0988641320247,67.9805663711855,
12.));
#156033=CARTESIAN_POINT('Ctrl Pts',(-29.0985536415531,68.0077883850121,
12.));
#156034=CARTESIAN_POINT('Ctrl Pts',(-29.0982179124097,68.0350458525551,
12.));
#156035=CARTESIAN_POINT('Ctrl Pts',(-29.0978568968657,68.0623386822863,
12.));
#156036=CARTESIAN_POINT('Ctrl Pts',(-29.0974705474259,68.0896667829567,
12.));
#156037=CARTESIAN_POINT('Ctrl Pts',(-29.0970588175728,68.1170300646987,
12.));
#156038=CARTESIAN_POINT('Ctrl Pts',(-29.0966216624743,68.1444284400742,
12.));
#156039=CARTESIAN_POINT('Ctrl Pts',(-29.0961590399046,68.1718618254281,
12.));
#156040=CARTESIAN_POINT('Ctrl Pts',(-29.0956709104627,68.1993301412061,
12.));
#156041=CARTESIAN_POINT('Ctrl Pts',(-29.095230591515,68.2229056854683,12.));
#156042=CARTESIAN_POINT('Ctrl Pts',(-29.094879194787,68.2409993690197,12.));
#156043=CARTESIAN_POINT('Ctrl Pts',(-29.0946280433337,68.2535957747187,
12.));
#156044=CARTESIAN_POINT('Ctrl Pts',(-29.0944846386568,68.2606847334987,
12.));
#156045=CARTESIAN_POINT('Ctrl Pts',(-29.0944526440266,68.2622612910177,
12.));
#156046=CARTESIAN_POINT('',(-28.8072485549236,63.7976679095314,0.));
#156047=CARTESIAN_POINT('',(-28.8072485549236,63.7976679095314,0.));
#156048=CARTESIAN_POINT('Ctrl Pts',(-29.0944526440266,68.2622612910177,
0.));
#156049=CARTESIAN_POINT('Ctrl Pts',(-29.0944846386568,68.2606847334987,
0.));
#156050=CARTESIAN_POINT('Ctrl Pts',(-29.0946280433337,68.2535957747187,
0.));
#156051=CARTESIAN_POINT('Ctrl Pts',(-29.094879194787,68.2409993690197,0.));
#156052=CARTESIAN_POINT('Ctrl Pts',(-29.095230591515,68.2229056854683,0.));
#156053=CARTESIAN_POINT('Ctrl Pts',(-29.0956709104627,68.1993301412061,
0.));
#156054=CARTESIAN_POINT('Ctrl Pts',(-29.0961590399046,68.1718618254281,
0.));
#156055=CARTESIAN_POINT('Ctrl Pts',(-29.0966216624743,68.1444284400742,
0.));
#156056=CARTESIAN_POINT('Ctrl Pts',(-29.0970588175728,68.1170300646987,
0.));
#156057=CARTESIAN_POINT('Ctrl Pts',(-29.0974705474259,68.0896667829567,
0.));
#156058=CARTESIAN_POINT('Ctrl Pts',(-29.0978568968657,68.0623386822863,
0.));
#156059=CARTESIAN_POINT('Ctrl Pts',(-29.0982179124097,68.0350458525551,
0.));
#156060=CARTESIAN_POINT('Ctrl Pts',(-29.0985536415531,68.0077883850121,
0.));
#156061=CARTESIAN_POINT('Ctrl Pts',(-29.0988641320247,67.9805663711855,
0.));
#156062=CARTESIAN_POINT('Ctrl Pts',(-29.0991494309404,67.9533799016148,
0.));
#156063=CARTESIAN_POINT('Ctrl Pts',(-29.099409584422,67.9262290652829,0.));
#156064=CARTESIAN_POINT('Ctrl Pts',(-29.0996446380626,67.8991139503193,
0.));
#156065=CARTESIAN_POINT('Ctrl Pts',(-29.0998546372032,67.8720346444124,
0.));
#156066=CARTESIAN_POINT('Ctrl Pts',(-29.1000396272867,67.8449912353329,
0.));
#156067=CARTESIAN_POINT('Ctrl Pts',(-29.1001996541842,67.8179838114099,
0.));
#156068=CARTESIAN_POINT('Ctrl Pts',(-29.1003347645294,67.7910124620135,
0.));
#156069=CARTESIAN_POINT('Ctrl Pts',(-29.1004450055643,67.7640772773387,
0.));
#156070=CARTESIAN_POINT('Ctrl Pts',(-29.1005304249987,67.7371783482035,
0.));
#156071=CARTESIAN_POINT('Ctrl Pts',(-29.1005910708624,67.7103157658296,
0.));
#156072=CARTESIAN_POINT('Ctrl Pts',(-29.1006269913747,67.6834896216461,
0.));
#156073=CARTESIAN_POINT('Ctrl Pts',(-29.1006382347814,67.6567000070326,
0.));
#156074=CARTESIAN_POINT('Ctrl Pts',(-29.100624849358,67.6299470133295,0.));
#156075=CARTESIAN_POINT('Ctrl Pts',(-29.1005868834866,67.6032307319623,
0.));
#156076=CARTESIAN_POINT('Ctrl Pts',(-29.1005243857139,67.5765512545281,
0.));
#156077=CARTESIAN_POINT('Ctrl Pts',(-29.1004374048148,67.5499086728888,
0.));
#156078=CARTESIAN_POINT('Ctrl Pts',(-29.1003259898682,67.5233030792704,
0.));
#156079=CARTESIAN_POINT('Ctrl Pts',(-29.1001901902909,67.4967345663096,
0.));
#156080=CARTESIAN_POINT('Ctrl Pts',(-29.1000300557955,67.4702032270048,
0.));
#156081=CARTESIAN_POINT('Ctrl Pts',(-29.0998456363683,67.4437091546859,
0.));
#156082=CARTESIAN_POINT('Ctrl Pts',(-29.0996369822418,67.4172524429727,
0.));
#156083=CARTESIAN_POINT('Ctrl Pts',(-29.0994041438719,67.3908331857323,
0.));
#156084=CARTESIAN_POINT('Ctrl Pts',(-29.0991471719176,67.3644514770387,
0.));
#156085=CARTESIAN_POINT('Ctrl Pts',(-29.0988661172531,67.3381074112027,
0.));
#156086=CARTESIAN_POINT('Ctrl Pts',(-29.0985610309771,67.311801082792,0.));
#156087=CARTESIAN_POINT('Ctrl Pts',(-29.0982319644277,67.2855325866517,
0.));
#156088=CARTESIAN_POINT('Ctrl Pts',(-29.0978789691962,67.2593020179209,
0.));
#156089=CARTESIAN_POINT('Ctrl Pts',(-29.097502097147,67.2331094720471,0.));
#156090=CARTESIAN_POINT('Ctrl Pts',(-29.0971014004131,67.2069550447883,
0.));
#156091=CARTESIAN_POINT('Ctrl Pts',(-29.096676931389,67.1808388322109,0.));
#156092=CARTESIAN_POINT('Ctrl Pts',(-29.0962287427273,67.1547609306843,
0.));
#156093=CARTESIAN_POINT('Ctrl Pts',(-29.0957568873358,67.1287214368746,
0.));
#156094=CARTESIAN_POINT('Ctrl Pts',(-29.0952614183779,67.1027204477311,
0.));
#156095=CARTESIAN_POINT('Ctrl Pts',(-29.0947423892727,67.0767580604879,
0.));
#156096=CARTESIAN_POINT('Ctrl Pts',(-29.0941998536959,67.0508343726776,
0.));
#156097=CARTESIAN_POINT('Ctrl Pts',(-29.0936338655828,67.0249494821363,
0.));
#156098=CARTESIAN_POINT('Ctrl Pts',(-29.0930444791328,66.9991034870083,
0.));
#156099=CARTESIAN_POINT('Ctrl Pts',(-29.092431748817,66.9732964857466,0.));
#156100=CARTESIAN_POINT('Ctrl Pts',(-29.0917957293826,66.9475285771135,
0.));
#156101=CARTESIAN_POINT('Ctrl Pts',(-29.0911364758487,66.9217998601885,
0.));
#156102=CARTESIAN_POINT('Ctrl Pts',(-29.0904540435065,66.8961104343707,
0.));
#156103=CARTESIAN_POINT('Ctrl Pts',(-29.0897484879207,66.8704603993794,
0.));
#156104=CARTESIAN_POINT('Ctrl Pts',(-29.0890198649323,66.8448498552503,
0.));
#156105=CARTESIAN_POINT('Ctrl Pts',(-29.088268230663,66.8192789023312,0.));
#156106=CARTESIAN_POINT('Ctrl Pts',(-29.0874936415132,66.793747641293,0.));
#156107=CARTESIAN_POINT('Ctrl Pts',(-29.0866961541626,66.7682561731341,
0.));
#156108=CARTESIAN_POINT('Ctrl Pts',(-29.0858758255729,66.7428045991841,
0.));
#156109=CARTESIAN_POINT('Ctrl Pts',(-29.0850327129916,66.7173930211022,
0.));
#156110=CARTESIAN_POINT('Ctrl Pts',(-29.0841668739588,66.6920215408751,
0.));
#156111=CARTESIAN_POINT('Ctrl Pts',(-29.083278366305,66.6666902608249,0.));
#156112=CARTESIAN_POINT('Ctrl Pts',(-29.0823672481507,66.6413992836147,
0.));
#156113=CARTESIAN_POINT('Ctrl Pts',(-29.0814335779084,66.6161487122502,
0.));
#156114=CARTESIAN_POINT('Ctrl Pts',(-29.0804774142854,66.59093865008,0.));
#156115=CARTESIAN_POINT('Ctrl Pts',(-29.0794988162897,66.5657692007906,
0.));
#156116=CARTESIAN_POINT('Ctrl Pts',(-29.0784978432301,66.5406404684132,
0.));
#156117=CARTESIAN_POINT('Ctrl Pts',(-29.0774745547152,66.5155525573323,
0.));
#156118=CARTESIAN_POINT('Ctrl Pts',(-29.0764290106554,66.4905055722868,
0.));
#156119=CARTESIAN_POINT('Ctrl Pts',(-29.0753612712666,66.4654996183731,
0.));
#156120=CARTESIAN_POINT('Ctrl Pts',(-29.0742713970755,66.4405348010388,
0.));
#156121=CARTESIAN_POINT('Ctrl Pts',(-29.0731594489211,66.4156112260887,
0.));
#156122=CARTESIAN_POINT('Ctrl Pts',(-29.072025487953,66.3907289996932,0.));
#156123=CARTESIAN_POINT('Ctrl Pts',(-29.0708695756334,66.3658882283903,
0.));
#156124=CARTESIAN_POINT('Ctrl Pts',(-29.0696917737399,66.3410890190884,
0.));
#156125=CARTESIAN_POINT('Ctrl Pts',(-29.0684921443721,66.3163314790615,
0.));
#156126=CARTESIAN_POINT('Ctrl Pts',(-29.067270749953,66.2916157159536,0.));
#156127=CARTESIAN_POINT('Ctrl Pts',(-29.0660276532274,66.2669418377871,
0.));
#156128=CARTESIAN_POINT('Ctrl Pts',(-29.0647629172645,66.2423099529669,
0.));
#156129=CARTESIAN_POINT('Ctrl Pts',(-29.0634766054598,66.2177201702818,
0.));
#156130=CARTESIAN_POINT('Ctrl Pts',(-29.062168781542,66.1931725989008,0.));
#156131=CARTESIAN_POINT('Ctrl Pts',(-29.0608395095747,66.1686673483757,
0.));
#156132=CARTESIAN_POINT('Ctrl Pts',(-29.0594888539558,66.144204528652,0.));
#156133=CARTESIAN_POINT('Ctrl Pts',(-29.0581168794191,66.1197842500714,
0.));
#156134=CARTESIAN_POINT('Ctrl Pts',(-29.0567236510372,66.0954066233752,
0.));
#156135=CARTESIAN_POINT('Ctrl Pts',(-29.0553092342275,66.0710717597003,
0.));
#156136=CARTESIAN_POINT('Ctrl Pts',(-29.0538736947547,66.0467797705806,
0.));
#156137=CARTESIAN_POINT('Ctrl Pts',(-29.0524170987303,66.0225307679584,
0.));
#156138=CARTESIAN_POINT('Ctrl Pts',(-29.0509395126141,65.9983248641877,
0.));
#156139=CARTESIAN_POINT('Ctrl Pts',(-29.0494410032173,65.9741621720372,
0.));
#156140=CARTESIAN_POINT('Ctrl Pts',(-29.0479216377082,65.9500428046873,
0.));
#156141=CARTESIAN_POINT('Ctrl Pts',(-29.0463814836159,65.9259668757309,
0.));
#156142=CARTESIAN_POINT('Ctrl Pts',(-29.0448206088288,65.9019344991854,
0.));
#156143=CARTESIAN_POINT('Ctrl Pts',(-29.0432390815977,65.8779457894959,
0.));
#156144=CARTESIAN_POINT('Ctrl Pts',(-29.0416369705375,65.854000861539,0.));
#156145=CARTESIAN_POINT('Ctrl Pts',(-29.0400143446341,65.8300998306198,
0.));
#156146=CARTESIAN_POINT('Ctrl Pts',(-29.0383712732473,65.8062428124723,
0.));
#156147=CARTESIAN_POINT('Ctrl Pts',(-29.0367078261107,65.7824299232715,
0.));
#156148=CARTESIAN_POINT('Ctrl Pts',(-29.0350240733333,65.7586612796375,
0.));
#156149=CARTESIAN_POINT('Ctrl Pts',(-29.0333200854026,65.7349369986382,
0.));
#156150=CARTESIAN_POINT('Ctrl Pts',(-29.0315959331911,65.7112571977874,
0.));
#156151=CARTESIAN_POINT('Ctrl Pts',(-29.0298516879599,65.6876219950465,
0.));
#156152=CARTESIAN_POINT('Ctrl Pts',(-29.0280874213584,65.664031508836,0.));
#156153=CARTESIAN_POINT('Ctrl Pts',(-29.0263032054261,65.6404858580391,
0.));
#156154=CARTESIAN_POINT('Ctrl Pts',(-29.0244991125962,65.6169851620054,
0.));
#156155=CARTESIAN_POINT('Ctrl Pts',(-29.0226752157013,65.593529540548,0.));
#156156=CARTESIAN_POINT('Ctrl Pts',(-29.0208315879778,65.5701191139455,
0.));
#156157=CARTESIAN_POINT('Ctrl Pts',(-29.0189683030654,65.5467540029546,
0.));
#156158=CARTESIAN_POINT('Ctrl Pts',(-29.01708543501,65.523434328815,0.));
#156159=CARTESIAN_POINT('Ctrl Pts',(-29.015183058267,65.5001602132524,0.));
#156160=CARTESIAN_POINT('Ctrl Pts',(-29.0132612477075,65.4769317784754,
0.));
#156161=CARTESIAN_POINT('Ctrl Pts',(-29.0113200786219,65.4537491471782,
0.));
#156162=CARTESIAN_POINT('Ctrl Pts',(-29.0093596267198,65.4306124425524,
0.));
#156163=CARTESIAN_POINT('Ctrl Pts',(-29.0073799681336,65.4075217882921,
0.));
#156164=CARTESIAN_POINT('Ctrl Pts',(-29.0053811794214,65.3844773085976,
0.));
#156165=CARTESIAN_POINT('Ctrl Pts',(-29.0033633375745,65.3614791281725,
0.));
#156166=CARTESIAN_POINT('Ctrl Pts',(-29.0013265200201,65.3385273722278,
0.));
#156167=CARTESIAN_POINT('Ctrl Pts',(-28.9992708046223,65.3156221664942,
0.));
#156168=CARTESIAN_POINT('Ctrl Pts',(-28.9971962696848,65.2927636372261,
0.));
#156169=CARTESIAN_POINT('Ctrl Pts',(-28.9951029939551,65.2699519112052,
0.));
#156170=CARTESIAN_POINT('Ctrl Pts',(-28.9929910566314,65.2471871157375,
0.));
#156171=CARTESIAN_POINT('Ctrl Pts',(-28.9908605373652,65.2244693786586,
0.));
#156172=CARTESIAN_POINT('Ctrl Pts',(-28.9887115162626,65.2017988283465,
0.));
#156173=CARTESIAN_POINT('Ctrl Pts',(-28.9865440738882,65.1791755937254,
0.));
#156174=CARTESIAN_POINT('Ctrl Pts',(-28.9843582912697,65.1565998042705,
0.));
#156175=CARTESIAN_POINT('Ctrl Pts',(-28.9821542499049,65.1340715900042,
0.));
#156176=CARTESIAN_POINT('Ctrl Pts',(-28.9799320317648,65.111591081505,0.));
#156177=CARTESIAN_POINT('Ctrl Pts',(-28.9776917192936,65.0891584099174,
0.));
#156178=CARTESIAN_POINT('Ctrl Pts',(-28.9754333954134,65.0667737069562,
0.));
#156179=CARTESIAN_POINT('Ctrl Pts',(-28.9731571435281,65.0444371049082,
0.));
#156180=CARTESIAN_POINT('Ctrl Pts',(-28.9708630475298,65.0221487366279,
0.));
#156181=CARTESIAN_POINT('Ctrl Pts',(-28.9685511918017,64.9999087355504,
0.));
#156182=CARTESIAN_POINT('Ctrl Pts',(-28.9662216612216,64.9777172357028,
0.));
#156183=CARTESIAN_POINT('Ctrl Pts',(-28.9638745411677,64.955574371711,0.));
#156184=CARTESIAN_POINT('Ctrl Pts',(-28.961509917525,64.9334802788037,0.));
#156185=CARTESIAN_POINT('Ctrl Pts',(-28.9591278766934,64.9114350928124,
0.));
#156186=CARTESIAN_POINT('Ctrl Pts',(-28.9567285055866,64.8894389501799,
0.));
#156187=CARTESIAN_POINT('Ctrl Pts',(-28.9543118916327,64.8674919879646,
0.));
#156188=CARTESIAN_POINT('Ctrl Pts',(-28.9518781227765,64.8455943438423,
0.));
#156189=CARTESIAN_POINT('Ctrl Pts',(-28.9494272874833,64.8237461561024,
0.));
#156190=CARTESIAN_POINT('Ctrl Pts',(-28.9469594747436,64.8019475636454,
0.));
#156191=CARTESIAN_POINT('Ctrl Pts',(-28.9444747740815,64.7801987060097,
0.));
#156192=CARTESIAN_POINT('Ctrl Pts',(-28.9419732755659,64.7584997233889,
0.));
#156193=CARTESIAN_POINT('Ctrl Pts',(-28.9394550698201,64.7368507566461,
0.));
#156194=CARTESIAN_POINT('Ctrl Pts',(-28.9369202480383,64.715251947327,0.));
#156195=CARTESIAN_POINT('Ctrl Pts',(-28.934368901987,64.6937034376591,0.));
#156196=CARTESIAN_POINT('Ctrl Pts',(-28.9318011239905,64.6722053705389,
0.));
#156197=CARTESIAN_POINT('Ctrl Pts',(-28.9292170069219,64.6507578895155,
0.));
#156198=CARTESIAN_POINT('Ctrl Pts',(-28.9266166441956,64.6293611387753,
0.));
#156199=CARTESIAN_POINT('Ctrl Pts',(-28.9240001297553,64.6080152631065,
0.));
#156200=CARTESIAN_POINT('Ctrl Pts',(-28.9213675580996,64.5867204079452,
0.));
#156201=CARTESIAN_POINT('Ctrl Pts',(-28.9187190243231,64.5654767194487,
0.));
#156202=CARTESIAN_POINT('Ctrl Pts',(-28.9160546241538,64.544284344556,0.));
#156203=CARTESIAN_POINT('Ctrl Pts',(-28.9133744539943,64.5231434310457,
0.));
#156204=CARTESIAN_POINT('Ctrl Pts',(-28.9106786109639,64.5020541275927,
0.));
#156205=CARTESIAN_POINT('Ctrl Pts',(-28.9079671928253,64.4810165836568,
0.));
#156206=CARTESIAN_POINT('Ctrl Pts',(-28.9052402979055,64.460030949357,0.));
#156207=CARTESIAN_POINT('Ctrl Pts',(-28.9024980250309,64.439097375364,0.));
#156208=CARTESIAN_POINT('Ctrl Pts',(-28.899740473435,64.41821601274,0.));
#156209=CARTESIAN_POINT('Ctrl Pts',(-28.8969677427519,64.3973870129201,
0.));
#156210=CARTESIAN_POINT('Ctrl Pts',(-28.8941799332312,64.3766105280715,
0.));
#156211=CARTESIAN_POINT('Ctrl Pts',(-28.8913771459327,64.3558867114087,
0.));
#156212=CARTESIAN_POINT('Ctrl Pts',(-28.888559482892,64.3352157174606,0.));
#156213=CARTESIAN_POINT('Ctrl Pts',(-28.8857270473944,64.3145977025005,
0.));
#156214=CARTESIAN_POINT('Ctrl Pts',(-28.8828799437922,64.2940328242482,
0.));
#156215=CARTESIAN_POINT('Ctrl Pts',(-28.8800182770052,64.2735212410682,
0.));
#156216=CARTESIAN_POINT('Ctrl Pts',(-28.8771421521058,64.2530631112926,
0.));
#156217=CARTESIAN_POINT('Ctrl Pts',(-28.8742516738959,64.232658592528,0.));
#156218=CARTESIAN_POINT('Ctrl Pts',(-28.8713469464205,64.2123078408507,
0.));
#156219=CARTESIAN_POINT('Ctrl Pts',(-28.8684280739033,64.1920110123342,
0.));
#156220=CARTESIAN_POINT('Ctrl Pts',(-28.8654951618659,64.1717682648708,
0.));
#156221=CARTESIAN_POINT('Ctrl Pts',(-28.8625483180433,64.1515797596555,
0.));
#156222=CARTESIAN_POINT('Ctrl Pts',(-28.8595876537132,64.1314456633345,
0.));
#156223=CARTESIAN_POINT('Ctrl Pts',(-28.8566132838157,64.1113661481918,
0.));
#156224=CARTESIAN_POINT('Ctrl Pts',(-28.8536253241837,64.0913413876586,
0.));
#156225=CARTESIAN_POINT('Ctrl Pts',(-28.8506238891087,64.0713715523588,
0.));
#156226=CARTESIAN_POINT('Ctrl Pts',(-28.8476090892242,64.0514568066659,
0.));
#156227=CARTESIAN_POINT('Ctrl Pts',(-28.8445810281275,64.0315973031994,
0.));
#156228=CARTESIAN_POINT('Ctrl Pts',(-28.841539805646,64.0117931881364,0.));
#156229=CARTESIAN_POINT('Ctrl Pts',(-28.8384855243267,63.9920446117632,
0.));
#156230=CARTESIAN_POINT('Ctrl Pts',(-28.8354182946601,63.9723517369614,
0.));
#156231=CARTESIAN_POINT('Ctrl Pts',(-28.8323382413753,63.9527147494351,
0.));
#156232=CARTESIAN_POINT('Ctrl Pts',(-28.8292455077494,63.9331338646868,
0.));
#156233=CARTESIAN_POINT('Ctrl Pts',(-28.826140242322,63.9136093063647,0.));
#156234=CARTESIAN_POINT('Ctrl Pts',(-28.8230225863142,63.894141285685,0.));
#156235=CARTESIAN_POINT('Ctrl Pts',(-28.8198926619893,63.8747299825383,
0.));
#156236=CARTESIAN_POINT('Ctrl Pts',(-28.8167505576806,63.8553755207732,
0.));
#156237=CARTESIAN_POINT('Ctrl Pts',(-28.8135963263557,63.8360779670225,
0.));
#156238=CARTESIAN_POINT('Ctrl Pts',(-28.8110632621133,63.8206854735372,
0.));
#156239=CARTESIAN_POINT('Ctrl Pts',(-28.8091580239664,63.809166727145,0.));
#156240=CARTESIAN_POINT('Ctrl Pts',(-28.8078854475473,63.8014989507575,
0.));
#156241=CARTESIAN_POINT('Ctrl Pts',(-28.8072485549236,63.7976679095314,
0.));
#156242=CARTESIAN_POINT('Ctrl Pts',(-22.9976507259816,70.8615414811572,
0.));
#156243=CARTESIAN_POINT('Ctrl Pts',(-22.9976507259816,70.8615414811572,
12.));
#156244=CARTESIAN_POINT('Ctrl Pts',(-22.9983100639391,70.8559846928,0.));
#156245=CARTESIAN_POINT('Ctrl Pts',(-22.9983100639391,70.8559846928,12.));
#156246=CARTESIAN_POINT('Ctrl Pts',(-22.9996258555291,70.8448742696689,
0.));
#156247=CARTESIAN_POINT('Ctrl Pts',(-22.9996258555291,70.8448742696689,
12.));
#156248=CARTESIAN_POINT('Ctrl Pts',(-23.0015908899394,70.8282180957225,
0.));
#156249=CARTESIAN_POINT('Ctrl Pts',(-23.0015908899394,70.8282180957225,
12.));
#156250=CARTESIAN_POINT('Ctrl Pts',(-23.0041936291625,70.8060287860585,
0.));
#156251=CARTESIAN_POINT('Ctrl Pts',(-23.0041936291625,70.8060287860585,
12.));
#156252=CARTESIAN_POINT('Ctrl Pts',(-23.0074182063786,70.7783236951202,
0.));
#156253=CARTESIAN_POINT('Ctrl Pts',(-23.0074182063786,70.7783236951202,
12.));
#156254=CARTESIAN_POINT('Ctrl Pts',(-23.0106139366046,70.750650169619,0.));
#156255=CARTESIAN_POINT('Ctrl Pts',(-23.0106139366046,70.750650169619,12.));
#156256=CARTESIAN_POINT('Ctrl Pts',(-23.0137808248924,70.7230082425413,
0.));
#156257=CARTESIAN_POINT('Ctrl Pts',(-23.0137808248924,70.7230082425413,
12.));
#156258=CARTESIAN_POINT('Ctrl Pts',(-23.0169188841045,70.6953979633426,
0.));
#156259=CARTESIAN_POINT('Ctrl Pts',(-23.0169188841045,70.6953979633426,
12.));
#156260=CARTESIAN_POINT('Ctrl Pts',(-23.0200281385833,70.6678194023135,
0.));
#156261=CARTESIAN_POINT('Ctrl Pts',(-23.0200281385833,70.6678194023135,
12.));
#156262=CARTESIAN_POINT('Ctrl Pts',(-23.0231086235186,70.6402726486453,
0.));
#156263=CARTESIAN_POINT('Ctrl Pts',(-23.0231086235186,70.6402726486453,
12.));
#156264=CARTESIAN_POINT('Ctrl Pts',(-23.026160381013,70.6127578036673,0.));
#156265=CARTESIAN_POINT('Ctrl Pts',(-23.026160381013,70.6127578036673,12.));
#156266=CARTESIAN_POINT('Ctrl Pts',(-23.0291834570663,70.5852749754082,
0.));
#156267=CARTESIAN_POINT('Ctrl Pts',(-23.0291834570663,70.5852749754082,
12.));
#156268=CARTESIAN_POINT('Ctrl Pts',(-23.0321778982711,70.5578242727627,
0.));
#156269=CARTESIAN_POINT('Ctrl Pts',(-23.0321778982711,70.5578242727627,
12.));
#156270=CARTESIAN_POINT('Ctrl Pts',(-23.0351437484336,70.5304057994631,
0.));
#156271=CARTESIAN_POINT('Ctrl Pts',(-23.0351437484336,70.5304057994631,
12.));
#156272=CARTESIAN_POINT('Ctrl Pts',(-23.0380810458271,70.5030196492003,
0.));
#156273=CARTESIAN_POINT('Ctrl Pts',(-23.0380810458271,70.5030196492003,
12.));
#156274=CARTESIAN_POINT('Ctrl Pts',(-23.0409898250756,70.4756659090209,
0.));
#156275=CARTESIAN_POINT('Ctrl Pts',(-23.0409898250756,70.4756659090209,
12.));
#156276=CARTESIAN_POINT('Ctrl Pts',(-23.0438701185013,70.4483446617614,
0.));
#156277=CARTESIAN_POINT('Ctrl Pts',(-23.0438701185013,70.4483446617614,
12.));
#156278=CARTESIAN_POINT('Ctrl Pts',(-23.0467219577291,70.4210559889348,
0.));
#156279=CARTESIAN_POINT('Ctrl Pts',(-23.0467219577291,70.4210559889348,
12.));
#156280=CARTESIAN_POINT('Ctrl Pts',(-23.0495453750763,70.3937999732267,
0.));
#156281=CARTESIAN_POINT('Ctrl Pts',(-23.0495453750763,70.3937999732267,
12.));
#156282=CARTESIAN_POINT('Ctrl Pts',(-23.0523404053172,70.3665767016542,
0.));
#156283=CARTESIAN_POINT('Ctrl Pts',(-23.0523404053172,70.3665767016542,
12.));
#156284=CARTESIAN_POINT('Ctrl Pts',(-23.0551070854926,70.3393862652297,
0.));
#156285=CARTESIAN_POINT('Ctrl Pts',(-23.0551070854926,70.3393862652297,
12.));
#156286=CARTESIAN_POINT('Ctrl Pts',(-23.0578454541104,70.3122287575335,
0.));
#156287=CARTESIAN_POINT('Ctrl Pts',(-23.0578454541104,70.3122287575335,
12.));
#156288=CARTESIAN_POINT('Ctrl Pts',(-23.0605555505321,70.2851042736066,
0.));
#156289=CARTESIAN_POINT('Ctrl Pts',(-23.0605555505321,70.2851042736066,
12.));
#156290=CARTESIAN_POINT('Ctrl Pts',(-23.0632374143279,70.2580129087888,
0.));
#156291=CARTESIAN_POINT('Ctrl Pts',(-23.0632374143279,70.2580129087888,
12.));
#156292=CARTESIAN_POINT('Ctrl Pts',(-23.0658910845433,70.2309547573815,
0.));
#156293=CARTESIAN_POINT('Ctrl Pts',(-23.0658910845433,70.2309547573815,
12.));
#156294=CARTESIAN_POINT('Ctrl Pts',(-23.0685165993691,70.2039299120488,
0.));
#156295=CARTESIAN_POINT('Ctrl Pts',(-23.0685165993691,70.2039299120488,
12.));
#156296=CARTESIAN_POINT('Ctrl Pts',(-23.0711139965439,70.1769384645586,
0.));
#156297=CARTESIAN_POINT('Ctrl Pts',(-23.0711139965439,70.1769384645586,
12.));
#156298=CARTESIAN_POINT('Ctrl Pts',(-23.0736833135938,70.1499805062172,
0.));
#156299=CARTESIAN_POINT('Ctrl Pts',(-23.0736833135938,70.1499805062172,
12.));
#156300=CARTESIAN_POINT('Ctrl Pts',(-23.0762245881389,70.123056128422,0.));
#156301=CARTESIAN_POINT('Ctrl Pts',(-23.0762245881389,70.123056128422,12.));
#156302=CARTESIAN_POINT('Ctrl Pts',(-23.0787378581774,70.0961654231639,
0.));
#156303=CARTESIAN_POINT('Ctrl Pts',(-23.0787378581774,70.0961654231639,
12.));
#156304=CARTESIAN_POINT('Ctrl Pts',(-23.0812231623765,70.0693084835373,
0.));
#156305=CARTESIAN_POINT('Ctrl Pts',(-23.0812231623765,70.0693084835373,
12.));
#156306=CARTESIAN_POINT('Ctrl Pts',(-23.0836805399374,70.0424854035115,
0.));
#156307=CARTESIAN_POINT('Ctrl Pts',(-23.0836805399374,70.0424854035115,
12.));
#156308=CARTESIAN_POINT('Ctrl Pts',(-23.0861100304729,70.0156962777169,
0.));
#156309=CARTESIAN_POINT('Ctrl Pts',(-23.0861100304729,70.0156962777169,
12.));
#156310=CARTESIAN_POINT('Ctrl Pts',(-23.0885116738798,69.9889412012143,
0.));
#156311=CARTESIAN_POINT('Ctrl Pts',(-23.0885116738798,69.9889412012143,
12.));
#156312=CARTESIAN_POINT('Ctrl Pts',(-23.0908855102251,69.9622202692873,
0.));
#156313=CARTESIAN_POINT('Ctrl Pts',(-23.0908855102251,69.9622202692873,
12.));
#156314=CARTESIAN_POINT('Ctrl Pts',(-23.0932315796067,69.9355335771729,
0.));
#156315=CARTESIAN_POINT('Ctrl Pts',(-23.0932315796067,69.9355335771729,
12.));
#156316=CARTESIAN_POINT('Ctrl Pts',(-23.0955499221558,69.9088812200713,
0.));
#156317=CARTESIAN_POINT('Ctrl Pts',(-23.0955499221558,69.9088812200713,
12.));
#156318=CARTESIAN_POINT('Ctrl Pts',(-23.0978405781021,69.8822632932768,
0.));
#156319=CARTESIAN_POINT('Ctrl Pts',(-23.0978405781021,69.8822632932768,
12.));
#156320=CARTESIAN_POINT('Ctrl Pts',(-23.1001035878241,69.8556798922693,
0.));
#156321=CARTESIAN_POINT('Ctrl Pts',(-23.1001035878241,69.8556798922693,
12.));
#156322=CARTESIAN_POINT('Ctrl Pts',(-23.1023389919051,69.8291311128118,
0.));
#156323=CARTESIAN_POINT('Ctrl Pts',(-23.1023389919051,69.8291311128118,
12.));
#156324=CARTESIAN_POINT('Ctrl Pts',(-23.1045468311991,69.8026170510572,
0.));
#156325=CARTESIAN_POINT('Ctrl Pts',(-23.1045468311991,69.8026170510572,
12.));
#156326=CARTESIAN_POINT('Ctrl Pts',(-23.106727146861,69.7761378035964,0.));
#156327=CARTESIAN_POINT('Ctrl Pts',(-23.106727146861,69.7761378035964,12.));
#156328=CARTESIAN_POINT('Ctrl Pts',(-23.1088799803089,69.7496934674069,
0.));
#156329=CARTESIAN_POINT('Ctrl Pts',(-23.1088799803089,69.7496934674069,
12.));
#156330=CARTESIAN_POINT('Ctrl Pts',(-23.1110053732046,69.7232841398197,
0.));
#156331=CARTESIAN_POINT('Ctrl Pts',(-23.1110053732046,69.7232841398197,
12.));
#156332=CARTESIAN_POINT('Ctrl Pts',(-23.1131033674301,69.6969099184767,
0.));
#156333=CARTESIAN_POINT('Ctrl Pts',(-23.1131033674301,69.6969099184767,
12.));
#156334=CARTESIAN_POINT('Ctrl Pts',(-23.1151740050681,69.6705709012852,
0.));
#156335=CARTESIAN_POINT('Ctrl Pts',(-23.1151740050681,69.6705709012852,
12.));
#156336=CARTESIAN_POINT('Ctrl Pts',(-23.1172173283859,69.6442671863765,
0.));
#156337=CARTESIAN_POINT('Ctrl Pts',(-23.1172173283859,69.6442671863765,
12.));
#156338=CARTESIAN_POINT('Ctrl Pts',(-23.1192333798441,69.6179988721365,
0.));
#156339=CARTESIAN_POINT('Ctrl Pts',(-23.1192333798441,69.6179988721365,
12.));
#156340=CARTESIAN_POINT('Ctrl Pts',(-23.1212222021051,69.5917660572265,
0.));
#156341=CARTESIAN_POINT('Ctrl Pts',(-23.1212222021051,69.5917660572265,
12.));
#156342=CARTESIAN_POINT('Ctrl Pts',(-23.1231838380452,69.5655688406052,
0.));
#156343=CARTESIAN_POINT('Ctrl Pts',(-23.1231838380452,69.5655688406052,
12.));
#156344=CARTESIAN_POINT('Ctrl Pts',(-23.1251183307676,69.539407321546,0.));
#156345=CARTESIAN_POINT('Ctrl Pts',(-23.1251183307676,69.539407321546,12.));
#156346=CARTESIAN_POINT('Ctrl Pts',(-23.1270257236204,69.5132815996537,
0.));
#156347=CARTESIAN_POINT('Ctrl Pts',(-23.1270257236204,69.5132815996537,
12.));
#156348=CARTESIAN_POINT('Ctrl Pts',(-23.1289060601924,69.4871917748654,
0.));
#156349=CARTESIAN_POINT('Ctrl Pts',(-23.1289060601924,69.4871917748654,
12.));
#156350=CARTESIAN_POINT('Ctrl Pts',(-23.1307593843061,69.4611379474484,
0.));
#156351=CARTESIAN_POINT('Ctrl Pts',(-23.1307593843061,69.4611379474484,
12.));
#156352=CARTESIAN_POINT('Ctrl Pts',(-23.1325857400144,69.4351202179946,
0.));
#156353=CARTESIAN_POINT('Ctrl Pts',(-23.1325857400144,69.4351202179946,
12.));
#156354=CARTESIAN_POINT('Ctrl Pts',(-23.1343851715989,69.4091386874132,
0.));
#156355=CARTESIAN_POINT('Ctrl Pts',(-23.1343851715989,69.4091386874132,
12.));
#156356=CARTESIAN_POINT('Ctrl Pts',(-23.1361577235709,69.3831934569183,
0.));
#156357=CARTESIAN_POINT('Ctrl Pts',(-23.1361577235709,69.3831934569183,
12.));
#156358=CARTESIAN_POINT('Ctrl Pts',(-23.1379034406718,69.3572846280297,
0.));
#156359=CARTESIAN_POINT('Ctrl Pts',(-23.1379034406718,69.3572846280297,
12.));
#156360=CARTESIAN_POINT('Ctrl Pts',(-23.1396223678725,69.3314123025869,
0.));
#156361=CARTESIAN_POINT('Ctrl Pts',(-23.1396223678725,69.3314123025869,
12.));
#156362=CARTESIAN_POINT('Ctrl Pts',(-23.1413145503762,69.3055765827546,
0.));
#156363=CARTESIAN_POINT('Ctrl Pts',(-23.1413145503762,69.3055765827546,
12.));
#156364=CARTESIAN_POINT('Ctrl Pts',(-23.142980033622,69.2797775710273,0.));
#156365=CARTESIAN_POINT('Ctrl Pts',(-23.142980033622,69.2797775710273,12.));
#156366=CARTESIAN_POINT('Ctrl Pts',(-23.1446188632931,69.254015370231,0.));
#156367=CARTESIAN_POINT('Ctrl Pts',(-23.1446188632931,69.254015370231,12.));
#156368=CARTESIAN_POINT('Ctrl Pts',(-23.1462310853206,69.2282900835236,
0.));
#156369=CARTESIAN_POINT('Ctrl Pts',(-23.1462310853206,69.2282900835236,
12.));
#156370=CARTESIAN_POINT('Ctrl Pts',(-23.147816745879,69.2026018144028,0.));
#156371=CARTESIAN_POINT('Ctrl Pts',(-23.147816745879,69.2026018144028,12.));
#156372=CARTESIAN_POINT('Ctrl Pts',(-23.1493758913858,69.1769506667084,
0.));
#156373=CARTESIAN_POINT('Ctrl Pts',(-23.1493758913858,69.1769506667084,
12.));
#156374=CARTESIAN_POINT('Ctrl Pts',(-23.1509085685032,69.1513367446231,
0.));
#156375=CARTESIAN_POINT('Ctrl Pts',(-23.1509085685032,69.1513367446231,
12.));
#156376=CARTESIAN_POINT('Ctrl Pts',(-23.152414824141,69.1257601526687,0.));
#156377=CARTESIAN_POINT('Ctrl Pts',(-23.152414824141,69.1257601526687,12.));
#156378=CARTESIAN_POINT('Ctrl Pts',(-23.1538947054614,69.1002209957025,
0.));
#156379=CARTESIAN_POINT('Ctrl Pts',(-23.1538947054614,69.1002209957025,
12.));
#156380=CARTESIAN_POINT('Ctrl Pts',(-23.1553482598762,69.074719378928,0.));
#156381=CARTESIAN_POINT('Ctrl Pts',(-23.1553482598762,69.074719378928,12.));
#156382=CARTESIAN_POINT('Ctrl Pts',(-23.1567755350469,69.0492554078992,
0.));
#156383=CARTESIAN_POINT('Ctrl Pts',(-23.1567755350469,69.0492554078992,
12.));
#156384=CARTESIAN_POINT('Ctrl Pts',(-23.1581765788869,69.0238291885245,
0.));
#156385=CARTESIAN_POINT('Ctrl Pts',(-23.1581765788869,69.0238291885245,
12.));
#156386=CARTESIAN_POINT('Ctrl Pts',(-23.1595514395656,68.9984408270659,
0.));
#156387=CARTESIAN_POINT('Ctrl Pts',(-23.1595514395656,68.9984408270659,
12.));
#156388=CARTESIAN_POINT('Ctrl Pts',(-23.1609001655156,68.9730904301369,
0.));
#156389=CARTESIAN_POINT('Ctrl Pts',(-23.1609001655156,68.9730904301369,
12.));
#156390=CARTESIAN_POINT('Ctrl Pts',(-23.1622228054291,68.9477781047106,
0.));
#156391=CARTESIAN_POINT('Ctrl Pts',(-23.1622228054291,68.9477781047106,
12.));
#156392=CARTESIAN_POINT('Ctrl Pts',(-23.1635194082581,68.9225039581248,
0.));
#156393=CARTESIAN_POINT('Ctrl Pts',(-23.1635194082581,68.9225039581248,
12.));
#156394=CARTESIAN_POINT('Ctrl Pts',(-23.164790023215,68.8972680980842,0.));
#156395=CARTESIAN_POINT('Ctrl Pts',(-23.164790023215,68.8972680980842,12.));
#156396=CARTESIAN_POINT('Ctrl Pts',(-23.1660346997764,68.8720706326609,
0.));
#156397=CARTESIAN_POINT('Ctrl Pts',(-23.1660346997764,68.8720706326609,
12.));
#156398=CARTESIAN_POINT('Ctrl Pts',(-23.1672534876889,68.8469116702898,
0.));
#156399=CARTESIAN_POINT('Ctrl Pts',(-23.1672534876889,68.8469116702898,
12.));
#156400=CARTESIAN_POINT('Ctrl Pts',(-23.1684464369686,68.8217913197752,
0.));
#156401=CARTESIAN_POINT('Ctrl Pts',(-23.1684464369686,68.8217913197752,
12.));
#156402=CARTESIAN_POINT('Ctrl Pts',(-23.1696135978997,68.7967096902996,
0.));
#156403=CARTESIAN_POINT('Ctrl Pts',(-23.1696135978997,68.7967096902996,
12.));
#156404=CARTESIAN_POINT('Ctrl Pts',(-23.170755021036,68.771666891425,0.));
#156405=CARTESIAN_POINT('Ctrl Pts',(-23.170755021036,68.771666891425,12.));
#156406=CARTESIAN_POINT('Ctrl Pts',(-23.1718707572043,68.746663033096,0.));
#156407=CARTESIAN_POINT('Ctrl Pts',(-23.1718707572043,68.746663033096,12.));
#156408=CARTESIAN_POINT('Ctrl Pts',(-23.172960857511,68.7216982256341,0.));
#156409=CARTESIAN_POINT('Ctrl Pts',(-23.172960857511,68.7216982256341,12.));
#156410=CARTESIAN_POINT('Ctrl Pts',(-23.1740253733417,68.696772579744,0.));
#156411=CARTESIAN_POINT('Ctrl Pts',(-23.1740253733417,68.696772579744,12.));
#156412=CARTESIAN_POINT('Ctrl Pts',(-23.1750643563601,68.6718862065216,
0.));
#156413=CARTESIAN_POINT('Ctrl Pts',(-23.1750643563601,68.6718862065216,
12.));
#156414=CARTESIAN_POINT('Ctrl Pts',(-23.1760778585092,68.6470392174564,
0.));
#156415=CARTESIAN_POINT('Ctrl Pts',(-23.1760778585092,68.6470392174564,
12.));
#156416=CARTESIAN_POINT('Ctrl Pts',(-23.1770659320138,68.6222317244341,
0.));
#156417=CARTESIAN_POINT('Ctrl Pts',(-23.1770659320138,68.6222317244341,
12.));
#156418=CARTESIAN_POINT('Ctrl Pts',(-23.1780286293875,68.597463839733,0.));
#156419=CARTESIAN_POINT('Ctrl Pts',(-23.1780286293875,68.597463839733,12.));
#156420=CARTESIAN_POINT('Ctrl Pts',(-23.1789660034342,68.5727356760278,
0.));
#156421=CARTESIAN_POINT('Ctrl Pts',(-23.1789660034342,68.5727356760278,
12.));
#156422=CARTESIAN_POINT('Ctrl Pts',(-23.179878107245,68.5480473463985,0.));
#156423=CARTESIAN_POINT('Ctrl Pts',(-23.179878107245,68.5480473463985,12.));
#156424=CARTESIAN_POINT('Ctrl Pts',(-23.180764994201,68.5233989643345,0.));
#156425=CARTESIAN_POINT('Ctrl Pts',(-23.180764994201,68.5233989643345,12.));
#156426=CARTESIAN_POINT('Ctrl Pts',(-23.1816267179751,68.4987906437356,
0.));
#156427=CARTESIAN_POINT('Ctrl Pts',(-23.1816267179751,68.4987906437356,
12.));
#156428=CARTESIAN_POINT('Ctrl Pts',(-23.1824633325385,68.4742224989099,
0.));
#156429=CARTESIAN_POINT('Ctrl Pts',(-23.1824633325385,68.4742224989099,
12.));
#156430=CARTESIAN_POINT('Ctrl Pts',(-23.183274892163,68.4496946445758,0.));
#156431=CARTESIAN_POINT('Ctrl Pts',(-23.183274892163,68.4496946445758,12.));
#156432=CARTESIAN_POINT('Ctrl Pts',(-23.1840614514192,68.4252071958729,
0.));
#156433=CARTESIAN_POINT('Ctrl Pts',(-23.1840614514192,68.4252071958729,
12.));
#156434=CARTESIAN_POINT('Ctrl Pts',(-23.1848230651776,68.4007602683652,
0.));
#156435=CARTESIAN_POINT('Ctrl Pts',(-23.1848230651776,68.4007602683652,
12.));
#156436=CARTESIAN_POINT('Ctrl Pts',(-23.1855597886116,68.376353978044,0.));
#156437=CARTESIAN_POINT('Ctrl Pts',(-23.1855597886116,68.376353978044,12.));
#156438=CARTESIAN_POINT('Ctrl Pts',(-23.186271677203,68.3519884413246,0.));
#156439=CARTESIAN_POINT('Ctrl Pts',(-23.186271677203,68.3519884413246,12.));
#156440=CARTESIAN_POINT('Ctrl Pts',(-23.1869587867459,68.3276637750485,
0.));
#156441=CARTESIAN_POINT('Ctrl Pts',(-23.1869587867459,68.3276637750485,
12.));
#156442=CARTESIAN_POINT('Ctrl Pts',(-23.1876211733436,68.3033800964939,
0.));
#156443=CARTESIAN_POINT('Ctrl Pts',(-23.1876211733436,68.3033800964939,
12.));
#156444=CARTESIAN_POINT('Ctrl Pts',(-23.1882588934107,68.2791375233795,
0.));
#156445=CARTESIAN_POINT('Ctrl Pts',(-23.1882588934107,68.2791375233795,
12.));
#156446=CARTESIAN_POINT('Ctrl Pts',(-23.1888720036757,68.2549361738681,
0.));
#156447=CARTESIAN_POINT('Ctrl Pts',(-23.1888720036757,68.2549361738681,
12.));
#156448=CARTESIAN_POINT('Ctrl Pts',(-23.1894605611871,68.2307761665633,
0.));
#156449=CARTESIAN_POINT('Ctrl Pts',(-23.1894605611871,68.2307761665633,
12.));
#156450=CARTESIAN_POINT('Ctrl Pts',(-23.1900246233165,68.2066576205116,
0.));
#156451=CARTESIAN_POINT('Ctrl Pts',(-23.1900246233165,68.2066576205116,
12.));
#156452=CARTESIAN_POINT('Ctrl Pts',(-23.1905642477571,68.1825806552129,
0.));
#156453=CARTESIAN_POINT('Ctrl Pts',(-23.1905642477571,68.1825806552129,
12.));
#156454=CARTESIAN_POINT('Ctrl Pts',(-23.1910794925251,68.1585453906257,
0.));
#156455=CARTESIAN_POINT('Ctrl Pts',(-23.1910794925251,68.1585453906257,
12.));
#156456=CARTESIAN_POINT('Ctrl Pts',(-23.1915704159623,68.1345519471695,
0.));
#156457=CARTESIAN_POINT('Ctrl Pts',(-23.1915704159623,68.1345519471695,
12.));
#156458=CARTESIAN_POINT('Ctrl Pts',(-23.1920370767425,68.110600445723,0.));
#156459=CARTESIAN_POINT('Ctrl Pts',(-23.1920370767425,68.110600445723,12.));
#156460=CARTESIAN_POINT('Ctrl Pts',(-23.1924795338749,68.0866910076251,
0.));
#156461=CARTESIAN_POINT('Ctrl Pts',(-23.1924795338749,68.0866910076251,
12.));
#156462=CARTESIAN_POINT('Ctrl Pts',(-23.1928978467021,68.0628237546863,
0.));
#156463=CARTESIAN_POINT('Ctrl Pts',(-23.1928978467021,68.0628237546863,
12.));
#156464=CARTESIAN_POINT('Ctrl Pts',(-23.1932920749023,68.0389988091933,
0.));
#156465=CARTESIAN_POINT('Ctrl Pts',(-23.1932920749023,68.0389988091933,
12.));
#156466=CARTESIAN_POINT('Ctrl Pts',(-23.1936622784919,68.0152162939121,
0.));
#156467=CARTESIAN_POINT('Ctrl Pts',(-23.1936622784919,68.0152162939121,
12.));
#156468=CARTESIAN_POINT('Ctrl Pts',(-23.1940085178313,67.991476332086,0.));
#156469=CARTESIAN_POINT('Ctrl Pts',(-23.1940085178313,67.991476332086,12.));
#156470=CARTESIAN_POINT('Ctrl Pts',(-23.1943308536297,67.9677790474385,
0.));
#156471=CARTESIAN_POINT('Ctrl Pts',(-23.1943308536297,67.9677790474385,
12.));
#156472=CARTESIAN_POINT('Ctrl Pts',(-23.1946293469427,67.9441245641842,
0.));
#156473=CARTESIAN_POINT('Ctrl Pts',(-23.1946293469427,67.9441245641842,
12.));
#156474=CARTESIAN_POINT('Ctrl Pts',(-23.1949040591744,67.9205130070324,
0.));
#156475=CARTESIAN_POINT('Ctrl Pts',(-23.1949040591744,67.9205130070324,
12.));
#156476=CARTESIAN_POINT('Ctrl Pts',(-23.1951550520802,67.8969445011916,
0.));
#156477=CARTESIAN_POINT('Ctrl Pts',(-23.1951550520802,67.8969445011916,
12.));
#156478=CARTESIAN_POINT('Ctrl Pts',(-23.1953823877734,67.8734191723667,
0.));
#156479=CARTESIAN_POINT('Ctrl Pts',(-23.1953823877734,67.8734191723667,
12.));
#156480=CARTESIAN_POINT('Ctrl Pts',(-23.1955861287286,67.8499371467616,
0.));
#156481=CARTESIAN_POINT('Ctrl Pts',(-23.1955861287286,67.8499371467616,
12.));
#156482=CARTESIAN_POINT('Ctrl Pts',(-23.1957663377806,67.8264985510917,
0.));
#156483=CARTESIAN_POINT('Ctrl Pts',(-23.1957663377806,67.8264985510917,
12.));
#156484=CARTESIAN_POINT('Ctrl Pts',(-23.1959230781269,67.8031035125887,
0.));
#156485=CARTESIAN_POINT('Ctrl Pts',(-23.1959230781269,67.8031035125887,
12.));
#156486=CARTESIAN_POINT('Ctrl Pts',(-23.1960564133304,67.7797521590045,
0.));
#156487=CARTESIAN_POINT('Ctrl Pts',(-23.1960564133304,67.7797521590045,
12.));
#156488=CARTESIAN_POINT('Ctrl Pts',(-23.1961664073262,67.7564446186079,
0.));
#156489=CARTESIAN_POINT('Ctrl Pts',(-23.1961664073262,67.7564446186079,
12.));
#156490=CARTESIAN_POINT('Ctrl Pts',(-23.1962531244245,67.7331810201883,
0.));
#156491=CARTESIAN_POINT('Ctrl Pts',(-23.1962531244245,67.7331810201883,
12.));
#156492=CARTESIAN_POINT('Ctrl Pts',(-23.1963166293102,67.7099614930671,
0.));
#156493=CARTESIAN_POINT('Ctrl Pts',(-23.1963166293102,67.7099614930671,
12.));
#156494=CARTESIAN_POINT('Ctrl Pts',(-23.1963569870451,67.6867861671031,
0.));
#156495=CARTESIAN_POINT('Ctrl Pts',(-23.1963569870451,67.6867861671031,
12.));
#156496=CARTESIAN_POINT('Ctrl Pts',(-23.1963742630714,67.6636551726964,
0.));
#156497=CARTESIAN_POINT('Ctrl Pts',(-23.1963742630714,67.6636551726964,
12.));
#156498=CARTESIAN_POINT('Ctrl Pts',(-23.1963685232187,67.6405686407863,
0.));
#156499=CARTESIAN_POINT('Ctrl Pts',(-23.1963685232187,67.6405686407863,
12.));
#156500=CARTESIAN_POINT('Ctrl Pts',(-23.1963398337068,67.6175267028555,
0.));
#156501=CARTESIAN_POINT('Ctrl Pts',(-23.1963398337068,67.6175267028555,
12.));
#156502=CARTESIAN_POINT('Ctrl Pts',(-23.1962882611453,67.5945294909426,
0.));
#156503=CARTESIAN_POINT('Ctrl Pts',(-23.1962882611453,67.5945294909426,
12.));
#156504=CARTESIAN_POINT('Ctrl Pts',(-23.196213872536,67.5715771376461,0.));
#156505=CARTESIAN_POINT('Ctrl Pts',(-23.196213872536,67.5715771376461,12.));
#156506=CARTESIAN_POINT('Ctrl Pts',(-23.1961167352772,67.5486697761288,
0.));
#156507=CARTESIAN_POINT('Ctrl Pts',(-23.1961167352772,67.5486697761288,
12.));
#156508=CARTESIAN_POINT('Ctrl Pts',(-23.1959969171701,67.5258075401146,
0.));
#156509=CARTESIAN_POINT('Ctrl Pts',(-23.1959969171701,67.5258075401146,
12.));
#156510=CARTESIAN_POINT('Ctrl Pts',(-23.1958544864215,67.5029905638949,
0.));
#156511=CARTESIAN_POINT('Ctrl Pts',(-23.1958544864215,67.5029905638949,
12.));
#156512=CARTESIAN_POINT('Ctrl Pts',(-23.195689511644,67.4802189823408,0.));
#156513=CARTESIAN_POINT('Ctrl Pts',(-23.195689511644,67.4802189823408,12.));
#156514=CARTESIAN_POINT('Ctrl Pts',(-23.195502061859,67.4574929309076,0.));
#156515=CARTESIAN_POINT('Ctrl Pts',(-23.195502061859,67.4574929309076,12.));
#156516=CARTESIAN_POINT('Ctrl Pts',(-23.1952922065012,67.4348125456398,
0.));
#156517=CARTESIAN_POINT('Ctrl Pts',(-23.1952922065012,67.4348125456398,
12.));
#156518=CARTESIAN_POINT('Ctrl Pts',(-23.1950600154265,67.412177963168,0.));
#156519=CARTESIAN_POINT('Ctrl Pts',(-23.1950600154265,67.412177963168,12.));
#156520=CARTESIAN_POINT('Ctrl Pts',(-23.1948055589129,67.3895893207182,
0.));
#156521=CARTESIAN_POINT('Ctrl Pts',(-23.1948055589129,67.3895893207182,
12.));
#156522=CARTESIAN_POINT('Ctrl Pts',(-23.194528907661,67.3670467561212,0.));
#156523=CARTESIAN_POINT('Ctrl Pts',(-23.194528907661,67.3670467561212,12.));
#156524=CARTESIAN_POINT('Ctrl Pts',(-23.1942301327978,67.3445504078176,
0.));
#156525=CARTESIAN_POINT('Ctrl Pts',(-23.1942301327978,67.3445504078176,
12.));
#156526=CARTESIAN_POINT('Ctrl Pts',(-23.1939093058801,67.3221004148603,
0.));
#156527=CARTESIAN_POINT('Ctrl Pts',(-23.1939093058801,67.3221004148603,
12.));
#156528=CARTESIAN_POINT('Ctrl Pts',(-23.1935664989018,67.2996969169098,
0.));
#156529=CARTESIAN_POINT('Ctrl Pts',(-23.1935664989018,67.2996969169098,
12.));
#156530=CARTESIAN_POINT('Ctrl Pts',(-23.1932017842953,67.2773400542477,
0.));
#156531=CARTESIAN_POINT('Ctrl Pts',(-23.1932017842953,67.2773400542477,
12.));
#156532=CARTESIAN_POINT('Ctrl Pts',(-23.1928152349343,67.2550299677888,
0.));
#156533=CARTESIAN_POINT('Ctrl Pts',(-23.1928152349343,67.2550299677888,
12.));
#156534=CARTESIAN_POINT('Ctrl Pts',(-23.1924069241385,67.232766799088,0.));
#156535=CARTESIAN_POINT('Ctrl Pts',(-23.1924069241385,67.232766799088,12.));
#156536=CARTESIAN_POINT('Ctrl Pts',(-23.1919769256803,67.2105506903447,
0.));
#156537=CARTESIAN_POINT('Ctrl Pts',(-23.1919769256803,67.2105506903447,
12.));
#156538=CARTESIAN_POINT('Ctrl Pts',(-23.1915253137924,67.1883817844038,
0.));
#156539=CARTESIAN_POINT('Ctrl Pts',(-23.1915253137924,67.1883817844038,
12.));
#156540=CARTESIAN_POINT('Ctrl Pts',(-23.1910521631657,67.1662602247639,
0.));
#156541=CARTESIAN_POINT('Ctrl Pts',(-23.1910521631657,67.1662602247639,
12.));
#156542=CARTESIAN_POINT('Ctrl Pts',(-23.1905575489504,67.1441861555817,
0.));
#156543=CARTESIAN_POINT('Ctrl Pts',(-23.1905575489504,67.1441861555817,
12.));
#156544=CARTESIAN_POINT('Ctrl Pts',(-23.1900415467574,67.1221597216741,
0.));
#156545=CARTESIAN_POINT('Ctrl Pts',(-23.1900415467574,67.1221597216741,
12.));
#156546=CARTESIAN_POINT('Ctrl Pts',(-23.1895042326626,67.1001810685143,
0.));
#156547=CARTESIAN_POINT('Ctrl Pts',(-23.1895042326626,67.1001810685143,
12.));
#156548=CARTESIAN_POINT('Ctrl Pts',(-23.1889456832119,67.0782503422305,
0.));
#156549=CARTESIAN_POINT('Ctrl Pts',(-23.1889456832119,67.0782503422305,
12.));
#156550=CARTESIAN_POINT('Ctrl Pts',(-23.1883659754271,67.0563676896325,
0.));
#156551=CARTESIAN_POINT('Ctrl Pts',(-23.1883659754271,67.0563676896325,
12.));
#156552=CARTESIAN_POINT('Ctrl Pts',(-23.1877651868158,67.0345332582306,
0.));
#156553=CARTESIAN_POINT('Ctrl Pts',(-23.1877651868158,67.0345332582306,
12.));
#156554=CARTESIAN_POINT('Ctrl Pts',(-23.1871433953793,67.0127471962501,
0.));
#156555=CARTESIAN_POINT('Ctrl Pts',(-23.1871433953793,67.0127471962501,
12.));
#156556=CARTESIAN_POINT('Ctrl Pts',(-23.1865006796283,66.9910096526462,
0.));
#156557=CARTESIAN_POINT('Ctrl Pts',(-23.1865006796283,66.9910096526462,
12.));
#156558=CARTESIAN_POINT('Ctrl Pts',(-23.1858371185842,66.9693207771031,
0.));
#156559=CARTESIAN_POINT('Ctrl Pts',(-23.1858371185842,66.9693207771031,
12.));
#156560=CARTESIAN_POINT('Ctrl Pts',(-23.1851527917657,66.9476807200203,
0.));
#156561=CARTESIAN_POINT('Ctrl Pts',(-23.1851527917657,66.9476807200203,
12.));
#156562=CARTESIAN_POINT('Ctrl Pts',(-23.1844477791814,66.9260896324949,
0.));
#156563=CARTESIAN_POINT('Ctrl Pts',(-23.1844477791814,66.9260896324949,
12.));
#156564=CARTESIAN_POINT('Ctrl Pts',(-23.1837221613235,66.9045476663063,
0.));
#156565=CARTESIAN_POINT('Ctrl Pts',(-23.1837221613235,66.9045476663063,
12.));
#156566=CARTESIAN_POINT('Ctrl Pts',(-23.1829760191591,66.8830549738795,
0.));
#156567=CARTESIAN_POINT('Ctrl Pts',(-23.1829760191591,66.8830549738795,
12.));
#156568=CARTESIAN_POINT('Ctrl Pts',(-23.1822094341517,66.8616117083331,
0.));
#156569=CARTESIAN_POINT('Ctrl Pts',(-23.1822094341517,66.8616117083331,
12.));
#156570=CARTESIAN_POINT('Ctrl Pts',(-23.1814224882953,66.8402180235566,
0.));
#156571=CARTESIAN_POINT('Ctrl Pts',(-23.1814224882953,66.8402180235566,
12.));
#156572=CARTESIAN_POINT('Ctrl Pts',(-23.1806152641475,66.8188740742727,
0.));
#156573=CARTESIAN_POINT('Ctrl Pts',(-23.1806152641475,66.8188740742727,
12.));
#156574=CARTESIAN_POINT('Ctrl Pts',(-23.1797878448639,66.7975800161,0.));
#156575=CARTESIAN_POINT('Ctrl Pts',(-23.1797878448639,66.7975800161,12.));
#156576=CARTESIAN_POINT('Ctrl Pts',(-23.1789403142366,66.776336005612,0.));
#156577=CARTESIAN_POINT('Ctrl Pts',(-23.1789403142366,66.776336005612,12.));
#156578=CARTESIAN_POINT('Ctrl Pts',(-23.17807275663,66.7551422002204,0.));
#156579=CARTESIAN_POINT('Ctrl Pts',(-23.17807275663,66.7551422002204,12.));
#156580=CARTESIAN_POINT('Ctrl Pts',(-23.1771852569131,66.7339987580427,
0.));
#156581=CARTESIAN_POINT('Ctrl Pts',(-23.1771852569131,66.7339987580427,
12.));
#156582=CARTESIAN_POINT('Ctrl Pts',(-23.1762779004044,66.7129058377896,
0.));
#156583=CARTESIAN_POINT('Ctrl Pts',(-23.1762779004044,66.7129058377896,
12.));
#156584=CARTESIAN_POINT('Ctrl Pts',(-23.1753507727939,66.6918635985972,
0.));
#156585=CARTESIAN_POINT('Ctrl Pts',(-23.1753507727939,66.6918635985972,
12.));
#156586=CARTESIAN_POINT('Ctrl Pts',(-23.1744039601382,66.6708722000079,
0.));
#156587=CARTESIAN_POINT('Ctrl Pts',(-23.1744039601382,66.6708722000079,
12.));
#156588=CARTESIAN_POINT('Ctrl Pts',(-23.1734375490431,66.6499318023473,
0.));
#156589=CARTESIAN_POINT('Ctrl Pts',(-23.1734375490431,66.6499318023473,
12.));
#156590=CARTESIAN_POINT('Ctrl Pts',(-23.1724516268302,66.6290425670548,
0.));
#156591=CARTESIAN_POINT('Ctrl Pts',(-23.1724516268302,66.6290425670548,
12.));
#156592=CARTESIAN_POINT('Ctrl Pts',(-23.1714462816789,66.6082046569644,
0.));
#156593=CARTESIAN_POINT('Ctrl Pts',(-23.1714462816789,66.6082046569644,
12.));
#156594=CARTESIAN_POINT('Ctrl Pts',(-23.1704216028614,66.5874182367563,
0.));
#156595=CARTESIAN_POINT('Ctrl Pts',(-23.1704216028614,66.5874182367563,
12.));
#156596=CARTESIAN_POINT('Ctrl Pts',(-23.1693776805866,66.5666834726454,
0.));
#156597=CARTESIAN_POINT('Ctrl Pts',(-23.1693776805866,66.5666834726454,
12.));
#156598=CARTESIAN_POINT('Ctrl Pts',(-23.1683146055726,66.5460005315376,
0.));
#156599=CARTESIAN_POINT('Ctrl Pts',(-23.1683146055726,66.5460005315376,
12.));
#156600=CARTESIAN_POINT('Ctrl Pts',(-23.1672324686926,66.5253695803205,
0.));
#156601=CARTESIAN_POINT('Ctrl Pts',(-23.1672324686926,66.5253695803205,
12.));
#156602=CARTESIAN_POINT('Ctrl Pts',(-23.1661313606132,66.5047907851348,
0.));
#156603=CARTESIAN_POINT('Ctrl Pts',(-23.1661313606132,66.5047907851348,
12.));
#156604=CARTESIAN_POINT('Ctrl Pts',(-23.1650113713808,66.4842643105311,
0.));
#156605=CARTESIAN_POINT('Ctrl Pts',(-23.1650113713808,66.4842643105311,
12.));
#156606=CARTESIAN_POINT('Ctrl Pts',(-23.1638725912195,66.4637903210727,
0.));
#156607=CARTESIAN_POINT('Ctrl Pts',(-23.1638725912195,66.4637903210727,
12.));
#156608=CARTESIAN_POINT('Ctrl Pts',(-23.1627151114883,66.4433689832478,
0.));
#156609=CARTESIAN_POINT('Ctrl Pts',(-23.1627151114883,66.4433689832478,
12.));
#156610=CARTESIAN_POINT('Ctrl Pts',(-23.1615390254632,66.4230004670278,
0.));
#156611=CARTESIAN_POINT('Ctrl Pts',(-23.1615390254632,66.4230004670278,
12.));
#156612=CARTESIAN_POINT('Ctrl Pts',(-23.160344429474,66.4026849481232,0.));
#156613=CARTESIAN_POINT('Ctrl Pts',(-23.160344429474,66.4026849481232,12.));
#156614=CARTESIAN_POINT('Ctrl Pts',(-23.1591314230083,66.3824226081802,
0.));
#156615=CARTESIAN_POINT('Ctrl Pts',(-23.1591314230083,66.3824226081802,
12.));
#156616=CARTESIAN_POINT('Ctrl Pts',(-23.1579001063424,66.3622136300654,
0.));
#156617=CARTESIAN_POINT('Ctrl Pts',(-23.1579001063424,66.3622136300654,
12.));
#156618=CARTESIAN_POINT('Ctrl Pts',(-23.1566505784621,66.3420581937147,
0.));
#156619=CARTESIAN_POINT('Ctrl Pts',(-23.1566505784621,66.3420581937147,
12.));
#156620=CARTESIAN_POINT('Ctrl Pts',(-23.1553829352539,66.3219564725184,
0.));
#156621=CARTESIAN_POINT('Ctrl Pts',(-23.1553829352539,66.3219564725184,
12.));
#156622=CARTESIAN_POINT('Ctrl Pts',(-23.1540972666191,66.3019086275444,
0.));
#156623=CARTESIAN_POINT('Ctrl Pts',(-23.1540972666191,66.3019086275444,
12.));
#156624=CARTESIAN_POINT('Ctrl Pts',(-23.1527936592651,66.281914813114,0.));
#156625=CARTESIAN_POINT('Ctrl Pts',(-23.1527936592651,66.281914813114,12.));
#156626=CARTESIAN_POINT('Ctrl Pts',(-23.1514722022503,66.2619751878793,
0.));
#156627=CARTESIAN_POINT('Ctrl Pts',(-23.1514722022503,66.2619751878793,
12.));
#156628=CARTESIAN_POINT('Ctrl Pts',(-23.1501329914487,66.2420899237318,
0.));
#156629=CARTESIAN_POINT('Ctrl Pts',(-23.1501329914487,66.2420899237318,
12.));
#156630=CARTESIAN_POINT('Ctrl Pts',(-23.1487761349298,66.2222592165398,
0.));
#156631=CARTESIAN_POINT('Ctrl Pts',(-23.1487761349298,66.2222592165398,
12.));
#156632=CARTESIAN_POINT('Ctrl Pts',(-23.147401756643,66.2024832934733,0.));
#156633=CARTESIAN_POINT('Ctrl Pts',(-23.147401756643,66.2024832934733,12.));
#156634=CARTESIAN_POINT('Ctrl Pts',(-23.1460099850704,66.1827623902755,
0.));
#156635=CARTESIAN_POINT('Ctrl Pts',(-23.1460099850704,66.1827623902755,
12.));
#156636=CARTESIAN_POINT('Ctrl Pts',(-23.1446009424871,66.163096729667,0.));
#156637=CARTESIAN_POINT('Ctrl Pts',(-23.1446009424871,66.163096729667,12.));
#156638=CARTESIAN_POINT('Ctrl Pts',(-23.1431747350127,66.14348650151,0.));
#156639=CARTESIAN_POINT('Ctrl Pts',(-23.1431747350127,66.14348650151,12.));
#156640=CARTESIAN_POINT('Ctrl Pts',(-23.1417314398501,66.1239318368803,
0.));
#156641=CARTESIAN_POINT('Ctrl Pts',(-23.1417314398501,66.1239318368803,
12.));
#156642=CARTESIAN_POINT('Ctrl Pts',(-23.140271103958,66.1044328067739,0.));
#156643=CARTESIAN_POINT('Ctrl Pts',(-23.140271103958,66.1044328067739,12.));
#156644=CARTESIAN_POINT('Ctrl Pts',(-23.1390892229923,66.0888781152779,
0.));
#156645=CARTESIAN_POINT('Ctrl Pts',(-23.1390892229923,66.0888781152779,
12.));
#156646=CARTESIAN_POINT('Ctrl Pts',(-23.1381951597491,66.0772371487475,
0.));
#156647=CARTESIAN_POINT('Ctrl Pts',(-23.1381951597491,66.0772371487475,
12.));
#156648=CARTESIAN_POINT('Ctrl Pts',(-23.1375957166138,66.0694876382212,
0.));
#156649=CARTESIAN_POINT('Ctrl Pts',(-23.1375957166138,66.0694876382212,
12.));
#156650=CARTESIAN_POINT('Ctrl Pts',(-23.1372951448024,66.0656156664138,
0.));
#156651=CARTESIAN_POINT('Ctrl Pts',(-23.1372951448024,66.0656156664138,
12.));
#156652=CARTESIAN_POINT('',(-23.1372951448024,66.0656156664138,12.));
#156653=CARTESIAN_POINT('Ctrl Pts',(-23.1372951448024,66.0656156664138,
12.));
#156654=CARTESIAN_POINT('Ctrl Pts',(-23.1375957166138,66.0694876382212,
12.));
#156655=CARTESIAN_POINT('Ctrl Pts',(-23.1381951597491,66.0772371487475,
12.));
#156656=CARTESIAN_POINT('Ctrl Pts',(-23.1390892229923,66.0888781152779,
12.));
#156657=CARTESIAN_POINT('Ctrl Pts',(-23.140271103958,66.1044328067739,12.));
#156658=CARTESIAN_POINT('Ctrl Pts',(-23.1417314398501,66.1239318368803,
12.));
#156659=CARTESIAN_POINT('Ctrl Pts',(-23.1431747350127,66.14348650151,12.));
#156660=CARTESIAN_POINT('Ctrl Pts',(-23.1446009424871,66.163096729667,12.));
#156661=CARTESIAN_POINT('Ctrl Pts',(-23.1460099850704,66.1827623902755,
12.));
#156662=CARTESIAN_POINT('Ctrl Pts',(-23.147401756643,66.2024832934733,12.));
#156663=CARTESIAN_POINT('Ctrl Pts',(-23.1487761349298,66.2222592165398,
12.));
#156664=CARTESIAN_POINT('Ctrl Pts',(-23.1501329914487,66.2420899237318,
12.));
#156665=CARTESIAN_POINT('Ctrl Pts',(-23.1514722022503,66.2619751878793,
12.));
#156666=CARTESIAN_POINT('Ctrl Pts',(-23.1527936592651,66.281914813114,12.));
#156667=CARTESIAN_POINT('Ctrl Pts',(-23.1540972666191,66.3019086275444,
12.));
#156668=CARTESIAN_POINT('Ctrl Pts',(-23.1553829352539,66.3219564725184,
12.));
#156669=CARTESIAN_POINT('Ctrl Pts',(-23.1566505784621,66.3420581937147,
12.));
#156670=CARTESIAN_POINT('Ctrl Pts',(-23.1579001063424,66.3622136300654,
12.));
#156671=CARTESIAN_POINT('Ctrl Pts',(-23.1591314230083,66.3824226081802,
12.));
#156672=CARTESIAN_POINT('Ctrl Pts',(-23.160344429474,66.4026849481232,12.));
#156673=CARTESIAN_POINT('Ctrl Pts',(-23.1615390254632,66.4230004670278,
12.));
#156674=CARTESIAN_POINT('Ctrl Pts',(-23.1627151114883,66.4433689832478,
12.));
#156675=CARTESIAN_POINT('Ctrl Pts',(-23.1638725912195,66.4637903210727,
12.));
#156676=CARTESIAN_POINT('Ctrl Pts',(-23.1650113713808,66.4842643105311,
12.));
#156677=CARTESIAN_POINT('Ctrl Pts',(-23.1661313606132,66.5047907851348,
12.));
#156678=CARTESIAN_POINT('Ctrl Pts',(-23.1672324686926,66.5253695803205,
12.));
#156679=CARTESIAN_POINT('Ctrl Pts',(-23.1683146055726,66.5460005315376,
12.));
#156680=CARTESIAN_POINT('Ctrl Pts',(-23.1693776805866,66.5666834726454,
12.));
#156681=CARTESIAN_POINT('Ctrl Pts',(-23.1704216028614,66.5874182367563,
12.));
#156682=CARTESIAN_POINT('Ctrl Pts',(-23.1714462816789,66.6082046569644,
12.));
#156683=CARTESIAN_POINT('Ctrl Pts',(-23.1724516268302,66.6290425670548,
12.));
#156684=CARTESIAN_POINT('Ctrl Pts',(-23.1734375490431,66.6499318023473,
12.));
#156685=CARTESIAN_POINT('Ctrl Pts',(-23.1744039601382,66.6708722000079,
12.));
#156686=CARTESIAN_POINT('Ctrl Pts',(-23.1753507727939,66.6918635985972,
12.));
#156687=CARTESIAN_POINT('Ctrl Pts',(-23.1762779004044,66.7129058377896,
12.));
#156688=CARTESIAN_POINT('Ctrl Pts',(-23.1771852569131,66.7339987580427,
12.));
#156689=CARTESIAN_POINT('Ctrl Pts',(-23.17807275663,66.7551422002204,12.));
#156690=CARTESIAN_POINT('Ctrl Pts',(-23.1789403142366,66.776336005612,12.));
#156691=CARTESIAN_POINT('Ctrl Pts',(-23.1797878448639,66.7975800161,12.));
#156692=CARTESIAN_POINT('Ctrl Pts',(-23.1806152641475,66.8188740742727,
12.));
#156693=CARTESIAN_POINT('Ctrl Pts',(-23.1814224882953,66.8402180235566,
12.));
#156694=CARTESIAN_POINT('Ctrl Pts',(-23.1822094341517,66.8616117083331,
12.));
#156695=CARTESIAN_POINT('Ctrl Pts',(-23.1829760191591,66.8830549738795,
12.));
#156696=CARTESIAN_POINT('Ctrl Pts',(-23.1837221613235,66.9045476663063,
12.));
#156697=CARTESIAN_POINT('Ctrl Pts',(-23.1844477791814,66.9260896324949,
12.));
#156698=CARTESIAN_POINT('Ctrl Pts',(-23.1851527917657,66.9476807200203,
12.));
#156699=CARTESIAN_POINT('Ctrl Pts',(-23.1858371185842,66.9693207771031,
12.));
#156700=CARTESIAN_POINT('Ctrl Pts',(-23.1865006796283,66.9910096526462,
12.));
#156701=CARTESIAN_POINT('Ctrl Pts',(-23.1871433953793,67.0127471962501,
12.));
#156702=CARTESIAN_POINT('Ctrl Pts',(-23.1877651868158,67.0345332582306,
12.));
#156703=CARTESIAN_POINT('Ctrl Pts',(-23.1883659754271,67.0563676896325,
12.));
#156704=CARTESIAN_POINT('Ctrl Pts',(-23.1889456832119,67.0782503422305,
12.));
#156705=CARTESIAN_POINT('Ctrl Pts',(-23.1895042326626,67.1001810685143,
12.));
#156706=CARTESIAN_POINT('Ctrl Pts',(-23.1900415467574,67.1221597216741,
12.));
#156707=CARTESIAN_POINT('Ctrl Pts',(-23.1905575489504,67.1441861555817,
12.));
#156708=CARTESIAN_POINT('Ctrl Pts',(-23.1910521631657,67.1662602247639,
12.));
#156709=CARTESIAN_POINT('Ctrl Pts',(-23.1915253137924,67.1883817844038,
12.));
#156710=CARTESIAN_POINT('Ctrl Pts',(-23.1919769256803,67.2105506903447,
12.));
#156711=CARTESIAN_POINT('Ctrl Pts',(-23.1924069241385,67.232766799088,12.));
#156712=CARTESIAN_POINT('Ctrl Pts',(-23.1928152349343,67.2550299677888,
12.));
#156713=CARTESIAN_POINT('Ctrl Pts',(-23.1932017842953,67.2773400542477,
12.));
#156714=CARTESIAN_POINT('Ctrl Pts',(-23.1935664989018,67.2996969169098,
12.));
#156715=CARTESIAN_POINT('Ctrl Pts',(-23.1939093058801,67.3221004148603,
12.));
#156716=CARTESIAN_POINT('Ctrl Pts',(-23.1942301327978,67.3445504078176,
12.));
#156717=CARTESIAN_POINT('Ctrl Pts',(-23.194528907661,67.3670467561212,12.));
#156718=CARTESIAN_POINT('Ctrl Pts',(-23.1948055589129,67.3895893207182,
12.));
#156719=CARTESIAN_POINT('Ctrl Pts',(-23.1950600154265,67.412177963168,12.));
#156720=CARTESIAN_POINT('Ctrl Pts',(-23.1952922065012,67.4348125456398,
12.));
#156721=CARTESIAN_POINT('Ctrl Pts',(-23.195502061859,67.4574929309076,12.));
#156722=CARTESIAN_POINT('Ctrl Pts',(-23.195689511644,67.4802189823408,12.));
#156723=CARTESIAN_POINT('Ctrl Pts',(-23.1958544864215,67.5029905638949,
12.));
#156724=CARTESIAN_POINT('Ctrl Pts',(-23.1959969171701,67.5258075401146,
12.));
#156725=CARTESIAN_POINT('Ctrl Pts',(-23.1961167352772,67.5486697761288,
12.));
#156726=CARTESIAN_POINT('Ctrl Pts',(-23.196213872536,67.5715771376461,12.));
#156727=CARTESIAN_POINT('Ctrl Pts',(-23.1962882611453,67.5945294909426,
12.));
#156728=CARTESIAN_POINT('Ctrl Pts',(-23.1963398337068,67.6175267028555,
12.));
#156729=CARTESIAN_POINT('Ctrl Pts',(-23.1963685232187,67.6405686407863,
12.));
#156730=CARTESIAN_POINT('Ctrl Pts',(-23.1963742630714,67.6636551726964,
12.));
#156731=CARTESIAN_POINT('Ctrl Pts',(-23.1963569870451,67.6867861671031,
12.));
#156732=CARTESIAN_POINT('Ctrl Pts',(-23.1963166293102,67.7099614930671,
12.));
#156733=CARTESIAN_POINT('Ctrl Pts',(-23.1962531244245,67.7331810201883,
12.));
#156734=CARTESIAN_POINT('Ctrl Pts',(-23.1961664073262,67.7564446186079,
12.));
#156735=CARTESIAN_POINT('Ctrl Pts',(-23.1960564133304,67.7797521590045,
12.));
#156736=CARTESIAN_POINT('Ctrl Pts',(-23.1959230781269,67.8031035125887,
12.));
#156737=CARTESIAN_POINT('Ctrl Pts',(-23.1957663377806,67.8264985510917,
12.));
#156738=CARTESIAN_POINT('Ctrl Pts',(-23.1955861287286,67.8499371467616,
12.));
#156739=CARTESIAN_POINT('Ctrl Pts',(-23.1953823877734,67.8734191723667,
12.));
#156740=CARTESIAN_POINT('Ctrl Pts',(-23.1951550520802,67.8969445011916,
12.));
#156741=CARTESIAN_POINT('Ctrl Pts',(-23.1949040591744,67.9205130070324,
12.));
#156742=CARTESIAN_POINT('Ctrl Pts',(-23.1946293469427,67.9441245641842,
12.));
#156743=CARTESIAN_POINT('Ctrl Pts',(-23.1943308536297,67.9677790474385,
12.));
#156744=CARTESIAN_POINT('Ctrl Pts',(-23.1940085178313,67.991476332086,12.));
#156745=CARTESIAN_POINT('Ctrl Pts',(-23.1936622784919,68.0152162939121,
12.));
#156746=CARTESIAN_POINT('Ctrl Pts',(-23.1932920749023,68.0389988091933,
12.));
#156747=CARTESIAN_POINT('Ctrl Pts',(-23.1928978467021,68.0628237546863,
12.));
#156748=CARTESIAN_POINT('Ctrl Pts',(-23.1924795338749,68.0866910076251,
12.));
#156749=CARTESIAN_POINT('Ctrl Pts',(-23.1920370767425,68.110600445723,12.));
#156750=CARTESIAN_POINT('Ctrl Pts',(-23.1915704159623,68.1345519471695,
12.));
#156751=CARTESIAN_POINT('Ctrl Pts',(-23.1910794925251,68.1585453906257,
12.));
#156752=CARTESIAN_POINT('Ctrl Pts',(-23.1905642477571,68.1825806552129,
12.));
#156753=CARTESIAN_POINT('Ctrl Pts',(-23.1900246233165,68.2066576205116,
12.));
#156754=CARTESIAN_POINT('Ctrl Pts',(-23.1894605611871,68.2307761665633,
12.));
#156755=CARTESIAN_POINT('Ctrl Pts',(-23.1888720036757,68.2549361738681,
12.));
#156756=CARTESIAN_POINT('Ctrl Pts',(-23.1882588934107,68.2791375233795,
12.));
#156757=CARTESIAN_POINT('Ctrl Pts',(-23.1876211733436,68.3033800964939,
12.));
#156758=CARTESIAN_POINT('Ctrl Pts',(-23.1869587867459,68.3276637750485,
12.));
#156759=CARTESIAN_POINT('Ctrl Pts',(-23.186271677203,68.3519884413246,12.));
#156760=CARTESIAN_POINT('Ctrl Pts',(-23.1855597886116,68.376353978044,12.));
#156761=CARTESIAN_POINT('Ctrl Pts',(-23.1848230651776,68.4007602683652,
12.));
#156762=CARTESIAN_POINT('Ctrl Pts',(-23.1840614514192,68.4252071958729,
12.));
#156763=CARTESIAN_POINT('Ctrl Pts',(-23.183274892163,68.4496946445758,12.));
#156764=CARTESIAN_POINT('Ctrl Pts',(-23.1824633325385,68.4742224989099,
12.));
#156765=CARTESIAN_POINT('Ctrl Pts',(-23.1816267179751,68.4987906437356,
12.));
#156766=CARTESIAN_POINT('Ctrl Pts',(-23.180764994201,68.5233989643345,12.));
#156767=CARTESIAN_POINT('Ctrl Pts',(-23.179878107245,68.5480473463985,12.));
#156768=CARTESIAN_POINT('Ctrl Pts',(-23.1789660034342,68.5727356760278,
12.));
#156769=CARTESIAN_POINT('Ctrl Pts',(-23.1780286293875,68.597463839733,12.));
#156770=CARTESIAN_POINT('Ctrl Pts',(-23.1770659320138,68.6222317244341,
12.));
#156771=CARTESIAN_POINT('Ctrl Pts',(-23.1760778585092,68.6470392174564,
12.));
#156772=CARTESIAN_POINT('Ctrl Pts',(-23.1750643563601,68.6718862065216,
12.));
#156773=CARTESIAN_POINT('Ctrl Pts',(-23.1740253733417,68.696772579744,12.));
#156774=CARTESIAN_POINT('Ctrl Pts',(-23.172960857511,68.7216982256341,12.));
#156775=CARTESIAN_POINT('Ctrl Pts',(-23.1718707572043,68.746663033096,12.));
#156776=CARTESIAN_POINT('Ctrl Pts',(-23.170755021036,68.771666891425,12.));
#156777=CARTESIAN_POINT('Ctrl Pts',(-23.1696135978997,68.7967096902996,
12.));
#156778=CARTESIAN_POINT('Ctrl Pts',(-23.1684464369686,68.8217913197752,
12.));
#156779=CARTESIAN_POINT('Ctrl Pts',(-23.1672534876889,68.8469116702898,
12.));
#156780=CARTESIAN_POINT('Ctrl Pts',(-23.1660346997764,68.8720706326609,
12.));
#156781=CARTESIAN_POINT('Ctrl Pts',(-23.164790023215,68.8972680980842,12.));
#156782=CARTESIAN_POINT('Ctrl Pts',(-23.1635194082581,68.9225039581248,
12.));
#156783=CARTESIAN_POINT('Ctrl Pts',(-23.1622228054291,68.9477781047106,
12.));
#156784=CARTESIAN_POINT('Ctrl Pts',(-23.1609001655156,68.9730904301369,
12.));
#156785=CARTESIAN_POINT('Ctrl Pts',(-23.1595514395656,68.9984408270659,
12.));
#156786=CARTESIAN_POINT('Ctrl Pts',(-23.1581765788869,69.0238291885245,
12.));
#156787=CARTESIAN_POINT('Ctrl Pts',(-23.1567755350469,69.0492554078992,
12.));
#156788=CARTESIAN_POINT('Ctrl Pts',(-23.1553482598762,69.074719378928,12.));
#156789=CARTESIAN_POINT('Ctrl Pts',(-23.1538947054614,69.1002209957025,
12.));
#156790=CARTESIAN_POINT('Ctrl Pts',(-23.152414824141,69.1257601526687,12.));
#156791=CARTESIAN_POINT('Ctrl Pts',(-23.1509085685032,69.1513367446231,
12.));
#156792=CARTESIAN_POINT('Ctrl Pts',(-23.1493758913858,69.1769506667084,
12.));
#156793=CARTESIAN_POINT('Ctrl Pts',(-23.147816745879,69.2026018144028,12.));
#156794=CARTESIAN_POINT('Ctrl Pts',(-23.1462310853206,69.2282900835236,
12.));
#156795=CARTESIAN_POINT('Ctrl Pts',(-23.1446188632931,69.254015370231,12.));
#156796=CARTESIAN_POINT('Ctrl Pts',(-23.142980033622,69.2797775710273,12.));
#156797=CARTESIAN_POINT('Ctrl Pts',(-23.1413145503762,69.3055765827546,
12.));
#156798=CARTESIAN_POINT('Ctrl Pts',(-23.1396223678725,69.3314123025869,
12.));
#156799=CARTESIAN_POINT('Ctrl Pts',(-23.1379034406718,69.3572846280297,
12.));
#156800=CARTESIAN_POINT('Ctrl Pts',(-23.1361577235709,69.3831934569183,
12.));
#156801=CARTESIAN_POINT('Ctrl Pts',(-23.1343851715989,69.4091386874132,
12.));
#156802=CARTESIAN_POINT('Ctrl Pts',(-23.1325857400144,69.4351202179946,
12.));
#156803=CARTESIAN_POINT('Ctrl Pts',(-23.1307593843061,69.4611379474484,
12.));
#156804=CARTESIAN_POINT('Ctrl Pts',(-23.1289060601924,69.4871917748654,
12.));
#156805=CARTESIAN_POINT('Ctrl Pts',(-23.1270257236204,69.5132815996537,
12.));
#156806=CARTESIAN_POINT('Ctrl Pts',(-23.1251183307676,69.539407321546,12.));
#156807=CARTESIAN_POINT('Ctrl Pts',(-23.1231838380452,69.5655688406052,
12.));
#156808=CARTESIAN_POINT('Ctrl Pts',(-23.1212222021051,69.5917660572265,
12.));
#156809=CARTESIAN_POINT('Ctrl Pts',(-23.1192333798441,69.6179988721365,
12.));
#156810=CARTESIAN_POINT('Ctrl Pts',(-23.1172173283859,69.6442671863765,
12.));
#156811=CARTESIAN_POINT('Ctrl Pts',(-23.1151740050681,69.6705709012852,
12.));
#156812=CARTESIAN_POINT('Ctrl Pts',(-23.1131033674301,69.6969099184767,
12.));
#156813=CARTESIAN_POINT('Ctrl Pts',(-23.1110053732046,69.7232841398197,
12.));
#156814=CARTESIAN_POINT('Ctrl Pts',(-23.1088799803089,69.7496934674069,
12.));
#156815=CARTESIAN_POINT('Ctrl Pts',(-23.106727146861,69.7761378035964,12.));
#156816=CARTESIAN_POINT('Ctrl Pts',(-23.1045468311991,69.8026170510572,
12.));
#156817=CARTESIAN_POINT('Ctrl Pts',(-23.1023389919051,69.8291311128118,
12.));
#156818=CARTESIAN_POINT('Ctrl Pts',(-23.1001035878241,69.8556798922693,
12.));
#156819=CARTESIAN_POINT('Ctrl Pts',(-23.0978405781021,69.8822632932768,
12.));
#156820=CARTESIAN_POINT('Ctrl Pts',(-23.0955499221558,69.9088812200713,
12.));
#156821=CARTESIAN_POINT('Ctrl Pts',(-23.0932315796067,69.9355335771729,
12.));
#156822=CARTESIAN_POINT('Ctrl Pts',(-23.0908855102251,69.9622202692873,
12.));
#156823=CARTESIAN_POINT('Ctrl Pts',(-23.0885116738798,69.9889412012143,
12.));
#156824=CARTESIAN_POINT('Ctrl Pts',(-23.0861100304729,70.0156962777169,
12.));
#156825=CARTESIAN_POINT('Ctrl Pts',(-23.0836805399374,70.0424854035115,
12.));
#156826=CARTESIAN_POINT('Ctrl Pts',(-23.0812231623765,70.0693084835373,
12.));
#156827=CARTESIAN_POINT('Ctrl Pts',(-23.0787378581774,70.0961654231639,
12.));
#156828=CARTESIAN_POINT('Ctrl Pts',(-23.0762245881389,70.123056128422,12.));
#156829=CARTESIAN_POINT('Ctrl Pts',(-23.0736833135938,70.1499805062172,
12.));
#156830=CARTESIAN_POINT('Ctrl Pts',(-23.0711139965439,70.1769384645586,
12.));
#156831=CARTESIAN_POINT('Ctrl Pts',(-23.0685165993691,70.2039299120488,
12.));
#156832=CARTESIAN_POINT('Ctrl Pts',(-23.0658910845433,70.2309547573815,
12.));
#156833=CARTESIAN_POINT('Ctrl Pts',(-23.0632374143279,70.2580129087888,
12.));
#156834=CARTESIAN_POINT('Ctrl Pts',(-23.0605555505321,70.2851042736066,
12.));
#156835=CARTESIAN_POINT('Ctrl Pts',(-23.0578454541104,70.3122287575335,
12.));
#156836=CARTESIAN_POINT('Ctrl Pts',(-23.0551070854926,70.3393862652297,
12.));
#156837=CARTESIAN_POINT('Ctrl Pts',(-23.0523404053172,70.3665767016542,
12.));
#156838=CARTESIAN_POINT('Ctrl Pts',(-23.0495453750763,70.3937999732267,
12.));
#156839=CARTESIAN_POINT('Ctrl Pts',(-23.0467219577291,70.4210559889348,
12.));
#156840=CARTESIAN_POINT('Ctrl Pts',(-23.0438701185013,70.4483446617614,
12.));
#156841=CARTESIAN_POINT('Ctrl Pts',(-23.0409898250756,70.4756659090209,
12.));
#156842=CARTESIAN_POINT('Ctrl Pts',(-23.0384964376036,70.4991133648946,
12.));
#156843=CARTESIAN_POINT('Ctrl Pts',(-23.0365694096173,70.5171075702746,
12.));
#156844=CARTESIAN_POINT('Ctrl Pts',(-23.0352213647765,70.5296341535555,
12.));
#156845=CARTESIAN_POINT('Ctrl Pts',(-23.0344606623299,70.536683638166,12.));
#156846=CARTESIAN_POINT('Ctrl Pts',(-23.0342913834073,70.5382514078919,
12.));
#156847=CARTESIAN_POINT('',(-23.1372951448024,66.0656156664138,0.));
#156848=CARTESIAN_POINT('',(-23.1372951448024,66.0656156664138,0.));
#156849=CARTESIAN_POINT('Ctrl Pts',(-23.0342913834073,70.5382514078919,
0.));
#156850=CARTESIAN_POINT('Ctrl Pts',(-23.0344606623299,70.536683638166,0.));
#156851=CARTESIAN_POINT('Ctrl Pts',(-23.0352213647765,70.5296341535555,
0.));
#156852=CARTESIAN_POINT('Ctrl Pts',(-23.0365694096173,70.5171075702746,
0.));
#156853=CARTESIAN_POINT('Ctrl Pts',(-23.0384964376036,70.4991133648946,
0.));
#156854=CARTESIAN_POINT('Ctrl Pts',(-23.0409898250756,70.4756659090209,
0.));
#156855=CARTESIAN_POINT('Ctrl Pts',(-23.0438701185013,70.4483446617614,
0.));
#156856=CARTESIAN_POINT('Ctrl Pts',(-23.0467219577291,70.4210559889348,
0.));
#156857=CARTESIAN_POINT('Ctrl Pts',(-23.0495453750763,70.3937999732267,
0.));
#156858=CARTESIAN_POINT('Ctrl Pts',(-23.0523404053172,70.3665767016542,
0.));
#156859=CARTESIAN_POINT('Ctrl Pts',(-23.0551070854926,70.3393862652297,
0.));
#156860=CARTESIAN_POINT('Ctrl Pts',(-23.0578454541104,70.3122287575335,
0.));
#156861=CARTESIAN_POINT('Ctrl Pts',(-23.0605555505321,70.2851042736066,
0.));
#156862=CARTESIAN_POINT('Ctrl Pts',(-23.0632374143279,70.2580129087888,
0.));
#156863=CARTESIAN_POINT('Ctrl Pts',(-23.0658910845433,70.2309547573815,
0.));
#156864=CARTESIAN_POINT('Ctrl Pts',(-23.0685165993691,70.2039299120488,
0.));
#156865=CARTESIAN_POINT('Ctrl Pts',(-23.0711139965439,70.1769384645586,
0.));
#156866=CARTESIAN_POINT('Ctrl Pts',(-23.0736833135938,70.1499805062172,
0.));
#156867=CARTESIAN_POINT('Ctrl Pts',(-23.0762245881389,70.123056128422,0.));
#156868=CARTESIAN_POINT('Ctrl Pts',(-23.0787378581774,70.0961654231639,
0.));
#156869=CARTESIAN_POINT('Ctrl Pts',(-23.0812231623765,70.0693084835373,
0.));
#156870=CARTESIAN_POINT('Ctrl Pts',(-23.0836805399374,70.0424854035115,
0.));
#156871=CARTESIAN_POINT('Ctrl Pts',(-23.0861100304729,70.0156962777169,
0.));
#156872=CARTESIAN_POINT('Ctrl Pts',(-23.0885116738798,69.9889412012143,
0.));
#156873=CARTESIAN_POINT('Ctrl Pts',(-23.0908855102251,69.9622202692873,
0.));
#156874=CARTESIAN_POINT('Ctrl Pts',(-23.0932315796067,69.9355335771729,
0.));
#156875=CARTESIAN_POINT('Ctrl Pts',(-23.0955499221558,69.9088812200713,
0.));
#156876=CARTESIAN_POINT('Ctrl Pts',(-23.0978405781021,69.8822632932768,
0.));
#156877=CARTESIAN_POINT('Ctrl Pts',(-23.1001035878241,69.8556798922693,
0.));
#156878=CARTESIAN_POINT('Ctrl Pts',(-23.1023389919051,69.8291311128118,
0.));
#156879=CARTESIAN_POINT('Ctrl Pts',(-23.1045468311991,69.8026170510572,
0.));
#156880=CARTESIAN_POINT('Ctrl Pts',(-23.106727146861,69.7761378035964,0.));
#156881=CARTESIAN_POINT('Ctrl Pts',(-23.1088799803089,69.7496934674069,
0.));
#156882=CARTESIAN_POINT('Ctrl Pts',(-23.1110053732046,69.7232841398197,
0.));
#156883=CARTESIAN_POINT('Ctrl Pts',(-23.1131033674301,69.6969099184767,
0.));
#156884=CARTESIAN_POINT('Ctrl Pts',(-23.1151740050681,69.6705709012852,
0.));
#156885=CARTESIAN_POINT('Ctrl Pts',(-23.1172173283859,69.6442671863765,
0.));
#156886=CARTESIAN_POINT('Ctrl Pts',(-23.1192333798441,69.6179988721365,
0.));
#156887=CARTESIAN_POINT('Ctrl Pts',(-23.1212222021051,69.5917660572265,
0.));
#156888=CARTESIAN_POINT('Ctrl Pts',(-23.1231838380452,69.5655688406052,
0.));
#156889=CARTESIAN_POINT('Ctrl Pts',(-23.1251183307676,69.539407321546,0.));
#156890=CARTESIAN_POINT('Ctrl Pts',(-23.1270257236204,69.5132815996537,
0.));
#156891=CARTESIAN_POINT('Ctrl Pts',(-23.1289060601924,69.4871917748654,
0.));
#156892=CARTESIAN_POINT('Ctrl Pts',(-23.1307593843061,69.4611379474484,
0.));
#156893=CARTESIAN_POINT('Ctrl Pts',(-23.1325857400144,69.4351202179946,
0.));
#156894=CARTESIAN_POINT('Ctrl Pts',(-23.1343851715989,69.4091386874132,
0.));
#156895=CARTESIAN_POINT('Ctrl Pts',(-23.1361577235709,69.3831934569183,
0.));
#156896=CARTESIAN_POINT('Ctrl Pts',(-23.1379034406718,69.3572846280297,
0.));
#156897=CARTESIAN_POINT('Ctrl Pts',(-23.1396223678725,69.3314123025869,
0.));
#156898=CARTESIAN_POINT('Ctrl Pts',(-23.1413145503762,69.3055765827546,
0.));
#156899=CARTESIAN_POINT('Ctrl Pts',(-23.142980033622,69.2797775710273,0.));
#156900=CARTESIAN_POINT('Ctrl Pts',(-23.1446188632931,69.254015370231,0.));
#156901=CARTESIAN_POINT('Ctrl Pts',(-23.1462310853206,69.2282900835236,
0.));
#156902=CARTESIAN_POINT('Ctrl Pts',(-23.147816745879,69.2026018144028,0.));
#156903=CARTESIAN_POINT('Ctrl Pts',(-23.1493758913858,69.1769506667084,
0.));
#156904=CARTESIAN_POINT('Ctrl Pts',(-23.1509085685032,69.1513367446231,
0.));
#156905=CARTESIAN_POINT('Ctrl Pts',(-23.152414824141,69.1257601526687,0.));
#156906=CARTESIAN_POINT('Ctrl Pts',(-23.1538947054614,69.1002209957025,
0.));
#156907=CARTESIAN_POINT('Ctrl Pts',(-23.1553482598762,69.074719378928,0.));
#156908=CARTESIAN_POINT('Ctrl Pts',(-23.1567755350469,69.0492554078992,
0.));
#156909=CARTESIAN_POINT('Ctrl Pts',(-23.1581765788869,69.0238291885245,
0.));
#156910=CARTESIAN_POINT('Ctrl Pts',(-23.1595514395656,68.9984408270659,
0.));
#156911=CARTESIAN_POINT('Ctrl Pts',(-23.1609001655156,68.9730904301369,
0.));
#156912=CARTESIAN_POINT('Ctrl Pts',(-23.1622228054291,68.9477781047106,
0.));
#156913=CARTESIAN_POINT('Ctrl Pts',(-23.1635194082581,68.9225039581248,
0.));
#156914=CARTESIAN_POINT('Ctrl Pts',(-23.164790023215,68.8972680980842,0.));
#156915=CARTESIAN_POINT('Ctrl Pts',(-23.1660346997764,68.8720706326609,
0.));
#156916=CARTESIAN_POINT('Ctrl Pts',(-23.1672534876889,68.8469116702898,
0.));
#156917=CARTESIAN_POINT('Ctrl Pts',(-23.1684464369686,68.8217913197752,
0.));
#156918=CARTESIAN_POINT('Ctrl Pts',(-23.1696135978997,68.7967096902996,
0.));
#156919=CARTESIAN_POINT('Ctrl Pts',(-23.170755021036,68.771666891425,0.));
#156920=CARTESIAN_POINT('Ctrl Pts',(-23.1718707572043,68.746663033096,0.));
#156921=CARTESIAN_POINT('Ctrl Pts',(-23.172960857511,68.7216982256341,0.));
#156922=CARTESIAN_POINT('Ctrl Pts',(-23.1740253733417,68.696772579744,0.));
#156923=CARTESIAN_POINT('Ctrl Pts',(-23.1750643563601,68.6718862065216,
0.));
#156924=CARTESIAN_POINT('Ctrl Pts',(-23.1760778585092,68.6470392174564,
0.));
#156925=CARTESIAN_POINT('Ctrl Pts',(-23.1770659320138,68.6222317244341,
0.));
#156926=CARTESIAN_POINT('Ctrl Pts',(-23.1780286293875,68.597463839733,0.));
#156927=CARTESIAN_POINT('Ctrl Pts',(-23.1789660034342,68.5727356760278,
0.));
#156928=CARTESIAN_POINT('Ctrl Pts',(-23.179878107245,68.5480473463985,0.));
#156929=CARTESIAN_POINT('Ctrl Pts',(-23.180764994201,68.5233989643345,0.));
#156930=CARTESIAN_POINT('Ctrl Pts',(-23.1816267179751,68.4987906437356,
0.));
#156931=CARTESIAN_POINT('Ctrl Pts',(-23.1824633325385,68.4742224989099,
0.));
#156932=CARTESIAN_POINT('Ctrl Pts',(-23.183274892163,68.4496946445758,0.));
#156933=CARTESIAN_POINT('Ctrl Pts',(-23.1840614514192,68.4252071958729,
0.));
#156934=CARTESIAN_POINT('Ctrl Pts',(-23.1848230651776,68.4007602683652,
0.));
#156935=CARTESIAN_POINT('Ctrl Pts',(-23.1855597886116,68.376353978044,0.));
#156936=CARTESIAN_POINT('Ctrl Pts',(-23.186271677203,68.3519884413246,0.));
#156937=CARTESIAN_POINT('Ctrl Pts',(-23.1869587867459,68.3276637750485,
0.));
#156938=CARTESIAN_POINT('Ctrl Pts',(-23.1876211733436,68.3033800964939,
0.));
#156939=CARTESIAN_POINT('Ctrl Pts',(-23.1882588934107,68.2791375233795,
0.));
#156940=CARTESIAN_POINT('Ctrl Pts',(-23.1888720036757,68.2549361738681,
0.));
#156941=CARTESIAN_POINT('Ctrl Pts',(-23.1894605611871,68.2307761665633,
0.));
#156942=CARTESIAN_POINT('Ctrl Pts',(-23.1900246233165,68.2066576205116,
0.));
#156943=CARTESIAN_POINT('Ctrl Pts',(-23.1905642477571,68.1825806552129,
0.));
#156944=CARTESIAN_POINT('Ctrl Pts',(-23.1910794925251,68.1585453906257,
0.));
#156945=CARTESIAN_POINT('Ctrl Pts',(-23.1915704159623,68.1345519471695,
0.));
#156946=CARTESIAN_POINT('Ctrl Pts',(-23.1920370767425,68.110600445723,0.));
#156947=CARTESIAN_POINT('Ctrl Pts',(-23.1924795338749,68.0866910076251,
0.));
#156948=CARTESIAN_POINT('Ctrl Pts',(-23.1928978467021,68.0628237546863,
0.));
#156949=CARTESIAN_POINT('Ctrl Pts',(-23.1932920749023,68.0389988091933,
0.));
#156950=CARTESIAN_POINT('Ctrl Pts',(-23.1936622784919,68.0152162939121,
0.));
#156951=CARTESIAN_POINT('Ctrl Pts',(-23.1940085178313,67.991476332086,0.));
#156952=CARTESIAN_POINT('Ctrl Pts',(-23.1943308536297,67.9677790474385,
0.));
#156953=CARTESIAN_POINT('Ctrl Pts',(-23.1946293469427,67.9441245641842,
0.));
#156954=CARTESIAN_POINT('Ctrl Pts',(-23.1949040591744,67.9205130070324,
0.));
#156955=CARTESIAN_POINT('Ctrl Pts',(-23.1951550520802,67.8969445011916,
0.));
#156956=CARTESIAN_POINT('Ctrl Pts',(-23.1953823877734,67.8734191723667,
0.));
#156957=CARTESIAN_POINT('Ctrl Pts',(-23.1955861287286,67.8499371467616,
0.));
#156958=CARTESIAN_POINT('Ctrl Pts',(-23.1957663377806,67.8264985510917,
0.));
#156959=CARTESIAN_POINT('Ctrl Pts',(-23.1959230781269,67.8031035125887,
0.));
#156960=CARTESIAN_POINT('Ctrl Pts',(-23.1960564133304,67.7797521590045,
0.));
#156961=CARTESIAN_POINT('Ctrl Pts',(-23.1961664073262,67.7564446186079,
0.));
#156962=CARTESIAN_POINT('Ctrl Pts',(-23.1962531244245,67.7331810201883,
0.));
#156963=CARTESIAN_POINT('Ctrl Pts',(-23.1963166293102,67.7099614930671,
0.));
#156964=CARTESIAN_POINT('Ctrl Pts',(-23.1963569870451,67.6867861671031,
0.));
#156965=CARTESIAN_POINT('Ctrl Pts',(-23.1963742630714,67.6636551726964,
0.));
#156966=CARTESIAN_POINT('Ctrl Pts',(-23.1963685232187,67.6405686407863,
0.));
#156967=CARTESIAN_POINT('Ctrl Pts',(-23.1963398337068,67.6175267028555,
0.));
#156968=CARTESIAN_POINT('Ctrl Pts',(-23.1962882611453,67.5945294909426,
0.));
#156969=CARTESIAN_POINT('Ctrl Pts',(-23.196213872536,67.5715771376461,0.));
#156970=CARTESIAN_POINT('Ctrl Pts',(-23.1961167352772,67.5486697761288,
0.));
#156971=CARTESIAN_POINT('Ctrl Pts',(-23.1959969171701,67.5258075401146,
0.));
#156972=CARTESIAN_POINT('Ctrl Pts',(-23.1958544864215,67.5029905638949,
0.));
#156973=CARTESIAN_POINT('Ctrl Pts',(-23.195689511644,67.4802189823408,0.));
#156974=CARTESIAN_POINT('Ctrl Pts',(-23.195502061859,67.4574929309076,0.));
#156975=CARTESIAN_POINT('Ctrl Pts',(-23.1952922065012,67.4348125456398,
0.));
#156976=CARTESIAN_POINT('Ctrl Pts',(-23.1950600154265,67.412177963168,0.));
#156977=CARTESIAN_POINT('Ctrl Pts',(-23.1948055589129,67.3895893207182,
0.));
#156978=CARTESIAN_POINT('Ctrl Pts',(-23.194528907661,67.3670467561212,0.));
#156979=CARTESIAN_POINT('Ctrl Pts',(-23.1942301327978,67.3445504078176,
0.));
#156980=CARTESIAN_POINT('Ctrl Pts',(-23.1939093058801,67.3221004148603,
0.));
#156981=CARTESIAN_POINT('Ctrl Pts',(-23.1935664989018,67.2996969169098,
0.));
#156982=CARTESIAN_POINT('Ctrl Pts',(-23.1932017842953,67.2773400542477,
0.));
#156983=CARTESIAN_POINT('Ctrl Pts',(-23.1928152349343,67.2550299677888,
0.));
#156984=CARTESIAN_POINT('Ctrl Pts',(-23.1924069241385,67.232766799088,0.));
#156985=CARTESIAN_POINT('Ctrl Pts',(-23.1919769256803,67.2105506903447,
0.));
#156986=CARTESIAN_POINT('Ctrl Pts',(-23.1915253137924,67.1883817844038,
0.));
#156987=CARTESIAN_POINT('Ctrl Pts',(-23.1910521631657,67.1662602247639,
0.));
#156988=CARTESIAN_POINT('Ctrl Pts',(-23.1905575489504,67.1441861555817,
0.));
#156989=CARTESIAN_POINT('Ctrl Pts',(-23.1900415467574,67.1221597216741,
0.));
#156990=CARTESIAN_POINT('Ctrl Pts',(-23.1895042326626,67.1001810685143,
0.));
#156991=CARTESIAN_POINT('Ctrl Pts',(-23.1889456832119,67.0782503422305,
0.));
#156992=CARTESIAN_POINT('Ctrl Pts',(-23.1883659754271,67.0563676896325,
0.));
#156993=CARTESIAN_POINT('Ctrl Pts',(-23.1877651868158,67.0345332582306,
0.));
#156994=CARTESIAN_POINT('Ctrl Pts',(-23.1871433953793,67.0127471962501,
0.));
#156995=CARTESIAN_POINT('Ctrl Pts',(-23.1865006796283,66.9910096526462,
0.));
#156996=CARTESIAN_POINT('Ctrl Pts',(-23.1858371185842,66.9693207771031,
0.));
#156997=CARTESIAN_POINT('Ctrl Pts',(-23.1851527917657,66.9476807200203,
0.));
#156998=CARTESIAN_POINT('Ctrl Pts',(-23.1844477791814,66.9260896324949,
0.));
#156999=CARTESIAN_POINT('Ctrl Pts',(-23.1837221613235,66.9045476663063,
0.));
#157000=CARTESIAN_POINT('Ctrl Pts',(-23.1829760191591,66.8830549738795,
0.));
#157001=CARTESIAN_POINT('Ctrl Pts',(-23.1822094341517,66.8616117083331,
0.));
#157002=CARTESIAN_POINT('Ctrl Pts',(-23.1814224882953,66.8402180235566,
0.));
#157003=CARTESIAN_POINT('Ctrl Pts',(-23.1806152641475,66.8188740742727,
0.));
#157004=CARTESIAN_POINT('Ctrl Pts',(-23.1797878448639,66.7975800161,0.));
#157005=CARTESIAN_POINT('Ctrl Pts',(-23.1789403142366,66.776336005612,0.));
#157006=CARTESIAN_POINT('Ctrl Pts',(-23.17807275663,66.7551422002204,0.));
#157007=CARTESIAN_POINT('Ctrl Pts',(-23.1771852569131,66.7339987580427,
0.));
#157008=CARTESIAN_POINT('Ctrl Pts',(-23.1762779004044,66.7129058377896,
0.));
#157009=CARTESIAN_POINT('Ctrl Pts',(-23.1753507727939,66.6918635985972,
0.));
#157010=CARTESIAN_POINT('Ctrl Pts',(-23.1744039601382,66.6708722000079,
0.));
#157011=CARTESIAN_POINT('Ctrl Pts',(-23.1734375490431,66.6499318023473,
0.));
#157012=CARTESIAN_POINT('Ctrl Pts',(-23.1724516268302,66.6290425670548,
0.));
#157013=CARTESIAN_POINT('Ctrl Pts',(-23.1714462816789,66.6082046569644,
0.));
#157014=CARTESIAN_POINT('Ctrl Pts',(-23.1704216028614,66.5874182367563,
0.));
#157015=CARTESIAN_POINT('Ctrl Pts',(-23.1693776805866,66.5666834726454,
0.));
#157016=CARTESIAN_POINT('Ctrl Pts',(-23.1683146055726,66.5460005315376,
0.));
#157017=CARTESIAN_POINT('Ctrl Pts',(-23.1672324686926,66.5253695803205,
0.));
#157018=CARTESIAN_POINT('Ctrl Pts',(-23.1661313606132,66.5047907851348,
0.));
#157019=CARTESIAN_POINT('Ctrl Pts',(-23.1650113713808,66.4842643105311,
0.));
#157020=CARTESIAN_POINT('Ctrl Pts',(-23.1638725912195,66.4637903210727,
0.));
#157021=CARTESIAN_POINT('Ctrl Pts',(-23.1627151114883,66.4433689832478,
0.));
#157022=CARTESIAN_POINT('Ctrl Pts',(-23.1615390254632,66.4230004670278,
0.));
#157023=CARTESIAN_POINT('Ctrl Pts',(-23.160344429474,66.4026849481232,0.));
#157024=CARTESIAN_POINT('Ctrl Pts',(-23.1591314230083,66.3824226081802,
0.));
#157025=CARTESIAN_POINT('Ctrl Pts',(-23.1579001063424,66.3622136300654,
0.));
#157026=CARTESIAN_POINT('Ctrl Pts',(-23.1566505784621,66.3420581937147,
0.));
#157027=CARTESIAN_POINT('Ctrl Pts',(-23.1553829352539,66.3219564725184,
0.));
#157028=CARTESIAN_POINT('Ctrl Pts',(-23.1540972666191,66.3019086275444,
0.));
#157029=CARTESIAN_POINT('Ctrl Pts',(-23.1527936592651,66.281914813114,0.));
#157030=CARTESIAN_POINT('Ctrl Pts',(-23.1514722022503,66.2619751878793,
0.));
#157031=CARTESIAN_POINT('Ctrl Pts',(-23.1501329914487,66.2420899237318,
0.));
#157032=CARTESIAN_POINT('Ctrl Pts',(-23.1487761349298,66.2222592165398,
0.));
#157033=CARTESIAN_POINT('Ctrl Pts',(-23.147401756643,66.2024832934733,0.));
#157034=CARTESIAN_POINT('Ctrl Pts',(-23.1460099850704,66.1827623902755,
0.));
#157035=CARTESIAN_POINT('Ctrl Pts',(-23.1446009424871,66.163096729667,0.));
#157036=CARTESIAN_POINT('Ctrl Pts',(-23.1431747350127,66.14348650151,0.));
#157037=CARTESIAN_POINT('Ctrl Pts',(-23.1417314398501,66.1239318368803,
0.));
#157038=CARTESIAN_POINT('Ctrl Pts',(-23.140271103958,66.1044328067739,0.));
#157039=CARTESIAN_POINT('Ctrl Pts',(-23.1390892229923,66.0888781152779,
0.));
#157040=CARTESIAN_POINT('Ctrl Pts',(-23.1381951597491,66.0772371487475,
0.));
#157041=CARTESIAN_POINT('Ctrl Pts',(-23.1375957166138,66.0694876382212,
0.));
#157042=CARTESIAN_POINT('Ctrl Pts',(-23.1372951448024,66.0656156664138,
0.));
#157043=CARTESIAN_POINT('Ctrl Pts',(-16.7341474417544,72.5962692526112,
0.));
#157044=CARTESIAN_POINT('Ctrl Pts',(-16.7341474417544,72.5962692526112,
12.));
#157045=CARTESIAN_POINT('Ctrl Pts',(-16.7352885767485,72.5907910746008,
0.));
#157046=CARTESIAN_POINT('Ctrl Pts',(-16.7352885767485,72.5907910746008,
12.));
#157047=CARTESIAN_POINT('Ctrl Pts',(-16.7375676985344,72.5798376087774,
0.));
#157048=CARTESIAN_POINT('Ctrl Pts',(-16.7375676985344,72.5798376087774,
12.));
#157049=CARTESIAN_POINT('Ctrl Pts',(-16.7409769366072,72.5634160806351,
0.));
#157050=CARTESIAN_POINT('Ctrl Pts',(-16.7409769366072,72.5634160806351,
12.));
#157051=CARTESIAN_POINT('Ctrl Pts',(-16.7455036973866,72.5415380516637,
0.));
#157052=CARTESIAN_POINT('Ctrl Pts',(-16.7455036973866,72.5415380516637,
12.));
#157053=CARTESIAN_POINT('Ctrl Pts',(-16.7511306618915,72.514219427383,0.));
#157054=CARTESIAN_POINT('Ctrl Pts',(-16.7511306618915,72.514219427383,12.));
#157055=CARTESIAN_POINT('Ctrl Pts',(-16.7567261380687,72.4869297342427,
0.));
#157056=CARTESIAN_POINT('Ctrl Pts',(-16.7567261380687,72.4869297342427,
12.));
#157057=CARTESIAN_POINT('Ctrl Pts',(-16.7622901280758,72.4596690055437,
0.));
#157058=CARTESIAN_POINT('Ctrl Pts',(-16.7622901280758,72.4596690055437,
12.));
#157059=CARTESIAN_POINT('Ctrl Pts',(-16.7678226404162,72.4324372916746,
0.));
#157060=CARTESIAN_POINT('Ctrl Pts',(-16.7678226404162,72.4324372916746,
12.));
#157061=CARTESIAN_POINT('Ctrl Pts',(-16.7733236932135,72.4052346647799,
0.));
#157062=CARTESIAN_POINT('Ctrl Pts',(-16.7733236932135,72.4052346647799,
12.));
#157063=CARTESIAN_POINT('Ctrl Pts',(-16.7787933137498,72.3780612167786,
0.));
#157064=CARTESIAN_POINT('Ctrl Pts',(-16.7787933137498,72.3780612167786,
12.));
#157065=CARTESIAN_POINT('Ctrl Pts',(-16.7842315351363,72.3509170522838,
0.));
#157066=CARTESIAN_POINT('Ctrl Pts',(-16.7842315351363,72.3509170522838,
12.));
#157067=CARTESIAN_POINT('Ctrl Pts',(-16.7896383937822,72.3238022829223,
0.));
#157068=CARTESIAN_POINT('Ctrl Pts',(-16.7896383937822,72.3238022829223,
12.));
#157069=CARTESIAN_POINT('Ctrl Pts',(-16.7950139266122,72.2967170212353,
0.));
#157070=CARTESIAN_POINT('Ctrl Pts',(-16.7950139266122,72.2967170212353,
12.));
#157071=CARTESIAN_POINT('Ctrl Pts',(-16.8003581682248,72.2696613743782,
0.));
#157072=CARTESIAN_POINT('Ctrl Pts',(-16.8003581682248,72.2696613743782,
12.));
#157073=CARTESIAN_POINT('Ctrl Pts',(-16.8056711485821,72.2426354390213,
0.));
#157074=CARTESIAN_POINT('Ctrl Pts',(-16.8056711485821,72.2426354390213,
12.));
#157075=CARTESIAN_POINT('Ctrl Pts',(-16.8109528945896,72.2156393048975,
0.));
#157076=CARTESIAN_POINT('Ctrl Pts',(-16.8109528945896,72.2156393048975,
12.));
#157077=CARTESIAN_POINT('Ctrl Pts',(-16.8162034312269,72.1886730573452,
0.));
#157078=CARTESIAN_POINT('Ctrl Pts',(-16.8162034312269,72.1886730573452,
12.));
#157079=CARTESIAN_POINT('Ctrl Pts',(-16.8214227828943,72.1617367803235,
0.));
#157080=CARTESIAN_POINT('Ctrl Pts',(-16.8214227828943,72.1617367803235,
12.));
#157081=CARTESIAN_POINT('Ctrl Pts',(-16.8266109745795,72.13483055902,0.));
#157082=CARTESIAN_POINT('Ctrl Pts',(-16.8266109745795,72.13483055902,12.));
#157083=CARTESIAN_POINT('Ctrl Pts',(-16.8317680333404,72.1079544831513,
0.));
#157084=CARTESIAN_POINT('Ctrl Pts',(-16.8317680333404,72.1079544831513,
12.));
#157085=CARTESIAN_POINT('Ctrl Pts',(-16.8368939881446,72.0811086466121,
0.));
#157086=CARTESIAN_POINT('Ctrl Pts',(-16.8368939881446,72.0811086466121,
12.));
#157087=CARTESIAN_POINT('Ctrl Pts',(-16.8419888691976,72.0542931459825,
0.));
#157088=CARTESIAN_POINT('Ctrl Pts',(-16.8419888691976,72.0542931459825,
12.));
#157089=CARTESIAN_POINT('Ctrl Pts',(-16.8470527074275,72.0275080793727,
0.));
#157090=CARTESIAN_POINT('Ctrl Pts',(-16.8470527074275,72.0275080793727,
12.));
#157091=CARTESIAN_POINT('Ctrl Pts',(-16.8520855339446,72.0007535452081,
0.));
#157092=CARTESIAN_POINT('Ctrl Pts',(-16.8520855339446,72.0007535452081,
12.));
#157093=CARTESIAN_POINT('Ctrl Pts',(-16.8570873794269,71.9740296408347,
0.));
#157094=CARTESIAN_POINT('Ctrl Pts',(-16.8570873794269,71.9740296408347,
12.));
#157095=CARTESIAN_POINT('Ctrl Pts',(-16.8620582738437,71.9473364618922,
0.));
#157096=CARTESIAN_POINT('Ctrl Pts',(-16.8620582738437,71.9473364618922,
12.));
#157097=CARTESIAN_POINT('Ctrl Pts',(-16.866998246792,71.9206741030887,0.));
#157098=CARTESIAN_POINT('Ctrl Pts',(-16.866998246792,71.9206741030887,12.));
#157099=CARTESIAN_POINT('Ctrl Pts',(-16.871907327697,71.8940426586534,0.));
#157100=CARTESIAN_POINT('Ctrl Pts',(-16.871907327697,71.8940426586534,12.));
#157101=CARTESIAN_POINT('Ctrl Pts',(-16.87678554607,71.867442222915,0.));
#157102=CARTESIAN_POINT('Ctrl Pts',(-16.87678554607,71.867442222915,12.));
#157103=CARTESIAN_POINT('Ctrl Pts',(-16.881632931747,71.8408728908258,0.));
#157104=CARTESIAN_POINT('Ctrl Pts',(-16.881632931747,71.8408728908258,12.));
#157105=CARTESIAN_POINT('Ctrl Pts',(-16.8864495151344,71.8143347584962,
0.));
#157106=CARTESIAN_POINT('Ctrl Pts',(-16.8864495151344,71.8143347584962,
12.));
#157107=CARTESIAN_POINT('Ctrl Pts',(-16.8912353270942,71.7878279229546,
0.));
#157108=CARTESIAN_POINT('Ctrl Pts',(-16.8912353270942,71.7878279229546,
12.));
#157109=CARTESIAN_POINT('Ctrl Pts',(-16.895990398841,71.7613524819235,0.));
#157110=CARTESIAN_POINT('Ctrl Pts',(-16.895990398841,71.7613524819235,12.));
#157111=CARTESIAN_POINT('Ctrl Pts',(-16.9007147618344,71.7349085335796,
0.));
#157112=CARTESIAN_POINT('Ctrl Pts',(-16.9007147618344,71.7349085335796,
12.));
#157113=CARTESIAN_POINT('Ctrl Pts',(-16.9054084476847,71.7084961763357,
0.));
#157114=CARTESIAN_POINT('Ctrl Pts',(-16.9054084476847,71.7084961763357,
12.));
#157115=CARTESIAN_POINT('Ctrl Pts',(-16.9100714880368,71.6821155085612,
0.));
#157116=CARTESIAN_POINT('Ctrl Pts',(-16.9100714880368,71.6821155085612,
12.));
#157117=CARTESIAN_POINT('Ctrl Pts',(-16.9147039145717,71.6557666285917,
0.));
#157118=CARTESIAN_POINT('Ctrl Pts',(-16.9147039145717,71.6557666285917,
12.));
#157119=CARTESIAN_POINT('Ctrl Pts',(-16.9193057590607,71.6294496348653,
0.));
#157120=CARTESIAN_POINT('Ctrl Pts',(-16.9193057590607,71.6294496348653,
12.));
#157121=CARTESIAN_POINT('Ctrl Pts',(-16.9238770534071,71.6031646260174,
0.));
#157122=CARTESIAN_POINT('Ctrl Pts',(-16.9238770534071,71.6031646260174,
12.));
#157123=CARTESIAN_POINT('Ctrl Pts',(-16.9284178296933,71.5769117009842,
0.));
#157124=CARTESIAN_POINT('Ctrl Pts',(-16.9284178296933,71.5769117009842,
12.));
#157125=CARTESIAN_POINT('Ctrl Pts',(-16.9329281202377,71.5506909591129,
0.));
#157126=CARTESIAN_POINT('Ctrl Pts',(-16.9329281202377,71.5506909591129,
12.));
#157127=CARTESIAN_POINT('Ctrl Pts',(-16.9374079576201,71.5245025002139,
0.));
#157128=CARTESIAN_POINT('Ctrl Pts',(-16.9374079576201,71.5245025002139,
12.));
#157129=CARTESIAN_POINT('Ctrl Pts',(-16.9418573746489,71.4983464245055,
0.));
#157130=CARTESIAN_POINT('Ctrl Pts',(-16.9418573746489,71.4983464245055,
12.));
#157131=CARTESIAN_POINT('Ctrl Pts',(-16.9462764043443,71.4722228325794,
0.));
#157132=CARTESIAN_POINT('Ctrl Pts',(-16.9462764043443,71.4722228325794,
12.));
#157133=CARTESIAN_POINT('Ctrl Pts',(-16.9506650799189,71.4461318253563,
0.));
#157134=CARTESIAN_POINT('Ctrl Pts',(-16.9506650799189,71.4461318253563,
12.));
#157135=CARTESIAN_POINT('Ctrl Pts',(-16.9550234347621,71.4200735040384,
0.));
#157136=CARTESIAN_POINT('Ctrl Pts',(-16.9550234347621,71.4200735040384,
12.));
#157137=CARTESIAN_POINT('Ctrl Pts',(-16.9593515024276,71.3940479700677,
0.));
#157138=CARTESIAN_POINT('Ctrl Pts',(-16.9593515024276,71.3940479700677,
12.));
#157139=CARTESIAN_POINT('Ctrl Pts',(-16.9636493166397,71.3680553251562,
0.));
#157140=CARTESIAN_POINT('Ctrl Pts',(-16.9636493166397,71.3680553251562,
12.));
#157141=CARTESIAN_POINT('Ctrl Pts',(-16.9679169112994,71.3420956713082,
0.));
#157142=CARTESIAN_POINT('Ctrl Pts',(-16.9679169112994,71.3420956713082,
12.));
#157143=CARTESIAN_POINT('Ctrl Pts',(-16.9721543204951,71.3161691108427,
0.));
#157144=CARTESIAN_POINT('Ctrl Pts',(-16.9721543204951,71.3161691108427,
12.));
#157145=CARTESIAN_POINT('Ctrl Pts',(-16.9763615785137,71.290275746412,0.));
#157146=CARTESIAN_POINT('Ctrl Pts',(-16.9763615785137,71.290275746412,12.));
#157147=CARTESIAN_POINT('Ctrl Pts',(-16.9805387198571,71.2644156810198,
0.));
#157148=CARTESIAN_POINT('Ctrl Pts',(-16.9805387198571,71.2644156810198,
12.));
#157149=CARTESIAN_POINT('Ctrl Pts',(-16.9846857792384,71.2385890180221,
0.));
#157150=CARTESIAN_POINT('Ctrl Pts',(-16.9846857792384,71.2385890180221,
12.));
#157151=CARTESIAN_POINT('Ctrl Pts',(-16.9888027915742,71.212795861124,0.));
#157152=CARTESIAN_POINT('Ctrl Pts',(-16.9888027915742,71.212795861124,12.));
#157153=CARTESIAN_POINT('Ctrl Pts',(-16.9928897919828,71.187036314374,0.));
#157154=CARTESIAN_POINT('Ctrl Pts',(-16.9928897919828,71.187036314374,12.));
#157155=CARTESIAN_POINT('Ctrl Pts',(-16.9969468157824,71.1613104821568,
0.));
#157156=CARTESIAN_POINT('Ctrl Pts',(-16.9969468157824,71.1613104821568,
12.));
#157157=CARTESIAN_POINT('Ctrl Pts',(-17.0009738984936,71.1356184691806,
0.));
#157158=CARTESIAN_POINT('Ctrl Pts',(-17.0009738984936,71.1356184691806,
12.));
#157159=CARTESIAN_POINT('Ctrl Pts',(-17.0049710758394,71.1099603804786,
0.));
#157160=CARTESIAN_POINT('Ctrl Pts',(-17.0049710758394,71.1099603804786,
12.));
#157161=CARTESIAN_POINT('Ctrl Pts',(-17.0089383837437,71.0843363214221,
0.));
#157162=CARTESIAN_POINT('Ctrl Pts',(-17.0089383837437,71.0843363214221,
12.));
#157163=CARTESIAN_POINT('Ctrl Pts',(-17.0128758583335,71.0587463977268,
0.));
#157164=CARTESIAN_POINT('Ctrl Pts',(-17.0128758583335,71.0587463977268,
12.));
#157165=CARTESIAN_POINT('Ctrl Pts',(-17.0167835359419,71.0331907154574,
0.));
#157166=CARTESIAN_POINT('Ctrl Pts',(-17.0167835359419,71.0331907154574,
12.));
#157167=CARTESIAN_POINT('Ctrl Pts',(-17.0206614531166,71.0076693810301,
0.));
#157168=CARTESIAN_POINT('Ctrl Pts',(-17.0206614531166,71.0076693810301,
12.));
#157169=CARTESIAN_POINT('Ctrl Pts',(-17.0245096466229,70.9821825012136,
0.));
#157170=CARTESIAN_POINT('Ctrl Pts',(-17.0245096466229,70.9821825012136,
12.));
#157171=CARTESIAN_POINT('Ctrl Pts',(-17.0283281534392,70.956730183136,0.));
#157172=CARTESIAN_POINT('Ctrl Pts',(-17.0283281534392,70.956730183136,12.));
#157173=CARTESIAN_POINT('Ctrl Pts',(-17.0321170107564,70.9313125342876,
0.));
#157174=CARTESIAN_POINT('Ctrl Pts',(-17.0321170107564,70.9313125342876,
12.));
#157175=CARTESIAN_POINT('Ctrl Pts',(-17.0358762559786,70.9059296625214,
0.));
#157176=CARTESIAN_POINT('Ctrl Pts',(-17.0358762559786,70.9059296625214,
12.));
#157177=CARTESIAN_POINT('Ctrl Pts',(-17.0396059267277,70.8805816760501,
0.));
#157178=CARTESIAN_POINT('Ctrl Pts',(-17.0396059267277,70.8805816760501,
12.));
#157179=CARTESIAN_POINT('Ctrl Pts',(-17.0433060608475,70.8552686834423,
0.));
#157180=CARTESIAN_POINT('Ctrl Pts',(-17.0433060608475,70.8552686834423,
12.));
#157181=CARTESIAN_POINT('Ctrl Pts',(-17.0469766964001,70.8299907936334,
0.));
#157182=CARTESIAN_POINT('Ctrl Pts',(-17.0469766964001,70.8299907936334,
12.));
#157183=CARTESIAN_POINT('Ctrl Pts',(-17.0506178716662,70.8047481159298,
0.));
#157184=CARTESIAN_POINT('Ctrl Pts',(-17.0506178716662,70.8047481159298,
12.));
#157185=CARTESIAN_POINT('Ctrl Pts',(-17.0542296251462,70.7795407600127,
0.));
#157186=CARTESIAN_POINT('Ctrl Pts',(-17.0542296251462,70.7795407600127,
12.));
#157187=CARTESIAN_POINT('Ctrl Pts',(-17.0578119955651,70.754368835938,0.));
#157188=CARTESIAN_POINT('Ctrl Pts',(-17.0578119955651,70.754368835938,12.));
#157189=CARTESIAN_POINT('Ctrl Pts',(-17.0613650218789,70.7292324541348,
0.));
#157190=CARTESIAN_POINT('Ctrl Pts',(-17.0613650218789,70.7292324541348,
12.));
#157191=CARTESIAN_POINT('Ctrl Pts',(-17.0648887432714,70.7041317254128,
0.));
#157192=CARTESIAN_POINT('Ctrl Pts',(-17.0648887432714,70.7041317254128,
12.));
#157193=CARTESIAN_POINT('Ctrl Pts',(-17.0683831991532,70.6790667609678,
0.));
#157194=CARTESIAN_POINT('Ctrl Pts',(-17.0683831991532,70.6790667609678,
12.));
#157195=CARTESIAN_POINT('Ctrl Pts',(-17.0718484291623,70.6540376723839,
0.));
#157196=CARTESIAN_POINT('Ctrl Pts',(-17.0718484291623,70.6540376723839,
12.));
#157197=CARTESIAN_POINT('Ctrl Pts',(-17.0752844731679,70.6290445716341,
0.));
#157198=CARTESIAN_POINT('Ctrl Pts',(-17.0752844731679,70.6290445716341,
12.));
#157199=CARTESIAN_POINT('Ctrl Pts',(-17.0786913712767,70.6040875710762,
0.));
#157200=CARTESIAN_POINT('Ctrl Pts',(-17.0786913712767,70.6040875710762,
12.));
#157201=CARTESIAN_POINT('Ctrl Pts',(-17.0820691638314,70.5791667834599,
0.));
#157202=CARTESIAN_POINT('Ctrl Pts',(-17.0820691638314,70.5791667834599,
12.));
#157203=CARTESIAN_POINT('Ctrl Pts',(-17.085417891409,70.5542823219346,0.));
#157204=CARTESIAN_POINT('Ctrl Pts',(-17.085417891409,70.5542823219346,12.));
#157205=CARTESIAN_POINT('Ctrl Pts',(-17.0887375948221,70.5294343000516,
0.));
#157206=CARTESIAN_POINT('Ctrl Pts',(-17.0887375948221,70.5294343000516,
12.));
#157207=CARTESIAN_POINT('Ctrl Pts',(-17.0920283151217,70.5046228317669,
0.));
#157208=CARTESIAN_POINT('Ctrl Pts',(-17.0920283151217,70.5046228317669,
12.));
#157209=CARTESIAN_POINT('Ctrl Pts',(-17.0952900936044,70.4798480314364,
0.));
#157210=CARTESIAN_POINT('Ctrl Pts',(-17.0952900936044,70.4798480314364,
12.));
#157211=CARTESIAN_POINT('Ctrl Pts',(-17.098522971812,70.4551100138221,0.));
#157212=CARTESIAN_POINT('Ctrl Pts',(-17.098522971812,70.4551100138221,12.));
#157213=CARTESIAN_POINT('Ctrl Pts',(-17.1017269915289,70.4304088940998,
0.));
#157214=CARTESIAN_POINT('Ctrl Pts',(-17.1017269915289,70.4304088940998,
12.));
#157215=CARTESIAN_POINT('Ctrl Pts',(-17.1049021947833,70.4057447878621,
0.));
#157216=CARTESIAN_POINT('Ctrl Pts',(-17.1049021947833,70.4057447878621,
12.));
#157217=CARTESIAN_POINT('Ctrl Pts',(-17.10804862385,70.3811178111206,0.));
#157218=CARTESIAN_POINT('Ctrl Pts',(-17.10804862385,70.3811178111206,12.));
#157219=CARTESIAN_POINT('Ctrl Pts',(-17.111166321257,70.356528080303,0.));
#157220=CARTESIAN_POINT('Ctrl Pts',(-17.111166321257,70.356528080303,12.));
#157221=CARTESIAN_POINT('Ctrl Pts',(-17.1142553297869,70.3319757122577,
0.));
#157222=CARTESIAN_POINT('Ctrl Pts',(-17.1142553297869,70.3319757122577,
12.));
#157223=CARTESIAN_POINT('Ctrl Pts',(-17.1173156924734,70.3074608242613,
0.));
#157224=CARTESIAN_POINT('Ctrl Pts',(-17.1173156924734,70.3074608242613,
12.));
#157225=CARTESIAN_POINT('Ctrl Pts',(-17.1203474526031,70.2829835340239,
0.));
#157226=CARTESIAN_POINT('Ctrl Pts',(-17.1203474526031,70.2829835340239,
12.));
#157227=CARTESIAN_POINT('Ctrl Pts',(-17.1233506537176,70.2585439596899,
0.));
#157228=CARTESIAN_POINT('Ctrl Pts',(-17.1233506537176,70.2585439596899,
12.));
#157229=CARTESIAN_POINT('Ctrl Pts',(-17.1263253396202,70.2341422198363,
0.));
#157230=CARTESIAN_POINT('Ctrl Pts',(-17.1263253396202,70.2341422198363,
12.));
#157231=CARTESIAN_POINT('Ctrl Pts',(-17.1292715543779,70.2097784334749,
0.));
#157232=CARTESIAN_POINT('Ctrl Pts',(-17.1292715543779,70.2097784334749,
12.));
#157233=CARTESIAN_POINT('Ctrl Pts',(-17.1321893423183,70.1854527200636,
0.));
#157234=CARTESIAN_POINT('Ctrl Pts',(-17.1321893423183,70.1854527200636,
12.));
#157235=CARTESIAN_POINT('Ctrl Pts',(-17.1350787480313,70.1611651995085,
0.));
#157236=CARTESIAN_POINT('Ctrl Pts',(-17.1350787480313,70.1611651995085,
12.));
#157237=CARTESIAN_POINT('Ctrl Pts',(-17.1379398163708,70.1369159921686,
0.));
#157238=CARTESIAN_POINT('Ctrl Pts',(-17.1379398163708,70.1369159921686,
12.));
#157239=CARTESIAN_POINT('Ctrl Pts',(-17.1407725924615,70.1127052188515,
0.));
#157240=CARTESIAN_POINT('Ctrl Pts',(-17.1407725924615,70.1127052188515,
12.));
#157241=CARTESIAN_POINT('Ctrl Pts',(-17.1435771217015,70.0885330008169,
0.));
#157242=CARTESIAN_POINT('Ctrl Pts',(-17.1435771217015,70.0885330008169,
12.));
#157243=CARTESIAN_POINT('Ctrl Pts',(-17.1463534497592,70.0643994597865,
0.));
#157244=CARTESIAN_POINT('Ctrl Pts',(-17.1463534497592,70.0643994597865,
12.));
#157245=CARTESIAN_POINT('Ctrl Pts',(-17.1491016225748,70.0403047179481,
0.));
#157246=CARTESIAN_POINT('Ctrl Pts',(-17.1491016225748,70.0403047179481,
12.));
#157247=CARTESIAN_POINT('Ctrl Pts',(-17.1518216863624,70.0162488979587,
0.));
#157248=CARTESIAN_POINT('Ctrl Pts',(-17.1518216863624,70.0162488979587,
12.));
#157249=CARTESIAN_POINT('Ctrl Pts',(-17.1545136876162,69.9922321229428,
0.));
#157250=CARTESIAN_POINT('Ctrl Pts',(-17.1545136876162,69.9922321229428,
12.));
#157251=CARTESIAN_POINT('Ctrl Pts',(-17.157177673114,69.9682545164942,0.));
#157252=CARTESIAN_POINT('Ctrl Pts',(-17.157177673114,69.9682545164942,12.));
#157253=CARTESIAN_POINT('Ctrl Pts',(-17.1598136899144,69.9443162026865,
0.));
#157254=CARTESIAN_POINT('Ctrl Pts',(-17.1598136899144,69.9443162026865,
12.));
#157255=CARTESIAN_POINT('Ctrl Pts',(-17.1624217853577,69.9204173060779,
0.));
#157256=CARTESIAN_POINT('Ctrl Pts',(-17.1624217853577,69.9204173060779,
12.));
#157257=CARTESIAN_POINT('Ctrl Pts',(-17.1650020070686,69.8965579517147,
0.));
#157258=CARTESIAN_POINT('Ctrl Pts',(-17.1650020070686,69.8965579517147,
12.));
#157259=CARTESIAN_POINT('Ctrl Pts',(-17.1675544029622,69.8727382651292,
0.));
#157260=CARTESIAN_POINT('Ctrl Pts',(-17.1675544029622,69.8727382651292,
12.));
#157261=CARTESIAN_POINT('Ctrl Pts',(-17.1700790212476,69.8489583723417,
0.));
#157262=CARTESIAN_POINT('Ctrl Pts',(-17.1700790212476,69.8489583723417,
12.));
#157263=CARTESIAN_POINT('Ctrl Pts',(-17.1725759104254,69.8252183998713,
0.));
#157264=CARTESIAN_POINT('Ctrl Pts',(-17.1725759104254,69.8252183998713,
12.));
#157265=CARTESIAN_POINT('Ctrl Pts',(-17.1750451192887,69.8015184747404,
0.));
#157266=CARTESIAN_POINT('Ctrl Pts',(-17.1750451192887,69.8015184747404,
12.));
#157267=CARTESIAN_POINT('Ctrl Pts',(-17.1774866969256,69.7778587244788,
0.));
#157268=CARTESIAN_POINT('Ctrl Pts',(-17.1774866969256,69.7778587244788,
12.));
#157269=CARTESIAN_POINT('Ctrl Pts',(-17.1799006927256,69.7542392771216,
0.));
#157270=CARTESIAN_POINT('Ctrl Pts',(-17.1799006927256,69.7542392771216,
12.));
#157271=CARTESIAN_POINT('Ctrl Pts',(-17.1822871563835,69.7306602612125,
0.));
#157272=CARTESIAN_POINT('Ctrl Pts',(-17.1822871563835,69.7306602612125,
12.));
#157273=CARTESIAN_POINT('Ctrl Pts',(-17.1846461378966,69.7071218058149,
0.));
#157274=CARTESIAN_POINT('Ctrl Pts',(-17.1846461378966,69.7071218058149,
12.));
#157275=CARTESIAN_POINT('Ctrl Pts',(-17.1869776875663,69.6836240405152,
0.));
#157276=CARTESIAN_POINT('Ctrl Pts',(-17.1869776875663,69.6836240405152,
12.));
#157277=CARTESIAN_POINT('Ctrl Pts',(-17.1892818560004,69.6601670954277,
0.));
#157278=CARTESIAN_POINT('Ctrl Pts',(-17.1892818560004,69.6601670954277,
12.));
#157279=CARTESIAN_POINT('Ctrl Pts',(-17.1915586941198,69.6367511011927,
0.));
#157280=CARTESIAN_POINT('Ctrl Pts',(-17.1915586941198,69.6367511011927,
12.));
#157281=CARTESIAN_POINT('Ctrl Pts',(-17.193808253162,69.6133761889787,0.));
#157282=CARTESIAN_POINT('Ctrl Pts',(-17.193808253162,69.6133761889787,12.));
#157283=CARTESIAN_POINT('Ctrl Pts',(-17.1960305846787,69.5900424904954,
0.));
#157284=CARTESIAN_POINT('Ctrl Pts',(-17.1960305846787,69.5900424904954,
12.));
#157285=CARTESIAN_POINT('Ctrl Pts',(-17.198225740538,69.5667501379984,0.));
#157286=CARTESIAN_POINT('Ctrl Pts',(-17.198225740538,69.5667501379984,12.));
#157287=CARTESIAN_POINT('Ctrl Pts',(-17.2003937729266,69.5434992642932,
0.));
#157288=CARTESIAN_POINT('Ctrl Pts',(-17.2003937729266,69.5434992642932,
12.));
#157289=CARTESIAN_POINT('Ctrl Pts',(-17.2025347343568,69.5202900027329,
0.));
#157290=CARTESIAN_POINT('Ctrl Pts',(-17.2025347343568,69.5202900027329,
12.));
#157291=CARTESIAN_POINT('Ctrl Pts',(-17.2046486776697,69.497122487222,0.));
#157292=CARTESIAN_POINT('Ctrl Pts',(-17.2046486776697,69.497122487222,12.));
#157293=CARTESIAN_POINT('Ctrl Pts',(-17.2067356560326,69.4739968522271,
0.));
#157294=CARTESIAN_POINT('Ctrl Pts',(-17.2067356560326,69.4739968522271,
12.));
#157295=CARTESIAN_POINT('Ctrl Pts',(-17.208795722942,69.4509132327836,0.));
#157296=CARTESIAN_POINT('Ctrl Pts',(-17.208795722942,69.4509132327836,12.));
#157297=CARTESIAN_POINT('Ctrl Pts',(-17.2108289322258,69.4278717644989,
0.));
#157298=CARTESIAN_POINT('Ctrl Pts',(-17.2108289322258,69.4278717644989,
12.));
#157299=CARTESIAN_POINT('Ctrl Pts',(-17.2128353380511,69.4048725835516,
0.));
#157300=CARTESIAN_POINT('Ctrl Pts',(-17.2128353380511,69.4048725835516,
12.));
#157301=CARTESIAN_POINT('Ctrl Pts',(-17.2148149949261,69.3819158266955,
0.));
#157302=CARTESIAN_POINT('Ctrl Pts',(-17.2148149949261,69.3819158266955,
12.));
#157303=CARTESIAN_POINT('Ctrl Pts',(-17.2167679576991,69.359001631272,0.));
#157304=CARTESIAN_POINT('Ctrl Pts',(-17.2167679576991,69.359001631272,12.));
#157305=CARTESIAN_POINT('Ctrl Pts',(-17.2186942815604,69.3361301352149,
0.));
#157306=CARTESIAN_POINT('Ctrl Pts',(-17.2186942815604,69.3361301352149,
12.));
#157307=CARTESIAN_POINT('Ctrl Pts',(-17.2205940220455,69.3133014770541,
0.));
#157308=CARTESIAN_POINT('Ctrl Pts',(-17.2205940220455,69.3133014770541,
12.));
#157309=CARTESIAN_POINT('Ctrl Pts',(-17.2224672350432,69.2905157959142,
0.));
#157310=CARTESIAN_POINT('Ctrl Pts',(-17.2224672350432,69.2905157959142,
12.));
#157311=CARTESIAN_POINT('Ctrl Pts',(-17.2243139767963,69.26777323152,0.));
#157312=CARTESIAN_POINT('Ctrl Pts',(-17.2243139767963,69.26777323152,12.));
#157313=CARTESIAN_POINT('Ctrl Pts',(-17.2261343039015,69.2450739242092,
0.));
#157314=CARTESIAN_POINT('Ctrl Pts',(-17.2261343039015,69.2450739242092,
12.));
#157315=CARTESIAN_POINT('Ctrl Pts',(-17.2279282733119,69.2224180149377,
0.));
#157316=CARTESIAN_POINT('Ctrl Pts',(-17.2279282733119,69.2224180149377,
12.));
#157317=CARTESIAN_POINT('Ctrl Pts',(-17.229695942341,69.1998056452837,0.));
#157318=CARTESIAN_POINT('Ctrl Pts',(-17.229695942341,69.1998056452837,12.));
#157319=CARTESIAN_POINT('Ctrl Pts',(-17.2314373686705,69.1772369574462,
0.));
#157320=CARTESIAN_POINT('Ctrl Pts',(-17.2314373686705,69.1772369574462,
12.));
#157321=CARTESIAN_POINT('Ctrl Pts',(-17.2331526103511,69.1547120942542,
0.));
#157322=CARTESIAN_POINT('Ctrl Pts',(-17.2331526103511,69.1547120942542,
12.));
#157323=CARTESIAN_POINT('Ctrl Pts',(-17.2348417258017,69.1322311991759,
0.));
#157324=CARTESIAN_POINT('Ctrl Pts',(-17.2348417258017,69.1322311991759,
12.));
#157325=CARTESIAN_POINT('Ctrl Pts',(-17.2365047738125,69.1097944163243,
0.));
#157326=CARTESIAN_POINT('Ctrl Pts',(-17.2365047738125,69.1097944163243,
12.));
#157327=CARTESIAN_POINT('Ctrl Pts',(-17.238141813549,69.0874018904598,0.));
#157328=CARTESIAN_POINT('Ctrl Pts',(-17.238141813549,69.0874018904598,12.));
#157329=CARTESIAN_POINT('Ctrl Pts',(-17.2397529045587,69.0650537669859,
0.));
#157330=CARTESIAN_POINT('Ctrl Pts',(-17.2397529045587,69.0650537669859,
12.));
#157331=CARTESIAN_POINT('Ctrl Pts',(-17.2413381067722,69.0427501919636,
0.));
#157332=CARTESIAN_POINT('Ctrl Pts',(-17.2413381067722,69.0427501919636,
12.));
#157333=CARTESIAN_POINT('Ctrl Pts',(-17.2428974805043,69.0204913121226,
0.));
#157334=CARTESIAN_POINT('Ctrl Pts',(-17.2428974805043,69.0204913121226,
12.));
#157335=CARTESIAN_POINT('Ctrl Pts',(-17.2444310864585,68.9982772748694,
0.));
#157336=CARTESIAN_POINT('Ctrl Pts',(-17.2444310864585,68.9982772748694,
12.));
#157337=CARTESIAN_POINT('Ctrl Pts',(-17.2459389857327,68.9761082282922,
0.));
#157338=CARTESIAN_POINT('Ctrl Pts',(-17.2459389857327,68.9761082282922,
12.));
#157339=CARTESIAN_POINT('Ctrl Pts',(-17.2474212398275,68.9539843211618,
0.));
#157340=CARTESIAN_POINT('Ctrl Pts',(-17.2474212398275,68.9539843211618,
12.));
#157341=CARTESIAN_POINT('Ctrl Pts',(-17.248877910643,68.9319057029407,0.));
#157342=CARTESIAN_POINT('Ctrl Pts',(-17.248877910643,68.9319057029407,12.));
#157343=CARTESIAN_POINT('Ctrl Pts',(-17.2503090604792,68.9098725237868,
0.));
#157344=CARTESIAN_POINT('Ctrl Pts',(-17.2503090604792,68.9098725237868,
12.));
#157345=CARTESIAN_POINT('Ctrl Pts',(-17.2517147520376,68.8878849345557,
0.));
#157346=CARTESIAN_POINT('Ctrl Pts',(-17.2517147520376,68.8878849345557,
12.));
#157347=CARTESIAN_POINT('Ctrl Pts',(-17.2530950484259,68.8659430867977,
0.));
#157348=CARTESIAN_POINT('Ctrl Pts',(-17.2530950484259,68.8659430867977,
12.));
#157349=CARTESIAN_POINT('Ctrl Pts',(-17.2544500131627,68.8440471327563,
0.));
#157350=CARTESIAN_POINT('Ctrl Pts',(-17.2544500131627,68.8440471327563,
12.));
#157351=CARTESIAN_POINT('Ctrl Pts',(-17.2557797101816,68.8221972253954,
0.));
#157352=CARTESIAN_POINT('Ctrl Pts',(-17.2557797101816,68.8221972253954,
12.));
#157353=CARTESIAN_POINT('Ctrl Pts',(-17.2570842038385,68.8003935184193,
0.));
#157354=CARTESIAN_POINT('Ctrl Pts',(-17.2570842038385,68.8003935184193,
12.));
#157355=CARTESIAN_POINT('Ctrl Pts',(-17.2583635589197,68.7786361662876,
0.));
#157356=CARTESIAN_POINT('Ctrl Pts',(-17.2583635589197,68.7786361662876,
12.));
#157357=CARTESIAN_POINT('Ctrl Pts',(-17.2596178406545,68.7569253242312,
0.));
#157358=CARTESIAN_POINT('Ctrl Pts',(-17.2596178406545,68.7569253242312,
12.));
#157359=CARTESIAN_POINT('Ctrl Pts',(-17.2608471147178,68.7352611482519,
0.));
#157360=CARTESIAN_POINT('Ctrl Pts',(-17.2608471147178,68.7352611482519,
12.));
#157361=CARTESIAN_POINT('Ctrl Pts',(-17.2620514472176,68.7136437951075,
0.));
#157362=CARTESIAN_POINT('Ctrl Pts',(-17.2620514472176,68.7136437951075,
12.));
#157363=CARTESIAN_POINT('Ctrl Pts',(-17.263230904689,68.6920734222932,0.));
#157364=CARTESIAN_POINT('Ctrl Pts',(-17.263230904689,68.6920734222932,12.));
#157365=CARTESIAN_POINT('Ctrl Pts',(-17.2643855540896,68.6705501880263,
0.));
#157366=CARTESIAN_POINT('Ctrl Pts',(-17.2643855540896,68.6705501880263,
12.));
#157367=CARTESIAN_POINT('Ctrl Pts',(-17.2655154627935,68.6490742512085,
0.));
#157368=CARTESIAN_POINT('Ctrl Pts',(-17.2655154627935,68.6490742512085,
12.));
#157369=CARTESIAN_POINT('Ctrl Pts',(-17.2666206986091,68.6276457714757,
0.));
#157370=CARTESIAN_POINT('Ctrl Pts',(-17.2666206986091,68.6276457714757,
12.));
#157371=CARTESIAN_POINT('Ctrl Pts',(-17.2677013298061,68.6062649092781,
0.));
#157372=CARTESIAN_POINT('Ctrl Pts',(-17.2677013298061,68.6062649092781,
12.));
#157373=CARTESIAN_POINT('Ctrl Pts',(-17.2687574251429,68.5849318259449,
0.));
#157374=CARTESIAN_POINT('Ctrl Pts',(-17.2687574251429,68.5849318259449,
12.));
#157375=CARTESIAN_POINT('Ctrl Pts',(-17.2697890538956,68.5636466837502,
0.));
#157376=CARTESIAN_POINT('Ctrl Pts',(-17.2697890538956,68.5636466837502,
12.));
#157377=CARTESIAN_POINT('Ctrl Pts',(-17.2707962858912,68.5424096459746,
0.));
#157378=CARTESIAN_POINT('Ctrl Pts',(-17.2707962858912,68.5424096459746,
12.));
#157379=CARTESIAN_POINT('Ctrl Pts',(-17.2717791914538,68.5212208767835,
0.));
#157380=CARTESIAN_POINT('Ctrl Pts',(-17.2717791914538,68.5212208767835,
12.));
#157381=CARTESIAN_POINT('Ctrl Pts',(-17.2727378413485,68.5000805410897,
0.));
#157382=CARTESIAN_POINT('Ctrl Pts',(-17.2727378413485,68.5000805410897,
12.));
#157383=CARTESIAN_POINT('Ctrl Pts',(-17.2736723067367,68.4789888044357,
0.));
#157384=CARTESIAN_POINT('Ctrl Pts',(-17.2736723067367,68.4789888044357,
12.));
#157385=CARTESIAN_POINT('Ctrl Pts',(-17.2745826591125,68.4579458328208,
0.));
#157386=CARTESIAN_POINT('Ctrl Pts',(-17.2745826591125,68.4579458328208,
12.));
#157387=CARTESIAN_POINT('Ctrl Pts',(-17.2754689703001,68.4369517926803,
0.));
#157388=CARTESIAN_POINT('Ctrl Pts',(-17.2754689703001,68.4369517926803,
12.));
#157389=CARTESIAN_POINT('Ctrl Pts',(-17.2763313126026,68.4160068512781,
0.));
#157390=CARTESIAN_POINT('Ctrl Pts',(-17.2763313126026,68.4160068512781,
12.));
#157391=CARTESIAN_POINT('Ctrl Pts',(-17.2771697589387,68.3951111770498,
0.));
#157392=CARTESIAN_POINT('Ctrl Pts',(-17.2771697589387,68.3951111770498,
12.));
#157393=CARTESIAN_POINT('Ctrl Pts',(-17.2779843829605,68.374264939895,0.));
#157394=CARTESIAN_POINT('Ctrl Pts',(-17.2779843829605,68.374264939895,12.));
#157395=CARTESIAN_POINT('Ctrl Pts',(-17.2787752592475,68.353468311648,0.));
#157396=CARTESIAN_POINT('Ctrl Pts',(-17.2787752592475,68.353468311648,12.));
#157397=CARTESIAN_POINT('Ctrl Pts',(-17.2795424631789,68.3327214657533,
0.));
#157398=CARTESIAN_POINT('Ctrl Pts',(-17.2795424631789,68.3327214657533,
12.));
#157399=CARTESIAN_POINT('Ctrl Pts',(-17.2802860705807,68.3120245763884,
0.));
#157400=CARTESIAN_POINT('Ctrl Pts',(-17.2802860705807,68.3120245763884,
12.));
#157401=CARTESIAN_POINT('Ctrl Pts',(-17.2810061574352,68.2913778177258,
0.));
#157402=CARTESIAN_POINT('Ctrl Pts',(-17.2810061574352,68.2913778177258,
12.));
#157403=CARTESIAN_POINT('Ctrl Pts',(-17.2817027995838,68.2707813631761,
0.));
#157404=CARTESIAN_POINT('Ctrl Pts',(-17.2817027995838,68.2707813631761,
12.));
#157405=CARTESIAN_POINT('Ctrl Pts',(-17.2823760723886,68.250235384512,0.));
#157406=CARTESIAN_POINT('Ctrl Pts',(-17.2823760723886,68.250235384512,12.));
#157407=CARTESIAN_POINT('Ctrl Pts',(-17.2830260513879,68.2297400535339,
0.));
#157408=CARTESIAN_POINT('Ctrl Pts',(-17.2830260513879,68.2297400535339,
12.));
#157409=CARTESIAN_POINT('Ctrl Pts',(-17.2836528130825,68.2092955440591,
0.));
#157410=CARTESIAN_POINT('Ctrl Pts',(-17.2836528130825,68.2092955440591,
12.));
#157411=CARTESIAN_POINT('Ctrl Pts',(-17.2842564355796,68.1889020335418,
0.));
#157412=CARTESIAN_POINT('Ctrl Pts',(-17.2842564355796,68.1889020335418,
12.));
#157413=CARTESIAN_POINT('Ctrl Pts',(-17.2848369995283,68.1685597054193,
0.));
#157414=CARTESIAN_POINT('Ctrl Pts',(-17.2848369995283,68.1685597054193,
12.));
#157415=CARTESIAN_POINT('Ctrl Pts',(-17.2853945882059,68.1482687493176,
0.));
#157416=CARTESIAN_POINT('Ctrl Pts',(-17.2853945882059,68.1482687493176,
12.));
#157417=CARTESIAN_POINT('Ctrl Pts',(-17.2859292855694,68.1280293561473,
0.));
#157418=CARTESIAN_POINT('Ctrl Pts',(-17.2859292855694,68.1280293561473,
12.));
#157419=CARTESIAN_POINT('Ctrl Pts',(-17.2864411745455,68.1078417137865,
0.));
#157420=CARTESIAN_POINT('Ctrl Pts',(-17.2864411745455,68.1078417137865,
12.));
#157421=CARTESIAN_POINT('Ctrl Pts',(-17.2869303355438,68.0877060033229,
0.));
#157422=CARTESIAN_POINT('Ctrl Pts',(-17.2869303355438,68.0877060033229,
12.));
#157423=CARTESIAN_POINT('Ctrl Pts',(-17.2873968440855,68.0676223930469,
0.));
#157424=CARTESIAN_POINT('Ctrl Pts',(-17.2873968440855,68.0676223930469,
12.));
#157425=CARTESIAN_POINT('Ctrl Pts',(-17.2878407730981,68.0475910442494,
0.));
#157426=CARTESIAN_POINT('Ctrl Pts',(-17.2878407730981,68.0475910442494,
12.));
#157427=CARTESIAN_POINT('Ctrl Pts',(-17.2882621974737,68.027612122741,0.));
#157428=CARTESIAN_POINT('Ctrl Pts',(-17.2882621974737,68.027612122741,12.));
#157429=CARTESIAN_POINT('Ctrl Pts',(-17.28866119774,68.007685808115,0.));
#157430=CARTESIAN_POINT('Ctrl Pts',(-17.28866119774,68.007685808115,12.));
#157431=CARTESIAN_POINT('Ctrl Pts',(-17.2890378644843,67.9878123049133,
0.));
#157432=CARTESIAN_POINT('Ctrl Pts',(-17.2890378644843,67.9878123049133,
12.));
#157433=CARTESIAN_POINT('Ctrl Pts',(-17.2893923013852,67.9679918502441,
0.));
#157434=CARTESIAN_POINT('Ctrl Pts',(-17.2893923013852,67.9679918502441,
12.));
#157435=CARTESIAN_POINT('Ctrl Pts',(-17.2897246158895,67.9482246901517,
0.));
#157436=CARTESIAN_POINT('Ctrl Pts',(-17.2897246158895,67.9482246901517,
12.));
#157437=CARTESIAN_POINT('Ctrl Pts',(-17.2900349103956,67.9285110571662,
0.));
#157438=CARTESIAN_POINT('Ctrl Pts',(-17.2900349103956,67.9285110571662,
12.));
#157439=CARTESIAN_POINT('Ctrl Pts',(-17.2903232740717,67.908851149676,0.));
#157440=CARTESIAN_POINT('Ctrl Pts',(-17.2903232740717,67.908851149676,12.));
#157441=CARTESIAN_POINT('Ctrl Pts',(-17.2905897724029,67.8892451049871,
0.));
#157442=CARTESIAN_POINT('Ctrl Pts',(-17.2905897724029,67.8892451049871,
12.));
#157443=CARTESIAN_POINT('Ctrl Pts',(-17.2908344459816,67.8696929979178,
0.));
#157444=CARTESIAN_POINT('Ctrl Pts',(-17.2908344459816,67.8696929979178,
12.));
#157445=CARTESIAN_POINT('Ctrl Pts',(-17.2910127431203,67.8540944890057,
0.));
